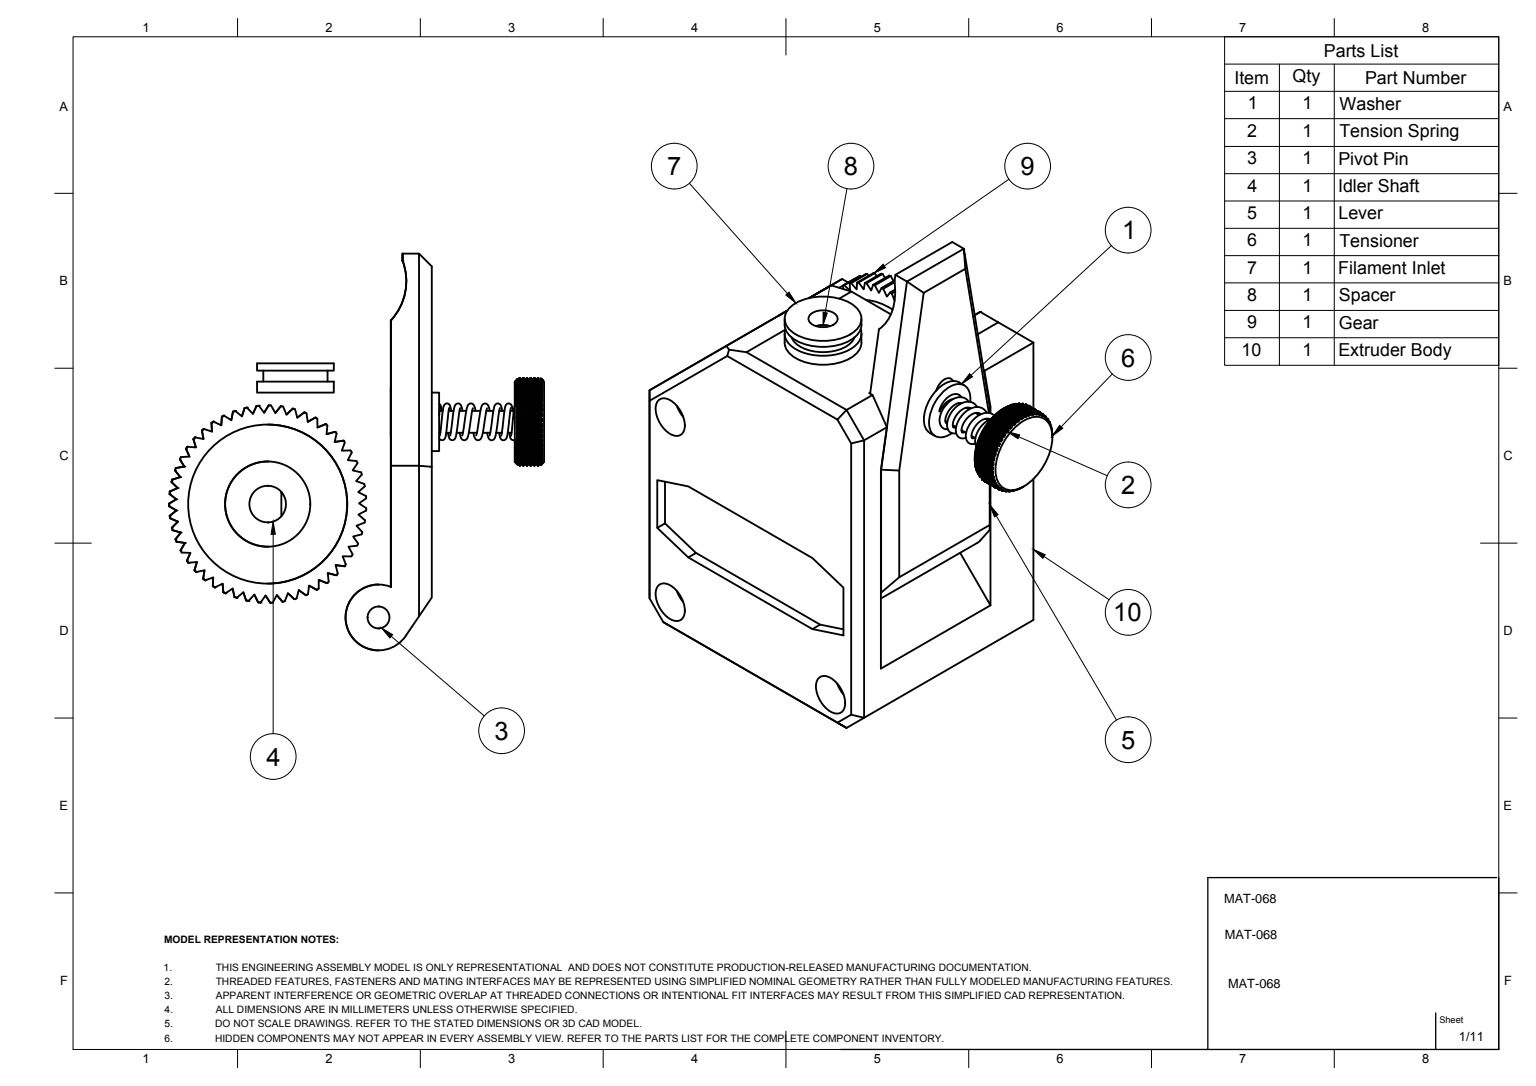
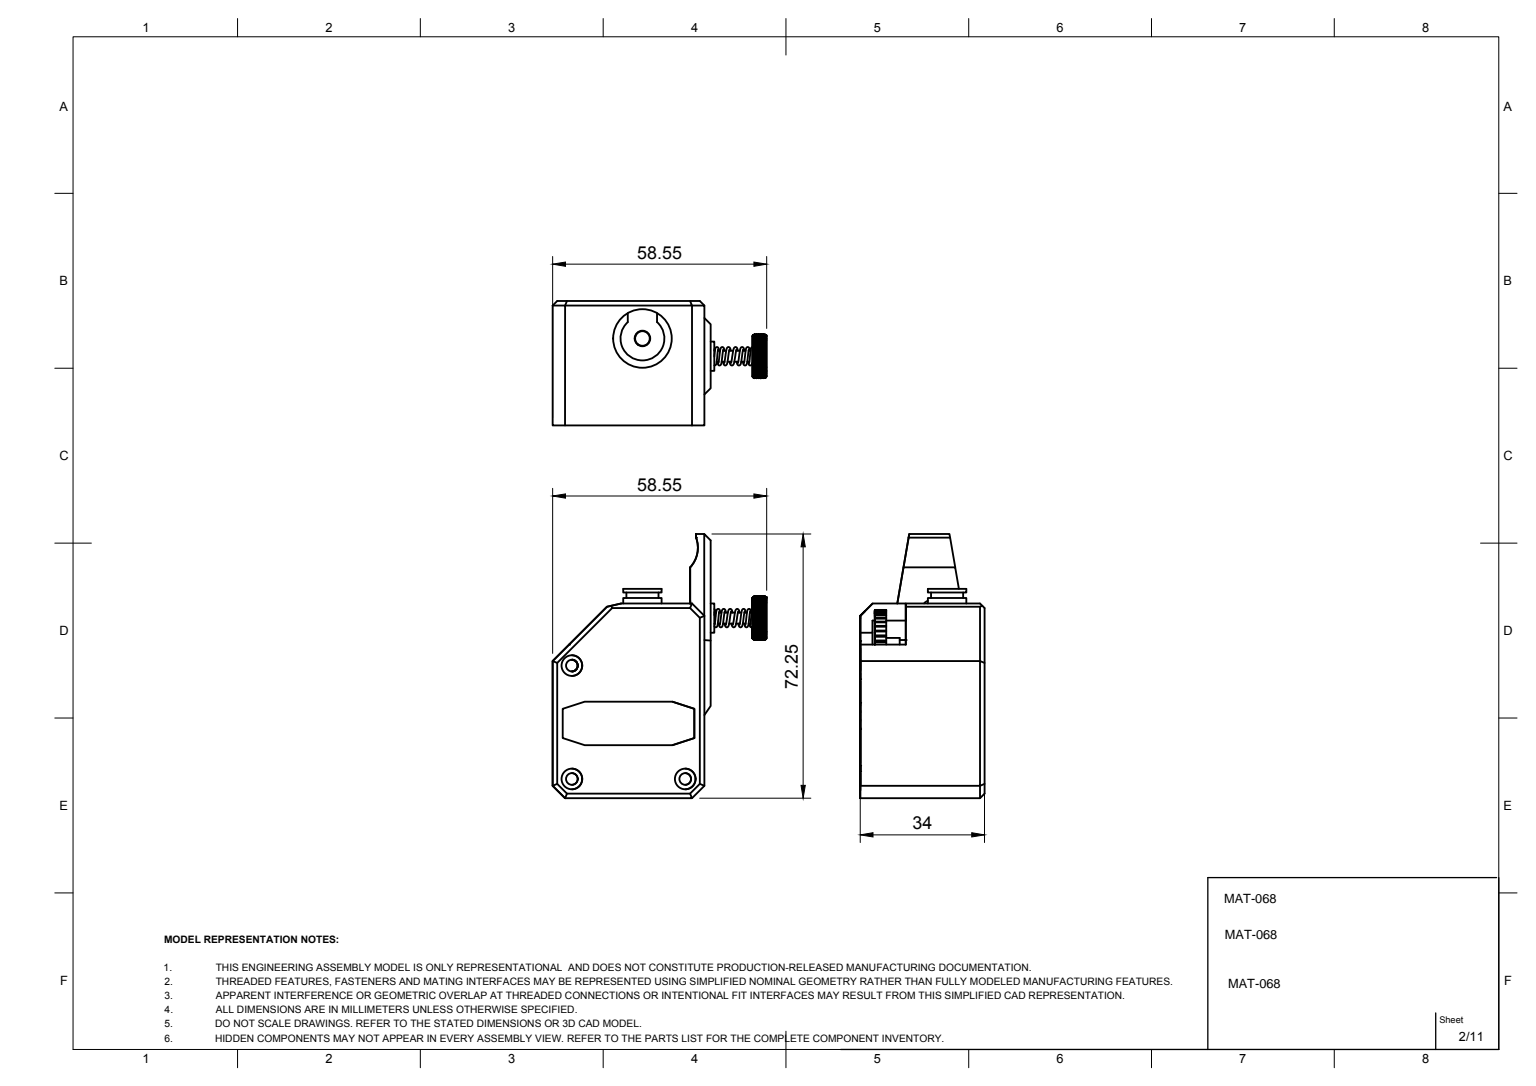
ISO-10303-21;
HEADER;
/* Generated by software containing ST-Developer
 * from STEP Tools, Inc. (www.steptools.com) 
 */

FILE_DESCRIPTION(
/* description */ ('CAx-IF Rec.Pracs.---Representation and Presentation of Product Manufa
cturing Information (PMI)---4.0---2014-10-13'),
/* implementation_level */ '2;1');

FILE_NAME(
/* name */ 'MAT-068',
/* time_stamp */ '2026-10-24T16:53:48-07:00',
/* author */ (''),
/* organization */ (''),
/* preprocessor_version */ 'ST-DEVELOPER v20.2',
/* originating_system */ 'Autodesk Translation Framework v15.17.0.0',
/* authorisation */ '');

FILE_SCHEMA (('AP242_MANAGED_MODEL_BASED_3D_ENGINEERING_MIM_LF { 1 0 10303 442 2 1 4 }'));
ENDSEC;

DATA;
#10=MECHANICAL_DESIGN_GEOMETRIC_PRESENTATION_REPRESENTATION('',(#3489,#3490,
#3491,#3492,#3493,#3494,#3495,#3496,#3497,#3498),#107910);
#11=ITEM_DEFINED_TRANSFORMATION($,$,#45659,#50366);
#12=ITEM_DEFINED_TRANSFORMATION($,$,#45668,#50367);
#13=ITEM_DEFINED_TRANSFORMATION($,$,#45671,#50368);
#14=ITEM_DEFINED_TRANSFORMATION($,$,#45680,#50369);
#15=ITEM_DEFINED_TRANSFORMATION($,$,#45688,#50370);
#16=ITEM_DEFINED_TRANSFORMATION($,$,#45717,#50371);
#17=ITEM_DEFINED_TRANSFORMATION($,$,#49877,#50372);
#18=ITEM_DEFINED_TRANSFORMATION($,$,#49890,#50373);
#19=ITEM_DEFINED_TRANSFORMATION($,$,#49899,#50374);
#20=ITEM_DEFINED_TRANSFORMATION($,$,#50173,#50375);
#21=(
REPRESENTATION_RELATIONSHIP($,$,#107947,#107946)
REPRESENTATION_RELATIONSHIP_WITH_TRANSFORMATION(#11)
SHAPE_REPRESENTATION_RELATIONSHIP()
);
#22=(
REPRESENTATION_RELATIONSHIP($,$,#107948,#107946)
REPRESENTATION_RELATIONSHIP_WITH_TRANSFORMATION(#12)
SHAPE_REPRESENTATION_RELATIONSHIP()
);
#23=(
REPRESENTATION_RELATIONSHIP($,$,#107949,#107946)
REPRESENTATION_RELATIONSHIP_WITH_TRANSFORMATION(#13)
SHAPE_REPRESENTATION_RELATIONSHIP()
);
#24=(
REPRESENTATION_RELATIONSHIP($,$,#107950,#107946)
REPRESENTATION_RELATIONSHIP_WITH_TRANSFORMATION(#14)
SHAPE_REPRESENTATION_RELATIONSHIP()
);
#25=(
REPRESENTATION_RELATIONSHIP($,$,#107951,#107946)
REPRESENTATION_RELATIONSHIP_WITH_TRANSFORMATION(#15)
SHAPE_REPRESENTATION_RELATIONSHIP()
);
#26=(
REPRESENTATION_RELATIONSHIP($,$,#107952,#107946)
REPRESENTATION_RELATIONSHIP_WITH_TRANSFORMATION(#16)
SHAPE_REPRESENTATION_RELATIONSHIP()
);
#27=(
REPRESENTATION_RELATIONSHIP($,$,#107953,#107946)
REPRESENTATION_RELATIONSHIP_WITH_TRANSFORMATION(#17)
SHAPE_REPRESENTATION_RELATIONSHIP()
);
#28=(
REPRESENTATION_RELATIONSHIP($,$,#107954,#107946)
REPRESENTATION_RELATIONSHIP_WITH_TRANSFORMATION(#18)
SHAPE_REPRESENTATION_RELATIONSHIP()
);
#29=(
REPRESENTATION_RELATIONSHIP($,$,#107955,#107946)
REPRESENTATION_RELATIONSHIP_WITH_TRANSFORMATION(#19)
SHAPE_REPRESENTATION_RELATIONSHIP()
);
#30=(
REPRESENTATION_RELATIONSHIP($,$,#107956,#107946)
REPRESENTATION_RELATIONSHIP_WITH_TRANSFORMATION(#20)
SHAPE_REPRESENTATION_RELATIONSHIP()
);
#31=CONTEXT_DEPENDENT_SHAPE_REPRESENTATION(#21,#107936);
#32=CONTEXT_DEPENDENT_SHAPE_REPRESENTATION(#22,#107937);
#33=CONTEXT_DEPENDENT_SHAPE_REPRESENTATION(#23,#107938);
#34=CONTEXT_DEPENDENT_SHAPE_REPRESENTATION(#24,#107939);
#35=CONTEXT_DEPENDENT_SHAPE_REPRESENTATION(#25,#107940);
#36=CONTEXT_DEPENDENT_SHAPE_REPRESENTATION(#26,#107941);
#37=CONTEXT_DEPENDENT_SHAPE_REPRESENTATION(#27,#107942);
#38=CONTEXT_DEPENDENT_SHAPE_REPRESENTATION(#28,#107943);
#39=CONTEXT_DEPENDENT_SHAPE_REPRESENTATION(#29,#107944);
#40=CONTEXT_DEPENDENT_SHAPE_REPRESENTATION(#30,#107945);
#41=NEXT_ASSEMBLY_USAGE_OCCURRENCE('Washer:1','Washer:1','Washer:1',#107958,
#107959,'Washer:1');
#42=NEXT_ASSEMBLY_USAGE_OCCURRENCE('Tension Spring:1',
'Tension Spring:1','Tension Spring:1',#107958,#107960,
'Tension Spring:1');
#43=NEXT_ASSEMBLY_USAGE_OCCURRENCE('Pivot Pin:1','Pivot Pin:1',
'Pivot Pin:1',#107958,#107961,'Pivot Pin:1');
#44=NEXT_ASSEMBLY_USAGE_OCCURRENCE('Idler Shaft:1','Idler Shaft:1',
'Idler Shaft:1',#107958,#107962,'Idler Shaft:1');
#45=NEXT_ASSEMBLY_USAGE_OCCURRENCE('Lever:1','Lever:1','Lever:1',#107958,
#107963,'Lever:1');
#46=NEXT_ASSEMBLY_USAGE_OCCURRENCE('Tensioner:1','Tensioner:1',
'Tensioner:1',#107958,#107964,'Tensioner:1');
#47=NEXT_ASSEMBLY_USAGE_OCCURRENCE('filament inlet:1',
'filament inlet:1','filament inlet:1',#107958,#107965,
'filament inlet:1');
#48=NEXT_ASSEMBLY_USAGE_OCCURRENCE('Spacer:1','Spacer:1','Spacer:1',#107958,
#107966,'Spacer:1');
#49=NEXT_ASSEMBLY_USAGE_OCCURRENCE('Gear:1','Gear:1','Gear:1',#107958,#107967,
'Gear:1');
#50=NEXT_ASSEMBLY_USAGE_OCCURRENCE('Extruder Body:1','Extruder Body:1',
'Extruder Body:1',#107958,#107968,'Extruder Body:1');
#51=(
BOUNDED_CURVE()
B_SPLINE_CURVE(2,(#91091,#91092,#91093,#91094,#91095),.UNSPECIFIED.,.F.,
 .F.)
B_SPLINE_CURVE_WITH_KNOTS((3,2,3),(0.457349576892943,0.480683592164461,
0.539236617436895),.UNSPECIFIED.)
CURVE()
GEOMETRIC_REPRESENTATION_ITEM()
RATIONAL_B_SPLINE_CURVE((0.999326490452302,0.99964606396824,1.,0.999111853439226,
0.998440080679707))
REPRESENTATION_ITEM('')
);
#52=(
BOUNDED_CURVE()
B_SPLINE_CURVE(2,(#91384,#91385,#91386,#91387,#91388),.UNSPECIFIED.,.F.,
 .F.)
B_SPLINE_CURVE_WITH_KNOTS((3,2,3),(0.457349576892961,0.480683592164461,
0.539236615838568),.UNSPECIFIED.)
CURVE()
GEOMETRIC_REPRESENTATION_ITEM()
RATIONAL_B_SPLINE_CURVE((0.999326490452302,0.999646063968241,1.,0.99911185346347,
0.998440080716382))
REPRESENTATION_ITEM('')
);
#53=(
BOUNDED_CURVE()
B_SPLINE_CURVE(2,(#91904,#91905,#91906,#91907,#91908),.UNSPECIFIED.,.F.,
 .F.)
B_SPLINE_CURVE_WITH_KNOTS((3,2,3),(0.457349576892952,0.480683592164462,
0.539236618408897),.UNSPECIFIED.)
CURVE()
GEOMETRIC_REPRESENTATION_ITEM()
RATIONAL_B_SPLINE_CURVE((0.999326490452302,0.999646063968241,1.,0.999111853424483,
0.998440080657404))
REPRESENTATION_ITEM('')
);
#54=(
BOUNDED_CURVE()
B_SPLINE_CURVE(2,(#92179,#92180,#92181,#92182,#92183),.UNSPECIFIED.,.F.,
 .F.)
B_SPLINE_CURVE_WITH_KNOTS((3,2,3),(0.457349576892958,0.480683592164462,
0.539236618408893),.UNSPECIFIED.)
CURVE()
GEOMETRIC_REPRESENTATION_ITEM()
RATIONAL_B_SPLINE_CURVE((0.999326490452302,0.999646063968241,1.,0.999111853424483,
0.998440080657404))
REPRESENTATION_ITEM('')
);
#55=(
BOUNDED_CURVE()
B_SPLINE_CURVE(2,(#92403,#92404,#92405,#92406,#92407),.UNSPECIFIED.,.F.,
 .F.)
B_SPLINE_CURVE_WITH_KNOTS((3,2,3),(0.457349576892958,0.480683592164463,
0.539236618408894),.UNSPECIFIED.)
CURVE()
GEOMETRIC_REPRESENTATION_ITEM()
RATIONAL_B_SPLINE_CURVE((0.999326490452302,0.999646063968241,1.,0.999111853424483,
0.998440080657404))
REPRESENTATION_ITEM('')
);
#56=(
BOUNDED_CURVE()
B_SPLINE_CURVE(2,(#92707,#92708,#92709,#92710,#92711),.UNSPECIFIED.,.F.,
 .F.)
B_SPLINE_CURVE_WITH_KNOTS((3,2,3),(0.457349576892963,0.480683592164461,
0.539236618408894),.UNSPECIFIED.)
CURVE()
GEOMETRIC_REPRESENTATION_ITEM()
RATIONAL_B_SPLINE_CURVE((0.999326490452302,0.999646063968241,1.,0.999111853424483,
0.998440080657404))
REPRESENTATION_ITEM('')
);
#57=(
BOUNDED_CURVE()
B_SPLINE_CURVE(2,(#93011,#93012,#93013,#93014,#93015),.UNSPECIFIED.,.F.,
 .F.)
B_SPLINE_CURVE_WITH_KNOTS((3,2,3),(0.457349576892959,0.480683592164461,
0.539236618408895),.UNSPECIFIED.)
CURVE()
GEOMETRIC_REPRESENTATION_ITEM()
RATIONAL_B_SPLINE_CURVE((0.999326490452302,0.999646063968241,1.,0.999111853424483,
0.998440080657404))
REPRESENTATION_ITEM('')
);
#58=(
BOUNDED_CURVE()
B_SPLINE_CURVE(2,(#93315,#93316,#93317,#93318,#93319),.UNSPECIFIED.,.F.,
 .F.)
B_SPLINE_CURVE_WITH_KNOTS((3,2,3),(0.457349576892959,0.480683592164461,
0.539236615838582),.UNSPECIFIED.)
CURVE()
GEOMETRIC_REPRESENTATION_ITEM()
RATIONAL_B_SPLINE_CURVE((0.999326490452302,0.999646063968241,1.,0.99911185346347,
0.998440080716382))
REPRESENTATION_ITEM('')
);
#59=(
BOUNDED_CURVE()
B_SPLINE_CURVE(2,(#93619,#93620,#93621,#93622,#93623),.UNSPECIFIED.,.F.,
 .F.)
B_SPLINE_CURVE_WITH_KNOTS((3,2,3),(0.457349576892961,0.480683592164461,
0.539236618408892),.UNSPECIFIED.)
CURVE()
GEOMETRIC_REPRESENTATION_ITEM()
RATIONAL_B_SPLINE_CURVE((0.999326490452302,0.999646063968241,1.,0.999111853424483,
0.998440080657404))
REPRESENTATION_ITEM('')
);
#60=(
BOUNDED_CURVE()
B_SPLINE_CURVE(2,(#93923,#93924,#93925,#93926,#93927),.UNSPECIFIED.,.F.,
 .F.)
B_SPLINE_CURVE_WITH_KNOTS((3,2,3),(0.457349576892952,0.480683592164462,
0.539236615838583),.UNSPECIFIED.)
CURVE()
GEOMETRIC_REPRESENTATION_ITEM()
RATIONAL_B_SPLINE_CURVE((0.999326490452302,0.999646063968241,1.,0.99911185346347,
0.998440080716382))
REPRESENTATION_ITEM('')
);
#61=(
BOUNDED_CURVE()
B_SPLINE_CURVE(2,(#94227,#94228,#94229,#94230,#94231),.UNSPECIFIED.,.F.,
 .F.)
B_SPLINE_CURVE_WITH_KNOTS((3,2,3),(0.457349576892963,0.48068359216447,0.539236618408901),
 .UNSPECIFIED.)
CURVE()
GEOMETRIC_REPRESENTATION_ITEM()
RATIONAL_B_SPLINE_CURVE((0.999326490452302,0.999646063968241,1.,0.999111853424483,
0.998440080657404))
REPRESENTATION_ITEM('')
);
#62=(
BOUNDED_CURVE()
B_SPLINE_CURVE(2,(#94531,#94532,#94533,#94534,#94535),.UNSPECIFIED.,.F.,
 .F.)
B_SPLINE_CURVE_WITH_KNOTS((3,2,3),(0.457349576892948,0.48068359216446,0.539236618408892),
 .UNSPECIFIED.)
CURVE()
GEOMETRIC_REPRESENTATION_ITEM()
RATIONAL_B_SPLINE_CURVE((0.999326490452302,0.999646063968241,1.,0.999111853424483,
0.998440080657404))
REPRESENTATION_ITEM('')
);
#63=(
BOUNDED_CURVE()
B_SPLINE_CURVE(2,(#94835,#94836,#94837,#94838,#94839),.UNSPECIFIED.,.F.,
 .F.)
B_SPLINE_CURVE_WITH_KNOTS((3,2,3),(0.457349576892957,0.480683592164462,
0.539236618408896),.UNSPECIFIED.)
CURVE()
GEOMETRIC_REPRESENTATION_ITEM()
RATIONAL_B_SPLINE_CURVE((0.999326490452302,0.999646063968241,1.,0.999111853424483,
0.998440080657404))
REPRESENTATION_ITEM('')
);
#64=(
BOUNDED_CURVE()
B_SPLINE_CURVE(2,(#95139,#95140,#95141,#95142,#95143),.UNSPECIFIED.,.F.,
 .F.)
B_SPLINE_CURVE_WITH_KNOTS((3,2,3),(0.457349576892956,0.48068359216446,0.539236617436898),
 .UNSPECIFIED.)
CURVE()
GEOMETRIC_REPRESENTATION_ITEM()
RATIONAL_B_SPLINE_CURVE((0.999326490452302,0.999646063968241,1.,0.999111853439226,
0.998440080679707))
REPRESENTATION_ITEM('')
);
#65=(
BOUNDED_CURVE()
B_SPLINE_CURVE(2,(#95443,#95444,#95445,#95446,#95447),.UNSPECIFIED.,.F.,
 .F.)
B_SPLINE_CURVE_WITH_KNOTS((3,2,3),(0.457349576892961,0.480683592164473,
0.539236615838594),.UNSPECIFIED.)
CURVE()
GEOMETRIC_REPRESENTATION_ITEM()
RATIONAL_B_SPLINE_CURVE((0.999326490452302,0.999646063968241,1.,0.99911185346347,
0.998440080716382))
REPRESENTATION_ITEM('')
);
#66=(
BOUNDED_CURVE()
B_SPLINE_CURVE(2,(#95747,#95748,#95749,#95750,#95751),.UNSPECIFIED.,.F.,
 .F.)
B_SPLINE_CURVE_WITH_KNOTS((3,2,3),(0.457349576892959,0.480683592164459,
0.539236618408898),.UNSPECIFIED.)
CURVE()
GEOMETRIC_REPRESENTATION_ITEM()
RATIONAL_B_SPLINE_CURVE((0.999326490452302,0.999646063968241,1.,0.999111853424483,
0.998440080657404))
REPRESENTATION_ITEM('')
);
#67=(
BOUNDED_CURVE()
B_SPLINE_CURVE(2,(#96051,#96052,#96053,#96054,#96055),.UNSPECIFIED.,.F.,
 .F.)
B_SPLINE_CURVE_WITH_KNOTS((3,2,3),(0.457349576892962,0.480683592164469,
0.539236618408905),.UNSPECIFIED.)
CURVE()
GEOMETRIC_REPRESENTATION_ITEM()
RATIONAL_B_SPLINE_CURVE((0.999326490452302,0.999646063968241,1.,0.999111853424483,
0.998440080657404))
REPRESENTATION_ITEM('')
);
#68=(
BOUNDED_CURVE()
B_SPLINE_CURVE(2,(#96355,#96356,#96357,#96358,#96359),.UNSPECIFIED.,.F.,
 .F.)
B_SPLINE_CURVE_WITH_KNOTS((3,2,3),(0.457349576892966,0.480683592164469,
0.539236618408905),.UNSPECIFIED.)
CURVE()
GEOMETRIC_REPRESENTATION_ITEM()
RATIONAL_B_SPLINE_CURVE((0.999326490452302,0.999646063968241,1.,0.999111853424483,
0.998440080657404))
REPRESENTATION_ITEM('')
);
#69=(
BOUNDED_CURVE()
B_SPLINE_CURVE(2,(#96659,#96660,#96661,#96662,#96663),.UNSPECIFIED.,.F.,
 .F.)
B_SPLINE_CURVE_WITH_KNOTS((3,2,3),(0.457349576892951,0.48068359216446,0.539236618408896),
 .UNSPECIFIED.)
CURVE()
GEOMETRIC_REPRESENTATION_ITEM()
RATIONAL_B_SPLINE_CURVE((0.999326490452302,0.999646063968241,1.,0.999111853424483,
0.998440080657404))
REPRESENTATION_ITEM('')
);
#70=(
BOUNDED_CURVE()
B_SPLINE_CURVE(2,(#96963,#96964,#96965,#96966,#96967),.UNSPECIFIED.,.F.,
 .F.)
B_SPLINE_CURVE_WITH_KNOTS((3,2,3),(0.457349576892956,0.480683592164461,
0.539236618408896),.UNSPECIFIED.)
CURVE()
GEOMETRIC_REPRESENTATION_ITEM()
RATIONAL_B_SPLINE_CURVE((0.999326490452302,0.999646063968241,1.,0.999111853424483,
0.998440080657404))
REPRESENTATION_ITEM('')
);
#71=(
BOUNDED_CURVE()
B_SPLINE_CURVE(2,(#97267,#97268,#97269,#97270,#97271),.UNSPECIFIED.,.F.,
 .F.)
B_SPLINE_CURVE_WITH_KNOTS((3,2,3),(0.457349576892952,0.480683592164461,
0.539236618408892),.UNSPECIFIED.)
CURVE()
GEOMETRIC_REPRESENTATION_ITEM()
RATIONAL_B_SPLINE_CURVE((0.999326490452302,0.999646063968241,1.,0.999111853424483,
0.998440080657404))
REPRESENTATION_ITEM('')
);
#72=(
BOUNDED_CURVE()
B_SPLINE_CURVE(2,(#97571,#97572,#97573,#97574,#97575),.UNSPECIFIED.,.F.,
 .F.)
B_SPLINE_CURVE_WITH_KNOTS((3,2,3),(0.457349576892964,0.480683592164459,
0.539236618408898),.UNSPECIFIED.)
CURVE()
GEOMETRIC_REPRESENTATION_ITEM()
RATIONAL_B_SPLINE_CURVE((0.999326490452302,0.999646063968241,1.,0.999111853424483,
0.998440080657404))
REPRESENTATION_ITEM('')
);
#73=(
BOUNDED_CURVE()
B_SPLINE_CURVE(2,(#97875,#97876,#97877,#97878,#97879),.UNSPECIFIED.,.F.,
 .F.)
B_SPLINE_CURVE_WITH_KNOTS((3,2,3),(0.457349576892949,0.480683592164462,
0.539236618408898),.UNSPECIFIED.)
CURVE()
GEOMETRIC_REPRESENTATION_ITEM()
RATIONAL_B_SPLINE_CURVE((0.999326490452302,0.999646063968241,1.,0.999111853424483,
0.998440080657404))
REPRESENTATION_ITEM('')
);
#74=(
BOUNDED_CURVE()
B_SPLINE_CURVE(2,(#98179,#98180,#98181,#98182,#98183),.UNSPECIFIED.,.F.,
 .F.)
B_SPLINE_CURVE_WITH_KNOTS((3,2,3),(0.457349576892952,0.48068359216446,0.539236615838581),
 .UNSPECIFIED.)
CURVE()
GEOMETRIC_REPRESENTATION_ITEM()
RATIONAL_B_SPLINE_CURVE((0.999326490452302,0.999646063968241,1.,0.99911185346347,
0.998440080716382))
REPRESENTATION_ITEM('')
);
#75=(
BOUNDED_CURVE()
B_SPLINE_CURVE(2,(#98483,#98484,#98485,#98486,#98487),.UNSPECIFIED.,.F.,
 .F.)
B_SPLINE_CURVE_WITH_KNOTS((3,2,3),(0.457349576892958,0.48068359216446,0.539236618408894),
 .UNSPECIFIED.)
CURVE()
GEOMETRIC_REPRESENTATION_ITEM()
RATIONAL_B_SPLINE_CURVE((0.999326490452302,0.999646063968241,1.,0.999111853424483,
0.998440080657404))
REPRESENTATION_ITEM('')
);
#76=(
BOUNDED_CURVE()
B_SPLINE_CURVE(2,(#98787,#98788,#98789,#98790,#98791),.UNSPECIFIED.,.F.,
 .F.)
B_SPLINE_CURVE_WITH_KNOTS((3,2,3),(0.457349576892947,0.480683592164461,
0.539236617436902),.UNSPECIFIED.)
CURVE()
GEOMETRIC_REPRESENTATION_ITEM()
RATIONAL_B_SPLINE_CURVE((0.999326490452302,0.999646063968241,1.,0.999111853439226,
0.998440080679707))
REPRESENTATION_ITEM('')
);
#77=(
BOUNDED_CURVE()
B_SPLINE_CURVE(2,(#99091,#99092,#99093,#99094,#99095),.UNSPECIFIED.,.F.,
 .F.)
B_SPLINE_CURVE_WITH_KNOTS((3,2,3),(0.457349576892974,0.48068359216447,0.539236615838595),
 .UNSPECIFIED.)
CURVE()
GEOMETRIC_REPRESENTATION_ITEM()
RATIONAL_B_SPLINE_CURVE((0.999326490452302,0.999646063968241,1.,0.99911185346347,
0.998440080716382))
REPRESENTATION_ITEM('')
);
#78=(
BOUNDED_CURVE()
B_SPLINE_CURVE(2,(#99395,#99396,#99397,#99398,#99399),.UNSPECIFIED.,.F.,
 .F.)
B_SPLINE_CURVE_WITH_KNOTS((3,2,3),(0.457349576892952,0.480683592164461,
0.539236615838591),.UNSPECIFIED.)
CURVE()
GEOMETRIC_REPRESENTATION_ITEM()
RATIONAL_B_SPLINE_CURVE((0.999326490452302,0.999646063968241,1.,0.99911185346347,
0.998440080716382))
REPRESENTATION_ITEM('')
);
#79=(
BOUNDED_CURVE()
B_SPLINE_CURVE(2,(#99699,#99700,#99701,#99702,#99703),.UNSPECIFIED.,.F.,
 .F.)
B_SPLINE_CURVE_WITH_KNOTS((3,2,3),(0.457349576892966,0.480683592164471,
0.539236615838593),.UNSPECIFIED.)
CURVE()
GEOMETRIC_REPRESENTATION_ITEM()
RATIONAL_B_SPLINE_CURVE((0.999326490452302,0.999646063968241,1.,0.99911185346347,
0.998440080716382))
REPRESENTATION_ITEM('')
);
#80=(
BOUNDED_CURVE()
B_SPLINE_CURVE(2,(#100003,#100004,#100005,#100006,#100007),
 .UNSPECIFIED.,.F.,.F.)
B_SPLINE_CURVE_WITH_KNOTS((3,2,3),(0.457349576892955,0.48068359216446,0.539236618408892),
 .UNSPECIFIED.)
CURVE()
GEOMETRIC_REPRESENTATION_ITEM()
RATIONAL_B_SPLINE_CURVE((0.999326490452302,0.999646063968241,1.,0.999111853424483,
0.998440080657404))
REPRESENTATION_ITEM('')
);
#81=(
BOUNDED_CURVE()
B_SPLINE_CURVE(2,(#100307,#100308,#100309,#100310,#100311),
 .UNSPECIFIED.,.F.,.F.)
B_SPLINE_CURVE_WITH_KNOTS((3,2,3),(0.457349576892948,0.480683592164461,
0.539236618408894),.UNSPECIFIED.)
CURVE()
GEOMETRIC_REPRESENTATION_ITEM()
RATIONAL_B_SPLINE_CURVE((0.999326490452302,0.999646063968241,1.,0.999111853424483,
0.998440080657404))
REPRESENTATION_ITEM('')
);
#82=(
BOUNDED_CURVE()
B_SPLINE_CURVE(2,(#100611,#100612,#100613,#100614,#100615),
 .UNSPECIFIED.,.F.,.F.)
B_SPLINE_CURVE_WITH_KNOTS((3,2,3),(0.457349576892958,0.480683592164462,
0.539236615838579),.UNSPECIFIED.)
CURVE()
GEOMETRIC_REPRESENTATION_ITEM()
RATIONAL_B_SPLINE_CURVE((0.999326490452302,0.999646063968241,1.,0.99911185346347,
0.998440080716382))
REPRESENTATION_ITEM('')
);
#83=(
BOUNDED_CURVE()
B_SPLINE_CURVE(2,(#100915,#100916,#100917,#100918,#100919),
 .UNSPECIFIED.,.F.,.F.)
B_SPLINE_CURVE_WITH_KNOTS((3,2,3),(0.457349576892956,0.48068359216446,0.539236618408897),
 .UNSPECIFIED.)
CURVE()
GEOMETRIC_REPRESENTATION_ITEM()
RATIONAL_B_SPLINE_CURVE((0.999326490452302,0.999646063968241,1.,0.999111853424483,
0.998440080657404))
REPRESENTATION_ITEM('')
);
#84=(
BOUNDED_CURVE()
B_SPLINE_CURVE(2,(#101219,#101220,#101221,#101222,#101223),
 .UNSPECIFIED.,.F.,.F.)
B_SPLINE_CURVE_WITH_KNOTS((3,2,3),(0.457349576892958,0.480683592164462,
0.539236618408895),.UNSPECIFIED.)
CURVE()
GEOMETRIC_REPRESENTATION_ITEM()
RATIONAL_B_SPLINE_CURVE((0.999326490452302,0.999646063968241,1.,0.999111853424483,
0.998440080657404))
REPRESENTATION_ITEM('')
);
#85=(
BOUNDED_CURVE()
B_SPLINE_CURVE(2,(#101523,#101524,#101525,#101526,#101527),
 .UNSPECIFIED.,.F.,.F.)
B_SPLINE_CURVE_WITH_KNOTS((3,2,3),(0.457349576892956,0.480683592164458,
0.539236615838573),.UNSPECIFIED.)
CURVE()
GEOMETRIC_REPRESENTATION_ITEM()
RATIONAL_B_SPLINE_CURVE((0.999326490452302,0.999646063968241,1.,0.99911185346347,
0.998440080716382))
REPRESENTATION_ITEM('')
);
#86=(
BOUNDED_CURVE()
B_SPLINE_CURVE(2,(#101827,#101828,#101829,#101830,#101831),
 .UNSPECIFIED.,.F.,.F.)
B_SPLINE_CURVE_WITH_KNOTS((3,2,3),(0.457349576892953,0.48068359216446,0.539236618408898),
 .UNSPECIFIED.)
CURVE()
GEOMETRIC_REPRESENTATION_ITEM()
RATIONAL_B_SPLINE_CURVE((0.999326490452302,0.999646063968241,1.,0.999111853424483,
0.998440080657404))
REPRESENTATION_ITEM('')
);
#87=(
BOUNDED_CURVE()
B_SPLINE_CURVE(2,(#102131,#102132,#102133,#102134,#102135),
 .UNSPECIFIED.,.F.,.F.)
B_SPLINE_CURVE_WITH_KNOTS((3,2,3),(0.457349576892963,0.480683592164461,
0.539236618408896),.UNSPECIFIED.)
CURVE()
GEOMETRIC_REPRESENTATION_ITEM()
RATIONAL_B_SPLINE_CURVE((0.999326490452302,0.999646063968241,1.,0.999111853424483,
0.998440080657404))
REPRESENTATION_ITEM('')
);
#88=(
BOUNDED_CURVE()
B_SPLINE_CURVE(2,(#102435,#102436,#102437,#102438,#102439),
 .UNSPECIFIED.,.F.,.F.)
B_SPLINE_CURVE_WITH_KNOTS((3,2,3),(0.457349576892965,0.480683592164474,
0.539236615838598),.UNSPECIFIED.)
CURVE()
GEOMETRIC_REPRESENTATION_ITEM()
RATIONAL_B_SPLINE_CURVE((0.999326490452302,0.999646063968241,1.,0.99911185346347,
0.998440080716382))
REPRESENTATION_ITEM('')
);
#89=(
BOUNDED_CURVE()
B_SPLINE_CURVE(2,(#102739,#102740,#102741,#102742,#102743),
 .UNSPECIFIED.,.F.,.F.)
B_SPLINE_CURVE_WITH_KNOTS((3,2,3),(0.457349576892951,0.480683592164463,
0.5392366174369),.UNSPECIFIED.)
CURVE()
GEOMETRIC_REPRESENTATION_ITEM()
RATIONAL_B_SPLINE_CURVE((0.999326490452302,0.999646063968241,1.,0.999111853439226,
0.998440080679707))
REPRESENTATION_ITEM('')
);
#90=(
BOUNDED_CURVE()
B_SPLINE_CURVE(2,(#103043,#103044,#103045,#103046,#103047),
 .UNSPECIFIED.,.F.,.F.)
B_SPLINE_CURVE_WITH_KNOTS((3,2,3),(0.45734957689296,0.480683592164459,0.539236618408886),
 .UNSPECIFIED.)
CURVE()
GEOMETRIC_REPRESENTATION_ITEM()
RATIONAL_B_SPLINE_CURVE((0.999326490452302,0.999646063968241,1.,0.999111853424483,
0.998440080657404))
REPRESENTATION_ITEM('')
);
#91=(
BOUNDED_CURVE()
B_SPLINE_CURVE(2,(#103347,#103348,#103349,#103350,#103351),
 .UNSPECIFIED.,.F.,.F.)
B_SPLINE_CURVE_WITH_KNOTS((3,2,3),(0.457349576892963,0.48068359216447,0.5392366184089),
 .UNSPECIFIED.)
CURVE()
GEOMETRIC_REPRESENTATION_ITEM()
RATIONAL_B_SPLINE_CURVE((0.999326490452302,0.999646063968241,1.,0.999111853424483,
0.998440080657404))
REPRESENTATION_ITEM('')
);
#92=(
BOUNDED_CURVE()
B_SPLINE_CURVE(2,(#103651,#103652,#103653,#103654,#103655),
 .UNSPECIFIED.,.F.,.F.)
B_SPLINE_CURVE_WITH_KNOTS((3,2,3),(0.457349576892972,0.480683592164467,
0.539236618408904),.UNSPECIFIED.)
CURVE()
GEOMETRIC_REPRESENTATION_ITEM()
RATIONAL_B_SPLINE_CURVE((0.999326490452302,0.999646063968241,1.,0.999111853424483,
0.998440080657404))
REPRESENTATION_ITEM('')
);
#93=(
BOUNDED_CURVE()
B_SPLINE_CURVE(2,(#103955,#103956,#103957,#103958,#103959),
 .UNSPECIFIED.,.F.,.F.)
B_SPLINE_CURVE_WITH_KNOTS((3,2,3),(0.457349576892955,0.480683592164463,
0.539236618408902),.UNSPECIFIED.)
CURVE()
GEOMETRIC_REPRESENTATION_ITEM()
RATIONAL_B_SPLINE_CURVE((0.999326490452302,0.999646063968241,1.,0.999111853424483,
0.998440080657404))
REPRESENTATION_ITEM('')
);
#94=(
BOUNDED_CURVE()
B_SPLINE_CURVE(2,(#104259,#104260,#104261,#104262,#104263),
 .UNSPECIFIED.,.F.,.F.)
B_SPLINE_CURVE_WITH_KNOTS((3,2,3),(0.457349576892956,0.48068359216446,0.539236618408889),
 .UNSPECIFIED.)
CURVE()
GEOMETRIC_REPRESENTATION_ITEM()
RATIONAL_B_SPLINE_CURVE((0.999326490452302,0.999646063968241,1.,0.999111853424483,
0.998440080657404))
REPRESENTATION_ITEM('')
);
#95=(
BOUNDED_CURVE()
B_SPLINE_CURVE(2,(#104563,#104564,#104565,#104566,#104567),
 .UNSPECIFIED.,.F.,.F.)
B_SPLINE_CURVE_WITH_KNOTS((3,2,3),(0.457349576892965,0.480683592164471,
0.539236618408903),.UNSPECIFIED.)
CURVE()
GEOMETRIC_REPRESENTATION_ITEM()
RATIONAL_B_SPLINE_CURVE((0.999326490452302,0.999646063968241,1.,0.999111853424483,
0.998440080657404))
REPRESENTATION_ITEM('')
);
#96=(
BOUNDED_CURVE()
B_SPLINE_CURVE(2,(#104867,#104868,#104869,#104870,#104871),
 .UNSPECIFIED.,.F.,.F.)
B_SPLINE_CURVE_WITH_KNOTS((3,2,3),(0.457349576892956,0.480683592164462,
0.539236618408896),.UNSPECIFIED.)
CURVE()
GEOMETRIC_REPRESENTATION_ITEM()
RATIONAL_B_SPLINE_CURVE((0.999326490452302,0.999646063968241,1.,0.999111853424483,
0.998440080657404))
REPRESENTATION_ITEM('')
);
#97=(
BOUNDED_CURVE()
B_SPLINE_CURVE(2,(#105171,#105172,#105173,#105174,#105175),
 .UNSPECIFIED.,.F.,.F.)
B_SPLINE_CURVE_WITH_KNOTS((3,2,3),(0.45734957689296,0.480683592164462,0.539236618408894),
 .UNSPECIFIED.)
CURVE()
GEOMETRIC_REPRESENTATION_ITEM()
RATIONAL_B_SPLINE_CURVE((0.999326490452302,0.999646063968241,1.,0.999111853424483,
0.998440080657404))
REPRESENTATION_ITEM('')
);
#98=(
BOUNDED_CURVE()
B_SPLINE_CURVE(2,(#105475,#105476,#105477,#105478,#105479),
 .UNSPECIFIED.,.F.,.F.)
B_SPLINE_CURVE_WITH_KNOTS((3,2,3),(0.457349576892957,0.480683592164459,
0.539236618408901),.UNSPECIFIED.)
CURVE()
GEOMETRIC_REPRESENTATION_ITEM()
RATIONAL_B_SPLINE_CURVE((0.999326490452302,0.999646063968241,1.,0.999111853424483,
0.998440080657404))
REPRESENTATION_ITEM('')
);
#99=(
BOUNDED_CURVE()
B_SPLINE_CURVE(2,(#105779,#105780,#105781,#105782,#105783),
 .UNSPECIFIED.,.F.,.F.)
B_SPLINE_CURVE_WITH_KNOTS((3,2,3),(0.457349576892957,0.480683592164462,
0.539236615838586),.UNSPECIFIED.)
CURVE()
GEOMETRIC_REPRESENTATION_ITEM()
RATIONAL_B_SPLINE_CURVE((0.999326490452302,0.999646063968241,1.,0.99911185346347,
0.998440080716382))
REPRESENTATION_ITEM('')
);
#100=(
BOUNDED_CURVE()
B_SPLINE_CURVE(2,(#106083,#106084,#106085,#106086,#106087),
 .UNSPECIFIED.,.F.,.F.)
B_SPLINE_CURVE_WITH_KNOTS((3,2,3),(0.457349576892964,0.480683592164471,
0.539236615838594),.UNSPECIFIED.)
CURVE()
GEOMETRIC_REPRESENTATION_ITEM()
RATIONAL_B_SPLINE_CURVE((0.999326490452302,0.999646063968241,1.,0.99911185346347,
0.998440080716382))
REPRESENTATION_ITEM('')
);
#101=(
BOUNDED_SURFACE()
B_SPLINE_SURFACE(1,2,((#65259,#65260,#65261),(#65262,#65263,#65264)),
 .UNSPECIFIED.,.F.,.F.,.F.)
B_SPLINE_SURFACE_WITH_KNOTS((2,2),(3,3),(0.,1.),(0.0556006976418392,0.0675888856590501),
 .UNSPECIFIED.)
GEOMETRIC_REPRESENTATION_ITEM()
RATIONAL_B_SPLINE_SURFACE(((0.996397562408606,0.996150386832629,0.997319912843745),
(0.996397562408606,0.996150386832629,0.997319912843745)))
REPRESENTATION_ITEM('')
SURFACE()
);
#102=(
BOUNDED_SURFACE()
B_SPLINE_SURFACE(1,2,((#65277,#65278,#65279),(#65280,#65281,#65282),(#65283,
#65284,#65285)),.UNSPECIFIED.,.F.,.F.,.F.)
B_SPLINE_SURFACE_WITH_KNOTS((2,1,2),(3,3),(-0.000171761237665326,1.,1.00600020634817),
(0.066589869885605,0.0751324139155164),.UNSPECIFIED.)
GEOMETRIC_REPRESENTATION_ITEM()
RATIONAL_B_SPLINE_SURFACE(((0.997134830028878,0.997884084852412,0.999352698774608),
(0.997134830028878,0.997884084852412,0.999352698774608),(0.997134830028879,
0.997884084852412,0.999352698774608)))
REPRESENTATION_ITEM('')
SURFACE()
);
#103=(
BOUNDED_SURFACE()
B_SPLINE_SURFACE(1,2,((#65395,#65396,#65397),(#65398,#65399,#65400),(#65401,
#65402,#65403)),.UNSPECIFIED.,.F.,.F.,.F.)
B_SPLINE_SURFACE_WITH_KNOTS((2,1,2),(3,3),(0.,1.,1.01),(0.0456081671210044,
0.057598944781882),.UNSPECIFIED.)
GEOMETRIC_REPRESENTATION_ITEM()
RATIONAL_B_SPLINE_SURFACE(((0.997793907739636,0.996365558499688,0.996354522974128),
(0.997793907739636,0.996365558499688,0.996354522974128),(0.997793907739636,
0.996365558499688,0.996354522974128)))
REPRESENTATION_ITEM('')
SURFACE()
);
#104=(
BOUNDED_SURFACE()
B_SPLINE_SURFACE(1,2,((#65416,#65417,#65418),(#65419,#65420,#65421),(#65422,
#65423,#65424)),.UNSPECIFIED.,.F.,.F.,.F.)
B_SPLINE_SURFACE_WITH_KNOTS((2,1,2),(3,3),(0.,1.,1.01),(0.0556006976418428,
0.0675888856590486),.UNSPECIFIED.)
GEOMETRIC_REPRESENTATION_ITEM()
RATIONAL_B_SPLINE_SURFACE(((0.996397562408606,0.996150386832629,0.997319912843744),
(0.996397562408606,0.996150386832629,0.997319912843744),(0.996397562408606,
0.996150386832629,0.997319912843744)))
REPRESENTATION_ITEM('')
SURFACE()
);
#105=(
BOUNDED_SURFACE()
B_SPLINE_SURFACE(1,2,((#65482,#65483,#65484),(#65485,#65486,#65487),(#65488,
#65489,#65490)),.UNSPECIFIED.,.F.,.F.,.F.)
B_SPLINE_SURFACE_WITH_KNOTS((2,1,2),(3,3),(-0.00286810173538045,0.,0.477902879811279),
(0.0466073985929118,0.053183492915798),.UNSPECIFIED.)
GEOMETRIC_REPRESENTATION_ITEM()
RATIONAL_B_SPLINE_SURFACE(((0.997565691989291,0.996847118055594,0.996554836292953),
(0.997565691989291,0.996847118055594,0.996554836292953),(0.997565691989291,
0.996847118055594,0.996554836292953)))
REPRESENTATION_ITEM('')
SURFACE()
);
#106=(
BOUNDED_SURFACE()
B_SPLINE_SURFACE(1,2,((#65501,#65502,#65503),(#65504,#65505,#65506),(#65507,
#65508,#65509)),.UNSPECIFIED.,.F.,.F.,.F.)
B_SPLINE_SURFACE_WITH_KNOTS((2,1,2),(3,3),(-0.00286764392039102,0.,0.477902879807514),
(0.0565997133101203,0.0631721430887056),.UNSPECIFIED.)
GEOMETRIC_REPRESENTATION_ITEM()
RATIONAL_B_SPLINE_SURFACE(((0.996366204684738,0.996295417244646,0.996650447003324),
(0.996366204684738,0.996295417244646,0.996650447003324),(0.996366204684738,
0.996295417244646,0.996650447003324)))
REPRESENTATION_ITEM('')
SURFACE()
);
#107=(
BOUNDED_SURFACE()
B_SPLINE_SURFACE(1,2,((#65532,#65533,#65534,#65535,#65536),(#65537,#65538,
#65539,#65540,#65541),(#65542,#65543,#65544,#65545,#65546)),
 .UNSPECIFIED.,.F.,.F.,.F.)
B_SPLINE_SURFACE_WITH_KNOTS((2,1,2),(3,2,3),(0.,1.,1.01),(0.03559319327139,
0.0384615384615384,0.0476086899858148),.UNSPECIFIED.)
GEOMETRIC_REPRESENTATION_ITEM()
RATIONAL_B_SPLINE_SURFACE(((0.998993602249807,0.999456249886298,1.,0.9982659811314,
0.997356751596327),(0.998993602249807,0.999456249886298,1.,0.9982659811314,
0.997356751596327),(0.998993602249807,0.999456249886298,1.,0.9982659811314,
0.997356751596327)))
REPRESENTATION_ITEM('')
SURFACE()
);
#108=(
BOUNDED_SURFACE()
B_SPLINE_SURFACE(1,2,((#65572,#65573,#65574),(#65575,#65576,#65577)),
 .UNSPECIFIED.,.F.,.F.,.F.)
B_SPLINE_SURFACE_WITH_KNOTS((2,2),(3,3),(0.,1.),(0.0456081671210079,0.0575989447818804),
 .UNSPECIFIED.)
GEOMETRIC_REPRESENTATION_ITEM()
RATIONAL_B_SPLINE_SURFACE(((0.997793907739635,0.996365558499688,0.996354522974128),
(0.997793907739635,0.996365558499688,0.996354522974128)))
REPRESENTATION_ITEM('')
SURFACE()
);
#109=(
BOUNDED_SURFACE()
B_SPLINE_SURFACE(1,2,((#65635,#65636,#65637,#65638,#65639),(#65640,#65641,
#65642,#65643,#65644),(#65645,#65646,#65647,#65648,#65649)),
 .UNSPECIFIED.,.F.,.F.,.F.)
B_SPLINE_SURFACE_WITH_KNOTS((2,1,2),(3,2,3),(-0.00286743094908464,0.,0.480770297171449),
(0.0365944846643089,0.0384615384615384,0.0431859280915203),
 .UNSPECIFIED.)
GEOMETRIC_REPRESENTATION_ITEM()
RATIONAL_B_SPLINE_SURFACE(((0.999326490452167,0.999646063968166,1.,0.999104400890347,
0.9984288220563),(0.999326490452167,0.999646063968166,1.,0.999104400890347,
0.9984288220563),(0.999326490452167,0.999646063968166,1.,0.999104400890347,
0.9984288220563)))
REPRESENTATION_ITEM('')
SURFACE()
);
#110=(
BOUNDED_SURFACE()
B_SPLINE_SURFACE(1,2,((#65665,#65666,#65667),(#65668,#65669,#65670),(#65671,
#65672,#65673)),.UNSPECIFIED.,.F.,.F.,.F.)
B_SPLINE_SURFACE_WITH_KNOTS((2,1,2),(3,3),(-0.0028681017738025,0.,0.477902879812032),
(0.046607398592911,0.0531834933545499),.UNSPECIFIED.)
GEOMETRIC_REPRESENTATION_ITEM()
RATIONAL_B_SPLINE_SURFACE(((0.997565691989291,0.99684711800765,0.996554836253951),
(0.997565691989291,0.99684711800765,0.996554836253951),(0.997565691989291,
0.99684711800765,0.996554836253951)))
REPRESENTATION_ITEM('')
SURFACE()
);
#111=(
BOUNDED_SURFACE()
B_SPLINE_SURFACE(1,2,((#65701,#65702,#65703),(#65704,#65705,#65706)),
 .UNSPECIFIED.,.F.,.F.,.F.)
B_SPLINE_SURFACE_WITH_KNOTS((2,2),(3,3),(0.,1.),(0.0255903596131799,0.0375948596693886),
 .UNSPECIFIED.)
GEOMETRIC_REPRESENTATION_ITEM()
RATIONAL_B_SPLINE_SURFACE(((0.996753121755999,0.997505687613148,0.999678813023854),
(0.996753121755999,0.997505687613148,0.999678813023854)))
REPRESENTATION_ITEM('')
SURFACE()
);
#112=(
BOUNDED_SURFACE()
B_SPLINE_SURFACE(1,2,((#65719,#65720,#65721,#65722,#65723),(#65724,#65725,
#65726,#65727,#65728),(#65729,#65730,#65731,#65732,#65733)),
 .UNSPECIFIED.,.F.,.F.,.F.)
B_SPLINE_SURFACE_WITH_KNOTS((2,1,2),(3,2,3),(0.,1.,1.01),(0.0355931932713904,
0.0384615384615384,0.0476086899858121),.UNSPECIFIED.)
GEOMETRIC_REPRESENTATION_ITEM()
RATIONAL_B_SPLINE_SURFACE(((0.998993602249807,0.999456249886298,1.,0.998265981131401,
0.997356751596327),(0.998993602249807,0.999456249886298,1.,0.998265981131401,
0.997356751596327),(0.998993602249807,0.999456249886298,1.,0.998265981131401,
0.997356751596327)))
REPRESENTATION_ITEM('')
SURFACE()
);
#113=(
BOUNDED_SURFACE()
B_SPLINE_SURFACE(1,2,((#65830,#65831,#65832,#65833,#65834),(#65835,#65836,
#65837,#65838,#65839)),.UNSPECIFIED.,.F.,.F.,.F.)
B_SPLINE_SURFACE_WITH_KNOTS((2,2),(3,2,3),(0.,0.480770297146589),(0.0365944846642941,
0.0384615384615384,0.0431859280915188),.UNSPECIFIED.)
GEOMETRIC_REPRESENTATION_ITEM()
RATIONAL_B_SPLINE_SURFACE(((0.999326490452162,0.999646063968163,1.,0.999104400890347,
0.9984288220563),(0.999326490452162,0.999646063968163,1.,0.999104400890347,
0.9984288220563)))
REPRESENTATION_ITEM('')
SURFACE()
);
#114=(
BOUNDED_SURFACE()
B_SPLINE_SURFACE(1,2,((#65900,#65901,#65902),(#65903,#65904,#65905),(#65906,
#65907,#65908)),.UNSPECIFIED.,.F.,.F.,.F.)
B_SPLINE_SURFACE_WITH_KNOTS((2,1,2),(3,3),(-0.01,0.,1.),(0.0255903596131809,
0.0375948596693858),.UNSPECIFIED.)
GEOMETRIC_REPRESENTATION_ITEM()
RATIONAL_B_SPLINE_SURFACE(((0.996753121755999,0.997505687613148,0.999678813023853),
(0.996753121755999,0.997505687613148,0.999678813023853),(0.996753121755999,
0.997505687613148,0.999678813023853)))
REPRESENTATION_ITEM('')
SURFACE()
);
#115=(
BOUNDED_SURFACE()
B_SPLINE_SURFACE(1,2,((#66030,#66031,#66032),(#66033,#66034,#66035),(#66036,
#66037,#66038)),.UNSPECIFIED.,.F.,.F.,.F.)
B_SPLINE_SURFACE_WITH_KNOTS((2,1,2),(3,3),(-0.01,0.,1.00000001517992),(0.00560769168370699,
0.0176009700440532),.UNSPECIFIED.)
GEOMETRIC_REPRESENTATION_ITEM()
RATIONAL_B_SPLINE_SURFACE(((0.99818389211382,0.99657330421516,0.996380621259469),
(0.99818389211382,0.99657330421516,0.996380621259469),(0.99818389211382,
0.99657330421516,0.996380621259469)))
REPRESENTATION_ITEM('')
SURFACE()
);
#116=(
BOUNDED_SURFACE()
B_SPLINE_SURFACE(1,2,((#66180,#66181,#66182),(#66183,#66184,#66185),(#66186,
#66187,#66188)),.UNSPECIFIED.,.F.,.F.,.F.)
B_SPLINE_SURFACE_WITH_KNOTS((2,1,2),(3,3),(-0.01,0.,1.00000001523837),(0.0056076916836887,
0.0176009700440532),.UNSPECIFIED.)
GEOMETRIC_REPRESENTATION_ITEM()
RATIONAL_B_SPLINE_SURFACE(((0.998183892113825,0.99657330421516,0.996380621259469),
(0.998183892113825,0.99657330421516,0.996380621259469),(0.998183892113825,
0.99657330421516,0.996380621259469)))
REPRESENTATION_ITEM('')
SURFACE()
);
#117=(
BOUNDED_SURFACE()
B_SPLINE_SURFACE(1,2,((#66306,#66307,#66308),(#66309,#66310,#66311)),
 .UNSPECIFIED.,.F.,.F.,.F.)
B_SPLINE_SURFACE_WITH_KNOTS((2,2),(3,3),(0.,1.),(0.0556006976418416,0.0675888856590493),
 .UNSPECIFIED.)
GEOMETRIC_REPRESENTATION_ITEM()
RATIONAL_B_SPLINE_SURFACE(((0.996397562408606,0.996150386832629,0.997319912843745),
(0.996397562408606,0.996150386832629,0.997319912843745)))
REPRESENTATION_ITEM('')
SURFACE()
);
#118=(
BOUNDED_SURFACE()
B_SPLINE_SURFACE(1,2,((#66374,#66375,#66376),(#66377,#66378,#66379),(#66380,
#66381,#66382)),.UNSPECIFIED.,.F.,.F.,.F.)
B_SPLINE_SURFACE_WITH_KNOTS((2,1,2),(3,3),(0.,1.,1.01),(0.0456081671210036,
0.0575989447818809),.UNSPECIFIED.)
GEOMETRIC_REPRESENTATION_ITEM()
RATIONAL_B_SPLINE_SURFACE(((0.997793907739636,0.996365558499688,0.996354522974128),
(0.997793907739636,0.996365558499688,0.996354522974128),(0.997793907739636,
0.996365558499688,0.996354522974128)))
REPRESENTATION_ITEM('')
SURFACE()
);
#119=(
BOUNDED_SURFACE()
B_SPLINE_SURFACE(1,2,((#66394,#66395,#66396),(#66397,#66398,#66399),(#66400,
#66401,#66402)),.UNSPECIFIED.,.F.,.F.,.F.)
B_SPLINE_SURFACE_WITH_KNOTS((2,1,2),(3,3),(-0.00286810173540422,0.,0.477902879809766),
(0.0466073985929115,0.0531834929157974),.UNSPECIFIED.)
GEOMETRIC_REPRESENTATION_ITEM()
RATIONAL_B_SPLINE_SURFACE(((0.997565691989291,0.996847118055594,0.996554836292953),
(0.997565691989291,0.996847118055594,0.996554836292953),(0.997565691989291,
0.996847118055593,0.996554836292953)))
REPRESENTATION_ITEM('')
SURFACE()
);
#120=(
BOUNDED_SURFACE()
B_SPLINE_SURFACE(1,2,((#66448,#66449,#66450,#66451,#66452),(#66453,#66454,
#66455,#66456,#66457),(#66458,#66459,#66460,#66461,#66462)),
 .UNSPECIFIED.,.F.,.F.,.F.)
B_SPLINE_SURFACE_WITH_KNOTS((2,1,2),(3,2,3),(0.,1.,1.01),(0.0355931932713902,
0.0384615384615384,0.0476086899858131),.UNSPECIFIED.)
GEOMETRIC_REPRESENTATION_ITEM()
RATIONAL_B_SPLINE_SURFACE(((0.998993602249807,0.999456249886298,1.,0.998265981131401,
0.997356751596327),(0.998993602249807,0.999456249886298,1.,0.998265981131401,
0.997356751596327),(0.998993602249807,0.999456249886298,1.,0.998265981131401,
0.997356751596327)))
REPRESENTATION_ITEM('')
SURFACE()
);
#121=(
BOUNDED_SURFACE()
B_SPLINE_SURFACE(1,2,((#66510,#66511,#66512,#66513,#66514),(#66515,#66516,
#66517,#66518,#66519),(#66520,#66521,#66522,#66523,#66524)),
 .UNSPECIFIED.,.F.,.F.,.F.)
B_SPLINE_SURFACE_WITH_KNOTS((2,1,2),(3,2,3),(-0.00286743095031093,0.,0.480770297170425),
(0.0365944846643235,0.0384615384615384,0.0431859280915194),
 .UNSPECIFIED.)
GEOMETRIC_REPRESENTATION_ITEM()
RATIONAL_B_SPLINE_SURFACE(((0.999326490452172,0.999646063968169,1.,0.999104400890347,
0.9984288220563),(0.999326490452172,0.999646063968169,1.,0.999104400890347,
0.9984288220563),(0.999326490452172,0.999646063968169,1.,0.999104400890347,
0.9984288220563)))
REPRESENTATION_ITEM('')
SURFACE()
);
#122=(
BOUNDED_SURFACE()
B_SPLINE_SURFACE(1,2,((#66551,#66552,#66553),(#66554,#66555,#66556)),
 .UNSPECIFIED.,.F.,.F.,.F.)
B_SPLINE_SURFACE_WITH_KNOTS((2,2),(3,3),(0.,1.),(0.025590359613181,0.0375948596693881),
 .UNSPECIFIED.)
GEOMETRIC_REPRESENTATION_ITEM()
RATIONAL_B_SPLINE_SURFACE(((0.996753121755999,0.997505687613148,0.999678813023854),
(0.996753121755999,0.997505687613148,0.999678813023854)))
REPRESENTATION_ITEM('')
SURFACE()
);
#123=(
BOUNDED_SURFACE()
B_SPLINE_SURFACE(1,2,((#66591,#66592,#66593),(#66594,#66595,#66596),(#66597,
#66598,#66599)),.UNSPECIFIED.,.F.,.F.,.F.)
B_SPLINE_SURFACE_WITH_KNOTS((2,1,2),(3,3),(-0.00286823356222208,0.,0.477902879811012),
(0.0265907346180619,0.0331702037252919),.UNSPECIFIED.)
GEOMETRIC_REPRESENTATION_ITEM()
RATIONAL_B_SPLINE_SURFACE(((0.996888414395785,0.99736576547994,0.998269846384985),
(0.996888414395785,0.99736576547994,0.998269846384985),(0.996888414395785,
0.99736576547994,0.998269846384985)))
REPRESENTATION_ITEM('')
SURFACE()
);
#124=(
BOUNDED_SURFACE()
B_SPLINE_SURFACE(1,2,((#66698,#66699,#66700),(#66701,#66702,#66703),(#66704,
#66705,#66706),(#66707,#66708,#66709)),.UNSPECIFIED.,.F.,.F.,.F.)
B_SPLINE_SURFACE_WITH_KNOTS((2,1,1,2),(3,3),(-0.01,0.,1.,1.0101),(0.00560769168370619,
0.0176009700440517),.UNSPECIFIED.)
GEOMETRIC_REPRESENTATION_ITEM()
RATIONAL_B_SPLINE_SURFACE(((0.99818389211382,0.99657330421516,0.996380621259469),
(0.99818389211382,0.99657330421516,0.996380621259469),(0.99818389211382,
0.99657330421516,0.996380621259469),(0.99818389211382,0.99657330421516,
0.996380621259469)))
REPRESENTATION_ITEM('')
SURFACE()
);
#125=(
BOUNDED_SURFACE()
B_SPLINE_SURFACE(1,2,((#66832,#66833,#66834),(#66835,#66836,#66837)),
 .UNSPECIFIED.,.F.,.F.,.F.)
B_SPLINE_SURFACE_WITH_KNOTS((2,2),(3,3),(0.,1.),(0.0556006976418412,0.0675888856590511),
 .UNSPECIFIED.)
GEOMETRIC_REPRESENTATION_ITEM()
RATIONAL_B_SPLINE_SURFACE(((0.996397562408606,0.996150386832629,0.997319912843745),
(0.996397562408606,0.996150386832629,0.997319912843745)))
REPRESENTATION_ITEM('')
SURFACE()
);
#126=(
BOUNDED_SURFACE()
B_SPLINE_SURFACE(1,2,((#66906,#66907,#66908),(#66909,#66910,#66911),(#66912,
#66913,#66914)),.UNSPECIFIED.,.F.,.F.,.F.)
B_SPLINE_SURFACE_WITH_KNOTS((2,1,2),(3,3),(0.,1.,1.01),(0.0456081671210034,
0.0575989447818821),.UNSPECIFIED.)
GEOMETRIC_REPRESENTATION_ITEM()
RATIONAL_B_SPLINE_SURFACE(((0.997793907739636,0.996365558499688,0.996354522974128),
(0.997793907739636,0.996365558499688,0.996354522974128),(0.997793907739636,
0.996365558499688,0.996354522974128)))
REPRESENTATION_ITEM('')
SURFACE()
);
#127=(
BOUNDED_SURFACE()
B_SPLINE_SURFACE(1,2,((#66949,#66950,#66951),(#66952,#66953,#66954),(#66955,
#66956,#66957)),.UNSPECIFIED.,.F.,.F.,.F.)
B_SPLINE_SURFACE_WITH_KNOTS((2,1,2),(3,3),(-0.00286810173547451,0.,0.477902879808668),
(0.0466073985929113,0.0531834929157984),.UNSPECIFIED.)
GEOMETRIC_REPRESENTATION_ITEM()
RATIONAL_B_SPLINE_SURFACE(((0.997565691989291,0.996847118055593,0.996554836292953),
(0.997565691989291,0.996847118055593,0.996554836292953),(0.997565691989291,
0.996847118055593,0.996554836292953)))
REPRESENTATION_ITEM('')
SURFACE()
);
#128=(
BOUNDED_SURFACE()
B_SPLINE_SURFACE(1,2,((#66968,#66969,#66970,#66971,#66972),(#66973,#66974,
#66975,#66976,#66977),(#66978,#66979,#66980,#66981,#66982)),
 .UNSPECIFIED.,.F.,.F.,.F.)
B_SPLINE_SURFACE_WITH_KNOTS((2,1,2),(3,2,3),(0.,1.,1.01),(0.0355931932713904,
0.0384615384615384,0.0476086899858127),.UNSPECIFIED.)
GEOMETRIC_REPRESENTATION_ITEM()
RATIONAL_B_SPLINE_SURFACE(((0.998993602249807,0.999456249886298,1.,0.998265981131401,
0.997356751596327),(0.998993602249807,0.999456249886298,1.,0.998265981131401,
0.997356751596327),(0.998993602249807,0.999456249886298,1.,0.998265981131401,
0.997356751596327)))
REPRESENTATION_ITEM('')
SURFACE()
);
#129=(
BOUNDED_SURFACE()
B_SPLINE_SURFACE(1,2,((#67007,#67008,#67009,#67010,#67011),(#67012,#67013,
#67014,#67015,#67016),(#67017,#67018,#67019,#67020,#67021)),
 .UNSPECIFIED.,.F.,.F.,.F.)
B_SPLINE_SURFACE_WITH_KNOTS((2,1,2),(3,2,3),(-0.00141401191197287,0.,0.480770297102985),
(0.0365944846645793,0.0384615384615384,0.0431859280915182),
 .UNSPECIFIED.)
GEOMETRIC_REPRESENTATION_ITEM()
RATIONAL_B_SPLINE_SURFACE(((0.99932649045226,0.999646063968218,1.,0.999104400890347,
0.9984288220563),(0.99932649045226,0.999646063968218,1.,0.999104400890347,
0.9984288220563),(0.99932649045226,0.999646063968218,1.,0.999104400890347,
0.9984288220563)))
REPRESENTATION_ITEM('')
SURFACE()
);
#130=(
BOUNDED_SURFACE()
B_SPLINE_SURFACE(1,2,((#67077,#67078,#67079),(#67080,#67081,#67082),(#67083,
#67084,#67085)),.UNSPECIFIED.,.F.,.F.,.F.)
B_SPLINE_SURFACE_WITH_KNOTS((2,1,2),(3,3),(0.,1.,1.01),(0.0255903596131785,
0.0375948596693883),.UNSPECIFIED.)
GEOMETRIC_REPRESENTATION_ITEM()
RATIONAL_B_SPLINE_SURFACE(((0.996753121755999,0.997505687613148,0.999678813023854),
(0.996753121755999,0.997505687613148,0.999678813023854),(0.996753121755999,
0.997505687613148,0.999678813023854)))
REPRESENTATION_ITEM('')
SURFACE()
);
#131=(
BOUNDED_SURFACE()
B_SPLINE_SURFACE(1,2,((#67120,#67121,#67122),(#67123,#67124,#67125),(#67126,
#67127,#67128)),.UNSPECIFIED.,.F.,.F.,.F.)
B_SPLINE_SURFACE_WITH_KNOTS((2,1,2),(3,3),(-0.00286823356243391,0.,0.477902879809815),
(0.0265907346180619,0.0331702037252936),.UNSPECIFIED.)
GEOMETRIC_REPRESENTATION_ITEM()
RATIONAL_B_SPLINE_SURFACE(((0.996888414395785,0.997365765479939,0.998269846384985),
(0.996888414395785,0.997365765479939,0.998269846384985),(0.996888414395785,
0.997365765479939,0.998269846384985)))
REPRESENTATION_ITEM('')
SURFACE()
);
#132=(
BOUNDED_SURFACE()
B_SPLINE_SURFACE(1,2,((#67195,#67196,#67197),(#67198,#67199,#67200),(#67201,
#67202,#67203)),.UNSPECIFIED.,.F.,.F.,.F.)
B_SPLINE_SURFACE_WITH_KNOTS((2,1,2),(3,3),(-0.00286753128221124,0.,0.477902879810469),
(0.0166015299238957,0.023173678811188),.UNSPECIFIED.)
GEOMETRIC_REPRESENTATION_ITEM()
RATIONAL_B_SPLINE_SURFACE(((0.996422581660833,0.996252244737342,0.996507688616405),
(0.996422581660833,0.996252244737342,0.996507688616405),(0.996422581660833,
0.996252244737342,0.996507688616405)))
REPRESENTATION_ITEM('')
SURFACE()
);
#133=(
BOUNDED_SURFACE()
B_SPLINE_SURFACE(1,2,((#67220,#67221,#67222),(#67223,#67224,#67225),(#67226,
#67227,#67228),(#67229,#67230,#67231)),.UNSPECIFIED.,.F.,.F.,.F.)
B_SPLINE_SURFACE_WITH_KNOTS((2,1,1,2),(3,3),(-0.0101,0.,1.,1.01),(0.00560769168370512,
0.0176009700440517),.UNSPECIFIED.)
GEOMETRIC_REPRESENTATION_ITEM()
RATIONAL_B_SPLINE_SURFACE(((0.99818389211382,0.99657330421516,0.996380621259469),
(0.99818389211382,0.99657330421516,0.996380621259469),(0.99818389211382,
0.99657330421516,0.996380621259469),(0.99818389211382,0.99657330421516,
0.996380621259469)))
REPRESENTATION_ITEM('')
SURFACE()
);
#134=(
BOUNDED_SURFACE()
B_SPLINE_SURFACE(1,2,((#67354,#67355,#67356),(#67357,#67358,#67359)),
 .UNSPECIFIED.,.F.,.F.,.F.)
B_SPLINE_SURFACE_WITH_KNOTS((2,2),(3,3),(0.,1.),(0.0556006976418415,0.0675888856590488),
 .UNSPECIFIED.)
GEOMETRIC_REPRESENTATION_ITEM()
RATIONAL_B_SPLINE_SURFACE(((0.996397562408606,0.996150386832629,0.997319912843745),
(0.996397562408606,0.996150386832629,0.997319912843745)))
REPRESENTATION_ITEM('')
SURFACE()
);
#135=(
BOUNDED_SURFACE()
B_SPLINE_SURFACE(1,2,((#67428,#67429,#67430),(#67431,#67432,#67433),(#67434,
#67435,#67436)),.UNSPECIFIED.,.F.,.F.,.F.)
B_SPLINE_SURFACE_WITH_KNOTS((2,1,2),(3,3),(0.,1.,1.01),(0.0456081671210055,
0.0575989447818817),.UNSPECIFIED.)
GEOMETRIC_REPRESENTATION_ITEM()
RATIONAL_B_SPLINE_SURFACE(((0.997793907739636,0.996365558499688,0.996354522974128),
(0.997793907739636,0.996365558499688,0.996354522974128),(0.997793907739636,
0.996365558499688,0.996354522974128)))
REPRESENTATION_ITEM('')
SURFACE()
);
#136=(
BOUNDED_SURFACE()
B_SPLINE_SURFACE(1,2,((#67471,#67472,#67473),(#67474,#67475,#67476),(#67477,
#67478,#67479)),.UNSPECIFIED.,.F.,.F.,.F.)
B_SPLINE_SURFACE_WITH_KNOTS((2,1,2),(3,3),(-0.00286810173546857,0.,0.477902879806836),
(0.0466073985929116,0.0531834929157973),.UNSPECIFIED.)
GEOMETRIC_REPRESENTATION_ITEM()
RATIONAL_B_SPLINE_SURFACE(((0.997565691989291,0.996847118055594,0.996554836292953),
(0.997565691989291,0.996847118055594,0.996554836292953),(0.997565691989291,
0.996847118055594,0.996554836292953)))
REPRESENTATION_ITEM('')
SURFACE()
);
#137=(
BOUNDED_SURFACE()
B_SPLINE_SURFACE(1,2,((#67496,#67497,#67498,#67499,#67500),(#67501,#67502,
#67503,#67504,#67505),(#67506,#67507,#67508,#67509,#67510)),
 .UNSPECIFIED.,.F.,.F.,.F.)
B_SPLINE_SURFACE_WITH_KNOTS((2,1,2),(3,2,3),(0.,1.,1.01),(0.0355931932713903,
0.0384615384615384,0.0476086899858126),.UNSPECIFIED.)
GEOMETRIC_REPRESENTATION_ITEM()
RATIONAL_B_SPLINE_SURFACE(((0.998993602249807,0.999456249886298,1.,0.998265981131401,
0.997356751596327),(0.998993602249807,0.999456249886298,1.,0.998265981131401,
0.997356751596327),(0.998993602249807,0.999456249886298,1.,0.998265981131401,
0.997356751596327)))
REPRESENTATION_ITEM('')
SURFACE()
);
#138=(
BOUNDED_SURFACE()
B_SPLINE_SURFACE(1,2,((#67558,#67559,#67560,#67561,#67562),(#67563,#67564,
#67565,#67566,#67567),(#67568,#67569,#67570,#67571,#67572)),
 .UNSPECIFIED.,.F.,.F.,.F.)
B_SPLINE_SURFACE_WITH_KNOTS((2,1,2),(3,2,3),(-0.00141401191198394,0.,0.480770297101345),
(0.0365944846645757,0.0384615384615384,0.0431859280915184),
 .UNSPECIFIED.)
GEOMETRIC_REPRESENTATION_ITEM()
RATIONAL_B_SPLINE_SURFACE(((0.999326490452258,0.999646063968217,1.,0.999104400890347,
0.9984288220563),(0.999326490452258,0.999646063968217,1.,0.999104400890347,
0.9984288220563),(0.999326490452258,0.999646063968217,1.,0.999104400890347,
0.9984288220563)))
REPRESENTATION_ITEM('')
SURFACE()
);
#139=(
BOUNDED_SURFACE()
B_SPLINE_SURFACE(1,2,((#67588,#67589,#67590),(#67591,#67592,#67593),(#67594,
#67595,#67596)),.UNSPECIFIED.,.F.,.F.,.F.)
B_SPLINE_SURFACE_WITH_KNOTS((2,1,2),(3,3),(0.,1.,1.01),(0.0255903596131788,
0.0375948596693866),.UNSPECIFIED.)
GEOMETRIC_REPRESENTATION_ITEM()
RATIONAL_B_SPLINE_SURFACE(((0.996753121755999,0.997505687613147,0.999678813023853),
(0.996753121755999,0.997505687613147,0.999678813023853),(0.996753121755999,
0.997505687613147,0.999678813023853)))
REPRESENTATION_ITEM('')
SURFACE()
);
#140=(
BOUNDED_SURFACE()
B_SPLINE_SURFACE(1,2,((#67608,#67609,#67610),(#67611,#67612,#67613),(#67614,
#67615,#67616)),.UNSPECIFIED.,.F.,.F.,.F.)
B_SPLINE_SURFACE_WITH_KNOTS((2,1,2),(3,3),(-0.00286823356237821,0.,0.477902879808255),
(0.0265907346180626,0.0331702037252925),.UNSPECIFIED.)
GEOMETRIC_REPRESENTATION_ITEM()
RATIONAL_B_SPLINE_SURFACE(((0.996888414395785,0.997365765479939,0.998269846384986),
(0.996888414395785,0.997365765479939,0.998269846384986),(0.996888414395785,
0.997365765479939,0.998269846384986)))
REPRESENTATION_ITEM('')
SURFACE()
);
#141=(
BOUNDED_SURFACE()
B_SPLINE_SURFACE(1,2,((#67717,#67718,#67719),(#67720,#67721,#67722),(#67723,
#67724,#67725)),.UNSPECIFIED.,.F.,.F.,.F.)
B_SPLINE_SURFACE_WITH_KNOTS((2,1,2),(3,3),(-0.00286753128227487,0.,0.477902879809176),
(0.0166015299238962,0.0231736788111887),.UNSPECIFIED.)
GEOMETRIC_REPRESENTATION_ITEM()
RATIONAL_B_SPLINE_SURFACE(((0.996422581660833,0.996252244737342,0.996507688616405),
(0.996422581660833,0.996252244737342,0.996507688616404),(0.996422581660833,
0.996252244737342,0.996507688616404)))
REPRESENTATION_ITEM('')
SURFACE()
);
#142=(
BOUNDED_SURFACE()
B_SPLINE_SURFACE(1,2,((#67742,#67743,#67744),(#67745,#67746,#67747),(#67748,
#67749,#67750)),.UNSPECIFIED.,.F.,.F.,.F.)
B_SPLINE_SURFACE_WITH_KNOTS((2,1,2),(3,3),(-0.01,0.,1.),(0.00560769168370637,
0.0176009700440516),.UNSPECIFIED.)
GEOMETRIC_REPRESENTATION_ITEM()
RATIONAL_B_SPLINE_SURFACE(((0.99818389211382,0.99657330421516,0.996380621259469),
(0.99818389211382,0.99657330421516,0.996380621259469),(0.99818389211382,
0.99657330421516,0.996380621259469)))
REPRESENTATION_ITEM('')
SURFACE()
);
#143=(
BOUNDED_SURFACE()
B_SPLINE_SURFACE(1,2,((#67785,#67786,#67787),(#67788,#67789,#67790),(#67791,
#67792,#67793)),.UNSPECIFIED.,.F.,.F.,.F.)
B_SPLINE_SURFACE_WITH_KNOTS((2,1,2),(3,3),(-0.00206901892693671,0.,0.346769728509108),
(0.0066071315471312,0.0131849431468896),.UNSPECIFIED.)
GEOMETRIC_REPRESENTATION_ITEM()
RATIONAL_B_SPLINE_SURFACE(((0.997925307359465,0.997106772384946,0.996714752253861),
(0.997925307359465,0.997106772384946,0.996714752253861),(0.997925307359465,
0.997106772384946,0.996714752253861)))
REPRESENTATION_ITEM('')
SURFACE()
);
#144=(
BOUNDED_SURFACE()
B_SPLINE_SURFACE(1,2,((#67866,#67867,#67868),(#67869,#67870,#67871)),
 .UNSPECIFIED.,.F.,.F.,.F.)
B_SPLINE_SURFACE_WITH_KNOTS((2,2),(3,3),(0.,1.),(0.0556006976418457,0.0675888856590507),
 .UNSPECIFIED.)
GEOMETRIC_REPRESENTATION_ITEM()
RATIONAL_B_SPLINE_SURFACE(((0.996397562408606,0.996150386832629,0.997319912843745),
(0.996397562408606,0.996150386832629,0.997319912843745)))
REPRESENTATION_ITEM('')
SURFACE()
);
#145=(
BOUNDED_SURFACE()
B_SPLINE_SURFACE(1,2,((#67940,#67941,#67942),(#67943,#67944,#67945),(#67946,
#67947,#67948)),.UNSPECIFIED.,.F.,.F.,.F.)
B_SPLINE_SURFACE_WITH_KNOTS((2,1,2),(3,3),(0.,1.,1.01),(0.0456081671210043,
0.0575989447818814),.UNSPECIFIED.)
GEOMETRIC_REPRESENTATION_ITEM()
RATIONAL_B_SPLINE_SURFACE(((0.997793907739636,0.996365558499688,0.996354522974128),
(0.997793907739636,0.996365558499688,0.996354522974128),(0.997793907739636,
0.996365558499688,0.996354522974128)))
REPRESENTATION_ITEM('')
SURFACE()
);
#146=(
BOUNDED_SURFACE()
B_SPLINE_SURFACE(1,2,((#67983,#67984,#67985),(#67986,#67987,#67988),(#67989,
#67990,#67991)),.UNSPECIFIED.,.F.,.F.,.F.)
B_SPLINE_SURFACE_WITH_KNOTS((2,1,2),(3,3),(-0.00286810173237255,0.,0.477902879804808),
(0.0466073985929115,0.0531834929157976),.UNSPECIFIED.)
GEOMETRIC_REPRESENTATION_ITEM()
RATIONAL_B_SPLINE_SURFACE(((0.997565691989291,0.996847118055593,0.996554836292953),
(0.997565691989291,0.996847118055593,0.996554836292953),(0.997565691989291,
0.996847118055593,0.996554836292953)))
REPRESENTATION_ITEM('')
SURFACE()
);
#147=(
BOUNDED_SURFACE()
B_SPLINE_SURFACE(1,2,((#68008,#68009,#68010,#68011,#68012),(#68013,#68014,
#68015,#68016,#68017),(#68018,#68019,#68020,#68021,#68022)),
 .UNSPECIFIED.,.F.,.F.,.F.)
B_SPLINE_SURFACE_WITH_KNOTS((2,1,2),(3,2,3),(0.,1.,1.01),(0.0355931932713902,
0.0384615384615384,0.0476086899858139),.UNSPECIFIED.)
GEOMETRIC_REPRESENTATION_ITEM()
RATIONAL_B_SPLINE_SURFACE(((0.998993602249807,0.999456249886298,1.,0.998265981131401,
0.997356751596327),(0.998993602249807,0.999456249886298,1.,0.998265981131401,
0.997356751596327),(0.998993602249807,0.999456249886298,1.,0.998265981131401,
0.997356751596327)))
REPRESENTATION_ITEM('')
SURFACE()
);
#148=(
BOUNDED_SURFACE()
B_SPLINE_SURFACE(1,2,((#68070,#68071,#68072,#68073,#68074),(#68075,#68076,
#68077,#68078,#68079),(#68080,#68081,#68082,#68083,#68084)),
 .UNSPECIFIED.,.F.,.F.,.F.)
B_SPLINE_SURFACE_WITH_KNOTS((2,1,2),(3,2,3),(-0.00141401191198009,0.,0.480770297099536),
(0.0365944846645796,0.0384615384615384,0.0431859280915184),
 .UNSPECIFIED.)
GEOMETRIC_REPRESENTATION_ITEM()
RATIONAL_B_SPLINE_SURFACE(((0.99932649045226,0.999646063968218,1.,0.999104400890347,
0.9984288220563),(0.99932649045226,0.999646063968218,1.,0.999104400890347,
0.9984288220563),(0.99932649045226,0.999646063968218,1.,0.999104400890347,
0.9984288220563)))
REPRESENTATION_ITEM('')
SURFACE()
);
#149=(
BOUNDED_SURFACE()
B_SPLINE_SURFACE(1,2,((#68111,#68112,#68113),(#68114,#68115,#68116),(#68117,
#68118,#68119)),.UNSPECIFIED.,.F.,.F.,.F.)
B_SPLINE_SURFACE_WITH_KNOTS((2,1,2),(3,3),(0.,1.,1.01),(0.025590359613181,
0.0375948596693874),.UNSPECIFIED.)
GEOMETRIC_REPRESENTATION_ITEM()
RATIONAL_B_SPLINE_SURFACE(((0.996753121755999,0.997505687613148,0.999678813023853),
(0.996753121755999,0.997505687613148,0.999678813023853),(0.996753121755999,
0.997505687613148,0.999678813023853)))
REPRESENTATION_ITEM('')
SURFACE()
);
#150=(
BOUNDED_SURFACE()
B_SPLINE_SURFACE(1,2,((#68154,#68155,#68156),(#68157,#68158,#68159),(#68160,
#68161,#68162)),.UNSPECIFIED.,.F.,.F.,.F.)
B_SPLINE_SURFACE_WITH_KNOTS((2,1,2),(3,3),(-0.00286823045912087,0.,0.477902879806536),
(0.0265907346180616,0.0331702036774538),.UNSPECIFIED.)
GEOMETRIC_REPRESENTATION_ITEM()
RATIONAL_B_SPLINE_SURFACE(((0.996888414395785,0.997365765476469,0.998269846371838),
(0.996888414395785,0.997365765476469,0.998269846371838),(0.996888414395785,
0.997365765476469,0.998269846371838)))
REPRESENTATION_ITEM('')
SURFACE()
);
#151=(
BOUNDED_SURFACE()
B_SPLINE_SURFACE(1,2,((#68200,#68201,#68202),(#68203,#68204,#68205),(#68206,
#68207,#68208)),.UNSPECIFIED.,.F.,.F.,.F.)
B_SPLINE_SURFACE_WITH_KNOTS((2,1,2),(3,3),(-0.00286753128222655,0.,0.477902879807592),
(0.0166015299238958,0.0231736788111887),.UNSPECIFIED.)
GEOMETRIC_REPRESENTATION_ITEM()
RATIONAL_B_SPLINE_SURFACE(((0.996422581660833,0.996252244737342,0.996507688616404),
(0.996422581660833,0.996252244737342,0.996507688616404),(0.996422581660833,
0.996252244737342,0.996507688616404)))
REPRESENTATION_ITEM('')
SURFACE()
);
#152=(
BOUNDED_SURFACE()
B_SPLINE_SURFACE(1,2,((#68254,#68255,#68256),(#68257,#68258,#68259),(#68260,
#68261,#68262)),.UNSPECIFIED.,.F.,.F.,.F.)
B_SPLINE_SURFACE_WITH_KNOTS((2,1,2),(3,3),(0.,1.,1.01),(0.00560769170937608,
0.0176009697616828),.UNSPECIFIED.)
GEOMETRIC_REPRESENTATION_ITEM()
RATIONAL_B_SPLINE_SURFACE(((0.998183892106926,0.996573304252667,0.996380621268542),
(0.998183892106926,0.996573304252667,0.996380621268542),(0.998183892106926,
0.996573304252667,0.996380621268542)))
REPRESENTATION_ITEM('')
SURFACE()
);
#153=(
BOUNDED_SURFACE()
B_SPLINE_SURFACE(1,2,((#68297,#68298,#68299),(#68300,#68301,#68302),(#68303,
#68304,#68305)),.UNSPECIFIED.,.F.,.F.,.F.)
B_SPLINE_SURFACE_WITH_KNOTS((2,1,2),(3,3),(-0.00206901892698856,0.,0.346769728507897),
(0.00660713154714496,0.0131849431468368),.UNSPECIFIED.)
GEOMETRIC_REPRESENTATION_ITEM()
RATIONAL_B_SPLINE_SURFACE(((0.997925307359461,0.997106772384952,0.996714752253867),
(0.997925307359461,0.997106772384952,0.996714752253867),(0.997925307359461,
0.997106772384952,0.996714752253867)))
REPRESENTATION_ITEM('')
SURFACE()
);
#154=(
BOUNDED_SURFACE()
B_SPLINE_SURFACE(1,2,((#68378,#68379,#68380),(#68381,#68382,#68383)),
 .UNSPECIFIED.,.F.,.F.,.F.)
B_SPLINE_SURFACE_WITH_KNOTS((2,2),(3,3),(0.,1.),(0.0556006976418394,0.0675888856590502),
 .UNSPECIFIED.)
GEOMETRIC_REPRESENTATION_ITEM()
RATIONAL_B_SPLINE_SURFACE(((0.996397562408606,0.996150386832629,0.997319912843745),
(0.996397562408606,0.996150386832629,0.997319912843745)))
REPRESENTATION_ITEM('')
SURFACE()
);
#155=(
BOUNDED_SURFACE()
B_SPLINE_SURFACE(1,2,((#68452,#68453,#68454),(#68455,#68456,#68457),(#68458,
#68459,#68460)),.UNSPECIFIED.,.F.,.F.,.F.)
B_SPLINE_SURFACE_WITH_KNOTS((2,1,2),(3,3),(0.,1.,1.01),(0.0456081671210063,
0.0575989447818833),.UNSPECIFIED.)
GEOMETRIC_REPRESENTATION_ITEM()
RATIONAL_B_SPLINE_SURFACE(((0.997793907739636,0.996365558499688,0.996354522974128),
(0.997793907739636,0.996365558499688,0.996354522974128),(0.997793907739636,
0.996365558499688,0.996354522974128)))
REPRESENTATION_ITEM('')
SURFACE()
);
#156=(
BOUNDED_SURFACE()
B_SPLINE_SURFACE(1,2,((#68495,#68496,#68497),(#68498,#68499,#68500),(#68501,
#68502,#68503)),.UNSPECIFIED.,.F.,.F.,.F.)
B_SPLINE_SURFACE_WITH_KNOTS((2,1,2),(3,3),(-0.00286810173241533,0.,0.477902879802667),
(0.0466073985929121,0.053183492915798),.UNSPECIFIED.)
GEOMETRIC_REPRESENTATION_ITEM()
RATIONAL_B_SPLINE_SURFACE(((0.997565691989291,0.996847118055593,0.996554836292953),
(0.997565691989291,0.996847118055593,0.996554836292953),(0.997565691989291,
0.996847118055593,0.996554836292953)))
REPRESENTATION_ITEM('')
SURFACE()
);
#157=(
BOUNDED_SURFACE()
B_SPLINE_SURFACE(1,2,((#68520,#68521,#68522,#68523,#68524),(#68525,#68526,
#68527,#68528,#68529),(#68530,#68531,#68532,#68533,#68534)),
 .UNSPECIFIED.,.F.,.F.,.F.)
B_SPLINE_SURFACE_WITH_KNOTS((2,1,2),(3,2,3),(0.,1.,1.01),(0.0355931932713904,
0.0384615384615384,0.0476086899858132),.UNSPECIFIED.)
GEOMETRIC_REPRESENTATION_ITEM()
RATIONAL_B_SPLINE_SURFACE(((0.998993602249807,0.999456249886298,1.,0.998265981131401,
0.997356751596327),(0.998993602249807,0.999456249886298,1.,0.998265981131401,
0.997356751596327),(0.998993602249807,0.999456249886298,1.,0.998265981131401,
0.997356751596327)))
REPRESENTATION_ITEM('')
SURFACE()
);
#158=(
BOUNDED_SURFACE()
B_SPLINE_SURFACE(1,2,((#68582,#68583,#68584,#68585,#68586),(#68587,#68588,
#68589,#68590,#68591),(#68592,#68593,#68594,#68595,#68596)),
 .UNSPECIFIED.,.F.,.F.,.F.)
B_SPLINE_SURFACE_WITH_KNOTS((2,1,2),(3,2,3),(-0.00141401191198431,0.,0.480770297097393),
(0.0365944846645793,0.0384615384615384,0.043185928091518),.UNSPECIFIED.)
GEOMETRIC_REPRESENTATION_ITEM()
RATIONAL_B_SPLINE_SURFACE(((0.99932649045226,0.999646063968218,1.,0.999104400890347,
0.9984288220563),(0.99932649045226,0.999646063968218,1.,0.999104400890347,
0.9984288220563),(0.99932649045226,0.999646063968218,1.,0.999104400890347,
0.9984288220563)))
REPRESENTATION_ITEM('')
SURFACE()
);
#159=(
BOUNDED_SURFACE()
B_SPLINE_SURFACE(1,2,((#68623,#68624,#68625),(#68626,#68627,#68628),(#68629,
#68630,#68631)),.UNSPECIFIED.,.F.,.F.,.F.)
B_SPLINE_SURFACE_WITH_KNOTS((2,1,2),(3,3),(0.,1.,1.01),(0.0255903596131799,
0.0375948596693881),.UNSPECIFIED.)
GEOMETRIC_REPRESENTATION_ITEM()
RATIONAL_B_SPLINE_SURFACE(((0.996753121755999,0.997505687613148,0.999678813023854),
(0.996753121755999,0.997505687613148,0.999678813023854),(0.996753121755999,
0.997505687613148,0.999678813023854)))
REPRESENTATION_ITEM('')
SURFACE()
);
#160=(
BOUNDED_SURFACE()
B_SPLINE_SURFACE(1,2,((#68666,#68667,#68668),(#68669,#68670,#68671),(#68672,
#68673,#68674)),.UNSPECIFIED.,.F.,.F.,.F.)
B_SPLINE_SURFACE_WITH_KNOTS((2,1,2),(3,3),(-0.00286823356251491,0.,0.477902879804656),
(0.0265907346180619,0.0331702037252935),.UNSPECIFIED.)
GEOMETRIC_REPRESENTATION_ITEM()
RATIONAL_B_SPLINE_SURFACE(((0.996888414395785,0.997365765479939,0.998269846384986),
(0.996888414395785,0.997365765479939,0.998269846384986),(0.996888414395785,
0.997365765479939,0.998269846384986)))
REPRESENTATION_ITEM('')
SURFACE()
);
#161=(
BOUNDED_SURFACE()
B_SPLINE_SURFACE(1,2,((#68741,#68742,#68743),(#68744,#68745,#68746),(#68747,
#68748,#68749)),.UNSPECIFIED.,.F.,.F.,.F.)
B_SPLINE_SURFACE_WITH_KNOTS((2,1,2),(3,3),(-0.00286753128226436,0.,0.477902879805871),
(0.0166015299238958,0.0231736788111887),.UNSPECIFIED.)
GEOMETRIC_REPRESENTATION_ITEM()
RATIONAL_B_SPLINE_SURFACE(((0.996422581660833,0.996252244737342,0.996507688616404),
(0.996422581660833,0.996252244737342,0.996507688616404),(0.996422581660833,
0.996252244737342,0.996507688616404)))
REPRESENTATION_ITEM('')
SURFACE()
);
#162=(
BOUNDED_SURFACE()
B_SPLINE_SURFACE(1,2,((#68760,#68761,#68762),(#68763,#68764,#68765),(#68766,
#68767,#68768),(#68769,#68770,#68771)),.UNSPECIFIED.,.F.,.F.,.F.)
B_SPLINE_SURFACE_WITH_KNOTS((2,1,1,2),(3,3),(-0.0101,0.,1.,1.01),(0.00560769168370509,
0.0176009700440523),.UNSPECIFIED.)
GEOMETRIC_REPRESENTATION_ITEM()
RATIONAL_B_SPLINE_SURFACE(((0.998183892113821,0.99657330421516,0.996380621259469),
(0.998183892113821,0.99657330421516,0.996380621259469),(0.998183892113821,
0.99657330421516,0.996380621259469),(0.998183892113821,0.99657330421516,
0.996380621259469)))
REPRESENTATION_ITEM('')
SURFACE()
);
#163=(
BOUNDED_SURFACE()
B_SPLINE_SURFACE(1,2,((#68783,#68784,#68785),(#68786,#68787,#68788),(#68789,
#68790,#68791)),.UNSPECIFIED.,.F.,.F.,.F.)
B_SPLINE_SURFACE_WITH_KNOTS((2,1,2),(3,3),(-0.00206901892703507,0.,0.346769728506472),
(0.00660713154710819,0.0131849431468896),.UNSPECIFIED.)
GEOMETRIC_REPRESENTATION_ITEM()
RATIONAL_B_SPLINE_SURFACE(((0.997925307359471,0.997106772384947,0.99671475225386),
(0.997925307359471,0.997106772384947,0.99671475225386),(0.997925307359471,
0.997106772384947,0.99671475225386)))
REPRESENTATION_ITEM('')
SURFACE()
);
#164=(
BOUNDED_SURFACE()
B_SPLINE_SURFACE(1,2,((#68893,#68894,#68895),(#68896,#68897,#68898)),
 .UNSPECIFIED.,.F.,.F.,.F.)
B_SPLINE_SURFACE_WITH_KNOTS((2,2),(3,3),(0.,1.),(0.0556006976418427,0.0675888856590493),
 .UNSPECIFIED.)
GEOMETRIC_REPRESENTATION_ITEM()
RATIONAL_B_SPLINE_SURFACE(((0.996397562408606,0.996150386832629,0.997319912843745),
(0.996397562408606,0.996150386832629,0.997319912843745)))
REPRESENTATION_ITEM('')
SURFACE()
);
#165=(
BOUNDED_SURFACE()
B_SPLINE_SURFACE(1,2,((#68967,#68968,#68969),(#68970,#68971,#68972),(#68973,
#68974,#68975)),.UNSPECIFIED.,.F.,.F.,.F.)
B_SPLINE_SURFACE_WITH_KNOTS((2,1,2),(3,3),(0.,1.,1.01),(0.0456081671210056,
0.0575989447818805),.UNSPECIFIED.)
GEOMETRIC_REPRESENTATION_ITEM()
RATIONAL_B_SPLINE_SURFACE(((0.997793907739636,0.996365558499688,0.996354522974128),
(0.997793907739636,0.996365558499688,0.996354522974128),(0.997793907739636,
0.996365558499688,0.996354522974128)))
REPRESENTATION_ITEM('')
SURFACE()
);
#166=(
BOUNDED_SURFACE()
B_SPLINE_SURFACE(1,2,((#69010,#69011,#69012),(#69013,#69014,#69015),(#69016,
#69017,#69018)),.UNSPECIFIED.,.F.,.F.,.F.)
B_SPLINE_SURFACE_WITH_KNOTS((2,1,2),(3,3),(-0.00286810173213876,0.,0.477902879800509),
(0.0466073985929119,0.0531834929157981),.UNSPECIFIED.)
GEOMETRIC_REPRESENTATION_ITEM()
RATIONAL_B_SPLINE_SURFACE(((0.997565691989292,0.996847118055594,0.996554836292953),
(0.997565691989292,0.996847118055594,0.996554836292953),(0.997565691989292,
0.996847118055594,0.996554836292953)))
REPRESENTATION_ITEM('')
SURFACE()
);
#167=(
BOUNDED_SURFACE()
B_SPLINE_SURFACE(1,2,((#69035,#69036,#69037,#69038,#69039),(#69040,#69041,
#69042,#69043,#69044),(#69045,#69046,#69047,#69048,#69049)),
 .UNSPECIFIED.,.F.,.F.,.F.)
B_SPLINE_SURFACE_WITH_KNOTS((2,1,2),(3,2,3),(0.,1.,1.01),(0.0355931932713901,
0.0384615384615384,0.0476086899858143),.UNSPECIFIED.)
GEOMETRIC_REPRESENTATION_ITEM()
RATIONAL_B_SPLINE_SURFACE(((0.998993602249807,0.999456249886298,1.,0.998265981131401,
0.997356751596327),(0.998993602249807,0.999456249886298,1.,0.998265981131401,
0.997356751596327),(0.998993602249807,0.999456249886298,1.,0.998265981131401,
0.997356751596327)))
REPRESENTATION_ITEM('')
SURFACE()
);
#168=(
BOUNDED_SURFACE()
B_SPLINE_SURFACE(1,2,((#69097,#69098,#69099,#69100,#69101),(#69102,#69103,
#69104,#69105,#69106),(#69107,#69108,#69109,#69110,#69111)),
 .UNSPECIFIED.,.F.,.F.,.F.)
B_SPLINE_SURFACE_WITH_KNOTS((2,1,2),(3,2,3),(-0.00141401191198412,0.,0.480770297095169),
(0.0365944846645757,0.0384615384615384,0.0431859280915181),
 .UNSPECIFIED.)
GEOMETRIC_REPRESENTATION_ITEM()
RATIONAL_B_SPLINE_SURFACE(((0.999326490452259,0.999646063968217,1.,0.999104400890347,
0.9984288220563),(0.999326490452259,0.999646063968217,1.,0.999104400890347,
0.9984288220563),(0.999326490452259,0.999646063968217,1.,0.999104400890347,
0.9984288220563)))
REPRESENTATION_ITEM('')
SURFACE()
);
#169=(
BOUNDED_SURFACE()
B_SPLINE_SURFACE(1,2,((#69138,#69139,#69140),(#69141,#69142,#69143),(#69144,
#69145,#69146)),.UNSPECIFIED.,.F.,.F.,.F.)
B_SPLINE_SURFACE_WITH_KNOTS((2,1,2),(3,3),(0.,1.,1.01),(0.0255903596131801,
0.0375948596693865),.UNSPECIFIED.)
GEOMETRIC_REPRESENTATION_ITEM()
RATIONAL_B_SPLINE_SURFACE(((0.996753121755999,0.997505687613148,0.999678813023853),
(0.996753121755999,0.997505687613148,0.999678813023853),(0.996753121755999,
0.997505687613148,0.999678813023853)))
REPRESENTATION_ITEM('')
SURFACE()
);
#170=(
BOUNDED_SURFACE()
B_SPLINE_SURFACE(1,2,((#69181,#69182,#69183),(#69184,#69185,#69186),(#69187,
#69188,#69189)),.UNSPECIFIED.,.F.,.F.,.F.)
B_SPLINE_SURFACE_WITH_KNOTS((2,1,2),(3,3),(-0.00286823356233756,0.,0.477902879802539),
(0.0265907346180619,0.0331702037252928),.UNSPECIFIED.)
GEOMETRIC_REPRESENTATION_ITEM()
RATIONAL_B_SPLINE_SURFACE(((0.996888414395785,0.997365765479939,0.998269846384985),
(0.996888414395785,0.997365765479939,0.998269846384985),(0.996888414395785,
0.997365765479939,0.998269846384985)))
REPRESENTATION_ITEM('')
SURFACE()
);
#171=(
BOUNDED_SURFACE()
B_SPLINE_SURFACE(1,2,((#69256,#69257,#69258),(#69259,#69260,#69261),(#69262,
#69263,#69264)),.UNSPECIFIED.,.F.,.F.,.F.)
B_SPLINE_SURFACE_WITH_KNOTS((2,1,2),(3,3),(-0.0028675312823971,0.,0.47790287980379),
(0.016601529923896,0.0231736788111898),.UNSPECIFIED.)
GEOMETRIC_REPRESENTATION_ITEM()
RATIONAL_B_SPLINE_SURFACE(((0.996422581660833,0.996252244737342,0.996507688616404),
(0.996422581660833,0.996252244737342,0.996507688616404),(0.996422581660833,
0.996252244737342,0.996507688616404)))
REPRESENTATION_ITEM('')
SURFACE()
);
#172=(
BOUNDED_SURFACE()
B_SPLINE_SURFACE(1,2,((#69281,#69282,#69283),(#69284,#69285,#69286),(#69287,
#69288,#69289),(#69290,#69291,#69292)),.UNSPECIFIED.,.F.,.F.,.F.)
B_SPLINE_SURFACE_WITH_KNOTS((2,1,1,2),(3,3),(-0.0101,0.,1.,1.01),(0.00560769168370544,
0.0176009700440511),.UNSPECIFIED.)
GEOMETRIC_REPRESENTATION_ITEM()
RATIONAL_B_SPLINE_SURFACE(((0.99818389211382,0.99657330421516,0.996380621259469),
(0.99818389211382,0.99657330421516,0.996380621259469),(0.99818389211382,
0.99657330421516,0.996380621259469),(0.99818389211382,0.99657330421516,
0.996380621259469)))
REPRESENTATION_ITEM('')
SURFACE()
);
#173=(
BOUNDED_SURFACE()
B_SPLINE_SURFACE(1,2,((#69327,#69328,#69329),(#69330,#69331,#69332),(#69333,
#69334,#69335)),.UNSPECIFIED.,.F.,.F.,.F.)
B_SPLINE_SURFACE_WITH_KNOTS((2,1,2),(3,3),(-0.00206901892705003,0.,0.346769728504996),
(0.0066071315471665,0.0131849431468897),.UNSPECIFIED.)
GEOMETRIC_REPRESENTATION_ITEM()
RATIONAL_B_SPLINE_SURFACE(((0.997925307359456,0.997106772384944,0.99671475225386),
(0.997925307359456,0.997106772384944,0.99671475225386),(0.997925307359456,
0.997106772384944,0.99671475225386)))
REPRESENTATION_ITEM('')
SURFACE()
);
#174=(
BOUNDED_SURFACE()
B_SPLINE_SURFACE(1,2,((#69408,#69409,#69410),(#69411,#69412,#69413)),
 .UNSPECIFIED.,.F.,.F.,.F.)
B_SPLINE_SURFACE_WITH_KNOTS((2,2),(3,3),(0.,1.),(0.0556006976418448,0.0675888856590502),
 .UNSPECIFIED.)
GEOMETRIC_REPRESENTATION_ITEM()
RATIONAL_B_SPLINE_SURFACE(((0.996397562408606,0.996150386832629,0.997319912843745),
(0.996397562408606,0.996150386832629,0.997319912843745)))
REPRESENTATION_ITEM('')
SURFACE()
);
#175=(
BOUNDED_SURFACE()
B_SPLINE_SURFACE(1,2,((#69482,#69483,#69484),(#69485,#69486,#69487),(#69488,
#69489,#69490)),.UNSPECIFIED.,.F.,.F.,.F.)
B_SPLINE_SURFACE_WITH_KNOTS((2,1,2),(3,3),(0.,1.,1.01),(0.0456081671210065,
0.0575989447818822),.UNSPECIFIED.)
GEOMETRIC_REPRESENTATION_ITEM()
RATIONAL_B_SPLINE_SURFACE(((0.997793907739636,0.996365558499688,0.996354522974128),
(0.997793907739636,0.996365558499688,0.996354522974128),(0.997793907739636,
0.996365558499688,0.996354522974128)))
REPRESENTATION_ITEM('')
SURFACE()
);
#176=(
BOUNDED_SURFACE()
B_SPLINE_SURFACE(1,2,((#69525,#69526,#69527),(#69528,#69529,#69530),(#69531,
#69532,#69533)),.UNSPECIFIED.,.F.,.F.,.F.)
B_SPLINE_SURFACE_WITH_KNOTS((2,1,2),(3,3),(-0.0028681017353746,0.,0.477902879797914),
(0.0466073985929116,0.0531834929157982),.UNSPECIFIED.)
GEOMETRIC_REPRESENTATION_ITEM()
RATIONAL_B_SPLINE_SURFACE(((0.997565691989291,0.996847118055594,0.996554836292953),
(0.997565691989291,0.996847118055594,0.996554836292953),(0.997565691989291,
0.996847118055594,0.996554836292953)))
REPRESENTATION_ITEM('')
SURFACE()
);
#177=(
BOUNDED_SURFACE()
B_SPLINE_SURFACE(1,2,((#69550,#69551,#69552,#69553,#69554),(#69555,#69556,
#69557,#69558,#69559),(#69560,#69561,#69562,#69563,#69564)),
 .UNSPECIFIED.,.F.,.F.,.F.)
B_SPLINE_SURFACE_WITH_KNOTS((2,1,2),(3,2,3),(0.,1.,1.01),(0.0355931932713903,
0.0384615384615384,0.0476086899858138),.UNSPECIFIED.)
GEOMETRIC_REPRESENTATION_ITEM()
RATIONAL_B_SPLINE_SURFACE(((0.998993602249807,0.999456249886298,1.,0.998265981131401,
0.997356751596327),(0.998993602249807,0.999456249886298,1.,0.998265981131401,
0.997356751596327),(0.998993602249807,0.999456249886298,1.,0.998265981131401,
0.997356751596327)))
REPRESENTATION_ITEM('')
SURFACE()
);
#178=(
BOUNDED_SURFACE()
B_SPLINE_SURFACE(1,2,((#69612,#69613,#69614,#69615,#69616),(#69617,#69618,
#69619,#69620,#69621),(#69622,#69623,#69624,#69625,#69626)),
 .UNSPECIFIED.,.F.,.F.,.F.)
B_SPLINE_SURFACE_WITH_KNOTS((2,1,2),(3,2,3),(-0.0014140119119741,0.,0.480770297092789),
(0.0365944846645798,0.0384615384615384,0.0431859280915187),
 .UNSPECIFIED.)
GEOMETRIC_REPRESENTATION_ITEM()
RATIONAL_B_SPLINE_SURFACE(((0.99932649045226,0.999646063968218,1.,0.999104400890347,
0.9984288220563),(0.99932649045226,0.999646063968218,1.,0.999104400890347,
0.9984288220563),(0.99932649045226,0.999646063968218,1.,0.999104400890347,
0.9984288220563)))
REPRESENTATION_ITEM('')
SURFACE()
);
#179=(
BOUNDED_SURFACE()
B_SPLINE_SURFACE(1,2,((#69653,#69654,#69655),(#69656,#69657,#69658),(#69659,
#69660,#69661)),.UNSPECIFIED.,.F.,.F.,.F.)
B_SPLINE_SURFACE_WITH_KNOTS((2,1,2),(3,3),(0.,1.,1.01),(0.0255903596131829,
0.0375948596693895),.UNSPECIFIED.)
GEOMETRIC_REPRESENTATION_ITEM()
RATIONAL_B_SPLINE_SURFACE(((0.996753121755999,0.997505687613148,0.999678813023854),
(0.996753121755999,0.997505687613148,0.999678813023854),(0.996753121755999,
0.997505687613148,0.999678813023854)))
REPRESENTATION_ITEM('')
SURFACE()
);
#180=(
BOUNDED_SURFACE()
B_SPLINE_SURFACE(1,2,((#69696,#69697,#69698),(#69699,#69700,#69701),(#69702,
#69703,#69704)),.UNSPECIFIED.,.F.,.F.,.F.)
B_SPLINE_SURFACE_WITH_KNOTS((2,1,2),(3,3),(-0.0028682335623885,0.,0.477902879800222),
(0.0265907346180618,0.0331702037252924),.UNSPECIFIED.)
GEOMETRIC_REPRESENTATION_ITEM()
RATIONAL_B_SPLINE_SURFACE(((0.996888414395785,0.997365765479939,0.998269846384985),
(0.996888414395785,0.997365765479939,0.998269846384985),(0.996888414395785,
0.997365765479939,0.998269846384985)))
REPRESENTATION_ITEM('')
SURFACE()
);
#181=(
BOUNDED_SURFACE()
B_SPLINE_SURFACE(1,2,((#69771,#69772,#69773),(#69774,#69775,#69776),(#69777,
#69778,#69779)),.UNSPECIFIED.,.F.,.F.,.F.)
B_SPLINE_SURFACE_WITH_KNOTS((2,1,2),(3,3),(-0.00286753128209166,0.,0.477902879801465),
(0.0166015299238953,0.0231736788111885),.UNSPECIFIED.)
GEOMETRIC_REPRESENTATION_ITEM()
RATIONAL_B_SPLINE_SURFACE(((0.996422581660833,0.996252244737341,0.996507688616404),
(0.996422581660833,0.996252244737341,0.996507688616404),(0.996422581660833,
0.996252244737341,0.996507688616404)))
REPRESENTATION_ITEM('')
SURFACE()
);
#182=(
BOUNDED_SURFACE()
B_SPLINE_SURFACE(1,2,((#69796,#69797,#69798),(#69799,#69800,#69801),(#69802,
#69803,#69804),(#69805,#69806,#69807)),.UNSPECIFIED.,.F.,.F.,.F.)
B_SPLINE_SURFACE_WITH_KNOTS((2,1,1,2),(3,3),(-0.0101,0.,1.,1.01),(0.00560769168370701,
0.0176009700440521),.UNSPECIFIED.)
GEOMETRIC_REPRESENTATION_ITEM()
RATIONAL_B_SPLINE_SURFACE(((0.99818389211382,0.99657330421516,0.996380621259469),
(0.99818389211382,0.99657330421516,0.996380621259469),(0.99818389211382,
0.99657330421516,0.996380621259469),(0.99818389211382,0.99657330421516,
0.996380621259469)))
REPRESENTATION_ITEM('')
SURFACE()
);
#183=(
BOUNDED_SURFACE()
B_SPLINE_SURFACE(1,2,((#69842,#69843,#69844),(#69845,#69846,#69847),(#69848,
#69849,#69850)),.UNSPECIFIED.,.F.,.F.,.F.)
B_SPLINE_SURFACE_WITH_KNOTS((2,1,2),(3,3),(-0.00206901892700914,0.,0.346769728503543),
(0.00660713154717611,0.0131849431468889),.UNSPECIFIED.)
GEOMETRIC_REPRESENTATION_ITEM()
RATIONAL_B_SPLINE_SURFACE(((0.997925307359454,0.997106772384943,0.99671475225386),
(0.997925307359454,0.997106772384943,0.99671475225386),(0.997925307359454,
0.997106772384943,0.99671475225386)))
REPRESENTATION_ITEM('')
SURFACE()
);
#184=(
BOUNDED_SURFACE()
B_SPLINE_SURFACE(1,2,((#69923,#69924,#69925),(#69926,#69927,#69928)),
 .UNSPECIFIED.,.F.,.F.,.F.)
B_SPLINE_SURFACE_WITH_KNOTS((2,2),(3,3),(0.,1.),(0.0556006976418403,0.0675888856590522),
 .UNSPECIFIED.)
GEOMETRIC_REPRESENTATION_ITEM()
RATIONAL_B_SPLINE_SURFACE(((0.996397562408606,0.996150386832629,0.997319912843745),
(0.996397562408606,0.996150386832629,0.997319912843745)))
REPRESENTATION_ITEM('')
SURFACE()
);
#185=(
BOUNDED_SURFACE()
B_SPLINE_SURFACE(1,2,((#69997,#69998,#69999),(#70000,#70001,#70002),(#70003,
#70004,#70005)),.UNSPECIFIED.,.F.,.F.,.F.)
B_SPLINE_SURFACE_WITH_KNOTS((2,1,2),(3,3),(0.,1.,1.01),(0.0456081671210032,
0.0575989447818836),.UNSPECIFIED.)
GEOMETRIC_REPRESENTATION_ITEM()
RATIONAL_B_SPLINE_SURFACE(((0.997793907739636,0.996365558499688,0.996354522974128),
(0.997793907739636,0.996365558499688,0.996354522974128),(0.997793907739636,
0.996365558499688,0.996354522974128)))
REPRESENTATION_ITEM('')
SURFACE()
);
#186=(
BOUNDED_SURFACE()
B_SPLINE_SURFACE(1,2,((#70040,#70041,#70042),(#70043,#70044,#70045),(#70046,
#70047,#70048)),.UNSPECIFIED.,.F.,.F.,.F.)
B_SPLINE_SURFACE_WITH_KNOTS((2,1,2),(3,3),(-0.00286810173537214,0.,0.477902879795336),
(0.0466073985929122,0.0531834929157976),.UNSPECIFIED.)
GEOMETRIC_REPRESENTATION_ITEM()
RATIONAL_B_SPLINE_SURFACE(((0.997565691989291,0.996847118055594,0.996554836292953),
(0.997565691989291,0.996847118055594,0.996554836292953),(0.997565691989291,
0.996847118055594,0.996554836292953)))
REPRESENTATION_ITEM('')
SURFACE()
);
#187=(
BOUNDED_SURFACE()
B_SPLINE_SURFACE(1,2,((#70065,#70066,#70067,#70068,#70069),(#70070,#70071,
#70072,#70073,#70074),(#70075,#70076,#70077,#70078,#70079)),
 .UNSPECIFIED.,.F.,.F.,.F.)
B_SPLINE_SURFACE_WITH_KNOTS((2,1,2),(3,2,3),(0.,1.,1.01),(0.0355931932713903,
0.0384615384615384,0.0476086899858143),.UNSPECIFIED.)
GEOMETRIC_REPRESENTATION_ITEM()
RATIONAL_B_SPLINE_SURFACE(((0.998993602249807,0.999456249886298,1.,0.998265981131401,
0.997356751596327),(0.998993602249807,0.999456249886298,1.,0.998265981131401,
0.997356751596327),(0.998993602249807,0.999456249886298,1.,0.998265981131401,
0.997356751596327)))
REPRESENTATION_ITEM('')
SURFACE()
);
#188=(
BOUNDED_SURFACE()
B_SPLINE_SURFACE(1,2,((#70127,#70128,#70129,#70130,#70131),(#70132,#70133,
#70134,#70135,#70136),(#70137,#70138,#70139,#70140,#70141)),
 .UNSPECIFIED.,.F.,.F.,.F.)
B_SPLINE_SURFACE_WITH_KNOTS((2,1,2),(3,2,3),(-0.00141401191198383,0.,0.480770297090291),
(0.0365944846645756,0.0384615384615384,0.0431859280915189),
 .UNSPECIFIED.)
GEOMETRIC_REPRESENTATION_ITEM()
RATIONAL_B_SPLINE_SURFACE(((0.999326490452258,0.999646063968217,1.,0.999104400890347,
0.9984288220563),(0.999326490452258,0.999646063968217,1.,0.999104400890347,
0.9984288220563),(0.999326490452258,0.999646063968217,1.,0.999104400890347,
0.9984288220563)))
REPRESENTATION_ITEM('')
SURFACE()
);
#189=(
BOUNDED_SURFACE()
B_SPLINE_SURFACE(1,2,((#70168,#70169,#70170),(#70171,#70172,#70173),(#70174,
#70175,#70176)),.UNSPECIFIED.,.F.,.F.,.F.)
B_SPLINE_SURFACE_WITH_KNOTS((2,1,2),(3,3),(0.,1.,1.01),(0.0255903596131799,
0.0375948596693882),.UNSPECIFIED.)
GEOMETRIC_REPRESENTATION_ITEM()
RATIONAL_B_SPLINE_SURFACE(((0.996753121755999,0.997505687613148,0.999678813023854),
(0.996753121755999,0.997505687613148,0.999678813023854),(0.996753121755999,
0.997505687613148,0.999678813023854)))
REPRESENTATION_ITEM('')
SURFACE()
);
#190=(
BOUNDED_SURFACE()
B_SPLINE_SURFACE(1,2,((#70211,#70212,#70213),(#70214,#70215,#70216),(#70217,
#70218,#70219)),.UNSPECIFIED.,.F.,.F.,.F.)
B_SPLINE_SURFACE_WITH_KNOTS((2,1,2),(3,3),(-0.00286823356229767,0.,0.477902879797869),
(0.0265907346180625,0.0331702037252934),.UNSPECIFIED.)
GEOMETRIC_REPRESENTATION_ITEM()
RATIONAL_B_SPLINE_SURFACE(((0.996888414395785,0.997365765479939,0.998269846384985),
(0.996888414395785,0.997365765479939,0.998269846384985),(0.996888414395785,
0.997365765479939,0.998269846384985)))
REPRESENTATION_ITEM('')
SURFACE()
);
#191=(
BOUNDED_SURFACE()
B_SPLINE_SURFACE(1,2,((#70286,#70287,#70288),(#70289,#70290,#70291),(#70292,
#70293,#70294)),.UNSPECIFIED.,.F.,.F.,.F.)
B_SPLINE_SURFACE_WITH_KNOTS((2,1,2),(3,3),(-0.0028675312822896,0.,0.477902879799127),
(0.0166015299238957,0.0231736788111886),.UNSPECIFIED.)
GEOMETRIC_REPRESENTATION_ITEM()
RATIONAL_B_SPLINE_SURFACE(((0.996422581660833,0.996252244737342,0.996507688616404),
(0.996422581660833,0.996252244737342,0.996507688616404),(0.996422581660833,
0.996252244737342,0.996507688616404)))
REPRESENTATION_ITEM('')
SURFACE()
);
#192=(
BOUNDED_SURFACE()
B_SPLINE_SURFACE(1,2,((#70311,#70312,#70313),(#70314,#70315,#70316),(#70317,
#70318,#70319),(#70320,#70321,#70322)),.UNSPECIFIED.,.F.,.F.,.F.)
B_SPLINE_SURFACE_WITH_KNOTS((2,1,1,2),(3,3),(-0.0101,0.,1.,1.01),(0.00560769168370382,
0.0176009700440517),.UNSPECIFIED.)
GEOMETRIC_REPRESENTATION_ITEM()
RATIONAL_B_SPLINE_SURFACE(((0.998183892113821,0.99657330421516,0.996380621259469),
(0.998183892113821,0.99657330421516,0.996380621259469),(0.998183892113821,
0.99657330421516,0.996380621259469),(0.998183892113821,0.99657330421516,
0.996380621259469)))
REPRESENTATION_ITEM('')
SURFACE()
);
#193=(
BOUNDED_SURFACE()
B_SPLINE_SURFACE(1,2,((#70357,#70358,#70359),(#70360,#70361,#70362),(#70363,
#70364,#70365)),.UNSPECIFIED.,.F.,.F.,.F.)
B_SPLINE_SURFACE_WITH_KNOTS((2,1,2),(3,3),(-0.00206901892692145,0.,0.346769728502048),
(0.0066071315471865,0.0131849431468885),.UNSPECIFIED.)
GEOMETRIC_REPRESENTATION_ITEM()
RATIONAL_B_SPLINE_SURFACE(((0.997925307359452,0.997106772384943,0.996714752253861),
(0.997925307359452,0.997106772384943,0.996714752253861),(0.997925307359452,
0.997106772384943,0.996714752253861)))
REPRESENTATION_ITEM('')
SURFACE()
);
#194=(
BOUNDED_SURFACE()
B_SPLINE_SURFACE(1,2,((#70438,#70439,#70440),(#70441,#70442,#70443)),
 .UNSPECIFIED.,.F.,.F.,.F.)
B_SPLINE_SURFACE_WITH_KNOTS((2,2),(3,3),(0.,1.),(0.0556006976418414,0.0675888856590493),
 .UNSPECIFIED.)
GEOMETRIC_REPRESENTATION_ITEM()
RATIONAL_B_SPLINE_SURFACE(((0.996397562408606,0.996150386832629,0.997319912843745),
(0.996397562408606,0.996150386832629,0.997319912843745)))
REPRESENTATION_ITEM('')
SURFACE()
);
#195=(
BOUNDED_SURFACE()
B_SPLINE_SURFACE(1,2,((#70512,#70513,#70514),(#70515,#70516,#70517),(#70518,
#70519,#70520)),.UNSPECIFIED.,.F.,.F.,.F.)
B_SPLINE_SURFACE_WITH_KNOTS((2,1,2),(3,3),(0.,1.,1.01),(0.0456081671210046,
0.0575989447818808),.UNSPECIFIED.)
GEOMETRIC_REPRESENTATION_ITEM()
RATIONAL_B_SPLINE_SURFACE(((0.997793907739636,0.996365558499688,0.996354522974128),
(0.997793907739636,0.996365558499688,0.996354522974128),(0.997793907739636,
0.996365558499688,0.996354522974128)))
REPRESENTATION_ITEM('')
SURFACE()
);
#196=(
BOUNDED_SURFACE()
B_SPLINE_SURFACE(1,2,((#70555,#70556,#70557),(#70558,#70559,#70560),(#70561,
#70562,#70563)),.UNSPECIFIED.,.F.,.F.,.F.)
B_SPLINE_SURFACE_WITH_KNOTS((2,1,2),(3,3),(-0.00286810173532013,0.,0.477902879792973),
(0.0466073985929103,0.0531834929157972),.UNSPECIFIED.)
GEOMETRIC_REPRESENTATION_ITEM()
RATIONAL_B_SPLINE_SURFACE(((0.997565691989292,0.996847118055594,0.996554836292953),
(0.997565691989292,0.996847118055594,0.996554836292953),(0.997565691989292,
0.996847118055594,0.996554836292953)))
REPRESENTATION_ITEM('')
SURFACE()
);
#197=(
BOUNDED_SURFACE()
B_SPLINE_SURFACE(1,2,((#70580,#70581,#70582,#70583,#70584),(#70585,#70586,
#70587,#70588,#70589),(#70590,#70591,#70592,#70593,#70594)),
 .UNSPECIFIED.,.F.,.F.,.F.)
B_SPLINE_SURFACE_WITH_KNOTS((2,1,2),(3,2,3),(0.,1.,1.01),(0.0355931932713892,
0.0384615384615384,0.0476086899858129),.UNSPECIFIED.)
GEOMETRIC_REPRESENTATION_ITEM()
RATIONAL_B_SPLINE_SURFACE(((0.998993602249806,0.999456249886298,1.,0.998265981131401,
0.997356751596327),(0.998993602249806,0.999456249886298,1.,0.998265981131401,
0.997356751596327),(0.998993602249806,0.999456249886298,1.,0.998265981131401,
0.997356751596327)))
REPRESENTATION_ITEM('')
SURFACE()
);
#198=(
BOUNDED_SURFACE()
B_SPLINE_SURFACE(1,2,((#70642,#70643,#70644,#70645,#70646),(#70647,#70648,
#70649,#70650,#70651),(#70652,#70653,#70654,#70655,#70656)),
 .UNSPECIFIED.,.F.,.F.,.F.)
B_SPLINE_SURFACE_WITH_KNOTS((2,1,2),(3,2,3),(-0.00141401191198409,0.,0.480770297087816),
(0.0365944846645747,0.0384615384615384,0.0431859280915185),
 .UNSPECIFIED.)
GEOMETRIC_REPRESENTATION_ITEM()
RATIONAL_B_SPLINE_SURFACE(((0.999326490452258,0.999646063968217,1.,0.999104400890347,
0.9984288220563),(0.999326490452258,0.999646063968217,1.,0.999104400890347,
0.9984288220563),(0.999326490452258,0.999646063968217,1.,0.999104400890347,
0.9984288220563)))
REPRESENTATION_ITEM('')
SURFACE()
);
#199=(
BOUNDED_SURFACE()
B_SPLINE_SURFACE(1,2,((#70683,#70684,#70685),(#70686,#70687,#70688),(#70689,
#70690,#70691)),.UNSPECIFIED.,.F.,.F.,.F.)
B_SPLINE_SURFACE_WITH_KNOTS((2,1,2),(3,3),(0.,1.,1.01),(0.0255903596131799,
0.0375948596693877),.UNSPECIFIED.)
GEOMETRIC_REPRESENTATION_ITEM()
RATIONAL_B_SPLINE_SURFACE(((0.996753121755999,0.997505687613148,0.999678813023853),
(0.996753121755999,0.997505687613148,0.999678813023853),(0.996753121755999,
0.997505687613148,0.999678813023853)))
REPRESENTATION_ITEM('')
SURFACE()
);
#200=(
BOUNDED_SURFACE()
B_SPLINE_SURFACE(1,2,((#70726,#70727,#70728),(#70729,#70730,#70731),(#70732,
#70733,#70734)),.UNSPECIFIED.,.F.,.F.,.F.)
B_SPLINE_SURFACE_WITH_KNOTS((2,1,2),(3,3),(-0.00286823356226583,0.,0.477902879795317),
(0.0265907346180613,0.0331702037252919),.UNSPECIFIED.)
GEOMETRIC_REPRESENTATION_ITEM()
RATIONAL_B_SPLINE_SURFACE(((0.996888414395785,0.997365765479939,0.998269846384985),
(0.996888414395785,0.997365765479939,0.998269846384985),(0.996888414395785,
0.997365765479939,0.998269846384985)))
REPRESENTATION_ITEM('')
SURFACE()
);
#201=(
BOUNDED_SURFACE()
B_SPLINE_SURFACE(1,2,((#70801,#70802,#70803),(#70804,#70805,#70806),(#70807,
#70808,#70809)),.UNSPECIFIED.,.F.,.F.,.F.)
B_SPLINE_SURFACE_WITH_KNOTS((2,1,2),(3,3),(-0.00286753114057915,0.,0.477902879796716),
(0.0166015299238963,0.0231736788090048),.UNSPECIFIED.)
GEOMETRIC_REPRESENTATION_ITEM()
RATIONAL_B_SPLINE_SURFACE(((0.996422581660833,0.996252244737398,0.996507688616234),
(0.996422581660833,0.996252244737398,0.996507688616234),(0.996422581660833,
0.996252244737398,0.996507688616234)))
REPRESENTATION_ITEM('')
SURFACE()
);
#202=(
BOUNDED_SURFACE()
B_SPLINE_SURFACE(1,2,((#70826,#70827,#70828),(#70829,#70830,#70831),(#70832,
#70833,#70834),(#70835,#70836,#70837)),.UNSPECIFIED.,.F.,.F.,.F.)
B_SPLINE_SURFACE_WITH_KNOTS((2,1,1,2),(3,3),(-0.0101,0.,1.,1.01),(0.00560769168370605,
0.0176009700440523),.UNSPECIFIED.)
GEOMETRIC_REPRESENTATION_ITEM()
RATIONAL_B_SPLINE_SURFACE(((0.99818389211382,0.99657330421516,0.996380621259469),
(0.99818389211382,0.99657330421516,0.996380621259469),(0.99818389211382,
0.99657330421516,0.996380621259469),(0.99818389211382,0.99657330421516,
0.996380621259469)))
REPRESENTATION_ITEM('')
SURFACE()
);
#203=(
BOUNDED_SURFACE()
B_SPLINE_SURFACE(1,2,((#70872,#70873,#70874),(#70875,#70876,#70877),(#70878,
#70879,#70880)),.UNSPECIFIED.,.F.,.F.,.F.)
B_SPLINE_SURFACE_WITH_KNOTS((2,1,2),(3,3),(-0.00206901892691817,0.,0.346769728500459),
(0.00660713154719582,0.0131849431468882),.UNSPECIFIED.)
GEOMETRIC_REPRESENTATION_ITEM()
RATIONAL_B_SPLINE_SURFACE(((0.997925307359449,0.997106772384942,0.99671475225386),
(0.997925307359449,0.997106772384942,0.996714752253861),(0.997925307359449,
0.997106772384942,0.996714752253861)))
REPRESENTATION_ITEM('')
SURFACE()
);
#204=(
BOUNDED_SURFACE()
B_SPLINE_SURFACE(1,2,((#70953,#70954,#70955),(#70956,#70957,#70958)),
 .UNSPECIFIED.,.F.,.F.,.F.)
B_SPLINE_SURFACE_WITH_KNOTS((2,2),(3,3),(0.,1.),(0.0556006976418436,0.0675888856590503),
 .UNSPECIFIED.)
GEOMETRIC_REPRESENTATION_ITEM()
RATIONAL_B_SPLINE_SURFACE(((0.996397562408606,0.996150386832629,0.997319912843745),
(0.996397562408606,0.996150386832629,0.997319912843745)))
REPRESENTATION_ITEM('')
SURFACE()
);
#205=(
BOUNDED_SURFACE()
B_SPLINE_SURFACE(1,2,((#71027,#71028,#71029),(#71030,#71031,#71032),(#71033,
#71034,#71035)),.UNSPECIFIED.,.F.,.F.,.F.)
B_SPLINE_SURFACE_WITH_KNOTS((2,1,2),(3,3),(0.,1.,1.01),(0.0456081671210056,
0.0575989447818813),.UNSPECIFIED.)
GEOMETRIC_REPRESENTATION_ITEM()
RATIONAL_B_SPLINE_SURFACE(((0.997793907739636,0.996365558499688,0.996354522974128),
(0.997793907739636,0.996365558499688,0.996354522974128),(0.997793907739636,
0.996365558499688,0.996354522974128)))
REPRESENTATION_ITEM('')
SURFACE()
);
#206=(
BOUNDED_SURFACE()
B_SPLINE_SURFACE(1,2,((#71070,#71071,#71072),(#71073,#71074,#71075),(#71076,
#71077,#71078)),.UNSPECIFIED.,.F.,.F.,.F.)
B_SPLINE_SURFACE_WITH_KNOTS((2,1,2),(3,3),(-0.00286810173524515,0.,0.477902879790257),
(0.0466073985929112,0.0531834929157974),.UNSPECIFIED.)
GEOMETRIC_REPRESENTATION_ITEM()
RATIONAL_B_SPLINE_SURFACE(((0.997565691989291,0.996847118055594,0.996554836292953),
(0.997565691989291,0.996847118055594,0.996554836292953),(0.997565691989291,
0.996847118055594,0.996554836292953)))
REPRESENTATION_ITEM('')
SURFACE()
);
#207=(
BOUNDED_SURFACE()
B_SPLINE_SURFACE(1,2,((#71095,#71096,#71097,#71098,#71099),(#71100,#71101,
#71102,#71103,#71104),(#71105,#71106,#71107,#71108,#71109)),
 .UNSPECIFIED.,.F.,.F.,.F.)
B_SPLINE_SURFACE_WITH_KNOTS((2,1,2),(3,2,3),(0.,1.,1.01),(0.0355931932713904,
0.0384615384615384,0.0476086899858132),.UNSPECIFIED.)
GEOMETRIC_REPRESENTATION_ITEM()
RATIONAL_B_SPLINE_SURFACE(((0.998993602249807,0.999456249886298,1.,0.998265981131401,
0.997356751596327),(0.998993602249807,0.999456249886298,1.,0.998265981131401,
0.997356751596327),(0.998993602249807,0.999456249886298,1.,0.998265981131401,
0.997356751596327)))
REPRESENTATION_ITEM('')
SURFACE()
);
#208=(
BOUNDED_SURFACE()
B_SPLINE_SURFACE(1,2,((#71157,#71158,#71159,#71160,#71161),(#71162,#71163,
#71164,#71165,#71166),(#71167,#71168,#71169,#71170,#71171)),
 .UNSPECIFIED.,.F.,.F.,.F.)
B_SPLINE_SURFACE_WITH_KNOTS((2,1,2),(3,2,3),(-0.00141401191198426,0.,0.480770297085224),
(0.0365944846645756,0.0384615384615384,0.0431859280915178),
 .UNSPECIFIED.)
GEOMETRIC_REPRESENTATION_ITEM()
RATIONAL_B_SPLINE_SURFACE(((0.999326490452258,0.999646063968217,1.,0.999104400890347,
0.9984288220563),(0.999326490452258,0.999646063968217,1.,0.999104400890347,
0.9984288220563),(0.999326490452258,0.999646063968217,1.,0.999104400890347,
0.9984288220563)))
REPRESENTATION_ITEM('')
SURFACE()
);
#209=(
BOUNDED_SURFACE()
B_SPLINE_SURFACE(1,2,((#71198,#71199,#71200),(#71201,#71202,#71203),(#71204,
#71205,#71206)),.UNSPECIFIED.,.F.,.F.,.F.)
B_SPLINE_SURFACE_WITH_KNOTS((2,1,2),(3,3),(0.,1.,1.01),(0.0255903596131787,
0.0375948596693877),.UNSPECIFIED.)
GEOMETRIC_REPRESENTATION_ITEM()
RATIONAL_B_SPLINE_SURFACE(((0.996753121755999,0.997505687613148,0.999678813023853),
(0.996753121755999,0.997505687613148,0.999678813023853),(0.996753121755999,
0.997505687613148,0.999678813023853)))
REPRESENTATION_ITEM('')
SURFACE()
);
#210=(
BOUNDED_SURFACE()
B_SPLINE_SURFACE(1,2,((#71241,#71242,#71243),(#71244,#71245,#71246),(#71247,
#71248,#71249)),.UNSPECIFIED.,.F.,.F.,.F.)
B_SPLINE_SURFACE_WITH_KNOTS((2,1,2),(3,3),(-0.00286823356222536,0.,0.477902879792683),
(0.0265907346180612,0.0331702037252918),.UNSPECIFIED.)
GEOMETRIC_REPRESENTATION_ITEM()
RATIONAL_B_SPLINE_SURFACE(((0.996888414395785,0.997365765479939,0.998269846384985),
(0.996888414395785,0.997365765479939,0.998269846384985),(0.996888414395785,
0.997365765479939,0.998269846384985)))
REPRESENTATION_ITEM('')
SURFACE()
);
#211=(
BOUNDED_SURFACE()
B_SPLINE_SURFACE(1,2,((#71316,#71317,#71318),(#71319,#71320,#71321),(#71322,
#71323,#71324)),.UNSPECIFIED.,.F.,.F.,.F.)
B_SPLINE_SURFACE_WITH_KNOTS((2,1,2),(3,3),(-0.00286753074374937,0.,0.477902879794037),
(0.0166015299238958,0.023173678802883),.UNSPECIFIED.)
GEOMETRIC_REPRESENTATION_ITEM()
RATIONAL_B_SPLINE_SURFACE(((0.996422581660833,0.996252244737557,0.996507688615759),
(0.996422581660833,0.996252244737557,0.996507688615759),(0.996422581660833,
0.996252244737557,0.996507688615759)))
REPRESENTATION_ITEM('')
SURFACE()
);
#212=(
BOUNDED_SURFACE()
B_SPLINE_SURFACE(1,2,((#71341,#71342,#71343),(#71344,#71345,#71346),(#71347,
#71348,#71349),(#71350,#71351,#71352)),.UNSPECIFIED.,.F.,.F.,.F.)
B_SPLINE_SURFACE_WITH_KNOTS((2,1,1,2),(3,3),(-0.0101,0.,1.,1.01),(0.00560769168370419,
0.0176009700440507),.UNSPECIFIED.)
GEOMETRIC_REPRESENTATION_ITEM()
RATIONAL_B_SPLINE_SURFACE(((0.998183892113821,0.99657330421516,0.996380621259469),
(0.998183892113821,0.99657330421516,0.996380621259469),(0.998183892113821,
0.99657330421516,0.996380621259469),(0.998183892113821,0.99657330421516,
0.996380621259469)))
REPRESENTATION_ITEM('')
SURFACE()
);
#213=(
BOUNDED_SURFACE()
B_SPLINE_SURFACE(1,2,((#71387,#71388,#71389),(#71390,#71391,#71392),(#71393,
#71394,#71395)),.UNSPECIFIED.,.F.,.F.,.F.)
B_SPLINE_SURFACE_WITH_KNOTS((2,1,2),(3,3),(-0.00206901892690419,0.,0.346769728499074),
(0.00660713154720198,0.0131849431468887),.UNSPECIFIED.)
GEOMETRIC_REPRESENTATION_ITEM()
RATIONAL_B_SPLINE_SURFACE(((0.997925307359448,0.997106772384942,0.996714752253861),
(0.997925307359448,0.997106772384942,0.996714752253861),(0.997925307359448,
0.997106772384942,0.996714752253861)))
REPRESENTATION_ITEM('')
SURFACE()
);
#214=(
BOUNDED_SURFACE()
B_SPLINE_SURFACE(1,2,((#71468,#71469,#71470),(#71471,#71472,#71473)),
 .UNSPECIFIED.,.F.,.F.,.F.)
B_SPLINE_SURFACE_WITH_KNOTS((2,2),(3,3),(0.,1.),(0.0556006976418414,0.06758888565905),
 .UNSPECIFIED.)
GEOMETRIC_REPRESENTATION_ITEM()
RATIONAL_B_SPLINE_SURFACE(((0.996397562408606,0.996150386832629,0.997319912843745),
(0.996397562408606,0.996150386832629,0.997319912843745)))
REPRESENTATION_ITEM('')
SURFACE()
);
#215=(
BOUNDED_SURFACE()
B_SPLINE_SURFACE(1,2,((#71542,#71543,#71544),(#71545,#71546,#71547),(#71548,
#71549,#71550)),.UNSPECIFIED.,.F.,.F.,.F.)
B_SPLINE_SURFACE_WITH_KNOTS((2,1,2),(3,3),(0.,1.,1.01),(0.0456081671210075,
0.0575989447818828),.UNSPECIFIED.)
GEOMETRIC_REPRESENTATION_ITEM()
RATIONAL_B_SPLINE_SURFACE(((0.997793907739635,0.996365558499688,0.996354522974128),
(0.997793907739635,0.996365558499688,0.996354522974128),(0.997793907739635,
0.996365558499688,0.996354522974128)))
REPRESENTATION_ITEM('')
SURFACE()
);
#216=(
BOUNDED_SURFACE()
B_SPLINE_SURFACE(1,2,((#71585,#71586,#71587),(#71588,#71589,#71590),(#71591,
#71592,#71593)),.UNSPECIFIED.,.F.,.F.,.F.)
B_SPLINE_SURFACE_WITH_KNOTS((2,1,2),(3,3),(-0.00286810172002,0.,0.477902879787716),
(0.0466073985929109,0.0531834927425526),.UNSPECIFIED.)
GEOMETRIC_REPRESENTATION_ITEM()
RATIONAL_B_SPLINE_SURFACE(((0.997565691989291,0.996847118074524,0.996554836308353),
(0.997565691989291,0.996847118074524,0.996554836308353),(0.997565691989291,
0.996847118074524,0.996554836308353)))
REPRESENTATION_ITEM('')
SURFACE()
);
#217=(
BOUNDED_SURFACE()
B_SPLINE_SURFACE(1,2,((#71610,#71611,#71612,#71613,#71614),(#71615,#71616,
#71617,#71618,#71619),(#71620,#71621,#71622,#71623,#71624)),
 .UNSPECIFIED.,.F.,.F.,.F.)
B_SPLINE_SURFACE_WITH_KNOTS((2,1,2),(3,2,3),(0.,1.,1.01),(0.0355931932713914,
0.0384615384615384,0.0476086899858133),.UNSPECIFIED.)
GEOMETRIC_REPRESENTATION_ITEM()
RATIONAL_B_SPLINE_SURFACE(((0.998993602249807,0.999456249886298,1.,0.998265981131401,
0.997356751596327),(0.998993602249807,0.999456249886298,1.,0.998265981131401,
0.997356751596327),(0.998993602249807,0.999456249886298,1.,0.998265981131401,
0.997356751596327)))
REPRESENTATION_ITEM('')
SURFACE()
);
#218=(
BOUNDED_SURFACE()
B_SPLINE_SURFACE(1,2,((#71672,#71673,#71674,#71675,#71676),(#71677,#71678,
#71679,#71680,#71681),(#71682,#71683,#71684,#71685,#71686)),
 .UNSPECIFIED.,.F.,.F.,.F.)
B_SPLINE_SURFACE_WITH_KNOTS((2,1,2),(3,2,3),(-0.00286742666571506,0.,0.480770297123148),
(0.0365944846644088,0.0384615384615384,0.043185928091519),.UNSPECIFIED.)
GEOMETRIC_REPRESENTATION_ITEM()
RATIONAL_B_SPLINE_SURFACE(((0.999326490452201,0.999646063968185,1.,0.999104400890347,
0.9984288220563),(0.999326490452201,0.999646063968185,1.,0.999104400890347,
0.9984288220563),(0.999326490452201,0.999646063968185,1.,0.999104400890347,
0.9984288220563)))
REPRESENTATION_ITEM('')
SURFACE()
);
#219=(
BOUNDED_SURFACE()
B_SPLINE_SURFACE(1,2,((#71713,#71714,#71715),(#71716,#71717,#71718),(#71719,
#71720,#71721)),.UNSPECIFIED.,.F.,.F.,.F.)
B_SPLINE_SURFACE_WITH_KNOTS((2,1,2),(3,3),(0.,1.,1.01),(0.025590359613181,
0.0375948596693869),.UNSPECIFIED.)
GEOMETRIC_REPRESENTATION_ITEM()
RATIONAL_B_SPLINE_SURFACE(((0.996753121755999,0.997505687613148,0.999678813023853),
(0.996753121755999,0.997505687613148,0.999678813023853),(0.996753121755999,
0.997505687613148,0.999678813023853)))
REPRESENTATION_ITEM('')
SURFACE()
);
#220=(
BOUNDED_SURFACE()
B_SPLINE_SURFACE(1,2,((#71756,#71757,#71758),(#71759,#71760,#71761),(#71762,
#71763,#71764)),.UNSPECIFIED.,.F.,.F.,.F.)
B_SPLINE_SURFACE_WITH_KNOTS((2,1,2),(3,3),(-0.00286823257317966,0.,0.477902879790169),
(0.0265907346180612,0.0331702037100437),.UNSPECIFIED.)
GEOMETRIC_REPRESENTATION_ITEM()
RATIONAL_B_SPLINE_SURFACE(((0.996888414395785,0.997365765478833,0.998269846380795),
(0.996888414395785,0.997365765478833,0.998269846380795),(0.996888414395785,
0.997365765478833,0.998269846380795)))
REPRESENTATION_ITEM('')
SURFACE()
);
#221=(
BOUNDED_SURFACE()
B_SPLINE_SURFACE(1,2,((#71831,#71832,#71833),(#71834,#71835,#71836),(#71837,
#71838,#71839)),.UNSPECIFIED.,.F.,.F.,.F.)
B_SPLINE_SURFACE_WITH_KNOTS((2,1,2),(3,3),(-0.00286753114053279,0.,0.477902879791518),
(0.0166015299238948,0.0231736788090038),.UNSPECIFIED.)
GEOMETRIC_REPRESENTATION_ITEM()
RATIONAL_B_SPLINE_SURFACE(((0.996422581660833,0.996252244737398,0.996507688616235),
(0.996422581660833,0.996252244737398,0.996507688616234),(0.996422581660833,
0.996252244737398,0.996507688616235)))
REPRESENTATION_ITEM('')
SURFACE()
);
#222=(
BOUNDED_SURFACE()
B_SPLINE_SURFACE(1,2,((#71856,#71857,#71858),(#71859,#71860,#71861),(#71862,
#71863,#71864),(#71865,#71866,#71867)),.UNSPECIFIED.,.F.,.F.,.F.)
B_SPLINE_SURFACE_WITH_KNOTS((2,1,1,2),(3,3),(-0.0101,0.,1.,1.01),(0.00560769168370626,
0.0176009700440511),.UNSPECIFIED.)
GEOMETRIC_REPRESENTATION_ITEM()
RATIONAL_B_SPLINE_SURFACE(((0.99818389211382,0.99657330421516,0.996380621259469),
(0.99818389211382,0.99657330421516,0.996380621259469),(0.99818389211382,
0.99657330421516,0.996380621259469),(0.99818389211382,0.99657330421516,
0.996380621259469)))
REPRESENTATION_ITEM('')
SURFACE()
);
#223=(
BOUNDED_SURFACE()
B_SPLINE_SURFACE(1,2,((#71902,#71903,#71904),(#71905,#71906,#71907),(#71908,
#71909,#71910)),.UNSPECIFIED.,.F.,.F.,.F.)
B_SPLINE_SURFACE_WITH_KNOTS((2,1,2),(3,3),(-0.00206901892684705,0.,0.346769728497568),
(0.00660713154720629,0.0131849431468891),.UNSPECIFIED.)
GEOMETRIC_REPRESENTATION_ITEM()
RATIONAL_B_SPLINE_SURFACE(((0.997925307359447,0.997106772384942,0.996714752253861),
(0.997925307359447,0.997106772384942,0.996714752253861),(0.997925307359447,
0.997106772384942,0.996714752253861)))
REPRESENTATION_ITEM('')
SURFACE()
);
#224=(
BOUNDED_SURFACE()
B_SPLINE_SURFACE(1,2,((#71983,#71984,#71985),(#71986,#71987,#71988)),
 .UNSPECIFIED.,.F.,.F.,.F.)
B_SPLINE_SURFACE_WITH_KNOTS((2,2),(3,3),(0.,1.),(0.0556006976418414,0.0675888856590497),
 .UNSPECIFIED.)
GEOMETRIC_REPRESENTATION_ITEM()
RATIONAL_B_SPLINE_SURFACE(((0.996397562408606,0.996150386832629,0.997319912843745),
(0.996397562408606,0.996150386832629,0.997319912843745)))
REPRESENTATION_ITEM('')
SURFACE()
);
#225=(
BOUNDED_SURFACE()
B_SPLINE_SURFACE(1,2,((#72057,#72058,#72059),(#72060,#72061,#72062),(#72063,
#72064,#72065)),.UNSPECIFIED.,.F.,.F.,.F.)
B_SPLINE_SURFACE_WITH_KNOTS((2,1,2),(3,3),(0.,1.,1.01),(0.0456081671210055,
0.0575989447818817),.UNSPECIFIED.)
GEOMETRIC_REPRESENTATION_ITEM()
RATIONAL_B_SPLINE_SURFACE(((0.997793907739636,0.996365558499688,0.996354522974128),
(0.997793907739636,0.996365558499688,0.996354522974128),(0.997793907739636,
0.996365558499688,0.996354522974128)))
REPRESENTATION_ITEM('')
SURFACE()
);
#226=(
BOUNDED_SURFACE()
B_SPLINE_SURFACE(1,2,((#72100,#72101,#72102),(#72103,#72104,#72105),(#72106,
#72107,#72108)),.UNSPECIFIED.,.F.,.F.,.F.)
B_SPLINE_SURFACE_WITH_KNOTS((2,1,2),(3,3),(-0.00286810173515641,0.,0.477902879786463),
(0.0466073985929113,0.0531834929157985),.UNSPECIFIED.)
GEOMETRIC_REPRESENTATION_ITEM()
RATIONAL_B_SPLINE_SURFACE(((0.997565691989292,0.996847118055594,0.996554836292953),
(0.997565691989292,0.996847118055594,0.996554836292953),(0.997565691989292,
0.996847118055594,0.996554836292953)))
REPRESENTATION_ITEM('')
SURFACE()
);
#227=(
BOUNDED_SURFACE()
B_SPLINE_SURFACE(1,2,((#72125,#72126,#72127,#72128,#72129),(#72130,#72131,
#72132,#72133,#72134),(#72135,#72136,#72137,#72138,#72139)),
 .UNSPECIFIED.,.F.,.F.,.F.)
B_SPLINE_SURFACE_WITH_KNOTS((2,1,2),(3,2,3),(0.,1.,1.01),(0.0355931932713902,
0.0384615384615384,0.0476086899858155),.UNSPECIFIED.)
GEOMETRIC_REPRESENTATION_ITEM()
RATIONAL_B_SPLINE_SURFACE(((0.998993602249807,0.999456249886298,1.,0.9982659811314,
0.997356751596326),(0.998993602249807,0.999456249886298,1.,0.9982659811314,
0.997356751596326),(0.998993602249807,0.999456249886298,1.,0.9982659811314,
0.997356751596326)))
REPRESENTATION_ITEM('')
SURFACE()
);
#228=(
BOUNDED_SURFACE()
B_SPLINE_SURFACE(1,2,((#72187,#72188,#72189,#72190,#72191),(#72192,#72193,
#72194,#72195,#72196),(#72197,#72198,#72199,#72200,#72201)),
 .UNSPECIFIED.,.F.,.F.,.F.)
B_SPLINE_SURFACE_WITH_KNOTS((2,1,2),(3,2,3),(-0.00286743097398646,0.,0.480770297146974),
(0.0365944846644077,0.0384615384615384,0.0431859280915196),
 .UNSPECIFIED.)
GEOMETRIC_REPRESENTATION_ITEM()
RATIONAL_B_SPLINE_SURFACE(((0.999326490452201,0.999646063968185,1.,0.999104400890347,
0.9984288220563),(0.999326490452201,0.999646063968185,1.,0.999104400890347,
0.9984288220563),(0.999326490452201,0.999646063968185,1.,0.999104400890347,
0.9984288220563)))
REPRESENTATION_ITEM('')
SURFACE()
);
#229=(
BOUNDED_SURFACE()
B_SPLINE_SURFACE(1,2,((#72228,#72229,#72230),(#72231,#72232,#72233),(#72234,
#72235,#72236)),.UNSPECIFIED.,.F.,.F.,.F.)
B_SPLINE_SURFACE_WITH_KNOTS((2,1,2),(3,3),(0.,1.,1.01),(0.0255903596131818,
0.0375948596693897),.UNSPECIFIED.)
GEOMETRIC_REPRESENTATION_ITEM()
RATIONAL_B_SPLINE_SURFACE(((0.996753121755999,0.997505687613148,0.999678813023854),
(0.996753121755999,0.997505687613148,0.999678813023854),(0.996753121755999,
0.997505687613148,0.999678813023854)))
REPRESENTATION_ITEM('')
SURFACE()
);
#230=(
BOUNDED_SURFACE()
B_SPLINE_SURFACE(1,2,((#72271,#72272,#72273),(#72274,#72275,#72276),(#72277,
#72278,#72279)),.UNSPECIFIED.,.F.,.F.,.F.)
B_SPLINE_SURFACE_WITH_KNOTS((2,1,2),(3,3),(-0.00286823045902527,0.,0.477902879787612),
(0.0265907346180616,0.0331702036774543),.UNSPECIFIED.)
GEOMETRIC_REPRESENTATION_ITEM()
RATIONAL_B_SPLINE_SURFACE(((0.996888414395785,0.997365765476469,0.998269846371839),
(0.996888414395785,0.997365765476469,0.998269846371839),(0.996888414395785,
0.997365765476469,0.998269846371839)))
REPRESENTATION_ITEM('')
SURFACE()
);
#231=(
BOUNDED_SURFACE()
B_SPLINE_SURFACE(1,2,((#72346,#72347,#72348),(#72349,#72350,#72351),(#72352,
#72353,#72354)),.UNSPECIFIED.,.F.,.F.,.F.)
B_SPLINE_SURFACE_WITH_KNOTS((2,1,2),(3,3),(-0.00286753128207188,0.,0.477902879788894),
(0.0166015299238944,0.0231736788111879),.UNSPECIFIED.)
GEOMETRIC_REPRESENTATION_ITEM()
RATIONAL_B_SPLINE_SURFACE(((0.996422581660833,0.996252244737341,0.996507688616404),
(0.996422581660833,0.996252244737341,0.996507688616404),(0.996422581660833,
0.996252244737341,0.996507688616404)))
REPRESENTATION_ITEM('')
SURFACE()
);
#232=(
BOUNDED_SURFACE()
B_SPLINE_SURFACE(1,2,((#72371,#72372,#72373),(#72374,#72375,#72376),(#72377,
#72378,#72379),(#72380,#72381,#72382)),.UNSPECIFIED.,.F.,.F.,.F.)
B_SPLINE_SURFACE_WITH_KNOTS((2,1,1,2),(3,3),(-0.0101,0.,1.,1.01),(0.00560769168370511,
0.0176009700440523),.UNSPECIFIED.)
GEOMETRIC_REPRESENTATION_ITEM()
RATIONAL_B_SPLINE_SURFACE(((0.998183892113821,0.99657330421516,0.996380621259469),
(0.998183892113821,0.99657330421516,0.996380621259469),(0.998183892113821,
0.99657330421516,0.996380621259469),(0.998183892113821,0.99657330421516,
0.996380621259469)))
REPRESENTATION_ITEM('')
SURFACE()
);
#233=(
BOUNDED_SURFACE()
B_SPLINE_SURFACE(1,2,((#72417,#72418,#72419),(#72420,#72421,#72422),(#72423,
#72424,#72425)),.UNSPECIFIED.,.F.,.F.,.F.)
B_SPLINE_SURFACE_WITH_KNOTS((2,1,2),(3,3),(-0.00206901892682504,0.,0.346769728496379),
(0.0066071315472073,0.0131849431468888),.UNSPECIFIED.)
GEOMETRIC_REPRESENTATION_ITEM()
RATIONAL_B_SPLINE_SURFACE(((0.997925307359446,0.997106772384942,0.996714752253861),
(0.997925307359446,0.997106772384942,0.996714752253861),(0.997925307359446,
0.997106772384942,0.996714752253861)))
REPRESENTATION_ITEM('')
SURFACE()
);
#234=(
BOUNDED_SURFACE()
B_SPLINE_SURFACE(1,2,((#72498,#72499,#72500),(#72501,#72502,#72503)),
 .UNSPECIFIED.,.F.,.F.,.F.)
B_SPLINE_SURFACE_WITH_KNOTS((2,2),(3,3),(0.,1.),(0.0556006976418428,0.0675888856590498),
 .UNSPECIFIED.)
GEOMETRIC_REPRESENTATION_ITEM()
RATIONAL_B_SPLINE_SURFACE(((0.996397562408606,0.996150386832629,0.997319912843745),
(0.996397562408606,0.996150386832629,0.997319912843745)))
REPRESENTATION_ITEM('')
SURFACE()
);
#235=(
BOUNDED_SURFACE()
B_SPLINE_SURFACE(1,2,((#72572,#72573,#72574),(#72575,#72576,#72577),(#72578,
#72579,#72580)),.UNSPECIFIED.,.F.,.F.,.F.)
B_SPLINE_SURFACE_WITH_KNOTS((2,1,2),(3,3),(0.,1.,1.01),(0.0456081671210033,
0.057598944781882),.UNSPECIFIED.)
GEOMETRIC_REPRESENTATION_ITEM()
RATIONAL_B_SPLINE_SURFACE(((0.997793907739636,0.996365558499688,0.996354522974128),
(0.997793907739636,0.996365558499688,0.996354522974128),(0.997793907739636,
0.996365558499688,0.996354522974128)))
REPRESENTATION_ITEM('')
SURFACE()
);
#236=(
BOUNDED_SURFACE()
B_SPLINE_SURFACE(1,2,((#72615,#72616,#72617),(#72618,#72619,#72620),(#72621,
#72622,#72623)),.UNSPECIFIED.,.F.,.F.,.F.)
B_SPLINE_SURFACE_WITH_KNOTS((2,1,2),(3,3),(-0.00286810173510994,0.,0.477902879786495),
(0.0466073985929119,0.0531834929157975),.UNSPECIFIED.)
GEOMETRIC_REPRESENTATION_ITEM()
RATIONAL_B_SPLINE_SURFACE(((0.997565691989291,0.996847118055594,0.996554836292953),
(0.997565691989291,0.996847118055594,0.996554836292953),(0.997565691989291,
0.996847118055594,0.996554836292953)))
REPRESENTATION_ITEM('')
SURFACE()
);
#237=(
BOUNDED_SURFACE()
B_SPLINE_SURFACE(1,2,((#72640,#72641,#72642,#72643,#72644),(#72645,#72646,
#72647,#72648,#72649),(#72650,#72651,#72652,#72653,#72654)),
 .UNSPECIFIED.,.F.,.F.,.F.)
B_SPLINE_SURFACE_WITH_KNOTS((2,1,2),(3,2,3),(0.,1.,1.01),(0.0355931932713904,
0.0384615384615384,0.0476086899858138),.UNSPECIFIED.)
GEOMETRIC_REPRESENTATION_ITEM()
RATIONAL_B_SPLINE_SURFACE(((0.998993602249807,0.999456249886298,1.,0.998265981131401,
0.997356751596327),(0.998993602249807,0.999456249886298,1.,0.998265981131401,
0.997356751596327),(0.998993602249807,0.999456249886298,1.,0.998265981131401,
0.997356751596327)))
REPRESENTATION_ITEM('')
SURFACE()
);
#238=(
BOUNDED_SURFACE()
B_SPLINE_SURFACE(1,2,((#72702,#72703,#72704,#72705,#72706),(#72707,#72708,
#72709,#72710,#72711),(#72712,#72713,#72714,#72715,#72716)),
 .UNSPECIFIED.,.F.,.F.,.F.)
B_SPLINE_SURFACE_WITH_KNOTS((2,1,2),(3,2,3),(-0.00141401191198139,0.,0.480770297079875),
(0.0365944846645798,0.0384615384615384,0.0431859280915183),
 .UNSPECIFIED.)
GEOMETRIC_REPRESENTATION_ITEM()
RATIONAL_B_SPLINE_SURFACE(((0.99932649045226,0.999646063968218,1.,0.999104400890347,
0.9984288220563),(0.99932649045226,0.999646063968218,1.,0.999104400890347,
0.9984288220563),(0.99932649045226,0.999646063968218,1.,0.999104400890347,
0.9984288220563)))
REPRESENTATION_ITEM('')
SURFACE()
);
#239=(
BOUNDED_SURFACE()
B_SPLINE_SURFACE(1,2,((#72743,#72744,#72745),(#72746,#72747,#72748),(#72749,
#72750,#72751)),.UNSPECIFIED.,.F.,.F.,.F.)
B_SPLINE_SURFACE_WITH_KNOTS((2,1,2),(3,3),(0.,1.,1.01),(0.0255903596131808,
0.0375948596693885),.UNSPECIFIED.)
GEOMETRIC_REPRESENTATION_ITEM()
RATIONAL_B_SPLINE_SURFACE(((0.996753121755999,0.997505687613148,0.999678813023854),
(0.996753121755999,0.997505687613148,0.999678813023854),(0.996753121755999,
0.997505687613148,0.999678813023854)))
REPRESENTATION_ITEM('')
SURFACE()
);
#240=(
BOUNDED_SURFACE()
B_SPLINE_SURFACE(1,2,((#72786,#72787,#72788),(#72789,#72790,#72791),(#72792,
#72793,#72794)),.UNSPECIFIED.,.F.,.F.,.F.)
B_SPLINE_SURFACE_WITH_KNOTS((2,1,2),(3,3),(-0.00286823356224596,0.,0.47790287978649),
(0.0265907346180609,0.0331702037252913),.UNSPECIFIED.)
GEOMETRIC_REPRESENTATION_ITEM()
RATIONAL_B_SPLINE_SURFACE(((0.996888414395785,0.997365765479939,0.998269846384985),
(0.996888414395785,0.997365765479939,0.998269846384985),(0.996888414395785,
0.997365765479939,0.998269846384985)))
REPRESENTATION_ITEM('')
SURFACE()
);
#241=(
BOUNDED_SURFACE()
B_SPLINE_SURFACE(1,2,((#72861,#72862,#72863),(#72864,#72865,#72866),(#72867,
#72868,#72869)),.UNSPECIFIED.,.F.,.F.,.F.)
B_SPLINE_SURFACE_WITH_KNOTS((2,1,2),(3,3),(-0.00286753128217537,0.,0.477902879803344),
(0.0166015299238946,0.0231736788111885),.UNSPECIFIED.)
GEOMETRIC_REPRESENTATION_ITEM()
RATIONAL_B_SPLINE_SURFACE(((0.996422581660833,0.996252244737341,0.996507688616404),
(0.996422581660833,0.996252244737341,0.996507688616404),(0.996422581660833,
0.996252244737341,0.996507688616404)))
REPRESENTATION_ITEM('')
SURFACE()
);
#242=(
BOUNDED_SURFACE()
B_SPLINE_SURFACE(1,2,((#72886,#72887,#72888),(#72889,#72890,#72891),(#72892,
#72893,#72894),(#72895,#72896,#72897)),.UNSPECIFIED.,.F.,.F.,.F.)
B_SPLINE_SURFACE_WITH_KNOTS((2,1,1,2),(3,3),(-0.0101,0.,1.,1.01),(0.0056076916837073,
0.0176009700440516),.UNSPECIFIED.)
GEOMETRIC_REPRESENTATION_ITEM()
RATIONAL_B_SPLINE_SURFACE(((0.99818389211382,0.99657330421516,0.996380621259469),
(0.99818389211382,0.99657330421516,0.996380621259469),(0.99818389211382,
0.99657330421516,0.996380621259469),(0.99818389211382,0.99657330421516,
0.996380621259469)))
REPRESENTATION_ITEM('')
SURFACE()
);
#243=(
BOUNDED_SURFACE()
B_SPLINE_SURFACE(1,2,((#72932,#72933,#72934),(#72935,#72936,#72937),(#72938,
#72939,#72940)),.UNSPECIFIED.,.F.,.F.,.F.)
B_SPLINE_SURFACE_WITH_KNOTS((2,1,2),(3,3),(-0.00206901892514686,0.,0.346769728494917),
(0.00660713154720862,0.0131849431292488),.UNSPECIFIED.)
GEOMETRIC_REPRESENTATION_ITEM()
RATIONAL_B_SPLINE_SURFACE(((0.997925307359446,0.997106772387137,0.996714752255963),
(0.997925307359446,0.997106772387137,0.996714752255963),(0.997925307359446,
0.997106772387137,0.996714752255963)))
REPRESENTATION_ITEM('')
SURFACE()
);
#244=(
BOUNDED_SURFACE()
B_SPLINE_SURFACE(1,2,((#73013,#73014,#73015),(#73016,#73017,#73018)),
 .UNSPECIFIED.,.F.,.F.,.F.)
B_SPLINE_SURFACE_WITH_KNOTS((2,2),(3,3),(0.,1.),(0.0556006976418414,0.0675888856590506),
 .UNSPECIFIED.)
GEOMETRIC_REPRESENTATION_ITEM()
RATIONAL_B_SPLINE_SURFACE(((0.996397562408606,0.996150386832629,0.997319912843745),
(0.996397562408606,0.996150386832629,0.997319912843745)))
REPRESENTATION_ITEM('')
SURFACE()
);
#245=(
BOUNDED_SURFACE()
B_SPLINE_SURFACE(1,2,((#73087,#73088,#73089),(#73090,#73091,#73092)),
 .UNSPECIFIED.,.F.,.F.,.F.)
B_SPLINE_SURFACE_WITH_KNOTS((2,2),(3,3),(0.,1.),(0.0456081671210034,0.0575989447818825),
 .UNSPECIFIED.)
GEOMETRIC_REPRESENTATION_ITEM()
RATIONAL_B_SPLINE_SURFACE(((0.997793907739636,0.996365558499688,0.996354522974128),
(0.997793907739636,0.996365558499688,0.996354522974128)))
REPRESENTATION_ITEM('')
SURFACE()
);
#246=(
BOUNDED_SURFACE()
B_SPLINE_SURFACE(1,2,((#73159,#73160,#73161,#73162,#73163),(#73164,#73165,
#73166,#73167,#73168),(#73169,#73170,#73171,#73172,#73173)),
 .UNSPECIFIED.,.F.,.F.,.F.)
B_SPLINE_SURFACE_WITH_KNOTS((2,1,2),(3,2,3),(0.,1.,1.01),(0.0355931932713903,
0.0384615384615384,0.0476086899858127),.UNSPECIFIED.)
GEOMETRIC_REPRESENTATION_ITEM()
RATIONAL_B_SPLINE_SURFACE(((0.998993602249807,0.999456249886298,1.,0.998265981131401,
0.997356751596327),(0.998993602249807,0.999456249886298,1.,0.998265981131401,
0.997356751596327),(0.998993602249807,0.999456249886298,1.,0.998265981131401,
0.997356751596327)))
REPRESENTATION_ITEM('')
SURFACE()
);
#247=(
BOUNDED_SURFACE()
B_SPLINE_SURFACE(1,2,((#73221,#73222,#73223,#73224,#73225),(#73226,#73227,
#73228,#73229,#73230),(#73231,#73232,#73233,#73234,#73235)),
 .UNSPECIFIED.,.F.,.F.,.F.)
B_SPLINE_SURFACE_WITH_KNOTS((2,1,2),(3,2,3),(-0.00141401191198094,0.,0.480770297079957),
(0.0365944846645789,0.0384615384615384,0.0431859280915187),
 .UNSPECIFIED.)
GEOMETRIC_REPRESENTATION_ITEM()
RATIONAL_B_SPLINE_SURFACE(((0.99932649045226,0.999646063968218,1.,0.999104400890347,
0.9984288220563),(0.99932649045226,0.999646063968218,1.,0.999104400890347,
0.9984288220563),(0.99932649045226,0.999646063968218,1.,0.999104400890347,
0.9984288220563)))
REPRESENTATION_ITEM('')
SURFACE()
);
#248=(
BOUNDED_SURFACE()
B_SPLINE_SURFACE(1,2,((#73262,#73263,#73264),(#73265,#73266,#73267),(#73268,
#73269,#73270)),.UNSPECIFIED.,.F.,.F.,.F.)
B_SPLINE_SURFACE_WITH_KNOTS((2,1,2),(3,3),(0.,1.,1.01),(0.0255903596131778,
0.0375948596693862),.UNSPECIFIED.)
GEOMETRIC_REPRESENTATION_ITEM()
RATIONAL_B_SPLINE_SURFACE(((0.996753121755999,0.997505687613147,0.999678813023853),
(0.996753121755999,0.997505687613147,0.999678813023853),(0.996753121755999,
0.997505687613147,0.999678813023853)))
REPRESENTATION_ITEM('')
SURFACE()
);
#249=(
BOUNDED_SURFACE()
B_SPLINE_SURFACE(1,2,((#73305,#73306,#73307),(#73308,#73309,#73310),(#73311,
#73312,#73313)),.UNSPECIFIED.,.F.,.F.,.F.)
B_SPLINE_SURFACE_WITH_KNOTS((2,1,2),(3,3),(-0.00286823045909901,0.,0.477902879786441),
(0.0265907346180619,0.0331702036774536),.UNSPECIFIED.)
GEOMETRIC_REPRESENTATION_ITEM()
RATIONAL_B_SPLINE_SURFACE(((0.996888414395785,0.997365765476469,0.998269846371839),
(0.996888414395785,0.997365765476469,0.998269846371839),(0.996888414395785,
0.997365765476469,0.998269846371839)))
REPRESENTATION_ITEM('')
SURFACE()
);
#250=(
BOUNDED_SURFACE()
B_SPLINE_SURFACE(1,2,((#73380,#73381,#73382),(#73383,#73384,#73385),(#73386,
#73387,#73388)),.UNSPECIFIED.,.F.,.F.,.F.)
B_SPLINE_SURFACE_WITH_KNOTS((2,1,2),(3,3),(-0.00286753128207195,0.,0.477902879786496),
(0.0166015299238956,0.0231736788111879),.UNSPECIFIED.)
GEOMETRIC_REPRESENTATION_ITEM()
RATIONAL_B_SPLINE_SURFACE(((0.996422581660832,0.996252244737341,0.996507688616404),
(0.996422581660832,0.996252244737341,0.996507688616404),(0.996422581660832,
0.996252244737341,0.996507688616404)))
REPRESENTATION_ITEM('')
SURFACE()
);
#251=(
BOUNDED_SURFACE()
B_SPLINE_SURFACE(1,2,((#73405,#73406,#73407),(#73408,#73409,#73410),(#73411,
#73412,#73413),(#73414,#73415,#73416)),.UNSPECIFIED.,.F.,.F.,.F.)
B_SPLINE_SURFACE_WITH_KNOTS((2,1,1,2),(3,3),(-0.0101,0.,1.,1.01),(0.00560769168370627,
0.0176009700440521),.UNSPECIFIED.)
GEOMETRIC_REPRESENTATION_ITEM()
RATIONAL_B_SPLINE_SURFACE(((0.99818389211382,0.99657330421516,0.996380621259469),
(0.99818389211382,0.99657330421516,0.996380621259469),(0.99818389211382,
0.99657330421516,0.996380621259469),(0.99818389211382,0.99657330421516,
0.996380621259469)))
REPRESENTATION_ITEM('')
SURFACE()
);
#252=(
BOUNDED_SURFACE()
B_SPLINE_SURFACE(1,2,((#73451,#73452,#73453),(#73454,#73455,#73456),(#73457,
#73458,#73459)),.UNSPECIFIED.,.F.,.F.,.F.)
B_SPLINE_SURFACE_WITH_KNOTS((2,1,2),(3,3),(-0.0020690189250989,0.,0.346769728493813),
(0.00660713154720725,0.0131849431292534),.UNSPECIFIED.)
GEOMETRIC_REPRESENTATION_ITEM()
RATIONAL_B_SPLINE_SURFACE(((0.997925307359446,0.997106772387136,0.996714752255963),
(0.997925307359446,0.997106772387136,0.996714752255963),(0.997925307359446,
0.997106772387136,0.996714752255963)))
REPRESENTATION_ITEM('')
SURFACE()
);
#253=(
BOUNDED_SURFACE()
B_SPLINE_SURFACE(1,2,((#73532,#73533,#73534),(#73535,#73536,#73537)),
 .UNSPECIFIED.,.F.,.F.,.F.)
B_SPLINE_SURFACE_WITH_KNOTS((2,2),(3,3),(0.,1.),(0.0556006976418393,0.0675888856590512),
 .UNSPECIFIED.)
GEOMETRIC_REPRESENTATION_ITEM()
RATIONAL_B_SPLINE_SURFACE(((0.996397562408606,0.996150386832629,0.997319912843745),
(0.996397562408606,0.996150386832629,0.997319912843745)))
REPRESENTATION_ITEM('')
SURFACE()
);
#254=(
BOUNDED_SURFACE()
B_SPLINE_SURFACE(1,2,((#73606,#73607,#73608),(#73609,#73610,#73611),(#73612,
#73613,#73614)),.UNSPECIFIED.,.F.,.F.,.F.)
B_SPLINE_SURFACE_WITH_KNOTS((2,1,2),(3,3),(0.,1.,1.01),(0.0456081671210001,
0.0575989447818822),.UNSPECIFIED.)
GEOMETRIC_REPRESENTATION_ITEM()
RATIONAL_B_SPLINE_SURFACE(((0.997793907739637,0.996365558499688,0.996354522974128),
(0.997793907739637,0.996365558499688,0.996354522974128),(0.997793907739637,
0.996365558499688,0.996354522974128)))
REPRESENTATION_ITEM('')
SURFACE()
);
#255=(
BOUNDED_SURFACE()
B_SPLINE_SURFACE(1,2,((#73649,#73650,#73651),(#73652,#73653,#73654),(#73655,
#73656,#73657)),.UNSPECIFIED.,.F.,.F.,.F.)
B_SPLINE_SURFACE_WITH_KNOTS((2,1,2),(3,3),(-0.0028681017350075,0.,0.47790287978652),
(0.0466073985929105,0.0531834929157979),.UNSPECIFIED.)
GEOMETRIC_REPRESENTATION_ITEM()
RATIONAL_B_SPLINE_SURFACE(((0.997565691989291,0.996847118055594,0.996554836292953),
(0.997565691989291,0.996847118055594,0.996554836292953),(0.997565691989291,
0.996847118055594,0.996554836292953)))
REPRESENTATION_ITEM('')
SURFACE()
);
#256=(
BOUNDED_SURFACE()
B_SPLINE_SURFACE(1,2,((#73674,#73675,#73676,#73677,#73678),(#73679,#73680,
#73681,#73682,#73683),(#73684,#73685,#73686,#73687,#73688)),
 .UNSPECIFIED.,.F.,.F.,.F.)
B_SPLINE_SURFACE_WITH_KNOTS((2,1,2),(3,2,3),(0.,1.,1.01),(0.0355931932713903,
0.0384615384615384,0.0476086899858126),.UNSPECIFIED.)
GEOMETRIC_REPRESENTATION_ITEM()
RATIONAL_B_SPLINE_SURFACE(((0.998993602249807,0.999456249886298,1.,0.998265981131401,
0.997356751596327),(0.998993602249807,0.999456249886298,1.,0.998265981131401,
0.997356751596327),(0.998993602249807,0.999456249886298,1.,0.998265981131401,
0.997356751596327)))
REPRESENTATION_ITEM('')
SURFACE()
);
#257=(
BOUNDED_SURFACE()
B_SPLINE_SURFACE(1,2,((#73736,#73737,#73738,#73739,#73740),(#73741,#73742,
#73743,#73744,#73745),(#73746,#73747,#73748,#73749,#73750)),
 .UNSPECIFIED.,.F.,.F.,.F.)
B_SPLINE_SURFACE_WITH_KNOTS((2,1,2),(3,2,3),(-0.00286743098086898,0.,0.480770297146936),
(0.0365944846643956,0.0384615384615384,0.0431859280915195),
 .UNSPECIFIED.)
GEOMETRIC_REPRESENTATION_ITEM()
RATIONAL_B_SPLINE_SURFACE(((0.999326490452197,0.999646063968182,1.,0.999104400890347,
0.9984288220563),(0.999326490452197,0.999646063968182,1.,0.999104400890347,
0.9984288220563),(0.999326490452197,0.999646063968182,1.,0.999104400890347,
0.9984288220563)))
REPRESENTATION_ITEM('')
SURFACE()
);
#258=(
BOUNDED_SURFACE()
B_SPLINE_SURFACE(1,2,((#73777,#73778,#73779),(#73780,#73781,#73782),(#73783,
#73784,#73785)),.UNSPECIFIED.,.F.,.F.,.F.)
B_SPLINE_SURFACE_WITH_KNOTS((2,1,2),(3,3),(0.,1.,1.01),(0.0255903596131777,
0.0375948596693867),.UNSPECIFIED.)
GEOMETRIC_REPRESENTATION_ITEM()
RATIONAL_B_SPLINE_SURFACE(((0.996753121755999,0.997505687613147,0.999678813023853),
(0.996753121755999,0.997505687613147,0.999678813023853),(0.996753121755999,
0.997505687613147,0.999678813023853)))
REPRESENTATION_ITEM('')
SURFACE()
);
#259=(
BOUNDED_SURFACE()
B_SPLINE_SURFACE(1,2,((#73820,#73821,#73822),(#73823,#73824,#73825),(#73826,
#73827,#73828)),.UNSPECIFIED.,.F.,.F.,.F.)
B_SPLINE_SURFACE_WITH_KNOTS((2,1,2),(3,3),(-0.00286823356216264,0.,0.477902879786493),
(0.0265907346180615,0.0331702037252919),.UNSPECIFIED.)
GEOMETRIC_REPRESENTATION_ITEM()
RATIONAL_B_SPLINE_SURFACE(((0.996888414395785,0.997365765479939,0.998269846384985),
(0.996888414395785,0.997365765479939,0.998269846384985),(0.996888414395785,
0.997365765479939,0.998269846384985)))
REPRESENTATION_ITEM('')
SURFACE()
);
#260=(
BOUNDED_SURFACE()
B_SPLINE_SURFACE(1,2,((#73895,#73896,#73897),(#73898,#73899,#73900),(#73901,
#73902,#73903)),.UNSPECIFIED.,.F.,.F.,.F.)
B_SPLINE_SURFACE_WITH_KNOTS((2,1,2),(3,3),(-0.00286753128208516,0.,0.47790287978643),
(0.0166015299238966,0.0231736788111885),.UNSPECIFIED.)
GEOMETRIC_REPRESENTATION_ITEM()
RATIONAL_B_SPLINE_SURFACE(((0.996422581660833,0.996252244737341,0.996507688616404),
(0.996422581660833,0.996252244737341,0.996507688616404),(0.996422581660833,
0.996252244737341,0.996507688616404)))
REPRESENTATION_ITEM('')
SURFACE()
);
#261=(
BOUNDED_SURFACE()
B_SPLINE_SURFACE(1,2,((#73920,#73921,#73922),(#73923,#73924,#73925),(#73926,
#73927,#73928),(#73929,#73930,#73931)),.UNSPECIFIED.,.F.,.F.,.F.)
B_SPLINE_SURFACE_WITH_KNOTS((2,1,1,2),(3,3),(-0.0101,0.,1.,1.01),(0.00560769168370496,
0.0176009700440518),.UNSPECIFIED.)
GEOMETRIC_REPRESENTATION_ITEM()
RATIONAL_B_SPLINE_SURFACE(((0.998183892113821,0.99657330421516,0.996380621259469),
(0.998183892113821,0.99657330421516,0.996380621259469),(0.998183892113821,
0.99657330421516,0.996380621259469),(0.998183892113821,0.99657330421516,
0.996380621259469)))
REPRESENTATION_ITEM('')
SURFACE()
);
#262=(
BOUNDED_SURFACE()
B_SPLINE_SURFACE(1,2,((#73966,#73967,#73968),(#73969,#73970,#73971),(#73972,
#73973,#73974)),.UNSPECIFIED.,.F.,.F.,.F.)
B_SPLINE_SURFACE_WITH_KNOTS((2,1,2),(3,3),(-0.00206901892662539,0.,0.346769728493036),
(0.00660713154720504,0.013184943146903),.UNSPECIFIED.)
GEOMETRIC_REPRESENTATION_ITEM()
RATIONAL_B_SPLINE_SURFACE(((0.997925307359447,0.99710677238494,0.996714752253859),
(0.997925307359447,0.99710677238494,0.996714752253859),(0.997925307359447,
0.99710677238494,0.996714752253859)))
REPRESENTATION_ITEM('')
SURFACE()
);
#263=(
BOUNDED_SURFACE()
B_SPLINE_SURFACE(1,2,((#74047,#74048,#74049),(#74050,#74051,#74052)),
 .UNSPECIFIED.,.F.,.F.,.F.)
B_SPLINE_SURFACE_WITH_KNOTS((2,2),(3,3),(0.,1.),(0.0556006976418428,0.0675888856590492),
 .UNSPECIFIED.)
GEOMETRIC_REPRESENTATION_ITEM()
RATIONAL_B_SPLINE_SURFACE(((0.996397562408606,0.996150386832629,0.997319912843745),
(0.996397562408606,0.996150386832629,0.997319912843745)))
REPRESENTATION_ITEM('')
SURFACE()
);
#264=(
BOUNDED_SURFACE()
B_SPLINE_SURFACE(1,2,((#74121,#74122,#74123),(#74124,#74125,#74126),(#74127,
#74128,#74129)),.UNSPECIFIED.,.F.,.F.,.F.)
B_SPLINE_SURFACE_WITH_KNOTS((2,1,2),(3,3),(0.,1.,1.01),(0.0456081671210057,
0.0575989447818801),.UNSPECIFIED.)
GEOMETRIC_REPRESENTATION_ITEM()
RATIONAL_B_SPLINE_SURFACE(((0.997793907739636,0.996365558499688,0.996354522974128),
(0.997793907739636,0.996365558499688,0.996354522974128),(0.997793907739636,
0.996365558499688,0.996354522974128)))
REPRESENTATION_ITEM('')
SURFACE()
);
#265=(
BOUNDED_SURFACE()
B_SPLINE_SURFACE(1,2,((#74164,#74165,#74166),(#74167,#74168,#74169),(#74170,
#74171,#74172)),.UNSPECIFIED.,.F.,.F.,.F.)
B_SPLINE_SURFACE_WITH_KNOTS((2,1,2),(3,3),(-0.00286810173496387,0.,0.477902879786524),
(0.0466073985929113,0.0531834929157973),.UNSPECIFIED.)
GEOMETRIC_REPRESENTATION_ITEM()
RATIONAL_B_SPLINE_SURFACE(((0.997565691989291,0.996847118055594,0.996554836292953),
(0.997565691989291,0.996847118055594,0.996554836292953),(0.997565691989291,
0.996847118055594,0.996554836292953)))
REPRESENTATION_ITEM('')
SURFACE()
);
#266=(
BOUNDED_SURFACE()
B_SPLINE_SURFACE(1,2,((#74189,#74190,#74191,#74192,#74193),(#74194,#74195,
#74196,#74197,#74198),(#74199,#74200,#74201,#74202,#74203)),
 .UNSPECIFIED.,.F.,.F.,.F.)
B_SPLINE_SURFACE_WITH_KNOTS((2,1,2),(3,2,3),(0.,1.,1.01),(0.0355931932713904,
0.0384615384615384,0.047608689985811),.UNSPECIFIED.)
GEOMETRIC_REPRESENTATION_ITEM()
RATIONAL_B_SPLINE_SURFACE(((0.998993602249807,0.999456249886298,1.,0.998265981131401,
0.997356751596327),(0.998993602249807,0.999456249886298,1.,0.998265981131401,
0.997356751596327),(0.998993602249807,0.999456249886298,1.,0.998265981131401,
0.997356751596327)))
REPRESENTATION_ITEM('')
SURFACE()
);
#267=(
BOUNDED_SURFACE()
B_SPLINE_SURFACE(1,2,((#74251,#74252,#74253,#74254,#74255),(#74256,#74257,
#74258,#74259,#74260),(#74261,#74262,#74263,#74264,#74265)),
 .UNSPECIFIED.,.F.,.F.,.F.)
B_SPLINE_SURFACE_WITH_KNOTS((2,1,2),(3,2,3),(-0.00141401191198245,0.,0.48077029708073),
(0.0365944846645754,0.0384615384615384,0.0431859280915184),
 .UNSPECIFIED.)
GEOMETRIC_REPRESENTATION_ITEM()
RATIONAL_B_SPLINE_SURFACE(((0.999326490452258,0.999646063968217,1.,0.999104400890347,
0.9984288220563),(0.999326490452258,0.999646063968217,1.,0.999104400890347,
0.9984288220563),(0.999326490452258,0.999646063968217,1.,0.999104400890347,
0.9984288220563)))
REPRESENTATION_ITEM('')
SURFACE()
);
#268=(
BOUNDED_SURFACE()
B_SPLINE_SURFACE(1,2,((#74292,#74293,#74294),(#74295,#74296,#74297),(#74298,
#74299,#74300)),.UNSPECIFIED.,.F.,.F.,.F.)
B_SPLINE_SURFACE_WITH_KNOTS((2,1,2),(3,3),(0.,1.,1.01),(0.025590359613179,
0.0375948596693855),.UNSPECIFIED.)
GEOMETRIC_REPRESENTATION_ITEM()
RATIONAL_B_SPLINE_SURFACE(((0.996753121755999,0.997505687613147,0.999678813023853),
(0.996753121755999,0.997505687613147,0.999678813023853),(0.996753121755999,
0.997505687613147,0.999678813023853)))
REPRESENTATION_ITEM('')
SURFACE()
);
#269=(
BOUNDED_SURFACE()
B_SPLINE_SURFACE(1,2,((#74335,#74336,#74337),(#74338,#74339,#74340),(#74341,
#74342,#74343)),.UNSPECIFIED.,.F.,.F.,.F.)
B_SPLINE_SURFACE_WITH_KNOTS((2,1,2),(3,3),(-0.00286823356219737,0.,0.477902879786498),
(0.0265907346180618,0.0331702037252923),.UNSPECIFIED.)
GEOMETRIC_REPRESENTATION_ITEM()
RATIONAL_B_SPLINE_SURFACE(((0.996888414395785,0.997365765479939,0.998269846384985),
(0.996888414395785,0.997365765479939,0.998269846384985),(0.996888414395785,
0.997365765479939,0.998269846384985)))
REPRESENTATION_ITEM('')
SURFACE()
);
#270=(
BOUNDED_SURFACE()
B_SPLINE_SURFACE(1,2,((#74410,#74411,#74412),(#74413,#74414,#74415),(#74416,
#74417,#74418)),.UNSPECIFIED.,.F.,.F.,.F.)
B_SPLINE_SURFACE_WITH_KNOTS((2,1,2),(3,3),(-0.00286753128207131,0.,0.477902879786491),
(0.0166015299238959,0.0231736788111888),.UNSPECIFIED.)
GEOMETRIC_REPRESENTATION_ITEM()
RATIONAL_B_SPLINE_SURFACE(((0.996422581660833,0.996252244737342,0.996507688616404),
(0.996422581660833,0.996252244737342,0.996507688616404),(0.996422581660833,
0.996252244737342,0.996507688616404)))
REPRESENTATION_ITEM('')
SURFACE()
);
#271=(
BOUNDED_SURFACE()
B_SPLINE_SURFACE(1,2,((#74435,#74436,#74437),(#74438,#74439,#74440),(#74441,
#74442,#74443),(#74444,#74445,#74446)),.UNSPECIFIED.,.F.,.F.,.F.)
B_SPLINE_SURFACE_WITH_KNOTS((2,1,1,2),(3,3),(-0.0101,0.,1.,1.01),(0.00560769168370524,
0.0176009700440501),.UNSPECIFIED.)
GEOMETRIC_REPRESENTATION_ITEM()
RATIONAL_B_SPLINE_SURFACE(((0.998183892113821,0.99657330421516,0.996380621259469),
(0.998183892113821,0.99657330421516,0.996380621259469),(0.998183892113821,
0.99657330421516,0.996380621259469),(0.998183892113821,0.99657330421516,
0.996380621259469)))
REPRESENTATION_ITEM('')
SURFACE()
);
#272=(
BOUNDED_SURFACE()
B_SPLINE_SURFACE(1,2,((#74481,#74482,#74483),(#74484,#74485,#74486),(#74487,
#74488,#74489)),.UNSPECIFIED.,.F.,.F.,.F.)
B_SPLINE_SURFACE_WITH_KNOTS((2,1,2),(3,3),(-0.00206901892656846,0.,0.346769728493026),
(0.00660713154720006,0.0131849431469154),.UNSPECIFIED.)
GEOMETRIC_REPRESENTATION_ITEM()
RATIONAL_B_SPLINE_SURFACE(((0.997925307359448,0.997106772384939,0.996714752253857),
(0.997925307359448,0.997106772384939,0.996714752253857),(0.997925307359448,
0.997106772384939,0.996714752253857)))
REPRESENTATION_ITEM('')
SURFACE()
);
#273=(
BOUNDED_SURFACE()
B_SPLINE_SURFACE(1,2,((#74562,#74563,#74564),(#74565,#74566,#74567)),
 .UNSPECIFIED.,.F.,.F.,.F.)
B_SPLINE_SURFACE_WITH_KNOTS((2,2),(3,3),(0.,1.),(0.0556006976418415,0.0675888856590505),
 .UNSPECIFIED.)
GEOMETRIC_REPRESENTATION_ITEM()
RATIONAL_B_SPLINE_SURFACE(((0.996397562408606,0.996150386832629,0.997319912843745),
(0.996397562408606,0.996150386832629,0.997319912843745)))
REPRESENTATION_ITEM('')
SURFACE()
);
#274=(
BOUNDED_SURFACE()
B_SPLINE_SURFACE(1,2,((#74636,#74637,#74638),(#74639,#74640,#74641),(#74642,
#74643,#74644)),.UNSPECIFIED.,.F.,.F.,.F.)
B_SPLINE_SURFACE_WITH_KNOTS((2,1,2),(3,3),(0.,1.,1.01),(0.0456081671210066,
0.0575989447818817),.UNSPECIFIED.)
GEOMETRIC_REPRESENTATION_ITEM()
RATIONAL_B_SPLINE_SURFACE(((0.997793907739636,0.996365558499688,0.996354522974128),
(0.997793907739636,0.996365558499688,0.996354522974128),(0.997793907739636,
0.996365558499688,0.996354522974128)))
REPRESENTATION_ITEM('')
SURFACE()
);
#275=(
BOUNDED_SURFACE()
B_SPLINE_SURFACE(1,2,((#74679,#74680,#74681),(#74682,#74683,#74684),(#74685,
#74686,#74687)),.UNSPECIFIED.,.F.,.F.,.F.)
B_SPLINE_SURFACE_WITH_KNOTS((2,1,2),(3,3),(-0.00286810173489828,0.,0.477902879786517),
(0.0466073985929122,0.0531834929157977),.UNSPECIFIED.)
GEOMETRIC_REPRESENTATION_ITEM()
RATIONAL_B_SPLINE_SURFACE(((0.997565691989291,0.996847118055593,0.996554836292953),
(0.997565691989291,0.996847118055593,0.996554836292953),(0.997565691989291,
0.996847118055593,0.996554836292953)))
REPRESENTATION_ITEM('')
SURFACE()
);
#276=(
BOUNDED_SURFACE()
B_SPLINE_SURFACE(1,2,((#74704,#74705,#74706,#74707,#74708),(#74709,#74710,
#74711,#74712,#74713),(#74714,#74715,#74716,#74717,#74718)),
 .UNSPECIFIED.,.F.,.F.,.F.)
B_SPLINE_SURFACE_WITH_KNOTS((2,1,2),(3,2,3),(0.,1.,1.01),(0.0355931932713902,
0.0384615384615384,0.0476086899858138),.UNSPECIFIED.)
GEOMETRIC_REPRESENTATION_ITEM()
RATIONAL_B_SPLINE_SURFACE(((0.998993602249807,0.999456249886298,1.,0.998265981131401,
0.997356751596327),(0.998993602249807,0.999456249886298,1.,0.998265981131401,
0.997356751596327),(0.998993602249807,0.999456249886298,1.,0.998265981131401,
0.997356751596327)))
REPRESENTATION_ITEM('')
SURFACE()
);
#277=(
BOUNDED_SURFACE()
B_SPLINE_SURFACE(1,2,((#74766,#74767,#74768,#74769,#74770),(#74771,#74772,
#74773,#74774,#74775),(#74776,#74777,#74778,#74779,#74780)),
 .UNSPECIFIED.,.F.,.F.,.F.)
B_SPLINE_SURFACE_WITH_KNOTS((2,1,2),(3,2,3),(-0.00141401191198367,0.,0.480770297080774),
(0.0365944846645756,0.0384615384615384,0.0431859280915187),
 .UNSPECIFIED.)
GEOMETRIC_REPRESENTATION_ITEM()
RATIONAL_B_SPLINE_SURFACE(((0.999326490452259,0.999646063968217,1.,0.999104400890347,
0.9984288220563),(0.999326490452258,0.999646063968217,1.,0.999104400890347,
0.9984288220563),(0.999326490452258,0.999646063968217,1.,0.999104400890347,
0.9984288220563)))
REPRESENTATION_ITEM('')
SURFACE()
);
#278=(
BOUNDED_SURFACE()
B_SPLINE_SURFACE(1,2,((#74807,#74808,#74809),(#74810,#74811,#74812),(#74813,
#74814,#74815)),.UNSPECIFIED.,.F.,.F.,.F.)
B_SPLINE_SURFACE_WITH_KNOTS((2,1,2),(3,3),(0.,1.,1.01),(0.0255903596131811,
0.0375948596693875),.UNSPECIFIED.)
GEOMETRIC_REPRESENTATION_ITEM()
RATIONAL_B_SPLINE_SURFACE(((0.996753121755999,0.997505687613148,0.999678813023853),
(0.996753121755999,0.997505687613148,0.999678813023853),(0.996753121755999,
0.997505687613148,0.999678813023853)))
REPRESENTATION_ITEM('')
SURFACE()
);
#279=(
BOUNDED_SURFACE()
B_SPLINE_SURFACE(1,2,((#74850,#74851,#74852),(#74853,#74854,#74855),(#74856,
#74857,#74858)),.UNSPECIFIED.,.F.,.F.,.F.)
B_SPLINE_SURFACE_WITH_KNOTS((2,1,2),(3,3),(-0.00286823356220283,0.,0.477902879786487),
(0.0265907346180614,0.0331702037252926),.UNSPECIFIED.)
GEOMETRIC_REPRESENTATION_ITEM()
RATIONAL_B_SPLINE_SURFACE(((0.996888414395785,0.997365765479939,0.998269846384985),
(0.996888414395785,0.997365765479939,0.998269846384985),(0.996888414395785,
0.997365765479939,0.998269846384985)))
REPRESENTATION_ITEM('')
SURFACE()
);
#280=(
BOUNDED_SURFACE()
B_SPLINE_SURFACE(1,2,((#74925,#74926,#74927),(#74928,#74929,#74930),(#74931,
#74932,#74933)),.UNSPECIFIED.,.F.,.F.,.F.)
B_SPLINE_SURFACE_WITH_KNOTS((2,1,2),(3,3),(-0.00286753128207528,0.,0.477902879786539),
(0.0166015299238958,0.0231736788111881),.UNSPECIFIED.)
GEOMETRIC_REPRESENTATION_ITEM()
RATIONAL_B_SPLINE_SURFACE(((0.996422581660833,0.996252244737342,0.996507688616404),
(0.996422581660833,0.996252244737342,0.996507688616404),(0.996422581660833,
0.996252244737342,0.996507688616404)))
REPRESENTATION_ITEM('')
SURFACE()
);
#281=(
BOUNDED_SURFACE()
B_SPLINE_SURFACE(1,2,((#74950,#74951,#74952),(#74953,#74954,#74955),(#74956,
#74957,#74958),(#74959,#74960,#74961)),.UNSPECIFIED.,.F.,.F.,.F.)
B_SPLINE_SURFACE_WITH_KNOTS((2,1,1,2),(3,3),(-0.0101,0.,1.,1.01),(0.00560769168370515,
0.0176009700440511),.UNSPECIFIED.)
GEOMETRIC_REPRESENTATION_ITEM()
RATIONAL_B_SPLINE_SURFACE(((0.998183892113821,0.99657330421516,0.996380621259469),
(0.998183892113821,0.99657330421516,0.996380621259469),(0.998183892113821,
0.99657330421516,0.996380621259469),(0.998183892113821,0.99657330421516,
0.996380621259469)))
REPRESENTATION_ITEM('')
SURFACE()
);
#282=(
BOUNDED_SURFACE()
B_SPLINE_SURFACE(1,2,((#74996,#74997,#74998),(#74999,#75000,#75001),(#75002,
#75003,#75004)),.UNSPECIFIED.,.F.,.F.,.F.)
B_SPLINE_SURFACE_WITH_KNOTS((2,1,2),(3,3),(-0.00206901892653575,0.,0.346769728493005),
(0.00660713154719305,0.0131849431468706),.UNSPECIFIED.)
GEOMETRIC_REPRESENTATION_ITEM()
RATIONAL_B_SPLINE_SURFACE(((0.99792530735945,0.997106772384944,0.996714752253862),
(0.99792530735945,0.997106772384944,0.996714752253862),(0.99792530735945,
0.997106772384944,0.996714752253862)))
REPRESENTATION_ITEM('')
SURFACE()
);
#283=(
BOUNDED_SURFACE()
B_SPLINE_SURFACE(1,2,((#75077,#75078,#75079),(#75080,#75081,#75082)),
 .UNSPECIFIED.,.F.,.F.,.F.)
B_SPLINE_SURFACE_WITH_KNOTS((2,2),(3,3),(0.,1.),(0.0556006976418437,0.0675888856590508),
 .UNSPECIFIED.)
GEOMETRIC_REPRESENTATION_ITEM()
RATIONAL_B_SPLINE_SURFACE(((0.996397562408606,0.996150386832629,0.997319912843745),
(0.996397562408606,0.996150386832629,0.997319912843745)))
REPRESENTATION_ITEM('')
SURFACE()
);
#284=(
BOUNDED_SURFACE()
B_SPLINE_SURFACE(1,2,((#75151,#75152,#75153),(#75154,#75155,#75156),(#75157,
#75158,#75159)),.UNSPECIFIED.,.F.,.F.,.F.)
B_SPLINE_SURFACE_WITH_KNOTS((2,1,2),(3,3),(0.,1.,1.01),(0.0456081671210055,
0.0575989447818818),.UNSPECIFIED.)
GEOMETRIC_REPRESENTATION_ITEM()
RATIONAL_B_SPLINE_SURFACE(((0.997793907739636,0.996365558499688,0.996354522974128),
(0.997793907739636,0.996365558499688,0.996354522974128),(0.997793907739636,
0.996365558499688,0.996354522974128)))
REPRESENTATION_ITEM('')
SURFACE()
);
#285=(
BOUNDED_SURFACE()
B_SPLINE_SURFACE(1,2,((#75194,#75195,#75196),(#75197,#75198,#75199),(#75200,
#75201,#75202)),.UNSPECIFIED.,.F.,.F.,.F.)
B_SPLINE_SURFACE_WITH_KNOTS((2,1,2),(3,3),(-0.00286810173486603,0.,0.477902879786523),
(0.0466073985929115,0.0531834929157976),.UNSPECIFIED.)
GEOMETRIC_REPRESENTATION_ITEM()
RATIONAL_B_SPLINE_SURFACE(((0.997565691989291,0.996847118055594,0.996554836292953),
(0.997565691989291,0.996847118055594,0.996554836292953),(0.997565691989291,
0.996847118055594,0.996554836292953)))
REPRESENTATION_ITEM('')
SURFACE()
);
#286=(
BOUNDED_SURFACE()
B_SPLINE_SURFACE(1,2,((#75219,#75220,#75221,#75222,#75223),(#75224,#75225,
#75226,#75227,#75228),(#75229,#75230,#75231,#75232,#75233)),
 .UNSPECIFIED.,.F.,.F.,.F.)
B_SPLINE_SURFACE_WITH_KNOTS((2,1,2),(3,2,3),(0.,1.,1.01),(0.0355931932713902,
0.0384615384615384,0.0476086899858144),.UNSPECIFIED.)
GEOMETRIC_REPRESENTATION_ITEM()
RATIONAL_B_SPLINE_SURFACE(((0.998993602249807,0.999456249886298,1.,0.998265981131401,
0.997356751596327),(0.998993602249807,0.999456249886298,1.,0.998265981131401,
0.997356751596327),(0.998993602249807,0.999456249886298,1.,0.998265981131401,
0.997356751596327)))
REPRESENTATION_ITEM('')
SURFACE()
);
#287=(
BOUNDED_SURFACE()
B_SPLINE_SURFACE(1,2,((#75281,#75282,#75283,#75284,#75285),(#75286,#75287,
#75288,#75289,#75290),(#75291,#75292,#75293,#75294,#75295)),
 .UNSPECIFIED.,.F.,.F.,.F.)
B_SPLINE_SURFACE_WITH_KNOTS((2,1,2),(3,2,3),(-0.00286743098587475,0.,0.480770297146967),
(0.0365944846643704,0.0384615384615384,0.0431859280915192),
 .UNSPECIFIED.)
GEOMETRIC_REPRESENTATION_ITEM()
RATIONAL_B_SPLINE_SURFACE(((0.999326490452188,0.999646063968178,1.,0.999104400890346,
0.9984288220563),(0.999326490452188,0.999646063968178,1.,0.999104400890347,
0.9984288220563),(0.999326490452188,0.999646063968178,1.,0.999104400890347,
0.9984288220563)))
REPRESENTATION_ITEM('')
SURFACE()
);
#288=(
BOUNDED_SURFACE()
B_SPLINE_SURFACE(1,2,((#75322,#75323,#75324),(#75325,#75326,#75327),(#75328,
#75329,#75330)),.UNSPECIFIED.,.F.,.F.,.F.)
B_SPLINE_SURFACE_WITH_KNOTS((2,1,2),(3,3),(0.,1.,1.01),(0.025590359613181,
0.0375948596693885),.UNSPECIFIED.)
GEOMETRIC_REPRESENTATION_ITEM()
RATIONAL_B_SPLINE_SURFACE(((0.996753121755999,0.997505687613148,0.999678813023854),
(0.996753121755999,0.997505687613148,0.999678813023854),(0.996753121755999,
0.997505687613148,0.999678813023854)))
REPRESENTATION_ITEM('')
SURFACE()
);
#289=(
BOUNDED_SURFACE()
B_SPLINE_SURFACE(1,2,((#75365,#75366,#75367),(#75368,#75369,#75370),(#75371,
#75372,#75373)),.UNSPECIFIED.,.F.,.F.,.F.)
B_SPLINE_SURFACE_WITH_KNOTS((2,1,2),(3,3),(-0.00286823356216702,0.,0.477902879786504),
(0.0265907346180616,0.0331702037252923),.UNSPECIFIED.)
GEOMETRIC_REPRESENTATION_ITEM()
RATIONAL_B_SPLINE_SURFACE(((0.996888414395785,0.997365765479939,0.998269846384985),
(0.996888414395785,0.997365765479939,0.998269846384985),(0.996888414395785,
0.997365765479939,0.998269846384985)))
REPRESENTATION_ITEM('')
SURFACE()
);
#290=(
BOUNDED_SURFACE()
B_SPLINE_SURFACE(1,2,((#75440,#75441,#75442),(#75443,#75444,#75445),(#75446,
#75447,#75448)),.UNSPECIFIED.,.F.,.F.,.F.)
B_SPLINE_SURFACE_WITH_KNOTS((2,1,2),(3,3),(-0.00286753128206841,0.,0.477902879786505),
(0.0166015299238955,0.0231736788111888),.UNSPECIFIED.)
GEOMETRIC_REPRESENTATION_ITEM()
RATIONAL_B_SPLINE_SURFACE(((0.996422581660833,0.996252244737341,0.996507688616404),
(0.996422581660833,0.996252244737341,0.996507688616404),(0.996422581660833,
0.996252244737341,0.996507688616404)))
REPRESENTATION_ITEM('')
SURFACE()
);
#291=(
BOUNDED_SURFACE()
B_SPLINE_SURFACE(1,2,((#75465,#75466,#75467),(#75468,#75469,#75470),(#75471,
#75472,#75473),(#75474,#75475,#75476)),.UNSPECIFIED.,.F.,.F.,.F.)
B_SPLINE_SURFACE_WITH_KNOTS((2,1,1,2),(3,3),(-0.0101,0.,1.,1.01),(0.00560769168370622,
0.0176009700440522),.UNSPECIFIED.)
GEOMETRIC_REPRESENTATION_ITEM()
RATIONAL_B_SPLINE_SURFACE(((0.99818389211382,0.99657330421516,0.996380621259469),
(0.99818389211382,0.99657330421516,0.996380621259469),(0.99818389211382,
0.99657330421516,0.996380621259469),(0.99818389211382,0.99657330421516,
0.996380621259469)))
REPRESENTATION_ITEM('')
SURFACE()
);
#292=(
BOUNDED_SURFACE()
B_SPLINE_SURFACE(1,2,((#75511,#75512,#75513),(#75514,#75515,#75516),(#75517,
#75518,#75519)),.UNSPECIFIED.,.F.,.F.,.F.)
B_SPLINE_SURFACE_WITH_KNOTS((2,1,2),(3,3),(-0.00206901892646732,0.,0.346769728493036),
(0.00660713154718544,0.013184943146879),.UNSPECIFIED.)
GEOMETRIC_REPRESENTATION_ITEM()
RATIONAL_B_SPLINE_SURFACE(((0.997925307359452,0.997106772384944,0.996714752253861),
(0.997925307359452,0.997106772384944,0.996714752253861),(0.997925307359452,
0.997106772384944,0.996714752253861)))
REPRESENTATION_ITEM('')
SURFACE()
);
#293=(
BOUNDED_SURFACE()
B_SPLINE_SURFACE(1,2,((#75592,#75593,#75594),(#75595,#75596,#75597)),
 .UNSPECIFIED.,.F.,.F.,.F.)
B_SPLINE_SURFACE_WITH_KNOTS((2,2),(3,3),(0.,1.),(0.0556006976418415,0.0675888856590505),
 .UNSPECIFIED.)
GEOMETRIC_REPRESENTATION_ITEM()
RATIONAL_B_SPLINE_SURFACE(((0.996397562408606,0.996150386832629,0.997319912843745),
(0.996397562408606,0.996150386832629,0.997319912843745)))
REPRESENTATION_ITEM('')
SURFACE()
);
#294=(
BOUNDED_SURFACE()
B_SPLINE_SURFACE(1,2,((#75666,#75667,#75668),(#75669,#75670,#75671)),
 .UNSPECIFIED.,.F.,.F.,.F.)
B_SPLINE_SURFACE_WITH_KNOTS((2,2),(3,3),(0.,1.),(0.0456081671210054,0.0575989447818824),
 .UNSPECIFIED.)
GEOMETRIC_REPRESENTATION_ITEM()
RATIONAL_B_SPLINE_SURFACE(((0.997793907739636,0.996365558499688,0.996354522974128),
(0.997793907739636,0.996365558499688,0.996354522974128)))
REPRESENTATION_ITEM('')
SURFACE()
);
#295=(
BOUNDED_SURFACE()
B_SPLINE_SURFACE(1,2,((#75738,#75739,#75740,#75741,#75742),(#75743,#75744,
#75745,#75746,#75747),(#75748,#75749,#75750,#75751,#75752)),
 .UNSPECIFIED.,.F.,.F.,.F.)
B_SPLINE_SURFACE_WITH_KNOTS((2,1,2),(3,2,3),(0.,1.,1.01),(0.0355931932713902,
0.0384615384615384,0.0476086899858138),.UNSPECIFIED.)
GEOMETRIC_REPRESENTATION_ITEM()
RATIONAL_B_SPLINE_SURFACE(((0.998993602249807,0.999456249886298,1.,0.998265981131401,
0.997356751596327),(0.998993602249807,0.999456249886298,1.,0.998265981131401,
0.997356751596327),(0.998993602249807,0.999456249886298,1.,0.998265981131401,
0.997356751596327)))
REPRESENTATION_ITEM('')
SURFACE()
);
#296=(
BOUNDED_SURFACE()
B_SPLINE_SURFACE(1,2,((#75800,#75801,#75802,#75803,#75804),(#75805,#75806,
#75807,#75808,#75809),(#75810,#75811,#75812,#75813,#75814)),
 .UNSPECIFIED.,.F.,.F.,.F.)
B_SPLINE_SURFACE_WITH_KNOTS((2,1,2),(3,2,3),(-0.00141401191198346,0.,0.480770297080816),
(0.0365944846645752,0.0384615384615384,0.0431859280915184),
 .UNSPECIFIED.)
GEOMETRIC_REPRESENTATION_ITEM()
RATIONAL_B_SPLINE_SURFACE(((0.999326490452258,0.999646063968217,1.,0.999104400890347,
0.9984288220563),(0.999326490452258,0.999646063968217,1.,0.999104400890347,
0.9984288220563),(0.999326490452258,0.999646063968217,1.,0.999104400890347,
0.9984288220563)))
REPRESENTATION_ITEM('')
SURFACE()
);
#297=(
BOUNDED_SURFACE()
B_SPLINE_SURFACE(1,2,((#75841,#75842,#75843),(#75844,#75845,#75846),(#75847,
#75848,#75849)),.UNSPECIFIED.,.F.,.F.,.F.)
B_SPLINE_SURFACE_WITH_KNOTS((2,1,2),(3,3),(0.,1.,1.01),(0.025590359613181,
0.0375948596693879),.UNSPECIFIED.)
GEOMETRIC_REPRESENTATION_ITEM()
RATIONAL_B_SPLINE_SURFACE(((0.996753121755999,0.997505687613148,0.999678813023854),
(0.996753121755999,0.997505687613148,0.999678813023854),(0.996753121755999,
0.997505687613148,0.999678813023854)))
REPRESENTATION_ITEM('')
SURFACE()
);
#298=(
BOUNDED_SURFACE()
B_SPLINE_SURFACE(1,2,((#75884,#75885,#75886),(#75887,#75888,#75889),(#75890,
#75891,#75892)),.UNSPECIFIED.,.F.,.F.,.F.)
B_SPLINE_SURFACE_WITH_KNOTS((2,1,2),(3,3),(-0.00286823045904505,0.,0.477902879786501),
(0.0265907346180621,0.0331702036774533),.UNSPECIFIED.)
GEOMETRIC_REPRESENTATION_ITEM()
RATIONAL_B_SPLINE_SURFACE(((0.996888414395786,0.997365765476469,0.998269846371839),
(0.996888414395786,0.997365765476469,0.998269846371839),(0.996888414395786,
0.997365765476469,0.998269846371839)))
REPRESENTATION_ITEM('')
SURFACE()
);
#299=(
BOUNDED_SURFACE()
B_SPLINE_SURFACE(1,2,((#75959,#75960,#75961),(#75962,#75963,#75964),(#75965,
#75966,#75967)),.UNSPECIFIED.,.F.,.F.,.F.)
B_SPLINE_SURFACE_WITH_KNOTS((2,1,2),(3,3),(-0.00286753128206318,0.,0.477902879786521),
(0.0166015299238956,0.0231736788111887),.UNSPECIFIED.)
GEOMETRIC_REPRESENTATION_ITEM()
RATIONAL_B_SPLINE_SURFACE(((0.996422581660833,0.996252244737341,0.996507688616404),
(0.996422581660833,0.996252244737341,0.996507688616404),(0.996422581660833,
0.996252244737341,0.996507688616404)))
REPRESENTATION_ITEM('')
SURFACE()
);
#300=(
BOUNDED_SURFACE()
B_SPLINE_SURFACE(1,2,((#75984,#75985,#75986),(#75987,#75988,#75989),(#75990,
#75991,#75992),(#75993,#75994,#75995)),.UNSPECIFIED.,.F.,.F.,.F.)
B_SPLINE_SURFACE_WITH_KNOTS((2,1,1,2),(3,3),(-0.0101,0.,1.,1.01),(0.00560769168370531,
0.0176009700440517),.UNSPECIFIED.)
GEOMETRIC_REPRESENTATION_ITEM()
RATIONAL_B_SPLINE_SURFACE(((0.998183892113821,0.99657330421516,0.996380621259469),
(0.998183892113821,0.99657330421516,0.996380621259469),(0.998183892113821,
0.99657330421516,0.996380621259469),(0.998183892113821,0.99657330421516,
0.996380621259469)))
REPRESENTATION_ITEM('')
SURFACE()
);
#301=(
BOUNDED_SURFACE()
B_SPLINE_SURFACE(1,2,((#76030,#76031,#76032),(#76033,#76034,#76035),(#76036,
#76037,#76038)),.UNSPECIFIED.,.F.,.F.,.F.)
B_SPLINE_SURFACE_WITH_KNOTS((2,1,2),(3,3),(-0.00206901892640366,0.,0.346769728493003),
(0.00660713154717563,0.013184943146939),.UNSPECIFIED.)
GEOMETRIC_REPRESENTATION_ITEM()
RATIONAL_B_SPLINE_SURFACE(((0.997925307359454,0.997106772384937,0.996714752253855),
(0.997925307359454,0.997106772384937,0.996714752253855),(0.997925307359454,
0.997106772384937,0.996714752253854)))
REPRESENTATION_ITEM('')
SURFACE()
);
#302=(
BOUNDED_SURFACE()
B_SPLINE_SURFACE(1,2,((#76111,#76112,#76113),(#76114,#76115,#76116)),
 .UNSPECIFIED.,.F.,.F.,.F.)
B_SPLINE_SURFACE_WITH_KNOTS((2,2),(3,3),(0.,1.),(0.0556006976418414,0.0675888856590511),
 .UNSPECIFIED.)
GEOMETRIC_REPRESENTATION_ITEM()
RATIONAL_B_SPLINE_SURFACE(((0.996397562408606,0.996150386832629,0.997319912843745),
(0.996397562408606,0.996150386832629,0.997319912843745)))
REPRESENTATION_ITEM('')
SURFACE()
);
#303=(
BOUNDED_SURFACE()
B_SPLINE_SURFACE(1,2,((#76185,#76186,#76187),(#76188,#76189,#76190),(#76191,
#76192,#76193)),.UNSPECIFIED.,.F.,.F.,.F.)
B_SPLINE_SURFACE_WITH_KNOTS((2,1,2),(3,3),(0.,1.,1.01),(0.0456081671210045,
0.0575989447818814),.UNSPECIFIED.)
GEOMETRIC_REPRESENTATION_ITEM()
RATIONAL_B_SPLINE_SURFACE(((0.997793907739636,0.996365558499688,0.996354522974128),
(0.997793907739636,0.996365558499688,0.996354522974128),(0.997793907739636,
0.996365558499688,0.996354522974128)))
REPRESENTATION_ITEM('')
SURFACE()
);
#304=(
BOUNDED_SURFACE()
B_SPLINE_SURFACE(1,2,((#76228,#76229,#76230),(#76231,#76232,#76233),(#76234,
#76235,#76236)),.UNSPECIFIED.,.F.,.F.,.F.)
B_SPLINE_SURFACE_WITH_KNOTS((2,1,2),(3,3),(-0.00286810173474343,0.,0.477902879786529),
(0.0466073985929116,0.0531834929157972),.UNSPECIFIED.)
GEOMETRIC_REPRESENTATION_ITEM()
RATIONAL_B_SPLINE_SURFACE(((0.997565691989291,0.996847118055594,0.996554836292953),
(0.997565691989291,0.996847118055594,0.996554836292953),(0.997565691989291,
0.996847118055594,0.996554836292953)))
REPRESENTATION_ITEM('')
SURFACE()
);
#305=(
BOUNDED_SURFACE()
B_SPLINE_SURFACE(1,2,((#76314,#76315,#76316,#76317,#76318),(#76319,#76320,
#76321,#76322,#76323)),.UNSPECIFIED.,.F.,.F.,.F.)
B_SPLINE_SURFACE_WITH_KNOTS((2,2),(3,2,3),(0.,0.480770297080784),(0.0365944846645756,
0.0384615384615384,0.0431859280915184),.UNSPECIFIED.)
GEOMETRIC_REPRESENTATION_ITEM()
RATIONAL_B_SPLINE_SURFACE(((0.999326490452258,0.999646063968217,1.,0.999104400890347,
0.9984288220563),(0.999326490452258,0.999646063968217,1.,0.999104400890347,
0.9984288220563)))
REPRESENTATION_ITEM('')
SURFACE()
);
#306=(
BOUNDED_SURFACE()
B_SPLINE_SURFACE(1,2,((#76350,#76351,#76352),(#76353,#76354,#76355),(#76356,
#76357,#76358)),.UNSPECIFIED.,.F.,.F.,.F.)
B_SPLINE_SURFACE_WITH_KNOTS((2,1,2),(3,3),(0.,1.,1.01),(0.02559035961318,
0.0375948596693876),.UNSPECIFIED.)
GEOMETRIC_REPRESENTATION_ITEM()
RATIONAL_B_SPLINE_SURFACE(((0.996753121755999,0.997505687613148,0.999678813023853),
(0.996753121755999,0.997505687613148,0.999678813023853),(0.996753121755999,
0.997505687613148,0.999678813023853)))
REPRESENTATION_ITEM('')
SURFACE()
);
#307=(
BOUNDED_SURFACE()
B_SPLINE_SURFACE(1,2,((#76393,#76394,#76395),(#76396,#76397,#76398),(#76399,
#76400,#76401)),.UNSPECIFIED.,.F.,.F.,.F.)
B_SPLINE_SURFACE_WITH_KNOTS((2,1,2),(3,3),(-0.00286823045901626,0.,0.47790287978655),
(0.0265907346180616,0.0331702036774535),.UNSPECIFIED.)
GEOMETRIC_REPRESENTATION_ITEM()
RATIONAL_B_SPLINE_SURFACE(((0.996888414395785,0.997365765476469,0.998269846371839),
(0.996888414395785,0.997365765476469,0.998269846371838),(0.996888414395785,
0.997365765476469,0.998269846371838)))
REPRESENTATION_ITEM('')
SURFACE()
);
#308=(
BOUNDED_SURFACE()
B_SPLINE_SURFACE(1,2,((#76468,#76469,#76470),(#76471,#76472,#76473),(#76474,
#76475,#76476)),.UNSPECIFIED.,.F.,.F.,.F.)
B_SPLINE_SURFACE_WITH_KNOTS((2,1,2),(3,3),(-0.00286753128201114,0.,0.477902879786504),
(0.0166015299238954,0.0231736788111883),.UNSPECIFIED.)
GEOMETRIC_REPRESENTATION_ITEM()
RATIONAL_B_SPLINE_SURFACE(((0.996422581660833,0.996252244737342,0.996507688616404),
(0.996422581660833,0.996252244737342,0.996507688616404),(0.996422581660833,
0.996252244737342,0.996507688616404)))
REPRESENTATION_ITEM('')
SURFACE()
);
#309=(
BOUNDED_SURFACE()
B_SPLINE_SURFACE(1,2,((#76493,#76494,#76495),(#76496,#76497,#76498),(#76499,
#76500,#76501),(#76502,#76503,#76504)),.UNSPECIFIED.,.F.,.F.,.F.)
B_SPLINE_SURFACE_WITH_KNOTS((2,1,1,2),(3,3),(-0.0101,0.,1.,1.01),(0.00560769168370589,
0.0176009700440522),.UNSPECIFIED.)
GEOMETRIC_REPRESENTATION_ITEM()
RATIONAL_B_SPLINE_SURFACE(((0.99818389211382,0.99657330421516,0.996380621259469),
(0.99818389211382,0.99657330421516,0.996380621259469),(0.99818389211382,
0.99657330421516,0.996380621259469),(0.99818389211382,0.99657330421516,
0.996380621259469)))
REPRESENTATION_ITEM('')
SURFACE()
);
#310=(
BOUNDED_SURFACE()
B_SPLINE_SURFACE(1,2,((#76539,#76540,#76541),(#76542,#76543,#76544),(#76545,
#76546,#76547)),.UNSPECIFIED.,.F.,.F.,.F.)
B_SPLINE_SURFACE_WITH_KNOTS((2,1,2),(3,3),(-0.00206901892635118,0.,0.346769728493102),
(0.00660713154716551,0.0131849431469464),.UNSPECIFIED.)
GEOMETRIC_REPRESENTATION_ITEM()
RATIONAL_B_SPLINE_SURFACE(((0.997925307359457,0.997106772384937,0.996714752253854),
(0.997925307359457,0.997106772384937,0.996714752253854),(0.997925307359457,
0.997106772384937,0.996714752253854)))
REPRESENTATION_ITEM('')
SURFACE()
);
#311=(
BOUNDED_SURFACE()
B_SPLINE_SURFACE(1,2,((#76620,#76621,#76622),(#76623,#76624,#76625)),
 .UNSPECIFIED.,.F.,.F.,.F.)
B_SPLINE_SURFACE_WITH_KNOTS((2,2),(3,3),(0.,1.),(0.0556006976418414,0.0675888856590506),
 .UNSPECIFIED.)
GEOMETRIC_REPRESENTATION_ITEM()
RATIONAL_B_SPLINE_SURFACE(((0.996397562408606,0.996150386832629,0.997319912843745),
(0.996397562408606,0.996150386832629,0.997319912843745)))
REPRESENTATION_ITEM('')
SURFACE()
);
#312=(
BOUNDED_SURFACE()
B_SPLINE_SURFACE(1,2,((#76694,#76695,#76696),(#76697,#76698,#76699)),
 .UNSPECIFIED.,.F.,.F.,.F.)
B_SPLINE_SURFACE_WITH_KNOTS((2,2),(3,3),(0.,1.),(0.0456081671210044,0.0575989447818824),
 .UNSPECIFIED.)
GEOMETRIC_REPRESENTATION_ITEM()
RATIONAL_B_SPLINE_SURFACE(((0.997793907739636,0.996365558499688,0.996354522974128),
(0.997793907739636,0.996365558499688,0.996354522974128)))
REPRESENTATION_ITEM('')
SURFACE()
);
#313=(
BOUNDED_SURFACE()
B_SPLINE_SURFACE(1,2,((#76766,#76767,#76768,#76769,#76770),(#76771,#76772,
#76773,#76774,#76775),(#76776,#76777,#76778,#76779,#76780)),
 .UNSPECIFIED.,.F.,.F.,.F.)
B_SPLINE_SURFACE_WITH_KNOTS((2,1,2),(3,2,3),(0.,1.,1.01),(0.0355931932713903,
0.0384615384615384,0.0476086899858133),.UNSPECIFIED.)
GEOMETRIC_REPRESENTATION_ITEM()
RATIONAL_B_SPLINE_SURFACE(((0.998993602249807,0.999456249886298,1.,0.998265981131401,
0.997356751596327),(0.998993602249807,0.999456249886298,1.,0.998265981131401,
0.997356751596327),(0.998993602249807,0.999456249886298,1.,0.998265981131401,
0.997356751596327)))
REPRESENTATION_ITEM('')
SURFACE()
);
#314=(
BOUNDED_SURFACE()
B_SPLINE_SURFACE(1,2,((#76828,#76829,#76830,#76831,#76832),(#76833,#76834,
#76835,#76836,#76837),(#76838,#76839,#76840,#76841,#76842)),
 .UNSPECIFIED.,.F.,.F.,.F.)
B_SPLINE_SURFACE_WITH_KNOTS((2,1,2),(3,2,3),(-0.00286743098833038,0.,0.480770297147049),
(0.0365944846643319,0.0384615384615384,0.0431859280915196),
 .UNSPECIFIED.)
GEOMETRIC_REPRESENTATION_ITEM()
RATIONAL_B_SPLINE_SURFACE(((0.999326490452175,0.99964606396817,1.,0.999104400890347,
0.9984288220563),(0.999326490452175,0.99964606396817,1.,0.999104400890347,
0.9984288220563),(0.999326490452175,0.99964606396817,1.,0.999104400890347,
0.9984288220563)))
REPRESENTATION_ITEM('')
SURFACE()
);
#315=(
BOUNDED_SURFACE()
B_SPLINE_SURFACE(1,2,((#76869,#76870,#76871),(#76872,#76873,#76874)),
 .UNSPECIFIED.,.F.,.F.,.F.)
B_SPLINE_SURFACE_WITH_KNOTS((2,2),(3,3),(0.,1.),(0.0255903596131787,0.0375948596693877),
 .UNSPECIFIED.)
GEOMETRIC_REPRESENTATION_ITEM()
RATIONAL_B_SPLINE_SURFACE(((0.996753121755999,0.997505687613147,0.999678813023853),
(0.996753121755999,0.997505687613147,0.999678813023853)))
REPRESENTATION_ITEM('')
SURFACE()
);
#316=(
BOUNDED_SURFACE()
B_SPLINE_SURFACE(1,2,((#76991,#76992,#76993),(#76994,#76995,#76996),(#76997,
#76998,#76999)),.UNSPECIFIED.,.F.,.F.,.F.)
B_SPLINE_SURFACE_WITH_KNOTS((2,1,2),(3,3),(-0.00286753114038783,0.,0.477902879786557),
(0.0166015299238959,0.0231736788090033),.UNSPECIFIED.)
GEOMETRIC_REPRESENTATION_ITEM()
RATIONAL_B_SPLINE_SURFACE(((0.996422581660833,0.996252244737399,0.996507688616235),
(0.996422581660833,0.996252244737399,0.996507688616235),(0.996422581660833,
0.996252244737399,0.996507688616235)))
REPRESENTATION_ITEM('')
SURFACE()
);
#317=(
BOUNDED_SURFACE()
B_SPLINE_SURFACE(1,2,((#77016,#77017,#77018),(#77019,#77020,#77021),(#77022,
#77023,#77024),(#77025,#77026,#77027)),.UNSPECIFIED.,.F.,.F.,.F.)
B_SPLINE_SURFACE_WITH_KNOTS((2,1,1,2),(3,3),(-0.0101,0.,1.,1.01),(0.00560769168370523,
0.0176009700440517),.UNSPECIFIED.)
GEOMETRIC_REPRESENTATION_ITEM()
RATIONAL_B_SPLINE_SURFACE(((0.99818389211382,0.99657330421516,0.996380621259469),
(0.99818389211382,0.99657330421516,0.996380621259469),(0.99818389211382,
0.99657330421516,0.996380621259469),(0.99818389211382,0.99657330421516,
0.996380621259469)))
REPRESENTATION_ITEM('')
SURFACE()
);
#318=(
BOUNDED_SURFACE()
B_SPLINE_SURFACE(1,2,((#77062,#77063,#77064),(#77065,#77066,#77067),(#77068,
#77069,#77070)),.UNSPECIFIED.,.F.,.F.,.F.)
B_SPLINE_SURFACE_WITH_KNOTS((2,1,2),(3,3),(-0.0020690189263002,0.,0.346769728493041),
(0.00660713154715324,0.0131849431469514),.UNSPECIFIED.)
GEOMETRIC_REPRESENTATION_ITEM()
RATIONAL_B_SPLINE_SURFACE(((0.99792530735946,0.997106772384937,0.996714752253853),
(0.99792530735946,0.997106772384937,0.996714752253853),(0.99792530735946,
0.997106772384937,0.996714752253853)))
REPRESENTATION_ITEM('')
SURFACE()
);
#319=(
BOUNDED_SURFACE()
B_SPLINE_SURFACE(1,2,((#77143,#77144,#77145),(#77146,#77147,#77148)),
 .UNSPECIFIED.,.F.,.F.,.F.)
B_SPLINE_SURFACE_WITH_KNOTS((2,2),(3,3),(0.,1.),(0.0556006976418415,0.06758888565905),
 .UNSPECIFIED.)
GEOMETRIC_REPRESENTATION_ITEM()
RATIONAL_B_SPLINE_SURFACE(((0.996397562408606,0.996150386832629,0.997319912843745),
(0.996397562408606,0.996150386832629,0.997319912843745)))
REPRESENTATION_ITEM('')
SURFACE()
);
#320=(
BOUNDED_SURFACE()
B_SPLINE_SURFACE(1,2,((#77217,#77218,#77219),(#77220,#77221,#77222),(#77223,
#77224,#77225)),.UNSPECIFIED.,.F.,.F.,.F.)
B_SPLINE_SURFACE_WITH_KNOTS((2,1,2),(3,3),(0.,1.,1.01),(0.0456081671210055,
0.0575989447818818),.UNSPECIFIED.)
GEOMETRIC_REPRESENTATION_ITEM()
RATIONAL_B_SPLINE_SURFACE(((0.997793907739636,0.996365558499688,0.996354522974128),
(0.997793907739636,0.996365558499688,0.996354522974128),(0.997793907739636,
0.996365558499688,0.996354522974128)))
REPRESENTATION_ITEM('')
SURFACE()
);
#321=(
BOUNDED_SURFACE()
B_SPLINE_SURFACE(1,2,((#77260,#77261,#77262),(#77263,#77264,#77265),(#77266,
#77267,#77268)),.UNSPECIFIED.,.F.,.F.,.F.)
B_SPLINE_SURFACE_WITH_KNOTS((2,1,2),(3,3),(-0.00286810173465011,0.,0.477902879786603),
(0.0466073985929122,0.0531834929157972),.UNSPECIFIED.)
GEOMETRIC_REPRESENTATION_ITEM()
RATIONAL_B_SPLINE_SURFACE(((0.997565691989291,0.996847118055594,0.996554836292953),
(0.997565691989291,0.996847118055594,0.996554836292953),(0.997565691989291,
0.996847118055594,0.996554836292953)))
REPRESENTATION_ITEM('')
SURFACE()
);
#322=(
BOUNDED_SURFACE()
B_SPLINE_SURFACE(1,2,((#77285,#77286,#77287,#77288,#77289),(#77290,#77291,
#77292,#77293,#77294),(#77295,#77296,#77297,#77298,#77299)),
 .UNSPECIFIED.,.F.,.F.,.F.)
B_SPLINE_SURFACE_WITH_KNOTS((2,1,2),(3,2,3),(0.,1.,1.01),(0.0355931932713912,
0.0384615384615384,0.0476086899858135),.UNSPECIFIED.)
GEOMETRIC_REPRESENTATION_ITEM()
RATIONAL_B_SPLINE_SURFACE(((0.998993602249807,0.999456249886298,1.,0.998265981131401,
0.997356751596327),(0.998993602249807,0.999456249886298,1.,0.998265981131401,
0.997356751596327),(0.998993602249807,0.999456249886298,1.,0.998265981131401,
0.997356751596327)))
REPRESENTATION_ITEM('')
SURFACE()
);
#323=(
BOUNDED_SURFACE()
B_SPLINE_SURFACE(1,2,((#77347,#77348,#77349,#77350,#77351),(#77352,#77353,
#77354,#77355,#77356),(#77357,#77358,#77359,#77360,#77361)),
 .UNSPECIFIED.,.F.,.F.,.F.)
B_SPLINE_SURFACE_WITH_KNOTS((2,1,2),(3,2,3),(-0.00286743098864766,0.,0.480770297147027),
(0.0365944846643192,0.0384615384615384,0.0431859280915204),
 .UNSPECIFIED.)
GEOMETRIC_REPRESENTATION_ITEM()
RATIONAL_B_SPLINE_SURFACE(((0.999326490452171,0.999646063968168,1.,0.999104400890346,
0.998428822056299),(0.999326490452171,0.999646063968168,1.,0.999104400890346,
0.998428822056299),(0.999326490452171,0.999646063968168,1.,0.999104400890346,
0.998428822056299)))
REPRESENTATION_ITEM('')
SURFACE()
);
#324=(
BOUNDED_SURFACE()
B_SPLINE_SURFACE(1,2,((#77388,#77389,#77390),(#77391,#77392,#77393),(#77394,
#77395,#77396)),.UNSPECIFIED.,.F.,.F.,.F.)
B_SPLINE_SURFACE_WITH_KNOTS((2,1,2),(3,3),(0.,1.,1.01),(0.02559035961318,
0.0375948596693866),.UNSPECIFIED.)
GEOMETRIC_REPRESENTATION_ITEM()
RATIONAL_B_SPLINE_SURFACE(((0.996753121755999,0.997505687613148,0.999678813023853),
(0.996753121755999,0.997505687613148,0.999678813023853),(0.996753121755999,
0.997505687613148,0.999678813023853)))
REPRESENTATION_ITEM('')
SURFACE()
);
#325=(
BOUNDED_SURFACE()
B_SPLINE_SURFACE(1,2,((#77431,#77432,#77433),(#77434,#77435,#77436),(#77437,
#77438,#77439)),.UNSPECIFIED.,.F.,.F.,.F.)
B_SPLINE_SURFACE_WITH_KNOTS((2,1,2),(3,3),(-0.00286823356211481,0.,0.477902879786507),
(0.0265907346180626,0.0331702037252924),.UNSPECIFIED.)
GEOMETRIC_REPRESENTATION_ITEM()
RATIONAL_B_SPLINE_SURFACE(((0.996888414395785,0.997365765479939,0.998269846384985),
(0.996888414395785,0.997365765479939,0.998269846384985),(0.996888414395785,
0.997365765479939,0.998269846384985)))
REPRESENTATION_ITEM('')
SURFACE()
);
#326=(
BOUNDED_SURFACE()
B_SPLINE_SURFACE(1,2,((#77538,#77539,#77540),(#77541,#77542,#77543),(#77544,
#77545,#77546),(#77547,#77548,#77549)),.UNSPECIFIED.,.F.,.F.,.F.)
B_SPLINE_SURFACE_WITH_KNOTS((2,1,1,2),(3,3),(-0.0101,0.,1.,1.01),(0.00560769168370627,
0.0176009700440506),.UNSPECIFIED.)
GEOMETRIC_REPRESENTATION_ITEM()
RATIONAL_B_SPLINE_SURFACE(((0.99818389211382,0.99657330421516,0.996380621259469),
(0.99818389211382,0.99657330421516,0.996380621259469),(0.99818389211382,
0.99657330421516,0.996380621259469),(0.99818389211382,0.99657330421516,
0.996380621259469)))
REPRESENTATION_ITEM('')
SURFACE()
);
#327=(
BOUNDED_SURFACE()
B_SPLINE_SURFACE(1,2,((#77584,#77585,#77586),(#77587,#77588,#77589),(#77590,
#77591,#77592)),.UNSPECIFIED.,.F.,.F.,.F.)
B_SPLINE_SURFACE_WITH_KNOTS((2,1,2),(3,3),(-0.00206901892627739,0.,0.346769728493106),
(0.00660713154713986,0.013184943146955),.UNSPECIFIED.)
GEOMETRIC_REPRESENTATION_ITEM()
RATIONAL_B_SPLINE_SURFACE(((0.997925307359463,0.997106772384937,0.996714752253853),
(0.997925307359463,0.997106772384937,0.996714752253853),(0.997925307359463,
0.997106772384937,0.996714752253853)))
REPRESENTATION_ITEM('')
SURFACE()
);
#328=(
BOUNDED_SURFACE()
B_SPLINE_SURFACE(1,2,((#77665,#77666,#77667),(#77668,#77669,#77670)),
 .UNSPECIFIED.,.F.,.F.,.F.)
B_SPLINE_SURFACE_WITH_KNOTS((2,2),(3,3),(0.,1.),(0.0556006976418401,0.0675888856590505),
 .UNSPECIFIED.)
GEOMETRIC_REPRESENTATION_ITEM()
RATIONAL_B_SPLINE_SURFACE(((0.996397562408606,0.996150386832629,0.997319912843745),
(0.996397562408606,0.996150386832629,0.997319912843745)))
REPRESENTATION_ITEM('')
SURFACE()
);
#329=(
BOUNDED_SURFACE()
B_SPLINE_SURFACE(1,2,((#77739,#77740,#77741),(#77742,#77743,#77744),(#77745,
#77746,#77747)),.UNSPECIFIED.,.F.,.F.,.F.)
B_SPLINE_SURFACE_WITH_KNOTS((2,1,2),(3,3),(0.,1.,1.01),(0.0456081671210034,
0.0575989447818819),.UNSPECIFIED.)
GEOMETRIC_REPRESENTATION_ITEM()
RATIONAL_B_SPLINE_SURFACE(((0.997793907739636,0.996365558499688,0.996354522974128),
(0.997793907739636,0.996365558499688,0.996354522974128),(0.997793907739636,
0.996365558499688,0.996354522974128)))
REPRESENTATION_ITEM('')
SURFACE()
);
#330=(
BOUNDED_SURFACE()
B_SPLINE_SURFACE(1,2,((#77782,#77783,#77784),(#77785,#77786,#77787),(#77788,
#77789,#77790)),.UNSPECIFIED.,.F.,.F.,.F.)
B_SPLINE_SURFACE_WITH_KNOTS((2,1,2),(3,3),(-0.00286810173460448,0.,0.477902879786547),
(0.0466073985929112,0.0531834929157984),.UNSPECIFIED.)
GEOMETRIC_REPRESENTATION_ITEM()
RATIONAL_B_SPLINE_SURFACE(((0.997565691989291,0.996847118055593,0.996554836292953),
(0.997565691989291,0.996847118055593,0.996554836292953),(0.997565691989291,
0.996847118055593,0.996554836292953)))
REPRESENTATION_ITEM('')
SURFACE()
);
#331=(
BOUNDED_SURFACE()
B_SPLINE_SURFACE(1,2,((#77807,#77808,#77809,#77810,#77811),(#77812,#77813,
#77814,#77815,#77816),(#77817,#77818,#77819,#77820,#77821)),
 .UNSPECIFIED.,.F.,.F.,.F.)
B_SPLINE_SURFACE_WITH_KNOTS((2,1,2),(3,2,3),(0.,1.,1.01),(0.0355931932713902,
0.0384615384615384,0.0476086899858139),.UNSPECIFIED.)
GEOMETRIC_REPRESENTATION_ITEM()
RATIONAL_B_SPLINE_SURFACE(((0.998993602249807,0.999456249886298,1.,0.998265981131401,
0.997356751596327),(0.998993602249807,0.999456249886298,1.,0.998265981131401,
0.997356751596327),(0.998993602249807,0.999456249886298,1.,0.998265981131401,
0.997356751596327)))
REPRESENTATION_ITEM('')
SURFACE()
);
#332=(
BOUNDED_SURFACE()
B_SPLINE_SURFACE(1,2,((#77869,#77870,#77871,#77872,#77873),(#77874,#77875,
#77876,#77877,#77878),(#77879,#77880,#77881,#77882,#77883)),
 .UNSPECIFIED.,.F.,.F.,.F.)
B_SPLINE_SURFACE_WITH_KNOTS((2,1,2),(3,2,3),(-0.00286743098852175,0.,0.480770297147094),
(0.0365944846643036,0.0384615384615384,0.04318592809152),.UNSPECIFIED.)
GEOMETRIC_REPRESENTATION_ITEM()
RATIONAL_B_SPLINE_SURFACE(((0.999326490452165,0.999646063968165,1.,0.999104400890347,
0.9984288220563),(0.999326490452165,0.999646063968165,1.,0.999104400890347,
0.9984288220563),(0.999326490452165,0.999646063968165,1.,0.999104400890347,
0.9984288220563)))
REPRESENTATION_ITEM('')
SURFACE()
);
#333=(
BOUNDED_SURFACE()
B_SPLINE_SURFACE(1,2,((#77910,#77911,#77912),(#77913,#77914,#77915),(#77916,
#77917,#77918)),.UNSPECIFIED.,.F.,.F.,.F.)
B_SPLINE_SURFACE_WITH_KNOTS((2,1,2),(3,3),(0.,1.,1.01),(0.0255903596131798,
0.0375948596693887),.UNSPECIFIED.)
GEOMETRIC_REPRESENTATION_ITEM()
RATIONAL_B_SPLINE_SURFACE(((0.996753121755999,0.997505687613148,0.999678813023854),
(0.996753121755999,0.997505687613148,0.999678813023854),(0.996753121755999,
0.997505687613148,0.999678813023854)))
REPRESENTATION_ITEM('')
SURFACE()
);
#334=(
BOUNDED_SURFACE()
B_SPLINE_SURFACE(1,2,((#77953,#77954,#77955),(#77956,#77957,#77958),(#77959,
#77960,#77961)),.UNSPECIFIED.,.F.,.F.,.F.)
B_SPLINE_SURFACE_WITH_KNOTS((2,1,2),(3,3),(-0.0028682325730164,0.,0.477902879786577),
(0.0265907346180616,0.0331702037100451),.UNSPECIFIED.)
GEOMETRIC_REPRESENTATION_ITEM()
RATIONAL_B_SPLINE_SURFACE(((0.996888414395785,0.997365765478833,0.998269846380795),
(0.996888414395785,0.997365765478833,0.998269846380795),(0.996888414395785,
0.997365765478833,0.998269846380795)))
REPRESENTATION_ITEM('')
SURFACE()
);
#335=(
BOUNDED_SURFACE()
B_SPLINE_SURFACE(1,2,((#78028,#78029,#78030),(#78031,#78032,#78033),(#78034,
#78035,#78036)),.UNSPECIFIED.,.F.,.F.,.F.)
B_SPLINE_SURFACE_WITH_KNOTS((2,1,2),(3,3),(-0.0028675311404356,0.,0.47790287978656),
(0.0166015299238945,0.023173678809005),.UNSPECIFIED.)
GEOMETRIC_REPRESENTATION_ITEM()
RATIONAL_B_SPLINE_SURFACE(((0.996422581660833,0.996252244737399,0.996507688616235),
(0.996422581660833,0.996252244737399,0.996507688616235),(0.996422581660833,
0.996252244737399,0.996507688616235)))
REPRESENTATION_ITEM('')
SURFACE()
);
#336=(
BOUNDED_SURFACE()
B_SPLINE_SURFACE(1,2,((#78053,#78054,#78055),(#78056,#78057,#78058),(#78059,
#78060,#78061)),.UNSPECIFIED.,.F.,.F.,.F.)
B_SPLINE_SURFACE_WITH_KNOTS((2,1,2),(3,3),(-0.01,0.,1.00000001523966),(0.00560769168370504,
0.0176009700440523),.UNSPECIFIED.)
GEOMETRIC_REPRESENTATION_ITEM()
RATIONAL_B_SPLINE_SURFACE(((0.998183892113821,0.99657330421516,0.996380621259469),
(0.998183892113821,0.99657330421516,0.996380621259469),(0.998183892113821,
0.99657330421516,0.996380621259469)))
REPRESENTATION_ITEM('')
SURFACE()
);
#337=(
BOUNDED_SURFACE()
B_SPLINE_SURFACE(1,2,((#78184,#78185,#78186),(#78187,#78188,#78189)),
 .UNSPECIFIED.,.F.,.F.,.F.)
B_SPLINE_SURFACE_WITH_KNOTS((2,2),(3,3),(0.,1.),(0.0556006976418415,0.0675888856590494),
 .UNSPECIFIED.)
GEOMETRIC_REPRESENTATION_ITEM()
RATIONAL_B_SPLINE_SURFACE(((0.996397562408606,0.996150386832629,0.997319912843745),
(0.996397562408606,0.996150386832629,0.997319912843745)))
REPRESENTATION_ITEM('')
SURFACE()
);
#338=(
BOUNDED_SURFACE()
B_SPLINE_SURFACE(1,2,((#78258,#78259,#78260),(#78261,#78262,#78263),(#78264,
#78265,#78266)),.UNSPECIFIED.,.F.,.F.,.F.)
B_SPLINE_SURFACE_WITH_KNOTS((2,1,2),(3,3),(0.,1.,1.01),(0.0456081671210047,
0.0575989447818808),.UNSPECIFIED.)
GEOMETRIC_REPRESENTATION_ITEM()
RATIONAL_B_SPLINE_SURFACE(((0.997793907739636,0.996365558499688,0.996354522974128),
(0.997793907739636,0.996365558499688,0.996354522974128),(0.997793907739636,
0.996365558499688,0.996354522974128)))
REPRESENTATION_ITEM('')
SURFACE()
);
#339=(
BOUNDED_SURFACE()
B_SPLINE_SURFACE(1,2,((#78301,#78302,#78303),(#78304,#78305,#78306),(#78307,
#78308,#78309)),.UNSPECIFIED.,.F.,.F.,.F.)
B_SPLINE_SURFACE_WITH_KNOTS((2,1,2),(3,3),(-0.00286810171938679,0.,0.47790287978657),
(0.0466073985929119,0.0531834927425516),.UNSPECIFIED.)
GEOMETRIC_REPRESENTATION_ITEM()
RATIONAL_B_SPLINE_SURFACE(((0.997565691989291,0.996847118074524,0.996554836308353),
(0.997565691989291,0.996847118074524,0.996554836308353),(0.997565691989291,
0.996847118074524,0.996554836308353)))
REPRESENTATION_ITEM('')
SURFACE()
);
#340=(
BOUNDED_SURFACE()
B_SPLINE_SURFACE(1,2,((#78326,#78327,#78328,#78329,#78330),(#78331,#78332,
#78333,#78334,#78335),(#78336,#78337,#78338,#78339,#78340)),
 .UNSPECIFIED.,.F.,.F.,.F.)
B_SPLINE_SURFACE_WITH_KNOTS((2,1,2),(3,2,3),(0.,1.,1.01),(0.0355931932713914,
0.0384615384615384,0.0476086899858119),.UNSPECIFIED.)
GEOMETRIC_REPRESENTATION_ITEM()
RATIONAL_B_SPLINE_SURFACE(((0.998993602249807,0.999456249886298,1.,0.998265981131401,
0.997356751596327),(0.998993602249807,0.999456249886298,1.,0.998265981131401,
0.997356751596327),(0.998993602249807,0.999456249886298,1.,0.998265981131401,
0.997356751596327)))
REPRESENTATION_ITEM('')
SURFACE()
);
#341=(
BOUNDED_SURFACE()
B_SPLINE_SURFACE(1,2,((#78388,#78389,#78390,#78391,#78392),(#78393,#78394,
#78395,#78396,#78397),(#78398,#78399,#78400,#78401,#78402)),
 .UNSPECIFIED.,.F.,.F.,.F.)
B_SPLINE_SURFACE_WITH_KNOTS((2,1,2),(3,2,3),(-0.00286742668227491,0.,0.480770297121352),
(0.03659448466429,0.0384615384615384,0.0431859280915197),.UNSPECIFIED.)
GEOMETRIC_REPRESENTATION_ITEM()
RATIONAL_B_SPLINE_SURFACE(((0.99932649045216,0.999646063968162,1.,0.999104400890347,
0.9984288220563),(0.99932649045216,0.999646063968162,1.,0.999104400890347,
0.9984288220563),(0.99932649045216,0.999646063968162,1.,0.999104400890347,
0.9984288220563)))
REPRESENTATION_ITEM('')
SURFACE()
);
#342=(
BOUNDED_SURFACE()
B_SPLINE_SURFACE(1,2,((#78429,#78430,#78431),(#78432,#78433,#78434),(#78435,
#78436,#78437)),.UNSPECIFIED.,.F.,.F.,.F.)
B_SPLINE_SURFACE_WITH_KNOTS((2,1,2),(3,3),(0.,1.,1.01),(0.02559035961318,
0.0375948596693869),.UNSPECIFIED.)
GEOMETRIC_REPRESENTATION_ITEM()
RATIONAL_B_SPLINE_SURFACE(((0.996753121755999,0.997505687613148,0.999678813023853),
(0.996753121755999,0.997505687613148,0.999678813023853),(0.996753121755999,
0.997505687613148,0.999678813023853)))
REPRESENTATION_ITEM('')
SURFACE()
);
#343=(
BOUNDED_SURFACE()
B_SPLINE_SURFACE(1,2,((#78472,#78473,#78474),(#78475,#78476,#78477),(#78478,
#78479,#78480)),.UNSPECIFIED.,.F.,.F.,.F.)
B_SPLINE_SURFACE_WITH_KNOTS((2,1,2),(3,3),(-0.00286823257304667,0.,0.477902879786519),
(0.0265907346180622,0.0331702037100437),.UNSPECIFIED.)
GEOMETRIC_REPRESENTATION_ITEM()
RATIONAL_B_SPLINE_SURFACE(((0.996888414395785,0.997365765478833,0.998269846380795),
(0.996888414395785,0.997365765478833,0.998269846380795),(0.996888414395785,
0.997365765478833,0.998269846380795)))
REPRESENTATION_ITEM('')
SURFACE()
);
#344=(
BOUNDED_SURFACE()
B_SPLINE_SURFACE(1,2,((#78547,#78548,#78549),(#78550,#78551,#78552),(#78553,
#78554,#78555)),.UNSPECIFIED.,.F.,.F.,.F.)
B_SPLINE_SURFACE_WITH_KNOTS((2,1,2),(3,3),(-0.00286753114035171,0.,0.477902879786553),
(0.0166015299238961,0.0231736788090039),.UNSPECIFIED.)
GEOMETRIC_REPRESENTATION_ITEM()
RATIONAL_B_SPLINE_SURFACE(((0.996422581660833,0.996252244737399,0.996507688616235),
(0.996422581660833,0.996252244737399,0.996507688616235),(0.996422581660833,
0.996252244737398,0.996507688616234)))
REPRESENTATION_ITEM('')
SURFACE()
);
#345=(
BOUNDED_SURFACE()
B_SPLINE_SURFACE(1,2,((#78572,#78573,#78574),(#78575,#78576,#78577),(#78578,
#78579,#78580),(#78581,#78582,#78583)),.UNSPECIFIED.,.F.,.F.,.F.)
B_SPLINE_SURFACE_WITH_KNOTS((2,1,1,2),(3,3),(-0.0101,0.,1.,1.01),(0.00560769168370619,
0.0176009700440505),.UNSPECIFIED.)
GEOMETRIC_REPRESENTATION_ITEM()
RATIONAL_B_SPLINE_SURFACE(((0.99818389211382,0.99657330421516,0.996380621259469),
(0.99818389211382,0.99657330421516,0.996380621259469),(0.99818389211382,
0.99657330421516,0.996380621259469),(0.99818389211382,0.99657330421516,
0.996380621259469)))
REPRESENTATION_ITEM('')
SURFACE()
);
#346=(
BOUNDED_SURFACE()
B_SPLINE_SURFACE(1,2,((#78618,#78619,#78620),(#78621,#78622,#78623),(#78624,
#78625,#78626)),.UNSPECIFIED.,.F.,.F.,.F.)
B_SPLINE_SURFACE_WITH_KNOTS((2,1,2),(3,3),(-0.00206901892609941,0.,0.346769728493053),
(0.00660713154711239,0.0131849431469057),.UNSPECIFIED.)
GEOMETRIC_REPRESENTATION_ITEM()
RATIONAL_B_SPLINE_SURFACE(((0.99792530735947,0.997106772384945,0.996714752253859),
(0.99792530735947,0.997106772384945,0.996714752253859),(0.99792530735947,
0.997106772384945,0.996714752253859)))
REPRESENTATION_ITEM('')
SURFACE()
);
#347=(
BOUNDED_SURFACE()
B_SPLINE_SURFACE(1,2,((#78699,#78700,#78701),(#78702,#78703,#78704)),
 .UNSPECIFIED.,.F.,.F.,.F.)
B_SPLINE_SURFACE_WITH_KNOTS((2,2),(3,3),(0.,1.),(0.0556006976418415,0.0675888856590505),
 .UNSPECIFIED.)
GEOMETRIC_REPRESENTATION_ITEM()
RATIONAL_B_SPLINE_SURFACE(((0.996397562408606,0.996150386832629,0.997319912843745),
(0.996397562408606,0.996150386832629,0.997319912843745)))
REPRESENTATION_ITEM('')
SURFACE()
);
#348=(
BOUNDED_SURFACE()
B_SPLINE_SURFACE(1,2,((#78773,#78774,#78775),(#78776,#78777,#78778),(#78779,
#78780,#78781)),.UNSPECIFIED.,.F.,.F.,.F.)
B_SPLINE_SURFACE_WITH_KNOTS((2,1,2),(3,3),(0.,1.,1.01),(0.0456081671210044,
0.0575989447818814),.UNSPECIFIED.)
GEOMETRIC_REPRESENTATION_ITEM()
RATIONAL_B_SPLINE_SURFACE(((0.997793907739636,0.996365558499688,0.996354522974128),
(0.997793907739636,0.996365558499688,0.996354522974128),(0.997793907739636,
0.996365558499688,0.996354522974128)))
REPRESENTATION_ITEM('')
SURFACE()
);
#349=(
BOUNDED_SURFACE()
B_SPLINE_SURFACE(1,2,((#78816,#78817,#78818),(#78819,#78820,#78821),(#78822,
#78823,#78824)),.UNSPECIFIED.,.F.,.F.,.F.)
B_SPLINE_SURFACE_WITH_KNOTS((2,1,2),(3,3),(-0.00286810173453871,0.,0.477902879786588),
(0.0466073985929109,0.0531834929157976),.UNSPECIFIED.)
GEOMETRIC_REPRESENTATION_ITEM()
RATIONAL_B_SPLINE_SURFACE(((0.997565691989291,0.996847118055593,0.996554836292953),
(0.997565691989291,0.996847118055593,0.996554836292953),(0.997565691989291,
0.996847118055593,0.996554836292953)))
REPRESENTATION_ITEM('')
SURFACE()
);
#350=(
BOUNDED_SURFACE()
B_SPLINE_SURFACE(1,2,((#78841,#78842,#78843,#78844,#78845),(#78846,#78847,
#78848,#78849,#78850),(#78851,#78852,#78853,#78854,#78855)),
 .UNSPECIFIED.,.F.,.F.,.F.)
B_SPLINE_SURFACE_WITH_KNOTS((2,1,2),(3,2,3),(0.,1.,1.01),(0.0355931932713903,
0.0384615384615384,0.0476086899858134),.UNSPECIFIED.)
GEOMETRIC_REPRESENTATION_ITEM()
RATIONAL_B_SPLINE_SURFACE(((0.998993602249807,0.999456249886298,1.,0.998265981131401,
0.997356751596327),(0.998993602249807,0.999456249886298,1.,0.998265981131401,
0.997356751596327),(0.998993602249807,0.999456249886298,1.,0.998265981131401,
0.997356751596327)))
REPRESENTATION_ITEM('')
SURFACE()
);
#351=(
BOUNDED_SURFACE()
B_SPLINE_SURFACE(1,2,((#78903,#78904,#78905,#78906,#78907),(#78908,#78909,
#78910,#78911,#78912),(#78913,#78914,#78915,#78916,#78917)),
 .UNSPECIFIED.,.F.,.F.,.F.)
B_SPLINE_SURFACE_WITH_KNOTS((2,1,2),(3,2,3),(-0.00141401191198416,0.,0.480770297080041),
(0.0365944846645786,0.0384615384615384,0.0431859280915184),
 .UNSPECIFIED.)
GEOMETRIC_REPRESENTATION_ITEM()
RATIONAL_B_SPLINE_SURFACE(((0.999326490452259,0.999646063968217,1.,0.999104400890347,
0.9984288220563),(0.999326490452259,0.999646063968217,1.,0.999104400890347,
0.9984288220563),(0.999326490452259,0.999646063968217,1.,0.999104400890347,
0.9984288220563)))
REPRESENTATION_ITEM('')
SURFACE()
);
#352=(
BOUNDED_SURFACE()
B_SPLINE_SURFACE(1,2,((#78944,#78945,#78946),(#78947,#78948,#78949),(#78950,
#78951,#78952)),.UNSPECIFIED.,.F.,.F.,.F.)
B_SPLINE_SURFACE_WITH_KNOTS((2,1,2),(3,3),(0.,1.,1.01),(0.0255903596131787,
0.0375948596693877),.UNSPECIFIED.)
GEOMETRIC_REPRESENTATION_ITEM()
RATIONAL_B_SPLINE_SURFACE(((0.996753121755999,0.997505687613148,0.999678813023853),
(0.996753121755999,0.997505687613148,0.999678813023853),(0.996753121755999,
0.997505687613148,0.999678813023853)))
REPRESENTATION_ITEM('')
SURFACE()
);
#353=(
BOUNDED_SURFACE()
B_SPLINE_SURFACE(1,2,((#78987,#78988,#78989),(#78990,#78991,#78992),(#78993,
#78994,#78995)),.UNSPECIFIED.,.F.,.F.,.F.)
B_SPLINE_SURFACE_WITH_KNOTS((2,1,2),(3,3),(-0.00286823356215784,0.,0.477902879786496),
(0.0265907346180615,0.0331702037252929),.UNSPECIFIED.)
GEOMETRIC_REPRESENTATION_ITEM()
RATIONAL_B_SPLINE_SURFACE(((0.996888414395785,0.997365765479939,0.998269846384985),
(0.996888414395785,0.997365765479939,0.998269846384985),(0.996888414395785,
0.997365765479939,0.998269846384985)))
REPRESENTATION_ITEM('')
SURFACE()
);
#354=(
BOUNDED_SURFACE()
B_SPLINE_SURFACE(1,2,((#79062,#79063,#79064),(#79065,#79066,#79067),(#79068,
#79069,#79070)),.UNSPECIFIED.,.F.,.F.,.F.)
B_SPLINE_SURFACE_WITH_KNOTS((2,1,2),(3,3),(-0.00286753074356712,0.,0.47790287978649),
(0.0166015299238963,0.0231736788028835),.UNSPECIFIED.)
GEOMETRIC_REPRESENTATION_ITEM()
RATIONAL_B_SPLINE_SURFACE(((0.996422581660833,0.996252244737557,0.996507688615759),
(0.996422581660833,0.996252244737557,0.996507688615759),(0.996422581660833,
0.996252244737557,0.996507688615759)))
REPRESENTATION_ITEM('')
SURFACE()
);
#355=(
BOUNDED_SURFACE()
B_SPLINE_SURFACE(1,2,((#79087,#79088,#79089),(#79090,#79091,#79092),(#79093,
#79094,#79095),(#79096,#79097,#79098)),.UNSPECIFIED.,.F.,.F.,.F.)
B_SPLINE_SURFACE_WITH_KNOTS((2,1,1,2),(3,3),(-0.0101,0.,1.,1.01),(0.00560769168370609,
0.0176009700440527),.UNSPECIFIED.)
GEOMETRIC_REPRESENTATION_ITEM()
RATIONAL_B_SPLINE_SURFACE(((0.99818389211382,0.99657330421516,0.996380621259469),
(0.99818389211382,0.99657330421516,0.996380621259469),(0.99818389211382,
0.99657330421516,0.996380621259469),(0.99818389211382,0.99657330421516,
0.996380621259469)))
REPRESENTATION_ITEM('')
SURFACE()
);
#356=(
BOUNDED_SURFACE()
B_SPLINE_SURFACE(1,2,((#79133,#79134,#79135),(#79136,#79137,#79138),(#79139,
#79140,#79141)),.UNSPECIFIED.,.F.,.F.,.F.)
B_SPLINE_SURFACE_WITH_KNOTS((2,1,2),(3,3),(-0.00206901892446915,0.,0.346769728493051),
(0.00660713154709824,0.0131849431293194),.UNSPECIFIED.)
GEOMETRIC_REPRESENTATION_ITEM()
RATIONAL_B_SPLINE_SURFACE(((0.997925307359474,0.997106772387135,0.996714752255955),
(0.997925307359474,0.997106772387135,0.996714752255955),(0.997925307359474,
0.997106772387135,0.996714752255955)))
REPRESENTATION_ITEM('')
SURFACE()
);
#357=(
BOUNDED_SURFACE()
B_SPLINE_SURFACE(1,2,((#79214,#79215,#79216),(#79217,#79218,#79219)),
 .UNSPECIFIED.,.F.,.F.,.F.)
B_SPLINE_SURFACE_WITH_KNOTS((2,2),(3,3),(0.,1.),(0.0556006976418428,0.0675888856590498),
 .UNSPECIFIED.)
GEOMETRIC_REPRESENTATION_ITEM()
RATIONAL_B_SPLINE_SURFACE(((0.996397562408606,0.996150386832629,0.997319912843745),
(0.996397562408606,0.996150386832629,0.997319912843745)))
REPRESENTATION_ITEM('')
SURFACE()
);
#358=(
BOUNDED_SURFACE()
B_SPLINE_SURFACE(1,2,((#79288,#79289,#79290),(#79291,#79292,#79293),(#79294,
#79295,#79296)),.UNSPECIFIED.,.F.,.F.,.F.)
B_SPLINE_SURFACE_WITH_KNOTS((2,1,2),(3,3),(0.,1.,1.01),(0.0456081671210055,
0.0575989447818819),.UNSPECIFIED.)
GEOMETRIC_REPRESENTATION_ITEM()
RATIONAL_B_SPLINE_SURFACE(((0.997793907739636,0.996365558499688,0.996354522974128),
(0.997793907739636,0.996365558499688,0.996354522974128),(0.997793907739636,
0.996365558499688,0.996354522974128)))
REPRESENTATION_ITEM('')
SURFACE()
);
#359=(
BOUNDED_SURFACE()
B_SPLINE_SURFACE(1,2,((#79331,#79332,#79333),(#79334,#79335,#79336),(#79337,
#79338,#79339)),.UNSPECIFIED.,.F.,.F.,.F.)
B_SPLINE_SURFACE_WITH_KNOTS((2,1,2),(3,3),(-0.00286810173451702,0.,0.47790287978659),
(0.0466073985929117,0.0531834929157972),.UNSPECIFIED.)
GEOMETRIC_REPRESENTATION_ITEM()
RATIONAL_B_SPLINE_SURFACE(((0.997565691989291,0.996847118055593,0.996554836292953),
(0.997565691989291,0.996847118055593,0.996554836292953),(0.997565691989291,
0.996847118055594,0.996554836292953)))
REPRESENTATION_ITEM('')
SURFACE()
);
#360=(
BOUNDED_SURFACE()
B_SPLINE_SURFACE(1,2,((#79356,#79357,#79358,#79359,#79360),(#79361,#79362,
#79363,#79364,#79365),(#79366,#79367,#79368,#79369,#79370)),
 .UNSPECIFIED.,.F.,.F.,.F.)
B_SPLINE_SURFACE_WITH_KNOTS((2,1,2),(3,2,3),(0.,1.,1.01),(0.0355931932713904,
0.0384615384615384,0.0476086899858127),.UNSPECIFIED.)
GEOMETRIC_REPRESENTATION_ITEM()
RATIONAL_B_SPLINE_SURFACE(((0.998993602249807,0.999456249886298,1.,0.998265981131401,
0.997356751596327),(0.998993602249807,0.999456249886298,1.,0.998265981131401,
0.997356751596327),(0.998993602249807,0.999456249886298,1.,0.998265981131401,
0.997356751596327)))
REPRESENTATION_ITEM('')
SURFACE()
);
#361=(
BOUNDED_SURFACE()
B_SPLINE_SURFACE(1,2,((#79418,#79419,#79420,#79421,#79422),(#79423,#79424,
#79425,#79426,#79427),(#79428,#79429,#79430,#79431,#79432)),
 .UNSPECIFIED.,.F.,.F.,.F.)
B_SPLINE_SURFACE_WITH_KNOTS((2,1,2),(3,2,3),(-0.00286743098642913,0.,0.480770297146903),
(0.0365944846642603,0.0384615384615384,0.0431859280915195),
 .UNSPECIFIED.)
GEOMETRIC_REPRESENTATION_ITEM()
RATIONAL_B_SPLINE_SURFACE(((0.999326490452151,0.999646063968157,1.,0.999104400890347,
0.9984288220563),(0.999326490452151,0.999646063968157,1.,0.999104400890347,
0.9984288220563),(0.999326490452151,0.999646063968157,1.,0.999104400890347,
0.9984288220563)))
REPRESENTATION_ITEM('')
SURFACE()
);
#362=(
BOUNDED_SURFACE()
B_SPLINE_SURFACE(1,2,((#79459,#79460,#79461),(#79462,#79463,#79464),(#79465,
#79466,#79467)),.UNSPECIFIED.,.F.,.F.,.F.)
B_SPLINE_SURFACE_WITH_KNOTS((2,1,2),(3,3),(0.,1.,1.01),(0.0255903596131786,
0.0375948596693872),.UNSPECIFIED.)
GEOMETRIC_REPRESENTATION_ITEM()
RATIONAL_B_SPLINE_SURFACE(((0.996753121755999,0.997505687613147,0.999678813023853),
(0.996753121755999,0.997505687613147,0.999678813023853),(0.996753121755999,
0.997505687613147,0.999678813023853)))
REPRESENTATION_ITEM('')
SURFACE()
);
#363=(
BOUNDED_SURFACE()
B_SPLINE_SURFACE(1,2,((#79502,#79503,#79504),(#79505,#79506,#79507),(#79508,
#79509,#79510)),.UNSPECIFIED.,.F.,.F.,.F.)
B_SPLINE_SURFACE_WITH_KNOTS((2,1,2),(3,3),(-0.00286823356208571,0.,0.477902879786613),
(0.0265907346180613,0.0331702037252923),.UNSPECIFIED.)
GEOMETRIC_REPRESENTATION_ITEM()
RATIONAL_B_SPLINE_SURFACE(((0.996888414395785,0.997365765479939,0.998269846384985),
(0.996888414395785,0.997365765479939,0.998269846384985),(0.996888414395785,
0.997365765479939,0.998269846384985)))
REPRESENTATION_ITEM('')
SURFACE()
);
#364=(
BOUNDED_SURFACE()
B_SPLINE_SURFACE(1,2,((#79577,#79578,#79579),(#79580,#79581,#79582),(#79583,
#79584,#79585)),.UNSPECIFIED.,.F.,.F.,.F.)
B_SPLINE_SURFACE_WITH_KNOTS((2,1,2),(3,3),(-0.00286753128194045,0.,0.477902879786441),
(0.0166015299238959,0.0231736788111881),.UNSPECIFIED.)
GEOMETRIC_REPRESENTATION_ITEM()
RATIONAL_B_SPLINE_SURFACE(((0.996422581660833,0.996252244737342,0.996507688616404),
(0.996422581660833,0.996252244737342,0.996507688616404),(0.996422581660833,
0.996252244737342,0.996507688616404)))
REPRESENTATION_ITEM('')
SURFACE()
);
#365=(
BOUNDED_SURFACE()
B_SPLINE_SURFACE(1,2,((#79602,#79603,#79604),(#79605,#79606,#79607),(#79608,
#79609,#79610),(#79611,#79612,#79613)),.UNSPECIFIED.,.F.,.F.,.F.)
B_SPLINE_SURFACE_WITH_KNOTS((2,1,1,2),(3,3),(-0.0101,0.,1.,1.01),(0.00560769168370533,
0.0176009700440512),.UNSPECIFIED.)
GEOMETRIC_REPRESENTATION_ITEM()
RATIONAL_B_SPLINE_SURFACE(((0.998183892113821,0.99657330421516,0.996380621259469),
(0.998183892113821,0.99657330421516,0.996380621259469),(0.998183892113821,
0.99657330421516,0.996380621259469),(0.998183892113821,0.99657330421516,
0.996380621259469)))
REPRESENTATION_ITEM('')
SURFACE()
);
#366=(
BOUNDED_SURFACE()
B_SPLINE_SURFACE(1,2,((#79648,#79649,#79650),(#79651,#79652,#79653),(#79654,
#79655,#79656)),.UNSPECIFIED.,.F.,.F.,.F.)
B_SPLINE_SURFACE_WITH_KNOTS((2,1,2),(3,3),(-0.00206901892451206,0.,0.346769728493621),
(0.00660713154708297,0.0131849431293158),.UNSPECIFIED.)
GEOMETRIC_REPRESENTATION_ITEM()
RATIONAL_B_SPLINE_SURFACE(((0.997925307359477,0.997106772387136,0.996714752255955),
(0.997925307359477,0.997106772387136,0.996714752255955),(0.997925307359477,
0.997106772387136,0.996714752255955)))
REPRESENTATION_ITEM('')
SURFACE()
);
#367=(
BOUNDED_SURFACE()
B_SPLINE_SURFACE(1,2,((#79729,#79730,#79731),(#79732,#79733,#79734)),
 .UNSPECIFIED.,.F.,.F.,.F.)
B_SPLINE_SURFACE_WITH_KNOTS((2,2),(3,3),(0.,1.),(0.0556006976418427,0.0675888856590503),
 .UNSPECIFIED.)
GEOMETRIC_REPRESENTATION_ITEM()
RATIONAL_B_SPLINE_SURFACE(((0.996397562408606,0.996150386832629,0.997319912843745),
(0.996397562408606,0.996150386832629,0.997319912843745)))
REPRESENTATION_ITEM('')
SURFACE()
);
#368=(
BOUNDED_SURFACE()
B_SPLINE_SURFACE(1,2,((#79803,#79804,#79805),(#79806,#79807,#79808),(#79809,
#79810,#79811)),.UNSPECIFIED.,.F.,.F.,.F.)
B_SPLINE_SURFACE_WITH_KNOTS((2,1,2),(3,3),(0.,1.,1.01),(0.0456081671210046,
0.0575989447818824),.UNSPECIFIED.)
GEOMETRIC_REPRESENTATION_ITEM()
RATIONAL_B_SPLINE_SURFACE(((0.997793907739636,0.996365558499688,0.996354522974129),
(0.997793907739636,0.996365558499688,0.996354522974129),(0.997793907739636,
0.996365558499688,0.996354522974129)))
REPRESENTATION_ITEM('')
SURFACE()
);
#369=(
BOUNDED_SURFACE()
B_SPLINE_SURFACE(1,2,((#79846,#79847,#79848),(#79849,#79850,#79851),(#79852,
#79853,#79854)),.UNSPECIFIED.,.F.,.F.,.F.)
B_SPLINE_SURFACE_WITH_KNOTS((2,1,2),(3,3),(-0.00286810173448454,0.,0.477902879786614),
(0.0466073985929115,0.0531834929157978),.UNSPECIFIED.)
GEOMETRIC_REPRESENTATION_ITEM()
RATIONAL_B_SPLINE_SURFACE(((0.997565691989291,0.996847118055593,0.996554836292953),
(0.997565691989291,0.996847118055593,0.996554836292953),(0.997565691989291,
0.996847118055593,0.996554836292953)))
REPRESENTATION_ITEM('')
SURFACE()
);
#370=(
BOUNDED_SURFACE()
B_SPLINE_SURFACE(1,2,((#79871,#79872,#79873,#79874,#79875),(#79876,#79877,
#79878,#79879,#79880),(#79881,#79882,#79883,#79884,#79885)),
 .UNSPECIFIED.,.F.,.F.,.F.)
B_SPLINE_SURFACE_WITH_KNOTS((2,1,2),(3,2,3),(0.,1.,1.01),(0.0355931932713903,
0.0384615384615384,0.0476086899858137),.UNSPECIFIED.)
GEOMETRIC_REPRESENTATION_ITEM()
RATIONAL_B_SPLINE_SURFACE(((0.998993602249807,0.999456249886298,1.,0.998265981131401,
0.997356751596327),(0.998993602249807,0.999456249886298,1.,0.998265981131401,
0.997356751596327),(0.998993602249807,0.999456249886298,1.,0.998265981131401,
0.997356751596327)))
REPRESENTATION_ITEM('')
SURFACE()
);
#371=(
BOUNDED_SURFACE()
B_SPLINE_SURFACE(1,2,((#79933,#79934,#79935,#79936,#79937),(#79938,#79939,
#79940,#79941,#79942),(#79943,#79944,#79945,#79946,#79947)),
 .UNSPECIFIED.,.F.,.F.,.F.)
B_SPLINE_SURFACE_WITH_KNOTS((2,1,2),(3,2,3),(-0.00141401191197124,0.,0.48077029708092),
(0.0365944846645755,0.0384615384615384,0.0431859280915187),
 .UNSPECIFIED.)
GEOMETRIC_REPRESENTATION_ITEM()
RATIONAL_B_SPLINE_SURFACE(((0.999326490452259,0.999646063968217,1.,0.999104400890347,
0.9984288220563),(0.999326490452259,0.999646063968217,1.,0.999104400890347,
0.9984288220563),(0.999326490452259,0.999646063968217,1.,0.999104400890347,
0.9984288220563)))
REPRESENTATION_ITEM('')
SURFACE()
);
#372=(
BOUNDED_SURFACE()
B_SPLINE_SURFACE(1,2,((#79974,#79975,#79976),(#79977,#79978,#79979),(#79980,
#79981,#79982)),.UNSPECIFIED.,.F.,.F.,.F.)
B_SPLINE_SURFACE_WITH_KNOTS((2,1,2),(3,3),(0.,1.,1.01),(0.0255903596131801,
0.037594859669387),.UNSPECIFIED.)
GEOMETRIC_REPRESENTATION_ITEM()
RATIONAL_B_SPLINE_SURFACE(((0.996753121755999,0.997505687613148,0.999678813023853),
(0.996753121755999,0.997505687613148,0.999678813023853),(0.996753121755999,
0.997505687613148,0.999678813023853)))
REPRESENTATION_ITEM('')
SURFACE()
);
#373=(
BOUNDED_SURFACE()
B_SPLINE_SURFACE(1,2,((#80017,#80018,#80019),(#80020,#80021,#80022),(#80023,
#80024,#80025)),.UNSPECIFIED.,.F.,.F.,.F.)
B_SPLINE_SURFACE_WITH_KNOTS((2,1,2),(3,3),(-0.00286823356213617,0.,0.477902879786565),
(0.0265907346180619,0.0331702037252924),.UNSPECIFIED.)
GEOMETRIC_REPRESENTATION_ITEM()
RATIONAL_B_SPLINE_SURFACE(((0.996888414395785,0.997365765479939,0.998269846384985),
(0.996888414395785,0.997365765479939,0.998269846384985),(0.996888414395785,
0.997365765479939,0.998269846384985)))
REPRESENTATION_ITEM('')
SURFACE()
);
#374=(
BOUNDED_SURFACE()
B_SPLINE_SURFACE(1,2,((#80092,#80093,#80094),(#80095,#80096,#80097),(#80098,
#80099,#80100)),.UNSPECIFIED.,.F.,.F.,.F.)
B_SPLINE_SURFACE_WITH_KNOTS((2,1,2),(3,3),(-0.00286753128190398,0.,0.477902879786596),
(0.0166015299238956,0.0231736788111882),.UNSPECIFIED.)
GEOMETRIC_REPRESENTATION_ITEM()
RATIONAL_B_SPLINE_SURFACE(((0.996422581660833,0.996252244737342,0.996507688616404),
(0.996422581660833,0.996252244737342,0.996507688616404),(0.996422581660833,
0.996252244737342,0.996507688616404)))
REPRESENTATION_ITEM('')
SURFACE()
);
#375=(
BOUNDED_SURFACE()
B_SPLINE_SURFACE(1,2,((#80117,#80118,#80119),(#80120,#80121,#80122),(#80123,
#80124,#80125),(#80126,#80127,#80128)),.UNSPECIFIED.,.F.,.F.,.F.)
B_SPLINE_SURFACE_WITH_KNOTS((2,1,1,2),(3,3),(-0.0101,0.,1.,1.01),(0.00560769168370618,
0.0176009700440517),.UNSPECIFIED.)
GEOMETRIC_REPRESENTATION_ITEM()
RATIONAL_B_SPLINE_SURFACE(((0.99818389211382,0.99657330421516,0.996380621259469),
(0.99818389211382,0.99657330421516,0.996380621259469),(0.99818389211382,
0.99657330421516,0.996380621259469),(0.99818389211382,0.99657330421516,
0.996380621259469)))
REPRESENTATION_ITEM('')
SURFACE()
);
#376=(
BOUNDED_SURFACE()
B_SPLINE_SURFACE(1,2,((#80163,#80164,#80165),(#80166,#80167,#80168),(#80169,
#80170,#80171)),.UNSPECIFIED.,.F.,.F.,.F.)
B_SPLINE_SURFACE_WITH_KNOTS((2,1,2),(3,3),(-0.00206901892603345,0.,0.346769728494672),
(0.00660713154706902,0.013184943146953),.UNSPECIFIED.)
GEOMETRIC_REPRESENTATION_ITEM()
RATIONAL_B_SPLINE_SURFACE(((0.99792530735948,0.997106772384942,0.996714752253853),
(0.99792530735948,0.997106772384942,0.996714752253853),(0.99792530735948,
0.997106772384942,0.996714752253853)))
REPRESENTATION_ITEM('')
SURFACE()
);
#377=(
BOUNDED_SURFACE()
B_SPLINE_SURFACE(1,2,((#80244,#80245,#80246),(#80247,#80248,#80249)),
 .UNSPECIFIED.,.F.,.F.,.F.)
B_SPLINE_SURFACE_WITH_KNOTS((2,2),(3,3),(0.,1.),(0.0556006976418414,0.0675888856590506),
 .UNSPECIFIED.)
GEOMETRIC_REPRESENTATION_ITEM()
RATIONAL_B_SPLINE_SURFACE(((0.996397562408606,0.996150386832629,0.997319912843745),
(0.996397562408606,0.996150386832629,0.997319912843745)))
REPRESENTATION_ITEM('')
SURFACE()
);
#378=(
BOUNDED_SURFACE()
B_SPLINE_SURFACE(1,2,((#80318,#80319,#80320),(#80321,#80322,#80323),(#80324,
#80325,#80326)),.UNSPECIFIED.,.F.,.F.,.F.)
B_SPLINE_SURFACE_WITH_KNOTS((2,1,2),(3,3),(0.,1.,1.01),(0.0456081671210044,
0.0575989447818825),.UNSPECIFIED.)
GEOMETRIC_REPRESENTATION_ITEM()
RATIONAL_B_SPLINE_SURFACE(((0.997793907739636,0.996365558499688,0.996354522974128),
(0.997793907739636,0.996365558499688,0.996354522974128),(0.997793907739636,
0.996365558499688,0.996354522974128)))
REPRESENTATION_ITEM('')
SURFACE()
);
#379=(
BOUNDED_SURFACE()
B_SPLINE_SURFACE(1,2,((#80361,#80362,#80363),(#80364,#80365,#80366),(#80367,
#80368,#80369)),.UNSPECIFIED.,.F.,.F.,.F.)
B_SPLINE_SURFACE_WITH_KNOTS((2,1,2),(3,3),(-0.00286810173447193,0.,0.4779028797867),
(0.0466073985929119,0.0531834929157973),.UNSPECIFIED.)
GEOMETRIC_REPRESENTATION_ITEM()
RATIONAL_B_SPLINE_SURFACE(((0.997565691989291,0.996847118055594,0.996554836292953),
(0.997565691989291,0.996847118055594,0.996554836292953),(0.997565691989291,
0.996847118055594,0.996554836292953)))
REPRESENTATION_ITEM('')
SURFACE()
);
#380=(
BOUNDED_SURFACE()
B_SPLINE_SURFACE(1,2,((#80386,#80387,#80388,#80389,#80390),(#80391,#80392,
#80393,#80394,#80395),(#80396,#80397,#80398,#80399,#80400)),
 .UNSPECIFIED.,.F.,.F.,.F.)
B_SPLINE_SURFACE_WITH_KNOTS((2,1,2),(3,2,3),(0.,1.,1.01),(0.0355931932713903,
0.0384615384615384,0.0476086899858133),.UNSPECIFIED.)
GEOMETRIC_REPRESENTATION_ITEM()
RATIONAL_B_SPLINE_SURFACE(((0.998993602249807,0.999456249886298,1.,0.998265981131401,
0.997356751596327),(0.998993602249807,0.999456249886298,1.,0.998265981131401,
0.997356751596327),(0.998993602249807,0.999456249886298,1.,0.998265981131401,
0.997356751596327)))
REPRESENTATION_ITEM('')
SURFACE()
);
#381=(
BOUNDED_SURFACE()
B_SPLINE_SURFACE(1,2,((#80448,#80449,#80450,#80451,#80452),(#80453,#80454,
#80455,#80456,#80457),(#80458,#80459,#80460,#80461,#80462)),
 .UNSPECIFIED.,.F.,.F.,.F.)
B_SPLINE_SURFACE_WITH_KNOTS((2,1,2),(3,2,3),(-0.00141401191198348,0.,0.480770297080689),
(0.0365944846645759,0.0384615384615384,0.0431859280915187),
 .UNSPECIFIED.)
GEOMETRIC_REPRESENTATION_ITEM()
RATIONAL_B_SPLINE_SURFACE(((0.999326490452259,0.999646063968217,1.,0.999104400890347,
0.9984288220563),(0.999326490452259,0.999646063968217,1.,0.999104400890347,
0.9984288220563),(0.999326490452259,0.999646063968217,1.,0.999104400890347,
0.9984288220563)))
REPRESENTATION_ITEM('')
SURFACE()
);
#382=(
BOUNDED_SURFACE()
B_SPLINE_SURFACE(1,2,((#80489,#80490,#80491),(#80492,#80493,#80494),(#80495,
#80496,#80497)),.UNSPECIFIED.,.F.,.F.,.F.)
B_SPLINE_SURFACE_WITH_KNOTS((2,1,2),(3,3),(0.,1.,1.01),(0.0255903596131798,
0.0375948596693881),.UNSPECIFIED.)
GEOMETRIC_REPRESENTATION_ITEM()
RATIONAL_B_SPLINE_SURFACE(((0.996753121755999,0.997505687613148,0.999678813023854),
(0.996753121755999,0.997505687613148,0.999678813023854),(0.996753121755999,
0.997505687613148,0.999678813023854)))
REPRESENTATION_ITEM('')
SURFACE()
);
#383=(
BOUNDED_SURFACE()
B_SPLINE_SURFACE(1,2,((#80532,#80533,#80534),(#80535,#80536,#80537),(#80538,
#80539,#80540)),.UNSPECIFIED.,.F.,.F.,.F.)
B_SPLINE_SURFACE_WITH_KNOTS((2,1,2),(3,3),(-0.00286823045888591,0.,0.477902879786571),
(0.0265907346180616,0.0331702036774535),.UNSPECIFIED.)
GEOMETRIC_REPRESENTATION_ITEM()
RATIONAL_B_SPLINE_SURFACE(((0.996888414395785,0.997365765476469,0.998269846371838),
(0.996888414395785,0.997365765476469,0.998269846371838),(0.996888414395785,
0.997365765476469,0.998269846371838)))
REPRESENTATION_ITEM('')
SURFACE()
);
#384=(
BOUNDED_SURFACE()
B_SPLINE_SURFACE(1,2,((#80607,#80608,#80609),(#80610,#80611,#80612),(#80613,
#80614,#80615)),.UNSPECIFIED.,.F.,.F.,.F.)
B_SPLINE_SURFACE_WITH_KNOTS((2,1,2),(3,3),(-0.00286753128209032,0.,0.477902879786622),
(0.016601529923896,0.0231736788111887),.UNSPECIFIED.)
GEOMETRIC_REPRESENTATION_ITEM()
RATIONAL_B_SPLINE_SURFACE(((0.996422581660833,0.996252244737342,0.996507688616404),
(0.996422581660833,0.996252244737342,0.996507688616404),(0.996422581660833,
0.996252244737342,0.996507688616404)))
REPRESENTATION_ITEM('')
SURFACE()
);
#385=(
BOUNDED_SURFACE()
B_SPLINE_SURFACE(1,2,((#80632,#80633,#80634),(#80635,#80636,#80637),(#80638,
#80639,#80640),(#80641,#80642,#80643)),.UNSPECIFIED.,.F.,.F.,.F.)
B_SPLINE_SURFACE_WITH_KNOTS((2,1,1,2),(3,3),(-0.0101,0.,1.,1.01),(0.00560769168370516,
0.0176009700440517),.UNSPECIFIED.)
GEOMETRIC_REPRESENTATION_ITEM()
RATIONAL_B_SPLINE_SURFACE(((0.998183892113821,0.99657330421516,0.996380621259469),
(0.998183892113821,0.99657330421516,0.996380621259469),(0.998183892113821,
0.99657330421516,0.996380621259469),(0.998183892113821,0.99657330421516,
0.996380621259469)))
REPRESENTATION_ITEM('')
SURFACE()
);
#386=(
BOUNDED_SURFACE()
B_SPLINE_SURFACE(1,2,((#80678,#80679,#80680),(#80681,#80682,#80683),(#80684,
#80685,#80686)),.UNSPECIFIED.,.F.,.F.,.F.)
B_SPLINE_SURFACE_WITH_KNOTS((2,1,2),(3,3),(-0.00206901892596923,0.,0.346769728495858),
(0.00660713154705422,0.0131849431469467),.UNSPECIFIED.)
GEOMETRIC_REPRESENTATION_ITEM()
RATIONAL_B_SPLINE_SURFACE(((0.997925307359485,0.997106772384944,0.996714752253854),
(0.997925307359485,0.997106772384944,0.996714752253854),(0.997925307359485,
0.997106772384944,0.996714752253854)))
REPRESENTATION_ITEM('')
SURFACE()
);
#387=(
BOUNDED_SURFACE()
B_SPLINE_SURFACE(1,2,((#80759,#80760,#80761),(#80762,#80763,#80764)),
 .UNSPECIFIED.,.F.,.F.,.F.)
B_SPLINE_SURFACE_WITH_KNOTS((2,2),(3,3),(0.,1.),(0.0556006976418415,0.0675888856590506),
 .UNSPECIFIED.)
GEOMETRIC_REPRESENTATION_ITEM()
RATIONAL_B_SPLINE_SURFACE(((0.996397562408606,0.996150386832629,0.997319912843745),
(0.996397562408606,0.996150386832629,0.997319912843745)))
REPRESENTATION_ITEM('')
SURFACE()
);
#388=(
BOUNDED_SURFACE()
B_SPLINE_SURFACE(1,2,((#80833,#80834,#80835),(#80836,#80837,#80838),(#80839,
#80840,#80841)),.UNSPECIFIED.,.F.,.F.,.F.)
B_SPLINE_SURFACE_WITH_KNOTS((2,1,2),(3,3),(0.,1.,1.01),(0.0456081671210032,
0.0575989447818814),.UNSPECIFIED.)
GEOMETRIC_REPRESENTATION_ITEM()
RATIONAL_B_SPLINE_SURFACE(((0.997793907739636,0.996365558499688,0.996354522974128),
(0.997793907739636,0.996365558499688,0.996354522974128),(0.997793907739636,
0.996365558499688,0.996354522974128)))
REPRESENTATION_ITEM('')
SURFACE()
);
#389=(
BOUNDED_SURFACE()
B_SPLINE_SURFACE(1,2,((#80876,#80877,#80878),(#80879,#80880,#80881),(#80882,
#80883,#80884)),.UNSPECIFIED.,.F.,.F.,.F.)
B_SPLINE_SURFACE_WITH_KNOTS((2,1,2),(3,3),(-0.00286810173442196,0.,0.477902879786453),
(0.0466073985929114,0.0531834929157971),.UNSPECIFIED.)
GEOMETRIC_REPRESENTATION_ITEM()
RATIONAL_B_SPLINE_SURFACE(((0.997565691989291,0.996847118055594,0.996554836292953),
(0.997565691989291,0.996847118055594,0.996554836292953),(0.997565691989291,
0.996847118055594,0.996554836292953)))
REPRESENTATION_ITEM('')
SURFACE()
);
#390=(
BOUNDED_SURFACE()
B_SPLINE_SURFACE(1,2,((#80901,#80902,#80903,#80904,#80905),(#80906,#80907,
#80908,#80909,#80910),(#80911,#80912,#80913,#80914,#80915)),
 .UNSPECIFIED.,.F.,.F.,.F.)
B_SPLINE_SURFACE_WITH_KNOTS((2,1,2),(3,2,3),(0.,1.,1.01),(0.0355931932713903,
0.0384615384615384,0.0476086899858133),.UNSPECIFIED.)
GEOMETRIC_REPRESENTATION_ITEM()
RATIONAL_B_SPLINE_SURFACE(((0.998993602249807,0.999456249886298,1.,0.998265981131401,
0.997356751596327),(0.998993602249807,0.999456249886298,1.,0.998265981131401,
0.997356751596327),(0.998993602249807,0.999456249886298,1.,0.998265981131401,
0.997356751596327)))
REPRESENTATION_ITEM('')
SURFACE()
);
#391=(
BOUNDED_SURFACE()
B_SPLINE_SURFACE(1,2,((#80963,#80964,#80965,#80966,#80967),(#80968,#80969,
#80970,#80971,#80972),(#80973,#80974,#80975,#80976,#80977)),
 .UNSPECIFIED.,.F.,.F.,.F.)
B_SPLINE_SURFACE_WITH_KNOTS((2,1,2),(3,2,3),(-0.0014140119119804,0.,0.480770297080892),
(0.0365944846645756,0.0384615384615384,0.0431859280915182),
 .UNSPECIFIED.)
GEOMETRIC_REPRESENTATION_ITEM()
RATIONAL_B_SPLINE_SURFACE(((0.999326490452258,0.999646063968217,1.,0.999104400890347,
0.9984288220563),(0.999326490452258,0.999646063968217,1.,0.999104400890347,
0.9984288220563),(0.999326490452258,0.999646063968217,1.,0.999104400890347,
0.9984288220563)))
REPRESENTATION_ITEM('')
SURFACE()
);
#392=(
BOUNDED_SURFACE()
B_SPLINE_SURFACE(1,2,((#81004,#81005,#81006),(#81007,#81008,#81009),(#81010,
#81011,#81012)),.UNSPECIFIED.,.F.,.F.,.F.)
B_SPLINE_SURFACE_WITH_KNOTS((2,1,2),(3,3),(0.,1.,1.01),(0.0255903596131789,
0.0375948596693871),.UNSPECIFIED.)
GEOMETRIC_REPRESENTATION_ITEM()
RATIONAL_B_SPLINE_SURFACE(((0.996753121755999,0.997505687613148,0.999678813023853),
(0.996753121755999,0.997505687613148,0.999678813023853),(0.996753121755999,
0.997505687613148,0.999678813023853)))
REPRESENTATION_ITEM('')
SURFACE()
);
#393=(
BOUNDED_SURFACE()
B_SPLINE_SURFACE(1,2,((#81047,#81048,#81049),(#81050,#81051,#81052),(#81053,
#81054,#81055)),.UNSPECIFIED.,.F.,.F.,.F.)
B_SPLINE_SURFACE_WITH_KNOTS((2,1,2),(3,3),(-0.00286823356211971,0.,0.477902879786608),
(0.0265907346180618,0.0331702037252924),.UNSPECIFIED.)
GEOMETRIC_REPRESENTATION_ITEM()
RATIONAL_B_SPLINE_SURFACE(((0.996888414395785,0.997365765479939,0.998269846384985),
(0.996888414395785,0.997365765479939,0.998269846384985),(0.996888414395785,
0.997365765479939,0.998269846384985)))
REPRESENTATION_ITEM('')
SURFACE()
);
#394=(
BOUNDED_SURFACE()
B_SPLINE_SURFACE(1,2,((#81122,#81123,#81124),(#81125,#81126,#81127),(#81128,
#81129,#81130)),.UNSPECIFIED.,.F.,.F.,.F.)
B_SPLINE_SURFACE_WITH_KNOTS((2,1,2),(3,3),(-0.00286753128194112,0.,0.477902879786505),
(0.0166015299238958,0.0231736788111885),.UNSPECIFIED.)
GEOMETRIC_REPRESENTATION_ITEM()
RATIONAL_B_SPLINE_SURFACE(((0.996422581660833,0.996252244737342,0.996507688616404),
(0.996422581660833,0.996252244737342,0.996507688616404),(0.996422581660833,
0.996252244737342,0.996507688616404)))
REPRESENTATION_ITEM('')
SURFACE()
);
#395=(
BOUNDED_SURFACE()
B_SPLINE_SURFACE(1,2,((#81147,#81148,#81149),(#81150,#81151,#81152),(#81153,
#81154,#81155),(#81156,#81157,#81158)),.UNSPECIFIED.,.F.,.F.,.F.)
B_SPLINE_SURFACE_WITH_KNOTS((2,1,1,2),(3,3),(-0.0101,0.,1.,1.01),(0.00560769168370521,
0.0176009700440511),.UNSPECIFIED.)
GEOMETRIC_REPRESENTATION_ITEM()
RATIONAL_B_SPLINE_SURFACE(((0.998183892113821,0.99657330421516,0.996380621259469),
(0.998183892113821,0.99657330421516,0.996380621259469),(0.998183892113821,
0.99657330421516,0.996380621259469),(0.998183892113821,0.99657330421516,
0.996380621259469)))
REPRESENTATION_ITEM('')
SURFACE()
);
#396=(
BOUNDED_SURFACE()
B_SPLINE_SURFACE(1,2,((#81193,#81194,#81195),(#81196,#81197,#81198),(#81199,
#81200,#81201)),.UNSPECIFIED.,.F.,.F.,.F.)
B_SPLINE_SURFACE_WITH_KNOTS((2,1,2),(3,3),(-0.00206901892602457,0.,0.346769728497025),
(0.00660713154704112,0.0131849431469406),.UNSPECIFIED.)
GEOMETRIC_REPRESENTATION_ITEM()
RATIONAL_B_SPLINE_SURFACE(((0.997925307359487,0.997106772384945,0.996714752253855),
(0.997925307359487,0.997106772384945,0.996714752253855),(0.997925307359487,
0.997106772384945,0.996714752253855)))
REPRESENTATION_ITEM('')
SURFACE()
);
#397=(
BOUNDED_SURFACE()
B_SPLINE_SURFACE(1,2,((#81274,#81275,#81276),(#81277,#81278,#81279)),
 .UNSPECIFIED.,.F.,.F.,.F.)
B_SPLINE_SURFACE_WITH_KNOTS((2,2),(3,3),(0.,1.),(0.0556006976418426,0.067588885659051),
 .UNSPECIFIED.)
GEOMETRIC_REPRESENTATION_ITEM()
RATIONAL_B_SPLINE_SURFACE(((0.996397562408606,0.996150386832629,0.997319912843745),
(0.996397562408606,0.996150386832629,0.997319912843745)))
REPRESENTATION_ITEM('')
SURFACE()
);
#398=(
BOUNDED_SURFACE()
B_SPLINE_SURFACE(1,2,((#81348,#81349,#81350),(#81351,#81352,#81353)),
 .UNSPECIFIED.,.F.,.F.,.F.)
B_SPLINE_SURFACE_WITH_KNOTS((2,2),(3,3),(0.,1.),(0.0456081671210033,0.0575989447818814),
 .UNSPECIFIED.)
GEOMETRIC_REPRESENTATION_ITEM()
RATIONAL_B_SPLINE_SURFACE(((0.997793907739636,0.996365558499688,0.996354522974128),
(0.997793907739636,0.996365558499688,0.996354522974128)))
REPRESENTATION_ITEM('')
SURFACE()
);
#399=(
BOUNDED_SURFACE()
B_SPLINE_SURFACE(1,2,((#81420,#81421,#81422,#81423,#81424),(#81425,#81426,
#81427,#81428,#81429),(#81430,#81431,#81432,#81433,#81434)),
 .UNSPECIFIED.,.F.,.F.,.F.)
B_SPLINE_SURFACE_WITH_KNOTS((2,1,2),(3,2,3),(0.,1.,1.01),(0.0355931932713904,
0.0384615384615384,0.0476086899858126),.UNSPECIFIED.)
GEOMETRIC_REPRESENTATION_ITEM()
RATIONAL_B_SPLINE_SURFACE(((0.998993602249807,0.999456249886298,1.,0.998265981131401,
0.997356751596327),(0.998993602249807,0.999456249886298,1.,0.998265981131401,
0.997356751596327),(0.998993602249807,0.999456249886298,1.,0.998265981131401,
0.997356751596327)))
REPRESENTATION_ITEM('')
SURFACE()
);
#400=(
BOUNDED_SURFACE()
B_SPLINE_SURFACE(1,2,((#81482,#81483,#81484,#81485,#81486),(#81487,#81488,
#81489,#81490,#81491),(#81492,#81493,#81494,#81495,#81496)),
 .UNSPECIFIED.,.F.,.F.,.F.)
B_SPLINE_SURFACE_WITH_KNOTS((2,1,2),(3,2,3),(-0.00141401191198374,0.,0.480770297080743),
(0.0365944846645755,0.0384615384615384,0.0431859280915181),
 .UNSPECIFIED.)
GEOMETRIC_REPRESENTATION_ITEM()
RATIONAL_B_SPLINE_SURFACE(((0.999326490452259,0.999646063968217,1.,0.999104400890347,
0.9984288220563),(0.999326490452258,0.999646063968217,1.,0.999104400890347,
0.9984288220563),(0.999326490452258,0.999646063968217,1.,0.999104400890347,
0.9984288220563)))
REPRESENTATION_ITEM('')
SURFACE()
);
#401=(
BOUNDED_SURFACE()
B_SPLINE_SURFACE(1,2,((#81523,#81524,#81525),(#81526,#81527,#81528),(#81529,
#81530,#81531)),.UNSPECIFIED.,.F.,.F.,.F.)
B_SPLINE_SURFACE_WITH_KNOTS((2,1,2),(3,3),(0.,1.,1.01),(0.0255903596131787,
0.0375948596693867),.UNSPECIFIED.)
GEOMETRIC_REPRESENTATION_ITEM()
RATIONAL_B_SPLINE_SURFACE(((0.996753121755999,0.997505687613147,0.999678813023853),
(0.996753121755999,0.997505687613147,0.999678813023853),(0.996753121755999,
0.997505687613147,0.999678813023853)))
REPRESENTATION_ITEM('')
SURFACE()
);
#402=(
BOUNDED_SURFACE()
B_SPLINE_SURFACE(1,2,((#81566,#81567,#81568),(#81569,#81570,#81571),(#81572,
#81573,#81574)),.UNSPECIFIED.,.F.,.F.,.F.)
B_SPLINE_SURFACE_WITH_KNOTS((2,1,2),(3,3),(-0.00286823356207599,0.,0.477902879786576),
(0.0265907346180618,0.0331702037252926),.UNSPECIFIED.)
GEOMETRIC_REPRESENTATION_ITEM()
RATIONAL_B_SPLINE_SURFACE(((0.996888414395785,0.997365765479939,0.998269846384985),
(0.996888414395785,0.997365765479939,0.998269846384985),(0.996888414395785,
0.997365765479939,0.998269846384985)))
REPRESENTATION_ITEM('')
SURFACE()
);
#403=(
BOUNDED_SURFACE()
B_SPLINE_SURFACE(1,2,((#81641,#81642,#81643),(#81644,#81645,#81646),(#81647,
#81648,#81649)),.UNSPECIFIED.,.F.,.F.,.F.)
B_SPLINE_SURFACE_WITH_KNOTS((2,1,2),(3,3),(-0.00286753074348226,0.,0.477902879786661),
(0.0166015299238961,0.0231736788028833),.UNSPECIFIED.)
GEOMETRIC_REPRESENTATION_ITEM()
RATIONAL_B_SPLINE_SURFACE(((0.996422581660833,0.996252244737557,0.996507688615759),
(0.996422581660833,0.996252244737557,0.996507688615759),(0.996422581660833,
0.996252244737557,0.996507688615759)))
REPRESENTATION_ITEM('')
SURFACE()
);
#404=(
BOUNDED_SURFACE()
B_SPLINE_SURFACE(1,2,((#81666,#81667,#81668),(#81669,#81670,#81671),(#81672,
#81673,#81674),(#81675,#81676,#81677)),.UNSPECIFIED.,.F.,.F.,.F.)
B_SPLINE_SURFACE_WITH_KNOTS((2,1,1,2),(3,3),(-0.0101,0.,1.,1.01),(0.0056076916837051,
0.0176009700440511),.UNSPECIFIED.)
GEOMETRIC_REPRESENTATION_ITEM()
RATIONAL_B_SPLINE_SURFACE(((0.998183892113821,0.99657330421516,0.996380621259469),
(0.998183892113821,0.99657330421516,0.996380621259469),(0.998183892113821,
0.99657330421516,0.996380621259469),(0.998183892113821,0.99657330421516,
0.996380621259469)))
REPRESENTATION_ITEM('')
SURFACE()
);
#405=(
BOUNDED_SURFACE()
B_SPLINE_SURFACE(1,2,((#81712,#81713,#81714),(#81715,#81716,#81717),(#81718,
#81719,#81720)),.UNSPECIFIED.,.F.,.F.,.F.)
B_SPLINE_SURFACE_WITH_KNOTS((2,1,2),(3,3),(-0.0020690189259847,0.,0.346769728498705),
(0.00660713154702827,0.0131849431469338),.UNSPECIFIED.)
GEOMETRIC_REPRESENTATION_ITEM()
RATIONAL_B_SPLINE_SURFACE(((0.997925307359491,0.997106772384947,0.996714752253855),
(0.997925307359491,0.997106772384947,0.996714752253855),(0.997925307359491,
0.997106772384947,0.996714752253855)))
REPRESENTATION_ITEM('')
SURFACE()
);
#406=(
BOUNDED_SURFACE()
B_SPLINE_SURFACE(1,2,((#81793,#81794,#81795),(#81796,#81797,#81798)),
 .UNSPECIFIED.,.F.,.F.,.F.)
B_SPLINE_SURFACE_WITH_KNOTS((2,2),(3,3),(0.,1.),(0.0556006976418394,0.0675888856590496),
 .UNSPECIFIED.)
GEOMETRIC_REPRESENTATION_ITEM()
RATIONAL_B_SPLINE_SURFACE(((0.996397562408606,0.996150386832629,0.997319912843745),
(0.996397562408606,0.996150386832629,0.997319912843745)))
REPRESENTATION_ITEM('')
SURFACE()
);
#407=(
BOUNDED_SURFACE()
B_SPLINE_SURFACE(1,2,((#81867,#81868,#81869),(#81870,#81871,#81872),(#81873,
#81874,#81875)),.UNSPECIFIED.,.F.,.F.,.F.)
B_SPLINE_SURFACE_WITH_KNOTS((2,1,2),(3,3),(0.,1.,1.01),(0.0456081671210036,
0.0575989447818819),.UNSPECIFIED.)
GEOMETRIC_REPRESENTATION_ITEM()
RATIONAL_B_SPLINE_SURFACE(((0.997793907739636,0.996365558499688,0.996354522974128),
(0.997793907739636,0.996365558499688,0.996354522974128),(0.997793907739636,
0.996365558499688,0.996354522974128)))
REPRESENTATION_ITEM('')
SURFACE()
);
#408=(
BOUNDED_SURFACE()
B_SPLINE_SURFACE(1,2,((#81910,#81911,#81912),(#81913,#81914,#81915),(#81916,
#81917,#81918)),.UNSPECIFIED.,.F.,.F.,.F.)
B_SPLINE_SURFACE_WITH_KNOTS((2,1,2),(3,3),(-0.00286810173449685,0.,0.477902879786636),
(0.0466073985929117,0.0531834929157983),.UNSPECIFIED.)
GEOMETRIC_REPRESENTATION_ITEM()
RATIONAL_B_SPLINE_SURFACE(((0.997565691989291,0.996847118055593,0.996554836292953),
(0.997565691989291,0.996847118055593,0.996554836292953),(0.997565691989291,
0.996847118055593,0.996554836292953)))
REPRESENTATION_ITEM('')
SURFACE()
);
#409=(
BOUNDED_SURFACE()
B_SPLINE_SURFACE(1,2,((#81996,#81997,#81998,#81999,#82000),(#82001,#82002,
#82003,#82004,#82005)),.UNSPECIFIED.,.F.,.F.,.F.)
B_SPLINE_SURFACE_WITH_KNOTS((2,2),(3,2,3),(0.,0.480770297080763),(0.0365944846645756,
0.0384615384615384,0.0431859280915182),.UNSPECIFIED.)
GEOMETRIC_REPRESENTATION_ITEM()
RATIONAL_B_SPLINE_SURFACE(((0.999326490452258,0.999646063968217,1.,0.999104400890347,
0.9984288220563),(0.999326490452258,0.999646063968217,1.,0.999104400890347,
0.9984288220563)))
REPRESENTATION_ITEM('')
SURFACE()
);
#410=(
BOUNDED_SURFACE()
B_SPLINE_SURFACE(1,2,((#82032,#82033,#82034),(#82035,#82036,#82037),(#82038,
#82039,#82040)),.UNSPECIFIED.,.F.,.F.,.F.)
B_SPLINE_SURFACE_WITH_KNOTS((2,1,2),(3,3),(0.,1.,1.01),(0.0255903596131788,
0.0375948596693871),.UNSPECIFIED.)
GEOMETRIC_REPRESENTATION_ITEM()
RATIONAL_B_SPLINE_SURFACE(((0.996753121755999,0.997505687613148,0.999678813023853),
(0.996753121755999,0.997505687613148,0.999678813023853),(0.996753121755999,
0.997505687613148,0.999678813023853)))
REPRESENTATION_ITEM('')
SURFACE()
);
#411=(
BOUNDED_SURFACE()
B_SPLINE_SURFACE(1,2,((#82075,#82076,#82077),(#82078,#82079,#82080),(#82081,
#82082,#82083)),.UNSPECIFIED.,.F.,.F.,.F.)
B_SPLINE_SURFACE_WITH_KNOTS((2,1,2),(3,3),(-0.00286823356213975,0.,0.47790287978654),
(0.0265907346180619,0.0331702037252932),.UNSPECIFIED.)
GEOMETRIC_REPRESENTATION_ITEM()
RATIONAL_B_SPLINE_SURFACE(((0.996888414395785,0.997365765479939,0.998269846384986),
(0.996888414395785,0.997365765479939,0.998269846384986),(0.996888414395785,
0.997365765479939,0.998269846384986)))
REPRESENTATION_ITEM('')
SURFACE()
);
#412=(
BOUNDED_SURFACE()
B_SPLINE_SURFACE(1,2,((#82150,#82151,#82152),(#82153,#82154,#82155),(#82156,
#82157,#82158)),.UNSPECIFIED.,.F.,.F.,.F.)
B_SPLINE_SURFACE_WITH_KNOTS((2,1,2),(3,3),(-0.00286753128198799,0.,0.477902879786589),
(0.0166015299238963,0.023173678811189),.UNSPECIFIED.)
GEOMETRIC_REPRESENTATION_ITEM()
RATIONAL_B_SPLINE_SURFACE(((0.996422581660833,0.996252244737342,0.996507688616404),
(0.996422581660833,0.996252244737342,0.996507688616404),(0.996422581660833,
0.996252244737342,0.996507688616404)))
REPRESENTATION_ITEM('')
SURFACE()
);
#413=(
BOUNDED_SURFACE()
B_SPLINE_SURFACE(1,2,((#82175,#82176,#82177),(#82178,#82179,#82180),(#82181,
#82182,#82183),(#82184,#82185,#82186)),.UNSPECIFIED.,.F.,.F.,.F.)
B_SPLINE_SURFACE_WITH_KNOTS((2,1,1,2),(3,3),(-0.0101,0.,1.,1.01),(0.00560769168370525,
0.0176009700440511),.UNSPECIFIED.)
GEOMETRIC_REPRESENTATION_ITEM()
RATIONAL_B_SPLINE_SURFACE(((0.99818389211382,0.99657330421516,0.996380621259469),
(0.99818389211382,0.99657330421516,0.996380621259469),(0.99818389211382,
0.99657330421516,0.996380621259469),(0.99818389211382,0.99657330421516,
0.996380621259469)))
REPRESENTATION_ITEM('')
SURFACE()
);
#414=(
BOUNDED_SURFACE()
B_SPLINE_SURFACE(1,2,((#82221,#82222,#82223),(#82224,#82225,#82226),(#82227,
#82228,#82229)),.UNSPECIFIED.,.F.,.F.,.F.)
B_SPLINE_SURFACE_WITH_KNOTS((2,1,2),(3,3),(-0.00206901892598934,0.,0.346769728500098),
(0.00660713154701696,0.0131849431469243),.UNSPECIFIED.)
GEOMETRIC_REPRESENTATION_ITEM()
RATIONAL_B_SPLINE_SURFACE(((0.997925307359493,0.997106772384949,0.996714752253856),
(0.997925307359493,0.997106772384949,0.996714752253856),(0.997925307359494,
0.997106772384949,0.996714752253856)))
REPRESENTATION_ITEM('')
SURFACE()
);
#415=(
BOUNDED_SURFACE()
B_SPLINE_SURFACE(1,2,((#82302,#82303,#82304),(#82305,#82306,#82307)),
 .UNSPECIFIED.,.F.,.F.,.F.)
B_SPLINE_SURFACE_WITH_KNOTS((2,2),(3,3),(0.,1.),(0.0556006976418415,0.0675888856590506),
 .UNSPECIFIED.)
GEOMETRIC_REPRESENTATION_ITEM()
RATIONAL_B_SPLINE_SURFACE(((0.996397562408606,0.996150386832629,0.997319912843745),
(0.996397562408606,0.996150386832629,0.997319912843745)))
REPRESENTATION_ITEM('')
SURFACE()
);
#416=(
BOUNDED_SURFACE()
B_SPLINE_SURFACE(1,2,((#82376,#82377,#82378),(#82379,#82380,#82381),(#82382,
#82383,#82384)),.UNSPECIFIED.,.F.,.F.,.F.)
B_SPLINE_SURFACE_WITH_KNOTS((2,1,2),(3,3),(0.,1.,1.01),(0.0456081671210023,
0.057598944781881),.UNSPECIFIED.)
GEOMETRIC_REPRESENTATION_ITEM()
RATIONAL_B_SPLINE_SURFACE(((0.997793907739637,0.996365558499688,0.996354522974128),
(0.997793907739637,0.996365558499688,0.996354522974128),(0.997793907739637,
0.996365558499688,0.996354522974128)))
REPRESENTATION_ITEM('')
SURFACE()
);
#417=(
BOUNDED_SURFACE()
B_SPLINE_SURFACE(1,2,((#82419,#82420,#82421),(#82422,#82423,#82424),(#82425,
#82426,#82427)),.UNSPECIFIED.,.F.,.F.,.F.)
B_SPLINE_SURFACE_WITH_KNOTS((2,1,2),(3,3),(-0.00286810173498889,0.,0.477902879865112),
(0.0466073985929115,0.0531834929157973),.UNSPECIFIED.)
GEOMETRIC_REPRESENTATION_ITEM()
RATIONAL_B_SPLINE_SURFACE(((0.997565691989291,0.996847118055594,0.996554836292953),
(0.997565691989291,0.996847118055594,0.996554836292953),(0.997565691989291,
0.996847118055593,0.996554836292953)))
REPRESENTATION_ITEM('')
SURFACE()
);
#418=(
BOUNDED_SURFACE()
B_SPLINE_SURFACE(1,2,((#82444,#82445,#82446,#82447,#82448),(#82449,#82450,
#82451,#82452,#82453),(#82454,#82455,#82456,#82457,#82458)),
 .UNSPECIFIED.,.F.,.F.,.F.)
B_SPLINE_SURFACE_WITH_KNOTS((2,1,2),(3,2,3),(0.,1.,1.01),(0.0355931932713904,
0.0384615384615384,0.0476086899858127),.UNSPECIFIED.)
GEOMETRIC_REPRESENTATION_ITEM()
RATIONAL_B_SPLINE_SURFACE(((0.998993602249807,0.999456249886298,1.,0.998265981131401,
0.997356751596327),(0.998993602249807,0.999456249886298,1.,0.998265981131401,
0.997356751596327),(0.998993602249807,0.999456249886298,1.,0.998265981131401,
0.997356751596327)))
REPRESENTATION_ITEM('')
SURFACE()
);
#419=(
BOUNDED_SURFACE()
B_SPLINE_SURFACE(1,2,((#82506,#82507,#82508,#82509,#82510),(#82511,#82512,
#82513,#82514,#82515),(#82516,#82517,#82518,#82519,#82520)),
 .UNSPECIFIED.,.F.,.F.,.F.)
B_SPLINE_SURFACE_WITH_KNOTS((2,1,2),(3,2,3),(-0.00141401191196798,0.,0.480770297080667),
(0.0365944846645755,0.0384615384615384,0.0431859280915186),
 .UNSPECIFIED.)
GEOMETRIC_REPRESENTATION_ITEM()
RATIONAL_B_SPLINE_SURFACE(((0.999326490452258,0.999646063968217,1.,0.999104400890347,
0.9984288220563),(0.999326490452259,0.999646063968217,1.,0.999104400890347,
0.9984288220563),(0.999326490452259,0.999646063968217,1.,0.999104400890347,
0.9984288220563)))
REPRESENTATION_ITEM('')
SURFACE()
);
#420=(
BOUNDED_SURFACE()
B_SPLINE_SURFACE(1,2,((#82547,#82548,#82549),(#82550,#82551,#82552)),
 .UNSPECIFIED.,.F.,.F.,.F.)
B_SPLINE_SURFACE_WITH_KNOTS((2,2),(3,3),(0.,1.),(0.0255903596131801,0.0375948596693865),
 .UNSPECIFIED.)
GEOMETRIC_REPRESENTATION_ITEM()
RATIONAL_B_SPLINE_SURFACE(((0.996753121755999,0.997505687613148,0.999678813023853),
(0.996753121755999,0.997505687613148,0.999678813023853)))
REPRESENTATION_ITEM('')
SURFACE()
);
#421=(
BOUNDED_SURFACE()
B_SPLINE_SURFACE(1,2,((#82669,#82670,#82671),(#82672,#82673,#82674),(#82675,
#82676,#82677)),.UNSPECIFIED.,.F.,.F.,.F.)
B_SPLINE_SURFACE_WITH_KNOTS((2,1,2),(3,3),(-0.00286753074352407,0.,0.477902879786511),
(0.0166015299238963,0.0231736788028833),.UNSPECIFIED.)
GEOMETRIC_REPRESENTATION_ITEM()
RATIONAL_B_SPLINE_SURFACE(((0.996422581660833,0.996252244737557,0.996507688615759),
(0.996422581660833,0.996252244737557,0.996507688615759),(0.996422581660833,
0.996252244737557,0.996507688615759)))
REPRESENTATION_ITEM('')
SURFACE()
);
#422=(
BOUNDED_SURFACE()
B_SPLINE_SURFACE(1,2,((#82694,#82695,#82696),(#82697,#82698,#82699),(#82700,
#82701,#82702),(#82703,#82704,#82705)),.UNSPECIFIED.,.F.,.F.,.F.)
B_SPLINE_SURFACE_WITH_KNOTS((2,1,1,2),(3,3),(-0.0101,0.,1.,1.01),(0.00560769168370406,
0.0176009700440506),.UNSPECIFIED.)
GEOMETRIC_REPRESENTATION_ITEM()
RATIONAL_B_SPLINE_SURFACE(((0.998183892113821,0.99657330421516,0.996380621259469),
(0.998183892113821,0.99657330421516,0.996380621259469),(0.998183892113821,
0.99657330421516,0.996380621259469),(0.998183892113821,0.99657330421516,
0.996380621259469)))
REPRESENTATION_ITEM('')
SURFACE()
);
#423=(
BOUNDED_SURFACE()
B_SPLINE_SURFACE(1,2,((#82740,#82741,#82742),(#82743,#82744,#82745),(#82746,
#82747,#82748)),.UNSPECIFIED.,.F.,.F.,.F.)
B_SPLINE_SURFACE_WITH_KNOTS((2,1,2),(3,3),(-0.00206901892599668,0.,0.346769728501626),
(0.0066071315470067,0.013184943146863),.UNSPECIFIED.)
GEOMETRIC_REPRESENTATION_ITEM()
RATIONAL_B_SPLINE_SURFACE(((0.997925307359496,0.997106772384957,0.996714752253863),
(0.997925307359496,0.997106772384957,0.996714752253863),(0.997925307359496,
0.997106772384957,0.996714752253863)))
REPRESENTATION_ITEM('')
SURFACE()
);
#424=(
BOUNDED_SURFACE()
B_SPLINE_SURFACE(1,2,((#82821,#82822,#82823),(#82824,#82825,#82826)),
 .UNSPECIFIED.,.F.,.F.,.F.)
B_SPLINE_SURFACE_WITH_KNOTS((2,2),(3,3),(0.,1.),(0.0556006976418438,0.0675888856590503),
 .UNSPECIFIED.)
GEOMETRIC_REPRESENTATION_ITEM()
RATIONAL_B_SPLINE_SURFACE(((0.996397562408606,0.996150386832629,0.997319912843745),
(0.996397562408606,0.996150386832629,0.997319912843745)))
REPRESENTATION_ITEM('')
SURFACE()
);
#425=(
BOUNDED_SURFACE()
B_SPLINE_SURFACE(1,2,((#82895,#82896,#82897),(#82898,#82899,#82900),(#82901,
#82902,#82903)),.UNSPECIFIED.,.F.,.F.,.F.)
B_SPLINE_SURFACE_WITH_KNOTS((2,1,2),(3,3),(0.,1.,1.01),(0.0456081671210055,
0.0575989447818814),.UNSPECIFIED.)
GEOMETRIC_REPRESENTATION_ITEM()
RATIONAL_B_SPLINE_SURFACE(((0.997793907739636,0.996365558499688,0.996354522974128),
(0.997793907739636,0.996365558499688,0.996354522974128),(0.997793907739636,
0.996365558499688,0.996354522974128)))
REPRESENTATION_ITEM('')
SURFACE()
);
#426=(
BOUNDED_SURFACE()
B_SPLINE_SURFACE(1,2,((#82938,#82939,#82940),(#82941,#82942,#82943),(#82944,
#82945,#82946)),.UNSPECIFIED.,.F.,.F.,.F.)
B_SPLINE_SURFACE_WITH_KNOTS((2,1,2),(3,3),(-0.00286810173450747,0.,0.477902879789481),
(0.046607398592912,0.0531834929157981),.UNSPECIFIED.)
GEOMETRIC_REPRESENTATION_ITEM()
RATIONAL_B_SPLINE_SURFACE(((0.997565691989291,0.996847118055593,0.996554836292953),
(0.997565691989291,0.996847118055593,0.996554836292953),(0.997565691989291,
0.996847118055593,0.996554836292953)))
REPRESENTATION_ITEM('')
SURFACE()
);
#427=(
BOUNDED_SURFACE()
B_SPLINE_SURFACE(1,2,((#82963,#82964,#82965,#82966,#82967),(#82968,#82969,
#82970,#82971,#82972),(#82973,#82974,#82975,#82976,#82977)),
 .UNSPECIFIED.,.F.,.F.,.F.)
B_SPLINE_SURFACE_WITH_KNOTS((2,1,2),(3,2,3),(0.,1.,1.01),(0.0355931932713904,
0.0384615384615384,0.0476086899858121),.UNSPECIFIED.)
GEOMETRIC_REPRESENTATION_ITEM()
RATIONAL_B_SPLINE_SURFACE(((0.998993602249807,0.999456249886298,1.,0.998265981131401,
0.997356751596327),(0.998993602249807,0.999456249886298,1.,0.998265981131401,
0.997356751596327),(0.998993602249807,0.999456249886298,1.,0.998265981131401,
0.997356751596327)))
REPRESENTATION_ITEM('')
SURFACE()
);
#428=(
BOUNDED_SURFACE()
B_SPLINE_SURFACE(1,2,((#83025,#83026,#83027,#83028,#83029),(#83030,#83031,
#83032,#83033,#83034),(#83035,#83036,#83037,#83038,#83039)),
 .UNSPECIFIED.,.F.,.F.,.F.)
B_SPLINE_SURFACE_WITH_KNOTS((2,1,2),(3,2,3),(-0.00141401191198176,0.,0.480770297081945),
(0.0365944846645797,0.0384615384615384,0.0431859280915184),
 .UNSPECIFIED.)
GEOMETRIC_REPRESENTATION_ITEM()
RATIONAL_B_SPLINE_SURFACE(((0.99932649045226,0.999646063968218,1.,0.999104400890347,
0.9984288220563),(0.99932649045226,0.999646063968218,1.,0.999104400890347,
0.9984288220563),(0.99932649045226,0.999646063968218,1.,0.999104400890347,
0.9984288220563)))
REPRESENTATION_ITEM('')
SURFACE()
);
#429=(
BOUNDED_SURFACE()
B_SPLINE_SURFACE(1,2,((#83066,#83067,#83068),(#83069,#83070,#83071),(#83072,
#83073,#83074)),.UNSPECIFIED.,.F.,.F.,.F.)
B_SPLINE_SURFACE_WITH_KNOTS((2,1,2),(3,3),(0.,1.,1.01),(0.0255903596131819,
0.0375948596693879),.UNSPECIFIED.)
GEOMETRIC_REPRESENTATION_ITEM()
RATIONAL_B_SPLINE_SURFACE(((0.996753121755999,0.997505687613148,0.999678813023854),
(0.996753121755999,0.997505687613148,0.999678813023854),(0.996753121755999,
0.997505687613148,0.999678813023854)))
REPRESENTATION_ITEM('')
SURFACE()
);
#430=(
BOUNDED_SURFACE()
B_SPLINE_SURFACE(1,2,((#83109,#83110,#83111),(#83112,#83113,#83114),(#83115,
#83116,#83117)),.UNSPECIFIED.,.F.,.F.,.F.)
B_SPLINE_SURFACE_WITH_KNOTS((2,1,2),(3,3),(-0.00286823356200407,0.,0.477902879786893),
(0.0265907346180622,0.033170203725293),.UNSPECIFIED.)
GEOMETRIC_REPRESENTATION_ITEM()
RATIONAL_B_SPLINE_SURFACE(((0.996888414395785,0.997365765479939,0.998269846384985),
(0.996888414395785,0.997365765479939,0.998269846384985),(0.996888414395785,
0.997365765479939,0.998269846384985)))
REPRESENTATION_ITEM('')
SURFACE()
);
#431=(
BOUNDED_SURFACE()
B_SPLINE_SURFACE(1,2,((#83216,#83217,#83218),(#83219,#83220,#83221),(#83222,
#83223,#83224),(#83225,#83226,#83227)),.UNSPECIFIED.,.F.,.F.,.F.)
B_SPLINE_SURFACE_WITH_KNOTS((2,1,1,2),(3,3),(-0.0101,0.,1.,1.01),(0.00560769168370728,
0.0176009700440516),.UNSPECIFIED.)
GEOMETRIC_REPRESENTATION_ITEM()
RATIONAL_B_SPLINE_SURFACE(((0.99818389211382,0.99657330421516,0.996380621259469),
(0.99818389211382,0.99657330421516,0.996380621259469),(0.99818389211382,
0.99657330421516,0.996380621259469),(0.99818389211382,0.99657330421516,
0.996380621259469)))
REPRESENTATION_ITEM('')
SURFACE()
);
#432=(
BOUNDED_SURFACE()
B_SPLINE_SURFACE(1,2,((#83262,#83263,#83264),(#83265,#83266,#83267),(#83268,
#83269,#83270)),.UNSPECIFIED.,.F.,.F.,.F.)
B_SPLINE_SURFACE_WITH_KNOTS((2,1,2),(3,3),(-0.00206901892604864,0.,0.346769728503092),
(0.00660713154699752,0.0131849431469057),.UNSPECIFIED.)
GEOMETRIC_REPRESENTATION_ITEM()
RATIONAL_B_SPLINE_SURFACE(((0.997925307359498,0.997106772384952,0.996714752253859),
(0.997925307359498,0.997106772384952,0.996714752253859),(0.997925307359498,
0.997106772384952,0.996714752253858)))
REPRESENTATION_ITEM('')
SURFACE()
);
#433=(
BOUNDED_SURFACE()
B_SPLINE_SURFACE(1,2,((#83343,#83344,#83345),(#83346,#83347,#83348)),
 .UNSPECIFIED.,.F.,.F.,.F.)
B_SPLINE_SURFACE_WITH_KNOTS((2,2),(3,3),(0.,1.),(0.0556006976418438,0.0675888856590507),
 .UNSPECIFIED.)
GEOMETRIC_REPRESENTATION_ITEM()
RATIONAL_B_SPLINE_SURFACE(((0.996397562408606,0.996150386832629,0.997319912843745),
(0.996397562408606,0.996150386832629,0.997319912843745)))
REPRESENTATION_ITEM('')
SURFACE()
);
#434=(
BOUNDED_SURFACE()
B_SPLINE_SURFACE(1,2,((#83417,#83418,#83419),(#83420,#83421,#83422),(#83423,
#83424,#83425)),.UNSPECIFIED.,.F.,.F.,.F.)
B_SPLINE_SURFACE_WITH_KNOTS((2,1,2),(3,3),(0.,1.,1.01),(0.0456081671210054,
0.0575989447818828),.UNSPECIFIED.)
GEOMETRIC_REPRESENTATION_ITEM()
RATIONAL_B_SPLINE_SURFACE(((0.997793907739636,0.996365558499688,0.996354522974128),
(0.997793907739636,0.996365558499688,0.996354522974128),(0.997793907739636,
0.996365558499688,0.996354522974128)))
REPRESENTATION_ITEM('')
SURFACE()
);
#435=(
BOUNDED_SURFACE()
B_SPLINE_SURFACE(1,2,((#83460,#83461,#83462),(#83463,#83464,#83465),(#83466,
#83467,#83468)),.UNSPECIFIED.,.F.,.F.,.F.)
B_SPLINE_SURFACE_WITH_KNOTS((2,1,2),(3,3),(-0.00286810173452563,0.,0.477902879792037),
(0.0466073985929119,0.0531834929157979),.UNSPECIFIED.)
GEOMETRIC_REPRESENTATION_ITEM()
RATIONAL_B_SPLINE_SURFACE(((0.997565691989291,0.996847118055594,0.996554836292953),
(0.997565691989291,0.996847118055594,0.996554836292953),(0.997565691989291,
0.996847118055594,0.996554836292953)))
REPRESENTATION_ITEM('')
SURFACE()
);
#436=(
BOUNDED_SURFACE()
B_SPLINE_SURFACE(1,2,((#83485,#83486,#83487,#83488,#83489),(#83490,#83491,
#83492,#83493,#83494),(#83495,#83496,#83497,#83498,#83499)),
 .UNSPECIFIED.,.F.,.F.,.F.)
B_SPLINE_SURFACE_WITH_KNOTS((2,1,2),(3,2,3),(0.,1.,1.01),(0.0355931932713903,
0.0384615384615384,0.0476086899858139),.UNSPECIFIED.)
GEOMETRIC_REPRESENTATION_ITEM()
RATIONAL_B_SPLINE_SURFACE(((0.998993602249807,0.999456249886298,1.,0.998265981131401,
0.997356751596327),(0.998993602249807,0.999456249886298,1.,0.998265981131401,
0.997356751596327),(0.998993602249807,0.999456249886298,1.,0.998265981131401,
0.997356751596327)))
REPRESENTATION_ITEM('')
SURFACE()
);
#437=(
BOUNDED_SURFACE()
B_SPLINE_SURFACE(1,2,((#83547,#83548,#83549,#83550,#83551),(#83552,#83553,
#83554,#83555,#83556),(#83557,#83558,#83559,#83560,#83561)),
 .UNSPECIFIED.,.F.,.F.,.F.)
B_SPLINE_SURFACE_WITH_KNOTS((2,1,2),(3,2,3),(-0.00141401191198388,0.,0.480770297084423),
(0.0365944846645751,0.0384615384615384,0.0431859280915186),
 .UNSPECIFIED.)
GEOMETRIC_REPRESENTATION_ITEM()
RATIONAL_B_SPLINE_SURFACE(((0.999326490452258,0.999646063968217,1.,0.999104400890347,
0.9984288220563),(0.999326490452258,0.999646063968217,1.,0.999104400890347,
0.9984288220563),(0.999326490452258,0.999646063968217,1.,0.999104400890347,
0.9984288220563)))
REPRESENTATION_ITEM('')
SURFACE()
);
#438=(
BOUNDED_SURFACE()
B_SPLINE_SURFACE(1,2,((#83588,#83589,#83590),(#83591,#83592,#83593),(#83594,
#83595,#83596)),.UNSPECIFIED.,.F.,.F.,.F.)
B_SPLINE_SURFACE_WITH_KNOTS((2,1,2),(3,3),(0.,1.,1.01),(0.0255903596131801,
0.0375948596693865),.UNSPECIFIED.)
GEOMETRIC_REPRESENTATION_ITEM()
RATIONAL_B_SPLINE_SURFACE(((0.996753121755999,0.997505687613148,0.999678813023853),
(0.996753121755999,0.997505687613148,0.999678813023853),(0.996753121755999,
0.997505687613148,0.999678813023853)))
REPRESENTATION_ITEM('')
SURFACE()
);
#439=(
BOUNDED_SURFACE()
B_SPLINE_SURFACE(1,2,((#83631,#83632,#83633),(#83634,#83635,#83636),(#83637,
#83638,#83639)),.UNSPECIFIED.,.F.,.F.,.F.)
B_SPLINE_SURFACE_WITH_KNOTS((2,1,2),(3,3),(-0.00286823045906607,0.,0.477902879789481),
(0.0265907346180612,0.0331702036774533),.UNSPECIFIED.)
GEOMETRIC_REPRESENTATION_ITEM()
RATIONAL_B_SPLINE_SURFACE(((0.996888414395785,0.997365765476469,0.998269846371838),
(0.996888414395785,0.997365765476469,0.998269846371838),(0.996888414395785,
0.997365765476469,0.998269846371838)))
REPRESENTATION_ITEM('')
SURFACE()
);
#440=(
BOUNDED_SURFACE()
B_SPLINE_SURFACE(1,2,((#83706,#83707,#83708),(#83709,#83710,#83711),(#83712,
#83713,#83714)),.UNSPECIFIED.,.F.,.F.,.F.)
B_SPLINE_SURFACE_WITH_KNOTS((2,1,2),(3,3),(-0.00286753114037982,0.,0.47790287978806),
(0.016601529923896,0.0231736788090044),.UNSPECIFIED.)
GEOMETRIC_REPRESENTATION_ITEM()
RATIONAL_B_SPLINE_SURFACE(((0.996422581660833,0.996252244737399,0.996507688616235),
(0.996422581660833,0.996252244737399,0.996507688616235),(0.996422581660833,
0.996252244737399,0.996507688616235)))
REPRESENTATION_ITEM('')
SURFACE()
);
#441=(
BOUNDED_SURFACE()
B_SPLINE_SURFACE(1,2,((#83731,#83732,#83733),(#83734,#83735,#83736),(#83737,
#83738,#83739)),.UNSPECIFIED.,.F.,.F.,.F.)
B_SPLINE_SURFACE_WITH_KNOTS((2,1,2),(3,3),(-0.01,0.,1.00000001523928),(0.0056076916837061,
0.0176009700440528),.UNSPECIFIED.)
GEOMETRIC_REPRESENTATION_ITEM()
RATIONAL_B_SPLINE_SURFACE(((0.99818389211382,0.99657330421516,0.996380621259469),
(0.99818389211382,0.99657330421516,0.996380621259469),(0.99818389211382,
0.99657330421516,0.996380621259469)))
REPRESENTATION_ITEM('')
SURFACE()
);
#442=(
BOUNDED_SURFACE()
B_SPLINE_SURFACE(1,2,((#83862,#83863,#83864),(#83865,#83866,#83867)),
 .UNSPECIFIED.,.F.,.F.,.F.)
B_SPLINE_SURFACE_WITH_KNOTS((2,2),(3,3),(0.,1.),(0.0556006976418436,0.0675888856590519),
 .UNSPECIFIED.)
GEOMETRIC_REPRESENTATION_ITEM()
RATIONAL_B_SPLINE_SURFACE(((0.996397562408606,0.996150386832629,0.997319912843745),
(0.996397562408606,0.996150386832629,0.997319912843745)))
REPRESENTATION_ITEM('')
SURFACE()
);
#443=(
BOUNDED_SURFACE()
B_SPLINE_SURFACE(1,2,((#83936,#83937,#83938),(#83939,#83940,#83941),(#83942,
#83943,#83944)),.UNSPECIFIED.,.F.,.F.,.F.)
B_SPLINE_SURFACE_WITH_KNOTS((2,1,2),(3,3),(0.,1.,1.01),(0.0456081671210043,
0.057598944781883),.UNSPECIFIED.)
GEOMETRIC_REPRESENTATION_ITEM()
RATIONAL_B_SPLINE_SURFACE(((0.997793907739636,0.996365558499688,0.996354522974128),
(0.997793907739636,0.996365558499688,0.996354522974128),(0.997793907739636,
0.996365558499688,0.996354522974128)))
REPRESENTATION_ITEM('')
SURFACE()
);
#444=(
BOUNDED_SURFACE()
B_SPLINE_SURFACE(1,2,((#83979,#83980,#83981),(#83982,#83983,#83984),(#83985,
#83986,#83987)),.UNSPECIFIED.,.F.,.F.,.F.)
B_SPLINE_SURFACE_WITH_KNOTS((2,1,2),(3,3),(-0.00286810173457896,0.,0.477902879794604),
(0.0466073985929109,0.0531834929157975),.UNSPECIFIED.)
GEOMETRIC_REPRESENTATION_ITEM()
RATIONAL_B_SPLINE_SURFACE(((0.997565691989291,0.996847118055594,0.996554836292953),
(0.997565691989291,0.996847118055594,0.996554836292953),(0.997565691989291,
0.996847118055594,0.996554836292953)))
REPRESENTATION_ITEM('')
SURFACE()
);
#445=(
BOUNDED_SURFACE()
B_SPLINE_SURFACE(1,2,((#84004,#84005,#84006,#84007,#84008),(#84009,#84010,
#84011,#84012,#84013),(#84014,#84015,#84016,#84017,#84018)),
 .UNSPECIFIED.,.F.,.F.,.F.)
B_SPLINE_SURFACE_WITH_KNOTS((2,1,2),(3,2,3),(0.,1.,1.01),(0.0355931932713903,
0.0384615384615384,0.0476086899858138),.UNSPECIFIED.)
GEOMETRIC_REPRESENTATION_ITEM()
RATIONAL_B_SPLINE_SURFACE(((0.998993602249807,0.999456249886298,1.,0.998265981131401,
0.997356751596327),(0.998993602249807,0.999456249886298,1.,0.998265981131401,
0.997356751596327),(0.998993602249807,0.999456249886298,1.,0.998265981131401,
0.997356751596327)))
REPRESENTATION_ITEM('')
SURFACE()
);
#446=(
BOUNDED_SURFACE()
B_SPLINE_SURFACE(1,2,((#84066,#84067,#84068,#84069,#84070),(#84071,#84072,
#84073,#84074,#84075),(#84076,#84077,#84078,#84079,#84080)),
 .UNSPECIFIED.,.F.,.F.,.F.)
B_SPLINE_SURFACE_WITH_KNOTS((2,1,2),(3,2,3),(-0.00286743096746644,0.,0.480770297153185),
(0.0365944846641764,0.0384615384615384,0.0431859280915206),
 .UNSPECIFIED.)
GEOMETRIC_REPRESENTATION_ITEM()
RATIONAL_B_SPLINE_SURFACE(((0.999326490452122,0.999646063968141,1.,0.999104400890346,
0.998428822056299),(0.999326490452122,0.999646063968141,1.,0.999104400890346,
0.998428822056299),(0.999326490452122,0.999646063968141,1.,0.999104400890346,
0.998428822056299)))
REPRESENTATION_ITEM('')
SURFACE()
);
#447=(
BOUNDED_SURFACE()
B_SPLINE_SURFACE(1,2,((#84107,#84108,#84109),(#84110,#84111,#84112),(#84113,
#84114,#84115)),.UNSPECIFIED.,.F.,.F.,.F.)
B_SPLINE_SURFACE_WITH_KNOTS((2,1,2),(3,3),(0.,1.,1.01),(0.0255903596131786,
0.0375948596693872),.UNSPECIFIED.)
GEOMETRIC_REPRESENTATION_ITEM()
RATIONAL_B_SPLINE_SURFACE(((0.996753121755999,0.997505687613147,0.999678813023853),
(0.996753121755999,0.997505687613147,0.999678813023853),(0.996753121755999,
0.997505687613147,0.999678813023853)))
REPRESENTATION_ITEM('')
SURFACE()
);
#448=(
BOUNDED_SURFACE()
B_SPLINE_SURFACE(1,2,((#84150,#84151,#84152),(#84153,#84154,#84155),(#84156,
#84157,#84158)),.UNSPECIFIED.,.F.,.F.,.F.)
B_SPLINE_SURFACE_WITH_KNOTS((2,1,2),(3,3),(-0.00286823356217506,0.,0.477902879792038),
(0.0265907346180622,0.0331702037252929),.UNSPECIFIED.)
GEOMETRIC_REPRESENTATION_ITEM()
RATIONAL_B_SPLINE_SURFACE(((0.996888414395785,0.997365765479939,0.998269846384985),
(0.996888414395785,0.997365765479939,0.998269846384985),(0.996888414395785,
0.997365765479939,0.998269846384985)))
REPRESENTATION_ITEM('')
SURFACE()
);
#449=(
BOUNDED_SURFACE()
B_SPLINE_SURFACE(1,2,((#84225,#84226,#84227),(#84228,#84229,#84230),(#84231,
#84232,#84233)),.UNSPECIFIED.,.F.,.F.,.F.)
B_SPLINE_SURFACE_WITH_KNOTS((2,1,2),(3,3),(-0.00286753114037473,0.,0.477902879790725),
(0.0166015299238962,0.0231736788090045),.UNSPECIFIED.)
GEOMETRIC_REPRESENTATION_ITEM()
RATIONAL_B_SPLINE_SURFACE(((0.996422581660833,0.996252244737398,0.996507688616234),
(0.996422581660833,0.996252244737398,0.996507688616234),(0.996422581660833,
0.996252244737399,0.996507688616235)))
REPRESENTATION_ITEM('')
SURFACE()
);
#450=(
BOUNDED_SURFACE()
B_SPLINE_SURFACE(1,2,((#84250,#84251,#84252),(#84253,#84254,#84255),(#84256,
#84257,#84258),(#84259,#84260,#84261)),.UNSPECIFIED.,.F.,.F.,.F.)
B_SPLINE_SURFACE_WITH_KNOTS((2,1,1,2),(3,3),(-0.0101,0.,1.,1.01),(0.00560769168370621,
0.0176009700440521),.UNSPECIFIED.)
GEOMETRIC_REPRESENTATION_ITEM()
RATIONAL_B_SPLINE_SURFACE(((0.99818389211382,0.99657330421516,0.996380621259469),
(0.99818389211382,0.99657330421516,0.996380621259469),(0.99818389211382,
0.99657330421516,0.996380621259469),(0.99818389211382,0.99657330421516,
0.996380621259469)))
REPRESENTATION_ITEM('')
SURFACE()
);
#451=(
BOUNDED_SURFACE()
B_SPLINE_SURFACE(1,2,((#84296,#84297,#84298),(#84299,#84300,#84301),(#84302,
#84303,#84304)),.UNSPECIFIED.,.F.,.F.,.F.)
B_SPLINE_SURFACE_WITH_KNOTS((2,1,2),(3,3),(-0.0020690189260231,0.,0.346769728505991),
(0.00660713154698392,0.0131849431468902),.UNSPECIFIED.)
GEOMETRIC_REPRESENTATION_ITEM()
RATIONAL_B_SPLINE_SURFACE(((0.997925307359502,0.997106772384955,0.996714752253861),
(0.997925307359502,0.997106772384955,0.996714752253861),(0.997925307359502,
0.997106772384955,0.996714752253861)))
REPRESENTATION_ITEM('')
SURFACE()
);
#452=(
BOUNDED_SURFACE()
B_SPLINE_SURFACE(1,2,((#84377,#84378,#84379),(#84380,#84381,#84382)),
 .UNSPECIFIED.,.F.,.F.,.F.)
B_SPLINE_SURFACE_WITH_KNOTS((2,2),(3,3),(0.,1.),(0.0556006976418385,0.0675888856590485),
 .UNSPECIFIED.)
GEOMETRIC_REPRESENTATION_ITEM()
RATIONAL_B_SPLINE_SURFACE(((0.996397562408606,0.996150386832629,0.997319912843744),
(0.996397562408606,0.996150386832629,0.997319912843744)))
REPRESENTATION_ITEM('')
SURFACE()
);
#453=(
BOUNDED_SURFACE()
B_SPLINE_SURFACE(1,2,((#84451,#84452,#84453),(#84454,#84455,#84456),(#84457,
#84458,#84459)),.UNSPECIFIED.,.F.,.F.,.F.)
B_SPLINE_SURFACE_WITH_KNOTS((2,1,2),(3,3),(0.,1.,1.01),(0.0456081671210087,
0.057598944781882),.UNSPECIFIED.)
GEOMETRIC_REPRESENTATION_ITEM()
RATIONAL_B_SPLINE_SURFACE(((0.997793907739635,0.996365558499688,0.996354522974128),
(0.997793907739635,0.996365558499688,0.996354522974128),(0.997793907739635,
0.996365558499688,0.996354522974128)))
REPRESENTATION_ITEM('')
SURFACE()
);
#454=(
BOUNDED_SURFACE()
B_SPLINE_SURFACE(1,2,((#84494,#84495,#84496),(#84497,#84498,#84499),(#84500,
#84501,#84502)),.UNSPECIFIED.,.F.,.F.,.F.)
B_SPLINE_SURFACE_WITH_KNOTS((2,1,2),(3,3),(-0.0028681017194608,0.,0.477902879797066),
(0.046607398592912,0.0531834927425532),.UNSPECIFIED.)
GEOMETRIC_REPRESENTATION_ITEM()
RATIONAL_B_SPLINE_SURFACE(((0.997565691989291,0.996847118074524,0.996554836308353),
(0.997565691989291,0.996847118074524,0.996554836308353),(0.997565691989291,
0.996847118074524,0.996554836308353)))
REPRESENTATION_ITEM('')
SURFACE()
);
#455=(
BOUNDED_SURFACE()
B_SPLINE_SURFACE(1,2,((#84519,#84520,#84521,#84522,#84523),(#84524,#84525,
#84526,#84527,#84528),(#84529,#84530,#84531,#84532,#84533)),
 .UNSPECIFIED.,.F.,.F.,.F.)
B_SPLINE_SURFACE_WITH_KNOTS((2,1,2),(3,2,3),(0.,1.,1.01),(0.0355931932713903,
0.0384615384615384,0.0476086899858133),.UNSPECIFIED.)
GEOMETRIC_REPRESENTATION_ITEM()
RATIONAL_B_SPLINE_SURFACE(((0.998993602249807,0.999456249886298,1.,0.998265981131401,
0.997356751596327),(0.998993602249807,0.999456249886298,1.,0.998265981131401,
0.997356751596327),(0.998993602249807,0.999456249886298,1.,0.998265981131401,
0.997356751596327)))
REPRESENTATION_ITEM('')
SURFACE()
);
#456=(
BOUNDED_SURFACE()
B_SPLINE_SURFACE(1,2,((#84581,#84582,#84583,#84584,#84585),(#84586,#84587,
#84588,#84589,#84590),(#84591,#84592,#84593,#84594,#84595)),
 .UNSPECIFIED.,.F.,.F.,.F.)
B_SPLINE_SURFACE_WITH_KNOTS((2,1,2),(3,2,3),(-0.00286742665919738,0.,0.480770297130077),
(0.036594484664175,0.0384615384615384,0.0431859280915206),.UNSPECIFIED.)
GEOMETRIC_REPRESENTATION_ITEM()
RATIONAL_B_SPLINE_SURFACE(((0.999326490452121,0.99964606396814,1.,0.999104400890346,
0.998428822056299),(0.999326490452121,0.99964606396814,1.,0.999104400890346,
0.998428822056299),(0.999326490452121,0.99964606396814,1.,0.999104400890346,
0.998428822056299)))
REPRESENTATION_ITEM('')
SURFACE()
);
#457=(
BOUNDED_SURFACE()
B_SPLINE_SURFACE(1,2,((#84622,#84623,#84624),(#84625,#84626,#84627),(#84628,
#84629,#84630)),.UNSPECIFIED.,.F.,.F.,.F.)
B_SPLINE_SURFACE_WITH_KNOTS((2,1,2),(3,3),(0.,1.,1.01),(0.02559035961318,
0.0375948596693871),.UNSPECIFIED.)
GEOMETRIC_REPRESENTATION_ITEM()
RATIONAL_B_SPLINE_SURFACE(((0.996753121755999,0.997505687613148,0.999678813023853),
(0.996753121755999,0.997505687613148,0.999678813023853),(0.996753121755999,
0.997505687613148,0.999678813023853)))
REPRESENTATION_ITEM('')
SURFACE()
);
#458=(
BOUNDED_SURFACE()
B_SPLINE_SURFACE(1,2,((#84665,#84666,#84667),(#84668,#84669,#84670),(#84671,
#84672,#84673)),.UNSPECIFIED.,.F.,.F.,.F.)
B_SPLINE_SURFACE_WITH_KNOTS((2,1,2),(3,3),(-0.00286823257315062,0.,0.477902879794566),
(0.0265907346180623,0.0331702037100443),.UNSPECIFIED.)
GEOMETRIC_REPRESENTATION_ITEM()
RATIONAL_B_SPLINE_SURFACE(((0.996888414395785,0.997365765478833,0.998269846380795),
(0.996888414395785,0.997365765478833,0.998269846380795),(0.996888414395785,
0.997365765478833,0.998269846380795)))
REPRESENTATION_ITEM('')
SURFACE()
);
#459=(
BOUNDED_SURFACE()
B_SPLINE_SURFACE(1,2,((#84740,#84741,#84742),(#84743,#84744,#84745),(#84746,
#84747,#84748)),.UNSPECIFIED.,.F.,.F.,.F.)
B_SPLINE_SURFACE_WITH_KNOTS((2,1,2),(3,3),(-0.00286753114032031,0.,0.477902879793208),
(0.0166015299238958,0.0231736788090044),.UNSPECIFIED.)
GEOMETRIC_REPRESENTATION_ITEM()
RATIONAL_B_SPLINE_SURFACE(((0.996422581660833,0.996252244737398,0.996507688616235),
(0.996422581660833,0.996252244737398,0.996507688616235),(0.996422581660833,
0.996252244737399,0.996507688616235)))
REPRESENTATION_ITEM('')
SURFACE()
);
#460=(
BOUNDED_SURFACE()
B_SPLINE_SURFACE(1,2,((#84765,#84766,#84767),(#84768,#84769,#84770),(#84771,
#84772,#84773),(#84774,#84775,#84776)),.UNSPECIFIED.,.F.,.F.,.F.)
B_SPLINE_SURFACE_WITH_KNOTS((2,1,1,2),(3,3),(-0.0101,0.,1.,1.01),(0.00560769168370516,
0.0176009700440511),.UNSPECIFIED.)
GEOMETRIC_REPRESENTATION_ITEM()
RATIONAL_B_SPLINE_SURFACE(((0.998183892113821,0.99657330421516,0.996380621259469),
(0.998183892113821,0.99657330421516,0.996380621259469),(0.998183892113821,
0.99657330421516,0.996380621259469),(0.998183892113821,0.99657330421516,
0.996380621259469)))
REPRESENTATION_ITEM('')
SURFACE()
);
#461=(
BOUNDED_SURFACE()
B_SPLINE_SURFACE(1,2,((#84811,#84812,#84813),(#84814,#84815,#84816),(#84817,
#84818,#84819)),.UNSPECIFIED.,.F.,.F.,.F.)
B_SPLINE_SURFACE_WITH_KNOTS((2,1,2),(3,3),(-0.00206901892615475,0.,0.346769728507453),
(0.00660713154697986,0.0131849431468375),.UNSPECIFIED.)
GEOMETRIC_REPRESENTATION_ITEM()
RATIONAL_B_SPLINE_SURFACE(((0.997925307359503,0.997106772384962,0.996714752253866),
(0.997925307359503,0.997106772384962,0.996714752253866),(0.997925307359503,
0.997106772384962,0.996714752253866)))
REPRESENTATION_ITEM('')
SURFACE()
);
#462=(
BOUNDED_SURFACE()
B_SPLINE_SURFACE(1,2,((#84892,#84893,#84894),(#84895,#84896,#84897)),
 .UNSPECIFIED.,.F.,.F.,.F.)
B_SPLINE_SURFACE_WITH_KNOTS((2,2),(3,3),(0.,1.),(0.0556006976418427,0.0675888856590499),
 .UNSPECIFIED.)
GEOMETRIC_REPRESENTATION_ITEM()
RATIONAL_B_SPLINE_SURFACE(((0.996397562408606,0.996150386832629,0.997319912843745),
(0.996397562408606,0.996150386832629,0.997319912843745)))
REPRESENTATION_ITEM('')
SURFACE()
);
#463=(
BOUNDED_SURFACE()
B_SPLINE_SURFACE(1,2,((#84966,#84967,#84968),(#84969,#84970,#84971),(#84972,
#84973,#84974)),.UNSPECIFIED.,.F.,.F.,.F.)
B_SPLINE_SURFACE_WITH_KNOTS((2,1,2),(3,3),(0.,1.,1.01),(0.0456081671210024,
0.0575989447818799),.UNSPECIFIED.)
GEOMETRIC_REPRESENTATION_ITEM()
RATIONAL_B_SPLINE_SURFACE(((0.997793907739637,0.996365558499689,0.996354522974128),
(0.997793907739637,0.996365558499689,0.996354522974128),(0.997793907739637,
0.996365558499689,0.996354522974128)))
REPRESENTATION_ITEM('')
SURFACE()
);
#464=(
BOUNDED_SURFACE()
B_SPLINE_SURFACE(1,2,((#85009,#85010,#85011),(#85012,#85013,#85014),(#85015,
#85016,#85017)),.UNSPECIFIED.,.F.,.F.,.F.)
B_SPLINE_SURFACE_WITH_KNOTS((2,1,2),(3,3),(-0.00286810173468854,0.,0.47790287979959),
(0.0466073985929113,0.0531834929157972),.UNSPECIFIED.)
GEOMETRIC_REPRESENTATION_ITEM()
RATIONAL_B_SPLINE_SURFACE(((0.997565691989291,0.996847118055593,0.996554836292953),
(0.997565691989291,0.996847118055593,0.996554836292953),(0.997565691989291,
0.996847118055593,0.996554836292953)))
REPRESENTATION_ITEM('')
SURFACE()
);
#465=(
BOUNDED_SURFACE()
B_SPLINE_SURFACE(1,2,((#85034,#85035,#85036,#85037,#85038),(#85039,#85040,
#85041,#85042,#85043),(#85044,#85045,#85046,#85047,#85048)),
 .UNSPECIFIED.,.F.,.F.,.F.)
B_SPLINE_SURFACE_WITH_KNOTS((2,1,2),(3,2,3),(0.,1.,1.01),(0.0355931932713903,
0.0384615384615384,0.0476086899858149),.UNSPECIFIED.)
GEOMETRIC_REPRESENTATION_ITEM()
RATIONAL_B_SPLINE_SURFACE(((0.998993602249807,0.999456249886298,1.,0.9982659811314,
0.997356751596327),(0.998993602249807,0.999456249886298,1.,0.9982659811314,
0.997356751596327),(0.998993602249807,0.999456249886298,1.,0.9982659811314,
0.997356751596327)))
REPRESENTATION_ITEM('')
SURFACE()
);
#466=(
BOUNDED_SURFACE()
B_SPLINE_SURFACE(1,2,((#85096,#85097,#85098,#85099,#85100),(#85101,#85102,
#85103,#85104,#85105),(#85106,#85107,#85108,#85109,#85110)),
 .UNSPECIFIED.,.F.,.F.,.F.)
B_SPLINE_SURFACE_WITH_KNOTS((2,1,2),(3,2,3),(-0.00141401191198397,0.,0.480770297092029),
(0.0365944846645762,0.0384615384615384,0.043185928091518),.UNSPECIFIED.)
GEOMETRIC_REPRESENTATION_ITEM()
RATIONAL_B_SPLINE_SURFACE(((0.999326490452258,0.999646063968217,1.,0.999104400890347,
0.9984288220563),(0.999326490452259,0.999646063968217,1.,0.999104400890347,
0.9984288220563),(0.999326490452259,0.999646063968217,1.,0.999104400890347,
0.9984288220563)))
REPRESENTATION_ITEM('')
SURFACE()
);
#467=(
BOUNDED_SURFACE()
B_SPLINE_SURFACE(1,2,((#85137,#85138,#85139),(#85140,#85141,#85142),(#85143,
#85144,#85145)),.UNSPECIFIED.,.F.,.F.,.F.)
B_SPLINE_SURFACE_WITH_KNOTS((2,1,2),(3,3),(0.,1.,1.01),(0.025590359613181,
0.0375948596693886),.UNSPECIFIED.)
GEOMETRIC_REPRESENTATION_ITEM()
RATIONAL_B_SPLINE_SURFACE(((0.996753121755999,0.997505687613148,0.999678813023854),
(0.996753121755999,0.997505687613148,0.999678813023854),(0.996753121755999,
0.997505687613148,0.999678813023854)))
REPRESENTATION_ITEM('')
SURFACE()
);
#468=(
BOUNDED_SURFACE()
B_SPLINE_SURFACE(1,2,((#85180,#85181,#85182),(#85183,#85184,#85185),(#85186,
#85187,#85188)),.UNSPECIFIED.,.F.,.F.,.F.)
B_SPLINE_SURFACE_WITH_KNOTS((2,1,2),(3,3),(-0.00286823356219242,0.,0.477902879797069),
(0.0265907346180625,0.0331702037252923),.UNSPECIFIED.)
GEOMETRIC_REPRESENTATION_ITEM()
RATIONAL_B_SPLINE_SURFACE(((0.996888414395785,0.997365765479939,0.998269846384986),
(0.996888414395785,0.997365765479939,0.998269846384985),(0.996888414395786,
0.997365765479939,0.998269846384985)))
REPRESENTATION_ITEM('')
SURFACE()
);
#469=(
BOUNDED_SURFACE()
B_SPLINE_SURFACE(1,2,((#85255,#85256,#85257),(#85258,#85259,#85260),(#85261,
#85262,#85263)),.UNSPECIFIED.,.F.,.F.,.F.)
B_SPLINE_SURFACE_WITH_KNOTS((2,1,2),(3,3),(-0.00286753128209527,0.,0.477902879795792),
(0.016601529923896,0.0231736788111884),.UNSPECIFIED.)
GEOMETRIC_REPRESENTATION_ITEM()
RATIONAL_B_SPLINE_SURFACE(((0.996422581660833,0.996252244737341,0.996507688616404),
(0.996422581660833,0.996252244737341,0.996507688616404),(0.996422581660833,
0.996252244737341,0.996507688616404)))
REPRESENTATION_ITEM('')
SURFACE()
);
#470=(
BOUNDED_SURFACE()
B_SPLINE_SURFACE(1,2,((#85280,#85281,#85282),(#85283,#85284,#85285),(#85286,
#85287,#85288),(#85289,#85290,#85291)),.UNSPECIFIED.,.F.,.F.,.F.)
B_SPLINE_SURFACE_WITH_KNOTS((2,1,1,2),(3,3),(-0.0101,0.,1.,1.01),(0.00560769168370618,
0.0176009700440511),.UNSPECIFIED.)
GEOMETRIC_REPRESENTATION_ITEM()
RATIONAL_B_SPLINE_SURFACE(((0.99818389211382,0.99657330421516,0.996380621259469),
(0.99818389211382,0.99657330421516,0.996380621259469),(0.99818389211382,
0.99657330421516,0.996380621259469),(0.99818389211382,0.99657330421516,
0.996380621259469)))
REPRESENTATION_ITEM('')
SURFACE()
);
#471=(
BOUNDED_SURFACE()
B_SPLINE_SURFACE(1,2,((#85326,#85327,#85328),(#85329,#85330,#85331),(#85332,
#85333,#85334)),.UNSPECIFIED.,.F.,.F.,.F.)
B_SPLINE_SURFACE_WITH_KNOTS((2,1,2),(3,3),(-0.00206901892616219,0.,0.346769728508837),
(0.0066071315469777,0.0131849431468903),.UNSPECIFIED.)
GEOMETRIC_REPRESENTATION_ITEM()
RATIONAL_B_SPLINE_SURFACE(((0.997925307359503,0.997106772384955,0.996714752253861),
(0.997925307359503,0.997106772384955,0.99671475225386),(0.997925307359504,
0.997106772384955,0.99671475225386)))
REPRESENTATION_ITEM('')
SURFACE()
);
#472=(
BOUNDED_SURFACE()
B_SPLINE_SURFACE(1,2,((#85407,#85408,#85409),(#85410,#85411,#85412)),
 .UNSPECIFIED.,.F.,.F.,.F.)
B_SPLINE_SURFACE_WITH_KNOTS((2,2),(3,3),(0.,1.),(0.0556006976418383,0.0675888856590508),
 .UNSPECIFIED.)
GEOMETRIC_REPRESENTATION_ITEM()
RATIONAL_B_SPLINE_SURFACE(((0.996397562408606,0.996150386832629,0.997319912843745),
(0.996397562408606,0.996150386832629,0.997319912843745)))
REPRESENTATION_ITEM('')
SURFACE()
);
#473=(
BOUNDED_SURFACE()
B_SPLINE_SURFACE(1,2,((#85481,#85482,#85483),(#85484,#85485,#85486),(#85487,
#85488,#85489)),.UNSPECIFIED.,.F.,.F.,.F.)
B_SPLINE_SURFACE_WITH_KNOTS((2,1,2),(3,3),(0.,1.,1.01),(0.0456081671210034,
0.057598944781882),.UNSPECIFIED.)
GEOMETRIC_REPRESENTATION_ITEM()
RATIONAL_B_SPLINE_SURFACE(((0.997793907739636,0.996365558499688,0.996354522974128),
(0.997793907739636,0.996365558499688,0.996354522974128),(0.997793907739636,
0.996365558499688,0.996354522974128)))
REPRESENTATION_ITEM('')
SURFACE()
);
#474=(
BOUNDED_SURFACE()
B_SPLINE_SURFACE(1,2,((#85524,#85525,#85526),(#85527,#85528,#85529),(#85530,
#85531,#85532)),.UNSPECIFIED.,.F.,.F.,.F.)
B_SPLINE_SURFACE_WITH_KNOTS((2,1,2),(3,3),(-0.00286810173476254,0.,0.477902879801921),
(0.0466073985929117,0.0531834929157977),.UNSPECIFIED.)
GEOMETRIC_REPRESENTATION_ITEM()
RATIONAL_B_SPLINE_SURFACE(((0.997565691989291,0.996847118055594,0.996554836292953),
(0.997565691989291,0.996847118055594,0.996554836292953),(0.997565691989291,
0.996847118055594,0.996554836292953)))
REPRESENTATION_ITEM('')
SURFACE()
);
#475=(
BOUNDED_SURFACE()
B_SPLINE_SURFACE(1,2,((#85549,#85550,#85551,#85552,#85553),(#85554,#85555,
#85556,#85557,#85558),(#85559,#85560,#85561,#85562,#85563)),
 .UNSPECIFIED.,.F.,.F.,.F.)
B_SPLINE_SURFACE_WITH_KNOTS((2,1,2),(3,2,3),(0.,1.,1.01),(0.0355931932713904,
0.0384615384615384,0.0476086899858116),.UNSPECIFIED.)
GEOMETRIC_REPRESENTATION_ITEM()
RATIONAL_B_SPLINE_SURFACE(((0.998993602249807,0.999456249886298,1.,0.998265981131401,
0.997356751596327),(0.998993602249807,0.999456249886298,1.,0.998265981131401,
0.997356751596327),(0.998993602249807,0.999456249886298,1.,0.998265981131401,
0.997356751596327)))
REPRESENTATION_ITEM('')
SURFACE()
);
#476=(
BOUNDED_SURFACE()
B_SPLINE_SURFACE(1,2,((#85611,#85612,#85613,#85614,#85615),(#85616,#85617,
#85618,#85619,#85620),(#85621,#85622,#85623,#85624,#85625)),
 .UNSPECIFIED.,.F.,.F.,.F.)
B_SPLINE_SURFACE_WITH_KNOTS((2,1,2),(3,2,3),(-0.00141401191198296,0.,0.480770297094429),
(0.0365944846645748,0.0384615384615384,0.0431859280915183),
 .UNSPECIFIED.)
GEOMETRIC_REPRESENTATION_ITEM()
RATIONAL_B_SPLINE_SURFACE(((0.999326490452258,0.999646063968217,1.,0.999104400890347,
0.9984288220563),(0.999326490452258,0.999646063968217,1.,0.999104400890347,
0.9984288220563),(0.999326490452258,0.999646063968217,1.,0.999104400890347,
0.9984288220563)))
REPRESENTATION_ITEM('')
SURFACE()
);
#477=(
BOUNDED_SURFACE()
B_SPLINE_SURFACE(1,2,((#85652,#85653,#85654),(#85655,#85656,#85657),(#85658,
#85659,#85660)),.UNSPECIFIED.,.F.,.F.,.F.)
B_SPLINE_SURFACE_WITH_KNOTS((2,1,2),(3,3),(0.,1.,1.01),(0.0255903596131811,
0.0375948596693879),.UNSPECIFIED.)
GEOMETRIC_REPRESENTATION_ITEM()
RATIONAL_B_SPLINE_SURFACE(((0.996753121755999,0.997505687613148,0.999678813023854),
(0.996753121755999,0.997505687613148,0.999678813023854),(0.996753121755999,
0.997505687613148,0.999678813023854)))
REPRESENTATION_ITEM('')
SURFACE()
);
#478=(
BOUNDED_SURFACE()
B_SPLINE_SURFACE(1,2,((#85695,#85696,#85697),(#85698,#85699,#85700),(#85701,
#85702,#85703)),.UNSPECIFIED.,.F.,.F.,.F.)
B_SPLINE_SURFACE_WITH_KNOTS((2,1,2),(3,3),(-0.00286823356221668,0.,0.477902879799528),
(0.0265907346180627,0.0331702037252926),.UNSPECIFIED.)
GEOMETRIC_REPRESENTATION_ITEM()
RATIONAL_B_SPLINE_SURFACE(((0.996888414395785,0.997365765479939,0.998269846384985),
(0.996888414395785,0.997365765479939,0.998269846384985),(0.996888414395785,
0.997365765479939,0.998269846384985)))
REPRESENTATION_ITEM('')
SURFACE()
);
#479=(
BOUNDED_SURFACE()
B_SPLINE_SURFACE(1,2,((#85770,#85771,#85772),(#85773,#85774,#85775),(#85776,
#85777,#85778)),.UNSPECIFIED.,.F.,.F.,.F.)
B_SPLINE_SURFACE_WITH_KNOTS((2,1,2),(3,3),(-0.00286753128205672,0.,0.477902879798263),
(0.0166015299238967,0.0231736788111887),.UNSPECIFIED.)
GEOMETRIC_REPRESENTATION_ITEM()
RATIONAL_B_SPLINE_SURFACE(((0.996422581660833,0.996252244737342,0.996507688616404),
(0.996422581660833,0.996252244737342,0.996507688616404),(0.996422581660833,
0.996252244737342,0.996507688616404)))
REPRESENTATION_ITEM('')
SURFACE()
);
#480=(
BOUNDED_SURFACE()
B_SPLINE_SURFACE(1,2,((#85795,#85796,#85797),(#85798,#85799,#85800),(#85801,
#85802,#85803),(#85804,#85805,#85806)),.UNSPECIFIED.,.F.,.F.,.F.)
B_SPLINE_SURFACE_WITH_KNOTS((2,1,1,2),(3,3),(-0.0101,0.,1.,1.01),(0.00560769168370501,
0.0176009700440522),.UNSPECIFIED.)
GEOMETRIC_REPRESENTATION_ITEM()
RATIONAL_B_SPLINE_SURFACE(((0.998183892113821,0.99657330421516,0.996380621259469),
(0.998183892113821,0.99657330421516,0.996380621259469),(0.998183892113821,
0.99657330421516,0.996380621259469),(0.998183892113821,0.99657330421516,
0.996380621259469)))
REPRESENTATION_ITEM('')
SURFACE()
);
#481=(
BOUNDED_SURFACE()
B_SPLINE_SURFACE(1,2,((#85841,#85842,#85843),(#85844,#85845,#85846),(#85847,
#85848,#85849)),.UNSPECIFIED.,.F.,.F.,.F.)
B_SPLINE_SURFACE_WITH_KNOTS((2,1,2),(3,3),(-0.00206901892463095,0.,0.346769728509987),
(0.00660713154697685,0.0131849431292506),.UNSPECIFIED.)
GEOMETRIC_REPRESENTATION_ITEM()
RATIONAL_B_SPLINE_SURFACE(((0.997925307359503,0.99710677238715,0.996714752255963),
(0.997925307359503,0.99710677238715,0.996714752255963),(0.997925307359503,
0.99710677238715,0.996714752255963)))
REPRESENTATION_ITEM('')
SURFACE()
);
#482=(
BOUNDED_SURFACE()
B_SPLINE_SURFACE(1,2,((#85922,#85923,#85924),(#85925,#85926,#85927)),
 .UNSPECIFIED.,.F.,.F.,.F.)
B_SPLINE_SURFACE_WITH_KNOTS((2,2),(3,3),(0.,1.),(0.0556006976418437,0.0675888856590492),
 .UNSPECIFIED.)
GEOMETRIC_REPRESENTATION_ITEM()
RATIONAL_B_SPLINE_SURFACE(((0.996397562408606,0.996150386832629,0.997319912843745),
(0.996397562408606,0.996150386832629,0.997319912843745)))
REPRESENTATION_ITEM('')
SURFACE()
);
#483=(
BOUNDED_SURFACE()
B_SPLINE_SURFACE(1,2,((#85996,#85997,#85998),(#85999,#86000,#86001),(#86002,
#86003,#86004)),.UNSPECIFIED.,.F.,.F.,.F.)
B_SPLINE_SURFACE_WITH_KNOTS((2,1,2),(3,3),(0.,1.,1.01),(0.0456081671210057,
0.0575989447818802),.UNSPECIFIED.)
GEOMETRIC_REPRESENTATION_ITEM()
RATIONAL_B_SPLINE_SURFACE(((0.997793907739636,0.996365558499688,0.996354522974128),
(0.997793907739636,0.996365558499688,0.996354522974128),(0.997793907739636,
0.996365558499688,0.996354522974128)))
REPRESENTATION_ITEM('')
SURFACE()
);
#484=(
BOUNDED_SURFACE()
B_SPLINE_SURFACE(1,2,((#86039,#86040,#86041),(#86042,#86043,#86044),(#86045,
#86046,#86047)),.UNSPECIFIED.,.F.,.F.,.F.)
B_SPLINE_SURFACE_WITH_KNOTS((2,1,2),(3,3),(-0.00286810173481973,0.,0.477902879804097),
(0.0466073985929127,0.053183492915797),.UNSPECIFIED.)
GEOMETRIC_REPRESENTATION_ITEM()
RATIONAL_B_SPLINE_SURFACE(((0.997565691989291,0.996847118055594,0.996554836292953),
(0.997565691989291,0.996847118055594,0.996554836292953),(0.997565691989291,
0.996847118055594,0.996554836292953)))
REPRESENTATION_ITEM('')
SURFACE()
);
#485=(
BOUNDED_SURFACE()
B_SPLINE_SURFACE(1,2,((#86064,#86065,#86066,#86067,#86068),(#86069,#86070,
#86071,#86072,#86073),(#86074,#86075,#86076,#86077,#86078)),
 .UNSPECIFIED.,.F.,.F.,.F.)
B_SPLINE_SURFACE_WITH_KNOTS((2,1,2),(3,2,3),(0.,1.,1.01),(0.0355931932713904,
0.0384615384615384,0.0476086899858128),.UNSPECIFIED.)
GEOMETRIC_REPRESENTATION_ITEM()
RATIONAL_B_SPLINE_SURFACE(((0.998993602249807,0.999456249886298,1.,0.998265981131401,
0.997356751596327),(0.998993602249807,0.999456249886298,1.,0.998265981131401,
0.997356751596327),(0.998993602249807,0.999456249886298,1.,0.998265981131401,
0.997356751596327)))
REPRESENTATION_ITEM('')
SURFACE()
);
#486=(
BOUNDED_SURFACE()
B_SPLINE_SURFACE(1,2,((#86126,#86127,#86128,#86129,#86130),(#86131,#86132,
#86133,#86134,#86135),(#86136,#86137,#86138,#86139,#86140)),
 .UNSPECIFIED.,.F.,.F.,.F.)
B_SPLINE_SURFACE_WITH_KNOTS((2,1,2),(3,2,3),(-0.00141401191198409,0.,0.4807702970967),
(0.0365944846645792,0.0384615384615384,0.043185928091518),.UNSPECIFIED.)
GEOMETRIC_REPRESENTATION_ITEM()
RATIONAL_B_SPLINE_SURFACE(((0.999326490452259,0.999646063968217,1.,0.999104400890347,
0.9984288220563),(0.999326490452259,0.999646063968217,1.,0.999104400890347,
0.9984288220563),(0.999326490452259,0.999646063968217,1.,0.999104400890347,
0.9984288220563)))
REPRESENTATION_ITEM('')
SURFACE()
);
#487=(
BOUNDED_SURFACE()
B_SPLINE_SURFACE(1,2,((#86167,#86168,#86169),(#86170,#86171,#86172),(#86173,
#86174,#86175)),.UNSPECIFIED.,.F.,.F.,.F.)
B_SPLINE_SURFACE_WITH_KNOTS((2,1,2),(3,3),(0.,1.,1.01),(0.0255903596131777,
0.0375948596693867),.UNSPECIFIED.)
GEOMETRIC_REPRESENTATION_ITEM()
RATIONAL_B_SPLINE_SURFACE(((0.996753121755999,0.997505687613147,0.999678813023853),
(0.996753121755999,0.997505687613147,0.999678813023853),(0.996753121755999,
0.997505687613147,0.999678813023853)))
REPRESENTATION_ITEM('')
SURFACE()
);
#488=(
BOUNDED_SURFACE()
B_SPLINE_SURFACE(1,2,((#86210,#86211,#86212),(#86213,#86214,#86215),(#86216,
#86217,#86218)),.UNSPECIFIED.,.F.,.F.,.F.)
B_SPLINE_SURFACE_WITH_KNOTS((2,1,2),(3,3),(-0.00286823356225374,0.,0.477902879801828),
(0.0265907346180626,0.0331702037252923),.UNSPECIFIED.)
GEOMETRIC_REPRESENTATION_ITEM()
RATIONAL_B_SPLINE_SURFACE(((0.996888414395785,0.997365765479939,0.998269846384985),
(0.996888414395785,0.997365765479939,0.998269846384985),(0.996888414395785,
0.997365765479939,0.998269846384985)))
REPRESENTATION_ITEM('')
SURFACE()
);
#489=(
BOUNDED_SURFACE()
B_SPLINE_SURFACE(1,2,((#86285,#86286,#86287),(#86288,#86289,#86290),(#86291,
#86292,#86293)),.UNSPECIFIED.,.F.,.F.,.F.)
B_SPLINE_SURFACE_WITH_KNOTS((2,1,2),(3,3),(-0.00286753128208184,0.,0.477902879800619),
(0.0166015299238959,0.0231736788111884),.UNSPECIFIED.)
GEOMETRIC_REPRESENTATION_ITEM()
RATIONAL_B_SPLINE_SURFACE(((0.996422581660833,0.996252244737341,0.996507688616404),
(0.996422581660833,0.996252244737341,0.996507688616404),(0.996422581660833,
0.996252244737341,0.996507688616404)))
REPRESENTATION_ITEM('')
SURFACE()
);
#490=(
BOUNDED_SURFACE()
B_SPLINE_SURFACE(1,2,((#86310,#86311,#86312),(#86313,#86314,#86315),(#86316,
#86317,#86318),(#86319,#86320,#86321)),.UNSPECIFIED.,.F.,.F.,.F.)
B_SPLINE_SURFACE_WITH_KNOTS((2,1,1,2),(3,3),(-0.0101,0.,1.,1.01),(0.00560769168370726,
0.0176009700440521),.UNSPECIFIED.)
GEOMETRIC_REPRESENTATION_ITEM()
RATIONAL_B_SPLINE_SURFACE(((0.99818389211382,0.99657330421516,0.996380621259469),
(0.99818389211382,0.99657330421516,0.996380621259469),(0.99818389211382,
0.99657330421516,0.996380621259469),(0.99818389211382,0.99657330421516,
0.996380621259469)))
REPRESENTATION_ITEM('')
SURFACE()
);
#491=(
BOUNDED_SURFACE()
B_SPLINE_SURFACE(1,2,((#86356,#86357,#86358),(#86359,#86360,#86361),(#86362,
#86363,#86364)),.UNSPECIFIED.,.F.,.F.,.F.)
B_SPLINE_SURFACE_WITH_KNOTS((2,1,2),(3,3),(-0.00206901892625295,0.,0.346769728511189),
(0.00660713154697812,0.013184943146838),.UNSPECIFIED.)
GEOMETRIC_REPRESENTATION_ITEM()
RATIONAL_B_SPLINE_SURFACE(((0.997925307359503,0.997106772384961,0.996714752253866),
(0.997925307359503,0.997106772384961,0.996714752253866),(0.997925307359503,
0.997106772384961,0.996714752253866)))
REPRESENTATION_ITEM('')
SURFACE()
);
#492=(
BOUNDED_SURFACE()
B_SPLINE_SURFACE(1,2,((#86437,#86438,#86439),(#86440,#86441,#86442)),
 .UNSPECIFIED.,.F.,.F.,.F.)
B_SPLINE_SURFACE_WITH_KNOTS((2,2),(3,3),(0.,1.),(0.0556006976418426,0.0675888856590519),
 .UNSPECIFIED.)
GEOMETRIC_REPRESENTATION_ITEM()
RATIONAL_B_SPLINE_SURFACE(((0.996397562408606,0.996150386832629,0.997319912843745),
(0.996397562408606,0.996150386832629,0.997319912843745)))
REPRESENTATION_ITEM('')
SURFACE()
);
#493=(
BOUNDED_SURFACE()
B_SPLINE_SURFACE(1,2,((#86511,#86512,#86513),(#86514,#86515,#86516),(#86517,
#86518,#86519)),.UNSPECIFIED.,.F.,.F.,.F.)
B_SPLINE_SURFACE_WITH_KNOTS((2,1,2),(3,3),(0.,1.,1.01),(0.0456081671210031,
0.0575989447818832),.UNSPECIFIED.)
GEOMETRIC_REPRESENTATION_ITEM()
RATIONAL_B_SPLINE_SURFACE(((0.997793907739636,0.996365558499688,0.996354522974128),
(0.997793907739636,0.996365558499688,0.996354522974128),(0.997793907739636,
0.996365558499688,0.996354522974128)))
REPRESENTATION_ITEM('')
SURFACE()
);
#494=(
BOUNDED_SURFACE()
B_SPLINE_SURFACE(1,2,((#86554,#86555,#86556),(#86557,#86558,#86559),(#86560,
#86561,#86562)),.UNSPECIFIED.,.F.,.F.,.F.)
B_SPLINE_SURFACE_WITH_KNOTS((2,1,2),(3,3),(-0.00286810173489927,0.,0.477902879806116),
(0.046607398592912,0.0531834929157973),.UNSPECIFIED.)
GEOMETRIC_REPRESENTATION_ITEM()
RATIONAL_B_SPLINE_SURFACE(((0.997565691989291,0.996847118055593,0.996554836292953),
(0.997565691989291,0.996847118055593,0.996554836292953),(0.997565691989291,
0.996847118055593,0.996554836292953)))
REPRESENTATION_ITEM('')
SURFACE()
);
#495=(
BOUNDED_SURFACE()
B_SPLINE_SURFACE(1,2,((#86579,#86580,#86581,#86582,#86583),(#86584,#86585,
#86586,#86587,#86588),(#86589,#86590,#86591,#86592,#86593)),
 .UNSPECIFIED.,.F.,.F.,.F.)
B_SPLINE_SURFACE_WITH_KNOTS((2,1,2),(3,2,3),(0.,1.,1.01),(0.0355931932713903,
0.0384615384615384,0.0476086899858138),.UNSPECIFIED.)
GEOMETRIC_REPRESENTATION_ITEM()
RATIONAL_B_SPLINE_SURFACE(((0.998993602249807,0.999456249886298,1.,0.998265981131401,
0.997356751596327),(0.998993602249807,0.999456249886298,1.,0.998265981131401,
0.997356751596327),(0.998993602249807,0.999456249886298,1.,0.998265981131401,
0.997356751596327)))
REPRESENTATION_ITEM('')
SURFACE()
);
#496=(
BOUNDED_SURFACE()
B_SPLINE_SURFACE(1,2,((#86641,#86642,#86643,#86644,#86645),(#86646,#86647,
#86648,#86649,#86650),(#86651,#86652,#86653,#86654,#86655)),
 .UNSPECIFIED.,.F.,.F.,.F.)
B_SPLINE_SURFACE_WITH_KNOTS((2,1,2),(3,2,3),(-0.00286743095560886,0.,0.480770297165012),
(0.0365944846641869,0.0384615384615384,0.0431859280915204),
 .UNSPECIFIED.)
GEOMETRIC_REPRESENTATION_ITEM()
RATIONAL_B_SPLINE_SURFACE(((0.999326490452125,0.999646063968143,1.,0.999104400890347,
0.9984288220563),(0.999326490452125,0.999646063968143,1.,0.999104400890347,
0.9984288220563),(0.999326490452125,0.999646063968143,1.,0.999104400890347,
0.9984288220563)))
REPRESENTATION_ITEM('')
SURFACE()
);
#497=(
BOUNDED_SURFACE()
B_SPLINE_SURFACE(1,2,((#86682,#86683,#86684),(#86685,#86686,#86687),(#86688,
#86689,#86690)),.UNSPECIFIED.,.F.,.F.,.F.)
B_SPLINE_SURFACE_WITH_KNOTS((2,1,2),(3,3),(0.,1.,1.01),(0.0255903596131801,
0.0375948596693875),.UNSPECIFIED.)
GEOMETRIC_REPRESENTATION_ITEM()
RATIONAL_B_SPLINE_SURFACE(((0.996753121755999,0.997505687613148,0.999678813023853),
(0.996753121755999,0.997505687613148,0.999678813023853),(0.996753121755999,
0.997505687613148,0.999678813023853)))
REPRESENTATION_ITEM('')
SURFACE()
);
#498=(
BOUNDED_SURFACE()
B_SPLINE_SURFACE(1,2,((#86725,#86726,#86727),(#86728,#86729,#86730),(#86731,
#86732,#86733)),.UNSPECIFIED.,.F.,.F.,.F.)
B_SPLINE_SURFACE_WITH_KNOTS((2,1,2),(3,3),(-0.00286823356225963,0.,0.477902879804001),
(0.0265907346180617,0.0331702037252925),.UNSPECIFIED.)
GEOMETRIC_REPRESENTATION_ITEM()
RATIONAL_B_SPLINE_SURFACE(((0.996888414395785,0.997365765479939,0.998269846384985),
(0.996888414395785,0.997365765479939,0.998269846384985),(0.996888414395785,
0.997365765479939,0.998269846384985)))
REPRESENTATION_ITEM('')
SURFACE()
);
#499=(
BOUNDED_SURFACE()
B_SPLINE_SURFACE(1,2,((#86800,#86801,#86802),(#86803,#86804,#86805),(#86806,
#86807,#86808)),.UNSPECIFIED.,.F.,.F.,.F.)
B_SPLINE_SURFACE_WITH_KNOTS((2,1,2),(3,3),(-0.0028675312820472,0.,0.477902879803021),
(0.0166015299238958,0.023173678811189),.UNSPECIFIED.)
GEOMETRIC_REPRESENTATION_ITEM()
RATIONAL_B_SPLINE_SURFACE(((0.996422581660833,0.996252244737342,0.996507688616404),
(0.996422581660833,0.996252244737342,0.996507688616404),(0.996422581660833,
0.996252244737342,0.996507688616404)))
REPRESENTATION_ITEM('')
SURFACE()
);
#500=(
BOUNDED_SURFACE()
B_SPLINE_SURFACE(1,2,((#86825,#86826,#86827),(#86828,#86829,#86830),(#86831,
#86832,#86833),(#86834,#86835,#86836)),.UNSPECIFIED.,.F.,.F.,.F.)
B_SPLINE_SURFACE_WITH_KNOTS((2,1,1,2),(3,3),(-0.0101,0.,1.,1.01),(0.00560769168370729,
0.0176009700440515),.UNSPECIFIED.)
GEOMETRIC_REPRESENTATION_ITEM()
RATIONAL_B_SPLINE_SURFACE(((0.99818389211382,0.99657330421516,0.996380621259469),
(0.99818389211382,0.99657330421516,0.996380621259469),(0.99818389211382,
0.99657330421516,0.996380621259469),(0.99818389211382,0.99657330421516,
0.996380621259469)))
REPRESENTATION_ITEM('')
SURFACE()
);
#501=(
BOUNDED_SURFACE()
B_SPLINE_SURFACE(1,2,((#86871,#86872,#86873),(#86874,#86875,#86876),(#86877,
#86878,#86879)),.UNSPECIFIED.,.F.,.F.,.F.)
B_SPLINE_SURFACE_WITH_KNOTS((2,1,2),(3,3),(-0.00206901892633123,0.,0.346769728512148),
(0.00660713154698074,0.0131849431468902),.UNSPECIFIED.)
GEOMETRIC_REPRESENTATION_ITEM()
RATIONAL_B_SPLINE_SURFACE(((0.997925307359502,0.997106772384955,0.99671475225386),
(0.997925307359502,0.997106772384955,0.99671475225386),(0.997925307359502,
0.997106772384955,0.99671475225386)))
REPRESENTATION_ITEM('')
SURFACE()
);
#502=(
BOUNDED_SURFACE()
B_SPLINE_SURFACE(1,2,((#86952,#86953,#86954),(#86955,#86956,#86957)),
 .UNSPECIFIED.,.F.,.F.,.F.)
B_SPLINE_SURFACE_WITH_KNOTS((2,2),(3,3),(0.,1.),(0.0556006976418428,0.0675888856590498),
 .UNSPECIFIED.)
GEOMETRIC_REPRESENTATION_ITEM()
RATIONAL_B_SPLINE_SURFACE(((0.996397562408606,0.996150386832629,0.997319912843745),
(0.996397562408606,0.996150386832629,0.997319912843745)))
REPRESENTATION_ITEM('')
SURFACE()
);
#503=(
BOUNDED_SURFACE()
B_SPLINE_SURFACE(1,2,((#87026,#87027,#87028),(#87029,#87030,#87031),(#87032,
#87033,#87034)),.UNSPECIFIED.,.F.,.F.,.F.)
B_SPLINE_SURFACE_WITH_KNOTS((2,1,2),(3,3),(0.,1.,1.01),(0.0456081671210065,
0.0575989447818823),.UNSPECIFIED.)
GEOMETRIC_REPRESENTATION_ITEM()
RATIONAL_B_SPLINE_SURFACE(((0.997793907739636,0.996365558499688,0.996354522974128),
(0.997793907739636,0.996365558499688,0.996354522974128),(0.997793907739636,
0.996365558499688,0.996354522974128)))
REPRESENTATION_ITEM('')
SURFACE()
);
#504=(
BOUNDED_SURFACE()
B_SPLINE_SURFACE(1,2,((#87069,#87070,#87071),(#87072,#87073,#87074),(#87075,
#87076,#87077)),.UNSPECIFIED.,.F.,.F.,.F.)
B_SPLINE_SURFACE_WITH_KNOTS((2,1,2),(3,3),(-0.00286810173493617,0.,0.477902879807942),
(0.046607398592912,0.0531834929157968),.UNSPECIFIED.)
GEOMETRIC_REPRESENTATION_ITEM()
RATIONAL_B_SPLINE_SURFACE(((0.997565691989291,0.996847118055594,0.996554836292953),
(0.997565691989291,0.996847118055594,0.996554836292953),(0.997565691989291,
0.996847118055594,0.996554836292953)))
REPRESENTATION_ITEM('')
SURFACE()
);
#505=(
BOUNDED_SURFACE()
B_SPLINE_SURFACE(1,2,((#87094,#87095,#87096,#87097,#87098),(#87099,#87100,
#87101,#87102,#87103),(#87104,#87105,#87106,#87107,#87108)),
 .UNSPECIFIED.,.F.,.F.,.F.)
B_SPLINE_SURFACE_WITH_KNOTS((2,1,2),(3,2,3),(0.,1.,1.01),(0.0355931932713904,
0.0384615384615384,0.0476086899858133),.UNSPECIFIED.)
GEOMETRIC_REPRESENTATION_ITEM()
RATIONAL_B_SPLINE_SURFACE(((0.998993602249807,0.999456249886298,1.,0.998265981131401,
0.997356751596327),(0.998993602249807,0.999456249886298,1.,0.998265981131401,
0.997356751596327),(0.998993602249807,0.999456249886298,1.,0.998265981131401,
0.997356751596327)))
REPRESENTATION_ITEM('')
SURFACE()
);
#506=(
BOUNDED_SURFACE()
B_SPLINE_SURFACE(1,2,((#87156,#87157,#87158,#87159,#87160),(#87161,#87162,
#87163,#87164,#87165),(#87166,#87167,#87168,#87169,#87170)),
 .UNSPECIFIED.,.F.,.F.,.F.)
B_SPLINE_SURFACE_WITH_KNOTS((2,1,2),(3,2,3),(-0.00141401191198266,0.,0.48077029710071),
(0.0365944846645759,0.0384615384615384,0.0431859280915189),
 .UNSPECIFIED.)
GEOMETRIC_REPRESENTATION_ITEM()
RATIONAL_B_SPLINE_SURFACE(((0.999326490452258,0.999646063968217,1.,0.999104400890347,
0.9984288220563),(0.999326490452258,0.999646063968217,1.,0.999104400890347,
0.9984288220563),(0.999326490452258,0.999646063968217,1.,0.999104400890347,
0.9984288220563)))
REPRESENTATION_ITEM('')
SURFACE()
);
#507=(
BOUNDED_SURFACE()
B_SPLINE_SURFACE(1,2,((#87197,#87198,#87199),(#87200,#87201,#87202),(#87203,
#87204,#87205)),.UNSPECIFIED.,.F.,.F.,.F.)
B_SPLINE_SURFACE_WITH_KNOTS((2,1,2),(3,3),(0.,1.,1.01),(0.0255903596131819,
0.0375948596693869),.UNSPECIFIED.)
GEOMETRIC_REPRESENTATION_ITEM()
RATIONAL_B_SPLINE_SURFACE(((0.996753121755999,0.997505687613148,0.999678813023853),
(0.996753121755999,0.997505687613148,0.999678813023853),(0.996753121755999,
0.997505687613148,0.999678813023853)))
REPRESENTATION_ITEM('')
SURFACE()
);
#508=(
BOUNDED_SURFACE()
B_SPLINE_SURFACE(1,2,((#87240,#87241,#87242),(#87243,#87244,#87245),(#87246,
#87247,#87248)),.UNSPECIFIED.,.F.,.F.,.F.)
B_SPLINE_SURFACE_WITH_KNOTS((2,1,2),(3,3),(-0.00286823356225022,0.,0.477902879806047),
(0.0265907346180628,0.0331702037252935),.UNSPECIFIED.)
GEOMETRIC_REPRESENTATION_ITEM()
RATIONAL_B_SPLINE_SURFACE(((0.996888414395785,0.997365765479939,0.998269846384985),
(0.996888414395785,0.997365765479939,0.998269846384985),(0.996888414395785,
0.997365765479939,0.998269846384985)))
REPRESENTATION_ITEM('')
SURFACE()
);
#509=(
BOUNDED_SURFACE()
B_SPLINE_SURFACE(1,2,((#87315,#87316,#87317),(#87318,#87319,#87320),(#87321,
#87322,#87323)),.UNSPECIFIED.,.F.,.F.,.F.)
B_SPLINE_SURFACE_WITH_KNOTS((2,1,2),(3,3),(-0.00286753074368029,0.,0.47790287980504),
(0.0166015299238948,0.0231736788028833),.UNSPECIFIED.)
GEOMETRIC_REPRESENTATION_ITEM()
RATIONAL_B_SPLINE_SURFACE(((0.996422581660833,0.996252244737556,0.996507688615758),
(0.996422581660833,0.996252244737556,0.996507688615758),(0.996422581660833,
0.996252244737556,0.996507688615758)))
REPRESENTATION_ITEM('')
SURFACE()
);
#510=(
BOUNDED_SURFACE()
B_SPLINE_SURFACE(1,2,((#87340,#87341,#87342),(#87343,#87344,#87345),(#87346,
#87347,#87348),(#87349,#87350,#87351)),.UNSPECIFIED.,.F.,.F.,.F.)
B_SPLINE_SURFACE_WITH_KNOTS((2,1,1,2),(3,3),(-0.0101,0.,1.,1.01),(0.00560769168370531,
0.0176009700440506),.UNSPECIFIED.)
GEOMETRIC_REPRESENTATION_ITEM()
RATIONAL_B_SPLINE_SURFACE(((0.99818389211382,0.99657330421516,0.996380621259469),
(0.99818389211382,0.99657330421516,0.996380621259469),(0.99818389211382,
0.99657330421516,0.996380621259469),(0.99818389211382,0.99657330421516,
0.996380621259469)))
REPRESENTATION_ITEM('')
SURFACE()
);
#511=(
BOUNDED_SURFACE()
B_SPLINE_SURFACE(1,2,((#87386,#87387,#87388),(#87389,#87390,#87391),(#87392,
#87393,#87394)),.UNSPECIFIED.,.F.,.F.,.F.)
B_SPLINE_SURFACE_WITH_KNOTS((2,1,2),(3,3),(-0.00206901892636993,0.,0.346769728513067),
(0.00660713154698595,0.0131849431468901),.UNSPECIFIED.)
GEOMETRIC_REPRESENTATION_ITEM()
RATIONAL_B_SPLINE_SURFACE(((0.997925307359501,0.997106772384955,0.99671475225386),
(0.997925307359501,0.997106772384955,0.99671475225386),(0.997925307359501,
0.997106772384955,0.99671475225386)))
REPRESENTATION_ITEM('')
SURFACE()
);
#512=(
BOUNDED_SURFACE()
B_SPLINE_SURFACE(1,2,((#87467,#87468,#87469),(#87470,#87471,#87472)),
 .UNSPECIFIED.,.F.,.F.,.F.)
B_SPLINE_SURFACE_WITH_KNOTS((2,2),(3,3),(0.,1.),(0.0556006976418437,0.0675888856590502),
 .UNSPECIFIED.)
GEOMETRIC_REPRESENTATION_ITEM()
RATIONAL_B_SPLINE_SURFACE(((0.996397562408606,0.996150386832629,0.997319912843745),
(0.996397562408606,0.996150386832629,0.997319912843745)))
REPRESENTATION_ITEM('')
SURFACE()
);
#513=(
BOUNDED_SURFACE()
B_SPLINE_SURFACE(1,2,((#87541,#87542,#87543),(#87544,#87545,#87546),(#87547,
#87548,#87549)),.UNSPECIFIED.,.F.,.F.,.F.)
B_SPLINE_SURFACE_WITH_KNOTS((2,1,2),(3,3),(0.,1.,1.01),(0.0456081671210055,
0.0575989447818823),.UNSPECIFIED.)
GEOMETRIC_REPRESENTATION_ITEM()
RATIONAL_B_SPLINE_SURFACE(((0.997793907739636,0.996365558499688,0.996354522974128),
(0.997793907739636,0.996365558499688,0.996354522974128),(0.997793907739636,
0.996365558499688,0.996354522974128)))
REPRESENTATION_ITEM('')
SURFACE()
);
#514=(
BOUNDED_SURFACE()
B_SPLINE_SURFACE(1,2,((#87584,#87585,#87586),(#87587,#87588,#87589),(#87590,
#87591,#87592)),.UNSPECIFIED.,.F.,.F.,.F.)
B_SPLINE_SURFACE_WITH_KNOTS((2,1,2),(3,3),(-0.00286810173500546,0.,0.477902879809462),
(0.0466073985929117,0.0531834929157977),.UNSPECIFIED.)
GEOMETRIC_REPRESENTATION_ITEM()
RATIONAL_B_SPLINE_SURFACE(((0.997565691989291,0.996847118055593,0.996554836292953),
(0.997565691989291,0.996847118055593,0.996554836292953),(0.997565691989291,
0.996847118055593,0.996554836292953)))
REPRESENTATION_ITEM('')
SURFACE()
);
#515=(
BOUNDED_SURFACE()
B_SPLINE_SURFACE(1,2,((#87609,#87610,#87611,#87612,#87613),(#87614,#87615,
#87616,#87617,#87618),(#87619,#87620,#87621,#87622,#87623)),
 .UNSPECIFIED.,.F.,.F.,.F.)
B_SPLINE_SURFACE_WITH_KNOTS((2,1,2),(3,2,3),(0.,1.,1.01),(0.0355931932713903,
0.0384615384615384,0.0476086899858143),.UNSPECIFIED.)
GEOMETRIC_REPRESENTATION_ITEM()
RATIONAL_B_SPLINE_SURFACE(((0.998993602249807,0.999456249886298,1.,0.998265981131401,
0.997356751596327),(0.998993602249807,0.999456249886298,1.,0.998265981131401,
0.997356751596327),(0.998993602249807,0.999456249886298,1.,0.998265981131401,
0.997356751596327)))
REPRESENTATION_ITEM('')
SURFACE()
);
#516=(
BOUNDED_SURFACE()
B_SPLINE_SURFACE(1,2,((#87671,#87672,#87673,#87674,#87675),(#87676,#87677,
#87678,#87679,#87680),(#87681,#87682,#87683,#87684,#87685)),
 .UNSPECIFIED.,.F.,.F.,.F.)
B_SPLINE_SURFACE_WITH_KNOTS((2,1,2),(3,2,3),(-0.00286743095205352,0.,0.480770297168586),
(0.0365944846642022,0.0384615384615384,0.04318592809152),.UNSPECIFIED.)
GEOMETRIC_REPRESENTATION_ITEM()
RATIONAL_B_SPLINE_SURFACE(((0.999326490452131,0.999646063968146,1.,0.999104400890347,
0.9984288220563),(0.999326490452131,0.999646063968146,1.,0.999104400890347,
0.998428822056299),(0.999326490452131,0.999646063968146,1.,0.999104400890347,
0.998428822056299)))
REPRESENTATION_ITEM('')
SURFACE()
);
#517=(
BOUNDED_SURFACE()
B_SPLINE_SURFACE(1,2,((#87712,#87713,#87714),(#87715,#87716,#87717),(#87718,
#87719,#87720)),.UNSPECIFIED.,.F.,.F.,.F.)
B_SPLINE_SURFACE_WITH_KNOTS((2,1,2),(3,3),(0.,1.,1.01),(0.025590359613181,
0.0375948596693874),.UNSPECIFIED.)
GEOMETRIC_REPRESENTATION_ITEM()
RATIONAL_B_SPLINE_SURFACE(((0.996753121755999,0.997505687613148,0.999678813023853),
(0.996753121755999,0.997505687613148,0.999678813023853),(0.996753121755999,
0.997505687613148,0.999678813023853)))
REPRESENTATION_ITEM('')
SURFACE()
);
#518=(
BOUNDED_SURFACE()
B_SPLINE_SURFACE(1,2,((#87755,#87756,#87757),(#87758,#87759,#87760),(#87761,
#87762,#87763)),.UNSPECIFIED.,.F.,.F.,.F.)
B_SPLINE_SURFACE_WITH_KNOTS((2,1,2),(3,3),(-0.00286823356227653,0.,0.477902879807841),
(0.0265907346180622,0.0331702037252924),.UNSPECIFIED.)
GEOMETRIC_REPRESENTATION_ITEM()
RATIONAL_B_SPLINE_SURFACE(((0.996888414395785,0.997365765479939,0.998269846384985),
(0.996888414395785,0.997365765479939,0.998269846384985),(0.996888414395785,
0.997365765479939,0.998269846384985)))
REPRESENTATION_ITEM('')
SURFACE()
);
#519=(
BOUNDED_SURFACE()
B_SPLINE_SURFACE(1,2,((#87830,#87831,#87832),(#87833,#87834,#87835),(#87836,
#87837,#87838)),.UNSPECIFIED.,.F.,.F.,.F.)
B_SPLINE_SURFACE_WITH_KNOTS((2,1,2),(3,3),(-0.00286753128216935,0.,0.477902879807046),
(0.0166015299238956,0.0231736788111884),.UNSPECIFIED.)
GEOMETRIC_REPRESENTATION_ITEM()
RATIONAL_B_SPLINE_SURFACE(((0.996422581660833,0.996252244737342,0.996507688616404),
(0.996422581660833,0.996252244737342,0.996507688616404),(0.996422581660833,
0.996252244737342,0.996507688616404)))
REPRESENTATION_ITEM('')
SURFACE()
);
#520=(
BOUNDED_SURFACE()
B_SPLINE_SURFACE(1,2,((#87855,#87856,#87857),(#87858,#87859,#87860),(#87861,
#87862,#87863),(#87864,#87865,#87866)),.UNSPECIFIED.,.F.,.F.,.F.)
B_SPLINE_SURFACE_WITH_KNOTS((2,1,1,2),(3,3),(-0.0101,0.,1.,1.01),(0.00560769168370714,
0.0176009700440521),.UNSPECIFIED.)
GEOMETRIC_REPRESENTATION_ITEM()
RATIONAL_B_SPLINE_SURFACE(((0.99818389211382,0.99657330421516,0.996380621259469),
(0.99818389211382,0.99657330421516,0.996380621259469),(0.99818389211382,
0.99657330421516,0.996380621259469),(0.99818389211382,0.99657330421516,
0.996380621259469)))
REPRESENTATION_ITEM('')
SURFACE()
);
#521=(
BOUNDED_SURFACE()
B_SPLINE_SURFACE(1,2,((#87901,#87902,#87903),(#87904,#87905,#87906),(#87907,
#87908,#87909)),.UNSPECIFIED.,.F.,.F.,.F.)
B_SPLINE_SURFACE_WITH_KNOTS((2,1,2),(3,3),(-0.00206901892643086,0.,0.346769728513646),
(0.00660713154699298,0.0131849431468898),.UNSPECIFIED.)
GEOMETRIC_REPRESENTATION_ITEM()
RATIONAL_B_SPLINE_SURFACE(((0.997925307359499,0.997106772384954,0.99671475225386),
(0.997925307359499,0.997106772384954,0.99671475225386),(0.997925307359499,
0.997106772384954,0.99671475225386)))
REPRESENTATION_ITEM('')
SURFACE()
);
#522=(
BOUNDED_SURFACE()
B_SPLINE_SURFACE(1,2,((#87982,#87983,#87984),(#87985,#87986,#87987)),
 .UNSPECIFIED.,.F.,.F.,.F.)
B_SPLINE_SURFACE_WITH_KNOTS((2,2),(3,3),(0.,1.),(0.0556006976418426,0.0675888856590509),
 .UNSPECIFIED.)
GEOMETRIC_REPRESENTATION_ITEM()
RATIONAL_B_SPLINE_SURFACE(((0.996397562408606,0.996150386832629,0.997319912843745),
(0.996397562408606,0.996150386832629,0.997319912843745)))
REPRESENTATION_ITEM('')
SURFACE()
);
#523=(
BOUNDED_SURFACE()
B_SPLINE_SURFACE(1,2,((#88056,#88057,#88058),(#88059,#88060,#88061),(#88062,
#88063,#88064)),.UNSPECIFIED.,.F.,.F.,.F.)
B_SPLINE_SURFACE_WITH_KNOTS((2,1,2),(3,3),(0.,1.,1.01),(0.0456081671207015,
0.0575989447852278),.UNSPECIFIED.)
GEOMETRIC_REPRESENTATION_ITEM()
RATIONAL_B_SPLINE_SURFACE(((0.997793907739708,0.99636555849929,0.996354522974122),
(0.997793907739708,0.99636555849929,0.996354522974122),(0.997793907739708,
0.99636555849929,0.996354522974122)))
REPRESENTATION_ITEM('')
SURFACE()
);
#524=(
BOUNDED_SURFACE()
B_SPLINE_SURFACE(1,2,((#88099,#88100,#88101),(#88102,#88103,#88104),(#88105,
#88106,#88107)),.UNSPECIFIED.,.F.,.F.,.F.)
B_SPLINE_SURFACE_WITH_KNOTS((2,1,2),(3,3),(-0.00286810173509,0.,0.477902879810816),
(0.0466073985929116,0.053183492915798),.UNSPECIFIED.)
GEOMETRIC_REPRESENTATION_ITEM()
RATIONAL_B_SPLINE_SURFACE(((0.997565691989291,0.996847118055594,0.996554836292953),
(0.997565691989291,0.996847118055594,0.996554836292953),(0.997565691989291,
0.996847118055594,0.996554836292953)))
REPRESENTATION_ITEM('')
SURFACE()
);
#525=(
BOUNDED_SURFACE()
B_SPLINE_SURFACE(1,2,((#88124,#88125,#88126,#88127,#88128),(#88129,#88130,
#88131,#88132,#88133),(#88134,#88135,#88136,#88137,#88138)),
 .UNSPECIFIED.,.F.,.F.,.F.)
B_SPLINE_SURFACE_WITH_KNOTS((2,1,2),(3,2,3),(0.,1.,1.01),(0.0355931932713903,
0.0384615384615384,0.0476086899858139),.UNSPECIFIED.)
GEOMETRIC_REPRESENTATION_ITEM()
RATIONAL_B_SPLINE_SURFACE(((0.998993602249807,0.999456249886298,1.,0.998265981131401,
0.997356751596327),(0.998993602249807,0.999456249886298,1.,0.998265981131401,
0.997356751596327),(0.998993602249807,0.999456249886298,1.,0.998265981131401,
0.997356751596327)))
REPRESENTATION_ITEM('')
SURFACE()
);
#526=(
BOUNDED_SURFACE()
B_SPLINE_SURFACE(1,2,((#88186,#88187,#88188,#88189,#88190),(#88191,#88192,
#88193,#88194,#88195),(#88196,#88197,#88198,#88199,#88200)),
 .UNSPECIFIED.,.F.,.F.,.F.)
B_SPLINE_SURFACE_WITH_KNOTS((2,1,2),(3,2,3),(-0.00141401191198401,0.,0.480770297103859),
(0.0365944846645752,0.0384615384615384,0.0431859280915187),
 .UNSPECIFIED.)
GEOMETRIC_REPRESENTATION_ITEM()
RATIONAL_B_SPLINE_SURFACE(((0.999326490452258,0.999646063968217,1.,0.999104400890347,
0.9984288220563),(0.999326490452258,0.999646063968217,1.,0.999104400890347,
0.9984288220563),(0.999326490452258,0.999646063968217,1.,0.999104400890347,
0.9984288220563)))
REPRESENTATION_ITEM('')
SURFACE()
);
#527=(
BOUNDED_SURFACE()
B_SPLINE_SURFACE(1,2,((#88227,#88228,#88229),(#88230,#88231,#88232),(#88233,
#88234,#88235)),.UNSPECIFIED.,.F.,.F.,.F.)
B_SPLINE_SURFACE_WITH_KNOTS((2,1,2),(3,3),(0.,1.,1.01),(0.0255903596131799,
0.0375948596693882),.UNSPECIFIED.)
GEOMETRIC_REPRESENTATION_ITEM()
RATIONAL_B_SPLINE_SURFACE(((0.996753121755999,0.997505687613148,0.999678813023854),
(0.996753121755999,0.997505687613148,0.999678813023854),(0.996753121755999,
0.997505687613148,0.999678813023854)))
REPRESENTATION_ITEM('')
SURFACE()
);
#528=(
BOUNDED_SURFACE()
B_SPLINE_SURFACE(1,2,((#88270,#88271,#88272),(#88273,#88274,#88275),(#88276,
#88277,#88278)),.UNSPECIFIED.,.F.,.F.,.F.)
B_SPLINE_SURFACE_WITH_KNOTS((2,1,2),(3,3),(-0.00286823356231214,0.,0.477902879809393),
(0.0265907346180619,0.033170203725292),.UNSPECIFIED.)
GEOMETRIC_REPRESENTATION_ITEM()
RATIONAL_B_SPLINE_SURFACE(((0.996888414395785,0.997365765479939,0.998269846384985),
(0.996888414395785,0.997365765479939,0.998269846384985),(0.996888414395785,
0.997365765479939,0.998269846384985)))
REPRESENTATION_ITEM('')
SURFACE()
);
#529=(
BOUNDED_SURFACE()
B_SPLINE_SURFACE(1,2,((#88345,#88346,#88347),(#88348,#88349,#88350),(#88351,
#88352,#88353)),.UNSPECIFIED.,.F.,.F.,.F.)
B_SPLINE_SURFACE_WITH_KNOTS((2,1,2),(3,3),(-0.00286753074372667,0.,0.477902879808682),
(0.0166015299238963,0.023173678802884),.UNSPECIFIED.)
GEOMETRIC_REPRESENTATION_ITEM()
RATIONAL_B_SPLINE_SURFACE(((0.996422581660833,0.996252244737557,0.996507688615759),
(0.996422581660833,0.996252244737557,0.996507688615759),(0.996422581660833,
0.996252244737557,0.996507688615759)))
REPRESENTATION_ITEM('')
SURFACE()
);
#530=(
BOUNDED_SURFACE()
B_SPLINE_SURFACE(1,2,((#88370,#88371,#88372),(#88373,#88374,#88375),(#88376,
#88377,#88378),(#88379,#88380,#88381)),.UNSPECIFIED.,.F.,.F.,.F.)
B_SPLINE_SURFACE_WITH_KNOTS((2,1,1,2),(3,3),(-0.0101,0.,1.,1.01),(0.00560769168370498,
0.0176009700440528),.UNSPECIFIED.)
GEOMETRIC_REPRESENTATION_ITEM()
RATIONAL_B_SPLINE_SURFACE(((0.998183892113821,0.99657330421516,0.996380621259469),
(0.998183892113821,0.99657330421516,0.996380621259469),(0.998183892113821,
0.99657330421516,0.996380621259469),(0.998183892113821,0.99657330421516,
0.996380621259469)))
REPRESENTATION_ITEM('')
SURFACE()
);
#531=(
BOUNDED_SURFACE()
B_SPLINE_SURFACE(1,2,((#88416,#88417,#88418),(#88419,#88420,#88421),(#88422,
#88423,#88424)),.UNSPECIFIED.,.F.,.F.,.F.)
B_SPLINE_SURFACE_WITH_KNOTS((2,1,2),(3,3),(-0.00206901892651131,0.,0.346769728514169),
(0.00660713154700106,0.0131849431468915),.UNSPECIFIED.)
GEOMETRIC_REPRESENTATION_ITEM()
RATIONAL_B_SPLINE_SURFACE(((0.997925307359498,0.997106772384953,0.99671475225386),
(0.997925307359498,0.997106772384953,0.99671475225386),(0.997925307359498,
0.997106772384953,0.99671475225386)))
REPRESENTATION_ITEM('')
SURFACE()
);
#532=(
BOUNDED_SURFACE()
B_SPLINE_SURFACE(1,2,((#88506,#88507,#88508),(#88509,#88510,#88511),(#88512,
#88513,#88514)),.UNSPECIFIED.,.F.,.F.,.F.)
B_SPLINE_SURFACE_WITH_KNOTS((2,1,2),(3,3),(-0.01,0.,1.),(0.0556006976418415,
0.0675888856590499),.UNSPECIFIED.)
GEOMETRIC_REPRESENTATION_ITEM()
RATIONAL_B_SPLINE_SURFACE(((0.996397562408606,0.996150386832629,0.997319912843745),
(0.996397562408606,0.996150386832629,0.997319912843745),(0.996397562408606,
0.996150386832629,0.997319912843745)))
REPRESENTATION_ITEM('')
SURFACE()
);
#533=(
BOUNDED_SURFACE()
B_SPLINE_SURFACE(1,2,((#88574,#88575,#88576),(#88577,#88578,#88579)),
 .UNSPECIFIED.,.F.,.F.,.F.)
B_SPLINE_SURFACE_WITH_KNOTS((2,2),(3,3),(0.,1.),(0.0456081671210044,0.0575989447818823),
 .UNSPECIFIED.)
GEOMETRIC_REPRESENTATION_ITEM()
RATIONAL_B_SPLINE_SURFACE(((0.997793907739636,0.996365558499688,0.996354522974128),
(0.997793907739636,0.996365558499688,0.996354522974128)))
REPRESENTATION_ITEM('')
SURFACE()
);
#534=(
BOUNDED_SURFACE()
B_SPLINE_SURFACE(1,2,((#88646,#88647,#88648,#88649,#88650),(#88651,#88652,
#88653,#88654,#88655),(#88656,#88657,#88658,#88659,#88660)),
 .UNSPECIFIED.,.F.,.F.,.F.)
B_SPLINE_SURFACE_WITH_KNOTS((2,1,2),(3,2,3),(0.,1.,1.01),(0.0355931932713903,
0.0384615384615384,0.0476086899858139),.UNSPECIFIED.)
GEOMETRIC_REPRESENTATION_ITEM()
RATIONAL_B_SPLINE_SURFACE(((0.998993602249807,0.999456249886298,1.,0.998265981131401,
0.997356751596327),(0.998993602249807,0.999456249886298,1.,0.998265981131401,
0.997356751596327),(0.998993602249807,0.999456249886298,1.,0.998265981131401,
0.997356751596327)))
REPRESENTATION_ITEM('')
SURFACE()
);
#535=(
BOUNDED_SURFACE()
B_SPLINE_SURFACE(1,2,((#88708,#88709,#88710,#88711,#88712),(#88713,#88714,
#88715,#88716,#88717),(#88718,#88719,#88720,#88721,#88722)),
 .UNSPECIFIED.,.F.,.F.,.F.)
B_SPLINE_SURFACE_WITH_KNOTS((2,1,2),(3,2,3),(-0.0014140119119827,0.,0.480770297104947),
(0.0365944846645793,0.0384615384615384,0.0431859280915189),
 .UNSPECIFIED.)
GEOMETRIC_REPRESENTATION_ITEM()
RATIONAL_B_SPLINE_SURFACE(((0.99932649045226,0.999646063968218,1.,0.999104400890347,
0.9984288220563),(0.99932649045226,0.999646063968218,1.,0.999104400890347,
0.9984288220563),(0.99932649045226,0.999646063968218,1.,0.999104400890347,
0.9984288220563)))
REPRESENTATION_ITEM('')
SURFACE()
);
#536=(
BOUNDED_SURFACE()
B_SPLINE_SURFACE(1,2,((#88749,#88750,#88751),(#88752,#88753,#88754),(#88755,
#88756,#88757)),.UNSPECIFIED.,.F.,.F.,.F.)
B_SPLINE_SURFACE_WITH_KNOTS((2,1,2),(3,3),(0.,1.,1.01),(0.0255903596131785,
0.0375948596693877),.UNSPECIFIED.)
GEOMETRIC_REPRESENTATION_ITEM()
RATIONAL_B_SPLINE_SURFACE(((0.996753121755999,0.997505687613148,0.999678813023853),
(0.996753121755999,0.997505687613148,0.999678813023853),(0.996753121755999,
0.997505687613148,0.999678813023853)))
REPRESENTATION_ITEM('')
SURFACE()
);
#537=(
BOUNDED_SURFACE()
B_SPLINE_SURFACE(1,2,((#88792,#88793,#88794),(#88795,#88796,#88797),(#88798,
#88799,#88800)),.UNSPECIFIED.,.F.,.F.,.F.)
B_SPLINE_SURFACE_WITH_KNOTS((2,1,2),(3,3),(-0.00286823356223954,0.,0.477902879810711),
(0.0265907346180618,0.0331702037252911),.UNSPECIFIED.)
GEOMETRIC_REPRESENTATION_ITEM()
RATIONAL_B_SPLINE_SURFACE(((0.996888414395785,0.997365765479939,0.998269846384985),
(0.996888414395785,0.997365765479939,0.998269846384985),(0.996888414395785,
0.997365765479939,0.998269846384985)))
REPRESENTATION_ITEM('')
SURFACE()
);
#538=(
BOUNDED_SURFACE()
B_SPLINE_SURFACE(1,2,((#88867,#88868,#88869),(#88870,#88871,#88872),(#88873,
#88874,#88875)),.UNSPECIFIED.,.F.,.F.,.F.)
B_SPLINE_SURFACE_WITH_KNOTS((2,1,2),(3,3),(-0.00286753128216343,0.,0.477902879810108),
(0.0166015299238955,0.0231736788111875),.UNSPECIFIED.)
GEOMETRIC_REPRESENTATION_ITEM()
RATIONAL_B_SPLINE_SURFACE(((0.996422581660833,0.996252244737342,0.996507688616404),
(0.996422581660833,0.996252244737342,0.996507688616404),(0.996422581660833,
0.996252244737342,0.996507688616404)))
REPRESENTATION_ITEM('')
SURFACE()
);
#539=(
BOUNDED_SURFACE()
B_SPLINE_SURFACE(1,2,((#88892,#88893,#88894),(#88895,#88896,#88897),(#88898,
#88899,#88900),(#88901,#88902,#88903)),.UNSPECIFIED.,.F.,.F.,.F.)
B_SPLINE_SURFACE_WITH_KNOTS((2,1,1,2),(3,3),(-0.0101,0.,1.,1.01),(0.00560769168370538,
0.0176009700440511),.UNSPECIFIED.)
GEOMETRIC_REPRESENTATION_ITEM()
RATIONAL_B_SPLINE_SURFACE(((0.99818389211382,0.99657330421516,0.996380621259469),
(0.99818389211382,0.99657330421516,0.996380621259469),(0.99818389211382,
0.99657330421516,0.996380621259469),(0.99818389211382,0.99657330421516,
0.996380621259469)))
REPRESENTATION_ITEM('')
SURFACE()
);
#540=(
BOUNDED_SURFACE()
B_SPLINE_SURFACE(1,2,((#88938,#88939,#88940),(#88941,#88942,#88943),(#88944,
#88945,#88946)),.UNSPECIFIED.,.F.,.F.,.F.)
B_SPLINE_SURFACE_WITH_KNOTS((2,1,2),(3,3),(-0.00206901892655097,0.,0.346769728514504),
(0.00660713154700985,0.0131849431468903),.UNSPECIFIED.)
GEOMETRIC_REPRESENTATION_ITEM()
RATIONAL_B_SPLINE_SURFACE(((0.997925307359495,0.997106772384953,0.99671475225386),
(0.997925307359495,0.997106772384953,0.99671475225386),(0.997925307359495,
0.997106772384953,0.99671475225386)))
REPRESENTATION_ITEM('')
SURFACE()
);
#541=(
BOUNDED_SURFACE()
B_SPLINE_SURFACE(1,2,((#88983,#88984,#88985),(#88986,#88987,#88988)),
 .UNSPECIFIED.,.F.,.F.,.F.)
B_SPLINE_SURFACE_WITH_KNOTS((2,2),(3,3),(0.,1.),(0.0556006976418414,0.0675888856590499),
 .UNSPECIFIED.)
GEOMETRIC_REPRESENTATION_ITEM()
RATIONAL_B_SPLINE_SURFACE(((0.996397562408606,0.996150386832629,0.997319912843745),
(0.996397562408606,0.996150386832629,0.997319912843745)))
REPRESENTATION_ITEM('')
SURFACE()
);
#542=(
BOUNDED_SURFACE()
B_SPLINE_SURFACE(1,2,((#89048,#89049,#89050),(#89051,#89052,#89053),(#89054,
#89055,#89056),(#89057,#89058,#89059)),.UNSPECIFIED.,.F.,.F.,.F.)
B_SPLINE_SURFACE_WITH_KNOTS((2,1,1,2),(3,3),(-0.01,0.,1.,1.0101),(0.0456081671210032,
0.0575989447818821),.UNSPECIFIED.)
GEOMETRIC_REPRESENTATION_ITEM()
RATIONAL_B_SPLINE_SURFACE(((0.997793907739636,0.996365558499688,0.996354522974128),
(0.997793907739636,0.996365558499688,0.996354522974128),(0.997793907739636,
0.996365558499688,0.996354522974128),(0.997793907739636,0.996365558499688,
0.996354522974128)))
REPRESENTATION_ITEM('')
SURFACE()
);
#543=(
BOUNDED_SURFACE()
B_SPLINE_SURFACE(1,2,((#89094,#89095,#89096),(#89097,#89098,#89099),(#89100,
#89101,#89102)),.UNSPECIFIED.,.F.,.F.,.F.)
B_SPLINE_SURFACE_WITH_KNOTS((2,1,2),(3,3),(-0.00286810173515549,0.,0.477902879812476),
(0.0466073985929118,0.0531834929157986),.UNSPECIFIED.)
GEOMETRIC_REPRESENTATION_ITEM()
RATIONAL_B_SPLINE_SURFACE(((0.997565691989291,0.996847118055593,0.996554836292953),
(0.997565691989291,0.996847118055593,0.996554836292953),(0.997565691989291,
0.996847118055593,0.996554836292953)))
REPRESENTATION_ITEM('')
SURFACE()
);
#544=(
BOUNDED_SURFACE()
B_SPLINE_SURFACE(1,2,((#89171,#89172,#89173,#89174,#89175),(#89176,#89177,
#89178,#89179,#89180)),.UNSPECIFIED.,.F.,.F.,.F.)
B_SPLINE_SURFACE_WITH_KNOTS((2,2),(3,2,3),(0.,0.480770297105795),(0.0365944846645799,
0.0384615384615384,0.0431859280915184),.UNSPECIFIED.)
GEOMETRIC_REPRESENTATION_ITEM()
RATIONAL_B_SPLINE_SURFACE(((0.99932649045226,0.999646063968218,1.,0.999104400890347,
0.9984288220563),(0.99932649045226,0.999646063968218,1.,0.999104400890347,
0.9984288220563)))
REPRESENTATION_ITEM('')
SURFACE()
);
#545=(
BOUNDED_SURFACE()
B_SPLINE_SURFACE(1,2,((#89196,#89197,#89198),(#89199,#89200,#89201),(#89202,
#89203,#89204)),.UNSPECIFIED.,.F.,.F.,.F.)
B_SPLINE_SURFACE_WITH_KNOTS((2,1,2),(3,3),(-0.000171761234198046,1.,1.00600020634825),
(0.066589869885604,0.0751324139120509),.UNSPECIFIED.)
GEOMETRIC_REPRESENTATION_ITEM()
RATIONAL_B_SPLINE_SURFACE(((0.997134830028879,0.997884084852109,0.999352698773416),
(0.997134830028879,0.997884084852109,0.999352698773416),(0.997134830028878,
0.997884084852109,0.999352698773416)))
REPRESENTATION_ITEM('')
SURFACE()
);
#546=(
BOUNDED_SURFACE()
B_SPLINE_SURFACE(1,2,((#89254,#89255,#89256),(#89257,#89258,#89259),(#89260,
#89261,#89262)),.UNSPECIFIED.,.F.,.F.,.F.)
B_SPLINE_SURFACE_WITH_KNOTS((2,1,2),(3,3),(0.,1.,1.01),(0.0255903596131786,
0.0375948596693877),.UNSPECIFIED.)
GEOMETRIC_REPRESENTATION_ITEM()
RATIONAL_B_SPLINE_SURFACE(((0.996753121755999,0.997505687613148,0.999678813023853),
(0.996753121755999,0.997505687613148,0.999678813023853),(0.996753121755999,
0.997505687613148,0.999678813023853)))
REPRESENTATION_ITEM('')
SURFACE()
);
#547=(
BOUNDED_SURFACE()
B_SPLINE_SURFACE(1,2,((#89297,#89298,#89299),(#89300,#89301,#89302),(#89303,
#89304,#89305)),.UNSPECIFIED.,.F.,.F.,.F.)
B_SPLINE_SURFACE_WITH_KNOTS((2,1,2),(3,3),(-0.00286823356227599,0.,0.477902879811651),
(0.0265907346180628,0.033170203725292),.UNSPECIFIED.)
GEOMETRIC_REPRESENTATION_ITEM()
RATIONAL_B_SPLINE_SURFACE(((0.996888414395785,0.997365765479939,0.998269846384985),
(0.996888414395785,0.997365765479939,0.998269846384985),(0.996888414395785,
0.997365765479939,0.998269846384985)))
REPRESENTATION_ITEM('')
SURFACE()
);
#548=(
BOUNDED_SURFACE()
B_SPLINE_SURFACE(1,2,((#89372,#89373,#89374),(#89375,#89376,#89377),(#89378,
#89379,#89380)),.UNSPECIFIED.,.F.,.F.,.F.)
B_SPLINE_SURFACE_WITH_KNOTS((2,1,2),(3,3),(-0.00286753074369785,0.,0.477902879811209),
(0.0166015299238962,0.0231736788028824),.UNSPECIFIED.)
GEOMETRIC_REPRESENTATION_ITEM()
RATIONAL_B_SPLINE_SURFACE(((0.996422581660833,0.996252244737557,0.996507688615759),
(0.996422581660833,0.996252244737557,0.996507688615759),(0.996422581660833,
0.996252244737558,0.996507688615759)))
REPRESENTATION_ITEM('')
SURFACE()
);
#549=(
BOUNDED_SURFACE()
B_SPLINE_SURFACE(1,2,((#89397,#89398,#89399),(#89400,#89401,#89402),(#89403,
#89404,#89405),(#89406,#89407,#89408)),.UNSPECIFIED.,.F.,.F.,.F.)
B_SPLINE_SURFACE_WITH_KNOTS((2,1,1,2),(3,3),(-0.0101,0.,1.,1.01),(0.00560769168370639,
0.0176009700440511),.UNSPECIFIED.)
GEOMETRIC_REPRESENTATION_ITEM()
RATIONAL_B_SPLINE_SURFACE(((0.99818389211382,0.99657330421516,0.996380621259469),
(0.99818389211382,0.99657330421516,0.996380621259469),(0.99818389211382,
0.99657330421516,0.996380621259469),(0.99818389211382,0.99657330421516,
0.996380621259469)))
REPRESENTATION_ITEM('')
SURFACE()
);
#550=(
BOUNDED_SURFACE()
B_SPLINE_SURFACE(1,2,((#89443,#89444,#89445),(#89446,#89447,#89448),(#89449,
#89450,#89451)),.UNSPECIFIED.,.F.,.F.,.F.)
B_SPLINE_SURFACE_WITH_KNOTS((2,1,2),(3,3),(-0.00206901892662418,0.,0.346769728514616),
(0.00660713154702066,0.0131849431468895),.UNSPECIFIED.)
GEOMETRIC_REPRESENTATION_ITEM()
RATIONAL_B_SPLINE_SURFACE(((0.997925307359492,0.997106772384953,0.99671475225386),
(0.997925307359492,0.997106772384953,0.99671475225386),(0.997925307359492,
0.997106772384953,0.99671475225386)))
REPRESENTATION_ITEM('')
SURFACE()
);
#551=(
BOUNDED_SURFACE()
B_SPLINE_SURFACE(1,2,((#89507,#89508,#89509),(#89510,#89511,#89512)),
 .UNSPECIFIED.,.F.,.F.,.F.)
B_SPLINE_SURFACE_WITH_KNOTS((2,2),(3,3),(0.,1.),(0.0456081671210045,0.0575989447818819),
 .UNSPECIFIED.)
GEOMETRIC_REPRESENTATION_ITEM()
RATIONAL_B_SPLINE_SURFACE(((0.997793907739636,0.996365558499688,0.996354522974128),
(0.997793907739636,0.996365558499688,0.996354522974128)))
REPRESENTATION_ITEM('')
SURFACE()
);
#552=(
BOUNDED_SURFACE()
B_SPLINE_SURFACE(1,2,((#89570,#89571,#89572,#89573,#89574),(#89575,#89576,
#89577,#89578,#89579),(#89580,#89581,#89582,#89583,#89584),(#89585,#89586,
#89587,#89588,#89589)),.UNSPECIFIED.,.F.,.F.,.F.)
B_SPLINE_SURFACE_WITH_KNOTS((2,1,1,2),(3,2,3),(-0.01,0.,1.,1.0101),(0.0355931932713904,
0.0384615384615384,0.0476086899858126),.UNSPECIFIED.)
GEOMETRIC_REPRESENTATION_ITEM()
RATIONAL_B_SPLINE_SURFACE(((0.998993602249807,0.999456249886298,1.,0.998265981131401,
0.997356751596327),(0.998993602249807,0.999456249886298,1.,0.998265981131401,
0.997356751596327),(0.998993602249807,0.999456249886298,1.,0.998265981131401,
0.997356751596327),(0.998993602249807,0.999456249886298,1.,0.998265981131401,
0.997356751596327)))
REPRESENTATION_ITEM('')
SURFACE()
);
#553=(
BOUNDED_SURFACE()
B_SPLINE_SURFACE(1,2,((#89637,#89638,#89639,#89640,#89641),(#89642,#89643,
#89644,#89645,#89646),(#89647,#89648,#89649,#89650,#89651)),
 .UNSPECIFIED.,.F.,.F.,.F.)
B_SPLINE_SURFACE_WITH_KNOTS((2,1,2),(3,2,3),(-0.00141401191197939,0.,0.480770297106305),
(0.0365944846645761,0.0384615384615384,0.0431859280915181),
 .UNSPECIFIED.)
GEOMETRIC_REPRESENTATION_ITEM()
RATIONAL_B_SPLINE_SURFACE(((0.999326490452259,0.999646063968217,1.,0.999104400890347,
0.9984288220563),(0.999326490452259,0.999646063968217,1.,0.999104400890347,
0.9984288220563),(0.999326490452259,0.999646063968217,1.,0.999104400890347,
0.9984288220563)))
REPRESENTATION_ITEM('')
SURFACE()
);
#554=(
BOUNDED_SURFACE()
B_SPLINE_SURFACE(1,2,((#89659,#89660,#89661),(#89662,#89663,#89664)),
 .UNSPECIFIED.,.F.,.F.,.F.)
B_SPLINE_SURFACE_WITH_KNOTS((2,2),(3,3),(0.,1.),(0.02559035961318,0.0375948596693869),
 .UNSPECIFIED.)
GEOMETRIC_REPRESENTATION_ITEM()
RATIONAL_B_SPLINE_SURFACE(((0.996753121755999,0.997505687613148,0.999678813023853),
(0.996753121755999,0.997505687613148,0.999678813023853)))
REPRESENTATION_ITEM('')
SURFACE()
);
#555=(
BOUNDED_SURFACE()
B_SPLINE_SURFACE(1,2,((#89725,#89726,#89727),(#89728,#89729,#89730),(#89731,
#89732,#89733)),.UNSPECIFIED.,.F.,.F.,.F.)
B_SPLINE_SURFACE_WITH_KNOTS((2,1,2),(3,3),(-0.000171761234875073,1.,1.00600020634811),
(0.0665898698856039,0.0751324139127276),.UNSPECIFIED.)
GEOMETRIC_REPRESENTATION_ITEM()
RATIONAL_B_SPLINE_SURFACE(((0.997134830028879,0.997884084852167,0.999352698773649),
(0.997134830028879,0.997884084852167,0.999352698773649),(0.997134830028879,
0.997884084852167,0.999352698773649)))
REPRESENTATION_ITEM('')
SURFACE()
);
#556=(
BOUNDED_SURFACE()
B_SPLINE_SURFACE(1,2,((#89772,#89773,#89774),(#89775,#89776,#89777),(#89778,
#89779,#89780),(#89781,#89782,#89783)),.UNSPECIFIED.,.F.,.F.,.F.)
B_SPLINE_SURFACE_WITH_KNOTS((2,1,1,2),(3,3),(-0.01,0.,1.,1.0101),(0.0556006976418396,
0.0675888856590483),.UNSPECIFIED.)
GEOMETRIC_REPRESENTATION_ITEM()
RATIONAL_B_SPLINE_SURFACE(((0.996397562408606,0.996150386832629,0.997319912843744),
(0.996397562408606,0.996150386832629,0.997319912843744),(0.996397562408606,
0.996150386832629,0.997319912843744),(0.996397562408606,0.996150386832629,
0.997319912843744)))
REPRESENTATION_ITEM('')
SURFACE()
);
#557=(
BOUNDED_SURFACE()
B_SPLINE_SURFACE(1,2,((#89899,#89900,#89901),(#89902,#89903,#89904),(#89905,
#89906,#89907)),.UNSPECIFIED.,.F.,.F.,.F.)
B_SPLINE_SURFACE_WITH_KNOTS((2,1,2),(3,3),(-0.00286753114067742,0.,0.477902879812045),
(0.0166015299238962,0.0231736788090054),.UNSPECIFIED.)
GEOMETRIC_REPRESENTATION_ITEM()
RATIONAL_B_SPLINE_SURFACE(((0.996422581660833,0.996252244737399,0.996507688616235),
(0.996422581660833,0.996252244737399,0.996507688616235),(0.996422581660833,
0.996252244737399,0.996507688616235)))
REPRESENTATION_ITEM('')
SURFACE()
);
#558=(
BOUNDED_SURFACE()
B_SPLINE_SURFACE(1,2,((#89924,#89925,#89926),(#89927,#89928,#89929),(#89930,
#89931,#89932),(#89933,#89934,#89935)),.UNSPECIFIED.,.F.,.F.,.F.)
B_SPLINE_SURFACE_WITH_KNOTS((2,1,1,2),(3,3),(-0.0101,0.,1.,1.01),(0.00560769168370519,
0.0176009700440511),.UNSPECIFIED.)
GEOMETRIC_REPRESENTATION_ITEM()
RATIONAL_B_SPLINE_SURFACE(((0.998183892113821,0.99657330421516,0.996380621259469),
(0.998183892113821,0.99657330421516,0.996380621259469),(0.998183892113821,
0.99657330421516,0.996380621259469),(0.998183892113821,0.99657330421516,
0.996380621259469)))
REPRESENTATION_ITEM('')
SURFACE()
);
#559=(
BOUNDED_SURFACE()
B_SPLINE_SURFACE(1,2,((#89970,#89971,#89972),(#89973,#89974,#89975),(#89976,
#89977,#89978)),.UNSPECIFIED.,.F.,.F.,.F.)
B_SPLINE_SURFACE_WITH_KNOTS((2,1,2),(3,3),(-0.00206901892668318,0.,0.346769728514577),
(0.00660713154703276,0.0131849431468903),.UNSPECIFIED.)
GEOMETRIC_REPRESENTATION_ITEM()
RATIONAL_B_SPLINE_SURFACE(((0.99792530735949,0.997106772384952,0.996714752253861),
(0.99792530735949,0.997106772384952,0.996714752253861),(0.99792530735949,
0.997106772384952,0.996714752253861)))
REPRESENTATION_ITEM('')
SURFACE()
);
#560=(
BOUNDED_SURFACE()
B_SPLINE_SURFACE(1,2,((#90104,#90105,#90106,#90107,#90108),(#90109,#90110,
#90111,#90112,#90113)),.UNSPECIFIED.,.F.,.F.,.F.)
B_SPLINE_SURFACE_WITH_KNOTS((2,2),(3,2,3),(0.,0.480770297106543),(0.0365944846645797,
0.0384615384615384,0.0431859280915183),.UNSPECIFIED.)
GEOMETRIC_REPRESENTATION_ITEM()
RATIONAL_B_SPLINE_SURFACE(((0.999326490452259,0.999646063968217,1.,0.999104400890347,
0.9984288220563),(0.999326490452259,0.999646063968217,1.,0.999104400890347,
0.9984288220563)))
REPRESENTATION_ITEM('')
SURFACE()
);
#561=(
BOUNDED_SURFACE()
B_SPLINE_SURFACE(1,2,((#90121,#90122,#90123),(#90124,#90125,#90126),(#90127,
#90128,#90129),(#90130,#90131,#90132)),.UNSPECIFIED.,.F.,.F.,.F.)
B_SPLINE_SURFACE_WITH_KNOTS((2,1,1,2),(3,3),(-0.01,0.,1.,1.0101),(0.0255903596131811,
0.0375948596693868),.UNSPECIFIED.)
GEOMETRIC_REPRESENTATION_ITEM()
RATIONAL_B_SPLINE_SURFACE(((0.996753121755999,0.997505687613148,0.999678813023853),
(0.996753121755999,0.997505687613148,0.999678813023853),(0.996753121755999,
0.997505687613148,0.999678813023853),(0.996753121755999,0.997505687613148,
0.999678813023853)))
REPRESENTATION_ITEM('')
SURFACE()
);
#562=(
BOUNDED_SURFACE()
B_SPLINE_SURFACE(1,2,((#90167,#90168,#90169),(#90170,#90171,#90172),(#90173,
#90174,#90175)),.UNSPECIFIED.,.F.,.F.,.F.)
B_SPLINE_SURFACE_WITH_KNOTS((2,1,2),(3,3),(-0.00286823356239707,0.,0.47790287981273),
(0.0265907346180625,0.033170203725292),.UNSPECIFIED.)
GEOMETRIC_REPRESENTATION_ITEM()
RATIONAL_B_SPLINE_SURFACE(((0.996888414395785,0.997365765479939,0.998269846384985),
(0.996888414395785,0.997365765479939,0.998269846384985),(0.996888414395785,
0.997365765479939,0.998269846384985)))
REPRESENTATION_ITEM('')
SURFACE()
);
#563=(
BOUNDED_SURFACE()
B_SPLINE_SURFACE(1,2,((#90290,#90291,#90292),(#90293,#90294,#90295),(#90296,
#90297,#90298)),.UNSPECIFIED.,.F.,.F.,.F.)
B_SPLINE_SURFACE_WITH_KNOTS((2,1,2),(3,3),(-0.00286833998609553,0.,0.477902879812572),
(0.0665898698862494,0.073171619874849),.UNSPECIFIED.)
GEOMETRIC_REPRESENTATION_ITEM()
RATIONAL_B_SPLINE_SURFACE(((0.997134830028992,0.997712106295797,0.998716408300625),
(0.997134830028992,0.997712106295797,0.998716408300625),(0.997134830028992,
0.997712106295797,0.998716408300625)))
REPRESENTATION_ITEM('')
SURFACE()
);
#564=(
BOUNDED_SURFACE()
B_SPLINE_SURFACE(1,2,((#90306,#90307,#90308),(#90309,#90310,#90311),(#90312,
#90313,#90314),(#90315,#90316,#90317)),.UNSPECIFIED.,.F.,.F.,.F.)
B_SPLINE_SURFACE_WITH_KNOTS((2,1,1,2),(3,3),(-0.0101,0.,1.,1.01),(0.0556006976418405,
0.0675888856590483),.UNSPECIFIED.)
GEOMETRIC_REPRESENTATION_ITEM()
RATIONAL_B_SPLINE_SURFACE(((0.996397562408606,0.996150386832629,0.997319912843744),
(0.996397562408606,0.996150386832629,0.997319912843744),(0.996397562408606,
0.996150386832629,0.997319912843744),(0.996397562408606,0.996150386832629,
0.997319912843744)))
REPRESENTATION_ITEM('')
SURFACE()
);
#565=(
BOUNDED_SURFACE()
B_SPLINE_SURFACE(1,2,((#90377,#90378,#90379),(#90380,#90381,#90382),(#90383,
#90384,#90385),(#90386,#90387,#90388)),.UNSPECIFIED.,.F.,.F.,.F.)
B_SPLINE_SURFACE_WITH_KNOTS((2,1,1,2),(3,3),(-0.01,0.,1.,1.0101),(0.0456081671210023,
0.0575989447818803),.UNSPECIFIED.)
GEOMETRIC_REPRESENTATION_ITEM()
RATIONAL_B_SPLINE_SURFACE(((0.997793907739637,0.996365558499688,0.996354522974128),
(0.997793907739637,0.996365558499688,0.996354522974128),(0.997793907739637,
0.996365558499688,0.996354522974128),(0.997793907739637,0.996365558499688,
0.996354522974128)))
REPRESENTATION_ITEM('')
SURFACE()
);
#566=(
BOUNDED_SURFACE()
B_SPLINE_SURFACE(1,2,((#90423,#90424,#90425),(#90426,#90427,#90428),(#90429,
#90430,#90431)),.UNSPECIFIED.,.F.,.F.,.F.)
B_SPLINE_SURFACE_WITH_KNOTS((2,1,2),(3,3),(-0.0028681017353273,0.,0.477902879815827),
(0.0466073985929115,0.0531834929157966),.UNSPECIFIED.)
GEOMETRIC_REPRESENTATION_ITEM()
RATIONAL_B_SPLINE_SURFACE(((0.997565691989291,0.996847118055594,0.996554836292953),
(0.997565691989291,0.996847118055594,0.996554836292953),(0.997565691989291,
0.996847118055594,0.996554836292953)))
REPRESENTATION_ITEM('')
SURFACE()
);
#567=(
BOUNDED_SURFACE()
B_SPLINE_SURFACE(1,2,((#90445,#90446,#90447),(#90448,#90449,#90450),(#90451,
#90452,#90453),(#90454,#90455,#90456)),.UNSPECIFIED.,.F.,.F.,.F.)
B_SPLINE_SURFACE_WITH_KNOTS((2,1,1,2),(3,3),(-0.0101,0.,1.,1.01),(0.0056076916837051,
0.0176009700440511),.UNSPECIFIED.)
GEOMETRIC_REPRESENTATION_ITEM()
RATIONAL_B_SPLINE_SURFACE(((0.998183892113821,0.99657330421516,0.996380621259469),
(0.998183892113821,0.99657330421516,0.996380621259469),(0.998183892113821,
0.99657330421516,0.996380621259469),(0.998183892113821,0.99657330421516,
0.996380621259469)))
REPRESENTATION_ITEM('')
SURFACE()
);
#568=(
BOUNDED_SURFACE()
B_SPLINE_SURFACE(1,2,((#90491,#90492,#90493),(#90494,#90495,#90496),(#90497,
#90498,#90499)),.UNSPECIFIED.,.F.,.F.,.F.)
B_SPLINE_SURFACE_WITH_KNOTS((2,1,2),(3,3),(-0.00206901892672331,0.,0.346769728514296),
(0.00660713154704671,0.0131849431468893),.UNSPECIFIED.)
GEOMETRIC_REPRESENTATION_ITEM()
RATIONAL_B_SPLINE_SURFACE(((0.997925307359486,0.997106772384951,0.99671475225386),
(0.997925307359486,0.997106772384951,0.99671475225386),(0.997925307359486,
0.997106772384951,0.99671475225386)))
REPRESENTATION_ITEM('')
SURFACE()
);
#569=(
BOUNDED_SURFACE()
B_SPLINE_SURFACE(1,2,((#90573,#90574,#90575),(#90576,#90577,#90578)),
 .UNSPECIFIED.,.F.,.F.,.F.)
B_SPLINE_SURFACE_WITH_KNOTS((2,2),(3,3),(0.,1.),(0.0255903596131799,0.0375948596693882),
 .UNSPECIFIED.)
GEOMETRIC_REPRESENTATION_ITEM()
RATIONAL_B_SPLINE_SURFACE(((0.996753121755999,0.997505687613148,0.999678813023854),
(0.996753121755999,0.997505687613148,0.999678813023854)))
REPRESENTATION_ITEM('')
SURFACE()
);
#570=(
BOUNDED_SURFACE()
B_SPLINE_SURFACE(1,2,((#90635,#90636,#90637),(#90638,#90639,#90640),(#90641,
#90642,#90643),(#90644,#90645,#90646)),.UNSPECIFIED.,.F.,.F.,.F.)
B_SPLINE_SURFACE_WITH_KNOTS((2,1,1,2),(3,3),(-0.00600004466592092,0.,1.,
1.00399715809618),(0.0166015299238287,0.0265907346180642),.UNSPECIFIED.)
GEOMETRIC_REPRESENTATION_ITEM()
RATIONAL_B_SPLINE_SURFACE(((0.996422581660836,0.996163681501244,0.996888414395786),
(0.996422581660836,0.996163681501244,0.996888414395786),(0.996422581660836,
0.996163681501244,0.996888414395786),(0.996422581660836,0.996163681501244,
0.996888414395786)))
REPRESENTATION_ITEM('')
SURFACE()
);
#571=(
BOUNDED_SURFACE()
B_SPLINE_SURFACE(1,2,((#90680,#90681,#90682),(#90683,#90684,#90685),(#90686,
#90687,#90688)),.UNSPECIFIED.,.F.,.F.,.F.)
B_SPLINE_SURFACE_WITH_KNOTS((2,1,2),(3,3),(-0.00286753114071372,0.,0.477902879812748),
(0.0166015299238963,0.0231736788090055),.UNSPECIFIED.)
GEOMETRIC_REPRESENTATION_ITEM()
RATIONAL_B_SPLINE_SURFACE(((0.996422581660833,0.996252244737399,0.996507688616235),
(0.996422581660833,0.996252244737399,0.996507688616235),(0.996422581660833,
0.996252244737399,0.996507688616235)))
REPRESENTATION_ITEM('')
SURFACE()
);
#572=(
BOUNDED_SURFACE()
B_SPLINE_SURFACE(1,2,((#90696,#90697,#90698),(#90699,#90700,#90701),(#90702,
#90703,#90704)),.UNSPECIFIED.,.F.,.F.,.F.)
B_SPLINE_SURFACE_WITH_KNOTS((2,1,2),(3,3),(-0.01,0.,1.00000001523839),(0.00560769168370637,
0.0176009700440516),.UNSPECIFIED.)
GEOMETRIC_REPRESENTATION_ITEM()
RATIONAL_B_SPLINE_SURFACE(((0.99818389211382,0.99657330421516,0.996380621259469),
(0.99818389211382,0.99657330421516,0.996380621259469),(0.99818389211382,
0.99657330421516,0.996380621259469)))
REPRESENTATION_ITEM('')
SURFACE()
);
#573=(
BOUNDED_SURFACE()
B_SPLINE_SURFACE(1,2,((#90757,#90758,#90759),(#90760,#90761,#90762),(#90763,
#90764,#90765)),.UNSPECIFIED.,.F.,.F.,.F.)
B_SPLINE_SURFACE_WITH_KNOTS((2,1,2),(3,3),(-0.000171761236754886,1.,1.00600020634818),
(0.0665898698856032,0.0751324139146066),.UNSPECIFIED.)
GEOMETRIC_REPRESENTATION_ITEM()
RATIONAL_B_SPLINE_SURFACE(((0.997134830028878,0.997884084852332,0.999352698774295),
(0.997134830028878,0.997884084852332,0.999352698774295),(0.997134830028878,
0.997884084852332,0.999352698774295)))
REPRESENTATION_ITEM('')
SURFACE()
);
#574=(
BOUNDED_SURFACE()
B_SPLINE_SURFACE(1,2,((#90780,#90781,#90782),(#90783,#90784,#90785),(#90786,
#90787,#90788)),.UNSPECIFIED.,.F.,.F.,.F.)
B_SPLINE_SURFACE_WITH_KNOTS((2,1,2),(3,3),(-0.00286833998615812,0.,0.477902879812017),
(0.0665898698862492,0.07317161987485),.UNSPECIFIED.)
GEOMETRIC_REPRESENTATION_ITEM()
RATIONAL_B_SPLINE_SURFACE(((0.997134830028992,0.997712106295797,0.998716408300625),
(0.997134830028992,0.997712106295797,0.998716408300625),(0.997134830028992,
0.997712106295797,0.998716408300625)))
REPRESENTATION_ITEM('')
SURFACE()
);
#575=(
BOUNDED_SURFACE()
B_SPLINE_SURFACE(1,2,((#90796,#90797,#90798),(#90799,#90800,#90801),(#90802,
#90803,#90804)),.UNSPECIFIED.,.F.,.F.,.F.)
B_SPLINE_SURFACE_WITH_KNOTS((2,1,2),(3,3),(-0.01,0.,1.),(0.0556006976418417,
0.0675888856590487),.UNSPECIFIED.)
GEOMETRIC_REPRESENTATION_ITEM()
RATIONAL_B_SPLINE_SURFACE(((0.996397562408606,0.996150386832629,0.997319912843744),
(0.996397562408606,0.996150386832629,0.997319912843744),(0.996397562408606,
0.996150386832629,0.997319912843744)))
REPRESENTATION_ITEM('')
SURFACE()
);
#576=(
BOUNDED_SURFACE()
B_SPLINE_SURFACE(1,2,((#90840,#90841,#90842),(#90843,#90844,#90845),(#90846,
#90847,#90848)),.UNSPECIFIED.,.F.,.F.,.F.)
B_SPLINE_SURFACE_WITH_KNOTS((2,1,2),(3,3),(-0.00286764392049501,0.,0.47790287980793),
(0.0565997133101191,0.0631721430887064),.UNSPECIFIED.)
GEOMETRIC_REPRESENTATION_ITEM()
RATIONAL_B_SPLINE_SURFACE(((0.996366204684739,0.996295417244646,0.996650447003323),
(0.996366204684739,0.996295417244646,0.996650447003323),(0.996366204684738,
0.996295417244646,0.996650447003323)))
REPRESENTATION_ITEM('')
SURFACE()
);
#577=(
BOUNDED_SURFACE()
B_SPLINE_SURFACE(1,2,((#90856,#90857,#90858),(#90859,#90860,#90861),(#90862,
#90863,#90864),(#90865,#90866,#90867)),.UNSPECIFIED.,.F.,.F.,.F.)
B_SPLINE_SURFACE_WITH_KNOTS((2,1,1,2),(3,3),(-0.0101,0.,1.,1.01),(0.0456081671210031,
0.057598944781881),.UNSPECIFIED.)
GEOMETRIC_REPRESENTATION_ITEM()
RATIONAL_B_SPLINE_SURFACE(((0.997793907739636,0.996365558499688,0.996354522974128),
(0.997793907739636,0.996365558499688,0.996354522974128),(0.997793907739636,
0.996365558499688,0.996354522974128),(0.997793907739636,0.996365558499688,
0.996354522974128)))
REPRESENTATION_ITEM('')
SURFACE()
);
#578=(
BOUNDED_SURFACE()
B_SPLINE_SURFACE(1,2,((#90901,#90902,#90903),(#90904,#90905,#90906),(#90907,
#90908,#90909)),.UNSPECIFIED.,.F.,.F.,.F.)
B_SPLINE_SURFACE_WITH_KNOTS((2,1,2),(3,3),(-0.00286810173531933,0.,0.477902879812644),
(0.046607398592911,0.0531834929157964),.UNSPECIFIED.)
GEOMETRIC_REPRESENTATION_ITEM()
RATIONAL_B_SPLINE_SURFACE(((0.997565691989291,0.996847118055594,0.996554836292953),
(0.997565691989291,0.996847118055594,0.996554836292953),(0.997565691989291,
0.996847118055594,0.996554836292953)))
REPRESENTATION_ITEM('')
SURFACE()
);
#579=(
BOUNDED_SURFACE()
B_SPLINE_SURFACE(1,2,((#90917,#90918,#90919,#90920,#90921),(#90922,#90923,
#90924,#90925,#90926),(#90927,#90928,#90929,#90930,#90931),(#90932,#90933,
#90934,#90935,#90936)),.UNSPECIFIED.,.F.,.F.,.F.)
B_SPLINE_SURFACE_WITH_KNOTS((2,1,1,2),(3,2,3),(-0.01,0.,1.,1.0101),(0.0355931932713894,
0.0384615384615384,0.0476086899858116),.UNSPECIFIED.)
GEOMETRIC_REPRESENTATION_ITEM()
RATIONAL_B_SPLINE_SURFACE(((0.998993602249806,0.999456249886298,1.,0.998265981131401,
0.997356751596327),(0.998993602249806,0.999456249886298,1.,0.998265981131401,
0.997356751596327),(0.998993602249806,0.999456249886298,1.,0.998265981131401,
0.997356751596327),(0.998993602249806,0.999456249886298,1.,0.998265981131401,
0.997356751596327)))
REPRESENTATION_ITEM('')
SURFACE()
);
#580=(
BOUNDED_SURFACE()
B_SPLINE_SURFACE(1,2,((#90983,#90984,#90985,#90986,#90987),(#90988,#90989,
#90990,#90991,#90992),(#90993,#90994,#90995,#90996,#90997)),
 .UNSPECIFIED.,.F.,.F.,.F.)
B_SPLINE_SURFACE_WITH_KNOTS((2,1,2),(3,2,3),(-0.00286743094794425,0.,0.48077029717846),
(0.0365944846642787,0.0384615384615384,0.0431859280915192),
 .UNSPECIFIED.)
GEOMETRIC_REPRESENTATION_ITEM()
RATIONAL_B_SPLINE_SURFACE(((0.999326490452157,0.99964606396816,1.,0.999104400890347,
0.998428822056299),(0.999326490452157,0.99964606396816,1.,0.999104400890347,
0.998428822056299),(0.999326490452157,0.99964606396816,1.,0.999104400890347,
0.998428822056299)))
REPRESENTATION_ITEM('')
SURFACE()
);
#581=(
BOUNDED_SURFACE()
B_SPLINE_SURFACE(1,2,((#91058,#91059,#91060),(#91061,#91062,#91063)),
 .UNSPECIFIED.,.F.,.F.,.F.)
B_SPLINE_SURFACE_WITH_KNOTS((2,2),(3,3),(0.,1.),(0.0255903596132002,0.0375948596691635),
 .UNSPECIFIED.)
GEOMETRIC_REPRESENTATION_ITEM()
RATIONAL_B_SPLINE_SURFACE(((0.996753121756002,0.997505687613137,0.999678813023772),
(0.996753121756002,0.997505687613137,0.999678813023772)))
REPRESENTATION_ITEM('')
SURFACE()
);
#582=(
BOUNDED_SURFACE()
B_SPLINE_SURFACE(1,2,((#91081,#91082,#91083,#91084,#91085),(#91086,#91087,
#91088,#91089,#91090)),.UNSPECIFIED.,.F.,.F.,.F.)
B_SPLINE_SURFACE_WITH_KNOTS((2,2),(3,2,3),(0.519229702917177,1.),(0.0365944846644287,
0.0384615384615384,0.0431859278099541),.UNSPECIFIED.)
GEOMETRIC_REPRESENTATION_ITEM()
RATIONAL_B_SPLINE_SURFACE(((0.999326490452208,0.999646063968189,1.,0.999104400943723,
0.998428822136826),(0.999326490452208,0.999646063968189,1.,0.999104400943723,
0.998428822136826)))
REPRESENTATION_ITEM('')
SURFACE()
);
#583=(
BOUNDED_SURFACE()
B_SPLINE_SURFACE(1,2,((#91146,#91147,#91148),(#91149,#91150,#91151)),
 .UNSPECIFIED.,.F.,.F.,.F.)
B_SPLINE_SURFACE_WITH_KNOTS((2,2),(3,3),(0.,1.),(0.0456081671210052,0.0575989447818612),
 .UNSPECIFIED.)
GEOMETRIC_REPRESENTATION_ITEM()
RATIONAL_B_SPLINE_SURFACE(((0.997793907739636,0.996365558499691,0.996354522974128),
(0.997793907739636,0.996365558499691,0.996354522974128)))
REPRESENTATION_ITEM('')
SURFACE()
);
#584=(
BOUNDED_SURFACE()
B_SPLINE_SURFACE(1,2,((#91186,#91187,#91188),(#91189,#91190,#91191)),
 .UNSPECIFIED.,.F.,.F.,.F.)
B_SPLINE_SURFACE_WITH_KNOTS((2,2),(3,3),(0.,1.),(0.0556006976522449,0.067588885544615),
 .UNSPECIFIED.)
GEOMETRIC_REPRESENTATION_ITEM()
RATIONAL_B_SPLINE_SURFACE(((0.996397562408177,0.996150386836003,0.997319912821417),
(0.996397562408177,0.996150386836003,0.997319912821417)))
REPRESENTATION_ITEM('')
SURFACE()
);
#585=(
BOUNDED_SURFACE()
B_SPLINE_SURFACE(1,2,((#91226,#91227,#91228),(#91229,#91230,#91231)),
 .UNSPECIFIED.,.F.,.F.,.F.)
B_SPLINE_SURFACE_WITH_KNOTS((2,2),(3,3),(0.,1.),(0.0657448619281078,0.0758849574338243),
 .UNSPECIFIED.)
GEOMETRIC_REPRESENTATION_ITEM()
RATIONAL_B_SPLINE_SURFACE(((0.996993639757276,0.997798549146192,0.999617032345115),
(0.996993639757276,0.997798549146192,0.999617032345115)))
REPRESENTATION_ITEM('')
SURFACE()
);
#586=(
BOUNDED_SURFACE()
B_SPLINE_SURFACE(1,2,((#91272,#91273,#91274),(#91275,#91276,#91277)),
 .UNSPECIFIED.,.F.,.F.,.F.)
B_SPLINE_SURFACE_WITH_KNOTS((2,2),(3,3),(0.,1.),(0.00560769170938426,0.0176009697615929),
 .UNSPECIFIED.)
GEOMETRIC_REPRESENTATION_ITEM()
RATIONAL_B_SPLINE_SURFACE(((0.998183892106924,0.996573304252679,0.996380621268545),
(0.998183892106924,0.996573304252679,0.996380621268545)))
REPRESENTATION_ITEM('')
SURFACE()
);
#587=(
BOUNDED_SURFACE()
B_SPLINE_SURFACE(1,2,((#91368,#91369,#91370),(#91371,#91372,#91373)),
 .UNSPECIFIED.,.F.,.F.,.F.)
B_SPLINE_SURFACE_WITH_KNOTS((2,2),(3,3),(0.,1.),(0.00560769170938315,0.0176009697615924),
 .UNSPECIFIED.)
GEOMETRIC_REPRESENTATION_ITEM()
RATIONAL_B_SPLINE_SURFACE(((0.998183892106924,0.996573304252679,0.996380621268545),
(0.998183892106924,0.996573304252679,0.996380621268545)))
REPRESENTATION_ITEM('')
SURFACE()
);
#588=(
BOUNDED_SURFACE()
B_SPLINE_SURFACE(1,2,((#91374,#91375,#91376,#91377,#91378),(#91379,#91380,
#91381,#91382,#91383)),.UNSPECIFIED.,.F.,.F.,.F.)
B_SPLINE_SURFACE_WITH_KNOTS((2,2),(3,2,3),(0.519229702914946,1.),(0.0365944846644327,
0.0384615384615384,0.0431859276813001),.UNSPECIFIED.)
GEOMETRIC_REPRESENTATION_ITEM()
RATIONAL_B_SPLINE_SURFACE(((0.999326490452209,0.999646063968189,1.,0.999104400968112,
0.998428822173621),(0.999326490452209,0.999646063968189,1.,0.999104400968112,
0.998428822173621)))
REPRESENTATION_ITEM('')
SURFACE()
);
#589=(
BOUNDED_SURFACE()
B_SPLINE_SURFACE(1,2,((#91456,#91457,#91458),(#91459,#91460,#91461)),
 .UNSPECIFIED.,.F.,.F.,.F.)
B_SPLINE_SURFACE_WITH_KNOTS((2,2),(3,3),(0.,1.),(0.045608167121004,0.0575989447818607),
 .UNSPECIFIED.)
GEOMETRIC_REPRESENTATION_ITEM()
RATIONAL_B_SPLINE_SURFACE(((0.997793907739636,0.996365558499691,0.996354522974128),
(0.997793907739636,0.996365558499691,0.996354522974128)))
REPRESENTATION_ITEM('')
SURFACE()
);
#590=(
BOUNDED_SURFACE()
B_SPLINE_SURFACE(1,2,((#91496,#91497,#91498),(#91499,#91500,#91501)),
 .UNSPECIFIED.,.F.,.F.,.F.)
B_SPLINE_SURFACE_WITH_KNOTS((2,2),(3,3),(0.,1.),(0.0556006976522436,0.0675888855446153),
 .UNSPECIFIED.)
GEOMETRIC_REPRESENTATION_ITEM()
RATIONAL_B_SPLINE_SURFACE(((0.996397562408177,0.996150386836003,0.997319912821417),
(0.996397562408177,0.996150386836003,0.997319912821417)))
REPRESENTATION_ITEM('')
SURFACE()
);
#591=(
BOUNDED_SURFACE()
B_SPLINE_SURFACE(1,2,((#91536,#91537,#91538),(#91539,#91540,#91541)),
 .UNSPECIFIED.,.F.,.F.,.F.)
B_SPLINE_SURFACE_WITH_KNOTS((2,2),(3,3),(0.,1.),(0.0657450014656856,0.0758834225204709),
 .UNSPECIFIED.)
GEOMETRIC_REPRESENTATION_ITEM()
RATIONAL_B_SPLINE_SURFACE(((0.99699366191014,0.997798452328481,0.99961648183819),
(0.99699366191014,0.997798452328481,0.99961648183819)))
REPRESENTATION_ITEM('')
SURFACE()
);
#592=(
BOUNDED_SURFACE()
B_SPLINE_SURFACE(1,2,((#91592,#91593,#91594),(#91595,#91596,#91597)),
 .UNSPECIFIED.,.F.,.F.,.F.)
B_SPLINE_SURFACE_WITH_KNOTS((2,2),(3,3),(0.,1.),(0.0255903596132011,0.037594859669167),
 .UNSPECIFIED.)
GEOMETRIC_REPRESENTATION_ITEM()
RATIONAL_B_SPLINE_SURFACE(((0.996753121756002,0.997505687613138,0.999678813023773),
(0.996753121756002,0.997505687613138,0.999678813023773)))
REPRESENTATION_ITEM('')
SURFACE()
);
#593=(
BOUNDED_SURFACE()
B_SPLINE_SURFACE(1,2,((#91672,#91673,#91674),(#91675,#91676,#91677)),
 .UNSPECIFIED.,.F.,.F.,.F.)
B_SPLINE_SURFACE_WITH_KNOTS((2,2),(3,3),(0.,1.),(0.00560769170938355,0.0176009697615912),
 .UNSPECIFIED.)
GEOMETRIC_REPRESENTATION_ITEM()
RATIONAL_B_SPLINE_SURFACE(((0.998183892106924,0.996573304252679,0.996380621268545),
(0.998183892106924,0.996573304252679,0.996380621268545)))
REPRESENTATION_ITEM('')
SURFACE()
);
#594=(
BOUNDED_SURFACE()
B_SPLINE_SURFACE(1,2,((#91762,#91763,#91764),(#91765,#91766,#91767)),
 .UNSPECIFIED.,.F.,.F.,.F.)
B_SPLINE_SURFACE_WITH_KNOTS((2,2),(3,3),(0.,1.),(0.0456081671210064,0.0575989447818599),
 .UNSPECIFIED.)
GEOMETRIC_REPRESENTATION_ITEM()
RATIONAL_B_SPLINE_SURFACE(((0.997793907739636,0.996365558499691,0.996354522974128),
(0.997793907739636,0.996365558499691,0.996354522974128)))
REPRESENTATION_ITEM('')
SURFACE()
);
#595=(
BOUNDED_SURFACE()
B_SPLINE_SURFACE(1,2,((#91802,#91803,#91804),(#91805,#91806,#91807)),
 .UNSPECIFIED.,.F.,.F.,.F.)
B_SPLINE_SURFACE_WITH_KNOTS((2,2),(3,3),(0.,1.),(0.0556006976522427,0.0675888855446155),
 .UNSPECIFIED.)
GEOMETRIC_REPRESENTATION_ITEM()
RATIONAL_B_SPLINE_SURFACE(((0.996397562408177,0.996150386836003,0.997319912821417),
(0.996397562408177,0.996150386836003,0.997319912821417)))
REPRESENTATION_ITEM('')
SURFACE()
);
#596=(
BOUNDED_SURFACE()
B_SPLINE_SURFACE(1,2,((#91842,#91843,#91844),(#91845,#91846,#91847)),
 .UNSPECIFIED.,.F.,.F.,.F.)
B_SPLINE_SURFACE_WITH_KNOTS((2,2),(3,3),(0.,1.),(0.065744861928108,0.0758849574338245),
 .UNSPECIFIED.)
GEOMETRIC_REPRESENTATION_ITEM()
RATIONAL_B_SPLINE_SURFACE(((0.996993639757276,0.997798549146192,0.999617032345115),
(0.996993639757276,0.997798549146192,0.999617032345115)))
REPRESENTATION_ITEM('')
SURFACE()
);
#597=(
BOUNDED_SURFACE()
B_SPLINE_SURFACE(1,2,((#91882,#91883,#91884),(#91885,#91886,#91887)),
 .UNSPECIFIED.,.F.,.F.,.F.)
B_SPLINE_SURFACE_WITH_KNOTS((2,2),(3,3),(0.,1.),(0.0255903596131999,0.0375948596691669),
 .UNSPECIFIED.)
GEOMETRIC_REPRESENTATION_ITEM()
RATIONAL_B_SPLINE_SURFACE(((0.996753121756002,0.997505687613138,0.999678813023773),
(0.996753121756002,0.997505687613138,0.999678813023773)))
REPRESENTATION_ITEM('')
SURFACE()
);
#598=(
BOUNDED_SURFACE()
B_SPLINE_SURFACE(1,2,((#91910,#91911,#91912,#91913,#91914),(#91915,#91916,
#91917,#91918,#91919)),.UNSPECIFIED.,.F.,.F.,.F.)
B_SPLINE_SURFACE_WITH_KNOTS((2,2),(3,2,3),(0.519229702917952,1.),(0.0365944846644359,
0.0384615384615384,0.0431859278882002),.UNSPECIFIED.)
GEOMETRIC_REPRESENTATION_ITEM()
RATIONAL_B_SPLINE_SURFACE(((0.99932649045221,0.99964606396819,1.,0.99910440092889,
0.998428822114449),(0.99932649045221,0.99964606396819,1.,0.99910440092889,
0.998428822114449)))
REPRESENTATION_ITEM('')
SURFACE()
);
#599=(
BOUNDED_SURFACE()
B_SPLINE_SURFACE(1,2,((#91976,#91977,#91978),(#91979,#91980,#91981)),
 .UNSPECIFIED.,.F.,.F.,.F.)
B_SPLINE_SURFACE_WITH_KNOTS((2,2),(3,3),(0.,1.),(0.00560769170938407,0.0176009697615916),
 .UNSPECIFIED.)
GEOMETRIC_REPRESENTATION_ITEM()
RATIONAL_B_SPLINE_SURFACE(((0.998183892106924,0.996573304252679,0.996380621268545),
(0.998183892106924,0.996573304252679,0.996380621268545)))
REPRESENTATION_ITEM('')
SURFACE()
);
#600=(
BOUNDED_SURFACE()
B_SPLINE_SURFACE(1,2,((#92066,#92067,#92068),(#92069,#92070,#92071)),
 .UNSPECIFIED.,.F.,.F.,.F.)
B_SPLINE_SURFACE_WITH_KNOTS((2,2),(3,3),(0.,1.),(0.0255903596131989,0.0375948596691652),
 .UNSPECIFIED.)
GEOMETRIC_REPRESENTATION_ITEM()
RATIONAL_B_SPLINE_SURFACE(((0.996753121756001,0.997505687613137,0.999678813023773),
(0.996753121756001,0.997505687613137,0.999678813023773)))
REPRESENTATION_ITEM('')
SURFACE()
);
#601=(
BOUNDED_SURFACE()
B_SPLINE_SURFACE(1,2,((#92106,#92107,#92108),(#92109,#92110,#92111)),
 .UNSPECIFIED.,.F.,.F.,.F.)
B_SPLINE_SURFACE_WITH_KNOTS((2,2),(3,3),(0.,1.),(0.0556006976522448,0.0675888855446141),
 .UNSPECIFIED.)
GEOMETRIC_REPRESENTATION_ITEM()
RATIONAL_B_SPLINE_SURFACE(((0.996397562408177,0.996150386836003,0.997319912821417),
(0.996397562408177,0.996150386836003,0.997319912821417)))
REPRESENTATION_ITEM('')
SURFACE()
);
#602=(
BOUNDED_SURFACE()
B_SPLINE_SURFACE(1,2,((#92146,#92147,#92148),(#92149,#92150,#92151)),
 .UNSPECIFIED.,.F.,.F.,.F.)
B_SPLINE_SURFACE_WITH_KNOTS((2,2),(3,3),(0.,1.),(0.0657448619281069,0.0758849574338248),
 .UNSPECIFIED.)
GEOMETRIC_REPRESENTATION_ITEM()
RATIONAL_B_SPLINE_SURFACE(((0.996993639757276,0.997798549146192,0.999617032345115),
(0.996993639757276,0.997798549146192,0.999617032345115)))
REPRESENTATION_ITEM('')
SURFACE()
);
#603=(
BOUNDED_SURFACE()
B_SPLINE_SURFACE(1,2,((#92169,#92170,#92171,#92172,#92173),(#92174,#92175,
#92176,#92177,#92178)),.UNSPECIFIED.,.F.,.F.,.F.)
B_SPLINE_SURFACE_WITH_KNOTS((2,2),(3,2,3),(0.519229702915815,1.),(0.0365944846644425,
0.0384615384615384,0.0431859278882058),.UNSPECIFIED.)
GEOMETRIC_REPRESENTATION_ITEM()
RATIONAL_B_SPLINE_SURFACE(((0.999326490452213,0.999646063968191,1.,0.999104400928889,
0.998428822114447),(0.999326490452213,0.999646063968191,1.,0.999104400928889,
0.998428822114447)))
REPRESENTATION_ITEM('')
SURFACE()
);
#604=(
BOUNDED_SURFACE()
B_SPLINE_SURFACE(1,2,((#92200,#92201,#92202),(#92203,#92204,#92205)),
 .UNSPECIFIED.,.F.,.F.,.F.)
B_SPLINE_SURFACE_WITH_KNOTS((2,2),(3,3),(0.,1.),(0.0456081671210052,0.0575989447818616),
 .UNSPECIFIED.)
GEOMETRIC_REPRESENTATION_ITEM()
RATIONAL_B_SPLINE_SURFACE(((0.997793907739636,0.996365558499691,0.996354522974128),
(0.997793907739636,0.996365558499691,0.996354522974128)))
REPRESENTATION_ITEM('')
SURFACE()
);
#605=(
BOUNDED_SURFACE()
B_SPLINE_SURFACE(1,2,((#92280,#92281,#92282),(#92283,#92284,#92285)),
 .UNSPECIFIED.,.F.,.F.,.F.)
B_SPLINE_SURFACE_WITH_KNOTS((2,2),(3,3),(0.,1.),(0.00560769170938321,0.0176009697615924),
 .UNSPECIFIED.)
GEOMETRIC_REPRESENTATION_ITEM()
RATIONAL_B_SPLINE_SURFACE(((0.998183892106924,0.996573304252679,0.996380621268545),
(0.998183892106924,0.996573304252679,0.996380621268545)))
REPRESENTATION_ITEM('')
SURFACE()
);
#606=(
BOUNDED_SURFACE()
B_SPLINE_SURFACE(1,2,((#92370,#92371,#92372),(#92373,#92374,#92375)),
 .UNSPECIFIED.,.F.,.F.,.F.)
B_SPLINE_SURFACE_WITH_KNOTS((2,2),(3,3),(0.,1.),(0.0255903596131988,0.0375948596691661),
 .UNSPECIFIED.)
GEOMETRIC_REPRESENTATION_ITEM()
RATIONAL_B_SPLINE_SURFACE(((0.996753121756001,0.997505687613137,0.999678813023773),
(0.996753121756001,0.997505687613137,0.999678813023773)))
REPRESENTATION_ITEM('')
SURFACE()
);
#607=(
BOUNDED_SURFACE()
B_SPLINE_SURFACE(1,2,((#92393,#92394,#92395,#92396,#92397),(#92398,#92399,
#92400,#92401,#92402)),.UNSPECIFIED.,.F.,.F.,.F.)
B_SPLINE_SURFACE_WITH_KNOTS((2,2),(3,2,3),(0.519229702913765,1.),(0.0365944846644499,
0.0384615384615384,0.0431859278882126),.UNSPECIFIED.)
GEOMETRIC_REPRESENTATION_ITEM()
RATIONAL_B_SPLINE_SURFACE(((0.999326490452215,0.999646063968193,1.,0.999104400928888,
0.998428822114445),(0.999326490452215,0.999646063968193,1.,0.999104400928888,
0.998428822114445)))
REPRESENTATION_ITEM('')
SURFACE()
);
#608=(
BOUNDED_SURFACE()
B_SPLINE_SURFACE(1,2,((#92441,#92442,#92443),(#92444,#92445,#92446)),
 .UNSPECIFIED.,.F.,.F.,.F.)
B_SPLINE_SURFACE_WITH_KNOTS((2,2),(3,3),(0.,1.),(0.0657448619281088,0.0758849574338248),
 .UNSPECIFIED.)
GEOMETRIC_REPRESENTATION_ITEM()
RATIONAL_B_SPLINE_SURFACE(((0.996993639757276,0.997798549146193,0.999617032345115),
(0.996993639757276,0.997798549146193,0.999617032345115)))
REPRESENTATION_ITEM('')
SURFACE()
);
#609=(
BOUNDED_SURFACE()
B_SPLINE_SURFACE(1,2,((#92498,#92499,#92500),(#92501,#92502,#92503)),
 .UNSPECIFIED.,.F.,.F.,.F.)
B_SPLINE_SURFACE_WITH_KNOTS((2,2),(3,3),(0.,1.),(0.0456081671210064,0.0575989447818615),
 .UNSPECIFIED.)
GEOMETRIC_REPRESENTATION_ITEM()
RATIONAL_B_SPLINE_SURFACE(((0.997793907739636,0.996365558499691,0.996354522974128),
(0.997793907739636,0.996365558499691,0.996354522974128)))
REPRESENTATION_ITEM('')
SURFACE()
);
#610=(
BOUNDED_SURFACE()
B_SPLINE_SURFACE(1,2,((#92504,#92505,#92506),(#92507,#92508,#92509)),
 .UNSPECIFIED.,.F.,.F.,.F.)
B_SPLINE_SURFACE_WITH_KNOTS((2,2),(3,3),(0.,1.),(0.0556006976522447,0.0675888855446161),
 .UNSPECIFIED.)
GEOMETRIC_REPRESENTATION_ITEM()
RATIONAL_B_SPLINE_SURFACE(((0.996397562408177,0.996150386836003,0.997319912821417),
(0.996397562408177,0.996150386836003,0.997319912821417)))
REPRESENTATION_ITEM('')
SURFACE()
);
#611=(
BOUNDED_SURFACE()
B_SPLINE_SURFACE(1,2,((#92584,#92585,#92586),(#92587,#92588,#92589)),
 .UNSPECIFIED.,.F.,.F.,.F.)
B_SPLINE_SURFACE_WITH_KNOTS((2,2),(3,3),(0.,1.),(0.00560769170938333,0.0176009697615919),
 .UNSPECIFIED.)
GEOMETRIC_REPRESENTATION_ITEM()
RATIONAL_B_SPLINE_SURFACE(((0.998183892106924,0.996573304252679,0.996380621268545),
(0.998183892106924,0.996573304252679,0.996380621268545)))
REPRESENTATION_ITEM('')
SURFACE()
);
#612=(
BOUNDED_SURFACE()
B_SPLINE_SURFACE(1,2,((#92674,#92675,#92676),(#92677,#92678,#92679)),
 .UNSPECIFIED.,.F.,.F.,.F.)
B_SPLINE_SURFACE_WITH_KNOTS((2,2),(3,3),(0.,1.),(0.0255903596131999,0.037594859669166),
 .UNSPECIFIED.)
GEOMETRIC_REPRESENTATION_ITEM()
RATIONAL_B_SPLINE_SURFACE(((0.996753121756002,0.997505687613138,0.999678813023773),
(0.996753121756002,0.997505687613138,0.999678813023773)))
REPRESENTATION_ITEM('')
SURFACE()
);
#613=(
BOUNDED_SURFACE()
B_SPLINE_SURFACE(1,2,((#92697,#92698,#92699,#92700,#92701),(#92702,#92703,
#92704,#92705,#92706)),.UNSPECIFIED.,.F.,.F.,.F.)
B_SPLINE_SURFACE_WITH_KNOTS((2,2),(3,2,3),(0.519229702912058,1.),(0.0365944846644593,
0.0384615384615384,0.0431859278882214),.UNSPECIFIED.)
GEOMETRIC_REPRESENTATION_ITEM()
RATIONAL_B_SPLINE_SURFACE(((0.999326490452218,0.999646063968195,1.,0.999104400928886,
0.998428822114442),(0.999326490452218,0.999646063968195,1.,0.999104400928886,
0.998428822114442)))
REPRESENTATION_ITEM('')
SURFACE()
);
#614=(
BOUNDED_SURFACE()
B_SPLINE_SURFACE(1,2,((#92762,#92763,#92764),(#92765,#92766,#92767)),
 .UNSPECIFIED.,.F.,.F.,.F.)
B_SPLINE_SURFACE_WITH_KNOTS((2,2),(3,3),(0.,1.),(0.0456081671210073,0.057598944781862),
 .UNSPECIFIED.)
GEOMETRIC_REPRESENTATION_ITEM()
RATIONAL_B_SPLINE_SURFACE(((0.997793907739635,0.99636555849969,0.996354522974128),
(0.997793907739635,0.99636555849969,0.996354522974128)))
REPRESENTATION_ITEM('')
SURFACE()
);
#615=(
BOUNDED_SURFACE()
B_SPLINE_SURFACE(1,2,((#92802,#92803,#92804),(#92805,#92806,#92807)),
 .UNSPECIFIED.,.F.,.F.,.F.)
B_SPLINE_SURFACE_WITH_KNOTS((2,2),(3,3),(0.,1.),(0.0556006976522459,0.0675888855446161),
 .UNSPECIFIED.)
GEOMETRIC_REPRESENTATION_ITEM()
RATIONAL_B_SPLINE_SURFACE(((0.996397562408177,0.996150386836003,0.997319912821417),
(0.996397562408177,0.996150386836003,0.997319912821417)))
REPRESENTATION_ITEM('')
SURFACE()
);
#616=(
BOUNDED_SURFACE()
B_SPLINE_SURFACE(1,2,((#92808,#92809,#92810),(#92811,#92812,#92813)),
 .UNSPECIFIED.,.F.,.F.,.F.)
B_SPLINE_SURFACE_WITH_KNOTS((2,2),(3,3),(0.,1.),(0.0657448619281089,0.0758849574338248),
 .UNSPECIFIED.)
GEOMETRIC_REPRESENTATION_ITEM()
RATIONAL_B_SPLINE_SURFACE(((0.996993639757276,0.997798549146193,0.999617032345115),
(0.996993639757276,0.997798549146193,0.999617032345115)))
REPRESENTATION_ITEM('')
SURFACE()
);
#617=(
BOUNDED_SURFACE()
B_SPLINE_SURFACE(1,2,((#92888,#92889,#92890),(#92891,#92892,#92893)),
 .UNSPECIFIED.,.F.,.F.,.F.)
B_SPLINE_SURFACE_WITH_KNOTS((2,2),(3,3),(0.,1.),(0.00560769170938518,0.0176009697615933),
 .UNSPECIFIED.)
GEOMETRIC_REPRESENTATION_ITEM()
RATIONAL_B_SPLINE_SURFACE(((0.998183892106923,0.996573304252679,0.996380621268545),
(0.998183892106923,0.996573304252679,0.996380621268545)))
REPRESENTATION_ITEM('')
SURFACE()
);
#618=(
BOUNDED_SURFACE()
B_SPLINE_SURFACE(1,2,((#92978,#92979,#92980),(#92981,#92982,#92983)),
 .UNSPECIFIED.,.F.,.F.,.F.)
B_SPLINE_SURFACE_WITH_KNOTS((2,2),(3,3),(0.,1.),(0.025590359613201,0.0375948596691667),
 .UNSPECIFIED.)
GEOMETRIC_REPRESENTATION_ITEM()
RATIONAL_B_SPLINE_SURFACE(((0.996753121756002,0.997505687613138,0.999678813023773),
(0.996753121756002,0.997505687613138,0.999678813023773)))
REPRESENTATION_ITEM('')
SURFACE()
);
#619=(
BOUNDED_SURFACE()
B_SPLINE_SURFACE(1,2,((#93001,#93002,#93003,#93004,#93005),(#93006,#93007,
#93008,#93009,#93010)),.UNSPECIFIED.,.F.,.F.,.F.)
B_SPLINE_SURFACE_WITH_KNOTS((2,2),(3,2,3),(0.519229702910745,1.),(0.0365944846644696,
0.0384615384615384,0.0431859278882312),.UNSPECIFIED.)
GEOMETRIC_REPRESENTATION_ITEM()
RATIONAL_B_SPLINE_SURFACE(((0.999326490452223,0.999646063968197,1.,0.999104400928884,
0.998428822114439),(0.999326490452222,0.999646063968197,1.,0.999104400928884,
0.998428822114439)))
REPRESENTATION_ITEM('')
SURFACE()
);
#620=(
BOUNDED_SURFACE()
B_SPLINE_SURFACE(1,2,((#93066,#93067,#93068),(#93069,#93070,#93071)),
 .UNSPECIFIED.,.F.,.F.,.F.)
B_SPLINE_SURFACE_WITH_KNOTS((2,2),(3,3),(0.,1.),(0.045608167121007,0.0575989447818626),
 .UNSPECIFIED.)
GEOMETRIC_REPRESENTATION_ITEM()
RATIONAL_B_SPLINE_SURFACE(((0.997793907739636,0.996365558499691,0.996354522974128),
(0.997793907739636,0.996365558499691,0.996354522974128)))
REPRESENTATION_ITEM('')
SURFACE()
);
#621=(
BOUNDED_SURFACE()
B_SPLINE_SURFACE(1,2,((#93106,#93107,#93108),(#93109,#93110,#93111)),
 .UNSPECIFIED.,.F.,.F.,.F.)
B_SPLINE_SURFACE_WITH_KNOTS((2,2),(3,3),(0.,1.),(0.0556006976522467,0.0675888855446182),
 .UNSPECIFIED.)
GEOMETRIC_REPRESENTATION_ITEM()
RATIONAL_B_SPLINE_SURFACE(((0.996397562408177,0.996150386836003,0.997319912821418),
(0.996397562408177,0.996150386836003,0.997319912821418)))
REPRESENTATION_ITEM('')
SURFACE()
);
#622=(
BOUNDED_SURFACE()
B_SPLINE_SURFACE(1,2,((#93112,#93113,#93114),(#93115,#93116,#93117)),
 .UNSPECIFIED.,.F.,.F.,.F.)
B_SPLINE_SURFACE_WITH_KNOTS((2,2),(3,3),(0.,1.),(0.0657448619281111,0.0758849574338245),
 .UNSPECIFIED.)
GEOMETRIC_REPRESENTATION_ITEM()
RATIONAL_B_SPLINE_SURFACE(((0.996993639757276,0.997798549146193,0.999617032345115),
(0.996993639757276,0.997798549146193,0.999617032345115)))
REPRESENTATION_ITEM('')
SURFACE()
);
#623=(
BOUNDED_SURFACE()
B_SPLINE_SURFACE(1,2,((#93192,#93193,#93194),(#93195,#93196,#93197)),
 .UNSPECIFIED.,.F.,.F.,.F.)
B_SPLINE_SURFACE_WITH_KNOTS((2,2),(3,3),(0.,1.),(0.00560769170938328,0.0176009697615929),
 .UNSPECIFIED.)
GEOMETRIC_REPRESENTATION_ITEM()
RATIONAL_B_SPLINE_SURFACE(((0.998183892106924,0.996573304252679,0.996380621268545),
(0.998183892106924,0.996573304252679,0.996380621268545)))
REPRESENTATION_ITEM('')
SURFACE()
);
#624=(
BOUNDED_SURFACE()
B_SPLINE_SURFACE(1,2,((#93282,#93283,#93284),(#93285,#93286,#93287)),
 .UNSPECIFIED.,.F.,.F.,.F.)
B_SPLINE_SURFACE_WITH_KNOTS((2,2),(3,3),(0.,1.),(0.0255903596132023,0.0375948596691656),
 .UNSPECIFIED.)
GEOMETRIC_REPRESENTATION_ITEM()
RATIONAL_B_SPLINE_SURFACE(((0.996753121756002,0.997505687613138,0.999678813023773),
(0.996753121756002,0.997505687613138,0.999678813023773)))
REPRESENTATION_ITEM('')
SURFACE()
);
#625=(
BOUNDED_SURFACE()
B_SPLINE_SURFACE(1,2,((#93305,#93306,#93307,#93308,#93309),(#93310,#93311,
#93312,#93313,#93314)),.UNSPECIFIED.,.F.,.F.,.F.)
B_SPLINE_SURFACE_WITH_KNOTS((2,2),(3,2,3),(0.519229702909494,1.),(0.0365944846644814,
0.0384615384615384,0.0431859276813475),.UNSPECIFIED.)
GEOMETRIC_REPRESENTATION_ITEM()
RATIONAL_B_SPLINE_SURFACE(((0.999326490452226,0.999646063968199,1.,0.999104400968103,
0.998428822173607),(0.999326490452226,0.999646063968199,1.,0.999104400968103,
0.998428822173607)))
REPRESENTATION_ITEM('')
SURFACE()
);
#626=(
BOUNDED_SURFACE()
B_SPLINE_SURFACE(1,2,((#93370,#93371,#93372),(#93373,#93374,#93375)),
 .UNSPECIFIED.,.F.,.F.,.F.)
B_SPLINE_SURFACE_WITH_KNOTS((2,2),(3,3),(0.,1.),(0.0456081671210083,0.0575989447818618),
 .UNSPECIFIED.)
GEOMETRIC_REPRESENTATION_ITEM()
RATIONAL_B_SPLINE_SURFACE(((0.997793907739635,0.996365558499691,0.996354522974128),
(0.997793907739635,0.996365558499691,0.996354522974128)))
REPRESENTATION_ITEM('')
SURFACE()
);
#627=(
BOUNDED_SURFACE()
B_SPLINE_SURFACE(1,2,((#93410,#93411,#93412),(#93413,#93414,#93415)),
 .UNSPECIFIED.,.F.,.F.,.F.)
B_SPLINE_SURFACE_WITH_KNOTS((2,2),(3,3),(0.,1.),(0.0556006976522459,0.067588885544616),
 .UNSPECIFIED.)
GEOMETRIC_REPRESENTATION_ITEM()
RATIONAL_B_SPLINE_SURFACE(((0.996397562408177,0.996150386836003,0.997319912821417),
(0.996397562408177,0.996150386836003,0.997319912821417)))
REPRESENTATION_ITEM('')
SURFACE()
);
#628=(
BOUNDED_SURFACE()
B_SPLINE_SURFACE(1,2,((#93416,#93417,#93418),(#93419,#93420,#93421)),
 .UNSPECIFIED.,.F.,.F.,.F.)
B_SPLINE_SURFACE_WITH_KNOTS((2,2),(3,3),(0.,1.),(0.0657448619281089,0.0758849574338248),
 .UNSPECIFIED.)
GEOMETRIC_REPRESENTATION_ITEM()
RATIONAL_B_SPLINE_SURFACE(((0.996993639757276,0.997798549146193,0.999617032345115),
(0.996993639757276,0.997798549146193,0.999617032345115)))
REPRESENTATION_ITEM('')
SURFACE()
);
#629=(
BOUNDED_SURFACE()
B_SPLINE_SURFACE(1,2,((#93496,#93497,#93498),(#93499,#93500,#93501)),
 .UNSPECIFIED.,.F.,.F.,.F.)
B_SPLINE_SURFACE_WITH_KNOTS((2,2),(3,3),(0.,1.),(0.00560769170938487,0.0176009697615911),
 .UNSPECIFIED.)
GEOMETRIC_REPRESENTATION_ITEM()
RATIONAL_B_SPLINE_SURFACE(((0.998183892106923,0.996573304252679,0.996380621268545),
(0.998183892106923,0.996573304252679,0.996380621268545)))
REPRESENTATION_ITEM('')
SURFACE()
);
#630=(
BOUNDED_SURFACE()
B_SPLINE_SURFACE(1,2,((#93586,#93587,#93588),(#93589,#93590,#93591)),
 .UNSPECIFIED.,.F.,.F.,.F.)
B_SPLINE_SURFACE_WITH_KNOTS((2,2),(3,3),(0.,1.),(0.0255903596132002,0.0375948596691649),
 .UNSPECIFIED.)
GEOMETRIC_REPRESENTATION_ITEM()
RATIONAL_B_SPLINE_SURFACE(((0.996753121756002,0.997505687613138,0.999678813023773),
(0.996753121756002,0.997505687613138,0.999678813023773)))
REPRESENTATION_ITEM('')
SURFACE()
);
#631=(
BOUNDED_SURFACE()
B_SPLINE_SURFACE(1,2,((#93609,#93610,#93611,#93612,#93613),(#93614,#93615,
#93616,#93617,#93618)),.UNSPECIFIED.,.F.,.F.,.F.)
B_SPLINE_SURFACE_WITH_KNOTS((2,2),(3,2,3),(0.519229702908737,1.),(0.0365944846644944,
0.0384615384615384,0.0431859278882546),.UNSPECIFIED.)
GEOMETRIC_REPRESENTATION_ITEM()
RATIONAL_B_SPLINE_SURFACE(((0.999326490452231,0.999646063968201,1.,0.99910440092888,
0.998428822114433),(0.999326490452231,0.999646063968201,1.,0.99910440092888,
0.998428822114433)))
REPRESENTATION_ITEM('')
SURFACE()
);
#632=(
BOUNDED_SURFACE()
B_SPLINE_SURFACE(1,2,((#93674,#93675,#93676),(#93677,#93678,#93679)),
 .UNSPECIFIED.,.F.,.F.,.F.)
B_SPLINE_SURFACE_WITH_KNOTS((2,2),(3,3),(0.,1.),(0.0456081671210051,0.0575989447818623),
 .UNSPECIFIED.)
GEOMETRIC_REPRESENTATION_ITEM()
RATIONAL_B_SPLINE_SURFACE(((0.997793907739636,0.99636555849969,0.996354522974128),
(0.997793907739636,0.99636555849969,0.996354522974128)))
REPRESENTATION_ITEM('')
SURFACE()
);
#633=(
BOUNDED_SURFACE()
B_SPLINE_SURFACE(1,2,((#93714,#93715,#93716),(#93717,#93718,#93719)),
 .UNSPECIFIED.,.F.,.F.,.F.)
B_SPLINE_SURFACE_WITH_KNOTS((2,2),(3,3),(0.,1.),(0.0556006976522459,0.067588885544615),
 .UNSPECIFIED.)
GEOMETRIC_REPRESENTATION_ITEM()
RATIONAL_B_SPLINE_SURFACE(((0.996397562408177,0.996150386836003,0.997319912821417),
(0.996397562408177,0.996150386836003,0.997319912821417)))
REPRESENTATION_ITEM('')
SURFACE()
);
#634=(
BOUNDED_SURFACE()
B_SPLINE_SURFACE(1,2,((#93720,#93721,#93722),(#93723,#93724,#93725)),
 .UNSPECIFIED.,.F.,.F.,.F.)
B_SPLINE_SURFACE_WITH_KNOTS((2,2),(3,3),(0.,1.),(0.0657448619281078,0.0758849574338246),
 .UNSPECIFIED.)
GEOMETRIC_REPRESENTATION_ITEM()
RATIONAL_B_SPLINE_SURFACE(((0.996993639757276,0.997798549146192,0.999617032345115),
(0.996993639757276,0.997798549146192,0.999617032345115)))
REPRESENTATION_ITEM('')
SURFACE()
);
#635=(
BOUNDED_SURFACE()
B_SPLINE_SURFACE(1,2,((#93800,#93801,#93802),(#93803,#93804,#93805)),
 .UNSPECIFIED.,.F.,.F.,.F.)
B_SPLINE_SURFACE_WITH_KNOTS((2,2),(3,3),(0.,1.),(0.00560769170938445,0.0176009697615928),
 .UNSPECIFIED.)
GEOMETRIC_REPRESENTATION_ITEM()
RATIONAL_B_SPLINE_SURFACE(((0.998183892106924,0.996573304252679,0.996380621268545),
(0.998183892106924,0.996573304252679,0.996380621268545)))
REPRESENTATION_ITEM('')
SURFACE()
);
#636=(
BOUNDED_SURFACE()
B_SPLINE_SURFACE(1,2,((#93890,#93891,#93892),(#93893,#93894,#93895)),
 .UNSPECIFIED.,.F.,.F.,.F.)
B_SPLINE_SURFACE_WITH_KNOTS((2,2),(3,3),(0.,1.),(0.0255903596131976,0.037594859669167),
 .UNSPECIFIED.)
GEOMETRIC_REPRESENTATION_ITEM()
RATIONAL_B_SPLINE_SURFACE(((0.996753121756001,0.997505687613137,0.999678813023773),
(0.996753121756001,0.997505687613137,0.999678813023773)))
REPRESENTATION_ITEM('')
SURFACE()
);
#637=(
BOUNDED_SURFACE()
B_SPLINE_SURFACE(1,2,((#93913,#93914,#93915,#93916,#93917),(#93918,#93919,
#93920,#93921,#93922)),.UNSPECIFIED.,.F.,.F.,.F.)
B_SPLINE_SURFACE_WITH_KNOTS((2,2),(3,2,3),(0.519229702908059,1.),(0.0365944846645068,
0.0384615384615384,0.0431859276813725),.UNSPECIFIED.)
GEOMETRIC_REPRESENTATION_ITEM()
RATIONAL_B_SPLINE_SURFACE(((0.999326490452235,0.999646063968204,1.,0.999104400968098,
0.9984288221736),(0.999326490452235,0.999646063968204,1.,0.999104400968098,
0.9984288221736)))
REPRESENTATION_ITEM('')
SURFACE()
);
#638=(
BOUNDED_SURFACE()
B_SPLINE_SURFACE(1,2,((#93978,#93979,#93980),(#93981,#93982,#93983)),
 .UNSPECIFIED.,.F.,.F.,.F.)
B_SPLINE_SURFACE_WITH_KNOTS((2,2),(3,3),(0.,1.),(0.0456081671210074,0.0575989447818625),
 .UNSPECIFIED.)
GEOMETRIC_REPRESENTATION_ITEM()
RATIONAL_B_SPLINE_SURFACE(((0.997793907739636,0.996365558499691,0.996354522974128),
(0.997793907739636,0.996365558499691,0.996354522974128)))
REPRESENTATION_ITEM('')
SURFACE()
);
#639=(
BOUNDED_SURFACE()
B_SPLINE_SURFACE(1,2,((#94018,#94019,#94020),(#94021,#94022,#94023)),
 .UNSPECIFIED.,.F.,.F.,.F.)
B_SPLINE_SURFACE_WITH_KNOTS((2,2),(3,3),(0.,1.),(0.0556006976522466,0.0675888855446203),
 .UNSPECIFIED.)
GEOMETRIC_REPRESENTATION_ITEM()
RATIONAL_B_SPLINE_SURFACE(((0.996397562408177,0.996150386836003,0.997319912821418),
(0.996397562408177,0.996150386836003,0.997319912821418)))
REPRESENTATION_ITEM('')
SURFACE()
);
#640=(
BOUNDED_SURFACE()
B_SPLINE_SURFACE(1,2,((#94024,#94025,#94026),(#94027,#94028,#94029)),
 .UNSPECIFIED.,.F.,.F.,.F.)
B_SPLINE_SURFACE_WITH_KNOTS((2,2),(3,3),(0.,1.),(0.0657448619281133,0.0758849574338239),
 .UNSPECIFIED.)
GEOMETRIC_REPRESENTATION_ITEM()
RATIONAL_B_SPLINE_SURFACE(((0.996993639757277,0.997798549146193,0.999617032345115),
(0.996993639757277,0.997798549146193,0.999617032345115)))
REPRESENTATION_ITEM('')
SURFACE()
);
#641=(
BOUNDED_SURFACE()
B_SPLINE_SURFACE(1,2,((#94104,#94105,#94106),(#94107,#94108,#94109)),
 .UNSPECIFIED.,.F.,.F.,.F.)
B_SPLINE_SURFACE_WITH_KNOTS((2,2),(3,3),(0.,1.),(0.00560769170938316,0.0176009697615929),
 .UNSPECIFIED.)
GEOMETRIC_REPRESENTATION_ITEM()
RATIONAL_B_SPLINE_SURFACE(((0.998183892106924,0.996573304252679,0.996380621268545),
(0.998183892106924,0.996573304252679,0.996380621268545)))
REPRESENTATION_ITEM('')
SURFACE()
);
#642=(
BOUNDED_SURFACE()
B_SPLINE_SURFACE(1,2,((#94194,#94195,#94196),(#94197,#94198,#94199)),
 .UNSPECIFIED.,.F.,.F.,.F.)
B_SPLINE_SURFACE_WITH_KNOTS((2,2),(3,3),(0.,1.),(0.0255903596132013,0.0375948596691634),
 .UNSPECIFIED.)
GEOMETRIC_REPRESENTATION_ITEM()
RATIONAL_B_SPLINE_SURFACE(((0.996753121756002,0.997505687613138,0.999678813023772),
(0.996753121756002,0.997505687613138,0.999678813023772)))
REPRESENTATION_ITEM('')
SURFACE()
);
#643=(
BOUNDED_SURFACE()
B_SPLINE_SURFACE(1,2,((#94217,#94218,#94219,#94220,#94221),(#94222,#94223,
#94224,#94225,#94226)),.UNSPECIFIED.,.F.,.F.,.F.)
B_SPLINE_SURFACE_WITH_KNOTS((2,2),(3,2,3),(0.519229702907959,1.),(0.0365944846645215,
0.0384615384615384,0.0431859278882817),.UNSPECIFIED.)
GEOMETRIC_REPRESENTATION_ITEM()
RATIONAL_B_SPLINE_SURFACE(((0.99932649045224,0.999646063968206,1.,0.999104400928875,
0.998428822114425),(0.99932649045224,0.999646063968206,1.,0.999104400928875,
0.998428822114425)))
REPRESENTATION_ITEM('')
SURFACE()
);
#644=(
BOUNDED_SURFACE()
B_SPLINE_SURFACE(1,2,((#94282,#94283,#94284),(#94285,#94286,#94287)),
 .UNSPECIFIED.,.F.,.F.,.F.)
B_SPLINE_SURFACE_WITH_KNOTS((2,2),(3,3),(0.,1.),(0.0456081671210053,0.0575989447818599),
 .UNSPECIFIED.)
GEOMETRIC_REPRESENTATION_ITEM()
RATIONAL_B_SPLINE_SURFACE(((0.997793907739636,0.996365558499691,0.996354522974128),
(0.997793907739636,0.996365558499691,0.996354522974128)))
REPRESENTATION_ITEM('')
SURFACE()
);
#645=(
BOUNDED_SURFACE()
B_SPLINE_SURFACE(1,2,((#94322,#94323,#94324),(#94325,#94326,#94327)),
 .UNSPECIFIED.,.F.,.F.,.F.)
B_SPLINE_SURFACE_WITH_KNOTS((2,2),(3,3),(0.,1.),(0.0556006976522416,0.0675888855446144),
 .UNSPECIFIED.)
GEOMETRIC_REPRESENTATION_ITEM()
RATIONAL_B_SPLINE_SURFACE(((0.996397562408177,0.996150386836003,0.997319912821417),
(0.996397562408177,0.996150386836003,0.997319912821417)))
REPRESENTATION_ITEM('')
SURFACE()
);
#646=(
BOUNDED_SURFACE()
B_SPLINE_SURFACE(1,2,((#94328,#94329,#94330),(#94331,#94332,#94333)),
 .UNSPECIFIED.,.F.,.F.,.F.)
B_SPLINE_SURFACE_WITH_KNOTS((2,2),(3,3),(0.,1.),(0.0657448619281068,0.0758849574338251),
 .UNSPECIFIED.)
GEOMETRIC_REPRESENTATION_ITEM()
RATIONAL_B_SPLINE_SURFACE(((0.996993639757276,0.997798549146192,0.999617032345115),
(0.996993639757276,0.997798549146192,0.999617032345115)))
REPRESENTATION_ITEM('')
SURFACE()
);
#647=(
BOUNDED_SURFACE()
B_SPLINE_SURFACE(1,2,((#94408,#94409,#94410),(#94411,#94412,#94413)),
 .UNSPECIFIED.,.F.,.F.,.F.)
B_SPLINE_SURFACE_WITH_KNOTS((2,2),(3,3),(0.,1.),(0.00560769170938346,0.0176009697615929),
 .UNSPECIFIED.)
GEOMETRIC_REPRESENTATION_ITEM()
RATIONAL_B_SPLINE_SURFACE(((0.998183892106924,0.996573304252679,0.996380621268545),
(0.998183892106924,0.996573304252679,0.996380621268545)))
REPRESENTATION_ITEM('')
SURFACE()
);
#648=(
BOUNDED_SURFACE()
B_SPLINE_SURFACE(1,2,((#94498,#94499,#94500),(#94501,#94502,#94503)),
 .UNSPECIFIED.,.F.,.F.,.F.)
B_SPLINE_SURFACE_WITH_KNOTS((2,2),(3,3),(0.,1.),(0.0255903596132008,0.0375948596691676),
 .UNSPECIFIED.)
GEOMETRIC_REPRESENTATION_ITEM()
RATIONAL_B_SPLINE_SURFACE(((0.996753121756002,0.997505687613138,0.999678813023774),
(0.996753121756002,0.997505687613138,0.999678813023774)))
REPRESENTATION_ITEM('')
SURFACE()
);
#649=(
BOUNDED_SURFACE()
B_SPLINE_SURFACE(1,2,((#94521,#94522,#94523,#94524,#94525),(#94526,#94527,
#94528,#94529,#94530)),.UNSPECIFIED.,.F.,.F.,.F.)
B_SPLINE_SURFACE_WITH_KNOTS((2,2),(3,2,3),(0.519229702908038,1.),(0.0365944846645354,
0.0384615384615384,0.0431859278882965),.UNSPECIFIED.)
GEOMETRIC_REPRESENTATION_ITEM()
RATIONAL_B_SPLINE_SURFACE(((0.999326490452245,0.999646063968209,1.,0.999104400928872,
0.998428822114421),(0.999326490452245,0.999646063968209,1.,0.999104400928872,
0.998428822114421)))
REPRESENTATION_ITEM('')
SURFACE()
);
#650=(
BOUNDED_SURFACE()
B_SPLINE_SURFACE(1,2,((#94586,#94587,#94588),(#94589,#94590,#94591)),
 .UNSPECIFIED.,.F.,.F.,.F.)
B_SPLINE_SURFACE_WITH_KNOTS((2,2),(3,3),(0.,1.),(0.0456081671210039,0.0575989447818623),
 .UNSPECIFIED.)
GEOMETRIC_REPRESENTATION_ITEM()
RATIONAL_B_SPLINE_SURFACE(((0.997793907739636,0.996365558499691,0.996354522974129),
(0.997793907739636,0.996365558499691,0.996354522974129)))
REPRESENTATION_ITEM('')
SURFACE()
);
#651=(
BOUNDED_SURFACE()
B_SPLINE_SURFACE(1,2,((#94626,#94627,#94628),(#94629,#94630,#94631)),
 .UNSPECIFIED.,.F.,.F.,.F.)
B_SPLINE_SURFACE_WITH_KNOTS((2,2),(3,3),(0.,1.),(0.0556006976522458,0.0675888855446171),
 .UNSPECIFIED.)
GEOMETRIC_REPRESENTATION_ITEM()
RATIONAL_B_SPLINE_SURFACE(((0.996397562408177,0.996150386836003,0.997319912821417),
(0.996397562408177,0.996150386836003,0.997319912821417)))
REPRESENTATION_ITEM('')
SURFACE()
);
#652=(
BOUNDED_SURFACE()
B_SPLINE_SURFACE(1,2,((#94632,#94633,#94634),(#94635,#94636,#94637)),
 .UNSPECIFIED.,.F.,.F.,.F.)
B_SPLINE_SURFACE_WITH_KNOTS((2,2),(3,3),(0.,1.),(0.06574486192811,0.0758849574338243),
 .UNSPECIFIED.)
GEOMETRIC_REPRESENTATION_ITEM()
RATIONAL_B_SPLINE_SURFACE(((0.996993639757276,0.997798549146193,0.999617032345115),
(0.996993639757276,0.997798549146193,0.999617032345115)))
REPRESENTATION_ITEM('')
SURFACE()
);
#653=(
BOUNDED_SURFACE()
B_SPLINE_SURFACE(1,2,((#94712,#94713,#94714),(#94715,#94716,#94717)),
 .UNSPECIFIED.,.F.,.F.,.F.)
B_SPLINE_SURFACE_WITH_KNOTS((2,2),(3,3),(0.,1.),(0.00560769170938328,0.0176009697615924),
 .UNSPECIFIED.)
GEOMETRIC_REPRESENTATION_ITEM()
RATIONAL_B_SPLINE_SURFACE(((0.998183892106924,0.996573304252679,0.996380621268545),
(0.998183892106924,0.996573304252679,0.996380621268545)))
REPRESENTATION_ITEM('')
SURFACE()
);
#654=(
BOUNDED_SURFACE()
B_SPLINE_SURFACE(1,2,((#94802,#94803,#94804),(#94805,#94806,#94807)),
 .UNSPECIFIED.,.F.,.F.,.F.)
B_SPLINE_SURFACE_WITH_KNOTS((2,2),(3,3),(0.,1.),(0.0255903596131998,0.0375948596691678),
 .UNSPECIFIED.)
GEOMETRIC_REPRESENTATION_ITEM()
RATIONAL_B_SPLINE_SURFACE(((0.996753121756002,0.997505687613138,0.999678813023774),
(0.996753121756002,0.997505687613138,0.999678813023774)))
REPRESENTATION_ITEM('')
SURFACE()
);
#655=(
BOUNDED_SURFACE()
B_SPLINE_SURFACE(1,2,((#94825,#94826,#94827,#94828,#94829),(#94830,#94831,
#94832,#94833,#94834)),.UNSPECIFIED.,.F.,.F.,.F.)
B_SPLINE_SURFACE_WITH_KNOTS((2,2),(3,2,3),(0.519229702908415,1.),(0.0365944846645497,
0.0384615384615384,0.0431859278883109),.UNSPECIFIED.)
GEOMETRIC_REPRESENTATION_ITEM()
RATIONAL_B_SPLINE_SURFACE(((0.99932649045225,0.999646063968212,1.,0.999104400928869,
0.998428822114416),(0.99932649045225,0.999646063968212,1.,0.999104400928869,
0.998428822114416)))
REPRESENTATION_ITEM('')
SURFACE()
);
#656=(
BOUNDED_SURFACE()
B_SPLINE_SURFACE(1,2,((#94890,#94891,#94892),(#94893,#94894,#94895)),
 .UNSPECIFIED.,.F.,.F.,.F.)
B_SPLINE_SURFACE_WITH_KNOTS((2,2),(3,3),(0.,1.),(0.045608167121011,0.0575989447818594),
 .UNSPECIFIED.)
GEOMETRIC_REPRESENTATION_ITEM()
RATIONAL_B_SPLINE_SURFACE(((0.997793907739635,0.996365558499691,0.996354522974128),
(0.997793907739635,0.996365558499691,0.996354522974128)))
REPRESENTATION_ITEM('')
SURFACE()
);
#657=(
BOUNDED_SURFACE()
B_SPLINE_SURFACE(1,2,((#94930,#94931,#94932),(#94933,#94934,#94935)),
 .UNSPECIFIED.,.F.,.F.,.F.)
B_SPLINE_SURFACE_WITH_KNOTS((2,2),(3,3),(0.,1.),(0.0556006976522414,0.0675888855446165),
 .UNSPECIFIED.)
GEOMETRIC_REPRESENTATION_ITEM()
RATIONAL_B_SPLINE_SURFACE(((0.996397562408177,0.996150386836003,0.997319912821417),
(0.996397562408177,0.996150386836003,0.997319912821417)))
REPRESENTATION_ITEM('')
SURFACE()
);
#658=(
BOUNDED_SURFACE()
B_SPLINE_SURFACE(1,2,((#94936,#94937,#94938),(#94939,#94940,#94941)),
 .UNSPECIFIED.,.F.,.F.,.F.)
B_SPLINE_SURFACE_WITH_KNOTS((2,2),(3,3),(0.,1.),(0.0657448619281089,0.0758849574338246),
 .UNSPECIFIED.)
GEOMETRIC_REPRESENTATION_ITEM()
RATIONAL_B_SPLINE_SURFACE(((0.996993639757276,0.997798549146193,0.999617032345115),
(0.996993639757276,0.997798549146193,0.999617032345115)))
REPRESENTATION_ITEM('')
SURFACE()
);
#659=(
BOUNDED_SURFACE()
B_SPLINE_SURFACE(1,2,((#95016,#95017,#95018),(#95019,#95020,#95021)),
 .UNSPECIFIED.,.F.,.F.,.F.)
B_SPLINE_SURFACE_WITH_KNOTS((2,2),(3,3),(0.,1.),(0.00560769170938354,0.0176009697615918),
 .UNSPECIFIED.)
GEOMETRIC_REPRESENTATION_ITEM()
RATIONAL_B_SPLINE_SURFACE(((0.998183892106924,0.996573304252679,0.996380621268545),
(0.998183892106924,0.996573304252679,0.996380621268545)))
REPRESENTATION_ITEM('')
SURFACE()
);
#660=(
BOUNDED_SURFACE()
B_SPLINE_SURFACE(1,2,((#95106,#95107,#95108),(#95109,#95110,#95111)),
 .UNSPECIFIED.,.F.,.F.,.F.)
B_SPLINE_SURFACE_WITH_KNOTS((2,2),(3,3),(0.,1.),(0.0255903596131989,0.037594859669165),
 .UNSPECIFIED.)
GEOMETRIC_REPRESENTATION_ITEM()
RATIONAL_B_SPLINE_SURFACE(((0.996753121756001,0.997505687613137,0.999678813023773),
(0.996753121756001,0.997505687613137,0.999678813023773)))
REPRESENTATION_ITEM('')
SURFACE()
);
#661=(
BOUNDED_SURFACE()
B_SPLINE_SURFACE(1,2,((#95129,#95130,#95131,#95132,#95133),(#95134,#95135,
#95136,#95137,#95138)),.UNSPECIFIED.,.F.,.F.,.F.)
B_SPLINE_SURFACE_WITH_KNOTS((2,2),(3,2,3),(0.519229702909028,1.),(0.036594484664565,
0.0384615384615384,0.0431859278100856),.UNSPECIFIED.)
GEOMETRIC_REPRESENTATION_ITEM()
RATIONAL_B_SPLINE_SURFACE(((0.999326490452255,0.999646063968215,1.,0.999104400943698,
0.998428822136789),(0.999326490452255,0.999646063968215,1.,0.999104400943698,
0.998428822136789)))
REPRESENTATION_ITEM('')
SURFACE()
);
#662=(
BOUNDED_SURFACE()
B_SPLINE_SURFACE(1,2,((#95194,#95195,#95196),(#95197,#95198,#95199)),
 .UNSPECIFIED.,.F.,.F.,.F.)
B_SPLINE_SURFACE_WITH_KNOTS((2,2),(3,3),(0.,1.),(0.0456081671210063,0.0575989447818626),
 .UNSPECIFIED.)
GEOMETRIC_REPRESENTATION_ITEM()
RATIONAL_B_SPLINE_SURFACE(((0.997793907739636,0.99636555849969,0.996354522974128),
(0.997793907739636,0.99636555849969,0.996354522974128)))
REPRESENTATION_ITEM('')
SURFACE()
);
#663=(
BOUNDED_SURFACE()
B_SPLINE_SURFACE(1,2,((#95234,#95235,#95236),(#95237,#95238,#95239)),
 .UNSPECIFIED.,.F.,.F.,.F.)
B_SPLINE_SURFACE_WITH_KNOTS((2,2),(3,3),(0.,1.),(0.0556006976522473,0.0675888855446128),
 .UNSPECIFIED.)
GEOMETRIC_REPRESENTATION_ITEM()
RATIONAL_B_SPLINE_SURFACE(((0.996397562408177,0.996150386836004,0.997319912821417),
(0.996397562408177,0.996150386836004,0.997319912821417)))
REPRESENTATION_ITEM('')
SURFACE()
);
#664=(
BOUNDED_SURFACE()
B_SPLINE_SURFACE(1,2,((#95240,#95241,#95242),(#95243,#95244,#95245)),
 .UNSPECIFIED.,.F.,.F.,.F.)
B_SPLINE_SURFACE_WITH_KNOTS((2,2),(3,3),(0.,1.),(0.0657448619281057,0.0758849574338256),
 .UNSPECIFIED.)
GEOMETRIC_REPRESENTATION_ITEM()
RATIONAL_B_SPLINE_SURFACE(((0.996993639757275,0.997798549146192,0.999617032345116),
(0.996993639757275,0.997798549146192,0.999617032345116)))
REPRESENTATION_ITEM('')
SURFACE()
);
#665=(
BOUNDED_SURFACE()
B_SPLINE_SURFACE(1,2,((#95320,#95321,#95322),(#95323,#95324,#95325)),
 .UNSPECIFIED.,.F.,.F.,.F.)
B_SPLINE_SURFACE_WITH_KNOTS((2,2),(3,3),(0.,1.),(0.00560769170938434,0.0176009697615933),
 .UNSPECIFIED.)
GEOMETRIC_REPRESENTATION_ITEM()
RATIONAL_B_SPLINE_SURFACE(((0.998183892106924,0.996573304252679,0.996380621268545),
(0.998183892106924,0.996573304252679,0.996380621268545)))
REPRESENTATION_ITEM('')
SURFACE()
);
#666=(
BOUNDED_SURFACE()
B_SPLINE_SURFACE(1,2,((#95410,#95411,#95412),(#95413,#95414,#95415)),
 .UNSPECIFIED.,.F.,.F.,.F.)
B_SPLINE_SURFACE_WITH_KNOTS((2,2),(3,3),(0.,1.),(0.0255903596132,0.037594859669166),
 .UNSPECIFIED.)
GEOMETRIC_REPRESENTATION_ITEM()
RATIONAL_B_SPLINE_SURFACE(((0.996753121756002,0.997505687613138,0.999678813023773),
(0.996753121756002,0.997505687613138,0.999678813023773)))
REPRESENTATION_ITEM('')
SURFACE()
);
#667=(
BOUNDED_SURFACE()
B_SPLINE_SURFACE(1,2,((#95433,#95434,#95435,#95436,#95437),(#95438,#95439,
#95440,#95441,#95442)),.UNSPECIFIED.,.F.,.F.,.F.)
B_SPLINE_SURFACE_WITH_KNOTS((2,2),(3,2,3),(0.519229702909967,1.),(0.0365944846645798,
0.0384615384615384,0.0431859276814445),.UNSPECIFIED.)
GEOMETRIC_REPRESENTATION_ITEM()
RATIONAL_B_SPLINE_SURFACE(((0.99932649045226,0.999646063968218,1.,0.999104400968085,
0.99842882217358),(0.99932649045226,0.999646063968218,1.,0.999104400968085,
0.99842882217358)))
REPRESENTATION_ITEM('')
SURFACE()
);
#668=(
BOUNDED_SURFACE()
B_SPLINE_SURFACE(1,2,((#95498,#95499,#95500),(#95501,#95502,#95503)),
 .UNSPECIFIED.,.F.,.F.,.F.)
B_SPLINE_SURFACE_WITH_KNOTS((2,2),(3,3),(0.,1.),(0.0456081671210074,0.0575989447818626),
 .UNSPECIFIED.)
GEOMETRIC_REPRESENTATION_ITEM()
RATIONAL_B_SPLINE_SURFACE(((0.997793907739635,0.996365558499691,0.996354522974128),
(0.997793907739635,0.996365558499691,0.996354522974128)))
REPRESENTATION_ITEM('')
SURFACE()
);
#669=(
BOUNDED_SURFACE()
B_SPLINE_SURFACE(1,2,((#95538,#95539,#95540),(#95541,#95542,#95543)),
 .UNSPECIFIED.,.F.,.F.,.F.)
B_SPLINE_SURFACE_WITH_KNOTS((2,2),(3,3),(0.,1.),(0.0556006976522466,0.0675888855446202),
 .UNSPECIFIED.)
GEOMETRIC_REPRESENTATION_ITEM()
RATIONAL_B_SPLINE_SURFACE(((0.996397562408177,0.996150386836003,0.997319912821418),
(0.996397562408177,0.996150386836003,0.997319912821418)))
REPRESENTATION_ITEM('')
SURFACE()
);
#670=(
BOUNDED_SURFACE()
B_SPLINE_SURFACE(1,2,((#95544,#95545,#95546),(#95547,#95548,#95549)),
 .UNSPECIFIED.,.F.,.F.,.F.)
B_SPLINE_SURFACE_WITH_KNOTS((2,2),(3,3),(0.,1.),(0.0657448619281132,0.0758849574338236),
 .UNSPECIFIED.)
GEOMETRIC_REPRESENTATION_ITEM()
RATIONAL_B_SPLINE_SURFACE(((0.996993639757277,0.997798549146193,0.999617032345115),
(0.996993639757277,0.997798549146193,0.999617032345115)))
REPRESENTATION_ITEM('')
SURFACE()
);
#671=(
BOUNDED_SURFACE()
B_SPLINE_SURFACE(1,2,((#95624,#95625,#95626),(#95627,#95628,#95629)),
 .UNSPECIFIED.,.F.,.F.,.F.)
B_SPLINE_SURFACE_WITH_KNOTS((2,2),(3,3),(0.,1.),(0.00560769170938474,0.0176009697615934),
 .UNSPECIFIED.)
GEOMETRIC_REPRESENTATION_ITEM()
RATIONAL_B_SPLINE_SURFACE(((0.998183892106924,0.996573304252679,0.996380621268545),
(0.998183892106924,0.996573304252679,0.996380621268545)))
REPRESENTATION_ITEM('')
SURFACE()
);
#672=(
BOUNDED_SURFACE()
B_SPLINE_SURFACE(1,2,((#95714,#95715,#95716),(#95717,#95718,#95719)),
 .UNSPECIFIED.,.F.,.F.,.F.)
B_SPLINE_SURFACE_WITH_KNOTS((2,2),(3,3),(0.,1.),(0.0255903596132025,0.0375948596691633),
 .UNSPECIFIED.)
GEOMETRIC_REPRESENTATION_ITEM()
RATIONAL_B_SPLINE_SURFACE(((0.996753121756002,0.997505687613138,0.999678813023772),
(0.996753121756002,0.997505687613138,0.999678813023772)))
REPRESENTATION_ITEM('')
SURFACE()
);
#673=(
BOUNDED_SURFACE()
B_SPLINE_SURFACE(1,2,((#95737,#95738,#95739,#95740,#95741),(#95742,#95743,
#95744,#95745,#95746)),.UNSPECIFIED.,.F.,.F.,.F.)
B_SPLINE_SURFACE_WITH_KNOTS((2,2),(3,2,3),(0.519229702911282,1.),(0.036594484664593,
0.0384615384615384,0.0431859278883545),.UNSPECIFIED.)
GEOMETRIC_REPRESENTATION_ITEM()
RATIONAL_B_SPLINE_SURFACE(((0.999326490452264,0.99964606396822,1.,0.999104400928861,
0.998428822114404),(0.999326490452264,0.99964606396822,1.,0.999104400928861,
0.998428822114404)))
REPRESENTATION_ITEM('')
SURFACE()
);
#674=(
BOUNDED_SURFACE()
B_SPLINE_SURFACE(1,2,((#95802,#95803,#95804),(#95805,#95806,#95807)),
 .UNSPECIFIED.,.F.,.F.,.F.)
B_SPLINE_SURFACE_WITH_KNOTS((2,2),(3,3),(0.,1.),(0.045608167121007,0.0575989447818626),
 .UNSPECIFIED.)
GEOMETRIC_REPRESENTATION_ITEM()
RATIONAL_B_SPLINE_SURFACE(((0.997793907739636,0.996365558499691,0.996354522974128),
(0.997793907739636,0.996365558499691,0.996354522974128)))
REPRESENTATION_ITEM('')
SURFACE()
);
#675=(
BOUNDED_SURFACE()
B_SPLINE_SURFACE(1,2,((#95842,#95843,#95844),(#95845,#95846,#95847)),
 .UNSPECIFIED.,.F.,.F.,.F.)
B_SPLINE_SURFACE_WITH_KNOTS((2,2),(3,3),(0.,1.),(0.0556006976522468,0.067588885544617),
 .UNSPECIFIED.)
GEOMETRIC_REPRESENTATION_ITEM()
RATIONAL_B_SPLINE_SURFACE(((0.996397562408177,0.996150386836003,0.997319912821417),
(0.996397562408177,0.996150386836003,0.997319912821417)))
REPRESENTATION_ITEM('')
SURFACE()
);
#676=(
BOUNDED_SURFACE()
B_SPLINE_SURFACE(1,2,((#95848,#95849,#95850),(#95851,#95852,#95853)),
 .UNSPECIFIED.,.F.,.F.,.F.)
B_SPLINE_SURFACE_WITH_KNOTS((2,2),(3,3),(0.,1.),(0.06574486192811,0.0758849574338238),
 .UNSPECIFIED.)
GEOMETRIC_REPRESENTATION_ITEM()
RATIONAL_B_SPLINE_SURFACE(((0.996993639757276,0.997798549146193,0.999617032345115),
(0.996993639757276,0.997798549146193,0.999617032345115)))
REPRESENTATION_ITEM('')
SURFACE()
);
#677=(
BOUNDED_SURFACE()
B_SPLINE_SURFACE(1,2,((#95928,#95929,#95930),(#95931,#95932,#95933)),
 .UNSPECIFIED.,.F.,.F.,.F.)
B_SPLINE_SURFACE_WITH_KNOTS((2,2),(3,3),(0.,1.),(0.00560769170938203,0.017600969761593),
 .UNSPECIFIED.)
GEOMETRIC_REPRESENTATION_ITEM()
RATIONAL_B_SPLINE_SURFACE(((0.998183892106924,0.996573304252679,0.996380621268545),
(0.998183892106924,0.996573304252679,0.996380621268545)))
REPRESENTATION_ITEM('')
SURFACE()
);
#678=(
BOUNDED_SURFACE()
B_SPLINE_SURFACE(1,2,((#96018,#96019,#96020),(#96021,#96022,#96023)),
 .UNSPECIFIED.,.F.,.F.,.F.)
B_SPLINE_SURFACE_WITH_KNOTS((2,2),(3,3),(0.,1.),(0.0255903596131999,0.0375948596691669),
 .UNSPECIFIED.)
GEOMETRIC_REPRESENTATION_ITEM()
RATIONAL_B_SPLINE_SURFACE(((0.996753121756002,0.997505687613138,0.999678813023773),
(0.996753121756002,0.997505687613138,0.999678813023773)))
REPRESENTATION_ITEM('')
SURFACE()
);
#679=(
BOUNDED_SURFACE()
B_SPLINE_SURFACE(1,2,((#96041,#96042,#96043,#96044,#96045),(#96046,#96047,
#96048,#96049,#96050)),.UNSPECIFIED.,.F.,.F.,.F.)
B_SPLINE_SURFACE_WITH_KNOTS((2,2),(3,2,3),(0.51922970291275,1.),(0.036594484664607,
0.0384615384615384,0.0431859278883671),.UNSPECIFIED.)
GEOMETRIC_REPRESENTATION_ITEM()
RATIONAL_B_SPLINE_SURFACE(((0.999326490452269,0.999646063968222,1.,0.999104400928858,
0.998428822114401),(0.999326490452269,0.999646063968222,1.,0.999104400928858,
0.998428822114401)))
REPRESENTATION_ITEM('')
SURFACE()
);
#680=(
BOUNDED_SURFACE()
B_SPLINE_SURFACE(1,2,((#96106,#96107,#96108),(#96109,#96110,#96111)),
 .UNSPECIFIED.,.F.,.F.,.F.)
B_SPLINE_SURFACE_WITH_KNOTS((2,2),(3,3),(0.,1.),(0.0456081671210039,0.0575989447818618),
 .UNSPECIFIED.)
GEOMETRIC_REPRESENTATION_ITEM()
RATIONAL_B_SPLINE_SURFACE(((0.997793907739636,0.996365558499691,0.996354522974128),
(0.997793907739636,0.996365558499691,0.996354522974128)))
REPRESENTATION_ITEM('')
SURFACE()
);
#681=(
BOUNDED_SURFACE()
B_SPLINE_SURFACE(1,2,((#96146,#96147,#96148),(#96149,#96150,#96151)),
 .UNSPECIFIED.,.F.,.F.,.F.)
B_SPLINE_SURFACE_WITH_KNOTS((2,2),(3,3),(0.,1.),(0.0556006976522446,0.0675888855446173),
 .UNSPECIFIED.)
GEOMETRIC_REPRESENTATION_ITEM()
RATIONAL_B_SPLINE_SURFACE(((0.996397562408177,0.996150386836003,0.997319912821418),
(0.996397562408177,0.996150386836003,0.997319912821418)))
REPRESENTATION_ITEM('')
SURFACE()
);
#682=(
BOUNDED_SURFACE()
B_SPLINE_SURFACE(1,2,((#96152,#96153,#96154),(#96155,#96156,#96157)),
 .UNSPECIFIED.,.F.,.F.,.F.)
B_SPLINE_SURFACE_WITH_KNOTS((2,2),(3,3),(0.,1.),(0.0657448619281101,0.0758849574338239),
 .UNSPECIFIED.)
GEOMETRIC_REPRESENTATION_ITEM()
RATIONAL_B_SPLINE_SURFACE(((0.996993639757276,0.997798549146193,0.999617032345115),
(0.996993639757276,0.997798549146193,0.999617032345115)))
REPRESENTATION_ITEM('')
SURFACE()
);
#683=(
BOUNDED_SURFACE()
B_SPLINE_SURFACE(1,2,((#96232,#96233,#96234),(#96235,#96236,#96237)),
 .UNSPECIFIED.,.F.,.F.,.F.)
B_SPLINE_SURFACE_WITH_KNOTS((2,2),(3,3),(0.,1.),(0.00560769170938346,0.0176009697615912),
 .UNSPECIFIED.)
GEOMETRIC_REPRESENTATION_ITEM()
RATIONAL_B_SPLINE_SURFACE(((0.998183892106924,0.996573304252679,0.996380621268545),
(0.998183892106924,0.996573304252679,0.996380621268545)))
REPRESENTATION_ITEM('')
SURFACE()
);
#684=(
BOUNDED_SURFACE()
B_SPLINE_SURFACE(1,2,((#96322,#96323,#96324),(#96325,#96326,#96327)),
 .UNSPECIFIED.,.F.,.F.,.F.)
B_SPLINE_SURFACE_WITH_KNOTS((2,2),(3,3),(0.,1.),(0.0255903596131992,0.0375948596691636),
 .UNSPECIFIED.)
GEOMETRIC_REPRESENTATION_ITEM()
RATIONAL_B_SPLINE_SURFACE(((0.996753121756001,0.997505687613137,0.999678813023772),
(0.996753121756001,0.997505687613137,0.999678813023772)))
REPRESENTATION_ITEM('')
SURFACE()
);
#685=(
BOUNDED_SURFACE()
B_SPLINE_SURFACE(1,2,((#96345,#96346,#96347,#96348,#96349),(#96350,#96351,
#96352,#96353,#96354)),.UNSPECIFIED.,.F.,.F.,.F.)
B_SPLINE_SURFACE_WITH_KNOTS((2,2),(3,2,3),(0.51922970291459,1.),(0.0365944846646184,
0.0384615384615384,0.0431859278883792),.UNSPECIFIED.)
GEOMETRIC_REPRESENTATION_ITEM()
RATIONAL_B_SPLINE_SURFACE(((0.999326490452273,0.999646063968225,1.,0.999104400928856,
0.998428822114397),(0.999326490452273,0.999646063968225,1.,0.999104400928856,
0.998428822114397)))
REPRESENTATION_ITEM('')
SURFACE()
);
#686=(
BOUNDED_SURFACE()
B_SPLINE_SURFACE(1,2,((#96410,#96411,#96412),(#96413,#96414,#96415)),
 .UNSPECIFIED.,.F.,.F.,.F.)
B_SPLINE_SURFACE_WITH_KNOTS((2,2),(3,3),(0.,1.),(0.0456081671210053,0.0575989447818604),
 .UNSPECIFIED.)
GEOMETRIC_REPRESENTATION_ITEM()
RATIONAL_B_SPLINE_SURFACE(((0.997793907739636,0.996365558499691,0.996354522974128),
(0.997793907739636,0.996365558499691,0.996354522974128)))
REPRESENTATION_ITEM('')
SURFACE()
);
#687=(
BOUNDED_SURFACE()
B_SPLINE_SURFACE(1,2,((#96450,#96451,#96452),(#96453,#96454,#96455)),
 .UNSPECIFIED.,.F.,.F.,.F.)
B_SPLINE_SURFACE_WITH_KNOTS((2,2),(3,3),(0.,1.),(0.0556006976522424,0.0675888855446163),
 .UNSPECIFIED.)
GEOMETRIC_REPRESENTATION_ITEM()
RATIONAL_B_SPLINE_SURFACE(((0.996397562408177,0.996150386836003,0.997319912821417),
(0.996397562408177,0.996150386836003,0.997319912821417)))
REPRESENTATION_ITEM('')
SURFACE()
);
#688=(
BOUNDED_SURFACE()
B_SPLINE_SURFACE(1,2,((#96456,#96457,#96458),(#96459,#96460,#96461)),
 .UNSPECIFIED.,.F.,.F.,.F.)
B_SPLINE_SURFACE_WITH_KNOTS((2,2),(3,3),(0.,1.),(0.065744861928109,0.0758849574338236),
 .UNSPECIFIED.)
GEOMETRIC_REPRESENTATION_ITEM()
RATIONAL_B_SPLINE_SURFACE(((0.996993639757276,0.997798549146192,0.999617032345115),
(0.996993639757276,0.997798549146192,0.999617032345115)))
REPRESENTATION_ITEM('')
SURFACE()
);
#689=(
BOUNDED_SURFACE()
B_SPLINE_SURFACE(1,2,((#96536,#96537,#96538),(#96539,#96540,#96541)),
 .UNSPECIFIED.,.F.,.F.,.F.)
B_SPLINE_SURFACE_WITH_KNOTS((2,2),(3,3),(0.,1.),(0.00560769170938321,0.0176009697615924),
 .UNSPECIFIED.)
GEOMETRIC_REPRESENTATION_ITEM()
RATIONAL_B_SPLINE_SURFACE(((0.998183892106924,0.996573304252679,0.996380621268545),
(0.998183892106924,0.996573304252679,0.996380621268545)))
REPRESENTATION_ITEM('')
SURFACE()
);
#690=(
BOUNDED_SURFACE()
B_SPLINE_SURFACE(1,2,((#96626,#96627,#96628),(#96629,#96630,#96631)),
 .UNSPECIFIED.,.F.,.F.,.F.)
B_SPLINE_SURFACE_WITH_KNOTS((2,2),(3,3),(0.,1.),(0.0255903596131988,0.0375948596691661),
 .UNSPECIFIED.)
GEOMETRIC_REPRESENTATION_ITEM()
RATIONAL_B_SPLINE_SURFACE(((0.996753121756001,0.997505687613137,0.999678813023773),
(0.996753121756001,0.997505687613137,0.999678813023773)))
REPRESENTATION_ITEM('')
SURFACE()
);
#691=(
BOUNDED_SURFACE()
B_SPLINE_SURFACE(1,2,((#96649,#96650,#96651,#96652,#96653),(#96654,#96655,
#96656,#96657,#96658)),.UNSPECIFIED.,.F.,.F.,.F.)
B_SPLINE_SURFACE_WITH_KNOTS((2,2),(3,2,3),(0.519229702916504,1.),(0.036594484664629,
0.0384615384615384,0.0431859278883907),.UNSPECIFIED.)
GEOMETRIC_REPRESENTATION_ITEM()
RATIONAL_B_SPLINE_SURFACE(((0.999326490452277,0.999646063968227,1.,0.999104400928854,
0.998428822114394),(0.999326490452277,0.999646063968227,1.,0.999104400928854,
0.998428822114394)))
REPRESENTATION_ITEM('')
SURFACE()
);
#692=(
BOUNDED_SURFACE()
B_SPLINE_SURFACE(1,2,((#96714,#96715,#96716),(#96717,#96718,#96719)),
 .UNSPECIFIED.,.F.,.F.,.F.)
B_SPLINE_SURFACE_WITH_KNOTS((2,2),(3,3),(0.,1.),(0.0456081671210051,0.0575989447818622),
 .UNSPECIFIED.)
GEOMETRIC_REPRESENTATION_ITEM()
RATIONAL_B_SPLINE_SURFACE(((0.997793907739636,0.996365558499691,0.996354522974128),
(0.997793907739636,0.996365558499691,0.996354522974128)))
REPRESENTATION_ITEM('')
SURFACE()
);
#693=(
BOUNDED_SURFACE()
B_SPLINE_SURFACE(1,2,((#96754,#96755,#96756),(#96757,#96758,#96759)),
 .UNSPECIFIED.,.F.,.F.,.F.)
B_SPLINE_SURFACE_WITH_KNOTS((2,2),(3,3),(0.,1.),(0.0556006976522459,0.0675888855446151),
 .UNSPECIFIED.)
GEOMETRIC_REPRESENTATION_ITEM()
RATIONAL_B_SPLINE_SURFACE(((0.996397562408177,0.996150386836003,0.997319912821417),
(0.996397562408177,0.996150386836003,0.997319912821417)))
REPRESENTATION_ITEM('')
SURFACE()
);
#694=(
BOUNDED_SURFACE()
B_SPLINE_SURFACE(1,2,((#96760,#96761,#96762),(#96763,#96764,#96765)),
 .UNSPECIFIED.,.F.,.F.,.F.)
B_SPLINE_SURFACE_WITH_KNOTS((2,2),(3,3),(0.,1.),(0.065744861928108,0.0758849574338239),
 .UNSPECIFIED.)
GEOMETRIC_REPRESENTATION_ITEM()
RATIONAL_B_SPLINE_SURFACE(((0.996993639757276,0.997798549146192,0.999617032345115),
(0.996993639757276,0.997798549146192,0.999617032345115)))
REPRESENTATION_ITEM('')
SURFACE()
);
#695=(
BOUNDED_SURFACE()
B_SPLINE_SURFACE(1,2,((#96840,#96841,#96842),(#96843,#96844,#96845)),
 .UNSPECIFIED.,.F.,.F.,.F.)
B_SPLINE_SURFACE_WITH_KNOTS((2,2),(3,3),(0.,1.),(0.0056076917093823,0.0176009697615919),
 .UNSPECIFIED.)
GEOMETRIC_REPRESENTATION_ITEM()
RATIONAL_B_SPLINE_SURFACE(((0.998183892106924,0.996573304252679,0.996380621268545),
(0.998183892106924,0.996573304252679,0.996380621268545)))
REPRESENTATION_ITEM('')
SURFACE()
);
#696=(
BOUNDED_SURFACE()
B_SPLINE_SURFACE(1,2,((#96930,#96931,#96932),(#96933,#96934,#96935)),
 .UNSPECIFIED.,.F.,.F.,.F.)
B_SPLINE_SURFACE_WITH_KNOTS((2,2),(3,3),(0.,1.),(0.0255903596131989,0.0375948596691636),
 .UNSPECIFIED.)
GEOMETRIC_REPRESENTATION_ITEM()
RATIONAL_B_SPLINE_SURFACE(((0.996753121756001,0.997505687613137,0.999678813023772),
(0.996753121756001,0.997505687613137,0.999678813023772)))
REPRESENTATION_ITEM('')
SURFACE()
);
#697=(
BOUNDED_SURFACE()
B_SPLINE_SURFACE(1,2,((#96953,#96954,#96955,#96956,#96957),(#96958,#96959,
#96960,#96961,#96962)),.UNSPECIFIED.,.F.,.F.,.F.)
B_SPLINE_SURFACE_WITH_KNOTS((2,2),(3,2,3),(0.519229702918739,1.),(0.0365944846646386,
0.0384615384615384,0.0431859278884007),.UNSPECIFIED.)
GEOMETRIC_REPRESENTATION_ITEM()
RATIONAL_B_SPLINE_SURFACE(((0.99932649045228,0.999646063968229,1.,0.999104400928852,
0.998428822114391),(0.99932649045228,0.999646063968229,1.,0.999104400928852,
0.998428822114391)))
REPRESENTATION_ITEM('')
SURFACE()
);
#698=(
BOUNDED_SURFACE()
B_SPLINE_SURFACE(1,2,((#97018,#97019,#97020),(#97021,#97022,#97023)),
 .UNSPECIFIED.,.F.,.F.,.F.)
B_SPLINE_SURFACE_WITH_KNOTS((2,2),(3,3),(0.,1.),(0.0456081671210051,0.0575989447818617),
 .UNSPECIFIED.)
GEOMETRIC_REPRESENTATION_ITEM()
RATIONAL_B_SPLINE_SURFACE(((0.997793907739636,0.996365558499691,0.996354522974128),
(0.997793907739636,0.996365558499691,0.996354522974128)))
REPRESENTATION_ITEM('')
SURFACE()
);
#699=(
BOUNDED_SURFACE()
B_SPLINE_SURFACE(1,2,((#97058,#97059,#97060),(#97061,#97062,#97063)),
 .UNSPECIFIED.,.F.,.F.,.F.)
B_SPLINE_SURFACE_WITH_KNOTS((2,2),(3,3),(0.,1.),(0.0556006976522445,0.0675888855446183),
 .UNSPECIFIED.)
GEOMETRIC_REPRESENTATION_ITEM()
RATIONAL_B_SPLINE_SURFACE(((0.996397562408177,0.996150386836003,0.997319912821418),
(0.996397562408177,0.996150386836003,0.997319912821418)))
REPRESENTATION_ITEM('')
SURFACE()
);
#700=(
BOUNDED_SURFACE()
B_SPLINE_SURFACE(1,2,((#97064,#97065,#97066),(#97067,#97068,#97069)),
 .UNSPECIFIED.,.F.,.F.,.F.)
B_SPLINE_SURFACE_WITH_KNOTS((2,2),(3,3),(0.,1.),(0.0657448619281112,0.0758849574338233),
 .UNSPECIFIED.)
GEOMETRIC_REPRESENTATION_ITEM()
RATIONAL_B_SPLINE_SURFACE(((0.996993639757276,0.997798549146193,0.999617032345115),
(0.996993639757276,0.997798549146193,0.999617032345115)))
REPRESENTATION_ITEM('')
SURFACE()
);
#701=(
BOUNDED_SURFACE()
B_SPLINE_SURFACE(1,2,((#97144,#97145,#97146),(#97147,#97148,#97149)),
 .UNSPECIFIED.,.F.,.F.,.F.)
B_SPLINE_SURFACE_WITH_KNOTS((2,2),(3,3),(0.,1.),(0.00560769170938328,0.0176009697615924),
 .UNSPECIFIED.)
GEOMETRIC_REPRESENTATION_ITEM()
RATIONAL_B_SPLINE_SURFACE(((0.998183892106924,0.996573304252679,0.996380621268545),
(0.998183892106924,0.996573304252679,0.996380621268545)))
REPRESENTATION_ITEM('')
SURFACE()
);
#702=(
BOUNDED_SURFACE()
B_SPLINE_SURFACE(1,2,((#97234,#97235,#97236),(#97237,#97238,#97239)),
 .UNSPECIFIED.,.F.,.F.,.F.)
B_SPLINE_SURFACE_WITH_KNOTS((2,2),(3,3),(0.,1.),(0.0255903596132,0.0375948596691669),
 .UNSPECIFIED.)
GEOMETRIC_REPRESENTATION_ITEM()
RATIONAL_B_SPLINE_SURFACE(((0.996753121756002,0.997505687613138,0.999678813023773),
(0.996753121756002,0.997505687613138,0.999678813023773)))
REPRESENTATION_ITEM('')
SURFACE()
);
#703=(
BOUNDED_SURFACE()
B_SPLINE_SURFACE(1,2,((#97257,#97258,#97259,#97260,#97261),(#97262,#97263,
#97264,#97265,#97266)),.UNSPECIFIED.,.F.,.F.,.F.)
B_SPLINE_SURFACE_WITH_KNOTS((2,2),(3,2,3),(0.519229702920879,1.),(0.0365944846646469,
0.0384615384615384,0.0431859278884089),.UNSPECIFIED.)
GEOMETRIC_REPRESENTATION_ITEM()
RATIONAL_B_SPLINE_SURFACE(((0.999326490452283,0.99964606396823,1.,0.99910440092885,
0.998428822114389),(0.999326490452283,0.99964606396823,1.,0.99910440092885,
0.998428822114389)))
REPRESENTATION_ITEM('')
SURFACE()
);
#704=(
BOUNDED_SURFACE()
B_SPLINE_SURFACE(1,2,((#97322,#97323,#97324),(#97325,#97326,#97327)),
 .UNSPECIFIED.,.F.,.F.,.F.)
B_SPLINE_SURFACE_WITH_KNOTS((2,2),(3,3),(0.,1.),(0.0456081671210064,0.0575989447818616),
 .UNSPECIFIED.)
GEOMETRIC_REPRESENTATION_ITEM()
RATIONAL_B_SPLINE_SURFACE(((0.997793907739636,0.996365558499691,0.996354522974128),
(0.997793907739636,0.996365558499691,0.996354522974128)))
REPRESENTATION_ITEM('')
SURFACE()
);
#705=(
BOUNDED_SURFACE()
B_SPLINE_SURFACE(1,2,((#97362,#97363,#97364),(#97365,#97366,#97367)),
 .UNSPECIFIED.,.F.,.F.,.F.)
B_SPLINE_SURFACE_WITH_KNOTS((2,2),(3,3),(0.,1.),(0.0556006976522447,0.0675888855446172),
 .UNSPECIFIED.)
GEOMETRIC_REPRESENTATION_ITEM()
RATIONAL_B_SPLINE_SURFACE(((0.996397562408177,0.996150386836003,0.997319912821417),
(0.996397562408177,0.996150386836003,0.997319912821417)))
REPRESENTATION_ITEM('')
SURFACE()
);
#706=(
BOUNDED_SURFACE()
B_SPLINE_SURFACE(1,2,((#97368,#97369,#97370),(#97371,#97372,#97373)),
 .UNSPECIFIED.,.F.,.F.,.F.)
B_SPLINE_SURFACE_WITH_KNOTS((2,2),(3,3),(0.,1.),(0.0657448619281101,0.0758849574338232),
 .UNSPECIFIED.)
GEOMETRIC_REPRESENTATION_ITEM()
RATIONAL_B_SPLINE_SURFACE(((0.996993639757276,0.997798549146193,0.999617032345115),
(0.996993639757276,0.997798549146193,0.999617032345115)))
REPRESENTATION_ITEM('')
SURFACE()
);
#707=(
BOUNDED_SURFACE()
B_SPLINE_SURFACE(1,2,((#97448,#97449,#97450),(#97451,#97452,#97453)),
 .UNSPECIFIED.,.F.,.F.,.F.)
B_SPLINE_SURFACE_WITH_KNOTS((2,2),(3,3),(0.,1.),(0.00560769170938317,0.0176009697615924),
 .UNSPECIFIED.)
GEOMETRIC_REPRESENTATION_ITEM()
RATIONAL_B_SPLINE_SURFACE(((0.998183892106924,0.996573304252679,0.996380621268545),
(0.998183892106924,0.996573304252679,0.996380621268545)))
REPRESENTATION_ITEM('')
SURFACE()
);
#708=(
BOUNDED_SURFACE()
B_SPLINE_SURFACE(1,2,((#97538,#97539,#97540),(#97541,#97542,#97543)),
 .UNSPECIFIED.,.F.,.F.,.F.)
B_SPLINE_SURFACE_WITH_KNOTS((2,2),(3,3),(0.,1.),(0.0255903596132,0.0375948596691668),
 .UNSPECIFIED.)
GEOMETRIC_REPRESENTATION_ITEM()
RATIONAL_B_SPLINE_SURFACE(((0.996753121756002,0.997505687613138,0.999678813023773),
(0.996753121756002,0.997505687613138,0.999678813023773)))
REPRESENTATION_ITEM('')
SURFACE()
);
#709=(
BOUNDED_SURFACE()
B_SPLINE_SURFACE(1,2,((#97561,#97562,#97563,#97564,#97565),(#97566,#97567,
#97568,#97569,#97570)),.UNSPECIFIED.,.F.,.F.,.F.)
B_SPLINE_SURFACE_WITH_KNOTS((2,2),(3,2,3),(0.519229702923312,1.),(0.0365944846646546,
0.0384615384615384,0.0431859278884165),.UNSPECIFIED.)
GEOMETRIC_REPRESENTATION_ITEM()
RATIONAL_B_SPLINE_SURFACE(((0.999326490452285,0.999646063968232,1.,0.999104400928849,
0.998428822114386),(0.999326490452285,0.999646063968232,1.,0.999104400928849,
0.998428822114386)))
REPRESENTATION_ITEM('')
SURFACE()
);
#710=(
BOUNDED_SURFACE()
B_SPLINE_SURFACE(1,2,((#97626,#97627,#97628),(#97629,#97630,#97631)),
 .UNSPECIFIED.,.F.,.F.,.F.)
B_SPLINE_SURFACE_WITH_KNOTS((2,2),(3,3),(0.,1.),(0.0456081671210064,0.057598944781862),
 .UNSPECIFIED.)
GEOMETRIC_REPRESENTATION_ITEM()
RATIONAL_B_SPLINE_SURFACE(((0.997793907739636,0.996365558499691,0.996354522974128),
(0.997793907739636,0.996365558499691,0.996354522974128)))
REPRESENTATION_ITEM('')
SURFACE()
);
#711=(
BOUNDED_SURFACE()
B_SPLINE_SURFACE(1,2,((#97666,#97667,#97668),(#97669,#97670,#97671)),
 .UNSPECIFIED.,.F.,.F.,.F.)
B_SPLINE_SURFACE_WITH_KNOTS((2,2),(3,3),(0.,1.),(0.0556006976522457,0.0675888855446172),
 .UNSPECIFIED.)
GEOMETRIC_REPRESENTATION_ITEM()
RATIONAL_B_SPLINE_SURFACE(((0.996397562408177,0.996150386836003,0.997319912821417),
(0.996397562408177,0.996150386836003,0.997319912821417)))
REPRESENTATION_ITEM('')
SURFACE()
);
#712=(
BOUNDED_SURFACE()
B_SPLINE_SURFACE(1,2,((#97672,#97673,#97674),(#97675,#97676,#97677)),
 .UNSPECIFIED.,.F.,.F.,.F.)
B_SPLINE_SURFACE_WITH_KNOTS((2,2),(3,3),(0.,1.),(0.0657448619281102,0.0758849574338228),
 .UNSPECIFIED.)
GEOMETRIC_REPRESENTATION_ITEM()
RATIONAL_B_SPLINE_SURFACE(((0.996993639757276,0.997798549146193,0.999617032345115),
(0.996993639757276,0.997798549146193,0.999617032345115)))
REPRESENTATION_ITEM('')
SURFACE()
);
#713=(
BOUNDED_SURFACE()
B_SPLINE_SURFACE(1,2,((#97752,#97753,#97754),(#97755,#97756,#97757)),
 .UNSPECIFIED.,.F.,.F.,.F.)
B_SPLINE_SURFACE_WITH_KNOTS((2,2),(3,3),(0.,1.),(0.00560769170938325,0.0176009697615924),
 .UNSPECIFIED.)
GEOMETRIC_REPRESENTATION_ITEM()
RATIONAL_B_SPLINE_SURFACE(((0.998183892106924,0.996573304252679,0.996380621268545),
(0.998183892106924,0.996573304252679,0.996380621268545)))
REPRESENTATION_ITEM('')
SURFACE()
);
#714=(
BOUNDED_SURFACE()
B_SPLINE_SURFACE(1,2,((#97842,#97843,#97844),(#97845,#97846,#97847)),
 .UNSPECIFIED.,.F.,.F.,.F.)
B_SPLINE_SURFACE_WITH_KNOTS((2,2),(3,3),(0.,1.),(0.0255903596131989,0.0375948596691661),
 .UNSPECIFIED.)
GEOMETRIC_REPRESENTATION_ITEM()
RATIONAL_B_SPLINE_SURFACE(((0.996753121756001,0.997505687613137,0.999678813023773),
(0.996753121756001,0.997505687613137,0.999678813023773)))
REPRESENTATION_ITEM('')
SURFACE()
);
#715=(
BOUNDED_SURFACE()
B_SPLINE_SURFACE(1,2,((#97865,#97866,#97867,#97868,#97869),(#97870,#97871,
#97872,#97873,#97874)),.UNSPECIFIED.,.F.,.F.,.F.)
B_SPLINE_SURFACE_WITH_KNOTS((2,2),(3,2,3),(0.519229702925686,1.),(0.0365944846646577,
0.0384615384615384,0.0431859278884218),.UNSPECIFIED.)
GEOMETRIC_REPRESENTATION_ITEM()
RATIONAL_B_SPLINE_SURFACE(((0.999326490452286,0.999646063968232,1.,0.999104400928848,
0.998428822114385),(0.999326490452286,0.999646063968232,1.,0.999104400928848,
0.998428822114385)))
REPRESENTATION_ITEM('')
SURFACE()
);
#716=(
BOUNDED_SURFACE()
B_SPLINE_SURFACE(1,2,((#97930,#97931,#97932),(#97933,#97934,#97935)),
 .UNSPECIFIED.,.F.,.F.,.F.)
B_SPLINE_SURFACE_WITH_KNOTS((2,2),(3,3),(0.,1.),(0.0456081671210071,0.057598944781862),
 .UNSPECIFIED.)
GEOMETRIC_REPRESENTATION_ITEM()
RATIONAL_B_SPLINE_SURFACE(((0.997793907739636,0.996365558499691,0.996354522974128),
(0.997793907739636,0.996365558499691,0.996354522974128)))
REPRESENTATION_ITEM('')
SURFACE()
);
#717=(
BOUNDED_SURFACE()
B_SPLINE_SURFACE(1,2,((#97970,#97971,#97972),(#97973,#97974,#97975)),
 .UNSPECIFIED.,.F.,.F.,.F.)
B_SPLINE_SURFACE_WITH_KNOTS((2,2),(3,3),(0.,1.),(0.0556006976522457,0.0675888855446172),
 .UNSPECIFIED.)
GEOMETRIC_REPRESENTATION_ITEM()
RATIONAL_B_SPLINE_SURFACE(((0.996397562408177,0.996150386836003,0.997319912821417),
(0.996397562408177,0.996150386836003,0.997319912821417)))
REPRESENTATION_ITEM('')
SURFACE()
);
#718=(
BOUNDED_SURFACE()
B_SPLINE_SURFACE(1,2,((#97976,#97977,#97978),(#97979,#97980,#97981)),
 .UNSPECIFIED.,.F.,.F.,.F.)
B_SPLINE_SURFACE_WITH_KNOTS((2,2),(3,3),(0.,1.),(0.0657448619281102,0.0758849574338228),
 .UNSPECIFIED.)
GEOMETRIC_REPRESENTATION_ITEM()
RATIONAL_B_SPLINE_SURFACE(((0.996993639757276,0.997798549146193,0.999617032345115),
(0.996993639757276,0.997798549146193,0.999617032345115)))
REPRESENTATION_ITEM('')
SURFACE()
);
#719=(
BOUNDED_SURFACE()
B_SPLINE_SURFACE(1,2,((#98056,#98057,#98058),(#98059,#98060,#98061)),
 .UNSPECIFIED.,.F.,.F.,.F.)
B_SPLINE_SURFACE_WITH_KNOTS((2,2),(3,3),(0.,1.),(0.0056076917093843,0.0176009697615923),
 .UNSPECIFIED.)
GEOMETRIC_REPRESENTATION_ITEM()
RATIONAL_B_SPLINE_SURFACE(((0.998183892106924,0.996573304252679,0.996380621268545),
(0.998183892106924,0.996573304252679,0.996380621268545)))
REPRESENTATION_ITEM('')
SURFACE()
);
#720=(
BOUNDED_SURFACE()
B_SPLINE_SURFACE(1,2,((#98146,#98147,#98148),(#98149,#98150,#98151)),
 .UNSPECIFIED.,.F.,.F.,.F.)
B_SPLINE_SURFACE_WITH_KNOTS((2,2),(3,3),(0.,1.),(0.0255903596131988,0.037594859669166),
 .UNSPECIFIED.)
GEOMETRIC_REPRESENTATION_ITEM()
RATIONAL_B_SPLINE_SURFACE(((0.996753121756001,0.997505687613137,0.999678813023773),
(0.996753121756001,0.997505687613137,0.999678813023773)))
REPRESENTATION_ITEM('')
SURFACE()
);
#721=(
BOUNDED_SURFACE()
B_SPLINE_SURFACE(1,2,((#98169,#98170,#98171,#98172,#98173),(#98174,#98175,
#98176,#98177,#98178)),.UNSPECIFIED.,.F.,.F.,.F.)
B_SPLINE_SURFACE_WITH_KNOTS((2,2),(3,2,3),(0.519229702928186,1.),(0.0365944846646617,
0.0384615384615384,0.0431859276815302),.UNSPECIFIED.)
GEOMETRIC_REPRESENTATION_ITEM()
RATIONAL_B_SPLINE_SURFACE(((0.999326490452288,0.999646063968233,1.,0.999104400968069,
0.998428822173555),(0.999326490452288,0.999646063968233,1.,0.999104400968069,
0.998428822173555)))
REPRESENTATION_ITEM('')
SURFACE()
);
#722=(
BOUNDED_SURFACE()
B_SPLINE_SURFACE(1,2,((#98234,#98235,#98236),(#98237,#98238,#98239)),
 .UNSPECIFIED.,.F.,.F.,.F.)
B_SPLINE_SURFACE_WITH_KNOTS((2,2),(3,3),(0.,1.),(0.0456081671210064,0.0575989447818616),
 .UNSPECIFIED.)
GEOMETRIC_REPRESENTATION_ITEM()
RATIONAL_B_SPLINE_SURFACE(((0.997793907739636,0.996365558499691,0.996354522974128),
(0.997793907739636,0.996365558499691,0.996354522974128)))
REPRESENTATION_ITEM('')
SURFACE()
);
#723=(
BOUNDED_SURFACE()
B_SPLINE_SURFACE(1,2,((#98274,#98275,#98276),(#98277,#98278,#98279)),
 .UNSPECIFIED.,.F.,.F.,.F.)
B_SPLINE_SURFACE_WITH_KNOTS((2,2),(3,3),(0.,1.),(0.0556006976522447,0.0675888855446151),
 .UNSPECIFIED.)
GEOMETRIC_REPRESENTATION_ITEM()
RATIONAL_B_SPLINE_SURFACE(((0.996397562408177,0.996150386836003,0.997319912821417),
(0.996397562408177,0.996150386836003,0.997319912821417)))
REPRESENTATION_ITEM('')
SURFACE()
);
#724=(
BOUNDED_SURFACE()
B_SPLINE_SURFACE(1,2,((#98280,#98281,#98282),(#98283,#98284,#98285)),
 .UNSPECIFIED.,.F.,.F.,.F.)
B_SPLINE_SURFACE_WITH_KNOTS((2,2),(3,3),(0.,1.),(0.065744861928108,0.075884957433823),
 .UNSPECIFIED.)
GEOMETRIC_REPRESENTATION_ITEM()
RATIONAL_B_SPLINE_SURFACE(((0.996993639757276,0.997798549146192,0.999617032345115),
(0.996993639757276,0.997798549146192,0.999617032345115)))
REPRESENTATION_ITEM('')
SURFACE()
);
#725=(
BOUNDED_SURFACE()
B_SPLINE_SURFACE(1,2,((#98360,#98361,#98362),(#98363,#98364,#98365)),
 .UNSPECIFIED.,.F.,.F.,.F.)
B_SPLINE_SURFACE_WITH_KNOTS((2,2),(3,3),(0.,1.),(0.00560769170938324,0.017600969761593),
 .UNSPECIFIED.)
GEOMETRIC_REPRESENTATION_ITEM()
RATIONAL_B_SPLINE_SURFACE(((0.998183892106924,0.996573304252679,0.996380621268545),
(0.998183892106924,0.996573304252679,0.996380621268545)))
REPRESENTATION_ITEM('')
SURFACE()
);
#726=(
BOUNDED_SURFACE()
B_SPLINE_SURFACE(1,2,((#98450,#98451,#98452),(#98453,#98454,#98455)),
 .UNSPECIFIED.,.F.,.F.,.F.)
B_SPLINE_SURFACE_WITH_KNOTS((2,2),(3,3),(0.,1.),(0.0255903596132001,0.0375948596691658),
 .UNSPECIFIED.)
GEOMETRIC_REPRESENTATION_ITEM()
RATIONAL_B_SPLINE_SURFACE(((0.996753121756002,0.997505687613138,0.999678813023773),
(0.996753121756002,0.997505687613138,0.999678813023773)))
REPRESENTATION_ITEM('')
SURFACE()
);
#727=(
BOUNDED_SURFACE()
B_SPLINE_SURFACE(1,2,((#98473,#98474,#98475,#98476,#98477),(#98478,#98479,
#98480,#98481,#98482)),.UNSPECIFIED.,.F.,.F.,.F.)
B_SPLINE_SURFACE_WITH_KNOTS((2,2),(3,2,3),(0.519229702930507,1.),(0.0365944846646633,
0.0384615384615384,0.0431859278884275),.UNSPECIFIED.)
GEOMETRIC_REPRESENTATION_ITEM()
RATIONAL_B_SPLINE_SURFACE(((0.999326490452288,0.999646063968233,1.,0.999104400928847,
0.998428822114384),(0.999326490452288,0.999646063968233,1.,0.999104400928847,
0.998428822114384)))
REPRESENTATION_ITEM('')
SURFACE()
);
#728=(
BOUNDED_SURFACE()
B_SPLINE_SURFACE(1,2,((#98538,#98539,#98540),(#98541,#98542,#98543)),
 .UNSPECIFIED.,.F.,.F.,.F.)
B_SPLINE_SURFACE_WITH_KNOTS((2,2),(3,3),(0.,1.),(0.0456081671210063,0.0575989447818616),
 .UNSPECIFIED.)
GEOMETRIC_REPRESENTATION_ITEM()
RATIONAL_B_SPLINE_SURFACE(((0.997793907739636,0.996365558499691,0.996354522974128),
(0.997793907739636,0.996365558499691,0.996354522974128)))
REPRESENTATION_ITEM('')
SURFACE()
);
#729=(
BOUNDED_SURFACE()
B_SPLINE_SURFACE(1,2,((#98578,#98579,#98580),(#98581,#98582,#98583)),
 .UNSPECIFIED.,.F.,.F.,.F.)
B_SPLINE_SURFACE_WITH_KNOTS((2,2),(3,3),(0.,1.),(0.0556006976522446,0.0675888855446162),
 .UNSPECIFIED.)
GEOMETRIC_REPRESENTATION_ITEM()
RATIONAL_B_SPLINE_SURFACE(((0.996397562408177,0.996150386836003,0.997319912821417),
(0.996397562408177,0.996150386836003,0.997319912821417)))
REPRESENTATION_ITEM('')
SURFACE()
);
#730=(
BOUNDED_SURFACE()
B_SPLINE_SURFACE(1,2,((#98584,#98585,#98586),(#98587,#98588,#98589)),
 .UNSPECIFIED.,.F.,.F.,.F.)
B_SPLINE_SURFACE_WITH_KNOTS((2,2),(3,3),(0.,1.),(0.0657448619281091,0.0758849574338227),
 .UNSPECIFIED.)
GEOMETRIC_REPRESENTATION_ITEM()
RATIONAL_B_SPLINE_SURFACE(((0.996993639757276,0.997798549146192,0.999617032345115),
(0.996993639757276,0.997798549146192,0.999617032345115)))
REPRESENTATION_ITEM('')
SURFACE()
);
#731=(
BOUNDED_SURFACE()
B_SPLINE_SURFACE(1,2,((#98664,#98665,#98666),(#98667,#98668,#98669)),
 .UNSPECIFIED.,.F.,.F.,.F.)
B_SPLINE_SURFACE_WITH_KNOTS((2,2),(3,3),(0.,1.),(0.00560769170938338,0.0176009697615912),
 .UNSPECIFIED.)
GEOMETRIC_REPRESENTATION_ITEM()
RATIONAL_B_SPLINE_SURFACE(((0.998183892106924,0.996573304252679,0.996380621268545),
(0.998183892106924,0.996573304252679,0.996380621268545)))
REPRESENTATION_ITEM('')
SURFACE()
);
#732=(
BOUNDED_SURFACE()
B_SPLINE_SURFACE(1,2,((#98754,#98755,#98756),(#98757,#98758,#98759)),
 .UNSPECIFIED.,.F.,.F.,.F.)
B_SPLINE_SURFACE_WITH_KNOTS((2,2),(3,3),(0.,1.),(0.0255903596132001,0.037594859669166),
 .UNSPECIFIED.)
GEOMETRIC_REPRESENTATION_ITEM()
RATIONAL_B_SPLINE_SURFACE(((0.996753121756002,0.997505687613138,0.999678813023773),
(0.996753121756002,0.997505687613138,0.999678813023773)))
REPRESENTATION_ITEM('')
SURFACE()
);
#733=(
BOUNDED_SURFACE()
B_SPLINE_SURFACE(1,2,((#98777,#98778,#98779,#98780,#98781),(#98782,#98783,
#98784,#98785,#98786)),.UNSPECIFIED.,.F.,.F.,.F.)
B_SPLINE_SURFACE_WITH_KNOTS((2,2),(3,2,3),(0.519229702931999,1.),(0.0365944846646612,
0.0384615384615384,0.0431859278101874),.UNSPECIFIED.)
GEOMETRIC_REPRESENTATION_ITEM()
RATIONAL_B_SPLINE_SURFACE(((0.999326490452287,0.999646063968233,1.,0.999104400943679,
0.998428822136759),(0.999326490452287,0.999646063968233,1.,0.999104400943679,
0.998428822136759)))
REPRESENTATION_ITEM('')
SURFACE()
);
#734=(
BOUNDED_SURFACE()
B_SPLINE_SURFACE(1,2,((#98842,#98843,#98844),(#98845,#98846,#98847)),
 .UNSPECIFIED.,.F.,.F.,.F.)
B_SPLINE_SURFACE_WITH_KNOTS((2,2),(3,3),(0.,1.),(0.0456081671210053,0.0575989447818606),
 .UNSPECIFIED.)
GEOMETRIC_REPRESENTATION_ITEM()
RATIONAL_B_SPLINE_SURFACE(((0.997793907739636,0.996365558499691,0.996354522974128),
(0.997793907739636,0.996365558499691,0.996354522974128)))
REPRESENTATION_ITEM('')
SURFACE()
);
#735=(
BOUNDED_SURFACE()
B_SPLINE_SURFACE(1,2,((#98882,#98883,#98884),(#98885,#98886,#98887)),
 .UNSPECIFIED.,.F.,.F.,.F.)
B_SPLINE_SURFACE_WITH_KNOTS((2,2),(3,3),(0.,1.),(0.0556006976522437,0.0675888855446153),
 .UNSPECIFIED.)
GEOMETRIC_REPRESENTATION_ITEM()
RATIONAL_B_SPLINE_SURFACE(((0.996397562408177,0.996150386836003,0.997319912821417),
(0.996397562408177,0.996150386836003,0.997319912821417)))
REPRESENTATION_ITEM('')
SURFACE()
);
#736=(
BOUNDED_SURFACE()
B_SPLINE_SURFACE(1,2,((#98888,#98889,#98890),(#98891,#98892,#98893)),
 .UNSPECIFIED.,.F.,.F.,.F.)
B_SPLINE_SURFACE_WITH_KNOTS((2,2),(3,3),(0.,1.),(0.0657448619281082,0.0758849574338225),
 .UNSPECIFIED.)
GEOMETRIC_REPRESENTATION_ITEM()
RATIONAL_B_SPLINE_SURFACE(((0.996993639757276,0.997798549146192,0.999617032345115),
(0.996993639757276,0.997798549146192,0.999617032345115)))
REPRESENTATION_ITEM('')
SURFACE()
);
#737=(
BOUNDED_SURFACE()
B_SPLINE_SURFACE(1,2,((#98968,#98969,#98970),(#98971,#98972,#98973)),
 .UNSPECIFIED.,.F.,.F.,.F.)
B_SPLINE_SURFACE_WITH_KNOTS((2,2),(3,3),(0.,1.),(0.00560769170938422,0.0176009697615929),
 .UNSPECIFIED.)
GEOMETRIC_REPRESENTATION_ITEM()
RATIONAL_B_SPLINE_SURFACE(((0.998183892106924,0.996573304252679,0.996380621268545),
(0.998183892106924,0.996573304252679,0.996380621268545)))
REPRESENTATION_ITEM('')
SURFACE()
);
#738=(
BOUNDED_SURFACE()
B_SPLINE_SURFACE(1,2,((#99058,#99059,#99060),(#99061,#99062,#99063)),
 .UNSPECIFIED.,.F.,.F.,.F.)
B_SPLINE_SURFACE_WITH_KNOTS((2,2),(3,3),(0.,1.),(0.0255903596131999,0.037594859669168),
 .UNSPECIFIED.)
GEOMETRIC_REPRESENTATION_ITEM()
RATIONAL_B_SPLINE_SURFACE(((0.996753121756002,0.997505687613138,0.999678813023774),
(0.996753121756002,0.997505687613138,0.999678813023774)))
REPRESENTATION_ITEM('')
SURFACE()
);
#739=(
BOUNDED_SURFACE()
B_SPLINE_SURFACE(1,2,((#99081,#99082,#99083,#99084,#99085),(#99086,#99087,
#99088,#99089,#99090)),.UNSPECIFIED.,.F.,.F.,.F.)
B_SPLINE_SURFACE_WITH_KNOTS((2,2),(3,2,3),(0.519229702931916,1.),(0.0365944846646506,
0.0384615384615384,0.0431859276815304),.UNSPECIFIED.)
GEOMETRIC_REPRESENTATION_ITEM()
RATIONAL_B_SPLINE_SURFACE(((0.999326490452284,0.999646063968231,1.,0.999104400968068,
0.998428822173555),(0.999326490452284,0.999646063968231,1.,0.999104400968068,
0.998428822173555)))
REPRESENTATION_ITEM('')
SURFACE()
);
#740=(
BOUNDED_SURFACE()
B_SPLINE_SURFACE(1,2,((#99146,#99147,#99148),(#99149,#99150,#99151)),
 .UNSPECIFIED.,.F.,.F.,.F.)
B_SPLINE_SURFACE_WITH_KNOTS((2,2),(3,3),(0.,1.),(0.0456081671210071,0.057598944781862),
 .UNSPECIFIED.)
GEOMETRIC_REPRESENTATION_ITEM()
RATIONAL_B_SPLINE_SURFACE(((0.997793907739636,0.996365558499691,0.996354522974128),
(0.997793907739636,0.996365558499691,0.996354522974128)))
REPRESENTATION_ITEM('')
SURFACE()
);
#741=(
BOUNDED_SURFACE()
B_SPLINE_SURFACE(1,2,((#99186,#99187,#99188),(#99189,#99190,#99191)),
 .UNSPECIFIED.,.F.,.F.,.F.)
B_SPLINE_SURFACE_WITH_KNOTS((2,2),(3,3),(0.,1.),(0.0556006976522447,0.0675888855446163),
 .UNSPECIFIED.)
GEOMETRIC_REPRESENTATION_ITEM()
RATIONAL_B_SPLINE_SURFACE(((0.996397562408177,0.996150386836003,0.997319912821417),
(0.996397562408177,0.996150386836003,0.997319912821417)))
REPRESENTATION_ITEM('')
SURFACE()
);
#742=(
BOUNDED_SURFACE()
B_SPLINE_SURFACE(1,2,((#99192,#99193,#99194),(#99195,#99196,#99197)),
 .UNSPECIFIED.,.F.,.F.,.F.)
B_SPLINE_SURFACE_WITH_KNOTS((2,2),(3,3),(0.,1.),(0.0657450014656867,0.0758834225204695),
 .UNSPECIFIED.)
GEOMETRIC_REPRESENTATION_ITEM()
RATIONAL_B_SPLINE_SURFACE(((0.99699366191014,0.997798452328481,0.99961648183819),
(0.99699366191014,0.997798452328481,0.99961648183819)))
REPRESENTATION_ITEM('')
SURFACE()
);
#743=(
BOUNDED_SURFACE()
B_SPLINE_SURFACE(1,2,((#99272,#99273,#99274),(#99275,#99276,#99277)),
 .UNSPECIFIED.,.F.,.F.,.F.)
B_SPLINE_SURFACE_WITH_KNOTS((2,2),(3,3),(0.,1.),(0.0056076917093829,0.0176009697615918),
 .UNSPECIFIED.)
GEOMETRIC_REPRESENTATION_ITEM()
RATIONAL_B_SPLINE_SURFACE(((0.998183892106924,0.996573304252679,0.996380621268545),
(0.998183892106924,0.996573304252679,0.996380621268545)))
REPRESENTATION_ITEM('')
SURFACE()
);
#744=(
BOUNDED_SURFACE()
B_SPLINE_SURFACE(1,2,((#99362,#99363,#99364),(#99365,#99366,#99367)),
 .UNSPECIFIED.,.F.,.F.,.F.)
B_SPLINE_SURFACE_WITH_KNOTS((2,2),(3,3),(0.,1.),(0.0255903596131988,0.037594859669165),
 .UNSPECIFIED.)
GEOMETRIC_REPRESENTATION_ITEM()
RATIONAL_B_SPLINE_SURFACE(((0.996753121756001,0.997505687613137,0.999678813023773),
(0.996753121756001,0.997505687613137,0.999678813023773)))
REPRESENTATION_ITEM('')
SURFACE()
);
#745=(
BOUNDED_SURFACE()
B_SPLINE_SURFACE(1,2,((#99385,#99386,#99387,#99388,#99389),(#99390,#99391,
#99392,#99393,#99394)),.UNSPECIFIED.,.F.,.F.,.F.)
B_SPLINE_SURFACE_WITH_KNOTS((2,2),(3,2,3),(0.519229702931731,1.),(0.0365944846646451,
0.0384615384615384,0.0431859276815275),.UNSPECIFIED.)
GEOMETRIC_REPRESENTATION_ITEM()
RATIONAL_B_SPLINE_SURFACE(((0.999326490452282,0.99964606396823,1.,0.999104400968069,
0.998428822173556),(0.999326490452282,0.99964606396823,1.,0.999104400968069,
0.998428822173556)))
REPRESENTATION_ITEM('')
SURFACE()
);
#746=(
BOUNDED_SURFACE()
B_SPLINE_SURFACE(1,2,((#99450,#99451,#99452),(#99453,#99454,#99455)),
 .UNSPECIFIED.,.F.,.F.,.F.)
B_SPLINE_SURFACE_WITH_KNOTS((2,2),(3,3),(0.,1.),(0.0456081671210062,0.0575989447818616),
 .UNSPECIFIED.)
GEOMETRIC_REPRESENTATION_ITEM()
RATIONAL_B_SPLINE_SURFACE(((0.997793907739636,0.996365558499691,0.996354522974128),
(0.997793907739636,0.996365558499691,0.996354522974128)))
REPRESENTATION_ITEM('')
SURFACE()
);
#747=(
BOUNDED_SURFACE()
B_SPLINE_SURFACE(1,2,((#99490,#99491,#99492),(#99493,#99494,#99495)),
 .UNSPECIFIED.,.F.,.F.,.F.)
B_SPLINE_SURFACE_WITH_KNOTS((2,2),(3,3),(0.,1.),(0.0556006976522447,0.0675888855446162),
 .UNSPECIFIED.)
GEOMETRIC_REPRESENTATION_ITEM()
RATIONAL_B_SPLINE_SURFACE(((0.996397562408177,0.996150386836003,0.997319912821417),
(0.996397562408177,0.996150386836003,0.997319912821417)))
REPRESENTATION_ITEM('')
SURFACE()
);
#748=(
BOUNDED_SURFACE()
B_SPLINE_SURFACE(1,2,((#99496,#99497,#99498),(#99499,#99500,#99501)),
 .UNSPECIFIED.,.F.,.F.,.F.)
B_SPLINE_SURFACE_WITH_KNOTS((2,2),(3,3),(0.,1.),(0.0657448619281091,0.0758849574338226),
 .UNSPECIFIED.)
GEOMETRIC_REPRESENTATION_ITEM()
RATIONAL_B_SPLINE_SURFACE(((0.996993639757276,0.997798549146192,0.999617032345115),
(0.996993639757276,0.997798549146192,0.999617032345115)))
REPRESENTATION_ITEM('')
SURFACE()
);
#749=(
BOUNDED_SURFACE()
B_SPLINE_SURFACE(1,2,((#99576,#99577,#99578),(#99579,#99580,#99581)),
 .UNSPECIFIED.,.F.,.F.,.F.)
B_SPLINE_SURFACE_WITH_KNOTS((2,2),(3,3),(0.,1.),(0.00560769170938373,0.0176009697615924),
 .UNSPECIFIED.)
GEOMETRIC_REPRESENTATION_ITEM()
RATIONAL_B_SPLINE_SURFACE(((0.998183892106924,0.996573304252679,0.996380621268545),
(0.998183892106924,0.996573304252679,0.996380621268545)))
REPRESENTATION_ITEM('')
SURFACE()
);
#750=(
BOUNDED_SURFACE()
B_SPLINE_SURFACE(1,2,((#99666,#99667,#99668),(#99669,#99670,#99671)),
 .UNSPECIFIED.,.F.,.F.,.F.)
B_SPLINE_SURFACE_WITH_KNOTS((2,2),(3,3),(0.,1.),(0.0255903596132,0.037594859669166),
 .UNSPECIFIED.)
GEOMETRIC_REPRESENTATION_ITEM()
RATIONAL_B_SPLINE_SURFACE(((0.996753121756002,0.997505687613138,0.999678813023773),
(0.996753121756002,0.997505687613138,0.999678813023773)))
REPRESENTATION_ITEM('')
SURFACE()
);
#751=(
BOUNDED_SURFACE()
B_SPLINE_SURFACE(1,2,((#99689,#99690,#99691,#99692,#99693),(#99694,#99695,
#99696,#99697,#99698)),.UNSPECIFIED.,.F.,.F.,.F.)
B_SPLINE_SURFACE_WITH_KNOTS((2,2),(3,2,3),(0.519229702931711,1.),(0.036594484664649,
0.0384615384615384,0.043185927681521),.UNSPECIFIED.)
GEOMETRIC_REPRESENTATION_ITEM()
RATIONAL_B_SPLINE_SURFACE(((0.999326490452283,0.999646063968231,1.,0.99910440096807,
0.998428822173557),(0.999326490452283,0.999646063968231,1.,0.99910440096807,
0.998428822173557)))
REPRESENTATION_ITEM('')
SURFACE()
);
#752=(
BOUNDED_SURFACE()
B_SPLINE_SURFACE(1,2,((#99754,#99755,#99756),(#99757,#99758,#99759)),
 .UNSPECIFIED.,.F.,.F.,.F.)
B_SPLINE_SURFACE_WITH_KNOTS((2,2),(3,3),(0.,1.),(0.0456081671210063,0.0575989447818621),
 .UNSPECIFIED.)
GEOMETRIC_REPRESENTATION_ITEM()
RATIONAL_B_SPLINE_SURFACE(((0.997793907739636,0.996365558499691,0.996354522974128),
(0.997793907739636,0.996365558499691,0.996354522974128)))
REPRESENTATION_ITEM('')
SURFACE()
);
#753=(
BOUNDED_SURFACE()
B_SPLINE_SURFACE(1,2,((#99794,#99795,#99796),(#99797,#99798,#99799)),
 .UNSPECIFIED.,.F.,.F.,.F.)
B_SPLINE_SURFACE_WITH_KNOTS((2,2),(3,3),(0.,1.),(0.0556006976522445,0.0675888855446172),
 .UNSPECIFIED.)
GEOMETRIC_REPRESENTATION_ITEM()
RATIONAL_B_SPLINE_SURFACE(((0.996397562408177,0.996150386836003,0.997319912821417),
(0.996397562408177,0.996150386836003,0.997319912821417)))
REPRESENTATION_ITEM('')
SURFACE()
);
#754=(
BOUNDED_SURFACE()
B_SPLINE_SURFACE(1,2,((#99800,#99801,#99802),(#99803,#99804,#99805)),
 .UNSPECIFIED.,.F.,.F.,.F.)
B_SPLINE_SURFACE_WITH_KNOTS((2,2),(3,3),(0.,1.),(0.0657448619281102,0.0758849574338218),
 .UNSPECIFIED.)
GEOMETRIC_REPRESENTATION_ITEM()
RATIONAL_B_SPLINE_SURFACE(((0.996993639757276,0.997798549146192,0.999617032345114),
(0.996993639757276,0.997798549146192,0.999617032345114)))
REPRESENTATION_ITEM('')
SURFACE()
);
#755=(
BOUNDED_SURFACE()
B_SPLINE_SURFACE(1,2,((#99880,#99881,#99882),(#99883,#99884,#99885)),
 .UNSPECIFIED.,.F.,.F.,.F.)
B_SPLINE_SURFACE_WITH_KNOTS((2,2),(3,3),(0.,1.),(0.0056076917093831,0.017600969761593),
 .UNSPECIFIED.)
GEOMETRIC_REPRESENTATION_ITEM()
RATIONAL_B_SPLINE_SURFACE(((0.998183892106924,0.996573304252679,0.996380621268545),
(0.998183892106924,0.996573304252679,0.996380621268545)))
REPRESENTATION_ITEM('')
SURFACE()
);
#756=(
BOUNDED_SURFACE()
B_SPLINE_SURFACE(1,2,((#99970,#99971,#99972),(#99973,#99974,#99975)),
 .UNSPECIFIED.,.F.,.F.,.F.)
B_SPLINE_SURFACE_WITH_KNOTS((2,2),(3,3),(0.,1.),(0.025590359613201,0.0375948596691668),
 .UNSPECIFIED.)
GEOMETRIC_REPRESENTATION_ITEM()
RATIONAL_B_SPLINE_SURFACE(((0.996753121756002,0.997505687613138,0.999678813023773),
(0.996753121756002,0.997505687613138,0.999678813023773)))
REPRESENTATION_ITEM('')
SURFACE()
);
#757=(
BOUNDED_SURFACE()
B_SPLINE_SURFACE(1,2,((#99993,#99994,#99995,#99996,#99997),(#99998,#99999,
#100000,#100001,#100002)),.UNSPECIFIED.,.F.,.F.,.F.)
B_SPLINE_SURFACE_WITH_KNOTS((2,2),(3,2,3),(0.519229702931684,1.),(0.0365944846646416,
0.0384615384615384,0.0431859278884089),.UNSPECIFIED.)
GEOMETRIC_REPRESENTATION_ITEM()
RATIONAL_B_SPLINE_SURFACE(((0.999326490452281,0.999646063968229,1.,0.99910440092885,
0.998428822114388),(0.999326490452281,0.999646063968229,1.,0.99910440092885,
0.998428822114388)))
REPRESENTATION_ITEM('')
SURFACE()
);
#758=(
BOUNDED_SURFACE()
B_SPLINE_SURFACE(1,2,((#100058,#100059,#100060),(#100061,#100062,#100063)),
 .UNSPECIFIED.,.F.,.F.,.F.)
B_SPLINE_SURFACE_WITH_KNOTS((2,2),(3,3),(0.,1.),(0.0456081671210073,0.0575989447818615),
 .UNSPECIFIED.)
GEOMETRIC_REPRESENTATION_ITEM()
RATIONAL_B_SPLINE_SURFACE(((0.997793907739636,0.996365558499691,0.996354522974128),
(0.997793907739636,0.996365558499691,0.996354522974128)))
REPRESENTATION_ITEM('')
SURFACE()
);
#759=(
BOUNDED_SURFACE()
B_SPLINE_SURFACE(1,2,((#100098,#100099,#100100),(#100101,#100102,#100103)),
 .UNSPECIFIED.,.F.,.F.,.F.)
B_SPLINE_SURFACE_WITH_KNOTS((2,2),(3,3),(0.,1.),(0.0556006976522446,0.0675888855446172),
 .UNSPECIFIED.)
GEOMETRIC_REPRESENTATION_ITEM()
RATIONAL_B_SPLINE_SURFACE(((0.996397562408177,0.996150386836003,0.997319912821418),
(0.996397562408177,0.996150386836003,0.997319912821418)))
REPRESENTATION_ITEM('')
SURFACE()
);
#760=(
BOUNDED_SURFACE()
B_SPLINE_SURFACE(1,2,((#100104,#100105,#100106),(#100107,#100108,#100109)),
 .UNSPECIFIED.,.F.,.F.,.F.)
B_SPLINE_SURFACE_WITH_KNOTS((2,2),(3,3),(0.,1.),(0.0657448619281101,0.0758849574338219),
 .UNSPECIFIED.)
GEOMETRIC_REPRESENTATION_ITEM()
RATIONAL_B_SPLINE_SURFACE(((0.996993639757276,0.997798549146193,0.999617032345114),
(0.996993639757276,0.997798549146193,0.999617032345114)))
REPRESENTATION_ITEM('')
SURFACE()
);
#761=(
BOUNDED_SURFACE()
B_SPLINE_SURFACE(1,2,((#100184,#100185,#100186),(#100187,#100188,#100189)),
 .UNSPECIFIED.,.F.,.F.,.F.)
B_SPLINE_SURFACE_WITH_KNOTS((2,2),(3,3),(0.,1.),(0.00560769170938418,0.0176009697615923),
 .UNSPECIFIED.)
GEOMETRIC_REPRESENTATION_ITEM()
RATIONAL_B_SPLINE_SURFACE(((0.998183892106923,0.996573304252679,0.996380621268545),
(0.998183892106923,0.996573304252679,0.996380621268545)))
REPRESENTATION_ITEM('')
SURFACE()
);
#762=(
BOUNDED_SURFACE()
B_SPLINE_SURFACE(1,2,((#100274,#100275,#100276),(#100277,#100278,#100279)),
 .UNSPECIFIED.,.F.,.F.,.F.)
B_SPLINE_SURFACE_WITH_KNOTS((2,2),(3,3),(0.,1.),(0.025590359613201,0.0375948596691677),
 .UNSPECIFIED.)
GEOMETRIC_REPRESENTATION_ITEM()
RATIONAL_B_SPLINE_SURFACE(((0.996753121756002,0.997505687613138,0.999678813023774),
(0.996753121756002,0.997505687613138,0.999678813023774)))
REPRESENTATION_ITEM('')
SURFACE()
);
#763=(
BOUNDED_SURFACE()
B_SPLINE_SURFACE(1,2,((#100297,#100298,#100299,#100300,#100301),(#100302,
#100303,#100304,#100305,#100306)),.UNSPECIFIED.,.F.,.F.,.F.)
B_SPLINE_SURFACE_WITH_KNOTS((2,2),(3,2,3),(0.519229702931402,1.),(0.0365944846646318,
0.0384615384615384,0.0431859278884006),.UNSPECIFIED.)
GEOMETRIC_REPRESENTATION_ITEM()
RATIONAL_B_SPLINE_SURFACE(((0.999326490452278,0.999646063968227,1.,0.999104400928852,
0.998428822114391),(0.999326490452278,0.999646063968227,1.,0.999104400928852,
0.998428822114391)))
REPRESENTATION_ITEM('')
SURFACE()
);
#764=(
BOUNDED_SURFACE()
B_SPLINE_SURFACE(1,2,((#100362,#100363,#100364),(#100365,#100366,#100367)),
 .UNSPECIFIED.,.F.,.F.,.F.)
B_SPLINE_SURFACE_WITH_KNOTS((2,2),(3,3),(0.,1.),(0.045608167121007,0.0575989447818626),
 .UNSPECIFIED.)
GEOMETRIC_REPRESENTATION_ITEM()
RATIONAL_B_SPLINE_SURFACE(((0.997793907739636,0.996365558499691,0.996354522974128),
(0.997793907739636,0.996365558499691,0.996354522974128)))
REPRESENTATION_ITEM('')
SURFACE()
);
#765=(
BOUNDED_SURFACE()
B_SPLINE_SURFACE(1,2,((#100402,#100403,#100404),(#100405,#100406,#100407)),
 .UNSPECIFIED.,.F.,.F.,.F.)
B_SPLINE_SURFACE_WITH_KNOTS((2,2),(3,3),(0.,1.),(0.0556006976522468,0.0675888855446172),
 .UNSPECIFIED.)
GEOMETRIC_REPRESENTATION_ITEM()
RATIONAL_B_SPLINE_SURFACE(((0.996397562408177,0.996150386836004,0.997319912821418),
(0.996397562408177,0.996150386836004,0.997319912821418)))
REPRESENTATION_ITEM('')
SURFACE()
);
#766=(
BOUNDED_SURFACE()
B_SPLINE_SURFACE(1,2,((#100408,#100409,#100410),(#100411,#100412,#100413)),
 .UNSPECIFIED.,.F.,.F.,.F.)
B_SPLINE_SURFACE_WITH_KNOTS((2,2),(3,3),(0.,1.),(0.0657448619281104,0.075884957433822),
 .UNSPECIFIED.)
GEOMETRIC_REPRESENTATION_ITEM()
RATIONAL_B_SPLINE_SURFACE(((0.996993639757276,0.997798549146193,0.999617032345114),
(0.996993639757276,0.997798549146193,0.999617032345114)))
REPRESENTATION_ITEM('')
SURFACE()
);
#767=(
BOUNDED_SURFACE()
B_SPLINE_SURFACE(1,2,((#100488,#100489,#100490),(#100491,#100492,#100493)),
 .UNSPECIFIED.,.F.,.F.,.F.)
B_SPLINE_SURFACE_WITH_KNOTS((2,2),(3,3),(0.,1.),(0.00560769170938319,0.0176009697615929),
 .UNSPECIFIED.)
GEOMETRIC_REPRESENTATION_ITEM()
RATIONAL_B_SPLINE_SURFACE(((0.998183892106924,0.996573304252679,0.996380621268545),
(0.998183892106924,0.996573304252679,0.996380621268545)))
REPRESENTATION_ITEM('')
SURFACE()
);
#768=(
BOUNDED_SURFACE()
B_SPLINE_SURFACE(1,2,((#100578,#100579,#100580),(#100581,#100582,#100583)),
 .UNSPECIFIED.,.F.,.F.,.F.)
B_SPLINE_SURFACE_WITH_KNOTS((2,2),(3,3),(0.,1.),(0.0255903596132008,0.037594859669168),
 .UNSPECIFIED.)
GEOMETRIC_REPRESENTATION_ITEM()
RATIONAL_B_SPLINE_SURFACE(((0.996753121756002,0.997505687613138,0.999678813023774),
(0.996753121756002,0.997505687613138,0.999678813023774)))
REPRESENTATION_ITEM('')
SURFACE()
);
#769=(
BOUNDED_SURFACE()
B_SPLINE_SURFACE(1,2,((#100601,#100602,#100603,#100604,#100605),(#100606,
#100607,#100608,#100609,#100610)),.UNSPECIFIED.,.F.,.F.,.F.)
B_SPLINE_SURFACE_WITH_KNOTS((2,2),(3,2,3),(0.519229702931324,1.),(0.0365944846646224,
0.0384615384615384,0.0431859276814949),.UNSPECIFIED.)
GEOMETRIC_REPRESENTATION_ITEM()
RATIONAL_B_SPLINE_SURFACE(((0.999326490452275,0.999646063968226,1.,0.999104400968075,
0.998428822173566),(0.999326490452275,0.999646063968226,1.,0.999104400968075,
0.998428822173566)))
REPRESENTATION_ITEM('')
SURFACE()
);
#770=(
BOUNDED_SURFACE()
B_SPLINE_SURFACE(1,2,((#100666,#100667,#100668),(#100669,#100670,#100671)),
 .UNSPECIFIED.,.F.,.F.,.F.)
B_SPLINE_SURFACE_WITH_KNOTS((2,2),(3,3),(0.,1.),(0.0456081671210084,0.0575989447818613),
 .UNSPECIFIED.)
GEOMETRIC_REPRESENTATION_ITEM()
RATIONAL_B_SPLINE_SURFACE(((0.997793907739635,0.996365558499691,0.996354522974128),
(0.997793907739635,0.996365558499691,0.996354522974128)))
REPRESENTATION_ITEM('')
SURFACE()
);
#771=(
BOUNDED_SURFACE()
B_SPLINE_SURFACE(1,2,((#100706,#100707,#100708),(#100709,#100710,#100711)),
 .UNSPECIFIED.,.F.,.F.,.F.)
B_SPLINE_SURFACE_WITH_KNOTS((2,2),(3,3),(0.,1.),(0.0556006976522446,0.0675888855446172),
 .UNSPECIFIED.)
GEOMETRIC_REPRESENTATION_ITEM()
RATIONAL_B_SPLINE_SURFACE(((0.996397562408177,0.996150386836003,0.997319912821417),
(0.996397562408177,0.996150386836003,0.997319912821417)))
REPRESENTATION_ITEM('')
SURFACE()
);
#772=(
BOUNDED_SURFACE()
B_SPLINE_SURFACE(1,2,((#100712,#100713,#100714),(#100715,#100716,#100717)),
 .UNSPECIFIED.,.F.,.F.,.F.)
B_SPLINE_SURFACE_WITH_KNOTS((2,2),(3,3),(0.,1.),(0.0657448619281102,0.0758849574338218),
 .UNSPECIFIED.)
GEOMETRIC_REPRESENTATION_ITEM()
RATIONAL_B_SPLINE_SURFACE(((0.996993639757276,0.997798549146193,0.999617032345114),
(0.996993639757276,0.997798549146193,0.999617032345114)))
REPRESENTATION_ITEM('')
SURFACE()
);
#773=(
BOUNDED_SURFACE()
B_SPLINE_SURFACE(1,2,((#100792,#100793,#100794),(#100795,#100796,#100797)),
 .UNSPECIFIED.,.F.,.F.,.F.)
B_SPLINE_SURFACE_WITH_KNOTS((2,2),(3,3),(0.,1.),(0.00560769170938338,0.0176009697615918),
 .UNSPECIFIED.)
GEOMETRIC_REPRESENTATION_ITEM()
RATIONAL_B_SPLINE_SURFACE(((0.998183892106924,0.996573304252679,0.996380621268545),
(0.998183892106924,0.996573304252679,0.996380621268545)))
REPRESENTATION_ITEM('')
SURFACE()
);
#774=(
BOUNDED_SURFACE()
B_SPLINE_SURFACE(1,2,((#100882,#100883,#100884),(#100885,#100886,#100887)),
 .UNSPECIFIED.,.F.,.F.,.F.)
B_SPLINE_SURFACE_WITH_KNOTS((2,2),(3,3),(0.,1.),(0.0255903596131989,0.0375948596691661),
 .UNSPECIFIED.)
GEOMETRIC_REPRESENTATION_ITEM()
RATIONAL_B_SPLINE_SURFACE(((0.996753121756001,0.997505687613137,0.999678813023773),
(0.996753121756001,0.997505687613137,0.999678813023773)))
REPRESENTATION_ITEM('')
SURFACE()
);
#775=(
BOUNDED_SURFACE()
B_SPLINE_SURFACE(1,2,((#100905,#100906,#100907,#100908,#100909),(#100910,
#100911,#100912,#100913,#100914)),.UNSPECIFIED.,.F.,.F.,.F.)
B_SPLINE_SURFACE_WITH_KNOTS((2,2),(3,2,3),(0.519229702931156,1.),(0.0365944846646104,
0.0384615384615384,0.0431859278883797),.UNSPECIFIED.)
GEOMETRIC_REPRESENTATION_ITEM()
RATIONAL_B_SPLINE_SURFACE(((0.99932649045227,0.999646063968223,1.,0.999104400928856,
0.998428822114396),(0.99932649045227,0.999646063968223,1.,0.999104400928856,
0.998428822114396)))
REPRESENTATION_ITEM('')
SURFACE()
);
#776=(
BOUNDED_SURFACE()
B_SPLINE_SURFACE(1,2,((#100970,#100971,#100972),(#100973,#100974,#100975)),
 .UNSPECIFIED.,.F.,.F.,.F.)
B_SPLINE_SURFACE_WITH_KNOTS((2,2),(3,3),(0.,1.),(0.0456081671210071,0.0575989447818621),
 .UNSPECIFIED.)
GEOMETRIC_REPRESENTATION_ITEM()
RATIONAL_B_SPLINE_SURFACE(((0.997793907739635,0.996365558499691,0.996354522974128),
(0.997793907739635,0.996365558499691,0.996354522974128)))
REPRESENTATION_ITEM('')
SURFACE()
);
#777=(
BOUNDED_SURFACE()
B_SPLINE_SURFACE(1,2,((#101010,#101011,#101012),(#101013,#101014,#101015)),
 .UNSPECIFIED.,.F.,.F.,.F.)
B_SPLINE_SURFACE_WITH_KNOTS((2,2),(3,3),(0.,1.),(0.0556006976522457,0.0675888855446171),
 .UNSPECIFIED.)
GEOMETRIC_REPRESENTATION_ITEM()
RATIONAL_B_SPLINE_SURFACE(((0.996397562408177,0.996150386836003,0.997319912821417),
(0.996397562408177,0.996150386836003,0.997319912821417)))
REPRESENTATION_ITEM('')
SURFACE()
);
#778=(
BOUNDED_SURFACE()
B_SPLINE_SURFACE(1,2,((#101016,#101017,#101018),(#101019,#101020,#101021)),
 .UNSPECIFIED.,.F.,.F.,.F.)
B_SPLINE_SURFACE_WITH_KNOTS((2,2),(3,3),(0.,1.),(0.0657448619281101,0.0758849574338219),
 .UNSPECIFIED.)
GEOMETRIC_REPRESENTATION_ITEM()
RATIONAL_B_SPLINE_SURFACE(((0.996993639757276,0.997798549146193,0.999617032345114),
(0.996993639757276,0.997798549146193,0.999617032345114)))
REPRESENTATION_ITEM('')
SURFACE()
);
#779=(
BOUNDED_SURFACE()
B_SPLINE_SURFACE(1,2,((#101096,#101097,#101098),(#101099,#101100,#101101)),
 .UNSPECIFIED.,.F.,.F.,.F.)
B_SPLINE_SURFACE_WITH_KNOTS((2,2),(3,3),(0.,1.),(0.00560769170938345,0.0176009697615912),
 .UNSPECIFIED.)
GEOMETRIC_REPRESENTATION_ITEM()
RATIONAL_B_SPLINE_SURFACE(((0.998183892106924,0.996573304252679,0.996380621268545),
(0.998183892106924,0.996573304252679,0.996380621268545)))
REPRESENTATION_ITEM('')
SURFACE()
);
#780=(
BOUNDED_SURFACE()
B_SPLINE_SURFACE(1,2,((#101186,#101187,#101188),(#101189,#101190,#101191)),
 .UNSPECIFIED.,.F.,.F.,.F.)
B_SPLINE_SURFACE_WITH_KNOTS((2,2),(3,3),(0.,1.),(0.0255903596131981,0.0375948596691614),
 .UNSPECIFIED.)
GEOMETRIC_REPRESENTATION_ITEM()
RATIONAL_B_SPLINE_SURFACE(((0.996753121756001,0.997505687613137,0.999678813023771),
(0.996753121756001,0.997505687613137,0.999678813023771)))
REPRESENTATION_ITEM('')
SURFACE()
);
#781=(
BOUNDED_SURFACE()
B_SPLINE_SURFACE(1,2,((#101209,#101210,#101211,#101212,#101213),(#101214,
#101215,#101216,#101217,#101218)),.UNSPECIFIED.,.F.,.F.,.F.)
B_SPLINE_SURFACE_WITH_KNOTS((2,2),(3,2,3),(0.519229702931099,1.),(0.0365944846645983,
0.0384615384615384,0.0431859278883673),.UNSPECIFIED.)
GEOMETRIC_REPRESENTATION_ITEM()
RATIONAL_B_SPLINE_SURFACE(((0.999326490452266,0.999646063968221,1.,0.999104400928858,
0.998428822114401),(0.999326490452266,0.999646063968221,1.,0.999104400928858,
0.998428822114401)))
REPRESENTATION_ITEM('')
SURFACE()
);
#782=(
BOUNDED_SURFACE()
B_SPLINE_SURFACE(1,2,((#101274,#101275,#101276),(#101277,#101278,#101279)),
 .UNSPECIFIED.,.F.,.F.,.F.)
B_SPLINE_SURFACE_WITH_KNOTS((2,2),(3,3),(0.,1.),(0.0456081671210021,0.0575989447818602),
 .UNSPECIFIED.)
GEOMETRIC_REPRESENTATION_ITEM()
RATIONAL_B_SPLINE_SURFACE(((0.997793907739637,0.996365558499691,0.996354522974128),
(0.997793907739637,0.996365558499691,0.996354522974128)))
REPRESENTATION_ITEM('')
SURFACE()
);
#783=(
BOUNDED_SURFACE()
B_SPLINE_SURFACE(1,2,((#101314,#101315,#101316),(#101317,#101318,#101319)),
 .UNSPECIFIED.,.F.,.F.,.F.)
B_SPLINE_SURFACE_WITH_KNOTS((2,2),(3,3),(0.,1.),(0.0556006976522425,0.0675888855446155),
 .UNSPECIFIED.)
GEOMETRIC_REPRESENTATION_ITEM()
RATIONAL_B_SPLINE_SURFACE(((0.996397562408177,0.996150386836003,0.997319912821417),
(0.996397562408177,0.996150386836003,0.997319912821417)))
REPRESENTATION_ITEM('')
SURFACE()
);
#784=(
BOUNDED_SURFACE()
B_SPLINE_SURFACE(1,2,((#101320,#101321,#101322),(#101323,#101324,#101325)),
 .UNSPECIFIED.,.F.,.F.,.F.)
B_SPLINE_SURFACE_WITH_KNOTS((2,2),(3,3),(0.,1.),(0.0657448619281082,0.0758849574338231),
 .UNSPECIFIED.)
GEOMETRIC_REPRESENTATION_ITEM()
RATIONAL_B_SPLINE_SURFACE(((0.996993639757276,0.997798549146192,0.999617032345115),
(0.996993639757276,0.997798549146192,0.999617032345115)))
REPRESENTATION_ITEM('')
SURFACE()
);
#785=(
BOUNDED_SURFACE()
B_SPLINE_SURFACE(1,2,((#101400,#101401,#101402),(#101403,#101404,#101405)),
 .UNSPECIFIED.,.F.,.F.,.F.)
B_SPLINE_SURFACE_WITH_KNOTS((2,2),(3,3),(0.,1.),(0.00560769170938436,0.0176009697615923),
 .UNSPECIFIED.)
GEOMETRIC_REPRESENTATION_ITEM()
RATIONAL_B_SPLINE_SURFACE(((0.998183892106924,0.996573304252679,0.996380621268545),
(0.998183892106924,0.996573304252679,0.996380621268545)))
REPRESENTATION_ITEM('')
SURFACE()
);
#786=(
BOUNDED_SURFACE()
B_SPLINE_SURFACE(1,2,((#101490,#101491,#101492),(#101493,#101494,#101495)),
 .UNSPECIFIED.,.F.,.F.,.F.)
B_SPLINE_SURFACE_WITH_KNOTS((2,2),(3,3),(0.,1.),(0.0255903596131979,0.0375948596691638),
 .UNSPECIFIED.)
GEOMETRIC_REPRESENTATION_ITEM()
RATIONAL_B_SPLINE_SURFACE(((0.996753121756001,0.997505687613137,0.999678813023772),
(0.996753121756001,0.997505687613137,0.999678813023772)))
REPRESENTATION_ITEM('')
SURFACE()
);
#787=(
BOUNDED_SURFACE()
B_SPLINE_SURFACE(1,2,((#101513,#101514,#101515,#101516,#101517),(#101518,
#101519,#101520,#101521,#101522)),.UNSPECIFIED.,.F.,.F.,.F.)
B_SPLINE_SURFACE_WITH_KNOTS((2,2),(3,2,3),(0.519229702930943,1.),(0.0365944846645846,
0.0384615384615384,0.0431859276814578),.UNSPECIFIED.)
GEOMETRIC_REPRESENTATION_ITEM()
RATIONAL_B_SPLINE_SURFACE(((0.999326490452261,0.999646063968218,1.,0.999104400968082,
0.998428822173576),(0.999326490452261,0.999646063968218,1.,0.999104400968082,
0.998428822173576)))
REPRESENTATION_ITEM('')
SURFACE()
);
#788=(
BOUNDED_SURFACE()
B_SPLINE_SURFACE(1,2,((#101578,#101579,#101580),(#101581,#101582,#101583)),
 .UNSPECIFIED.,.F.,.F.,.F.)
B_SPLINE_SURFACE_WITH_KNOTS((2,2),(3,3),(0.,1.),(0.0456081671210052,0.0575989447818616),
 .UNSPECIFIED.)
GEOMETRIC_REPRESENTATION_ITEM()
RATIONAL_B_SPLINE_SURFACE(((0.997793907739636,0.996365558499691,0.996354522974128),
(0.997793907739636,0.996365558499691,0.996354522974128)))
REPRESENTATION_ITEM('')
SURFACE()
);
#789=(
BOUNDED_SURFACE()
B_SPLINE_SURFACE(1,2,((#101618,#101619,#101620),(#101621,#101622,#101623)),
 .UNSPECIFIED.,.F.,.F.,.F.)
B_SPLINE_SURFACE_WITH_KNOTS((2,2),(3,3),(0.,1.),(0.0556006976522446,0.0675888855446172),
 .UNSPECIFIED.)
GEOMETRIC_REPRESENTATION_ITEM()
RATIONAL_B_SPLINE_SURFACE(((0.996397562408177,0.996150386836003,0.997319912821417),
(0.996397562408177,0.996150386836003,0.997319912821417)))
REPRESENTATION_ITEM('')
SURFACE()
);
#790=(
BOUNDED_SURFACE()
B_SPLINE_SURFACE(1,2,((#101624,#101625,#101626),(#101627,#101628,#101629)),
 .UNSPECIFIED.,.F.,.F.,.F.)
B_SPLINE_SURFACE_WITH_KNOTS((2,2),(3,3),(0.,1.),(0.0657448619281102,0.0758849574338215),
 .UNSPECIFIED.)
GEOMETRIC_REPRESENTATION_ITEM()
RATIONAL_B_SPLINE_SURFACE(((0.996993639757276,0.997798549146193,0.999617032345114),
(0.996993639757276,0.997798549146193,0.999617032345114)))
REPRESENTATION_ITEM('')
SURFACE()
);
#791=(
BOUNDED_SURFACE()
B_SPLINE_SURFACE(1,2,((#101704,#101705,#101706),(#101707,#101708,#101709)),
 .UNSPECIFIED.,.F.,.F.,.F.)
B_SPLINE_SURFACE_WITH_KNOTS((2,2),(3,3),(0.,1.),(0.00560769170938512,0.0176009697615927),
 .UNSPECIFIED.)
GEOMETRIC_REPRESENTATION_ITEM()
RATIONAL_B_SPLINE_SURFACE(((0.998183892106923,0.996573304252679,0.996380621268545),
(0.998183892106923,0.996573304252679,0.996380621268545)))
REPRESENTATION_ITEM('')
SURFACE()
);
#792=(
BOUNDED_SURFACE()
B_SPLINE_SURFACE(1,2,((#101794,#101795,#101796),(#101797,#101798,#101799)),
 .UNSPECIFIED.,.F.,.F.,.F.)
B_SPLINE_SURFACE_WITH_KNOTS((2,2),(3,3),(0.,1.),(0.0255903596132013,0.0375948596691634),
 .UNSPECIFIED.)
GEOMETRIC_REPRESENTATION_ITEM()
RATIONAL_B_SPLINE_SURFACE(((0.996753121756002,0.997505687613138,0.999678813023772),
(0.996753121756002,0.997505687613138,0.999678813023772)))
REPRESENTATION_ITEM('')
SURFACE()
);
#793=(
BOUNDED_SURFACE()
B_SPLINE_SURFACE(1,2,((#101817,#101818,#101819,#101820,#101821),(#101822,
#101823,#101824,#101825,#101826)),.UNSPECIFIED.,.F.,.F.,.F.)
B_SPLINE_SURFACE_WITH_KNOTS((2,2),(3,2,3),(0.519229702930844,1.),(0.0365944846645699,
0.0384615384615384,0.0431859278883406),.UNSPECIFIED.)
GEOMETRIC_REPRESENTATION_ITEM()
RATIONAL_B_SPLINE_SURFACE(((0.999326490452256,0.999646063968215,1.,0.999104400928863,
0.998428822114408),(0.999326490452256,0.999646063968215,1.,0.999104400928863,
0.998428822114408)))
REPRESENTATION_ITEM('')
SURFACE()
);
#794=(
BOUNDED_SURFACE()
B_SPLINE_SURFACE(1,2,((#101882,#101883,#101884),(#101885,#101886,#101887)),
 .UNSPECIFIED.,.F.,.F.,.F.)
B_SPLINE_SURFACE_WITH_KNOTS((2,2),(3,3),(0.,1.),(0.0456081671210051,0.0575989447818622),
 .UNSPECIFIED.)
GEOMETRIC_REPRESENTATION_ITEM()
RATIONAL_B_SPLINE_SURFACE(((0.997793907739636,0.996365558499691,0.996354522974128),
(0.997793907739636,0.996365558499691,0.996354522974128)))
REPRESENTATION_ITEM('')
SURFACE()
);
#795=(
BOUNDED_SURFACE()
B_SPLINE_SURFACE(1,2,((#101922,#101923,#101924),(#101925,#101926,#101927)),
 .UNSPECIFIED.,.F.,.F.,.F.)
B_SPLINE_SURFACE_WITH_KNOTS((2,2),(3,3),(0.,1.),(0.0556006976522459,0.0675888855446171),
 .UNSPECIFIED.)
GEOMETRIC_REPRESENTATION_ITEM()
RATIONAL_B_SPLINE_SURFACE(((0.996397562408177,0.996150386836003,0.997319912821417),
(0.996397562408177,0.996150386836003,0.997319912821417)))
REPRESENTATION_ITEM('')
SURFACE()
);
#796=(
BOUNDED_SURFACE()
B_SPLINE_SURFACE(1,2,((#101928,#101929,#101930),(#101931,#101932,#101933)),
 .UNSPECIFIED.,.F.,.F.,.F.)
B_SPLINE_SURFACE_WITH_KNOTS((2,2),(3,3),(0.,1.),(0.0657448619281102,0.0758849574338221),
 .UNSPECIFIED.)
GEOMETRIC_REPRESENTATION_ITEM()
RATIONAL_B_SPLINE_SURFACE(((0.996993639757276,0.997798549146193,0.999617032345114),
(0.996993639757276,0.997798549146193,0.999617032345114)))
REPRESENTATION_ITEM('')
SURFACE()
);
#797=(
BOUNDED_SURFACE()
B_SPLINE_SURFACE(1,2,((#102008,#102009,#102010),(#102011,#102012,#102013)),
 .UNSPECIFIED.,.F.,.F.,.F.)
B_SPLINE_SURFACE_WITH_KNOTS((2,2),(3,3),(0.,1.),(0.00560769170938337,0.0176009697615918),
 .UNSPECIFIED.)
GEOMETRIC_REPRESENTATION_ITEM()
RATIONAL_B_SPLINE_SURFACE(((0.998183892106924,0.996573304252679,0.996380621268545),
(0.998183892106924,0.996573304252679,0.996380621268545)))
REPRESENTATION_ITEM('')
SURFACE()
);
#798=(
BOUNDED_SURFACE()
B_SPLINE_SURFACE(1,2,((#102098,#102099,#102100),(#102101,#102102,#102103)),
 .UNSPECIFIED.,.F.,.F.,.F.)
B_SPLINE_SURFACE_WITH_KNOTS((2,2),(3,3),(0.,1.),(0.0255903596132021,0.0375948596691676),
 .UNSPECIFIED.)
GEOMETRIC_REPRESENTATION_ITEM()
RATIONAL_B_SPLINE_SURFACE(((0.996753121756002,0.997505687613138,0.999678813023774),
(0.996753121756002,0.997505687613138,0.999678813023774)))
REPRESENTATION_ITEM('')
SURFACE()
);
#799=(
BOUNDED_SURFACE()
B_SPLINE_SURFACE(1,2,((#102121,#102122,#102123,#102124,#102125),(#102126,
#102127,#102128,#102129,#102130)),.UNSPECIFIED.,.F.,.F.,.F.)
B_SPLINE_SURFACE_WITH_KNOTS((2,2),(3,2,3),(0.519229702930734,1.),(0.0365944846645561,
0.0384615384615384,0.0431859278883255),.UNSPECIFIED.)
GEOMETRIC_REPRESENTATION_ITEM()
RATIONAL_B_SPLINE_SURFACE(((0.999326490452252,0.999646063968213,1.,0.999104400928866,
0.998428822114412),(0.999326490452252,0.999646063968213,1.,0.999104400928866,
0.998428822114412)))
REPRESENTATION_ITEM('')
SURFACE()
);
#800=(
BOUNDED_SURFACE()
B_SPLINE_SURFACE(1,2,((#102186,#102187,#102188),(#102189,#102190,#102191)),
 .UNSPECIFIED.,.F.,.F.,.F.)
B_SPLINE_SURFACE_WITH_KNOTS((2,2),(3,3),(0.,1.),(0.0456081671210071,0.0575989447818615),
 .UNSPECIFIED.)
GEOMETRIC_REPRESENTATION_ITEM()
RATIONAL_B_SPLINE_SURFACE(((0.997793907739636,0.996365558499691,0.996354522974128),
(0.997793907739636,0.996365558499691,0.996354522974128)))
REPRESENTATION_ITEM('')
SURFACE()
);
#801=(
BOUNDED_SURFACE()
B_SPLINE_SURFACE(1,2,((#102226,#102227,#102228),(#102229,#102230,#102231)),
 .UNSPECIFIED.,.F.,.F.,.F.)
B_SPLINE_SURFACE_WITH_KNOTS((2,2),(3,3),(0.,1.),(0.0556006976522447,0.0675888855446152),
 .UNSPECIFIED.)
GEOMETRIC_REPRESENTATION_ITEM()
RATIONAL_B_SPLINE_SURFACE(((0.996397562408177,0.996150386836003,0.997319912821417),
(0.996397562408177,0.996150386836003,0.997319912821417)))
REPRESENTATION_ITEM('')
SURFACE()
);
#802=(
BOUNDED_SURFACE()
B_SPLINE_SURFACE(1,2,((#102232,#102233,#102234),(#102235,#102236,#102237)),
 .UNSPECIFIED.,.F.,.F.,.F.)
B_SPLINE_SURFACE_WITH_KNOTS((2,2),(3,3),(0.,1.),(0.0657448619281081,0.0758849574338218),
 .UNSPECIFIED.)
GEOMETRIC_REPRESENTATION_ITEM()
RATIONAL_B_SPLINE_SURFACE(((0.996993639757276,0.997798549146192,0.999617032345114),
(0.996993639757276,0.997798549146192,0.999617032345114)))
REPRESENTATION_ITEM('')
SURFACE()
);
#803=(
BOUNDED_SURFACE()
B_SPLINE_SURFACE(1,2,((#102312,#102313,#102314),(#102315,#102316,#102317)),
 .UNSPECIFIED.,.F.,.F.,.F.)
B_SPLINE_SURFACE_WITH_KNOTS((2,2),(3,3),(0.,1.),(0.00560769170938437,0.0176009697615918),
 .UNSPECIFIED.)
GEOMETRIC_REPRESENTATION_ITEM()
RATIONAL_B_SPLINE_SURFACE(((0.998183892106924,0.996573304252679,0.996380621268545),
(0.998183892106924,0.996573304252679,0.996380621268545)))
REPRESENTATION_ITEM('')
SURFACE()
);
#804=(
BOUNDED_SURFACE()
B_SPLINE_SURFACE(1,2,((#102402,#102403,#102404),(#102405,#102406,#102407)),
 .UNSPECIFIED.,.F.,.F.,.F.)
B_SPLINE_SURFACE_WITH_KNOTS((2,2),(3,3),(0.,1.),(0.0255903596132008,0.0375948596691702),
 .UNSPECIFIED.)
GEOMETRIC_REPRESENTATION_ITEM()
RATIONAL_B_SPLINE_SURFACE(((0.996753121756002,0.997505687613138,0.999678813023775),
(0.996753121756002,0.997505687613138,0.999678813023775)))
REPRESENTATION_ITEM('')
SURFACE()
);
#805=(
BOUNDED_SURFACE()
B_SPLINE_SURFACE(1,2,((#102425,#102426,#102427,#102428,#102429),(#102430,
#102431,#102432,#102433,#102434)),.UNSPECIFIED.,.F.,.F.,.F.)
B_SPLINE_SURFACE_WITH_KNOTS((2,2),(3,2,3),(0.519229702930626,1.),(0.0365944846645412,
0.0384615384615384,0.0431859276814168),.UNSPECIFIED.)
GEOMETRIC_REPRESENTATION_ITEM()
RATIONAL_B_SPLINE_SURFACE(((0.999326490452246,0.99964606396821,1.,0.99910440096809,
0.998428822173588),(0.999326490452246,0.99964606396821,1.,0.99910440096809,
0.998428822173588)))
REPRESENTATION_ITEM('')
SURFACE()
);
#806=(
BOUNDED_SURFACE()
B_SPLINE_SURFACE(1,2,((#102490,#102491,#102492),(#102493,#102494,#102495)),
 .UNSPECIFIED.,.F.,.F.,.F.)
B_SPLINE_SURFACE_WITH_KNOTS((2,2),(3,3),(0.,1.),(0.0456081671210094,0.0575989447818618),
 .UNSPECIFIED.)
GEOMETRIC_REPRESENTATION_ITEM()
RATIONAL_B_SPLINE_SURFACE(((0.997793907739635,0.996365558499691,0.996354522974128),
(0.997793907739635,0.996365558499691,0.996354522974128)))
REPRESENTATION_ITEM('')
SURFACE()
);
#807=(
BOUNDED_SURFACE()
B_SPLINE_SURFACE(1,2,((#102530,#102531,#102532),(#102533,#102534,#102535)),
 .UNSPECIFIED.,.F.,.F.,.F.)
B_SPLINE_SURFACE_WITH_KNOTS((2,2),(3,3),(0.,1.),(0.0556006976522449,0.0675888855446151),
 .UNSPECIFIED.)
GEOMETRIC_REPRESENTATION_ITEM()
RATIONAL_B_SPLINE_SURFACE(((0.996397562408177,0.996150386836003,0.997319912821417),
(0.996397562408177,0.996150386836003,0.997319912821417)))
REPRESENTATION_ITEM('')
SURFACE()
);
#808=(
BOUNDED_SURFACE()
B_SPLINE_SURFACE(1,2,((#102536,#102537,#102538),(#102539,#102540,#102541)),
 .UNSPECIFIED.,.F.,.F.,.F.)
B_SPLINE_SURFACE_WITH_KNOTS((2,2),(3,3),(0.,1.),(0.0657448619281081,0.0758849574338224),
 .UNSPECIFIED.)
GEOMETRIC_REPRESENTATION_ITEM()
RATIONAL_B_SPLINE_SURFACE(((0.996993639757276,0.997798549146192,0.999617032345114),
(0.996993639757276,0.997798549146192,0.999617032345114)))
REPRESENTATION_ITEM('')
SURFACE()
);
#809=(
BOUNDED_SURFACE()
B_SPLINE_SURFACE(1,2,((#102616,#102617,#102618),(#102619,#102620,#102621)),
 .UNSPECIFIED.,.F.,.F.,.F.)
B_SPLINE_SURFACE_WITH_KNOTS((2,2),(3,3),(0.,1.),(0.00560769170938164,0.0176009697615925),
 .UNSPECIFIED.)
GEOMETRIC_REPRESENTATION_ITEM()
RATIONAL_B_SPLINE_SURFACE(((0.998183892106924,0.996573304252679,0.996380621268545),
(0.998183892106924,0.996573304252679,0.996380621268545)))
REPRESENTATION_ITEM('')
SURFACE()
);
#810=(
BOUNDED_SURFACE()
B_SPLINE_SURFACE(1,2,((#102706,#102707,#102708),(#102709,#102710,#102711)),
 .UNSPECIFIED.,.F.,.F.,.F.)
B_SPLINE_SURFACE_WITH_KNOTS((2,2),(3,3),(0.,1.),(0.0255903596131988,0.0375948596691661),
 .UNSPECIFIED.)
GEOMETRIC_REPRESENTATION_ITEM()
RATIONAL_B_SPLINE_SURFACE(((0.996753121756001,0.997505687613137,0.999678813023773),
(0.996753121756001,0.997505687613137,0.999678813023773)))
REPRESENTATION_ITEM('')
SURFACE()
);
#811=(
BOUNDED_SURFACE()
B_SPLINE_SURFACE(1,2,((#102729,#102730,#102731,#102732,#102733),(#102734,
#102735,#102736,#102737,#102738)),.UNSPECIFIED.,.F.,.F.,.F.)
B_SPLINE_SURFACE_WITH_KNOTS((2,2),(3,2,3),(0.519229702930531,1.),(0.0365944846645262,
0.0384615384615384,0.0431859278100564),.UNSPECIFIED.)
GEOMETRIC_REPRESENTATION_ITEM()
RATIONAL_B_SPLINE_SURFACE(((0.999326490452241,0.999646063968207,1.,0.999104400943704,
0.998428822136797),(0.999326490452241,0.999646063968207,1.,0.999104400943704,
0.998428822136797)))
REPRESENTATION_ITEM('')
SURFACE()
);
#812=(
BOUNDED_SURFACE()
B_SPLINE_SURFACE(1,2,((#102794,#102795,#102796),(#102797,#102798,#102799)),
 .UNSPECIFIED.,.F.,.F.,.F.)
B_SPLINE_SURFACE_WITH_KNOTS((2,2),(3,3),(0.,1.),(0.0456081671210071,0.0575989447818625),
 .UNSPECIFIED.)
GEOMETRIC_REPRESENTATION_ITEM()
RATIONAL_B_SPLINE_SURFACE(((0.997793907739635,0.99636555849969,0.996354522974128),
(0.997793907739635,0.99636555849969,0.996354522974128)))
REPRESENTATION_ITEM('')
SURFACE()
);
#813=(
BOUNDED_SURFACE()
B_SPLINE_SURFACE(1,2,((#102834,#102835,#102836),(#102837,#102838,#102839)),
 .UNSPECIFIED.,.F.,.F.,.F.)
B_SPLINE_SURFACE_WITH_KNOTS((2,2),(3,3),(0.,1.),(0.0556006976522469,0.067588885544616),
 .UNSPECIFIED.)
GEOMETRIC_REPRESENTATION_ITEM()
RATIONAL_B_SPLINE_SURFACE(((0.996397562408177,0.996150386836004,0.997319912821417),
(0.996397562408177,0.996150386836004,0.997319912821417)))
REPRESENTATION_ITEM('')
SURFACE()
);
#814=(
BOUNDED_SURFACE()
B_SPLINE_SURFACE(1,2,((#102840,#102841,#102842),(#102843,#102844,#102845)),
 .UNSPECIFIED.,.F.,.F.,.F.)
B_SPLINE_SURFACE_WITH_KNOTS((2,2),(3,3),(0.,1.),(0.0657448619281091,0.0758849574338235),
 .UNSPECIFIED.)
GEOMETRIC_REPRESENTATION_ITEM()
RATIONAL_B_SPLINE_SURFACE(((0.996993639757276,0.997798549146192,0.999617032345115),
(0.996993639757276,0.997798549146192,0.999617032345115)))
REPRESENTATION_ITEM('')
SURFACE()
);
#815=(
BOUNDED_SURFACE()
B_SPLINE_SURFACE(1,2,((#102920,#102921,#102922),(#102923,#102924,#102925)),
 .UNSPECIFIED.,.F.,.F.,.F.)
B_SPLINE_SURFACE_WITH_KNOTS((2,2),(3,3),(0.,1.),(0.00560769170938326,0.0176009697615917),
 .UNSPECIFIED.)
GEOMETRIC_REPRESENTATION_ITEM()
RATIONAL_B_SPLINE_SURFACE(((0.998183892106924,0.996573304252679,0.996380621268545),
(0.998183892106924,0.996573304252679,0.996380621268545)))
REPRESENTATION_ITEM('')
SURFACE()
);
#816=(
BOUNDED_SURFACE()
B_SPLINE_SURFACE(1,2,((#103010,#103011,#103012),(#103013,#103014,#103015)),
 .UNSPECIFIED.,.F.,.F.,.F.)
B_SPLINE_SURFACE_WITH_KNOTS((2,2),(3,3),(0.,1.),(0.0255903596132,0.0375948596691658),
 .UNSPECIFIED.)
GEOMETRIC_REPRESENTATION_ITEM()
RATIONAL_B_SPLINE_SURFACE(((0.996753121756002,0.997505687613138,0.999678813023773),
(0.996753121756002,0.997505687613138,0.999678813023773)))
REPRESENTATION_ITEM('')
SURFACE()
);
#817=(
BOUNDED_SURFACE()
B_SPLINE_SURFACE(1,2,((#103033,#103034,#103035,#103036,#103037),(#103038,
#103039,#103040,#103041,#103042)),.UNSPECIFIED.,.F.,.F.,.F.)
B_SPLINE_SURFACE_WITH_KNOTS((2,2),(3,2,3),(0.519229702930332,1.),(0.0365944846645122,
0.0384615384615384,0.0431859278882811),.UNSPECIFIED.)
GEOMETRIC_REPRESENTATION_ITEM()
RATIONAL_B_SPLINE_SURFACE(((0.999326490452237,0.999646063968205,1.,0.999104400928875,
0.998428822114426),(0.999326490452237,0.999646063968205,1.,0.999104400928875,
0.998428822114426)))
REPRESENTATION_ITEM('')
SURFACE()
);
#818=(
BOUNDED_SURFACE()
B_SPLINE_SURFACE(1,2,((#103098,#103099,#103100),(#103101,#103102,#103103)),
 .UNSPECIFIED.,.F.,.F.,.F.)
B_SPLINE_SURFACE_WITH_KNOTS((2,2),(3,3),(0.,1.),(0.0456081671210064,0.0575989447818616),
 .UNSPECIFIED.)
GEOMETRIC_REPRESENTATION_ITEM()
RATIONAL_B_SPLINE_SURFACE(((0.997793907739636,0.996365558499691,0.996354522974128),
(0.997793907739636,0.996365558499691,0.996354522974128)))
REPRESENTATION_ITEM('')
SURFACE()
);
#819=(
BOUNDED_SURFACE()
B_SPLINE_SURFACE(1,2,((#103138,#103139,#103140),(#103141,#103142,#103143)),
 .UNSPECIFIED.,.F.,.F.,.F.)
B_SPLINE_SURFACE_WITH_KNOTS((2,2),(3,3),(0.,1.),(0.0556006976522446,0.067588885544616),
 .UNSPECIFIED.)
GEOMETRIC_REPRESENTATION_ITEM()
RATIONAL_B_SPLINE_SURFACE(((0.996397562408177,0.996150386836003,0.997319912821417),
(0.996397562408177,0.996150386836003,0.997319912821417)))
REPRESENTATION_ITEM('')
SURFACE()
);
#820=(
BOUNDED_SURFACE()
B_SPLINE_SURFACE(1,2,((#103144,#103145,#103146),(#103147,#103148,#103149)),
 .UNSPECIFIED.,.F.,.F.,.F.)
B_SPLINE_SURFACE_WITH_KNOTS((2,2),(3,3),(0.,1.),(0.0657448619281089,0.0758849574338229),
 .UNSPECIFIED.)
GEOMETRIC_REPRESENTATION_ITEM()
RATIONAL_B_SPLINE_SURFACE(((0.996993639757276,0.997798549146192,0.999617032345115),
(0.996993639757276,0.997798549146192,0.999617032345115)))
REPRESENTATION_ITEM('')
SURFACE()
);
#821=(
BOUNDED_SURFACE()
B_SPLINE_SURFACE(1,2,((#103224,#103225,#103226),(#103227,#103228,#103229)),
 .UNSPECIFIED.,.F.,.F.,.F.)
B_SPLINE_SURFACE_WITH_KNOTS((2,2),(3,3),(0.,1.),(0.005607691709382,0.0176009697615936),
 .UNSPECIFIED.)
GEOMETRIC_REPRESENTATION_ITEM()
RATIONAL_B_SPLINE_SURFACE(((0.998183892106924,0.996573304252679,0.996380621268545),
(0.998183892106924,0.996573304252679,0.996380621268545)))
REPRESENTATION_ITEM('')
SURFACE()
);
#822=(
BOUNDED_SURFACE()
B_SPLINE_SURFACE(1,2,((#103314,#103315,#103316),(#103317,#103318,#103319)),
 .UNSPECIFIED.,.F.,.F.,.F.)
B_SPLINE_SURFACE_WITH_KNOTS((2,2),(3,3),(0.,1.),(0.0255903596132,0.037594859669166),
 .UNSPECIFIED.)
GEOMETRIC_REPRESENTATION_ITEM()
RATIONAL_B_SPLINE_SURFACE(((0.996753121756002,0.997505687613138,0.999678813023773),
(0.996753121756002,0.997505687613138,0.999678813023773)))
REPRESENTATION_ITEM('')
SURFACE()
);
#823=(
BOUNDED_SURFACE()
B_SPLINE_SURFACE(1,2,((#103337,#103338,#103339,#103340,#103341),(#103342,
#103343,#103344,#103345,#103346)),.UNSPECIFIED.,.F.,.F.,.F.)
B_SPLINE_SURFACE_WITH_KNOTS((2,2),(3,2,3),(0.519229702930221,1.),(0.0365944846644977,
0.0384615384615384,0.0431859278882677),.UNSPECIFIED.)
GEOMETRIC_REPRESENTATION_ITEM()
RATIONAL_B_SPLINE_SURFACE(((0.999326490452232,0.999646063968202,1.,0.999104400928877,
0.998428822114429),(0.999326490452232,0.999646063968202,1.,0.999104400928877,
0.998428822114429)))
REPRESENTATION_ITEM('')
SURFACE()
);
#824=(
BOUNDED_SURFACE()
B_SPLINE_SURFACE(1,2,((#103402,#103403,#103404),(#103405,#103406,#103407)),
 .UNSPECIFIED.,.F.,.F.,.F.)
B_SPLINE_SURFACE_WITH_KNOTS((2,2),(3,3),(0.,1.),(0.0456081671210053,0.0575989447818605),
 .UNSPECIFIED.)
GEOMETRIC_REPRESENTATION_ITEM()
RATIONAL_B_SPLINE_SURFACE(((0.997793907739636,0.996365558499691,0.996354522974128),
(0.997793907739636,0.996365558499691,0.996354522974128)))
REPRESENTATION_ITEM('')
SURFACE()
);
#825=(
BOUNDED_SURFACE()
B_SPLINE_SURFACE(1,2,((#103442,#103443,#103444),(#103445,#103446,#103447)),
 .UNSPECIFIED.,.F.,.F.,.F.)
B_SPLINE_SURFACE_WITH_KNOTS((2,2),(3,3),(0.,1.),(0.0556006976522437,0.0675888855446152),
 .UNSPECIFIED.)
GEOMETRIC_REPRESENTATION_ITEM()
RATIONAL_B_SPLINE_SURFACE(((0.996397562408177,0.996150386836003,0.997319912821417),
(0.996397562408177,0.996150386836003,0.997319912821417)))
REPRESENTATION_ITEM('')
SURFACE()
);
#826=(
BOUNDED_SURFACE()
B_SPLINE_SURFACE(1,2,((#103448,#103449,#103450),(#103451,#103452,#103453)),
 .UNSPECIFIED.,.F.,.F.,.F.)
B_SPLINE_SURFACE_WITH_KNOTS((2,2),(3,3),(0.,1.),(0.065744861928108,0.0758849574338232),
 .UNSPECIFIED.)
GEOMETRIC_REPRESENTATION_ITEM()
RATIONAL_B_SPLINE_SURFACE(((0.996993639757276,0.997798549146192,0.999617032345115),
(0.996993639757276,0.997798549146192,0.999617032345115)))
REPRESENTATION_ITEM('')
SURFACE()
);
#827=(
BOUNDED_SURFACE()
B_SPLINE_SURFACE(1,2,((#103528,#103529,#103530),(#103531,#103532,#103533)),
 .UNSPECIFIED.,.F.,.F.,.F.)
B_SPLINE_SURFACE_WITH_KNOTS((2,2),(3,3),(0.,1.),(0.00560769170938538,0.0176009697615917),
 .UNSPECIFIED.)
GEOMETRIC_REPRESENTATION_ITEM()
RATIONAL_B_SPLINE_SURFACE(((0.998183892106923,0.996573304252679,0.996380621268545),
(0.998183892106923,0.996573304252679,0.996380621268545)))
REPRESENTATION_ITEM('')
SURFACE()
);
#828=(
BOUNDED_SURFACE()
B_SPLINE_SURFACE(1,2,((#103618,#103619,#103620),(#103621,#103622,#103623)),
 .UNSPECIFIED.,.F.,.F.,.F.)
B_SPLINE_SURFACE_WITH_KNOTS((2,2),(3,3),(0.,1.),(0.0255903596132031,0.0375948596691665),
 .UNSPECIFIED.)
GEOMETRIC_REPRESENTATION_ITEM()
RATIONAL_B_SPLINE_SURFACE(((0.996753121756002,0.997505687613138,0.999678813023773),
(0.996753121756002,0.997505687613138,0.999678813023773)))
REPRESENTATION_ITEM('')
SURFACE()
);
#829=(
BOUNDED_SURFACE()
B_SPLINE_SURFACE(1,2,((#103641,#103642,#103643,#103644,#103645),(#103646,
#103647,#103648,#103649,#103650)),.UNSPECIFIED.,.F.,.F.,.F.)
B_SPLINE_SURFACE_WITH_KNOTS((2,2),(3,2,3),(0.519229702930174,1.),(0.0365944846644854,
0.0384615384615384,0.0431859278882548),.UNSPECIFIED.)
GEOMETRIC_REPRESENTATION_ITEM()
RATIONAL_B_SPLINE_SURFACE(((0.999326490452227,0.999646063968199,1.,0.99910440092888,
0.998428822114433),(0.999326490452227,0.999646063968199,1.,0.99910440092888,
0.998428822114433)))
REPRESENTATION_ITEM('')
SURFACE()
);
#830=(
BOUNDED_SURFACE()
B_SPLINE_SURFACE(1,2,((#103706,#103707,#103708),(#103709,#103710,#103711)),
 .UNSPECIFIED.,.F.,.F.,.F.)
B_SPLINE_SURFACE_WITH_KNOTS((2,2),(3,3),(0.,1.),(0.0456081671210082,0.057598944781862),
 .UNSPECIFIED.)
GEOMETRIC_REPRESENTATION_ITEM()
RATIONAL_B_SPLINE_SURFACE(((0.997793907739635,0.996365558499691,0.996354522974128),
(0.997793907739635,0.996365558499691,0.996354522974128)))
REPRESENTATION_ITEM('')
SURFACE()
);
#831=(
BOUNDED_SURFACE()
B_SPLINE_SURFACE(1,2,((#103746,#103747,#103748),(#103749,#103750,#103751)),
 .UNSPECIFIED.,.F.,.F.,.F.)
B_SPLINE_SURFACE_WITH_KNOTS((2,2),(3,3),(0.,1.),(0.0556006976522477,0.067588885544619),
 .UNSPECIFIED.)
GEOMETRIC_REPRESENTATION_ITEM()
RATIONAL_B_SPLINE_SURFACE(((0.996397562408177,0.996150386836004,0.997319912821418),
(0.996397562408177,0.996150386836004,0.997319912821418)))
REPRESENTATION_ITEM('')
SURFACE()
);
#832=(
BOUNDED_SURFACE()
B_SPLINE_SURFACE(1,2,((#103752,#103753,#103754),(#103755,#103756,#103757)),
 .UNSPECIFIED.,.F.,.F.,.F.)
B_SPLINE_SURFACE_WITH_KNOTS((2,2),(3,3),(0.,1.),(0.0657448619281122,0.0758849574338225),
 .UNSPECIFIED.)
GEOMETRIC_REPRESENTATION_ITEM()
RATIONAL_B_SPLINE_SURFACE(((0.996993639757277,0.997798549146193,0.999617032345115),
(0.996993639757277,0.997798549146193,0.999617032345115)))
REPRESENTATION_ITEM('')
SURFACE()
);
#833=(
BOUNDED_SURFACE()
B_SPLINE_SURFACE(1,2,((#103832,#103833,#103834),(#103835,#103836,#103837)),
 .UNSPECIFIED.,.F.,.F.,.F.)
B_SPLINE_SURFACE_WITH_KNOTS((2,2),(3,3),(0.,1.),(0.00560769170938322,0.0176009697615935),
 .UNSPECIFIED.)
GEOMETRIC_REPRESENTATION_ITEM()
RATIONAL_B_SPLINE_SURFACE(((0.998183892106924,0.996573304252679,0.996380621268545),
(0.998183892106924,0.996573304252679,0.996380621268545)))
REPRESENTATION_ITEM('')
SURFACE()
);
#834=(
BOUNDED_SURFACE()
B_SPLINE_SURFACE(1,2,((#103922,#103923,#103924),(#103925,#103926,#103927)),
 .UNSPECIFIED.,.F.,.F.,.F.)
B_SPLINE_SURFACE_WITH_KNOTS((2,2),(3,3),(0.,1.),(0.0255903596131996,0.0375948596691703),
 .UNSPECIFIED.)
GEOMETRIC_REPRESENTATION_ITEM()
RATIONAL_B_SPLINE_SURFACE(((0.996753121756002,0.997505687613138,0.999678813023775),
(0.996753121756002,0.997505687613138,0.999678813023775)))
REPRESENTATION_ITEM('')
SURFACE()
);
#835=(
BOUNDED_SURFACE()
B_SPLINE_SURFACE(1,2,((#103945,#103946,#103947,#103948,#103949),(#103950,
#103951,#103952,#103953,#103954)),.UNSPECIFIED.,.F.,.F.,.F.)
B_SPLINE_SURFACE_WITH_KNOTS((2,2),(3,2,3),(0.519229702929906,1.),(0.036594484664473,
0.0384615384615384,0.043185927888243),.UNSPECIFIED.)
GEOMETRIC_REPRESENTATION_ITEM()
RATIONAL_B_SPLINE_SURFACE(((0.999326490452223,0.999646063968197,1.,0.999104400928882,
0.998428822114436),(0.999326490452223,0.999646063968197,1.,0.999104400928882,
0.998428822114436)))
REPRESENTATION_ITEM('')
SURFACE()
);
#836=(
BOUNDED_SURFACE()
B_SPLINE_SURFACE(1,2,((#104010,#104011,#104012),(#104013,#104014,#104015)),
 .UNSPECIFIED.,.F.,.F.,.F.)
B_SPLINE_SURFACE_WITH_KNOTS((2,2),(3,3),(0.,1.),(0.0456081671210071,0.0575989447818621),
 .UNSPECIFIED.)
GEOMETRIC_REPRESENTATION_ITEM()
RATIONAL_B_SPLINE_SURFACE(((0.997793907739636,0.996365558499691,0.996354522974128),
(0.997793907739636,0.996365558499691,0.996354522974128)))
REPRESENTATION_ITEM('')
SURFACE()
);
#837=(
BOUNDED_SURFACE()
B_SPLINE_SURFACE(1,2,((#104050,#104051,#104052),(#104053,#104054,#104055)),
 .UNSPECIFIED.,.F.,.F.,.F.)
B_SPLINE_SURFACE_WITH_KNOTS((2,2),(3,3),(0.,1.),(0.055600697652246,0.0675888855446162),
 .UNSPECIFIED.)
GEOMETRIC_REPRESENTATION_ITEM()
RATIONAL_B_SPLINE_SURFACE(((0.996397562408177,0.996150386836003,0.997319912821417),
(0.996397562408177,0.996150386836003,0.997319912821417)))
REPRESENTATION_ITEM('')
SURFACE()
);
#838=(
BOUNDED_SURFACE()
B_SPLINE_SURFACE(1,2,((#104056,#104057,#104058),(#104059,#104060,#104061)),
 .UNSPECIFIED.,.F.,.F.,.F.)
B_SPLINE_SURFACE_WITH_KNOTS((2,2),(3,3),(0.,1.),(0.0657448619281092,0.0758849574338239),
 .UNSPECIFIED.)
GEOMETRIC_REPRESENTATION_ITEM()
RATIONAL_B_SPLINE_SURFACE(((0.996993639757276,0.997798549146193,0.999617032345115),
(0.996993639757276,0.997798549146193,0.999617032345115)))
REPRESENTATION_ITEM('')
SURFACE()
);
#839=(
BOUNDED_SURFACE()
B_SPLINE_SURFACE(1,2,((#104130,#104131,#104132),(#104133,#104134,#104135)),
 .UNSPECIFIED.,.F.,.F.,.F.)
B_SPLINE_SURFACE_WITH_KNOTS((2,2),(3,3),(0.,1.),(0.00560769170938336,0.0176009697615918),
 .UNSPECIFIED.)
GEOMETRIC_REPRESENTATION_ITEM()
RATIONAL_B_SPLINE_SURFACE(((0.998183892106924,0.996573304252679,0.996380621268545),
(0.998183892106924,0.996573304252679,0.996380621268545)))
REPRESENTATION_ITEM('')
SURFACE()
);
#840=(
BOUNDED_SURFACE()
B_SPLINE_SURFACE(1,2,((#104226,#104227,#104228),(#104229,#104230,#104231)),
 .UNSPECIFIED.,.F.,.F.,.F.)
B_SPLINE_SURFACE_WITH_KNOTS((2,2),(3,3),(0.,1.),(0.0255903596132001,0.0375948596691636),
 .UNSPECIFIED.)
GEOMETRIC_REPRESENTATION_ITEM()
RATIONAL_B_SPLINE_SURFACE(((0.996753121756002,0.997505687613137,0.999678813023772),
(0.996753121756002,0.997505687613137,0.999678813023772)))
REPRESENTATION_ITEM('')
SURFACE()
);
#841=(
BOUNDED_SURFACE()
B_SPLINE_SURFACE(1,2,((#104249,#104250,#104251,#104252,#104253),(#104254,
#104255,#104256,#104257,#104258)),.UNSPECIFIED.,.F.,.F.,.F.)
B_SPLINE_SURFACE_WITH_KNOTS((2,2),(3,2,3),(0.519229702929822,1.),(0.0365944846644523,
0.0384615384615384,0.0431859278882314),.UNSPECIFIED.)
GEOMETRIC_REPRESENTATION_ITEM()
RATIONAL_B_SPLINE_SURFACE(((0.999326490452216,0.999646063968193,1.,0.999104400928884,
0.998428822114439),(0.999326490452216,0.999646063968193,1.,0.999104400928884,
0.998428822114439)))
REPRESENTATION_ITEM('')
SURFACE()
);
#842=(
BOUNDED_SURFACE()
B_SPLINE_SURFACE(1,2,((#104314,#104315,#104316),(#104317,#104318,#104319)),
 .UNSPECIFIED.,.F.,.F.,.F.)
B_SPLINE_SURFACE_WITH_KNOTS((2,2),(3,3),(0.,1.),(0.0456081671210085,0.0575989447818603),
 .UNSPECIFIED.)
GEOMETRIC_REPRESENTATION_ITEM()
RATIONAL_B_SPLINE_SURFACE(((0.997793907739635,0.996365558499691,0.996354522974128),
(0.997793907739635,0.996365558499691,0.996354522974128)))
REPRESENTATION_ITEM('')
SURFACE()
);
#843=(
BOUNDED_SURFACE()
B_SPLINE_SURFACE(1,2,((#104354,#104355,#104356),(#104357,#104358,#104359)),
 .UNSPECIFIED.,.F.,.F.,.F.)
B_SPLINE_SURFACE_WITH_KNOTS((2,2),(3,3),(0.,1.),(0.0556006976522427,0.0675888855446153),
 .UNSPECIFIED.)
GEOMETRIC_REPRESENTATION_ITEM()
RATIONAL_B_SPLINE_SURFACE(((0.996397562408177,0.996150386836003,0.997319912821417),
(0.996397562408177,0.996150386836003,0.997319912821417)))
REPRESENTATION_ITEM('')
SURFACE()
);
#844=(
BOUNDED_SURFACE()
B_SPLINE_SURFACE(1,2,((#104360,#104361,#104362),(#104363,#104364,#104365)),
 .UNSPECIFIED.,.F.,.F.,.F.)
B_SPLINE_SURFACE_WITH_KNOTS((2,2),(3,3),(0.,1.),(0.065744861928108,0.0758849574338233),
 .UNSPECIFIED.)
GEOMETRIC_REPRESENTATION_ITEM()
RATIONAL_B_SPLINE_SURFACE(((0.996993639757276,0.997798549146192,0.999617032345115),
(0.996993639757276,0.997798549146192,0.999617032345115)))
REPRESENTATION_ITEM('')
SURFACE()
);
#845=(
BOUNDED_SURFACE()
B_SPLINE_SURFACE(1,2,((#104440,#104441,#104442),(#104443,#104444,#104445)),
 .UNSPECIFIED.,.F.,.F.,.F.)
B_SPLINE_SURFACE_WITH_KNOTS((2,2),(3,3),(0.,1.),(0.00560769170938435,0.0176009697615927),
 .UNSPECIFIED.)
GEOMETRIC_REPRESENTATION_ITEM()
RATIONAL_B_SPLINE_SURFACE(((0.998183892106924,0.996573304252679,0.996380621268545),
(0.998183892106924,0.996573304252679,0.996380621268545)))
REPRESENTATION_ITEM('')
SURFACE()
);
#846=(
BOUNDED_SURFACE()
B_SPLINE_SURFACE(1,2,((#104530,#104531,#104532),(#104533,#104534,#104535)),
 .UNSPECIFIED.,.F.,.F.,.F.)
B_SPLINE_SURFACE_WITH_KNOTS((2,2),(3,3),(0.,1.),(0.025590359613201,0.0375948596691668),
 .UNSPECIFIED.)
GEOMETRIC_REPRESENTATION_ITEM()
RATIONAL_B_SPLINE_SURFACE(((0.996753121756002,0.997505687613138,0.999678813023773),
(0.996753121756002,0.997505687613138,0.999678813023773)))
REPRESENTATION_ITEM('')
SURFACE()
);
#847=(
BOUNDED_SURFACE()
B_SPLINE_SURFACE(1,2,((#104553,#104554,#104555,#104556,#104557),(#104558,
#104559,#104560,#104561,#104562)),.UNSPECIFIED.,.F.,.F.,.F.)
B_SPLINE_SURFACE_WITH_KNOTS((2,2),(3,2,3),(0.519229702929727,1.),(0.0365944846644431,
0.0384615384615384,0.0431859278882212),.UNSPECIFIED.)
GEOMETRIC_REPRESENTATION_ITEM()
RATIONAL_B_SPLINE_SURFACE(((0.999326490452213,0.999646063968191,1.,0.999104400928886,
0.998428822114442),(0.999326490452213,0.999646063968191,1.,0.999104400928886,
0.998428822114442)))
REPRESENTATION_ITEM('')
SURFACE()
);
#848=(
BOUNDED_SURFACE()
B_SPLINE_SURFACE(1,2,((#104618,#104619,#104620),(#104621,#104622,#104623)),
 .UNSPECIFIED.,.F.,.F.,.F.)
B_SPLINE_SURFACE_WITH_KNOTS((2,2),(3,3),(0.,1.),(0.0456081671210059,0.0575989447818637),
 .UNSPECIFIED.)
GEOMETRIC_REPRESENTATION_ITEM()
RATIONAL_B_SPLINE_SURFACE(((0.997793907739636,0.99636555849969,0.996354522974128),
(0.997793907739636,0.99636555849969,0.996354522974128)))
REPRESENTATION_ITEM('')
SURFACE()
);
#849=(
BOUNDED_SURFACE()
B_SPLINE_SURFACE(1,2,((#104658,#104659,#104660),(#104661,#104662,#104663)),
 .UNSPECIFIED.,.F.,.F.,.F.)
B_SPLINE_SURFACE_WITH_KNOTS((2,2),(3,3),(0.,1.),(0.055600697652249,0.0675888855446156),
 .UNSPECIFIED.)
GEOMETRIC_REPRESENTATION_ITEM()
RATIONAL_B_SPLINE_SURFACE(((0.996397562408177,0.996150386836004,0.997319912821417),
(0.996397562408177,0.996150386836004,0.997319912821417)))
REPRESENTATION_ITEM('')
SURFACE()
);
#850=(
BOUNDED_SURFACE()
B_SPLINE_SURFACE(1,2,((#104664,#104665,#104666),(#104667,#104668,#104669)),
 .UNSPECIFIED.,.F.,.F.,.F.)
B_SPLINE_SURFACE_WITH_KNOTS((2,2),(3,3),(0.,1.),(0.0657448619281089,0.0758849574338234),
 .UNSPECIFIED.)
GEOMETRIC_REPRESENTATION_ITEM()
RATIONAL_B_SPLINE_SURFACE(((0.996993639757276,0.997798549146192,0.999617032345115),
(0.996993639757276,0.997798549146192,0.999617032345115)))
REPRESENTATION_ITEM('')
SURFACE()
);
#851=(
BOUNDED_SURFACE()
B_SPLINE_SURFACE(1,2,((#104744,#104745,#104746),(#104747,#104748,#104749)),
 .UNSPECIFIED.,.F.,.F.,.F.)
B_SPLINE_SURFACE_WITH_KNOTS((2,2),(3,3),(0.,1.),(0.00560769170938427,0.0176009697615923),
 .UNSPECIFIED.)
GEOMETRIC_REPRESENTATION_ITEM()
RATIONAL_B_SPLINE_SURFACE(((0.998183892106924,0.996573304252679,0.996380621268545),
(0.998183892106924,0.996573304252679,0.996380621268545)))
REPRESENTATION_ITEM('')
SURFACE()
);
#852=(
BOUNDED_SURFACE()
B_SPLINE_SURFACE(1,2,((#104834,#104835,#104836),(#104837,#104838,#104839)),
 .UNSPECIFIED.,.F.,.F.,.F.)
B_SPLINE_SURFACE_WITH_KNOTS((2,2),(3,3),(0.,1.),(0.0255903596131988,0.0375948596691661),
 .UNSPECIFIED.)
GEOMETRIC_REPRESENTATION_ITEM()
RATIONAL_B_SPLINE_SURFACE(((0.996753121756001,0.997505687613137,0.999678813023773),
(0.996753121756001,0.997505687613137,0.999678813023773)))
REPRESENTATION_ITEM('')
SURFACE()
);
#853=(
BOUNDED_SURFACE()
B_SPLINE_SURFACE(1,2,((#104857,#104858,#104859,#104860,#104861),(#104862,
#104863,#104864,#104865,#104866)),.UNSPECIFIED.,.F.,.F.,.F.)
B_SPLINE_SURFACE_WITH_KNOTS((2,2),(3,2,3),(0.519229702929575,1.),(0.0365944846644434,
0.0384615384615384,0.0431859278882126),.UNSPECIFIED.)
GEOMETRIC_REPRESENTATION_ITEM()
RATIONAL_B_SPLINE_SURFACE(((0.999326490452213,0.999646063968191,1.,0.999104400928888,
0.998428822114445),(0.999326490452213,0.999646063968191,1.,0.999104400928888,
0.998428822114445)))
REPRESENTATION_ITEM('')
SURFACE()
);
#854=(
BOUNDED_SURFACE()
B_SPLINE_SURFACE(1,2,((#104922,#104923,#104924),(#104925,#104926,#104927)),
 .UNSPECIFIED.,.F.,.F.,.F.)
B_SPLINE_SURFACE_WITH_KNOTS((2,2),(3,3),(0.,1.),(0.0456081671210072,0.0575989447818615),
 .UNSPECIFIED.)
GEOMETRIC_REPRESENTATION_ITEM()
RATIONAL_B_SPLINE_SURFACE(((0.997793907739636,0.996365558499691,0.996354522974128),
(0.997793907739636,0.996365558499691,0.996354522974128)))
REPRESENTATION_ITEM('')
SURFACE()
);
#855=(
BOUNDED_SURFACE()
B_SPLINE_SURFACE(1,2,((#104962,#104963,#104964),(#104965,#104966,#104967)),
 .UNSPECIFIED.,.F.,.F.,.F.)
B_SPLINE_SURFACE_WITH_KNOTS((2,2),(3,3),(0.,1.),(0.0556006976522444,0.0675888855446182),
 .UNSPECIFIED.)
GEOMETRIC_REPRESENTATION_ITEM()
RATIONAL_B_SPLINE_SURFACE(((0.996397562408177,0.996150386836003,0.997319912821418),
(0.996397562408177,0.996150386836003,0.997319912821418)))
REPRESENTATION_ITEM('')
SURFACE()
);
#856=(
BOUNDED_SURFACE()
B_SPLINE_SURFACE(1,2,((#104968,#104969,#104970),(#104971,#104972,#104973)),
 .UNSPECIFIED.,.F.,.F.,.F.)
B_SPLINE_SURFACE_WITH_KNOTS((2,2),(3,3),(0.,1.),(0.0657448619281111,0.0758849574338232),
 .UNSPECIFIED.)
GEOMETRIC_REPRESENTATION_ITEM()
RATIONAL_B_SPLINE_SURFACE(((0.996993639757276,0.997798549146193,0.999617032345115),
(0.996993639757276,0.997798549146193,0.999617032345115)))
REPRESENTATION_ITEM('')
SURFACE()
);
#857=(
BOUNDED_SURFACE()
B_SPLINE_SURFACE(1,2,((#105048,#105049,#105050),(#105051,#105052,#105053)),
 .UNSPECIFIED.,.F.,.F.,.F.)
B_SPLINE_SURFACE_WITH_KNOTS((2,2),(3,3),(0.,1.),(0.00560769170938328,0.0176009697615924),
 .UNSPECIFIED.)
GEOMETRIC_REPRESENTATION_ITEM()
RATIONAL_B_SPLINE_SURFACE(((0.998183892106924,0.996573304252679,0.996380621268545),
(0.998183892106924,0.996573304252679,0.996380621268545)))
REPRESENTATION_ITEM('')
SURFACE()
);
#858=(
BOUNDED_SURFACE()
B_SPLINE_SURFACE(1,2,((#105138,#105139,#105140),(#105141,#105142,#105143)),
 .UNSPECIFIED.,.F.,.F.,.F.)
B_SPLINE_SURFACE_WITH_KNOTS((2,2),(3,3),(0.,1.),(0.025590359613199,0.0375948596691636),
 .UNSPECIFIED.)
GEOMETRIC_REPRESENTATION_ITEM()
RATIONAL_B_SPLINE_SURFACE(((0.996753121756001,0.997505687613137,0.999678813023772),
(0.996753121756001,0.997505687613137,0.999678813023772)))
REPRESENTATION_ITEM('')
SURFACE()
);
#859=(
BOUNDED_SURFACE()
B_SPLINE_SURFACE(1,2,((#105161,#105162,#105163,#105164,#105165),(#105166,
#105167,#105168,#105169,#105170)),.UNSPECIFIED.,.F.,.F.,.F.)
B_SPLINE_SURFACE_WITH_KNOTS((2,2),(3,2,3),(0.519229702927906,1.),(0.0365944846644382,
0.0384615384615384,0.0431859278882051),.UNSPECIFIED.)
GEOMETRIC_REPRESENTATION_ITEM()
RATIONAL_B_SPLINE_SURFACE(((0.999326490452211,0.999646063968191,1.,0.999104400928889,
0.998428822114447),(0.999326490452211,0.999646063968191,1.,0.999104400928889,
0.998428822114447)))
REPRESENTATION_ITEM('')
SURFACE()
);
#860=(
BOUNDED_SURFACE()
B_SPLINE_SURFACE(1,2,((#105226,#105227,#105228),(#105229,#105230,#105231)),
 .UNSPECIFIED.,.F.,.F.,.F.)
B_SPLINE_SURFACE_WITH_KNOTS((2,2),(3,3),(0.,1.),(0.0456081671210052,0.0575989447818616),
 .UNSPECIFIED.)
GEOMETRIC_REPRESENTATION_ITEM()
RATIONAL_B_SPLINE_SURFACE(((0.997793907739636,0.996365558499691,0.996354522974128),
(0.997793907739636,0.996365558499691,0.996354522974128)))
REPRESENTATION_ITEM('')
SURFACE()
);
#861=(
BOUNDED_SURFACE()
B_SPLINE_SURFACE(1,2,((#105266,#105267,#105268),(#105269,#105270,#105271)),
 .UNSPECIFIED.,.F.,.F.,.F.)
B_SPLINE_SURFACE_WITH_KNOTS((2,2),(3,3),(0.,1.),(0.0556006976522447,0.0675888855446152),
 .UNSPECIFIED.)
GEOMETRIC_REPRESENTATION_ITEM()
RATIONAL_B_SPLINE_SURFACE(((0.996397562408177,0.996150386836003,0.997319912821417),
(0.996397562408177,0.996150386836003,0.997319912821417)))
REPRESENTATION_ITEM('')
SURFACE()
);
#862=(
BOUNDED_SURFACE()
B_SPLINE_SURFACE(1,2,((#105272,#105273,#105274),(#105275,#105276,#105277)),
 .UNSPECIFIED.,.F.,.F.,.F.)
B_SPLINE_SURFACE_WITH_KNOTS((2,2),(3,3),(0.,1.),(0.065744861928108,0.0758849574338236),
 .UNSPECIFIED.)
GEOMETRIC_REPRESENTATION_ITEM()
RATIONAL_B_SPLINE_SURFACE(((0.996993639757276,0.997798549146192,0.999617032345115),
(0.996993639757276,0.997798549146192,0.999617032345115)))
REPRESENTATION_ITEM('')
SURFACE()
);
#863=(
BOUNDED_SURFACE()
B_SPLINE_SURFACE(1,2,((#105352,#105353,#105354),(#105355,#105356,#105357)),
 .UNSPECIFIED.,.F.,.F.,.F.)
B_SPLINE_SURFACE_WITH_KNOTS((2,2),(3,3),(0.,1.),(0.00560769170938434,0.0176009697615923),
 .UNSPECIFIED.)
GEOMETRIC_REPRESENTATION_ITEM()
RATIONAL_B_SPLINE_SURFACE(((0.998183892106924,0.996573304252679,0.996380621268545),
(0.998183892106924,0.996573304252679,0.996380621268545)))
REPRESENTATION_ITEM('')
SURFACE()
);
#864=(
BOUNDED_SURFACE()
B_SPLINE_SURFACE(1,2,((#105442,#105443,#105444),(#105445,#105446,#105447)),
 .UNSPECIFIED.,.F.,.F.,.F.)
B_SPLINE_SURFACE_WITH_KNOTS((2,2),(3,3),(0.,1.),(0.0255903596132011,0.0375948596691667),
 .UNSPECIFIED.)
GEOMETRIC_REPRESENTATION_ITEM()
RATIONAL_B_SPLINE_SURFACE(((0.996753121756002,0.997505687613138,0.999678813023773),
(0.996753121756002,0.997505687613138,0.999678813023773)))
REPRESENTATION_ITEM('')
SURFACE()
);
#865=(
BOUNDED_SURFACE()
B_SPLINE_SURFACE(1,2,((#105465,#105466,#105467,#105468,#105469),(#105470,
#105471,#105472,#105473,#105474)),.UNSPECIFIED.,.F.,.F.,.F.)
B_SPLINE_SURFACE_WITH_KNOTS((2,2),(3,2,3),(0.519229702925083,1.),(0.0365944846644329,
0.0384615384615384,0.0431859278882006),.UNSPECIFIED.)
GEOMETRIC_REPRESENTATION_ITEM()
RATIONAL_B_SPLINE_SURFACE(((0.99932649045221,0.99964606396819,1.,0.99910440092889,
0.998428822114448),(0.99932649045221,0.99964606396819,1.,0.99910440092889,
0.998428822114448)))
REPRESENTATION_ITEM('')
SURFACE()
);
#866=(
BOUNDED_SURFACE()
B_SPLINE_SURFACE(1,2,((#105530,#105531,#105532),(#105533,#105534,#105535)),
 .UNSPECIFIED.,.F.,.F.,.F.)
B_SPLINE_SURFACE_WITH_KNOTS((2,2),(3,3),(0.,1.),(0.0456081671210051,0.0575989447818617),
 .UNSPECIFIED.)
GEOMETRIC_REPRESENTATION_ITEM()
RATIONAL_B_SPLINE_SURFACE(((0.997793907739636,0.996365558499691,0.996354522974128),
(0.997793907739636,0.996365558499691,0.996354522974128)))
REPRESENTATION_ITEM('')
SURFACE()
);
#867=(
BOUNDED_SURFACE()
B_SPLINE_SURFACE(1,2,((#105570,#105571,#105572),(#105573,#105574,#105575)),
 .UNSPECIFIED.,.F.,.F.,.F.)
B_SPLINE_SURFACE_WITH_KNOTS((2,2),(3,3),(0.,1.),(0.0556006976522446,0.0675888855446173),
 .UNSPECIFIED.)
GEOMETRIC_REPRESENTATION_ITEM()
RATIONAL_B_SPLINE_SURFACE(((0.996397562408177,0.996150386836003,0.997319912821418),
(0.996397562408177,0.996150386836003,0.997319912821418)))
REPRESENTATION_ITEM('')
SURFACE()
);
#868=(
BOUNDED_SURFACE()
B_SPLINE_SURFACE(1,2,((#105576,#105577,#105578),(#105579,#105580,#105581)),
 .UNSPECIFIED.,.F.,.F.,.F.)
B_SPLINE_SURFACE_WITH_KNOTS((2,2),(3,3),(0.,1.),(0.0657448619281101,0.0758849574338238),
 .UNSPECIFIED.)
GEOMETRIC_REPRESENTATION_ITEM()
RATIONAL_B_SPLINE_SURFACE(((0.996993639757276,0.997798549146193,0.999617032345115),
(0.996993639757276,0.997798549146193,0.999617032345115)))
REPRESENTATION_ITEM('')
SURFACE()
);
#869=(
BOUNDED_SURFACE()
B_SPLINE_SURFACE(1,2,((#105656,#105657,#105658),(#105659,#105660,#105661)),
 .UNSPECIFIED.,.F.,.F.,.F.)
B_SPLINE_SURFACE_WITH_KNOTS((2,2),(3,3),(0.,1.),(0.00560769170938528,0.0176009697615926),
 .UNSPECIFIED.)
GEOMETRIC_REPRESENTATION_ITEM()
RATIONAL_B_SPLINE_SURFACE(((0.998183892106923,0.996573304252679,0.996380621268545),
(0.998183892106923,0.996573304252679,0.996380621268545)))
REPRESENTATION_ITEM('')
SURFACE()
);
#870=(
BOUNDED_SURFACE()
B_SPLINE_SURFACE(1,2,((#105746,#105747,#105748),(#105749,#105750,#105751)),
 .UNSPECIFIED.,.F.,.F.,.F.)
B_SPLINE_SURFACE_WITH_KNOTS((2,2),(3,3),(0.,1.),(0.0255903596132,0.0375948596691668),
 .UNSPECIFIED.)
GEOMETRIC_REPRESENTATION_ITEM()
RATIONAL_B_SPLINE_SURFACE(((0.996753121756002,0.997505687613138,0.999678813023773),
(0.996753121756002,0.997505687613138,0.999678813023773)))
REPRESENTATION_ITEM('')
SURFACE()
);
#871=(
BOUNDED_SURFACE()
B_SPLINE_SURFACE(1,2,((#105769,#105770,#105771,#105772,#105773),(#105774,
#105775,#105776,#105777,#105778)),.UNSPECIFIED.,.F.,.F.,.F.)
B_SPLINE_SURFACE_WITH_KNOTS((2,2),(3,2,3),(0.5192297029227,1.),(0.0365944846644306,
0.0384615384615384,0.0431859276813022),.UNSPECIFIED.)
GEOMETRIC_REPRESENTATION_ITEM()
RATIONAL_B_SPLINE_SURFACE(((0.999326490452209,0.999646063968189,1.,0.999104400968112,
0.99842882217362),(0.999326490452208,0.999646063968189,1.,0.999104400968112,
0.99842882217362)))
REPRESENTATION_ITEM('')
SURFACE()
);
#872=(
BOUNDED_SURFACE()
B_SPLINE_SURFACE(1,2,((#105834,#105835,#105836),(#105837,#105838,#105839)),
 .UNSPECIFIED.,.F.,.F.,.F.)
B_SPLINE_SURFACE_WITH_KNOTS((2,2),(3,3),(0.,1.),(0.0456081671210065,0.0575989447818604),
 .UNSPECIFIED.)
GEOMETRIC_REPRESENTATION_ITEM()
RATIONAL_B_SPLINE_SURFACE(((0.997793907739636,0.996365558499691,0.996354522974128),
(0.997793907739636,0.996365558499691,0.996354522974128)))
REPRESENTATION_ITEM('')
SURFACE()
);
#873=(
BOUNDED_SURFACE()
B_SPLINE_SURFACE(1,2,((#105874,#105875,#105876),(#105877,#105878,#105879)),
 .UNSPECIFIED.,.F.,.F.,.F.)
B_SPLINE_SURFACE_WITH_KNOTS((2,2),(3,3),(0.,1.),(0.0556006976522425,0.0675888855446154),
 .UNSPECIFIED.)
GEOMETRIC_REPRESENTATION_ITEM()
RATIONAL_B_SPLINE_SURFACE(((0.996397562408177,0.996150386836003,0.997319912821417),
(0.996397562408177,0.996150386836003,0.997319912821417)))
REPRESENTATION_ITEM('')
SURFACE()
);
#874=(
BOUNDED_SURFACE()
B_SPLINE_SURFACE(1,2,((#105880,#105881,#105882),(#105883,#105884,#105885)),
 .UNSPECIFIED.,.F.,.F.,.F.)
B_SPLINE_SURFACE_WITH_KNOTS((2,2),(3,3),(0.,1.),(0.065744861928108,0.075884957433824),
 .UNSPECIFIED.)
GEOMETRIC_REPRESENTATION_ITEM()
RATIONAL_B_SPLINE_SURFACE(((0.996993639757276,0.997798549146192,0.999617032345115),
(0.996993639757276,0.997798549146192,0.999617032345115)))
REPRESENTATION_ITEM('')
SURFACE()
);
#875=(
BOUNDED_SURFACE()
B_SPLINE_SURFACE(1,2,((#105960,#105961,#105962),(#105963,#105964,#105965)),
 .UNSPECIFIED.,.F.,.F.,.F.)
B_SPLINE_SURFACE_WITH_KNOTS((2,2),(3,3),(0.,1.),(0.00560769170938643,0.0176009697615936),
 .UNSPECIFIED.)
GEOMETRIC_REPRESENTATION_ITEM()
RATIONAL_B_SPLINE_SURFACE(((0.998183892106923,0.996573304252679,0.996380621268545),
(0.998183892106923,0.996573304252679,0.996380621268545)))
REPRESENTATION_ITEM('')
SURFACE()
);
#876=(
BOUNDED_SURFACE()
B_SPLINE_SURFACE(1,2,((#106050,#106051,#106052),(#106053,#106054,#106055)),
 .UNSPECIFIED.,.F.,.F.,.F.)
B_SPLINE_SURFACE_WITH_KNOTS((2,2),(3,3),(0.,1.),(0.025590359613201,0.037594859669168),
 .UNSPECIFIED.)
GEOMETRIC_REPRESENTATION_ITEM()
RATIONAL_B_SPLINE_SURFACE(((0.996753121756002,0.997505687613138,0.999678813023774),
(0.996753121756002,0.997505687613138,0.999678813023774)))
REPRESENTATION_ITEM('')
SURFACE()
);
#877=(
BOUNDED_SURFACE()
B_SPLINE_SURFACE(1,2,((#106073,#106074,#106075,#106076,#106077),(#106078,
#106079,#106080,#106081,#106082)),.UNSPECIFIED.,.F.,.F.,.F.)
B_SPLINE_SURFACE_WITH_KNOTS((2,2),(3,2,3),(0.519229702919849,1.),(0.0365944846644282,
0.0384615384615384,0.043185927681299),.UNSPECIFIED.)
GEOMETRIC_REPRESENTATION_ITEM()
RATIONAL_B_SPLINE_SURFACE(((0.999326490452208,0.999646063968189,1.,0.999104400968112,
0.998428822173621),(0.999326490452208,0.999646063968189,1.,0.999104400968112,
0.998428822173621)))
REPRESENTATION_ITEM('')
SURFACE()
);
#878=(
BOUNDED_SURFACE()
B_SPLINE_SURFACE(1,2,((#106138,#106139,#106140),(#106141,#106142,#106143)),
 .UNSPECIFIED.,.F.,.F.,.F.)
B_SPLINE_SURFACE_WITH_KNOTS((2,2),(3,3),(0.,1.),(0.0456081671210094,0.0575989447818618),
 .UNSPECIFIED.)
GEOMETRIC_REPRESENTATION_ITEM()
RATIONAL_B_SPLINE_SURFACE(((0.997793907739635,0.996365558499691,0.996354522974128),
(0.997793907739635,0.996365558499691,0.996354522974128)))
REPRESENTATION_ITEM('')
SURFACE()
);
#879=(
BOUNDED_SURFACE()
B_SPLINE_SURFACE(1,2,((#106178,#106179,#106180),(#106181,#106182,#106183)),
 .UNSPECIFIED.,.F.,.F.,.F.)
B_SPLINE_SURFACE_WITH_KNOTS((2,2),(3,3),(0.,1.),(0.0556006976522459,0.067588885544616),
 .UNSPECIFIED.)
GEOMETRIC_REPRESENTATION_ITEM()
RATIONAL_B_SPLINE_SURFACE(((0.996397562408177,0.996150386836004,0.997319912821417),
(0.996397562408177,0.996150386836004,0.997319912821417)))
REPRESENTATION_ITEM('')
SURFACE()
);
#880=(
BOUNDED_SURFACE()
B_SPLINE_SURFACE(1,2,((#106184,#106185,#106186),(#106187,#106188,#106189)),
 .UNSPECIFIED.,.F.,.F.,.F.)
B_SPLINE_SURFACE_WITH_KNOTS((2,2),(3,3),(0.,1.),(0.0657448619281089,0.0758849574338248),
 .UNSPECIFIED.)
GEOMETRIC_REPRESENTATION_ITEM()
RATIONAL_B_SPLINE_SURFACE(((0.996993639757276,0.997798549146193,0.999617032345115),
(0.996993639757276,0.997798549146193,0.999617032345115)))
REPRESENTATION_ITEM('')
SURFACE()
);
#881=CONICAL_SURFACE('',#45721,0.006,0.78539816339745);
#882=CONICAL_SURFACE('',#45823,0.0055,0.78539816339746);
#883=CONICAL_SURFACE('',#50193,0.005875,0.694738276196703);
#884=ELLIPSE('',#45698,0.00800033336362062,0.00788400944250588);
#885=ELLIPSE('',#45699,0.00800033336362222,0.0078840094425091);
#886=ELLIPSE('',#46076,0.00505204240379114,0.00230472370237008);
#887=ELLIPSE('',#46082,0.00460880147227119,0.00192167872360598);
#888=ELLIPSE('',#46092,0.00865509473932915,0.00758557668119749);
#889=ELLIPSE('',#46180,0.00621516716548231,0.00601620425193647);
#890=ELLIPSE('',#46181,0.00648423822157093,0.00593239723153129);
#891=ELLIPSE('',#46187,0.0070905986611636,0.0012893204637363);
#892=ELLIPSE('',#46191,0.0050534643241034,0.00230601081969104);
#893=ELLIPSE('',#46202,0.00865512552606261,0.00758560652833544);
#894=ELLIPSE('',#46246,0.00621537602140178,0.00601630533451007);
#895=ELLIPSE('',#46247,0.00648435333080737,0.00593260142270717);
#896=ELLIPSE('',#46249,0.00709129851600952,0.00128949452168959);
#897=ELLIPSE('',#46252,0.00505210470082459,0.00230478008540994);
#898=ELLIPSE('',#46263,0.00865513528145594,0.00758561599623131);
#899=ELLIPSE('',#46307,0.00621524391851374,0.00601624139928821);
#900=ELLIPSE('',#46308,0.0064843122029582,0.00593252852474117);
#901=ELLIPSE('',#46310,0.00709039114265013,0.00128926885533352);
#902=ELLIPSE('',#46313,0.00505390723859556,0.00230641180953775);
#903=ELLIPSE('',#46324,0.00865509821766808,0.00758558009748805);
#904=ELLIPSE('',#46368,0.00621529545248987,0.00601626634096811);
#905=ELLIPSE('',#46369,0.0064843319772775,0.00593256359853056);
#906=ELLIPSE('',#46371,0.00709065821253241,0.0012893352089985);
#907=ELLIPSE('',#46374,0.0050890313490455,0.00233831897377822);
#908=ELLIPSE('',#46385,0.00865510845069279,0.00758559005407188);
#909=ELLIPSE('',#46429,0.00621534731034554,0.0060162914392953);
#910=ELLIPSE('',#46430,0.00648437887335218,0.00593264681892162);
#911=ELLIPSE('',#46432,0.00709002873922731,0.00128917846438477);
#912=ELLIPSE('',#46435,0.0050520856182914,0.00230476281589073);
#913=ELLIPSE('',#46446,0.00865511426296996,0.00758559562353494);
#914=ELLIPSE('',#46490,0.00621521803085549,0.00601622887006362);
#915=ELLIPSE('',#46491,0.00648442221515968,0.00593272364388297);
#916=ELLIPSE('',#46493,0.00709090319602856,0.00128939616487807);
#917=ELLIPSE('',#46496,0.00505269719487927,0.00230531637340278);
#918=ELLIPSE('',#46507,0.00865513573468569,0.00758561645123289);
#919=ELLIPSE('',#46551,0.00621526992760936,0.00601625398735536);
#920=ELLIPSE('',#46552,0.00648433724962787,0.00593257294843176);
#921=ELLIPSE('',#46554,0.00709023333512276,0.00128922949570934);
#922=ELLIPSE('',#46557,0.0050526446036089,0.00230526876880624);
#923=ELLIPSE('',#46568,0.00865513735985754,0.00758561798170201);
#924=ELLIPSE('',#46612,0.00621519248449229,0.00601621650592652);
#925=ELLIPSE('',#46613,0.00648435975442786,0.00593261285788805);
#926=ELLIPSE('',#46615,0.00709078687884672,0.00128936725092669);
#927=ELLIPSE('',#46618,0.00505218071000825,0.00230484888152921);
#928=ELLIPSE('',#46629,0.00865511153964906,0.0075855930117702);
#929=ELLIPSE('',#46673,0.00621521819686636,0.00601622895043552);
#930=ELLIPSE('',#46674,0.00648435621900189,0.0059326065851825);
#931=ELLIPSE('',#46676,0.00709157095271754,0.00128956239099297);
#932=ELLIPSE('',#46679,0.00505287260556312,0.00230547515433253);
#933=ELLIPSE('',#46690,0.00865512124916736,0.00758560240185387);
#934=ELLIPSE('',#46734,0.00621534747320918,0.00601629151811313);
#935=ELLIPSE('',#46735,0.00648436926222662,0.00593262969405175);
#936=ELLIPSE('',#46737,0.00709121156280895,0.00128947288156415);
#937=ELLIPSE('',#46740,0.00505234254805064,0.00230499536293981);
#938=ELLIPSE('',#46751,0.00865510577377427,0.00758558737369668);
#939=ELLIPSE('',#46795,0.0062152056610705,0.00601622288331262);
#940=ELLIPSE('',#46796,0.00648437614788083,0.00593264193050572);
#941=ELLIPSE('',#46798,0.00709079551933392,0.00128936945124519);
#942=ELLIPSE('',#46801,0.00505308063550296,0.00230566346961813);
#943=ELLIPSE('',#46812,0.00865516464328738,0.00758564444626258);
#944=ELLIPSE('',#46856,0.00621525717507994,0.00601624781537191);
#945=ELLIPSE('',#46857,0.00648435399756577,0.00593260264617468);
#946=ELLIPSE('',#46859,0.00709125807572499,0.00128948456247621);
#947=ELLIPSE('',#46862,0.00505407572626888,0.00230656436075209);
#948=ELLIPSE('',#46873,0.00865507611239517,0.00758555855456918);
#949=ELLIPSE('',#46917,0.00621529569567966,0.00601626645859758);
#950=ELLIPSE('',#46918,0.00648434122881266,0.00593257999422627);
#951=ELLIPSE('',#46920,0.00709052630964259,0.00128930239034199);
#952=ELLIPSE('',#46923,0.00505216738260241,0.00230483681883502);
#953=ELLIPSE('',#46934,0.0086551013472187,0.00758558314017204);
#954=ELLIPSE('',#46978,0.00621523480011978,0.0060162369862471);
#955=ELLIPSE('',#46979,0.00648435210818557,0.00593259930385406);
#956=ELLIPSE('',#46981,0.00709110677776559,0.0012894465833154);
#957=ELLIPSE('',#46984,0.00505386286247069,0.00230637163389658);
#958=ELLIPSE('',#46995,0.00865508082772966,0.00758556319306449);
#959=ELLIPSE('',#47039,0.00621524583016535,0.00601624232453474);
#960=ELLIPSE('',#47040,0.00648433993340202,0.00593257769459382);
#961=ELLIPSE('',#47042,0.00709064233112991,0.0012893311074234);
#962=ELLIPSE('',#47045,0.00497700215010779,0.00223729133900348);
#963=ELLIPSE('',#47056,0.0086551050322695,0.00758558656708154);
#964=ELLIPSE('',#47100,0.00621523774150067,0.0060162384097202);
#965=ELLIPSE('',#47101,0.0064843246995372,0.00593255066143694);
#966=ELLIPSE('',#47103,0.00709045075792868,0.00128928348314944);
#967=ELLIPSE('',#47106,0.0049942788104379,0.00225273055972324);
#968=ELLIPSE('',#47117,0.00865514878432738,0.00758562908741592);
#969=ELLIPSE('',#47161,0.00621525709474776,0.00601624777632549);
#970=ELLIPSE('',#47162,0.00648435246172703,0.00593259993727655);
#971=ELLIPSE('',#47164,0.00709029022462916,0.00128924346647885);
#972=ELLIPSE('',#47167,0.00505405294220357,0.00230654373401579);
#973=ELLIPSE('',#47178,0.00865514566750678,0.00758562601058983);
#974=ELLIPSE('',#47222,0.00621520533038221,0.00601622272323379);
#975=ELLIPSE('',#47223,0.00648434821407422,0.00593259239188297);
#976=ELLIPSE('',#47225,0.00709096491369054,0.00128941161665014);
#977=ELLIPSE('',#47228,0.00505353081443679,0.00230607101122026);
#978=ELLIPSE('',#47239,0.00865505354911252,0.00758553677638153);
#979=ELLIPSE('',#47283,0.00621527010598489,0.00601625407364374);
#980=ELLIPSE('',#47284,0.00648438806646418,0.00593266310364782);
#981=ELLIPSE('',#47286,0.00709071191997087,0.0012893485270995);
#982=ELLIPSE('',#47289,0.00505346384021596,0.00230601037853248);
#983=ELLIPSE('',#47300,0.00865510202610495,0.00758558385576672);
#984=ELLIPSE('',#47344,0.00621524420609326,0.00601624153854915);
#985=ELLIPSE('',#47345,0.00648436364018349,0.00593261972706044);
#986=ELLIPSE('',#47347,0.00709069660148338,0.0012893447619227);
#987=ELLIPSE('',#47350,0.00505505780866651,0.00230745364042269);
#988=ELLIPSE('',#47361,0.00865515793670053,0.0075856380555555);
#989=ELLIPSE('',#47405,0.00621521863585752,0.00601622916295315);
#990=ELLIPSE('',#47406,0.00648436189412657,0.0059326166804513);
#991=ELLIPSE('',#47408,0.00709088846227213,0.00128939245022837);
#992=ELLIPSE('',#47411,0.00504563136550804,0.00229892492076941);
#993=ELLIPSE('',#47422,0.00865510725747081,0.00758558883147086);
#994=ELLIPSE('',#47466,0.00621519257981388,0.00601621655201505);
#995=ELLIPSE('',#47467,0.0064843435728204,0.00593258411188729);
#996=ELLIPSE('',#47469,0.00709119685945131,0.00128946934905443);
#997=ELLIPSE('',#47472,0.00505391488108627,0.00230641873073941);
#998=ELLIPSE('',#47483,0.00865515520019524,0.00758563531672948);
#999=ELLIPSE('',#47527,0.00621537347876877,0.00601630410400769);
#1000=ELLIPSE('',#47528,0.0064843388243652,0.00593257571394916);
#1001=ELLIPSE('',#47530,0.00709076450352905,0.00128936161857139);
#1002=ELLIPSE('',#47533,0.005053948238314,0.00230644893380194);
#1003=ELLIPSE('',#47544,0.00865509653169551,0.00758557854237256);
#1004=ELLIPSE('',#47588,0.00621514106793808,0.00601619162089527);
#1005=ELLIPSE('',#47589,0.00648424807037612,0.00593241469410971);
#1006=ELLIPSE('',#47591,0.00709079105844187,0.00128936836893104);
#1007=ELLIPSE('',#47594,0.00505231057978,0.00230496642628584);
#1008=ELLIPSE('',#47605,0.00865508149523495,0.00758556383848639);
#1009=ELLIPSE('',#47649,0.00621539900993303,0.00601631646068148);
#1010=ELLIPSE('',#47650,0.00648433706096967,0.00593257260494097);
#1011=ELLIPSE('',#47652,0.00709114959659087,0.0012894575414131);
#1012=ELLIPSE('',#47655,0.00505417128153103,0.00230665088079652);
#1013=ELLIPSE('',#47666,0.00865512007154011,0.00758560124867166);
#1014=ELLIPSE('',#47710,0.0062153221253105,0.00601627925005241);
#1015=ELLIPSE('',#47711,0.00648437107278222,0.00593263291279239);
#1016=ELLIPSE('',#47713,0.00709055276537754,0.00128930892171807);
#1017=ELLIPSE('',#47716,0.00504571052979579,0.00229899647725242);
#1018=ELLIPSE('',#47727,0.00865515831542652,0.00758563843237898);
#1019=ELLIPSE('',#47771,0.00621504059289944,0.00601614299178234);
#1020=ELLIPSE('',#47772,0.00648435366732346,0.00593260206262849);
#1021=ELLIPSE('',#47774,0.00709067179251568,0.00128933848534169);
#1022=ELLIPSE('',#47777,0.0049748455941374,0.00223536775184007);
#1023=ELLIPSE('',#47788,0.00865512077413154,0.00758560196280287);
#1024=ELLIPSE('',#47832,0.00621529596421664,0.00601626658841289);
#1025=ELLIPSE('',#47833,0.00648438623642478,0.00593265985810756);
#1026=ELLIPSE('',#47835,0.0070908495799914,0.00128938276638011);
#1027=ELLIPSE('',#47838,0.00498598901432705,0.00224531598960363);
#1028=ELLIPSE('',#47849,0.00865514380798239,0.00758562431463873);
#1029=ELLIPSE('',#47893,0.00621521820687037,0.00601622895494);
#1030=ELLIPSE('',#47894,0.00648432613400307,0.00593255322684216);
#1031=ELLIPSE('',#47896,0.00709071216078011,0.00128934845297877);
#1032=ELLIPSE('',#47899,0.00505220961919958,0.00230487504732119);
#1033=ELLIPSE('',#47910,0.00865515886241701,0.00758563894485504);
#1034=ELLIPSE('',#47954,0.00621539897200116,0.00601631644192197);
#1035=ELLIPSE('',#47955,0.00648429433668458,0.00593249679273564);
#1036=ELLIPSE('',#47957,0.00709092653210478,0.00128940198033132);
#1037=ELLIPSE('',#47960,0.00505363409789085,0.00230616451930728);
#1038=ELLIPSE('',#47971,0.00865511993115791,0.00758560120699035);
#1039=ELLIPSE('',#48015,0.00621534716993814,0.00601629137100437);
#1040=ELLIPSE('',#48016,0.00648432509643861,0.0059325513838022);
#1041=ELLIPSE('',#48018,0.0070912200594845,0.00128947495864189);
#1042=ELLIPSE('',#48021,0.00505222431865997,0.00230488835088698);
#1043=ELLIPSE('',#48032,0.00865506890500387,0.00758555170092938);
#1044=ELLIPSE('',#48076,0.00621514063419339,0.00601619141091768);
#1045=ELLIPSE('',#48077,0.00648435306981849,0.00593260099471013);
#1046=ELLIPSE('',#48079,0.00709071025182221,0.00128934820887216);
#1047=ELLIPSE('',#48082,0.00505327809031931,0.00230584221748581);
#1048=ELLIPSE('',#48093,0.00865515228595944,0.00758563259983201);
#1049=ELLIPSE('',#48137,0.00621534746386843,0.00601629151335203);
#1050=ELLIPSE('',#48138,0.00648433641997979,0.00593257147747394);
#1051=ELLIPSE('',#48140,0.00709090941811193,0.00128939770831554);
#1052=ELLIPSE('',#48143,0.00505253275184091,0.00230516752406919);
#1053=ELLIPSE('',#48154,0.00865507528679423,0.00758555773898941);
#1054=ELLIPSE('',#48198,0.00621533449362357,0.00601628523588446);
#1055=ELLIPSE('',#48199,0.00648433275812308,0.0059325649596866);
#1056=ELLIPSE('',#48201,0.00709058807553439,0.00128931769610372);
#1057=ELLIPSE('',#48204,0.00505264582740208,0.00230526987582819);
#1058=ELLIPSE('',#48215,0.00865516225075192,0.00758564219542599);
#1059=ELLIPSE('',#48259,0.00621532149524689,0.00601627894494369);
#1060=ELLIPSE('',#48260,0.00648439073664356,0.00593266783283331);
#1061=ELLIPSE('',#48262,0.00709118291446364,0.00128946573593998);
#1062=ELLIPSE('',#48265,0.00505239964645357,0.00230504704486186);
#1063=ELLIPSE('',#48276,0.0086550935418262,0.00758557553418211);
#1064=ELLIPSE('',#48320,0.00621523121561208,0.00601623525106577);
#1065=ELLIPSE('',#48321,0.0064843641048612,0.00593262058267339);
#1066=ELLIPSE('',#48323,0.00709104236502589,0.00128943077820424);
#1067=ELLIPSE('',#48326,0.0050525425659858,0.0023051764069886);
#1068=ELLIPSE('',#48337,0.00865508682964421,0.00758556902181305);
#1069=ELLIPSE('',#48381,0.00621523116343429,0.00601623522580888);
#1070=ELLIPSE('',#48382,0.0064843477615119,0.00593259158809656);
#1071=ELLIPSE('',#48384,0.00709066162127243,0.0012893359428282);
#1072=ELLIPSE('',#48387,0.00498500862158727,0.00224443989119654);
#1073=ELLIPSE('',#48398,0.00865510656953884,0.00758558822009033);
#1074=ELLIPSE('',#48442,0.00621517946931786,0.0060162102065265);
#1075=ELLIPSE('',#48443,0.00648435291446554,0.00593260071268177);
#1076=ELLIPSE('',#48445,0.00709069939164397,0.00128934538239027);
#1077=ELLIPSE('',#48448,0.00505387585032357,0.00230638339351009);
#1078=ELLIPSE('',#48459,0.00865517106043899,0.00758565079628095);
#1079=ELLIPSE('',#48503,0.00621524417632009,0.00601624152393858);
#1080=ELLIPSE('',#48504,0.00648433396300445,0.00593256709201826);
#1081=ELLIPSE('',#48506,0.00709056942096103,0.00128931313168986);
#1082=ELLIPSE('',#48509,0.00505243006869415,0.00230507457996915);
#1083=ELLIPSE('',#48520,0.00865518739164197,0.00758566662396141);
#1084=ELLIPSE('',#48564,0.00621526384282503,0.00601625104227291);
#1085=ELLIPSE('',#48565,0.00648434251869749,0.00593258228049829);
#1086=ELLIPSE('',#48567,0.00709045845399877,0.00128928544995619);
#1087=ELLIPSE('',#48570,0.00505342198852363,0.00230597248826897);
#1088=ELLIPSE('',#48581,0.00865509832858885,0.00758558021126826);
#1089=ELLIPSE('',#48625,0.00621520544883468,0.00601622278028145);
#1090=ELLIPSE('',#48626,0.00648436223366202,0.00593261726583697);
#1091=ELLIPSE('',#48628,0.00709066606273037,0.0012893371910688);
#1092=ELLIPSE('',#48631,0.00505290596600244,0.00230550535243315);
#1093=ELLIPSE('',#48642,0.00865511613860218,0.00758559749223903);
#1094=ELLIPSE('',#48686,0.00621524420773405,0.0060162415391342);
#1095=ELLIPSE('',#48687,0.00648436382412113,0.00593262008351636);
#1096=ELLIPSE('',#48689,0.00709084298865159,0.00128938119659501);
#1097=ELLIPSE('',#48692,0.00505273138252932,0.00230534731942932);
#1098=ELLIPSE('',#48703,0.00865515121971655,0.00758563144244627);
#1099=ELLIPSE('',#48747,0.00621534729708559,0.00601629143262738);
#1100=ELLIPSE('',#48748,0.00648437791316611,0.0059326450846128);
#1101=ELLIPSE('',#48750,0.00709077396930198,0.00128936401951887);
#1102=ELLIPSE('',#48758,0.0050525152800079,0.00230515170877071);
#1103=ELLIPSE('',#48764,0.00865510594678074,0.00758558765394751);
#1104=ELLIPSE('',#48808,0.00621537342646163,0.00601630407875128);
#1105=ELLIPSE('',#48809,0.00648430341187163,0.00593251290911168);
#1106=ELLIPSE('',#48811,0.00709066882204238,0.00128933789968135);
#1107=ELLIPSE('',#48824,0.00505237134147902,0.0023050214260488);
#1108=ELLIPSE('',#48830,0.00865513889575835,0.00758561962224155);
#1109=ELLIPSE('',#48869,0.00621527020298751,0.00601625412034941);
#1110=ELLIPSE('',#48870,0.00648435578149643,0.00593260581661072);
#1111=ELLIPSE('',#48872,0.00709059988545386,0.00128932076398224);
#1112=ELLIPSE('',#48893,0.00865512097604794,0.00758560212593767);
#1113=ELLIPSE('',#48902,0.00460921634661896,0.00192202285706926);
#1114=ELLIPSE('',#48930,0.00621514084277246,0.00601619151211962);
#1115=ELLIPSE('',#48931,0.0064843629627248,0.00593261855117462);
#1116=ELLIPSE('',#48933,0.00709081214989054,0.00128937362404988);
#1117=ELLIPSE('',#48965,0.00461178042656441,0.00192415041839508);
#1118=ELLIPSE('',#48971,0.00865515359670422,0.00758563388640994);
#1119=ELLIPSE('',#48991,0.00621526986242424,0.0060162539556225);
#1120=ELLIPSE('',#48992,0.00648432994839084,0.00593255998262295);
#1121=ELLIPSE('',#48994,0.00709045362965754,0.00128928441829338);
#1122=ELLIPSE('',#49031,0.00505250516664137,0.00230514255651931);
#1123=ELLIPSE('',#49037,0.00865516221802523,0.00758564206595745);
#1124=ELLIPSE('',#49052,0.00621521875625456,0.00601622922104769);
#1125=ELLIPSE('',#49053,0.0064843251186602,0.00593255145155149);
#1126=ELLIPSE('',#49055,0.00709092921434546,0.00128940267805035);
#1127=ELLIPSE('',#49099,0.00460883271893841,0.00192170463706111);
#1128=ELLIPSE('',#49105,0.00865514794548704,0.00758562834632257);
#1129=ELLIPSE('',#49113,0.00621529595082828,0.00601626658192771);
#1130=ELLIPSE('',#49114,0.00648438224890444,0.00593265271232124);
#1131=ELLIPSE('',#49116,0.00709044419804569,0.00128928198746711);
#1132=ELLIPSE('',#49118,0.00621547662594353,0.00601635402501883);
#1133=ELLIPSE('',#49119,0.00648431602834799,0.00593253527427483);
#1134=ELLIPSE('',#49121,0.00709091596384868,0.00128939945197051);
#1135=ELLIPSE('',#49123,0.00865512107813427,0.00758560229656082);
#1136=TOROIDAL_SURFACE('',#45672,0.001,0.0005);
#1137=B_SPLINE_CURVE_WITH_KNOTS('',3,(#63074,#63075,#63076,#63077,#63078,
#63079,#63080,#63081,#63082,#63083,#63084,#63085,#63086,#63087,#63088,#63089,
#63090,#63091,#63092,#63093,#63094,#63095,#63096,#63097,#63098,#63099,#63100,
#63101,#63102,#63103,#63104,#63105,#63106,#63107,#63108,#63109,#63110,#63111,
#63112,#63113,#63114,#63115,#63116,#63117,#63118,#63119,#63120,#63121,#63122,
#63123,#63124,#63125,#63126,#63127,#63128,#63129,#63130,#63131,#63132,#63133,
#63134,#63135,#63136,#63137,#63138,#63139,#63140,#63141,#63142,#63143,#63144,
#63145,#63146,#63147,#63148,#63149,#63150,#63151,#63152,#63153,#63154,#63155,
#63156),.UNSPECIFIED.,.T.,.F.,(4,2,2,2,2,2,2,2,2,2,2,2,3,2,2,2,2,2,2,2,
2,2,2,2,2,2,2,2,2,2,2,2,2,2,2,2,2,2,2,2,4),(-0.599947803193285,-0.598210079042782,
-0.595023554691837,-0.589519553668659,-0.577119648198067,-0.557048780033889,
-0.513453225651634,-0.469622814326577,-0.408953064788174,-0.324588709422408,
-0.21162571525016,-0.096634471246167,0.,0.0616122332173725,0.106433599409592,
0.154580821050161,0.198356973080929,0.2347927451485,0.252280410989761,0.259282926921628,
0.262487356696865,0.264544192713024,0.266469924405381,0.268877657633077,
0.272576047854324,0.281287606126543,0.323717973586198,0.361493711229503,
0.406553787309279,0.452201240933876,0.498262558787684,0.554089254539195,
0.609870344197402,0.658248710788607,0.705297953991042,0.768328967391763,
0.788964957538382,0.796607886518312,0.800333694334371,0.802819259400907,
0.803509190912599),.UNSPECIFIED.);
#1138=B_SPLINE_CURVE_WITH_KNOTS('',3,(#63158,#63159,#63160,#63161,#63162,
#63163,#63164,#63165,#63166,#63167,#63168,#63169,#63170,#63171,#63172,#63173,
#63174,#63175,#63176,#63177,#63178,#63179,#63180,#63181,#63182,#63183,#63184,
#63185,#63186,#63187,#63188,#63189,#63190,#63191,#63192,#63193,#63194,#63195,
#63196,#63197,#63198,#63199,#63200,#63201,#63202,#63203,#63204,#63205,#63206,
#63207,#63208,#63209,#63210,#63211,#63212,#63213,#63214,#63215,#63216,#63217,
#63218,#63219,#63220,#63221,#63222,#63223,#63224,#63225,#63226,#63227,#63228,
#63229,#63230,#63231,#63232,#63233,#63234,#63235,#63236,#63237,#63238,#63239,
#63240,#63241,#63242,#63243,#63244,#63245,#63246,#63247,#63248,#63249,#63250,
#63251,#63252,#63253,#63254,#63255,#63256,#63257,#63258,#63259,#63260,#63261,
#63262,#63263,#63264,#63265,#63266,#63267,#63268,#63269,#63270,#63271,#63272,
#63273),.UNSPECIFIED.,.F.,.F.,(4,2,2,2,2,2,2,2,2,2,2,2,2,2,2,2,2,2,2,2,
2,2,2,2,2,2,2,2,2,2,2,2,2,2,2,2,2,2,2,2,2,2,2,2,2,2,2,2,2,2,2,2,2,2,2,2,
2,4),(-0.961745163027192,-0.959551497797208,-0.949439372246509,-0.939327246695811,
-0.929215121145113,-0.919102995594415,-0.90600602698209,-0.892909058369764,
-0.879812089757439,-0.866715121145113,-0.853618152532788,-0.840521183920462,
-0.827424215308137,-0.814327246695811,-0.801230278083486,-0.78813330947116,
-0.775036340858835,-0.761939372246509,-0.748842403634184,-0.735745435021858,
-0.722648466409533,-0.709551497797208,-0.696454529184882,-0.683357560572557,
-0.670260591960231,-0.657163623347906,-0.630969686123255,-0.604775748898604,
-0.578581811673953,-0.552387874449302,-0.526193937224651,-0.5,-0.484375,
-0.46875,-0.453125,-0.4375,-0.421875,-0.40625,-0.390625,-0.375,-0.359375,
-0.34375,-0.328125,-0.3125,-0.296875,-0.28125,-0.265625,-0.25,-0.234375,
-0.21875,-0.203125,-0.1875,-0.171875,-0.15625,-0.140625,-0.125,-0.109375,
-0.0989179337808057),.UNSPECIFIED.);
#1139=B_SPLINE_CURVE_WITH_KNOTS('',3,(#63275,#63276,#63277,#63278,#63279,
#63280,#63281,#63282,#63283,#63284,#63285,#63286,#63287,#63288,#63289,#63290,
#63291,#63292,#63293,#63294,#63295,#63296,#63297,#63298,#63299,#63300,#63301,
#63302,#63303,#63304,#63305,#63306,#63307,#63308,#63309,#63310,#63311,#63312,
#63313,#63314,#63315,#63316,#63317,#63318,#63319,#63320),.UNSPECIFIED.,
 .F.,.F.,(4,2,2,2,2,2,2,2,2,2,2,2,2,2,2,2,2,2,2,2,2,2,4),(-0.312874562310564,
-0.312343318679824,-0.311777586933697,-0.310438784231193,-0.306394877451961,
-0.293785182499551,-0.270387674138583,-0.246836971206823,-0.225592982310943,
-0.204563523252551,-0.183676969037245,-0.162538995601613,-0.140338814786806,
-0.119352240670363,-0.0971458868601155,-0.0708223711118798,-0.0453771530160624,
-0.0210971413466181,-0.00826159404632588,-0.00338196220690753,-0.00156167910744416,
-0.000763386858963189,-1.00001651581749E-6),.UNSPECIFIED.);
#1140=B_SPLINE_CURVE_WITH_KNOTS('',3,(#63321,#63322,#63323,#63324,#63325,
#63326,#63327,#63328,#63329,#63330,#63331,#63332,#63333,#63334,#63335,#63336,
#63337,#63338,#63339,#63340,#63341,#63342,#63343,#63344,#63345,#63346,#63347,
#63348,#63349,#63350,#63351,#63352,#63353,#63354,#63355,#63356,#63357,#63358,
#63359,#63360,#63361,#63362),.UNSPECIFIED.,.F.,.F.,(4,2,2,2,2,2,2,2,2,2,
2,2,2,2,2,2,2,2,2,2,4),(-0.324422676430501,-0.322867183051822,-0.321207977750209,
-0.317288633341995,-0.30789162270818,-0.28791232922133,-0.250322309326329,
-0.219033304596212,-0.190889649268595,-0.159649528873206,-0.130027804319714,
-0.101827459859418,-0.0752726588112276,-0.0561355587291201,-0.0422771346435577,
-0.0237288423555526,-0.01099220502612,-0.00489383549143937,-0.00219752038096737,
-0.00104712084043852,-1.00002643327324E-6),.UNSPECIFIED.);
#1141=B_SPLINE_CURVE_WITH_KNOTS('',3,(#63387,#63388,#63389,#63390,#63391,
#63392,#63393,#63394,#63395,#63396,#63397,#63398,#63399,#63400,#63401,#63402,
#63403,#63404,#63405,#63406,#63407,#63408,#63409,#63410,#63411,#63412,#63413),
 .UNSPECIFIED.,.F.,.F.,(4,3,2,2,2,2,2,2,2,2,2,2,4),(-0.0542367397696986,
0.,0.0558778999014289,0.111755799802858,0.16455192751495,0.212643516719156,
0.260735105923363,0.308826695127569,0.356918284331776,0.409714412043867,
0.465592311945296,0.521470211846725,0.575706951616422),.UNSPECIFIED.);
#1142=B_SPLINE_CURVE_WITH_KNOTS('',3,(#63532,#63533,#63534,#63535,#63536,
#63537),.UNSPECIFIED.,.F.,.F.,(4,2,4),(0.00611332411698155,0.00920174751816869,
0.0184034950186372),.UNSPECIFIED.);
#1143=B_SPLINE_CURVE_WITH_KNOTS('',3,(#63542,#63543,#63544,#63545),
 .UNSPECIFIED.,.F.,.F.,(4,4),(0.,0.00611332411698155),.UNSPECIFIED.);
#1144=B_SPLINE_CURVE_WITH_KNOTS('',3,(#63551,#63552,#63553,#63554,#63555,
#63556),.UNSPECIFIED.,.F.,.F.,(4,2,4),(-0.0184046527946452,-0.00920271228272339,
-9.99999999399051E-7),.UNSPECIFIED.);
#1145=B_SPLINE_CURVE_WITH_KNOTS('',3,(#63558,#63559,#63560,#63561,#63562,
#63563),.UNSPECIFIED.,.F.,.F.,(4,2,4),(-0.0184034950181132,-0.00920121908066632,
0.),.UNSPECIFIED.);
#1146=B_SPLINE_CURVE_WITH_KNOTS('',3,(#63569,#63570,#63571,#63572,#63573,
#63574),.UNSPECIFIED.,.F.,.F.,(4,2,4),(-0.0184046552084519,-0.00920271305813145,
-9.99999998350369E-7),.UNSPECIFIED.);
#1147=B_SPLINE_CURVE_WITH_KNOTS('',3,(#63576,#63577,#63578,#63579,#63580,
#63581),.UNSPECIFIED.,.F.,.F.,(4,2,4),(-0.0184034950162585,-0.00920171905417117,
0.),.UNSPECIFIED.);
#1148=B_SPLINE_CURVE_WITH_KNOTS('',3,(#63587,#63588,#63589,#63590,#63591,
#63592),.UNSPECIFIED.,.F.,.F.,(4,2,4),(-0.0184046525439867,-0.00920271218195336,
-9.99999998588597E-7),.UNSPECIFIED.);
#1149=B_SPLINE_CURVE_WITH_KNOTS('',3,(#63594,#63595,#63596,#63597,#63598,
#63599),.UNSPECIFIED.,.F.,.F.,(4,2,4),(-0.0184034950137807,-0.0092012190782782,
0.),.UNSPECIFIED.);
#1150=B_SPLINE_CURVE_WITH_KNOTS('',3,(#63605,#63606,#63607,#63608,#63609,
#63610),.UNSPECIFIED.,.F.,.F.,(4,2,4),(-0.0184046538139259,-0.0092027126177381,
-9.99999998292297E-7),.UNSPECIFIED.);
#1151=B_SPLINE_CURVE_WITH_KNOTS('',3,(#63612,#63613,#63614,#63615,#63616,
#63617),.UNSPECIFIED.,.F.,.F.,(4,2,4),(-0.0184034922219404,-0.00920171720053826,
0.),.UNSPECIFIED.);
#1152=B_SPLINE_CURVE_WITH_KNOTS('',3,(#63623,#63624,#63625,#63626,#63627,
#63628),.UNSPECIFIED.,.F.,.F.,(4,2,4),(-0.0184046552625379,-0.00920321307301659,
-9.99999997544632E-7),.UNSPECIFIED.);
#1153=B_SPLINE_CURVE_WITH_KNOTS('',3,(#63630,#63631,#63632,#63633,#63634,
#63635),.UNSPECIFIED.,.F.,.F.,(4,2,4),(-0.0184034934971486,-0.00920171804671571,
0.),.UNSPECIFIED.);
#1154=B_SPLINE_CURVE_WITH_KNOTS('',3,(#63641,#63642,#63643,#63644,#63645,
#63646),.UNSPECIFIED.,.F.,.F.,(4,2,4),(-0.0184046527956429,-0.00920271228294938,
-9.9999999874853E-7),.UNSPECIFIED.);
#1155=B_SPLINE_CURVE_WITH_KNOTS('',3,(#63648,#63649,#63650,#63651,#63652,
#63653),.UNSPECIFIED.,.F.,.F.,(4,2,4),(-0.0184034934960222,-0.00920121807191662,
0.),.UNSPECIFIED.);
#1156=B_SPLINE_CURVE_WITH_KNOTS('',3,(#63659,#63660,#63661,#63662,#63663,
#63664),.UNSPECIFIED.,.F.,.F.,(4,2,4),(-0.0184046552623352,-0.00920321307304284,
-9.99999995192347E-7),.UNSPECIFIED.);
#1157=B_SPLINE_CURVE_WITH_KNOTS('',3,(#63666,#63667,#63668,#63669,#63670,
#63671),.UNSPECIFIED.,.F.,.F.,(4,2,4),(-0.0184034950209319,-0.00920171905609732,
0.),.UNSPECIFIED.);
#1158=B_SPLINE_CURVE_WITH_KNOTS('',3,(#63677,#63678,#63679,#63680,#63681,
#63682),.UNSPECIFIED.,.F.,.F.,(4,2,4),(-0.0184046552624292,-0.00920321307301334,
-9.99999998405054E-7),.UNSPECIFIED.);
#1159=B_SPLINE_CURVE_WITH_KNOTS('',3,(#63684,#63685,#63686,#63687,#63688,
#63689),.UNSPECIFIED.,.F.,.F.,(4,2,4),(-0.0184034922316533,-0.00920121723059212,
0.),.UNSPECIFIED.);
#1160=B_SPLINE_CURVE_WITH_KNOTS('',3,(#63695,#63696,#63697,#63698,#63699,
#63700),.UNSPECIFIED.,.F.,.F.,(4,2,4),(-0.0184046538159848,-0.00920321259746976,
-9.99999995355411E-7),.UNSPECIFIED.);
#1161=B_SPLINE_CURVE_WITH_KNOTS('',3,(#63702,#63703,#63704,#63705,#63706,
#63707),.UNSPECIFIED.,.F.,.F.,(4,2,4),(-0.0184034935073226,-0.00920121807649925,
0.),.UNSPECIFIED.);
#1162=B_SPLINE_CURVE_WITH_KNOTS('',3,(#63713,#63714,#63715,#63716,#63717,
#63718),.UNSPECIFIED.,.F.,.F.,(4,2,4),(-0.0184046538140245,-0.00920321259680655,
-9.99999999765078E-7),.UNSPECIFIED.);
#1163=B_SPLINE_CURVE_WITH_KNOTS('',3,(#63720,#63721,#63722,#63723,#63724,
#63725),.UNSPECIFIED.,.F.,.F.,(4,2,4),(-0.0184034922241276,-0.0092017172013849,
0.),.UNSPECIFIED.);
#1164=B_SPLINE_CURVE_WITH_KNOTS('',3,(#63731,#63732,#63733,#63734,#63735,
#63736),.UNSPECIFIED.,.F.,.F.,(4,2,4),(-0.0184046552624612,-0.009203213073035,
-9.99999994151513E-7),.UNSPECIFIED.);
#1165=B_SPLINE_CURVE_WITH_KNOTS('',3,(#63738,#63739,#63740,#63741,#63742,
#63743),.UNSPECIFIED.,.F.,.F.,(4,2,4),(-0.018403495013842,-0.00920171905315888,
0.),.UNSPECIFIED.);
#1166=B_SPLINE_CURVE_WITH_KNOTS('',3,(#63749,#63750,#63751,#63752,#63753,
#63754),.UNSPECIFIED.,.F.,.F.,(4,2,4),(-0.0184046538158014,-0.00920321259735261,
-9.99999998127499E-7),.UNSPECIFIED.);
#1167=B_SPLINE_CURVE_WITH_KNOTS('',3,(#63756,#63757,#63758,#63759,#63760,
#63761),.UNSPECIFIED.,.F.,.F.,(4,2,4),(-0.0184034935026953,-0.00920121807403472,
0.),.UNSPECIFIED.);
#1168=B_SPLINE_CURVE_WITH_KNOTS('',3,(#63767,#63768,#63769,#63770,#63771,
#63772),.UNSPECIFIED.,.F.,.F.,(4,2,4),(-0.018404655262374,-0.00920271309393877,
-1.00000000437944E-6),.UNSPECIFIED.);
#1169=B_SPLINE_CURVE_WITH_KNOTS('',3,(#63774,#63775,#63776,#63777,#63778,
#63779),.UNSPECIFIED.,.F.,.F.,(4,2,4),(-0.0184034922298959,-0.00920171720445481,
0.),.UNSPECIFIED.);
#1170=B_SPLINE_CURVE_WITH_KNOTS('',3,(#63785,#63786,#63787,#63788,#63789,
#63790),.UNSPECIFIED.,.F.,.F.,(4,2,4),(-0.0184046538164437,-0.00920321259763748,
-9.99999998085865E-7),.UNSPECIFIED.);
#1171=B_SPLINE_CURVE_WITH_KNOTS('',3,(#63792,#63793,#63794,#63795,#63796,
#63797),.UNSPECIFIED.,.F.,.F.,(4,2,4),(-0.0184034922283115,-0.00920121722873323,
0.),.UNSPECIFIED.);
#1172=B_SPLINE_CURVE_WITH_KNOTS('',3,(#63803,#63804,#63805,#63806,#63807,
#63808),.UNSPECIFIED.,.F.,.F.,(4,2,4),(-0.0184046552620133,-0.0092027130938019,
-1.00000000659958E-6),.UNSPECIFIED.);
#1173=B_SPLINE_CURVE_WITH_KNOTS('',3,(#63810,#63811,#63812,#63813,#63814,
#63815),.UNSPECIFIED.,.F.,.F.,(4,2,4),(-0.0184034950211358,-0.00920121908139663,
0.),.UNSPECIFIED.);
#1174=B_SPLINE_CURVE_WITH_KNOTS('',3,(#63821,#63822,#63823,#63824,#63825,
#63826),.UNSPECIFIED.,.F.,.F.,(4,2,4),(-0.0184046552623167,-0.00920321307295721,
-9.99999992049028E-7),.UNSPECIFIED.);
#1175=B_SPLINE_CURVE_WITH_KNOTS('',3,(#63828,#63829,#63830,#63831,#63832,
#63833),.UNSPECIFIED.,.F.,.F.,(4,2,4),(-0.018403495020376,-0.00920171905578727,
0.),.UNSPECIFIED.);
#1176=B_SPLINE_CURVE_WITH_KNOTS('',3,(#63839,#63840,#63841,#63842,#63843,
#63844),.UNSPECIFIED.,.F.,.F.,(4,2,4),(-0.0184046552623086,-0.00920321307293521,
-9.99999992045558E-7),.UNSPECIFIED.);
#1177=B_SPLINE_CURVE_WITH_KNOTS('',3,(#63846,#63847,#63848,#63849,#63850,
#63851),.UNSPECIFIED.,.F.,.F.,(4,2,4),(-0.0184034950217447,-0.00920121908163889,
0.),.UNSPECIFIED.);
#1178=B_SPLINE_CURVE_WITH_KNOTS('',3,(#63857,#63858,#63859,#63860,#63861,
#63862),.UNSPECIFIED.,.F.,.F.,(4,2,4),(-0.0184046538153619,-0.00920321259730723,
-9.99999998842205E-7),.UNSPECIFIED.);
#1179=B_SPLINE_CURVE_WITH_KNOTS('',3,(#63864,#63865,#63866,#63867,#63868,
#63869),.UNSPECIFIED.,.F.,.F.,(4,2,4),(-0.018403492225561,-0.00920171720238882,
0.),.UNSPECIFIED.);
#1180=B_SPLINE_CURVE_WITH_KNOTS('',3,(#63875,#63876,#63877,#63878,#63879,
#63880),.UNSPECIFIED.,.F.,.F.,(4,2,4),(-0.0184046552621458,-0.00920321307288206,
-9.99999994595602E-7),.UNSPECIFIED.);
#1181=B_SPLINE_CURVE_WITH_KNOTS('',3,(#63882,#63883,#63884,#63885,#63886,
#63887),.UNSPECIFIED.,.F.,.F.,(4,2,4),(-0.0184034922345392,-0.0092017172066897,
0.),.UNSPECIFIED.);
#1182=B_SPLINE_CURVE_WITH_KNOTS('',3,(#63893,#63894,#63895,#63896,#63897,
#63898),.UNSPECIFIED.,.F.,.F.,(4,2,4),(-0.0184046552622753,-0.00920321307294581,
-9.9999999906078E-7),.UNSPECIFIED.);
#1183=B_SPLINE_CURVE_WITH_KNOTS('',3,(#63900,#63901,#63902,#63903,#63904,
#63905),.UNSPECIFIED.,.F.,.F.,(4,2,4),(-0.0184034950134852,-0.00920121907819735,
0.),.UNSPECIFIED.);
#1184=B_SPLINE_CURVE_WITH_KNOTS('',3,(#63911,#63912,#63913,#63914,#63915,
#63916),.UNSPECIFIED.,.F.,.F.,(4,2,4),(-0.0184046552618532,-0.0092032130728355,
-9.99999998443218E-7),.UNSPECIFIED.);
#1185=B_SPLINE_CURVE_WITH_KNOTS('',3,(#63918,#63919,#63920,#63921,#63922,
#63923),.UNSPECIFIED.,.F.,.F.,(4,2,4),(-0.0184034950182595,-0.00920121908026001,
0.),.UNSPECIFIED.);
#1186=B_SPLINE_CURVE_WITH_KNOTS('',3,(#63929,#63930,#63931,#63932,#63933,
#63934),.UNSPECIFIED.,.F.,.F.,(4,2,4),(-0.0184046552615148,-0.00920321307277643,
-9.9999999743014E-7),.UNSPECIFIED.);
#1187=B_SPLINE_CURVE_WITH_KNOTS('',3,(#63936,#63937,#63938,#63939,#63940,
#63941),.UNSPECIFIED.,.F.,.F.,(4,2,4),(-0.0184034935070808,-0.00920121807681914,
0.),.UNSPECIFIED.);
#1188=B_SPLINE_CURVE_WITH_KNOTS('',3,(#63947,#63948,#63949,#63950,#63951,
#63952),.UNSPECIFIED.,.F.,.F.,(4,2,4),(-0.0184046538151697,-0.0092027126181944,
-9.99999999591605E-7),.UNSPECIFIED.);
#1189=B_SPLINE_CURVE_WITH_KNOTS('',3,(#63954,#63955,#63956,#63957,#63958,
#63959),.UNSPECIFIED.,.F.,.F.,(4,2,4),(-0.0184034935055579,-0.00920171805030441,
0.),.UNSPECIFIED.);
#1190=B_SPLINE_CURVE_WITH_KNOTS('',3,(#63965,#63966,#63967,#63968,#63969,
#63970),.UNSPECIFIED.,.F.,.F.,(4,2,4),(-0.0184046552616214,-0.00920321307281472,
-9.99999998259338E-7),.UNSPECIFIED.);
#1191=B_SPLINE_CURVE_WITH_KNOTS('',3,(#63972,#63973,#63974,#63975,#63976,
#63977),.UNSPECIFIED.,.F.,.F.,(4,2,4),(-0.0184034950180823,-0.00920171905488093,
0.),.UNSPECIFIED.);
#1192=B_SPLINE_CURVE_WITH_KNOTS('',3,(#63983,#63984,#63985,#63986,#63987,
#63988),.UNSPECIFIED.,.F.,.F.,(4,2,4),(-0.0184046552617036,-0.00920321307280033,
-9.99999998373829E-7),.UNSPECIFIED.);
#1193=B_SPLINE_CURVE_WITH_KNOTS('',3,(#63990,#63991,#63992,#63993,#63994,
#63995),.UNSPECIFIED.,.F.,.F.,(4,2,4),(-0.018403495017296,-0.00920171905455372,
0.),.UNSPECIFIED.);
#1194=B_SPLINE_CURVE_WITH_KNOTS('',3,(#64001,#64002,#64003,#64004,#64005,
#64006),.UNSPECIFIED.,.F.,.F.,(4,2,4),(-0.018404652798285,-0.0092027122837556,
-9.99999999265477E-7),.UNSPECIFIED.);
#1195=B_SPLINE_CURVE_WITH_KNOTS('',3,(#64008,#64009,#64010,#64011,#64012,
#64013),.UNSPECIFIED.,.F.,.F.,(4,2,4),(-0.0184034950141069,-0.00920121907865255,
0.),.UNSPECIFIED.);
#1196=B_SPLINE_CURVE_WITH_KNOTS('',3,(#64019,#64020,#64021,#64022,#64023,
#64024),.UNSPECIFIED.,.F.,.F.,(4,2,4),(-0.018404655262912,-0.00920271309410598,
-9.9999999990559E-7),.UNSPECIFIED.);
#1197=B_SPLINE_CURVE_WITH_KNOTS('',3,(#64026,#64027,#64028,#64029,#64030,
#64031),.UNSPECIFIED.,.F.,.F.,(4,2,4),(-0.0184034935030653,-0.00920121807424569,
0.),.UNSPECIFIED.);
#1198=B_SPLINE_CURVE_WITH_KNOTS('',3,(#64037,#64038,#64039,#64040,#64041,
#64042),.UNSPECIFIED.,.F.,.F.,(4,2,4),(-0.0184046538166818,-0.00920321259763074,
-9.99999998269746E-7),.UNSPECIFIED.);
#1199=B_SPLINE_CURVE_WITH_KNOTS('',3,(#64044,#64045,#64046,#64047,#64048,
#64049),.UNSPECIFIED.,.F.,.F.,(4,2,4),(-0.0184034935060984,-0.00920171805076214,
0.),.UNSPECIFIED.);
#1200=B_SPLINE_CURVE_WITH_KNOTS('',3,(#64055,#64056,#64057,#64058,#64059,
#64060),.UNSPECIFIED.,.F.,.F.,(4,2,4),(-0.0184046552627787,-0.00920271309404019,
-1.00000000020223E-6),.UNSPECIFIED.);
#1201=B_SPLINE_CURVE_WITH_KNOTS('',3,(#64062,#64063,#64064,#64065,#64066,
#64067),.UNSPECIFIED.,.F.,.F.,(4,2,4),(-0.0184034950154033,-0.00920121907917747,
0.),.UNSPECIFIED.);
#1202=B_SPLINE_CURVE_WITH_KNOTS('',3,(#64073,#64074,#64075,#64076,#64077,
#64078),.UNSPECIFIED.,.F.,.F.,(4,2,4),(-0.0184046527954837,-0.00920271228290404,
-9.99999998804041E-7),.UNSPECIFIED.);
#1203=B_SPLINE_CURVE_WITH_KNOTS('',3,(#64080,#64081,#64082,#64083,#64084,
#64085),.UNSPECIFIED.,.F.,.F.,(4,2,4),(-0.0184034922305112,-0.00920171720460419,
0.),.UNSPECIFIED.);
#1204=B_SPLINE_CURVE_WITH_KNOTS('',3,(#64091,#64092,#64093,#64094,#64095,
#64096),.UNSPECIFIED.,.F.,.F.,(4,2,4),(-0.0184046538149872,-0.00920271261810088,
-9.99999999161394E-7),.UNSPECIFIED.);
#1205=B_SPLINE_CURVE_WITH_KNOTS('',3,(#64098,#64099,#64100,#64101,#64102,
#64103),.UNSPECIFIED.,.F.,.F.,(4,2,4),(-0.0184034950171307,-0.00920121907998442,
0.),.UNSPECIFIED.);
#1206=B_SPLINE_CURVE_WITH_KNOTS('',3,(#64109,#64110,#64111,#64112,#64113,
#64114),.UNSPECIFIED.,.F.,.F.,(4,2,4),(-0.0184046552620757,-0.00920271309386517,
-9.99999998351278E-7),.UNSPECIFIED.);
#1207=B_SPLINE_CURVE_WITH_KNOTS('',3,(#64116,#64117,#64118,#64119,#64120,
#64121),.UNSPECIFIED.,.F.,.F.,(4,2,4),(-0.0184034950179269,-0.00920121908024188,
0.),.UNSPECIFIED.);
#1208=B_SPLINE_CURVE_WITH_KNOTS('',3,(#64127,#64128,#64129,#64130,#64131,
#64132),.UNSPECIFIED.,.F.,.F.,(4,2,4),(-0.0184046552620944,-0.00920321307293593,
-9.99999996004197E-7),.UNSPECIFIED.);
#1209=B_SPLINE_CURVE_WITH_KNOTS('',3,(#64134,#64135,#64136,#64137,#64138,
#64139),.UNSPECIFIED.,.F.,.F.,(4,2,4),(-0.018403495018241,-0.00920121908043562,
0.),.UNSPECIFIED.);
#1210=B_SPLINE_CURVE_WITH_KNOTS('',3,(#64145,#64146,#64147,#64148,#64149,
#64150),.UNSPECIFIED.,.F.,.F.,(4,2,4),(-0.0184046552624699,-0.00920271309392275,
-9.99999999333132E-7),.UNSPECIFIED.);
#1211=B_SPLINE_CURVE_WITH_KNOTS('',3,(#64152,#64153,#64154,#64155,#64156,
#64157),.UNSPECIFIED.,.F.,.F.,(4,2,4),(-0.0184034935021887,-0.00920171804868947,
0.),.UNSPECIFIED.);
#1212=B_SPLINE_CURVE_WITH_KNOTS('',3,(#64163,#64164,#64165,#64166,#64167,
#64168),.UNSPECIFIED.,.F.,.F.,(4,2,4),(-0.018404655261847,-0.00920321307284733,
-9.9999999673972E-7),.UNSPECIFIED.);
#1213=B_SPLINE_CURVE_WITH_KNOTS('',3,(#64170,#64171,#64172,#64173,#64174,
#64175),.UNSPECIFIED.,.F.,.F.,(4,2,4),(-0.0184034950156038,-0.00920171905399093,
0.),.UNSPECIFIED.);
#1214=B_SPLINE_CURVE_WITH_KNOTS('',3,(#64181,#64182,#64183,#64184,#64185,
#64186),.UNSPECIFIED.,.F.,.F.,(4,2,4),(-0.0184046552619265,-0.00920271309381794,
-1.00000000422852E-6),.UNSPECIFIED.);
#1215=B_SPLINE_CURVE_WITH_KNOTS('',3,(#64188,#64189,#64190,#64191,#64192,
#64193),.UNSPECIFIED.,.F.,.F.,(4,2,4),(-0.0184034935053294,-0.00920171805006122,
0.),.UNSPECIFIED.);
#1216=B_SPLINE_CURVE_WITH_KNOTS('',3,(#64199,#64200,#64201,#64202,#64203,
#64204),.UNSPECIFIED.,.F.,.F.,(4,2,4),(-0.0184046552617174,-0.0092027130937688,
-1.0000000028737E-6),.UNSPECIFIED.);
#1217=B_SPLINE_CURVE_WITH_KNOTS('',3,(#64206,#64207,#64208,#64209,#64210,
#64211),.UNSPECIFIED.,.F.,.F.,(4,2,4),(-0.0184034935071716,-0.00920121807651139,
0.),.UNSPECIFIED.);
#1218=B_SPLINE_CURVE_WITH_KNOTS('',3,(#64217,#64218,#64219,#64220,#64221,
#64222),.UNSPECIFIED.,.F.,.F.,(4,2,4),(-0.0184046552619574,-0.00920321307285213,
-9.99999993825385E-7),.UNSPECIFIED.);
#1219=B_SPLINE_CURVE_WITH_KNOTS('',3,(#64224,#64225,#64226,#64227,#64228,
#64229),.UNSPECIFIED.,.F.,.F.,(4,2,4),(-0.0184034950150159,-0.0092012190789793,
0.),.UNSPECIFIED.);
#1220=B_SPLINE_CURVE_WITH_KNOTS('',3,(#64235,#64236,#64237,#64238,#64239,
#64240),.UNSPECIFIED.,.F.,.F.,(4,2,4),(-0.0184046538169765,-0.00920321259774155,
-9.99999998980983E-7),.UNSPECIFIED.);
#1221=B_SPLINE_CURVE_WITH_KNOTS('',3,(#64242,#64243,#64244,#64245,#64246,
#64247),.UNSPECIFIED.,.F.,.F.,(4,2,4),(-0.0184034922295949,-0.00920171720370545,
0.),.UNSPECIFIED.);
#1222=B_SPLINE_CURVE_WITH_KNOTS('',3,(#64253,#64254,#64255,#64256,#64257,
#64258),.UNSPECIFIED.,.F.,.F.,(4,2,4),(-0.0184046552619846,-0.00920321307289419,
-9.99999994213963E-7),.UNSPECIFIED.);
#1223=B_SPLINE_CURVE_WITH_KNOTS('',3,(#64260,#64261,#64262,#64263,#64264,
#64265),.UNSPECIFIED.,.F.,.F.,(4,2,4),(-0.0184034950135014,-0.00920121907842531,
0.),.UNSPECIFIED.);
#1224=B_SPLINE_CURVE_WITH_KNOTS('',3,(#64271,#64272,#64273,#64274,#64275,
#64276),.UNSPECIFIED.,.F.,.F.,(4,2,4),(-0.0184046552620079,-0.00920321307288379,
-9.99999996600942E-7),.UNSPECIFIED.);
#1225=B_SPLINE_CURVE_WITH_KNOTS('',3,(#64278,#64279,#64280,#64281,#64282,
#64283),.UNSPECIFIED.,.F.,.F.,(4,2,4),(-0.0184034934973619,-0.00920121807230492,
0.),.UNSPECIFIED.);
#1226=B_SPLINE_CURVE_WITH_KNOTS('',3,(#64289,#64290,#64291,#64292,#64293,
#64294),.UNSPECIFIED.,.F.,.F.,(4,2,4),(-0.0184046552621581,-0.00920271309384943,
-1.00000000408974E-6),.UNSPECIFIED.);
#1227=B_SPLINE_CURVE_WITH_KNOTS('',3,(#64296,#64297,#64298,#64299,#64300,
#64301),.UNSPECIFIED.,.F.,.F.,(4,2,4),(-0.0184034935033682,-0.00920171804998622,
0.),.UNSPECIFIED.);
#1228=B_SPLINE_CURVE_WITH_KNOTS('',3,(#64307,#64308,#64309,#64310,#64311,
#64312),.UNSPECIFIED.,.F.,.F.,(4,2,4),(-0.0184046552616837,-0.00920271309374225,
-1.0000000056235E-6),.UNSPECIFIED.);
#1229=B_SPLINE_CURVE_WITH_KNOTS('',3,(#64314,#64315,#64316,#64317,#64318,
#64319),.UNSPECIFIED.,.F.,.F.,(4,2,4),(-0.0184034922272409,-0.0092012172282045,
0.),.UNSPECIFIED.);
#1230=B_SPLINE_CURVE_WITH_KNOTS('',3,(#64325,#64326,#64327,#64328,#64329,
#64330),.UNSPECIFIED.,.F.,.F.,(4,2,4),(-0.01840465526186,-0.00920321307287029,
-9.99999999317519E-7),.UNSPECIFIED.);
#1231=B_SPLINE_CURVE_WITH_KNOTS('',3,(#64332,#64333,#64334,#64335,#64336,
#64337),.UNSPECIFIED.,.F.,.F.,(4,2,4),(-0.0184034950163261,-0.00920121907951736,
0.),.UNSPECIFIED.);
#1232=B_SPLINE_CURVE_WITH_KNOTS('',3,(#64343,#64344,#64345,#64346,#64347,
#64348),.UNSPECIFIED.,.F.,.F.,(4,2,4),(-0.0184046527928335,-0.00920321226108215,
-9.99999998651385E-7),.UNSPECIFIED.);
#1233=B_SPLINE_CURVE_WITH_KNOTS('',3,(#64350,#64351,#64352,#64353,#64354,
#64355),.UNSPECIFIED.,.F.,.F.,(4,2,4),(-0.0184034935007121,-0.0092012180734001,
0.),.UNSPECIFIED.);
#1234=B_SPLINE_CURVE_WITH_KNOTS('',3,(#64361,#64362,#64363,#64364,#64365,
#64366),.UNSPECIFIED.,.F.,.F.,(4,2,4),(-0.01840465526219,-0.00920271309386883,
-1.0000000022093E-6),.UNSPECIFIED.);
#1235=B_SPLINE_CURVE_WITH_KNOTS('',3,(#64368,#64369,#64370,#64371,#64372,
#64373),.UNSPECIFIED.,.F.,.F.,(4,2,4),(-0.0184034950219852,-0.00920171905652633,
0.),.UNSPECIFIED.);
#1236=B_SPLINE_CURVE_WITH_KNOTS('',3,(#64379,#64380,#64381,#64382,#64383,
#64384),.UNSPECIFIED.,.F.,.F.,(4,2,4),(-0.0184046538120481,-0.00920321259614537,
-9.9999999918915E-7),.UNSPECIFIED.);
#1237=B_SPLINE_CURVE_WITH_KNOTS('',3,(#64386,#64387,#64388,#64389,#64390,
#64391),.UNSPECIFIED.,.F.,.F.,(4,2,4),(-0.0184034950175798,-0.00920171905480655,
0.),.UNSPECIFIED.);
#1238=B_SPLINE_CURVE_WITH_KNOTS('',3,(#64397,#64398,#64399,#64400,#64401,
#64402),.UNSPECIFIED.,.F.,.F.,(4,2,4),(-0.0184046552618216,-0.00920271309381456,
-9.99999998805776E-7),.UNSPECIFIED.);
#1239=B_SPLINE_CURVE_WITH_KNOTS('',3,(#64404,#64405,#64406,#64407,#64408,
#64409),.UNSPECIFIED.,.F.,.F.,(4,2,4),(-0.0184034950228819,-0.00920171905700514,
0.),.UNSPECIFIED.);
#1240=B_SPLINE_CURVE_WITH_KNOTS('',3,(#64415,#64416,#64417,#64418,#64419,
#64420),.UNSPECIFIED.,.F.,.F.,(4,2,4),(-0.0184046552095742,-0.00920271305842647,
-9.9999999915099E-7),.UNSPECIFIED.);
#1241=B_SPLINE_CURVE_WITH_KNOTS('',3,(#64422,#64423,#64424,#64425,#64426,
#64427),.UNSPECIFIED.,.F.,.F.,(4,2,4),(-0.0184034935059472,-0.00920171805058506,
0.),.UNSPECIFIED.);
#1242=B_SPLINE_CURVE_WITH_KNOTS('',3,(#64432,#64433,#64434,#64435,#64436,
#64437),.UNSPECIFIED.,.F.,.F.,(4,2,4),(-0.01840465254103,-0.00920271218116683,
-9.99999999315784E-7),.UNSPECIFIED.);
#1243=B_SPLINE_CURVE_WITH_KNOTS('',3,(#64441,#64442,#64443,#64444),
 .UNSPECIFIED.,.F.,.F.,(4,4),(0.0165621619175432,0.0219133296771791),
 .UNSPECIFIED.);
#1244=B_SPLINE_CURVE_WITH_KNOTS('',3,(#64449,#64450,#64451,#64452,#64453,
#64454),.UNSPECIFIED.,.F.,.F.,(4,2,4),(9.99962477529338E-7,0.0105693184169416,
0.0165621619175432),.UNSPECIFIED.);
#1245=B_SPLINE_CURVE_WITH_KNOTS('',3,(#64464,#64465,#64466,#64467),
 .UNSPECIFIED.,.F.,.F.,(4,4),(4.75255497207553,4.76308887897647),
 .UNSPECIFIED.);
#1246=B_SPLINE_CURVE_WITH_KNOTS('',3,(#64479,#64480,#64481,#64482),
 .UNSPECIFIED.,.F.,.F.,(4,4),(4.75255497207216,4.76308887897314),
 .UNSPECIFIED.);
#1247=B_SPLINE_CURVE_WITH_KNOTS('',3,(#64494,#64495,#64496,#64497),
 .UNSPECIFIED.,.F.,.F.,(4,4),(4.75255497206109,4.7630888789621),
 .UNSPECIFIED.);
#1248=B_SPLINE_CURVE_WITH_KNOTS('',3,(#64509,#64510,#64511,#64512),
 .UNSPECIFIED.,.F.,.F.,(4,4),(4.75255497207336,4.76308887897441),
 .UNSPECIFIED.);
#1249=B_SPLINE_CURVE_WITH_KNOTS('',3,(#64524,#64525,#64526,#64527),
 .UNSPECIFIED.,.F.,.F.,(4,4),(4.7525549721169,4.763088879018),
 .UNSPECIFIED.);
#1250=B_SPLINE_CURVE_WITH_KNOTS('',3,(#64539,#64540,#64541,#64542),
 .UNSPECIFIED.,.F.,.F.,(4,4),(4.75255497216149,4.76308887906267),
 .UNSPECIFIED.);
#1251=B_SPLINE_CURVE_WITH_KNOTS('',3,(#64554,#64555,#64556,#64557),
 .UNSPECIFIED.,.F.,.F.,(4,4),(4.75255497220882,4.76308887911007),
 .UNSPECIFIED.);
#1252=B_SPLINE_CURVE_WITH_KNOTS('',3,(#64569,#64570,#64571,#64572),
 .UNSPECIFIED.,.F.,.F.,(4,4),(4.75255497220738,4.76308887910871),
 .UNSPECIFIED.);
#1253=B_SPLINE_CURVE_WITH_KNOTS('',3,(#64584,#64585,#64586,#64587),
 .UNSPECIFIED.,.F.,.F.,(4,4),(4.75255497208619,4.7630888789876),
 .UNSPECIFIED.);
#1254=B_SPLINE_CURVE_WITH_KNOTS('',3,(#64599,#64600,#64601,#64602),
 .UNSPECIFIED.,.F.,.F.,(4,4),(4.75255497206892,4.76308887897041),
 .UNSPECIFIED.);
#1255=B_SPLINE_CURVE_WITH_KNOTS('',3,(#64614,#64615,#64616,#64617),
 .UNSPECIFIED.,.F.,.F.,(4,4),(4.75255497207531,4.7630888789769),
 .UNSPECIFIED.);
#1256=B_SPLINE_CURVE_WITH_KNOTS('',3,(#64629,#64630,#64631,#64632),
 .UNSPECIFIED.,.F.,.F.,(4,4),(4.75255497209236,4.76308887899405),
 .UNSPECIFIED.);
#1257=B_SPLINE_CURVE_WITH_KNOTS('',3,(#64644,#64645,#64646,#64647),
 .UNSPECIFIED.,.F.,.F.,(4,4),(4.75255497206474,4.76308887896652),
 .UNSPECIFIED.);
#1258=B_SPLINE_CURVE_WITH_KNOTS('',3,(#64659,#64660,#64661,#64662),
 .UNSPECIFIED.,.F.,.F.,(4,4),(4.75255497207158,4.76308887897344),
 .UNSPECIFIED.);
#1259=B_SPLINE_CURVE_WITH_KNOTS('',3,(#64674,#64675,#64676,#64677),
 .UNSPECIFIED.,.F.,.F.,(4,4),(4.75255497208885,4.76308887899078),
 .UNSPECIFIED.);
#1260=B_SPLINE_CURVE_WITH_KNOTS('',3,(#64689,#64690,#64691,#64692),
 .UNSPECIFIED.,.F.,.F.,(4,4),(4.75255497206809,4.76308887897013),
 .UNSPECIFIED.);
#1261=B_SPLINE_CURVE_WITH_KNOTS('',3,(#64704,#64705,#64706,#64707),
 .UNSPECIFIED.,.F.,.F.,(4,4),(4.75255497207646,4.76308887897857),
 .UNSPECIFIED.);
#1262=B_SPLINE_CURVE_WITH_KNOTS('',3,(#64719,#64720,#64721,#64722),
 .UNSPECIFIED.,.F.,.F.,(4,4),(4.75255497207436,4.76308887897653),
 .UNSPECIFIED.);
#1263=B_SPLINE_CURVE_WITH_KNOTS('',3,(#64734,#64735,#64736,#64737),
 .UNSPECIFIED.,.F.,.F.,(4,4),(4.75255497208078,4.763088878983),
 .UNSPECIFIED.);
#1264=B_SPLINE_CURVE_WITH_KNOTS('',3,(#64749,#64750,#64751,#64752),
 .UNSPECIFIED.,.F.,.F.,(4,4),(4.75255497227339,4.76308887917565),
 .UNSPECIFIED.);
#1265=B_SPLINE_CURVE_WITH_KNOTS('',3,(#64764,#64765,#64766,#64767),
 .UNSPECIFIED.,.F.,.F.,(4,4),(4.75255497224816,4.76308887915048),
 .UNSPECIFIED.);
#1266=B_SPLINE_CURVE_WITH_KNOTS('',3,(#64779,#64780,#64781,#64782),
 .UNSPECIFIED.,.F.,.F.,(4,4),(4.75255497220241,4.76308887910477),
 .UNSPECIFIED.);
#1267=B_SPLINE_CURVE_WITH_KNOTS('',3,(#64794,#64795,#64796,#64797),
 .UNSPECIFIED.,.F.,.F.,(4,4),(4.75255497215918,4.76308887906153),
 .UNSPECIFIED.);
#1268=B_SPLINE_CURVE_WITH_KNOTS('',3,(#64809,#64810,#64811,#64812),
 .UNSPECIFIED.,.F.,.F.,(4,4),(4.752554972119,4.7630888790214),
 .UNSPECIFIED.);
#1269=B_SPLINE_CURVE_WITH_KNOTS('',3,(#64824,#64825,#64826,#64827),
 .UNSPECIFIED.,.F.,.F.,(4,4),(4.75255497209406,4.76308887915569),
 .UNSPECIFIED.);
#1270=B_SPLINE_CURVE_WITH_KNOTS('',3,(#64839,#64840,#64841,#64842),
 .UNSPECIFIED.,.F.,.F.,(4,4),(4.75255497213315,4.76308887903548),
 .UNSPECIFIED.);
#1271=B_SPLINE_CURVE_WITH_KNOTS('',3,(#64854,#64855,#64856,#64857),
 .UNSPECIFIED.,.F.,.F.,(4,4),(4.75255497214093,4.76308887904322),
 .UNSPECIFIED.);
#1272=B_SPLINE_CURVE_WITH_KNOTS('',3,(#64869,#64870,#64871,#64872),
 .UNSPECIFIED.,.F.,.F.,(4,4),(4.75255497222018,4.76308887912243),
 .UNSPECIFIED.);
#1273=B_SPLINE_CURVE_WITH_KNOTS('',3,(#64884,#64885,#64886,#64887),
 .UNSPECIFIED.,.F.,.F.,(4,4),(4.75255497202817,4.76308887893043),
 .UNSPECIFIED.);
#1274=B_SPLINE_CURVE_WITH_KNOTS('',3,(#64899,#64900,#64901,#64902),
 .UNSPECIFIED.,.F.,.F.,(4,4),(4.75255497204426,4.76308887894642),
 .UNSPECIFIED.);
#1275=B_SPLINE_CURVE_WITH_KNOTS('',3,(#64914,#64915,#64916,#64917),
 .UNSPECIFIED.,.F.,.F.,(4,4),(4.75255497203009,4.76308887893217),
 .UNSPECIFIED.);
#1276=B_SPLINE_CURVE_WITH_KNOTS('',3,(#64929,#64930,#64931,#64932),
 .UNSPECIFIED.,.F.,.F.,(4,4),(4.7525549720349,4.76308887893693),
 .UNSPECIFIED.);
#1277=B_SPLINE_CURVE_WITH_KNOTS('',3,(#64944,#64945,#64946,#64947),
 .UNSPECIFIED.,.F.,.F.,(4,4),(4.75255497200156,4.76308887890348),
 .UNSPECIFIED.);
#1278=B_SPLINE_CURVE_WITH_KNOTS('',3,(#64959,#64960,#64961,#64962),
 .UNSPECIFIED.,.F.,.F.,(4,4),(4.75255497203018,4.76308887893203),
 .UNSPECIFIED.);
#1279=B_SPLINE_CURVE_WITH_KNOTS('',3,(#64974,#64975,#64976,#64977),
 .UNSPECIFIED.,.F.,.F.,(4,4),(4.75255497199264,4.7630888788944),
 .UNSPECIFIED.);
#1280=B_SPLINE_CURVE_WITH_KNOTS('',3,(#64989,#64990,#64991,#64992),
 .UNSPECIFIED.,.F.,.F.,(4,4),(4.75255497198854,4.76308887889023),
 .UNSPECIFIED.);
#1281=B_SPLINE_CURVE_WITH_KNOTS('',3,(#65004,#65005,#65006,#65007),
 .UNSPECIFIED.,.F.,.F.,(4,4),(4.75255497197651,4.76308887887812),
 .UNSPECIFIED.);
#1282=B_SPLINE_CURVE_WITH_KNOTS('',3,(#65019,#65020,#65021,#65022),
 .UNSPECIFIED.,.F.,.F.,(4,4),(4.75255497195996,4.76308887886144),
 .UNSPECIFIED.);
#1283=B_SPLINE_CURVE_WITH_KNOTS('',3,(#65034,#65035,#65036,#65037),
 .UNSPECIFIED.,.F.,.F.,(4,4),(4.75255497195405,4.76308887885545),
 .UNSPECIFIED.);
#1284=B_SPLINE_CURVE_WITH_KNOTS('',3,(#65049,#65050,#65051,#65052),
 .UNSPECIFIED.,.F.,.F.,(4,4),(4.75255497194695,4.76308887884825),
 .UNSPECIFIED.);
#1285=B_SPLINE_CURVE_WITH_KNOTS('',3,(#65064,#65065,#65066,#65067),
 .UNSPECIFIED.,.F.,.F.,(4,4),(4.7525549719234,4.76308887882463),
 .UNSPECIFIED.);
#1286=B_SPLINE_CURVE_WITH_KNOTS('',3,(#65079,#65080,#65081,#65082),
 .UNSPECIFIED.,.F.,.F.,(4,4),(4.75255497193489,4.76308887883606),
 .UNSPECIFIED.);
#1287=B_SPLINE_CURVE_WITH_KNOTS('',3,(#65094,#65095,#65096,#65097),
 .UNSPECIFIED.,.F.,.F.,(4,4),(4.75255497192173,4.76308887882284),
 .UNSPECIFIED.);
#1288=B_SPLINE_CURVE_WITH_KNOTS('',3,(#65109,#65110,#65111,#65112),
 .UNSPECIFIED.,.F.,.F.,(4,4),(4.75255497191409,4.76308887881513),
 .UNSPECIFIED.);
#1289=B_SPLINE_CURVE_WITH_KNOTS('',3,(#65124,#65125,#65126,#65127),
 .UNSPECIFIED.,.F.,.F.,(4,4),(4.75255497190642,4.76308887880743),
 .UNSPECIFIED.);
#1290=B_SPLINE_CURVE_WITH_KNOTS('',3,(#65139,#65140,#65141,#65142),
 .UNSPECIFIED.,.F.,.F.,(4,4),(4.75255497190071,4.76308887880165),
 .UNSPECIFIED.);
#1291=B_SPLINE_CURVE_WITH_KNOTS('',3,(#65154,#65155,#65156,#65157),
 .UNSPECIFIED.,.F.,.F.,(4,4),(4.75255497189559,4.76308887879652),
 .UNSPECIFIED.);
#1292=B_SPLINE_CURVE_WITH_KNOTS('',3,(#65169,#65170,#65171,#65172),
 .UNSPECIFIED.,.F.,.F.,(4,4),(4.75255497189571,4.76308887879664),
 .UNSPECIFIED.);
#1293=B_SPLINE_CURVE_WITH_KNOTS('',3,(#65184,#65185,#65186,#65187),
 .UNSPECIFIED.,.F.,.F.,(4,4),(4.75255497188971,4.76308887879064),
 .UNSPECIFIED.);
#1294=B_SPLINE_CURVE_WITH_KNOTS('',3,(#65198,#65199,#65200,#65201),
 .UNSPECIFIED.,.F.,.F.,(4,4),(4.75255497186513,4.76308887897258),
 .UNSPECIFIED.);
#1295=B_SPLINE_CURVE_WITH_KNOTS('',3,(#65223,#65224,#65225,#65226,#65227,
#65228,#65229),.UNSPECIFIED.,.F.,.F.,(4,3,4),(0.,0.5,0.999990117119694),
 .UNSPECIFIED.);
#1296=B_SPLINE_CURVE_WITH_KNOTS('',3,(#65252,#65253,#65254,#65255,#65256,
#65257),.UNSPECIFIED.,.F.,.F.,(4,2,4),(0.,0.0198677118939269,0.039736333875931),
 .UNSPECIFIED.);
#1297=B_SPLINE_CURVE_WITH_KNOTS('',3,(#65287,#65288,#65289,#65290,#65291,
#65292,#65293),.UNSPECIFIED.,.F.,.F.,(4,3,4),(0.,0.5,0.999990115107466),
 .UNSPECIFIED.);
#1298=B_SPLINE_CURVE_WITH_KNOTS('',3,(#65319,#65320,#65321,#65322,#65323,
#65324),.UNSPECIFIED.,.F.,.F.,(4,2,4),(0.,0.019903067966103,0.0398070346017422),
 .UNSPECIFIED.);
#1299=B_SPLINE_CURVE_WITH_KNOTS('',3,(#65346,#65347,#65348,#65349,#65350,
#65351),.UNSPECIFIED.,.F.,.F.,(4,2,4),(0.,0.0198677117249203,0.0397363335964693),
 .UNSPECIFIED.);
#1300=B_SPLINE_CURVE_WITH_KNOTS('',3,(#65375,#65376,#65377,#65378,#65379,
#65380),.UNSPECIFIED.,.F.,.F.,(4,2,4),(0.,0.0198973966006019,0.0397956843350417),
 .UNSPECIFIED.);
#1301=B_SPLINE_CURVE_WITH_KNOTS('',3,(#65453,#65454,#65455,#65456,#65457,
#65458),.UNSPECIFIED.,.F.,.F.,(4,2,4),(0.,0.0198994178811908,0.0397997368662755),
 .UNSPECIFIED.);
#1302=B_SPLINE_CURVE_WITH_KNOTS('',3,(#65475,#65476,#65477,#65478,#65479,
#65480),.UNSPECIFIED.,.F.,.F.,(4,2,4),(0.,0.0198973966005004,0.039795684334322),
 .UNSPECIFIED.);
#1303=B_SPLINE_CURVE_WITH_KNOTS('',3,(#65494,#65495,#65496,#65497,#65498,
#65499),.UNSPECIFIED.,.F.,.F.,(4,2,4),(0.,0.0198905179568995,0.0397819072566626),
 .UNSPECIFIED.);
#1304=B_SPLINE_CURVE_WITH_KNOTS('',3,(#65514,#65515,#65516,#65517,#65518,
#65519),.UNSPECIFIED.,.F.,.F.,(4,2,4),(0.,0.0199030098319572,0.0398069010941151),
 .UNSPECIFIED.);
#1305=B_SPLINE_CURVE_WITH_KNOTS('',3,(#65549,#65550,#65551,#65552,#65553,
#65554,#65555),.UNSPECIFIED.,.F.,.F.,(4,3,4),(0.0365944846647011,0.0384615384615384,
0.0431466153076602),.UNSPECIFIED.);
#1306=B_SPLINE_CURVE_WITH_KNOTS('',3,(#65557,#65558,#65559,#65560,#65561,
#65562,#65563,#65564),.UNSPECIFIED.,.F.,.F.,(4,2,2,4),(1.77350755374016E-6,
0.00863675573580245,0.0171409052851941,0.0172810535282736),
 .UNSPECIFIED.);
#1307=B_SPLINE_CURVE_WITH_KNOTS('',3,(#65606,#65607,#65608,#65609,#65610,
#65611),.UNSPECIFIED.,.F.,.F.,(4,2,4),(0.,0.0198536183249784,0.0397081496300452),
 .UNSPECIFIED.);
#1308=B_SPLINE_CURVE_WITH_KNOTS('',3,(#65628,#65629,#65630,#65631,#65632,
#65633),.UNSPECIFIED.,.F.,.F.,(4,2,4),(0.,0.0198994178801103,0.039799736862051),
 .UNSPECIFIED.);
#1309=B_SPLINE_CURVE_WITH_KNOTS('',3,(#65652,#65653,#65654,#65655,#65656,
#65657),.UNSPECIFIED.,.F.,.F.,(4,2,4),(-0.00212389296650024,-0.00106194370310601,
0.),.UNSPECIFIED.);
#1310=B_SPLINE_CURVE_WITH_KNOTS('',3,(#65658,#65659,#65660,#65661,#65662,
#65663),.UNSPECIFIED.,.F.,.F.,(4,2,4),(9.99998418911506E-7,0.0193527846137979,
0.0387045795163393),.UNSPECIFIED.);
#1311=B_SPLINE_CURVE_WITH_KNOTS('',3,(#65678,#65679,#65680,#65681,#65682,
#65683),.UNSPECIFIED.,.F.,.F.,(4,2,4),(0.,0.0198905190016668,0.0397819091577267),
 .UNSPECIFIED.);
#1312=B_SPLINE_CURVE_WITH_KNOTS('',3,(#65688,#65689,#65690,#65691,#65692,
#65693),.UNSPECIFIED.,.F.,.F.,(4,2,4),(-0.00212486200559533,-0.00106293275925874,
-9.99999998182793E-7),.UNSPECIFIED.);
#1313=B_SPLINE_CURVE_WITH_KNOTS('',3,(#65741,#65742,#65743,#65744,#65745,
#65746,#65747),.UNSPECIFIED.,.F.,.F.,(4,3,4),(0.0365944846647015,0.0384615384615384,
0.0431466153076587),.UNSPECIFIED.);
#1314=B_SPLINE_CURVE_WITH_KNOTS('',3,(#65749,#65750,#65751,#65752,#65753,
#65754,#65755,#65756),.UNSPECIFIED.,.F.,.F.,(4,2,2,4),(1.77292721144812E-6,
0.00863675579268646,0.0171409291098449,0.0172810748822113),
 .UNSPECIFIED.);
#1315=B_SPLINE_CURVE_WITH_KNOTS('',3,(#65775,#65776,#65777,#65778,#65779,
#65780),.UNSPECIFIED.,.F.,.F.,(4,2,4),(0.,0.0198583386697715,0.0397175618272593),
 .UNSPECIFIED.);
#1316=B_SPLINE_CURVE_WITH_KNOTS('',3,(#65797,#65798,#65799,#65800,#65801,
#65802),.UNSPECIFIED.,.F.,.F.,(4,2,4),(0.,0.0198536183213069,0.0397081496154716),
 .UNSPECIFIED.);
#1317=B_SPLINE_CURVE_WITH_KNOTS('',3,(#65823,#65824,#65825,#65826,#65827,
#65828),.UNSPECIFIED.,.F.,.F.,(4,2,4),(0.,0.019876258198358,0.0397534246592788),
 .UNSPECIFIED.);
#1318=B_SPLINE_CURVE_WITH_KNOTS('',3,(#65843,#65844,#65845,#65846,#65847,
#65848),.UNSPECIFIED.,.F.,.F.,(4,2,4),(-0.00212389454210504,-0.00106194431286647,
0.),.UNSPECIFIED.);
#1319=B_SPLINE_CURVE_WITH_KNOTS('',3,(#65849,#65850,#65851,#65852,#65853,
#65854),.UNSPECIFIED.,.F.,.F.,(4,2,4),(9.99998417577743E-7,0.0193522748428586,
0.038704569289107),.UNSPECIFIED.);
#1320=B_SPLINE_CURVE_WITH_KNOTS('',3,(#65866,#65867,#65868,#65869,#65870,
#65871),.UNSPECIFIED.,.F.,.F.,(4,2,4),(-0.00212486139194619,-0.00106293275903844,
-1.00000000112337E-6),.UNSPECIFIED.);
#1321=B_SPLINE_CURVE_WITH_KNOTS('',3,(#65937,#65938,#65939,#65940,#65941,
#65942),.UNSPECIFIED.,.F.,.F.,(4,2,4),(0.,0.0199008240806452,0.0398025406855435),
 .UNSPECIFIED.);
#1322=B_SPLINE_CURVE_WITH_KNOTS('',3,(#65959,#65960,#65961,#65962,#65963,
#65964),.UNSPECIFIED.,.F.,.F.,(4,2,4),(0.,0.0198583386680412,0.0397175618203158),
 .UNSPECIFIED.);
#1323=B_SPLINE_CURVE_WITH_KNOTS('',3,(#65985,#65986,#65987,#65988,#65989,
#65990),.UNSPECIFIED.,.F.,.F.,(4,2,4),(0.,0.0199042621693574,0.0398094213946847),
 .UNSPECIFIED.);
#1324=B_SPLINE_CURVE_WITH_KNOTS('',3,(#66012,#66013,#66014,#66015,#66016,
#66017),.UNSPECIFIED.,.F.,.F.,(4,2,4),(0.,0.0198762582949225,0.0397534248643712),
 .UNSPECIFIED.);
#1325=B_SPLINE_CURVE_WITH_KNOTS('',3,(#66095,#66096,#66097,#66098,#66099,
#66100),.UNSPECIFIED.,.F.,.F.,(4,2,4),(0.,0.019895479367571,0.0397918615427886),
 .UNSPECIFIED.);
#1326=B_SPLINE_CURVE_WITH_KNOTS('',3,(#66117,#66118,#66119,#66120,#66121,
#66122),.UNSPECIFIED.,.F.,.F.,(4,2,4),(0.,0.0199008240758206,0.0398025406664044),
 .UNSPECIFIED.);
#1327=B_SPLINE_CURVE_WITH_KNOTS('',3,(#66162,#66163,#66164,#66165,#66166,
#66167),.UNSPECIFIED.,.F.,.F.,(4,2,4),(0.,0.0199042621633849,0.0398094213825159),
 .UNSPECIFIED.);
#1328=B_SPLINE_CURVE_WITH_KNOTS('',3,(#66218,#66219,#66220,#66221,#66222,
#66223),.UNSPECIFIED.,.F.,.F.,(4,2,4),(0.,0.0198954793631272,0.0397918615243005),
 .UNSPECIFIED.);
#1329=B_SPLINE_CURVE_WITH_KNOTS('',3,(#66264,#66265,#66266,#66267,#66268,
#66269,#66270),.UNSPECIFIED.,.F.,.F.,(4,3,4),(0.,0.5,0.99999011712143),
 .UNSPECIFIED.);
#1330=B_SPLINE_CURVE_WITH_KNOTS('',3,(#66293,#66294,#66295,#66296,#66297,
#66298),.UNSPECIFIED.,.F.,.F.,(4,2,4),(0.,0.0198677118963707,0.0397363338857673),
 .UNSPECIFIED.);
#1331=B_SPLINE_CURVE_WITH_KNOTS('',3,(#66340,#66341,#66342,#66343,#66344,
#66345),.UNSPECIFIED.,.F.,.F.,(4,2,4),(0.,0.0198973966012806,0.0397956843374697),
 .UNSPECIFIED.);
#1332=B_SPLINE_CURVE_WITH_KNOTS('',3,(#66367,#66368,#66369,#66370,#66371,
#66372),.UNSPECIFIED.,.F.,.F.,(4,2,4),(0.,0.0199030679677246,0.0398070346083461),
 .UNSPECIFIED.);
#1333=B_SPLINE_CURVE_WITH_KNOTS('',3,(#66406,#66407,#66408,#66409,#66410,
#66411),.UNSPECIFIED.,.F.,.F.,(4,2,4),(0.,0.0198905179566254,0.039781907255294),
 .UNSPECIFIED.);
#1334=B_SPLINE_CURVE_WITH_KNOTS('',3,(#66436,#66437,#66438,#66439,#66440,
#66441),.UNSPECIFIED.,.F.,.F.,(4,2,4),(0.,0.0198994178826517,0.0397997368722785),
 .UNSPECIFIED.);
#1335=B_SPLINE_CURVE_WITH_KNOTS('',3,(#66465,#66466,#66467,#66468,#66469,
#66470,#66471),.UNSPECIFIED.,.F.,.F.,(4,3,4),(0.0365944846647268,0.0384615384615384,
0.0431466153076594),.UNSPECIFIED.);
#1336=B_SPLINE_CURVE_WITH_KNOTS('',3,(#66472,#66473,#66474,#66475,#66476,
#66477,#66478,#66479),.UNSPECIFIED.,.F.,.F.,(4,2,2,4),(1.77350715213377E-6,
0.0086367558589756,0.0171409489082422,0.0172810924755889),.UNSPECIFIED.);
#1337=B_SPLINE_CURVE_WITH_KNOTS('',3,(#66504,#66505,#66506,#66507,#66508,
#66509),.UNSPECIFIED.,.F.,.F.,(4,2,4),(0.,0.0198536183240437,0.0397081496263899),
 .UNSPECIFIED.);
#1338=B_SPLINE_CURVE_WITH_KNOTS('',3,(#66527,#66528,#66529,#66530,#66531,
#66532),.UNSPECIFIED.,.F.,.F.,(4,2,4),(-0.0021238913584622,-0.00106194304649518,
0.),.UNSPECIFIED.);
#1339=B_SPLINE_CURVE_WITH_KNOTS('',3,(#66533,#66534,#66535,#66536,#66537,
#66538),.UNSPECIFIED.,.F.,.F.,(4,2,4),(9.99998417920556E-7,0.0193527846142068,
0.0387045795170656),.UNSPECIFIED.);
#1340=B_SPLINE_CURVE_WITH_KNOTS('',3,(#66544,#66545,#66546,#66547,#66548,
#66549),.UNSPECIFIED.,.F.,.F.,(4,2,4),(-0.00212486263447062,-0.00106293275266832,
-9.99999998948673E-7),.UNSPECIFIED.);
#1341=B_SPLINE_CURVE_WITH_KNOTS('',3,(#66585,#66586,#66587,#66588,#66589,
#66590),.UNSPECIFIED.,.F.,.F.,(4,2,4),(0.,0.0198583386708035,0.0397175618316024),
 .UNSPECIFIED.);
#1342=B_SPLINE_CURVE_WITH_KNOTS('',3,(#66603,#66604,#66605,#66606,#66607,
#66608),.UNSPECIFIED.,.F.,.F.,(4,2,4),(0.,0.0198761967030548,0.0397532849661016),
 .UNSPECIFIED.);
#1343=B_SPLINE_CURVE_WITH_KNOTS('',3,(#66660,#66661,#66662,#66663,#66664,
#66665),.UNSPECIFIED.,.F.,.F.,(4,2,4),(0.,0.0199008240827659,0.0398025406936002),
 .UNSPECIFIED.);
#1344=B_SPLINE_CURVE_WITH_KNOTS('',3,(#66685,#66686,#66687,#66688,#66689,
#66690),.UNSPECIFIED.,.F.,.F.,(4,2,4),(0.,0.0199042621706517,0.0398094213994398),
 .UNSPECIFIED.);
#1345=B_SPLINE_CURVE_WITH_KNOTS('',3,(#66738,#66739,#66740,#66741,#66742,
#66743),.UNSPECIFIED.,.F.,.F.,(4,2,4),(0.,0.0198954793707845,0.0397918615553697),
 .UNSPECIFIED.);
#1346=B_SPLINE_CURVE_WITH_KNOTS('',3,(#66790,#66791,#66792,#66793,#66794,
#66795,#66796),.UNSPECIFIED.,.F.,.F.,(4,3,4),(0.,0.5,0.999990117122412),
 .UNSPECIFIED.);
#1347=B_SPLINE_CURVE_WITH_KNOTS('',3,(#66819,#66820,#66821,#66822,#66823,
#66824),.UNSPECIFIED.,.F.,.F.,(4,2,4),(0.,0.019867711898593,0.0397363338947165),
 .UNSPECIFIED.);
#1348=B_SPLINE_CURVE_WITH_KNOTS('',3,(#66866,#66867,#66868,#66869,#66870,
#66871),.UNSPECIFIED.,.F.,.F.,(4,2,4),(0.,0.0198973966022289,0.0397956843415848),
 .UNSPECIFIED.);
#1349=B_SPLINE_CURVE_WITH_KNOTS('',3,(#66893,#66894,#66895,#66896,#66897,
#66898),.UNSPECIFIED.,.F.,.F.,(4,2,4),(0.,0.0199030679688408,0.03980703461301),
 .UNSPECIFIED.);
#1350=B_SPLINE_CURVE_WITH_KNOTS('',3,(#66943,#66944,#66945,#66946,#66947,
#66948),.UNSPECIFIED.,.F.,.F.,(4,2,4),(0.,0.0198994178838214,0.0397997368769709),
 .UNSPECIFIED.);
#1351=B_SPLINE_CURVE_WITH_KNOTS('',3,(#66961,#66962,#66963,#66964,#66965,
#66966),.UNSPECIFIED.,.F.,.F.,(4,2,4),(0.,0.0198905179566607,0.0397819072561946),
 .UNSPECIFIED.);
#1352=B_SPLINE_CURVE_WITH_KNOTS('',3,(#66985,#66986,#66987,#66988,#66989,
#66990,#66991),.UNSPECIFIED.,.F.,.F.,(4,3,4),(0.036594484664701,0.0384615384615384,
0.0431466153076598),.UNSPECIFIED.);
#1353=B_SPLINE_CURVE_WITH_KNOTS('',3,(#66992,#66993,#66994,#66995,#66996,
#66997,#66998,#66999),.UNSPECIFIED.,.F.,.F.,(4,2,2,4),(1.77257448215108E-6,
0.00863675575236804,0.0171409239383189,0.0172810702978924),
 .UNSPECIFIED.);
#1354=B_SPLINE_CURVE_WITH_KNOTS('',3,(#67024,#67025,#67026,#67027,#67028,
#67029),.UNSPECIFIED.,.F.,.F.,(4,2,4),(-0.00212388996317658,-0.00106194249137579,
0.),.UNSPECIFIED.);
#1355=B_SPLINE_CURVE_WITH_KNOTS('',3,(#67030,#67031,#67032,#67033,#67034,
#67035),.UNSPECIFIED.,.F.,.F.,(4,2,4),(9.99998418160754E-7,0.0193522753881725,
0.0387045692982265),.UNSPECIFIED.);
#1356=B_SPLINE_CURVE_WITH_KNOTS('',3,(#67060,#67061,#67062,#67063,#67064,
#67065),.UNSPECIFIED.,.F.,.F.,(4,2,4),(0.,0.0198536183256091,0.039708149632394),
 .UNSPECIFIED.);
#1357=B_SPLINE_CURVE_WITH_KNOTS('',3,(#67070,#67071,#67072,#67073,#67074,
#67075),.UNSPECIFIED.,.F.,.F.,(4,2,4),(-0.00212486323669885,-0.00106293276579889,
-9.99999996992874E-7),.UNSPECIFIED.);
#1358=B_SPLINE_CURVE_WITH_KNOTS('',3,(#67114,#67115,#67116,#67117,#67118,
#67119),.UNSPECIFIED.,.F.,.F.,(4,2,4),(0.,0.0198583386720477,0.0397175618366298),
 .UNSPECIFIED.);
#1359=B_SPLINE_CURVE_WITH_KNOTS('',3,(#67132,#67133,#67134,#67135,#67136,
#67137),.UNSPECIFIED.,.F.,.F.,(4,2,4),(0.,0.0198761966979935,0.0397532849518538),
 .UNSPECIFIED.);
#1360=B_SPLINE_CURVE_WITH_KNOTS('',3,(#67189,#67190,#67191,#67192,#67193,
#67194),.UNSPECIFIED.,.F.,.F.,(4,2,4),(0.,0.0199008240838985,0.039802540698102),
 .UNSPECIFIED.);
#1361=B_SPLINE_CURVE_WITH_KNOTS('',3,(#67207,#67208,#67209,#67210,#67211,
#67212),.UNSPECIFIED.,.F.,.F.,(4,2,4),(0.,0.0199042047183892,0.039809289175465),
 .UNSPECIFIED.);
#1362=B_SPLINE_CURVE_WITH_KNOTS('',3,(#67260,#67261,#67262,#67263,#67264,
#67265),.UNSPECIFIED.,.F.,.F.,(4,2,4),(0.,0.0198954793043815,0.0397918613553301),
 .UNSPECIFIED.);
#1363=B_SPLINE_CURVE_WITH_KNOTS('',3,(#67312,#67313,#67314,#67315,#67316,
#67317,#67318),.UNSPECIFIED.,.F.,.F.,(4,3,4),(0.,0.5,0.999990117123793),
 .UNSPECIFIED.);
#1364=B_SPLINE_CURVE_WITH_KNOTS('',3,(#67341,#67342,#67343,#67344,#67345,
#67346),.UNSPECIFIED.,.F.,.F.,(4,2,4),(0.,0.0198677119029657,0.039736333911811),
 .UNSPECIFIED.);
#1365=B_SPLINE_CURVE_WITH_KNOTS('',3,(#67388,#67389,#67390,#67391,#67392,
#67393),.UNSPECIFIED.,.F.,.F.,(4,2,4),(0.,0.0198973966033577,0.0397956843461078),
 .UNSPECIFIED.);
#1366=B_SPLINE_CURVE_WITH_KNOTS('',3,(#67415,#67416,#67417,#67418,#67419,
#67420),.UNSPECIFIED.,.F.,.F.,(4,2,4),(0.,0.0199030679707897,0.0398070346211267),
 .UNSPECIFIED.);
#1367=B_SPLINE_CURVE_WITH_KNOTS('',3,(#67465,#67466,#67467,#67468,#67469,
#67470),.UNSPECIFIED.,.F.,.F.,(4,2,4),(0.,0.0198994178847544,0.0397997368809266),
 .UNSPECIFIED.);
#1368=B_SPLINE_CURVE_WITH_KNOTS('',3,(#67483,#67484,#67485,#67486,#67487,
#67488),.UNSPECIFIED.,.F.,.F.,(4,2,4),(0.,0.0198905179563737,0.0397819072583148),
 .UNSPECIFIED.);
#1369=B_SPLINE_CURVE_WITH_KNOTS('',3,(#67513,#67514,#67515,#67516,#67517,
#67518,#67519),.UNSPECIFIED.,.F.,.F.,(4,3,4),(0.0365944846647015,0.0384615384615384,
0.0431466153076599),.UNSPECIFIED.);
#1370=B_SPLINE_CURVE_WITH_KNOTS('',3,(#67520,#67521,#67522,#67523,#67524,
#67525,#67526,#67527),.UNSPECIFIED.,.F.,.F.,(4,2,2,4),(1.77257433175202E-6,
0.00863675581122146,0.0171409325034123,0.0172810779526648),
 .UNSPECIFIED.);
#1371=B_SPLINE_CURVE_WITH_KNOTS('',3,(#67552,#67553,#67554,#67555,#67556,
#67557),.UNSPECIFIED.,.F.,.F.,(4,2,4),(0.,0.0198536183270368,0.0397081496382176),
 .UNSPECIFIED.);
#1372=B_SPLINE_CURVE_WITH_KNOTS('',3,(#67575,#67576,#67577,#67578,#67579,
#67580),.UNSPECIFIED.,.F.,.F.,(4,2,4),(-0.00212388914888901,-0.00106194216549549,
0.),.UNSPECIFIED.);
#1373=B_SPLINE_CURVE_WITH_KNOTS('',3,(#67581,#67582,#67583,#67584,#67585,
#67586),.UNSPECIFIED.,.F.,.F.,(4,2,4),(9.99998418999774E-7,0.019352785409166,
0.0387045795316142),.UNSPECIFIED.);
#1374=B_SPLINE_CURVE_WITH_KNOTS('',3,(#67620,#67621,#67622,#67623,#67624,
#67625),.UNSPECIFIED.,.F.,.F.,(4,2,4),(0.,0.0198761967017776,0.0397532849566243),
 .UNSPECIFIED.);
#1375=B_SPLINE_CURVE_WITH_KNOTS('',3,(#67631,#67632,#67633,#67634,#67635,
#67636),.UNSPECIFIED.,.F.,.F.,(4,2,4),(-0.00212486385494385,-0.00106293276454614,
-1.00000000456354E-6),.UNSPECIFIED.);
#1376=B_SPLINE_CURVE_WITH_KNOTS('',3,(#67655,#67656,#67657,#67658,#67659,
#67660),.UNSPECIFIED.,.F.,.F.,(4,2,4),(0.,0.0198583386741828,0.0397175618451867),
 .UNSPECIFIED.);
#1377=B_SPLINE_CURVE_WITH_KNOTS('',3,(#67711,#67712,#67713,#67714,#67715,
#67716),.UNSPECIFIED.,.F.,.F.,(4,2,4),(0.,0.0199008240853172,0.0398025407040322),
 .UNSPECIFIED.);
#1378=B_SPLINE_CURVE_WITH_KNOTS('',3,(#67729,#67730,#67731,#67732,#67733,
#67734),.UNSPECIFIED.,.F.,.F.,(4,2,4),(0.,0.0199042047179996,0.0398092891748803),
 .UNSPECIFIED.);
#1379=B_SPLINE_CURVE_WITH_KNOTS('',3,(#67779,#67780,#67781,#67782,#67783,
#67784),.UNSPECIFIED.,.F.,.F.,(4,2,4),(0.,0.0198954793727932,0.0397918615634901),
 .UNSPECIFIED.);
#1380=B_SPLINE_CURVE_WITH_KNOTS('',3,(#67824,#67825,#67826,#67827,#67828,
#67829,#67830),.UNSPECIFIED.,.F.,.F.,(4,3,4),(0.,0.5,0.999990117126542),
 .UNSPECIFIED.);
#1381=B_SPLINE_CURVE_WITH_KNOTS('',3,(#67853,#67854,#67855,#67856,#67857,
#67858),.UNSPECIFIED.,.F.,.F.,(4,2,4),(0.,0.0198677119061941,0.0397363339249417),
 .UNSPECIFIED.);
#1382=B_SPLINE_CURVE_WITH_KNOTS('',3,(#67900,#67901,#67902,#67903,#67904,
#67905),.UNSPECIFIED.,.F.,.F.,(4,2,4),(0.,0.0198973966042074,0.0397956843497479),
 .UNSPECIFIED.);
#1383=B_SPLINE_CURVE_WITH_KNOTS('',3,(#67927,#67928,#67929,#67930,#67931,
#67932),.UNSPECIFIED.,.F.,.F.,(4,2,4),(0.,0.0199030679727059,0.0398070346286982),
 .UNSPECIFIED.);
#1384=B_SPLINE_CURVE_WITH_KNOTS('',3,(#67977,#67978,#67979,#67980,#67981,
#67982),.UNSPECIFIED.,.F.,.F.,(4,2,4),(0.,0.0198994178163347,0.0397997366745588),
 .UNSPECIFIED.);
#1385=B_SPLINE_CURVE_WITH_KNOTS('',3,(#67995,#67996,#67997,#67998,#67999,
#68000),.UNSPECIFIED.,.F.,.F.,(4,2,4),(0.,0.0198905179567855,0.0397819072575837),
 .UNSPECIFIED.);
#1386=B_SPLINE_CURVE_WITH_KNOTS('',3,(#68025,#68026,#68027,#68028,#68029,
#68030,#68031),.UNSPECIFIED.,.F.,.F.,(4,3,4),(0.0365944846647011,0.0384615384615384,
0.0431466153076599),.UNSPECIFIED.);
#1387=B_SPLINE_CURVE_WITH_KNOTS('',3,(#68032,#68033,#68034,#68035,#68036,
#68037,#68038,#68039),.UNSPECIFIED.,.F.,.F.,(4,2,2,4),(1.77256723985765E-6,
0.00863675584772395,0.017140965275147,0.0172811072181662),.UNSPECIFIED.);
#1388=B_SPLINE_CURVE_WITH_KNOTS('',3,(#68064,#68065,#68066,#68067,#68068,
#68069),.UNSPECIFIED.,.F.,.F.,(4,2,4),(0.,0.0198536183277256,0.0397081496406794),
 .UNSPECIFIED.);
#1389=B_SPLINE_CURVE_WITH_KNOTS('',3,(#68087,#68088,#68089,#68090,#68091,
#68092),.UNSPECIFIED.,.F.,.F.,(4,2,4),(-0.00212388605083564,-0.00106194091765259,
0.),.UNSPECIFIED.);
#1390=B_SPLINE_CURVE_WITH_KNOTS('',3,(#68093,#68094,#68095,#68096,#68097,
#68098),.UNSPECIFIED.,.F.,.F.,(4,2,4),(9.99998419401124E-7,0.0193527854087786,
0.0387045795309009),.UNSPECIFIED.);
#1391=B_SPLINE_CURVE_WITH_KNOTS('',3,(#68104,#68105,#68106,#68107,#68108,
#68109),.UNSPECIFIED.,.F.,.F.,(4,2,4),(-0.00212486447982969,-0.00106293277044209,
-9.99999998075674E-7),.UNSPECIFIED.);
#1392=B_SPLINE_CURVE_WITH_KNOTS('',3,(#68148,#68149,#68150,#68151,#68152,
#68153),.UNSPECIFIED.,.F.,.F.,(4,2,4),(0.,0.0198583386755922,0.0397175618510719),
 .UNSPECIFIED.);
#1393=B_SPLINE_CURVE_WITH_KNOTS('',3,(#68166,#68167,#68168,#68169,#68170,
#68171),.UNSPECIFIED.,.F.,.F.,(4,2,4),(0.,0.0198761965810603,0.039753284719404),
 .UNSPECIFIED.);
#1394=B_SPLINE_CURVE_WITH_KNOTS('',3,(#68212,#68213,#68214,#68215,#68216,
#68217),.UNSPECIFIED.,.F.,.F.,(4,2,4),(0.,0.0199042047183857,0.0398092891790922),
 .UNSPECIFIED.);
#1395=B_SPLINE_CURVE_WITH_KNOTS('',3,(#68242,#68243,#68244,#68245,#68246,
#68247),.UNSPECIFIED.,.F.,.F.,(4,2,4),(0.,0.0199008240861043,0.0398025407072504),
 .UNSPECIFIED.);
#1396=B_SPLINE_CURVE_WITH_KNOTS('',3,(#68291,#68292,#68293,#68294,#68295,
#68296),.UNSPECIFIED.,.F.,.F.,(4,2,4),(0.,0.0198954793743314,0.0397918615697323),
 .UNSPECIFIED.);
#1397=B_SPLINE_CURVE_WITH_KNOTS('',3,(#68336,#68337,#68338,#68339,#68340,
#68341,#68342),.UNSPECIFIED.,.F.,.F.,(4,3,4),(0.,0.5,0.9999901171293),
 .UNSPECIFIED.);
#1398=B_SPLINE_CURVE_WITH_KNOTS('',3,(#68365,#68366,#68367,#68368,#68369,
#68370),.UNSPECIFIED.,.F.,.F.,(4,2,4),(0.,0.0198677119105387,0.0397363339423693),
 .UNSPECIFIED.);
#1399=B_SPLINE_CURVE_WITH_KNOTS('',3,(#68412,#68413,#68414,#68415,#68416,
#68417),.UNSPECIFIED.,.F.,.F.,(4,2,4),(0.,0.019897396605077,0.0397956843531935),
 .UNSPECIFIED.);
#1400=B_SPLINE_CURVE_WITH_KNOTS('',3,(#68439,#68440,#68441,#68442,#68443,
#68444),.UNSPECIFIED.,.F.,.F.,(4,2,4),(0.,0.0199030679766039,0.0398070346443927),
 .UNSPECIFIED.);
#1401=B_SPLINE_CURVE_WITH_KNOTS('',3,(#68489,#68490,#68491,#68492,#68493,
#68494),.UNSPECIFIED.,.F.,.F.,(4,2,4),(0.,0.0198994178865019,0.0397997368880701),
 .UNSPECIFIED.);
#1402=B_SPLINE_CURVE_WITH_KNOTS('',3,(#68507,#68508,#68509,#68510,#68511,
#68512),.UNSPECIFIED.,.F.,.F.,(4,2,4),(0.,0.0198905179569301,0.0397819072590209),
 .UNSPECIFIED.);
#1403=B_SPLINE_CURVE_WITH_KNOTS('',3,(#68537,#68538,#68539,#68540,#68541,
#68542,#68543),.UNSPECIFIED.,.F.,.F.,(4,3,4),(0.0365944846647007,0.0384615384615384,
0.0431466153076595),.UNSPECIFIED.);
#1404=B_SPLINE_CURVE_WITH_KNOTS('',3,(#68544,#68545,#68546,#68547,#68548,
#68549,#68550,#68551),.UNSPECIFIED.,.F.,.F.,(4,2,2,4),(1.77256358031356E-6,
0.00863675581093288,0.017140951289934,0.0172810947306584),.UNSPECIFIED.);
#1405=B_SPLINE_CURVE_WITH_KNOTS('',3,(#68576,#68577,#68578,#68579,#68580,
#68581),.UNSPECIFIED.,.F.,.F.,(4,2,4),(0.,0.0198536183285242,0.0397081496440867),
 .UNSPECIFIED.);
#1406=B_SPLINE_CURVE_WITH_KNOTS('',3,(#68599,#68600,#68601,#68602,#68603,
#68604),.UNSPECIFIED.,.F.,.F.,(4,2,4),(-0.00212388353492024,-0.00106193992386253,
0.),.UNSPECIFIED.);
#1407=B_SPLINE_CURVE_WITH_KNOTS('',3,(#68605,#68606,#68607,#68608,#68609,
#68610),.UNSPECIFIED.,.F.,.F.,(4,2,4),(9.99998415477424E-7,0.0193522803902194,
0.0387045693967639),.UNSPECIFIED.);
#1408=B_SPLINE_CURVE_WITH_KNOTS('',3,(#68616,#68617,#68618,#68619,#68620,
#68621),.UNSPECIFIED.,.F.,.F.,(4,2,4),(-0.00212486501284603,-0.00106293275806993,
-9.99999997913477E-7),.UNSPECIFIED.);
#1409=B_SPLINE_CURVE_WITH_KNOTS('',3,(#68660,#68661,#68662,#68663,#68664,
#68665),.UNSPECIFIED.,.F.,.F.,(4,2,4),(0.,0.0198583386762458,0.0397175618534314),
 .UNSPECIFIED.);
#1410=B_SPLINE_CURVE_WITH_KNOTS('',3,(#68678,#68679,#68680,#68681,#68682,
#68683),.UNSPECIFIED.,.F.,.F.,(4,2,4),(0.,0.019876196696537,0.0397532849500752),
 .UNSPECIFIED.);
#1411=B_SPLINE_CURVE_WITH_KNOTS('',3,(#68735,#68736,#68737,#68738,#68739,
#68740),.UNSPECIFIED.,.F.,.F.,(4,2,4),(0.,0.0199008240870978,0.039802540710855),
 .UNSPECIFIED.);
#1412=B_SPLINE_CURVE_WITH_KNOTS('',3,(#68753,#68754,#68755,#68756,#68757,
#68758),.UNSPECIFIED.,.F.,.F.,(4,2,4),(0.,0.019904204718409,0.0398092891761761),
 .UNSPECIFIED.);
#1413=B_SPLINE_CURVE_WITH_KNOTS('',3,(#68817,#68818,#68819,#68820,#68821,
#68822),.UNSPECIFIED.,.F.,.F.,(4,2,4),(0.,0.0198954793770109,0.039791861578122),
 .UNSPECIFIED.);
#1414=B_SPLINE_CURVE_WITH_KNOTS('',3,(#68851,#68852,#68853,#68854,#68855,
#68856,#68857),.UNSPECIFIED.,.F.,.F.,(4,3,4),(0.,0.5,0.999990117130999),
 .UNSPECIFIED.);
#1415=B_SPLINE_CURVE_WITH_KNOTS('',3,(#68880,#68881,#68882,#68883,#68884,
#68885),.UNSPECIFIED.,.F.,.F.,(4,2,4),(0.,0.0198677119151675,0.0397363339609174),
 .UNSPECIFIED.);
#1416=B_SPLINE_CURVE_WITH_KNOTS('',3,(#68927,#68928,#68929,#68930,#68931,
#68932),.UNSPECIFIED.,.F.,.F.,(4,2,4),(0.,0.0198973966056516,0.039795684355372),
 .UNSPECIFIED.);
#1417=B_SPLINE_CURVE_WITH_KNOTS('',3,(#68954,#68955,#68956,#68957,#68958,
#68959),.UNSPECIFIED.,.F.,.F.,(4,2,4),(0.,0.0199030679802205,0.0398070346592923),
 .UNSPECIFIED.);
#1418=B_SPLINE_CURVE_WITH_KNOTS('',3,(#69004,#69005,#69006,#69007,#69008,
#69009),.UNSPECIFIED.,.F.,.F.,(4,2,4),(0.,0.0198994178870172,0.0397997368900241),
 .UNSPECIFIED.);
#1419=B_SPLINE_CURVE_WITH_KNOTS('',3,(#69022,#69023,#69024,#69025,#69026,
#69027),.UNSPECIFIED.,.F.,.F.,(4,2,4),(0.,0.0198905179567028,0.039781907256152),
 .UNSPECIFIED.);
#1420=B_SPLINE_CURVE_WITH_KNOTS('',3,(#69052,#69053,#69054,#69055,#69056,
#69057,#69058),.UNSPECIFIED.,.F.,.F.,(4,3,4),(0.0365944846647009,0.0384615384615384,
0.0431466153076596),.UNSPECIFIED.);
#1421=B_SPLINE_CURVE_WITH_KNOTS('',3,(#69059,#69060,#69061,#69062,#69063,
#69064,#69065,#69066),.UNSPECIFIED.,.F.,.F.,(4,2,2,4),(1.77256703655956E-6,
0.00863675592193242,0.017140984838655,0.0172811247032637),.UNSPECIFIED.);
#1422=B_SPLINE_CURVE_WITH_KNOTS('',3,(#69091,#69092,#69093,#69094,#69095,
#69096),.UNSPECIFIED.,.F.,.F.,(4,2,4),(0.,0.0198536183299061,0.0397081496493331),
 .UNSPECIFIED.);
#1423=B_SPLINE_CURVE_WITH_KNOTS('',3,(#69114,#69115,#69116,#69117,#69118,
#69119),.UNSPECIFIED.,.F.,.F.,(4,2,4),(-0.00212388200777003,-0.0010619393097638,
0.),.UNSPECIFIED.);
#1424=B_SPLINE_CURVE_WITH_KNOTS('',3,(#69120,#69121,#69122,#69123,#69124,
#69125),.UNSPECIFIED.,.F.,.F.,(4,2,4),(9.99998423274043E-7,0.01935278540972,
0.0387045795326976),.UNSPECIFIED.);
#1425=B_SPLINE_CURVE_WITH_KNOTS('',3,(#69131,#69132,#69133,#69134,#69135,
#69136),.UNSPECIFIED.,.F.,.F.,(4,2,4),(-0.0021248655886198,-0.00106293276740361,
-9.99999997247777E-7),.UNSPECIFIED.);
#1426=B_SPLINE_CURVE_WITH_KNOTS('',3,(#69175,#69176,#69177,#69178,#69179,
#69180),.UNSPECIFIED.,.F.,.F.,(4,2,4),(0.,0.0198583386771501,0.0397175618572917),
 .UNSPECIFIED.);
#1427=B_SPLINE_CURVE_WITH_KNOTS('',3,(#69193,#69194,#69195,#69196,#69197,
#69198),.UNSPECIFIED.,.F.,.F.,(4,2,4),(0.,0.0198761966897326,0.0397532849443772),
 .UNSPECIFIED.);
#1428=B_SPLINE_CURVE_WITH_KNOTS('',3,(#69250,#69251,#69252,#69253,#69254,
#69255),.UNSPECIFIED.,.F.,.F.,(4,2,4),(0.,0.0199008240880666,0.0398025407146116),
 .UNSPECIFIED.);
#1429=B_SPLINE_CURVE_WITH_KNOTS('',3,(#69268,#69269,#69270,#69271,#69272,
#69273),.UNSPECIFIED.,.F.,.F.,(4,2,4),(0.,0.0199042047186014,0.0398092891759251),
 .UNSPECIFIED.);
#1430=B_SPLINE_CURVE_WITH_KNOTS('',3,(#69321,#69322,#69323,#69324,#69325,
#69326),.UNSPECIFIED.,.F.,.F.,(4,2,4),(0.,0.019895479376471,0.039791861578371),
 .UNSPECIFIED.);
#1431=B_SPLINE_CURVE_WITH_KNOTS('',3,(#69366,#69367,#69368,#69369,#69370,
#69371,#69372),.UNSPECIFIED.,.F.,.F.,(4,3,4),(0.,0.5,0.999990117134267),
 .UNSPECIFIED.);
#1432=B_SPLINE_CURVE_WITH_KNOTS('',3,(#69395,#69396,#69397,#69398,#69399,
#69400),.UNSPECIFIED.,.F.,.F.,(4,2,4),(0.,0.0198677119197326,0.0397363339795572),
 .UNSPECIFIED.);
#1433=B_SPLINE_CURVE_WITH_KNOTS('',3,(#69442,#69443,#69444,#69445,#69446,
#69447),.UNSPECIFIED.,.F.,.F.,(4,2,4),(0.,0.0198973966056449,0.0397956843554118),
 .UNSPECIFIED.);
#1434=B_SPLINE_CURVE_WITH_KNOTS('',3,(#69469,#69470,#69471,#69472,#69473,
#69474),.UNSPECIFIED.,.F.,.F.,(4,2,4),(0.,0.0199030679854828,0.0398070346804227),
 .UNSPECIFIED.);
#1435=B_SPLINE_CURVE_WITH_KNOTS('',3,(#69519,#69520,#69521,#69522,#69523,
#69524),.UNSPECIFIED.,.F.,.F.,(4,2,4),(0.,0.0198994178876402,0.0397997368926258),
 .UNSPECIFIED.);
#1436=B_SPLINE_CURVE_WITH_KNOTS('',3,(#69537,#69538,#69539,#69540,#69541,
#69542),.UNSPECIFIED.,.F.,.F.,(4,2,4),(0.,0.019890517957229,0.0397819072577925),
 .UNSPECIFIED.);
#1437=B_SPLINE_CURVE_WITH_KNOTS('',3,(#69567,#69568,#69569,#69570,#69571,
#69572,#69573),.UNSPECIFIED.,.F.,.F.,(4,3,4),(0.036594484664701,0.0384615384615384,
0.0431466153076602),.UNSPECIFIED.);
#1438=B_SPLINE_CURVE_WITH_KNOTS('',3,(#69574,#69575,#69576,#69577,#69578,
#69579,#69580,#69581),.UNSPECIFIED.,.F.,.F.,(4,2,2,4),(1.77256732140101E-6,
0.00863675581872223,0.0171409391189963,0.0172810838451956),
 .UNSPECIFIED.);
#1439=B_SPLINE_CURVE_WITH_KNOTS('',3,(#69606,#69607,#69608,#69609,#69610,
#69611),.UNSPECIFIED.,.F.,.F.,(4,2,4),(0.,0.0198536183299362,0.0397081496494468),
 .UNSPECIFIED.);
#1440=B_SPLINE_CURVE_WITH_KNOTS('',3,(#69629,#69630,#69631,#69632,#69633,
#69634),.UNSPECIFIED.,.F.,.F.,(4,2,4),(-0.00212387831185543,-0.00106193782572264,
0.),.UNSPECIFIED.);
#1441=B_SPLINE_CURVE_WITH_KNOTS('',3,(#69635,#69636,#69637,#69638,#69639,
#69640),.UNSPECIFIED.,.F.,.F.,(4,2,4),(9.99998423982381E-7,0.0193522753882191,
0.038704569298396),.UNSPECIFIED.);
#1442=B_SPLINE_CURVE_WITH_KNOTS('',3,(#69646,#69647,#69648,#69649,#69650,
#69651),.UNSPECIFIED.,.F.,.F.,(4,2,4),(-0.00212486605241449,-0.00106293275969741,
-9.99999995914859E-7),.UNSPECIFIED.);
#1443=B_SPLINE_CURVE_WITH_KNOTS('',3,(#69690,#69691,#69692,#69693,#69694,
#69695),.UNSPECIFIED.,.F.,.F.,(4,2,4),(0.,0.019858338677387,0.0397175618584201),
 .UNSPECIFIED.);
#1444=B_SPLINE_CURVE_WITH_KNOTS('',3,(#69708,#69709,#69710,#69711,#69712,
#69713),.UNSPECIFIED.,.F.,.F.,(4,2,4),(0.,0.0198761967027802,0.0397532849636417),
 .UNSPECIFIED.);
#1445=B_SPLINE_CURVE_WITH_KNOTS('',3,(#69765,#69766,#69767,#69768,#69769,
#69770),.UNSPECIFIED.,.F.,.F.,(4,2,4),(0.,0.0199008240889834,0.039802540718122),
 .UNSPECIFIED.);
#1446=B_SPLINE_CURVE_WITH_KNOTS('',3,(#69783,#69784,#69785,#69786,#69787,
#69788),.UNSPECIFIED.,.F.,.F.,(4,2,4),(0.,0.0199042047184434,0.0398092891758487),
 .UNSPECIFIED.);
#1447=B_SPLINE_CURVE_WITH_KNOTS('',3,(#69836,#69837,#69838,#69839,#69840,
#69841),.UNSPECIFIED.,.F.,.F.,(4,2,4),(0.,0.0198954793771532,0.0397918615810156),
 .UNSPECIFIED.);
#1448=B_SPLINE_CURVE_WITH_KNOTS('',3,(#69881,#69882,#69883,#69884,#69885,
#69886,#69887),.UNSPECIFIED.,.F.,.F.,(4,3,4),(0.,0.5,0.999990117136375),
 .UNSPECIFIED.);
#1449=B_SPLINE_CURVE_WITH_KNOTS('',3,(#69910,#69911,#69912,#69913,#69914,
#69915),.UNSPECIFIED.,.F.,.F.,(4,2,4),(0.,0.0198677119243952,0.0397363339986725),
 .UNSPECIFIED.);
#1450=B_SPLINE_CURVE_WITH_KNOTS('',3,(#69957,#69958,#69959,#69960,#69961,
#69962),.UNSPECIFIED.,.F.,.F.,(4,2,4),(0.,0.0198973966060797,0.0397956843571033),
 .UNSPECIFIED.);
#1451=B_SPLINE_CURVE_WITH_KNOTS('',3,(#69984,#69985,#69986,#69987,#69988,
#69989),.UNSPECIFIED.,.F.,.F.,(4,2,4),(0.,0.0199030679898499,0.0398070346983652),
 .UNSPECIFIED.);
#1452=B_SPLINE_CURVE_WITH_KNOTS('',3,(#70034,#70035,#70036,#70037,#70038,
#70039),.UNSPECIFIED.,.F.,.F.,(4,2,4),(0.,0.0198994178878564,0.03979973689336),
 .UNSPECIFIED.);
#1453=B_SPLINE_CURVE_WITH_KNOTS('',3,(#70052,#70053,#70054,#70055,#70056,
#70057),.UNSPECIFIED.,.F.,.F.,(4,2,4),(0.,0.0198905179571636,0.0397819072599618),
 .UNSPECIFIED.);
#1454=B_SPLINE_CURVE_WITH_KNOTS('',3,(#70082,#70083,#70084,#70085,#70086,
#70087,#70088),.UNSPECIFIED.,.F.,.F.,(4,3,4),(0.0365944846647013,0.0384615384615384,
0.0431466153076604),.UNSPECIFIED.);
#1455=B_SPLINE_CURVE_WITH_KNOTS('',3,(#70089,#70090,#70091,#70092,#70093,
#70094,#70095,#70096),.UNSPECIFIED.,.F.,.F.,(4,2,2,4),(1.7725671724742E-6,
0.00863675585766041,0.0171409671998102,0.0172811089329915),
 .UNSPECIFIED.);
#1456=B_SPLINE_CURVE_WITH_KNOTS('',3,(#70121,#70122,#70123,#70124,#70125,
#70126),.UNSPECIFIED.,.F.,.F.,(4,2,4),(0.,0.0198536183343959,0.0397081496659324),
 .UNSPECIFIED.);
#1457=B_SPLINE_CURVE_WITH_KNOTS('',3,(#70144,#70145,#70146,#70147,#70148,
#70149),.UNSPECIFIED.,.F.,.F.,(4,2,4),(-0.00212387641773327,-0.0010619370665021,
0.),.UNSPECIFIED.);
#1458=B_SPLINE_CURVE_WITH_KNOTS('',3,(#70150,#70151,#70152,#70153,#70154,
#70155),.UNSPECIFIED.,.F.,.F.,(4,2,4),(9.99998414701243E-7,0.0193527803906903,
0.0387045693989795),.UNSPECIFIED.);
#1459=B_SPLINE_CURVE_WITH_KNOTS('',3,(#70161,#70162,#70163,#70164,#70165,
#70166),.UNSPECIFIED.,.F.,.F.,(4,2,4),(-0.00212486654942059,-0.00106293276399481,
-9.99999993921228E-7),.UNSPECIFIED.);
#1460=B_SPLINE_CURVE_WITH_KNOTS('',3,(#70205,#70206,#70207,#70208,#70209,
#70210),.UNSPECIFIED.,.F.,.F.,(4,2,4),(0.,0.0198583386780391,0.0397175618608395),
 .UNSPECIFIED.);
#1461=B_SPLINE_CURVE_WITH_KNOTS('',3,(#70223,#70224,#70225,#70226,#70227,
#70228),.UNSPECIFIED.,.F.,.F.,(4,2,4),(0.,0.0198761967007073,0.0397532849594556),
 .UNSPECIFIED.);
#1462=B_SPLINE_CURVE_WITH_KNOTS('',3,(#70280,#70281,#70282,#70283,#70284,
#70285),.UNSPECIFIED.,.F.,.F.,(4,2,4),(0.,0.0199008240893237,0.0398025407191679),
 .UNSPECIFIED.);
#1463=B_SPLINE_CURVE_WITH_KNOTS('',3,(#70298,#70299,#70300,#70301,#70302,
#70303),.UNSPECIFIED.,.F.,.F.,(4,2,4),(0.,0.0199042047187462,0.0398092891746098),
 .UNSPECIFIED.);
#1464=B_SPLINE_CURVE_WITH_KNOTS('',3,(#70351,#70352,#70353,#70354,#70355,
#70356),.UNSPECIFIED.,.F.,.F.,(4,2,4),(0.,0.019895479377941,0.0397918615841521),
 .UNSPECIFIED.);
#1465=B_SPLINE_CURVE_WITH_KNOTS('',3,(#70396,#70397,#70398,#70399,#70400,
#70401,#70402),.UNSPECIFIED.,.F.,.F.,(4,3,4),(0.,0.5,0.999990117139493),
 .UNSPECIFIED.);
#1466=B_SPLINE_CURVE_WITH_KNOTS('',3,(#70425,#70426,#70427,#70428,#70429,
#70430),.UNSPECIFIED.,.F.,.F.,(4,2,4),(0.,0.0198677119298734,0.0397363340203713),
 .UNSPECIFIED.);
#1467=B_SPLINE_CURVE_WITH_KNOTS('',3,(#70472,#70473,#70474,#70475,#70476,
#70477),.UNSPECIFIED.,.F.,.F.,(4,2,4),(0.,0.019897396605761,0.0397956843558467),
 .UNSPECIFIED.);
#1468=B_SPLINE_CURVE_WITH_KNOTS('',3,(#70499,#70500,#70501,#70502,#70503,
#70504),.UNSPECIFIED.,.F.,.F.,(4,2,4),(0.,0.0199030679943856,0.0398070347169293),
 .UNSPECIFIED.);
#1469=B_SPLINE_CURVE_WITH_KNOTS('',3,(#70549,#70550,#70551,#70552,#70553,
#70554),.UNSPECIFIED.,.F.,.F.,(4,2,4),(0.,0.0198994178880039,0.0397997368943815),
 .UNSPECIFIED.);
#1470=B_SPLINE_CURVE_WITH_KNOTS('',3,(#70567,#70568,#70569,#70570,#70571,
#70572),.UNSPECIFIED.,.F.,.F.,(4,2,4),(0.,0.0198905179572561,0.039781907255197),
 .UNSPECIFIED.);
#1471=B_SPLINE_CURVE_WITH_KNOTS('',3,(#70597,#70598,#70599,#70600,#70601,
#70602,#70603),.UNSPECIFIED.,.F.,.F.,(4,3,4),(0.0365944846647005,0.0384615384615384,
0.04314661530766),.UNSPECIFIED.);
#1472=B_SPLINE_CURVE_WITH_KNOTS('',3,(#70604,#70605,#70606,#70607,#70608,
#70609,#70610,#70611),.UNSPECIFIED.,.F.,.F.,(4,2,2,4),(1.77256358748408E-6,
0.00863675582048878,0.0171409428335954,0.0172810871701512),
 .UNSPECIFIED.);
#1473=B_SPLINE_CURVE_WITH_KNOTS('',3,(#70636,#70637,#70638,#70639,#70640,
#70641),.UNSPECIFIED.,.F.,.F.,(4,2,4),(0.,0.0198536183313603,0.0397081496548265),
 .UNSPECIFIED.);
#1474=B_SPLINE_CURVE_WITH_KNOTS('',3,(#70659,#70660,#70661,#70662,#70663,
#70664),.UNSPECIFIED.,.F.,.F.,(4,2,4),(-0.00212387341997532,-0.00106193587239301,
0.),.UNSPECIFIED.);
#1475=B_SPLINE_CURVE_WITH_KNOTS('',3,(#70665,#70666,#70667,#70668,#70669,
#70670),.UNSPECIFIED.,.F.,.F.,(4,2,4),(9.99998417067894E-7,0.0193527854098381,
0.0387045795330794),.UNSPECIFIED.);
#1476=B_SPLINE_CURVE_WITH_KNOTS('',3,(#70676,#70677,#70678,#70679,#70680,
#70681),.UNSPECIFIED.,.F.,.F.,(4,2,4),(-0.00212486691426954,-0.00106293276048919,
-9.99999995782153E-7),.UNSPECIFIED.);
#1477=B_SPLINE_CURVE_WITH_KNOTS('',3,(#70720,#70721,#70722,#70723,#70724,
#70725),.UNSPECIFIED.,.F.,.F.,(4,2,4),(0.,0.0198583386780509,0.0397175618608029),
 .UNSPECIFIED.);
#1478=B_SPLINE_CURVE_WITH_KNOTS('',3,(#70738,#70739,#70740,#70741,#70742,
#70743),.UNSPECIFIED.,.F.,.F.,(4,2,4),(0.,0.019876196698291,0.0397532849502144),
 .UNSPECIFIED.);
#1479=B_SPLINE_CURVE_WITH_KNOTS('',3,(#70795,#70796,#70797,#70798,#70799,
#70800),.UNSPECIFIED.,.F.,.F.,(4,2,4),(0.,0.0199008240898987,0.0398025407215578),
 .UNSPECIFIED.);
#1480=B_SPLINE_CURVE_WITH_KNOTS('',3,(#70813,#70814,#70815,#70816,#70817,
#70818),.UNSPECIFIED.,.F.,.F.,(4,2,4),(0.,0.0199042047126661,0.0398092891636698),
 .UNSPECIFIED.);
#1481=B_SPLINE_CURVE_WITH_KNOTS('',3,(#70866,#70867,#70868,#70869,#70870,
#70871),.UNSPECIFIED.,.F.,.F.,(4,2,4),(0.,0.0198954793785179,0.0397918615868151),
 .UNSPECIFIED.);
#1482=B_SPLINE_CURVE_WITH_KNOTS('',3,(#70911,#70912,#70913,#70914,#70915,
#70916,#70917),.UNSPECIFIED.,.F.,.F.,(4,3,4),(0.,0.5,0.99999011714245),
 .UNSPECIFIED.);
#1483=B_SPLINE_CURVE_WITH_KNOTS('',3,(#70940,#70941,#70942,#70943,#70944,
#70945),.UNSPECIFIED.,.F.,.F.,(4,2,4),(0.,0.0198677119349441,0.0397363340407095),
 .UNSPECIFIED.);
#1484=B_SPLINE_CURVE_WITH_KNOTS('',3,(#70987,#70988,#70989,#70990,#70991,
#70992),.UNSPECIFIED.,.F.,.F.,(4,2,4),(0.,0.0198973966055972,0.0397956843554853),
 .UNSPECIFIED.);
#1485=B_SPLINE_CURVE_WITH_KNOTS('',3,(#71014,#71015,#71016,#71017,#71018,
#71019),.UNSPECIFIED.,.F.,.F.,(4,2,4),(0.,0.0199030680000759,0.0398070347395109),
 .UNSPECIFIED.);
#1486=B_SPLINE_CURVE_WITH_KNOTS('',3,(#71064,#71065,#71066,#71067,#71068,
#71069),.UNSPECIFIED.,.F.,.F.,(4,2,4),(0.,0.0198994178881233,0.0397997368947557),
 .UNSPECIFIED.);
#1487=B_SPLINE_CURVE_WITH_KNOTS('',3,(#71082,#71083,#71084,#71085,#71086,
#71087),.UNSPECIFIED.,.F.,.F.,(4,2,4),(0.,0.0198905179572044,0.039781907261386),
 .UNSPECIFIED.);
#1488=B_SPLINE_CURVE_WITH_KNOTS('',3,(#71112,#71113,#71114,#71115,#71116,
#71117,#71118),.UNSPECIFIED.,.F.,.F.,(4,3,4),(0.0365944846647007,0.0384615384615384,
0.0431466153076593),.UNSPECIFIED.);
#1489=B_SPLINE_CURVE_WITH_KNOTS('',3,(#71119,#71120,#71121,#71122,#71123,
#71124,#71125,#71126),.UNSPECIFIED.,.F.,.F.,(4,2,2,4),(1.77256357976421E-6,
0.00863675581873873,0.017140945662596,0.0172810896980204),.UNSPECIFIED.);
#1490=B_SPLINE_CURVE_WITH_KNOTS('',3,(#71151,#71152,#71153,#71154,#71155,
#71156),.UNSPECIFIED.,.F.,.F.,(4,2,4),(0.,0.0198536183310732,0.03970814965373),
 .UNSPECIFIED.);
#1491=B_SPLINE_CURVE_WITH_KNOTS('',3,(#71174,#71175,#71176,#71177,#71178,
#71179),.UNSPECIFIED.,.F.,.F.,(4,2,4),(-0.00212387063254784,-0.00106193475602023,
0.),.UNSPECIFIED.);
#1492=B_SPLINE_CURVE_WITH_KNOTS('',3,(#71180,#71181,#71182,#71183,#71184,
#71185),.UNSPECIFIED.,.F.,.F.,(4,2,4),(9.99998414999011E-7,0.0193527753884389,
0.0387045692999441),.UNSPECIFIED.);
#1493=B_SPLINE_CURVE_WITH_KNOTS('',3,(#71191,#71192,#71193,#71194,#71195,
#71196),.UNSPECIFIED.,.F.,.F.,(4,2,4),(-0.00212486729427008,-0.00106293276111579,
-9.99999993211292E-7),.UNSPECIFIED.);
#1494=B_SPLINE_CURVE_WITH_KNOTS('',3,(#71235,#71236,#71237,#71238,#71239,
#71240),.UNSPECIFIED.,.F.,.F.,(4,2,4),(0.,0.019858338678372,0.0397175618622352),
 .UNSPECIFIED.);
#1495=B_SPLINE_CURVE_WITH_KNOTS('',3,(#71253,#71254,#71255,#71256,#71257,
#71258),.UNSPECIFIED.,.F.,.F.,(4,2,4),(0.,0.0198761967066437,0.0397532849678352),
 .UNSPECIFIED.);
#1496=B_SPLINE_CURVE_WITH_KNOTS('',3,(#71310,#71311,#71312,#71313,#71314,
#71315),.UNSPECIFIED.,.F.,.F.,(4,2,4),(0.,0.0199008240895588,0.0398025407203014),
 .UNSPECIFIED.);
#1497=B_SPLINE_CURVE_WITH_KNOTS('',3,(#71328,#71329,#71330,#71331,#71332,
#71333),.UNSPECIFIED.,.F.,.F.,(4,2,4),(0.,0.0199042046961962,0.0398092891330403),
 .UNSPECIFIED.);
#1498=B_SPLINE_CURVE_WITH_KNOTS('',3,(#71381,#71382,#71383,#71384,#71385,
#71386),.UNSPECIFIED.,.F.,.F.,(4,2,4),(0.,0.0198954793788172,0.0397918615878541),
 .UNSPECIFIED.);
#1499=B_SPLINE_CURVE_WITH_KNOTS('',3,(#71426,#71427,#71428,#71429,#71430,
#71431,#71432),.UNSPECIFIED.,.F.,.F.,(4,3,4),(0.,0.5,0.999990117145692),
 .UNSPECIFIED.);
#1500=B_SPLINE_CURVE_WITH_KNOTS('',3,(#71455,#71456,#71457,#71458,#71459,
#71460),.UNSPECIFIED.,.F.,.F.,(4,2,4),(0.,0.0198677119382913,0.0397363340538751),
 .UNSPECIFIED.);
#1501=B_SPLINE_CURVE_WITH_KNOTS('',3,(#71502,#71503,#71504,#71505,#71506,
#71507),.UNSPECIFIED.,.F.,.F.,(4,2,4),(0.,0.0198973966054705,0.0397956843550537),
 .UNSPECIFIED.);
#1502=B_SPLINE_CURVE_WITH_KNOTS('',3,(#71529,#71530,#71531,#71532,#71533,
#71534),.UNSPECIFIED.,.F.,.F.,(4,2,4),(0.,0.019903068003928,0.0398070347549453),
 .UNSPECIFIED.);
#1503=B_SPLINE_CURVE_WITH_KNOTS('',3,(#71579,#71580,#71581,#71582,#71583,
#71584),.UNSPECIFIED.,.F.,.F.,(4,2,4),(0.,0.0198994178874679,0.0397997368920064),
 .UNSPECIFIED.);
#1504=B_SPLINE_CURVE_WITH_KNOTS('',3,(#71597,#71598,#71599,#71600,#71601,
#71602),.UNSPECIFIED.,.F.,.F.,(4,2,4),(0.,0.0198905174414553,0.0397819062199287),
 .UNSPECIFIED.);
#1505=B_SPLINE_CURVE_WITH_KNOTS('',3,(#71627,#71628,#71629,#71630,#71631,
#71632,#71633),.UNSPECIFIED.,.F.,.F.,(4,3,4),(0.0365944846647015,0.0384615384615384,
0.0431466153076595),.UNSPECIFIED.);
#1506=B_SPLINE_CURVE_WITH_KNOTS('',3,(#71634,#71635,#71636,#71637,#71638,
#71639,#71640,#71641),.UNSPECIFIED.,.F.,.F.,(4,2,2,4),(1.77291495321644E-6,
0.00863675579526595,0.0171409306756836,0.0172810762685451),
 .UNSPECIFIED.);
#1507=B_SPLINE_CURVE_WITH_KNOTS('',3,(#71666,#71667,#71668,#71669,#71670,
#71671),.UNSPECIFIED.,.F.,.F.,(4,2,4),(0.,0.0198536183312814,0.0397081496542885),
 .UNSPECIFIED.);
#1508=B_SPLINE_CURVE_WITH_KNOTS('',3,(#71689,#71690,#71691,#71692,#71693,
#71694),.UNSPECIFIED.,.F.,.F.,(4,2,4),(-0.00212386760957224,-0.00106193354766672,
0.),.UNSPECIFIED.);
#1509=B_SPLINE_CURVE_WITH_KNOTS('',3,(#71695,#71696,#71697,#71698,#71699,
#71700),.UNSPECIFIED.,.F.,.F.,(4,2,4),(9.99998413909848E-7,0.0193527748421895,
0.038704569287749),.UNSPECIFIED.);
#1510=B_SPLINE_CURVE_WITH_KNOTS('',3,(#71706,#71707,#71708,#71709,#71710,
#71711),.UNSPECIFIED.,.F.,.F.,(4,2,4),(-0.0021248675435194,-0.00106293275918252,
-1.00000000268332E-6),.UNSPECIFIED.);
#1511=B_SPLINE_CURVE_WITH_KNOTS('',3,(#71750,#71751,#71752,#71753,#71754,
#71755),.UNSPECIFIED.,.F.,.F.,(4,2,4),(0.,0.0198583386782803,0.0397175618619299),
 .UNSPECIFIED.);
#1512=B_SPLINE_CURVE_WITH_KNOTS('',3,(#71768,#71769,#71770,#71771,#71772,
#71773),.UNSPECIFIED.,.F.,.F.,(4,2,4),(0.,0.0198761966619282,0.0397532848848484),
 .UNSPECIFIED.);
#1513=B_SPLINE_CURVE_WITH_KNOTS('',3,(#71825,#71826,#71827,#71828,#71829,
#71830),.UNSPECIFIED.,.F.,.F.,(4,2,4),(0.,0.0199008240900917,0.0398025407223278),
 .UNSPECIFIED.);
#1514=B_SPLINE_CURVE_WITH_KNOTS('',3,(#71843,#71844,#71845,#71846,#71847,
#71848),.UNSPECIFIED.,.F.,.F.,(4,2,4),(0.,0.0199042047128343,0.0398092891614523),
 .UNSPECIFIED.);
#1515=B_SPLINE_CURVE_WITH_KNOTS('',3,(#71896,#71897,#71898,#71899,#71900,
#71901),.UNSPECIFIED.,.F.,.F.,(4,2,4),(0.,0.0198954793788647,0.0397918615880732),
 .UNSPECIFIED.);
#1516=B_SPLINE_CURVE_WITH_KNOTS('',3,(#71941,#71942,#71943,#71944,#71945,
#71946,#71947),.UNSPECIFIED.,.F.,.F.,(4,3,4),(0.,0.5,0.999990117148444),
 .UNSPECIFIED.);
#1517=B_SPLINE_CURVE_WITH_KNOTS('',3,(#71970,#71971,#71972,#71973,#71974,
#71975),.UNSPECIFIED.,.F.,.F.,(4,2,4),(0.,0.0198677119395526,0.0397363340592826),
 .UNSPECIFIED.);
#1518=B_SPLINE_CURVE_WITH_KNOTS('',3,(#72017,#72018,#72019,#72020,#72021,
#72022),.UNSPECIFIED.,.F.,.F.,(4,2,4),(0.,0.0198973966050765,0.0397956843534938),
 .UNSPECIFIED.);
#1519=B_SPLINE_CURVE_WITH_KNOTS('',3,(#72044,#72045,#72046,#72047,#72048,
#72049),.UNSPECIFIED.,.F.,.F.,(4,2,4),(0.,0.0199030680059554,0.0398070347632472),
 .UNSPECIFIED.);
#1520=B_SPLINE_CURVE_WITH_KNOTS('',3,(#72094,#72095,#72096,#72097,#72098,
#72099),.UNSPECIFIED.,.F.,.F.,(4,2,4),(0.,0.0198994178873714,0.0397997368914788),
 .UNSPECIFIED.);
#1521=B_SPLINE_CURVE_WITH_KNOTS('',3,(#72112,#72113,#72114,#72115,#72116,
#72117),.UNSPECIFIED.,.F.,.F.,(4,2,4),(0.,0.0198905179568428,0.0397819072611588),
 .UNSPECIFIED.);
#1522=B_SPLINE_CURVE_WITH_KNOTS('',3,(#72142,#72143,#72144,#72145,#72146,
#72147,#72148),.UNSPECIFIED.,.F.,.F.,(4,3,4),(0.0365944846647007,0.0384615384615384,
0.0431466153076601),.UNSPECIFIED.);
#1523=B_SPLINE_CURVE_WITH_KNOTS('',3,(#72149,#72150,#72151,#72152,#72153,
#72154,#72155,#72156),.UNSPECIFIED.,.F.,.F.,(4,2,2,4),(1.77349251834674E-6,
0.00863675583297312,0.017140940164705,0.0172810846677369),.UNSPECIFIED.);
#1524=B_SPLINE_CURVE_WITH_KNOTS('',3,(#72181,#72182,#72183,#72184,#72185,
#72186),.UNSPECIFIED.,.F.,.F.,(4,2,4),(0.,0.0198536183306229,0.0397081496516829),
 .UNSPECIFIED.);
#1525=B_SPLINE_CURVE_WITH_KNOTS('',3,(#72204,#72205,#72206,#72207,#72208,
#72209),.UNSPECIFIED.,.F.,.F.,(4,2,4),(-0.00212386483367974,-0.00106193243731324,
0.),.UNSPECIFIED.);
#1526=B_SPLINE_CURVE_WITH_KNOTS('',3,(#72210,#72211,#72212,#72213,#72214,
#72215),.UNSPECIFIED.,.F.,.F.,(4,2,4),(9.99998414062903E-7,0.0193527795959641,
0.0387045693836927),.UNSPECIFIED.);
#1527=B_SPLINE_CURVE_WITH_KNOTS('',3,(#72221,#72222,#72223,#72224,#72225,
#72226),.UNSPECIFIED.,.F.,.F.,(4,2,4),(-0.0021248677897174,-0.00106293276009572,
-1.0000000007246E-6),.UNSPECIFIED.);
#1528=B_SPLINE_CURVE_WITH_KNOTS('',3,(#72265,#72266,#72267,#72268,#72269,
#72270),.UNSPECIFIED.,.F.,.F.,(4,2,4),(0.,0.0198583386780633,0.0397175618609683),
 .UNSPECIFIED.);
#1529=B_SPLINE_CURVE_WITH_KNOTS('',3,(#72283,#72284,#72285,#72286,#72287,
#72288),.UNSPECIFIED.,.F.,.F.,(4,2,4),(0.,0.0198761965838071,0.0397532847185604),
 .UNSPECIFIED.);
#1530=B_SPLINE_CURVE_WITH_KNOTS('',3,(#72340,#72341,#72342,#72343,#72344,
#72345),.UNSPECIFIED.,.F.,.F.,(4,2,4),(0.,0.0199008240900329,0.0398025407218782),
 .UNSPECIFIED.);
#1531=B_SPLINE_CURVE_WITH_KNOTS('',3,(#72358,#72359,#72360,#72361,#72362,
#72363),.UNSPECIFIED.,.F.,.F.,(4,2,4),(0.,0.0199042047189754,0.0398092891731179),
 .UNSPECIFIED.);
#1532=B_SPLINE_CURVE_WITH_KNOTS('',3,(#72411,#72412,#72413,#72414,#72415,
#72416),.UNSPECIFIED.,.F.,.F.,(4,2,4),(0.,0.0198954793789966,0.0397918615887045),
 .UNSPECIFIED.);
#1533=B_SPLINE_CURVE_WITH_KNOTS('',3,(#72456,#72457,#72458,#72459,#72460,
#72461,#72462),.UNSPECIFIED.,.F.,.F.,(4,3,4),(0.,0.5,0.999990117151347),
 .UNSPECIFIED.);
#1534=B_SPLINE_CURVE_WITH_KNOTS('',3,(#72485,#72486,#72487,#72488,#72489,
#72490),.UNSPECIFIED.,.F.,.F.,(4,2,4),(0.,0.0198677119409769,0.0397363340651177),
 .UNSPECIFIED.);
#1535=B_SPLINE_CURVE_WITH_KNOTS('',3,(#72532,#72533,#72534,#72535,#72536,
#72537),.UNSPECIFIED.,.F.,.F.,(4,2,4),(0.,0.0198973966047253,0.0397956843521631),
 .UNSPECIFIED.);
#1536=B_SPLINE_CURVE_WITH_KNOTS('',3,(#72559,#72560,#72561,#72562,#72563,
#72564),.UNSPECIFIED.,.F.,.F.,(4,2,4),(0.,0.0199030680072161,0.0398070347685307),
 .UNSPECIFIED.);
#1537=B_SPLINE_CURVE_WITH_KNOTS('',3,(#72609,#72610,#72611,#72612,#72613,
#72614),.UNSPECIFIED.,.F.,.F.,(4,2,4),(0.,0.0198994178862985,0.0397997368875154),
 .UNSPECIFIED.);
#1538=B_SPLINE_CURVE_WITH_KNOTS('',3,(#72627,#72628,#72629,#72630,#72631,
#72632),.UNSPECIFIED.,.F.,.F.,(4,2,4),(0.,0.0198905179568695,0.0397819072595301),
 .UNSPECIFIED.);
#1539=B_SPLINE_CURVE_WITH_KNOTS('',3,(#72657,#72658,#72659,#72660,#72661,
#72662,#72663),.UNSPECIFIED.,.F.,.F.,(4,3,4),(0.0365944846647013,0.0384615384615384,
0.0431466153076599),.UNSPECIFIED.);
#1540=B_SPLINE_CURVE_WITH_KNOTS('',3,(#72664,#72665,#72666,#72667,#72668,
#72669,#72670,#72671),.UNSPECIFIED.,.F.,.F.,(4,2,2,4),(1.77256738873533E-6,
0.00863675579260533,0.0171409324946532,0.0172810779368845),
 .UNSPECIFIED.);
#1541=B_SPLINE_CURVE_WITH_KNOTS('',3,(#72696,#72697,#72698,#72699,#72700,
#72701),.UNSPECIFIED.,.F.,.F.,(4,2,4),(0.,0.0198536183302958,0.0397081496500012),
 .UNSPECIFIED.);
#1542=B_SPLINE_CURVE_WITH_KNOTS('',3,(#72719,#72720,#72721,#72722,#72723,
#72724),.UNSPECIFIED.,.F.,.F.,(4,2,4),(-0.00212386114999187,-0.00106193096416825,
0.),.UNSPECIFIED.);
#1543=B_SPLINE_CURVE_WITH_KNOTS('',3,(#72725,#72726,#72727,#72728,#72729,
#72730),.UNSPECIFIED.,.F.,.F.,(4,2,4),(9.99998414494249E-7,0.0193527803897854,
0.0387045693971851),.UNSPECIFIED.);
#1544=B_SPLINE_CURVE_WITH_KNOTS('',3,(#72736,#72737,#72738,#72739,#72740,
#72741),.UNSPECIFIED.,.F.,.F.,(4,2,4),(-0.00212486788589273,-0.00106293275882422,
-1.00000000009728E-6),.UNSPECIFIED.);
#1545=B_SPLINE_CURVE_WITH_KNOTS('',3,(#72780,#72781,#72782,#72783,#72784,
#72785),.UNSPECIFIED.,.F.,.F.,(4,2,4),(0.,0.0198583386778968,0.0397175618601019),
 .UNSPECIFIED.);
#1546=B_SPLINE_CURVE_WITH_KNOTS('',3,(#72798,#72799,#72800,#72801,#72802,
#72803),.UNSPECIFIED.,.F.,.F.,(4,2,4),(0.,0.0198761967018805,0.0397532849590274),
 .UNSPECIFIED.);
#1547=B_SPLINE_CURVE_WITH_KNOTS('',3,(#72855,#72856,#72857,#72858,#72859,
#72860),.UNSPECIFIED.,.F.,.F.,(4,2,4),(0.,0.0199008240895138,0.0398025407194746),
 .UNSPECIFIED.);
#1548=B_SPLINE_CURVE_WITH_KNOTS('',3,(#72873,#72874,#72875,#72876,#72877,
#72878),.UNSPECIFIED.,.F.,.F.,(4,2,4),(0.,0.0199042047188044,0.0398092891658421),
 .UNSPECIFIED.);
#1549=B_SPLINE_CURVE_WITH_KNOTS('',3,(#72926,#72927,#72928,#72929,#72930,
#72931),.UNSPECIFIED.,.F.,.F.,(4,2,4),(0.,0.0198954793786522,0.0397918615872593),
 .UNSPECIFIED.);
#1550=B_SPLINE_CURVE_WITH_KNOTS('',3,(#72971,#72972,#72973,#72974,#72975,
#72976,#72977),.UNSPECIFIED.,.F.,.F.,(4,3,4),(0.,0.5,0.99999011715422),
 .UNSPECIFIED.);
#1551=B_SPLINE_CURVE_WITH_KNOTS('',3,(#73000,#73001,#73002,#73003,#73004,
#73005),.UNSPECIFIED.,.F.,.F.,(4,2,4),(0.,0.0198677119426146,0.0397363340713369),
 .UNSPECIFIED.);
#1552=B_SPLINE_CURVE_WITH_KNOTS('',3,(#73047,#73048,#73049,#73050,#73051,
#73052),.UNSPECIFIED.,.F.,.F.,(4,2,4),(0.,0.0198973966035302,0.0397956843468986),
 .UNSPECIFIED.);
#1553=B_SPLINE_CURVE_WITH_KNOTS('',3,(#73074,#73075,#73076,#73077,#73078,
#73079),.UNSPECIFIED.,.F.,.F.,(4,2,4),(0.,0.0199030680084652,0.0398070347735349),
 .UNSPECIFIED.);
#1554=B_SPLINE_CURVE_WITH_KNOTS('',3,(#73121,#73122,#73123,#73124,#73125,
#73126),.UNSPECIFIED.,.F.,.F.,(4,2,4),(0.,0.0198994178853394,0.0397997368837477),
 .UNSPECIFIED.);
#1555=B_SPLINE_CURVE_WITH_KNOTS('',3,(#73146,#73147,#73148,#73149,#73150,
#73151),.UNSPECIFIED.,.F.,.F.,(4,2,4),(0.,0.0198905727746721,0.0397820348055632),
 .UNSPECIFIED.);
#1556=B_SPLINE_CURVE_WITH_KNOTS('',3,(#73176,#73177,#73178,#73179,#73180,
#73181,#73182),.UNSPECIFIED.,.F.,.F.,(4,3,4),(0.0365944846647006,0.0384615384615384,
0.0431466153076602),.UNSPECIFIED.);
#1557=B_SPLINE_CURVE_WITH_KNOTS('',3,(#73183,#73184,#73185,#73186,#73187,
#73188,#73189,#73190),.UNSPECIFIED.,.F.,.F.,(4,2,2,4),(1.77256368440199E-6,
0.00863675579558576,0.0171409356063339,0.0172810807143027),
 .UNSPECIFIED.);
#1558=B_SPLINE_CURVE_WITH_KNOTS('',3,(#73215,#73216,#73217,#73218,#73219,
#73220),.UNSPECIFIED.,.F.,.F.,(4,2,4),(0.,0.0198536183296266,0.0397081496475667),
 .UNSPECIFIED.);
#1559=B_SPLINE_CURVE_WITH_KNOTS('',3,(#73238,#73239,#73240,#73241,#73242,
#73243),.UNSPECIFIED.,.F.,.F.,(4,2,4),(-0.0021238584746236,-0.00106192989366009,
0.),.UNSPECIFIED.);
#1560=B_SPLINE_CURVE_WITH_KNOTS('',3,(#73244,#73245,#73246,#73247,#73248,
#73249),.UNSPECIFIED.,.F.,.F.,(4,2,4),(9.99998415229336E-7,0.0193527803903097,
0.0387045693981831),.UNSPECIFIED.);
#1561=B_SPLINE_CURVE_WITH_KNOTS('',3,(#73255,#73256,#73257,#73258,#73259,
#73260),.UNSPECIFIED.,.F.,.F.,(4,2,4),(-0.00212486797083145,-0.00106293275865109,
-9.99999996147095E-7),.UNSPECIFIED.);
#1562=B_SPLINE_CURVE_WITH_KNOTS('',3,(#73299,#73300,#73301,#73302,#73303,
#73304),.UNSPECIFIED.,.F.,.F.,(4,2,4),(0.,0.0198583386770375,0.0397175618570197),
 .UNSPECIFIED.);
#1563=B_SPLINE_CURVE_WITH_KNOTS('',3,(#73317,#73318,#73319,#73320,#73321,
#73322),.UNSPECIFIED.,.F.,.F.,(4,2,4),(0.,0.0198761965570183,0.039753284662268),
 .UNSPECIFIED.);
#1564=B_SPLINE_CURVE_WITH_KNOTS('',3,(#73374,#73375,#73376,#73377,#73378,
#73379),.UNSPECIFIED.,.F.,.F.,(4,2,4),(0.,0.0199008240890413,0.0398025407175076),
 .UNSPECIFIED.);
#1565=B_SPLINE_CURVE_WITH_KNOTS('',3,(#73392,#73393,#73394,#73395,#73396,
#73397),.UNSPECIFIED.,.F.,.F.,(4,2,4),(0.,0.0199042047190454,0.0398092891796812),
 .UNSPECIFIED.);
#1566=B_SPLINE_CURVE_WITH_KNOTS('',3,(#73445,#73446,#73447,#73448,#73449,
#73450),.UNSPECIFIED.,.F.,.F.,(4,2,4),(0.,0.019895479378126,0.0397918615851958),
 .UNSPECIFIED.);
#1567=B_SPLINE_CURVE_WITH_KNOTS('',3,(#73490,#73491,#73492,#73493,#73494,
#73495,#73496),.UNSPECIFIED.,.F.,.F.,(4,3,4),(0.,0.5,0.999990117157017),
 .UNSPECIFIED.);
#1568=B_SPLINE_CURVE_WITH_KNOTS('',3,(#73519,#73520,#73521,#73522,#73523,
#73524),.UNSPECIFIED.,.F.,.F.,(4,2,4),(0.,0.0198677119443712,0.0397363340782618),
 .UNSPECIFIED.);
#1569=B_SPLINE_CURVE_WITH_KNOTS('',3,(#73566,#73567,#73568,#73569,#73570,
#73571),.UNSPECIFIED.,.F.,.F.,(4,2,4),(0.,0.0198973966024781,0.0397956843428114),
 .UNSPECIFIED.);
#1570=B_SPLINE_CURVE_WITH_KNOTS('',3,(#73593,#73594,#73595,#73596,#73597,
#73598),.UNSPECIFIED.,.F.,.F.,(4,2,4),(0.,0.0199030680104709,0.0398070347819283),
 .UNSPECIFIED.);
#1571=B_SPLINE_CURVE_WITH_KNOTS('',3,(#73643,#73644,#73645,#73646,#73647,
#73648),.UNSPECIFIED.,.F.,.F.,(4,2,4),(0.,0.0198994178844569,0.0397997368800826),
 .UNSPECIFIED.);
#1572=B_SPLINE_CURVE_WITH_KNOTS('',3,(#73661,#73662,#73663,#73664,#73665,
#73666),.UNSPECIFIED.,.F.,.F.,(4,2,4),(0.,0.0198905179569914,0.0397819072575795),
 .UNSPECIFIED.);
#1573=B_SPLINE_CURVE_WITH_KNOTS('',3,(#73691,#73692,#73693,#73694,#73695,
#73696,#73697),.UNSPECIFIED.,.F.,.F.,(4,3,4),(0.0365944846647009,0.0384615384615384,
0.04314661530766),.UNSPECIFIED.);
#1574=B_SPLINE_CURVE_WITH_KNOTS('',3,(#73698,#73699,#73700,#73701,#73702,
#73703,#73704,#73705),.UNSPECIFIED.,.F.,.F.,(4,2,2,4),(1.77349250019423E-6,
0.00863675584712622,0.017140946030412,0.0172810899018738),.UNSPECIFIED.);
#1575=B_SPLINE_CURVE_WITH_KNOTS('',3,(#73730,#73731,#73732,#73733,#73734,
#73735),.UNSPECIFIED.,.F.,.F.,(4,2,4),(0.,0.0198536183292936,0.0397081496458144),
 .UNSPECIFIED.);
#1576=B_SPLINE_CURVE_WITH_KNOTS('',3,(#73753,#73754,#73755,#73756,#73757,
#73758),.UNSPECIFIED.,.F.,.F.,(4,2,4),(-0.00212385697820441,-0.00106192928909173,
0.),.UNSPECIFIED.);
#1577=B_SPLINE_CURVE_WITH_KNOTS('',3,(#73759,#73760,#73761,#73762,#73763,
#73764),.UNSPECIFIED.,.F.,.F.,(4,2,4),(9.99998411255266E-7,0.0193532896046044,
0.0387045796181942),.UNSPECIFIED.);
#1578=B_SPLINE_CURVE_WITH_KNOTS('',3,(#73770,#73771,#73772,#73773,#73774,
#73775),.UNSPECIFIED.,.F.,.F.,(4,2,4),(-0.00212486795133422,-0.0010629327604503,
-9.99999996965017E-7),.UNSPECIFIED.);
#1579=B_SPLINE_CURVE_WITH_KNOTS('',3,(#73814,#73815,#73816,#73817,#73818,
#73819),.UNSPECIFIED.,.F.,.F.,(4,2,4),(0.,0.0198583386764475,0.0397175618547699),
 .UNSPECIFIED.);
#1580=B_SPLINE_CURVE_WITH_KNOTS('',3,(#73832,#73833,#73834,#73835,#73836,
#73837),.UNSPECIFIED.,.F.,.F.,(4,2,4),(0.,0.0198761967067316,0.0397532849617256),
 .UNSPECIFIED.);
#1581=B_SPLINE_CURVE_WITH_KNOTS('',3,(#73889,#73890,#73891,#73892,#73893,
#73894),.UNSPECIFIED.,.F.,.F.,(4,2,4),(0.,0.0199008240884147,0.0398025407150453),
 .UNSPECIFIED.);
#1582=B_SPLINE_CURVE_WITH_KNOTS('',3,(#73907,#73908,#73909,#73910,#73911,
#73912),.UNSPECIFIED.,.F.,.F.,(4,2,4),(0.,0.0199042047189995,0.0398092891650532),
 .UNSPECIFIED.);
#1583=B_SPLINE_CURVE_WITH_KNOTS('',3,(#73960,#73961,#73962,#73963,#73964,
#73965),.UNSPECIFIED.,.F.,.F.,(4,2,4),(0.,0.0198954793777621,0.0397918615838469),
 .UNSPECIFIED.);
#1584=B_SPLINE_CURVE_WITH_KNOTS('',3,(#74005,#74006,#74007,#74008,#74009,
#74010,#74011),.UNSPECIFIED.,.F.,.F.,(4,3,4),(0.,0.5,0.99999011715892),
 .UNSPECIFIED.);
#1585=B_SPLINE_CURVE_WITH_KNOTS('',3,(#74034,#74035,#74036,#74037,#74038,
#74039),.UNSPECIFIED.,.F.,.F.,(4,2,4),(0.,0.0198677119454309,0.0397363340830025),
 .UNSPECIFIED.);
#1586=B_SPLINE_CURVE_WITH_KNOTS('',3,(#74081,#74082,#74083,#74084,#74085,
#74086),.UNSPECIFIED.,.F.,.F.,(4,2,4),(0.,0.0198973966015896,0.0397956843389232),
 .UNSPECIFIED.);
#1587=B_SPLINE_CURVE_WITH_KNOTS('',3,(#74108,#74109,#74110,#74111,#74112,
#74113),.UNSPECIFIED.,.F.,.F.,(4,2,4),(0.,0.0199030680114917,0.0398070347856482),
 .UNSPECIFIED.);
#1588=B_SPLINE_CURVE_WITH_KNOTS('',3,(#74158,#74159,#74160,#74161,#74162,
#74163),.UNSPECIFIED.,.F.,.F.,(4,2,4),(0.,0.0198994178840687,0.0397997368781493),
 .UNSPECIFIED.);
#1589=B_SPLINE_CURVE_WITH_KNOTS('',3,(#74176,#74177,#74178,#74179,#74180,
#74181),.UNSPECIFIED.,.F.,.F.,(4,2,4),(0.,0.019890517957065,0.0397819072698597),
 .UNSPECIFIED.);
#1590=B_SPLINE_CURVE_WITH_KNOTS('',3,(#74206,#74207,#74208,#74209,#74210,
#74211,#74212),.UNSPECIFIED.,.F.,.F.,(4,3,4),(0.0365944846647012,0.0384615384615384,
0.0431466153076599),.UNSPECIFIED.);
#1591=B_SPLINE_CURVE_WITH_KNOTS('',3,(#74213,#74214,#74215,#74216,#74217,
#74218,#74219,#74220),.UNSPECIFIED.,.F.,.F.,(4,2,2,4),(1.7725636922617E-6,
0.00863675577788347,0.0171409340540784,0.0172810793308343),
 .UNSPECIFIED.);
#1592=B_SPLINE_CURVE_WITH_KNOTS('',3,(#74245,#74246,#74247,#74248,#74249,
#74250),.UNSPECIFIED.,.F.,.F.,(4,2,4),(0.,0.0198536183279069,0.0397081496402279),
 .UNSPECIFIED.);
#1593=B_SPLINE_CURVE_WITH_KNOTS('',3,(#74268,#74269,#74270,#74271,#74272,
#74273),.UNSPECIFIED.,.F.,.F.,(4,2,4),(-0.00212385473939844,-0.00106192839292651,
0.),.UNSPECIFIED.);
#1594=B_SPLINE_CURVE_WITH_KNOTS('',3,(#74274,#74275,#74276,#74277,#74278,
#74279),.UNSPECIFIED.,.F.,.F.,(4,2,4),(9.99998421610724E-7,0.0193522803912436,
0.0387045693987194),.UNSPECIFIED.);
#1595=B_SPLINE_CURVE_WITH_KNOTS('',3,(#74285,#74286,#74287,#74288,#74289,
#74290),.UNSPECIFIED.,.F.,.F.,(4,2,4),(-0.0021248678892231,-0.00106293275681277,
-1.00000000261284E-6),.UNSPECIFIED.);
#1596=B_SPLINE_CURVE_WITH_KNOTS('',3,(#74329,#74330,#74331,#74332,#74333,
#74334),.UNSPECIFIED.,.F.,.F.,(4,2,4),(0.,0.0198583386753345,0.039717561849955),
 .UNSPECIFIED.);
#1597=B_SPLINE_CURVE_WITH_KNOTS('',3,(#74347,#74348,#74349,#74350,#74351,
#74352),.UNSPECIFIED.,.F.,.F.,(4,2,4),(0.,0.0198761967127292,0.0397532849960256),
 .UNSPECIFIED.);
#1598=B_SPLINE_CURVE_WITH_KNOTS('',3,(#74404,#74405,#74406,#74407,#74408,
#74409),.UNSPECIFIED.,.F.,.F.,(4,2,4),(0.,0.0199008240880627,0.0398025407135643),
 .UNSPECIFIED.);
#1599=B_SPLINE_CURVE_WITH_KNOTS('',3,(#74422,#74423,#74424,#74425,#74426,
#74427),.UNSPECIFIED.,.F.,.F.,(4,2,4),(0.,0.0199042047187738,0.0398092891784042),
 .UNSPECIFIED.);
#1600=B_SPLINE_CURVE_WITH_KNOTS('',3,(#74475,#74476,#74477,#74478,#74479,
#74480),.UNSPECIFIED.,.F.,.F.,(4,2,4),(0.,0.0198954793773227,0.0397918615821683),
 .UNSPECIFIED.);
#1601=B_SPLINE_CURVE_WITH_KNOTS('',3,(#74520,#74521,#74522,#74523,#74524,
#74525,#74526),.UNSPECIFIED.,.F.,.F.,(4,3,4),(0.,0.5,0.99999011716107),
 .UNSPECIFIED.);
#1602=B_SPLINE_CURVE_WITH_KNOTS('',3,(#74549,#74550,#74551,#74552,#74553,
#74554),.UNSPECIFIED.,.F.,.F.,(4,2,4),(0.,0.0198677119468207,0.0397363340885719),
 .UNSPECIFIED.);
#1603=B_SPLINE_CURVE_WITH_KNOTS('',3,(#74596,#74597,#74598,#74599,#74600,
#74601),.UNSPECIFIED.,.F.,.F.,(4,2,4),(0.,0.0198973966000579,0.0397956843329122),
 .UNSPECIFIED.);
#1604=B_SPLINE_CURVE_WITH_KNOTS('',3,(#74623,#74624,#74625,#74626,#74627,
#74628),.UNSPECIFIED.,.F.,.F.,(4,2,4),(0.,0.01990306801314,0.0398070347925831),
 .UNSPECIFIED.);
#1605=B_SPLINE_CURVE_WITH_KNOTS('',3,(#74673,#74674,#74675,#74676,#74677,
#74678),.UNSPECIFIED.,.F.,.F.,(4,2,4),(0.,0.0198994178828134,0.0397997368733775),
 .UNSPECIFIED.);
#1606=B_SPLINE_CURVE_WITH_KNOTS('',3,(#74691,#74692,#74693,#74694,#74695,
#74696),.UNSPECIFIED.,.F.,.F.,(4,2,4),(0.,0.0198905179570001,0.0397819072527676),
 .UNSPECIFIED.);
#1607=B_SPLINE_CURVE_WITH_KNOTS('',3,(#74721,#74722,#74723,#74724,#74725,
#74726,#74727),.UNSPECIFIED.,.F.,.F.,(4,3,4),(0.0365944846647015,0.0384615384615384,
0.0431466153076602),.UNSPECIFIED.);
#1608=B_SPLINE_CURVE_WITH_KNOTS('',3,(#74728,#74729,#74730,#74731,#74732,
#74733,#74734,#74735),.UNSPECIFIED.,.F.,.F.,(4,2,2,4),(1.77256369998672E-6,
0.00863675578444654,0.0171409282122659,0.0172810740976024),
 .UNSPECIFIED.);
#1609=B_SPLINE_CURVE_WITH_KNOTS('',3,(#74760,#74761,#74762,#74763,#74764,
#74765),.UNSPECIFIED.,.F.,.F.,(4,2,4),(0.,0.0198536183267392,0.039708149635655),
 .UNSPECIFIED.);
#1610=B_SPLINE_CURVE_WITH_KNOTS('',3,(#74783,#74784,#74785,#74786,#74787,
#74788),.UNSPECIFIED.,.F.,.F.,(4,2,4),(-0.00212385284338186,-0.00106192763760952,
0.),.UNSPECIFIED.);
#1611=B_SPLINE_CURVE_WITH_KNOTS('',3,(#74789,#74790,#74791,#74792,#74793,
#74794),.UNSPECIFIED.,.F.,.F.,(4,2,4),(9.99998414498686E-7,0.0193532903994283,
0.0387045796339771),.UNSPECIFIED.);
#1612=B_SPLINE_CURVE_WITH_KNOTS('',3,(#74800,#74801,#74802,#74803,#74804,
#74805),.UNSPECIFIED.,.F.,.F.,(4,2,4),(-0.00212486777295456,-0.00106293276548707,
-1.00000000054809E-6),.UNSPECIFIED.);
#1613=B_SPLINE_CURVE_WITH_KNOTS('',3,(#74844,#74845,#74846,#74847,#74848,
#74849),.UNSPECIFIED.,.F.,.F.,(4,2,4),(0.,0.0198583386744434,0.0397175618466529),
 .UNSPECIFIED.);
#1614=B_SPLINE_CURVE_WITH_KNOTS('',3,(#74862,#74863,#74864,#74865,#74866,
#74867),.UNSPECIFIED.,.F.,.F.,(4,2,4),(0.,0.0198761967069154,0.0397532849758011),
 .UNSPECIFIED.);
#1615=B_SPLINE_CURVE_WITH_KNOTS('',3,(#74919,#74920,#74921,#74922,#74923,
#74924),.UNSPECIFIED.,.F.,.F.,(4,2,4),(0.,0.0199008240869926,0.0398025407092003),
 .UNSPECIFIED.);
#1616=B_SPLINE_CURVE_WITH_KNOTS('',3,(#74937,#74938,#74939,#74940,#74941,
#74942),.UNSPECIFIED.,.F.,.F.,(4,2,4),(0.,0.0199042047190074,0.0398092891779339),
 .UNSPECIFIED.);
#1617=B_SPLINE_CURVE_WITH_KNOTS('',3,(#74990,#74991,#74992,#74993,#74994,
#74995),.UNSPECIFIED.,.F.,.F.,(4,2,4),(0.,0.0198954793762232,0.0397918615774369),
 .UNSPECIFIED.);
#1618=B_SPLINE_CURVE_WITH_KNOTS('',3,(#75035,#75036,#75037,#75038,#75039,
#75040,#75041),.UNSPECIFIED.,.F.,.F.,(4,3,4),(0.,0.5,0.999990117163183),
 .UNSPECIFIED.);
#1619=B_SPLINE_CURVE_WITH_KNOTS('',3,(#75064,#75065,#75066,#75067,#75068,
#75069),.UNSPECIFIED.,.F.,.F.,(4,2,4),(0.,0.0198677119479282,0.0397363340928585),
 .UNSPECIFIED.);
#1620=B_SPLINE_CURVE_WITH_KNOTS('',3,(#75111,#75112,#75113,#75114,#75115,
#75116),.UNSPECIFIED.,.F.,.F.,(4,2,4),(0.,0.0198973965989467,0.039795684329128),
 .UNSPECIFIED.);
#1621=B_SPLINE_CURVE_WITH_KNOTS('',3,(#75138,#75139,#75140,#75141,#75142,
#75143),.UNSPECIFIED.,.F.,.F.,(4,2,4),(0.,0.0199030680141118,0.0398070347963341),
 .UNSPECIFIED.);
#1622=B_SPLINE_CURVE_WITH_KNOTS('',3,(#75188,#75189,#75190,#75191,#75192,
#75193),.UNSPECIFIED.,.F.,.F.,(4,2,4),(0.,0.0198994178815675,0.0397997368683613),
 .UNSPECIFIED.);
#1623=B_SPLINE_CURVE_WITH_KNOTS('',3,(#75206,#75207,#75208,#75209,#75210,
#75211),.UNSPECIFIED.,.F.,.F.,(4,2,4),(0.,0.0198905179569802,0.0397819072620881),
 .UNSPECIFIED.);
#1624=B_SPLINE_CURVE_WITH_KNOTS('',3,(#75236,#75237,#75238,#75239,#75240,
#75241,#75242),.UNSPECIFIED.,.F.,.F.,(4,3,4),(0.0365944846647007,0.0384615384615384,
0.0431466153076595),.UNSPECIFIED.);
#1625=B_SPLINE_CURVE_WITH_KNOTS('',3,(#75243,#75244,#75245,#75246,#75247,
#75248,#75249,#75250),.UNSPECIFIED.,.F.,.F.,(4,2,2,4),(1.77349269128769E-6,
0.00863675576722594,0.0171409186233939,0.0172810654209329),
 .UNSPECIFIED.);
#1626=B_SPLINE_CURVE_WITH_KNOTS('',3,(#75275,#75276,#75277,#75278,#75279,
#75280),.UNSPECIFIED.,.F.,.F.,(4,2,4),(0.,0.0198536183260036,0.0397081496324284),
 .UNSPECIFIED.);
#1627=B_SPLINE_CURVE_WITH_KNOTS('',3,(#75298,#75299,#75300,#75301,#75302,
#75303),.UNSPECIFIED.,.F.,.F.,(4,2,4),(-0.00212385118147093,-0.00106192697594493,
0.),.UNSPECIFIED.);
#1628=B_SPLINE_CURVE_WITH_KNOTS('',3,(#75304,#75305,#75306,#75307,#75308,
#75309),.UNSPECIFIED.,.F.,.F.,(4,2,4),(9.99998416995636E-7,0.0193522795956267,
0.0387045693813799),.UNSPECIFIED.);
#1629=B_SPLINE_CURVE_WITH_KNOTS('',3,(#75315,#75316,#75317,#75318,#75319,
#75320),.UNSPECIFIED.,.F.,.F.,(4,2,4),(-0.00212486747589103,-0.00106293275719458,
-9.99999997170799E-7),.UNSPECIFIED.);
#1630=B_SPLINE_CURVE_WITH_KNOTS('',3,(#75359,#75360,#75361,#75362,#75363,
#75364),.UNSPECIFIED.,.F.,.F.,(4,2,4),(0.,0.0198583386732508,0.0397175618416976),
 .UNSPECIFIED.);
#1631=B_SPLINE_CURVE_WITH_KNOTS('',3,(#75377,#75378,#75379,#75380,#75381,
#75382),.UNSPECIFIED.,.F.,.F.,(4,2,4),(0.,0.019876196698315,0.0397532849596158),
 .UNSPECIFIED.);
#1632=B_SPLINE_CURVE_WITH_KNOTS('',3,(#75434,#75435,#75436,#75437,#75438,
#75439),.UNSPECIFIED.,.F.,.F.,(4,2,4),(0.,0.0199008240858154,0.0398025407041441),
 .UNSPECIFIED.);
#1633=B_SPLINE_CURVE_WITH_KNOTS('',3,(#75452,#75453,#75454,#75455,#75456,
#75457),.UNSPECIFIED.,.F.,.F.,(4,2,4),(0.,0.019904204718824,0.0398092891828929),
 .UNSPECIFIED.);
#1634=B_SPLINE_CURVE_WITH_KNOTS('',3,(#75505,#75506,#75507,#75508,#75509,
#75510),.UNSPECIFIED.,.F.,.F.,(4,2,4),(0.,0.0198954793749717,0.0397918615725202),
 .UNSPECIFIED.);
#1635=B_SPLINE_CURVE_WITH_KNOTS('',3,(#75550,#75551,#75552,#75553,#75554,
#75555,#75556),.UNSPECIFIED.,.F.,.F.,(4,3,4),(0.,0.5,0.999990117164291),
 .UNSPECIFIED.);
#1636=B_SPLINE_CURVE_WITH_KNOTS('',3,(#75579,#75580,#75581,#75582,#75583,
#75584),.UNSPECIFIED.,.F.,.F.,(4,2,4),(0.,0.0198677119492189,0.0397363340978274),
 .UNSPECIFIED.);
#1637=B_SPLINE_CURVE_WITH_KNOTS('',3,(#75626,#75627,#75628,#75629,#75630,
#75631),.UNSPECIFIED.,.F.,.F.,(4,2,4),(0.,0.0198973965974829,0.0397956843228074),
 .UNSPECIFIED.);
#1638=B_SPLINE_CURVE_WITH_KNOTS('',3,(#75653,#75654,#75655,#75656,#75657,
#75658),.UNSPECIFIED.,.F.,.F.,(4,2,4),(0.,0.0199030680152636,0.0398070348010775),
 .UNSPECIFIED.);
#1639=B_SPLINE_CURVE_WITH_KNOTS('',3,(#75700,#75701,#75702,#75703,#75704,
#75705),.UNSPECIFIED.,.F.,.F.,(4,2,4),(0.,0.0198994178801307,0.0397997368625414),
 .UNSPECIFIED.);
#1640=B_SPLINE_CURVE_WITH_KNOTS('',3,(#75725,#75726,#75727,#75728,#75729,
#75730),.UNSPECIFIED.,.F.,.F.,(4,2,4),(0.,0.019890572780449,0.0397820348288668),
 .UNSPECIFIED.);
#1641=B_SPLINE_CURVE_WITH_KNOTS('',3,(#75755,#75756,#75757,#75758,#75759,
#75760,#75761),.UNSPECIFIED.,.F.,.F.,(4,3,4),(0.0365944846647011,0.0384615384615384,
0.0431466153076599),.UNSPECIFIED.);
#1642=B_SPLINE_CURVE_WITH_KNOTS('',3,(#75762,#75763,#75764,#75765,#75766,
#75767,#75768,#75769),.UNSPECIFIED.,.F.,.F.,(4,2,2,4),(1.77256738234578E-6,
0.00863675579810489,0.0171409372906893,0.0172810822319369),
 .UNSPECIFIED.);
#1643=B_SPLINE_CURVE_WITH_KNOTS('',3,(#75794,#75795,#75796,#75797,#75798,
#75799),.UNSPECIFIED.,.F.,.F.,(4,2,4),(0.,0.019853618324023,0.0397081496247761),
 .UNSPECIFIED.);
#1644=B_SPLINE_CURVE_WITH_KNOTS('',3,(#75817,#75818,#75819,#75820,#75821,
#75822),.UNSPECIFIED.,.F.,.F.,(4,2,4),(-0.00212384980647466,-0.00106192642804374,
0.),.UNSPECIFIED.);
#1645=B_SPLINE_CURVE_WITH_KNOTS('',3,(#75823,#75824,#75825,#75826,#75827,
#75828),.UNSPECIFIED.,.F.,.F.,(4,2,4),(9.99998416490131E-7,0.0193522803905122,
0.0387045693972246),.UNSPECIFIED.);
#1646=B_SPLINE_CURVE_WITH_KNOTS('',3,(#75834,#75835,#75836,#75837,#75838,
#75839),.UNSPECIFIED.,.F.,.F.,(4,2,4),(-0.00212486726074812,-0.00106293276493776,
-9.99999998992909E-7),.UNSPECIFIED.);
#1647=B_SPLINE_CURVE_WITH_KNOTS('',3,(#75878,#75879,#75880,#75881,#75882,
#75883),.UNSPECIFIED.,.F.,.F.,(4,2,4),(0.,0.0198583386718413,0.0397175618360036),
 .UNSPECIFIED.);
#1648=B_SPLINE_CURVE_WITH_KNOTS('',3,(#75896,#75897,#75898,#75899,#75900,
#75901),.UNSPECIFIED.,.F.,.F.,(4,2,4),(0.,0.0198761965659768,0.0397532846823463),
 .UNSPECIFIED.);
#1649=B_SPLINE_CURVE_WITH_KNOTS('',3,(#75953,#75954,#75955,#75956,#75957,
#75958),.UNSPECIFIED.,.F.,.F.,(4,2,4),(0.,0.0199008240845495,0.0398025406993579),
 .UNSPECIFIED.);
#1650=B_SPLINE_CURVE_WITH_KNOTS('',3,(#75971,#75972,#75973,#75974,#75975,
#75976),.UNSPECIFIED.,.F.,.F.,(4,2,4),(0.,0.0199042047188238,0.0398092891624507),
 .UNSPECIFIED.);
#1651=B_SPLINE_CURVE_WITH_KNOTS('',3,(#76024,#76025,#76026,#76027,#76028,
#76029),.UNSPECIFIED.,.F.,.F.,(4,2,4),(0.,0.0198954793737053,0.0397918615673638),
 .UNSPECIFIED.);
#1652=B_SPLINE_CURVE_WITH_KNOTS('',3,(#76069,#76070,#76071,#76072,#76073,
#76074,#76075),.UNSPECIFIED.,.F.,.F.,(4,3,4),(0.,0.5,0.999990117165551),
 .UNSPECIFIED.);
#1653=B_SPLINE_CURVE_WITH_KNOTS('',3,(#76098,#76099,#76100,#76101,#76102,
#76103),.UNSPECIFIED.,.F.,.F.,(4,2,4),(0.,0.0198677119501225,0.0397363341016526),
 .UNSPECIFIED.);
#1654=B_SPLINE_CURVE_WITH_KNOTS('',3,(#76145,#76146,#76147,#76148,#76149,
#76150),.UNSPECIFIED.,.F.,.F.,(4,2,4),(0.,0.0198973965964354,0.0397956843184013),
 .UNSPECIFIED.);
#1655=B_SPLINE_CURVE_WITH_KNOTS('',3,(#76172,#76173,#76174,#76175,#76176,
#76177),.UNSPECIFIED.,.F.,.F.,(4,2,4),(0.,0.0199030680160421,0.0398070348041842),
 .UNSPECIFIED.);
#1656=B_SPLINE_CURVE_WITH_KNOTS('',3,(#76222,#76223,#76224,#76225,#76226,
#76227),.UNSPECIFIED.,.F.,.F.,(4,2,4),(0.,0.0198994178785787,0.0397997368562093),
 .UNSPECIFIED.);
#1657=B_SPLINE_CURVE_WITH_KNOTS('',3,(#76240,#76241,#76242,#76243,#76244,
#76245),.UNSPECIFIED.,.F.,.F.,(4,2,4),(0.,0.019890517956938,0.0397819072549784),
 .UNSPECIFIED.);
#1658=B_SPLINE_CURVE_WITH_KNOTS('',3,(#76271,#76272,#76273,#76274,#76275,
#76276),.UNSPECIFIED.,.F.,.F.,(4,2,4),(0.036594484664701,0.0384615384615384,
0.0431466153076599),.UNSPECIFIED.);
#1659=B_SPLINE_CURVE_WITH_KNOTS('',3,(#76277,#76278,#76279,#76280,#76281,
#76282,#76283),.UNSPECIFIED.,.F.,.F.,(4,3,4),(0.,0.00863415824006578,0.0172757258251161),
 .UNSPECIFIED.);
#1660=B_SPLINE_CURVE_WITH_KNOTS('',3,(#76308,#76309,#76310,#76311,#76312,
#76313),.UNSPECIFIED.,.F.,.F.,(4,2,4),(0.,0.0198541182823923,0.0397081495471127),
 .UNSPECIFIED.);
#1661=B_SPLINE_CURVE_WITH_KNOTS('',3,(#76326,#76327,#76328,#76329,#76330,
#76331),.UNSPECIFIED.,.F.,.F.,(4,2,4),(-0.00212384884036098,-0.00106192603334971,
0.),.UNSPECIFIED.);
#1662=B_SPLINE_CURVE_WITH_KNOTS('',3,(#76332,#76333,#76334,#76335,#76336,
#76337),.UNSPECIFIED.,.F.,.F.,(4,2,4),(9.99998417286137E-7,0.0193522803914762,
0.0387045693990307),.UNSPECIFIED.);
#1663=B_SPLINE_CURVE_WITH_KNOTS('',3,(#76343,#76344,#76345,#76346,#76347,
#76348),.UNSPECIFIED.,.F.,.F.,(4,2,4),(-0.00212486683933188,-0.0010629327524213,
-9.99999998585899E-7),.UNSPECIFIED.);
#1664=B_SPLINE_CURVE_WITH_KNOTS('',3,(#76387,#76388,#76389,#76390,#76391,
#76392),.UNSPECIFIED.,.F.,.F.,(4,2,4),(0.,0.0198583386710425,0.0397175618327234),
 .UNSPECIFIED.);
#1665=B_SPLINE_CURVE_WITH_KNOTS('',3,(#76405,#76406,#76407,#76408,#76409,
#76410),.UNSPECIFIED.,.F.,.F.,(4,2,4),(0.,0.0198761965784973,0.0397532847182389),
 .UNSPECIFIED.);
#1666=B_SPLINE_CURVE_WITH_KNOTS('',3,(#76462,#76463,#76464,#76465,#76466,
#76467),.UNSPECIFIED.,.F.,.F.,(4,2,4),(0.,0.0199008240829753,0.0398025406932351),
 .UNSPECIFIED.);
#1667=B_SPLINE_CURVE_WITH_KNOTS('',3,(#76480,#76481,#76482,#76483,#76484,
#76485),.UNSPECIFIED.,.F.,.F.,(4,2,4),(0.,0.0199047046187306,0.0398092889177888),
 .UNSPECIFIED.);
#1668=B_SPLINE_CURVE_WITH_KNOTS('',3,(#76533,#76534,#76535,#76536,#76537,
#76538),.UNSPECIFIED.,.F.,.F.,(4,2,4),(0.,0.0198954793723645,0.0397918615620052),
 .UNSPECIFIED.);
#1669=B_SPLINE_CURVE_WITH_KNOTS('',3,(#76578,#76579,#76580,#76581,#76582,
#76583,#76584),.UNSPECIFIED.,.F.,.F.,(4,3,4),(0.,0.5,0.999990117166381),
 .UNSPECIFIED.);
#1670=B_SPLINE_CURVE_WITH_KNOTS('',3,(#76607,#76608,#76609,#76610,#76611,
#76612),.UNSPECIFIED.,.F.,.F.,(4,2,4),(0.,0.0198677119506905,0.0397363341039637),
 .UNSPECIFIED.);
#1671=B_SPLINE_CURVE_WITH_KNOTS('',3,(#76654,#76655,#76656,#76657,#76658,
#76659),.UNSPECIFIED.,.F.,.F.,(4,2,4),(0.,0.0198973965943807,0.0397956843103301),
 .UNSPECIFIED.);
#1672=B_SPLINE_CURVE_WITH_KNOTS('',3,(#76681,#76682,#76683,#76684,#76685,
#76686),.UNSPECIFIED.,.F.,.F.,(4,2,4),(0.,0.0199030680172143,0.0398070348088722),
 .UNSPECIFIED.);
#1673=B_SPLINE_CURVE_WITH_KNOTS('',3,(#76728,#76729,#76730,#76731,#76732,
#76733),.UNSPECIFIED.,.F.,.F.,(4,2,4),(0.,0.0198994178771943,0.0397997368507428),
 .UNSPECIFIED.);
#1674=B_SPLINE_CURVE_WITH_KNOTS('',3,(#76753,#76754,#76755,#76756,#76757,
#76758),.UNSPECIFIED.,.F.,.F.,(4,2,4),(0.,0.0198905727828279,0.0397820348383145),
 .UNSPECIFIED.);
#1675=B_SPLINE_CURVE_WITH_KNOTS('',3,(#76783,#76784,#76785,#76786,#76787,
#76788,#76789),.UNSPECIFIED.,.F.,.F.,(4,3,4),(0.0365944846647011,0.0384615384615384,
0.0431466153076597),.UNSPECIFIED.);
#1676=B_SPLINE_CURVE_WITH_KNOTS('',3,(#76790,#76791,#76792,#76793,#76794,
#76795,#76796,#76797),.UNSPECIFIED.,.F.,.F.,(4,2,2,4),(1.77349269003237E-6,
0.00863675577167021,0.0171409216007662,0.0172810680711004),
 .UNSPECIFIED.);
#1677=B_SPLINE_CURVE_WITH_KNOTS('',3,(#76822,#76823,#76824,#76825,#76826,
#76827),.UNSPECIFIED.,.F.,.F.,(4,2,4),(0.,0.0198536183208147,0.0397081496118954),
 .UNSPECIFIED.);
#1678=B_SPLINE_CURVE_WITH_KNOTS('',3,(#76845,#76846,#76847,#76848,#76849,
#76850),.UNSPECIFIED.,.F.,.F.,(4,2,4),(-0.00212384825724064,-0.00106192581024466,
0.),.UNSPECIFIED.);
#1679=B_SPLINE_CURVE_WITH_KNOTS('',3,(#76851,#76852,#76853,#76854,#76855,
#76856),.UNSPECIFIED.,.F.,.F.,(4,2,4),(9.99998417360777E-7,0.0193522795962004,
0.0387045693826146),.UNSPECIFIED.);
#1680=B_SPLINE_CURVE_WITH_KNOTS('',3,(#76862,#76863,#76864,#76865,#76866,
#76867),.UNSPECIFIED.,.F.,.F.,(4,2,4),(-0.00212486648408312,-0.00106293275900954,
-9.99999996604845E-7),.UNSPECIFIED.);
#1681=B_SPLINE_CURVE_WITH_KNOTS('',3,(#76903,#76904,#76905,#76906,#76907,
#76908),.UNSPECIFIED.,.F.,.F.,(4,2,4),(0.,0.0198583386697237,0.0397175618277278),
 .UNSPECIFIED.);
#1682=B_SPLINE_CURVE_WITH_KNOTS('',3,(#76928,#76929,#76930,#76931,#76932,
#76933),.UNSPECIFIED.,.F.,.F.,(4,2,4),(0.,0.0198762582556093,0.0397534248900765),
 .UNSPECIFIED.);
#1683=B_SPLINE_CURVE_WITH_KNOTS('',3,(#76985,#76986,#76987,#76988,#76989,
#76990),.UNSPECIFIED.,.F.,.F.,(4,2,4),(0.,0.019901323992909,0.0398025404511413),
 .UNSPECIFIED.);
#1684=B_SPLINE_CURVE_WITH_KNOTS('',3,(#77003,#77004,#77005,#77006,#77007,
#77008),.UNSPECIFIED.,.F.,.F.,(4,2,4),(0.,0.019904204713085,0.0398092891717569),
 .UNSPECIFIED.);
#1685=B_SPLINE_CURVE_WITH_KNOTS('',3,(#77056,#77057,#77058,#77059,#77060,
#77061),.UNSPECIFIED.,.F.,.F.,(4,2,4),(0.,0.0198954793706761,0.0397918615552283),
 .UNSPECIFIED.);
#1686=B_SPLINE_CURVE_WITH_KNOTS('',3,(#77101,#77102,#77103,#77104,#77105,
#77106,#77107),.UNSPECIFIED.,.F.,.F.,(4,3,4),(0.,0.5,0.999990117166621),
 .UNSPECIFIED.);
#1687=B_SPLINE_CURVE_WITH_KNOTS('',3,(#77130,#77131,#77132,#77133,#77134,
#77135),.UNSPECIFIED.,.F.,.F.,(4,2,4),(0.,0.0198677119511838,0.0397363341058345),
 .UNSPECIFIED.);
#1688=B_SPLINE_CURVE_WITH_KNOTS('',3,(#77177,#77178,#77179,#77180,#77181,
#77182),.UNSPECIFIED.,.F.,.F.,(4,2,4),(0.,0.0198973965935688,0.0397956843067912),
 .UNSPECIFIED.);
#1689=B_SPLINE_CURVE_WITH_KNOTS('',3,(#77204,#77205,#77206,#77207,#77208,
#77209),.UNSPECIFIED.,.F.,.F.,(4,2,4),(0.,0.0199030680177893,0.0398070348110941),
 .UNSPECIFIED.);
#1690=B_SPLINE_CURVE_WITH_KNOTS('',3,(#77254,#77255,#77256,#77257,#77258,
#77259),.UNSPECIFIED.,.F.,.F.,(4,2,4),(0.,0.0198994178756067,0.0397997368447963),
 .UNSPECIFIED.);
#1691=B_SPLINE_CURVE_WITH_KNOTS('',3,(#77272,#77273,#77274,#77275,#77276,
#77277),.UNSPECIFIED.,.F.,.F.,(4,2,4),(0.,0.0198905179569198,0.039781907258255),
 .UNSPECIFIED.);
#1692=B_SPLINE_CURVE_WITH_KNOTS('',3,(#77302,#77303,#77304,#77305,#77306,
#77307,#77308),.UNSPECIFIED.,.F.,.F.,(4,3,4),(0.0365944846647018,0.0384615384615384,
0.0431466153076603),.UNSPECIFIED.);
#1693=B_SPLINE_CURVE_WITH_KNOTS('',3,(#77309,#77310,#77311,#77312,#77313,
#77314,#77315,#77316),.UNSPECIFIED.,.F.,.F.,(4,2,2,4),(1.7734928133057E-6,
0.00863675575681659,0.0171409114737263,0.017281059029724),.UNSPECIFIED.);
#1694=B_SPLINE_CURVE_WITH_KNOTS('',3,(#77341,#77342,#77343,#77344,#77345,
#77346),.UNSPECIFIED.,.F.,.F.,(4,2,4),(0.,0.0198536183197665,0.0397081496077481),
 .UNSPECIFIED.);
#1695=B_SPLINE_CURVE_WITH_KNOTS('',3,(#77364,#77365,#77366,#77367,#77368,
#77369),.UNSPECIFIED.,.F.,.F.,(4,2,4),(-0.0021238480623822,-0.00106192573417119,
0.),.UNSPECIFIED.);
#1696=B_SPLINE_CURVE_WITH_KNOTS('',3,(#77370,#77371,#77372,#77373,#77374,
#77375),.UNSPECIFIED.,.F.,.F.,(4,2,4),(9.99998409595905E-7,0.0193532896051288,
0.0387045796195939),.UNSPECIFIED.);
#1697=B_SPLINE_CURVE_WITH_KNOTS('',3,(#77381,#77382,#77383,#77384,#77385,
#77386),.UNSPECIFIED.,.F.,.F.,(4,2,4),(-0.00212486601988817,-0.00106293275364175,
-1.00000000020982E-6),.UNSPECIFIED.);
#1698=B_SPLINE_CURVE_WITH_KNOTS('',3,(#77425,#77426,#77427,#77428,#77429,
#77430),.UNSPECIFIED.,.F.,.F.,(4,2,4),(0.,0.0198583386674524,0.0397175618184792),
 .UNSPECIFIED.);
#1699=B_SPLINE_CURVE_WITH_KNOTS('',3,(#77443,#77444,#77445,#77446,#77447,
#77448),.UNSPECIFIED.,.F.,.F.,(4,2,4),(0.,0.0198761967044215,0.039753284959996),
 .UNSPECIFIED.);
#1700=B_SPLINE_CURVE_WITH_KNOTS('',3,(#77500,#77501,#77502,#77503,#77504,
#77505),.UNSPECIFIED.,.F.,.F.,(4,2,4),(0.,0.0199008240805986,0.0398025406833724),
 .UNSPECIFIED.);
#1701=B_SPLINE_CURVE_WITH_KNOTS('',3,(#77525,#77526,#77527,#77528,#77529,
#77530),.UNSPECIFIED.,.F.,.F.,(4,2,4),(0.,0.0199042622206626,0.039809421612776),
 .UNSPECIFIED.);
#1702=B_SPLINE_CURVE_WITH_KNOTS('',3,(#77578,#77579,#77580,#77581,#77582,
#77583),.UNSPECIFIED.,.F.,.F.,(4,2,4),(0.,0.0198954793698275,0.0397918615516674),
 .UNSPECIFIED.);
#1703=B_SPLINE_CURVE_WITH_KNOTS('',3,(#77623,#77624,#77625,#77626,#77627,
#77628,#77629),.UNSPECIFIED.,.F.,.F.,(4,3,4),(0.,0.5,0.999990117166003),
 .UNSPECIFIED.);
#1704=B_SPLINE_CURVE_WITH_KNOTS('',3,(#77652,#77653,#77654,#77655,#77656,
#77657),.UNSPECIFIED.,.F.,.F.,(4,2,4),(0.,0.0198677119515248,0.0397363341074989),
 .UNSPECIFIED.);
#1705=B_SPLINE_CURVE_WITH_KNOTS('',3,(#77699,#77700,#77701,#77702,#77703,
#77704),.UNSPECIFIED.,.F.,.F.,(4,2,4),(0.,0.0198973965915467,0.0397956842989783),
 .UNSPECIFIED.);
#1706=B_SPLINE_CURVE_WITH_KNOTS('',3,(#77726,#77727,#77728,#77729,#77730,
#77731),.UNSPECIFIED.,.F.,.F.,(4,2,4),(0.,0.0199030680180883,0.0398070348124307),
 .UNSPECIFIED.);
#1707=B_SPLINE_CURVE_WITH_KNOTS('',3,(#77776,#77777,#77778,#77779,#77780,
#77781),.UNSPECIFIED.,.F.,.F.,(4,2,4),(0.,0.0198994178738356,0.0397997368373613),
 .UNSPECIFIED.);
#1708=B_SPLINE_CURVE_WITH_KNOTS('',3,(#77794,#77795,#77796,#77797,#77798,
#77799),.UNSPECIFIED.,.F.,.F.,(4,2,4),(0.,0.0198905179569007,0.0397819072607639),
 .UNSPECIFIED.);
#1709=B_SPLINE_CURVE_WITH_KNOTS('',3,(#77824,#77825,#77826,#77827,#77828,
#77829,#77830),.UNSPECIFIED.,.F.,.F.,(4,3,4),(0.0365944846647006,0.0384615384615384,
0.0431466153076599),.UNSPECIFIED.);
#1710=B_SPLINE_CURVE_WITH_KNOTS('',3,(#77831,#77832,#77833,#77834,#77835,
#77836,#77837,#77838),.UNSPECIFIED.,.F.,.F.,(4,2,2,4),(1.77349264648523E-6,
0.00863675580432023,0.017140932899279,0.0172810781627562),.UNSPECIFIED.);
#1711=B_SPLINE_CURVE_WITH_KNOTS('',3,(#77863,#77864,#77865,#77866,#77867,
#77868),.UNSPECIFIED.,.F.,.F.,(4,2,4),(0.,0.0198536183179197,0.0397081496007127),
 .UNSPECIFIED.);
#1712=B_SPLINE_CURVE_WITH_KNOTS('',3,(#77886,#77887,#77888,#77889,#77890,
#77891),.UNSPECIFIED.,.F.,.F.,(4,2,4),(-0.00212384826848124,-0.00106192580172268,
0.),.UNSPECIFIED.);
#1713=B_SPLINE_CURVE_WITH_KNOTS('',3,(#77892,#77893,#77894,#77895,#77896,
#77897),.UNSPECIFIED.,.F.,.F.,(4,2,4),(9.99998409484697E-7,0.0193527745925596,
0.0387045692823788),.UNSPECIFIED.);
#1714=B_SPLINE_CURVE_WITH_KNOTS('',3,(#77903,#77904,#77905,#77906,#77907,
#77908),.UNSPECIFIED.,.F.,.F.,(4,2,4),(-0.00212486549577526,-0.00106293274763414,
-9.99999999081163E-7),.UNSPECIFIED.);
#1715=B_SPLINE_CURVE_WITH_KNOTS('',3,(#77947,#77948,#77949,#77950,#77951,
#77952),.UNSPECIFIED.,.F.,.F.,(4,2,4),(0.,0.0198583386666685,0.0397175618153152),
 .UNSPECIFIED.);
#1716=B_SPLINE_CURVE_WITH_KNOTS('',3,(#77965,#77966,#77967,#77968,#77969,
#77970),.UNSPECIFIED.,.F.,.F.,(4,2,4),(0.,0.0198761966603836,0.0397532848690265),
 .UNSPECIFIED.);
#1717=B_SPLINE_CURVE_WITH_KNOTS('',3,(#78022,#78023,#78024,#78025,#78026,
#78027),.UNSPECIFIED.,.F.,.F.,(4,2,4),(0.,0.0199008240786792,0.039802540676266),
 .UNSPECIFIED.);
#1718=B_SPLINE_CURVE_WITH_KNOTS('',3,(#78040,#78041,#78042,#78043,#78044,
#78045),.UNSPECIFIED.,.F.,.F.,(4,2,4),(0.,0.0199042047132145,0.0398092891672759),
 .UNSPECIFIED.);
#1719=B_SPLINE_CURVE_WITH_KNOTS('',3,(#78090,#78091,#78092,#78093,#78094,
#78095),.UNSPECIFIED.,.F.,.F.,(4,2,4),(0.,0.0198954793679848,0.0397918615443618),
 .UNSPECIFIED.);
#1720=B_SPLINE_CURVE_WITH_KNOTS('',3,(#78142,#78143,#78144,#78145,#78146,
#78147,#78148),.UNSPECIFIED.,.F.,.F.,(4,3,4),(0.,0.5,0.999990117166367),
 .UNSPECIFIED.);
#1721=B_SPLINE_CURVE_WITH_KNOTS('',3,(#78171,#78172,#78173,#78174,#78175,
#78176),.UNSPECIFIED.,.F.,.F.,(4,2,4),(0.,0.0198677119512784,0.039736334106876),
 .UNSPECIFIED.);
#1722=B_SPLINE_CURVE_WITH_KNOTS('',3,(#78218,#78219,#78220,#78221,#78222,
#78223),.UNSPECIFIED.,.F.,.F.,(4,2,4),(0.,0.019897396590471,0.0397956842942256),
 .UNSPECIFIED.);
#1723=B_SPLINE_CURVE_WITH_KNOTS('',3,(#78245,#78246,#78247,#78248,#78249,
#78250),.UNSPECIFIED.,.F.,.F.,(4,2,4),(0.,0.0199030680183993,0.0398070348136018),
 .UNSPECIFIED.);
#1724=B_SPLINE_CURVE_WITH_KNOTS('',3,(#78295,#78296,#78297,#78298,#78299,
#78300),.UNSPECIFIED.,.F.,.F.,(4,2,4),(0.,0.0198994178727326,0.0397997368327952),
 .UNSPECIFIED.);
#1725=B_SPLINE_CURVE_WITH_KNOTS('',3,(#78313,#78314,#78315,#78316,#78317,
#78318),.UNSPECIFIED.,.F.,.F.,(4,2,4),(0.,0.0198905174670392,0.0397819062735446),
 .UNSPECIFIED.);
#1726=B_SPLINE_CURVE_WITH_KNOTS('',3,(#78343,#78344,#78345,#78346,#78347,
#78348,#78349),.UNSPECIFIED.,.F.,.F.,(4,3,4),(0.0365944846647016,0.0384615384615384,
0.0431466153076595),.UNSPECIFIED.);
#1727=B_SPLINE_CURVE_WITH_KNOTS('',3,(#78350,#78351,#78352,#78353,#78354,
#78355,#78356,#78357),.UNSPECIFIED.,.F.,.F.,(4,2,2,4),(1.77292731488234E-6,
0.00863675577096559,0.0171409248953735,0.0172810711148425),
 .UNSPECIFIED.);
#1728=B_SPLINE_CURVE_WITH_KNOTS('',3,(#78382,#78383,#78384,#78385,#78386,
#78387),.UNSPECIFIED.,.F.,.F.,(4,2,4),(0.,0.0198536183160875,0.0397081495930974),
 .UNSPECIFIED.);
#1729=B_SPLINE_CURVE_WITH_KNOTS('',3,(#78405,#78406,#78407,#78408,#78409,
#78410),.UNSPECIFIED.,.F.,.F.,(4,2,4),(-0.00212384862416112,-0.00106192594848514,
0.),.UNSPECIFIED.);
#1730=B_SPLINE_CURVE_WITH_KNOTS('',3,(#78411,#78412,#78413,#78414,#78415,
#78416),.UNSPECIFIED.,.F.,.F.,(4,2,4),(9.9999841687486E-7,0.0193527898667748,
0.0387045796213571),.UNSPECIFIED.);
#1731=B_SPLINE_CURVE_WITH_KNOTS('',3,(#78422,#78423,#78424,#78425,#78426,
#78427),.UNSPECIFIED.,.F.,.F.,(4,2,4),(-0.00212486503056007,-0.00106293275801356,
-1.00000000012482E-6),.UNSPECIFIED.);
#1732=B_SPLINE_CURVE_WITH_KNOTS('',3,(#78466,#78467,#78468,#78469,#78470,
#78471),.UNSPECIFIED.,.F.,.F.,(4,2,4),(0.,0.0198583386648012,0.0397175618073442),
 .UNSPECIFIED.);
#1733=B_SPLINE_CURVE_WITH_KNOTS('',3,(#78484,#78485,#78486,#78487,#78488,
#78489),.UNSPECIFIED.,.F.,.F.,(4,2,4),(0.,0.0198761966601199,0.0397532848749042),
 .UNSPECIFIED.);
#1734=B_SPLINE_CURVE_WITH_KNOTS('',3,(#78541,#78542,#78543,#78544,#78545,
#78546),.UNSPECIFIED.,.F.,.F.,(4,2,4),(0.,0.0199008240773645,0.0398025406710212),
 .UNSPECIFIED.);
#1735=B_SPLINE_CURVE_WITH_KNOTS('',3,(#78559,#78560,#78561,#78562,#78563,
#78564),.UNSPECIFIED.,.F.,.F.,(4,2,4),(0.,0.0199042047128573,0.0398092891591882),
 .UNSPECIFIED.);
#1736=B_SPLINE_CURVE_WITH_KNOTS('',3,(#78612,#78613,#78614,#78615,#78616,
#78617),.UNSPECIFIED.,.F.,.F.,(4,2,4),(0.,0.0198954793664142,0.0397918615380289),
 .UNSPECIFIED.);
#1737=B_SPLINE_CURVE_WITH_KNOTS('',3,(#78657,#78658,#78659,#78660,#78661,
#78662,#78663),.UNSPECIFIED.,.F.,.F.,(4,3,4),(0.,0.5,0.999990117164971),
 .UNSPECIFIED.);
#1738=B_SPLINE_CURVE_WITH_KNOTS('',3,(#78686,#78687,#78688,#78689,#78690,
#78691),.UNSPECIFIED.,.F.,.F.,(4,2,4),(0.,0.0198677119514339,0.0397363341070424),
 .UNSPECIFIED.);
#1739=B_SPLINE_CURVE_WITH_KNOTS('',3,(#78733,#78734,#78735,#78736,#78737,
#78738),.UNSPECIFIED.,.F.,.F.,(4,2,4),(0.,0.0198973965889047,0.0397956842881278),
 .UNSPECIFIED.);
#1740=B_SPLINE_CURVE_WITH_KNOTS('',3,(#78760,#78761,#78762,#78763,#78764,
#78765),.UNSPECIFIED.,.F.,.F.,(4,2,4),(0.,0.0199030680184938,0.0398070348140193),
 .UNSPECIFIED.);
#1741=B_SPLINE_CURVE_WITH_KNOTS('',3,(#78810,#78811,#78812,#78813,#78814,
#78815),.UNSPECIFIED.,.F.,.F.,(4,2,4),(0.,0.0198994178707068,0.0397997368248638),
 .UNSPECIFIED.);
#1742=B_SPLINE_CURVE_WITH_KNOTS('',3,(#78828,#78829,#78830,#78831,#78832,
#78833),.UNSPECIFIED.,.F.,.F.,(4,2,4),(0.,0.0198905179572786,0.0397819072688436),
 .UNSPECIFIED.);
#1743=B_SPLINE_CURVE_WITH_KNOTS('',3,(#78858,#78859,#78860,#78861,#78862,
#78863,#78864),.UNSPECIFIED.,.F.,.F.,(4,3,4),(0.0365944846647006,0.0384615384615384,
0.0431466153076599),.UNSPECIFIED.);
#1744=B_SPLINE_CURVE_WITH_KNOTS('',3,(#78865,#78866,#78867,#78868,#78869,
#78870,#78871,#78872),.UNSPECIFIED.,.F.,.F.,(4,2,2,4),(1.77258020099164E-6,
0.00863675570858734,0.0171409061550788,0.0172810544018275),
 .UNSPECIFIED.);
#1745=B_SPLINE_CURVE_WITH_KNOTS('',3,(#78897,#78898,#78899,#78900,#78901,
#78902),.UNSPECIFIED.,.F.,.F.,(4,2,4),(0.,0.0198536183145067,0.0397081495869588),
 .UNSPECIFIED.);
#1746=B_SPLINE_CURVE_WITH_KNOTS('',3,(#78920,#78921,#78922,#78923,#78924,
#78925),.UNSPECIFIED.,.F.,.F.,(4,2,4),(-0.00212384856218078,-0.00106192592379002,
0.),.UNSPECIFIED.);
#1747=B_SPLINE_CURVE_WITH_KNOTS('',3,(#78926,#78927,#78928,#78929,#78930,
#78931),.UNSPECIFIED.,.F.,.F.,(4,2,4),(9.99998415920771E-7,0.0193527803902452,
0.0387045693980609),.UNSPECIFIED.);
#1748=B_SPLINE_CURVE_WITH_KNOTS('',3,(#78937,#78938,#78939,#78940,#78941,
#78942),.UNSPECIFIED.,.F.,.F.,(4,2,4),(-0.00212486443485167,-0.00106293275784374,
-9.99999999056443E-7),.UNSPECIFIED.);
#1749=B_SPLINE_CURVE_WITH_KNOTS('',3,(#78981,#78982,#78983,#78984,#78985,
#78986),.UNSPECIFIED.,.F.,.F.,(4,2,4),(0.,0.0198583386637869,0.0397175618035615),
 .UNSPECIFIED.);
#1750=B_SPLINE_CURVE_WITH_KNOTS('',3,(#78999,#79000,#79001,#79002,#79003,
#79004),.UNSPECIFIED.,.F.,.F.,(4,2,4),(0.,0.0198761967104589,0.0397532849902813),
 .UNSPECIFIED.);
#1751=B_SPLINE_CURVE_WITH_KNOTS('',3,(#79056,#79057,#79058,#79059,#79060,
#79061),.UNSPECIFIED.,.F.,.F.,(4,2,4),(0.,0.0199008240757587,0.0398025406643214),
 .UNSPECIFIED.);
#1752=B_SPLINE_CURVE_WITH_KNOTS('',3,(#79074,#79075,#79076,#79077,#79078,
#79079),.UNSPECIFIED.,.F.,.F.,(4,2,4),(0.,0.0199042046967123,0.0398092891327804),
 .UNSPECIFIED.);
#1753=B_SPLINE_CURVE_WITH_KNOTS('',3,(#79127,#79128,#79129,#79130,#79131,
#79132),.UNSPECIFIED.,.F.,.F.,(4,2,4),(0.,0.0198954793650519,0.039791861532841),
 .UNSPECIFIED.);
#1754=B_SPLINE_CURVE_WITH_KNOTS('',3,(#79172,#79173,#79174,#79175,#79176,
#79177,#79178),.UNSPECIFIED.,.F.,.F.,(4,3,4),(0.,0.5,0.999990117164572),
 .UNSPECIFIED.);
#1755=B_SPLINE_CURVE_WITH_KNOTS('',3,(#79201,#79202,#79203,#79204,#79205,
#79206),.UNSPECIFIED.,.F.,.F.,(4,2,4),(0.,0.019867711951081,0.0397363341059826),
 .UNSPECIFIED.);
#1756=B_SPLINE_CURVE_WITH_KNOTS('',3,(#79248,#79249,#79250,#79251,#79252,
#79253),.UNSPECIFIED.,.F.,.F.,(4,2,4),(0.,0.0198973965879299,0.0397956842843274),
 .UNSPECIFIED.);
#1757=B_SPLINE_CURVE_WITH_KNOTS('',3,(#79275,#79276,#79277,#79278,#79279,
#79280),.UNSPECIFIED.,.F.,.F.,(4,2,4),(0.,0.0199030680185526,0.0398070348141684),
 .UNSPECIFIED.);
#1758=B_SPLINE_CURVE_WITH_KNOTS('',3,(#79325,#79326,#79327,#79328,#79329,
#79330),.UNSPECIFIED.,.F.,.F.,(4,2,4),(0.,0.0198994178698969,0.0397997368217084),
 .UNSPECIFIED.);
#1759=B_SPLINE_CURVE_WITH_KNOTS('',3,(#79343,#79344,#79345,#79346,#79347,
#79348),.UNSPECIFIED.,.F.,.F.,(4,2,4),(0.,0.0198905179572962,0.039781907256784),
 .UNSPECIFIED.);
#1760=B_SPLINE_CURVE_WITH_KNOTS('',3,(#79373,#79374,#79375,#79376,#79377,
#79378,#79379),.UNSPECIFIED.,.F.,.F.,(4,3,4),(0.0365944846647006,0.0384615384615384,
0.0431466153076591),.UNSPECIFIED.);
#1761=B_SPLINE_CURVE_WITH_KNOTS('',3,(#79380,#79381,#79382,#79383,#79384,
#79385,#79386,#79387),.UNSPECIFIED.,.F.,.F.,(4,2,2,4),(1.77350751380791E-6,
0.0086367557881011,0.0171409177879644,0.0172810646875839),.UNSPECIFIED.);
#1762=B_SPLINE_CURVE_WITH_KNOTS('',3,(#79412,#79413,#79414,#79415,#79416,
#79417),.UNSPECIFIED.,.F.,.F.,(4,2,4),(0.,0.0198536183132773,0.0397081495822158),
 .UNSPECIFIED.);
#1763=B_SPLINE_CURVE_WITH_KNOTS('',3,(#79435,#79436,#79437,#79438,#79439,
#79440),.UNSPECIFIED.,.F.,.F.,(4,2,4),(-0.00212385087314715,-0.00106192684123349,
0.),.UNSPECIFIED.);
#1764=B_SPLINE_CURVE_WITH_KNOTS('',3,(#79441,#79442,#79443,#79444,#79445,
#79446),.UNSPECIFIED.,.F.,.F.,(4,2,4),(9.99998417712879E-7,0.0193527846157326,
0.0387045795193881),.UNSPECIFIED.);
#1765=B_SPLINE_CURVE_WITH_KNOTS('',3,(#79452,#79453,#79454,#79455,#79456,
#79457),.UNSPECIFIED.,.F.,.F.,(4,2,4),(-0.00212486389546323,-0.0010629327504673,
-9.99999998651385E-7),.UNSPECIFIED.);
#1766=B_SPLINE_CURVE_WITH_KNOTS('',3,(#79496,#79497,#79498,#79499,#79500,
#79501),.UNSPECIFIED.,.F.,.F.,(4,2,4),(0.,0.0198583386619873,0.0397175617964205),
 .UNSPECIFIED.);
#1767=B_SPLINE_CURVE_WITH_KNOTS('',3,(#79514,#79515,#79516,#79517,#79518,
#79519),.UNSPECIFIED.,.F.,.F.,(4,2,4),(0.,0.0198761967014612,0.0397532849518429),
 .UNSPECIFIED.);
#1768=B_SPLINE_CURVE_WITH_KNOTS('',3,(#79571,#79572,#79573,#79574,#79575,
#79576),.UNSPECIFIED.,.F.,.F.,(4,2,4),(0.,0.0199008240741428,0.0398025406583395),
 .UNSPECIFIED.);
#1769=B_SPLINE_CURVE_WITH_KNOTS('',3,(#79589,#79590,#79591,#79592,#79593,
#79594),.UNSPECIFIED.,.F.,.F.,(4,2,4),(0.,0.0199042047186291,0.0398092891745138),
 .UNSPECIFIED.);
#1770=B_SPLINE_CURVE_WITH_KNOTS('',3,(#79642,#79643,#79644,#79645,#79646,
#79647),.UNSPECIFIED.,.F.,.F.,(4,2,4),(0.,0.0198954793632857,0.0397918615254757),
 .UNSPECIFIED.);
#1771=B_SPLINE_CURVE_WITH_KNOTS('',3,(#79687,#79688,#79689,#79690,#79691,
#79692,#79693),.UNSPECIFIED.,.F.,.F.,(4,3,4),(0.,0.5,0.999990117162871),
 .UNSPECIFIED.);
#1772=B_SPLINE_CURVE_WITH_KNOTS('',3,(#79716,#79717,#79718,#79719,#79720,
#79721),.UNSPECIFIED.,.F.,.F.,(4,2,4),(0.,0.0198677119513824,0.0397363341067771),
 .UNSPECIFIED.);
#1773=B_SPLINE_CURVE_WITH_KNOTS('',3,(#79763,#79764,#79765,#79766,#79767,
#79768),.UNSPECIFIED.,.F.,.F.,(4,2,4),(0.,0.019897396586304,0.0397956842776212),
 .UNSPECIFIED.);
#1774=B_SPLINE_CURVE_WITH_KNOTS('',3,(#79790,#79791,#79792,#79793,#79794,
#79795),.UNSPECIFIED.,.F.,.F.,(4,2,4),(0.,0.0199030680185807,0.0398070348140608),
 .UNSPECIFIED.);
#1775=B_SPLINE_CURVE_WITH_KNOTS('',3,(#79840,#79841,#79842,#79843,#79844,
#79845),.UNSPECIFIED.,.F.,.F.,(4,2,4),(0.,0.0198994178679604,0.0397997368137069),
 .UNSPECIFIED.);
#1776=B_SPLINE_CURVE_WITH_KNOTS('',3,(#79858,#79859,#79860,#79861,#79862,
#79863),.UNSPECIFIED.,.F.,.F.,(4,2,4),(0.,0.0198905179567476,0.0397819072467453),
 .UNSPECIFIED.);
#1777=B_SPLINE_CURVE_WITH_KNOTS('',3,(#79888,#79889,#79890,#79891,#79892,
#79893,#79894),.UNSPECIFIED.,.F.,.F.,(4,3,4),(0.0365944846647015,0.0384615384615384,
0.0431466153076602),.UNSPECIFIED.);
#1778=B_SPLINE_CURVE_WITH_KNOTS('',3,(#79895,#79896,#79897,#79898,#79899,
#79900,#79901,#79902),.UNSPECIFIED.,.F.,.F.,(4,2,2,4),(1.77257984617272E-6,
0.00863675584960567,0.0171409478371716,0.0172810916427102),
 .UNSPECIFIED.);
#1779=B_SPLINE_CURVE_WITH_KNOTS('',3,(#79927,#79928,#79929,#79930,#79931,
#79932),.UNSPECIFIED.,.F.,.F.,(4,2,4),(0.,0.0198536183117049,0.0397081495761841),
 .UNSPECIFIED.);
#1780=B_SPLINE_CURVE_WITH_KNOTS('',3,(#79950,#79951,#79952,#79953,#79954,
#79955),.UNSPECIFIED.,.F.,.F.,(4,2,4),(-0.00212385226401534,-0.00106192740973201,
0.),.UNSPECIFIED.);
#1781=B_SPLINE_CURVE_WITH_KNOTS('',3,(#79956,#79957,#79958,#79959,#79960,
#79961),.UNSPECIFIED.,.F.,.F.,(4,2,4),(9.99998417825365E-7,0.0193527904136142,
0.0387045796348744),.UNSPECIFIED.);
#1782=B_SPLINE_CURVE_WITH_KNOTS('',3,(#79967,#79968,#79969,#79970,#79971,
#79972),.UNSPECIFIED.,.F.,.F.,(4,2,4),(-0.00212486331074845,-0.00106293275284134,
-1.00000000155683E-6),.UNSPECIFIED.);
#1783=B_SPLINE_CURVE_WITH_KNOTS('',3,(#80011,#80012,#80013,#80014,#80015,
#80016),.UNSPECIFIED.,.F.,.F.,(4,2,4),(0.,0.0198583386611987,0.0397175617931082),
 .UNSPECIFIED.);
#1784=B_SPLINE_CURVE_WITH_KNOTS('',3,(#80029,#80030,#80031,#80032,#80033,
#80034),.UNSPECIFIED.,.F.,.F.,(4,2,4),(0.,0.0198761966899037,0.039753284941563),
 .UNSPECIFIED.);
#1785=B_SPLINE_CURVE_WITH_KNOTS('',3,(#80086,#80087,#80088,#80089,#80090,
#80091),.UNSPECIFIED.,.F.,.F.,(4,2,4),(0.,0.0199008240728521,0.0398025406528661),
 .UNSPECIFIED.);
#1786=B_SPLINE_CURVE_WITH_KNOTS('',3,(#80104,#80105,#80106,#80107,#80108,
#80109),.UNSPECIFIED.,.F.,.F.,(4,2,4),(0.,0.0199042047187496,0.03980928917477),
 .UNSPECIFIED.);
#1787=B_SPLINE_CURVE_WITH_KNOTS('',3,(#80157,#80158,#80159,#80160,#80161,
#80162),.UNSPECIFIED.,.F.,.F.,(4,2,4),(0.,0.0198954793619581,0.0397918615199839),
 .UNSPECIFIED.);
#1788=B_SPLINE_CURVE_WITH_KNOTS('',3,(#80202,#80203,#80204,#80205,#80206,
#80207,#80208),.UNSPECIFIED.,.F.,.F.,(4,3,4),(0.,0.5,0.999990117160646),
 .UNSPECIFIED.);
#1789=B_SPLINE_CURVE_WITH_KNOTS('',3,(#80231,#80232,#80233,#80234,#80235,
#80236),.UNSPECIFIED.,.F.,.F.,(4,2,4),(0.,0.0198677119502807,0.039736334103427),
 .UNSPECIFIED.);
#1790=B_SPLINE_CURVE_WITH_KNOTS('',3,(#80278,#80279,#80280,#80281,#80282,
#80283),.UNSPECIFIED.,.F.,.F.,(4,2,4),(0.,0.0198973965839471,0.0397956842684524),
 .UNSPECIFIED.);
#1791=B_SPLINE_CURVE_WITH_KNOTS('',3,(#80305,#80306,#80307,#80308,#80309,
#80310),.UNSPECIFIED.,.F.,.F.,(4,2,4),(0.,0.0199030680177332,0.0398070348109682),
 .UNSPECIFIED.);
#1792=B_SPLINE_CURVE_WITH_KNOTS('',3,(#80355,#80356,#80357,#80358,#80359,
#80360),.UNSPECIFIED.,.F.,.F.,(4,2,4),(0.,0.0198994178663628,0.0397997368074939),
 .UNSPECIFIED.);
#1793=B_SPLINE_CURVE_WITH_KNOTS('',3,(#80373,#80374,#80375,#80376,#80377,
#80378),.UNSPECIFIED.,.F.,.F.,(4,2,4),(0.,0.0198905179571887,0.0397819072607149),
 .UNSPECIFIED.);
#1794=B_SPLINE_CURVE_WITH_KNOTS('',3,(#80403,#80404,#80405,#80406,#80407,
#80408,#80409),.UNSPECIFIED.,.F.,.F.,(4,3,4),(0.0365944846647005,0.0384615384615384,
0.0431466153076602),.UNSPECIFIED.);
#1795=B_SPLINE_CURVE_WITH_KNOTS('',3,(#80410,#80411,#80412,#80413,#80414,
#80415,#80416,#80417),.UNSPECIFIED.,.F.,.F.,(4,2,2,4),(1.77257993802502E-6,
0.00863675581682755,0.0171409344827175,0.0172810797173663),
 .UNSPECIFIED.);
#1796=B_SPLINE_CURVE_WITH_KNOTS('',3,(#80442,#80443,#80444,#80445,#80446,
#80447),.UNSPECIFIED.,.F.,.F.,(4,2,4),(0.,0.0198536183101753,0.0397081495702501),
 .UNSPECIFIED.);
#1797=B_SPLINE_CURVE_WITH_KNOTS('',3,(#80465,#80466,#80467,#80468,#80469,
#80470),.UNSPECIFIED.,.F.,.F.,(4,2,4),(-0.0021238541167507,-0.00106192814372196,
0.),.UNSPECIFIED.);
#1798=B_SPLINE_CURVE_WITH_KNOTS('',3,(#80471,#80472,#80473,#80474,#80475,
#80476),.UNSPECIFIED.,.F.,.F.,(4,2,4),(9.99998419123142E-7,0.0193527904127871,
0.0387045796331662),.UNSPECIFIED.);
#1799=B_SPLINE_CURVE_WITH_KNOTS('',3,(#80482,#80483,#80484,#80485,#80486,
#80487),.UNSPECIFIED.,.F.,.F.,(4,2,4),(-0.00212486283058553,-0.00106293276585407,
-1.00000000193045E-6),.UNSPECIFIED.);
#1800=B_SPLINE_CURVE_WITH_KNOTS('',3,(#80526,#80527,#80528,#80529,#80530,
#80531),.UNSPECIFIED.,.F.,.F.,(4,2,4),(0.,0.0198583386596414,0.0397175617869763),
 .UNSPECIFIED.);
#1801=B_SPLINE_CURVE_WITH_KNOTS('',3,(#80544,#80545,#80546,#80547,#80548,
#80549),.UNSPECIFIED.,.F.,.F.,(4,2,4),(0.,0.0198761965688489,0.0397532846844471),
 .UNSPECIFIED.);
#1802=B_SPLINE_CURVE_WITH_KNOTS('',3,(#80601,#80602,#80603,#80604,#80605,
#80606),.UNSPECIFIED.,.F.,.F.,(4,2,4),(0.,0.0199008240713145,0.0398025406471834),
 .UNSPECIFIED.);
#1803=B_SPLINE_CURVE_WITH_KNOTS('',3,(#80619,#80620,#80621,#80622,#80623,
#80624),.UNSPECIFIED.,.F.,.F.,(4,2,4),(0.,0.0199042047187008,0.0398092891715554),
 .UNSPECIFIED.);
#1804=B_SPLINE_CURVE_WITH_KNOTS('',3,(#80672,#80673,#80674,#80675,#80676,
#80677),.UNSPECIFIED.,.F.,.F.,(4,2,4),(0.,0.019895979281645,0.0397918613086002),
 .UNSPECIFIED.);
#1805=B_SPLINE_CURVE_WITH_KNOTS('',3,(#80717,#80718,#80719,#80720,#80721,
#80722,#80723),.UNSPECIFIED.,.F.,.F.,(4,3,4),(0.,0.5,0.99999011715943),
 .UNSPECIFIED.);
#1806=B_SPLINE_CURVE_WITH_KNOTS('',3,(#80746,#80747,#80748,#80749,#80750,
#80751),.UNSPECIFIED.,.F.,.F.,(4,2,4),(0.,0.0198677119493813,0.0397363340992066),
 .UNSPECIFIED.);
#1807=B_SPLINE_CURVE_WITH_KNOTS('',3,(#80793,#80794,#80795,#80796,#80797,
#80798),.UNSPECIFIED.,.F.,.F.,(4,2,4),(0.,0.0198973965800523,0.0397956842522655),
 .UNSPECIFIED.);
#1808=B_SPLINE_CURVE_WITH_KNOTS('',3,(#80820,#80821,#80822,#80823,#80824,
#80825),.UNSPECIFIED.,.F.,.F.,(4,2,4),(0.,0.0199030680179019,0.0398070348114157),
 .UNSPECIFIED.);
#1809=B_SPLINE_CURVE_WITH_KNOTS('',3,(#80870,#80871,#80872,#80873,#80874,
#80875),.UNSPECIFIED.,.F.,.F.,(4,2,4),(0.,0.0198994178626952,0.0397997367921896),
 .UNSPECIFIED.);
#1810=B_SPLINE_CURVE_WITH_KNOTS('',3,(#80888,#80889,#80890,#80891,#80892,
#80893),.UNSPECIFIED.,.F.,.F.,(4,2,4),(0.,0.0198905179575111,0.0397819072674916),
 .UNSPECIFIED.);
#1811=B_SPLINE_CURVE_WITH_KNOTS('',3,(#80918,#80919,#80920,#80921,#80922,
#80923,#80924),.UNSPECIFIED.,.F.,.F.,(4,3,4),(0.0365944846647006,0.0384615384615384,
0.0431466153076597),.UNSPECIFIED.);
#1812=B_SPLINE_CURVE_WITH_KNOTS('',3,(#80925,#80926,#80927,#80928,#80929,
#80930,#80931,#80932),.UNSPECIFIED.,.F.,.F.,(4,2,2,4),(1.77257997374341E-6,
0.00863675581523217,0.0171409311328255,0.0172810767227047),
 .UNSPECIFIED.);
#1813=B_SPLINE_CURVE_WITH_KNOTS('',3,(#80957,#80958,#80959,#80960,#80961,
#80962),.UNSPECIFIED.,.F.,.F.,(4,2,4),(0.,0.0198536183074313,0.0397081495588918),
 .UNSPECIFIED.);
#1814=B_SPLINE_CURVE_WITH_KNOTS('',3,(#80980,#80981,#80982,#80983,#80984,
#80985),.UNSPECIFIED.,.F.,.F.,(4,2,4),(-0.00212385633540368,-0.00106192904131713,
0.),.UNSPECIFIED.);
#1815=B_SPLINE_CURVE_WITH_KNOTS('',3,(#80986,#80987,#80988,#80989,#80990,
#80991),.UNSPECIFIED.,.F.,.F.,(4,2,4),(9.99998410553807E-7,0.0193527753876696,
0.0387045692985089),.UNSPECIFIED.);
#1816=B_SPLINE_CURVE_WITH_KNOTS('',3,(#80997,#80998,#80999,#81000,#81001,
#81002),.UNSPECIFIED.,.F.,.F.,(4,2,4),(-0.0021248622707656,-0.00106293276671975,
-1.00000000055655E-6),.UNSPECIFIED.);
#1817=B_SPLINE_CURVE_WITH_KNOTS('',3,(#81041,#81042,#81043,#81044,#81045,
#81046),.UNSPECIFIED.,.F.,.F.,(4,2,4),(0.,0.0198583386584655,0.0397175617823022),
 .UNSPECIFIED.);
#1818=B_SPLINE_CURVE_WITH_KNOTS('',3,(#81059,#81060,#81061,#81062,#81063,
#81064),.UNSPECIFIED.,.F.,.F.,(4,2,4),(0.,0.0198761967007967,0.0397532849597277),
 .UNSPECIFIED.);
#1819=B_SPLINE_CURVE_WITH_KNOTS('',3,(#81116,#81117,#81118,#81119,#81120,
#81121),.UNSPECIFIED.,.F.,.F.,(4,2,4),(0.,0.0199008240701687,0.0398025406425139),
 .UNSPECIFIED.);
#1820=B_SPLINE_CURVE_WITH_KNOTS('',3,(#81134,#81135,#81136,#81137,#81138,
#81139),.UNSPECIFIED.,.F.,.F.,(4,2,4),(0.,0.0199042047188792,0.0398092891791789),
 .UNSPECIFIED.);
#1821=B_SPLINE_CURVE_WITH_KNOTS('',3,(#81187,#81188,#81189,#81190,#81191,
#81192),.UNSPECIFIED.,.F.,.F.,(4,2,4),(0.,0.0198954793595894,0.0397918615110356),
 .UNSPECIFIED.);
#1822=B_SPLINE_CURVE_WITH_KNOTS('',3,(#81232,#81233,#81234,#81235,#81236,
#81237,#81238),.UNSPECIFIED.,.F.,.F.,(4,3,4),(0.,0.5,0.999990117156445),
 .UNSPECIFIED.);
#1823=B_SPLINE_CURVE_WITH_KNOTS('',3,(#81261,#81262,#81263,#81264,#81265,
#81266),.UNSPECIFIED.,.F.,.F.,(4,2,4),(0.,0.0198677119497614,0.0397363341009546),
 .UNSPECIFIED.);
#1824=B_SPLINE_CURVE_WITH_KNOTS('',3,(#81308,#81309,#81310,#81311,#81312,
#81313),.UNSPECIFIED.,.F.,.F.,(4,2,4),(0.,0.0198973965760269,0.0397956842361046),
 .UNSPECIFIED.);
#1825=B_SPLINE_CURVE_WITH_KNOTS('',3,(#81335,#81336,#81337,#81338,#81339,
#81340),.UNSPECIFIED.,.F.,.F.,(4,2,4),(0.,0.0199030680172686,0.0398070348086195),
 .UNSPECIFIED.);
#1826=B_SPLINE_CURVE_WITH_KNOTS('',3,(#81382,#81383,#81384,#81385,#81386,
#81387),.UNSPECIFIED.,.F.,.F.,(4,2,4),(0.,0.0198994178579901,0.0397997367735032),
 .UNSPECIFIED.);
#1827=B_SPLINE_CURVE_WITH_KNOTS('',3,(#81407,#81408,#81409,#81410,#81411,
#81412),.UNSPECIFIED.,.F.,.F.,(4,2,4),(0.,0.0198905727828699,0.0397820348380782),
 .UNSPECIFIED.);
#1828=B_SPLINE_CURVE_WITH_KNOTS('',3,(#81437,#81438,#81439,#81440,#81441,
#81442,#81443),.UNSPECIFIED.,.F.,.F.,(4,3,4),(0.0365944846647011,0.0384615384615384,
0.0431466153076595),.UNSPECIFIED.);
#1829=B_SPLINE_CURVE_WITH_KNOTS('',3,(#81444,#81445,#81446,#81447,#81448,
#81449,#81450,#81451),.UNSPECIFIED.,.F.,.F.,(4,2,2,4),(1.77258011691398E-6,
0.00863675577077701,0.0171409165754082,0.017281063727439),.UNSPECIFIED.);
#1830=B_SPLINE_CURVE_WITH_KNOTS('',3,(#81476,#81477,#81478,#81479,#81480,
#81481),.UNSPECIFIED.,.F.,.F.,(4,2,4),(0.,0.0198536183030717,0.039708149541506),
 .UNSPECIFIED.);
#1831=B_SPLINE_CURVE_WITH_KNOTS('',3,(#81499,#81500,#81501,#81502,#81503,
#81504),.UNSPECIFIED.,.F.,.F.,(4,2,4),(-0.00212385871063614,-0.00106192998404695,
0.),.UNSPECIFIED.);
#1832=B_SPLINE_CURVE_WITH_KNOTS('',3,(#81505,#81506,#81507,#81508,#81509,
#81510),.UNSPECIFIED.,.F.,.F.,(4,2,4),(9.99998418614826E-7,0.0193527904140548,
0.0387045796357254),.UNSPECIFIED.);
#1833=B_SPLINE_CURVE_WITH_KNOTS('',3,(#81516,#81517,#81518,#81519,#81520,
#81521),.UNSPECIFIED.,.F.,.F.,(4,2,4),(-0.00212486175378365,-0.00106293276587914,
-1.00000000015431E-6),.UNSPECIFIED.);
#1834=B_SPLINE_CURVE_WITH_KNOTS('',3,(#81560,#81561,#81562,#81563,#81564,
#81565),.UNSPECIFIED.,.F.,.F.,(4,2,4),(0.,0.0198583386549503,0.0397175617682779),
 .UNSPECIFIED.);
#1835=B_SPLINE_CURVE_WITH_KNOTS('',3,(#81578,#81579,#81580,#81581,#81582,
#81583),.UNSPECIFIED.,.F.,.F.,(4,2,4),(0.,0.0198761966973816,0.0397532849399191),
 .UNSPECIFIED.);
#1836=B_SPLINE_CURVE_WITH_KNOTS('',3,(#81635,#81636,#81637,#81638,#81639,
#81640),.UNSPECIFIED.,.F.,.F.,(4,2,4),(0.,0.0199008240672371,0.0398025406305121),
 .UNSPECIFIED.);
#1837=B_SPLINE_CURVE_WITH_KNOTS('',3,(#81653,#81654,#81655,#81656,#81657,
#81658),.UNSPECIFIED.,.F.,.F.,(4,2,4),(0.,0.0199042046967335,0.0398092891201385),
 .UNSPECIFIED.);
#1838=B_SPLINE_CURVE_WITH_KNOTS('',3,(#81706,#81707,#81708,#81709,#81710,
#81711),.UNSPECIFIED.,.F.,.F.,(4,2,4),(0.,0.0198954793574705,0.0397918615025454),
 .UNSPECIFIED.);
#1839=B_SPLINE_CURVE_WITH_KNOTS('',3,(#81751,#81752,#81753,#81754,#81755,
#81756,#81757),.UNSPECIFIED.,.F.,.F.,(4,3,4),(0.,0.5,0.999990117154057),
 .UNSPECIFIED.);
#1840=B_SPLINE_CURVE_WITH_KNOTS('',3,(#81780,#81781,#81782,#81783,#81784,
#81785),.UNSPECIFIED.,.F.,.F.,(4,2,4),(0.,0.0198677119483035,0.0397363340951872),
 .UNSPECIFIED.);
#1841=B_SPLINE_CURVE_WITH_KNOTS('',3,(#81827,#81828,#81829,#81830,#81831,
#81832),.UNSPECIFIED.,.F.,.F.,(4,2,4),(0.,0.0198973965729276,0.0397956842231821),
 .UNSPECIFIED.);
#1842=B_SPLINE_CURVE_WITH_KNOTS('',3,(#81854,#81855,#81856,#81857,#81858,
#81859),.UNSPECIFIED.,.F.,.F.,(4,2,4),(0.,0.0199030680155105,0.0398070348020406),
 .UNSPECIFIED.);
#1843=B_SPLINE_CURVE_WITH_KNOTS('',3,(#81904,#81905,#81906,#81907,#81908,
#81909),.UNSPECIFIED.,.F.,.F.,(4,2,4),(0.,0.0198994178544206,0.0397997367588171),
 .UNSPECIFIED.);
#1844=B_SPLINE_CURVE_WITH_KNOTS('',3,(#81922,#81923,#81924,#81925,#81926,
#81927),.UNSPECIFIED.,.F.,.F.,(4,2,4),(0.,0.0198905179573927,0.0397819072603145),
 .UNSPECIFIED.);
#1845=B_SPLINE_CURVE_WITH_KNOTS('',3,(#81953,#81954,#81955,#81956,#81957,
#81958),.UNSPECIFIED.,.F.,.F.,(4,2,4),(0.0365944846647007,0.0384615384615384,
0.0431466153076597),.UNSPECIFIED.);
#1846=B_SPLINE_CURVE_WITH_KNOTS('',3,(#81959,#81960,#81961,#81962,#81963,
#81964,#81965),.UNSPECIFIED.,.F.,.F.,(4,3,4),(0.,0.00863415824062196,0.0172757271482925),
 .UNSPECIFIED.);
#1847=B_SPLINE_CURVE_WITH_KNOTS('',3,(#81990,#81991,#81992,#81993,#81994,
#81995),.UNSPECIFIED.,.F.,.F.,(4,2,4),(0.,0.0198536182496097,0.0397081494264778),
 .UNSPECIFIED.);
#1848=B_SPLINE_CURVE_WITH_KNOTS('',3,(#82008,#82009,#82010,#82011,#82012,
#82013),.UNSPECIFIED.,.F.,.F.,(4,2,4),(-0.00212386114214876,-0.00106193095631279,
0.),.UNSPECIFIED.);
#1849=B_SPLINE_CURVE_WITH_KNOTS('',3,(#82014,#82015,#82016,#82017,#82018,
#82019),.UNSPECIFIED.,.F.,.F.,(4,2,4),(9.99998416295649E-7,0.0193522753878931,
0.0387045692978022),.UNSPECIFIED.);
#1850=B_SPLINE_CURVE_WITH_KNOTS('',3,(#82025,#82026,#82027,#82028,#82029,
#82030),.UNSPECIFIED.,.F.,.F.,(4,2,4),(-0.00212486125230607,-0.00106293276248913,
-9.99999999050588E-7),.UNSPECIFIED.);
#1851=B_SPLINE_CURVE_WITH_KNOTS('',3,(#82069,#82070,#82071,#82072,#82073,
#82074),.UNSPECIFIED.,.F.,.F.,(4,2,4),(0.,0.0198583386509932,0.0397175617519128),
 .UNSPECIFIED.);
#1852=B_SPLINE_CURVE_WITH_KNOTS('',3,(#82087,#82088,#82089,#82090,#82091,
#82092),.UNSPECIFIED.,.F.,.F.,(4,2,4),(0.,0.0198761967152631,0.0397532849904637),
 .UNSPECIFIED.);
#1853=B_SPLINE_CURVE_WITH_KNOTS('',3,(#82144,#82145,#82146,#82147,#82148,
#82149),.UNSPECIFIED.,.F.,.F.,(4,2,4),(0.,0.0199008240626534,0.0398025406124932),
 .UNSPECIFIED.);
#1854=B_SPLINE_CURVE_WITH_KNOTS('',3,(#82162,#82163,#82164,#82165,#82166,
#82167),.UNSPECIFIED.,.F.,.F.,(4,2,4),(0.,0.0199042047190279,0.0398092891738967),
 .UNSPECIFIED.);
#1855=B_SPLINE_CURVE_WITH_KNOTS('',3,(#82215,#82216,#82217,#82218,#82219,
#82220),.UNSPECIFIED.,.F.,.F.,(4,2,4),(0.,0.019895479353864,0.039791861487405),
 .UNSPECIFIED.);
#1856=B_SPLINE_CURVE_WITH_KNOTS('',3,(#82260,#82261,#82262,#82263,#82264,
#82265,#82266),.UNSPECIFIED.,.F.,.F.,(4,3,4),(0.,0.5,0.999990117151758),
 .UNSPECIFIED.);
#1857=B_SPLINE_CURVE_WITH_KNOTS('',3,(#82289,#82290,#82291,#82292,#82293,
#82294),.UNSPECIFIED.,.F.,.F.,(4,2,4),(0.,0.0198677119425251,0.0397363340720499),
 .UNSPECIFIED.);
#1858=B_SPLINE_CURVE_WITH_KNOTS('',3,(#82336,#82337,#82338,#82339,#82340,
#82341),.UNSPECIFIED.,.F.,.F.,(4,2,4),(0.,0.019897396570235,0.03979568421255),
 .UNSPECIFIED.);
#1859=B_SPLINE_CURVE_WITH_KNOTS('',3,(#82363,#82364,#82365,#82366,#82367,
#82368),.UNSPECIFIED.,.F.,.F.,(4,2,4),(0.,0.0199030680124401,0.039807034789456),
 .UNSPECIFIED.);
#1860=B_SPLINE_CURVE_WITH_KNOTS('',3,(#82413,#82414,#82415,#82416,#82417,
#82418),.UNSPECIFIED.,.F.,.F.,(4,2,4),(0.,0.0198994177390595,0.0397997364069847),
 .UNSPECIFIED.);
#1861=B_SPLINE_CURVE_WITH_KNOTS('',3,(#82431,#82432,#82433,#82434,#82435,
#82436),.UNSPECIFIED.,.F.,.F.,(4,2,4),(0.,0.0198905179574466,0.0397819072636344),
 .UNSPECIFIED.);
#1862=B_SPLINE_CURVE_WITH_KNOTS('',3,(#82461,#82462,#82463,#82464,#82465,
#82466,#82467),.UNSPECIFIED.,.F.,.F.,(4,3,4),(0.036594484664701,0.0384615384615384,
0.0431466153076601),.UNSPECIFIED.);
#1863=B_SPLINE_CURVE_WITH_KNOTS('',3,(#82468,#82469,#82470,#82471,#82472,
#82473,#82474,#82475),.UNSPECIFIED.,.F.,.F.,(4,2,2,4),(1.7725796662609E-6,
0.00863675589283121,0.0171409825398772,0.017281122632475),.UNSPECIFIED.);
#1864=B_SPLINE_CURVE_WITH_KNOTS('',3,(#82500,#82501,#82502,#82503,#82504,
#82505),.UNSPECIFIED.,.F.,.F.,(4,2,4),(0.,0.0198536182960252,0.0397081495129872),
 .UNSPECIFIED.);
#1865=B_SPLINE_CURVE_WITH_KNOTS('',3,(#82523,#82524,#82525,#82526,#82527,
#82528),.UNSPECIFIED.,.F.,.F.,(4,2,4),(-0.00212386406946142,-0.00106193213051581,
0.),.UNSPECIFIED.);
#1866=B_SPLINE_CURVE_WITH_KNOTS('',3,(#82529,#82530,#82531,#82532,#82533,
#82534),.UNSPECIFIED.,.F.,.F.,(4,2,4),(9.999984119248E-7,0.0193527803903459,
0.0387045693982159),.UNSPECIFIED.);
#1867=B_SPLINE_CURVE_WITH_KNOTS('',3,(#82540,#82541,#82542,#82543,#82544,
#82545),.UNSPECIFIED.,.F.,.F.,(4,2,4),(-0.00212486080361574,-0.0010629327631662,
-9.9999995856301E-7),.UNSPECIFIED.);
#1868=B_SPLINE_CURVE_WITH_KNOTS('',3,(#82581,#82582,#82583,#82584,#82585,
#82586),.UNSPECIFIED.,.F.,.F.,(4,2,4),(0.,0.0198583386475972,0.0397175617382976),
 .UNSPECIFIED.);
#1869=B_SPLINE_CURVE_WITH_KNOTS('',3,(#82606,#82607,#82608,#82609,#82610,
#82611),.UNSPECIFIED.,.F.,.F.,(4,2,4),(0.,0.0198762583887502,0.0397534251573493),
 .UNSPECIFIED.);
#1870=B_SPLINE_CURVE_WITH_KNOTS('',3,(#82663,#82664,#82665,#82666,#82667,
#82668),.UNSPECIFIED.,.F.,.F.,(4,2,4),(0.,0.0199008240587804,0.0398025405967764),
 .UNSPECIFIED.);
#1871=B_SPLINE_CURVE_WITH_KNOTS('',3,(#82681,#82682,#82683,#82684,#82685,
#82686),.UNSPECIFIED.,.F.,.F.,(4,2,4),(0.,0.0199042046968128,0.0398092891349481),
 .UNSPECIFIED.);
#1872=B_SPLINE_CURVE_WITH_KNOTS('',3,(#82734,#82735,#82736,#82737,#82738,
#82739),.UNSPECIFIED.,.F.,.F.,(4,2,4),(0.,0.0198954793496364,0.0397918614699736),
 .UNSPECIFIED.);
#1873=B_SPLINE_CURVE_WITH_KNOTS('',3,(#82779,#82780,#82781,#82782,#82783,
#82784,#82785),.UNSPECIFIED.,.F.,.F.,(4,3,4),(0.,0.5,0.999990117148265),
 .UNSPECIFIED.);
#1874=B_SPLINE_CURVE_WITH_KNOTS('',3,(#82808,#82809,#82810,#82811,#82812,
#82813),.UNSPECIFIED.,.F.,.F.,(4,2,4),(0.,0.0198677119379566,0.0397363340538177),
 .UNSPECIFIED.);
#1875=B_SPLINE_CURVE_WITH_KNOTS('',3,(#82855,#82856,#82857,#82858,#82859,
#82860),.UNSPECIFIED.,.F.,.F.,(4,2,4),(0.,0.0198973965677259,0.039795684202283),
 .UNSPECIFIED.);
#1876=B_SPLINE_CURVE_WITH_KNOTS('',3,(#82882,#82883,#82884,#82885,#82886,
#82887),.UNSPECIFIED.,.F.,.F.,(4,2,4),(0.,0.0199030680078316,0.0398070347704704),
 .UNSPECIFIED.);
#1877=B_SPLINE_CURVE_WITH_KNOTS('',3,(#82932,#82933,#82934,#82935,#82936,
#82937),.UNSPECIFIED.,.F.,.F.,(4,2,4),(0.,0.0198994178487356,0.0397997367357689),
 .UNSPECIFIED.);
#1878=B_SPLINE_CURVE_WITH_KNOTS('',3,(#82950,#82951,#82952,#82953,#82954,
#82955),.UNSPECIFIED.,.F.,.F.,(4,2,4),(0.,0.0198905179573299,0.0397819072639096),
 .UNSPECIFIED.);
#1879=B_SPLINE_CURVE_WITH_KNOTS('',3,(#82980,#82981,#82982,#82983,#82984,
#82985,#82986),.UNSPECIFIED.,.F.,.F.,(4,3,4),(0.0365944846647014,0.0384615384615384,
0.04314661530766),.UNSPECIFIED.);
#1880=B_SPLINE_CURVE_WITH_KNOTS('',3,(#82987,#82988,#82989,#82990,#82991,
#82992,#82993,#82994),.UNSPECIFIED.,.F.,.F.,(4,2,2,4),(1.77257983382598E-6,
0.00863675586255013,0.0171409553449648,0.0172810983525703),
 .UNSPECIFIED.);
#1881=B_SPLINE_CURVE_WITH_KNOTS('',3,(#83019,#83020,#83021,#83022,#83023,
#83024),.UNSPECIFIED.,.F.,.F.,(4,2,4),(0.,0.0198536182927432,0.0397081495002002),
 .UNSPECIFIED.);
#1882=B_SPLINE_CURVE_WITH_KNOTS('',3,(#83042,#83043,#83044,#83045,#83046,
#83047),.UNSPECIFIED.,.F.,.F.,(4,2,4),(-0.00212386589842508,-0.00106193285457721,
0.),.UNSPECIFIED.);
#1883=B_SPLINE_CURVE_WITH_KNOTS('',3,(#83048,#83049,#83050,#83051,#83052,
#83053),.UNSPECIFIED.,.F.,.F.,(4,2,4),(9.999984136454E-7,0.0193527803893325,
0.0387045693968282),.UNSPECIFIED.);
#1884=B_SPLINE_CURVE_WITH_KNOTS('',3,(#83059,#83060,#83061,#83062,#83063,
#83064),.UNSPECIFIED.,.F.,.F.,(4,2,4),(-0.00212486040271112,-0.00106293276267297,
-9.99999999499947E-7),.UNSPECIFIED.);
#1885=B_SPLINE_CURVE_WITH_KNOTS('',3,(#83103,#83104,#83105,#83106,#83107,
#83108),.UNSPECIFIED.,.F.,.F.,(4,2,4),(0.,0.0198583386450044,0.0397175617275022),
 .UNSPECIFIED.);
#1886=B_SPLINE_CURVE_WITH_KNOTS('',3,(#83121,#83122,#83123,#83124,#83125,
#83126),.UNSPECIFIED.,.F.,.F.,(4,2,4),(0.,0.0198761966898207,0.0397532849432792),
 .UNSPECIFIED.);
#1887=B_SPLINE_CURVE_WITH_KNOTS('',3,(#83178,#83179,#83180,#83181,#83182,
#83183),.UNSPECIFIED.,.F.,.F.,(4,2,4),(0.,0.0199008240557302,0.0398025405845411),
 .UNSPECIFIED.);
#1888=B_SPLINE_CURVE_WITH_KNOTS('',3,(#83203,#83204,#83205,#83206,#83207,
#83208),.UNSPECIFIED.,.F.,.F.,(4,2,4),(0.,0.0199042622253509,0.0398094216210589),
 .UNSPECIFIED.);
#1889=B_SPLINE_CURVE_WITH_KNOTS('',3,(#83256,#83257,#83258,#83259,#83260,
#83261),.UNSPECIFIED.,.F.,.F.,(4,2,4),(0.,0.0198954793460365,0.039791861455587),
 .UNSPECIFIED.);
#1890=B_SPLINE_CURVE_WITH_KNOTS('',3,(#83301,#83302,#83303,#83304,#83305,
#83306,#83307),.UNSPECIFIED.,.F.,.F.,(4,3,4),(0.,0.5,0.999990117145585),
 .UNSPECIFIED.);
#1891=B_SPLINE_CURVE_WITH_KNOTS('',3,(#83330,#83331,#83332,#83333,#83334,
#83335),.UNSPECIFIED.,.F.,.F.,(4,2,4),(0.,0.0198677119330699,0.0397363340341339),
 .UNSPECIFIED.);
#1892=B_SPLINE_CURVE_WITH_KNOTS('',3,(#83377,#83378,#83379,#83380,#83381,
#83382),.UNSPECIFIED.,.F.,.F.,(4,2,4),(0.,0.0198973965657402,0.0397956841946094),
 .UNSPECIFIED.);
#1893=B_SPLINE_CURVE_WITH_KNOTS('',3,(#83404,#83405,#83406,#83407,#83408,
#83409),.UNSPECIFIED.,.F.,.F.,(4,2,4),(0.,0.0199030680030106,0.0398070347510793),
 .UNSPECIFIED.);
#1894=B_SPLINE_CURVE_WITH_KNOTS('',3,(#83454,#83455,#83456,#83457,#83458,
#83459),.UNSPECIFIED.,.F.,.F.,(4,2,4),(0.,0.0198994178466467,0.0397997367273577),
 .UNSPECIFIED.);
#1895=B_SPLINE_CURVE_WITH_KNOTS('',3,(#83472,#83473,#83474,#83475,#83476,
#83477),.UNSPECIFIED.,.F.,.F.,(4,2,4),(0.,0.0198905179575656,0.0397819072622247),
 .UNSPECIFIED.);
#1896=B_SPLINE_CURVE_WITH_KNOTS('',3,(#83502,#83503,#83504,#83505,#83506,
#83507,#83508),.UNSPECIFIED.,.F.,.F.,(4,3,4),(0.0365944846647009,0.0384615384615384,
0.0431466153076601),.UNSPECIFIED.);
#1897=B_SPLINE_CURVE_WITH_KNOTS('',3,(#83509,#83510,#83511,#83512,#83513,
#83514,#83515,#83516),.UNSPECIFIED.,.F.,.F.,(4,2,2,4),(1.77257991476566E-6,
0.00863675580737219,0.017140944467863,0.017281088627107),.UNSPECIFIED.);
#1898=B_SPLINE_CURVE_WITH_KNOTS('',3,(#83541,#83542,#83543,#83544,#83545,
#83546),.UNSPECIFIED.,.F.,.F.,(4,2,4),(0.,0.0198536182901603,0.0397081494900814),
 .UNSPECIFIED.);
#1899=B_SPLINE_CURVE_WITH_KNOTS('',3,(#83564,#83565,#83566,#83567,#83568,
#83569),.UNSPECIFIED.,.F.,.F.,(4,2,4),(-0.00212386958331815,-0.0010619343358337,
0.),.UNSPECIFIED.);
#1900=B_SPLINE_CURVE_WITH_KNOTS('',3,(#83570,#83571,#83572,#83573,#83574,
#83575),.UNSPECIFIED.,.F.,.F.,(4,2,4),(9.99998417085594E-7,0.0193527904138238,
0.0387045796352013),.UNSPECIFIED.);
#1901=B_SPLINE_CURVE_WITH_KNOTS('',3,(#83581,#83582,#83583,#83584,#83585,
#83586),.UNSPECIFIED.,.F.,.F.,(4,2,4),(-0.00212486007883822,-0.00106293276263092,
-1.00000000208484E-6),.UNSPECIFIED.);
#1902=B_SPLINE_CURVE_WITH_KNOTS('',3,(#83625,#83626,#83627,#83628,#83629,
#83630),.UNSPECIFIED.,.F.,.F.,(4,2,4),(0.,0.0198583386419039,0.0397175617148195),
 .UNSPECIFIED.);
#1903=B_SPLINE_CURVE_WITH_KNOTS('',3,(#83643,#83644,#83645,#83646,#83647,
#83648),.UNSPECIFIED.,.F.,.F.,(4,2,4),(0.,0.0198761965843594,0.0397532847208746),
 .UNSPECIFIED.);
#1904=B_SPLINE_CURVE_WITH_KNOTS('',3,(#83700,#83701,#83702,#83703,#83704,
#83705),.UNSPECIFIED.,.F.,.F.,(4,2,4),(0.,0.0199008240528343,0.0398025405727771),
 .UNSPECIFIED.);
#1905=B_SPLINE_CURVE_WITH_KNOTS('',3,(#83718,#83719,#83720,#83721,#83722,
#83723),.UNSPECIFIED.,.F.,.F.,(4,2,4),(0.,0.0199042047135222,0.039809289172212),
 .UNSPECIFIED.);
#1906=B_SPLINE_CURVE_WITH_KNOTS('',3,(#83768,#83769,#83770,#83771,#83772,
#83773),.UNSPECIFIED.,.F.,.F.,(4,2,4),(0.,0.0198954793428837,0.0397918614431882),
 .UNSPECIFIED.);
#1907=B_SPLINE_CURVE_WITH_KNOTS('',3,(#83820,#83821,#83822,#83823,#83824,
#83825,#83826),.UNSPECIFIED.,.F.,.F.,(4,3,4),(0.,0.5,0.999990117143057),
 .UNSPECIFIED.);
#1908=B_SPLINE_CURVE_WITH_KNOTS('',3,(#83849,#83850,#83851,#83852,#83853,
#83854),.UNSPECIFIED.,.F.,.F.,(4,2,4),(0.,0.0198677119280884,0.0397363340135476),
 .UNSPECIFIED.);
#1909=B_SPLINE_CURVE_WITH_KNOTS('',3,(#83896,#83897,#83898,#83899,#83900,
#83901),.UNSPECIFIED.,.F.,.F.,(4,2,4),(0.,0.0198973965647451,0.0397956841902401),
 .UNSPECIFIED.);
#1910=B_SPLINE_CURVE_WITH_KNOTS('',3,(#83923,#83924,#83925,#83926,#83927,
#83928),.UNSPECIFIED.,.F.,.F.,(4,2,4),(0.,0.0199030679985029,0.0398070347325486),
 .UNSPECIFIED.);
#1911=B_SPLINE_CURVE_WITH_KNOTS('',3,(#83973,#83974,#83975,#83976,#83977,
#83978),.UNSPECIFIED.,.F.,.F.,(4,2,4),(0.,0.0198994178454141,0.0397997367225458),
 .UNSPECIFIED.);
#1912=B_SPLINE_CURVE_WITH_KNOTS('',3,(#83991,#83992,#83993,#83994,#83995,
#83996),.UNSPECIFIED.,.F.,.F.,(4,2,4),(0.,0.0198905179578417,0.039781907267824),
 .UNSPECIFIED.);
#1913=B_SPLINE_CURVE_WITH_KNOTS('',3,(#84021,#84022,#84023,#84024,#84025,
#84026,#84027),.UNSPECIFIED.,.F.,.F.,(4,3,4),(0.0365944846647011,0.0384615384615384,
0.0431466153076598),.UNSPECIFIED.);
#1914=B_SPLINE_CURVE_WITH_KNOTS('',3,(#84028,#84029,#84030,#84031,#84032,
#84033,#84034,#84035),.UNSPECIFIED.,.F.,.F.,(4,2,2,4),(1.77350747916397E-6,
0.00863675580036768,0.017140922315829,0.0172810687295207),.UNSPECIFIED.);
#1915=B_SPLINE_CURVE_WITH_KNOTS('',3,(#84060,#84061,#84062,#84063,#84064,
#84065),.UNSPECIFIED.,.F.,.F.,(4,2,4),(0.,0.0198536182877321,0.0397081494798666),
 .UNSPECIFIED.);
#1916=B_SPLINE_CURVE_WITH_KNOTS('',3,(#84083,#84084,#84085,#84086,#84087,
#84088),.UNSPECIFIED.,.F.,.F.,(4,2,4),(-0.00212387260142457,-0.00106193554358744,
0.),.UNSPECIFIED.);
#1917=B_SPLINE_CURVE_WITH_KNOTS('',3,(#84089,#84090,#84091,#84092,#84093,
#84094),.UNSPECIFIED.,.F.,.F.,(4,2,4),(9.99998417845244E-7,0.0193527896159823,
0.0387045796147699),.UNSPECIFIED.);
#1918=B_SPLINE_CURVE_WITH_KNOTS('',3,(#84100,#84101,#84102,#84103,#84104,
#84105),.UNSPECIFIED.,.F.,.F.,(4,2,4),(-0.00212485975597055,-0.00106293275863081,
-1.00000000247038E-6),.UNSPECIFIED.);
#1919=B_SPLINE_CURVE_WITH_KNOTS('',3,(#84144,#84145,#84146,#84147,#84148,
#84149),.UNSPECIFIED.,.F.,.F.,(4,2,4),(0.,0.0198583386395679,0.0397175617056758),
 .UNSPECIFIED.);
#1920=B_SPLINE_CURVE_WITH_KNOTS('',3,(#84162,#84163,#84164,#84165,#84166,
#84167),.UNSPECIFIED.,.F.,.F.,(4,2,4),(0.,0.0198761966924393,0.0397532849423359),
 .UNSPECIFIED.);
#1921=B_SPLINE_CURVE_WITH_KNOTS('',3,(#84219,#84220,#84221,#84222,#84223,
#84224),.UNSPECIFIED.,.F.,.F.,(4,2,4),(0.,0.0199008240503633,0.0398025405628424),
 .UNSPECIFIED.);
#1922=B_SPLINE_CURVE_WITH_KNOTS('',3,(#84237,#84238,#84239,#84240,#84241,
#84242),.UNSPECIFIED.,.F.,.F.,(4,2,4),(0.,0.0199042047129859,0.0398092891685953),
 .UNSPECIFIED.);
#1923=B_SPLINE_CURVE_WITH_KNOTS('',3,(#84290,#84291,#84292,#84293,#84294,
#84295),.UNSPECIFIED.,.F.,.F.,(4,2,4),(0.,0.0198954793400186,0.0397918614313439),
 .UNSPECIFIED.);
#1924=B_SPLINE_CURVE_WITH_KNOTS('',3,(#84335,#84336,#84337,#84338,#84339,
#84340,#84341),.UNSPECIFIED.,.F.,.F.,(4,3,4),(0.,0.5,0.999990117139736),
 .UNSPECIFIED.);
#1925=B_SPLINE_CURVE_WITH_KNOTS('',3,(#84364,#84365,#84366,#84367,#84368,
#84369),.UNSPECIFIED.,.F.,.F.,(4,2,4),(0.,0.0198677119226095,0.0397363339916417),
 .UNSPECIFIED.);
#1926=B_SPLINE_CURVE_WITH_KNOTS('',3,(#84411,#84412,#84413,#84414,#84415,
#84416),.UNSPECIFIED.,.F.,.F.,(4,2,4),(0.,0.0198973965640123,0.0397956841869985),
 .UNSPECIFIED.);
#1927=B_SPLINE_CURVE_WITH_KNOTS('',3,(#84438,#84439,#84440,#84441,#84442,
#84443),.UNSPECIFIED.,.F.,.F.,(4,2,4),(0.,0.0199030679932799,0.0398070347114654),
 .UNSPECIFIED.);
#1928=B_SPLINE_CURVE_WITH_KNOTS('',3,(#84488,#84489,#84490,#84491,#84492,
#84493),.UNSPECIFIED.,.F.,.F.,(4,2,4),(0.,0.0198994178439414,0.0397997367162081),
 .UNSPECIFIED.);
#1929=B_SPLINE_CURVE_WITH_KNOTS('',3,(#84506,#84507,#84508,#84509,#84510,
#84511),.UNSPECIFIED.,.F.,.F.,(4,2,4),(0.,0.019890517442833,0.0397819062338529),
 .UNSPECIFIED.);
#1930=B_SPLINE_CURVE_WITH_KNOTS('',3,(#84536,#84537,#84538,#84539,#84540,
#84541,#84542),.UNSPECIFIED.,.F.,.F.,(4,3,4),(0.0365944846647008,0.0384615384615384,
0.0431466153076597),.UNSPECIFIED.);
#1931=B_SPLINE_CURVE_WITH_KNOTS('',3,(#84543,#84544,#84545,#84546,#84547,
#84548,#84549,#84550),.UNSPECIFIED.,.F.,.F.,(4,2,2,4),(1.77292709988644E-6,
0.0086367558366745,0.0171409573179643,0.0172811000564802),.UNSPECIFIED.);
#1932=B_SPLINE_CURVE_WITH_KNOTS('',3,(#84575,#84576,#84577,#84578,#84579,
#84580),.UNSPECIFIED.,.F.,.F.,(4,2,4),(0.,0.0198536182904639,0.0397081494895467),
 .UNSPECIFIED.);
#1933=B_SPLINE_CURVE_WITH_KNOTS('',3,(#84598,#84599,#84600,#84601,#84602,
#84603),.UNSPECIFIED.,.F.,.F.,(4,2,4),(-0.00212387561594626,-0.00106193674627472,
0.),.UNSPECIFIED.);
#1934=B_SPLINE_CURVE_WITH_KNOTS('',3,(#84604,#84605,#84606,#84607,#84608,
#84609),.UNSPECIFIED.,.F.,.F.,(4,2,4),(9.99998416488062E-7,0.0193532848499299,
0.0387045795217607),.UNSPECIFIED.);
#1935=B_SPLINE_CURVE_WITH_KNOTS('',3,(#84615,#84616,#84617,#84618,#84619,
#84620),.UNSPECIFIED.,.F.,.F.,(4,2,4),(-0.00212485951467819,-0.00106293276219924,
-1.00000000035185E-6),.UNSPECIFIED.);
#1936=B_SPLINE_CURVE_WITH_KNOTS('',3,(#84659,#84660,#84661,#84662,#84663,
#84664),.UNSPECIFIED.,.F.,.F.,(4,2,4),(0.,0.0198583386383744,0.0397175617010874),
 .UNSPECIFIED.);
#1937=B_SPLINE_CURVE_WITH_KNOTS('',3,(#84677,#84678,#84679,#84680,#84681,
#84682),.UNSPECIFIED.,.F.,.F.,(4,2,4),(0.,0.0198761966567487,0.0397532848798819),
 .UNSPECIFIED.);
#1938=B_SPLINE_CURVE_WITH_KNOTS('',3,(#84734,#84735,#84736,#84737,#84738,
#84739),.UNSPECIFIED.,.F.,.F.,(4,2,4),(0.,0.0199008240483616,0.0398025405546555),
 .UNSPECIFIED.);
#1939=B_SPLINE_CURVE_WITH_KNOTS('',3,(#84752,#84753,#84754,#84755,#84756,
#84757),.UNSPECIFIED.,.F.,.F.,(4,2,4),(0.,0.0199042047130261,0.0398092891574592),
 .UNSPECIFIED.);
#1940=B_SPLINE_CURVE_WITH_KNOTS('',3,(#84805,#84806,#84807,#84808,#84809,
#84810),.UNSPECIFIED.,.F.,.F.,(4,2,4),(0.,0.0198954793377787,0.0397918614218809),
 .UNSPECIFIED.);
#1941=B_SPLINE_CURVE_WITH_KNOTS('',3,(#84850,#84851,#84852,#84853,#84854,
#84855,#84856),.UNSPECIFIED.,.F.,.F.,(4,3,4),(0.,0.5,0.999990117136952),
 .UNSPECIFIED.);
#1942=B_SPLINE_CURVE_WITH_KNOTS('',3,(#84879,#84880,#84881,#84882,#84883,
#84884),.UNSPECIFIED.,.F.,.F.,(4,2,4),(0.,0.0198677119178716,0.0397363339724512),
 .UNSPECIFIED.);
#1943=B_SPLINE_CURVE_WITH_KNOTS('',3,(#84926,#84927,#84928,#84929,#84930,
#84931),.UNSPECIFIED.,.F.,.F.,(4,2,4),(0.,0.019897396564037,0.0397956841876327),
 .UNSPECIFIED.);
#1944=B_SPLINE_CURVE_WITH_KNOTS('',3,(#84953,#84954,#84955,#84956,#84957,
#84958),.UNSPECIFIED.,.F.,.F.,(4,2,4),(0.,0.0199030679169175,0.0398070344753143),
 .UNSPECIFIED.);
#1945=B_SPLINE_CURVE_WITH_KNOTS('',3,(#85003,#85004,#85005,#85006,#85007,
#85008),.UNSPECIFIED.,.F.,.F.,(4,2,4),(0.,0.0198994178439266,0.0397997367162002),
 .UNSPECIFIED.);
#1946=B_SPLINE_CURVE_WITH_KNOTS('',3,(#85021,#85022,#85023,#85024,#85025,
#85026),.UNSPECIFIED.,.F.,.F.,(4,2,4),(0.,0.0198905179576396,0.0397819072528401),
 .UNSPECIFIED.);
#1947=B_SPLINE_CURVE_WITH_KNOTS('',3,(#85051,#85052,#85053,#85054,#85055,
#85056,#85057),.UNSPECIFIED.,.F.,.F.,(4,3,4),(0.0365944846647013,0.0384615384615384,
0.0431466153076595),.UNSPECIFIED.);
#1948=B_SPLINE_CURVE_WITH_KNOTS('',3,(#85058,#85059,#85060,#85061,#85062,
#85063,#85064,#85065),.UNSPECIFIED.,.F.,.F.,(4,2,2,4),(1.77257998041709E-6,
0.00863675581017835,0.0171409340093189,0.0172810792958315),
 .UNSPECIFIED.);
#1949=B_SPLINE_CURVE_WITH_KNOTS('',3,(#85090,#85091,#85092,#85093,#85094,
#85095),.UNSPECIFIED.,.F.,.F.,(4,2,4),(0.,0.0198536182858879,0.0397081494725743),
 .UNSPECIFIED.);
#1950=B_SPLINE_CURVE_WITH_KNOTS('',3,(#85113,#85114,#85115,#85116,#85117,
#85118),.UNSPECIFIED.,.F.,.F.,(4,2,4),(-0.00212387854594797,-0.00106193791950009,
0.),.UNSPECIFIED.);
#1951=B_SPLINE_CURVE_WITH_KNOTS('',3,(#85119,#85120,#85121,#85122,#85123,
#85124),.UNSPECIFIED.,.F.,.F.,(4,2,4),(9.9999841885959E-7,0.019352785410249,
0.0387045795338068),.UNSPECIFIED.);
#1952=B_SPLINE_CURVE_WITH_KNOTS('',3,(#85130,#85131,#85132,#85133,#85134,
#85135),.UNSPECIFIED.,.F.,.F.,(4,2,4),(-0.00212485939877907,-0.00106293275771695,
-1.0000000009139E-6),.UNSPECIFIED.);
#1953=B_SPLINE_CURVE_WITH_KNOTS('',3,(#85174,#85175,#85176,#85177,#85178,
#85179),.UNSPECIFIED.,.F.,.F.,(4,2,4),(0.,0.0198583386375086,0.0397175616972905),
 .UNSPECIFIED.);
#1954=B_SPLINE_CURVE_WITH_KNOTS('',3,(#85192,#85193,#85194,#85195,#85196,
#85197),.UNSPECIFIED.,.F.,.F.,(4,2,4),(0.,0.0198761967049228,0.0397532849789576),
 .UNSPECIFIED.);
#1955=B_SPLINE_CURVE_WITH_KNOTS('',3,(#85249,#85250,#85251,#85252,#85253,
#85254),.UNSPECIFIED.,.F.,.F.,(4,2,4),(0.,0.0199008240467533,0.0398025405489657),
 .UNSPECIFIED.);
#1956=B_SPLINE_CURVE_WITH_KNOTS('',3,(#85267,#85268,#85269,#85270,#85271,
#85272),.UNSPECIFIED.,.F.,.F.,(4,2,4),(0.,0.0199042047189651,0.0398092891742666),
 .UNSPECIFIED.);
#1957=B_SPLINE_CURVE_WITH_KNOTS('',3,(#85320,#85321,#85322,#85323,#85324,
#85325),.UNSPECIFIED.,.F.,.F.,(4,2,4),(0.,0.0198954793358551,0.0397918614147188),
 .UNSPECIFIED.);
#1958=B_SPLINE_CURVE_WITH_KNOTS('',3,(#85365,#85366,#85367,#85368,#85369,
#85370,#85371),.UNSPECIFIED.,.F.,.F.,(4,3,4),(0.,0.5,0.999990117133631),
 .UNSPECIFIED.);
#1959=B_SPLINE_CURVE_WITH_KNOTS('',3,(#85394,#85395,#85396,#85397,#85398,
#85399),.UNSPECIFIED.,.F.,.F.,(4,2,4),(0.,0.0198677119133151,0.0397363339545231),
 .UNSPECIFIED.);
#1960=B_SPLINE_CURVE_WITH_KNOTS('',3,(#85441,#85442,#85443,#85444,#85445,
#85446),.UNSPECIFIED.,.F.,.F.,(4,2,4),(0.,0.019897396565073,0.0397956841914982),
 .UNSPECIFIED.);
#1961=B_SPLINE_CURVE_WITH_KNOTS('',3,(#85468,#85469,#85470,#85471,#85472,
#85473),.UNSPECIFIED.,.F.,.F.,(4,2,4),(0.,0.019903067983549,0.0398070346719),
 .UNSPECIFIED.);
#1962=B_SPLINE_CURVE_WITH_KNOTS('',3,(#85518,#85519,#85520,#85521,#85522,
#85523),.UNSPECIFIED.,.F.,.F.,(4,2,4),(0.,0.0198994178443784,0.0397997367178181),
 .UNSPECIFIED.);
#1963=B_SPLINE_CURVE_WITH_KNOTS('',3,(#85536,#85537,#85538,#85539,#85540,
#85541),.UNSPECIFIED.,.F.,.F.,(4,2,4),(0.,0.0198905179573494,0.0397819072555251),
 .UNSPECIFIED.);
#1964=B_SPLINE_CURVE_WITH_KNOTS('',3,(#85566,#85567,#85568,#85569,#85570,
#85571,#85572),.UNSPECIFIED.,.F.,.F.,(4,3,4),(0.0365944846647011,0.0384615384615384,
0.0431466153076598),.UNSPECIFIED.);
#1965=B_SPLINE_CURVE_WITH_KNOTS('',3,(#85573,#85574,#85575,#85576,#85577,
#85578,#85579,#85580),.UNSPECIFIED.,.F.,.F.,(4,2,2,4),(1.77257445604461E-6,
0.0086367557856313,0.017140932747332,0.0172810781644652),.UNSPECIFIED.);
#1966=B_SPLINE_CURVE_WITH_KNOTS('',3,(#85605,#85606,#85607,#85608,#85609,
#85610),.UNSPECIFIED.,.F.,.F.,(4,2,4),(0.,0.0198536182864876,0.0397081494752219),
 .UNSPECIFIED.);
#1967=B_SPLINE_CURVE_WITH_KNOTS('',3,(#85628,#85629,#85630,#85631,#85632,
#85633),.UNSPECIFIED.,.F.,.F.,(4,2,4),(-0.00212388115337583,-0.00106193896363325,
0.),.UNSPECIFIED.);
#1968=B_SPLINE_CURVE_WITH_KNOTS('',3,(#85634,#85635,#85636,#85637,#85638,
#85639),.UNSPECIFIED.,.F.,.F.,(4,2,4),(9.99998415348017E-7,0.0193527753883658,
0.0387045692997803),.UNSPECIFIED.);
#1969=B_SPLINE_CURVE_WITH_KNOTS('',3,(#85645,#85646,#85647,#85648,#85649,
#85650),.UNSPECIFIED.,.F.,.F.,(4,2,4),(-0.00212485930517326,-0.00106293276164361,
-9.99999999790814E-7),.UNSPECIFIED.);
#1970=B_SPLINE_CURVE_WITH_KNOTS('',3,(#85689,#85690,#85691,#85692,#85693,
#85694),.UNSPECIFIED.,.F.,.F.,(4,2,4),(0.,0.0198583386372447,0.0397175616961046),
 .UNSPECIFIED.);
#1971=B_SPLINE_CURVE_WITH_KNOTS('',3,(#85707,#85708,#85709,#85710,#85711,
#85712),.UNSPECIFIED.,.F.,.F.,(4,2,4),(0.,0.0198761967024035,0.0397532849668273),
 .UNSPECIFIED.);
#1972=B_SPLINE_CURVE_WITH_KNOTS('',3,(#85764,#85765,#85766,#85767,#85768,
#85769),.UNSPECIFIED.,.F.,.F.,(4,2,4),(0.,0.0199008240468501,0.0398025405488885),
 .UNSPECIFIED.);
#1973=B_SPLINE_CURVE_WITH_KNOTS('',3,(#85782,#85783,#85784,#85785,#85786,
#85787),.UNSPECIFIED.,.F.,.F.,(4,2,4),(0.,0.0199042047191258,0.0398092891768156),
 .UNSPECIFIED.);
#1974=B_SPLINE_CURVE_WITH_KNOTS('',3,(#85835,#85836,#85837,#85838,#85839,
#85840),.UNSPECIFIED.,.F.,.F.,(4,2,4),(0.,0.0198954793351462,0.0397918614117019),
 .UNSPECIFIED.);
#1975=B_SPLINE_CURVE_WITH_KNOTS('',3,(#85880,#85881,#85882,#85883,#85884,
#85885,#85886),.UNSPECIFIED.,.F.,.F.,(4,3,4),(0.,0.5,0.999990117130729),
 .UNSPECIFIED.);
#1976=B_SPLINE_CURVE_WITH_KNOTS('',3,(#85909,#85910,#85911,#85912,#85913,
#85914),.UNSPECIFIED.,.F.,.F.,(4,2,4),(0.,0.0198677119088387,0.039736333935962),
 .UNSPECIFIED.);
#1977=B_SPLINE_CURVE_WITH_KNOTS('',3,(#85956,#85957,#85958,#85959,#85960,
#85961),.UNSPECIFIED.,.F.,.F.,(4,2,4),(0.,0.0198973965662461,0.0397956841962341),
 .UNSPECIFIED.);
#1978=B_SPLINE_CURVE_WITH_KNOTS('',3,(#85983,#85984,#85985,#85986,#85987,
#85988),.UNSPECIFIED.,.F.,.F.,(4,2,4),(0.,0.0199030679089294,0.0398070344430507),
 .UNSPECIFIED.);
#1979=B_SPLINE_CURVE_WITH_KNOTS('',3,(#86033,#86034,#86035,#86036,#86037,
#86038),.UNSPECIFIED.,.F.,.F.,(4,2,4),(0.,0.0198994178459843,0.0397997367240867),
 .UNSPECIFIED.);
#1980=B_SPLINE_CURVE_WITH_KNOTS('',3,(#86051,#86052,#86053,#86054,#86055,
#86056),.UNSPECIFIED.,.F.,.F.,(4,2,4),(0.,0.0198905179578903,0.0397819072560775),
 .UNSPECIFIED.);
#1981=B_SPLINE_CURVE_WITH_KNOTS('',3,(#86081,#86082,#86083,#86084,#86085,
#86086,#86087),.UNSPECIFIED.,.F.,.F.,(4,3,4),(0.0365944846647006,0.0384615384615384,
0.0431466153076595),.UNSPECIFIED.);
#1982=B_SPLINE_CURVE_WITH_KNOTS('',3,(#86088,#86089,#86090,#86091,#86092,
#86093,#86094,#86095),.UNSPECIFIED.,.F.,.F.,(4,2,2,4),(1.77257423772781E-6,
0.00863675585116524,0.0171409641324324,0.0172811061893529),
 .UNSPECIFIED.);
#1983=B_SPLINE_CURVE_WITH_KNOTS('',3,(#86120,#86121,#86122,#86123,#86124,
#86125),.UNSPECIFIED.,.F.,.F.,(4,2,4),(0.,0.019853618287136,0.03970814947742),
 .UNSPECIFIED.);
#1984=B_SPLINE_CURVE_WITH_KNOTS('',3,(#86143,#86144,#86145,#86146,#86147,
#86148),.UNSPECIFIED.,.F.,.F.,(4,2,4),(-0.00212388284445759,-0.00106193963809625,
0.),.UNSPECIFIED.);
#1985=B_SPLINE_CURVE_WITH_KNOTS('',3,(#86149,#86150,#86151,#86152,#86153,
#86154),.UNSPECIFIED.,.F.,.F.,(4,2,4),(9.99998416549644E-7,0.019353285396123,
0.0387045795327764),.UNSPECIFIED.);
#1986=B_SPLINE_CURVE_WITH_KNOTS('',3,(#86160,#86161,#86162,#86163,#86164,
#86165),.UNSPECIFIED.,.F.,.F.,(4,2,4),(-0.00212485927854704,-0.00106293275914596,
-1.00000000017165E-6),.UNSPECIFIED.);
#1987=B_SPLINE_CURVE_WITH_KNOTS('',3,(#86204,#86205,#86206,#86207,#86208,
#86209),.UNSPECIFIED.,.F.,.F.,(4,2,4),(0.,0.0198583386380477,0.0397175616990257),
 .UNSPECIFIED.);
#1988=B_SPLINE_CURVE_WITH_KNOTS('',3,(#86222,#86223,#86224,#86225,#86226,
#86227),.UNSPECIFIED.,.F.,.F.,(4,2,4),(0.,0.0198761967031353,0.0397532849810569),
 .UNSPECIFIED.);
#1989=B_SPLINE_CURVE_WITH_KNOTS('',3,(#86279,#86280,#86281,#86282,#86283,
#86284),.UNSPECIFIED.,.F.,.F.,(4,2,4),(0.,0.0199008240464419,0.0398025405473232),
 .UNSPECIFIED.);
#1990=B_SPLINE_CURVE_WITH_KNOTS('',3,(#86297,#86298,#86299,#86300,#86301,
#86302),.UNSPECIFIED.,.F.,.F.,(4,2,4),(0.,0.0199042047190527,0.039809289180571),
 .UNSPECIFIED.);
#1991=B_SPLINE_CURVE_WITH_KNOTS('',3,(#86350,#86351,#86352,#86353,#86354,
#86355),.UNSPECIFIED.,.F.,.F.,(4,2,4),(0.,0.0198954793351661,0.0397918614116676),
 .UNSPECIFIED.);
#1992=B_SPLINE_CURVE_WITH_KNOTS('',3,(#86395,#86396,#86397,#86398,#86399,
#86400,#86401),.UNSPECIFIED.,.F.,.F.,(4,3,4),(0.,0.5,0.999990117128898),
 .UNSPECIFIED.);
#1993=B_SPLINE_CURVE_WITH_KNOTS('',3,(#86424,#86425,#86426,#86427,#86428,
#86429),.UNSPECIFIED.,.F.,.F.,(4,2,4),(0.,0.0198677119052138,0.0397363339218776),
 .UNSPECIFIED.);
#1994=B_SPLINE_CURVE_WITH_KNOTS('',3,(#86471,#86472,#86473,#86474,#86475,
#86476),.UNSPECIFIED.,.F.,.F.,(4,2,4),(0.,0.0198973965680208,0.0397956842029936),
 .UNSPECIFIED.);
#1995=B_SPLINE_CURVE_WITH_KNOTS('',3,(#86498,#86499,#86500,#86501,#86502,
#86503),.UNSPECIFIED.,.F.,.F.,(4,2,4),(0.,0.0199030679777334,0.0398070346486175),
 .UNSPECIFIED.);
#1996=B_SPLINE_CURVE_WITH_KNOTS('',3,(#86548,#86549,#86550,#86551,#86552,
#86553),.UNSPECIFIED.,.F.,.F.,(4,2,4),(0.,0.0198994178470161,0.0397997367286354),
 .UNSPECIFIED.);
#1997=B_SPLINE_CURVE_WITH_KNOTS('',3,(#86566,#86567,#86568,#86569,#86570,
#86571),.UNSPECIFIED.,.F.,.F.,(4,2,4),(0.,0.0198905179576503,0.0397819072501323),
 .UNSPECIFIED.);
#1998=B_SPLINE_CURVE_WITH_KNOTS('',3,(#86596,#86597,#86598,#86599,#86600,
#86601,#86602),.UNSPECIFIED.,.F.,.F.,(4,3,4),(0.0365944846647007,0.0384615384615384,
0.0431466153076595),.UNSPECIFIED.);
#1999=B_SPLINE_CURVE_WITH_KNOTS('',3,(#86603,#86604,#86605,#86606,#86607,
#86608,#86609,#86610),.UNSPECIFIED.,.F.,.F.,(4,2,2,4),(1.77350725314824E-6,
0.00863675587077613,0.0171409468521658,0.0172810906422092),
 .UNSPECIFIED.);
#2000=B_SPLINE_CURVE_WITH_KNOTS('',3,(#86635,#86636,#86637,#86638,#86639,
#86640),.UNSPECIFIED.,.F.,.F.,(4,2,4),(0.,0.0198536182885339,0.0397081494834228),
 .UNSPECIFIED.);
#2001=B_SPLINE_CURVE_WITH_KNOTS('',3,(#86658,#86659,#86660,#86661,#86662,
#86663),.UNSPECIFIED.,.F.,.F.,(4,2,4),(-0.00212388622566706,-0.00106194099469101,
0.),.UNSPECIFIED.);
#2002=B_SPLINE_CURVE_WITH_KNOTS('',3,(#86664,#86665,#86666,#86667,#86668,
#86669),.UNSPECIFIED.,.F.,.F.,(4,2,4),(9.99998417676033E-7,0.0193527846155029,
0.0387045795199078),.UNSPECIFIED.);
#2003=B_SPLINE_CURVE_WITH_KNOTS('',3,(#86675,#86676,#86677,#86678,#86679,
#86680),.UNSPECIFIED.,.F.,.F.,(4,2,4),(-0.00212485935732975,-0.00106293275849113,
-9.9999999990987E-7),.UNSPECIFIED.);
#2004=B_SPLINE_CURVE_WITH_KNOTS('',3,(#86719,#86720,#86721,#86722,#86723,
#86724),.UNSPECIFIED.,.F.,.F.,(4,2,4),(0.,0.0198583386387385,0.0397175617020387),
 .UNSPECIFIED.);
#2005=B_SPLINE_CURVE_WITH_KNOTS('',3,(#86737,#86738,#86739,#86740,#86741,
#86742),.UNSPECIFIED.,.F.,.F.,(4,2,4),(0.,0.0198761966976469,0.0397532849454558),
 .UNSPECIFIED.);
#2006=B_SPLINE_CURVE_WITH_KNOTS('',3,(#86794,#86795,#86796,#86797,#86798,
#86799),.UNSPECIFIED.,.F.,.F.,(4,2,4),(0.,0.0199008240470287,0.0398025405500045),
 .UNSPECIFIED.);
#2007=B_SPLINE_CURVE_WITH_KNOTS('',3,(#86812,#86813,#86814,#86815,#86816,
#86817),.UNSPECIFIED.,.F.,.F.,(4,2,4),(0.,0.0199042047189135,0.0398092891728897),
 .UNSPECIFIED.);
#2008=B_SPLINE_CURVE_WITH_KNOTS('',3,(#86865,#86866,#86867,#86868,#86869,
#86870),.UNSPECIFIED.,.F.,.F.,(4,2,4),(0.,0.0198954793353804,0.0397918614125083),
 .UNSPECIFIED.);
#2009=B_SPLINE_CURVE_WITH_KNOTS('',3,(#86910,#86911,#86912,#86913,#86914,
#86915,#86916),.UNSPECIFIED.,.F.,.F.,(4,3,4),(0.,0.5,0.99999011712649),
 .UNSPECIFIED.);
#2010=B_SPLINE_CURVE_WITH_KNOTS('',3,(#86939,#86940,#86941,#86942,#86943,
#86944),.UNSPECIFIED.,.F.,.F.,(4,2,4),(0.,0.0198677119013193,0.0397363339055224),
 .UNSPECIFIED.);
#2011=B_SPLINE_CURVE_WITH_KNOTS('',3,(#86986,#86987,#86988,#86989,#86990,
#86991),.UNSPECIFIED.,.F.,.F.,(4,2,4),(0.,0.0198973965708148,0.0397956842143026),
 .UNSPECIFIED.);
#2012=B_SPLINE_CURVE_WITH_KNOTS('',3,(#87013,#87014,#87015,#87016,#87017,
#87018),.UNSPECIFIED.,.F.,.F.,(4,2,4),(0.,0.019903067974991,0.039807034637192),
 .UNSPECIFIED.);
#2013=B_SPLINE_CURVE_WITH_KNOTS('',3,(#87063,#87064,#87065,#87066,#87067,
#87068),.UNSPECIFIED.,.F.,.F.,(4,2,4),(0.,0.019899417849379,0.039799736737851),
 .UNSPECIFIED.);
#2014=B_SPLINE_CURVE_WITH_KNOTS('',3,(#87081,#87082,#87083,#87084,#87085,
#87086),.UNSPECIFIED.,.F.,.F.,(4,2,4),(0.,0.0198905179576478,0.0397819072520095),
 .UNSPECIFIED.);
#2015=B_SPLINE_CURVE_WITH_KNOTS('',3,(#87111,#87112,#87113,#87114,#87115,
#87116,#87117),.UNSPECIFIED.,.F.,.F.,(4,3,4),(0.0365944846647008,0.0384615384615384,
0.0431466153076604),.UNSPECIFIED.);
#2016=B_SPLINE_CURVE_WITH_KNOTS('',3,(#87118,#87119,#87120,#87121,#87122,
#87123,#87124,#87125),.UNSPECIFIED.,.F.,.F.,(4,2,2,4),(1.77257424359709E-6,
0.00863675585403953,0.0171409617643079,0.0172811040803507),
 .UNSPECIFIED.);
#2017=B_SPLINE_CURVE_WITH_KNOTS('',3,(#87150,#87151,#87152,#87153,#87154,
#87155),.UNSPECIFIED.,.F.,.F.,(4,2,4),(0.,0.0198536182903914,0.0397081494910964),
 .UNSPECIFIED.);
#2018=B_SPLINE_CURVE_WITH_KNOTS('',3,(#87173,#87174,#87175,#87176,#87177,
#87178),.UNSPECIFIED.,.F.,.F.,(4,2,4),(-0.00212388840135336,-0.00106194186675072,
0.),.UNSPECIFIED.);
#2019=B_SPLINE_CURVE_WITH_KNOTS('',3,(#87179,#87180,#87181,#87182,#87183,
#87184),.UNSPECIFIED.,.F.,.F.,(4,2,4),(9.99998422430955E-7,0.0193522803908578,
0.0387045693979158),.UNSPECIFIED.);
#2020=B_SPLINE_CURVE_WITH_KNOTS('',3,(#87190,#87191,#87192,#87193,#87194,
#87195),.UNSPECIFIED.,.F.,.F.,(4,2,4),(-0.00212485944936608,-0.00106293276036146,
-9.99999998619293E-7),.UNSPECIFIED.);
#2021=B_SPLINE_CURVE_WITH_KNOTS('',3,(#87234,#87235,#87236,#87237,#87238,
#87239),.UNSPECIFIED.,.F.,.F.,(4,2,4),(0.,0.0198583386404155,0.0397175617084474),
 .UNSPECIFIED.);
#2022=B_SPLINE_CURVE_WITH_KNOTS('',3,(#87252,#87253,#87254,#87255,#87256,
#87257),.UNSPECIFIED.,.F.,.F.,(4,2,4),(0.,0.0198761967052115,0.039753284964214),
 .UNSPECIFIED.);
#2023=B_SPLINE_CURVE_WITH_KNOTS('',3,(#87309,#87310,#87311,#87312,#87313,
#87314),.UNSPECIFIED.,.F.,.F.,(4,2,4),(0.,0.0199008240486882,0.0398025405564813),
 .UNSPECIFIED.);
#2024=B_SPLINE_CURVE_WITH_KNOTS('',3,(#87327,#87328,#87329,#87330,#87331,
#87332),.UNSPECIFIED.,.F.,.F.,(4,2,4),(0.,0.0199042046968269,0.0398092891377679),
 .UNSPECIFIED.);
#2025=B_SPLINE_CURVE_WITH_KNOTS('',3,(#87380,#87381,#87382,#87383,#87384,
#87385),.UNSPECIFIED.,.F.,.F.,(4,2,4),(0.,0.0198954793366912,0.0397918614176109),
 .UNSPECIFIED.);
#2026=B_SPLINE_CURVE_WITH_KNOTS('',3,(#87425,#87426,#87427,#87428,#87429,
#87430,#87431),.UNSPECIFIED.,.F.,.F.,(4,3,4),(0.,0.5,0.999990117124345),
 .UNSPECIFIED.);
#2027=B_SPLINE_CURVE_WITH_KNOTS('',3,(#87454,#87455,#87456,#87457,#87458,
#87459),.UNSPECIFIED.,.F.,.F.,(4,2,4),(0.,0.0198677118984356,0.0397363338941566),
 .UNSPECIFIED.);
#2028=B_SPLINE_CURVE_WITH_KNOTS('',3,(#87501,#87502,#87503,#87504,#87505,
#87506),.UNSPECIFIED.,.F.,.F.,(4,2,4),(0.,0.0198973965734549,0.0397956842251395),
 .UNSPECIFIED.);
#2029=B_SPLINE_CURVE_WITH_KNOTS('',3,(#87528,#87529,#87530,#87531,#87532,
#87533),.UNSPECIFIED.,.F.,.F.,(4,2,4),(0.,0.0199030679732815,0.0398070346300929),
 .UNSPECIFIED.);
#2030=B_SPLINE_CURVE_WITH_KNOTS('',3,(#87578,#87579,#87580,#87581,#87582,
#87583),.UNSPECIFIED.,.F.,.F.,(4,2,4),(0.,0.0198994178519258,0.0397997367485529),
 .UNSPECIFIED.);
#2031=B_SPLINE_CURVE_WITH_KNOTS('',3,(#87596,#87597,#87598,#87599,#87600,
#87601),.UNSPECIFIED.,.F.,.F.,(4,2,4),(0.,0.0198905179577305,0.0397819072604309),
 .UNSPECIFIED.);
#2032=B_SPLINE_CURVE_WITH_KNOTS('',3,(#87626,#87627,#87628,#87629,#87630,
#87631,#87632),.UNSPECIFIED.,.F.,.F.,(4,3,4),(0.0365944846647008,0.0384615384615384,
0.0431466153076593),.UNSPECIFIED.);
#2033=B_SPLINE_CURVE_WITH_KNOTS('',3,(#87633,#87634,#87635,#87636,#87637,
#87638,#87639,#87640),.UNSPECIFIED.,.F.,.F.,(4,2,2,4),(1.77350726836409E-6,
0.00863675583502219,0.0171409422935184,0.0172810865614791),
 .UNSPECIFIED.);
#2034=B_SPLINE_CURVE_WITH_KNOTS('',3,(#87665,#87666,#87667,#87668,#87669,
#87670),.UNSPECIFIED.,.F.,.F.,(4,2,4),(0.,0.0198536182928153,0.0397081495005046),
 .UNSPECIFIED.);
#2035=B_SPLINE_CURVE_WITH_KNOTS('',3,(#87688,#87689,#87690,#87691,#87692,
#87693),.UNSPECIFIED.,.F.,.F.,(4,2,4),(-0.00212389023527468,-0.00106194259666521,
0.),.UNSPECIFIED.);
#2036=B_SPLINE_CURVE_WITH_KNOTS('',3,(#87694,#87695,#87696,#87697,#87698,
#87699),.UNSPECIFIED.,.F.,.F.,(4,2,4),(9.9999841659296E-7,0.0193527846149201,
0.0387045795187982),.UNSPECIFIED.);
#2037=B_SPLINE_CURVE_WITH_KNOTS('',3,(#87705,#87706,#87707,#87708,#87709,
#87710),.UNSPECIFIED.,.F.,.F.,(4,2,4),(-0.0021248596145857,-0.0010629327539674,
-9.9999999555859E-7),.UNSPECIFIED.);
#2038=B_SPLINE_CURVE_WITH_KNOTS('',3,(#87749,#87750,#87751,#87752,#87753,
#87754),.UNSPECIFIED.,.F.,.F.,(4,2,4),(0.,0.01985833864266,0.0397175617172488),
 .UNSPECIFIED.);
#2039=B_SPLINE_CURVE_WITH_KNOTS('',3,(#87767,#87768,#87769,#87770,#87771,
#87772),.UNSPECIFIED.,.F.,.F.,(4,2,4),(0.,0.0198761966927882,0.0397532849301295),
 .UNSPECIFIED.);
#2040=B_SPLINE_CURVE_WITH_KNOTS('',3,(#87824,#87825,#87826,#87827,#87828,
#87829),.UNSPECIFIED.,.F.,.F.,(4,2,4),(0.,0.0199008240501793,0.0398025405623191),
 .UNSPECIFIED.);
#2041=B_SPLINE_CURVE_WITH_KNOTS('',3,(#87842,#87843,#87844,#87845,#87846,
#87847),.UNSPECIFIED.,.F.,.F.,(4,2,4),(0.,0.0199042047187131,0.0398092891818602),
 .UNSPECIFIED.);
#2042=B_SPLINE_CURVE_WITH_KNOTS('',3,(#87895,#87896,#87897,#87898,#87899,
#87900),.UNSPECIFIED.,.F.,.F.,(4,2,4),(0.,0.0198954793377096,0.0397918614217478),
 .UNSPECIFIED.);
#2043=B_SPLINE_CURVE_WITH_KNOTS('',3,(#87949,#87950,#87951,#87952,#87953,
#87954,#87955),.UNSPECIFIED.,.F.,.F.,(4,3,4),(0.,0.5,0.999990117122682),
 .UNSPECIFIED.);
#2044=B_SPLINE_CURVE_WITH_KNOTS('',3,(#87975,#87976,#87977,#87978,#87979,
#87980),.UNSPECIFIED.,.F.,.F.,(4,2,4),(0.,0.0198677118957237,0.0397363338827323),
 .UNSPECIFIED.);
#2045=B_SPLINE_CURVE_WITH_KNOTS('',3,(#88016,#88017,#88018,#88019,#88020,
#88021),.UNSPECIFIED.,.F.,.F.,(4,2,4),(0.,0.019897396576599,0.0397956842383687),
 .UNSPECIFIED.);
#2046=B_SPLINE_CURVE_WITH_KNOTS('',3,(#88043,#88044,#88045,#88046,#88047,
#88048),.UNSPECIFIED.,.F.,.F.,(4,2,4),(0.,0.0199030679703947,0.0398070346186951),
 .UNSPECIFIED.);
#2047=B_SPLINE_CURVE_WITH_KNOTS('',3,(#88093,#88094,#88095,#88096,#88097,
#88098),.UNSPECIFIED.,.F.,.F.,(4,2,4),(0.,0.0198994178551836,0.0397997367613937),
 .UNSPECIFIED.);
#2048=B_SPLINE_CURVE_WITH_KNOTS('',3,(#88111,#88112,#88113,#88114,#88115,
#88116),.UNSPECIFIED.,.F.,.F.,(4,2,4),(0.,0.0198905179579926,0.0397819072597309),
 .UNSPECIFIED.);
#2049=B_SPLINE_CURVE_WITH_KNOTS('',3,(#88141,#88142,#88143,#88144,#88145,
#88146,#88147),.UNSPECIFIED.,.F.,.F.,(4,3,4),(0.0365944846647007,0.0384615384615384,
0.0431466153076602),.UNSPECIFIED.);
#2050=B_SPLINE_CURVE_WITH_KNOTS('',3,(#88148,#88149,#88150,#88151,#88152,
#88153,#88154,#88155),.UNSPECIFIED.,.F.,.F.,(4,2,2,4),(1.77257431379691E-6,
0.00863675585003615,0.0171409480655562,0.0172810918447234),
 .UNSPECIFIED.);
#2051=B_SPLINE_CURVE_WITH_KNOTS('',3,(#88180,#88181,#88182,#88183,#88184,
#88185),.UNSPECIFIED.,.F.,.F.,(4,2,4),(0.,0.0198536182957362,0.0397081495124057),
 .UNSPECIFIED.);
#2052=B_SPLINE_CURVE_WITH_KNOTS('',3,(#88203,#88204,#88205,#88206,#88207,
#88208),.UNSPECIFIED.,.F.,.F.,(4,2,4),(-0.00212389196723753,-0.00106194329372377,
0.),.UNSPECIFIED.);
#2053=B_SPLINE_CURVE_WITH_KNOTS('',3,(#88209,#88210,#88211,#88212,#88213,
#88214),.UNSPECIFIED.,.F.,.F.,(4,2,4),(9.99998415913432E-7,0.0193532903992515,
0.0387045796335792),.UNSPECIFIED.);
#2054=B_SPLINE_CURVE_WITH_KNOTS('',3,(#88220,#88221,#88222,#88223,#88224,
#88225),.UNSPECIFIED.,.F.,.F.,(4,2,4),(-0.00212485993964147,-0.00106293276514982,
-9.99999999241842E-7),.UNSPECIFIED.);
#2055=B_SPLINE_CURVE_WITH_KNOTS('',3,(#88264,#88265,#88266,#88267,#88268,
#88269),.UNSPECIFIED.,.F.,.F.,(4,2,4),(0.,0.0198583386451148,0.0397175617274757),
 .UNSPECIFIED.);
#2056=B_SPLINE_CURVE_WITH_KNOTS('',3,(#88282,#88283,#88284,#88285,#88286,
#88287),.UNSPECIFIED.,.F.,.F.,(4,2,4),(0.,0.0198761967052751,0.0397532849527076),
 .UNSPECIFIED.);
#2057=B_SPLINE_CURVE_WITH_KNOTS('',3,(#88339,#88340,#88341,#88342,#88343,
#88344),.UNSPECIFIED.,.F.,.F.,(4,2,4),(0.,0.0199008240526954,0.0398025405729508),
 .UNSPECIFIED.);
#2058=B_SPLINE_CURVE_WITH_KNOTS('',3,(#88357,#88358,#88359,#88360,#88361,
#88362),.UNSPECIFIED.,.F.,.F.,(4,2,4),(0.,0.0199042046062945,0.03980928886621),
 .UNSPECIFIED.);
#2059=B_SPLINE_CURVE_WITH_KNOTS('',3,(#88410,#88411,#88412,#88413,#88414,
#88415),.UNSPECIFIED.,.F.,.F.,(4,2,4),(0.,0.0198954793402216,0.0397918614318321),
 .UNSPECIFIED.);
#2060=B_SPLINE_CURVE_WITH_KNOTS('',3,(#88473,#88474,#88475,#88476,#88477,
#88478,#88479),.UNSPECIFIED.,.F.,.F.,(4,3,4),(0.,0.5,0.999990117121439),
 .UNSPECIFIED.);
#2061=B_SPLINE_CURVE_WITH_KNOTS('',3,(#88499,#88500,#88501,#88502,#88503,
#88504),.UNSPECIFIED.,.F.,.F.,(4,2,4),(0.,0.0198677118935691,0.0397363338743666),
 .UNSPECIFIED.);
#2062=B_SPLINE_CURVE_WITH_KNOTS('',3,(#88543,#88544,#88545,#88546,#88547,
#88548),.UNSPECIFIED.,.F.,.F.,(4,2,4),(0.,0.0198973965805586,0.0397956842538152),
 .UNSPECIFIED.);
#2063=B_SPLINE_CURVE_WITH_KNOTS('',3,(#88567,#88568,#88569,#88570,#88571,
#88572),.UNSPECIFIED.,.F.,.F.,(4,2,4),(0.,0.0199030679694276,0.0398070346147848),
 .UNSPECIFIED.);
#2064=B_SPLINE_CURVE_WITH_KNOTS('',3,(#88608,#88609,#88610,#88611,#88612,
#88613),.UNSPECIFIED.,.F.,.F.,(4,2,4),(0.,0.0198994178595983,0.039799736779155),
 .UNSPECIFIED.);
#2065=B_SPLINE_CURVE_WITH_KNOTS('',3,(#88633,#88634,#88635,#88636,#88637,
#88638),.UNSPECIFIED.,.F.,.F.,(4,2,4),(0.,0.0198905727313931,0.0397820346291919),
 .UNSPECIFIED.);
#2066=B_SPLINE_CURVE_WITH_KNOTS('',3,(#88663,#88664,#88665,#88666,#88667,
#88668,#88669),.UNSPECIFIED.,.F.,.F.,(4,3,4),(0.0365944846647009,0.0384615384615384,
0.0431466153076604),.UNSPECIFIED.);
#2067=B_SPLINE_CURVE_WITH_KNOTS('',3,(#88670,#88671,#88672,#88673,#88674,
#88675,#88676,#88677),.UNSPECIFIED.,.F.,.F.,(4,2,2,4),(1.77257444760541E-6,
0.00863675578236859,0.0171409366166497,0.0172810816176936),
 .UNSPECIFIED.);
#2068=B_SPLINE_CURVE_WITH_KNOTS('',3,(#88702,#88703,#88704,#88705,#88706,
#88707),.UNSPECIFIED.,.F.,.F.,(4,2,4),(0.,0.0198536182988451,0.0397081495254481),
 .UNSPECIFIED.);
#2069=B_SPLINE_CURVE_WITH_KNOTS('',3,(#88725,#88726,#88727,#88728,#88729,
#88730),.UNSPECIFIED.,.F.,.F.,(4,2,4),(-0.0021238923472171,-0.00106194344129639,
0.),.UNSPECIFIED.);
#2070=B_SPLINE_CURVE_WITH_KNOTS('',3,(#88731,#88732,#88733,#88734,#88735,
#88736),.UNSPECIFIED.,.F.,.F.,(4,2,4),(9.99998416362877E-7,0.0193527803909816,
0.0387045693995249),.UNSPECIFIED.);
#2071=B_SPLINE_CURVE_WITH_KNOTS('',3,(#88742,#88743,#88744,#88745,#88746,
#88747),.UNSPECIFIED.,.F.,.F.,(4,2,4),(-0.00212486022885731,-0.00106293276487756,
-9.99999998945638E-7),.UNSPECIFIED.);
#2072=B_SPLINE_CURVE_WITH_KNOTS('',3,(#88786,#88787,#88788,#88789,#88790,
#88791),.UNSPECIFIED.,.F.,.F.,(4,2,4),(0.,0.0198583386481131,0.0397175617395592),
 .UNSPECIFIED.);
#2073=B_SPLINE_CURVE_WITH_KNOTS('',3,(#88804,#88805,#88806,#88807,#88808,
#88809),.UNSPECIFIED.,.F.,.F.,(4,2,4),(0.,0.0198761966972832,0.0397532849531587),
 .UNSPECIFIED.);
#2074=B_SPLINE_CURVE_WITH_KNOTS('',3,(#88861,#88862,#88863,#88864,#88865,
#88866),.UNSPECIFIED.,.F.,.F.,(4,2,4),(0.,0.0199008240549723,0.0398025405821787),
 .UNSPECIFIED.);
#2075=B_SPLINE_CURVE_WITH_KNOTS('',3,(#88879,#88880,#88881,#88882,#88883,
#88884),.UNSPECIFIED.,.F.,.F.,(4,2,4),(0.,0.0199042047186047,0.0398092891806177),
 .UNSPECIFIED.);
#2076=B_SPLINE_CURVE_WITH_KNOTS('',3,(#88932,#88933,#88934,#88935,#88936,
#88937),.UNSPECIFIED.,.F.,.F.,(4,2,4),(0.,0.0198954793430153,0.039791861443219),
 .UNSPECIFIED.);
#2077=B_SPLINE_CURVE_WITH_KNOTS('',3,(#89017,#89018,#89019,#89020,#89021,
#89022),.UNSPECIFIED.,.F.,.F.,(4,2,4),(0.,0.0198973965846368,0.0397956842709046),
 .UNSPECIFIED.);
#2078=B_SPLINE_CURVE_WITH_KNOTS('',3,(#89041,#89042,#89043,#89044,#89045,
#89046),.UNSPECIFIED.,.F.,.F.,(4,2,4),(0.,0.01990306796779,0.0398070346084726),
 .UNSPECIFIED.);
#2079=B_SPLINE_CURVE_WITH_KNOTS('',3,(#89088,#89089,#89090,#89091,#89092,
#89093),.UNSPECIFIED.,.F.,.F.,(4,2,4),(0.,0.0198994178631783,0.0397997367937552),
 .UNSPECIFIED.);
#2080=B_SPLINE_CURVE_WITH_KNOTS('',3,(#89103,#89104,#89105,#89106,#89107,
#89108),.UNSPECIFIED.,.F.,.F.,(4,2,4),(0.,0.0198905179573968,0.0397819072752402),
 .UNSPECIFIED.);
#2081=B_SPLINE_CURVE_WITH_KNOTS('',3,(#89128,#89129,#89130,#89131,#89132,
#89133),.UNSPECIFIED.,.F.,.F.,(4,2,4),(0.0365944846647011,0.0384615384615384,
0.0431466153076599),.UNSPECIFIED.);
#2082=B_SPLINE_CURVE_WITH_KNOTS('',3,(#89134,#89135,#89136,#89137,#89138,
#89139,#89140),.UNSPECIFIED.,.F.,.F.,(4,3,4),(0.,0.00863415824051205,0.0172757293265222),
 .UNSPECIFIED.);
#2083=B_SPLINE_CURVE_WITH_KNOTS('',3,(#89165,#89166,#89167,#89168,#89169,
#89170),.UNSPECIFIED.,.F.,.F.,(4,2,4),(0.,0.0198536182040679,0.0397081492848769),
 .UNSPECIFIED.);
#2084=B_SPLINE_CURVE_WITH_KNOTS('',3,(#89183,#89184,#89185,#89186,#89187,
#89188),.UNSPECIFIED.,.F.,.F.,(4,2,4),(-0.00212389330288763,-0.00106194382034054,
0.),.UNSPECIFIED.);
#2085=B_SPLINE_CURVE_WITH_KNOTS('',3,(#89189,#89190,#89191,#89192,#89193,
#89194),.UNSPECIFIED.,.F.,.F.,(4,2,4),(9.99998421535138E-7,0.0193527854095481,
0.0387045795324334),.UNSPECIFIED.);
#2086=B_SPLINE_CURVE_WITH_KNOTS('',3,(#89210,#89211,#89212,#89213,#89214,
#89215,#89216),.UNSPECIFIED.,.F.,.F.,(4,3,4),(0.,0.5,0.999990115097979),
 .UNSPECIFIED.);
#2087=B_SPLINE_CURVE_WITH_KNOTS('',3,(#89236,#89237,#89238,#89239,#89240,
#89241),.UNSPECIFIED.,.F.,.F.,(4,2,4),(0.,0.0198677117286434,0.0397363336110727),
 .UNSPECIFIED.);
#2088=B_SPLINE_CURVE_WITH_KNOTS('',3,(#89247,#89248,#89249,#89250,#89251,
#89252),.UNSPECIFIED.,.F.,.F.,(4,2,4),(-0.00212486061334155,-0.00106293276465332,
-9.99999994678421E-7),.UNSPECIFIED.);
#2089=B_SPLINE_CURVE_WITH_KNOTS('',3,(#89291,#89292,#89293,#89294,#89295,
#89296),.UNSPECIFIED.,.F.,.F.,(4,2,4),(0.,0.0198583386511999,0.0397175617526615),
 .UNSPECIFIED.);
#2090=B_SPLINE_CURVE_WITH_KNOTS('',3,(#89309,#89310,#89311,#89312,#89313,
#89314),.UNSPECIFIED.,.F.,.F.,(4,2,4),(0.,0.0198761967019296,0.0397532849637006),
 .UNSPECIFIED.);
#2091=B_SPLINE_CURVE_WITH_KNOTS('',3,(#89366,#89367,#89368,#89369,#89370,
#89371),.UNSPECIFIED.,.F.,.F.,(4,2,4),(0.,0.0199008240588883,0.0398025405977883),
 .UNSPECIFIED.);
#2092=B_SPLINE_CURVE_WITH_KNOTS('',3,(#89384,#89385,#89386,#89387,#89388,
#89389),.UNSPECIFIED.,.F.,.F.,(4,2,4),(0.,0.0199042046965285,0.039809289131505),
 .UNSPECIFIED.);
#2093=B_SPLINE_CURVE_WITH_KNOTS('',3,(#89437,#89438,#89439,#89440,#89441,
#89442),.UNSPECIFIED.,.F.,.F.,(4,2,4),(0.,0.0198954793465745,0.0397918614572659),
 .UNSPECIFIED.);
#2094=B_SPLINE_CURVE_WITH_KNOTS('',3,(#89484,#89485,#89486,#89487,#89488,
#89489),.UNSPECIFIED.,.F.,.F.,(4,2,4),(-0.00212486106831169,-0.00106293275660098,
-9.99999994408878E-7),.UNSPECIFIED.);
#2095=B_SPLINE_CURVE_WITH_KNOTS('',3,(#89491,#89492,#89493,#89494,#89495,
#89496),.UNSPECIFIED.,.F.,.F.,(4,2,4),(-0.00212389479901396,-0.00106194442085412,
0.),.UNSPECIFIED.);
#2096=B_SPLINE_CURVE_WITH_KNOTS('',3,(#89541,#89542,#89543,#89544,#89545,
#89546),.UNSPECIFIED.,.F.,.F.,(4,2,4),(0.,0.0198994178670901,0.0397997368094576),
 .UNSPECIFIED.);
#2097=B_SPLINE_CURVE_WITH_KNOTS('',3,(#89563,#89564,#89565,#89566,#89567,
#89568),.UNSPECIFIED.,.F.,.F.,(4,2,4),(0.,0.0198905727281448,0.0397820346162575),
 .UNSPECIFIED.);
#2098=B_SPLINE_CURVE_WITH_KNOTS('',3,(#89592,#89593,#89594,#89595,#89596,
#89597,#89598),.UNSPECIFIED.,.F.,.F.,(4,3,4),(0.036594484664701,0.0384615384615384,
0.0431466153076596),.UNSPECIFIED.);
#2099=B_SPLINE_CURVE_WITH_KNOTS('',3,(#89599,#89600,#89601,#89602,#89603,
#89604,#89605,#89606),.UNSPECIFIED.,.F.,.F.,(4,2,2,4),(1.7725797502064E-6,
0.00863675584056385,0.0171399056837115,0.0172810927018386),
 .UNSPECIFIED.);
#2100=B_SPLINE_CURVE_WITH_KNOTS('',3,(#89631,#89632,#89633,#89634,#89635,
#89636),.UNSPECIFIED.,.F.,.F.,(4,2,4),(0.,0.0198536183073532,0.0397081495597498),
 .UNSPECIFIED.);
#2101=B_SPLINE_CURVE_WITH_KNOTS('',3,(#89652,#89653,#89654,#89655,#89656,
#89657),.UNSPECIFIED.,.F.,.F.,(4,2,4),(9.99998420096059E-7,0.0193522753886915,
0.0387045692994476),.UNSPECIFIED.);
#2102=B_SPLINE_CURVE_WITH_KNOTS('',3,(#89693,#89694,#89695,#89696,#89697,
#89698),.UNSPECIFIED.,.F.,.F.,(4,2,4),(0.,0.019858338655085,0.0397175617676976),
 .UNSPECIFIED.);
#2103=B_SPLINE_CURVE_WITH_KNOTS('',3,(#89718,#89719,#89720,#89721,#89722,
#89723),.UNSPECIFIED.,.F.,.F.,(4,2,4),(0.,0.0198762583335164,0.0397534249341096),
 .UNSPECIFIED.);
#2104=B_SPLINE_CURVE_WITH_KNOTS('',3,(#89739,#89740,#89741,#89742,#89743,
#89744,#89745),.UNSPECIFIED.,.F.,.F.,(4,3,4),(0.,0.5,0.999990115106081),
 .UNSPECIFIED.);
#2105=B_SPLINE_CURVE_WITH_KNOTS('',3,(#89765,#89766,#89767,#89768,#89769,
#89770),.UNSPECIFIED.,.F.,.F.,(4,2,4),(0.,0.0198677117239206,0.0397363335921476),
 .UNSPECIFIED.);
#2106=B_SPLINE_CURVE_WITH_KNOTS('',3,(#89812,#89813,#89814,#89815,#89816,
#89817),.UNSPECIFIED.,.F.,.F.,(4,2,4),(0.,0.0198973965928252,0.0397956843034983),
 .UNSPECIFIED.);
#2107=B_SPLINE_CURVE_WITH_KNOTS('',3,(#89836,#89837,#89838,#89839,#89840,
#89841),.UNSPECIFIED.,.F.,.F.,(4,2,4),(0.,0.0199030679705157,0.0398070346190355),
 .UNSPECIFIED.);
#2108=B_SPLINE_CURVE_WITH_KNOTS('',3,(#89893,#89894,#89895,#89896,#89897,
#89898),.UNSPECIFIED.,.F.,.F.,(4,2,4),(0.,0.0199008240622871,0.0398025406117409),
 .UNSPECIFIED.);
#2109=B_SPLINE_CURVE_WITH_KNOTS('',3,(#89911,#89912,#89913,#89914,#89915,
#89916),.UNSPECIFIED.,.F.,.F.,(4,2,4),(0.,0.0199042047128084,0.0398092891706494),
 .UNSPECIFIED.);
#2110=B_SPLINE_CURVE_WITH_KNOTS('',3,(#89964,#89965,#89966,#89967,#89968,
#89969),.UNSPECIFIED.,.F.,.F.,(4,2,4),(0.,0.0198954793500795,0.0397918614720059),
 .UNSPECIFIED.);
#2111=B_SPLINE_CURVE_WITH_KNOTS('',3,(#90029,#90030,#90031,#90032,#90033,
#90034),.UNSPECIFIED.,.F.,.F.,(4,2,4),(-0.00212486151725449,-0.00106293276451091,
-9.99999995882767E-7),.UNSPECIFIED.);
#2112=B_SPLINE_CURVE_WITH_KNOTS('',3,(#90036,#90037,#90038,#90039,#90040,
#90041),.UNSPECIFIED.,.F.,.F.,(4,2,4),(-0.00212389433155121,-0.00106194422672578,
0.),.UNSPECIFIED.);
#2113=B_SPLINE_CURVE_WITH_KNOTS('',3,(#90061,#90062,#90063,#90064,#90065,
#90066),.UNSPECIFIED.,.F.,.F.,(4,2,4),(0.0365944846647011,0.0384615384615384,
0.0431466153076599),.UNSPECIFIED.);
#2114=B_SPLINE_CURVE_WITH_KNOTS('',3,(#90067,#90068,#90069,#90070,#90071,
#90072,#90073),.UNSPECIFIED.,.F.,.F.,(4,3,4),(0.,0.00863415823997989,0.0172757326529418),
 .UNSPECIFIED.);
#2115=B_SPLINE_CURVE_WITH_KNOTS('',3,(#90098,#90099,#90100,#90101,#90102,
#90103),.UNSPECIFIED.,.F.,.F.,(4,2,4),(0.,0.0198541182711426,0.039708149503461),
 .UNSPECIFIED.);
#2116=B_SPLINE_CURVE_WITH_KNOTS('',3,(#90114,#90115,#90116,#90117,#90118,
#90119),.UNSPECIFIED.,.F.,.F.,(4,2,4),(9.9999842080534E-7,0.0193527904135635,
0.0387045796346496),.UNSPECIFIED.);
#2117=B_SPLINE_CURVE_WITH_KNOTS('',3,(#90161,#90162,#90163,#90164,#90165,
#90166),.UNSPECIFIED.,.F.,.F.,(4,2,4),(0.,0.0198583386593065,0.0397175617852667),
 .UNSPECIFIED.);
#2118=B_SPLINE_CURVE_WITH_KNOTS('',3,(#90176,#90177,#90178,#90179,#90180,
#90181),.UNSPECIFIED.,.F.,.F.,(4,2,4),(0.,0.0198761967046,0.0397532849569533),
 .UNSPECIFIED.);
#2119=B_SPLINE_CURVE_WITH_KNOTS('',3,(#90227,#90228,#90229,#90230,#90231,
#90232),.UNSPECIFIED.,.F.,.F.,(4,2,4),(0.,0.0199008240664257,0.0398025406285198),
 .UNSPECIFIED.);
#2120=B_SPLINE_CURVE_WITH_KNOTS('',3,(#90252,#90253,#90254,#90255,#90256,
#90257),.UNSPECIFIED.,.F.,.F.,(4,2,4),(0.,0.0199042621650074,0.0398094213886953),
 .UNSPECIFIED.);
#2121=B_SPLINE_CURVE_WITH_KNOTS('',3,(#90280,#90281,#90282,#90283,#90284,
#90285,#90286),.UNSPECIFIED.,.F.,.F.,(4,3,4),(0.,0.5,0.999990117119127),
 .UNSPECIFIED.);
#2122=B_SPLINE_CURVE_WITH_KNOTS('',3,(#90299,#90300,#90301,#90302,#90303,
#90304),.UNSPECIFIED.,.F.,.F.,(4,2,4),(0.,0.0198676496451984,0.0397361927455519),
 .UNSPECIFIED.);
#2123=B_SPLINE_CURVE_WITH_KNOTS('',3,(#90346,#90347,#90348,#90349,#90350,
#90351),.UNSPECIFIED.,.F.,.F.,(4,2,4),(0.,0.0198973965961517,0.0397956843169669),
 .UNSPECIFIED.);
#2124=B_SPLINE_CURVE_WITH_KNOTS('',3,(#90370,#90371,#90372,#90373,#90374,
#90375),.UNSPECIFIED.,.F.,.F.,(4,2,4),(0.,0.019903067966377,0.0398070346026983),
 .UNSPECIFIED.);
#2125=B_SPLINE_CURVE_WITH_KNOTS('',3,(#90417,#90418,#90419,#90420,#90421,
#90422),.UNSPECIFIED.,.F.,.F.,(4,2,4),(0.,0.0198994178758511,0.039799736844854),
 .UNSPECIFIED.);
#2126=B_SPLINE_CURVE_WITH_KNOTS('',3,(#90432,#90433,#90434,#90435,#90436,
#90437),.UNSPECIFIED.,.F.,.F.,(4,2,4),(0.,0.0198905179572641,0.0397819072592456),
 .UNSPECIFIED.);
#2127=B_SPLINE_CURVE_WITH_KNOTS('',3,(#90485,#90486,#90487,#90488,#90489,
#90490),.UNSPECIFIED.,.F.,.F.,(4,2,4),(0.,0.0198954793536976,0.0397918614864844),
 .UNSPECIFIED.);
#2128=B_SPLINE_CURVE_WITH_KNOTS('',3,(#90523,#90524,#90525,#90526,#90527,
#90528),.UNSPECIFIED.,.F.,.F.,(4,2,4),(-0.00212486217399669,-0.0010629327504893,
-9.99999997006E-7),.UNSPECIFIED.);
#2129=B_SPLINE_CURVE_WITH_KNOTS('',3,(#90530,#90531,#90532,#90533,#90534,
#90535),.UNSPECIFIED.,.F.,.F.,(4,2,4),(-0.00212389488246331,-0.00106194445546336,
0.),.UNSPECIFIED.);
#2130=B_SPLINE_CURVE_WITH_KNOTS('',3,(#90606,#90607,#90608,#90609,#90610,
#90611),.UNSPECIFIED.,.F.,.F.,(4,2,4),(0.,0.0198583386615053,0.0397175617941277),
 .UNSPECIFIED.);
#2131=B_SPLINE_CURVE_WITH_KNOTS('',3,(#90628,#90629,#90630,#90631,#90632,
#90633),.UNSPECIFIED.,.F.,.F.,(4,2,4),(0.,0.019876258198031,0.0397534246582595),
 .UNSPECIFIED.);
#2132=B_SPLINE_CURVE_WITH_KNOTS('',3,(#90674,#90675,#90676,#90677,#90678,
#90679),.UNSPECIFIED.,.F.,.F.,(4,2,4),(0.,0.0199013242067181,0.0398025408594927),
 .UNSPECIFIED.);
#2133=B_SPLINE_CURVE_WITH_KNOTS('',3,(#90689,#90690,#90691,#90692,#90693,
#90694),.UNSPECIFIED.,.F.,.F.,(4,2,4),(0.,0.019904704836476,0.0398092893406518),
 .UNSPECIFIED.);
#2134=B_SPLINE_CURVE_WITH_KNOTS('',3,(#90733,#90734,#90735,#90736,#90737,
#90738),.UNSPECIFIED.,.F.,.F.,(4,2,4),(0.,0.0198954793582144,0.0397918615045159),
 .UNSPECIFIED.);
#2135=B_SPLINE_CURVE_WITH_KNOTS('',3,(#90771,#90772,#90773,#90774,#90775,
#90776,#90777),.UNSPECIFIED.,.F.,.F.,(4,3,4),(0.,0.5,0.999990115106096),
 .UNSPECIFIED.);
#2136=B_SPLINE_CURVE_WITH_KNOTS('',3,(#90789,#90790,#90791,#90792,#90793,
#90794),.UNSPECIFIED.,.F.,.F.,(4,2,4),(0.,0.0198676494907608,0.0397361925123579),
 .UNSPECIFIED.);
#2137=B_SPLINE_CURVE_WITH_KNOTS('',3,(#90832,#90833,#90834,#90835,#90836,
#90837),.UNSPECIFIED.,.F.,.F.,(4,2,4),(0.,0.0198973965979104,0.0397956843240261),
 .UNSPECIFIED.);
#2138=B_SPLINE_CURVE_WITH_KNOTS('',3,(#90849,#90850,#90851,#90852,#90853,
#90854),.UNSPECIFIED.,.F.,.F.,(4,2,4),(0.,0.0199030098322562,0.0398069010987286),
 .UNSPECIFIED.);
#2139=B_SPLINE_CURVE_WITH_KNOTS('',3,(#90895,#90896,#90897,#90898,#90899,
#90900),.UNSPECIFIED.,.F.,.F.,(4,2,4),(0.,0.0198994178785925,0.0397997368562008),
 .UNSPECIFIED.);
#2140=B_SPLINE_CURVE_WITH_KNOTS('',3,(#90910,#90911,#90912,#90913,#90914,
#90915),.UNSPECIFIED.,.F.,.F.,(4,2,4),(0.,0.0198905179570912,0.0397819072622904),
 .UNSPECIFIED.);
#2141=B_SPLINE_CURVE_WITH_KNOTS('',3,(#90939,#90940,#90941,#90942,#90943,
#90944,#90945),.UNSPECIFIED.,.F.,.F.,(4,3,4),(0.0365944846647076,0.0384615384615384,
0.043146615307659),.UNSPECIFIED.);
#2142=B_SPLINE_CURVE_WITH_KNOTS('',3,(#90946,#90947,#90948,#90949,#90950,
#90951,#90952,#90953),.UNSPECIFIED.,.F.,.F.,(4,2,2,4),(1.77350714240743E-6,
0.00863675589070899,0.0171399223480672,0.0172811074735198),
 .UNSPECIFIED.);
#2143=B_SPLINE_CURVE_WITH_KNOTS('',3,(#90977,#90978,#90979,#90980,#90981,
#90982),.UNSPECIFIED.,.F.,.F.,(4,2,4),(0.,0.0198536183202665,0.0397081496113208),
 .UNSPECIFIED.);
#2144=B_SPLINE_CURVE_WITH_KNOTS('',3,(#90998,#90999,#91000,#91001,#91002,
#91003),.UNSPECIFIED.,.F.,.F.,(4,2,4),(9.99998420192272E-7,0.0193527896174958,
0.0387045796181448),.UNSPECIFIED.);
#2145=B_SPLINE_CURVE_WITH_KNOTS('',3,(#91233,#91234,#91235,#91236),
 .UNSPECIFIED.,.F.,.F.,(4,4),(3.44076343139105E-7,9.58822346085573E-5),
 .UNSPECIFIED.);
#2146=B_SPLINE_CURVE_WITH_KNOTS('',3,(#91329,#91330,#91331,#91332),
 .UNSPECIFIED.,.F.,.F.,(4,4),(3.44076343937661E-7,9.58822346085479E-5),
 .UNSPECIFIED.);
#2147=B_SPLINE_CURVE_WITH_KNOTS('',3,(#91633,#91634,#91635,#91636),
 .UNSPECIFIED.,.F.,.F.,(4,4),(3.44076344756528E-7,9.58822346085586E-5),
 .UNSPECIFIED.);
#2148=B_SPLINE_CURVE_WITH_KNOTS('',3,(#91937,#91938,#91939,#91940),
 .UNSPECIFIED.,.F.,.F.,(4,4),(3.44076345613438E-7,9.5882234608549E-5),
 .UNSPECIFIED.);
#2149=B_SPLINE_CURVE_WITH_KNOTS('',3,(#92241,#92242,#92243,#92244),
 .UNSPECIFIED.,.F.,.F.,(4,4),(3.44076346610602E-7,9.5882234608586E-5),
 .UNSPECIFIED.);
#2150=B_SPLINE_CURVE_WITH_KNOTS('',3,(#92545,#92546,#92547,#92548),
 .UNSPECIFIED.,.F.,.F.,(4,4),(3.44076347442387E-7,9.58822346085427E-5),
 .UNSPECIFIED.);
#2151=B_SPLINE_CURVE_WITH_KNOTS('',3,(#92849,#92850,#92851,#92852),
 .UNSPECIFIED.,.F.,.F.,(4,4),(3.4407634849255E-7,9.58822346085551E-5),
 .UNSPECIFIED.);
#2152=B_SPLINE_CURVE_WITH_KNOTS('',3,(#93153,#93154,#93155,#93156),
 .UNSPECIFIED.,.F.,.F.,(4,4),(3.44076349385464E-7,9.58822346085304E-5),
 .UNSPECIFIED.);
#2153=B_SPLINE_CURVE_WITH_KNOTS('',3,(#93457,#93458,#93459,#93460),
 .UNSPECIFIED.,.F.,.F.,(4,4),(3.44076350325311E-7,9.5882234608509E-5),
 .UNSPECIFIED.);
#2154=B_SPLINE_CURVE_WITH_KNOTS('',3,(#93761,#93762,#93763,#93764),
 .UNSPECIFIED.,.F.,.F.,(4,4),(3.44076351419414E-7,9.58822346086072E-5),
 .UNSPECIFIED.);
#2155=B_SPLINE_CURVE_WITH_KNOTS('',3,(#94065,#94066,#94067,#94068),
 .UNSPECIFIED.,.F.,.F.,(4,4),(3.44076352242797E-7,9.58822346085252E-5),
 .UNSPECIFIED.);
#2156=B_SPLINE_CURVE_WITH_KNOTS('',3,(#94369,#94370,#94371,#94372),
 .UNSPECIFIED.,.F.,.F.,(4,4),(3.44076353092136E-7,9.58822346085853E-5),
 .UNSPECIFIED.);
#2157=B_SPLINE_CURVE_WITH_KNOTS('',3,(#94673,#94674,#94675,#94676),
 .UNSPECIFIED.,.F.,.F.,(4,4),(3.44076353913147E-7,9.58822346085855E-5),
 .UNSPECIFIED.);
#2158=B_SPLINE_CURVE_WITH_KNOTS('',3,(#94977,#94978,#94979,#94980),
 .UNSPECIFIED.,.F.,.F.,(4,4),(3.44076354603741E-7,9.58822346086191E-5),
 .UNSPECIFIED.);
#2159=B_SPLINE_CURVE_WITH_KNOTS('',3,(#95281,#95282,#95283,#95284),
 .UNSPECIFIED.,.F.,.F.,(4,4),(3.440763552087E-7,9.58822346085434E-5),
 .UNSPECIFIED.);
#2160=B_SPLINE_CURVE_WITH_KNOTS('',3,(#95585,#95586,#95587,#95588),
 .UNSPECIFIED.,.F.,.F.,(4,4),(3.44076355662546E-7,9.5882234608571E-5),
 .UNSPECIFIED.);
#2161=B_SPLINE_CURVE_WITH_KNOTS('',3,(#95889,#95890,#95891,#95892),
 .UNSPECIFIED.,.F.,.F.,(4,4),(3.44076356005326E-7,9.58822346085531E-5),
 .UNSPECIFIED.);
#2162=B_SPLINE_CURVE_WITH_KNOTS('',3,(#96193,#96194,#96195,#96196),
 .UNSPECIFIED.,.F.,.F.,(4,4),(3.44076356300518E-7,9.58822346085333E-5),
 .UNSPECIFIED.);
#2163=B_SPLINE_CURVE_WITH_KNOTS('',3,(#96497,#96498,#96499,#96500),
 .UNSPECIFIED.,.F.,.F.,(4,4),(3.44076356438746E-7,9.58822346085612E-5),
 .UNSPECIFIED.);
#2164=B_SPLINE_CURVE_WITH_KNOTS('',3,(#96801,#96802,#96803,#96804),
 .UNSPECIFIED.,.F.,.F.,(4,4),(3.44076356391263E-7,9.58822346085676E-5),
 .UNSPECIFIED.);
#2165=B_SPLINE_CURVE_WITH_KNOTS('',3,(#97105,#97106,#97107,#97108),
 .UNSPECIFIED.,.F.,.F.,(4,4),(3.44076356413286E-7,9.58822346085746E-5),
 .UNSPECIFIED.);
#2166=B_SPLINE_CURVE_WITH_KNOTS('',3,(#97409,#97410,#97411,#97412),
 .UNSPECIFIED.,.F.,.F.,(4,4),(3.44076356099639E-7,9.58822346086219E-5),
 .UNSPECIFIED.);
#2167=B_SPLINE_CURVE_WITH_KNOTS('',3,(#97713,#97714,#97715,#97716),
 .UNSPECIFIED.,.F.,.F.,(4,4),(3.44076355765E-7,9.58822346085517E-5),
 .UNSPECIFIED.);
#2168=B_SPLINE_CURVE_WITH_KNOTS('',3,(#98017,#98018,#98019,#98020),
 .UNSPECIFIED.,.F.,.F.,(4,4),(3.44076355331457E-7,9.58822346085816E-5),
 .UNSPECIFIED.);
#2169=B_SPLINE_CURVE_WITH_KNOTS('',3,(#98321,#98322,#98323,#98324),
 .UNSPECIFIED.,.F.,.F.,(4,4),(3.44076354721354E-7,9.58822346085665E-5),
 .UNSPECIFIED.);
#2170=B_SPLINE_CURVE_WITH_KNOTS('',3,(#98625,#98626,#98627,#98628),
 .UNSPECIFIED.,.F.,.F.,(4,4),(3.44076354108817E-7,9.5882234608515E-5),
 .UNSPECIFIED.);
#2171=B_SPLINE_CURVE_WITH_KNOTS('',3,(#98929,#98930,#98931,#98932),
 .UNSPECIFIED.,.F.,.F.,(4,4),(3.44076353460809E-7,9.58822346085927E-5),
 .UNSPECIFIED.);
#2172=B_SPLINE_CURVE_WITH_KNOTS('',3,(#99233,#99234,#99235,#99236),
 .UNSPECIFIED.,.F.,.F.,(4,4),(3.44076352635546E-7,9.58822346085778E-5),
 .UNSPECIFIED.);
#2173=B_SPLINE_CURVE_WITH_KNOTS('',3,(#99537,#99538,#99539,#99540),
 .UNSPECIFIED.,.F.,.F.,(4,4),(3.44076351743482E-7,9.58822346085721E-5),
 .UNSPECIFIED.);
#2174=B_SPLINE_CURVE_WITH_KNOTS('',3,(#99841,#99842,#99843,#99844),
 .UNSPECIFIED.,.F.,.F.,(4,4),(3.44076350748374E-7,9.58822346085306E-5),
 .UNSPECIFIED.);
#2175=B_SPLINE_CURVE_WITH_KNOTS('',3,(#100145,#100146,#100147,#100148),
 .UNSPECIFIED.,.F.,.F.,(4,4),(3.44076349811527E-7,9.58822346085378E-5),
 .UNSPECIFIED.);
#2176=B_SPLINE_CURVE_WITH_KNOTS('',3,(#100449,#100450,#100451,#100452),
 .UNSPECIFIED.,.F.,.F.,(4,4),(3.44076348755265E-7,9.58822346085592E-5),
 .UNSPECIFIED.);
#2177=B_SPLINE_CURVE_WITH_KNOTS('',3,(#100753,#100754,#100755,#100756),
 .UNSPECIFIED.,.F.,.F.,(4,4),(3.44076347719767E-7,9.58822346085908E-5),
 .UNSPECIFIED.);
#2178=B_SPLINE_CURVE_WITH_KNOTS('',3,(#101057,#101058,#101059,#101060),
 .UNSPECIFIED.,.F.,.F.,(4,4),(3.44076346912447E-7,9.588223460854E-5),
 .UNSPECIFIED.);
#2179=B_SPLINE_CURVE_WITH_KNOTS('',3,(#101361,#101362,#101363,#101364),
 .UNSPECIFIED.,.F.,.F.,(4,4),(3.44076345873186E-7,9.58822346084459E-5),
 .UNSPECIFIED.);
#2180=B_SPLINE_CURVE_WITH_KNOTS('',3,(#101665,#101666,#101667,#101668),
 .UNSPECIFIED.,.F.,.F.,(4,4),(3.44076345035861E-7,9.58822346085724E-5),
 .UNSPECIFIED.);
#2181=B_SPLINE_CURVE_WITH_KNOTS('',3,(#101969,#101970,#101971,#101972),
 .UNSPECIFIED.,.F.,.F.,(4,4),(3.4407634418853E-7,9.58822346084491E-5),
 .UNSPECIFIED.);
#2182=B_SPLINE_CURVE_WITH_KNOTS('',3,(#102273,#102274,#102275,#102276),
 .UNSPECIFIED.,.F.,.F.,(4,4),(3.44076343458719E-7,9.58822346085829E-5),
 .UNSPECIFIED.);
#2183=B_SPLINE_CURVE_WITH_KNOTS('',3,(#102577,#102578,#102579,#102580),
 .UNSPECIFIED.,.F.,.F.,(4,4),(3.4407634265707E-7,9.58822346085594E-5),
 .UNSPECIFIED.);
#2184=B_SPLINE_CURVE_WITH_KNOTS('',3,(#102881,#102882,#102883,#102884),
 .UNSPECIFIED.,.F.,.F.,(4,4),(3.44076342139102E-7,9.5882234608581E-5),
 .UNSPECIFIED.);
#2185=B_SPLINE_CURVE_WITH_KNOTS('',3,(#103185,#103186,#103187,#103188),
 .UNSPECIFIED.,.F.,.F.,(4,4),(3.44076341609194E-7,9.58822346085673E-5),
 .UNSPECIFIED.);
#2186=B_SPLINE_CURVE_WITH_KNOTS('',3,(#103489,#103490,#103491,#103492),
 .UNSPECIFIED.,.F.,.F.,(4,4),(3.44076341299288E-7,9.58822346085517E-5),
 .UNSPECIFIED.);
#2187=B_SPLINE_CURVE_WITH_KNOTS('',3,(#103793,#103794,#103795,#103796),
 .UNSPECIFIED.,.F.,.F.,(4,4),(3.44076341018736E-7,9.5882234608553E-5),
 .UNSPECIFIED.);
#2188=B_SPLINE_CURVE_WITH_KNOTS('',3,(#104137,#104138,#104139,#104140),
 .UNSPECIFIED.,.F.,.F.,(4,4),(3.44076340792074E-7,9.58822346085118E-5),
 .UNSPECIFIED.);
#2189=B_SPLINE_CURVE_WITH_KNOTS('',3,(#104401,#104402,#104403,#104404),
 .UNSPECIFIED.,.F.,.F.,(4,4),(3.44076340724659E-7,9.58822346085855E-5),
 .UNSPECIFIED.);
#2190=B_SPLINE_CURVE_WITH_KNOTS('',3,(#104705,#104706,#104707,#104708),
 .UNSPECIFIED.,.F.,.F.,(4,4),(3.44076340891315E-7,9.58822346085796E-5),
 .UNSPECIFIED.);
#2191=B_SPLINE_CURVE_WITH_KNOTS('',3,(#105009,#105010,#105011,#105012),
 .UNSPECIFIED.,.F.,.F.,(4,4),(3.4407634120523E-7,9.5882234608577E-5),
 .UNSPECIFIED.);
#2192=B_SPLINE_CURVE_WITH_KNOTS('',3,(#105313,#105314,#105315,#105316),
 .UNSPECIFIED.,.F.,.F.,(4,4),(3.44076341566053E-7,9.5882234608583E-5),
 .UNSPECIFIED.);
#2193=B_SPLINE_CURVE_WITH_KNOTS('',3,(#105617,#105618,#105619,#105620),
 .UNSPECIFIED.,.F.,.F.,(4,4),(3.44076341947078E-7,9.58822346086343E-5),
 .UNSPECIFIED.);
#2194=B_SPLINE_CURVE_WITH_KNOTS('',3,(#105921,#105922,#105923,#105924),
 .UNSPECIFIED.,.F.,.F.,(4,4),(3.44076342475543E-7,9.58822346086365E-5),
 .UNSPECIFIED.);
#2195=B_SPLINE_CURVE_WITH_KNOTS('',3,(#107237,#107238,#107239,#107240,#107241,
#107242,#107243,#107244,#107245,#107246,#107247,#107248,#107249,#107250,
#107251,#107252,#107253,#107254,#107255,#107256,#107257,#107258,#107259,
#107260,#107261,#107262,#107263,#107264,#107265,#107266,#107267,#107268,
#107269,#107270,#107271,#107272,#107273,#107274,#107275,#107276,#107277,
#107278),.UNSPECIFIED.,.T.,.F.,(4,2,2,2,2,2,2,2,2,2,2,2,2,2,2,2,2,2,2,2,
4),(0.,0.0683756752227249,0.13675135044545,0.193430456509981,0.239974549812452,
0.286518643114923,0.333062736417395,0.379606829719866,0.436285935784398,
0.504661611007122,0.573037286229846,0.641412961452571,0.709788636675295,
0.766467742739827,0.813011836042298,0.859555929344769,0.906100022647241,
0.952644115949712,1.00932322201424,1.07769889723697,1.14607457245969),
 .UNSPECIFIED.);
#2196=B_SPLINE_CURVE_WITH_KNOTS('',3,(#107310,#107311,#107312,#107313,#107314,
#107315,#107316,#107317),.UNSPECIFIED.,.F.,.F.,(4,2,2,4),(3.52079202383874,
3.52667424117723,4.17784077952384,4.18520413953086),.UNSPECIFIED.);
#2197=B_SPLINE_CURVE_WITH_KNOTS('',3,(#107322,#107323,#107324,#107325,#107326,
#107327,#107328,#107329),.UNSPECIFIED.,.F.,.F.,(4,2,2,4),(1.56581126613039,
1.57317462613742,2.22434116448402,2.23022338182252),.UNSPECIFIED.);
#2198=B_SPLINE_SURFACE_WITH_KNOTS('',3,3,((#61813,#61814,#61815,#61816,
#61817,#61818,#61819,#61820,#61821,#61822,#61823,#61824,#61825,#61826,#61827,
#61828,#61829,#61830,#61831,#61832,#61833,#61834,#61835,#61836,#61837,#61838,
#61839,#61840,#61841,#61842,#61843,#61844,#61845,#61846,#61847,#61848,#61849,
#61850,#61851,#61852,#61853,#61854,#61855,#61856,#61857,#61858,#61859,#61860,
#61861,#61862,#61863,#61864,#61865,#61866,#61867,#61868,#61869,#61870,#61871,
#61872,#61873,#61874,#61875,#61876,#61877,#61878,#61879,#61880,#61881,#61882,
#61883,#61884,#61885,#61886,#61887,#61888,#61889,#61890,#61891,#61892,#61893,
#61894,#61895,#61896,#61897,#61898,#61899,#61900,#61901,#61902,#61903,#61904,
#61905,#61906,#61907,#61908,#61909,#61910,#61911,#61912,#61913,#61914,#61915,
#61916,#61917,#61918,#61919,#61920,#61921,#61922,#61923,#61924,#61925,#61926,
#61927,#61928,#61929,#61930,#61931,#61932,#61933,#61934,#61935,#61936,#61937,
#61938),(#61939,#61940,#61941,#61942,#61943,#61944,#61945,#61946,#61947,
#61948,#61949,#61950,#61951,#61952,#61953,#61954,#61955,#61956,#61957,#61958,
#61959,#61960,#61961,#61962,#61963,#61964,#61965,#61966,#61967,#61968,#61969,
#61970,#61971,#61972,#61973,#61974,#61975,#61976,#61977,#61978,#61979,#61980,
#61981,#61982,#61983,#61984,#61985,#61986,#61987,#61988,#61989,#61990,#61991,
#61992,#61993,#61994,#61995,#61996,#61997,#61998,#61999,#62000,#62001,#62002,
#62003,#62004,#62005,#62006,#62007,#62008,#62009,#62010,#62011,#62012,#62013,
#62014,#62015,#62016,#62017,#62018,#62019,#62020,#62021,#62022,#62023,#62024,
#62025,#62026,#62027,#62028,#62029,#62030,#62031,#62032,#62033,#62034,#62035,
#62036,#62037,#62038,#62039,#62040,#62041,#62042,#62043,#62044,#62045,#62046,
#62047,#62048,#62049,#62050,#62051,#62052,#62053,#62054,#62055,#62056,#62057,
#62058,#62059,#62060,#62061,#62062,#62063,#62064),(#62065,#62066,#62067,
#62068,#62069,#62070,#62071,#62072,#62073,#62074,#62075,#62076,#62077,#62078,
#62079,#62080,#62081,#62082,#62083,#62084,#62085,#62086,#62087,#62088,#62089,
#62090,#62091,#62092,#62093,#62094,#62095,#62096,#62097,#62098,#62099,#62100,
#62101,#62102,#62103,#62104,#62105,#62106,#62107,#62108,#62109,#62110,#62111,
#62112,#62113,#62114,#62115,#62116,#62117,#62118,#62119,#62120,#62121,#62122,
#62123,#62124,#62125,#62126,#62127,#62128,#62129,#62130,#62131,#62132,#62133,
#62134,#62135,#62136,#62137,#62138,#62139,#62140,#62141,#62142,#62143,#62144,
#62145,#62146,#62147,#62148,#62149,#62150,#62151,#62152,#62153,#62154,#62155,
#62156,#62157,#62158,#62159,#62160,#62161,#62162,#62163,#62164,#62165,#62166,
#62167,#62168,#62169,#62170,#62171,#62172,#62173,#62174,#62175,#62176,#62177,
#62178,#62179,#62180,#62181,#62182,#62183,#62184,#62185,#62186,#62187,#62188,
#62189,#62190),(#62191,#62192,#62193,#62194,#62195,#62196,#62197,#62198,
#62199,#62200,#62201,#62202,#62203,#62204,#62205,#62206,#62207,#62208,#62209,
#62210,#62211,#62212,#62213,#62214,#62215,#62216,#62217,#62218,#62219,#62220,
#62221,#62222,#62223,#62224,#62225,#62226,#62227,#62228,#62229,#62230,#62231,
#62232,#62233,#62234,#62235,#62236,#62237,#62238,#62239,#62240,#62241,#62242,
#62243,#62244,#62245,#62246,#62247,#62248,#62249,#62250,#62251,#62252,#62253,
#62254,#62255,#62256,#62257,#62258,#62259,#62260,#62261,#62262,#62263,#62264,
#62265,#62266,#62267,#62268,#62269,#62270,#62271,#62272,#62273,#62274,#62275,
#62276,#62277,#62278,#62279,#62280,#62281,#62282,#62283,#62284,#62285,#62286,
#62287,#62288,#62289,#62290,#62291,#62292,#62293,#62294,#62295,#62296,#62297,
#62298,#62299,#62300,#62301,#62302,#62303,#62304,#62305,#62306,#62307,#62308,
#62309,#62310,#62311,#62312,#62313,#62314,#62315,#62316),(#62317,#62318,
#62319,#62320,#62321,#62322,#62323,#62324,#62325,#62326,#62327,#62328,#62329,
#62330,#62331,#62332,#62333,#62334,#62335,#62336,#62337,#62338,#62339,#62340,
#62341,#62342,#62343,#62344,#62345,#62346,#62347,#62348,#62349,#62350,#62351,
#62352,#62353,#62354,#62355,#62356,#62357,#62358,#62359,#62360,#62361,#62362,
#62363,#62364,#62365,#62366,#62367,#62368,#62369,#62370,#62371,#62372,#62373,
#62374,#62375,#62376,#62377,#62378,#62379,#62380,#62381,#62382,#62383,#62384,
#62385,#62386,#62387,#62388,#62389,#62390,#62391,#62392,#62393,#62394,#62395,
#62396,#62397,#62398,#62399,#62400,#62401,#62402,#62403,#62404,#62405,#62406,
#62407,#62408,#62409,#62410,#62411,#62412,#62413,#62414,#62415,#62416,#62417,
#62418,#62419,#62420,#62421,#62422,#62423,#62424,#62425,#62426,#62427,#62428,
#62429,#62430,#62431,#62432,#62433,#62434,#62435,#62436,#62437,#62438,#62439,
#62440,#62441,#62442),(#62443,#62444,#62445,#62446,#62447,#62448,#62449,
#62450,#62451,#62452,#62453,#62454,#62455,#62456,#62457,#62458,#62459,#62460,
#62461,#62462,#62463,#62464,#62465,#62466,#62467,#62468,#62469,#62470,#62471,
#62472,#62473,#62474,#62475,#62476,#62477,#62478,#62479,#62480,#62481,#62482,
#62483,#62484,#62485,#62486,#62487,#62488,#62489,#62490,#62491,#62492,#62493,
#62494,#62495,#62496,#62497,#62498,#62499,#62500,#62501,#62502,#62503,#62504,
#62505,#62506,#62507,#62508,#62509,#62510,#62511,#62512,#62513,#62514,#62515,
#62516,#62517,#62518,#62519,#62520,#62521,#62522,#62523,#62524,#62525,#62526,
#62527,#62528,#62529,#62530,#62531,#62532,#62533,#62534,#62535,#62536,#62537,
#62538,#62539,#62540,#62541,#62542,#62543,#62544,#62545,#62546,#62547,#62548,
#62549,#62550,#62551,#62552,#62553,#62554,#62555,#62556,#62557,#62558,#62559,
#62560,#62561,#62562,#62563,#62564,#62565,#62566,#62567,#62568),(#62569,
#62570,#62571,#62572,#62573,#62574,#62575,#62576,#62577,#62578,#62579,#62580,
#62581,#62582,#62583,#62584,#62585,#62586,#62587,#62588,#62589,#62590,#62591,
#62592,#62593,#62594,#62595,#62596,#62597,#62598,#62599,#62600,#62601,#62602,
#62603,#62604,#62605,#62606,#62607,#62608,#62609,#62610,#62611,#62612,#62613,
#62614,#62615,#62616,#62617,#62618,#62619,#62620,#62621,#62622,#62623,#62624,
#62625,#62626,#62627,#62628,#62629,#62630,#62631,#62632,#62633,#62634,#62635,
#62636,#62637,#62638,#62639,#62640,#62641,#62642,#62643,#62644,#62645,#62646,
#62647,#62648,#62649,#62650,#62651,#62652,#62653,#62654,#62655,#62656,#62657,
#62658,#62659,#62660,#62661,#62662,#62663,#62664,#62665,#62666,#62667,#62668,
#62669,#62670,#62671,#62672,#62673,#62674,#62675,#62676,#62677,#62678,#62679,
#62680,#62681,#62682,#62683,#62684,#62685,#62686,#62687,#62688,#62689,#62690,
#62691,#62692,#62693,#62694),(#62695,#62696,#62697,#62698,#62699,#62700,
#62701,#62702,#62703,#62704,#62705,#62706,#62707,#62708,#62709,#62710,#62711,
#62712,#62713,#62714,#62715,#62716,#62717,#62718,#62719,#62720,#62721,#62722,
#62723,#62724,#62725,#62726,#62727,#62728,#62729,#62730,#62731,#62732,#62733,
#62734,#62735,#62736,#62737,#62738,#62739,#62740,#62741,#62742,#62743,#62744,
#62745,#62746,#62747,#62748,#62749,#62750,#62751,#62752,#62753,#62754,#62755,
#62756,#62757,#62758,#62759,#62760,#62761,#62762,#62763,#62764,#62765,#62766,
#62767,#62768,#62769,#62770,#62771,#62772,#62773,#62774,#62775,#62776,#62777,
#62778,#62779,#62780,#62781,#62782,#62783,#62784,#62785,#62786,#62787,#62788,
#62789,#62790,#62791,#62792,#62793,#62794,#62795,#62796,#62797,#62798,#62799,
#62800,#62801,#62802,#62803,#62804,#62805,#62806,#62807,#62808,#62809,#62810,
#62811,#62812,#62813,#62814,#62815,#62816,#62817,#62818,#62819,#62820),
(#62821,#62822,#62823,#62824,#62825,#62826,#62827,#62828,#62829,#62830,
#62831,#62832,#62833,#62834,#62835,#62836,#62837,#62838,#62839,#62840,#62841,
#62842,#62843,#62844,#62845,#62846,#62847,#62848,#62849,#62850,#62851,#62852,
#62853,#62854,#62855,#62856,#62857,#62858,#62859,#62860,#62861,#62862,#62863,
#62864,#62865,#62866,#62867,#62868,#62869,#62870,#62871,#62872,#62873,#62874,
#62875,#62876,#62877,#62878,#62879,#62880,#62881,#62882,#62883,#62884,#62885,
#62886,#62887,#62888,#62889,#62890,#62891,#62892,#62893,#62894,#62895,#62896,
#62897,#62898,#62899,#62900,#62901,#62902,#62903,#62904,#62905,#62906,#62907,
#62908,#62909,#62910,#62911,#62912,#62913,#62914,#62915,#62916,#62917,#62918,
#62919,#62920,#62921,#62922,#62923,#62924,#62925,#62926,#62927,#62928,#62929,
#62930,#62931,#62932,#62933,#62934,#62935,#62936,#62937,#62938,#62939,#62940,
#62941,#62942,#62943,#62944,#62945,#62946),(#62947,#62948,#62949,#62950,
#62951,#62952,#62953,#62954,#62955,#62956,#62957,#62958,#62959,#62960,#62961,
#62962,#62963,#62964,#62965,#62966,#62967,#62968,#62969,#62970,#62971,#62972,
#62973,#62974,#62975,#62976,#62977,#62978,#62979,#62980,#62981,#62982,#62983,
#62984,#62985,#62986,#62987,#62988,#62989,#62990,#62991,#62992,#62993,#62994,
#62995,#62996,#62997,#62998,#62999,#63000,#63001,#63002,#63003,#63004,#63005,
#63006,#63007,#63008,#63009,#63010,#63011,#63012,#63013,#63014,#63015,#63016,
#63017,#63018,#63019,#63020,#63021,#63022,#63023,#63024,#63025,#63026,#63027,
#63028,#63029,#63030,#63031,#63032,#63033,#63034,#63035,#63036,#63037,#63038,
#63039,#63040,#63041,#63042,#63043,#63044,#63045,#63046,#63047,#63048,#63049,
#63050,#63051,#63052,#63053,#63054,#63055,#63056,#63057,#63058,#63059,#63060,
#63061,#63062,#63063,#63064,#63065,#63066,#63067,#63068,#63069,#63070,#63071,
#63072)),.UNSPECIFIED.,.T.,.F.,.F.,(4,2,2,2,4),(4,2,2,2,2,2,2,2,2,2,2,2,
2,2,2,2,2,2,2,2,2,2,2,2,2,2,2,2,2,2,2,2,2,2,2,2,2,2,2,2,2,2,2,2,2,2,2,2,
2,2,2,2,2,2,2,2,2,2,2,2,2,2,4),(0.,0.25,0.5,0.75,1.),(0.0266743037386738,
0.03125,0.046875,0.0625,0.078125,0.09375,0.109375,0.125,0.140625,0.15625,
0.171875,0.1875,0.203125,0.21875,0.234375,0.25,0.265625,0.28125,0.296875,
0.3125,0.328125,0.34375,0.359375,0.375,0.390625,0.40625,0.421875,0.4375,
0.453125,0.46875,0.484375,0.5,0.526193937224651,0.552387874449302,0.578581811673953,
0.604775748898604,0.630969686123255,0.657163623347906,0.670260591960231,
0.683357560572557,0.696454529184882,0.709551497797208,0.722648466409533,
0.735745435021858,0.748842403634184,0.761939372246509,0.775036340858835,
0.78813330947116,0.801230278083486,0.814327246695811,0.827424215308137,
0.840521183920462,0.853618152532788,0.866715121145113,0.879812089757439,
0.892909058369764,0.90600602698209,0.919102995594415,0.929215121145113,
0.939327246695811,0.949439372246509,0.959551497797208,0.967322126402602),
 .UNSPECIFIED.);
#2199=B_SPLINE_SURFACE_WITH_KNOTS('',3,3,((#65202,#65203,#65204,#65205),
(#65206,#65207,#65208,#65209),(#65210,#65211,#65212,#65213),(#65214,#65215,
#65216,#65217)),.UNSPECIFIED.,.F.,.F.,.F.,(4,4),(4,4),(-0.000171895435141639,
1.00600020634823),(0.0665898698856052,0.0751325481130375),.UNSPECIFIED.);
#2200=B_SPLINE_SURFACE_WITH_KNOTS('',3,3,((#65233,#65234,#65235,#65236),
(#65237,#65238,#65239,#65240),(#65241,#65242,#65243,#65244),(#65245,#65246,
#65247,#65248)),.UNSPECIFIED.,.F.,.F.,.F.,(4,4),(4,4),(-0.00286833998603604,
0.477902879809884),(0.0665898698862512,0.0731716198748498),
 .UNSPECIFIED.);
#2201=B_SPLINE_SURFACE_WITH_KNOTS('',3,3,((#65300,#65301,#65302,#65303),
(#65304,#65305,#65306,#65307),(#65308,#65309,#65310,#65311),(#65312,#65313,
#65314,#65315)),.UNSPECIFIED.,.F.,.F.,.F.,(4,4),(4,4),(-0.00286764392048215,
0.477902879806999),(0.0565997133101203,0.0631721430887071),
 .UNSPECIFIED.);
#2202=B_SPLINE_SURFACE_WITH_KNOTS('',3,3,((#65326,#65327,#65328,#65329),
(#65330,#65331,#65332,#65333),(#65334,#65335,#65336,#65337),(#65338,#65339,
#65340,#65341)),.UNSPECIFIED.,.F.,.F.,.F.,(4,4),(4,4),(-0.00286833998604881,
0.477902879811004),(0.0665898698862518,0.0731716198748491),
 .UNSPECIFIED.);
#2203=B_SPLINE_SURFACE_WITH_KNOTS('',3,3,((#65358,#65359,#65360,#65361),
(#65362,#65363,#65364,#65365),(#65366,#65367,#65368,#65369),(#65370,#65371,
#65372,#65373)),.UNSPECIFIED.,.F.,.F.,.F.,(4,4),(4,4),(0.522097120207134,
1.00286791825535),(0.0600156865486949,0.0665898700060146),.UNSPECIFIED.);
#2204=B_SPLINE_SURFACE_WITH_KNOTS('',3,3,((#65436,#65437,#65438,#65439),
(#65440,#65441,#65442,#65443),(#65444,#65445,#65446,#65447),(#65448,#65449,
#65450,#65451)),.UNSPECIFIED.,.F.,.F.,.F.,(4,4),(4,4),(0.52209712020793,
1.00286780122186),(0.050026355085867,0.056599713310142),.UNSPECIFIED.);
#2205=B_SPLINE_SURFACE_WITH_KNOTS('',3,3,((#65459,#65460,#65461,#65462),
(#65463,#65464,#65465,#65466),(#65467,#65468,#65469,#65470),(#65471,#65472,
#65473,#65474)),.UNSPECIFIED.,.F.,.F.,.F.,(4,4),(4,4),(0.522097120207881,
1.0028679182553),(0.0600156865486941,0.0665898700060137),.UNSPECIFIED.);
#2206=B_SPLINE_SURFACE_WITH_KNOTS('',3,3,((#65589,#65590,#65591,#65592),
(#65593,#65594,#65595,#65596),(#65597,#65598,#65599,#65600),(#65601,#65602,
#65603,#65604)),.UNSPECIFIED.,.F.,.F.,.F.,(4,4),(4,4),(0.522097120205934,
1.00286848452567),(0.0400218729465712,0.0466073985929453),.UNSPECIFIED.);
#2207=B_SPLINE_SURFACE_WITH_KNOTS('',3,3,((#65612,#65613,#65614,#65615),
(#65616,#65617,#65618,#65619),(#65620,#65621,#65622,#65623),(#65624,#65625,
#65626,#65627)),.UNSPECIFIED.,.F.,.F.,.F.,(4,4),(4,4),(0.522097120207841,
1.0028678012217),(0.0500263550858681,0.0565997133101407),.UNSPECIFIED.);
#2208=B_SPLINE_SURFACE_WITH_KNOTS('',3,3,((#65758,#65759,#65760,#65761),
(#65762,#65763,#65764,#65765),(#65766,#65767,#65768,#65769),(#65770,#65771,
#65772,#65773)),.UNSPECIFIED.,.F.,.F.,.F.,(4,4),(4,4),(0.52209712020777,
1.0028686220115),(0.0300094532292152,0.0365944846647039),.UNSPECIFIED.);
#2209=B_SPLINE_SURFACE_WITH_KNOTS('',3,3,((#65781,#65782,#65783,#65784),
(#65785,#65786,#65787,#65788),(#65789,#65790,#65791,#65792),(#65793,#65794,
#65795,#65796)),.UNSPECIFIED.,.F.,.F.,.F.,(4,4),(4,4),(0.522097120207815,
1.00286848452581),(0.0400218729465705,0.0466073985929441),.UNSPECIFIED.);
#2210=B_SPLINE_SURFACE_WITH_KNOTS('',3,3,((#65804,#65805,#65806,#65807),
(#65808,#65809,#65810,#65811),(#65812,#65813,#65814,#65815),(#65816,#65817,
#65818,#65819)),.UNSPECIFIED.,.F.,.F.,.F.,(4,4),(4,4),(-0.00286823045918448,
0.477902879812007),(0.0265907346180622,0.0331702036774535),
 .UNSPECIFIED.);
#2211=B_SPLINE_SURFACE_WITH_KNOTS('',3,3,((#65872,#65873,#65874,#65875),
(#65876,#65877,#65878,#65879),(#65880,#65881,#65882,#65883),(#65884,#65885,
#65886,#65887)),.UNSPECIFIED.,.F.,.F.,.F.,(4,4),(4,4),(-0.00600003960325622,
1.),(0.0166015299238292,0.0265907346494256),.UNSPECIFIED.);
#2212=B_SPLINE_SURFACE_WITH_KNOTS('',3,3,((#65920,#65921,#65922,#65923),
(#65924,#65925,#65926,#65927),(#65928,#65929,#65930,#65931),(#65932,#65933,
#65934,#65935)),.UNSPECIFIED.,.F.,.F.,.F.,(4,4),(4,4),(0.522097120207639,
1.00286780293604),(0.0200175229645447,0.0265907346360307),.UNSPECIFIED.);
#2213=B_SPLINE_SURFACE_WITH_KNOTS('',3,3,((#65943,#65944,#65945,#65946),
(#65947,#65948,#65949,#65950),(#65951,#65952,#65953,#65954),(#65955,#65956,
#65957,#65958)),.UNSPECIFIED.,.F.,.F.,.F.,(4,4),(4,4),(0.522097120207691,
1.00286862201147),(0.0300094532292164,0.0365944846647027),.UNSPECIFIED.);
#2214=B_SPLINE_SURFACE_WITH_KNOTS('',3,3,((#65966,#65967,#65968,#65969),
(#65970,#65971,#65972,#65973),(#65974,#65975,#65976,#65977),(#65978,#65979,
#65980,#65981)),.UNSPECIFIED.,.F.,.F.,.F.,(4,4),(4,4),(-0.00286753128226228,
0.477902879812248),(0.0166015299238962,0.0231736788111887),
 .UNSPECIFIED.);
#2215=B_SPLINE_SURFACE_WITH_KNOTS('',3,3,((#65992,#65993,#65994,#65995),
(#65996,#65997,#65998,#65999),(#66000,#66001,#66002,#66003),(#66004,#66005,
#66006,#66007)),.UNSPECIFIED.,.F.,.F.,.F.,(4,4),(4,4),(-0.00286823257327278,
0.477902879814032),(0.0265907346180614,0.0331702037100441),
 .UNSPECIFIED.);
#2216=B_SPLINE_SURFACE_WITH_KNOTS('',3,3,((#66051,#66052,#66053,#66054),
(#66055,#66056,#66057,#66058),(#66059,#66060,#66061,#66062),(#66063,#66064,
#66065,#66066)),.UNSPECIFIED.,.F.,.F.,.F.,(4,4),(4,4),(-0.00600003960402798,
1.),(0.0166015299238298,0.0265907346180636),.UNSPECIFIED.);
#2217=B_SPLINE_SURFACE_WITH_KNOTS('',3,3,((#66078,#66079,#66080,#66081),
(#66082,#66083,#66084,#66085),(#66086,#66087,#66088,#66089),(#66090,#66091,
#66092,#66093)),.UNSPECIFIED.,.F.,.F.,.F.,(4,4),(4,4),(0.522097120211835,
1.00286791014268),(0.0100271466749328,0.0166015302184286),.UNSPECIFIED.);
#2218=B_SPLINE_SURFACE_WITH_KNOTS('',3,3,((#66101,#66102,#66103,#66104),
(#66105,#66106,#66107,#66108),(#66109,#66110,#66111,#66112),(#66113,#66114,
#66115,#66116)),.UNSPECIFIED.,.F.,.F.,.F.,(4,4),(4,4),(0.522097120210755,
1.00286780410477),(0.0200175229646526,0.0265907346180628),.UNSPECIFIED.);
#2219=B_SPLINE_SURFACE_WITH_KNOTS('',3,3,((#66124,#66125,#66126,#66127),
(#66128,#66129,#66130,#66131),(#66132,#66133,#66134,#66135),(#66136,#66137,
#66138,#66139)),.UNSPECIFIED.,.F.,.F.,.F.,(4,4),(4,4),(-0.00206901892528682,
0.346769728512502),(0.00660713154708869,0.0131849431292509),
 .UNSPECIFIED.);
#2220=B_SPLINE_SURFACE_WITH_KNOTS('',3,3,((#66142,#66143,#66144,#66145),
(#66146,#66147,#66148,#66149),(#66150,#66151,#66152,#66153),(#66154,#66155,
#66156,#66157)),.UNSPECIFIED.,.F.,.F.,.F.,(4,4),(4,4),(-0.00286753114059943,
0.477902879812669),(0.0166015299238967,0.0231736788090041),
 .UNSPECIFIED.);
#2221=B_SPLINE_SURFACE_WITH_KNOTS('',3,3,((#66202,#66203,#66204,#66205),
(#66206,#66207,#66208,#66209),(#66210,#66211,#66212,#66213),(#66214,#66215,
#66216,#66217)),.UNSPECIFIED.,.F.,.F.,.F.,(4,4),(4,4),(0.522097120209506,
1.00286791014276),(0.0100271466749321,0.0166015302184266),.UNSPECIFIED.);
#2222=B_SPLINE_SURFACE_WITH_KNOTS('',3,3,((#66225,#66226,#66227,#66228),
(#66229,#66230,#66231,#66232),(#66233,#66234,#66235,#66236),(#66237,#66238,
#66239,#66240)),.UNSPECIFIED.,.F.,.F.,.F.,(4,4),(4,4),(-0.00206901892681215,
0.346769728513212),(0.00660713154707451,0.0131849431468889),
 .UNSPECIFIED.);
#2223=B_SPLINE_SURFACE_WITH_KNOTS('',3,3,((#66243,#66244,#66245,#66246),
(#66247,#66248,#66249,#66250),(#66251,#66252,#66253,#66254),(#66255,#66256,
#66257,#66258)),.UNSPECIFIED.,.F.,.F.,.F.,(4,4),(4,4),(-0.00017189543604345,
1.00600020634822),(0.0665898698856049,0.0751325481139401),.UNSPECIFIED.);
#2224=B_SPLINE_SURFACE_WITH_KNOTS('',3,3,((#66274,#66275,#66276,#66277),
(#66278,#66279,#66280,#66281),(#66282,#66283,#66284,#66285),(#66286,#66287,
#66288,#66289)),.UNSPECIFIED.,.F.,.F.,.F.,(4,4),(4,4),(-0.00286833998606733,
0.477902879808364),(0.0665898698862513,0.0731716198748499),
 .UNSPECIFIED.);
#2225=B_SPLINE_SURFACE_WITH_KNOTS('',3,3,((#66323,#66324,#66325,#66326),
(#66327,#66328,#66329,#66330),(#66331,#66332,#66333,#66334),(#66335,#66336,
#66337,#66338)),.UNSPECIFIED.,.F.,.F.,.F.,(4,4),(4,4),(0.522097120207237,
1.00286791825536),(0.060015686548694,0.0665898700060145),.UNSPECIFIED.);
#2226=B_SPLINE_SURFACE_WITH_KNOTS('',3,3,((#66348,#66349,#66350,#66351),
(#66352,#66353,#66354,#66355),(#66356,#66357,#66358,#66359),(#66360,#66361,
#66362,#66363)),.UNSPECIFIED.,.F.,.F.,.F.,(4,4),(4,4),(-0.00286764392041053,
0.477902879806332),(0.0565997133101199,0.0631721430887065),
 .UNSPECIFIED.);
#2227=B_SPLINE_SURFACE_WITH_KNOTS('',3,3,((#66419,#66420,#66421,#66422),
(#66423,#66424,#66425,#66426),(#66427,#66428,#66429,#66430),(#66431,#66432,
#66433,#66434)),.UNSPECIFIED.,.F.,.F.,.F.,(4,4),(4,4),(0.522097120208047,
1.00286780122186),(0.0500263550858671,0.0565997133101429),.UNSPECIFIED.);
#2228=B_SPLINE_SURFACE_WITH_KNOTS('',3,3,((#66487,#66488,#66489,#66490),
(#66491,#66492,#66493,#66494),(#66495,#66496,#66497,#66498),(#66499,#66500,
#66501,#66502)),.UNSPECIFIED.,.F.,.F.,.F.,(4,4),(4,4),(0.522097120207861,
1.00286848452579),(0.04002187294657,0.0466073985929448),.UNSPECIFIED.);
#2229=B_SPLINE_SURFACE_WITH_KNOTS('',3,3,((#66568,#66569,#66570,#66571),
(#66572,#66573,#66574,#66575),(#66576,#66577,#66578,#66579),(#66580,#66581,
#66582,#66583)),.UNSPECIFIED.,.F.,.F.,.F.,(4,4),(4,4),(0.522097120207821,
1.00286862201146),(0.0300094532292163,0.0365944846647042),.UNSPECIFIED.);
#2230=B_SPLINE_SURFACE_WITH_KNOTS('',3,3,((#66616,#66617,#66618,#66619),
(#66620,#66621,#66622,#66623),(#66624,#66625,#66626,#66627),(#66628,#66629,
#66630,#66631)),.UNSPECIFIED.,.F.,.F.,.F.,(4,4),(4,4),(-0.00600003961893236,
1.00000000246922),(0.0166015299238283,0.0265907346180639),.UNSPECIFIED.);
#2231=B_SPLINE_SURFACE_WITH_KNOTS('',3,3,((#66643,#66644,#66645,#66646),
(#66647,#66648,#66649,#66650),(#66651,#66652,#66653,#66654),(#66655,#66656,
#66657,#66658)),.UNSPECIFIED.,.F.,.F.,.F.,(4,4),(4,4),(0.522097120207632,
1.00286780410469),(0.0200175229646513,0.0265907346180639),.UNSPECIFIED.);
#2232=B_SPLINE_SURFACE_WITH_KNOTS('',3,3,((#66666,#66667,#66668,#66669),
(#66670,#66671,#66672,#66673),(#66674,#66675,#66676,#66677),(#66678,#66679,
#66680,#66681)),.UNSPECIFIED.,.F.,.F.,.F.,(4,4),(4,4),(-0.00286753128237169,
0.477902879811433),(0.0166015299238964,0.0231736788111891),
 .UNSPECIFIED.);
#2233=B_SPLINE_SURFACE_WITH_KNOTS('',3,3,((#66721,#66722,#66723,#66724),
(#66725,#66726,#66727,#66728),(#66729,#66730,#66731,#66732),(#66733,#66734,
#66735,#66736)),.UNSPECIFIED.,.F.,.F.,.F.,(4,4),(4,4),(0.52209712020752,
1.00286791014276),(0.0100271466749314,0.0166015302184266),.UNSPECIFIED.);
#2234=B_SPLINE_SURFACE_WITH_KNOTS('',3,3,((#66744,#66745,#66746,#66747),
(#66748,#66749,#66750,#66751),(#66752,#66753,#66754,#66755),(#66756,#66757,
#66758,#66759)),.UNSPECIFIED.,.F.,.F.,.F.,(4,4),(4,4),(-0.00206901892532922,
0.346769728511554),(0.006607131547103,0.0131849431292508),.UNSPECIFIED.);
#2235=B_SPLINE_SURFACE_WITH_KNOTS('',3,3,((#66769,#66770,#66771,#66772),
(#66773,#66774,#66775,#66776),(#66777,#66778,#66779,#66780),(#66781,#66782,
#66783,#66784)),.UNSPECIFIED.,.F.,.F.,.F.,(4,4),(4,4),(-0.000171895436876361,
1.0060002063483),(0.0665898698856048,0.0751325481147718),.UNSPECIFIED.);
#2236=B_SPLINE_SURFACE_WITH_KNOTS('',3,3,((#66800,#66801,#66802,#66803),
(#66804,#66805,#66806,#66807),(#66808,#66809,#66810,#66811),(#66812,#66813,
#66814,#66815)),.UNSPECIFIED.,.F.,.F.,.F.,(4,4),(4,4),(-0.00286833998598439,
0.477902879806776),(0.0665898698862512,0.0731716198748508),
 .UNSPECIFIED.);
#2237=B_SPLINE_SURFACE_WITH_KNOTS('',3,3,((#66849,#66850,#66851,#66852),
(#66853,#66854,#66855,#66856),(#66857,#66858,#66859,#66860),(#66861,#66862,
#66863,#66864)),.UNSPECIFIED.,.F.,.F.,.F.,(4,4),(4,4),(0.52209712020747,
1.00286791825534),(0.0600156865486935,0.0665898700060149),.UNSPECIFIED.);
#2238=B_SPLINE_SURFACE_WITH_KNOTS('',3,3,((#66874,#66875,#66876,#66877),
(#66878,#66879,#66880,#66881),(#66882,#66883,#66884,#66885),(#66886,#66887,
#66888,#66889)),.UNSPECIFIED.,.F.,.F.,.F.,(4,4),(4,4),(-0.00286764392048183,
0.477902879805442),(0.0565997133101207,0.0631721430887071),
 .UNSPECIFIED.);
#2239=B_SPLINE_SURFACE_WITH_KNOTS('',3,3,((#66926,#66927,#66928,#66929),
(#66930,#66931,#66932,#66933),(#66934,#66935,#66936,#66937),(#66938,#66939,
#66940,#66941)),.UNSPECIFIED.,.F.,.F.,.F.,(4,4),(4,4),(0.52209712020814,
1.00286780122194),(0.0500263550858672,0.0565997133101429),.UNSPECIFIED.);
#2240=B_SPLINE_SURFACE_WITH_KNOTS('',3,3,((#67043,#67044,#67045,#67046),
(#67047,#67048,#67049,#67050),(#67051,#67052,#67053,#67054),(#67055,#67056,
#67057,#67058)),.UNSPECIFIED.,.F.,.F.,.F.,(4,4),(4,4),(0.522097120207753,
1.00286848452573),(0.0400218729465699,0.0466073985929442),.UNSPECIFIED.);
#2241=B_SPLINE_SURFACE_WITH_KNOTS('',3,3,((#67097,#67098,#67099,#67100),
(#67101,#67102,#67103,#67104),(#67105,#67106,#67107,#67108),(#67109,#67110,
#67111,#67112)),.UNSPECIFIED.,.F.,.F.,.F.,(4,4),(4,4),(0.522097120207934,
1.00286862201156),(0.0300094532292163,0.0365944846647036),.UNSPECIFIED.);
#2242=B_SPLINE_SURFACE_WITH_KNOTS('',3,3,((#67145,#67146,#67147,#67148),
(#67149,#67150,#67151,#67152),(#67153,#67154,#67155,#67156),(#67157,#67158,
#67159,#67160)),.UNSPECIFIED.,.F.,.F.,.F.,(4,4),(4,4),(-0.00600003960417136,
1.),(0.0166015299238285,0.0265907346180639),.UNSPECIFIED.);
#2243=B_SPLINE_SURFACE_WITH_KNOTS('',3,3,((#67172,#67173,#67174,#67175),
(#67176,#67177,#67178,#67179),(#67180,#67181,#67182,#67183),(#67184,#67185,
#67186,#67187)),.UNSPECIFIED.,.F.,.F.,.F.,(4,4),(4,4),(0.522097120207778,
1.00286780410464),(0.0200175229646509,0.0265907346180637),.UNSPECIFIED.);
#2244=B_SPLINE_SURFACE_WITH_KNOTS('',3,3,((#67243,#67244,#67245,#67246),
(#67247,#67248,#67249,#67250),(#67251,#67252,#67253,#67254),(#67255,#67256,
#67257,#67258)),.UNSPECIFIED.,.F.,.F.,.F.,(4,4),(4,4),(0.522097120207468,
1.00286791014282),(0.0100271466749307,0.0166015302184274),.UNSPECIFIED.);
#2245=B_SPLINE_SURFACE_WITH_KNOTS('',3,3,((#67266,#67267,#67268,#67269),
(#67270,#67271,#67272,#67273),(#67274,#67275,#67276,#67277),(#67278,#67279,
#67280,#67281)),.UNSPECIFIED.,.F.,.F.,.F.,(4,4),(4,4),(-0.00206901892691836,
0.346769728510449),(0.0066071315471172,0.01318494314689),.UNSPECIFIED.);
#2246=B_SPLINE_SURFACE_WITH_KNOTS('',3,3,((#67291,#67292,#67293,#67294),
(#67295,#67296,#67297,#67298),(#67299,#67300,#67301,#67302),(#67303,#67304,
#67305,#67306)),.UNSPECIFIED.,.F.,.F.,.F.,(4,4),(4,4),(-0.000171895437594373,
1.00600020634835),(0.0665898698856038,0.0751325481154914),.UNSPECIFIED.);
#2247=B_SPLINE_SURFACE_WITH_KNOTS('',3,3,((#67322,#67323,#67324,#67325),
(#67326,#67327,#67328,#67329),(#67330,#67331,#67332,#67333),(#67334,#67335,
#67336,#67337)),.UNSPECIFIED.,.F.,.F.,.F.,(4,4),(4,4),(-0.00286833998596821,
0.477902879804721),(0.0665898698862504,0.0731716198748499),
 .UNSPECIFIED.);
#2248=B_SPLINE_SURFACE_WITH_KNOTS('',3,3,((#67371,#67372,#67373,#67374),
(#67375,#67376,#67377,#67378),(#67379,#67380,#67381,#67382),(#67383,#67384,
#67385,#67386)),.UNSPECIFIED.,.F.,.F.,.F.,(4,4),(4,4),(0.522097120207427,
1.00286791825535),(0.0600156865486936,0.0665898700060144),.UNSPECIFIED.);
#2249=B_SPLINE_SURFACE_WITH_KNOTS('',3,3,((#67396,#67397,#67398,#67399),
(#67400,#67401,#67402,#67403),(#67404,#67405,#67406,#67407),(#67408,#67409,
#67410,#67411)),.UNSPECIFIED.,.F.,.F.,.F.,(4,4),(4,4),(-0.0028676439203989,
0.477902879804634),(0.0565997133101206,0.0631721430887066),
 .UNSPECIFIED.);
#2250=B_SPLINE_SURFACE_WITH_KNOTS('',3,3,((#67448,#67449,#67450,#67451),
(#67452,#67453,#67454,#67455),(#67456,#67457,#67458,#67459),(#67460,#67461,
#67462,#67463)),.UNSPECIFIED.,.F.,.F.,.F.,(4,4),(4,4),(0.522097120208323,
1.00286780122187),(0.0500263550858673,0.0565997133101427),.UNSPECIFIED.);
#2251=B_SPLINE_SURFACE_WITH_KNOTS('',3,3,((#67535,#67536,#67537,#67538),
(#67539,#67540,#67541,#67542),(#67543,#67544,#67545,#67546),(#67547,#67548,
#67549,#67550)),.UNSPECIFIED.,.F.,.F.,.F.,(4,4),(4,4),(0.522097120207898,
1.00286848452575),(0.0400218729465706,0.0466073985929453),.UNSPECIFIED.);
#2252=B_SPLINE_SURFACE_WITH_KNOTS('',3,3,((#67638,#67639,#67640,#67641),
(#67642,#67643,#67644,#67645),(#67646,#67647,#67648,#67649),(#67650,#67651,
#67652,#67653)),.UNSPECIFIED.,.F.,.F.,.F.,(4,4),(4,4),(0.52209712020705,
1.00286862201153),(0.0300094532292157,0.0365944846647043),.UNSPECIFIED.);
#2253=B_SPLINE_SURFACE_WITH_KNOTS('',3,3,((#67667,#67668,#67669,#67670),
(#67671,#67672,#67673,#67674),(#67675,#67676,#67677,#67678),(#67679,#67680,
#67681,#67682)),.UNSPECIFIED.,.F.,.F.,.F.,(4,4),(4,4),(-0.00600003961898803,
1.00000000246933),(0.0166015299238284,0.0265907346180633),.UNSPECIFIED.);
#2254=B_SPLINE_SURFACE_WITH_KNOTS('',3,3,((#67694,#67695,#67696,#67697),
(#67698,#67699,#67700,#67701),(#67702,#67703,#67704,#67705),(#67706,#67707,
#67708,#67709)),.UNSPECIFIED.,.F.,.F.,.F.,(4,4),(4,4),(0.522097120207611,
1.00286780410466),(0.0200175229646512,0.026590734618064),.UNSPECIFIED.);
#2255=B_SPLINE_SURFACE_WITH_KNOTS('',3,3,((#67762,#67763,#67764,#67765),
(#67766,#67767,#67768,#67769),(#67770,#67771,#67772,#67773),(#67774,#67775,
#67776,#67777)),.UNSPECIFIED.,.F.,.F.,.F.,(4,4),(4,4),(0.522097120207844,
1.00286791014275),(0.010027146674931,0.0166015302184281),.UNSPECIFIED.);
#2256=B_SPLINE_SURFACE_WITH_KNOTS('',3,3,((#67803,#67804,#67805,#67806),
(#67807,#67808,#67809,#67810),(#67811,#67812,#67813,#67814),(#67815,#67816,
#67817,#67818)),.UNSPECIFIED.,.F.,.F.,.F.,(4,4),(4,4),(-0.000171895438429025,
1.00600020634782),(0.0665898698856051,0.0751325481163243),.UNSPECIFIED.);
#2257=B_SPLINE_SURFACE_WITH_KNOTS('',3,3,((#67834,#67835,#67836,#67837),
(#67838,#67839,#67840,#67841),(#67842,#67843,#67844,#67845),(#67846,#67847,
#67848,#67849)),.UNSPECIFIED.,.F.,.F.,.F.,(4,4),(4,4),(-0.00286833998609855,
0.477902879802562),(0.0665898698862514,0.0731716198748506),
 .UNSPECIFIED.);
#2258=B_SPLINE_SURFACE_WITH_KNOTS('',3,3,((#67883,#67884,#67885,#67886),
(#67887,#67888,#67889,#67890),(#67891,#67892,#67893,#67894),(#67895,#67896,
#67897,#67898)),.UNSPECIFIED.,.F.,.F.,.F.,(4,4),(4,4),(0.522097120207539,
1.00286791825532),(0.0600156865486929,0.0665898700060141),.UNSPECIFIED.);
#2259=B_SPLINE_SURFACE_WITH_KNOTS('',3,3,((#67908,#67909,#67910,#67911),
(#67912,#67913,#67914,#67915),(#67916,#67917,#67918,#67919),(#67920,#67921,
#67922,#67923)),.UNSPECIFIED.,.F.,.F.,.F.,(4,4),(4,4),(-0.00286764392058903,
0.477902879803589),(0.0565997133101206,0.0631721430887071),
 .UNSPECIFIED.);
#2260=B_SPLINE_SURFACE_WITH_KNOTS('',3,3,((#67960,#67961,#67962,#67963),
(#67964,#67965,#67966,#67967),(#67968,#67969,#67970,#67971),(#67972,#67973,
#67974,#67975)),.UNSPECIFIED.,.F.,.F.,.F.,(4,4),(4,4),(0.522097120208424,
1.00286780122193),(0.0500263550858662,0.0565997133101414),.UNSPECIFIED.);
#2261=B_SPLINE_SURFACE_WITH_KNOTS('',3,3,((#68047,#68048,#68049,#68050),
(#68051,#68052,#68053,#68054),(#68055,#68056,#68057,#68058),(#68059,#68060,
#68061,#68062)),.UNSPECIFIED.,.F.,.F.,.F.,(4,4),(4,4),(0.522097120208083,
1.00286848452576),(0.0400218729465703,0.046607398592945),.UNSPECIFIED.);
#2262=B_SPLINE_SURFACE_WITH_KNOTS('',3,3,((#68131,#68132,#68133,#68134),
(#68135,#68136,#68137,#68138),(#68139,#68140,#68141,#68142),(#68143,#68144,
#68145,#68146)),.UNSPECIFIED.,.F.,.F.,.F.,(4,4),(4,4),(0.522097120207127,
1.00286862201156),(0.0300094532292159,0.0365944846647045),.UNSPECIFIED.);
#2263=B_SPLINE_SURFACE_WITH_KNOTS('',3,3,((#68173,#68174,#68175,#68176),
(#68177,#68178,#68179,#68180),(#68181,#68182,#68183,#68184),(#68185,#68186,
#68187,#68188)),.UNSPECIFIED.,.F.,.F.,.F.,(4,4),(4,4),(-0.00600003961897224,
1.00000000246921),(0.0166015299238289,0.0265907346180631),.UNSPECIFIED.);
#2264=B_SPLINE_SURFACE_WITH_KNOTS('',3,3,((#68225,#68226,#68227,#68228),
(#68229,#68230,#68231,#68232),(#68233,#68234,#68235,#68236),(#68237,#68238,
#68239,#68240)),.UNSPECIFIED.,.F.,.F.,.F.,(4,4),(4,4),(0.522097120208025,
1.0028678041047),(0.0200175229646515,0.0265907346180654),.UNSPECIFIED.);
#2265=B_SPLINE_SURFACE_WITH_KNOTS('',3,3,((#68274,#68275,#68276,#68277),
(#68278,#68279,#68280,#68281),(#68282,#68283,#68284,#68285),(#68286,#68287,
#68288,#68289)),.UNSPECIFIED.,.F.,.F.,.F.,(4,4),(4,4),(0.522097120207859,
1.0028679101242),(0.0100271466766969,0.0166015299239905),.UNSPECIFIED.);
#2266=B_SPLINE_SURFACE_WITH_KNOTS('',3,3,((#68315,#68316,#68317,#68318),
(#68319,#68320,#68321,#68322),(#68323,#68324,#68325,#68326),(#68327,#68328,
#68329,#68330)),.UNSPECIFIED.,.F.,.F.,.F.,(4,4),(4,4),(-0.000171895439399329,
1.00600020634824),(0.0665898698856054,0.075132548117295),.UNSPECIFIED.);
#2267=B_SPLINE_SURFACE_WITH_KNOTS('',3,3,((#68346,#68347,#68348,#68349),
(#68350,#68351,#68352,#68353),(#68354,#68355,#68356,#68357),(#68358,#68359,
#68360,#68361)),.UNSPECIFIED.,.F.,.F.,.F.,(4,4),(4,4),(-0.00286833998591409,
0.477902879800245),(0.0665898698862516,0.0731716198748497),
 .UNSPECIFIED.);
#2268=B_SPLINE_SURFACE_WITH_KNOTS('',3,3,((#68395,#68396,#68397,#68398),
(#68399,#68400,#68401,#68402),(#68403,#68404,#68405,#68406),(#68407,#68408,
#68409,#68410)),.UNSPECIFIED.,.F.,.F.,.F.,(4,4),(4,4),(0.522097120207782,
1.00286791825533),(0.0600156865486934,0.0665898700060146),.UNSPECIFIED.);
#2269=B_SPLINE_SURFACE_WITH_KNOTS('',3,3,((#68420,#68421,#68422,#68423),
(#68424,#68425,#68426,#68427),(#68428,#68429,#68430,#68431),(#68432,#68433,
#68434,#68435)),.UNSPECIFIED.,.F.,.F.,.F.,(4,4),(4,4),(-0.00286764392045514,
0.477902879801544),(0.0565997133101201,0.0631721430887063),
 .UNSPECIFIED.);
#2270=B_SPLINE_SURFACE_WITH_KNOTS('',3,3,((#68472,#68473,#68474,#68475),
(#68476,#68477,#68478,#68479),(#68480,#68481,#68482,#68483),(#68484,#68485,
#68486,#68487)),.UNSPECIFIED.,.F.,.F.,.F.,(4,4),(4,4),(0.522097120208516,
1.00286780122182),(0.0500263550858674,0.056599713310142),.UNSPECIFIED.);
#2271=B_SPLINE_SURFACE_WITH_KNOTS('',3,3,((#68559,#68560,#68561,#68562),
(#68563,#68564,#68565,#68566),(#68567,#68568,#68569,#68570),(#68571,#68572,
#68573,#68574)),.UNSPECIFIED.,.F.,.F.,.F.,(4,4),(4,4),(0.522097120208114,
1.00286848452572),(0.04002187294657,0.0466073985929447),.UNSPECIFIED.);
#2272=B_SPLINE_SURFACE_WITH_KNOTS('',3,3,((#68643,#68644,#68645,#68646),
(#68647,#68648,#68649,#68650),(#68651,#68652,#68653,#68654),(#68655,#68656,
#68657,#68658)),.UNSPECIFIED.,.F.,.F.,.F.,(4,4),(4,4),(0.522097120207307,
1.00286862201159),(0.0300094532292165,0.036594484664703),.UNSPECIFIED.);
#2273=B_SPLINE_SURFACE_WITH_KNOTS('',3,3,((#68691,#68692,#68693,#68694),
(#68695,#68696,#68697,#68698),(#68699,#68700,#68701,#68702),(#68703,#68704,
#68705,#68706)),.UNSPECIFIED.,.F.,.F.,.F.,(4,4),(4,4),(-0.00600003961900311,
1.00000000246904),(0.0166015299238284,0.0265907346180639),.UNSPECIFIED.);
#2274=B_SPLINE_SURFACE_WITH_KNOTS('',3,3,((#68718,#68719,#68720,#68721),
(#68722,#68723,#68724,#68725),(#68726,#68727,#68728,#68729),(#68730,#68731,
#68732,#68733)),.UNSPECIFIED.,.F.,.F.,.F.,(4,4),(4,4),(0.522097120208122,
1.00286780410469),(0.0200175229646511,0.0265907346180648),.UNSPECIFIED.);
#2275=B_SPLINE_SURFACE_WITH_KNOTS('',3,3,((#68800,#68801,#68802,#68803),
(#68804,#68805,#68806,#68807),(#68808,#68809,#68810,#68811),(#68812,#68813,
#68814,#68815)),.UNSPECIFIED.,.F.,.F.,.F.,(4,4),(4,4),(0.522097120208081,
1.00286791016343),(0.0100271466746118,0.0166015302184275),.UNSPECIFIED.);
#2276=B_SPLINE_SURFACE_WITH_KNOTS('',3,3,((#68830,#68831,#68832,#68833),
(#68834,#68835,#68836,#68837),(#68838,#68839,#68840,#68841),(#68842,#68843,
#68844,#68845)),.UNSPECIFIED.,.F.,.F.,.F.,(4,4),(4,4),(-0.000171895439914325,
1.00600020634824),(0.0665898698856042,0.0751325481178124),.UNSPECIFIED.);
#2277=B_SPLINE_SURFACE_WITH_KNOTS('',3,3,((#68861,#68862,#68863,#68864),
(#68865,#68866,#68867,#68868),(#68869,#68870,#68871,#68872),(#68873,#68874,
#68875,#68876)),.UNSPECIFIED.,.F.,.F.,.F.,(4,4),(4,4),(-0.00286833998599997,
0.477902879797889),(0.0665898698862502,0.0731716198748498),
 .UNSPECIFIED.);
#2278=B_SPLINE_SURFACE_WITH_KNOTS('',3,3,((#68910,#68911,#68912,#68913),
(#68914,#68915,#68916,#68917),(#68918,#68919,#68920,#68921),(#68922,#68923,
#68924,#68925)),.UNSPECIFIED.,.F.,.F.,.F.,(4,4),(4,4),(0.522097120207876,
1.00286791825534),(0.0600156865486929,0.0665898700060145),.UNSPECIFIED.);
#2279=B_SPLINE_SURFACE_WITH_KNOTS('',3,3,((#68935,#68936,#68937,#68938),
(#68939,#68940,#68941,#68942),(#68943,#68944,#68945,#68946),(#68947,#68948,
#68949,#68950)),.UNSPECIFIED.,.F.,.F.,.F.,(4,4),(4,4),(-0.00286764392042158,
0.477902879799075),(0.0565997133101205,0.0631721430887066),
 .UNSPECIFIED.);
#2280=B_SPLINE_SURFACE_WITH_KNOTS('',3,3,((#68987,#68988,#68989,#68990),
(#68991,#68992,#68993,#68994),(#68995,#68996,#68997,#68998),(#68999,#69000,
#69001,#69002)),.UNSPECIFIED.,.F.,.F.,.F.,(4,4),(4,4),(0.522097120208699,
1.0028678012219),(0.0500263550858663,0.056599713310142),.UNSPECIFIED.);
#2281=B_SPLINE_SURFACE_WITH_KNOTS('',3,3,((#69074,#69075,#69076,#69077),
(#69078,#69079,#69080,#69081),(#69082,#69083,#69084,#69085),(#69086,#69087,
#69088,#69089)),.UNSPECIFIED.,.F.,.F.,.F.,(4,4),(4,4),(0.522097120208235,
1.00286848452568),(0.0400218729465703,0.0466073985929451),.UNSPECIFIED.);
#2282=B_SPLINE_SURFACE_WITH_KNOTS('',3,3,((#69158,#69159,#69160,#69161),
(#69162,#69163,#69164,#69165),(#69166,#69167,#69168,#69169),(#69170,#69171,
#69172,#69173)),.UNSPECIFIED.,.F.,.F.,.F.,(4,4),(4,4),(0.522097120207369,
1.00286862201154),(0.0300094532292155,0.0365944846647039),.UNSPECIFIED.);
#2283=B_SPLINE_SURFACE_WITH_KNOTS('',3,3,((#69206,#69207,#69208,#69209),
(#69210,#69211,#69212,#69213),(#69214,#69215,#69216,#69217),(#69218,#69219,
#69220,#69221)),.UNSPECIFIED.,.F.,.F.,.F.,(4,4),(4,4),(-0.00600003961895626,
1.00000000246898),(0.0166015299238287,0.0265907346180638),.UNSPECIFIED.);
#2284=B_SPLINE_SURFACE_WITH_KNOTS('',3,3,((#69233,#69234,#69235,#69236),
(#69237,#69238,#69239,#69240),(#69241,#69242,#69243,#69244),(#69245,#69246,
#69247,#69248)),.UNSPECIFIED.,.F.,.F.,.F.,(4,4),(4,4),(0.52209712020829,
1.00286780410469),(0.0200175229646519,0.0265907346180654),.UNSPECIFIED.);
#2285=B_SPLINE_SURFACE_WITH_KNOTS('',3,3,((#69304,#69305,#69306,#69307),
(#69308,#69309,#69310,#69311),(#69312,#69313,#69314,#69315),(#69316,#69317,
#69318,#69319)),.UNSPECIFIED.,.F.,.F.,.F.,(4,4),(4,4),(0.522097120208155,
1.00286791014275),(0.0100271466749312,0.0166015302184278),.UNSPECIFIED.);
#2286=B_SPLINE_SURFACE_WITH_KNOTS('',3,3,((#69345,#69346,#69347,#69348),
(#69349,#69350,#69351,#69352),(#69353,#69354,#69355,#69356),(#69357,#69358,
#69359,#69360)),.UNSPECIFIED.,.F.,.F.,.F.,(4,4),(4,4),(-0.000171895440587519,
1.00600020634826),(0.0665898698856032,0.075132548118484),.UNSPECIFIED.);
#2287=B_SPLINE_SURFACE_WITH_KNOTS('',3,3,((#69376,#69377,#69378,#69379),
(#69380,#69381,#69382,#69383),(#69384,#69385,#69386,#69387),(#69388,#69389,
#69390,#69391)),.UNSPECIFIED.,.F.,.F.,.F.,(4,4),(4,4),(-0.00286833998609265,
0.477902879795302),(0.0665898698862507,0.0731716198748496),
 .UNSPECIFIED.);
#2288=B_SPLINE_SURFACE_WITH_KNOTS('',3,3,((#69425,#69426,#69427,#69428),
(#69429,#69430,#69431,#69432),(#69433,#69434,#69435,#69436),(#69437,#69438,
#69439,#69440)),.UNSPECIFIED.,.F.,.F.,.F.,(4,4),(4,4),(0.522097120207918,
1.0028679182553),(0.0600156865486945,0.0665898700060156),.UNSPECIFIED.);
#2289=B_SPLINE_SURFACE_WITH_KNOTS('',3,3,((#69450,#69451,#69452,#69453),
(#69454,#69455,#69456,#69457),(#69458,#69459,#69460,#69461),(#69462,#69463,
#69464,#69465)),.UNSPECIFIED.,.F.,.F.,.F.,(4,4),(4,4),(-0.00286764392026509,
0.477902879796714),(0.0565997133101197,0.0631721430887055),
 .UNSPECIFIED.);
#2290=B_SPLINE_SURFACE_WITH_KNOTS('',3,3,((#69502,#69503,#69504,#69505),
(#69506,#69507,#69508,#69509),(#69510,#69511,#69512,#69513),(#69514,#69515,
#69516,#69517)),.UNSPECIFIED.,.F.,.F.,.F.,(4,4),(4,4),(0.522097120208835,
1.00286780122186),(0.0500263550858674,0.0565997133101427),.UNSPECIFIED.);
#2291=B_SPLINE_SURFACE_WITH_KNOTS('',3,3,((#69589,#69590,#69591,#69592),
(#69593,#69594,#69595,#69596),(#69597,#69598,#69599,#69600),(#69601,#69602,
#69603,#69604)),.UNSPECIFIED.,.F.,.F.,.F.,(4,4),(4,4),(0.522097120208443,
1.00286848452571),(0.0400218729465707,0.0466073985929442),.UNSPECIFIED.);
#2292=B_SPLINE_SURFACE_WITH_KNOTS('',3,3,((#69673,#69674,#69675,#69676),
(#69677,#69678,#69679,#69680),(#69681,#69682,#69683,#69684),(#69685,#69686,
#69687,#69688)),.UNSPECIFIED.,.F.,.F.,.F.,(4,4),(4,4),(0.522097120207526,
1.00286862201152),(0.0300094532292168,0.0365944846647034),.UNSPECIFIED.);
#2293=B_SPLINE_SURFACE_WITH_KNOTS('',3,3,((#69721,#69722,#69723,#69724),
(#69725,#69726,#69727,#69728),(#69729,#69730,#69731,#69732),(#69733,#69734,
#69735,#69736)),.UNSPECIFIED.,.F.,.F.,.F.,(4,4),(4,4),(-0.00600003961890225,
1.00000000246947),(0.0166015299238274,0.0265907346180638),.UNSPECIFIED.);
#2294=B_SPLINE_SURFACE_WITH_KNOTS('',3,3,((#69748,#69749,#69750,#69751),
(#69752,#69753,#69754,#69755),(#69756,#69757,#69758,#69759),(#69760,#69761,
#69762,#69763)),.UNSPECIFIED.,.F.,.F.,.F.,(4,4),(4,4),(0.522097120208393,
1.00286780410469),(0.0200175229646505,0.0265907346180638),.UNSPECIFIED.);
#2295=B_SPLINE_SURFACE_WITH_KNOTS('',3,3,((#69819,#69820,#69821,#69822),
(#69823,#69824,#69825,#69826),(#69827,#69828,#69829,#69830),(#69831,#69832,
#69833,#69834)),.UNSPECIFIED.,.F.,.F.,.F.,(4,4),(4,4),(0.522097120208245,
1.00286791014273),(0.0100271466749314,0.0166015302184273),.UNSPECIFIED.);
#2296=B_SPLINE_SURFACE_WITH_KNOTS('',3,3,((#69860,#69861,#69862,#69863),
(#69864,#69865,#69866,#69867),(#69868,#69869,#69870,#69871),(#69872,#69873,
#69874,#69875)),.UNSPECIFIED.,.F.,.F.,.F.,(4,4),(4,4),(-0.000171895440979682,
1.00600020634811),(0.0665898698856036,0.0751325481188771),.UNSPECIFIED.);
#2297=B_SPLINE_SURFACE_WITH_KNOTS('',3,3,((#69891,#69892,#69893,#69894),
(#69895,#69896,#69897,#69898),(#69899,#69900,#69901,#69902),(#69903,#69904,
#69905,#69906)),.UNSPECIFIED.,.F.,.F.,.F.,(4,4),(4,4),(-0.00286833998597401,
0.477902879792813),(0.0665898698862506,0.0731716198748496),
 .UNSPECIFIED.);
#2298=B_SPLINE_SURFACE_WITH_KNOTS('',3,3,((#69940,#69941,#69942,#69943),
(#69944,#69945,#69946,#69947),(#69948,#69949,#69950,#69951),(#69952,#69953,
#69954,#69955)),.UNSPECIFIED.,.F.,.F.,.F.,(4,4),(4,4),(0.522097120208123,
1.0028679182553),(0.0600156865486942,0.0665898700060151),.UNSPECIFIED.);
#2299=B_SPLINE_SURFACE_WITH_KNOTS('',3,3,((#69965,#69966,#69967,#69968),
(#69969,#69970,#69971,#69972),(#69973,#69974,#69975,#69976),(#69977,#69978,
#69979,#69980)),.UNSPECIFIED.,.F.,.F.,.F.,(4,4),(4,4),(-0.00286764392041422,
0.477902879794138),(0.0565997133101191,0.0631721430887055),
 .UNSPECIFIED.);
#2300=B_SPLINE_SURFACE_WITH_KNOTS('',3,3,((#70017,#70018,#70019,#70020),
(#70021,#70022,#70023,#70024),(#70025,#70026,#70027,#70028),(#70029,#70030,
#70031,#70032)),.UNSPECIFIED.,.F.,.F.,.F.,(4,4),(4,4),(0.522097120208892,
1.00286780122189),(0.0500263550858667,0.0565997133101436),.UNSPECIFIED.);
#2301=B_SPLINE_SURFACE_WITH_KNOTS('',3,3,((#70104,#70105,#70106,#70107),
(#70108,#70109,#70110,#70111),(#70112,#70113,#70114,#70115),(#70116,#70117,
#70118,#70119)),.UNSPECIFIED.,.F.,.F.,.F.,(4,4),(4,4),(0.522097120208542,
1.00286848452571),(0.04002187294657,0.046607398592945),.UNSPECIFIED.);
#2302=B_SPLINE_SURFACE_WITH_KNOTS('',3,3,((#70188,#70189,#70190,#70191),
(#70192,#70193,#70194,#70195),(#70196,#70197,#70198,#70199),(#70200,#70201,
#70202,#70203)),.UNSPECIFIED.,.F.,.F.,.F.,(4,4),(4,4),(0.522097120207708,
1.00286862201152),(0.0300094532292153,0.0365944846647039),.UNSPECIFIED.);
#2303=B_SPLINE_SURFACE_WITH_KNOTS('',3,3,((#70236,#70237,#70238,#70239),
(#70240,#70241,#70242,#70243),(#70244,#70245,#70246,#70247),(#70248,#70249,
#70250,#70251)),.UNSPECIFIED.,.F.,.F.,.F.,(4,4),(4,4),(-0.0060000396189727,
1.00000000246903),(0.0166015299238285,0.0265907346180665),.UNSPECIFIED.);
#2304=B_SPLINE_SURFACE_WITH_KNOTS('',3,3,((#70263,#70264,#70265,#70266),
(#70267,#70268,#70269,#70270),(#70271,#70272,#70273,#70274),(#70275,#70276,
#70277,#70278)),.UNSPECIFIED.,.F.,.F.,.F.,(4,4),(4,4),(0.522097120208515,
1.0028678041046),(0.0200175229646511,0.0265907346180649),.UNSPECIFIED.);
#2305=B_SPLINE_SURFACE_WITH_KNOTS('',3,3,((#70334,#70335,#70336,#70337),
(#70338,#70339,#70340,#70341),(#70342,#70343,#70344,#70345),(#70346,#70347,
#70348,#70349)),.UNSPECIFIED.,.F.,.F.,.F.,(4,4),(4,4),(0.522097120208354,
1.00286791014275),(0.0100271466749302,0.0166015302184277),.UNSPECIFIED.);
#2306=B_SPLINE_SURFACE_WITH_KNOTS('',3,3,((#70375,#70376,#70377,#70378),
(#70379,#70380,#70381,#70382),(#70383,#70384,#70385,#70386),(#70387,#70388,
#70389,#70390)),.UNSPECIFIED.,.F.,.F.,.F.,(4,4),(4,4),(-0.000171895441186971,
1.00600020634811),(0.0665898698856045,0.0751325481190837),.UNSPECIFIED.);
#2307=B_SPLINE_SURFACE_WITH_KNOTS('',3,3,((#70406,#70407,#70408,#70409),
(#70410,#70411,#70412,#70413),(#70414,#70415,#70416,#70417),(#70418,#70419,
#70420,#70421)),.UNSPECIFIED.,.F.,.F.,.F.,(4,4),(4,4),(-0.00286833998595339,
0.477902879790259),(0.0665898698862505,0.0731716198748495),
 .UNSPECIFIED.);
#2308=B_SPLINE_SURFACE_WITH_KNOTS('',3,3,((#70455,#70456,#70457,#70458),
(#70459,#70460,#70461,#70462),(#70463,#70464,#70465,#70466),(#70467,#70468,
#70469,#70470)),.UNSPECIFIED.,.F.,.F.,.F.,(4,4),(4,4),(0.52209712020833,
1.00286791825539),(0.060015686548694,0.0665898700060138),.UNSPECIFIED.);
#2309=B_SPLINE_SURFACE_WITH_KNOTS('',3,3,((#70480,#70481,#70482,#70483),
(#70484,#70485,#70486,#70487),(#70488,#70489,#70490,#70491),(#70492,#70493,
#70494,#70495)),.UNSPECIFIED.,.F.,.F.,.F.,(4,4),(4,4),(-0.0028676439203935,
0.47790287979146),(0.0565997133101203,0.0631721430887067),.UNSPECIFIED.);
#2310=B_SPLINE_SURFACE_WITH_KNOTS('',3,3,((#70532,#70533,#70534,#70535),
(#70536,#70537,#70538,#70539),(#70540,#70541,#70542,#70543),(#70544,#70545,
#70546,#70547)),.UNSPECIFIED.,.F.,.F.,.F.,(4,4),(4,4),(0.522097120209094,
1.00286780122184),(0.0500263550858663,0.0565997133101416),.UNSPECIFIED.);
#2311=B_SPLINE_SURFACE_WITH_KNOTS('',3,3,((#70619,#70620,#70621,#70622),
(#70623,#70624,#70625,#70626),(#70627,#70628,#70629,#70630),(#70631,#70632,
#70633,#70634)),.UNSPECIFIED.,.F.,.F.,.F.,(4,4),(4,4),(0.522097120208589,
1.0028684845257),(0.0400218729465704,0.0466073985929445),.UNSPECIFIED.);
#2312=B_SPLINE_SURFACE_WITH_KNOTS('',3,3,((#70703,#70704,#70705,#70706),
(#70707,#70708,#70709,#70710),(#70711,#70712,#70713,#70714),(#70715,#70716,
#70717,#70718)),.UNSPECIFIED.,.F.,.F.,.F.,(4,4),(4,4),(0.522097120207781,
1.00286862201155),(0.0300094532292166,0.0365944846647042),.UNSPECIFIED.);
#2313=B_SPLINE_SURFACE_WITH_KNOTS('',3,3,((#70751,#70752,#70753,#70754),
(#70755,#70756,#70757,#70758),(#70759,#70760,#70761,#70762),(#70763,#70764,
#70765,#70766)),.UNSPECIFIED.,.F.,.F.,.F.,(4,4),(4,4),(-0.00600003962552284,
1.00000000356504),(0.0166015299238284,0.0265907346180639),.UNSPECIFIED.);
#2314=B_SPLINE_SURFACE_WITH_KNOTS('',3,3,((#70778,#70779,#70780,#70781),
(#70782,#70783,#70784,#70785),(#70786,#70787,#70788,#70789),(#70790,#70791,
#70792,#70793)),.UNSPECIFIED.,.F.,.F.,.F.,(4,4),(4,4),(0.522097120208704,
1.0028678041047),(0.0200175229646511,0.0265907346180645),.UNSPECIFIED.);
#2315=B_SPLINE_SURFACE_WITH_KNOTS('',3,3,((#70849,#70850,#70851,#70852),
(#70853,#70854,#70855,#70856),(#70857,#70858,#70859,#70860),(#70861,#70862,
#70863,#70864)),.UNSPECIFIED.,.F.,.F.,.F.,(4,4),(4,4),(0.522097120208485,
1.00286791014268),(0.0100271466749304,0.0166015302184274),.UNSPECIFIED.);
#2316=B_SPLINE_SURFACE_WITH_KNOTS('',3,3,((#70890,#70891,#70892,#70893),
(#70894,#70895,#70896,#70897),(#70898,#70899,#70900,#70901),(#70902,#70903,
#70904,#70905)),.UNSPECIFIED.,.F.,.F.,.F.,(4,4),(4,4),(-0.000171895441305832,
1.0060002063484),(0.0665898698856052,0.0751325481192021),.UNSPECIFIED.);
#2317=B_SPLINE_SURFACE_WITH_KNOTS('',3,3,((#70921,#70922,#70923,#70924),
(#70925,#70926,#70927,#70928),(#70929,#70930,#70931,#70932),(#70933,#70934,
#70935,#70936)),.UNSPECIFIED.,.F.,.F.,.F.,(4,4),(4,4),(-0.00286833998590792,
0.47790287978769),(0.0665898698862517,0.0731716198748515),.UNSPECIFIED.);
#2318=B_SPLINE_SURFACE_WITH_KNOTS('',3,3,((#70970,#70971,#70972,#70973),
(#70974,#70975,#70976,#70977),(#70978,#70979,#70980,#70981),(#70982,#70983,
#70984,#70985)),.UNSPECIFIED.,.F.,.F.,.F.,(4,4),(4,4),(0.522097120208308,
1.00286791825531),(0.0600156865486945,0.0665898700060152),.UNSPECIFIED.);
#2319=B_SPLINE_SURFACE_WITH_KNOTS('',3,3,((#70995,#70996,#70997,#70998),
(#70999,#71000,#71001,#71002),(#71003,#71004,#71005,#71006),(#71007,#71008,
#71009,#71010)),.UNSPECIFIED.,.F.,.F.,.F.,(4,4),(4,4),(-0.00286764392030075,
0.477902879788978),(0.0565997133101198,0.0631721430887066),
 .UNSPECIFIED.);
#2320=B_SPLINE_SURFACE_WITH_KNOTS('',3,3,((#71047,#71048,#71049,#71050),
(#71051,#71052,#71053,#71054),(#71055,#71056,#71057,#71058),(#71059,#71060,
#71061,#71062)),.UNSPECIFIED.,.F.,.F.,.F.,(4,4),(4,4),(0.522097120209165,
1.00286780122187),(0.0500263550858667,0.0565997133101418),.UNSPECIFIED.);
#2321=B_SPLINE_SURFACE_WITH_KNOTS('',3,3,((#71134,#71135,#71136,#71137),
(#71138,#71139,#71140,#71141),(#71142,#71143,#71144,#71145),(#71146,#71147,
#71148,#71149)),.UNSPECIFIED.,.F.,.F.,.F.,(4,4),(4,4),(0.522097120208777,
1.00286848452568),(0.0400218729465703,0.0466073985929443),.UNSPECIFIED.);
#2322=B_SPLINE_SURFACE_WITH_KNOTS('',3,3,((#71218,#71219,#71220,#71221),
(#71222,#71223,#71224,#71225),(#71226,#71227,#71228,#71229),(#71230,#71231,
#71232,#71233)),.UNSPECIFIED.,.F.,.F.,.F.,(4,4),(4,4),(0.522097120207874,
1.00286862201151),(0.030009453229216,0.0365944846647041),.UNSPECIFIED.);
#2323=B_SPLINE_SURFACE_WITH_KNOTS('',3,3,((#71266,#71267,#71268,#71269),
(#71270,#71271,#71272,#71273),(#71274,#71275,#71276,#71277),(#71278,#71279,
#71280,#71281)),.UNSPECIFIED.,.F.,.F.,.F.,(4,4),(4,4),(-0.00600003964383708,
1.00000000663581),(0.0166015299238285,0.0265907346180638),.UNSPECIFIED.);
#2324=B_SPLINE_SURFACE_WITH_KNOTS('',3,3,((#71293,#71294,#71295,#71296),
(#71297,#71298,#71299,#71300),(#71301,#71302,#71303,#71304),(#71305,#71306,
#71307,#71308)),.UNSPECIFIED.,.F.,.F.,.F.,(4,4),(4,4),(0.522097120208762,
1.00286780410467),(0.0200175229646509,0.0265907346180652),.UNSPECIFIED.);
#2325=B_SPLINE_SURFACE_WITH_KNOTS('',3,3,((#71364,#71365,#71366,#71367),
(#71368,#71369,#71370,#71371),(#71372,#71373,#71374,#71375),(#71376,#71377,
#71378,#71379)),.UNSPECIFIED.,.F.,.F.,.F.,(4,4),(4,4),(0.522097120208637,
1.0028679101427),(0.0100271466749316,0.016601530218427),.UNSPECIFIED.);
#2326=B_SPLINE_SURFACE_WITH_KNOTS('',3,3,((#71405,#71406,#71407,#71408),
(#71409,#71410,#71411,#71412),(#71413,#71414,#71415,#71416),(#71417,#71418,
#71419,#71420)),.UNSPECIFIED.,.F.,.F.,.F.,(4,4),(4,4),(-0.000171895441813873,
1.00600020634879),(0.0665898698856054,0.0751325481197112),.UNSPECIFIED.);
#2327=B_SPLINE_SURFACE_WITH_KNOTS('',3,3,((#71436,#71437,#71438,#71439),
(#71440,#71441,#71442,#71443),(#71444,#71445,#71446,#71447),(#71448,#71449,
#71450,#71451)),.UNSPECIFIED.,.F.,.F.,.F.,(4,4),(4,4),(-0.00286833998582016,
0.47790287978653),(0.0665898698862516,0.0731716198748501),.UNSPECIFIED.);
#2328=B_SPLINE_SURFACE_WITH_KNOTS('',3,3,((#71485,#71486,#71487,#71488),
(#71489,#71490,#71491,#71492),(#71493,#71494,#71495,#71496),(#71497,#71498,
#71499,#71500)),.UNSPECIFIED.,.F.,.F.,.F.,(4,4),(4,4),(0.52209712020856,
1.00286791825536),(0.0600156865486949,0.0665898700060146),.UNSPECIFIED.);
#2329=B_SPLINE_SURFACE_WITH_KNOTS('',3,3,((#71510,#71511,#71512,#71513),
(#71514,#71515,#71516,#71517),(#71518,#71519,#71520,#71521),(#71522,#71523,
#71524,#71525)),.UNSPECIFIED.,.F.,.F.,.F.,(4,4),(4,4),(-0.00286764392030322,
0.477902879786523),(0.0565997133101207,0.0631721430887062),
 .UNSPECIFIED.);
#2330=B_SPLINE_SURFACE_WITH_KNOTS('',3,3,((#71562,#71563,#71564,#71565),
(#71566,#71567,#71568,#71569),(#71570,#71571,#71572,#71573),(#71574,#71575,
#71576,#71577)),.UNSPECIFIED.,.F.,.F.,.F.,(4,4),(4,4),(0.522097120209218,
1.00286780122187),(0.0500263550858677,0.0565997133101425),.UNSPECIFIED.);
#2331=B_SPLINE_SURFACE_WITH_KNOTS('',3,3,((#71649,#71650,#71651,#71652),
(#71653,#71654,#71655,#71656),(#71657,#71658,#71659,#71660),(#71661,#71662,
#71663,#71664)),.UNSPECIFIED.,.F.,.F.,.F.,(4,4),(4,4),(0.522097120208972,
1.00286848452572),(0.0400218729465709,0.046607398592944),.UNSPECIFIED.);
#2332=B_SPLINE_SURFACE_WITH_KNOTS('',3,3,((#71733,#71734,#71735,#71736),
(#71737,#71738,#71739,#71740),(#71741,#71742,#71743,#71744),(#71745,#71746,
#71747,#71748)),.UNSPECIFIED.,.F.,.F.,.F.,(4,4),(4,4),(0.522097120207987,
1.00286862201156),(0.0300094532292159,0.0365944846647027),.UNSPECIFIED.);
#2333=B_SPLINE_SURFACE_WITH_KNOTS('',3,3,((#71781,#71782,#71783,#71784),
(#71785,#71786,#71787,#71788),(#71789,#71790,#71791,#71792),(#71793,#71794,
#71795,#71796)),.UNSPECIFIED.,.F.,.F.,.F.,(4,4),(4,4),(-0.00600003962543891,
1.00000000356508),(0.0166015299238274,0.0265907346180633),.UNSPECIFIED.);
#2334=B_SPLINE_SURFACE_WITH_KNOTS('',3,3,((#71808,#71809,#71810,#71811),
(#71812,#71813,#71814,#71815),(#71816,#71817,#71818,#71819),(#71820,#71821,
#71822,#71823)),.UNSPECIFIED.,.F.,.F.,.F.,(4,4),(4,4),(0.522097120208868,
1.00286780410463),(0.0200175229646521,0.0265907346180646),.UNSPECIFIED.);
#2335=B_SPLINE_SURFACE_WITH_KNOTS('',3,3,((#71879,#71880,#71881,#71882),
(#71883,#71884,#71885,#71886),(#71887,#71888,#71889,#71890),(#71891,#71892,
#71893,#71894)),.UNSPECIFIED.,.F.,.F.,.F.,(4,4),(4,4),(0.522097120208733,
1.00286791014268),(0.0100271466749324,0.0166015302184277),.UNSPECIFIED.);
#2336=B_SPLINE_SURFACE_WITH_KNOTS('',3,3,((#71920,#71921,#71922,#71923),
(#71924,#71925,#71926,#71927),(#71928,#71929,#71930,#71931),(#71932,#71933,
#71934,#71935)),.UNSPECIFIED.,.F.,.F.,.F.,(4,4),(4,4),(-0.000171895441749836,
1.00600020634798),(0.0665898698856038,0.0751325481196475),.UNSPECIFIED.);
#2337=B_SPLINE_SURFACE_WITH_KNOTS('',3,3,((#71951,#71952,#71953,#71954),
(#71955,#71956,#71957,#71958),(#71959,#71960,#71961,#71962),(#71963,#71964,
#71965,#71966)),.UNSPECIFIED.,.F.,.F.,.F.,(4,4),(4,4),(-0.00286833998593411,
0.477902879786537),(0.0665898698862503,0.0731716198748497),
 .UNSPECIFIED.);
#2338=B_SPLINE_SURFACE_WITH_KNOTS('',3,3,((#72000,#72001,#72002,#72003),
(#72004,#72005,#72006,#72007),(#72008,#72009,#72010,#72011),(#72012,#72013,
#72014,#72015)),.UNSPECIFIED.,.F.,.F.,.F.,(4,4),(4,4),(0.5220971202086,
1.00286791825529),(0.0600156865486942,0.0665898700060152),.UNSPECIFIED.);
#2339=B_SPLINE_SURFACE_WITH_KNOTS('',3,3,((#72025,#72026,#72027,#72028),
(#72029,#72030,#72031,#72032),(#72033,#72034,#72035,#72036),(#72037,#72038,
#72039,#72040)),.UNSPECIFIED.,.F.,.F.,.F.,(4,4),(4,4),(-0.00286764392031674,
0.477902879786535),(0.05659971331012,0.0631721430887066),.UNSPECIFIED.);
#2340=B_SPLINE_SURFACE_WITH_KNOTS('',3,3,((#72077,#72078,#72079,#72080),
(#72081,#72082,#72083,#72084),(#72085,#72086,#72087,#72088),(#72089,#72090,
#72091,#72092)),.UNSPECIFIED.,.F.,.F.,.F.,(4,4),(4,4),(0.522097120209359,
1.00286780122188),(0.0500263550858677,0.0565997133101425),.UNSPECIFIED.);
#2341=B_SPLINE_SURFACE_WITH_KNOTS('',3,3,((#72164,#72165,#72166,#72167),
(#72168,#72169,#72170,#72171),(#72172,#72173,#72174,#72175),(#72176,#72177,
#72178,#72179)),.UNSPECIFIED.,.F.,.F.,.F.,(4,4),(4,4),(0.522097120208958,
1.00286848452566),(0.0400218729465711,0.0466073985929456),.UNSPECIFIED.);
#2342=B_SPLINE_SURFACE_WITH_KNOTS('',3,3,((#72248,#72249,#72250,#72251),
(#72252,#72253,#72254,#72255),(#72256,#72257,#72258,#72259),(#72260,#72261,
#72262,#72263)),.UNSPECIFIED.,.F.,.F.,.F.,(4,4),(4,4),(0.52209712020823,
1.00286862201158),(0.0300094532292163,0.0365944846647038),.UNSPECIFIED.);
#2343=B_SPLINE_SURFACE_WITH_KNOTS('',3,3,((#72296,#72297,#72298,#72299),
(#72300,#72301,#72302,#72303),(#72304,#72305,#72306,#72307),(#72308,#72309,
#72310,#72311)),.UNSPECIFIED.,.F.,.F.,.F.,(4,4),(4,4),(-0.00600003961876303,
1.00000000246915),(0.0166015299238274,0.0265907346180639),.UNSPECIFIED.);
#2344=B_SPLINE_SURFACE_WITH_KNOTS('',3,3,((#72323,#72324,#72325,#72326),
(#72327,#72328,#72329,#72330),(#72331,#72332,#72333,#72334),(#72335,#72336,
#72337,#72338)),.UNSPECIFIED.,.F.,.F.,.F.,(4,4),(4,4),(0.52209712020903,
1.00286780410459),(0.0200175229646514,0.0265907346180651),.UNSPECIFIED.);
#2345=B_SPLINE_SURFACE_WITH_KNOTS('',3,3,((#72394,#72395,#72396,#72397),
(#72398,#72399,#72400,#72401),(#72402,#72403,#72404,#72405),(#72406,#72407,
#72408,#72409)),.UNSPECIFIED.,.F.,.F.,.F.,(4,4),(4,4),(0.522097120208794,
1.00286791014255),(0.0100271466749329,0.0166015302184292),.UNSPECIFIED.);
#2346=B_SPLINE_SURFACE_WITH_KNOTS('',3,3,((#72435,#72436,#72437,#72438),
(#72439,#72440,#72441,#72442),(#72443,#72444,#72445,#72446),(#72447,#72448,
#72449,#72450)),.UNSPECIFIED.,.F.,.F.,.F.,(4,4),(4,4),(-0.000171895441761731,
1.00600020634806),(0.0665898698856041,0.0751325481196596),.UNSPECIFIED.);
#2347=B_SPLINE_SURFACE_WITH_KNOTS('',3,3,((#72466,#72467,#72468,#72469),
(#72470,#72471,#72472,#72473),(#72474,#72475,#72476,#72477),(#72478,#72479,
#72480,#72481)),.UNSPECIFIED.,.F.,.F.,.F.,(4,4),(4,4),(-0.00286833998590083,
0.477902879786522),(0.0665898698862503,0.0731716198748499),
 .UNSPECIFIED.);
#2348=B_SPLINE_SURFACE_WITH_KNOTS('',3,3,((#72515,#72516,#72517,#72518),
(#72519,#72520,#72521,#72522),(#72523,#72524,#72525,#72526),(#72527,#72528,
#72529,#72530)),.UNSPECIFIED.,.F.,.F.,.F.,(4,4),(4,4),(0.522097120208708,
1.00286791825529),(0.060015686548694,0.0665898700060155),.UNSPECIFIED.);
#2349=B_SPLINE_SURFACE_WITH_KNOTS('',3,3,((#72540,#72541,#72542,#72543),
(#72544,#72545,#72546,#72547),(#72548,#72549,#72550,#72551),(#72552,#72553,
#72554,#72555)),.UNSPECIFIED.,.F.,.F.,.F.,(4,4),(4,4),(-0.00286764392027188,
0.477902879786551),(0.0565997133101198,0.0631721430887068),
 .UNSPECIFIED.);
#2350=B_SPLINE_SURFACE_WITH_KNOTS('',3,3,((#72592,#72593,#72594,#72595),
(#72596,#72597,#72598,#72599),(#72600,#72601,#72602,#72603),(#72604,#72605,
#72606,#72607)),.UNSPECIFIED.,.F.,.F.,.F.,(4,4),(4,4),(0.522097120209487,
1.00286780122187),(0.0500263550858668,0.0565997133101425),.UNSPECIFIED.);
#2351=B_SPLINE_SURFACE_WITH_KNOTS('',3,3,((#72679,#72680,#72681,#72682),
(#72683,#72684,#72685,#72686),(#72687,#72688,#72689,#72690),(#72691,#72692,
#72693,#72694)),.UNSPECIFIED.,.F.,.F.,.F.,(4,4),(4,4),(0.522097120209154,
1.00286848452568),(0.04002187294657,0.0466073985929447),.UNSPECIFIED.);
#2352=B_SPLINE_SURFACE_WITH_KNOTS('',3,3,((#72763,#72764,#72765,#72766),
(#72767,#72768,#72769,#72770),(#72771,#72772,#72773,#72774),(#72775,#72776,
#72777,#72778)),.UNSPECIFIED.,.F.,.F.,.F.,(4,4),(4,4),(0.522097120208207,
1.00286862201156),(0.0300094532292159,0.0365944846647044),.UNSPECIFIED.);
#2353=B_SPLINE_SURFACE_WITH_KNOTS('',3,3,((#72811,#72812,#72813,#72814),
(#72815,#72816,#72817,#72818),(#72819,#72820,#72821,#72822),(#72823,#72824,
#72825,#72826)),.UNSPECIFIED.,.F.,.F.,.F.,(4,4),(4,4),(-0.00600003961874595,
1.00000000246929),(0.0166015299238277,0.0265907346180653),.UNSPECIFIED.);
#2354=B_SPLINE_SURFACE_WITH_KNOTS('',3,3,((#72838,#72839,#72840,#72841),
(#72842,#72843,#72844,#72845),(#72846,#72847,#72848,#72849),(#72850,#72851,
#72852,#72853)),.UNSPECIFIED.,.F.,.F.,.F.,(4,4),(4,4),(0.522097120209191,
1.00286780410462),(0.0200175229646514,0.026590734618065),.UNSPECIFIED.);
#2355=B_SPLINE_SURFACE_WITH_KNOTS('',3,3,((#72909,#72910,#72911,#72912),
(#72913,#72914,#72915,#72916),(#72917,#72918,#72919,#72920),(#72921,#72922,
#72923,#72924)),.UNSPECIFIED.,.F.,.F.,.F.,(4,4),(4,4),(0.522097120208983,
1.00286791014259),(0.0100271466749312,0.0166015302184277),.UNSPECIFIED.);
#2356=B_SPLINE_SURFACE_WITH_KNOTS('',3,3,((#72950,#72951,#72952,#72953),
(#72954,#72955,#72956,#72957),(#72958,#72959,#72960,#72961),(#72962,#72963,
#72964,#72965)),.UNSPECIFIED.,.F.,.F.,.F.,(4,4),(4,4),(-0.000171895441537365,
1.00600020634792),(0.0665898698856057,0.0751325481194348),.UNSPECIFIED.);
#2357=B_SPLINE_SURFACE_WITH_KNOTS('',3,3,((#72981,#72982,#72983,#72984),
(#72985,#72986,#72987,#72988),(#72989,#72990,#72991,#72992),(#72993,#72994,
#72995,#72996)),.UNSPECIFIED.,.F.,.F.,.F.,(4,4),(4,4),(-0.00286833998593498,
0.477902879786539),(0.0665898698862505,0.073171619874851),.UNSPECIFIED.);
#2358=B_SPLINE_SURFACE_WITH_KNOTS('',3,3,((#73030,#73031,#73032,#73033),
(#73034,#73035,#73036,#73037),(#73038,#73039,#73040,#73041),(#73042,#73043,
#73044,#73045)),.UNSPECIFIED.,.F.,.F.,.F.,(4,4),(4,4),(0.52209712020883,
1.00286791825528),(0.0600156865486942,0.0665898700060142),.UNSPECIFIED.);
#2359=B_SPLINE_SURFACE_WITH_KNOTS('',3,3,((#73055,#73056,#73057,#73058),
(#73059,#73060,#73061,#73062),(#73063,#73064,#73065,#73066),(#73067,#73068,
#73069,#73070)),.UNSPECIFIED.,.F.,.F.,.F.,(4,4),(4,4),(-0.00286764392029753,
0.47790287978651),(0.0565997133101198,0.0631721430887059),.UNSPECIFIED.);
#2360=B_SPLINE_SURFACE_WITH_KNOTS('',3,3,((#73104,#73105,#73106,#73107),
(#73108,#73109,#73110,#73111),(#73112,#73113,#73114,#73115),(#73116,#73117,
#73118,#73119)),.UNSPECIFIED.,.F.,.F.,.F.,(4,4),(4,4),(0.522097120209604,
1.0028678012218),(0.0500263550858673,0.0565997133101429),.UNSPECIFIED.);
#2361=B_SPLINE_SURFACE_WITH_KNOTS('',3,3,((#73127,#73128,#73129,#73130),
(#73131,#73132,#73133,#73134),(#73135,#73136,#73137,#73138),(#73139,#73140,
#73141,#73142)),.UNSPECIFIED.,.F.,.F.,.F.,(4,4),(4,4),(-0.00286810177351708,
0.477902879786512),(0.0466073985929107,0.0531834933545498),
 .UNSPECIFIED.);
#2362=B_SPLINE_SURFACE_WITH_KNOTS('',3,3,((#73198,#73199,#73200,#73201),
(#73202,#73203,#73204,#73205),(#73206,#73207,#73208,#73209),(#73210,#73211,
#73212,#73213)),.UNSPECIFIED.,.F.,.F.,.F.,(4,4),(4,4),(0.522097120209231,
1.00286848452578),(0.0400218729465709,0.0466073985929455),.UNSPECIFIED.);
#2363=B_SPLINE_SURFACE_WITH_KNOTS('',3,3,((#73282,#73283,#73284,#73285),
(#73286,#73287,#73288,#73289),(#73290,#73291,#73292,#73293),(#73294,#73295,
#73296,#73297)),.UNSPECIFIED.,.F.,.F.,.F.,(4,4),(4,4),(0.522097120208532,
1.00286862201161),(0.0300094532292161,0.0365944846647031),.UNSPECIFIED.);
#2364=B_SPLINE_SURFACE_WITH_KNOTS('',3,3,((#73330,#73331,#73332,#73333),
(#73334,#73335,#73336,#73337),(#73338,#73339,#73340,#73341),(#73342,#73343,
#73344,#73345)),.UNSPECIFIED.,.F.,.F.,.F.,(4,4),(4,4),(-0.00600003961854877,
1.0000000024688),(0.0166015299238285,0.0265907346180647),.UNSPECIFIED.);
#2365=B_SPLINE_SURFACE_WITH_KNOTS('',3,3,((#73357,#73358,#73359,#73360),
(#73361,#73362,#73363,#73364),(#73365,#73366,#73367,#73368),(#73369,#73370,
#73371,#73372)),.UNSPECIFIED.,.F.,.F.,.F.,(4,4),(4,4),(0.522097120209233,
1.00286780410459),(0.020017522964652,0.026590734618065),.UNSPECIFIED.);
#2366=B_SPLINE_SURFACE_WITH_KNOTS('',3,3,((#73428,#73429,#73430,#73431),
(#73432,#73433,#73434,#73435),(#73436,#73437,#73438,#73439),(#73440,#73441,
#73442,#73443)),.UNSPECIFIED.,.F.,.F.,.F.,(4,4),(4,4),(0.522097120209193,
1.00286791014268),(0.0100271466749299,0.0166015302184267),.UNSPECIFIED.);
#2367=B_SPLINE_SURFACE_WITH_KNOTS('',3,3,((#73469,#73470,#73471,#73472),
(#73473,#73474,#73475,#73476),(#73477,#73478,#73479,#73480),(#73481,#73482,
#73483,#73484)),.UNSPECIFIED.,.F.,.F.,.F.,(4,4),(4,4),(-0.000171895441178554,
1.00600020634866),(0.0665898698856039,0.0751325481190739),.UNSPECIFIED.);
#2368=B_SPLINE_SURFACE_WITH_KNOTS('',3,3,((#73500,#73501,#73502,#73503),
(#73504,#73505,#73506,#73507),(#73508,#73509,#73510,#73511),(#73512,#73513,
#73514,#73515)),.UNSPECIFIED.,.F.,.F.,.F.,(4,4),(4,4),(-0.00286833998589992,
0.477902879786536),(0.066589869886251,0.0731716198748508),.UNSPECIFIED.);
#2369=B_SPLINE_SURFACE_WITH_KNOTS('',3,3,((#73549,#73550,#73551,#73552),
(#73553,#73554,#73555,#73556),(#73557,#73558,#73559,#73560),(#73561,#73562,
#73563,#73564)),.UNSPECIFIED.,.F.,.F.,.F.,(4,4),(4,4),(0.522097120208903,
1.00286791825528),(0.0600156865486934,0.0665898700060148),.UNSPECIFIED.);
#2370=B_SPLINE_SURFACE_WITH_KNOTS('',3,3,((#73574,#73575,#73576,#73577),
(#73578,#73579,#73580,#73581),(#73582,#73583,#73584,#73585),(#73586,#73587,
#73588,#73589)),.UNSPECIFIED.,.F.,.F.,.F.,(4,4),(4,4),(-0.00286764392025972,
0.477902879786554),(0.0565997133101205,0.0631721430887069),
 .UNSPECIFIED.);
#2371=B_SPLINE_SURFACE_WITH_KNOTS('',3,3,((#73626,#73627,#73628,#73629),
(#73630,#73631,#73632,#73633),(#73634,#73635,#73636,#73637),(#73638,#73639,
#73640,#73641)),.UNSPECIFIED.,.F.,.F.,.F.,(4,4),(4,4),(0.52209712020971,
1.00286780122195),(0.0500263550858671,0.0565997133101426),.UNSPECIFIED.);
#2372=B_SPLINE_SURFACE_WITH_KNOTS('',3,3,((#73713,#73714,#73715,#73716),
(#73717,#73718,#73719,#73720),(#73721,#73722,#73723,#73724),(#73725,#73726,
#73727,#73728)),.UNSPECIFIED.,.F.,.F.,.F.,(4,4),(4,4),(0.522097120209253,
1.0028684845256),(0.0400218729465702,0.046607398592945),.UNSPECIFIED.);
#2373=B_SPLINE_SURFACE_WITH_KNOTS('',3,3,((#73797,#73798,#73799,#73800),
(#73801,#73802,#73803,#73804),(#73805,#73806,#73807,#73808),(#73809,#73810,
#73811,#73812)),.UNSPECIFIED.,.F.,.F.,.F.,(4,4),(4,4),(0.52209712020847,
1.00286862201149),(0.0300094532292159,0.0365944846647042),.UNSPECIFIED.);
#2374=B_SPLINE_SURFACE_WITH_KNOTS('',3,3,((#73845,#73846,#73847,#73848),
(#73849,#73850,#73851,#73852),(#73853,#73854,#73855,#73856),(#73857,#73858,
#73859,#73860)),.UNSPECIFIED.,.F.,.F.,.F.,(4,4),(4,4),(-0.00600003961872756,
1.00000000246921),(0.0166015299238287,0.026590734618063),.UNSPECIFIED.);
#2375=B_SPLINE_SURFACE_WITH_KNOTS('',3,3,((#73872,#73873,#73874,#73875),
(#73876,#73877,#73878,#73879),(#73880,#73881,#73882,#73883),(#73884,#73885,
#73886,#73887)),.UNSPECIFIED.,.F.,.F.,.F.,(4,4),(4,4),(0.522097120209441,
1.00286780410464),(0.0200175229646508,0.0265907346180652),.UNSPECIFIED.);
#2376=B_SPLINE_SURFACE_WITH_KNOTS('',3,3,((#73943,#73944,#73945,#73946),
(#73947,#73948,#73949,#73950),(#73951,#73952,#73953,#73954),(#73955,#73956,
#73957,#73958)),.UNSPECIFIED.,.F.,.F.,.F.,(4,4),(4,4),(0.522097120209274,
1.00286791014271),(0.0100271466749308,0.0166015302184272),.UNSPECIFIED.);
#2377=B_SPLINE_SURFACE_WITH_KNOTS('',3,3,((#73984,#73985,#73986,#73987),
(#73988,#73989,#73990,#73991),(#73992,#73993,#73994,#73995),(#73996,#73997,
#73998,#73999)),.UNSPECIFIED.,.F.,.F.,.F.,(4,4),(4,4),(-0.000171895440844185,
1.00600020634819),(0.0665898698856036,0.0751325481187421),.UNSPECIFIED.);
#2378=B_SPLINE_SURFACE_WITH_KNOTS('',3,3,((#74015,#74016,#74017,#74018),
(#74019,#74020,#74021,#74022),(#74023,#74024,#74025,#74026),(#74027,#74028,
#74029,#74030)),.UNSPECIFIED.,.F.,.F.,.F.,(4,4),(4,4),(-0.00286833998589259,
0.477902879786537),(0.0665898698862502,0.0731716198748502),
 .UNSPECIFIED.);
#2379=B_SPLINE_SURFACE_WITH_KNOTS('',3,3,((#74064,#74065,#74066,#74067),
(#74068,#74069,#74070,#74071),(#74072,#74073,#74074,#74075),(#74076,#74077,
#74078,#74079)),.UNSPECIFIED.,.F.,.F.,.F.,(4,4),(4,4),(0.522097120208998,
1.0028679182553),(0.0600156865486937,0.0665898700060142),.UNSPECIFIED.);
#2380=B_SPLINE_SURFACE_WITH_KNOTS('',3,3,((#74089,#74090,#74091,#74092),
(#74093,#74094,#74095,#74096),(#74097,#74098,#74099,#74100),(#74101,#74102,
#74103,#74104)),.UNSPECIFIED.,.F.,.F.,.F.,(4,4),(4,4),(-0.00286764392026813,
0.477902879786526),(0.0565997133101208,0.0631721430887064),
 .UNSPECIFIED.);
#2381=B_SPLINE_SURFACE_WITH_KNOTS('',3,3,((#74141,#74142,#74143,#74144),
(#74145,#74146,#74147,#74148),(#74149,#74150,#74151,#74152),(#74153,#74154,
#74155,#74156)),.UNSPECIFIED.,.F.,.F.,.F.,(4,4),(4,4),(0.522097120209777,
1.00286780122189),(0.0500263550858672,0.0565997133101431),.UNSPECIFIED.);
#2382=B_SPLINE_SURFACE_WITH_KNOTS('',3,3,((#74228,#74229,#74230,#74231),
(#74232,#74233,#74234,#74235),(#74236,#74237,#74238,#74239),(#74240,#74241,
#74242,#74243)),.UNSPECIFIED.,.F.,.F.,.F.,(4,4),(4,4),(0.522097120209504,
1.00286848452574),(0.0400218729465704,0.046607398592945),.UNSPECIFIED.);
#2383=B_SPLINE_SURFACE_WITH_KNOTS('',3,3,((#74312,#74313,#74314,#74315),
(#74316,#74317,#74318,#74319),(#74320,#74321,#74322,#74323),(#74324,#74325,
#74326,#74327)),.UNSPECIFIED.,.F.,.F.,.F.,(4,4),(4,4),(0.52209712020866,
1.00286862201146),(0.0300094532292161,0.0365944846647038),.UNSPECIFIED.);
#2384=B_SPLINE_SURFACE_WITH_KNOTS('',3,3,((#74360,#74361,#74362,#74363),
(#74364,#74365,#74366,#74367),(#74368,#74369,#74370,#74371),(#74372,#74373,
#74374,#74375)),.UNSPECIFIED.,.F.,.F.,.F.,(4,4),(4,4),(-0.00600003961858661,
1.00000000246924),(0.0166015299238286,0.0265907346180638),.UNSPECIFIED.);
#2385=B_SPLINE_SURFACE_WITH_KNOTS('',3,3,((#74387,#74388,#74389,#74390),
(#74391,#74392,#74393,#74394),(#74395,#74396,#74397,#74398),(#74399,#74400,
#74401,#74402)),.UNSPECIFIED.,.F.,.F.,.F.,(4,4),(4,4),(0.522097120209524,
1.00286780410468),(0.020017522964651,0.0265907346180651),.UNSPECIFIED.);
#2386=B_SPLINE_SURFACE_WITH_KNOTS('',3,3,((#74458,#74459,#74460,#74461),
(#74462,#74463,#74464,#74465),(#74466,#74467,#74468,#74469),(#74470,#74471,
#74472,#74473)),.UNSPECIFIED.,.F.,.F.,.F.,(4,4),(4,4),(0.522097120209415,
1.00286791014287),(0.0100271466749306,0.0166015302184268),.UNSPECIFIED.);
#2387=B_SPLINE_SURFACE_WITH_KNOTS('',3,3,((#74499,#74500,#74501,#74502),
(#74503,#74504,#74505,#74506),(#74507,#74508,#74509,#74510),(#74511,#74512,
#74513,#74514)),.UNSPECIFIED.,.F.,.F.,.F.,(4,4),(4,4),(-0.000171895440408026,
1.0060002063483),(0.0665898698856056,0.0751325481183052),.UNSPECIFIED.);
#2388=B_SPLINE_SURFACE_WITH_KNOTS('',3,3,((#74530,#74531,#74532,#74533),
(#74534,#74535,#74536,#74537),(#74538,#74539,#74540,#74541),(#74542,#74543,
#74544,#74545)),.UNSPECIFIED.,.F.,.F.,.F.,(4,4),(4,4),(-0.00286833998588494,
0.477902879786516),(0.0665898698862518,0.0731716198748496),
 .UNSPECIFIED.);
#2389=B_SPLINE_SURFACE_WITH_KNOTS('',3,3,((#74579,#74580,#74581,#74582),
(#74583,#74584,#74585,#74586),(#74587,#74588,#74589,#74590),(#74591,#74592,
#74593,#74594)),.UNSPECIFIED.,.F.,.F.,.F.,(4,4),(4,4),(0.522097120209113,
1.00286791825532),(0.0600156865486933,0.066589870006014),.UNSPECIFIED.);
#2390=B_SPLINE_SURFACE_WITH_KNOTS('',3,3,((#74604,#74605,#74606,#74607),
(#74608,#74609,#74610,#74611),(#74612,#74613,#74614,#74615),(#74616,#74617,
#74618,#74619)),.UNSPECIFIED.,.F.,.F.,.F.,(4,4),(4,4),(-0.00286764392025136,
0.47790287978653),(0.0565997133101204,0.0631721430887062),.UNSPECIFIED.);
#2391=B_SPLINE_SURFACE_WITH_KNOTS('',3,3,((#74656,#74657,#74658,#74659),
(#74660,#74661,#74662,#74663),(#74664,#74665,#74666,#74667),(#74668,#74669,
#74670,#74671)),.UNSPECIFIED.,.F.,.F.,.F.,(4,4),(4,4),(0.52209712020994,
1.0028678012219),(0.0500263550858669,0.0565997133101416),.UNSPECIFIED.);
#2392=B_SPLINE_SURFACE_WITH_KNOTS('',3,3,((#74743,#74744,#74745,#74746),
(#74747,#74748,#74749,#74750),(#74751,#74752,#74753,#74754),(#74755,#74756,
#74757,#74758)),.UNSPECIFIED.,.F.,.F.,.F.,(4,4),(4,4),(0.522097120209583,
1.00286848452588),(0.0400218729465702,0.0466073985929453),.UNSPECIFIED.);
#2393=B_SPLINE_SURFACE_WITH_KNOTS('',3,3,((#74827,#74828,#74829,#74830),
(#74831,#74832,#74833,#74834),(#74835,#74836,#74837,#74838),(#74839,#74840,
#74841,#74842)),.UNSPECIFIED.,.F.,.F.,.F.,(4,4),(4,4),(0.522097120208653,
1.0028686220115),(0.0300094532292165,0.0365944846647038),.UNSPECIFIED.);
#2394=B_SPLINE_SURFACE_WITH_KNOTS('',3,3,((#74875,#74876,#74877,#74878),
(#74879,#74880,#74881,#74882),(#74883,#74884,#74885,#74886),(#74887,#74888,
#74889,#74890)),.UNSPECIFIED.,.F.,.F.,.F.,(4,4),(4,4),(-0.00600003961854107,
1.00000000246902),(0.0166015299238288,0.0265907346180632),.UNSPECIFIED.);
#2395=B_SPLINE_SURFACE_WITH_KNOTS('',3,3,((#74902,#74903,#74904,#74905),
(#74906,#74907,#74908,#74909),(#74910,#74911,#74912,#74913),(#74914,#74915,
#74916,#74917)),.UNSPECIFIED.,.F.,.F.,.F.,(4,4),(4,4),(0.522097120209538,
1.00286780410455),(0.0200175229646514,0.0265907346180652),.UNSPECIFIED.);
#2396=B_SPLINE_SURFACE_WITH_KNOTS('',3,3,((#74973,#74974,#74975,#74976),
(#74977,#74978,#74979,#74980),(#74981,#74982,#74983,#74984),(#74985,#74986,
#74987,#74988)),.UNSPECIFIED.,.F.,.F.,.F.,(4,4),(4,4),(0.522097120209429,
1.00286791014269),(0.0100271466749311,0.0166015302184276),.UNSPECIFIED.);
#2397=B_SPLINE_SURFACE_WITH_KNOTS('',3,3,((#75014,#75015,#75016,#75017),
(#75018,#75019,#75020,#75021),(#75022,#75023,#75024,#75025),(#75026,#75027,
#75028,#75029)),.UNSPECIFIED.,.F.,.F.,.F.,(4,4),(4,4),(-0.000171895439675098,
1.00600020634843),(0.0665898698856039,0.0751325481175709),.UNSPECIFIED.);
#2398=B_SPLINE_SURFACE_WITH_KNOTS('',3,3,((#75045,#75046,#75047,#75048),
(#75049,#75050,#75051,#75052),(#75053,#75054,#75055,#75056),(#75057,#75058,
#75059,#75060)),.UNSPECIFIED.,.F.,.F.,.F.,(4,4),(4,4),(-0.00286833998592894,
0.477902879786575),(0.0665898698862504,0.0731716198748503),
 .UNSPECIFIED.);
#2399=B_SPLINE_SURFACE_WITH_KNOTS('',3,3,((#75094,#75095,#75096,#75097),
(#75098,#75099,#75100,#75101),(#75102,#75103,#75104,#75105),(#75106,#75107,
#75108,#75109)),.UNSPECIFIED.,.F.,.F.,.F.,(4,4),(4,4),(0.52209712020939,
1.00286791825516),(0.0600156865486937,0.0665898700060151),.UNSPECIFIED.);
#2400=B_SPLINE_SURFACE_WITH_KNOTS('',3,3,((#75119,#75120,#75121,#75122),
(#75123,#75124,#75125,#75126),(#75127,#75128,#75129,#75130),(#75131,#75132,
#75133,#75134)),.UNSPECIFIED.,.F.,.F.,.F.,(4,4),(4,4),(-0.00286764392024561,
0.47790287978655),(0.0565997133101205,0.0631721430887062),.UNSPECIFIED.);
#2401=B_SPLINE_SURFACE_WITH_KNOTS('',3,3,((#75171,#75172,#75173,#75174),
(#75175,#75176,#75177,#75178),(#75179,#75180,#75181,#75182),(#75183,#75184,
#75185,#75186)),.UNSPECIFIED.,.F.,.F.,.F.,(4,4),(4,4),(0.522097120210138,
1.00286780122168),(0.0500263550858672,0.0565997133101423),.UNSPECIFIED.);
#2402=B_SPLINE_SURFACE_WITH_KNOTS('',3,3,((#75258,#75259,#75260,#75261),
(#75262,#75263,#75264,#75265),(#75266,#75267,#75268,#75269),(#75270,#75271,
#75272,#75273)),.UNSPECIFIED.,.F.,.F.,.F.,(4,4),(4,4),(0.522097120209848,
1.00286848452586),(0.0400218729465692,0.0466073985929449),.UNSPECIFIED.);
#2403=B_SPLINE_SURFACE_WITH_KNOTS('',3,3,((#75342,#75343,#75344,#75345),
(#75346,#75347,#75348,#75349),(#75350,#75351,#75352,#75353),(#75354,#75355,
#75356,#75357)),.UNSPECIFIED.,.F.,.F.,.F.,(4,4),(4,4),(0.52209712020886,
1.00286862201148),(0.0300094532292159,0.0365944846647037),.UNSPECIFIED.);
#2404=B_SPLINE_SURFACE_WITH_KNOTS('',3,3,((#75390,#75391,#75392,#75393),
(#75394,#75395,#75396,#75397),(#75398,#75399,#75400,#75401),(#75402,#75403,
#75404,#75405)),.UNSPECIFIED.,.F.,.F.,.F.,(4,4),(4,4),(-0.00600003961852695,
1.0000000024693),(0.0166015299238276,0.0265907346180643),.UNSPECIFIED.);
#2405=B_SPLINE_SURFACE_WITH_KNOTS('',3,3,((#75417,#75418,#75419,#75420),
(#75421,#75422,#75423,#75424),(#75425,#75426,#75427,#75428),(#75429,#75430,
#75431,#75432)),.UNSPECIFIED.,.F.,.F.,.F.,(4,4),(4,4),(0.522097120209692,
1.00286780410451),(0.0200175229646511,0.0265907346180654),.UNSPECIFIED.);
#2406=B_SPLINE_SURFACE_WITH_KNOTS('',3,3,((#75488,#75489,#75490,#75491),
(#75492,#75493,#75494,#75495),(#75496,#75497,#75498,#75499),(#75500,#75501,
#75502,#75503)),.UNSPECIFIED.,.F.,.F.,.F.,(4,4),(4,4),(0.522097120209553,
1.00286791014263),(0.0100271466749314,0.0166015302184278),.UNSPECIFIED.);
#2407=B_SPLINE_SURFACE_WITH_KNOTS('',3,3,((#75529,#75530,#75531,#75532),
(#75533,#75534,#75535,#75536),(#75537,#75538,#75539,#75540),(#75541,#75542,
#75543,#75544)),.UNSPECIFIED.,.F.,.F.,.F.,(4,4),(4,4),(-0.000171895438814887,
1.00600020634805),(0.0665898698856055,0.0751325481167114),.UNSPECIFIED.);
#2408=B_SPLINE_SURFACE_WITH_KNOTS('',3,3,((#75560,#75561,#75562,#75563),
(#75564,#75565,#75566,#75567),(#75568,#75569,#75570,#75571),(#75572,#75573,
#75574,#75575)),.UNSPECIFIED.,.F.,.F.,.F.,(4,4),(4,4),(-0.00286833998585249,
0.477902879786554),(0.0665898698862516,0.0731716198748504),
 .UNSPECIFIED.);
#2409=B_SPLINE_SURFACE_WITH_KNOTS('',3,3,((#75609,#75610,#75611,#75612),
(#75613,#75614,#75615,#75616),(#75617,#75618,#75619,#75620),(#75621,#75622,
#75623,#75624)),.UNSPECIFIED.,.F.,.F.,.F.,(4,4),(4,4),(0.522097120209408,
1.00286791825511),(0.0600156865486939,0.0665898700060147),.UNSPECIFIED.);
#2410=B_SPLINE_SURFACE_WITH_KNOTS('',3,3,((#75634,#75635,#75636,#75637),
(#75638,#75639,#75640,#75641),(#75642,#75643,#75644,#75645),(#75646,#75647,
#75648,#75649)),.UNSPECIFIED.,.F.,.F.,.F.,(4,4),(4,4),(-0.00286764392030078,
0.477902879786555),(0.0565997133101203,0.0631721430887069),
 .UNSPECIFIED.);
#2411=B_SPLINE_SURFACE_WITH_KNOTS('',3,3,((#75683,#75684,#75685,#75686),
(#75687,#75688,#75689,#75690),(#75691,#75692,#75693,#75694),(#75695,#75696,
#75697,#75698)),.UNSPECIFIED.,.F.,.F.,.F.,(4,4),(4,4),(0.522097120210099,
1.00286780122183),(0.050026355085867,0.0565997133101419),.UNSPECIFIED.);
#2412=B_SPLINE_SURFACE_WITH_KNOTS('',3,3,((#75706,#75707,#75708,#75709),
(#75710,#75711,#75712,#75713),(#75714,#75715,#75716,#75717),(#75718,#75719,
#75720,#75721)),.UNSPECIFIED.,.F.,.F.,.F.,(4,4),(4,4),(-0.00286810177325765,
0.477902879786541),(0.0466073985929107,0.05318349335455),.UNSPECIFIED.);
#2413=B_SPLINE_SURFACE_WITH_KNOTS('',3,3,((#75777,#75778,#75779,#75780),
(#75781,#75782,#75783,#75784),(#75785,#75786,#75787,#75788),(#75789,#75790,
#75791,#75792)),.UNSPECIFIED.,.F.,.F.,.F.,(4,4),(4,4),(0.522097120209848,
1.00286848452562),(0.0400218729465703,0.0466073985929447),.UNSPECIFIED.);
#2414=B_SPLINE_SURFACE_WITH_KNOTS('',3,3,((#75861,#75862,#75863,#75864),
(#75865,#75866,#75867,#75868),(#75869,#75870,#75871,#75872),(#75873,#75874,
#75875,#75876)),.UNSPECIFIED.,.F.,.F.,.F.,(4,4),(4,4),(0.522097120209105,
1.00286862201146),(0.0300094532292165,0.0365944846647027),.UNSPECIFIED.);
#2415=B_SPLINE_SURFACE_WITH_KNOTS('',3,3,((#75909,#75910,#75911,#75912),
(#75913,#75914,#75915,#75916),(#75917,#75918,#75919,#75920),(#75921,#75922,
#75923,#75924)),.UNSPECIFIED.,.F.,.F.,.F.,(4,4),(4,4),(-0.006000039618303,
1.00000000246901),(0.0166015299238286,0.026590734618064),.UNSPECIFIED.);
#2416=B_SPLINE_SURFACE_WITH_KNOTS('',3,3,((#75936,#75937,#75938,#75939),
(#75940,#75941,#75942,#75943),(#75944,#75945,#75946,#75947),(#75948,#75949,
#75950,#75951)),.UNSPECIFIED.,.F.,.F.,.F.,(4,4),(4,4),(0.522097120209899,
1.00286780410473),(0.0200175229646523,0.0265907346180642),.UNSPECIFIED.);
#2417=B_SPLINE_SURFACE_WITH_KNOTS('',3,3,((#76007,#76008,#76009,#76010),
(#76011,#76012,#76013,#76014),(#76015,#76016,#76017,#76018),(#76019,#76020,
#76021,#76022)),.UNSPECIFIED.,.F.,.F.,.F.,(4,4),(4,4),(0.5220971202096,
1.00286791014285),(0.0100271466749314,0.0166015302184275),.UNSPECIFIED.);
#2418=B_SPLINE_SURFACE_WITH_KNOTS('',3,3,((#76048,#76049,#76050,#76051),
(#76052,#76053,#76054,#76055),(#76056,#76057,#76058,#76059),(#76060,#76061,
#76062,#76063)),.UNSPECIFIED.,.F.,.F.,.F.,(4,4),(4,4),(-0.000171895438212527,
1.00600020634832),(0.0665898698856039,0.0751325481161105),.UNSPECIFIED.);
#2419=B_SPLINE_SURFACE_WITH_KNOTS('',3,3,((#76079,#76080,#76081,#76082),
(#76083,#76084,#76085,#76086),(#76087,#76088,#76089,#76090),(#76091,#76092,
#76093,#76094)),.UNSPECIFIED.,.F.,.F.,.F.,(4,4),(4,4),(-0.00286833998582986,
0.477902879786545),(0.0665898698862504,0.0731716198748493),
 .UNSPECIFIED.);
#2420=B_SPLINE_SURFACE_WITH_KNOTS('',3,3,((#76128,#76129,#76130,#76131),
(#76132,#76133,#76134,#76135),(#76136,#76137,#76138,#76139),(#76140,#76141,
#76142,#76143)),.UNSPECIFIED.,.F.,.F.,.F.,(4,4),(4,4),(0.522097120209601,
1.00286791825518),(0.060015686548695,0.0665898700060147),.UNSPECIFIED.);
#2421=B_SPLINE_SURFACE_WITH_KNOTS('',3,3,((#76153,#76154,#76155,#76156),
(#76157,#76158,#76159,#76160),(#76161,#76162,#76163,#76164),(#76165,#76166,
#76167,#76168)),.UNSPECIFIED.,.F.,.F.,.F.,(4,4),(4,4),(-0.00286764392023406,
0.477902879786583),(0.0565997133101206,0.0631721430887068),
 .UNSPECIFIED.);
#2422=B_SPLINE_SURFACE_WITH_KNOTS('',3,3,((#76205,#76206,#76207,#76208),
(#76209,#76210,#76211,#76212),(#76213,#76214,#76215,#76216),(#76217,#76218,
#76219,#76220)),.UNSPECIFIED.,.F.,.F.,.F.,(4,4),(4,4),(0.522097120210378,
1.00286780122182),(0.0500263550858676,0.0565997133101427),.UNSPECIFIED.);
#2423=B_SPLINE_SURFACE_WITH_KNOTS('',3,3,((#76253,#76254,#76255,#76256),
(#76257,#76258,#76259,#76260),(#76261,#76262,#76263,#76264),(#76265,#76266,
#76267,#76268)),.UNSPECIFIED.,.F.,.F.,.F.,(4,4),(4,4),(-0.0060001464356663,
1.),(0.0365944846640624,0.0466073985929451),.UNSPECIFIED.);
#2424=B_SPLINE_SURFACE_WITH_KNOTS('',3,3,((#76291,#76292,#76293,#76294),
(#76295,#76296,#76297,#76298),(#76299,#76300,#76301,#76302),(#76303,#76304,
#76305,#76306)),.UNSPECIFIED.,.F.,.F.,.F.,(4,4),(4,4),(0.522097120210012,
1.0028684845257),(0.0400218729465707,0.0466073985929451),.UNSPECIFIED.);
#2425=B_SPLINE_SURFACE_WITH_KNOTS('',3,3,((#76370,#76371,#76372,#76373),
(#76374,#76375,#76376,#76377),(#76378,#76379,#76380,#76381),(#76382,#76383,
#76384,#76385)),.UNSPECIFIED.,.F.,.F.,.F.,(4,4),(4,4),(0.522097120209054,
1.00286862201138),(0.0300094532292158,0.0365944846647039),.UNSPECIFIED.);
#2426=B_SPLINE_SURFACE_WITH_KNOTS('',3,3,((#76418,#76419,#76420,#76421),
(#76422,#76423,#76424,#76425),(#76426,#76427,#76428,#76429),(#76430,#76431,
#76432,#76433)),.UNSPECIFIED.,.F.,.F.,.F.,(4,4),(4,4),(-0.00600003961845795,
1.00000000246918),(0.0166015299238286,0.0265907346180636),.UNSPECIFIED.);
#2427=B_SPLINE_SURFACE_WITH_KNOTS('',3,3,((#76445,#76446,#76447,#76448),
(#76449,#76450,#76451,#76452),(#76453,#76454,#76455,#76456),(#76457,#76458,
#76459,#76460)),.UNSPECIFIED.,.F.,.F.,.F.,(4,4),(4,4),(0.522097120210085,
1.0028678041046),(0.0200175229646512,0.026590734618065),.UNSPECIFIED.);
#2428=B_SPLINE_SURFACE_WITH_KNOTS('',3,3,((#76516,#76517,#76518,#76519),
(#76520,#76521,#76522,#76523),(#76524,#76525,#76526,#76527),(#76528,#76529,
#76530,#76531)),.UNSPECIFIED.,.F.,.F.,.F.,(4,4),(4,4),(0.522097120209799,
1.00286791014274),(0.0100271466749313,0.0166015302184278),.UNSPECIFIED.);
#2429=B_SPLINE_SURFACE_WITH_KNOTS('',3,3,((#76557,#76558,#76559,#76560),
(#76561,#76562,#76563,#76564),(#76565,#76566,#76567,#76568),(#76569,#76570,
#76571,#76572)),.UNSPECIFIED.,.F.,.F.,.F.,(4,4),(4,4),(-0.000171895437403129,
1.00600020634821),(0.0665898698856045,0.0751325481152999),.UNSPECIFIED.);
#2430=B_SPLINE_SURFACE_WITH_KNOTS('',3,3,((#76588,#76589,#76590,#76591),
(#76592,#76593,#76594,#76595),(#76596,#76597,#76598,#76599),(#76600,#76601,
#76602,#76603)),.UNSPECIFIED.,.F.,.F.,.F.,(4,4),(4,4),(-0.00286833998592427,
0.477902879786586),(0.0665898698862519,0.0731716198748508),
 .UNSPECIFIED.);
#2431=B_SPLINE_SURFACE_WITH_KNOTS('',3,3,((#76637,#76638,#76639,#76640),
(#76641,#76642,#76643,#76644),(#76645,#76646,#76647,#76648),(#76649,#76650,
#76651,#76652)),.UNSPECIFIED.,.F.,.F.,.F.,(4,4),(4,4),(0.522097120209579,
1.00286791825534),(0.0600156865486934,0.0665898700060136),.UNSPECIFIED.);
#2432=B_SPLINE_SURFACE_WITH_KNOTS('',3,3,((#76662,#76663,#76664,#76665),
(#76666,#76667,#76668,#76669),(#76670,#76671,#76672,#76673),(#76674,#76675,
#76676,#76677)),.UNSPECIFIED.,.F.,.F.,.F.,(4,4),(4,4),(-0.00286764392025056,
0.477902879786533),(0.0565997133101202,0.0631721430887066),
 .UNSPECIFIED.);
#2433=B_SPLINE_SURFACE_WITH_KNOTS('',3,3,((#76711,#76712,#76713,#76714),
(#76715,#76716,#76717,#76718),(#76719,#76720,#76721,#76722),(#76723,#76724,
#76725,#76726)),.UNSPECIFIED.,.F.,.F.,.F.,(4,4),(4,4),(0.522097120210524,
1.00286780122199),(0.0500263550858677,0.0565997133101438),.UNSPECIFIED.);
#2434=B_SPLINE_SURFACE_WITH_KNOTS('',3,3,((#76734,#76735,#76736,#76737),
(#76738,#76739,#76740,#76741),(#76742,#76743,#76744,#76745),(#76746,#76747,
#76748,#76749)),.UNSPECIFIED.,.F.,.F.,.F.,(4,4),(4,4),(-0.00286810177311321,
0.477902879786528),(0.0466073985929115,0.0531834933545508),
 .UNSPECIFIED.);
#2435=B_SPLINE_SURFACE_WITH_KNOTS('',3,3,((#76805,#76806,#76807,#76808),
(#76809,#76810,#76811,#76812),(#76813,#76814,#76815,#76816),(#76817,#76818,
#76819,#76820)),.UNSPECIFIED.,.F.,.F.,.F.,(4,4),(4,4),(0.522097120210016,
1.00286848452579),(0.0400218729465696,0.0466073985929448),.UNSPECIFIED.);
#2436=B_SPLINE_SURFACE_WITH_KNOTS('',3,3,((#76886,#76887,#76888,#76889),
(#76890,#76891,#76892,#76893),(#76894,#76895,#76896,#76897),(#76898,#76899,
#76900,#76901)),.UNSPECIFIED.,.F.,.F.,.F.,(4,4),(4,4),(0.522097120209344,
1.00286862201151),(0.0300094532292164,0.0365944846647039),.UNSPECIFIED.);
#2437=B_SPLINE_SURFACE_WITH_KNOTS('',3,3,((#76909,#76910,#76911,#76912),
(#76913,#76914,#76915,#76916),(#76917,#76918,#76919,#76920),(#76921,#76922,
#76923,#76924)),.UNSPECIFIED.,.F.,.F.,.F.,(4,4),(4,4),(-0.00286823045904117,
0.477902879786487),(0.0265907346180614,0.0331702036774536),
 .UNSPECIFIED.);
#2438=B_SPLINE_SURFACE_WITH_KNOTS('',3,3,((#76941,#76942,#76943,#76944),
(#76945,#76946,#76947,#76948),(#76949,#76950,#76951,#76952),(#76953,#76954,
#76955,#76956)),.UNSPECIFIED.,.F.,.F.,.F.,(4,4),(4,4),(-0.00600003962494949,
1.00000000356517),(0.0166015299238284,0.0265907346180641),.UNSPECIFIED.);
#2439=B_SPLINE_SURFACE_WITH_KNOTS('',3,3,((#76968,#76969,#76970,#76971),
(#76972,#76973,#76974,#76975),(#76976,#76977,#76978,#76979),(#76980,#76981,
#76982,#76983)),.UNSPECIFIED.,.F.,.F.,.F.,(4,4),(4,4),(0.522097120210132,
1.00286780410458),(0.0200175229646515,0.0265907346180646),.UNSPECIFIED.);
#2440=B_SPLINE_SURFACE_WITH_KNOTS('',3,3,((#77039,#77040,#77041,#77042),
(#77043,#77044,#77045,#77046),(#77047,#77048,#77049,#77050),(#77051,#77052,
#77053,#77054)),.UNSPECIFIED.,.F.,.F.,.F.,(4,4),(4,4),(0.522097120209969,
1.00286791014268),(0.0100271466749314,0.0166015302184277),.UNSPECIFIED.);
#2441=B_SPLINE_SURFACE_WITH_KNOTS('',3,3,((#77080,#77081,#77082,#77083),
(#77084,#77085,#77086,#77087),(#77088,#77089,#77090,#77091),(#77092,#77093,
#77094,#77095)),.UNSPECIFIED.,.F.,.F.,.F.,(4,4),(4,4),(-0.000171895436535362,
1.00600020634832),(0.0665898698856043,0.075132548114432),.UNSPECIFIED.);
#2442=B_SPLINE_SURFACE_WITH_KNOTS('',3,3,((#77111,#77112,#77113,#77114),
(#77115,#77116,#77117,#77118),(#77119,#77120,#77121,#77122),(#77123,#77124,
#77125,#77126)),.UNSPECIFIED.,.F.,.F.,.F.,(4,4),(4,4),(-0.00286833998596488,
0.477902879786617),(0.0665898698862506,0.0731716198748498),
 .UNSPECIFIED.);
#2443=B_SPLINE_SURFACE_WITH_KNOTS('',3,3,((#77160,#77161,#77162,#77163),
(#77164,#77165,#77166,#77167),(#77168,#77169,#77170,#77171),(#77172,#77173,
#77174,#77175)),.UNSPECIFIED.,.F.,.F.,.F.,(4,4),(4,4),(0.522097120209847,
1.00286791825524),(0.0600156865486933,0.0665898700060139),.UNSPECIFIED.);
#2444=B_SPLINE_SURFACE_WITH_KNOTS('',3,3,((#77185,#77186,#77187,#77188),
(#77189,#77190,#77191,#77192),(#77193,#77194,#77195,#77196),(#77197,#77198,
#77199,#77200)),.UNSPECIFIED.,.F.,.F.,.F.,(4,4),(4,4),(-0.00286764392028603,
0.477902879786574),(0.0565997133101217,0.063172143088707),.UNSPECIFIED.);
#2445=B_SPLINE_SURFACE_WITH_KNOTS('',3,3,((#77237,#77238,#77239,#77240),
(#77241,#77242,#77243,#77244),(#77245,#77246,#77247,#77248),(#77249,#77250,
#77251,#77252)),.UNSPECIFIED.,.F.,.F.,.F.,(4,4),(4,4),(0.522097120210472,
1.00286780122192),(0.0500263550858672,0.0565997133101425),.UNSPECIFIED.);
#2446=B_SPLINE_SURFACE_WITH_KNOTS('',3,3,((#77324,#77325,#77326,#77327),
(#77328,#77329,#77330,#77331),(#77332,#77333,#77334,#77335),(#77336,#77337,
#77338,#77339)),.UNSPECIFIED.,.F.,.F.,.F.,(4,4),(4,4),(0.522097120210281,
1.00286848452586),(0.0400218729465702,0.0466073985929454),.UNSPECIFIED.);
#2447=B_SPLINE_SURFACE_WITH_KNOTS('',3,3,((#77408,#77409,#77410,#77411),
(#77412,#77413,#77414,#77415),(#77416,#77417,#77418,#77419),(#77420,#77421,
#77422,#77423)),.UNSPECIFIED.,.F.,.F.,.F.,(4,4),(4,4),(0.522097120209377,
1.00286862201145),(0.0300094532292159,0.0365944846647033),.UNSPECIFIED.);
#2448=B_SPLINE_SURFACE_WITH_KNOTS('',3,3,((#77456,#77457,#77458,#77459),
(#77460,#77461,#77462,#77463),(#77464,#77465,#77466,#77467),(#77468,#77469,
#77470,#77471)),.UNSPECIFIED.,.F.,.F.,.F.,(4,4),(4,4),(-0.00600003960349703,
1.),(0.0166015299238287,0.0265907346180644),.UNSPECIFIED.);
#2449=B_SPLINE_SURFACE_WITH_KNOTS('',3,3,((#77483,#77484,#77485,#77486),
(#77487,#77488,#77489,#77490),(#77491,#77492,#77493,#77494),(#77495,#77496,
#77497,#77498)),.UNSPECIFIED.,.F.,.F.,.F.,(4,4),(4,4),(0.522097120210262,
1.00286780410451),(0.0200175229646517,0.0265907346180652),.UNSPECIFIED.);
#2450=B_SPLINE_SURFACE_WITH_KNOTS('',3,3,((#77506,#77507,#77508,#77509),
(#77510,#77511,#77512,#77513),(#77514,#77515,#77516,#77517),(#77518,#77519,
#77520,#77521)),.UNSPECIFIED.,.F.,.F.,.F.,(4,4),(4,4),(-0.00286753114042522,
0.477902879786509),(0.0166015299238958,0.0231736788090039),
 .UNSPECIFIED.);
#2451=B_SPLINE_SURFACE_WITH_KNOTS('',3,3,((#77561,#77562,#77563,#77564),
(#77565,#77566,#77567,#77568),(#77569,#77570,#77571,#77572),(#77573,#77574,
#77575,#77576)),.UNSPECIFIED.,.F.,.F.,.F.,(4,4),(4,4),(0.522097120210089,
1.00286791014277),(0.0100271466749312,0.0166015302184273),.UNSPECIFIED.);
#2452=B_SPLINE_SURFACE_WITH_KNOTS('',3,3,((#77602,#77603,#77604,#77605),
(#77606,#77607,#77608,#77609),(#77610,#77611,#77612,#77613),(#77614,#77615,
#77616,#77617)),.UNSPECIFIED.,.F.,.F.,.F.,(4,4),(4,4),(-0.000171895435626065,
1.00600020634828),(0.0665898698856039,0.0751325481135236),.UNSPECIFIED.);
#2453=B_SPLINE_SURFACE_WITH_KNOTS('',3,3,((#77633,#77634,#77635,#77636),
(#77637,#77638,#77639,#77640),(#77641,#77642,#77643,#77644),(#77645,#77646,
#77647,#77648)),.UNSPECIFIED.,.F.,.F.,.F.,(4,4),(4,4),(-0.00286833998592586,
0.477902879786536),(0.0665898698862503,0.0731716198748495),
 .UNSPECIFIED.);
#2454=B_SPLINE_SURFACE_WITH_KNOTS('',3,3,((#77682,#77683,#77684,#77685),
(#77686,#77687,#77688,#77689),(#77690,#77691,#77692,#77693),(#77694,#77695,
#77696,#77697)),.UNSPECIFIED.,.F.,.F.,.F.,(4,4),(4,4),(0.522097120209945,
1.0028679182552),(0.0600156865486939,0.0665898700060147),.UNSPECIFIED.);
#2455=B_SPLINE_SURFACE_WITH_KNOTS('',3,3,((#77707,#77708,#77709,#77710),
(#77711,#77712,#77713,#77714),(#77715,#77716,#77717,#77718),(#77719,#77720,
#77721,#77722)),.UNSPECIFIED.,.F.,.F.,.F.,(4,4),(4,4),(-0.00286764392026067,
0.477902879786611),(0.0565997133101195,0.0631721430887069),
 .UNSPECIFIED.);
#2456=B_SPLINE_SURFACE_WITH_KNOTS('',3,3,((#77759,#77760,#77761,#77762),
(#77763,#77764,#77765,#77766),(#77767,#77768,#77769,#77770),(#77771,#77772,
#77773,#77774)),.UNSPECIFIED.,.F.,.F.,.F.,(4,4),(4,4),(0.522097120210691,
1.00286780122204),(0.0500263550858657,0.0565997133101437),.UNSPECIFIED.);
#2457=B_SPLINE_SURFACE_WITH_KNOTS('',3,3,((#77846,#77847,#77848,#77849),
(#77850,#77851,#77852,#77853),(#77854,#77855,#77856,#77857),(#77858,#77859,
#77860,#77861)),.UNSPECIFIED.,.F.,.F.,.F.,(4,4),(4,4),(0.522097120210333,
1.00286848452579),(0.0400218729465701,0.0466073985929457),.UNSPECIFIED.);
#2458=B_SPLINE_SURFACE_WITH_KNOTS('',3,3,((#77930,#77931,#77932,#77933),
(#77934,#77935,#77936,#77937),(#77938,#77939,#77940,#77941),(#77942,#77943,
#77944,#77945)),.UNSPECIFIED.,.F.,.F.,.F.,(4,4),(4,4),(0.522097120209519,
1.00286862201157),(0.0300094532292161,0.0365944846647038),.UNSPECIFIED.);
#2459=B_SPLINE_SURFACE_WITH_KNOTS('',3,3,((#77978,#77979,#77980,#77981),
(#77982,#77983,#77984,#77985),(#77986,#77987,#77988,#77989),(#77990,#77991,
#77992,#77993)),.UNSPECIFIED.,.F.,.F.,.F.,(4,4),(4,4),(-0.0060000396247669,
1.00000000356511),(0.0166015299238272,0.0265907346180642),.UNSPECIFIED.);
#2460=B_SPLINE_SURFACE_WITH_KNOTS('',3,3,((#78005,#78006,#78007,#78008),
(#78009,#78010,#78011,#78012),(#78013,#78014,#78015,#78016),(#78017,#78018,
#78019,#78020)),.UNSPECIFIED.,.F.,.F.,.F.,(4,4),(4,4),(0.522097120210314,
1.00286780410453),(0.0200175229646511,0.0265907346180649),.UNSPECIFIED.);
#2461=B_SPLINE_SURFACE_WITH_KNOTS('',3,3,((#78073,#78074,#78075,#78076),
(#78077,#78078,#78079,#78080),(#78081,#78082,#78083,#78084),(#78085,#78086,
#78087,#78088)),.UNSPECIFIED.,.F.,.F.,.F.,(4,4),(4,4),(0.522097120210105,
1.0028679101425),(0.0100271466749325,0.0166015302184282),.UNSPECIFIED.);
#2462=B_SPLINE_SURFACE_WITH_KNOTS('',3,3,((#78096,#78097,#78098,#78099),
(#78100,#78101,#78102,#78103),(#78104,#78105,#78106,#78107),(#78108,#78109,
#78110,#78111)),.UNSPECIFIED.,.F.,.F.,.F.,(4,4),(4,4),(-0.00206901892618064,
0.346769728493059),(0.00660713154712627,0.0131849431469577),
 .UNSPECIFIED.);
#2463=B_SPLINE_SURFACE_WITH_KNOTS('',3,3,((#78121,#78122,#78123,#78124),
(#78125,#78126,#78127,#78128),(#78129,#78130,#78131,#78132),(#78133,#78134,
#78135,#78136)),.UNSPECIFIED.,.F.,.F.,.F.,(4,4),(4,4),(-0.000171895434855279,
1.00600020634832),(0.0665898698856049,0.0751325481127517),.UNSPECIFIED.);
#2464=B_SPLINE_SURFACE_WITH_KNOTS('',3,3,((#78152,#78153,#78154,#78155),
(#78156,#78157,#78158,#78159),(#78160,#78161,#78162,#78163),(#78164,#78165,
#78166,#78167)),.UNSPECIFIED.,.F.,.F.,.F.,(4,4),(4,4),(-0.00286833998594799,
0.477902879786575),(0.066589869886252,0.0731716198748501),.UNSPECIFIED.);
#2465=B_SPLINE_SURFACE_WITH_KNOTS('',3,3,((#78201,#78202,#78203,#78204),
(#78205,#78206,#78207,#78208),(#78209,#78210,#78211,#78212),(#78213,#78214,
#78215,#78216)),.UNSPECIFIED.,.F.,.F.,.F.,(4,4),(4,4),(0.522097120210037,
1.00286791825517),(0.0600156865486943,0.0665898700060142),.UNSPECIFIED.);
#2466=B_SPLINE_SURFACE_WITH_KNOTS('',3,3,((#78226,#78227,#78228,#78229),
(#78230,#78231,#78232,#78233),(#78234,#78235,#78236,#78237),(#78238,#78239,
#78240,#78241)),.UNSPECIFIED.,.F.,.F.,.F.,(4,4),(4,4),(-0.00286764392024655,
0.477902879786472),(0.0565997133101204,0.0631721430887056),
 .UNSPECIFIED.);
#2467=B_SPLINE_SURFACE_WITH_KNOTS('',3,3,((#78278,#78279,#78280,#78281),
(#78282,#78283,#78284,#78285),(#78286,#78287,#78288,#78289),(#78290,#78291,
#78292,#78293)),.UNSPECIFIED.,.F.,.F.,.F.,(4,4),(4,4),(0.522097120210844,
1.0028678012219),(0.050026355085867,0.0565997133101422),.UNSPECIFIED.);
#2468=B_SPLINE_SURFACE_WITH_KNOTS('',3,3,((#78365,#78366,#78367,#78368),
(#78369,#78370,#78371,#78372),(#78373,#78374,#78375,#78376),(#78377,#78378,
#78379,#78380)),.UNSPECIFIED.,.F.,.F.,.F.,(4,4),(4,4),(0.522097120210373,
1.00286848452577),(0.0400218729465708,0.0466073985929444),.UNSPECIFIED.);
#2469=B_SPLINE_SURFACE_WITH_KNOTS('',3,3,((#78449,#78450,#78451,#78452),
(#78453,#78454,#78455,#78456),(#78457,#78458,#78459,#78460),(#78461,#78462,
#78463,#78464)),.UNSPECIFIED.,.F.,.F.,.F.,(4,4),(4,4),(0.522097120209569,
1.0028686220114),(0.0300094532292161,0.0365944846647028),.UNSPECIFIED.);
#2470=B_SPLINE_SURFACE_WITH_KNOTS('',3,3,((#78497,#78498,#78499,#78500),
(#78501,#78502,#78503,#78504),(#78505,#78506,#78507,#78508),(#78509,#78510,
#78511,#78512)),.UNSPECIFIED.,.F.,.F.,.F.,(4,4),(4,4),(-0.00600003962476691,
1.00000000356515),(0.016601529923829,0.0265907346180638),.UNSPECIFIED.);
#2471=B_SPLINE_SURFACE_WITH_KNOTS('',3,3,((#78524,#78525,#78526,#78527),
(#78528,#78529,#78530,#78531),(#78532,#78533,#78534,#78535),(#78536,#78537,
#78538,#78539)),.UNSPECIFIED.,.F.,.F.,.F.,(4,4),(4,4),(0.522097120210578,
1.0028678041046),(0.0200175229646522,0.0265907346180645),.UNSPECIFIED.);
#2472=B_SPLINE_SURFACE_WITH_KNOTS('',3,3,((#78595,#78596,#78597,#78598),
(#78599,#78600,#78601,#78602),(#78603,#78604,#78605,#78606),(#78607,#78608,
#78609,#78610)),.UNSPECIFIED.,.F.,.F.,.F.,(4,4),(4,4),(0.52209712021034,
1.00286791014272),(0.0100271466749315,0.0166015302184262),.UNSPECIFIED.);
#2473=B_SPLINE_SURFACE_WITH_KNOTS('',3,3,((#78636,#78637,#78638,#78639),
(#78640,#78641,#78642,#78643),(#78644,#78645,#78646,#78647),(#78648,#78649,
#78650,#78651)),.UNSPECIFIED.,.F.,.F.,.F.,(4,4),(4,4),(-0.000171895433735589,
1.00600020634835),(0.0665898698856037,0.0751325481116349),.UNSPECIFIED.);
#2474=B_SPLINE_SURFACE_WITH_KNOTS('',3,3,((#78667,#78668,#78669,#78670),
(#78671,#78672,#78673,#78674),(#78675,#78676,#78677,#78678),(#78679,#78680,
#78681,#78682)),.UNSPECIFIED.,.F.,.F.,.F.,(4,4),(4,4),(-0.00286833998586006,
0.477902879786518),(0.0665898698862502,0.0731716198748497),
 .UNSPECIFIED.);
#2475=B_SPLINE_SURFACE_WITH_KNOTS('',3,3,((#78716,#78717,#78718,#78719),
(#78720,#78721,#78722,#78723),(#78724,#78725,#78726,#78727),(#78728,#78729,
#78730,#78731)),.UNSPECIFIED.,.F.,.F.,.F.,(4,4),(4,4),(0.52209712021009,
1.00286791825523),(0.0600156865486944,0.0665898700060149),.UNSPECIFIED.);
#2476=B_SPLINE_SURFACE_WITH_KNOTS('',3,3,((#78741,#78742,#78743,#78744),
(#78745,#78746,#78747,#78748),(#78749,#78750,#78751,#78752),(#78753,#78754,
#78755,#78756)),.UNSPECIFIED.,.F.,.F.,.F.,(4,4),(4,4),(-0.00286764392027115,
0.477902879786605),(0.0565997133101205,0.0631721430887074),
 .UNSPECIFIED.);
#2477=B_SPLINE_SURFACE_WITH_KNOTS('',3,3,((#78793,#78794,#78795,#78796),
(#78797,#78798,#78799,#78800),(#78801,#78802,#78803,#78804),(#78805,#78806,
#78807,#78808)),.UNSPECIFIED.,.F.,.F.,.F.,(4,4),(4,4),(0.522097120210832,
1.00286780122184),(0.0500263550858676,0.0565997133101431),.UNSPECIFIED.);
#2478=B_SPLINE_SURFACE_WITH_KNOTS('',3,3,((#78880,#78881,#78882,#78883),
(#78884,#78885,#78886,#78887),(#78888,#78889,#78890,#78891),(#78892,#78893,
#78894,#78895)),.UNSPECIFIED.,.F.,.F.,.F.,(4,4),(4,4),(0.522097120210514,
1.00286848452574),(0.0400218729465704,0.0466073985929453),.UNSPECIFIED.);
#2479=B_SPLINE_SURFACE_WITH_KNOTS('',3,3,((#78964,#78965,#78966,#78967),
(#78968,#78969,#78970,#78971),(#78972,#78973,#78974,#78975),(#78976,#78977,
#78978,#78979)),.UNSPECIFIED.,.F.,.F.,.F.,(4,4),(4,4),(0.522097120209706,
1.00286862201148),(0.030009453229216,0.0365944846647038),.UNSPECIFIED.);
#2480=B_SPLINE_SURFACE_WITH_KNOTS('',3,3,((#79012,#79013,#79014,#79015),
(#79016,#79017,#79018,#79019),(#79020,#79021,#79022,#79023),(#79024,#79025,
#79026,#79027)),.UNSPECIFIED.,.F.,.F.,.F.,(4,4),(4,4),(-0.00600003964311649,
1.00000000663621),(0.0166015299238286,0.0265907346180639),.UNSPECIFIED.);
#2481=B_SPLINE_SURFACE_WITH_KNOTS('',3,3,((#79039,#79040,#79041,#79042),
(#79043,#79044,#79045,#79046),(#79047,#79048,#79049,#79050),(#79051,#79052,
#79053,#79054)),.UNSPECIFIED.,.F.,.F.,.F.,(4,4),(4,4),(0.522097120210579,
1.00286780410459),(0.0200175229646512,0.026590734618065),.UNSPECIFIED.);
#2482=B_SPLINE_SURFACE_WITH_KNOTS('',3,3,((#79110,#79111,#79112,#79113),
(#79114,#79115,#79116,#79117),(#79118,#79119,#79120,#79121),(#79122,#79123,
#79124,#79125)),.UNSPECIFIED.,.F.,.F.,.F.,(4,4),(4,4),(0.522097120210466,
1.00286791014274),(0.0100271466749329,0.0166015302184284),.UNSPECIFIED.);
#2483=B_SPLINE_SURFACE_WITH_KNOTS('',3,3,((#79151,#79152,#79153,#79154),
(#79155,#79156,#79157,#79158),(#79159,#79160,#79161,#79162),(#79163,#79164,
#79165,#79166)),.UNSPECIFIED.,.F.,.F.,.F.,(4,4),(4,4),(-0.000171895432979033,
1.00600020634818),(0.0665898698856052,0.0751325481108763),.UNSPECIFIED.);
#2484=B_SPLINE_SURFACE_WITH_KNOTS('',3,3,((#79182,#79183,#79184,#79185),
(#79186,#79187,#79188,#79189),(#79190,#79191,#79192,#79193),(#79194,#79195,
#79196,#79197)),.UNSPECIFIED.,.F.,.F.,.F.,(4,4),(4,4),(-0.00286833998587121,
0.477902879786704),(0.0665898698862514,0.0731716198748496),
 .UNSPECIFIED.);
#2485=B_SPLINE_SURFACE_WITH_KNOTS('',3,3,((#79231,#79232,#79233,#79234),
(#79235,#79236,#79237,#79238),(#79239,#79240,#79241,#79242),(#79243,#79244,
#79245,#79246)),.UNSPECIFIED.,.F.,.F.,.F.,(4,4),(4,4),(0.522097120210201,
1.0028679182551),(0.0600156865486941,0.0665898700060154),.UNSPECIFIED.);
#2486=B_SPLINE_SURFACE_WITH_KNOTS('',3,3,((#79256,#79257,#79258,#79259),
(#79260,#79261,#79262,#79263),(#79264,#79265,#79266,#79267),(#79268,#79269,
#79270,#79271)),.UNSPECIFIED.,.F.,.F.,.F.,(4,4),(4,4),(-0.00286764392018088,
0.477902879786574),(0.0565997133101201,0.0631721430887063),
 .UNSPECIFIED.);
#2487=B_SPLINE_SURFACE_WITH_KNOTS('',3,3,((#79308,#79309,#79310,#79311),
(#79312,#79313,#79314,#79315),(#79316,#79317,#79318,#79319),(#79320,#79321,
#79322,#79323)),.UNSPECIFIED.,.F.,.F.,.F.,(4,4),(4,4),(0.522097120211028,
1.00286780122187),(0.0500263550858676,0.0565997133101434),.UNSPECIFIED.);
#2488=B_SPLINE_SURFACE_WITH_KNOTS('',3,3,((#79395,#79396,#79397,#79398),
(#79399,#79400,#79401,#79402),(#79403,#79404,#79405,#79406),(#79407,#79408,
#79409,#79410)),.UNSPECIFIED.,.F.,.F.,.F.,(4,4),(4,4),(0.522097120210638,
1.00286848452575),(0.0400218729465699,0.046607398592945),.UNSPECIFIED.);
#2489=B_SPLINE_SURFACE_WITH_KNOTS('',3,3,((#79479,#79480,#79481,#79482),
(#79483,#79484,#79485,#79486),(#79487,#79488,#79489,#79490),(#79491,#79492,
#79493,#79494)),.UNSPECIFIED.,.F.,.F.,.F.,(4,4),(4,4),(0.522097120209859,
1.00286862201151),(0.0300094532292154,0.0365944846647027),.UNSPECIFIED.);
#2490=B_SPLINE_SURFACE_WITH_KNOTS('',3,3,((#79527,#79528,#79529,#79530),
(#79531,#79532,#79533,#79534),(#79535,#79536,#79537,#79538),(#79539,#79540,
#79541,#79542)),.UNSPECIFIED.,.F.,.F.,.F.,(4,4),(4,4),(-0.00600003961813093,
1.00000000246938),(0.0166015299238286,0.0265907346180632),.UNSPECIFIED.);
#2491=B_SPLINE_SURFACE_WITH_KNOTS('',3,3,((#79554,#79555,#79556,#79557),
(#79558,#79559,#79560,#79561),(#79562,#79563,#79564,#79565),(#79566,#79567,
#79568,#79569)),.UNSPECIFIED.,.F.,.F.,.F.,(4,4),(4,4),(0.522097120210637,
1.00286780410452),(0.0200175229646505,0.0265907346180656),.UNSPECIFIED.);
#2492=B_SPLINE_SURFACE_WITH_KNOTS('',3,3,((#79625,#79626,#79627,#79628),
(#79629,#79630,#79631,#79632),(#79633,#79634,#79635,#79636),(#79637,#79638,
#79639,#79640)),.UNSPECIFIED.,.F.,.F.,.F.,(4,4),(4,4),(0.522097120210457,
1.0028679101428),(0.0100271466749311,0.0166015302184272),.UNSPECIFIED.);
#2493=B_SPLINE_SURFACE_WITH_KNOTS('',3,3,((#79666,#79667,#79668,#79669),
(#79670,#79671,#79672,#79673),(#79674,#79675,#79676,#79677),(#79678,#79679,
#79680,#79681)),.UNSPECIFIED.,.F.,.F.,.F.,(4,4),(4,4),(-0.00017189543205102,
1.00600020634805),(0.0665898698856059,0.0751325481099475),.UNSPECIFIED.);
#2494=B_SPLINE_SURFACE_WITH_KNOTS('',3,3,((#79697,#79698,#79699,#79700),
(#79701,#79702,#79703,#79704),(#79705,#79706,#79707,#79708),(#79709,#79710,
#79711,#79712)),.UNSPECIFIED.,.F.,.F.,.F.,(4,4),(4,4),(-0.0028683399860157,
0.477902879786574),(0.0665898698862513,0.0731716198748509),
 .UNSPECIFIED.);
#2495=B_SPLINE_SURFACE_WITH_KNOTS('',3,3,((#79746,#79747,#79748,#79749),
(#79750,#79751,#79752,#79753),(#79754,#79755,#79756,#79757),(#79758,#79759,
#79760,#79761)),.UNSPECIFIED.,.F.,.F.,.F.,(4,4),(4,4),(0.522097120210386,
1.00286791825519),(0.0600156865486944,0.0665898700060139),.UNSPECIFIED.);
#2496=B_SPLINE_SURFACE_WITH_KNOTS('',3,3,((#79771,#79772,#79773,#79774),
(#79775,#79776,#79777,#79778),(#79779,#79780,#79781,#79782),(#79783,#79784,
#79785,#79786)),.UNSPECIFIED.,.F.,.F.,.F.,(4,4),(4,4),(-0.00286764392010482,
0.477902879786664),(0.0565997133101203,0.0631721430887056),
 .UNSPECIFIED.);
#2497=B_SPLINE_SURFACE_WITH_KNOTS('',3,3,((#79823,#79824,#79825,#79826),
(#79827,#79828,#79829,#79830),(#79831,#79832,#79833,#79834),(#79835,#79836,
#79837,#79838)),.UNSPECIFIED.,.F.,.F.,.F.,(4,4),(4,4),(0.522097120211212,
1.00286780122197),(0.0500263550858661,0.0565997133101428),.UNSPECIFIED.);
#2498=B_SPLINE_SURFACE_WITH_KNOTS('',3,3,((#79910,#79911,#79912,#79913),
(#79914,#79915,#79916,#79917),(#79918,#79919,#79920,#79921),(#79922,#79923,
#79924,#79925)),.UNSPECIFIED.,.F.,.F.,.F.,(4,4),(4,4),(0.522097120210728,
1.00286848452584),(0.04002187294657,0.0466073985929452),.UNSPECIFIED.);
#2499=B_SPLINE_SURFACE_WITH_KNOTS('',3,3,((#79994,#79995,#79996,#79997),
(#79998,#79999,#80000,#80001),(#80002,#80003,#80004,#80005),(#80006,#80007,
#80008,#80009)),.UNSPECIFIED.,.F.,.F.,.F.,(4,4),(4,4),(0.522097120209888,
1.00286862201144),(0.0300094532292169,0.0365944846647038),.UNSPECIFIED.);
#2500=B_SPLINE_SURFACE_WITH_KNOTS('',3,3,((#80042,#80043,#80044,#80045),
(#80046,#80047,#80048,#80049),(#80050,#80051,#80052,#80053),(#80054,#80055,
#80056,#80057)),.UNSPECIFIED.,.F.,.F.,.F.,(4,4),(4,4),(-0.00600003961812457,
1.00000000246936),(0.0166015299238285,0.0265907346180632),.UNSPECIFIED.);
#2501=B_SPLINE_SURFACE_WITH_KNOTS('',3,3,((#80069,#80070,#80071,#80072),
(#80073,#80074,#80075,#80076),(#80077,#80078,#80079,#80080),(#80081,#80082,
#80083,#80084)),.UNSPECIFIED.,.F.,.F.,.F.,(4,4),(4,4),(0.522097120210843,
1.00286780410462),(0.0200175229646514,0.026590734618064),.UNSPECIFIED.);
#2502=B_SPLINE_SURFACE_WITH_KNOTS('',3,3,((#80140,#80141,#80142,#80143),
(#80144,#80145,#80146,#80147),(#80148,#80149,#80150,#80151),(#80152,#80153,
#80154,#80155)),.UNSPECIFIED.,.F.,.F.,.F.,(4,4),(4,4),(0.522097120210691,
1.00286791014268),(0.0100271466749321,0.0166015302184286),.UNSPECIFIED.);
#2503=B_SPLINE_SURFACE_WITH_KNOTS('',3,3,((#80181,#80182,#80183,#80184),
(#80185,#80186,#80187,#80188),(#80189,#80190,#80191,#80192),(#80193,#80194,
#80195,#80196)),.UNSPECIFIED.,.F.,.F.,.F.,(4,4),(4,4),(-0.00017189543133579,
1.00600020634815),(0.0665898698856047,0.0751325481092326),.UNSPECIFIED.);
#2504=B_SPLINE_SURFACE_WITH_KNOTS('',3,3,((#80212,#80213,#80214,#80215),
(#80216,#80217,#80218,#80219),(#80220,#80221,#80222,#80223),(#80224,#80225,
#80226,#80227)),.UNSPECIFIED.,.F.,.F.,.F.,(4,4),(4,4),(-0.00286833998587508,
0.477902879786664),(0.0665898698862506,0.0731716198748496),
 .UNSPECIFIED.);
#2505=B_SPLINE_SURFACE_WITH_KNOTS('',3,3,((#80261,#80262,#80263,#80264),
(#80265,#80266,#80267,#80268),(#80269,#80270,#80271,#80272),(#80273,#80274,
#80275,#80276)),.UNSPECIFIED.,.F.,.F.,.F.,(4,4),(4,4),(0.522097120209475,
1.00286791825523),(0.0600156865486928,0.0665898700060142),.UNSPECIFIED.);
#2506=B_SPLINE_SURFACE_WITH_KNOTS('',3,3,((#80286,#80287,#80288,#80289),
(#80290,#80291,#80292,#80293),(#80294,#80295,#80296,#80297),(#80298,#80299,
#80300,#80301)),.UNSPECIFIED.,.F.,.F.,.F.,(4,4),(4,4),(-0.0028676439202061,
0.477902879786615),(0.0565997133101201,0.0631721430887064),
 .UNSPECIFIED.);
#2507=B_SPLINE_SURFACE_WITH_KNOTS('',3,3,((#80338,#80339,#80340,#80341),
(#80342,#80343,#80344,#80345),(#80346,#80347,#80348,#80349),(#80350,#80351,
#80352,#80353)),.UNSPECIFIED.,.F.,.F.,.F.,(4,4),(4,4),(0.522097120210878,
1.00286780122192),(0.0500263550858677,0.0565997133101427),.UNSPECIFIED.);
#2508=B_SPLINE_SURFACE_WITH_KNOTS('',3,3,((#80425,#80426,#80427,#80428),
(#80429,#80430,#80431,#80432),(#80433,#80434,#80435,#80436),(#80437,#80438,
#80439,#80440)),.UNSPECIFIED.,.F.,.F.,.F.,(4,4),(4,4),(0.522097120210891,
1.00286848452579),(0.0400218729465691,0.0466073985929451),.UNSPECIFIED.);
#2509=B_SPLINE_SURFACE_WITH_KNOTS('',3,3,((#80509,#80510,#80511,#80512),
(#80513,#80514,#80515,#80516),(#80517,#80518,#80519,#80520),(#80521,#80522,
#80523,#80524)),.UNSPECIFIED.,.F.,.F.,.F.,(4,4),(4,4),(0.522097120209977,
1.00286862201146),(0.0300094532292159,0.0365944846647041),.UNSPECIFIED.);
#2510=B_SPLINE_SURFACE_WITH_KNOTS('',3,3,((#80557,#80558,#80559,#80560),
(#80561,#80562,#80563,#80564),(#80565,#80566,#80567,#80568),(#80569,#80570,
#80571,#80572)),.UNSPECIFIED.,.F.,.F.,.F.,(4,4),(4,4),(-0.00600003961813121,
1.0000000024693),(0.0166015299238285,0.0265907346180638),.UNSPECIFIED.);
#2511=B_SPLINE_SURFACE_WITH_KNOTS('',3,3,((#80584,#80585,#80586,#80587),
(#80588,#80589,#80590,#80591),(#80592,#80593,#80594,#80595),(#80596,#80597,
#80598,#80599)),.UNSPECIFIED.,.F.,.F.,.F.,(4,4),(4,4),(0.522097120210981,
1.00286780410451),(0.0200175229646507,0.026590734618064),.UNSPECIFIED.);
#2512=B_SPLINE_SURFACE_WITH_KNOTS('',3,3,((#80655,#80656,#80657,#80658),
(#80659,#80660,#80661,#80662),(#80663,#80664,#80665,#80666),(#80667,#80668,
#80669,#80670)),.UNSPECIFIED.,.F.,.F.,.F.,(4,4),(4,4),(0.522097120210828,
1.00286791014284),(0.0100271466749304,0.0166015302184278),.UNSPECIFIED.);
#2513=B_SPLINE_SURFACE_WITH_KNOTS('',3,3,((#80696,#80697,#80698,#80699),
(#80700,#80701,#80702,#80703),(#80704,#80705,#80706,#80707),(#80708,#80709,
#80710,#80711)),.UNSPECIFIED.,.F.,.F.,.F.,(4,4),(4,4),(-0.00017189543037276,
1.00600020634836),(0.0665898698856047,0.0751325481082702),.UNSPECIFIED.);
#2514=B_SPLINE_SURFACE_WITH_KNOTS('',3,3,((#80727,#80728,#80729,#80730),
(#80731,#80732,#80733,#80734),(#80735,#80736,#80737,#80738),(#80739,#80740,
#80741,#80742)),.UNSPECIFIED.,.F.,.F.,.F.,(4,4),(4,4),(-0.00286833998584599,
0.477902879786607),(0.0665898698862517,0.07317161987485),.UNSPECIFIED.);
#2515=B_SPLINE_SURFACE_WITH_KNOTS('',3,3,((#80776,#80777,#80778,#80779),
(#80780,#80781,#80782,#80783),(#80784,#80785,#80786,#80787),(#80788,#80789,
#80790,#80791)),.UNSPECIFIED.,.F.,.F.,.F.,(4,4),(4,4),(0.522097120207303,
1.00286791825526),(0.0600156865486934,0.0665898700060142),.UNSPECIFIED.);
#2516=B_SPLINE_SURFACE_WITH_KNOTS('',3,3,((#80801,#80802,#80803,#80804),
(#80805,#80806,#80807,#80808),(#80809,#80810,#80811,#80812),(#80813,#80814,
#80815,#80816)),.UNSPECIFIED.,.F.,.F.,.F.,(4,4),(4,4),(-0.00286764392024303,
0.477902879786695),(0.0565997133101202,0.0631721430887064),
 .UNSPECIFIED.);
#2517=B_SPLINE_SURFACE_WITH_KNOTS('',3,3,((#80853,#80854,#80855,#80856),
(#80857,#80858,#80859,#80860),(#80861,#80862,#80863,#80864),(#80865,#80866,
#80867,#80868)),.UNSPECIFIED.,.F.,.F.,.F.,(4,4),(4,4),(0.522097120208596,
1.00286780122191),(0.0500263550858673,0.0565997133101421),.UNSPECIFIED.);
#2518=B_SPLINE_SURFACE_WITH_KNOTS('',3,3,((#80940,#80941,#80942,#80943),
(#80944,#80945,#80946,#80947),(#80948,#80949,#80950,#80951),(#80952,#80953,
#80954,#80955)),.UNSPECIFIED.,.F.,.F.,.F.,(4,4),(4,4),(0.522097120209593,
1.00286848452575),(0.0400218729465712,0.0466073985929449),.UNSPECIFIED.);
#2519=B_SPLINE_SURFACE_WITH_KNOTS('',3,3,((#81024,#81025,#81026,#81027),
(#81028,#81029,#81030,#81031),(#81032,#81033,#81034,#81035),(#81036,#81037,
#81038,#81039)),.UNSPECIFIED.,.F.,.F.,.F.,(4,4),(4,4),(0.522097120210169,
1.00286862201142),(0.0300094532292164,0.036594484664704),.UNSPECIFIED.);
#2520=B_SPLINE_SURFACE_WITH_KNOTS('',3,3,((#81072,#81073,#81074,#81075),
(#81076,#81077,#81078,#81079),(#81080,#81081,#81082,#81083),(#81084,#81085,
#81086,#81087)),.UNSPECIFIED.,.F.,.F.,.F.,(4,4),(4,4),(-0.00600003961800698,
1.00000000246934),(0.0166015299238286,0.0265907346180639),.UNSPECIFIED.);
#2521=B_SPLINE_SURFACE_WITH_KNOTS('',3,3,((#81099,#81100,#81101,#81102),
(#81103,#81104,#81105,#81106),(#81107,#81108,#81109,#81110),(#81111,#81112,
#81113,#81114)),.UNSPECIFIED.,.F.,.F.,.F.,(4,4),(4,4),(0.522097120210999,
1.0028678041046),(0.020017522964652,0.0265907346180649),.UNSPECIFIED.);
#2522=B_SPLINE_SURFACE_WITH_KNOTS('',3,3,((#81170,#81171,#81172,#81173),
(#81174,#81175,#81176,#81177),(#81178,#81179,#81180,#81181),(#81182,#81183,
#81184,#81185)),.UNSPECIFIED.,.F.,.F.,.F.,(4,4),(4,4),(0.522097120210868,
1.00286791014275),(0.0100271466749306,0.0166015302184266),.UNSPECIFIED.);
#2523=B_SPLINE_SURFACE_WITH_KNOTS('',3,3,((#81211,#81212,#81213,#81214),
(#81215,#81216,#81217,#81218),(#81219,#81220,#81221,#81222),(#81223,#81224,
#81225,#81226)),.UNSPECIFIED.,.F.,.F.,.F.,(4,4),(4,4),(-0.0001718954296519,
1.00600020634795),(0.0665898698856053,0.0751325481075477),.UNSPECIFIED.);
#2524=B_SPLINE_SURFACE_WITH_KNOTS('',3,3,((#81242,#81243,#81244,#81245),
(#81246,#81247,#81248,#81249),(#81250,#81251,#81252,#81253),(#81254,#81255,
#81256,#81257)),.UNSPECIFIED.,.F.,.F.,.F.,(4,4),(4,4),(-0.00286833998595421,
0.477902879786473),(0.0665898698862515,0.0731716198748503),
 .UNSPECIFIED.);
#2525=B_SPLINE_SURFACE_WITH_KNOTS('',3,3,((#81291,#81292,#81293,#81294),
(#81295,#81296,#81297,#81298),(#81299,#81300,#81301,#81302),(#81303,#81304,
#81305,#81306)),.UNSPECIFIED.,.F.,.F.,.F.,(4,4),(4,4),(0.522097120205134,
1.00286791825525),(0.060015686548694,0.0665898700060144),.UNSPECIFIED.);
#2526=B_SPLINE_SURFACE_WITH_KNOTS('',3,3,((#81316,#81317,#81318,#81319),
(#81320,#81321,#81322,#81323),(#81324,#81325,#81326,#81327),(#81328,#81329,
#81330,#81331)),.UNSPECIFIED.,.F.,.F.,.F.,(4,4),(4,4),(-0.00286764392015422,
0.477902879786423),(0.0565997133101208,0.0631721430887068),
 .UNSPECIFIED.);
#2527=B_SPLINE_SURFACE_WITH_KNOTS('',3,3,((#81365,#81366,#81367,#81368),
(#81369,#81370,#81371,#81372),(#81373,#81374,#81375,#81376),(#81377,#81378,
#81379,#81380)),.UNSPECIFIED.,.F.,.F.,.F.,(4,4),(4,4),(0.522097120206487,
1.00286780122197),(0.0500263550858671,0.0565997133101411),.UNSPECIFIED.);
#2528=B_SPLINE_SURFACE_WITH_KNOTS('',3,3,((#81388,#81389,#81390,#81391),
(#81392,#81393,#81394,#81395),(#81396,#81397,#81398,#81399),(#81400,#81401,
#81402,#81403)),.UNSPECIFIED.,.F.,.F.,.F.,(4,4),(4,4),(-0.00286810177283975,
0.477902879786577),(0.0466073985929119,0.0531834933545505),
 .UNSPECIFIED.);
#2529=B_SPLINE_SURFACE_WITH_KNOTS('',3,3,((#81459,#81460,#81461,#81462),
(#81463,#81464,#81465,#81466),(#81467,#81468,#81469,#81470),(#81471,#81472,
#81473,#81474)),.UNSPECIFIED.,.F.,.F.,.F.,(4,4),(4,4),(0.522097120207441,
1.00286848452585),(0.0400218729465689,0.0466073985929454),.UNSPECIFIED.);
#2530=B_SPLINE_SURFACE_WITH_KNOTS('',3,3,((#81543,#81544,#81545,#81546),
(#81547,#81548,#81549,#81550),(#81551,#81552,#81553,#81554),(#81555,#81556,
#81557,#81558)),.UNSPECIFIED.,.F.,.F.,.F.,(4,4),(4,4),(0.522097120208268,
1.00286862201145),(0.0300094532292153,0.0365944846647042),.UNSPECIFIED.);
#2531=B_SPLINE_SURFACE_WITH_KNOTS('',3,3,((#81591,#81592,#81593,#81594),
(#81595,#81596,#81597,#81598),(#81599,#81600,#81601,#81602),(#81603,#81604,
#81605,#81606)),.UNSPECIFIED.,.F.,.F.,.F.,(4,4),(4,4),(-0.00600003964319226,
1.00000000663601),(0.0166015299238287,0.0265907346180634),.UNSPECIFIED.);
#2532=B_SPLINE_SURFACE_WITH_KNOTS('',3,3,((#81618,#81619,#81620,#81621),
(#81622,#81623,#81624,#81625),(#81626,#81627,#81628,#81629),(#81630,#81631,
#81632,#81633)),.UNSPECIFIED.,.F.,.F.,.F.,(4,4),(4,4),(0.522097120209615,
1.00286780410456),(0.0200175229646514,0.0265907346180652),.UNSPECIFIED.);
#2533=B_SPLINE_SURFACE_WITH_KNOTS('',3,3,((#81689,#81690,#81691,#81692),
(#81693,#81694,#81695,#81696),(#81697,#81698,#81699,#81700),(#81701,#81702,
#81703,#81704)),.UNSPECIFIED.,.F.,.F.,.F.,(4,4),(4,4),(0.522097120210727,
1.0028679101428),(0.0100271466749319,0.0166015302184276),.UNSPECIFIED.);
#2534=B_SPLINE_SURFACE_WITH_KNOTS('',3,3,((#81730,#81731,#81732,#81733),
(#81734,#81735,#81736,#81737),(#81738,#81739,#81740,#81741),(#81742,#81743,
#81744,#81745)),.UNSPECIFIED.,.F.,.F.,.F.,(4,4),(4,4),(-0.00017189542896064,
1.00600020634802),(0.0665898698856043,0.0751325481068571),.UNSPECIFIED.);
#2535=B_SPLINE_SURFACE_WITH_KNOTS('',3,3,((#81761,#81762,#81763,#81764),
(#81765,#81766,#81767,#81768),(#81769,#81770,#81771,#81772),(#81773,#81774,
#81775,#81776)),.UNSPECIFIED.,.F.,.F.,.F.,(4,4),(4,4),(-0.00286833998593375,
0.47790287978645),(0.0665898698862501,0.07317161987485),.UNSPECIFIED.);
#2536=B_SPLINE_SURFACE_WITH_KNOTS('',3,3,((#81810,#81811,#81812,#81813),
(#81814,#81815,#81816,#81817),(#81818,#81819,#81820,#81821),(#81822,#81823,
#81824,#81825)),.UNSPECIFIED.,.F.,.F.,.F.,(4,4),(4,4),(0.522097120203271,
1.00286791825529),(0.0600156865486934,0.0665898700060131),.UNSPECIFIED.);
#2537=B_SPLINE_SURFACE_WITH_KNOTS('',3,3,((#81835,#81836,#81837,#81838),
(#81839,#81840,#81841,#81842),(#81843,#81844,#81845,#81846),(#81847,#81848,
#81849,#81850)),.UNSPECIFIED.,.F.,.F.,.F.,(4,4),(4,4),(-0.00286764392023632,
0.477902879786599),(0.0565997133101197,0.0631721430887068),
 .UNSPECIFIED.);
#2538=B_SPLINE_SURFACE_WITH_KNOTS('',3,3,((#81887,#81888,#81889,#81890),
(#81891,#81892,#81893,#81894),(#81895,#81896,#81897,#81898),(#81899,#81900,
#81901,#81902)),.UNSPECIFIED.,.F.,.F.,.F.,(4,4),(4,4),(0.522097120204332,
1.00286780122196),(0.0500263550858673,0.0565997133101428),.UNSPECIFIED.);
#2539=B_SPLINE_SURFACE_WITH_KNOTS('',3,3,((#81935,#81936,#81937,#81938),
(#81939,#81940,#81941,#81942),(#81943,#81944,#81945,#81946),(#81947,#81948,
#81949,#81950)),.UNSPECIFIED.,.F.,.F.,.F.,(4,4),(4,4),(-0.00600014643533104,
1.),(0.0365944846640577,0.046607398592944),.UNSPECIFIED.);
#2540=B_SPLINE_SURFACE_WITH_KNOTS('',3,3,((#81973,#81974,#81975,#81976),
(#81977,#81978,#81979,#81980),(#81981,#81982,#81983,#81984),(#81985,#81986,
#81987,#81988)),.UNSPECIFIED.,.F.,.F.,.F.,(4,4),(4,4),(0.522097120205363,
1.00286848452578),(0.0400218729465698,0.0466073985929445),.UNSPECIFIED.);
#2541=B_SPLINE_SURFACE_WITH_KNOTS('',3,3,((#82052,#82053,#82054,#82055),
(#82056,#82057,#82058,#82059),(#82060,#82061,#82062,#82063),(#82064,#82065,
#82066,#82067)),.UNSPECIFIED.,.F.,.F.,.F.,(4,4),(4,4),(0.522097120206,1.00286862201151),
(0.0300094532292161,0.0365944846647034),.UNSPECIFIED.);
#2542=B_SPLINE_SURFACE_WITH_KNOTS('',3,3,((#82100,#82101,#82102,#82103),
(#82104,#82105,#82106,#82107),(#82108,#82109,#82110,#82111),(#82112,#82113,
#82114,#82115)),.UNSPECIFIED.,.F.,.F.,.F.,(4,4),(4,4),(-0.00600003961801213,
1.00000000246949),(0.0166015299238286,0.0265907346180633),.UNSPECIFIED.);
#2543=B_SPLINE_SURFACE_WITH_KNOTS('',3,3,((#82127,#82128,#82129,#82130),
(#82131,#82132,#82133,#82134),(#82135,#82136,#82137,#82138),(#82139,#82140,
#82141,#82142)),.UNSPECIFIED.,.F.,.F.,.F.,(4,4),(4,4),(0.522097120207366,
1.00286780410456),(0.0200175229646512,0.0265907346180654),.UNSPECIFIED.);
#2544=B_SPLINE_SURFACE_WITH_KNOTS('',3,3,((#82198,#82199,#82200,#82201),
(#82202,#82203,#82204,#82205),(#82206,#82207,#82208,#82209),(#82210,#82211,
#82212,#82213)),.UNSPECIFIED.,.F.,.F.,.F.,(4,4),(4,4),(0.522097120208367,
1.00286791014273),(0.0100271466749317,0.0166015302184278),.UNSPECIFIED.);
#2545=B_SPLINE_SURFACE_WITH_KNOTS('',3,3,((#82239,#82240,#82241,#82242),
(#82243,#82244,#82245,#82246),(#82247,#82248,#82249,#82250),(#82251,#82252,
#82253,#82254)),.UNSPECIFIED.,.F.,.F.,.F.,(4,4),(4,4),(-0.000171895428571592,
1.00600020634813),(0.0665898698856047,0.0751325481064681),.UNSPECIFIED.);
#2546=B_SPLINE_SURFACE_WITH_KNOTS('',3,3,((#82270,#82271,#82272,#82273),
(#82274,#82275,#82276,#82277),(#82278,#82279,#82280,#82281),(#82282,#82283,
#82284,#82285)),.UNSPECIFIED.,.F.,.F.,.F.,(4,4),(4,4),(-0.00286833998598749,
0.477902879789405),(0.0665898698862508,0.0731716198748509),
 .UNSPECIFIED.);
#2547=B_SPLINE_SURFACE_WITH_KNOTS('',3,3,((#82319,#82320,#82321,#82322),
(#82323,#82324,#82325,#82326),(#82327,#82328,#82329,#82330),(#82331,#82332,
#82333,#82334)),.UNSPECIFIED.,.F.,.F.,.F.,(4,4),(4,4),(0.52209712020154,
1.00286791825529),(0.0600156865486932,0.0665898700060148),.UNSPECIFIED.);
#2548=B_SPLINE_SURFACE_WITH_KNOTS('',3,3,((#82344,#82345,#82346,#82347),
(#82348,#82349,#82350,#82351),(#82352,#82353,#82354,#82355),(#82356,#82357,
#82358,#82359)),.UNSPECIFIED.,.F.,.F.,.F.,(4,4),(4,4),(-0.00286764392027554,
0.477902879788135),(0.0565997133101202,0.0631721430887068),
 .UNSPECIFIED.);
#2549=B_SPLINE_SURFACE_WITH_KNOTS('',3,3,((#82396,#82397,#82398,#82399),
(#82400,#82401,#82402,#82403),(#82404,#82405,#82406,#82407),(#82408,#82409,
#82410,#82411)),.UNSPECIFIED.,.F.,.F.,.F.,(4,4),(4,4),(0.522097120202531,
1.00286780122197),(0.050026355085867,0.0565997133101419),.UNSPECIFIED.);
#2550=B_SPLINE_SURFACE_WITH_KNOTS('',3,3,((#82483,#82484,#82485,#82486),
(#82487,#82488,#82489,#82490),(#82491,#82492,#82493,#82494),(#82495,#82496,
#82497,#82498)),.UNSPECIFIED.,.F.,.F.,.F.,(4,4),(4,4),(0.522097120203339,
1.00286848452584),(0.0400218729465689,0.0466073985929463),.UNSPECIFIED.);
#2551=B_SPLINE_SURFACE_WITH_KNOTS('',3,3,((#82564,#82565,#82566,#82567),
(#82568,#82569,#82570,#82571),(#82572,#82573,#82574,#82575),(#82576,#82577,
#82578,#82579)),.UNSPECIFIED.,.F.,.F.,.F.,(4,4),(4,4),(0.522097120204001,
1.00286862201145),(0.0300094532292154,0.0365944846647039),.UNSPECIFIED.);
#2552=B_SPLINE_SURFACE_WITH_KNOTS('',3,3,((#82587,#82588,#82589,#82590),
(#82591,#82592,#82593,#82594),(#82595,#82596,#82597,#82598),(#82599,#82600,
#82601,#82602)),.UNSPECIFIED.,.F.,.F.,.F.,(4,4),(4,4),(-0.0028682335621104,
0.477902879786601),(0.026590734618062,0.0331702037252921),.UNSPECIFIED.);
#2553=B_SPLINE_SURFACE_WITH_KNOTS('',3,3,((#82619,#82620,#82621,#82622),
(#82623,#82624,#82625,#82626),(#82627,#82628,#82629,#82630),(#82631,#82632,
#82633,#82634)),.UNSPECIFIED.,.F.,.F.,.F.,(4,4),(4,4),(-0.00600003964307988,
1.00000000663629),(0.0166015299238289,0.0265907346180633),.UNSPECIFIED.);
#2554=B_SPLINE_SURFACE_WITH_KNOTS('',3,3,((#82646,#82647,#82648,#82649),
(#82650,#82651,#82652,#82653),(#82654,#82655,#82656,#82657),(#82658,#82659,
#82660,#82661)),.UNSPECIFIED.,.F.,.F.,.F.,(4,4),(4,4),(0.522097120205243,
1.00286780410455),(0.0200175229646507,0.0265907346180654),.UNSPECIFIED.);
#2555=B_SPLINE_SURFACE_WITH_KNOTS('',3,3,((#82717,#82718,#82719,#82720),
(#82721,#82722,#82723,#82724),(#82725,#82726,#82727,#82728),(#82729,#82730,
#82731,#82732)),.UNSPECIFIED.,.F.,.F.,.F.,(4,4),(4,4),(0.522097120206236,
1.00286791014282),(0.0100271466749313,0.0166015302184277),.UNSPECIFIED.);
#2556=B_SPLINE_SURFACE_WITH_KNOTS('',3,3,((#82758,#82759,#82760,#82761),
(#82762,#82763,#82764,#82765),(#82766,#82767,#82768,#82769),(#82770,#82771,
#82772,#82773)),.UNSPECIFIED.,.F.,.F.,.F.,(4,4),(4,4),(-0.000171895428076154,
1.00600020634796),(0.0665898698856047,0.0751325481059748),.UNSPECIFIED.);
#2557=B_SPLINE_SURFACE_WITH_KNOTS('',3,3,((#82789,#82790,#82791,#82792),
(#82793,#82794,#82795,#82796),(#82797,#82798,#82799,#82800),(#82801,#82802,
#82803,#82804)),.UNSPECIFIED.,.F.,.F.,.F.,(4,4),(4,4),(-0.002868339985951,
0.477902879791939),(0.0665898698862501,0.0731716198748492),
 .UNSPECIFIED.);
#2558=B_SPLINE_SURFACE_WITH_KNOTS('',3,3,((#82838,#82839,#82840,#82841),
(#82842,#82843,#82844,#82845),(#82846,#82847,#82848,#82849),(#82850,#82851,
#82852,#82853)),.UNSPECIFIED.,.F.,.F.,.F.,(4,4),(4,4),(0.522097120200109,
1.00286791825532),(0.0600156865486933,0.0665898700060144),.UNSPECIFIED.);
#2559=B_SPLINE_SURFACE_WITH_KNOTS('',3,3,((#82863,#82864,#82865,#82866),
(#82867,#82868,#82869,#82870),(#82871,#82872,#82873,#82874),(#82875,#82876,
#82877,#82878)),.UNSPECIFIED.,.F.,.F.,.F.,(4,4),(4,4),(-0.00286764392029188,
0.477902879790651),(0.0565997133101211,0.0631721430887068),
 .UNSPECIFIED.);
#2560=B_SPLINE_SURFACE_WITH_KNOTS('',3,3,((#82915,#82916,#82917,#82918),
(#82919,#82920,#82921,#82922),(#82923,#82924,#82925,#82926),(#82927,#82928,
#82929,#82930)),.UNSPECIFIED.,.F.,.F.,.F.,(4,4),(4,4),(0.522097120201025,
1.00286780122203),(0.0500263550858673,0.0565997133101423),.UNSPECIFIED.);
#2561=B_SPLINE_SURFACE_WITH_KNOTS('',3,3,((#83002,#83003,#83004,#83005),
(#83006,#83007,#83008,#83009),(#83010,#83011,#83012,#83013),(#83014,#83015,
#83016,#83017)),.UNSPECIFIED.,.F.,.F.,.F.,(4,4),(4,4),(0.522097120201695,
1.00286848452585),(0.0400218729465699,0.0466073985929445),.UNSPECIFIED.);
#2562=B_SPLINE_SURFACE_WITH_KNOTS('',3,3,((#83086,#83087,#83088,#83089),
(#83090,#83091,#83092,#83093),(#83094,#83095,#83096,#83097),(#83098,#83099,
#83100,#83101)),.UNSPECIFIED.,.F.,.F.,.F.,(4,4),(4,4),(0.522097120202243,
1.00286862201148),(0.0300094532292163,0.0365944846647038),.UNSPECIFIED.);
#2563=B_SPLINE_SURFACE_WITH_KNOTS('',3,3,((#83134,#83135,#83136,#83137),
(#83138,#83139,#83140,#83141),(#83142,#83143,#83144,#83145),(#83146,#83147,
#83148,#83149)),.UNSPECIFIED.,.F.,.F.,.F.,(4,4),(4,4),(-0.00600003960321525,
1.),(0.0166015299238289,0.0265907346180637),.UNSPECIFIED.);
#2564=B_SPLINE_SURFACE_WITH_KNOTS('',3,3,((#83161,#83162,#83163,#83164),
(#83165,#83166,#83167,#83168),(#83169,#83170,#83171,#83172),(#83173,#83174,
#83175,#83176)),.UNSPECIFIED.,.F.,.F.,.F.,(4,4),(4,4),(0.52209712020337,
1.00286780410461),(0.0200175229646522,0.0265907346180655),.UNSPECIFIED.);
#2565=B_SPLINE_SURFACE_WITH_KNOTS('',3,3,((#83184,#83185,#83186,#83187),
(#83188,#83189,#83190,#83191),(#83192,#83193,#83194,#83195),(#83196,#83197,
#83198,#83199)),.UNSPECIFIED.,.F.,.F.,.F.,(4,4),(4,4),(-0.00286753128207834,
0.477902879786653),(0.0166015299238961,0.0231736788111887),
 .UNSPECIFIED.);
#2566=B_SPLINE_SURFACE_WITH_KNOTS('',3,3,((#83239,#83240,#83241,#83242),
(#83243,#83244,#83245,#83246),(#83247,#83248,#83249,#83250),(#83251,#83252,
#83253,#83254)),.UNSPECIFIED.,.F.,.F.,.F.,(4,4),(4,4),(0.522097120204273,
1.00286791014282),(0.0100271466749313,0.0166015302184272),.UNSPECIFIED.);
#2567=B_SPLINE_SURFACE_WITH_KNOTS('',3,3,((#83280,#83281,#83282,#83283),
(#83284,#83285,#83286,#83287),(#83288,#83289,#83290,#83291),(#83292,#83293,
#83294,#83295)),.UNSPECIFIED.,.F.,.F.,.F.,(4,4),(4,4),(-0.000171895427606127,
1.006000206348),(0.0665898698856038,0.0751325481055029),.UNSPECIFIED.);
#2568=B_SPLINE_SURFACE_WITH_KNOTS('',3,3,((#83311,#83312,#83313,#83314),
(#83315,#83316,#83317,#83318),(#83319,#83320,#83321,#83322),(#83323,#83324,
#83325,#83326)),.UNSPECIFIED.,.F.,.F.,.F.,(4,4),(4,4),(-0.00286833998596085,
0.477902879794542),(0.0665898698862505,0.0731716198748491),
 .UNSPECIFIED.);
#2569=B_SPLINE_SURFACE_WITH_KNOTS('',3,3,((#83360,#83361,#83362,#83363),
(#83364,#83365,#83366,#83367),(#83368,#83369,#83370,#83371),(#83372,#83373,
#83374,#83375)),.UNSPECIFIED.,.F.,.F.,.F.,(4,4),(4,4),(0.522097120198851,
1.00286791825524),(0.060015686548694,0.0665898700060149),.UNSPECIFIED.);
#2570=B_SPLINE_SURFACE_WITH_KNOTS('',3,3,((#83385,#83386,#83387,#83388),
(#83389,#83390,#83391,#83392),(#83393,#83394,#83395,#83396),(#83397,#83398,
#83399,#83400)),.UNSPECIFIED.,.F.,.F.,.F.,(4,4),(4,4),(-0.00286764392021428,
0.477902879793322),(0.0565997133101211,0.063172143088707),.UNSPECIFIED.);
#2571=B_SPLINE_SURFACE_WITH_KNOTS('',3,3,((#83437,#83438,#83439,#83440),
(#83441,#83442,#83443,#83444),(#83445,#83446,#83447,#83448),(#83449,#83450,
#83451,#83452)),.UNSPECIFIED.,.F.,.F.,.F.,(4,4),(4,4),(0.522097120199709,
1.00286780122204),(0.0500263550858672,0.056599713310143),.UNSPECIFIED.);
#2572=B_SPLINE_SURFACE_WITH_KNOTS('',3,3,((#83524,#83525,#83526,#83527),
(#83528,#83529,#83530,#83531),(#83532,#83533,#83534,#83535),(#83536,#83537,
#83538,#83539)),.UNSPECIFIED.,.F.,.F.,.F.,(4,4),(4,4),(0.52209712020022,
1.00286848452585),(0.0400218729465699,0.0466073985929449),.UNSPECIFIED.);
#2573=B_SPLINE_SURFACE_WITH_KNOTS('',3,3,((#83608,#83609,#83610,#83611),
(#83612,#83613,#83614,#83615),(#83616,#83617,#83618,#83619),(#83620,#83621,
#83622,#83623)),.UNSPECIFIED.,.F.,.F.,.F.,(4,4),(4,4),(0.522097120200653,
1.00286862201151),(0.0300094532292151,0.0365944846647036),.UNSPECIFIED.);
#2574=B_SPLINE_SURFACE_WITH_KNOTS('',3,3,((#83656,#83657,#83658,#83659),
(#83660,#83661,#83662,#83663),(#83664,#83665,#83666,#83667),(#83668,#83669,
#83670,#83671)),.UNSPECIFIED.,.F.,.F.,.F.,(4,4),(4,4),(-0.0060000396247756,
1.00000000356517),(0.0166015299238288,0.0265907346180661),.UNSPECIFIED.);
#2575=B_SPLINE_SURFACE_WITH_KNOTS('',3,3,((#83683,#83684,#83685,#83686),
(#83687,#83688,#83689,#83690),(#83691,#83692,#83693,#83694),(#83695,#83696,
#83697,#83698)),.UNSPECIFIED.,.F.,.F.,.F.,(4,4),(4,4),(0.522097120201635,
1.0028678041046),(0.020017522964651,0.0265907346180654),.UNSPECIFIED.);
#2576=B_SPLINE_SURFACE_WITH_KNOTS('',3,3,((#83751,#83752,#83753,#83754),
(#83755,#83756,#83757,#83758),(#83759,#83760,#83761,#83762),(#83763,#83764,
#83765,#83766)),.UNSPECIFIED.,.F.,.F.,.F.,(4,4),(4,4),(0.522097120202428,
1.00286791014283),(0.0100271466749307,0.0166015302184278),.UNSPECIFIED.);
#2577=B_SPLINE_SURFACE_WITH_KNOTS('',3,3,((#83774,#83775,#83776,#83777),
(#83778,#83779,#83780,#83781),(#83782,#83783,#83784,#83785),(#83786,#83787,
#83788,#83789)),.UNSPECIFIED.,.F.,.F.,.F.,(4,4),(4,4),(-0.00206901892602344,
0.346769728504638),(0.00660713154698981,0.0131849431468423),
 .UNSPECIFIED.);
#2578=B_SPLINE_SURFACE_WITH_KNOTS('',3,3,((#83799,#83800,#83801,#83802),
(#83803,#83804,#83805,#83806),(#83807,#83808,#83809,#83810),(#83811,#83812,
#83813,#83814)),.UNSPECIFIED.,.F.,.F.,.F.,(4,4),(4,4),(-0.000171895427410773,
1.00600020634837),(0.0665898698856052,0.0751325481053073),.UNSPECIFIED.);
#2579=B_SPLINE_SURFACE_WITH_KNOTS('',3,3,((#83830,#83831,#83832,#83833),
(#83834,#83835,#83836,#83837),(#83838,#83839,#83840,#83841),(#83842,#83843,
#83844,#83845)),.UNSPECIFIED.,.F.,.F.,.F.,(4,4),(4,4),(-0.00286833998591909,
0.477902879796992),(0.0665898698862512,0.0731716198748501),
 .UNSPECIFIED.);
#2580=B_SPLINE_SURFACE_WITH_KNOTS('',3,3,((#83879,#83880,#83881,#83882),
(#83883,#83884,#83885,#83886),(#83887,#83888,#83889,#83890),(#83891,#83892,
#83893,#83894)),.UNSPECIFIED.,.F.,.F.,.F.,(4,4),(4,4),(0.522097120197966,
1.00286791825531),(0.0600156865486934,0.0665898700060137),.UNSPECIFIED.);
#2581=B_SPLINE_SURFACE_WITH_KNOTS('',3,3,((#83904,#83905,#83906,#83907),
(#83908,#83909,#83910,#83911),(#83912,#83913,#83914,#83915),(#83916,#83917,
#83918,#83919)),.UNSPECIFIED.,.F.,.F.,.F.,(4,4),(4,4),(-0.00286764392030516,
0.477902879795798),(0.0565997133101207,0.0631721430887073),
 .UNSPECIFIED.);
#2582=B_SPLINE_SURFACE_WITH_KNOTS('',3,3,((#83956,#83957,#83958,#83959),
(#83960,#83961,#83962,#83963),(#83964,#83965,#83966,#83967),(#83968,#83969,
#83970,#83971)),.UNSPECIFIED.,.F.,.F.,.F.,(4,4),(4,4),(0.522097120198643,
1.00286780122203),(0.0500263550858678,0.0565997133101423),.UNSPECIFIED.);
#2583=B_SPLINE_SURFACE_WITH_KNOTS('',3,3,((#84043,#84044,#84045,#84046),
(#84047,#84048,#84049,#84050),(#84051,#84052,#84053,#84054),(#84055,#84056,
#84057,#84058)),.UNSPECIFIED.,.F.,.F.,.F.,(4,4),(4,4),(0.52209712019902,
1.00286848452579),(0.0400218729465707,0.0466073985929451),.UNSPECIFIED.);
#2584=B_SPLINE_SURFACE_WITH_KNOTS('',3,3,((#84127,#84128,#84129,#84130),
(#84131,#84132,#84133,#84134),(#84135,#84136,#84137,#84138),(#84139,#84140,
#84141,#84142)),.UNSPECIFIED.,.F.,.F.,.F.,(4,4),(4,4),(0.522097120199269,
1.00286862201159),(0.0300094532292162,0.0365944846647032),.UNSPECIFIED.);
#2585=B_SPLINE_SURFACE_WITH_KNOTS('',3,3,((#84175,#84176,#84177,#84178),
(#84179,#84180,#84181,#84182),(#84183,#84184,#84185,#84186),(#84187,#84188,
#84189,#84190)),.UNSPECIFIED.,.F.,.F.,.F.,(4,4),(4,4),(-0.00600003962464963,
1.00000000356543),(0.0166015299238286,0.026590734618064),.UNSPECIFIED.);
#2586=B_SPLINE_SURFACE_WITH_KNOTS('',3,3,((#84202,#84203,#84204,#84205),
(#84206,#84207,#84208,#84209),(#84210,#84211,#84212,#84213),(#84214,#84215,
#84216,#84217)),.UNSPECIFIED.,.F.,.F.,.F.,(4,4),(4,4),(0.522097120200225,
1.00286780410463),(0.0200175229646515,0.0265907346180643),.UNSPECIFIED.);
#2587=B_SPLINE_SURFACE_WITH_KNOTS('',3,3,((#84273,#84274,#84275,#84276),
(#84277,#84278,#84279,#84280),(#84281,#84282,#84283,#84284),(#84285,#84286,
#84287,#84288)),.UNSPECIFIED.,.F.,.F.,.F.,(4,4),(4,4),(0.522097120200841,
1.00286791014282),(0.0100271466749316,0.0166015302184268),.UNSPECIFIED.);
#2588=B_SPLINE_SURFACE_WITH_KNOTS('',3,3,((#84314,#84315,#84316,#84317),
(#84318,#84319,#84320,#84321),(#84322,#84323,#84324,#84325),(#84326,#84327,
#84328,#84329)),.UNSPECIFIED.,.F.,.F.,.F.,(4,4),(4,4),(-0.00017189542728392,
1.00600020634822),(0.0665898698856043,0.0751325481051806),.UNSPECIFIED.);
#2589=B_SPLINE_SURFACE_WITH_KNOTS('',3,3,((#84345,#84346,#84347,#84348),
(#84349,#84350,#84351,#84352),(#84353,#84354,#84355,#84356),(#84357,#84358,
#84359,#84360)),.UNSPECIFIED.,.F.,.F.,.F.,(4,4),(4,4),(-0.00286833998600279,
0.47790287979949),(0.0665898698862503,0.0731716198748491),.UNSPECIFIED.);
#2590=B_SPLINE_SURFACE_WITH_KNOTS('',3,3,((#84394,#84395,#84396,#84397),
(#84398,#84399,#84400,#84401),(#84402,#84403,#84404,#84405),(#84406,#84407,
#84408,#84409)),.UNSPECIFIED.,.F.,.F.,.F.,(4,4),(4,4),(0.522097120197419,
1.00286791825534),(0.0600156865486943,0.0665898700060139),.UNSPECIFIED.);
#2591=B_SPLINE_SURFACE_WITH_KNOTS('',3,3,((#84419,#84420,#84421,#84422),
(#84423,#84424,#84425,#84426),(#84427,#84428,#84429,#84430),(#84431,#84432,
#84433,#84434)),.UNSPECIFIED.,.F.,.F.,.F.,(4,4),(4,4),(-0.00286764392029051,
0.477902879798242),(0.0565997133101205,0.0631721430887056),
 .UNSPECIFIED.);
#2592=B_SPLINE_SURFACE_WITH_KNOTS('',3,3,((#84471,#84472,#84473,#84474),
(#84475,#84476,#84477,#84478),(#84479,#84480,#84481,#84482),(#84483,#84484,
#84485,#84486)),.UNSPECIFIED.,.F.,.F.,.F.,(4,4),(4,4),(0.522097120197909,
1.00286780122208),(0.0500263550858677,0.0565997133101417),.UNSPECIFIED.);
#2593=B_SPLINE_SURFACE_WITH_KNOTS('',3,3,((#84558,#84559,#84560,#84561),
(#84562,#84563,#84564,#84565),(#84566,#84567,#84568,#84569),(#84570,#84571,
#84572,#84573)),.UNSPECIFIED.,.F.,.F.,.F.,(4,4),(4,4),(0.522097120198037,
1.00286848452582),(0.0400218729465713,0.0466073985929447),.UNSPECIFIED.);
#2594=B_SPLINE_SURFACE_WITH_KNOTS('',3,3,((#84642,#84643,#84644,#84645),
(#84646,#84647,#84648,#84649),(#84650,#84651,#84652,#84653),(#84654,#84655,
#84656,#84657)),.UNSPECIFIED.,.F.,.F.,.F.,(4,4),(4,4),(0.522097120198327,
1.00286862201147),(0.0300094532292163,0.0365944846647041),.UNSPECIFIED.);
#2595=B_SPLINE_SURFACE_WITH_KNOTS('',3,3,((#84690,#84691,#84692,#84693),
(#84694,#84695,#84696,#84697),(#84698,#84699,#84700,#84701),(#84702,#84703,
#84704,#84705)),.UNSPECIFIED.,.F.,.F.,.F.,(4,4),(4,4),(-0.00600003962474401,
1.00000000356551),(0.0166015299238287,0.0265907346180634),.UNSPECIFIED.);
#2596=B_SPLINE_SURFACE_WITH_KNOTS('',3,3,((#84717,#84718,#84719,#84720),
(#84721,#84722,#84723,#84724),(#84725,#84726,#84727,#84728),(#84729,#84730,
#84731,#84732)),.UNSPECIFIED.,.F.,.F.,.F.,(4,4),(4,4),(0.522097120199008,
1.00286780410468),(0.020017522964651,0.0265907346180643),.UNSPECIFIED.);
#2597=B_SPLINE_SURFACE_WITH_KNOTS('',3,3,((#84788,#84789,#84790,#84791),
(#84792,#84793,#84794,#84795),(#84796,#84797,#84798,#84799),(#84800,#84801,
#84802,#84803)),.UNSPECIFIED.,.F.,.F.,.F.,(4,4),(4,4),(0.522097120199533,
1.00286791014275),(0.0100271466749321,0.0166015302184269),.UNSPECIFIED.);
#2598=B_SPLINE_SURFACE_WITH_KNOTS('',3,3,((#84829,#84830,#84831,#84832),
(#84833,#84834,#84835,#84836),(#84837,#84838,#84839,#84840),(#84841,#84842,
#84843,#84844)),.UNSPECIFIED.,.F.,.F.,.F.,(4,4),(4,4),(-0.000171895427232253,
1.00600020634838),(0.0665898698856038,0.0751325481051289),.UNSPECIFIED.);
#2599=B_SPLINE_SURFACE_WITH_KNOTS('',3,3,((#84860,#84861,#84862,#84863),
(#84864,#84865,#84866,#84867),(#84868,#84869,#84870,#84871),(#84872,#84873,
#84874,#84875)),.UNSPECIFIED.,.F.,.F.,.F.,(4,4),(4,4),(-0.00286833998594681,
0.477902879801946),(0.0665898698862508,0.0731716198748497),
 .UNSPECIFIED.);
#2600=B_SPLINE_SURFACE_WITH_KNOTS('',3,3,((#84909,#84910,#84911,#84912),
(#84913,#84914,#84915,#84916),(#84917,#84918,#84919,#84920),(#84921,#84922,
#84923,#84924)),.UNSPECIFIED.,.F.,.F.,.F.,(4,4),(4,4),(0.522097120197177,
1.00286791825534),(0.0600156865486938,0.0665898700060139),.UNSPECIFIED.);
#2601=B_SPLINE_SURFACE_WITH_KNOTS('',3,3,((#84934,#84935,#84936,#84937),
(#84938,#84939,#84940,#84941),(#84942,#84943,#84944,#84945),(#84946,#84947,
#84948,#84949)),.UNSPECIFIED.,.F.,.F.,.F.,(4,4),(4,4),(-0.00286764392033648,
0.477902879800479),(0.056599713310121,0.0631721430887073),.UNSPECIFIED.);
#2602=B_SPLINE_SURFACE_WITH_KNOTS('',3,3,((#84986,#84987,#84988,#84989),
(#84990,#84991,#84992,#84993),(#84994,#84995,#84996,#84997),(#84998,#84999,
#85000,#85001)),.UNSPECIFIED.,.F.,.F.,.F.,(4,4),(4,4),(0.522097120197487,
1.00286780122204),(0.0500263550858663,0.0565997133101417),.UNSPECIFIED.);
#2603=B_SPLINE_SURFACE_WITH_KNOTS('',3,3,((#85073,#85074,#85075,#85076),
(#85077,#85078,#85079,#85080),(#85081,#85082,#85083,#85084),(#85085,#85086,
#85087,#85088)),.UNSPECIFIED.,.F.,.F.,.F.,(4,4),(4,4),(0.522097120197465,
1.00286848452583),(0.0400218729465712,0.0466073985929438),.UNSPECIFIED.);
#2604=B_SPLINE_SURFACE_WITH_KNOTS('',3,3,((#85157,#85158,#85159,#85160),
(#85161,#85162,#85163,#85164),(#85165,#85166,#85167,#85168),(#85169,#85170,
#85171,#85172)),.UNSPECIFIED.,.F.,.F.,.F.,(4,4),(4,4),(0.52209712019751,
1.00286862201153),(0.030009453229217,0.0365944846647047),.UNSPECIFIED.);
#2605=B_SPLINE_SURFACE_WITH_KNOTS('',3,3,((#85205,#85206,#85207,#85208),
(#85209,#85210,#85211,#85212),(#85213,#85214,#85215,#85216),(#85217,#85218,
#85219,#85220)),.UNSPECIFIED.,.F.,.F.,.F.,(4,4),(4,4),(-0.00600003961810723,
1.00000000246924),(0.0166015299238289,0.0265907346180637),.UNSPECIFIED.);
#2606=B_SPLINE_SURFACE_WITH_KNOTS('',3,3,((#85232,#85233,#85234,#85235),
(#85236,#85237,#85238,#85239),(#85240,#85241,#85242,#85243),(#85244,#85245,
#85246,#85247)),.UNSPECIFIED.,.F.,.F.,.F.,(4,4),(4,4),(0.522097120198131,
1.00286780410467),(0.020017522964652,0.0265907346180655),.UNSPECIFIED.);
#2607=B_SPLINE_SURFACE_WITH_KNOTS('',3,3,((#85303,#85304,#85305,#85306),
(#85307,#85308,#85309,#85310),(#85311,#85312,#85313,#85314),(#85315,#85316,
#85317,#85318)),.UNSPECIFIED.,.F.,.F.,.F.,(4,4),(4,4),(0.522097120198457,
1.00286791014282),(0.0100271466749326,0.0166015302184268),.UNSPECIFIED.);
#2608=B_SPLINE_SURFACE_WITH_KNOTS('',3,3,((#85344,#85345,#85346,#85347),
(#85348,#85349,#85350,#85351),(#85352,#85353,#85354,#85355),(#85356,#85357,
#85358,#85359)),.UNSPECIFIED.,.F.,.F.,.F.,(4,4),(4,4),(-0.000171895427308574,
1.00600020634819),(0.0665898698856039,0.075132548105205),.UNSPECIFIED.);
#2609=B_SPLINE_SURFACE_WITH_KNOTS('',3,3,((#85375,#85376,#85377,#85378),
(#85379,#85380,#85381,#85382),(#85383,#85384,#85385,#85386),(#85387,#85388,
#85389,#85390)),.UNSPECIFIED.,.F.,.F.,.F.,(4,4),(4,4),(-0.00286833998600449,
0.477902879804012),(0.0665898698862502,0.0731716198748502),
 .UNSPECIFIED.);
#2610=B_SPLINE_SURFACE_WITH_KNOTS('',3,3,((#85424,#85425,#85426,#85427),
(#85428,#85429,#85430,#85431),(#85432,#85433,#85434,#85435),(#85436,#85437,
#85438,#85439)),.UNSPECIFIED.,.F.,.F.,.F.,(4,4),(4,4),(0.522097120197181,
1.00286791825527),(0.060015686548694,0.0665898700060143),.UNSPECIFIED.);
#2611=B_SPLINE_SURFACE_WITH_KNOTS('',3,3,((#85449,#85450,#85451,#85452),
(#85453,#85454,#85455,#85456),(#85457,#85458,#85459,#85460),(#85461,#85462,
#85463,#85464)),.UNSPECIFIED.,.F.,.F.,.F.,(4,4),(4,4),(-0.0028676439203597,
0.477902879802986),(0.0565997133101214,0.0631721430887067),
 .UNSPECIFIED.);
#2612=B_SPLINE_SURFACE_WITH_KNOTS('',3,3,((#85501,#85502,#85503,#85504),
(#85505,#85506,#85507,#85508),(#85509,#85510,#85511,#85512),(#85513,#85514,
#85515,#85516)),.UNSPECIFIED.,.F.,.F.,.F.,(4,4),(4,4),(0.522097120197347,
1.00286780122201),(0.050026355085867,0.0565997133101426),.UNSPECIFIED.);
#2613=B_SPLINE_SURFACE_WITH_KNOTS('',3,3,((#85588,#85589,#85590,#85591),
(#85592,#85593,#85594,#85595),(#85596,#85597,#85598,#85599),(#85600,#85601,
#85602,#85603)),.UNSPECIFIED.,.F.,.F.,.F.,(4,4),(4,4),(0.522097120197233,
1.00286848452581),(0.0400218729465715,0.0466073985929451),.UNSPECIFIED.);
#2614=B_SPLINE_SURFACE_WITH_KNOTS('',3,3,((#85672,#85673,#85674,#85675),
(#85676,#85677,#85678,#85679),(#85680,#85681,#85682,#85683),(#85684,#85685,
#85686,#85687)),.UNSPECIFIED.,.F.,.F.,.F.,(4,4),(4,4),(0.522097120197018,
1.0028686220116),(0.0300094532292167,0.0365944846647034),.UNSPECIFIED.);
#2615=B_SPLINE_SURFACE_WITH_KNOTS('',3,3,((#85720,#85721,#85722,#85723),
(#85724,#85725,#85726,#85727),(#85728,#85729,#85730,#85731),(#85732,#85733,
#85734,#85735)),.UNSPECIFIED.,.F.,.F.,.F.,(4,4),(4,4),(-0.00600003961809443,
1.00000000246919),(0.0166015299238287,0.0265907346180648),.UNSPECIFIED.);
#2616=B_SPLINE_SURFACE_WITH_KNOTS('',3,3,((#85747,#85748,#85749,#85750),
(#85751,#85752,#85753,#85754),(#85755,#85756,#85757,#85758),(#85759,#85760,
#85761,#85762)),.UNSPECIFIED.,.F.,.F.,.F.,(4,4),(4,4),(0.522097120197489,
1.00286780410464),(0.020017522964652,0.0265907346180644),.UNSPECIFIED.);
#2617=B_SPLINE_SURFACE_WITH_KNOTS('',3,3,((#85818,#85819,#85820,#85821),
(#85822,#85823,#85824,#85825),(#85826,#85827,#85828,#85829),(#85830,#85831,
#85832,#85833)),.UNSPECIFIED.,.F.,.F.,.F.,(4,4),(4,4),(0.522097120197819,
1.00286791014287),(0.010027146674932,0.0166015302184279),.UNSPECIFIED.);
#2618=B_SPLINE_SURFACE_WITH_KNOTS('',3,3,((#85859,#85860,#85861,#85862),
(#85863,#85864,#85865,#85866),(#85867,#85868,#85869,#85870),(#85871,#85872,
#85873,#85874)),.UNSPECIFIED.,.F.,.F.,.F.,(4,4),(4,4),(-0.000171895427393694,
1.00600020634845),(0.0665898698856037,0.0751325481052895),.UNSPECIFIED.);
#2619=B_SPLINE_SURFACE_WITH_KNOTS('',3,3,((#85890,#85891,#85892,#85893),
(#85894,#85895,#85896,#85897),(#85898,#85899,#85900,#85901),(#85902,#85903,
#85904,#85905)),.UNSPECIFIED.,.F.,.F.,.F.,(4,4),(4,4),(-0.00286833998598056,
0.47790287980605),(0.0665898698862503,0.07317161987485),.UNSPECIFIED.);
#2620=B_SPLINE_SURFACE_WITH_KNOTS('',3,3,((#85939,#85940,#85941,#85942),
(#85943,#85944,#85945,#85946),(#85947,#85948,#85949,#85950),(#85951,#85952,
#85953,#85954)),.UNSPECIFIED.,.F.,.F.,.F.,(4,4),(4,4),(0.522097120197503,
1.00286791825538),(0.0600156865486932,0.066589870006015),.UNSPECIFIED.);
#2621=B_SPLINE_SURFACE_WITH_KNOTS('',3,3,((#85964,#85965,#85966,#85967),
(#85968,#85969,#85970,#85971),(#85972,#85973,#85974,#85975),(#85976,#85977,
#85978,#85979)),.UNSPECIFIED.,.F.,.F.,.F.,(4,4),(4,4),(-0.00286764392038191,
0.477902879804341),(0.0565997133101219,0.063172143088707),.UNSPECIFIED.);
#2622=B_SPLINE_SURFACE_WITH_KNOTS('',3,3,((#86016,#86017,#86018,#86019),
(#86020,#86021,#86022,#86023),(#86024,#86025,#86026,#86027),(#86028,#86029,
#86030,#86031)),.UNSPECIFIED.,.F.,.F.,.F.,(4,4),(4,4),(0.522097120197698,
1.00286780122194),(0.0500263550858669,0.0565997133101426),.UNSPECIFIED.);
#2623=B_SPLINE_SURFACE_WITH_KNOTS('',3,3,((#86103,#86104,#86105,#86106),
(#86107,#86108,#86109,#86110),(#86111,#86112,#86113,#86114),(#86115,#86116,
#86117,#86118)),.UNSPECIFIED.,.F.,.F.,.F.,(4,4),(4,4),(0.522097120197408,
1.00286848452587),(0.0400218729465692,0.0466073985929454),.UNSPECIFIED.);
#2624=B_SPLINE_SURFACE_WITH_KNOTS('',3,3,((#86187,#86188,#86189,#86190),
(#86191,#86192,#86193,#86194),(#86195,#86196,#86197,#86198),(#86199,#86200,
#86201,#86202)),.UNSPECIFIED.,.F.,.F.,.F.,(4,4),(4,4),(0.522097120197092,
1.00286862201155),(0.0300094532292162,0.0365944846647039),.UNSPECIFIED.);
#2625=B_SPLINE_SURFACE_WITH_KNOTS('',3,3,((#86235,#86236,#86237,#86238),
(#86239,#86240,#86241,#86242),(#86243,#86244,#86245,#86246),(#86247,#86248,
#86249,#86250)),.UNSPECIFIED.,.F.,.F.,.F.,(4,4),(4,4),(-0.00600003961847192,
1.00000000246937),(0.0166015299238286,0.0265907346180649),.UNSPECIFIED.);
#2626=B_SPLINE_SURFACE_WITH_KNOTS('',3,3,((#86262,#86263,#86264,#86265),
(#86266,#86267,#86268,#86269),(#86270,#86271,#86272,#86273),(#86274,#86275,
#86276,#86277)),.UNSPECIFIED.,.F.,.F.,.F.,(4,4),(4,4),(0.522097120197192,
1.00286780410466),(0.020017522964651,0.0265907346180642),.UNSPECIFIED.);
#2627=B_SPLINE_SURFACE_WITH_KNOTS('',3,3,((#86333,#86334,#86335,#86336),
(#86337,#86338,#86339,#86340),(#86341,#86342,#86343,#86344),(#86345,#86346,
#86347,#86348)),.UNSPECIFIED.,.F.,.F.,.F.,(4,4),(4,4),(0.522097120197277,
1.00286791014289),(0.0100271466749306,0.0166015302184277),.UNSPECIFIED.);
#2628=B_SPLINE_SURFACE_WITH_KNOTS('',3,3,((#86374,#86375,#86376,#86377),
(#86378,#86379,#86380,#86381),(#86382,#86383,#86384,#86385),(#86386,#86387,
#86388,#86389)),.UNSPECIFIED.,.F.,.F.,.F.,(4,4),(4,4),(-0.000171895427889023,
1.00600020634831),(0.0665898698856037,0.0751325481057876),.UNSPECIFIED.);
#2629=B_SPLINE_SURFACE_WITH_KNOTS('',3,3,((#86405,#86406,#86407,#86408),
(#86409,#86410,#86411,#86412),(#86413,#86414,#86415,#86416),(#86417,#86418,
#86419,#86420)),.UNSPECIFIED.,.F.,.F.,.F.,(4,4),(4,4),(-0.00286833998599298,
0.477902879807884),(0.0665898698862499,0.0731716198748494),
 .UNSPECIFIED.);
#2630=B_SPLINE_SURFACE_WITH_KNOTS('',3,3,((#86454,#86455,#86456,#86457),
(#86458,#86459,#86460,#86461),(#86462,#86463,#86464,#86465),(#86466,#86467,
#86468,#86469)),.UNSPECIFIED.,.F.,.F.,.F.,(4,4),(4,4),(0.522097120198093,
1.00286791825529),(0.0600156865486939,0.0665898700060143),.UNSPECIFIED.);
#2631=B_SPLINE_SURFACE_WITH_KNOTS('',3,3,((#86479,#86480,#86481,#86482),
(#86483,#86484,#86485,#86486),(#86487,#86488,#86489,#86490),(#86491,#86492,
#86493,#86494)),.UNSPECIFIED.,.F.,.F.,.F.,(4,4),(4,4),(-0.00286764392039988,
0.477902879805311),(0.0565997133101209,0.0631721430887081),
 .UNSPECIFIED.);
#2632=B_SPLINE_SURFACE_WITH_KNOTS('',3,3,((#86531,#86532,#86533,#86534),
(#86535,#86536,#86537,#86538),(#86539,#86540,#86541,#86542),(#86543,#86544,
#86545,#86546)),.UNSPECIFIED.,.F.,.F.,.F.,(4,4),(4,4),(0.522097120198022,
1.00286780122197),(0.0500263550858675,0.0565997133101425),.UNSPECIFIED.);
#2633=B_SPLINE_SURFACE_WITH_KNOTS('',3,3,((#86618,#86619,#86620,#86621),
(#86622,#86623,#86624,#86625),(#86626,#86627,#86628,#86629),(#86630,#86631,
#86632,#86633)),.UNSPECIFIED.,.F.,.F.,.F.,(4,4),(4,4),(0.522097120197733,
1.00286848452573),(0.0400218729465702,0.046607398592945),.UNSPECIFIED.);
#2634=B_SPLINE_SURFACE_WITH_KNOTS('',3,3,((#86702,#86703,#86704,#86705),
(#86706,#86707,#86708,#86709),(#86710,#86711,#86712,#86713),(#86714,#86715,
#86716,#86717)),.UNSPECIFIED.,.F.,.F.,.F.,(4,4),(4,4),(0.522097120197201,
1.00286862201148),(0.0300094532292163,0.0365944846647032),.UNSPECIFIED.);
#2635=B_SPLINE_SURFACE_WITH_KNOTS('',3,3,((#86750,#86751,#86752,#86753),
(#86754,#86755,#86756,#86757),(#86758,#86759,#86760,#86761),(#86762,#86763,
#86764,#86765)),.UNSPECIFIED.,.F.,.F.,.F.,(4,4),(4,4),(-0.006000039618272,
1.00000000246948),(0.0166015299238286,0.0265907346180638),.UNSPECIFIED.);
#2636=B_SPLINE_SURFACE_WITH_KNOTS('',3,3,((#86777,#86778,#86779,#86780),
(#86781,#86782,#86783,#86784),(#86785,#86786,#86787,#86788),(#86789,#86790,
#86791,#86792)),.UNSPECIFIED.,.F.,.F.,.F.,(4,4),(4,4),(0.522097120197316,
1.00286780410477),(0.0200175229646532,0.0265907346180642),.UNSPECIFIED.);
#2637=B_SPLINE_SURFACE_WITH_KNOTS('',3,3,((#86848,#86849,#86850,#86851),
(#86852,#86853,#86854,#86855),(#86856,#86857,#86858,#86859),(#86860,#86861,
#86862,#86863)),.UNSPECIFIED.,.F.,.F.,.F.,(4,4),(4,4),(0.522097120197198,
1.00286791014281),(0.0100271466749316,0.0166015302184268),.UNSPECIFIED.);
#2638=B_SPLINE_SURFACE_WITH_KNOTS('',3,3,((#86889,#86890,#86891,#86892),
(#86893,#86894,#86895,#86896),(#86897,#86898,#86899,#86900),(#86901,#86902,
#86903,#86904)),.UNSPECIFIED.,.F.,.F.,.F.,(4,4),(4,4),(-0.000171895428070672,
1.00600020634857),(0.0665898698856042,0.0751325481059675),.UNSPECIFIED.);
#2639=B_SPLINE_SURFACE_WITH_KNOTS('',3,3,((#86920,#86921,#86922,#86923),
(#86924,#86925,#86926,#86927),(#86928,#86929,#86930,#86931),(#86932,#86933,
#86934,#86935)),.UNSPECIFIED.,.F.,.F.,.F.,(4,4),(4,4),(-0.00286833998598336,
0.47790287980941),(0.0665898698862507,0.0731716198748504),.UNSPECIFIED.);
#2640=B_SPLINE_SURFACE_WITH_KNOTS('',3,3,((#86969,#86970,#86971,#86972),
(#86973,#86974,#86975,#86976),(#86977,#86978,#86979,#86980),(#86981,#86982,
#86983,#86984)),.UNSPECIFIED.,.F.,.F.,.F.,(4,4),(4,4),(0.522097120199068,
1.00286791825529),(0.0600156865486931,0.0665898700060154),.UNSPECIFIED.);
#2641=B_SPLINE_SURFACE_WITH_KNOTS('',3,3,((#86994,#86995,#86996,#86997),
(#86998,#86999,#87000,#87001),(#87002,#87003,#87004,#87005),(#87006,#87007,
#87008,#87009)),.UNSPECIFIED.,.F.,.F.,.F.,(4,4),(4,4),(-0.00286764392030641,
0.477902879806162),(0.0565997133101207,0.0631721430887058),
 .UNSPECIFIED.);
#2642=B_SPLINE_SURFACE_WITH_KNOTS('',3,3,((#87046,#87047,#87048,#87049),
(#87050,#87051,#87052,#87053),(#87054,#87055,#87056,#87057),(#87058,#87059,
#87060,#87061)),.UNSPECIFIED.,.F.,.F.,.F.,(4,4),(4,4),(0.522097120198757,
1.00286780122195),(0.0500263550858673,0.0565997133101423),.UNSPECIFIED.);
#2643=B_SPLINE_SURFACE_WITH_KNOTS('',3,3,((#87133,#87134,#87135,#87136),
(#87137,#87138,#87139,#87140),(#87141,#87142,#87143,#87144),(#87145,#87146,
#87147,#87148)),.UNSPECIFIED.,.F.,.F.,.F.,(4,4),(4,4),(0.52209712019838,
1.00286848452582),(0.0400218729465696,0.046607398592946),.UNSPECIFIED.);
#2644=B_SPLINE_SURFACE_WITH_KNOTS('',3,3,((#87217,#87218,#87219,#87220),
(#87221,#87222,#87223,#87224),(#87225,#87226,#87227,#87228),(#87229,#87230,
#87231,#87232)),.UNSPECIFIED.,.F.,.F.,.F.,(4,4),(4,4),(0.522097120197711,
1.00286862201152),(0.0300094532292164,0.0365944846647043),.UNSPECIFIED.);
#2645=B_SPLINE_SURFACE_WITH_KNOTS('',3,3,((#87265,#87266,#87267,#87268),
(#87269,#87270,#87271,#87272),(#87273,#87274,#87275,#87276),(#87277,#87278,
#87279,#87280)),.UNSPECIFIED.,.F.,.F.,.F.,(4,4),(4,4),(-0.00600003964343286,
1.00000000663609),(0.0166015299238276,0.0265907346180635),.UNSPECIFIED.);
#2646=B_SPLINE_SURFACE_WITH_KNOTS('',3,3,((#87292,#87293,#87294,#87295),
(#87296,#87297,#87298,#87299),(#87300,#87301,#87302,#87303),(#87304,#87305,
#87306,#87307)),.UNSPECIFIED.,.F.,.F.,.F.,(4,4),(4,4),(0.522097120197779,
1.0028678041047),(0.0200175229646511,0.0265907346180654),.UNSPECIFIED.);
#2647=B_SPLINE_SURFACE_WITH_KNOTS('',3,3,((#87363,#87364,#87365,#87366),
(#87367,#87368,#87369,#87370),(#87371,#87372,#87373,#87374),(#87375,#87376,
#87377,#87378)),.UNSPECIFIED.,.F.,.F.,.F.,(4,4),(4,4),(0.52209712019753,
1.00286791014286),(0.0100271466749306,0.0166015302184279),.UNSPECIFIED.);
#2648=B_SPLINE_SURFACE_WITH_KNOTS('',3,3,((#87404,#87405,#87406,#87407),
(#87408,#87409,#87410,#87411),(#87412,#87413,#87414,#87415),(#87416,#87417,
#87418,#87419)),.UNSPECIFIED.,.F.,.F.,.F.,(4,4),(4,4),(-0.000171895428638224,
1.00600020634821),(0.0665898698856058,0.0751325481065355),.UNSPECIFIED.);
#2649=B_SPLINE_SURFACE_WITH_KNOTS('',3,3,((#87435,#87436,#87437,#87438),
(#87439,#87440,#87441,#87442),(#87443,#87444,#87445,#87446),(#87447,#87448,
#87449,#87450)),.UNSPECIFIED.,.F.,.F.,.F.,(4,4),(4,4),(-0.00286833998602934,
0.477902879810758),(0.0665898698862525,0.0731716198748499),
 .UNSPECIFIED.);
#2650=B_SPLINE_SURFACE_WITH_KNOTS('',3,3,((#87484,#87485,#87486,#87487),
(#87488,#87489,#87490,#87491),(#87492,#87493,#87494,#87495),(#87496,#87497,
#87498,#87499)),.UNSPECIFIED.,.F.,.F.,.F.,(4,4),(4,4),(0.522097120200412,
1.00286791825534),(0.0600156865486936,0.0665898700060149),.UNSPECIFIED.);
#2651=B_SPLINE_SURFACE_WITH_KNOTS('',3,3,((#87509,#87510,#87511,#87512),
(#87513,#87514,#87515,#87516),(#87517,#87518,#87519,#87520),(#87521,#87522,
#87523,#87524)),.UNSPECIFIED.,.F.,.F.,.F.,(4,4),(4,4),(-0.00286764392033235,
0.477902879806884),(0.0565997133101206,0.0631721430887058),
 .UNSPECIFIED.);
#2652=B_SPLINE_SURFACE_WITH_KNOTS('',3,3,((#87561,#87562,#87563,#87564),
(#87565,#87566,#87567,#87568),(#87569,#87570,#87571,#87572),(#87573,#87574,
#87575,#87576)),.UNSPECIFIED.,.F.,.F.,.F.,(4,4),(4,4),(0.522097120200083,
1.00286780122198),(0.0500263550858671,0.0565997133101428),.UNSPECIFIED.);
#2653=B_SPLINE_SURFACE_WITH_KNOTS('',3,3,((#87648,#87649,#87650,#87651),
(#87652,#87653,#87654,#87655),(#87656,#87657,#87658,#87659),(#87660,#87661,
#87662,#87663)),.UNSPECIFIED.,.F.,.F.,.F.,(4,4),(4,4),(0.522097120199211,
1.00286848452593),(0.0400218729465695,0.0466073985929449),.UNSPECIFIED.);
#2654=B_SPLINE_SURFACE_WITH_KNOTS('',3,3,((#87732,#87733,#87734,#87735),
(#87736,#87737,#87738,#87739),(#87740,#87741,#87742,#87743),(#87744,#87745,
#87746,#87747)),.UNSPECIFIED.,.F.,.F.,.F.,(4,4),(4,4),(0.522097120198449,
1.00286862201144),(0.0300094532292165,0.0365944846647043),.UNSPECIFIED.);
#2655=B_SPLINE_SURFACE_WITH_KNOTS('',3,3,((#87780,#87781,#87782,#87783),
(#87784,#87785,#87786,#87787),(#87788,#87789,#87790,#87791),(#87792,#87793,
#87794,#87795)),.UNSPECIFIED.,.F.,.F.,.F.,(4,4),(4,4),(-0.00600003961843867,
1.00000000246921),(0.0166015299238294,0.0265907346180654),.UNSPECIFIED.);
#2656=B_SPLINE_SURFACE_WITH_KNOTS('',3,3,((#87807,#87808,#87809,#87810),
(#87811,#87812,#87813,#87814),(#87815,#87816,#87817,#87818),(#87819,#87820,
#87821,#87822)),.UNSPECIFIED.,.F.,.F.,.F.,(4,4),(4,4),(0.522097120198335,
1.00286780410464),(0.020017522964651,0.0265907346180648),.UNSPECIFIED.);
#2657=B_SPLINE_SURFACE_WITH_KNOTS('',3,3,((#87878,#87879,#87880,#87881),
(#87882,#87883,#87884,#87885),(#87886,#87887,#87888,#87889),(#87890,#87891,
#87892,#87893)),.UNSPECIFIED.,.F.,.F.,.F.,(4,4),(4,4),(0.522097120198003,
1.00286791014296),(0.0100271466749305,0.0166015302184264),.UNSPECIFIED.);
#2658=B_SPLINE_SURFACE_WITH_KNOTS('',3,3,((#87928,#87929,#87930,#87931),
(#87932,#87933,#87934,#87935),(#87936,#87937,#87938,#87939),(#87940,#87941,
#87942,#87943)),.UNSPECIFIED.,.F.,.F.,.F.,(4,4),(4,4),(-0.000171895430464311,
1.00600020634802),(0.0665898698856059,0.075132548107472),.UNSPECIFIED.);
#2659=B_SPLINE_SURFACE_WITH_KNOTS('',3,3,((#87959,#87960,#87961,#87962),
(#87963,#87964,#87965,#87966),(#87967,#87968,#87969,#87970),(#87971,#87972,
#87973,#87974)),.UNSPECIFIED.,.F.,.F.,.F.,(4,4),(4,4),(-0.00286833998604501,
0.477902879811737),(0.0665898698862518,0.0731716198748509),
 .UNSPECIFIED.);
#2660=B_SPLINE_SURFACE_WITH_KNOTS('',3,3,((#87999,#88000,#88001,#88002),
(#88003,#88004,#88005,#88006),(#88007,#88008,#88009,#88010),(#88011,#88012,
#88013,#88014)),.UNSPECIFIED.,.F.,.F.,.F.,(4,4),(4,4),(0.522097120201955,
1.00286791825535),(0.060015686548694,0.0665898700060146),.UNSPECIFIED.);
#2661=B_SPLINE_SURFACE_WITH_KNOTS('',3,3,((#88024,#88025,#88026,#88027),
(#88028,#88029,#88030,#88031),(#88032,#88033,#88034,#88035),(#88036,#88037,
#88038,#88039)),.UNSPECIFIED.,.F.,.F.,.F.,(4,4),(4,4),(-0.00286764392031658,
0.477902879807482),(0.0565997133101202,0.0631721430887052),
 .UNSPECIFIED.);
#2662=B_SPLINE_SURFACE_WITH_KNOTS('',3,3,((#88076,#88077,#88078,#88079),
(#88080,#88081,#88082,#88083),(#88084,#88085,#88086,#88087),(#88088,#88089,
#88090,#88091)),.UNSPECIFIED.,.F.,.F.,.F.,(4,4),(4,4),(0.522097120201401,
1.00286780122214),(0.050026355085846,0.0565997133136308),.UNSPECIFIED.);
#2663=B_SPLINE_SURFACE_WITH_KNOTS('',3,3,((#88163,#88164,#88165,#88166),
(#88167,#88168,#88169,#88170),(#88171,#88172,#88173,#88174),(#88175,#88176,
#88177,#88178)),.UNSPECIFIED.,.F.,.F.,.F.,(4,4),(4,4),(0.522097120200645,
1.0028684845258),(0.0400218729465706,0.046607398592945),.UNSPECIFIED.);
#2664=B_SPLINE_SURFACE_WITH_KNOTS('',3,3,((#88247,#88248,#88249,#88250),
(#88251,#88252,#88253,#88254),(#88255,#88256,#88257,#88258),(#88259,#88260,
#88261,#88262)),.UNSPECIFIED.,.F.,.F.,.F.,(4,4),(4,4),(0.52209712019984,
1.00286862201161),(0.030009453229216,0.0365944846647042),.UNSPECIFIED.);
#2665=B_SPLINE_SURFACE_WITH_KNOTS('',3,3,((#88295,#88296,#88297,#88298),
(#88299,#88300,#88301,#88302),(#88303,#88304,#88305,#88306),(#88307,#88308,
#88309,#88310)),.UNSPECIFIED.,.F.,.F.,.F.,(4,4),(4,4),(-0.00600003964349658,
1.00000000663616),(0.0166015299238282,0.0265907346180646),.UNSPECIFIED.);
#2666=B_SPLINE_SURFACE_WITH_KNOTS('',3,3,((#88322,#88323,#88324,#88325),
(#88326,#88327,#88328,#88329),(#88330,#88331,#88332,#88333),(#88334,#88335,
#88336,#88337)),.UNSPECIFIED.,.F.,.F.,.F.,(4,4),(4,4),(0.522097120199433,
1.00286780410456),(0.0200175229646522,0.0265907346180651),.UNSPECIFIED.);
#2667=B_SPLINE_SURFACE_WITH_KNOTS('',3,3,((#88393,#88394,#88395,#88396),
(#88397,#88398,#88399,#88400),(#88401,#88402,#88403,#88404),(#88405,#88406,
#88407,#88408)),.UNSPECIFIED.,.F.,.F.,.F.,(4,4),(4,4),(0.522097120198737,
1.00286791014283),(0.0100271466749313,0.0166015302184274),.UNSPECIFIED.);
#2668=B_SPLINE_SURFACE_WITH_KNOTS('',3,3,((#88452,#88453,#88454,#88455),
(#88456,#88457,#88458,#88459),(#88460,#88461,#88462,#88463),(#88464,#88465,
#88466,#88467)),.UNSPECIFIED.,.F.,.F.,.F.,(4,4),(4,4),(-0.00017189543000408,
1.00600020634828),(0.0665898698856059,0.0751325481078998),.UNSPECIFIED.);
#2669=B_SPLINE_SURFACE_WITH_KNOTS('',3,3,((#88483,#88484,#88485,#88486),
(#88487,#88488,#88489,#88490),(#88491,#88492,#88493,#88494),(#88495,#88496,
#88497,#88498)),.UNSPECIFIED.,.F.,.F.,.F.,(4,4),(4,4),(-0.00286833998600284,
0.47790287981238),(0.0665898698862513,0.0731716198748498),.UNSPECIFIED.);
#2670=B_SPLINE_SURFACE_WITH_KNOTS('',3,3,((#88526,#88527,#88528,#88529),
(#88530,#88531,#88532,#88533),(#88534,#88535,#88536,#88537),(#88538,#88539,
#88540,#88541)),.UNSPECIFIED.,.F.,.F.,.F.,(4,4),(4,4),(0.522097120203743,
1.00286791825528),(0.0600156865486936,0.0665898700060145),.UNSPECIFIED.);
#2671=B_SPLINE_SURFACE_WITH_KNOTS('',3,3,((#88551,#88552,#88553,#88554),
(#88555,#88556,#88557,#88558),(#88559,#88560,#88561,#88562),(#88563,#88564,
#88565,#88566)),.UNSPECIFIED.,.F.,.F.,.F.,(4,4),(4,4),(-0.00286764392046435,
0.477902879807759),(0.0565997133101208,0.0631721430887072),
 .UNSPECIFIED.);
#2672=B_SPLINE_SURFACE_WITH_KNOTS('',3,3,((#88591,#88592,#88593,#88594),
(#88595,#88596,#88597,#88598),(#88599,#88600,#88601,#88602),(#88603,#88604,
#88605,#88606)),.UNSPECIFIED.,.F.,.F.,.F.,(4,4),(4,4),(0.522097120203084,
1.00286780122204),(0.0500263550858665,0.0565997133101422),.UNSPECIFIED.);
#2673=B_SPLINE_SURFACE_WITH_KNOTS('',3,3,((#88614,#88615,#88616,#88617),
(#88618,#88619,#88620,#88621),(#88622,#88623,#88624,#88625),(#88626,#88627,
#88628,#88629)),.UNSPECIFIED.,.F.,.F.,.F.,(4,4),(4,4),(-0.00286810177351089,
0.477902879811734),(0.046607398592912,0.0531834933545505),.UNSPECIFIED.);
#2674=B_SPLINE_SURFACE_WITH_KNOTS('',3,3,((#88685,#88686,#88687,#88688),
(#88689,#88690,#88691,#88692),(#88693,#88694,#88695,#88696),(#88697,#88698,
#88699,#88700)),.UNSPECIFIED.,.F.,.F.,.F.,(4,4),(4,4),(0.522097120202046,
1.00286848452576),(0.0400218729465706,0.046607398592945),.UNSPECIFIED.);
#2675=B_SPLINE_SURFACE_WITH_KNOTS('',3,3,((#88769,#88770,#88771,#88772),
(#88773,#88774,#88775,#88776),(#88777,#88778,#88779,#88780),(#88781,#88782,
#88783,#88784)),.UNSPECIFIED.,.F.,.F.,.F.,(4,4),(4,4),(0.522097120201246,
1.0028686220115),(0.0300094532292166,0.0365944846647037),.UNSPECIFIED.);
#2676=B_SPLINE_SURFACE_WITH_KNOTS('',3,3,((#88817,#88818,#88819,#88820),
(#88821,#88822,#88823,#88824),(#88825,#88826,#88827,#88828),(#88829,#88830,
#88831,#88832)),.UNSPECIFIED.,.F.,.F.,.F.,(4,4),(4,4),(-0.00600003961857937,
1.00000000246931),(0.0166015299238284,0.0265907346180637),.UNSPECIFIED.);
#2677=B_SPLINE_SURFACE_WITH_KNOTS('',3,3,((#88844,#88845,#88846,#88847),
(#88848,#88849,#88850,#88851),(#88852,#88853,#88854,#88855),(#88856,#88857,
#88858,#88859)),.UNSPECIFIED.,.F.,.F.,.F.,(4,4),(4,4),(0.522097120200689,
1.00286780410456),(0.0200175229646513,0.0265907346180651),.UNSPECIFIED.);
#2678=B_SPLINE_SURFACE_WITH_KNOTS('',3,3,((#88915,#88916,#88917,#88918),
(#88919,#88920,#88921,#88922),(#88923,#88924,#88925,#88926),(#88927,#88928,
#88929,#88930)),.UNSPECIFIED.,.F.,.F.,.F.,(4,4),(4,4),(0.522097120199946,
1.00286791014292),(0.0100271466749312,0.0166015302184281),.UNSPECIFIED.);
#2679=B_SPLINE_SURFACE_WITH_KNOTS('',3,3,((#89000,#89001,#89002,#89003),
(#89004,#89005,#89006,#89007),(#89008,#89009,#89010,#89011),(#89012,#89013,
#89014,#89015)),.UNSPECIFIED.,.F.,.F.,.F.,(4,4),(4,4),(0.522097120206275,
1.00286791825534),(0.0600156865486935,0.0665898700060147),.UNSPECIFIED.);
#2680=B_SPLINE_SURFACE_WITH_KNOTS('',3,3,((#89025,#89026,#89027,#89028),
(#89029,#89030,#89031,#89032),(#89033,#89034,#89035,#89036),(#89037,#89038,
#89039,#89040)),.UNSPECIFIED.,.F.,.F.,.F.,(4,4),(4,4),(-0.00286764392045874,
0.477902879808112),(0.0565997133101205,0.0631721430887073),
 .UNSPECIFIED.);
#2681=B_SPLINE_SURFACE_WITH_KNOTS('',3,3,((#89071,#89072,#89073,#89074),
(#89075,#89076,#89077,#89078),(#89079,#89080,#89081,#89082),(#89083,#89084,
#89085,#89086)),.UNSPECIFIED.,.F.,.F.,.F.,(4,4),(4,4),(0.522097120204885,
1.00286780122186),(0.0500263550858663,0.0565997133101424),.UNSPECIFIED.);
#2682=B_SPLINE_SURFACE_WITH_KNOTS('',3,3,((#89110,#89111,#89112,#89113),
(#89114,#89115,#89116,#89117),(#89118,#89119,#89120,#89121),(#89122,#89123,
#89124,#89125)),.UNSPECIFIED.,.F.,.F.,.F.,(4,4),(4,4),(-0.00600014643596561,
1.),(0.036594484664054,0.0466073985929448),.UNSPECIFIED.);
#2683=B_SPLINE_SURFACE_WITH_KNOTS('',3,3,((#89148,#89149,#89150,#89151),
(#89152,#89153,#89154,#89155),(#89156,#89157,#89158,#89159),(#89160,#89161,
#89162,#89163)),.UNSPECIFIED.,.F.,.F.,.F.,(4,4),(4,4),(0.522097120203888,
1.00286848452563),(0.0400218729465705,0.046607398592945),.UNSPECIFIED.);
#2684=B_SPLINE_SURFACE_WITH_KNOTS('',3,3,((#89220,#89221,#89222,#89223),
(#89224,#89225,#89226,#89227),(#89228,#89229,#89230,#89231),(#89232,#89233,
#89234,#89235)),.UNSPECIFIED.,.F.,.F.,.F.,(4,4),(4,4),(-0.00286833998611542,
0.477902879815673),(0.0665898698862504,0.0731716198748485),
 .UNSPECIFIED.);
#2685=B_SPLINE_SURFACE_WITH_KNOTS('',3,3,((#89274,#89275,#89276,#89277),
(#89278,#89279,#89280,#89281),(#89282,#89283,#89284,#89285),(#89286,#89287,
#89288,#89289)),.UNSPECIFIED.,.F.,.F.,.F.,(4,4),(4,4),(0.52209712020296,
1.00286862201167),(0.0300094532292166,0.0365944846647042),.UNSPECIFIED.);
#2686=B_SPLINE_SURFACE_WITH_KNOTS('',3,3,((#89322,#89323,#89324,#89325),
(#89326,#89327,#89328,#89329),(#89330,#89331,#89332,#89333),(#89334,#89335,
#89336,#89337)),.UNSPECIFIED.,.F.,.F.,.F.,(4,4),(4,4),(-0.00600003964364205,
1.00000000663609),(0.0166015299238285,0.0265907346180648),.UNSPECIFIED.);
#2687=B_SPLINE_SURFACE_WITH_KNOTS('',3,3,((#89349,#89350,#89351,#89352),
(#89353,#89354,#89355,#89356),(#89357,#89358,#89359,#89360),(#89361,#89362,
#89363,#89364)),.UNSPECIFIED.,.F.,.F.,.F.,(4,4),(4,4),(0.522097120202179,
1.00286780410463),(0.020017522964651,0.026590734618065),.UNSPECIFIED.);
#2688=B_SPLINE_SURFACE_WITH_KNOTS('',3,3,((#89420,#89421,#89422,#89423),
(#89424,#89425,#89426,#89427),(#89428,#89429,#89430,#89431),(#89432,#89433,
#89434,#89435)),.UNSPECIFIED.,.F.,.F.,.F.,(4,4),(4,4),(0.522097120201302,
1.00286791014286),(0.0100271466749303,0.0166015302184269),.UNSPECIFIED.);
#2689=B_SPLINE_SURFACE_WITH_KNOTS('',3,3,((#89524,#89525,#89526,#89527),
(#89528,#89529,#89530,#89531),(#89532,#89533,#89534,#89535),(#89536,#89537,
#89538,#89539)),.UNSPECIFIED.,.F.,.F.,.F.,(4,4),(4,4),(0.52209712020732,
1.00286780122193),(0.050026355085867,0.0565997133101424),.UNSPECIFIED.);
#2690=B_SPLINE_SURFACE_WITH_KNOTS('',3,3,((#89547,#89548,#89549,#89550),
(#89551,#89552,#89553,#89554),(#89555,#89556,#89557,#89558),(#89559,#89560,
#89561,#89562)),.UNSPECIFIED.,.F.,.F.,.F.,(4,4),(4,4),(-0.00286810177367121,
0.477902879812735),(0.046607398592912,0.0531834933545511),.UNSPECIFIED.);
#2691=B_SPLINE_SURFACE_WITH_KNOTS('',3,3,((#89614,#89615,#89616,#89617),
(#89618,#89619,#89620,#89621),(#89622,#89623,#89624,#89625),(#89626,#89627,
#89628,#89629)),.UNSPECIFIED.,.F.,.F.,.F.,(4,4),(4,4),(0.522097120205853,
1.00286848452572),(0.0400218729465696,0.0466073985929448),.UNSPECIFIED.);
#2692=B_SPLINE_SURFACE_WITH_KNOTS('',3,3,((#89676,#89677,#89678,#89679),
(#89680,#89681,#89682,#89683),(#89684,#89685,#89686,#89687),(#89688,#89689,
#89690,#89691)),.UNSPECIFIED.,.F.,.F.,.F.,(4,4),(4,4),(0.52209712020468,
1.0028686220115),(0.0300094532292157,0.0365944846647038),.UNSPECIFIED.);
#2693=B_SPLINE_SURFACE_WITH_KNOTS('',3,3,((#89699,#89700,#89701,#89702),
(#89703,#89704,#89705,#89706),(#89707,#89708,#89709,#89710),(#89711,#89712,
#89713,#89714)),.UNSPECIFIED.,.F.,.F.,.F.,(4,4),(4,4),(-0.00286823356233573,
0.477902879812311),(0.0265907346180621,0.0331702037252922),
 .UNSPECIFIED.);
#2694=B_SPLINE_SURFACE_WITH_KNOTS('',3,3,((#89749,#89750,#89751,#89752),
(#89753,#89754,#89755,#89756),(#89757,#89758,#89759,#89760),(#89761,#89762,
#89763,#89764)),.UNSPECIFIED.,.F.,.F.,.F.,(4,4),(4,4),(-0.00286833998610001,
0.477902879812836),(0.0665898698862507,0.0731716198748494),
 .UNSPECIFIED.);
#2695=B_SPLINE_SURFACE_WITH_KNOTS('',3,3,((#89795,#89796,#89797,#89798),
(#89799,#89800,#89801,#89802),(#89803,#89804,#89805,#89806),(#89807,#89808,
#89809,#89810)),.UNSPECIFIED.,.F.,.F.,.F.,(4,4),(4,4),(0.522097120205365,
1.00286791825533),(0.0600156865486915,0.0665898700060128),.UNSPECIFIED.);
#2696=B_SPLINE_SURFACE_WITH_KNOTS('',3,3,((#89820,#89821,#89822,#89823),
(#89824,#89825,#89826,#89827),(#89828,#89829,#89830,#89831),(#89832,#89833,
#89834,#89835)),.UNSPECIFIED.,.F.,.F.,.F.,(4,4),(4,4),(-0.00286764392040503,
0.477902879811564),(0.0565997133101196,0.0631721430887057),
 .UNSPECIFIED.);
#2697=B_SPLINE_SURFACE_WITH_KNOTS('',3,3,((#89849,#89850,#89851,#89852),
(#89853,#89854,#89855,#89856),(#89857,#89858,#89859,#89860),(#89861,#89862,
#89863,#89864)),.UNSPECIFIED.,.F.,.F.,.F.,(4,4),(4,4),(-0.00600003962528381,
1.00000000356522),(0.0166015299238274,0.0265907346180631),.UNSPECIFIED.);
#2698=B_SPLINE_SURFACE_WITH_KNOTS('',3,3,((#89876,#89877,#89878,#89879),
(#89880,#89881,#89882,#89883),(#89884,#89885,#89886,#89887),(#89888,#89889,
#89890,#89891)),.UNSPECIFIED.,.F.,.F.,.F.,(4,4),(4,4),(0.522097120203962,
1.00286780410476),(0.0200175229646509,0.0265907346180654),.UNSPECIFIED.);
#2699=B_SPLINE_SURFACE_WITH_KNOTS('',3,3,((#89947,#89948,#89949,#89950),
(#89951,#89952,#89953,#89954),(#89955,#89956,#89957,#89958),(#89959,#89960,
#89961,#89962)),.UNSPECIFIED.,.F.,.F.,.F.,(4,4),(4,4),(0.52209712020327,
1.00286791014279),(0.0100271466749304,0.0166015302184271),.UNSPECIFIED.);
#2700=B_SPLINE_SURFACE_WITH_KNOTS('',3,3,((#90043,#90044,#90045,#90046),
(#90047,#90048,#90049,#90050),(#90051,#90052,#90053,#90054),(#90055,#90056,
#90057,#90058)),.UNSPECIFIED.,.F.,.F.,.F.,(4,4),(4,4),(-0.0060001464360308,
1.),(0.0365944846640544,0.0466073985929448),.UNSPECIFIED.);
#2701=B_SPLINE_SURFACE_WITH_KNOTS('',3,3,((#90081,#90082,#90083,#90084),
(#90085,#90086,#90087,#90088),(#90089,#90090,#90091,#90092),(#90093,#90094,
#90095,#90096)),.UNSPECIFIED.,.F.,.F.,.F.,(4,4),(4,4),(0.522097120208598,
1.00286848452568),(0.0400218729465714,0.0466073985929447),.UNSPECIFIED.);
#2702=B_SPLINE_SURFACE_WITH_KNOTS('',3,3,((#90144,#90145,#90146,#90147),
(#90148,#90149,#90150,#90151),(#90152,#90153,#90154,#90155),(#90156,#90157,
#90158,#90159)),.UNSPECIFIED.,.F.,.F.,.F.,(4,4),(4,4),(0.522097120206756,
1.00286862201145),(0.0300094532292163,0.0365944846647035),.UNSPECIFIED.);
#2703=B_SPLINE_SURFACE_WITH_KNOTS('',3,3,((#90183,#90184,#90185,#90186),
(#90187,#90188,#90189,#90190),(#90191,#90192,#90193,#90194),(#90195,#90196,
#90197,#90198)),.UNSPECIFIED.,.F.,.F.,.F.,(4,4),(4,4),(-0.00600003960396672,
1.),(0.0166015299238285,0.0265907346180638),.UNSPECIFIED.);
#2704=B_SPLINE_SURFACE_WITH_KNOTS('',3,3,((#90210,#90211,#90212,#90213),
(#90214,#90215,#90216,#90217),(#90218,#90219,#90220,#90221),(#90222,#90223,
#90224,#90225)),.UNSPECIFIED.,.F.,.F.,.F.,(4,4),(4,4),(0.522097120206069,
1.0028678041047),(0.0200175229646512,0.026590734618065),.UNSPECIFIED.);
#2705=B_SPLINE_SURFACE_WITH_KNOTS('',3,3,((#90233,#90234,#90235,#90236),
(#90237,#90238,#90239,#90240),(#90241,#90242,#90243,#90244),(#90245,#90246,
#90247,#90248)),.UNSPECIFIED.,.F.,.F.,.F.,(4,4),(4,4),(-0.00286753114062764,
0.477902879812649),(0.0166015299238962,0.0231736788090045),
 .UNSPECIFIED.);
#2706=B_SPLINE_SURFACE_WITH_KNOTS('',3,3,((#90259,#90260,#90261,#90262),
(#90263,#90264,#90265,#90266),(#90267,#90268,#90269,#90270),(#90271,#90272,
#90273,#90274)),.UNSPECIFIED.,.F.,.F.,.F.,(4,4),(4,4),(-0.000171895434491828,
1.00600020634819),(0.0665898698856031,0.0751325481108773),.UNSPECIFIED.);
#2707=B_SPLINE_SURFACE_WITH_KNOTS('',3,3,((#90329,#90330,#90331,#90332),
(#90333,#90334,#90335,#90336),(#90337,#90338,#90339,#90340),(#90341,#90342,
#90343,#90344)),.UNSPECIFIED.,.F.,.F.,.F.,(4,4),(4,4),(0.522097120206893,
1.00286791825543),(0.060015686548693,0.0665898700060125),.UNSPECIFIED.);
#2708=B_SPLINE_SURFACE_WITH_KNOTS('',3,3,((#90354,#90355,#90356,#90357),
(#90358,#90359,#90360,#90361),(#90362,#90363,#90364,#90365),(#90366,#90367,
#90368,#90369)),.UNSPECIFIED.,.F.,.F.,.F.,(4,4),(4,4),(-0.00286764392048026,
0.477902879808188),(0.056599713310119,0.0631721430887063),.UNSPECIFIED.);
#2709=B_SPLINE_SURFACE_WITH_KNOTS('',3,3,((#90400,#90401,#90402,#90403),
(#90404,#90405,#90406,#90407),(#90408,#90409,#90410,#90411),(#90412,#90413,
#90414,#90415)),.UNSPECIFIED.,.F.,.F.,.F.,(4,4),(4,4),(0.522097120206727,
1.00286780122188),(0.0500263550858663,0.0565997133101412),.UNSPECIFIED.);
#2710=B_SPLINE_SURFACE_WITH_KNOTS('',3,3,((#90468,#90469,#90470,#90471),
(#90472,#90473,#90474,#90475),(#90476,#90477,#90478,#90479),(#90480,#90481,
#90482,#90483)),.UNSPECIFIED.,.F.,.F.,.F.,(4,4),(4,4),(0.522097120204994,
1.0028679101427),(0.0100271466749314,0.0166015302184274),.UNSPECIFIED.);
#2711=B_SPLINE_SURFACE_WITH_KNOTS('',3,3,((#90589,#90590,#90591,#90592),
(#90593,#90594,#90595,#90596),(#90597,#90598,#90599,#90600),(#90601,#90602,
#90603,#90604)),.UNSPECIFIED.,.F.,.F.,.F.,(4,4),(4,4),(0.522097120209516,
1.00286862201142),(0.0300094532292164,0.0365944846647041),.UNSPECIFIED.);
#2712=B_SPLINE_SURFACE_WITH_KNOTS('',3,3,((#90612,#90613,#90614,#90615),
(#90616,#90617,#90618,#90619),(#90620,#90621,#90622,#90623),(#90624,#90625,
#90626,#90627)),.UNSPECIFIED.,.F.,.F.,.F.,(4,4),(4,4),(-0.00286823045920498,
0.477902879812828),(0.026590734618062,0.0331702036774536),.UNSPECIFIED.);
#2713=B_SPLINE_SURFACE_WITH_KNOTS('',3,3,((#90657,#90658,#90659,#90660),
(#90661,#90662,#90663,#90664),(#90665,#90666,#90667,#90668),(#90669,#90670,
#90671,#90672)),.UNSPECIFIED.,.F.,.F.,.F.,(4,4),(4,4),(0.522097120208285,
1.00286780410462),(0.0200175229646509,0.0265907346180644),.UNSPECIFIED.);
#2714=B_SPLINE_SURFACE_WITH_KNOTS('',3,3,((#90716,#90717,#90718,#90719),
(#90720,#90721,#90722,#90723),(#90724,#90725,#90726,#90727),(#90728,#90729,
#90730,#90731)),.UNSPECIFIED.,.F.,.F.,.F.,(4,4),(4,4),(0.522097120207253,
1.00286791014264),(0.0100271466749324,0.0166015302184276),.UNSPECIFIED.);
#2715=B_SPLINE_SURFACE_WITH_KNOTS('',3,3,((#90739,#90740,#90741,#90742),
(#90743,#90744,#90745,#90746),(#90747,#90748,#90749,#90750),(#90751,#90752,
#90753,#90754)),.UNSPECIFIED.,.F.,.F.,.F.,(4,4),(4,4),(-0.00206901892678166,
0.34676972851382),(0.00660713154702252,0.0131849431468904),
 .UNSPECIFIED.);
#2716=B_SPLINE_SURFACE_WITH_KNOTS('',3,3,((#90815,#90816,#90817,#90818),
(#90819,#90820,#90821,#90822),(#90823,#90824,#90825,#90826),(#90827,#90828,
#90829,#90830)),.UNSPECIFIED.,.F.,.F.,.F.,(4,4),(4,4),(0.522097120206813,
1.00286791825532),(0.0600156865486929,0.0665898700060134),.UNSPECIFIED.);
#2717=B_SPLINE_SURFACE_WITH_KNOTS('',3,3,((#90878,#90879,#90880,#90881),
(#90882,#90883,#90884,#90885),(#90886,#90887,#90888,#90889),(#90890,#90891,
#90892,#90893)),.UNSPECIFIED.,.F.,.F.,.F.,(4,4),(4,4),(0.522097120207726,
1.00286780122191),(0.0500263550858662,0.0565997133101415),.UNSPECIFIED.);
#2718=B_SPLINE_SURFACE_WITH_KNOTS('',3,3,((#90960,#90961,#90962,#90963),
(#90964,#90965,#90966,#90967),(#90968,#90969,#90970,#90971),(#90972,#90973,
#90974,#90975)),.UNSPECIFIED.,.F.,.F.,.F.,(4,4),(4,4),(0.522097120207574,
1.00286848452577),(0.0400218729465695,0.0466073985929437),.UNSPECIFIED.);
#2719=B_SPLINE_SURFACE_WITH_KNOTS('',3,3,((#91024,#91025,#91026,#91027),
(#91028,#91029,#91030,#91031),(#91032,#91033,#91034,#91035),(#91036,#91037,
#91038,#91039)),.UNSPECIFIED.,.F.,.F.,.F.,(4,4),(4,4),(0.522097120198755,
1.00286823669301),(0.0265907346180633,0.0331702036622765),.UNSPECIFIED.);
#2720=B_SPLINE_SURFACE_WITH_KNOTS('',3,3,((#91041,#91042,#91043,#91044),
(#91045,#91046,#91047,#91048),(#91049,#91050,#91051,#91052),(#91053,#91054,
#91055,#91056)),.UNSPECIFIED.,.F.,.F.,.F.,(4,4),(4,4),(-0.00286862201165793,
0.477902879801984),(0.0300094532292788,0.0365944846647005),
 .UNSPECIFIED.);
#2721=B_SPLINE_SURFACE_WITH_KNOTS('',3,3,((#91064,#91065,#91066,#91067),
(#91068,#91069,#91070,#91071),(#91072,#91073,#91074,#91075),(#91076,#91077,
#91078,#91079)),.UNSPECIFIED.,.F.,.F.,.F.,(4,4),(4,4),(-0.00286848453285561,
0.47790287980318),(0.0400218729466597,0.0466073985929426),.UNSPECIFIED.);
#2722=B_SPLINE_SURFACE_WITH_KNOTS('',3,3,((#91096,#91097,#91098,#91099),
(#91100,#91101,#91102,#91103),(#91104,#91105,#91106,#91107),(#91108,#91109,
#91110,#91111)),.UNSPECIFIED.,.F.,.F.,.F.,(4,4),(4,4),(0.,1.00600014639747),
(0.0365944846644987,0.046607398592915),.UNSPECIFIED.);
#2723=B_SPLINE_SURFACE_WITH_KNOTS('',3,3,((#91112,#91113,#91114,#91115),
(#91116,#91117,#91118,#91119),(#91120,#91121,#91122,#91123),(#91124,#91125,
#91126,#91127)),.UNSPECIFIED.,.F.,.F.,.F.,(4,4),(4,4),(-0.00286780122415295,
0.477902879802985),(0.0500263550858989,0.0565997133101389),
 .UNSPECIFIED.);
#2724=B_SPLINE_SURFACE_WITH_KNOTS('',3,3,((#91129,#91130,#91131,#91132),
(#91133,#91134,#91135,#91136),(#91137,#91138,#91139,#91140),(#91141,#91142,
#91143,#91144)),.UNSPECIFIED.,.F.,.F.,.F.,(4,4),(4,4),(0.522097120201262,
1.00286810177284),(0.0466073985929439,0.0531834933545494),.UNSPECIFIED.);
#2725=B_SPLINE_SURFACE_WITH_KNOTS('',3,3,((#91152,#91153,#91154,#91155),
(#91156,#91157,#91158,#91159),(#91160,#91161,#91162,#91163),(#91164,#91165,
#91166,#91167)),.UNSPECIFIED.,.F.,.F.,.F.,(4,4),(4,4),(-0.00286792598902313,
0.477902879802582),(0.0600156865494597,0.0665898698871158),
 .UNSPECIFIED.);
#2726=B_SPLINE_SURFACE_WITH_KNOTS('',3,3,((#91169,#91170,#91171,#91172),
(#91173,#91174,#91175,#91176),(#91177,#91178,#91179,#91180),(#91181,#91182,
#91183,#91184)),.UNSPECIFIED.,.F.,.F.,.F.,(4,4),(4,4),(0.522097120202546,
1.00286764392041),(0.0565997133101403,0.0631721430887051),.UNSPECIFIED.);
#2727=B_SPLINE_SURFACE_WITH_KNOTS('',3,3,((#91192,#91193,#91194,#91195),
(#91196,#91197,#91198,#91199),(#91200,#91201,#91202,#91203),(#91204,#91205,
#91206,#91207)),.UNSPECIFIED.,.F.,.F.,.F.,(4,4),(4,4),(0.522097120203716,
1.00286833998597),(0.0665898698871153,0.0731716198748442),.UNSPECIFIED.);
#2728=B_SPLINE_SURFACE_WITH_KNOTS('',3,3,((#91209,#91210,#91211,#91212),
(#91213,#91214,#91215,#91216),(#91217,#91218,#91219,#91220),(#91221,#91222,
#91223,#91224)),.UNSPECIFIED.,.F.,.F.,.F.,(4,4),(4,4),(-0.0012473153074531,
0.209045111704136),(0.0700194292965939,0.0749900982978269),
 .UNSPECIFIED.);
#2729=B_SPLINE_SURFACE_WITH_KNOTS('',3,3,((#91238,#91239,#91240,#91241),
(#91242,#91243,#91244,#91245),(#91246,#91247,#91248,#91249),(#91250,#91251,
#91252,#91253)),.UNSPECIFIED.,.F.,.F.,.F.,(4,4),(4,4),(-0.00286791014417758,
0.477902879802125),(0.0100271466769369,0.0166015299239865),
 .UNSPECIFIED.);
#2730=B_SPLINE_SURFACE_WITH_KNOTS('',3,3,((#91255,#91256,#91257,#91258),
(#91259,#91260,#91261,#91262),(#91263,#91264,#91265,#91266),(#91267,#91268,
#91269,#91270)),.UNSPECIFIED.,.F.,.F.,.F.,(4,4),(4,4),(0.653230271487925,
1.00206901891114),(0.00656788395392195,0.0131849432429873),
 .UNSPECIFIED.);
#2731=B_SPLINE_SURFACE_WITH_KNOTS('',3,3,((#91278,#91279,#91280,#91281),
(#91282,#91283,#91284,#91285),(#91286,#91287,#91288,#91289),(#91290,#91291,
#91292,#91293)),.UNSPECIFIED.,.F.,.F.,.F.,(4,4),(4,4),(0.,1.00600003961375),
(0.0166015299239895,0.0265907346180635),.UNSPECIFIED.);
#2732=B_SPLINE_SURFACE_WITH_KNOTS('',3,3,((#91296,#91297,#91298,#91299),
(#91300,#91301,#91302,#91303),(#91304,#91305,#91306,#91307),(#91308,#91309,
#91310,#91311)),.UNSPECIFIED.,.F.,.F.,.F.,(4,4),(4,4),(0.522097120198875,
1.0028675316012),(0.0166015299239866,0.0231736788037103),.UNSPECIFIED.);
#2733=B_SPLINE_SURFACE_WITH_KNOTS('',3,3,((#91312,#91313,#91314,#91315),
(#91316,#91317,#91318,#91319),(#91320,#91321,#91322,#91323),(#91324,#91325,
#91326,#91327)),.UNSPECIFIED.,.F.,.F.,.F.,(4,4),(4,4),(-0.00286780410483755,
0.47790287980203),(0.0200175229646903,0.0265907346180618),.UNSPECIFIED.);
#2734=B_SPLINE_SURFACE_WITH_KNOTS('',3,3,((#91334,#91335,#91336,#91337),
(#91338,#91339,#91340,#91341),(#91342,#91343,#91344,#91345),(#91346,#91347,
#91348,#91349)),.UNSPECIFIED.,.F.,.F.,.F.,(4,4),(4,4),(-0.00286791014425298,
0.477902879801941),(0.0100271466769356,0.0166015299239881),
 .UNSPECIFIED.);
#2735=B_SPLINE_SURFACE_WITH_KNOTS('',3,3,((#91351,#91352,#91353,#91354),
(#91355,#91356,#91357,#91358),(#91359,#91360,#91361,#91362),(#91363,#91364,
#91365,#91366)),.UNSPECIFIED.,.F.,.F.,.F.,(4,4),(4,4),(0.653230271487142,
1.002069018909),(0.00656788395391975,0.0131849432429877),.UNSPECIFIED.);
#2736=B_SPLINE_SURFACE_WITH_KNOTS('',3,3,((#91389,#91390,#91391,#91392),
(#91393,#91394,#91395,#91396),(#91397,#91398,#91399,#91400),(#91401,#91402,
#91403,#91404)),.UNSPECIFIED.,.F.,.F.,.F.,(4,4),(4,4),(-0.00286848453293753,
0.477902879803458),(0.0400218729466608,0.0466073985929422),
 .UNSPECIFIED.);
#2737=B_SPLINE_SURFACE_WITH_KNOTS('',3,3,((#91406,#91407,#91408,#91409),
(#91410,#91411,#91412,#91413),(#91414,#91415,#91416,#91417),(#91418,#91419,
#91420,#91421)),.UNSPECIFIED.,.F.,.F.,.F.,(4,4),(4,4),(0.,1.00600014639741),
(0.0365944846644992,0.0466073985929148),.UNSPECIFIED.);
#2738=B_SPLINE_SURFACE_WITH_KNOTS('',3,3,((#91422,#91423,#91424,#91425),
(#91426,#91427,#91428,#91429),(#91430,#91431,#91432,#91433),(#91434,#91435,
#91436,#91437)),.UNSPECIFIED.,.F.,.F.,.F.,(4,4),(4,4),(-0.00286780122418116,
0.477902879803416),(0.050026355085899,0.056599713310139),.UNSPECIFIED.);
#2739=B_SPLINE_SURFACE_WITH_KNOTS('',3,3,((#91439,#91440,#91441,#91442),
(#91443,#91444,#91445,#91446),(#91447,#91448,#91449,#91450),(#91451,#91452,
#91453,#91454)),.UNSPECIFIED.,.F.,.F.,.F.,(4,4),(4,4),(0.52209712019881,
1.00286810177268),(0.0466073985929444,0.053183492588891),.UNSPECIFIED.);
#2740=B_SPLINE_SURFACE_WITH_KNOTS('',3,3,((#91462,#91463,#91464,#91465),
(#91466,#91467,#91468,#91469),(#91470,#91471,#91472,#91473),(#91474,#91475,
#91476,#91477)),.UNSPECIFIED.,.F.,.F.,.F.,(4,4),(4,4),(-0.00286792598894552,
0.477902879803265),(0.0600156865494594,0.0665898698871161),
 .UNSPECIFIED.);
#2741=B_SPLINE_SURFACE_WITH_KNOTS('',3,3,((#91479,#91480,#91481,#91482),
(#91483,#91484,#91485,#91486),(#91487,#91488,#91489,#91490),(#91491,#91492,
#91493,#91494)),.UNSPECIFIED.,.F.,.F.,.F.,(4,4),(4,4),(0.522097120200067,
1.00286764392044),(0.0565997133101416,0.0631721430887055),.UNSPECIFIED.);
#2742=B_SPLINE_SURFACE_WITH_KNOTS('',3,3,((#91502,#91503,#91504,#91505),
(#91506,#91507,#91508,#91509),(#91510,#91511,#91512,#91513),(#91514,#91515,
#91516,#91517)),.UNSPECIFIED.,.F.,.F.,.F.,(4,4),(4,4),(0.522097120201106,
1.00286833998596),(0.0665898698871184,0.0731716198748444),.UNSPECIFIED.);
#2743=B_SPLINE_SURFACE_WITH_KNOTS('',3,3,((#91519,#91520,#91521,#91522),
(#91523,#91524,#91525,#91526),(#91527,#91528,#91529,#91530),(#91531,#91532,
#91533,#91534)),.UNSPECIFIED.,.F.,.F.,.F.,(4,4),(4,4),(-0.00124731530673201,
0.209045111704814),(0.0700194292966092,0.0749900982978298),
 .UNSPECIFIED.);
#2744=B_SPLINE_SURFACE_WITH_KNOTS('',3,3,((#91542,#91543,#91544,#91545),
(#91546,#91547,#91548,#91549),(#91550,#91551,#91552,#91553),(#91554,#91555,
#91556,#91557)),.UNSPECIFIED.,.F.,.F.,.F.,(4,4),(4,4),(-0.00286780410483184,
0.477902879802143),(0.0200175229646905,0.0265907346180623),
 .UNSPECIFIED.);
#2745=B_SPLINE_SURFACE_WITH_KNOTS('',3,3,((#91559,#91560,#91561,#91562),
(#91563,#91564,#91565,#91566),(#91567,#91568,#91569,#91570),(#91571,#91572,
#91573,#91574)),.UNSPECIFIED.,.F.,.F.,.F.,(4,4),(4,4),(0.5220971201967,
1.00286753160129),(0.0166015299239878,0.0231736788037118),.UNSPECIFIED.);
#2746=B_SPLINE_SURFACE_WITH_KNOTS('',3,3,((#91576,#91577,#91578,#91579),
(#91580,#91581,#91582,#91583),(#91584,#91585,#91586,#91587),(#91588,#91589,
#91590,#91591)),.UNSPECIFIED.,.F.,.F.,.F.,(4,4),(4,4),(0.,1.00600003961372),
(0.0166015299239882,0.0265907346180641),.UNSPECIFIED.);
#2747=B_SPLINE_SURFACE_WITH_KNOTS('',3,3,((#91600,#91601,#91602,#91603),
(#91604,#91605,#91606,#91607),(#91608,#91609,#91610,#91611),(#91612,#91613,
#91614,#91615)),.UNSPECIFIED.,.F.,.F.,.F.,(4,4),(4,4),(0.522097120197952,
1.00286823669295),(0.0265907346180637,0.0331702036051741),.UNSPECIFIED.);
#2748=B_SPLINE_SURFACE_WITH_KNOTS('',3,3,((#91616,#91617,#91618,#91619),
(#91620,#91621,#91622,#91623),(#91624,#91625,#91626,#91627),(#91628,#91629,
#91630,#91631)),.UNSPECIFIED.,.F.,.F.,.F.,(4,4),(4,4),(-0.00286862201161512,
0.477902879802719),(0.0300094532292791,0.0365944846647173),
 .UNSPECIFIED.);
#2749=B_SPLINE_SURFACE_WITH_KNOTS('',3,3,((#91638,#91639,#91640,#91641),
(#91642,#91643,#91644,#91645),(#91646,#91647,#91648,#91649),(#91650,#91651,
#91652,#91653)),.UNSPECIFIED.,.F.,.F.,.F.,(4,4),(4,4),(-0.00286791014429398,
0.477902879801375),(0.0100271466769348,0.0166015299239883),
 .UNSPECIFIED.);
#2750=B_SPLINE_SURFACE_WITH_KNOTS('',3,3,((#91655,#91656,#91657,#91658),
(#91659,#91660,#91661,#91662),(#91663,#91664,#91665,#91666),(#91667,#91668,
#91669,#91670)),.UNSPECIFIED.,.F.,.F.,.F.,(4,4),(4,4),(0.653230271486491,
1.00206901890709),(0.00656788395391518,0.013184943242987),.UNSPECIFIED.);
#2751=B_SPLINE_SURFACE_WITH_KNOTS('',3,3,((#91678,#91679,#91680,#91681),
(#91682,#91683,#91684,#91685),(#91686,#91687,#91688,#91689),(#91690,#91691,
#91692,#91693)),.UNSPECIFIED.,.F.,.F.,.F.,(4,4),(4,4),(-0.00286780410483956,
0.477902879801899),(0.0200175229646901,0.0265907346180625),
 .UNSPECIFIED.);
#2752=B_SPLINE_SURFACE_WITH_KNOTS('',3,3,((#91695,#91696,#91697,#91698),
(#91699,#91700,#91701,#91702),(#91703,#91704,#91705,#91706),(#91707,#91708,
#91709,#91710)),.UNSPECIFIED.,.F.,.F.,.F.,(4,4),(4,4),(0.52209712019461,
1.00286753160142),(0.0166015299239879,0.0231736788037111),.UNSPECIFIED.);
#2753=B_SPLINE_SURFACE_WITH_KNOTS('',3,3,((#91712,#91713,#91714,#91715),
(#91716,#91717,#91718,#91719),(#91720,#91721,#91722,#91723),(#91724,#91725,
#91726,#91727)),.UNSPECIFIED.,.F.,.F.,.F.,(4,4),(4,4),(0.,1.00600003961387),
(0.0166015299239869,0.0265907346180636),.UNSPECIFIED.);
#2754=B_SPLINE_SURFACE_WITH_KNOTS('',3,3,((#91728,#91729,#91730,#91731),
(#91732,#91733,#91734,#91735),(#91736,#91737,#91738,#91739),(#91740,#91741,
#91742,#91743)),.UNSPECIFIED.,.F.,.F.,.F.,(4,4),(4,4),(0.522097120196459,
1.00286810177292),(0.0466073985929452,0.0531834925888918),.UNSPECIFIED.);
#2755=B_SPLINE_SURFACE_WITH_KNOTS('',3,3,((#91745,#91746,#91747,#91748),
(#91749,#91750,#91751,#91752),(#91753,#91754,#91755,#91756),(#91757,#91758,
#91759,#91760)),.UNSPECIFIED.,.F.,.F.,.F.,(4,4),(4,4),(-0.00286780122426028,
0.477902879803546),(0.0500263550859001,0.056599713310138),.UNSPECIFIED.);
#2756=B_SPLINE_SURFACE_WITH_KNOTS('',3,3,((#91768,#91769,#91770,#91771),
(#91772,#91773,#91774,#91775),(#91776,#91777,#91778,#91779),(#91780,#91781,
#91782,#91783)),.UNSPECIFIED.,.F.,.F.,.F.,(4,4),(4,4),(-0.00286792598905476,
0.477902879803487),(0.0600156865494573,0.0665898698871151),
 .UNSPECIFIED.);
#2757=B_SPLINE_SURFACE_WITH_KNOTS('',3,3,((#91785,#91786,#91787,#91788),
(#91789,#91790,#91791,#91792),(#91793,#91794,#91795,#91796),(#91797,#91798,
#91799,#91800)),.UNSPECIFIED.,.F.,.F.,.F.,(4,4),(4,4),(0.522097120197693,
1.00286764392045),(0.0565997133101411,0.063172143088705),.UNSPECIFIED.);
#2758=B_SPLINE_SURFACE_WITH_KNOTS('',3,3,((#91808,#91809,#91810,#91811),
(#91812,#91813,#91814,#91815),(#91816,#91817,#91818,#91819),(#91820,#91821,
#91822,#91823)),.UNSPECIFIED.,.F.,.F.,.F.,(4,4),(4,4),(0.522097120198564,
1.002868339986),(0.0665898698871173,0.0731716198748439),.UNSPECIFIED.);
#2759=B_SPLINE_SURFACE_WITH_KNOTS('',3,3,((#91825,#91826,#91827,#91828),
(#91829,#91830,#91831,#91832),(#91833,#91834,#91835,#91836),(#91837,#91838,
#91839,#91840)),.UNSPECIFIED.,.F.,.F.,.F.,(4,4),(4,4),(-0.00124731530626188,
0.209045111705136),(0.0700194292966233,0.0749900982978318),
 .UNSPECIFIED.);
#2760=B_SPLINE_SURFACE_WITH_KNOTS('',3,3,((#91848,#91849,#91850,#91851),
(#91852,#91853,#91854,#91855),(#91856,#91857,#91858,#91859),(#91860,#91861,
#91862,#91863)),.UNSPECIFIED.,.F.,.F.,.F.,(4,4),(4,4),(-0.00286862201161757,
0.4779028798025),(0.0300094532292784,0.0365944846647023),.UNSPECIFIED.);
#2761=B_SPLINE_SURFACE_WITH_KNOTS('',3,3,((#91865,#91866,#91867,#91868),
(#91869,#91870,#91871,#91872),(#91873,#91874,#91875,#91876),(#91877,#91878,
#91879,#91880)),.UNSPECIFIED.,.F.,.F.,.F.,(4,4),(4,4),(0.522097120195729,
1.00286823669305),(0.0265907346180635,0.0331702036889927),.UNSPECIFIED.);
#2762=B_SPLINE_SURFACE_WITH_KNOTS('',3,3,((#91888,#91889,#91890,#91891),
(#91892,#91893,#91894,#91895),(#91896,#91897,#91898,#91899),(#91900,#91901,
#91902,#91903)),.UNSPECIFIED.,.F.,.F.,.F.,(4,4),(4,4),(0.,1.00600014639748),
(0.0365944846644978,0.0466073985929161),.UNSPECIFIED.);
#2763=B_SPLINE_SURFACE_WITH_KNOTS('',3,3,((#91920,#91921,#91922,#91923),
(#91924,#91925,#91926,#91927),(#91928,#91929,#91930,#91931),(#91932,#91933,
#91934,#91935)),.UNSPECIFIED.,.F.,.F.,.F.,(4,4),(4,4),(-0.00286848453299392,
0.47790287980232),(0.0400218729466594,0.046607398592943),.UNSPECIFIED.);
#2764=B_SPLINE_SURFACE_WITH_KNOTS('',3,3,((#91942,#91943,#91944,#91945),
(#91946,#91947,#91948,#91949),(#91950,#91951,#91952,#91953),(#91954,#91955,
#91956,#91957)),.UNSPECIFIED.,.F.,.F.,.F.,(4,4),(4,4),(-0.00286791014432967,
0.477902879800558),(0.0100271466769341,0.0166015299239865),
 .UNSPECIFIED.);
#2765=B_SPLINE_SURFACE_WITH_KNOTS('',3,3,((#91959,#91960,#91961,#91962),
(#91963,#91964,#91965,#91966),(#91967,#91968,#91969,#91970),(#91971,#91972,
#91973,#91974)),.UNSPECIFIED.,.F.,.F.,.F.,(4,4),(4,4),(0.65323027148601,
1.00206901890512),(0.00656788395390979,0.0131849432429878),
 .UNSPECIFIED.);
#2766=B_SPLINE_SURFACE_WITH_KNOTS('',3,3,((#91982,#91983,#91984,#91985),
(#91986,#91987,#91988,#91989),(#91990,#91991,#91992,#91993),(#91994,#91995,
#91996,#91997)),.UNSPECIFIED.,.F.,.F.,.F.,(4,4),(4,4),(-0.00286780410483655,
0.477902879801139),(0.0200175229646906,0.0265907346180617),
 .UNSPECIFIED.);
#2767=B_SPLINE_SURFACE_WITH_KNOTS('',3,3,((#91999,#92000,#92001,#92002),
(#92003,#92004,#92005,#92006),(#92007,#92008,#92009,#92010),(#92011,#92012,
#92013,#92014)),.UNSPECIFIED.,.F.,.F.,.F.,(4,4),(4,4),(0.522097120192733,
1.00286753160138),(0.016601529923988,0.0231736788037116),.UNSPECIFIED.);
#2768=B_SPLINE_SURFACE_WITH_KNOTS('',3,3,((#92016,#92017,#92018,#92019),
(#92020,#92021,#92022,#92023),(#92024,#92025,#92026,#92027),(#92028,#92029,
#92030,#92031)),.UNSPECIFIED.,.F.,.F.,.F.,(4,4),(4,4),(0.,1.00600003961361),
(0.0166015299239868,0.0265907346180624),.UNSPECIFIED.);
#2769=B_SPLINE_SURFACE_WITH_KNOTS('',3,3,((#92032,#92033,#92034,#92035),
(#92036,#92037,#92038,#92039),(#92040,#92041,#92042,#92043),(#92044,#92045,
#92046,#92047)),.UNSPECIFIED.,.F.,.F.,.F.,(4,4),(4,4),(-0.00286862201160953,
0.477902879801959),(0.0300094532292791,0.0365944846647172),
 .UNSPECIFIED.);
#2770=B_SPLINE_SURFACE_WITH_KNOTS('',3,3,((#92049,#92050,#92051,#92052),
(#92053,#92054,#92055,#92056),(#92057,#92058,#92059,#92060),(#92061,#92062,
#92063,#92064)),.UNSPECIFIED.,.F.,.F.,.F.,(4,4),(4,4),(0.522097120193524,
1.00286823669304),(0.026590734618063,0.0331702036889923),.UNSPECIFIED.);
#2771=B_SPLINE_SURFACE_WITH_KNOTS('',3,3,((#92072,#92073,#92074,#92075),
(#92076,#92077,#92078,#92079),(#92080,#92081,#92082,#92083),(#92084,#92085,
#92086,#92087)),.UNSPECIFIED.,.F.,.F.,.F.,(4,4),(4,4),(0.522097120195503,
1.00286764392042),(0.0565997133101417,0.0631721430887048),.UNSPECIFIED.);
#2772=B_SPLINE_SURFACE_WITH_KNOTS('',3,3,((#92089,#92090,#92091,#92092),
(#92093,#92094,#92095,#92096),(#92097,#92098,#92099,#92100),(#92101,#92102,
#92103,#92104)),.UNSPECIFIED.,.F.,.F.,.F.,(4,4),(4,4),(-0.00286792598905419,
0.477902879803423),(0.0600156865494597,0.0665898698871165),
 .UNSPECIFIED.);
#2773=B_SPLINE_SURFACE_WITH_KNOTS('',3,3,((#92112,#92113,#92114,#92115),
(#92116,#92117,#92118,#92119),(#92120,#92121,#92122,#92123),(#92124,#92125,
#92126,#92127)),.UNSPECIFIED.,.F.,.F.,.F.,(4,4),(4,4),(0.522097120196121,
1.00286833998585),(0.0665898698871173,0.073171619874844),.UNSPECIFIED.);
#2774=B_SPLINE_SURFACE_WITH_KNOTS('',3,3,((#92129,#92130,#92131,#92132),
(#92133,#92134,#92135,#92136),(#92137,#92138,#92139,#92140),(#92141,#92142,
#92143,#92144)),.UNSPECIFIED.,.F.,.F.,.F.,(4,4),(4,4),(-0.00124731530620073,
0.209045111705207),(0.0700194292966371,0.0749900982978334),
 .UNSPECIFIED.);
#2775=B_SPLINE_SURFACE_WITH_KNOTS('',3,3,((#92152,#92153,#92154,#92155),
(#92156,#92157,#92158,#92159),(#92160,#92161,#92162,#92163),(#92164,#92165,
#92166,#92167)),.UNSPECIFIED.,.F.,.F.,.F.,(4,4),(4,4),(-0.00286848453302246,
0.477902879801834),(0.0400218729466601,0.046607398592943),.UNSPECIFIED.);
#2776=B_SPLINE_SURFACE_WITH_KNOTS('',3,3,((#92184,#92185,#92186,#92187),
(#92188,#92189,#92190,#92191),(#92192,#92193,#92194,#92195),(#92196,#92197,
#92198,#92199)),.UNSPECIFIED.,.F.,.F.,.F.,(4,4),(4,4),(0.,1.00600014639736),
(0.0365944846644989,0.0466073985929157),.UNSPECIFIED.);
#2777=B_SPLINE_SURFACE_WITH_KNOTS('',3,3,((#92208,#92209,#92210,#92211),
(#92212,#92213,#92214,#92215),(#92216,#92217,#92218,#92219),(#92220,#92221,
#92222,#92223)),.UNSPECIFIED.,.F.,.F.,.F.,(4,4),(4,4),(0.522097120195486,
1.00286810177294),(0.0466073985929438,0.0531834933545495),.UNSPECIFIED.);
#2778=B_SPLINE_SURFACE_WITH_KNOTS('',3,3,((#92224,#92225,#92226,#92227),
(#92228,#92229,#92230,#92231),(#92232,#92233,#92234,#92235),(#92236,#92237,
#92238,#92239)),.UNSPECIFIED.,.F.,.F.,.F.,(4,4),(4,4),(-0.00286780122428723,
0.477902879802085),(0.0500263550858992,0.0565997133101407),
 .UNSPECIFIED.);
#2779=B_SPLINE_SURFACE_WITH_KNOTS('',3,3,((#92246,#92247,#92248,#92249),
(#92250,#92251,#92252,#92253),(#92254,#92255,#92256,#92257),(#92258,#92259,
#92260,#92261)),.UNSPECIFIED.,.F.,.F.,.F.,(4,4),(4,4),(-0.00286791014439694,
0.477902879799415),(0.0100271466769345,0.0166015299239855),
 .UNSPECIFIED.);
#2780=B_SPLINE_SURFACE_WITH_KNOTS('',3,3,((#92263,#92264,#92265,#92266),
(#92267,#92268,#92269,#92270),(#92271,#92272,#92273,#92274),(#92275,#92276,
#92277,#92278)),.UNSPECIFIED.,.F.,.F.,.F.,(4,4),(4,4),(0.653230271485745,
1.00206901890371),(0.00656788395390478,0.0131849432429869),
 .UNSPECIFIED.);
#2781=B_SPLINE_SURFACE_WITH_KNOTS('',3,3,((#92286,#92287,#92288,#92289),
(#92290,#92291,#92292,#92293),(#92294,#92295,#92296,#92297),(#92298,#92299,
#92300,#92301)),.UNSPECIFIED.,.F.,.F.,.F.,(4,4),(4,4),(-0.00286780410478452,
0.477902879800153),(0.0200175229646906,0.0265907346180619),
 .UNSPECIFIED.);
#2782=B_SPLINE_SURFACE_WITH_KNOTS('',3,3,((#92303,#92304,#92305,#92306),
(#92307,#92308,#92309,#92310),(#92311,#92312,#92313,#92314),(#92315,#92316,
#92317,#92318)),.UNSPECIFIED.,.F.,.F.,.F.,(4,4),(4,4),(0.522097120191154,
1.00286753160141),(0.016601529923988,0.0231736787930311),.UNSPECIFIED.);
#2783=B_SPLINE_SURFACE_WITH_KNOTS('',3,3,((#92320,#92321,#92322,#92323),
(#92324,#92325,#92326,#92327),(#92328,#92329,#92330,#92331),(#92332,#92333,
#92334,#92335)),.UNSPECIFIED.,.F.,.F.,.F.,(4,4),(4,4),(0.,1.00600003961398),
(0.0166015299239882,0.0265907346180622),.UNSPECIFIED.);
#2784=B_SPLINE_SURFACE_WITH_KNOTS('',3,3,((#92336,#92337,#92338,#92339),
(#92340,#92341,#92342,#92343),(#92344,#92345,#92346,#92347),(#92348,#92349,
#92350,#92351)),.UNSPECIFIED.,.F.,.F.,.F.,(4,4),(4,4),(-0.00286862201161503,
0.477902879801108),(0.0300094532292788,0.0365944846647166),
 .UNSPECIFIED.);
#2785=B_SPLINE_SURFACE_WITH_KNOTS('',3,3,((#92353,#92354,#92355,#92356),
(#92357,#92358,#92359,#92360),(#92361,#92362,#92363,#92364),(#92365,#92366,
#92367,#92368)),.UNSPECIFIED.,.F.,.F.,.F.,(4,4),(4,4),(0.522097120191805,
1.00286823669312),(0.0265907346180641,0.0331702036889924),.UNSPECIFIED.);
#2786=B_SPLINE_SURFACE_WITH_KNOTS('',3,3,((#92376,#92377,#92378,#92379),
(#92380,#92381,#92382,#92383),(#92384,#92385,#92386,#92387),(#92388,#92389,
#92390,#92391)),.UNSPECIFIED.,.F.,.F.,.F.,(4,4),(4,4),(-0.0028684845330722,
0.477902879801392),(0.0400218729466607,0.0466073985929435),
 .UNSPECIFIED.);
#2787=B_SPLINE_SURFACE_WITH_KNOTS('',3,3,((#92408,#92409,#92410,#92411),
(#92412,#92413,#92414,#92415),(#92416,#92417,#92418,#92419),(#92420,#92421,
#92422,#92423)),.UNSPECIFIED.,.F.,.F.,.F.,(4,4),(4,4),(0.,1.00600014639735),
(0.0365944846644988,0.0466073985929162),.UNSPECIFIED.);
#2788=B_SPLINE_SURFACE_WITH_KNOTS('',3,3,((#92424,#92425,#92426,#92427),
(#92428,#92429,#92430,#92431),(#92432,#92433,#92434,#92435),(#92436,#92437,
#92438,#92439)),.UNSPECIFIED.,.F.,.F.,.F.,(4,4),(4,4),(0.52209712019443,
1.00286833998601),(0.0665898698871202,0.073171619874844),.UNSPECIFIED.);
#2789=B_SPLINE_SURFACE_WITH_KNOTS('',3,3,((#92448,#92449,#92450,#92451),
(#92452,#92453,#92454,#92455),(#92456,#92457,#92458,#92459),(#92460,#92461,
#92462,#92463)),.UNSPECIFIED.,.F.,.F.,.F.,(4,4),(4,4),(-0.00124731530661292,
0.209045111704791),(0.0700194292966529,0.0749900982978302),
 .UNSPECIFIED.);
#2790=B_SPLINE_SURFACE_WITH_KNOTS('',3,3,((#92464,#92465,#92466,#92467),
(#92468,#92469,#92470,#92471),(#92472,#92473,#92474,#92475),(#92476,#92477,
#92478,#92479)),.UNSPECIFIED.,.F.,.F.,.F.,(4,4),(4,4),(-0.00286780122435983,
0.477902879801441),(0.0500263550858991,0.05659971331014),.UNSPECIFIED.);
#2791=B_SPLINE_SURFACE_WITH_KNOTS('',3,3,((#92481,#92482,#92483,#92484),
(#92485,#92486,#92487,#92488),(#92489,#92490,#92491,#92492),(#92493,#92494,
#92495,#92496)),.UNSPECIFIED.,.F.,.F.,.F.,(4,4),(4,4),(0.522097120193469,
1.00286810177265),(0.0466073985929449,0.0531834925888935),.UNSPECIFIED.);
#2792=B_SPLINE_SURFACE_WITH_KNOTS('',3,3,((#92512,#92513,#92514,#92515),
(#92516,#92517,#92518,#92519),(#92520,#92521,#92522,#92523),(#92524,#92525,
#92526,#92527)),.UNSPECIFIED.,.F.,.F.,.F.,(4,4),(4,4),(0.522097120195661,
1.00286764392054),(0.0565997133101417,0.0631721430887064),.UNSPECIFIED.);
#2793=B_SPLINE_SURFACE_WITH_KNOTS('',3,3,((#92528,#92529,#92530,#92531),
(#92532,#92533,#92534,#92535),(#92536,#92537,#92538,#92539),(#92540,#92541,
#92542,#92543)),.UNSPECIFIED.,.F.,.F.,.F.,(4,4),(4,4),(-0.00286792598902705,
0.477902879801742),(0.06001568654946,0.0665898698871169),.UNSPECIFIED.);
#2794=B_SPLINE_SURFACE_WITH_KNOTS('',3,3,((#92550,#92551,#92552,#92553),
(#92554,#92555,#92556,#92557),(#92558,#92559,#92560,#92561),(#92562,#92563,
#92564,#92565)),.UNSPECIFIED.,.F.,.F.,.F.,(4,4),(4,4),(-0.00286791014444834,
0.477902879798085),(0.0100271466769347,0.0166015299239865),
 .UNSPECIFIED.);
#2795=B_SPLINE_SURFACE_WITH_KNOTS('',3,3,((#92567,#92568,#92569,#92570),
(#92571,#92572,#92573,#92574),(#92575,#92576,#92577,#92578),(#92579,#92580,
#92581,#92582)),.UNSPECIFIED.,.F.,.F.,.F.,(4,4),(4,4),(0.653230271485697,
1.00206901890237),(0.00656788395389881,0.0131849432429867),
 .UNSPECIFIED.);
#2796=B_SPLINE_SURFACE_WITH_KNOTS('',3,3,((#92590,#92591,#92592,#92593),
(#92594,#92595,#92596,#92597),(#92598,#92599,#92600,#92601),(#92602,#92603,
#92604,#92605)),.UNSPECIFIED.,.F.,.F.,.F.,(4,4),(4,4),(-0.002867804104808,
0.477902879798951),(0.020017522964691,0.0265907346180616),.UNSPECIFIED.);
#2797=B_SPLINE_SURFACE_WITH_KNOTS('',3,3,((#92607,#92608,#92609,#92610),
(#92611,#92612,#92613,#92614),(#92615,#92616,#92617,#92618),(#92619,#92620,
#92621,#92622)),.UNSPECIFIED.,.F.,.F.,.F.,(4,4),(4,4),(0.52209712018981,
1.00286753160131),(0.0166015299239889,0.0231736788075213),.UNSPECIFIED.);
#2798=B_SPLINE_SURFACE_WITH_KNOTS('',3,3,((#92624,#92625,#92626,#92627),
(#92628,#92629,#92630,#92631),(#92632,#92633,#92634,#92635),(#92636,#92637,
#92638,#92639)),.UNSPECIFIED.,.F.,.F.,.F.,(4,4),(4,4),(0.,1.00600003961366),
(0.0166015299239869,0.0265907346180631),.UNSPECIFIED.);
#2799=B_SPLINE_SURFACE_WITH_KNOTS('',3,3,((#92640,#92641,#92642,#92643),
(#92644,#92645,#92646,#92647),(#92648,#92649,#92650,#92651),(#92652,#92653,
#92654,#92655)),.UNSPECIFIED.,.F.,.F.,.F.,(4,4),(4,4),(-0.00286862201162927,
0.477902879800058),(0.0300094532292786,0.0365944846647019),
 .UNSPECIFIED.);
#2800=B_SPLINE_SURFACE_WITH_KNOTS('',3,3,((#92657,#92658,#92659,#92660),
(#92661,#92662,#92663,#92664),(#92665,#92666,#92667,#92668),(#92669,#92670,
#92671,#92672)),.UNSPECIFIED.,.F.,.F.,.F.,(4,4),(4,4),(0.522097120190289,
1.00286823669302),(0.026590734618063,0.0331702036889927),.UNSPECIFIED.);
#2801=B_SPLINE_SURFACE_WITH_KNOTS('',3,3,((#92680,#92681,#92682,#92683),
(#92684,#92685,#92686,#92687),(#92688,#92689,#92690,#92691),(#92692,#92693,
#92694,#92695)),.UNSPECIFIED.,.F.,.F.,.F.,(4,4),(4,4),(-0.00286848453311717,
0.477902879800286),(0.0400218729466604,0.0466073985929421),
 .UNSPECIFIED.);
#2802=B_SPLINE_SURFACE_WITH_KNOTS('',3,3,((#92712,#92713,#92714,#92715),
(#92716,#92717,#92718,#92719),(#92720,#92721,#92722,#92723),(#92724,#92725,
#92726,#92727)),.UNSPECIFIED.,.F.,.F.,.F.,(4,4),(4,4),(0.,1.0060001463975),
(0.0365944846644987,0.0466073985929169),.UNSPECIFIED.);
#2803=B_SPLINE_SURFACE_WITH_KNOTS('',3,3,((#92728,#92729,#92730,#92731),
(#92732,#92733,#92734,#92735),(#92736,#92737,#92738,#92739),(#92740,#92741,
#92742,#92743)),.UNSPECIFIED.,.F.,.F.,.F.,(4,4),(4,4),(-0.00286780122439779,
0.477902879800689),(0.0500263550859002,0.0565997133101411),
 .UNSPECIFIED.);
#2804=B_SPLINE_SURFACE_WITH_KNOTS('',3,3,((#92745,#92746,#92747,#92748),
(#92749,#92750,#92751,#92752),(#92753,#92754,#92755,#92756),(#92757,#92758,
#92759,#92760)),.UNSPECIFIED.,.F.,.F.,.F.,(4,4),(4,4),(0.522097120191868,
1.00286810177297),(0.0466073985929451,0.0531834933545502),.UNSPECIFIED.);
#2805=B_SPLINE_SURFACE_WITH_KNOTS('',3,3,((#92768,#92769,#92770,#92771),
(#92772,#92773,#92774,#92775),(#92776,#92777,#92778,#92779),(#92780,#92781,
#92782,#92783)),.UNSPECIFIED.,.F.,.F.,.F.,(4,4),(4,4),(-0.00286792598900614,
0.47790287980102),(0.0600156865494604,0.0665898698871169),.UNSPECIFIED.);
#2806=B_SPLINE_SURFACE_WITH_KNOTS('',3,3,((#92785,#92786,#92787,#92788),
(#92789,#92790,#92791,#92792),(#92793,#92794,#92795,#92796),(#92797,#92798,
#92799,#92800)),.UNSPECIFIED.,.F.,.F.,.F.,(4,4),(4,4),(0.522097120194769,
1.00286764392045),(0.0565997133101423,0.0631721430887064),.UNSPECIFIED.);
#2807=B_SPLINE_SURFACE_WITH_KNOTS('',3,3,((#92816,#92817,#92818,#92819),
(#92820,#92821,#92822,#92823),(#92824,#92825,#92826,#92827),(#92828,#92829,
#92830,#92831)),.UNSPECIFIED.,.F.,.F.,.F.,(4,4),(4,4),(0.522097120193573,
1.00286833998603),(0.066589869887119,0.0731716198748446),.UNSPECIFIED.);
#2808=B_SPLINE_SURFACE_WITH_KNOTS('',3,3,((#92832,#92833,#92834,#92835),
(#92836,#92837,#92838,#92839),(#92840,#92841,#92842,#92843),(#92844,#92845,
#92846,#92847)),.UNSPECIFIED.,.F.,.F.,.F.,(4,4),(4,4),(-0.00124731530708468,
0.209045111704209),(0.070019429296666,0.0749900982978293),.UNSPECIFIED.);
#2809=B_SPLINE_SURFACE_WITH_KNOTS('',3,3,((#92854,#92855,#92856,#92857),
(#92858,#92859,#92860,#92861),(#92862,#92863,#92864,#92865),(#92866,#92867,
#92868,#92869)),.UNSPECIFIED.,.F.,.F.,.F.,(4,4),(4,4),(-0.00286791014448215,
0.477902879796417),(0.0100271466769337,0.0166015299239869),
 .UNSPECIFIED.);
#2810=B_SPLINE_SURFACE_WITH_KNOTS('',3,3,((#92871,#92872,#92873,#92874),
(#92875,#92876,#92877,#92878),(#92879,#92880,#92881,#92882),(#92883,#92884,
#92885,#92886)),.UNSPECIFIED.,.F.,.F.,.F.,(4,4),(4,4),(0.653230271485805,
1.00206901890132),(0.00656788395389165,0.0131849432429875),
 .UNSPECIFIED.);
#2811=B_SPLINE_SURFACE_WITH_KNOTS('',3,3,((#92894,#92895,#92896,#92897),
(#92898,#92899,#92900,#92901),(#92902,#92903,#92904,#92905),(#92906,#92907,
#92908,#92909)),.UNSPECIFIED.,.F.,.F.,.F.,(4,4),(4,4),(-0.00286780410477404,
0.477902879797415),(0.0200175229646904,0.0265907346180627),
 .UNSPECIFIED.);
#2812=B_SPLINE_SURFACE_WITH_KNOTS('',3,3,((#92911,#92912,#92913,#92914),
(#92915,#92916,#92917,#92918),(#92919,#92920,#92921,#92922),(#92923,#92924,
#92925,#92926)),.UNSPECIFIED.,.F.,.F.,.F.,(4,4),(4,4),(0.522097120188512,
1.00286753160135),(0.0166015299239885,0.0231736787930316),.UNSPECIFIED.);
#2813=B_SPLINE_SURFACE_WITH_KNOTS('',3,3,((#92928,#92929,#92930,#92931),
(#92932,#92933,#92934,#92935),(#92936,#92937,#92938,#92939),(#92940,#92941,
#92942,#92943)),.UNSPECIFIED.,.F.,.F.,.F.,(4,4),(4,4),(0.,1.00600003961351),
(0.0166015299239904,0.0265907346180641),.UNSPECIFIED.);
#2814=B_SPLINE_SURFACE_WITH_KNOTS('',3,3,((#92944,#92945,#92946,#92947),
(#92948,#92949,#92950,#92951),(#92952,#92953,#92954,#92955),(#92956,#92957,
#92958,#92959)),.UNSPECIFIED.,.F.,.F.,.F.,(4,4),(4,4),(-0.00286862201164203,
0.477902879798625),(0.0300094532292783,0.0365944846647018),
 .UNSPECIFIED.);
#2815=B_SPLINE_SURFACE_WITH_KNOTS('',3,3,((#92961,#92962,#92963,#92964),
(#92965,#92966,#92967,#92968),(#92969,#92970,#92971,#92972),(#92973,#92974,
#92975,#92976)),.UNSPECIFIED.,.F.,.F.,.F.,(4,4),(4,4),(0.522097120188926,
1.00286823669299),(0.0265907346180644,0.0331702036889922),.UNSPECIFIED.);
#2816=B_SPLINE_SURFACE_WITH_KNOTS('',3,3,((#92984,#92985,#92986,#92987),
(#92988,#92989,#92990,#92991),(#92992,#92993,#92994,#92995),(#92996,#92997,
#92998,#92999)),.UNSPECIFIED.,.F.,.F.,.F.,(4,4),(4,4),(-0.00286848453316085,
0.477902879799002),(0.0400218729466581,0.0466073985929425),
 .UNSPECIFIED.);
#2817=B_SPLINE_SURFACE_WITH_KNOTS('',3,3,((#93016,#93017,#93018,#93019),
(#93020,#93021,#93022,#93023),(#93024,#93025,#93026,#93027),(#93028,#93029,
#93030,#93031)),.UNSPECIFIED.,.F.,.F.,.F.,(4,4),(4,4),(0.,1.0060001463976),
(0.0365944846644989,0.0466073985929171),.UNSPECIFIED.);
#2818=B_SPLINE_SURFACE_WITH_KNOTS('',3,3,((#93032,#93033,#93034,#93035),
(#93036,#93037,#93038,#93039),(#93040,#93041,#93042,#93043),(#93044,#93045,
#93046,#93047)),.UNSPECIFIED.,.F.,.F.,.F.,(4,4),(4,4),(-0.00286780122443639,
0.477902879799573),(0.0500263550858993,0.0565997133101408),
 .UNSPECIFIED.);
#2819=B_SPLINE_SURFACE_WITH_KNOTS('',3,3,((#93049,#93050,#93051,#93052),
(#93053,#93054,#93055,#93056),(#93057,#93058,#93059,#93060),(#93061,#93062,
#93063,#93064)),.UNSPECIFIED.,.F.,.F.,.F.,(4,4),(4,4),(0.522097120190254,
1.00286810177252),(0.0466073985929451,0.0531834925888939),.UNSPECIFIED.);
#2820=B_SPLINE_SURFACE_WITH_KNOTS('',3,3,((#93072,#93073,#93074,#93075),
(#93076,#93077,#93078,#93079),(#93080,#93081,#93082,#93083),(#93084,#93085,
#93086,#93087)),.UNSPECIFIED.,.F.,.F.,.F.,(4,4),(4,4),(-0.00286792598898738,
0.477902879800105),(0.0600156865494592,0.0665898698871172),
 .UNSPECIFIED.);
#2821=B_SPLINE_SURFACE_WITH_KNOTS('',3,3,((#93089,#93090,#93091,#93092),
(#93093,#93094,#93095,#93096),(#93097,#93098,#93099,#93100),(#93101,#93102,
#93103,#93104)),.UNSPECIFIED.,.F.,.F.,.F.,(4,4),(4,4),(0.522097120193723,
1.00286764392043),(0.0565997133101425,0.0631721430887051),.UNSPECIFIED.);
#2822=B_SPLINE_SURFACE_WITH_KNOTS('',3,3,((#93120,#93121,#93122,#93123),
(#93124,#93125,#93126,#93127),(#93128,#93129,#93130,#93131),(#93132,#93133,
#93134,#93135)),.UNSPECIFIED.,.F.,.F.,.F.,(4,4),(4,4),(0.522097120191563,
1.00286833998597),(0.0665898698871186,0.0731716198748454),.UNSPECIFIED.);
#2823=B_SPLINE_SURFACE_WITH_KNOTS('',3,3,((#93136,#93137,#93138,#93139),
(#93140,#93141,#93142,#93143),(#93144,#93145,#93146,#93147),(#93148,#93149,
#93150,#93151)),.UNSPECIFIED.,.F.,.F.,.F.,(4,4),(4,4),(-0.00124731530803454,
0.209045111703296),(0.0700194292966781,0.0749900982978239),
 .UNSPECIFIED.);
#2824=B_SPLINE_SURFACE_WITH_KNOTS('',3,3,((#93158,#93159,#93160,#93161),
(#93162,#93163,#93164,#93165),(#93166,#93167,#93168,#93169),(#93170,#93171,
#93172,#93173)),.UNSPECIFIED.,.F.,.F.,.F.,(4,4),(4,4),(-0.00286791014452394,
0.477902879794564),(0.0100271466769348,0.0166015299239866),
 .UNSPECIFIED.);
#2825=B_SPLINE_SURFACE_WITH_KNOTS('',3,3,((#93175,#93176,#93177,#93178),
(#93179,#93180,#93181,#93182),(#93183,#93184,#93185,#93186),(#93187,#93188,
#93189,#93190)),.UNSPECIFIED.,.F.,.F.,.F.,(4,4),(4,4),(0.653230271486075,
1.00206901890076),(0.00656788395388381,0.0131849432429868),
 .UNSPECIFIED.);
#2826=B_SPLINE_SURFACE_WITH_KNOTS('',3,3,((#93198,#93199,#93200,#93201),
(#93202,#93203,#93204,#93205),(#93206,#93207,#93208,#93209),(#93210,#93211,
#93212,#93213)),.UNSPECIFIED.,.F.,.F.,.F.,(4,4),(4,4),(-0.002867804104759,
0.477902879795688),(0.0200175229646897,0.0265907346180626),
 .UNSPECIFIED.);
#2827=B_SPLINE_SURFACE_WITH_KNOTS('',3,3,((#93215,#93216,#93217,#93218),
(#93219,#93220,#93221,#93222),(#93223,#93224,#93225,#93226),(#93227,#93228,
#93229,#93230)),.UNSPECIFIED.,.F.,.F.,.F.,(4,4),(4,4),(0.522097120187777,
1.00286753160138),(0.0166015299239877,0.0231736788075219),.UNSPECIFIED.);
#2828=B_SPLINE_SURFACE_WITH_KNOTS('',3,3,((#93232,#93233,#93234,#93235),
(#93236,#93237,#93238,#93239),(#93240,#93241,#93242,#93243),(#93244,#93245,
#93246,#93247)),.UNSPECIFIED.,.F.,.F.,.F.,(4,4),(4,4),(0.,1.00600003961393),
(0.0166015299239902,0.0265907346180655),.UNSPECIFIED.);
#2829=B_SPLINE_SURFACE_WITH_KNOTS('',3,3,((#93248,#93249,#93250,#93251),
(#93252,#93253,#93254,#93255),(#93256,#93257,#93258,#93259),(#93260,#93261,
#93262,#93263)),.UNSPECIFIED.,.F.,.F.,.F.,(4,4),(4,4),(-0.0028686220116367,
0.477902879796942),(0.0300094532292783,0.0365944846647026),
 .UNSPECIFIED.);
#2830=B_SPLINE_SURFACE_WITH_KNOTS('',3,3,((#93265,#93266,#93267,#93268),
(#93269,#93270,#93271,#93272),(#93273,#93274,#93275,#93276),(#93277,#93278,
#93279,#93280)),.UNSPECIFIED.,.F.,.F.,.F.,(4,4),(4,4),(0.522097120188087,
1.00286823669321),(0.0265907346180629,0.0331702036889928),.UNSPECIFIED.);
#2831=B_SPLINE_SURFACE_WITH_KNOTS('',3,3,((#93288,#93289,#93290,#93291),
(#93292,#93293,#93294,#93295),(#93296,#93297,#93298,#93299),(#93300,#93301,
#93302,#93303)),.UNSPECIFIED.,.F.,.F.,.F.,(4,4),(4,4),(-0.00286848453322405,
0.477902879797452),(0.0400218729466589,0.0466073985929433),
 .UNSPECIFIED.);
#2832=B_SPLINE_SURFACE_WITH_KNOTS('',3,3,((#93320,#93321,#93322,#93323),
(#93324,#93325,#93326,#93327),(#93328,#93329,#93330,#93331),(#93332,#93333,
#93334,#93335)),.UNSPECIFIED.,.F.,.F.,.F.,(4,4),(4,4),(0.,1.00600014639746),
(0.0365944846644991,0.046607398592917),.UNSPECIFIED.);
#2833=B_SPLINE_SURFACE_WITH_KNOTS('',3,3,((#93336,#93337,#93338,#93339),
(#93340,#93341,#93342,#93343),(#93344,#93345,#93346,#93347),(#93348,#93349,
#93350,#93351)),.UNSPECIFIED.,.F.,.F.,.F.,(4,4),(4,4),(-0.00286780122450092,
0.477902879798157),(0.0500263550858995,0.0565997133101396),
 .UNSPECIFIED.);
#2834=B_SPLINE_SURFACE_WITH_KNOTS('',3,3,((#93353,#93354,#93355,#93356),
(#93357,#93358,#93359,#93360),(#93361,#93362,#93363,#93364),(#93365,#93366,
#93367,#93368)),.UNSPECIFIED.,.F.,.F.,.F.,(4,4),(4,4),(0.522097120189125,
1.00286810177271),(0.0466073985929443,0.0531834925888927),.UNSPECIFIED.);
#2835=B_SPLINE_SURFACE_WITH_KNOTS('',3,3,((#93376,#93377,#93378,#93379),
(#93380,#93381,#93382,#93383),(#93384,#93385,#93386,#93387),(#93388,#93389,
#93390,#93391)),.UNSPECIFIED.,.F.,.F.,.F.,(4,4),(4,4),(-0.00286792598902637,
0.477902879798802),(0.0600156865494596,0.0665898698871163),
 .UNSPECIFIED.);
#2836=B_SPLINE_SURFACE_WITH_KNOTS('',3,3,((#93393,#93394,#93395,#93396),
(#93397,#93398,#93399,#93400),(#93401,#93402,#93403,#93404),(#93405,#93406,
#93407,#93408)),.UNSPECIFIED.,.F.,.F.,.F.,(4,4),(4,4),(0.522097120193084,
1.00286764392051),(0.0565997133101423,0.0631721430887053),.UNSPECIFIED.);
#2837=B_SPLINE_SURFACE_WITH_KNOTS('',3,3,((#93424,#93425,#93426,#93427),
(#93428,#93429,#93430,#93431),(#93432,#93433,#93434,#93435),(#93436,#93437,
#93438,#93439)),.UNSPECIFIED.,.F.,.F.,.F.,(4,4),(4,4),(0.52209712019007,
1.00286833998607),(0.0665898698871196,0.0731716198748448),.UNSPECIFIED.);
#2838=B_SPLINE_SURFACE_WITH_KNOTS('',3,3,((#93440,#93441,#93442,#93443),
(#93444,#93445,#93446,#93447),(#93448,#93449,#93450,#93451),(#93452,#93453,
#93454,#93455)),.UNSPECIFIED.,.F.,.F.,.F.,(4,4),(4,4),(-0.00124731530915548,
0.209045111702115),(0.07001942929669,0.0749900982978186),.UNSPECIFIED.);
#2839=B_SPLINE_SURFACE_WITH_KNOTS('',3,3,((#93462,#93463,#93464,#93465),
(#93466,#93467,#93468,#93469),(#93470,#93471,#93472,#93473),(#93474,#93475,
#93476,#93477)),.UNSPECIFIED.,.F.,.F.,.F.,(4,4),(4,4),(-0.00286791014454036,
0.477902879792387),(0.0100271466769345,0.0166015299239863),
 .UNSPECIFIED.);
#2840=B_SPLINE_SURFACE_WITH_KNOTS('',3,3,((#93479,#93480,#93481,#93482),
(#93483,#93484,#93485,#93486),(#93487,#93488,#93489,#93490),(#93491,#93492,
#93493,#93494)),.UNSPECIFIED.,.F.,.F.,.F.,(4,4),(4,4),(0.653230271486586,
1.00206901890025),(0.00656788395387618,0.0131849432429879),
 .UNSPECIFIED.);
#2841=B_SPLINE_SURFACE_WITH_KNOTS('',3,3,((#93502,#93503,#93504,#93505),
(#93506,#93507,#93508,#93509),(#93510,#93511,#93512,#93513),(#93514,#93515,
#93516,#93517)),.UNSPECIFIED.,.F.,.F.,.F.,(4,4),(4,4),(-0.00286780410473863,
0.477902879793642),(0.0200175229646915,0.0265907346180612),
 .UNSPECIFIED.);
#2842=B_SPLINE_SURFACE_WITH_KNOTS('',3,3,((#93519,#93520,#93521,#93522),
(#93523,#93524,#93525,#93526),(#93527,#93528,#93529,#93530),(#93531,#93532,
#93533,#93534)),.UNSPECIFIED.,.F.,.F.,.F.,(4,4),(4,4),(0.522097120187455,
1.00286753160133),(0.0166015299239889,0.0231736787930312),.UNSPECIFIED.);
#2843=B_SPLINE_SURFACE_WITH_KNOTS('',3,3,((#93536,#93537,#93538,#93539),
(#93540,#93541,#93542,#93543),(#93544,#93545,#93546,#93547),(#93548,#93549,
#93550,#93551)),.UNSPECIFIED.,.F.,.F.,.F.,(4,4),(4,4),(0.,1.00600003961403),
(0.0166015299239862,0.0265907346180637),.UNSPECIFIED.);
#2844=B_SPLINE_SURFACE_WITH_KNOTS('',3,3,((#93552,#93553,#93554,#93555),
(#93556,#93557,#93558,#93559),(#93560,#93561,#93562,#93563),(#93564,#93565,
#93566,#93567)),.UNSPECIFIED.,.F.,.F.,.F.,(4,4),(4,4),(-0.00286862201162951,
0.477902879795088),(0.0300094532292795,0.0365944846647016),
 .UNSPECIFIED.);
#2845=B_SPLINE_SURFACE_WITH_KNOTS('',3,3,((#93569,#93570,#93571,#93572),
(#93573,#93574,#93575,#93576),(#93577,#93578,#93579,#93580),(#93581,#93582,
#93583,#93584)),.UNSPECIFIED.,.F.,.F.,.F.,(4,4),(4,4),(0.52209712018746,
1.00286823669317),(0.026590734618063,0.0331702036889934),.UNSPECIFIED.);
#2846=B_SPLINE_SURFACE_WITH_KNOTS('',3,3,((#93592,#93593,#93594,#93595),
(#93596,#93597,#93598,#93599),(#93600,#93601,#93602,#93603),(#93604,#93605,
#93606,#93607)),.UNSPECIFIED.,.F.,.F.,.F.,(4,4),(4,4),(-0.00286848453325639,
0.477902879795614),(0.0400218729466603,0.0466073985929429),
 .UNSPECIFIED.);
#2847=B_SPLINE_SURFACE_WITH_KNOTS('',3,3,((#93624,#93625,#93626,#93627),
(#93628,#93629,#93630,#93631),(#93632,#93633,#93634,#93635),(#93636,#93637,
#93638,#93639)),.UNSPECIFIED.,.F.,.F.,.F.,(4,4),(4,4),(0.,1.00600014639741),
(0.036594484664499,0.0466073985929158),.UNSPECIFIED.);
#2848=B_SPLINE_SURFACE_WITH_KNOTS('',3,3,((#93640,#93641,#93642,#93643),
(#93644,#93645,#93646,#93647),(#93648,#93649,#93650,#93651),(#93652,#93653,
#93654,#93655)),.UNSPECIFIED.,.F.,.F.,.F.,(4,4),(4,4),(-0.00286780122453885,
0.477902879796429),(0.0500263550859007,0.0565997133101406),
 .UNSPECIFIED.);
#2849=B_SPLINE_SURFACE_WITH_KNOTS('',3,3,((#93657,#93658,#93659,#93660),
(#93661,#93662,#93663,#93664),(#93665,#93666,#93667,#93668),(#93669,#93670,
#93671,#93672)),.UNSPECIFIED.,.F.,.F.,.F.,(4,4),(4,4),(0.522097120188107,
1.00286810177272),(0.0466073985929452,0.0531834925888921),.UNSPECIFIED.);
#2850=B_SPLINE_SURFACE_WITH_KNOTS('',3,3,((#93680,#93681,#93682,#93683),
(#93684,#93685,#93686,#93687),(#93688,#93689,#93690,#93691),(#93692,#93693,
#93694,#93695)),.UNSPECIFIED.,.F.,.F.,.F.,(4,4),(4,4),(-0.00286792598897243,
0.477902879797169),(0.0600156865494596,0.0665898698871175),
 .UNSPECIFIED.);
#2851=B_SPLINE_SURFACE_WITH_KNOTS('',3,3,((#93697,#93698,#93699,#93700),
(#93701,#93702,#93703,#93704),(#93705,#93706,#93707,#93708),(#93709,#93710,
#93711,#93712)),.UNSPECIFIED.,.F.,.F.,.F.,(4,4),(4,4),(0.522097120192675,
1.0028676439205),(0.0565997133101423,0.0631721430887056),.UNSPECIFIED.);
#2852=B_SPLINE_SURFACE_WITH_KNOTS('',3,3,((#93728,#93729,#93730,#93731),
(#93732,#93733,#93734,#93735),(#93736,#93737,#93738,#93739),(#93740,#93741,
#93742,#93743)),.UNSPECIFIED.,.F.,.F.,.F.,(4,4),(4,4),(0.522097120188981,
1.00286833998611),(0.0665898698871197,0.0731716198748445),.UNSPECIFIED.);
#2853=B_SPLINE_SURFACE_WITH_KNOTS('',3,3,((#93744,#93745,#93746,#93747),
(#93748,#93749,#93750,#93751),(#93752,#93753,#93754,#93755),(#93756,#93757,
#93758,#93759)),.UNSPECIFIED.,.F.,.F.,.F.,(4,4),(4,4),(-0.00124731531066159,
0.209045111700583),(0.0700194292967009,0.0749900982978111),
 .UNSPECIFIED.);
#2854=B_SPLINE_SURFACE_WITH_KNOTS('',3,3,((#93766,#93767,#93768,#93769),
(#93770,#93771,#93772,#93773),(#93774,#93775,#93776,#93777),(#93778,#93779,
#93780,#93781)),.UNSPECIFIED.,.F.,.F.,.F.,(4,4),(4,4),(-0.00286791014456512,
0.477902879790222),(0.0100271466769336,0.0166015299239865),
 .UNSPECIFIED.);
#2855=B_SPLINE_SURFACE_WITH_KNOTS('',3,3,((#93783,#93784,#93785,#93786),
(#93787,#93788,#93789,#93790),(#93791,#93792,#93793,#93794),(#93795,#93796,
#93797,#93798)),.UNSPECIFIED.,.F.,.F.,.F.,(4,4),(4,4),(0.653230271487221,
1.00206901890035),(0.00656788395386757,0.0131849432429867),
 .UNSPECIFIED.);
#2856=B_SPLINE_SURFACE_WITH_KNOTS('',3,3,((#93806,#93807,#93808,#93809),
(#93810,#93811,#93812,#93813),(#93814,#93815,#93816,#93817),(#93818,#93819,
#93820,#93821)),.UNSPECIFIED.,.F.,.F.,.F.,(4,4),(4,4),(-0.00286780410471625,
0.477902879791447),(0.0200175229646886,0.0265907346180621),
 .UNSPECIFIED.);
#2857=B_SPLINE_SURFACE_WITH_KNOTS('',3,3,((#93823,#93824,#93825,#93826),
(#93827,#93828,#93829,#93830),(#93831,#93832,#93833,#93834),(#93835,#93836,
#93837,#93838)),.UNSPECIFIED.,.F.,.F.,.F.,(4,4),(4,4),(0.522097120186926,
1.00286753160134),(0.0166015299239881,0.0231736788075218),.UNSPECIFIED.);
#2858=B_SPLINE_SURFACE_WITH_KNOTS('',3,3,((#93840,#93841,#93842,#93843),
(#93844,#93845,#93846,#93847),(#93848,#93849,#93850,#93851),(#93852,#93853,
#93854,#93855)),.UNSPECIFIED.,.F.,.F.,.F.,(4,4),(4,4),(0.,1.00600003961439),
(0.0166015299239894,0.0265907346180612),.UNSPECIFIED.);
#2859=B_SPLINE_SURFACE_WITH_KNOTS('',3,3,((#93856,#93857,#93858,#93859),
(#93860,#93861,#93862,#93863),(#93864,#93865,#93866,#93867),(#93868,#93869,
#93870,#93871)),.UNSPECIFIED.,.F.,.F.,.F.,(4,4),(4,4),(-0.00286862201160481,
0.477902879793087),(0.0300094532292791,0.0365944846647159),
 .UNSPECIFIED.);
#2860=B_SPLINE_SURFACE_WITH_KNOTS('',3,3,((#93873,#93874,#93875,#93876),
(#93877,#93878,#93879,#93880),(#93881,#93882,#93883,#93884),(#93885,#93886,
#93887,#93888)),.UNSPECIFIED.,.F.,.F.,.F.,(4,4),(4,4),(0.522097120186975,
1.00286823669319),(0.026590734618063,0.0331702036889921),.UNSPECIFIED.);
#2861=B_SPLINE_SURFACE_WITH_KNOTS('',3,3,((#93896,#93897,#93898,#93899),
(#93900,#93901,#93902,#93903),(#93904,#93905,#93906,#93907),(#93908,#93909,
#93910,#93911)),.UNSPECIFIED.,.F.,.F.,.F.,(4,4),(4,4),(-0.00286848453329562,
0.477902879793674),(0.0400218729466592,0.0466073985929428),
 .UNSPECIFIED.);
#2862=B_SPLINE_SURFACE_WITH_KNOTS('',3,3,((#93928,#93929,#93930,#93931),
(#93932,#93933,#93934,#93935),(#93936,#93937,#93938,#93939),(#93940,#93941,
#93942,#93943)),.UNSPECIFIED.,.F.,.F.,.F.,(4,4),(4,4),(0.,1.00600014639722),
(0.036594484664498,0.0466073985929171),.UNSPECIFIED.);
#2863=B_SPLINE_SURFACE_WITH_KNOTS('',3,3,((#93944,#93945,#93946,#93947),
(#93948,#93949,#93950,#93951),(#93952,#93953,#93954,#93955),(#93956,#93957,
#93958,#93959)),.UNSPECIFIED.,.F.,.F.,.F.,(4,4),(4,4),(-0.00286780122455666,
0.477902879794515),(0.0500263550858996,0.0565997133101404),
 .UNSPECIFIED.);
#2864=B_SPLINE_SURFACE_WITH_KNOTS('',3,3,((#93961,#93962,#93963,#93964),
(#93965,#93966,#93967,#93968),(#93969,#93970,#93971,#93972),(#93973,#93974,
#93975,#93976)),.UNSPECIFIED.,.F.,.F.,.F.,(4,4),(4,4),(0.522097120187377,
1.00286810177268),(0.046607398592944,0.0531834925888931),.UNSPECIFIED.);
#2865=B_SPLINE_SURFACE_WITH_KNOTS('',3,3,((#93984,#93985,#93986,#93987),
(#93988,#93989,#93990,#93991),(#93992,#93993,#93994,#93995),(#93996,#93997,
#93998,#93999)),.UNSPECIFIED.,.F.,.F.,.F.,(4,4),(4,4),(-0.00286792598896508,
0.477902879795425),(0.06001568654946,0.0665898698871157),.UNSPECIFIED.);
#2866=B_SPLINE_SURFACE_WITH_KNOTS('',3,3,((#94001,#94002,#94003,#94004),
(#94005,#94006,#94007,#94008),(#94009,#94010,#94011,#94012),(#94013,#94014,
#94015,#94016)),.UNSPECIFIED.,.F.,.F.,.F.,(4,4),(4,4),(0.522097120192157,
1.00286764392065),(0.056599713310142,0.0631721430887059),.UNSPECIFIED.);
#2867=B_SPLINE_SURFACE_WITH_KNOTS('',3,3,((#94032,#94033,#94034,#94035),
(#94036,#94037,#94038,#94039),(#94040,#94041,#94042,#94043),(#94044,#94045,
#94046,#94047)),.UNSPECIFIED.,.F.,.F.,.F.,(4,4),(4,4),(0.522097120187888,
1.00286833998592),(0.0665898698871188,0.0731716198748451),.UNSPECIFIED.);
#2868=B_SPLINE_SURFACE_WITH_KNOTS('',3,3,((#94048,#94049,#94050,#94051),
(#94052,#94053,#94054,#94055),(#94056,#94057,#94058,#94059),(#94060,#94061,
#94062,#94063)),.UNSPECIFIED.,.F.,.F.,.F.,(4,4),(4,4),(-0.0012473153123853,
0.20904511169894),(0.0700194292967067,0.0749900982978036),.UNSPECIFIED.);
#2869=B_SPLINE_SURFACE_WITH_KNOTS('',3,3,((#94070,#94071,#94072,#94073),
(#94074,#94075,#94076,#94077),(#94078,#94079,#94080,#94081),(#94082,#94083,
#94084,#94085)),.UNSPECIFIED.,.F.,.F.,.F.,(4,4),(4,4),(-0.00286791014463769,
0.477902879787847),(0.0100271466769354,0.0166015299239863),
 .UNSPECIFIED.);
#2870=B_SPLINE_SURFACE_WITH_KNOTS('',3,3,((#94087,#94088,#94089,#94090),
(#94091,#94092,#94093,#94094),(#94095,#94096,#94097,#94098),(#94099,#94100,
#94101,#94102)),.UNSPECIFIED.,.F.,.F.,.F.,(4,4),(4,4),(0.653230271487996,
1.00206901890057),(0.0065678839538601,0.0131849432428959),.UNSPECIFIED.);
#2871=B_SPLINE_SURFACE_WITH_KNOTS('',3,3,((#94110,#94111,#94112,#94113),
(#94114,#94115,#94116,#94117),(#94118,#94119,#94120,#94121),(#94122,#94123,
#94124,#94125)),.UNSPECIFIED.,.F.,.F.,.F.,(4,4),(4,4),(-0.00286780410470499,
0.477902879789078),(0.0200175229646918,0.0265907346180623),
 .UNSPECIFIED.);
#2872=B_SPLINE_SURFACE_WITH_KNOTS('',3,3,((#94127,#94128,#94129,#94130),
(#94131,#94132,#94133,#94134),(#94135,#94136,#94137,#94138),(#94139,#94140,
#94141,#94142)),.UNSPECIFIED.,.F.,.F.,.F.,(4,4),(4,4),(0.522097120187148,
1.00286753160136),(0.0166015299239889,0.023173678807522),.UNSPECIFIED.);
#2873=B_SPLINE_SURFACE_WITH_KNOTS('',3,3,((#94144,#94145,#94146,#94147),
(#94148,#94149,#94150,#94151),(#94152,#94153,#94154,#94155),(#94156,#94157,
#94158,#94159)),.UNSPECIFIED.,.F.,.F.,.F.,(4,4),(4,4),(0.,1.00600003961348),
(0.0166015299239894,0.0265907346180641),.UNSPECIFIED.);
#2874=B_SPLINE_SURFACE_WITH_KNOTS('',3,3,((#94160,#94161,#94162,#94163),
(#94164,#94165,#94166,#94167),(#94168,#94169,#94170,#94171),(#94172,#94173,
#94174,#94175)),.UNSPECIFIED.,.F.,.F.,.F.,(4,4),(4,4),(-0.00286862201164332,
0.47790287979074),(0.0300094532292789,0.0365944846647017),.UNSPECIFIED.);
#2875=B_SPLINE_SURFACE_WITH_KNOTS('',3,3,((#94177,#94178,#94179,#94180),
(#94181,#94182,#94183,#94184),(#94185,#94186,#94187,#94188),(#94189,#94190,
#94191,#94192)),.UNSPECIFIED.,.F.,.F.,.F.,(4,4),(4,4),(0.522097120187057,
1.00286823669314),(0.0265907346180631,0.0331702036889925),.UNSPECIFIED.);
#2876=B_SPLINE_SURFACE_WITH_KNOTS('',3,3,((#94200,#94201,#94202,#94203),
(#94204,#94205,#94206,#94207),(#94208,#94209,#94210,#94211),(#94212,#94213,
#94214,#94215)),.UNSPECIFIED.,.F.,.F.,.F.,(4,4),(4,4),(-0.00286848453332952,
0.477902879791493),(0.0400218729466608,0.0466073985929421),
 .UNSPECIFIED.);
#2877=B_SPLINE_SURFACE_WITH_KNOTS('',3,3,((#94232,#94233,#94234,#94235),
(#94236,#94237,#94238,#94239),(#94240,#94241,#94242,#94243),(#94244,#94245,
#94246,#94247)),.UNSPECIFIED.,.F.,.F.,.F.,(4,4),(4,4),(0.,1.00600014639748),
(0.0365944846644985,0.0466073985929158),.UNSPECIFIED.);
#2878=B_SPLINE_SURFACE_WITH_KNOTS('',3,3,((#94248,#94249,#94250,#94251),
(#94252,#94253,#94254,#94255),(#94256,#94257,#94258,#94259),(#94260,#94261,
#94262,#94263)),.UNSPECIFIED.,.F.,.F.,.F.,(4,4),(4,4),(-0.00286780122465239,
0.477902879792368),(0.0500263550858997,0.0565997133101407),
 .UNSPECIFIED.);
#2879=B_SPLINE_SURFACE_WITH_KNOTS('',3,3,((#94265,#94266,#94267,#94268),
(#94269,#94270,#94271,#94272),(#94273,#94274,#94275,#94276),(#94277,#94278,
#94279,#94280)),.UNSPECIFIED.,.F.,.F.,.F.,(4,4),(4,4),(0.522097120187087,
1.00286810177271),(0.046607398592944,0.0531834925888927),.UNSPECIFIED.);
#2880=B_SPLINE_SURFACE_WITH_KNOTS('',3,3,((#94288,#94289,#94290,#94291),
(#94292,#94293,#94294,#94295),(#94296,#94297,#94298,#94299),(#94300,#94301,
#94302,#94303)),.UNSPECIFIED.,.F.,.F.,.F.,(4,4),(4,4),(-0.00286792598898423,
0.477902879793432),(0.0600156865494613,0.0665898698871174),
 .UNSPECIFIED.);
#2881=B_SPLINE_SURFACE_WITH_KNOTS('',3,3,((#94305,#94306,#94307,#94308),
(#94309,#94310,#94311,#94312),(#94313,#94314,#94315,#94316),(#94317,#94318,
#94319,#94320)),.UNSPECIFIED.,.F.,.F.,.F.,(4,4),(4,4),(0.522097120191966,
1.00286764392046),(0.0565997133101417,0.0631721430887065),.UNSPECIFIED.);
#2882=B_SPLINE_SURFACE_WITH_KNOTS('',3,3,((#94336,#94337,#94338,#94339),
(#94340,#94341,#94342,#94343),(#94344,#94345,#94346,#94347),(#94348,#94349,
#94350,#94351)),.UNSPECIFIED.,.F.,.F.,.F.,(4,4),(4,4),(0.522097120187141,
1.00286833998606),(0.0665898698871199,0.0731716198748447),.UNSPECIFIED.);
#2883=B_SPLINE_SURFACE_WITH_KNOTS('',3,3,((#94352,#94353,#94354,#94355),
(#94356,#94357,#94358,#94359),(#94360,#94361,#94362,#94363),(#94364,#94365,
#94366,#94367)),.UNSPECIFIED.,.F.,.F.,.F.,(4,4),(4,4),(-0.00124731531428327,
0.20904511169693),(0.0700194292967153,0.0749900982977941),.UNSPECIFIED.);
#2884=B_SPLINE_SURFACE_WITH_KNOTS('',3,3,((#94374,#94375,#94376,#94377),
(#94378,#94379,#94380,#94381),(#94382,#94383,#94384,#94385),(#94386,#94387,
#94388,#94389)),.UNSPECIFIED.,.F.,.F.,.F.,(4,4),(4,4),(-0.00286791014465478,
0.47790287978797),(0.010027146676937,0.0166015299239869),.UNSPECIFIED.);
#2885=B_SPLINE_SURFACE_WITH_KNOTS('',3,3,((#94391,#94392,#94393,#94394),
(#94395,#94396,#94397,#94398),(#94399,#94400,#94401,#94402),(#94403,#94404,
#94405,#94406)),.UNSPECIFIED.,.F.,.F.,.F.,(4,4),(4,4),(0.653230271488951,
1.00206901890119),(0.00656788395403398,0.0131849432121938),
 .UNSPECIFIED.);
#2886=B_SPLINE_SURFACE_WITH_KNOTS('',3,3,((#94414,#94415,#94416,#94417),
(#94418,#94419,#94420,#94421),(#94422,#94423,#94424,#94425),(#94426,#94427,
#94428,#94429)),.UNSPECIFIED.,.F.,.F.,.F.,(4,4),(4,4),(-0.00286780410476047,
0.477902879787733),(0.0200175229646912,0.0265907346180626),
 .UNSPECIFIED.);
#2887=B_SPLINE_SURFACE_WITH_KNOTS('',3,3,((#94431,#94432,#94433,#94434),
(#94435,#94436,#94437,#94438),(#94439,#94440,#94441,#94442),(#94443,#94444,
#94445,#94446)),.UNSPECIFIED.,.F.,.F.,.F.,(4,4),(4,4),(0.522097120187582,
1.00286753160139),(0.016601529923988,0.0231736788075219),.UNSPECIFIED.);
#2888=B_SPLINE_SURFACE_WITH_KNOTS('',3,3,((#94448,#94449,#94450,#94451),
(#94452,#94453,#94454,#94455),(#94456,#94457,#94458,#94459),(#94460,#94461,
#94462,#94463)),.UNSPECIFIED.,.F.,.F.,.F.,(4,4),(4,4),(0.,1.00600003961397),
(0.0166015299239893,0.0265907346180646),.UNSPECIFIED.);
#2889=B_SPLINE_SURFACE_WITH_KNOTS('',3,3,((#94464,#94465,#94466,#94467),
(#94468,#94469,#94470,#94471),(#94472,#94473,#94474,#94475),(#94476,#94477,
#94478,#94479)),.UNSPECIFIED.,.F.,.F.,.F.,(4,4),(4,4),(-0.00286862201159924,
0.477902879789508),(0.0300094532292792,0.036594484664703),.UNSPECIFIED.);
#2890=B_SPLINE_SURFACE_WITH_KNOTS('',3,3,((#94481,#94482,#94483,#94484),
(#94485,#94486,#94487,#94488),(#94489,#94490,#94491,#94492),(#94493,#94494,
#94495,#94496)),.UNSPECIFIED.,.F.,.F.,.F.,(4,4),(4,4),(0.522097120187338,
1.00286823669316),(0.0265907346180638,0.0331702036889928),.UNSPECIFIED.);
#2891=B_SPLINE_SURFACE_WITH_KNOTS('',3,3,((#94504,#94505,#94506,#94507),
(#94508,#94509,#94510,#94511),(#94512,#94513,#94514,#94515),(#94516,#94517,
#94518,#94519)),.UNSPECIFIED.,.F.,.F.,.F.,(4,4),(4,4),(-0.0028684845333738,
0.477902879789181),(0.0400218729466608,0.0466073985929428),
 .UNSPECIFIED.);
#2892=B_SPLINE_SURFACE_WITH_KNOTS('',3,3,((#94536,#94537,#94538,#94539),
(#94540,#94541,#94542,#94543),(#94544,#94545,#94546,#94547),(#94548,#94549,
#94550,#94551)),.UNSPECIFIED.,.F.,.F.,.F.,(4,4),(4,4),(0.,1.00600014639733),
(0.0365944846644987,0.0466073985929149),.UNSPECIFIED.);
#2893=B_SPLINE_SURFACE_WITH_KNOTS('',3,3,((#94552,#94553,#94554,#94555),
(#94556,#94557,#94558,#94559),(#94560,#94561,#94562,#94563),(#94564,#94565,
#94566,#94567)),.UNSPECIFIED.,.F.,.F.,.F.,(4,4),(4,4),(-0.0028678012246552,
0.477902879790202),(0.0500263550859005,0.0565997133101566),
 .UNSPECIFIED.);
#2894=B_SPLINE_SURFACE_WITH_KNOTS('',3,3,((#94569,#94570,#94571,#94572),
(#94573,#94574,#94575,#94576),(#94577,#94578,#94579,#94580),(#94581,#94582,
#94583,#94584)),.UNSPECIFIED.,.F.,.F.,.F.,(4,4),(4,4),(0.522097120187115,
1.00286810177277),(0.0466073985929444,0.0531834925888919),.UNSPECIFIED.);
#2895=B_SPLINE_SURFACE_WITH_KNOTS('',3,3,((#94592,#94593,#94594,#94595),
(#94596,#94597,#94598,#94599),(#94600,#94601,#94602,#94603),(#94604,#94605,
#94606,#94607)),.UNSPECIFIED.,.F.,.F.,.F.,(4,4),(4,4),(-0.00286792598901002,
0.477902879791329),(0.0600156865494609,0.0665898698871177),
 .UNSPECIFIED.);
#2896=B_SPLINE_SURFACE_WITH_KNOTS('',3,3,((#94609,#94610,#94611,#94612),
(#94613,#94614,#94615,#94616),(#94617,#94618,#94619,#94620),(#94621,#94622,
#94623,#94624)),.UNSPECIFIED.,.F.,.F.,.F.,(4,4),(4,4),(0.522097120191972,
1.00286764392054),(0.0565997133101411,0.0631721430887067),.UNSPECIFIED.);
#2897=B_SPLINE_SURFACE_WITH_KNOTS('',3,3,((#94640,#94641,#94642,#94643),
(#94644,#94645,#94646,#94647),(#94648,#94649,#94650,#94651),(#94652,#94653,
#94654,#94655)),.UNSPECIFIED.,.F.,.F.,.F.,(4,4),(4,4),(0.522097120186964,
1.00286833998601),(0.0665898698871194,0.073171619874845),.UNSPECIFIED.);
#2898=B_SPLINE_SURFACE_WITH_KNOTS('',3,3,((#94656,#94657,#94658,#94659),
(#94660,#94661,#94662,#94663),(#94664,#94665,#94666,#94667),(#94668,#94669,
#94670,#94671)),.UNSPECIFIED.,.F.,.F.,.F.,(4,4),(4,4),(-0.00124731531647025,
0.209045111694821),(0.0700194292967201,0.0749900982977851),
 .UNSPECIFIED.);
#2899=B_SPLINE_SURFACE_WITH_KNOTS('',3,3,((#94678,#94679,#94680,#94681),
(#94682,#94683,#94684,#94685),(#94686,#94687,#94688,#94689),(#94690,#94691,
#94692,#94693)),.UNSPECIFIED.,.F.,.F.,.F.,(4,4),(4,4),(-0.00286791014469107,
0.477902879787991),(0.0100271466769376,0.0166015299239867),
 .UNSPECIFIED.);
#2900=B_SPLINE_SURFACE_WITH_KNOTS('',3,3,((#94695,#94696,#94697,#94698),
(#94699,#94700,#94701,#94702),(#94703,#94704,#94705,#94706),(#94707,#94708,
#94709,#94710)),.UNSPECIFIED.,.F.,.F.,.F.,(4,4),(4,4),(0.653230271490066,
1.00206901890208),(0.00656788395384224,0.013184943242989),.UNSPECIFIED.);
#2901=B_SPLINE_SURFACE_WITH_KNOTS('',3,3,((#94718,#94719,#94720,#94721),
(#94722,#94723,#94724,#94725),(#94726,#94727,#94728,#94729),(#94730,#94731,
#94732,#94733)),.UNSPECIFIED.,.F.,.F.,.F.,(4,4),(4,4),(-0.00286780410467914,
0.47790287978789),(0.0200175229646906,0.0265907346180624),.UNSPECIFIED.);
#2902=B_SPLINE_SURFACE_WITH_KNOTS('',3,3,((#94735,#94736,#94737,#94738),
(#94739,#94740,#94741,#94742),(#94743,#94744,#94745,#94746),(#94747,#94748,
#94749,#94750)),.UNSPECIFIED.,.F.,.F.,.F.,(4,4),(4,4),(0.522097120188421,
1.0028675316014),(0.0166015299239883,0.0231736788075223),.UNSPECIFIED.);
#2903=B_SPLINE_SURFACE_WITH_KNOTS('',3,3,((#94752,#94753,#94754,#94755),
(#94756,#94757,#94758,#94759),(#94760,#94761,#94762,#94763),(#94764,#94765,
#94766,#94767)),.UNSPECIFIED.,.F.,.F.,.F.,(4,4),(4,4),(0.,1.00600003961381),
(0.0166015299239883,0.0265907346180636),.UNSPECIFIED.);
#2904=B_SPLINE_SURFACE_WITH_KNOTS('',3,3,((#94768,#94769,#94770,#94771),
(#94772,#94773,#94774,#94775),(#94776,#94777,#94778,#94779),(#94780,#94781,
#94782,#94783)),.UNSPECIFIED.,.F.,.F.,.F.,(4,4),(4,4),(-0.00286862201160178,
0.477902879789629),(0.030009453229279,0.0365944846647018),.UNSPECIFIED.);
#2905=B_SPLINE_SURFACE_WITH_KNOTS('',3,3,((#94785,#94786,#94787,#94788),
(#94789,#94790,#94791,#94792),(#94793,#94794,#94795,#94796),(#94797,#94798,
#94799,#94800)),.UNSPECIFIED.,.F.,.F.,.F.,(4,4),(4,4),(0.522097120187916,
1.00286823669319),(0.0265907346180628,0.0331702036889921),.UNSPECIFIED.);
#2906=B_SPLINE_SURFACE_WITH_KNOTS('',3,3,((#94808,#94809,#94810,#94811),
(#94812,#94813,#94814,#94815),(#94816,#94817,#94818,#94819),(#94820,#94821,
#94822,#94823)),.UNSPECIFIED.,.F.,.F.,.F.,(4,4),(4,4),(-0.00286848453385445,
0.47790287986132),(0.0400218729466611,0.0466073985929426),.UNSPECIFIED.);
#2907=B_SPLINE_SURFACE_WITH_KNOTS('',3,3,((#94840,#94841,#94842,#94843),
(#94844,#94845,#94846,#94847),(#94848,#94849,#94850,#94851),(#94852,#94853,
#94854,#94855)),.UNSPECIFIED.,.F.,.F.,.F.,(4,4),(4,4),(0.,1.00600014639724),
(0.0365944846644992,0.0466073985929183),.UNSPECIFIED.);
#2908=B_SPLINE_SURFACE_WITH_KNOTS('',3,3,((#94856,#94857,#94858,#94859),
(#94860,#94861,#94862,#94863),(#94864,#94865,#94866,#94867),(#94868,#94869,
#94870,#94871)),.UNSPECIFIED.,.F.,.F.,.F.,(4,4),(4,4),(-0.00286780122466993,
0.477902879787799),(0.0500263550859,0.0565997133101405),.UNSPECIFIED.);
#2909=B_SPLINE_SURFACE_WITH_KNOTS('',3,3,((#94873,#94874,#94875,#94876),
(#94877,#94878,#94879,#94880),(#94881,#94882,#94883,#94884),(#94885,#94886,
#94887,#94888)),.UNSPECIFIED.,.F.,.F.,.F.,(4,4),(4,4),(0.522097120187333,
1.00286810177263),(0.0466073985929444,0.0531834925888926),.UNSPECIFIED.);
#2910=B_SPLINE_SURFACE_WITH_KNOTS('',3,3,((#94896,#94897,#94898,#94899),
(#94900,#94901,#94902,#94903),(#94904,#94905,#94906,#94907),(#94908,#94909,
#94910,#94911)),.UNSPECIFIED.,.F.,.F.,.F.,(4,4),(4,4),(-0.00286792598906402,
0.477902879788954),(0.0600156865494604,0.0665898698871162),
 .UNSPECIFIED.);
#2911=B_SPLINE_SURFACE_WITH_KNOTS('',3,3,((#94913,#94914,#94915,#94916),
(#94917,#94918,#94919,#94920),(#94921,#94922,#94923,#94924),(#94925,#94926,
#94927,#94928)),.UNSPECIFIED.,.F.,.F.,.F.,(4,4),(4,4),(0.52209712019194,
1.00286764392053),(0.0565997133101412,0.0631721430887059),.UNSPECIFIED.);
#2912=B_SPLINE_SURFACE_WITH_KNOTS('',3,3,((#94944,#94945,#94946,#94947),
(#94948,#94949,#94950,#94951),(#94952,#94953,#94954,#94955),(#94956,#94957,
#94958,#94959)),.UNSPECIFIED.,.F.,.F.,.F.,(4,4),(4,4),(0.522097120186829,
1.00286833998607),(0.0665898698871188,0.073171619874845),.UNSPECIFIED.);
#2913=B_SPLINE_SURFACE_WITH_KNOTS('',3,3,((#94960,#94961,#94962,#94963),
(#94964,#94965,#94966,#94967),(#94968,#94969,#94970,#94971),(#94972,#94973,
#94974,#94975)),.UNSPECIFIED.,.F.,.F.,.F.,(4,4),(4,4),(-0.00124731531869756,
0.209045111692496),(0.0700194292967225,0.0749900982977736),
 .UNSPECIFIED.);
#2914=B_SPLINE_SURFACE_WITH_KNOTS('',3,3,((#94982,#94983,#94984,#94985),
(#94986,#94987,#94988,#94989),(#94990,#94991,#94992,#94993),(#94994,#94995,
#94996,#94997)),.UNSPECIFIED.,.F.,.F.,.F.,(4,4),(4,4),(-0.00286791014473155,
0.477902879788205),(0.0100271466769362,0.0166015299239883),
 .UNSPECIFIED.);
#2915=B_SPLINE_SURFACE_WITH_KNOTS('',3,3,((#94999,#95000,#95001,#95002),
(#95003,#95004,#95005,#95006),(#95007,#95008,#95009,#95010),(#95011,#95012,
#95013,#95014)),.UNSPECIFIED.,.F.,.F.,.F.,(4,4),(4,4),(0.653230271491342,
1.00206901890342),(0.00656788395383524,0.0131849432428966),
 .UNSPECIFIED.);
#2916=B_SPLINE_SURFACE_WITH_KNOTS('',3,3,((#95022,#95023,#95024,#95025),
(#95026,#95027,#95028,#95029),(#95030,#95031,#95032,#95033),(#95034,#95035,
#95036,#95037)),.UNSPECIFIED.,.F.,.F.,.F.,(4,4),(4,4),(-0.00286780410464737,
0.477902879787977),(0.0200175229646909,0.0265907346180625),
 .UNSPECIFIED.);
#2917=B_SPLINE_SURFACE_WITH_KNOTS('',3,3,((#95039,#95040,#95041,#95042),
(#95043,#95044,#95045,#95046),(#95047,#95048,#95049,#95050),(#95051,#95052,
#95053,#95054)),.UNSPECIFIED.,.F.,.F.,.F.,(4,4),(4,4),(0.522097120189436,
1.0028675316014),(0.0166015299239882,0.0231736788037103),.UNSPECIFIED.);
#2918=B_SPLINE_SURFACE_WITH_KNOTS('',3,3,((#95056,#95057,#95058,#95059),
(#95060,#95061,#95062,#95063),(#95064,#95065,#95066,#95067),(#95068,#95069,
#95070,#95071)),.UNSPECIFIED.,.F.,.F.,.F.,(4,4),(4,4),(0.,1.00600003961361),
(0.0166015299239868,0.0265907346180623),.UNSPECIFIED.);
#2919=B_SPLINE_SURFACE_WITH_KNOTS('',3,3,((#95072,#95073,#95074,#95075),
(#95076,#95077,#95078,#95079),(#95080,#95081,#95082,#95083),(#95084,#95085,
#95086,#95087)),.UNSPECIFIED.,.F.,.F.,.F.,(4,4),(4,4),(-0.00286862201168353,
0.477902879789614),(0.0300094532292789,0.036594484664702),.UNSPECIFIED.);
#2920=B_SPLINE_SURFACE_WITH_KNOTS('',3,3,((#95089,#95090,#95091,#95092),
(#95093,#95094,#95095,#95096),(#95097,#95098,#95099,#95100),(#95101,#95102,
#95103,#95104)),.UNSPECIFIED.,.F.,.F.,.F.,(4,4),(4,4),(0.522097120188798,
1.00286823669314),(0.0265907346180632,0.0331702036622774),.UNSPECIFIED.);
#2921=B_SPLINE_SURFACE_WITH_KNOTS('',3,3,((#95112,#95113,#95114,#95115),
(#95116,#95117,#95118,#95119),(#95120,#95121,#95122,#95123),(#95124,#95125,
#95126,#95127)),.UNSPECIFIED.,.F.,.F.,.F.,(4,4),(4,4),(-0.00286848453343133,
0.477902879788268),(0.0400218729466607,0.046607398592943),.UNSPECIFIED.);
#2922=B_SPLINE_SURFACE_WITH_KNOTS('',3,3,((#95144,#95145,#95146,#95147),
(#95148,#95149,#95150,#95151),(#95152,#95153,#95154,#95155),(#95156,#95157,
#95158,#95159)),.UNSPECIFIED.,.F.,.F.,.F.,(4,4),(4,4),(0.,1.00600014639763),
(0.0365944846644997,0.0466073985929161),.UNSPECIFIED.);
#2923=B_SPLINE_SURFACE_WITH_KNOTS('',3,3,((#95160,#95161,#95162,#95163),
(#95164,#95165,#95166,#95167),(#95168,#95169,#95170,#95171),(#95172,#95173,
#95174,#95175)),.UNSPECIFIED.,.F.,.F.,.F.,(4,4),(4,4),(-0.00286780122468948,
0.477902879787664),(0.0500263550858997,0.0565997133101402),
 .UNSPECIFIED.);
#2924=B_SPLINE_SURFACE_WITH_KNOTS('',3,3,((#95177,#95178,#95179,#95180),
(#95181,#95182,#95183,#95184),(#95185,#95186,#95187,#95188),(#95189,#95190,
#95191,#95192)),.UNSPECIFIED.,.F.,.F.,.F.,(4,4),(4,4),(0.522097120187869,
1.00286810177258),(0.0466073985929447,0.0531834922865672),.UNSPECIFIED.);
#2925=B_SPLINE_SURFACE_WITH_KNOTS('',3,3,((#95200,#95201,#95202,#95203),
(#95204,#95205,#95206,#95207),(#95208,#95209,#95210,#95211),(#95212,#95213,
#95214,#95215)),.UNSPECIFIED.,.F.,.F.,.F.,(4,4),(4,4),(-0.00286792598893663,
0.477902879787536),(0.0600156865494607,0.0665898698871167),
 .UNSPECIFIED.);
#2926=B_SPLINE_SURFACE_WITH_KNOTS('',3,3,((#95217,#95218,#95219,#95220),
(#95221,#95222,#95223,#95224),(#95225,#95226,#95227,#95228),(#95229,#95230,
#95231,#95232)),.UNSPECIFIED.,.F.,.F.,.F.,(4,4),(4,4),(0.522097120192148,
1.00286764392044),(0.0565997133101418,0.0631721430887059),.UNSPECIFIED.);
#2927=B_SPLINE_SURFACE_WITH_KNOTS('',3,3,((#95248,#95249,#95250,#95251),
(#95252,#95253,#95254,#95255),(#95256,#95257,#95258,#95259),(#95260,#95261,
#95262,#95263)),.UNSPECIFIED.,.F.,.F.,.F.,(4,4),(4,4),(0.52209712018707,
1.00286833998598),(0.0665898698871193,0.0731716198748453),.UNSPECIFIED.);
#2928=B_SPLINE_SURFACE_WITH_KNOTS('',3,3,((#95264,#95265,#95266,#95267),
(#95268,#95269,#95270,#95271),(#95272,#95273,#95274,#95275),(#95276,#95277,
#95278,#95279)),.UNSPECIFIED.,.F.,.F.,.F.,(4,4),(4,4),(-0.00124731532117962,
0.209045111690077),(0.0700194292967239,0.0749900982977618),
 .UNSPECIFIED.);
#2929=B_SPLINE_SURFACE_WITH_KNOTS('',3,3,((#95286,#95287,#95288,#95289),
(#95290,#95291,#95292,#95293),(#95294,#95295,#95296,#95297),(#95298,#95299,
#95300,#95301)),.UNSPECIFIED.,.F.,.F.,.F.,(4,4),(4,4),(-0.00286791014476839,
0.477902879788331),(0.010027146676934,0.0166015299239869),.UNSPECIFIED.);
#2930=B_SPLINE_SURFACE_WITH_KNOTS('',3,3,((#95303,#95304,#95305,#95306),
(#95307,#95308,#95309,#95310),(#95311,#95312,#95313,#95314),(#95315,#95316,
#95317,#95318)),.UNSPECIFIED.,.F.,.F.,.F.,(4,4),(4,4),(0.653230271492636,
1.00206901890481),(0.00656788395382744,0.0131849432429878),
 .UNSPECIFIED.);
#2931=B_SPLINE_SURFACE_WITH_KNOTS('',3,3,((#95326,#95327,#95328,#95329),
(#95330,#95331,#95332,#95333),(#95334,#95335,#95336,#95337),(#95338,#95339,
#95340,#95341)),.UNSPECIFIED.,.F.,.F.,.F.,(4,4),(4,4),(-0.00286780410474824,
0.477902879788205),(0.0200175229646895,0.0265907346180613),
 .UNSPECIFIED.);
#2932=B_SPLINE_SURFACE_WITH_KNOTS('',3,3,((#95343,#95344,#95345,#95346),
(#95347,#95348,#95349,#95350),(#95351,#95352,#95353,#95354),(#95355,#95356,
#95357,#95358)),.UNSPECIFIED.,.F.,.F.,.F.,(4,4),(4,4),(0.522097120190702,
1.00286753160135),(0.0166015299239877,0.0231736788037103),.UNSPECIFIED.);
#2933=B_SPLINE_SURFACE_WITH_KNOTS('',3,3,((#95360,#95361,#95362,#95363),
(#95364,#95365,#95366,#95367),(#95368,#95369,#95370,#95371),(#95372,#95373,
#95374,#95375)),.UNSPECIFIED.,.F.,.F.,.F.,(4,4),(4,4),(0.,1.00600003961362),
(0.0166015299239903,0.0265907346180637),.UNSPECIFIED.);
#2934=B_SPLINE_SURFACE_WITH_KNOTS('',3,3,((#95376,#95377,#95378,#95379),
(#95380,#95381,#95382,#95383),(#95384,#95385,#95386,#95387),(#95388,#95389,
#95390,#95391)),.UNSPECIFIED.,.F.,.F.,.F.,(4,4),(4,4),(-0.0028686220116881,
0.477902879789794),(0.0300094532292792,0.0365944846647018),
 .UNSPECIFIED.);
#2935=B_SPLINE_SURFACE_WITH_KNOTS('',3,3,((#95393,#95394,#95395,#95396),
(#95397,#95398,#95399,#95400),(#95401,#95402,#95403,#95404),(#95405,#95406,
#95407,#95408)),.UNSPECIFIED.,.F.,.F.,.F.,(4,4),(4,4),(0.522097120190027,
1.00286823669311),(0.0265907346180631,0.0331702036889928),.UNSPECIFIED.);
#2936=B_SPLINE_SURFACE_WITH_KNOTS('',3,3,((#95416,#95417,#95418,#95419),
(#95420,#95421,#95422,#95423),(#95424,#95425,#95426,#95427),(#95428,#95429,
#95430,#95431)),.UNSPECIFIED.,.F.,.F.,.F.,(4,4),(4,4),(-0.00286848453347387,
0.477902879788492),(0.0400218729466595,0.0466073985929424),
 .UNSPECIFIED.);
#2937=B_SPLINE_SURFACE_WITH_KNOTS('',3,3,((#95448,#95449,#95450,#95451),
(#95452,#95453,#95454,#95455),(#95456,#95457,#95458,#95459),(#95460,#95461,
#95462,#95463)),.UNSPECIFIED.,.F.,.F.,.F.,(4,4),(4,4),(0.,1.00600014639749),
(0.0365944846644999,0.0466073985929169),.UNSPECIFIED.);
#2938=B_SPLINE_SURFACE_WITH_KNOTS('',3,3,((#95464,#95465,#95466,#95467),
(#95468,#95469,#95470,#95471),(#95472,#95473,#95474,#95475),(#95476,#95477,
#95478,#95479)),.UNSPECIFIED.,.F.,.F.,.F.,(4,4),(4,4),(-0.00286780122467789,
0.477902879787799),(0.0500263550858996,0.0565997133101406),
 .UNSPECIFIED.);
#2939=B_SPLINE_SURFACE_WITH_KNOTS('',3,3,((#95481,#95482,#95483,#95484),
(#95485,#95486,#95487,#95488),(#95489,#95490,#95491,#95492),(#95493,#95494,
#95495,#95496)),.UNSPECIFIED.,.F.,.F.,.F.,(4,4),(4,4),(0.522097120188824,
1.00286810177264),(0.0466073985929438,0.0531834925888932),.UNSPECIFIED.);
#2940=B_SPLINE_SURFACE_WITH_KNOTS('',3,3,((#95504,#95505,#95506,#95507),
(#95508,#95509,#95510,#95511),(#95512,#95513,#95514,#95515),(#95516,#95517,
#95518,#95519)),.UNSPECIFIED.,.F.,.F.,.F.,(4,4),(4,4),(-0.0028679259889164,
0.477902879787716),(0.0600156865494595,0.066589869887117),.UNSPECIFIED.);
#2941=B_SPLINE_SURFACE_WITH_KNOTS('',3,3,((#95521,#95522,#95523,#95524),
(#95525,#95526,#95527,#95528),(#95529,#95530,#95531,#95532),(#95533,#95534,
#95535,#95536)),.UNSPECIFIED.,.F.,.F.,.F.,(4,4),(4,4),(0.522097120192599,
1.00286764392051),(0.0565997133101417,0.0631721430887069),.UNSPECIFIED.);
#2942=B_SPLINE_SURFACE_WITH_KNOTS('',3,3,((#95552,#95553,#95554,#95555),
(#95556,#95557,#95558,#95559),(#95560,#95561,#95562,#95563),(#95564,#95565,
#95566,#95567)),.UNSPECIFIED.,.F.,.F.,.F.,(4,4),(4,4),(0.522097120187818,
1.00286833998607),(0.0665898698871186,0.0731716198748448),.UNSPECIFIED.);
#2943=B_SPLINE_SURFACE_WITH_KNOTS('',3,3,((#95568,#95569,#95570,#95571),
(#95572,#95573,#95574,#95575),(#95576,#95577,#95578,#95579),(#95580,#95581,
#95582,#95583)),.UNSPECIFIED.,.F.,.F.,.F.,(4,4),(4,4),(-0.0012473153236173,
0.209045111687613),(0.0700194292967237,0.0749900982977506),
 .UNSPECIFIED.);
#2944=B_SPLINE_SURFACE_WITH_KNOTS('',3,3,((#95590,#95591,#95592,#95593),
(#95594,#95595,#95596,#95597),(#95598,#95599,#95600,#95601),(#95602,#95603,
#95604,#95605)),.UNSPECIFIED.,.F.,.F.,.F.,(4,4),(4,4),(-0.00286791014474091,
0.477902879788312),(0.0100271466769347,0.0166015299239868),
 .UNSPECIFIED.);
#2945=B_SPLINE_SURFACE_WITH_KNOTS('',3,3,((#95607,#95608,#95609,#95610),
(#95611,#95612,#95613,#95614),(#95615,#95616,#95617,#95618),(#95619,#95620,
#95621,#95622)),.UNSPECIFIED.,.F.,.F.,.F.,(4,4),(4,4),(0.653230271494008,
1.00206901890662),(0.00656788395382045,0.0131849432428963),
 .UNSPECIFIED.);
#2946=B_SPLINE_SURFACE_WITH_KNOTS('',3,3,((#95630,#95631,#95632,#95633),
(#95634,#95635,#95636,#95637),(#95638,#95639,#95640,#95641),(#95642,#95643,
#95644,#95645)),.UNSPECIFIED.,.F.,.F.,.F.,(4,4),(4,4),(-0.00286780410476748,
0.477902879788327),(0.0200175229646906,0.0265907346180623),
 .UNSPECIFIED.);
#2947=B_SPLINE_SURFACE_WITH_KNOTS('',3,3,((#95647,#95648,#95649,#95650),
(#95651,#95652,#95653,#95654),(#95655,#95656,#95657,#95658),(#95659,#95660,
#95661,#95662)),.UNSPECIFIED.,.F.,.F.,.F.,(4,4),(4,4),(0.522097120192319,
1.00286753160135),(0.016601529923988,0.0231736788037106),.UNSPECIFIED.);
#2948=B_SPLINE_SURFACE_WITH_KNOTS('',3,3,((#95664,#95665,#95666,#95667),
(#95668,#95669,#95670,#95671),(#95672,#95673,#95674,#95675),(#95676,#95677,
#95678,#95679)),.UNSPECIFIED.,.F.,.F.,.F.,(4,4),(4,4),(0.,1.00600003961367),
(0.0166015299239903,0.0265907346180654),.UNSPECIFIED.);
#2949=B_SPLINE_SURFACE_WITH_KNOTS('',3,3,((#95680,#95681,#95682,#95683),
(#95684,#95685,#95686,#95687),(#95688,#95689,#95690,#95691),(#95692,#95693,
#95694,#95695)),.UNSPECIFIED.,.F.,.F.,.F.,(4,4),(4,4),(-0.00286862201167118,
0.477902879789893),(0.0300094532292783,0.0365944846647164),
 .UNSPECIFIED.);
#2950=B_SPLINE_SURFACE_WITH_KNOTS('',3,3,((#95697,#95698,#95699,#95700),
(#95701,#95702,#95703,#95704),(#95705,#95706,#95707,#95708),(#95709,#95710,
#95711,#95712)),.UNSPECIFIED.,.F.,.F.,.F.,(4,4),(4,4),(0.522097120191619,
1.0028682366931),(0.026590734618064,0.0331702036051744),.UNSPECIFIED.);
#2951=B_SPLINE_SURFACE_WITH_KNOTS('',3,3,((#95720,#95721,#95722,#95723),
(#95724,#95725,#95726,#95727),(#95728,#95729,#95730,#95731),(#95732,#95733,
#95734,#95735)),.UNSPECIFIED.,.F.,.F.,.F.,(4,4),(4,4),(-0.00286848453356115,
0.477902879788435),(0.0400218729466602,0.0466073985929428),
 .UNSPECIFIED.);
#2952=B_SPLINE_SURFACE_WITH_KNOTS('',3,3,((#95752,#95753,#95754,#95755),
(#95756,#95757,#95758,#95759),(#95760,#95761,#95762,#95763),(#95764,#95765,
#95766,#95767)),.UNSPECIFIED.,.F.,.F.,.F.,(4,4),(4,4),(0.,1.00600014639742),
(0.0365944846645018,0.046607398592917),.UNSPECIFIED.);
#2953=B_SPLINE_SURFACE_WITH_KNOTS('',3,3,((#95768,#95769,#95770,#95771),
(#95772,#95773,#95774,#95775),(#95776,#95777,#95778,#95779),(#95780,#95781,
#95782,#95783)),.UNSPECIFIED.,.F.,.F.,.F.,(4,4),(4,4),(-0.00286780122470004,
0.477902879787953),(0.0500263550858998,0.0565997133101408),
 .UNSPECIFIED.);
#2954=B_SPLINE_SURFACE_WITH_KNOTS('',3,3,((#95785,#95786,#95787,#95788),
(#95789,#95790,#95791,#95792),(#95793,#95794,#95795,#95796),(#95797,#95798,
#95799,#95800)),.UNSPECIFIED.,.F.,.F.,.F.,(4,4),(4,4),(0.522097120190077,
1.00286810177263),(0.0466073985929447,0.0531834925888939),.UNSPECIFIED.);
#2955=B_SPLINE_SURFACE_WITH_KNOTS('',3,3,((#95808,#95809,#95810,#95811),
(#95812,#95813,#95814,#95815),(#95816,#95817,#95818,#95819),(#95820,#95821,
#95822,#95823)),.UNSPECIFIED.,.F.,.F.,.F.,(4,4),(4,4),(-0.00286792598895217,
0.477902879787812),(0.0600156865494599,0.0665898698871171),
 .UNSPECIFIED.);
#2956=B_SPLINE_SURFACE_WITH_KNOTS('',3,3,((#95825,#95826,#95827,#95828),
(#95829,#95830,#95831,#95832),(#95833,#95834,#95835,#95836),(#95837,#95838,
#95839,#95840)),.UNSPECIFIED.,.F.,.F.,.F.,(4,4),(4,4),(0.522097120193104,
1.0028676439205),(0.0565997133101426,0.0631721430887066),.UNSPECIFIED.);
#2957=B_SPLINE_SURFACE_WITH_KNOTS('',3,3,((#95856,#95857,#95858,#95859),
(#95860,#95861,#95862,#95863),(#95864,#95865,#95866,#95867),(#95868,#95869,
#95870,#95871)),.UNSPECIFIED.,.F.,.F.,.F.,(4,4),(4,4),(0.522097120188608,
1.00286833998595),(0.0665898698871196,0.073171619874845),.UNSPECIFIED.);
#2958=B_SPLINE_SURFACE_WITH_KNOTS('',3,3,((#95872,#95873,#95874,#95875),
(#95876,#95877,#95878,#95879),(#95880,#95881,#95882,#95883),(#95884,#95885,
#95886,#95887)),.UNSPECIFIED.,.F.,.F.,.F.,(4,4),(4,4),(-0.00124731532625225,
0.209045111685989),(0.0700194292967225,0.0749900982977378),
 .UNSPECIFIED.);
#2959=B_SPLINE_SURFACE_WITH_KNOTS('',3,3,((#95894,#95895,#95896,#95897),
(#95898,#95899,#95900,#95901),(#95902,#95903,#95904,#95905),(#95906,#95907,
#95908,#95909)),.UNSPECIFIED.,.F.,.F.,.F.,(4,4),(4,4),(-0.00286791014464121,
0.477902879788685),(0.0100271466769344,0.0166015299239869),
 .UNSPECIFIED.);
#2960=B_SPLINE_SURFACE_WITH_KNOTS('',3,3,((#95911,#95912,#95913,#95914),
(#95915,#95916,#95917,#95918),(#95919,#95920,#95921,#95922),(#95923,#95924,
#95925,#95926)),.UNSPECIFIED.,.F.,.F.,.F.,(4,4),(4,4),(0.653230271495439,
1.00206901890855),(0.00656788395381374,0.0131849432429887),
 .UNSPECIFIED.);
#2961=B_SPLINE_SURFACE_WITH_KNOTS('',3,3,((#95934,#95935,#95936,#95937),
(#95938,#95939,#95940,#95941),(#95942,#95943,#95944,#95945),(#95946,#95947,
#95948,#95949)),.UNSPECIFIED.,.F.,.F.,.F.,(4,4),(4,4),(-0.00286780410480697,
0.477902879788339),(0.0200175229646895,0.026590734618062),.UNSPECIFIED.);
#2962=B_SPLINE_SURFACE_WITH_KNOTS('',3,3,((#95951,#95952,#95953,#95954),
(#95955,#95956,#95957,#95958),(#95959,#95960,#95961,#95962),(#95963,#95964,
#95965,#95966)),.UNSPECIFIED.,.F.,.F.,.F.,(4,4),(4,4),(0.522097120194227,
1.00286753160135),(0.0166015299239885,0.0231736788075229),.UNSPECIFIED.);
#2963=B_SPLINE_SURFACE_WITH_KNOTS('',3,3,((#95968,#95969,#95970,#95971),
(#95972,#95973,#95974,#95975),(#95976,#95977,#95978,#95979),(#95980,#95981,
#95982,#95983)),.UNSPECIFIED.,.F.,.F.,.F.,(4,4),(4,4),(0.,1.0060000396139),
(0.0166015299239893,0.0265907346180634),.UNSPECIFIED.);
#2964=B_SPLINE_SURFACE_WITH_KNOTS('',3,3,((#95984,#95985,#95986,#95987),
(#95988,#95989,#95990,#95991),(#95992,#95993,#95994,#95995),(#95996,#95997,
#95998,#95999)),.UNSPECIFIED.,.F.,.F.,.F.,(4,4),(4,4),(-0.00286862201168709,
0.477902879790105),(0.030009453229278,0.0365944846647019),.UNSPECIFIED.);
#2965=B_SPLINE_SURFACE_WITH_KNOTS('',3,3,((#96001,#96002,#96003,#96004),
(#96005,#96006,#96007,#96008),(#96009,#96010,#96011,#96012),(#96013,#96014,
#96015,#96016)),.UNSPECIFIED.,.F.,.F.,.F.,(4,4),(4,4),(0.522097120193262,
1.00286823669315),(0.0265907346180635,0.0331702036889921),.UNSPECIFIED.);
#2966=B_SPLINE_SURFACE_WITH_KNOTS('',3,3,((#96024,#96025,#96026,#96027),
(#96028,#96029,#96030,#96031),(#96032,#96033,#96034,#96035),(#96036,#96037,
#96038,#96039)),.UNSPECIFIED.,.F.,.F.,.F.,(4,4),(4,4),(-0.00286848453346161,
0.477902879788731),(0.0400218729466591,0.046607398592943),.UNSPECIFIED.);
#2967=B_SPLINE_SURFACE_WITH_KNOTS('',3,3,((#96056,#96057,#96058,#96059),
(#96060,#96061,#96062,#96063),(#96064,#96065,#96066,#96067),(#96068,#96069,
#96070,#96071)),.UNSPECIFIED.,.F.,.F.,.F.,(4,4),(4,4),(0.,1.00600014639745),
(0.0365944846645014,0.046607398592915),.UNSPECIFIED.);
#2968=B_SPLINE_SURFACE_WITH_KNOTS('',3,3,((#96072,#96073,#96074,#96075),
(#96076,#96077,#96078,#96079),(#96080,#96081,#96082,#96083),(#96084,#96085,
#96086,#96087)),.UNSPECIFIED.,.F.,.F.,.F.,(4,4),(4,4),(-0.00286780122479215,
0.477902879787963),(0.0500263550858996,0.0565997133101403),
 .UNSPECIFIED.);
#2969=B_SPLINE_SURFACE_WITH_KNOTS('',3,3,((#96089,#96090,#96091,#96092),
(#96093,#96094,#96095,#96096),(#96097,#96098,#96099,#96100),(#96101,#96102,
#96103,#96104)),.UNSPECIFIED.,.F.,.F.,.F.,(4,4),(4,4),(0.522097120191531,
1.00286810177261),(0.0466073985929444,0.0531834925888928),.UNSPECIFIED.);
#2970=B_SPLINE_SURFACE_WITH_KNOTS('',3,3,((#96112,#96113,#96114,#96115),
(#96116,#96117,#96118,#96119),(#96120,#96121,#96122,#96123),(#96124,#96125,
#96126,#96127)),.UNSPECIFIED.,.F.,.F.,.F.,(4,4),(4,4),(-0.0028679259889122,
0.47790287978794),(0.0600156865494595,0.0665898698871168),.UNSPECIFIED.);
#2971=B_SPLINE_SURFACE_WITH_KNOTS('',3,3,((#96129,#96130,#96131,#96132),
(#96133,#96134,#96135,#96136),(#96137,#96138,#96139,#96140),(#96141,#96142,
#96143,#96144)),.UNSPECIFIED.,.F.,.F.,.F.,(4,4),(4,4),(0.522097120193808,
1.00286764392049),(0.0565997133101416,0.0631721430887065),.UNSPECIFIED.);
#2972=B_SPLINE_SURFACE_WITH_KNOTS('',3,3,((#96160,#96161,#96162,#96163),
(#96164,#96165,#96166,#96167),(#96168,#96169,#96170,#96171),(#96172,#96173,
#96174,#96175)),.UNSPECIFIED.,.F.,.F.,.F.,(4,4),(4,4),(0.522097120189876,
1.00286833998599),(0.0665898698871201,0.073171619874845),.UNSPECIFIED.);
#2973=B_SPLINE_SURFACE_WITH_KNOTS('',3,3,((#96176,#96177,#96178,#96179),
(#96180,#96181,#96182,#96183),(#96184,#96185,#96186,#96187),(#96188,#96189,
#96190,#96191)),.UNSPECIFIED.,.F.,.F.,.F.,(4,4),(4,4),(-0.00124731532879475,
0.209045111684705),(0.070019429296718,0.0749900982977259),.UNSPECIFIED.);
#2974=B_SPLINE_SURFACE_WITH_KNOTS('',3,3,((#96198,#96199,#96200,#96201),
(#96202,#96203,#96204,#96205),(#96206,#96207,#96208,#96209),(#96210,#96211,
#96212,#96213)),.UNSPECIFIED.,.F.,.F.,.F.,(4,4),(4,4),(-0.00286791014460047,
0.477902879788786),(0.0100271466769346,0.0166015299239869),
 .UNSPECIFIED.);
#2975=B_SPLINE_SURFACE_WITH_KNOTS('',3,3,((#96215,#96216,#96217,#96218),
(#96219,#96220,#96221,#96222),(#96223,#96224,#96225,#96226),(#96227,#96228,
#96229,#96230)),.UNSPECIFIED.,.F.,.F.,.F.,(4,4),(4,4),(0.65323027149697,
1.00206901891073),(0.00656788395380929,0.0131849432428967),
 .UNSPECIFIED.);
#2976=B_SPLINE_SURFACE_WITH_KNOTS('',3,3,((#96238,#96239,#96240,#96241),
(#96242,#96243,#96244,#96245),(#96246,#96247,#96248,#96249),(#96250,#96251,
#96252,#96253)),.UNSPECIFIED.,.F.,.F.,.F.,(4,4),(4,4),(-0.0028678041047042,
0.477902879788517),(0.0200175229646909,0.0265907346180623),
 .UNSPECIFIED.);
#2977=B_SPLINE_SURFACE_WITH_KNOTS('',3,3,((#96255,#96256,#96257,#96258),
(#96259,#96260,#96261,#96262),(#96263,#96264,#96265,#96266),(#96267,#96268,
#96269,#96270)),.UNSPECIFIED.,.F.,.F.,.F.,(4,4),(4,4),(0.522097120196316,
1.00286753160137),(0.0166015299239891,0.0231736787930315),.UNSPECIFIED.);
#2978=B_SPLINE_SURFACE_WITH_KNOTS('',3,3,((#96272,#96273,#96274,#96275),
(#96276,#96277,#96278,#96279),(#96280,#96281,#96282,#96283),(#96284,#96285,
#96286,#96287)),.UNSPECIFIED.,.F.,.F.,.F.,(4,4),(4,4),(0.,1.00600003961326),
(0.016601529923986,0.0265907346180621),.UNSPECIFIED.);
#2979=B_SPLINE_SURFACE_WITH_KNOTS('',3,3,((#96288,#96289,#96290,#96291),
(#96292,#96293,#96294,#96295),(#96296,#96297,#96298,#96299),(#96300,#96301,
#96302,#96303)),.UNSPECIFIED.,.F.,.F.,.F.,(4,4),(4,4),(-0.002868622011607,
0.477902879790175),(0.0300094532292789,0.0365944846647016),
 .UNSPECIFIED.);
#2980=B_SPLINE_SURFACE_WITH_KNOTS('',3,3,((#96305,#96306,#96307,#96308),
(#96309,#96310,#96311,#96312),(#96313,#96314,#96315,#96316),(#96317,#96318,
#96319,#96320)),.UNSPECIFIED.,.F.,.F.,.F.,(4,4),(4,4),(0.522097120195324,
1.00286823669309),(0.0265907346180643,0.0331702036889928),.UNSPECIFIED.);
#2981=B_SPLINE_SURFACE_WITH_KNOTS('',3,3,((#96328,#96329,#96330,#96331),
(#96332,#96333,#96334,#96335),(#96336,#96337,#96338,#96339),(#96340,#96341,
#96342,#96343)),.UNSPECIFIED.,.F.,.F.,.F.,(4,4),(4,4),(-0.00286848453336819,
0.477902879788819),(0.0400218729466601,0.0466073985929425),
 .UNSPECIFIED.);
#2982=B_SPLINE_SURFACE_WITH_KNOTS('',3,3,((#96360,#96361,#96362,#96363),
(#96364,#96365,#96366,#96367),(#96368,#96369,#96370,#96371),(#96372,#96373,
#96374,#96375)),.UNSPECIFIED.,.F.,.F.,.F.,(4,4),(4,4),(0.,1.00600014639738),
(0.0365944846645024,0.0466073985929158),.UNSPECIFIED.);
#2983=B_SPLINE_SURFACE_WITH_KNOTS('',3,3,((#96376,#96377,#96378,#96379),
(#96380,#96381,#96382,#96383),(#96384,#96385,#96386,#96387),(#96388,#96389,
#96390,#96391)),.UNSPECIFIED.,.F.,.F.,.F.,(4,4),(4,4),(-0.00286780122472916,
0.477902879788083),(0.0500263550859002,0.0565997133101401),
 .UNSPECIFIED.);
#2984=B_SPLINE_SURFACE_WITH_KNOTS('',3,3,((#96393,#96394,#96395,#96396),
(#96397,#96398,#96399,#96400),(#96401,#96402,#96403,#96404),(#96405,#96406,
#96407,#96408)),.UNSPECIFIED.,.F.,.F.,.F.,(4,4),(4,4),(0.522097120193348,
1.0028681017726),(0.0466073985929442,0.0531834925888927),.UNSPECIFIED.);
#2985=B_SPLINE_SURFACE_WITH_KNOTS('',3,3,((#96416,#96417,#96418,#96419),
(#96420,#96421,#96422,#96423),(#96424,#96425,#96426,#96427),(#96428,#96429,
#96430,#96431)),.UNSPECIFIED.,.F.,.F.,.F.,(4,4),(4,4),(-0.00286792598894037,
0.477902879787975),(0.0600156865494599,0.0665898698871175),
 .UNSPECIFIED.);
#2986=B_SPLINE_SURFACE_WITH_KNOTS('',3,3,((#96433,#96434,#96435,#96436),
(#96437,#96438,#96439,#96440),(#96441,#96442,#96443,#96444),(#96445,#96446,
#96447,#96448)),.UNSPECIFIED.,.F.,.F.,.F.,(4,4),(4,4),(0.522097120194627,
1.00286764392052),(0.0565997133101422,0.0631721430887062),.UNSPECIFIED.);
#2987=B_SPLINE_SURFACE_WITH_KNOTS('',3,3,((#96464,#96465,#96466,#96467),
(#96468,#96469,#96470,#96471),(#96472,#96473,#96474,#96475),(#96476,#96477,
#96478,#96479)),.UNSPECIFIED.,.F.,.F.,.F.,(4,4),(4,4),(0.522097120191363,
1.00286833998609),(0.0665898698871185,0.0731716198748452),.UNSPECIFIED.);
#2988=B_SPLINE_SURFACE_WITH_KNOTS('',3,3,((#96480,#96481,#96482,#96483),
(#96484,#96485,#96486,#96487),(#96488,#96489,#96490,#96491),(#96492,#96493,
#96494,#96495)),.UNSPECIFIED.,.F.,.F.,.F.,(4,4),(4,4),(-0.00124731532115134,
0.209045111683166),(0.0700194292967135,0.0749900982977138),
 .UNSPECIFIED.);
#2989=B_SPLINE_SURFACE_WITH_KNOTS('',3,3,((#96502,#96503,#96504,#96505),
(#96506,#96507,#96508,#96509),(#96510,#96511,#96512,#96513),(#96514,#96515,
#96516,#96517)),.UNSPECIFIED.,.F.,.F.,.F.,(4,4),(4,4),(-0.00286791014476116,
0.477902879789011),(0.0100271466769342,0.0166015299239867),
 .UNSPECIFIED.);
#2990=B_SPLINE_SURFACE_WITH_KNOTS('',3,3,((#96519,#96520,#96521,#96522),
(#96523,#96524,#96525,#96526),(#96527,#96528,#96529,#96530),(#96531,#96532,
#96533,#96534)),.UNSPECIFIED.,.F.,.F.,.F.,(4,4),(4,4),(0.653230271498448,
1.00206901891297),(0.00656788395380222,0.013184943242988),.UNSPECIFIED.);
#2991=B_SPLINE_SURFACE_WITH_KNOTS('',3,3,((#96542,#96543,#96544,#96545),
(#96546,#96547,#96548,#96549),(#96550,#96551,#96552,#96553),(#96554,#96555,
#96556,#96557)),.UNSPECIFIED.,.F.,.F.,.F.,(4,4),(4,4),(-0.00286780410469616,
0.477902879788752),(0.0200175229646897,0.0265907346180627),
 .UNSPECIFIED.);
#2992=B_SPLINE_SURFACE_WITH_KNOTS('',3,3,((#96559,#96560,#96561,#96562),
(#96563,#96564,#96565,#96566),(#96567,#96568,#96569,#96570),(#96571,#96572,
#96573,#96574)),.UNSPECIFIED.,.F.,.F.,.F.,(4,4),(4,4),(0.522097120198486,
1.00286753160131),(0.0166015299239886,0.0231736788075218),.UNSPECIFIED.);
#2993=B_SPLINE_SURFACE_WITH_KNOTS('',3,3,((#96576,#96577,#96578,#96579),
(#96580,#96581,#96582,#96583),(#96584,#96585,#96586,#96587),(#96588,#96589,
#96590,#96591)),.UNSPECIFIED.,.F.,.F.,.F.,(4,4),(4,4),(0.,1.00600003961412),
(0.0166015299239884,0.0265907346180622),.UNSPECIFIED.);
#2994=B_SPLINE_SURFACE_WITH_KNOTS('',3,3,((#96592,#96593,#96594,#96595),
(#96596,#96597,#96598,#96599),(#96600,#96601,#96602,#96603),(#96604,#96605,
#96606,#96607)),.UNSPECIFIED.,.F.,.F.,.F.,(4,4),(4,4),(-0.00286862201157625,
0.477902879790364),(0.0300094532292792,0.0365944846647022),
 .UNSPECIFIED.);
#2995=B_SPLINE_SURFACE_WITH_KNOTS('',3,3,((#96609,#96610,#96611,#96612),
(#96613,#96614,#96615,#96616),(#96617,#96618,#96619,#96620),(#96621,#96622,
#96623,#96624)),.UNSPECIFIED.,.F.,.F.,.F.,(4,4),(4,4),(0.522097120197417,
1.0028682366931),(0.0265907346180633,0.0331702036889933),.UNSPECIFIED.);
#2996=B_SPLINE_SURFACE_WITH_KNOTS('',3,3,((#96632,#96633,#96634,#96635),
(#96636,#96637,#96638,#96639),(#96640,#96641,#96642,#96643),(#96644,#96645,
#96646,#96647)),.UNSPECIFIED.,.F.,.F.,.F.,(4,4),(4,4),(-0.00286848453359728,
0.477902879788827),(0.0400218729466586,0.0466073985929424),
 .UNSPECIFIED.);
#2997=B_SPLINE_SURFACE_WITH_KNOTS('',3,3,((#96664,#96665,#96666,#96667),
(#96668,#96669,#96670,#96671),(#96672,#96673,#96674,#96675),(#96676,#96677,
#96678,#96679)),.UNSPECIFIED.,.F.,.F.,.F.,(4,4),(4,4),(0.,1.00600014639725),
(0.0365944846645025,0.0466073985929155),.UNSPECIFIED.);
#2998=B_SPLINE_SURFACE_WITH_KNOTS('',3,3,((#96680,#96681,#96682,#96683),
(#96684,#96685,#96686,#96687),(#96688,#96689,#96690,#96691),(#96692,#96693,
#96694,#96695)),.UNSPECIFIED.,.F.,.F.,.F.,(4,4),(4,4),(-0.00286780122481621,
0.477902879788107),(0.0500263550858988,0.0565997133101405),
 .UNSPECIFIED.);
#2999=B_SPLINE_SURFACE_WITH_KNOTS('',3,3,((#96697,#96698,#96699,#96700),
(#96701,#96702,#96703,#96704),(#96705,#96706,#96707,#96708),(#96709,#96710,
#96711,#96712)),.UNSPECIFIED.,.F.,.F.,.F.,(4,4),(4,4),(0.5220971201952,
1.0028681017726),(0.0466073985929438,0.0531834925888936),.UNSPECIFIED.);
#3000=B_SPLINE_SURFACE_WITH_KNOTS('',3,3,((#96720,#96721,#96722,#96723),
(#96724,#96725,#96726,#96727),(#96728,#96729,#96730,#96731),(#96732,#96733,
#96734,#96735)),.UNSPECIFIED.,.F.,.F.,.F.,(4,4),(4,4),(-0.0028679259890384,
0.477902879788142),(0.0600156865494599,0.0665898698871172),
 .UNSPECIFIED.);
#3001=B_SPLINE_SURFACE_WITH_KNOTS('',3,3,((#96737,#96738,#96739,#96740),
(#96741,#96742,#96743,#96744),(#96745,#96746,#96747,#96748),(#96749,#96750,
#96751,#96752)),.UNSPECIFIED.,.F.,.F.,.F.,(4,4),(4,4),(0.522097120195508,
1.00286764392054),(0.0565997133101409,0.0631721430887068),.UNSPECIFIED.);
#3002=B_SPLINE_SURFACE_WITH_KNOTS('',3,3,((#96768,#96769,#96770,#96771),
(#96772,#96773,#96774,#96775),(#96776,#96777,#96778,#96779),(#96780,#96781,
#96782,#96783)),.UNSPECIFIED.,.F.,.F.,.F.,(4,4),(4,4),(0.52209712019312,
1.00286833998605),(0.066589869887118,0.0731716198748457),.UNSPECIFIED.);
#3003=B_SPLINE_SURFACE_WITH_KNOTS('',3,3,((#96784,#96785,#96786,#96787),
(#96788,#96789,#96790,#96791),(#96792,#96793,#96794,#96795),(#96796,#96797,
#96798,#96799)),.UNSPECIFIED.,.F.,.F.,.F.,(4,4),(4,4),(-0.0012473153211076,
0.209045111681666),(0.0700194292967032,0.0749900982977026),
 .UNSPECIFIED.);
#3004=B_SPLINE_SURFACE_WITH_KNOTS('',3,3,((#96806,#96807,#96808,#96809),
(#96810,#96811,#96812,#96813),(#96814,#96815,#96816,#96817),(#96818,#96819,
#96820,#96821)),.UNSPECIFIED.,.F.,.F.,.F.,(4,4),(4,4),(-0.00286791014473917,
0.477902879789097),(0.0100271466769336,0.0166015299239868),
 .UNSPECIFIED.);
#3005=B_SPLINE_SURFACE_WITH_KNOTS('',3,3,((#96823,#96824,#96825,#96826),
(#96827,#96828,#96829,#96830),(#96831,#96832,#96833,#96834),(#96835,#96836,
#96837,#96838)),.UNSPECIFIED.,.F.,.F.,.F.,(4,4),(4,4),(0.653230271499908,
1.00206901891551),(0.00656788395379813,0.0131849432429885),
 .UNSPECIFIED.);
#3006=B_SPLINE_SURFACE_WITH_KNOTS('',3,3,((#96846,#96847,#96848,#96849),
(#96850,#96851,#96852,#96853),(#96854,#96855,#96856,#96857),(#96858,#96859,
#96860,#96861)),.UNSPECIFIED.,.F.,.F.,.F.,(4,4),(4,4),(-0.00286780410476446,
0.477902879788805),(0.0200175229646903,0.0265907346180629),
 .UNSPECIFIED.);
#3007=B_SPLINE_SURFACE_WITH_KNOTS('',3,3,((#96863,#96864,#96865,#96866),
(#96867,#96868,#96869,#96870),(#96871,#96872,#96873,#96874),(#96875,#96876,
#96877,#96878)),.UNSPECIFIED.,.F.,.F.,.F.,(4,4),(4,4),(0.522097120200814,
1.00286753160131),(0.0166015299239891,0.0231736787930312),.UNSPECIFIED.);
#3008=B_SPLINE_SURFACE_WITH_KNOTS('',3,3,((#96880,#96881,#96882,#96883),
(#96884,#96885,#96886,#96887),(#96888,#96889,#96890,#96891),(#96892,#96893,
#96894,#96895)),.UNSPECIFIED.,.F.,.F.,.F.,(4,4),(4,4),(0.,1.00600003961374),
(0.0166015299239868,0.0265907346180621),.UNSPECIFIED.);
#3009=B_SPLINE_SURFACE_WITH_KNOTS('',3,3,((#96896,#96897,#96898,#96899),
(#96900,#96901,#96902,#96903),(#96904,#96905,#96906,#96907),(#96908,#96909,
#96910,#96911)),.UNSPECIFIED.,.F.,.F.,.F.,(4,4),(4,4),(-0.00286862201174504,
0.477902879790358),(0.0300094532292793,0.0365944846647016),
 .UNSPECIFIED.);
#3010=B_SPLINE_SURFACE_WITH_KNOTS('',3,3,((#96913,#96914,#96915,#96916),
(#96917,#96918,#96919,#96920),(#96921,#96922,#96923,#96924),(#96925,#96926,
#96927,#96928)),.UNSPECIFIED.,.F.,.F.,.F.,(4,4),(4,4),(0.522097120199715,
1.00286823669304),(0.0265907346180626,0.0331702036889934),.UNSPECIFIED.);
#3011=B_SPLINE_SURFACE_WITH_KNOTS('',3,3,((#96936,#96937,#96938,#96939),
(#96940,#96941,#96942,#96943),(#96944,#96945,#96946,#96947),(#96948,#96949,
#96950,#96951)),.UNSPECIFIED.,.F.,.F.,.F.,(4,4),(4,4),(-0.00286848453345688,
0.477902879788998),(0.0400218729466602,0.0466073985929435),
 .UNSPECIFIED.);
#3012=B_SPLINE_SURFACE_WITH_KNOTS('',3,3,((#96968,#96969,#96970,#96971),
(#96972,#96973,#96974,#96975),(#96976,#96977,#96978,#96979),(#96980,#96981,
#96982,#96983)),.UNSPECIFIED.,.F.,.F.,.F.,(4,4),(4,4),(0.,1.0060001463976),
(0.0365944846645024,0.0466073985929158),.UNSPECIFIED.);
#3013=B_SPLINE_SURFACE_WITH_KNOTS('',3,3,((#96984,#96985,#96986,#96987),
(#96988,#96989,#96990,#96991),(#96992,#96993,#96994,#96995),(#96996,#96997,
#96998,#96999)),.UNSPECIFIED.,.F.,.F.,.F.,(4,4),(4,4),(-0.00286780122472176,
0.47790287978859),(0.0500263550858996,0.0565997133101399),.UNSPECIFIED.);
#3014=B_SPLINE_SURFACE_WITH_KNOTS('',3,3,((#97001,#97002,#97003,#97004),
(#97005,#97006,#97007,#97008),(#97009,#97010,#97011,#97012),(#97013,#97014,
#97015,#97016)),.UNSPECIFIED.,.F.,.F.,.F.,(4,4),(4,4),(0.522097120197378,
1.00286810177282),(0.0466073985929436,0.0531834933545503),.UNSPECIFIED.);
#3015=B_SPLINE_SURFACE_WITH_KNOTS('',3,3,((#97024,#97025,#97026,#97027),
(#97028,#97029,#97030,#97031),(#97032,#97033,#97034,#97035),(#97036,#97037,
#97038,#97039)),.UNSPECIFIED.,.F.,.F.,.F.,(4,4),(4,4),(-0.00286792598899008,
0.477902879788161),(0.0600156865494598,0.0665898698871171),
 .UNSPECIFIED.);
#3016=B_SPLINE_SURFACE_WITH_KNOTS('',3,3,((#97041,#97042,#97043,#97044),
(#97045,#97046,#97047,#97048),(#97049,#97050,#97051,#97052),(#97053,#97054,
#97055,#97056)),.UNSPECIFIED.,.F.,.F.,.F.,(4,4),(4,4),(0.522097120196579,
1.00286764392047),(0.056599713310142,0.0631721430887062),.UNSPECIFIED.);
#3017=B_SPLINE_SURFACE_WITH_KNOTS('',3,3,((#97072,#97073,#97074,#97075),
(#97076,#97077,#97078,#97079),(#97080,#97081,#97082,#97083),(#97084,#97085,
#97086,#97087)),.UNSPECIFIED.,.F.,.F.,.F.,(4,4),(4,4),(0.522097120195032,
1.00286833998602),(0.0665898698871187,0.0731716198748464),.UNSPECIFIED.);
#3018=B_SPLINE_SURFACE_WITH_KNOTS('',3,3,((#97088,#97089,#97090,#97091),
(#97092,#97093,#97094,#97095),(#97096,#97097,#97098,#97099),(#97100,#97101,
#97102,#97103)),.UNSPECIFIED.,.F.,.F.,.F.,(4,4),(4,4),(-0.00124731532104556,
0.209045111680193),(0.0700194292966934,0.0749900982976918),
 .UNSPECIFIED.);
#3019=B_SPLINE_SURFACE_WITH_KNOTS('',3,3,((#97110,#97111,#97112,#97113),
(#97114,#97115,#97116,#97117),(#97118,#97119,#97120,#97121),(#97122,#97123,
#97124,#97125)),.UNSPECIFIED.,.F.,.F.,.F.,(4,4),(4,4),(-0.00286791014469159,
0.477902879789153),(0.0100271466769335,0.0166015299239866),
 .UNSPECIFIED.);
#3020=B_SPLINE_SURFACE_WITH_KNOTS('',3,3,((#97127,#97128,#97129,#97130),
(#97131,#97132,#97133,#97134),(#97135,#97136,#97137,#97138),(#97139,#97140,
#97141,#97142)),.UNSPECIFIED.,.F.,.F.,.F.,(4,4),(4,4),(0.65323027150149,
1.00206901891795),(0.0065678839537943,0.0131849432429871),.UNSPECIFIED.);
#3021=B_SPLINE_SURFACE_WITH_KNOTS('',3,3,((#97150,#97151,#97152,#97153),
(#97154,#97155,#97156,#97157),(#97158,#97159,#97160,#97161),(#97162,#97163,
#97164,#97165)),.UNSPECIFIED.,.F.,.F.,.F.,(4,4),(4,4),(-0.00286780410462738,
0.477902879788914),(0.0200175229646893,0.0265907346180623),
 .UNSPECIFIED.);
#3022=B_SPLINE_SURFACE_WITH_KNOTS('',3,3,((#97167,#97168,#97169,#97170),
(#97171,#97172,#97173,#97174),(#97175,#97176,#97177,#97178),(#97179,#97180,
#97181,#97182)),.UNSPECIFIED.,.F.,.F.,.F.,(4,4),(4,4),(0.522097120203192,
1.00286753160128),(0.0166015299239873,0.0231736788075223),.UNSPECIFIED.);
#3023=B_SPLINE_SURFACE_WITH_KNOTS('',3,3,((#97184,#97185,#97186,#97187),
(#97188,#97189,#97190,#97191),(#97192,#97193,#97194,#97195),(#97196,#97197,
#97198,#97199)),.UNSPECIFIED.,.F.,.F.,.F.,(4,4),(4,4),(0.,1.00600003961393),
(0.0166015299239881,0.0265907346180636),.UNSPECIFIED.);
#3024=B_SPLINE_SURFACE_WITH_KNOTS('',3,3,((#97200,#97201,#97202,#97203),
(#97204,#97205,#97206,#97207),(#97208,#97209,#97210,#97211),(#97212,#97213,
#97214,#97215)),.UNSPECIFIED.,.F.,.F.,.F.,(4,4),(4,4),(-0.00286862201168659,
0.477902879790677),(0.0300094532292788,0.0365944846647015),
 .UNSPECIFIED.);
#3025=B_SPLINE_SURFACE_WITH_KNOTS('',3,3,((#97217,#97218,#97219,#97220),
(#97221,#97222,#97223,#97224),(#97225,#97226,#97227,#97228),(#97229,#97230,
#97231,#97232)),.UNSPECIFIED.,.F.,.F.,.F.,(4,4),(4,4),(0.522097120202095,
1.00286823669305),(0.0265907346180628,0.0331702036889925),.UNSPECIFIED.);
#3026=B_SPLINE_SURFACE_WITH_KNOTS('',3,3,((#97240,#97241,#97242,#97243),
(#97244,#97245,#97246,#97247),(#97248,#97249,#97250,#97251),(#97252,#97253,
#97254,#97255)),.UNSPECIFIED.,.F.,.F.,.F.,(4,4),(4,4),(-0.00286848453351476,
0.47790287978917),(0.0400218729466592,0.0466073985929419),.UNSPECIFIED.);
#3027=B_SPLINE_SURFACE_WITH_KNOTS('',3,3,((#97272,#97273,#97274,#97275),
(#97276,#97277,#97278,#97279),(#97280,#97281,#97282,#97283),(#97284,#97285,
#97286,#97287)),.UNSPECIFIED.,.F.,.F.,.F.,(4,4),(4,4),(0.,1.00600014639755),
(0.0365944846645033,0.0466073985929164),.UNSPECIFIED.);
#3028=B_SPLINE_SURFACE_WITH_KNOTS('',3,3,((#97288,#97289,#97290,#97291),
(#97292,#97293,#97294,#97295),(#97296,#97297,#97298,#97299),(#97300,#97301,
#97302,#97303)),.UNSPECIFIED.,.F.,.F.,.F.,(4,4),(4,4),(-0.00286780122478771,
0.477902879788463),(0.0500263550858998,0.0565997133101397),
 .UNSPECIFIED.);
#3029=B_SPLINE_SURFACE_WITH_KNOTS('',3,3,((#97305,#97306,#97307,#97308),
(#97309,#97310,#97311,#97312),(#97313,#97314,#97315,#97316),(#97317,#97318,
#97319,#97320)),.UNSPECIFIED.,.F.,.F.,.F.,(4,4),(4,4),(0.522097120199638,
1.00286810177254),(0.0466073985929435,0.0531834925888921),.UNSPECIFIED.);
#3030=B_SPLINE_SURFACE_WITH_KNOTS('',3,3,((#97328,#97329,#97330,#97331),
(#97332,#97333,#97334,#97335),(#97336,#97337,#97338,#97339),(#97340,#97341,
#97342,#97343)),.UNSPECIFIED.,.F.,.F.,.F.,(4,4),(4,4),(-0.00286792598894184,
0.477902879788324),(0.0600156865494592,0.0665898698871167),
 .UNSPECIFIED.);
#3031=B_SPLINE_SURFACE_WITH_KNOTS('',3,3,((#97345,#97346,#97347,#97348),
(#97349,#97350,#97351,#97352),(#97353,#97354,#97355,#97356),(#97357,#97358,
#97359,#97360)),.UNSPECIFIED.,.F.,.F.,.F.,(4,4),(4,4),(0.522097120198475,
1.0028676439205),(0.0565997133101411,0.0631721430887063),.UNSPECIFIED.);
#3032=B_SPLINE_SURFACE_WITH_KNOTS('',3,3,((#97376,#97377,#97378,#97379),
(#97380,#97381,#97382,#97383),(#97384,#97385,#97386,#97387),(#97388,#97389,
#97390,#97391)),.UNSPECIFIED.,.F.,.F.,.F.,(4,4),(4,4),(0.522097120197217,
1.00286833998599),(0.0665898698871181,0.0731716198748449),.UNSPECIFIED.);
#3033=B_SPLINE_SURFACE_WITH_KNOTS('',3,3,((#97392,#97393,#97394,#97395),
(#97396,#97397,#97398,#97399),(#97400,#97401,#97402,#97403),(#97404,#97405,
#97406,#97407)),.UNSPECIFIED.,.F.,.F.,.F.,(4,4),(4,4),(-0.00124731532105012,
0.209045111678836),(0.0700194292966838,0.0749900982976822),
 .UNSPECIFIED.);
#3034=B_SPLINE_SURFACE_WITH_KNOTS('',3,3,((#97414,#97415,#97416,#97417),
(#97418,#97419,#97420,#97421),(#97422,#97423,#97424,#97425),(#97426,#97427,
#97428,#97429)),.UNSPECIFIED.,.F.,.F.,.F.,(4,4),(4,4),(-0.0028679101447297,
0.477902879789159),(0.0100271466769351,0.0166015299239871),
 .UNSPECIFIED.);
#3035=B_SPLINE_SURFACE_WITH_KNOTS('',3,3,((#97431,#97432,#97433,#97434),
(#97435,#97436,#97437,#97438),(#97439,#97440,#97441,#97442),(#97443,#97444,
#97445,#97446)),.UNSPECIFIED.,.F.,.F.,.F.,(4,4),(4,4),(0.653230271502837,
1.00206901892052),(0.00656788395379318,0.0131849432429889),
 .UNSPECIFIED.);
#3036=B_SPLINE_SURFACE_WITH_KNOTS('',3,3,((#97454,#97455,#97456,#97457),
(#97458,#97459,#97460,#97461),(#97462,#97463,#97464,#97465),(#97466,#97467,
#97468,#97469)),.UNSPECIFIED.,.F.,.F.,.F.,(4,4),(4,4),(-0.00286780410467987,
0.477902879789059),(0.0200175229646905,0.0265907346180626),
 .UNSPECIFIED.);
#3037=B_SPLINE_SURFACE_WITH_KNOTS('',3,3,((#97471,#97472,#97473,#97474),
(#97475,#97476,#97477,#97478),(#97479,#97480,#97481,#97482),(#97483,#97484,
#97485,#97486)),.UNSPECIFIED.,.F.,.F.,.F.,(4,4),(4,4),(0.522097120205828,
1.00286753160122),(0.016601529923988,0.0231736788075224),.UNSPECIFIED.);
#3038=B_SPLINE_SURFACE_WITH_KNOTS('',3,3,((#97488,#97489,#97490,#97491),
(#97492,#97493,#97494,#97495),(#97496,#97497,#97498,#97499),(#97500,#97501,
#97502,#97503)),.UNSPECIFIED.,.F.,.F.,.F.,(4,4),(4,4),(0.,1.00600003961379),
(0.016601529923988,0.0265907346180635),.UNSPECIFIED.);
#3039=B_SPLINE_SURFACE_WITH_KNOTS('',3,3,((#97504,#97505,#97506,#97507),
(#97508,#97509,#97510,#97511),(#97512,#97513,#97514,#97515),(#97516,#97517,
#97518,#97519)),.UNSPECIFIED.,.F.,.F.,.F.,(4,4),(4,4),(-0.00286862201166983,
0.477902879790738),(0.0300094532292793,0.0365944846647023),
 .UNSPECIFIED.);
#3040=B_SPLINE_SURFACE_WITH_KNOTS('',3,3,((#97521,#97522,#97523,#97524),
(#97525,#97526,#97527,#97528),(#97529,#97530,#97531,#97532),(#97533,#97534,
#97535,#97536)),.UNSPECIFIED.,.F.,.F.,.F.,(4,4),(4,4),(0.522097120204583,
1.00286823669297),(0.0265907346180627,0.0331702036051738),.UNSPECIFIED.);
#3041=B_SPLINE_SURFACE_WITH_KNOTS('',3,3,((#97544,#97545,#97546,#97547),
(#97548,#97549,#97550,#97551),(#97552,#97553,#97554,#97555),(#97556,#97557,
#97558,#97559)),.UNSPECIFIED.,.F.,.F.,.F.,(4,4),(4,4),(-0.0028684845334923,
0.477902879789434),(0.04002187294666,0.0466073985929439),.UNSPECIFIED.);
#3042=B_SPLINE_SURFACE_WITH_KNOTS('',3,3,((#97576,#97577,#97578,#97579),
(#97580,#97581,#97582,#97583),(#97584,#97585,#97586,#97587),(#97588,#97589,
#97590,#97591)),.UNSPECIFIED.,.F.,.F.,.F.,(4,4),(4,4),(0.,1.00600014639746),
(0.0365944846645047,0.0466073985929165),.UNSPECIFIED.);
#3043=B_SPLINE_SURFACE_WITH_KNOTS('',3,3,((#97592,#97593,#97594,#97595),
(#97596,#97597,#97598,#97599),(#97600,#97601,#97602,#97603),(#97604,#97605,
#97606,#97607)),.UNSPECIFIED.,.F.,.F.,.F.,(4,4),(4,4),(-0.00286780122482743,
0.477902879788715),(0.0500263550859003,0.0565997133101399),
 .UNSPECIFIED.);
#3044=B_SPLINE_SURFACE_WITH_KNOTS('',3,3,((#97609,#97610,#97611,#97612),
(#97613,#97614,#97615,#97616),(#97617,#97618,#97619,#97620),(#97621,#97622,
#97623,#97624)),.UNSPECIFIED.,.F.,.F.,.F.,(4,4),(4,4),(0.522097120202103,
1.00286810177252),(0.0466073985929445,0.0531834925888931),.UNSPECIFIED.);
#3045=B_SPLINE_SURFACE_WITH_KNOTS('',3,3,((#97632,#97633,#97634,#97635),
(#97636,#97637,#97638,#97639),(#97640,#97641,#97642,#97643),(#97644,#97645,
#97646,#97647)),.UNSPECIFIED.,.F.,.F.,.F.,(4,4),(4,4),(-0.00286792598910059,
0.477902879788515),(0.0600156865494612,0.0665898698871175),
 .UNSPECIFIED.);
#3046=B_SPLINE_SURFACE_WITH_KNOTS('',3,3,((#97649,#97650,#97651,#97652),
(#97653,#97654,#97655,#97656),(#97657,#97658,#97659,#97660),(#97661,#97662,
#97663,#97664)),.UNSPECIFIED.,.F.,.F.,.F.,(4,4),(4,4),(0.522097120200887,
1.0028676439205),(0.0565997133101418,0.0631721430887064),.UNSPECIFIED.);
#3047=B_SPLINE_SURFACE_WITH_KNOTS('',3,3,((#97680,#97681,#97682,#97683),
(#97684,#97685,#97686,#97687),(#97688,#97689,#97690,#97691),(#97692,#97693,
#97694,#97695)),.UNSPECIFIED.,.F.,.F.,.F.,(4,4),(4,4),(0.522097120199466,
1.00286833998596),(0.0665898698871184,0.0731716198748447),.UNSPECIFIED.);
#3048=B_SPLINE_SURFACE_WITH_KNOTS('',3,3,((#97696,#97697,#97698,#97699),
(#97700,#97701,#97702,#97703),(#97704,#97705,#97706,#97707),(#97708,#97709,
#97710,#97711)),.UNSPECIFIED.,.F.,.F.,.F.,(4,4),(4,4),(-0.0012473153211035,
0.2090451116773),(0.0700194292966747,0.0749900982976723),.UNSPECIFIED.);
#3049=B_SPLINE_SURFACE_WITH_KNOTS('',3,3,((#97718,#97719,#97720,#97721),
(#97722,#97723,#97724,#97725),(#97726,#97727,#97728,#97729),(#97730,#97731,
#97732,#97733)),.UNSPECIFIED.,.F.,.F.,.F.,(4,4),(4,4),(-0.00286791014464772,
0.477902879789483),(0.0100271466769355,0.0166015299239867),
 .UNSPECIFIED.);
#3050=B_SPLINE_SURFACE_WITH_KNOTS('',3,3,((#97735,#97736,#97737,#97738),
(#97739,#97740,#97741,#97742),(#97743,#97744,#97745,#97746),(#97747,#97748,
#97749,#97750)),.UNSPECIFIED.,.F.,.F.,.F.,(4,4),(4,4),(0.653230271504001,
1.00206901892309),(0.00656788395379142,0.0131849432429884),
 .UNSPECIFIED.);
#3051=B_SPLINE_SURFACE_WITH_KNOTS('',3,3,((#97758,#97759,#97760,#97761),
(#97762,#97763,#97764,#97765),(#97766,#97767,#97768,#97769),(#97770,#97771,
#97772,#97773)),.UNSPECIFIED.,.F.,.F.,.F.,(4,4),(4,4),(-0.00286780410480499,
0.477902879789146),(0.0200175229646898,0.0265907346180605),
 .UNSPECIFIED.);
#3052=B_SPLINE_SURFACE_WITH_KNOTS('',3,3,((#97775,#97776,#97777,#97778),
(#97779,#97780,#97781,#97782),(#97783,#97784,#97785,#97786),(#97787,#97788,
#97789,#97790)),.UNSPECIFIED.,.F.,.F.,.F.,(4,4),(4,4),(0.522097120208367,
1.0028675316012),(0.016601529923988,0.023173678807522),.UNSPECIFIED.);
#3053=B_SPLINE_SURFACE_WITH_KNOTS('',3,3,((#97792,#97793,#97794,#97795),
(#97796,#97797,#97798,#97799),(#97800,#97801,#97802,#97803),(#97804,#97805,
#97806,#97807)),.UNSPECIFIED.,.F.,.F.,.F.,(4,4),(4,4),(0.,1.0060000396137),
(0.016601529923988,0.0265907346180622),.UNSPECIFIED.);
#3054=B_SPLINE_SURFACE_WITH_KNOTS('',3,3,((#97808,#97809,#97810,#97811),
(#97812,#97813,#97814,#97815),(#97816,#97817,#97818,#97819),(#97820,#97821,
#97822,#97823)),.UNSPECIFIED.,.F.,.F.,.F.,(4,4),(4,4),(-0.00286862201158081,
0.47790287979081),(0.0300094532292784,0.0365944846647014),.UNSPECIFIED.);
#3055=B_SPLINE_SURFACE_WITH_KNOTS('',3,3,((#97825,#97826,#97827,#97828),
(#97829,#97830,#97831,#97832),(#97833,#97834,#97835,#97836),(#97837,#97838,
#97839,#97840)),.UNSPECIFIED.,.F.,.F.,.F.,(4,4),(4,4),(0.522097120207176,
1.00286823669295),(0.026590734618063,0.033170203688992),.UNSPECIFIED.);
#3056=B_SPLINE_SURFACE_WITH_KNOTS('',3,3,((#97848,#97849,#97850,#97851),
(#97852,#97853,#97854,#97855),(#97856,#97857,#97858,#97859),(#97860,#97861,
#97862,#97863)),.UNSPECIFIED.,.F.,.F.,.F.,(4,4),(4,4),(-0.00286848453347558,
0.477902879789301),(0.0400218729466597,0.0466073985929426),
 .UNSPECIFIED.);
#3057=B_SPLINE_SURFACE_WITH_KNOTS('',3,3,((#97880,#97881,#97882,#97883),
(#97884,#97885,#97886,#97887),(#97888,#97889,#97890,#97891),(#97892,#97893,
#97894,#97895)),.UNSPECIFIED.,.F.,.F.,.F.,(4,4),(4,4),(0.,1.00600014639744),
(0.0365944846645046,0.0466073985929167),.UNSPECIFIED.);
#3058=B_SPLINE_SURFACE_WITH_KNOTS('',3,3,((#97896,#97897,#97898,#97899),
(#97900,#97901,#97902,#97903),(#97904,#97905,#97906,#97907),(#97908,#97909,
#97910,#97911)),.UNSPECIFIED.,.F.,.F.,.F.,(4,4),(4,4),(-0.00286780122479574,
0.477902879788766),(0.0500263550859,0.0565997133101406),.UNSPECIFIED.);
#3059=B_SPLINE_SURFACE_WITH_KNOTS('',3,3,((#97913,#97914,#97915,#97916),
(#97917,#97918,#97919,#97920),(#97921,#97922,#97923,#97924),(#97925,#97926,
#97927,#97928)),.UNSPECIFIED.,.F.,.F.,.F.,(4,4),(4,4),(0.522097120204506,
1.00286810177246),(0.0466073985929448,0.0531834925888934),.UNSPECIFIED.);
#3060=B_SPLINE_SURFACE_WITH_KNOTS('',3,3,((#97936,#97937,#97938,#97939),
(#97940,#97941,#97942,#97943),(#97944,#97945,#97946,#97947),(#97948,#97949,
#97950,#97951)),.UNSPECIFIED.,.F.,.F.,.F.,(4,4),(4,4),(-0.00286792598892555,
0.477902879788712),(0.0600156865494599,0.0665898698871178),
 .UNSPECIFIED.);
#3061=B_SPLINE_SURFACE_WITH_KNOTS('',3,3,((#97953,#97954,#97955,#97956),
(#97957,#97958,#97959,#97960),(#97961,#97962,#97963,#97964),(#97965,#97966,
#97967,#97968)),.UNSPECIFIED.,.F.,.F.,.F.,(4,4),(4,4),(0.522097120203374,
1.00286764392044),(0.0565997133101419,0.0631721430887051),.UNSPECIFIED.);
#3062=B_SPLINE_SURFACE_WITH_KNOTS('',3,3,((#97984,#97985,#97986,#97987),
(#97988,#97989,#97990,#97991),(#97992,#97993,#97994,#97995),(#97996,#97997,
#97998,#97999)),.UNSPECIFIED.,.F.,.F.,.F.,(4,4),(4,4),(0.522097120201856,
1.00286833998603),(0.0665898698871177,0.0731716198748464),.UNSPECIFIED.);
#3063=B_SPLINE_SURFACE_WITH_KNOTS('',3,3,((#98000,#98001,#98002,#98003),
(#98004,#98005,#98006,#98007),(#98008,#98009,#98010,#98011),(#98012,#98013,
#98014,#98015)),.UNSPECIFIED.,.F.,.F.,.F.,(4,4),(4,4),(-0.00124731532103314,
0.209045111675863),(0.0700194292966633,0.074990098297664),.UNSPECIFIED.);
#3064=B_SPLINE_SURFACE_WITH_KNOTS('',3,3,((#98022,#98023,#98024,#98025),
(#98026,#98027,#98028,#98029),(#98030,#98031,#98032,#98033),(#98034,#98035,
#98036,#98037)),.UNSPECIFIED.,.F.,.F.,.F.,(4,4),(4,4),(-0.00286791014461308,
0.477902879789457),(0.0100271466769381,0.0166015299239867),
 .UNSPECIFIED.);
#3065=B_SPLINE_SURFACE_WITH_KNOTS('',3,3,((#98039,#98040,#98041,#98042),
(#98043,#98044,#98045,#98046),(#98047,#98048,#98049,#98050),(#98051,#98052,
#98053,#98054)),.UNSPECIFIED.,.F.,.F.,.F.,(4,4),(4,4),(0.653230271507036,
1.00206901892555),(0.00656788395397564,0.0131849432121935),
 .UNSPECIFIED.);
#3066=B_SPLINE_SURFACE_WITH_KNOTS('',3,3,((#98062,#98063,#98064,#98065),
(#98066,#98067,#98068,#98069),(#98070,#98071,#98072,#98073),(#98074,#98075,
#98076,#98077)),.UNSPECIFIED.,.F.,.F.,.F.,(4,4),(4,4),(-0.00286780410475934,
0.477902879789225),(0.02001752296469,0.026590734618062),.UNSPECIFIED.);
#3067=B_SPLINE_SURFACE_WITH_KNOTS('',3,3,((#98079,#98080,#98081,#98082),
(#98083,#98084,#98085,#98086),(#98087,#98088,#98089,#98090),(#98091,#98092,
#98093,#98094)),.UNSPECIFIED.,.F.,.F.,.F.,(4,4),(4,4),(0.522097120210828,
1.00286753160118),(0.0166015299239881,0.0231736788075221),.UNSPECIFIED.);
#3068=B_SPLINE_SURFACE_WITH_KNOTS('',3,3,((#98096,#98097,#98098,#98099),
(#98100,#98101,#98102,#98103),(#98104,#98105,#98106,#98107),(#98108,#98109,
#98110,#98111)),.UNSPECIFIED.,.F.,.F.,.F.,(4,4),(4,4),(0.,1.00600003961384),
(0.016601529923988,0.0265907346180622),.UNSPECIFIED.);
#3069=B_SPLINE_SURFACE_WITH_KNOTS('',3,3,((#98112,#98113,#98114,#98115),
(#98116,#98117,#98118,#98119),(#98120,#98121,#98122,#98123),(#98124,#98125,
#98126,#98127)),.UNSPECIFIED.,.F.,.F.,.F.,(4,4),(4,4),(-0.00286862201159159,
0.477902879791095),(0.0300094532292787,0.0365944846647163),
 .UNSPECIFIED.);
#3070=B_SPLINE_SURFACE_WITH_KNOTS('',3,3,((#98129,#98130,#98131,#98132),
(#98133,#98134,#98135,#98136),(#98137,#98138,#98139,#98140),(#98141,#98142,
#98143,#98144)),.UNSPECIFIED.,.F.,.F.,.F.,(4,4),(4,4),(0.522097120209687,
1.00286823669294),(0.0265907346180634,0.0331702036889921),.UNSPECIFIED.);
#3071=B_SPLINE_SURFACE_WITH_KNOTS('',3,3,((#98152,#98153,#98154,#98155),
(#98156,#98157,#98158,#98159),(#98160,#98161,#98162,#98163),(#98164,#98165,
#98166,#98167)),.UNSPECIFIED.,.F.,.F.,.F.,(4,4),(4,4),(-0.0028684845334302,
0.477902879789558),(0.0400218729466606,0.0466073985929422),
 .UNSPECIFIED.);
#3072=B_SPLINE_SURFACE_WITH_KNOTS('',3,3,((#98184,#98185,#98186,#98187),
(#98188,#98189,#98190,#98191),(#98192,#98193,#98194,#98195),(#98196,#98197,
#98198,#98199)),.UNSPECIFIED.,.F.,.F.,.F.,(4,4),(4,4),(0.,1.00600014639751),
(0.0365944846645049,0.0466073985929156),.UNSPECIFIED.);
#3073=B_SPLINE_SURFACE_WITH_KNOTS('',3,3,((#98200,#98201,#98202,#98203),
(#98204,#98205,#98206,#98207),(#98208,#98209,#98210,#98211),(#98212,#98213,
#98214,#98215)),.UNSPECIFIED.,.F.,.F.,.F.,(4,4),(4,4),(-0.00286780122473538,
0.477902879789028),(0.0500263550859005,0.0565997133101408),
 .UNSPECIFIED.);
#3074=B_SPLINE_SURFACE_WITH_KNOTS('',3,3,((#98217,#98218,#98219,#98220),
(#98221,#98222,#98223,#98224),(#98225,#98226,#98227,#98228),(#98229,#98230,
#98231,#98232)),.UNSPECIFIED.,.F.,.F.,.F.,(4,4),(4,4),(0.522097120207056,
1.00286810177249),(0.0466073985929443,0.0531834925888928),.UNSPECIFIED.);
#3075=B_SPLINE_SURFACE_WITH_KNOTS('',3,3,((#98240,#98241,#98242,#98243),
(#98244,#98245,#98246,#98247),(#98248,#98249,#98250,#98251),(#98252,#98253,
#98254,#98255)),.UNSPECIFIED.,.F.,.F.,.F.,(4,4),(4,4),(-0.00286792598897873,
0.47790287978871),(0.0600156865494609,0.0665898698871172),.UNSPECIFIED.);
#3076=B_SPLINE_SURFACE_WITH_KNOTS('',3,3,((#98257,#98258,#98259,#98260),
(#98261,#98262,#98263,#98264),(#98265,#98266,#98267,#98268),(#98269,#98270,
#98271,#98272)),.UNSPECIFIED.,.F.,.F.,.F.,(4,4),(4,4),(0.522097120205968,
1.00286764392047),(0.0565997133101421,0.0631721430887068),.UNSPECIFIED.);
#3077=B_SPLINE_SURFACE_WITH_KNOTS('',3,3,((#98288,#98289,#98290,#98291),
(#98292,#98293,#98294,#98295),(#98296,#98297,#98298,#98299),(#98300,#98301,
#98302,#98303)),.UNSPECIFIED.,.F.,.F.,.F.,(4,4),(4,4),(0.522097120204424,
1.00286833998594),(0.0665898698871185,0.073171619874845),.UNSPECIFIED.);
#3078=B_SPLINE_SURFACE_WITH_KNOTS('',3,3,((#98304,#98305,#98306,#98307),
(#98308,#98309,#98310,#98311),(#98312,#98313,#98314,#98315),(#98316,#98317,
#98318,#98319)),.UNSPECIFIED.,.F.,.F.,.F.,(4,4),(4,4),(-0.00124731532105512,
0.209045111674549),(0.0700194292966487,0.074990098297657),.UNSPECIFIED.);
#3079=B_SPLINE_SURFACE_WITH_KNOTS('',3,3,((#98326,#98327,#98328,#98329),
(#98330,#98331,#98332,#98333),(#98334,#98335,#98336,#98337),(#98338,#98339,
#98340,#98341)),.UNSPECIFIED.,.F.,.F.,.F.,(4,4),(4,4),(-0.00286791014458099,
0.477902879789525),(0.0100271466769368,0.0166015299239868),
 .UNSPECIFIED.);
#3080=B_SPLINE_SURFACE_WITH_KNOTS('',3,3,((#98343,#98344,#98345,#98346),
(#98347,#98348,#98349,#98350),(#98351,#98352,#98353,#98354),(#98355,#98356,
#98357,#98358)),.UNSPECIFIED.,.F.,.F.,.F.,(4,4),(4,4),(0.653230271506329,
1.00206901892807),(0.00656788395397555,0.0131849432122001),
 .UNSPECIFIED.);
#3081=B_SPLINE_SURFACE_WITH_KNOTS('',3,3,((#98366,#98367,#98368,#98369),
(#98370,#98371,#98372,#98373),(#98374,#98375,#98376,#98377),(#98378,#98379,
#98380,#98381)),.UNSPECIFIED.,.F.,.F.,.F.,(4,4),(4,4),(-0.00286780410469745,
0.477902879789348),(0.0200175229646915,0.026590734618063),.UNSPECIFIED.);
#3082=B_SPLINE_SURFACE_WITH_KNOTS('',3,3,((#98383,#98384,#98385,#98386),
(#98387,#98388,#98389,#98390),(#98391,#98392,#98393,#98394),(#98395,#98396,
#98397,#98398)),.UNSPECIFIED.,.F.,.F.,.F.,(4,4),(4,4),(0.522097120210687,
1.00286753160123),(0.016601529923989,0.023173678793031),.UNSPECIFIED.);
#3083=B_SPLINE_SURFACE_WITH_KNOTS('',3,3,((#98400,#98401,#98402,#98403),
(#98404,#98405,#98406,#98407),(#98408,#98409,#98410,#98411),(#98412,#98413,
#98414,#98415)),.UNSPECIFIED.,.F.,.F.,.F.,(4,4),(4,4),(0.,1.00600003961384),
(0.0166015299239892,0.0265907346180636),.UNSPECIFIED.);
#3084=B_SPLINE_SURFACE_WITH_KNOTS('',3,3,((#98416,#98417,#98418,#98419),
(#98420,#98421,#98422,#98423),(#98424,#98425,#98426,#98427),(#98428,#98429,
#98430,#98431)),.UNSPECIFIED.,.F.,.F.,.F.,(4,4),(4,4),(-0.00286862201150934,
0.477902879791048),(0.0300094532292786,0.0365944846647024),
 .UNSPECIFIED.);
#3085=B_SPLINE_SURFACE_WITH_KNOTS('',3,3,((#98433,#98434,#98435,#98436),
(#98437,#98438,#98439,#98440),(#98441,#98442,#98443,#98444),(#98445,#98446,
#98447,#98448)),.UNSPECIFIED.,.F.,.F.,.F.,(4,4),(4,4),(0.522097120210921,
1.00286823669297),(0.0265907346180638,0.0331702036889932),.UNSPECIFIED.);
#3086=B_SPLINE_SURFACE_WITH_KNOTS('',3,3,((#98456,#98457,#98458,#98459),
(#98460,#98461,#98462,#98463),(#98464,#98465,#98466,#98467),(#98468,#98469,
#98470,#98471)),.UNSPECIFIED.,.F.,.F.,.F.,(4,4),(4,4),(-0.00286848453340593,
0.47790287978974),(0.0400218729466611,0.0466073985929437),.UNSPECIFIED.);
#3087=B_SPLINE_SURFACE_WITH_KNOTS('',3,3,((#98488,#98489,#98490,#98491),
(#98492,#98493,#98494,#98495),(#98496,#98497,#98498,#98499),(#98500,#98501,
#98502,#98503)),.UNSPECIFIED.,.F.,.F.,.F.,(4,4),(4,4),(0.,1.00600014639748),
(0.0365944846645065,0.0466073985929166),.UNSPECIFIED.);
#3088=B_SPLINE_SURFACE_WITH_KNOTS('',3,3,((#98504,#98505,#98506,#98507),
(#98508,#98509,#98510,#98511),(#98512,#98513,#98514,#98515),(#98516,#98517,
#98518,#98519)),.UNSPECIFIED.,.F.,.F.,.F.,(4,4),(4,4),(-0.00286780122467488,
0.477902879789109),(0.0500263550859008,0.0565997133101401),
 .UNSPECIFIED.);
#3089=B_SPLINE_SURFACE_WITH_KNOTS('',3,3,((#98521,#98522,#98523,#98524),
(#98525,#98526,#98527,#98528),(#98529,#98530,#98531,#98532),(#98533,#98534,
#98535,#98536)),.UNSPECIFIED.,.F.,.F.,.F.,(4,4),(4,4),(0.522097120209639,
1.0028681017725),(0.0466073985929444,0.0531834925888927),.UNSPECIFIED.);
#3090=B_SPLINE_SURFACE_WITH_KNOTS('',3,3,((#98544,#98545,#98546,#98547),
(#98548,#98549,#98550,#98551),(#98552,#98553,#98554,#98555),(#98556,#98557,
#98558,#98559)),.UNSPECIFIED.,.F.,.F.,.F.,(4,4),(4,4),(-0.00286792598901557,
0.477902879789036),(0.0600156865494605,0.0665898698871177),
 .UNSPECIFIED.);
#3091=B_SPLINE_SURFACE_WITH_KNOTS('',3,3,((#98561,#98562,#98563,#98564),
(#98565,#98566,#98567,#98568),(#98569,#98570,#98571,#98572),(#98573,#98574,
#98575,#98576)),.UNSPECIFIED.,.F.,.F.,.F.,(4,4),(4,4),(0.522097120208366,
1.00286764392047),(0.056599713310141,0.0631721430887066),.UNSPECIFIED.);
#3092=B_SPLINE_SURFACE_WITH_KNOTS('',3,3,((#98592,#98593,#98594,#98595),
(#98596,#98597,#98598,#98599),(#98600,#98601,#98602,#98603),(#98604,#98605,
#98606,#98607)),.UNSPECIFIED.,.F.,.F.,.F.,(4,4),(4,4),(0.522097120206995,
1.00286833998595),(0.0665898698871194,0.0731716198748452),.UNSPECIFIED.);
#3093=B_SPLINE_SURFACE_WITH_KNOTS('',3,3,((#98608,#98609,#98610,#98611),
(#98612,#98613,#98614,#98615),(#98616,#98617,#98618,#98619),(#98620,#98621,
#98622,#98623)),.UNSPECIFIED.,.F.,.F.,.F.,(4,4),(4,4),(-0.00124731532103649,
0.209045111673288),(0.070019429296636,0.074990098297651),.UNSPECIFIED.);
#3094=B_SPLINE_SURFACE_WITH_KNOTS('',3,3,((#98630,#98631,#98632,#98633),
(#98634,#98635,#98636,#98637),(#98638,#98639,#98640,#98641),(#98642,#98643,
#98644,#98645)),.UNSPECIFIED.,.F.,.F.,.F.,(4,4),(4,4),(-0.00286791014454375,
0.477902879789698),(0.0100271466769373,0.0166015299239864),
 .UNSPECIFIED.);
#3095=B_SPLINE_SURFACE_WITH_KNOTS('',3,3,((#98647,#98648,#98649,#98650),
(#98651,#98652,#98653,#98654),(#98655,#98656,#98657,#98658),(#98659,#98660,
#98661,#98662)),.UNSPECIFIED.,.F.,.F.,.F.,(4,4),(4,4),(0.653230271507101,
1.00206901893051),(0.00656788395379447,0.0131849432429115),
 .UNSPECIFIED.);
#3096=B_SPLINE_SURFACE_WITH_KNOTS('',3,3,((#98670,#98671,#98672,#98673),
(#98674,#98675,#98676,#98677),(#98678,#98679,#98680,#98681),(#98682,#98683,
#98684,#98685)),.UNSPECIFIED.,.F.,.F.,.F.,(4,4),(4,4),(-0.00286780410484465,
0.47790287978942),(0.0200175229646894,0.0265907346180617),.UNSPECIFIED.);
#3097=B_SPLINE_SURFACE_WITH_KNOTS('',3,3,((#98687,#98688,#98689,#98690),
(#98691,#98692,#98693,#98694),(#98695,#98696,#98697,#98698),(#98699,#98700,
#98701,#98702)),.UNSPECIFIED.,.F.,.F.,.F.,(4,4),(4,4),(0.522097120210559,
1.00286753160123),(0.0166015299239872,0.0231736788037107),.UNSPECIFIED.);
#3098=B_SPLINE_SURFACE_WITH_KNOTS('',3,3,((#98704,#98705,#98706,#98707),
(#98708,#98709,#98710,#98711),(#98712,#98713,#98714,#98715),(#98716,#98717,
#98718,#98719)),.UNSPECIFIED.,.F.,.F.,.F.,(4,4),(4,4),(0.,1.00600003961392),
(0.016601529923987,0.0265907346180635),.UNSPECIFIED.);
#3099=B_SPLINE_SURFACE_WITH_KNOTS('',3,3,((#98720,#98721,#98722,#98723),
(#98724,#98725,#98726,#98727),(#98728,#98729,#98730,#98731),(#98732,#98733,
#98734,#98735)),.UNSPECIFIED.,.F.,.F.,.F.,(4,4),(4,4),(-0.00286862201165759,
0.477902879791254),(0.0300094532292787,0.0365944846647016),
 .UNSPECIFIED.);
#3100=B_SPLINE_SURFACE_WITH_KNOTS('',3,3,((#98737,#98738,#98739,#98740),
(#98741,#98742,#98743,#98744),(#98745,#98746,#98747,#98748),(#98749,#98750,
#98751,#98752)),.UNSPECIFIED.,.F.,.F.,.F.,(4,4),(4,4),(0.522097120210765,
1.00286823669301),(0.0265907346180635,0.0331702036622759),.UNSPECIFIED.);
#3101=B_SPLINE_SURFACE_WITH_KNOTS('',3,3,((#98760,#98761,#98762,#98763),
(#98764,#98765,#98766,#98767),(#98768,#98769,#98770,#98771),(#98772,#98773,
#98774,#98775)),.UNSPECIFIED.,.F.,.F.,.F.,(4,4),(4,4),(-0.00286848453341356,
0.477902879789721),(0.0400218729466614,0.0466073985929431),
 .UNSPECIFIED.);
#3102=B_SPLINE_SURFACE_WITH_KNOTS('',3,3,((#98792,#98793,#98794,#98795),
(#98796,#98797,#98798,#98799),(#98800,#98801,#98802,#98803),(#98804,#98805,
#98806,#98807)),.UNSPECIFIED.,.F.,.F.,.F.,(4,4),(4,4),(0.,1.00600014639744),
(0.0365944846645058,0.0466073985929154),.UNSPECIFIED.);
#3103=B_SPLINE_SURFACE_WITH_KNOTS('',3,3,((#98808,#98809,#98810,#98811),
(#98812,#98813,#98814,#98815),(#98816,#98817,#98818,#98819),(#98820,#98821,
#98822,#98823)),.UNSPECIFIED.,.F.,.F.,.F.,(4,4),(4,4),(-0.00286780122470342,
0.477902879789203),(0.0500263550858997,0.0565997133101398),
 .UNSPECIFIED.);
#3104=B_SPLINE_SURFACE_WITH_KNOTS('',3,3,((#98825,#98826,#98827,#98828),
(#98829,#98830,#98831,#98832),(#98833,#98834,#98835,#98836),(#98837,#98838,
#98839,#98840)),.UNSPECIFIED.,.F.,.F.,.F.,(4,4),(4,4),(0.522097120210796,
1.00286810177246),(0.0466073985929437,0.0531834922865657),.UNSPECIFIED.);
#3105=B_SPLINE_SURFACE_WITH_KNOTS('',3,3,((#98848,#98849,#98850,#98851),
(#98852,#98853,#98854,#98855),(#98856,#98857,#98858,#98859),(#98860,#98861,
#98862,#98863)),.UNSPECIFIED.,.F.,.F.,.F.,(4,4),(4,4),(-0.00286792598889512,
0.477902879788943),(0.060015686549461,0.0665898698871167),.UNSPECIFIED.);
#3106=B_SPLINE_SURFACE_WITH_KNOTS('',3,3,((#98865,#98866,#98867,#98868),
(#98869,#98870,#98871,#98872),(#98873,#98874,#98875,#98876),(#98877,#98878,
#98879,#98880)),.UNSPECIFIED.,.F.,.F.,.F.,(4,4),(4,4),(0.522097120210891,
1.0028676439204),(0.0565997133101416,0.0631721430887053),.UNSPECIFIED.);
#3107=B_SPLINE_SURFACE_WITH_KNOTS('',3,3,((#98896,#98897,#98898,#98899),
(#98900,#98901,#98902,#98903),(#98904,#98905,#98906,#98907),(#98908,#98909,
#98910,#98911)),.UNSPECIFIED.,.F.,.F.,.F.,(4,4),(4,4),(0.522097120209503,
1.00286833998596),(0.0665898698871188,0.073171619874845),.UNSPECIFIED.);
#3108=B_SPLINE_SURFACE_WITH_KNOTS('',3,3,((#98912,#98913,#98914,#98915),
(#98916,#98917,#98918,#98919),(#98920,#98921,#98922,#98923),(#98924,#98925,
#98926,#98927)),.UNSPECIFIED.,.F.,.F.,.F.,(4,4),(4,4),(-0.00124731532102576,
0.209045111672193),(0.0700194292966195,0.0749900982976457),
 .UNSPECIFIED.);
#3109=B_SPLINE_SURFACE_WITH_KNOTS('',3,3,((#98934,#98935,#98936,#98937),
(#98938,#98939,#98940,#98941),(#98942,#98943,#98944,#98945),(#98946,#98947,
#98948,#98949)),.UNSPECIFIED.,.F.,.F.,.F.,(4,4),(4,4),(-0.00286791014449015,
0.47790287978987),(0.0100271466769346,0.0166015299239873),.UNSPECIFIED.);
#3110=B_SPLINE_SURFACE_WITH_KNOTS('',3,3,((#98951,#98952,#98953,#98954),
(#98955,#98956,#98957,#98958),(#98959,#98960,#98961,#98962),(#98963,#98964,
#98965,#98966)),.UNSPECIFIED.,.F.,.F.,.F.,(4,4),(4,4),(0.653230271506975,
1.00206901893248),(0.00656788395379699,0.0131849432430145),
 .UNSPECIFIED.);
#3111=B_SPLINE_SURFACE_WITH_KNOTS('',3,3,((#98974,#98975,#98976,#98977),
(#98978,#98979,#98980,#98981),(#98982,#98983,#98984,#98985),(#98986,#98987,
#98988,#98989)),.UNSPECIFIED.,.F.,.F.,.F.,(4,4),(4,4),(-0.00286780410469933,
0.477902879789596),(0.0200175229646896,0.026590734618062),.UNSPECIFIED.);
#3112=B_SPLINE_SURFACE_WITH_KNOTS('',3,3,((#98991,#98992,#98993,#98994),
(#98995,#98996,#98997,#98998),(#98999,#99000,#99001,#99002),(#99003,#99004,
#99005,#99006)),.UNSPECIFIED.,.F.,.F.,.F.,(4,4),(4,4),(0.522097120210308,
1.00286753160123),(0.0166015299239883,0.0231736788037113),.UNSPECIFIED.);
#3113=B_SPLINE_SURFACE_WITH_KNOTS('',3,3,((#99008,#99009,#99010,#99011),
(#99012,#99013,#99014,#99015),(#99016,#99017,#99018,#99019),(#99020,#99021,
#99022,#99023)),.UNSPECIFIED.,.F.,.F.,.F.,(4,4),(4,4),(0.,1.0060000396139),
(0.0166015299239893,0.0265907346180633),.UNSPECIFIED.);
#3114=B_SPLINE_SURFACE_WITH_KNOTS('',3,3,((#99024,#99025,#99026,#99027),
(#99028,#99029,#99030,#99031),(#99032,#99033,#99034,#99035),(#99036,#99037,
#99038,#99039)),.UNSPECIFIED.,.F.,.F.,.F.,(4,4),(4,4),(-0.00286862201163364,
0.477902879791346),(0.030009453229279,0.0365944846647037),.UNSPECIFIED.);
#3115=B_SPLINE_SURFACE_WITH_KNOTS('',3,3,((#99041,#99042,#99043,#99044),
(#99045,#99046,#99047,#99048),(#99049,#99050,#99051,#99052),(#99053,#99054,
#99055,#99056)),.UNSPECIFIED.,.F.,.F.,.F.,(4,4),(4,4),(0.522097120210626,
1.00286823669299),(0.0265907346180645,0.0331702036622782),.UNSPECIFIED.);
#3116=B_SPLINE_SURFACE_WITH_KNOTS('',3,3,((#99064,#99065,#99066,#99067),
(#99068,#99069,#99070,#99071),(#99072,#99073,#99074,#99075),(#99076,#99077,
#99078,#99079)),.UNSPECIFIED.,.F.,.F.,.F.,(4,4),(4,4),(-0.00286848453330232,
0.47790287978981),(0.0400218729466605,0.0466073985929431),.UNSPECIFIED.);
#3117=B_SPLINE_SURFACE_WITH_KNOTS('',3,3,((#99096,#99097,#99098,#99099),
(#99100,#99101,#99102,#99103),(#99104,#99105,#99106,#99107),(#99108,#99109,
#99110,#99111)),.UNSPECIFIED.,.F.,.F.,.F.,(4,4),(4,4),(0.,1.0060001463974),
(0.036594484664507,0.0466073985929166),.UNSPECIFIED.);
#3118=B_SPLINE_SURFACE_WITH_KNOTS('',3,3,((#99112,#99113,#99114,#99115),
(#99116,#99117,#99118,#99119),(#99120,#99121,#99122,#99123),(#99124,#99125,
#99126,#99127)),.UNSPECIFIED.,.F.,.F.,.F.,(4,4),(4,4),(-0.00286780122463184,
0.477902879789366),(0.0500263550859003,0.0565997133101415),
 .UNSPECIFIED.);
#3119=B_SPLINE_SURFACE_WITH_KNOTS('',3,3,((#99129,#99130,#99131,#99132),
(#99133,#99134,#99135,#99136),(#99137,#99138,#99139,#99140),(#99141,#99142,
#99143,#99144)),.UNSPECIFIED.,.F.,.F.,.F.,(4,4),(4,4),(0.522097120210698,
1.0028681017726),(0.0466073985929441,0.0531834925888937),.UNSPECIFIED.);
#3120=B_SPLINE_SURFACE_WITH_KNOTS('',3,3,((#99152,#99153,#99154,#99155),
(#99156,#99157,#99158,#99159),(#99160,#99161,#99162,#99163),(#99164,#99165,
#99166,#99167)),.UNSPECIFIED.,.F.,.F.,.F.,(4,4),(4,4),(-0.00286792598895932,
0.477902879789034),(0.0600156865494597,0.0665898698871171),
 .UNSPECIFIED.);
#3121=B_SPLINE_SURFACE_WITH_KNOTS('',3,3,((#99169,#99170,#99171,#99172),
(#99173,#99174,#99175,#99176),(#99177,#99178,#99179,#99180),(#99181,#99182,
#99183,#99184)),.UNSPECIFIED.,.F.,.F.,.F.,(4,4),(4,4),(0.522097120210928,
1.00286764392042),(0.0565997133101425,0.0631721430887067),.UNSPECIFIED.);
#3122=B_SPLINE_SURFACE_WITH_KNOTS('',3,3,((#99200,#99201,#99202,#99203),
(#99204,#99205,#99206,#99207),(#99208,#99209,#99210,#99211),(#99212,#99213,
#99214,#99215)),.UNSPECIFIED.,.F.,.F.,.F.,(4,4),(4,4),(0.522097120210139,
1.002868339986),(0.0665898698871195,0.0731716198748449),.UNSPECIFIED.);
#3123=B_SPLINE_SURFACE_WITH_KNOTS('',3,3,((#99216,#99217,#99218,#99219),
(#99220,#99221,#99222,#99223),(#99224,#99225,#99226,#99227),(#99228,#99229,
#99230,#99231)),.UNSPECIFIED.,.F.,.F.,.F.,(4,4),(4,4),(-0.0012473153210028,
0.209045111671177),(0.0700194292966059,0.0749900982976427),
 .UNSPECIFIED.);
#3124=B_SPLINE_SURFACE_WITH_KNOTS('',3,3,((#99238,#99239,#99240,#99241),
(#99242,#99243,#99244,#99245),(#99246,#99247,#99248,#99249),(#99250,#99251,
#99252,#99253)),.UNSPECIFIED.,.F.,.F.,.F.,(4,4),(4,4),(-0.00286791014442176,
0.477902879789923),(0.0100271466769339,0.0166015299239868),
 .UNSPECIFIED.);
#3125=B_SPLINE_SURFACE_WITH_KNOTS('',3,3,((#99255,#99256,#99257,#99258),
(#99259,#99260,#99261,#99262),(#99263,#99264,#99265,#99266),(#99267,#99268,
#99269,#99270)),.UNSPECIFIED.,.F.,.F.,.F.,(4,4),(4,4),(0.653230271506902,
1.00206901893463),(0.00656788395380054,0.0131849432430249),
 .UNSPECIFIED.);
#3126=B_SPLINE_SURFACE_WITH_KNOTS('',3,3,((#99278,#99279,#99280,#99281),
(#99282,#99283,#99284,#99285),(#99286,#99287,#99288,#99289),(#99290,#99291,
#99292,#99293)),.UNSPECIFIED.,.F.,.F.,.F.,(4,4),(4,4),(-0.00286780410473915,
0.477902879789725),(0.0200175229646895,0.0265907346180625),
 .UNSPECIFIED.);
#3127=B_SPLINE_SURFACE_WITH_KNOTS('',3,3,((#99295,#99296,#99297,#99298),
(#99299,#99300,#99301,#99302),(#99303,#99304,#99305,#99306),(#99307,#99308,
#99309,#99310)),.UNSPECIFIED.,.F.,.F.,.F.,(4,4),(4,4),(0.522097120210315,
1.00286753160118),(0.0166015299239891,0.0231736788037108),.UNSPECIFIED.);
#3128=B_SPLINE_SURFACE_WITH_KNOTS('',3,3,((#99312,#99313,#99314,#99315),
(#99316,#99317,#99318,#99319),(#99320,#99321,#99322,#99323),(#99324,#99325,
#99326,#99327)),.UNSPECIFIED.,.F.,.F.,.F.,(4,4),(4,4),(0.,1.0060000396137),
(0.0166015299239869,0.0265907346180621),.UNSPECIFIED.);
#3129=B_SPLINE_SURFACE_WITH_KNOTS('',3,3,((#99328,#99329,#99330,#99331),
(#99332,#99333,#99334,#99335),(#99336,#99337,#99338,#99339),(#99340,#99341,
#99342,#99343)),.UNSPECIFIED.,.F.,.F.,.F.,(4,4),(4,4),(-0.00286862201153849,
0.477902879791419),(0.0300094532292795,0.0365944846647028),
 .UNSPECIFIED.);
#3130=B_SPLINE_SURFACE_WITH_KNOTS('',3,3,((#99345,#99346,#99347,#99348),
(#99349,#99350,#99351,#99352),(#99353,#99354,#99355,#99356),(#99357,#99358,
#99359,#99360)),.UNSPECIFIED.,.F.,.F.,.F.,(4,4),(4,4),(0.522097120210556,
1.00286823669293),(0.0265907346180642,0.0331702036889928),.UNSPECIFIED.);
#3131=B_SPLINE_SURFACE_WITH_KNOTS('',3,3,((#99368,#99369,#99370,#99371),
(#99372,#99373,#99374,#99375),(#99376,#99377,#99378,#99379),(#99380,#99381,
#99382,#99383)),.UNSPECIFIED.,.F.,.F.,.F.,(4,4),(4,4),(-0.00286848453325725,
0.477902879790036),(0.0400218729466594,0.0466073985929445),
 .UNSPECIFIED.);
#3132=B_SPLINE_SURFACE_WITH_KNOTS('',3,3,((#99400,#99401,#99402,#99403),
(#99404,#99405,#99406,#99407),(#99408,#99409,#99410,#99411),(#99412,#99413,
#99414,#99415)),.UNSPECIFIED.,.F.,.F.,.F.,(4,4),(4,4),(0.,1.00600014639735),
(0.0365944846645063,0.046607398592916),.UNSPECIFIED.);
#3133=B_SPLINE_SURFACE_WITH_KNOTS('',3,3,((#99416,#99417,#99418,#99419),
(#99420,#99421,#99422,#99423),(#99424,#99425,#99426,#99427),(#99428,#99429,
#99430,#99431)),.UNSPECIFIED.,.F.,.F.,.F.,(4,4),(4,4),(-0.00286780122456139,
0.477902879789289),(0.0500263550859003,0.0565997133101399),
 .UNSPECIFIED.);
#3134=B_SPLINE_SURFACE_WITH_KNOTS('',3,3,((#99433,#99434,#99435,#99436),
(#99437,#99438,#99439,#99440),(#99441,#99442,#99443,#99444),(#99445,#99446,
#99447,#99448)),.UNSPECIFIED.,.F.,.F.,.F.,(4,4),(4,4),(0.522097120210739,
1.00286810177251),(0.046607398592945,0.0531834925888924),.UNSPECIFIED.);
#3135=B_SPLINE_SURFACE_WITH_KNOTS('',3,3,((#99456,#99457,#99458,#99459),
(#99460,#99461,#99462,#99463),(#99464,#99465,#99466,#99467),(#99468,#99469,
#99470,#99471)),.UNSPECIFIED.,.F.,.F.,.F.,(4,4),(4,4),(-0.00286792598899,
0.477902879789314),(0.0600156865494594,0.0665898698871176),
 .UNSPECIFIED.);
#3136=B_SPLINE_SURFACE_WITH_KNOTS('',3,3,((#99473,#99474,#99475,#99476),
(#99477,#99478,#99479,#99480),(#99481,#99482,#99483,#99484),(#99485,#99486,
#99487,#99488)),.UNSPECIFIED.,.F.,.F.,.F.,(4,4),(4,4),(0.522097120210747,
1.00286764392045),(0.0565997133101418,0.0631721430887066),.UNSPECIFIED.);
#3137=B_SPLINE_SURFACE_WITH_KNOTS('',3,3,((#99504,#99505,#99506,#99507),
(#99508,#99509,#99510,#99511),(#99512,#99513,#99514,#99515),(#99516,#99517,
#99518,#99519)),.UNSPECIFIED.,.F.,.F.,.F.,(4,4),(4,4),(0.522097120209877,
1.00286833998603),(0.0665898698871188,0.0731716198748456),.UNSPECIFIED.);
#3138=B_SPLINE_SURFACE_WITH_KNOTS('',3,3,((#99520,#99521,#99522,#99523),
(#99524,#99525,#99526,#99527),(#99528,#99529,#99530,#99531),(#99532,#99533,
#99534,#99535)),.UNSPECIFIED.,.F.,.F.,.F.,(4,4),(4,4),(-0.00124731532106721,
0.209045111670196),(0.0700194292965919,0.0749900982976401),
 .UNSPECIFIED.);
#3139=B_SPLINE_SURFACE_WITH_KNOTS('',3,3,((#99542,#99543,#99544,#99545),
(#99546,#99547,#99548,#99549),(#99550,#99551,#99552,#99553),(#99554,#99555,
#99556,#99557)),.UNSPECIFIED.,.F.,.F.,.F.,(4,4),(4,4),(-0.00286791014437286,
0.477902879790058),(0.010027146676935,0.0166015299239852),.UNSPECIFIED.);
#3140=B_SPLINE_SURFACE_WITH_KNOTS('',3,3,((#99559,#99560,#99561,#99562),
(#99563,#99564,#99565,#99566),(#99567,#99568,#99569,#99570),(#99571,#99572,
#99573,#99574)),.UNSPECIFIED.,.F.,.F.,.F.,(4,4),(4,4),(0.653230271507036,
1.00206901892628),(0.00656788395380599,0.0131849432430315),
 .UNSPECIFIED.);
#3141=B_SPLINE_SURFACE_WITH_KNOTS('',3,3,((#99582,#99583,#99584,#99585),
(#99586,#99587,#99588,#99589),(#99590,#99591,#99592,#99593),(#99594,#99595,
#99596,#99597)),.UNSPECIFIED.,.F.,.F.,.F.,(4,4),(4,4),(-0.00286780410475729,
0.477902879789832),(0.02001752296469,0.026590734618062),.UNSPECIFIED.);
#3142=B_SPLINE_SURFACE_WITH_KNOTS('',3,3,((#99599,#99600,#99601,#99602),
(#99603,#99604,#99605,#99606),(#99607,#99608,#99609,#99610),(#99611,#99612,
#99613,#99614)),.UNSPECIFIED.,.F.,.F.,.F.,(4,4),(4,4),(0.52209712021033,
1.00286753160121),(0.0166015299239888,0.0231736788037107),.UNSPECIFIED.);
#3143=B_SPLINE_SURFACE_WITH_KNOTS('',3,3,((#99616,#99617,#99618,#99619),
(#99620,#99621,#99622,#99623),(#99624,#99625,#99626,#99627),(#99628,#99629,
#99630,#99631)),.UNSPECIFIED.,.F.,.F.,.F.,(4,4),(4,4),(0.,1.00600003961385),
(0.0166015299239882,0.0265907346180635),.UNSPECIFIED.);
#3144=B_SPLINE_SURFACE_WITH_KNOTS('',3,3,((#99632,#99633,#99634,#99635),
(#99636,#99637,#99638,#99639),(#99640,#99641,#99642,#99643),(#99644,#99645,
#99646,#99647)),.UNSPECIFIED.,.F.,.F.,.F.,(4,4),(4,4),(-0.00286862201164465,
0.477902879791502),(0.0300094532292795,0.0365944846647017),
 .UNSPECIFIED.);
#3145=B_SPLINE_SURFACE_WITH_KNOTS('',3,3,((#99649,#99650,#99651,#99652),
(#99653,#99654,#99655,#99656),(#99657,#99658,#99659,#99660),(#99661,#99662,
#99663,#99664)),.UNSPECIFIED.,.F.,.F.,.F.,(4,4),(4,4),(0.52209712021055,
1.00286823669298),(0.0265907346180646,0.0331702036051747),.UNSPECIFIED.);
#3146=B_SPLINE_SURFACE_WITH_KNOTS('',3,3,((#99672,#99673,#99674,#99675),
(#99676,#99677,#99678,#99679),(#99680,#99681,#99682,#99683),(#99684,#99685,
#99686,#99687)),.UNSPECIFIED.,.F.,.F.,.F.,(4,4),(4,4),(-0.00286848453320442,
0.477902879790044),(0.0400218729466604,0.0466073985929431),
 .UNSPECIFIED.);
#3147=B_SPLINE_SURFACE_WITH_KNOTS('',3,3,((#99704,#99705,#99706,#99707),
(#99708,#99709,#99710,#99711),(#99712,#99713,#99714,#99715),(#99716,#99717,
#99718,#99719)),.UNSPECIFIED.,.F.,.F.,.F.,(4,4),(4,4),(0.,1.00600014639742),
(0.0365944846645066,0.0466073985929164),.UNSPECIFIED.);
#3148=B_SPLINE_SURFACE_WITH_KNOTS('',3,3,((#99720,#99721,#99722,#99723),
(#99724,#99725,#99726,#99727),(#99728,#99729,#99730,#99731),(#99732,#99733,
#99734,#99735)),.UNSPECIFIED.,.F.,.F.,.F.,(4,4),(4,4),(-0.00286780122448064,
0.47790287978947),(0.0500263550859002,0.0565997133101405),.UNSPECIFIED.);
#3149=B_SPLINE_SURFACE_WITH_KNOTS('',3,3,((#99737,#99738,#99739,#99740),
(#99741,#99742,#99743,#99744),(#99745,#99746,#99747,#99748),(#99749,#99750,
#99751,#99752)),.UNSPECIFIED.,.F.,.F.,.F.,(4,4),(4,4),(0.522097120210521,
1.00286810177273),(0.0466073985929442,0.0531834933545511),.UNSPECIFIED.);
#3150=B_SPLINE_SURFACE_WITH_KNOTS('',3,3,((#99760,#99761,#99762,#99763),
(#99764,#99765,#99766,#99767),(#99768,#99769,#99770,#99771),(#99772,#99773,
#99774,#99775)),.UNSPECIFIED.,.F.,.F.,.F.,(4,4),(4,4),(-0.00286792598884402,
0.47790287978941),(0.0600156865494606,0.0665898698871172),.UNSPECIFIED.);
#3151=B_SPLINE_SURFACE_WITH_KNOTS('',3,3,((#99777,#99778,#99779,#99780),
(#99781,#99782,#99783,#99784),(#99785,#99786,#99787,#99788),(#99789,#99790,
#99791,#99792)),.UNSPECIFIED.,.F.,.F.,.F.,(4,4),(4,4),(0.522097120210711,
1.00286764392047),(0.0565997133101428,0.0631721430887067),.UNSPECIFIED.);
#3152=B_SPLINE_SURFACE_WITH_KNOTS('',3,3,((#99808,#99809,#99810,#99811),
(#99812,#99813,#99814,#99815),(#99816,#99817,#99818,#99819),(#99820,#99821,
#99822,#99823)),.UNSPECIFIED.,.F.,.F.,.F.,(4,4),(4,4),(0.522097120209842,
1.00286833998597),(0.0665898698871195,0.0731716198748457),.UNSPECIFIED.);
#3153=B_SPLINE_SURFACE_WITH_KNOTS('',3,3,((#99824,#99825,#99826,#99827),
(#99828,#99829,#99830,#99831),(#99832,#99833,#99834,#99835),(#99836,#99837,
#99838,#99839)),.UNSPECIFIED.,.F.,.F.,.F.,(4,4),(4,4),(-0.0012473153210368,
0.209045111669589),(0.0700194292965764,0.0749900982976409),
 .UNSPECIFIED.);
#3154=B_SPLINE_SURFACE_WITH_KNOTS('',3,3,((#99846,#99847,#99848,#99849),
(#99850,#99851,#99852,#99853),(#99854,#99855,#99856,#99857),(#99858,#99859,
#99860,#99861)),.UNSPECIFIED.,.F.,.F.,.F.,(4,4),(4,4),(-0.00286791014430819,
0.477902879790145),(0.0100271466769347,0.0166015299239866),
 .UNSPECIFIED.);
#3155=B_SPLINE_SURFACE_WITH_KNOTS('',3,3,((#99863,#99864,#99865,#99866),
(#99867,#99868,#99869,#99870),(#99871,#99872,#99873,#99874),(#99875,#99876,
#99877,#99878)),.UNSPECIFIED.,.F.,.F.,.F.,(4,4),(4,4),(0.65323027150708,
1.00206901892629),(0.00656788395381101,0.0131849432430403),
 .UNSPECIFIED.);
#3156=B_SPLINE_SURFACE_WITH_KNOTS('',3,3,((#99886,#99887,#99888,#99889),
(#99890,#99891,#99892,#99893),(#99894,#99895,#99896,#99897),(#99898,#99899,
#99900,#99901)),.UNSPECIFIED.,.F.,.F.,.F.,(4,4),(4,4),(-0.00286780410471765,
0.477902879789932),(0.0200175229646929,0.026590734618062),.UNSPECIFIED.);
#3157=B_SPLINE_SURFACE_WITH_KNOTS('',3,3,((#99903,#99904,#99905,#99906),
(#99907,#99908,#99909,#99910),(#99911,#99912,#99913,#99914),(#99915,#99916,
#99917,#99918)),.UNSPECIFIED.,.F.,.F.,.F.,(4,4),(4,4),(0.522097120210158,
1.00286753160114),(0.0166015299239891,0.0231736788075221),.UNSPECIFIED.);
#3158=B_SPLINE_SURFACE_WITH_KNOTS('',3,3,((#99920,#99921,#99922,#99923),
(#99924,#99925,#99926,#99927),(#99928,#99929,#99930,#99931),(#99932,#99933,
#99934,#99935)),.UNSPECIFIED.,.F.,.F.,.F.,(4,4),(4,4),(0.,1.00600003961369),
(0.0166015299239894,0.0265907346180634),.UNSPECIFIED.);
#3159=B_SPLINE_SURFACE_WITH_KNOTS('',3,3,((#99936,#99937,#99938,#99939),
(#99940,#99941,#99942,#99943),(#99944,#99945,#99946,#99947),(#99948,#99949,
#99950,#99951)),.UNSPECIFIED.,.F.,.F.,.F.,(4,4),(4,4),(-0.00286862201159803,
0.47790287979161),(0.0300094532292792,0.0365944846647022),.UNSPECIFIED.);
#3160=B_SPLINE_SURFACE_WITH_KNOTS('',3,3,((#99953,#99954,#99955,#99956),
(#99957,#99958,#99959,#99960),(#99961,#99962,#99963,#99964),(#99965,#99966,
#99967,#99968)),.UNSPECIFIED.,.F.,.F.,.F.,(4,4),(4,4),(0.52209712021027,
1.00286823669294),(0.0265907346180636,0.0331702036051739),.UNSPECIFIED.);
#3161=B_SPLINE_SURFACE_WITH_KNOTS('',3,3,((#99976,#99977,#99978,#99979),
(#99980,#99981,#99982,#99983),(#99984,#99985,#99986,#99987),(#99988,#99989,
#99990,#99991)),.UNSPECIFIED.,.F.,.F.,.F.,(4,4),(4,4),(-0.00286848453316211,
0.477902879790156),(0.0400218729466606,0.0466073985929427),
 .UNSPECIFIED.);
#3162=B_SPLINE_SURFACE_WITH_KNOTS('',3,3,((#100008,#100009,#100010,#100011),
(#100012,#100013,#100014,#100015),(#100016,#100017,#100018,#100019),(#100020,
#100021,#100022,#100023)),.UNSPECIFIED.,.F.,.F.,.F.,(4,4),(4,4),(0.,1.00600014639725),
(0.0365944846645068,0.0466073985929167),.UNSPECIFIED.);
#3163=B_SPLINE_SURFACE_WITH_KNOTS('',3,3,((#100024,#100025,#100026,#100027),
(#100028,#100029,#100030,#100031),(#100032,#100033,#100034,#100035),(#100036,
#100037,#100038,#100039)),.UNSPECIFIED.,.F.,.F.,.F.,(4,4),(4,4),(-0.00286780122448816,
0.477902879789605),(0.0500263550859002,0.0565997133101408),
 .UNSPECIFIED.);
#3164=B_SPLINE_SURFACE_WITH_KNOTS('',3,3,((#100041,#100042,#100043,#100044),
(#100045,#100046,#100047,#100048),(#100049,#100050,#100051,#100052),(#100053,
#100054,#100055,#100056)),.UNSPECIFIED.,.F.,.F.,.F.,(4,4),(4,4),(0.522097120210515,
1.00286810177255),(0.0466073985929452,0.0531834925888926),.UNSPECIFIED.);
#3165=B_SPLINE_SURFACE_WITH_KNOTS('',3,3,((#100064,#100065,#100066,#100067),
(#100068,#100069,#100070,#100071),(#100072,#100073,#100074,#100075),(#100076,
#100077,#100078,#100079)),.UNSPECIFIED.,.F.,.F.,.F.,(4,4),(4,4),(-0.00286792598896076,
0.477902879789448),(0.0600156865494602,0.0665898698871176),
 .UNSPECIFIED.);
#3166=B_SPLINE_SURFACE_WITH_KNOTS('',3,3,((#100081,#100082,#100083,#100084),
(#100085,#100086,#100087,#100088),(#100089,#100090,#100091,#100092),(#100093,
#100094,#100095,#100096)),.UNSPECIFIED.,.F.,.F.,.F.,(4,4),(4,4),(0.522097120210527,
1.00286764392044),(0.0565997133101414,0.0631721430887068),.UNSPECIFIED.);
#3167=B_SPLINE_SURFACE_WITH_KNOTS('',3,3,((#100112,#100113,#100114,#100115),
(#100116,#100117,#100118,#100119),(#100120,#100121,#100122,#100123),(#100124,
#100125,#100126,#100127)),.UNSPECIFIED.,.F.,.F.,.F.,(4,4),(4,4),(0.522097120209726,
1.00286833998588),(0.0665898698871198,0.0731716198748447),.UNSPECIFIED.);
#3168=B_SPLINE_SURFACE_WITH_KNOTS('',3,3,((#100128,#100129,#100130,#100131),
(#100132,#100133,#100134,#100135),(#100136,#100137,#100138,#100139),(#100140,
#100141,#100142,#100143)),.UNSPECIFIED.,.F.,.F.,.F.,(4,4),(4,4),(-0.00124731532101478,
0.209045111669004),(0.0700194292965637,0.0749900982976416),
 .UNSPECIFIED.);
#3169=B_SPLINE_SURFACE_WITH_KNOTS('',3,3,((#100150,#100151,#100152,#100153),
(#100154,#100155,#100156,#100157),(#100158,#100159,#100160,#100161),(#100162,
#100163,#100164,#100165)),.UNSPECIFIED.,.F.,.F.,.F.,(4,4),(4,4),(-0.00286791014427452,
0.477902879790323),(0.0100271466769346,0.0166015299239864),
 .UNSPECIFIED.);
#3170=B_SPLINE_SURFACE_WITH_KNOTS('',3,3,((#100167,#100168,#100169,#100170),
(#100171,#100172,#100173,#100174),(#100175,#100176,#100177,#100178),(#100179,
#100180,#100181,#100182)),.UNSPECIFIED.,.F.,.F.,.F.,(4,4),(4,4),(0.653230271507165,
1.00206901892629),(0.00656788395381716,0.0131849432430449),
 .UNSPECIFIED.);
#3171=B_SPLINE_SURFACE_WITH_KNOTS('',3,3,((#100190,#100191,#100192,#100193),
(#100194,#100195,#100196,#100197),(#100198,#100199,#100200,#100201),(#100202,
#100203,#100204,#100205)),.UNSPECIFIED.,.F.,.F.,.F.,(4,4),(4,4),(-0.00286780410474001,
0.477902879790114),(0.0200175229646904,0.0265907346180623),
 .UNSPECIFIED.);
#3172=B_SPLINE_SURFACE_WITH_KNOTS('',3,3,((#100207,#100208,#100209,#100210),
(#100211,#100212,#100213,#100214),(#100215,#100216,#100217,#100218),(#100219,
#100220,#100221,#100222)),.UNSPECIFIED.,.F.,.F.,.F.,(4,4),(4,4),(0.522097120209954,
1.00286753160118),(0.0166015299239876,0.0231736788075223),.UNSPECIFIED.);
#3173=B_SPLINE_SURFACE_WITH_KNOTS('',3,3,((#100224,#100225,#100226,#100227),
(#100228,#100229,#100230,#100231),(#100232,#100233,#100234,#100235),(#100236,
#100237,#100238,#100239)),.UNSPECIFIED.,.F.,.F.,.F.,(4,4),(4,4),(0.,1.00600003961382),
(0.0166015299239891,0.0265907346180641),.UNSPECIFIED.);
#3174=B_SPLINE_SURFACE_WITH_KNOTS('',3,3,((#100240,#100241,#100242,#100243),
(#100244,#100245,#100246,#100247),(#100248,#100249,#100250,#100251),(#100252,
#100253,#100254,#100255)),.UNSPECIFIED.,.F.,.F.,.F.,(4,4),(4,4),(-0.0028686220116151,
0.47790287979179),(0.0300094532292791,0.0365944846647015),.UNSPECIFIED.);
#3175=B_SPLINE_SURFACE_WITH_KNOTS('',3,3,((#100257,#100258,#100259,#100260),
(#100261,#100262,#100263,#100264),(#100265,#100266,#100267,#100268),(#100269,
#100270,#100271,#100272)),.UNSPECIFIED.,.F.,.F.,.F.,(4,4),(4,4),(0.522097120209979,
1.00286823669287),(0.0265907346180633,0.0331702036051745),.UNSPECIFIED.);
#3176=B_SPLINE_SURFACE_WITH_KNOTS('',3,3,((#100280,#100281,#100282,#100283),
(#100284,#100285,#100286,#100287),(#100288,#100289,#100290,#100291),(#100292,
#100293,#100294,#100295)),.UNSPECIFIED.,.F.,.F.,.F.,(4,4),(4,4),(-0.00286848453309324,
0.477902879790285),(0.0400218729466604,0.0466073985929427),
 .UNSPECIFIED.);
#3177=B_SPLINE_SURFACE_WITH_KNOTS('',3,3,((#100312,#100313,#100314,#100315),
(#100316,#100317,#100318,#100319),(#100320,#100321,#100322,#100323),(#100324,
#100325,#100326,#100327)),.UNSPECIFIED.,.F.,.F.,.F.,(4,4),(4,4),(0.,1.0060001463973),
(0.0365944846645066,0.0466073985929166),.UNSPECIFIED.);
#3178=B_SPLINE_SURFACE_WITH_KNOTS('',3,3,((#100328,#100329,#100330,#100331),
(#100332,#100333,#100334,#100335),(#100336,#100337,#100338,#100339),(#100340,
#100341,#100342,#100343)),.UNSPECIFIED.,.F.,.F.,.F.,(4,4),(4,4),(-0.00286780122440643,
0.47790287978969),(0.0500263550859002,0.0565997133101408),.UNSPECIFIED.);
#3179=B_SPLINE_SURFACE_WITH_KNOTS('',3,3,((#100345,#100346,#100347,#100348),
(#100349,#100350,#100351,#100352),(#100353,#100354,#100355,#100356),(#100357,
#100358,#100359,#100360)),.UNSPECIFIED.,.F.,.F.,.F.,(4,4),(4,4),(0.522097120210187,
1.00286810177275),(0.0466073985929441,0.0531834933545499),.UNSPECIFIED.);
#3180=B_SPLINE_SURFACE_WITH_KNOTS('',3,3,((#100368,#100369,#100370,#100371),
(#100372,#100373,#100374,#100375),(#100376,#100377,#100378,#100379),(#100380,
#100381,#100382,#100383)),.UNSPECIFIED.,.F.,.F.,.F.,(4,4),(4,4),(-0.0028679259889732,
0.477902879789529),(0.060015686549459,0.0665898698871156),.UNSPECIFIED.);
#3181=B_SPLINE_SURFACE_WITH_KNOTS('',3,3,((#100385,#100386,#100387,#100388),
(#100389,#100390,#100391,#100392),(#100393,#100394,#100395,#100396),(#100397,
#100398,#100399,#100400)),.UNSPECIFIED.,.F.,.F.,.F.,(4,4),(4,4),(0.52209712021033,
1.00286764392038),(0.0565997133101414,0.0631721430887063),.UNSPECIFIED.);
#3182=B_SPLINE_SURFACE_WITH_KNOTS('',3,3,((#100416,#100417,#100418,#100419),
(#100420,#100421,#100422,#100423),(#100424,#100425,#100426,#100427),(#100428,
#100429,#100430,#100431)),.UNSPECIFIED.,.F.,.F.,.F.,(4,4),(4,4),(0.522097120209495,
1.00286833998592),(0.0665898698871184,0.0731716198748455),.UNSPECIFIED.);
#3183=B_SPLINE_SURFACE_WITH_KNOTS('',3,3,((#100432,#100433,#100434,#100435),
(#100436,#100437,#100438,#100439),(#100440,#100441,#100442,#100443),(#100444,
#100445,#100446,#100447)),.UNSPECIFIED.,.F.,.F.,.F.,(4,4),(4,4),(-0.00124731532101882,
0.209045111668745),(0.0700194292965496,0.0749900982976448),
 .UNSPECIFIED.);
#3184=B_SPLINE_SURFACE_WITH_KNOTS('',3,3,((#100454,#100455,#100456,#100457),
(#100458,#100459,#100460,#100461),(#100462,#100463,#100464,#100465),(#100466,
#100467,#100468,#100469)),.UNSPECIFIED.,.F.,.F.,.F.,(4,4),(4,4),(-0.00286791014421451,
0.477902879790404),(0.0100271466769357,0.0166015299239858),
 .UNSPECIFIED.);
#3185=B_SPLINE_SURFACE_WITH_KNOTS('',3,3,((#100471,#100472,#100473,#100474),
(#100475,#100476,#100477,#100478),(#100479,#100480,#100481,#100482),(#100483,
#100484,#100485,#100486)),.UNSPECIFIED.,.F.,.F.,.F.,(4,4),(4,4),(0.653230271507083,
1.0020690189263),(0.0065678839538247,0.0131849432429598),.UNSPECIFIED.);
#3186=B_SPLINE_SURFACE_WITH_KNOTS('',3,3,((#100494,#100495,#100496,#100497),
(#100498,#100499,#100500,#100501),(#100502,#100503,#100504,#100505),(#100506,
#100507,#100508,#100509)),.UNSPECIFIED.,.F.,.F.,.F.,(4,4),(4,4),(-0.00286780410473929,
0.477902879790195),(0.0200175229646904,0.0265907346180615),
 .UNSPECIFIED.);
#3187=B_SPLINE_SURFACE_WITH_KNOTS('',3,3,((#100511,#100512,#100513,#100514),
(#100515,#100516,#100517,#100518),(#100519,#100520,#100521,#100522),(#100523,
#100524,#100525,#100526)),.UNSPECIFIED.,.F.,.F.,.F.,(4,4),(4,4),(0.522097120209717,
1.00286753160124),(0.0166015299239884,0.023173678807522),.UNSPECIFIED.);
#3188=B_SPLINE_SURFACE_WITH_KNOTS('',3,3,((#100528,#100529,#100530,#100531),
(#100532,#100533,#100534,#100535),(#100536,#100537,#100538,#100539),(#100540,
#100541,#100542,#100543)),.UNSPECIFIED.,.F.,.F.,.F.,(4,4),(4,4),(0.,1.00600003961404),
(0.0166015299239892,0.0265907346180639),.UNSPECIFIED.);
#3189=B_SPLINE_SURFACE_WITH_KNOTS('',3,3,((#100544,#100545,#100546,#100547),
(#100548,#100549,#100550,#100551),(#100552,#100553,#100554,#100555),(#100556,
#100557,#100558,#100559)),.UNSPECIFIED.,.F.,.F.,.F.,(4,4),(4,4),(-0.00286862201162821,
0.4779028797919),(0.0300094532292786,0.0365944846647022),.UNSPECIFIED.);
#3190=B_SPLINE_SURFACE_WITH_KNOTS('',3,3,((#100561,#100562,#100563,#100564),
(#100565,#100566,#100567,#100568),(#100569,#100570,#100571,#100572),(#100573,
#100574,#100575,#100576)),.UNSPECIFIED.,.F.,.F.,.F.,(4,4),(4,4),(0.522097120210013,
1.00286823669283),(0.0265907346180632,0.0331702036889939),.UNSPECIFIED.);
#3191=B_SPLINE_SURFACE_WITH_KNOTS('',3,3,((#100584,#100585,#100586,#100587),
(#100588,#100589,#100590,#100591),(#100592,#100593,#100594,#100595),(#100596,
#100597,#100598,#100599)),.UNSPECIFIED.,.F.,.F.,.F.,(4,4),(4,4),(-0.002868484533028,
0.477902879790492),(0.0400218729466594,0.0466073985929433),
 .UNSPECIFIED.);
#3192=B_SPLINE_SURFACE_WITH_KNOTS('',3,3,((#100616,#100617,#100618,#100619),
(#100620,#100621,#100622,#100623),(#100624,#100625,#100626,#100627),(#100628,
#100629,#100630,#100631)),.UNSPECIFIED.,.F.,.F.,.F.,(4,4),(4,4),(0.,1.00600014639751),
(0.0365944846645073,0.0466073985929175),.UNSPECIFIED.);
#3193=B_SPLINE_SURFACE_WITH_KNOTS('',3,3,((#100632,#100633,#100634,#100635),
(#100636,#100637,#100638,#100639),(#100640,#100641,#100642,#100643),(#100644,
#100645,#100646,#100647)),.UNSPECIFIED.,.F.,.F.,.F.,(4,4),(4,4),(-0.00286780122436653,
0.477902879789868),(0.0500263550858999,0.0565997133101414),
 .UNSPECIFIED.);
#3194=B_SPLINE_SURFACE_WITH_KNOTS('',3,3,((#100649,#100650,#100651,#100652),
(#100653,#100654,#100655,#100656),(#100657,#100658,#100659,#100660),(#100661,
#100662,#100663,#100664)),.UNSPECIFIED.,.F.,.F.,.F.,(4,4),(4,4),(0.522097120210068,
1.00286810177241),(0.0466073985929445,0.0531834925888927),.UNSPECIFIED.);
#3195=B_SPLINE_SURFACE_WITH_KNOTS('',3,3,((#100672,#100673,#100674,#100675),
(#100676,#100677,#100678,#100679),(#100680,#100681,#100682,#100683),(#100684,
#100685,#100686,#100687)),.UNSPECIFIED.,.F.,.F.,.F.,(4,4),(4,4),(-0.0028679259889283,
0.477902879789711),(0.0600156865494596,0.0665898698871177),
 .UNSPECIFIED.);
#3196=B_SPLINE_SURFACE_WITH_KNOTS('',3,3,((#100689,#100690,#100691,#100692),
(#100693,#100694,#100695,#100696),(#100697,#100698,#100699,#100700),(#100701,
#100702,#100703,#100704)),.UNSPECIFIED.,.F.,.F.,.F.,(4,4),(4,4),(0.522097120210247,
1.00286764392036),(0.0565997133101416,0.0631721430887064),.UNSPECIFIED.);
#3197=B_SPLINE_SURFACE_WITH_KNOTS('',3,3,((#100720,#100721,#100722,#100723),
(#100724,#100725,#100726,#100727),(#100728,#100729,#100730,#100731),(#100732,
#100733,#100734,#100735)),.UNSPECIFIED.,.F.,.F.,.F.,(4,4),(4,4),(0.522097120209502,
1.00286833998601),(0.0665898698871197,0.0731716198748448),.UNSPECIFIED.);
#3198=B_SPLINE_SURFACE_WITH_KNOTS('',3,3,((#100736,#100737,#100738,#100739),
(#100740,#100741,#100742,#100743),(#100744,#100745,#100746,#100747),(#100748,
#100749,#100750,#100751)),.UNSPECIFIED.,.F.,.F.,.F.,(4,4),(4,4),(-0.00124731532100415,
0.209045111668643),(0.0700194292965383,0.0749900982976484),
 .UNSPECIFIED.);
#3199=B_SPLINE_SURFACE_WITH_KNOTS('',3,3,((#100758,#100759,#100760,#100761),
(#100762,#100763,#100764,#100765),(#100766,#100767,#100768,#100769),(#100770,
#100771,#100772,#100773)),.UNSPECIFIED.,.F.,.F.,.F.,(4,4),(4,4),(-0.00286791014416191,
0.477902879790526),(0.0100271466769333,0.016601529923987),.UNSPECIFIED.);
#3200=B_SPLINE_SURFACE_WITH_KNOTS('',3,3,((#100775,#100776,#100777,#100778),
(#100779,#100780,#100781,#100782),(#100783,#100784,#100785,#100786),(#100787,
#100788,#100789,#100790)),.UNSPECIFIED.,.F.,.F.,.F.,(4,4),(4,4),(0.65323027150715,
1.0020690189263),(0.00656788395383221,0.0131849432429627),.UNSPECIFIED.);
#3201=B_SPLINE_SURFACE_WITH_KNOTS('',3,3,((#100798,#100799,#100800,#100801),
(#100802,#100803,#100804,#100805),(#100806,#100807,#100808,#100809),(#100810,
#100811,#100812,#100813)),.UNSPECIFIED.,.F.,.F.,.F.,(4,4),(4,4),(-0.00286780410472678,
0.47790287979035),(0.0200175229646902,0.0265907346180624),.UNSPECIFIED.);
#3202=B_SPLINE_SURFACE_WITH_KNOTS('',3,3,((#100815,#100816,#100817,#100818),
(#100819,#100820,#100821,#100822),(#100823,#100824,#100825,#100826),(#100827,
#100828,#100829,#100830)),.UNSPECIFIED.,.F.,.F.,.F.,(4,4),(4,4),(0.522097120209711,
1.00286753160107),(0.0166015299239882,0.0231736788075225),.UNSPECIFIED.);
#3203=B_SPLINE_SURFACE_WITH_KNOTS('',3,3,((#100832,#100833,#100834,#100835),
(#100836,#100837,#100838,#100839),(#100840,#100841,#100842,#100843),(#100844,
#100845,#100846,#100847)),.UNSPECIFIED.,.F.,.F.,.F.,(4,4),(4,4),(0.,1.00600003961419),
(0.0166015299239868,0.0265907346180623),.UNSPECIFIED.);
#3204=B_SPLINE_SURFACE_WITH_KNOTS('',3,3,((#100848,#100849,#100850,#100851),
(#100852,#100853,#100854,#100855),(#100856,#100857,#100858,#100859),(#100860,
#100861,#100862,#100863)),.UNSPECIFIED.,.F.,.F.,.F.,(4,4),(4,4),(-0.00286862201159017,
0.477902879792073),(0.0300094532292792,0.036594484664702),.UNSPECIFIED.);
#3205=B_SPLINE_SURFACE_WITH_KNOTS('',3,3,((#100865,#100866,#100867,#100868),
(#100869,#100870,#100871,#100872),(#100873,#100874,#100875,#100876),(#100877,
#100878,#100879,#100880)),.UNSPECIFIED.,.F.,.F.,.F.,(4,4),(4,4),(0.522097120209888,
1.00286823669285),(0.0265907346180635,0.0331702036889926),.UNSPECIFIED.);
#3206=B_SPLINE_SURFACE_WITH_KNOTS('',3,3,((#100888,#100889,#100890,#100891),
(#100892,#100893,#100894,#100895),(#100896,#100897,#100898,#100899),(#100900,
#100901,#100902,#100903)),.UNSPECIFIED.,.F.,.F.,.F.,(4,4),(4,4),(-0.00286848453299057,
0.477902879790606),(0.0400218729466602,0.0466073985929431),
 .UNSPECIFIED.);
#3207=B_SPLINE_SURFACE_WITH_KNOTS('',3,3,((#100920,#100921,#100922,#100923),
(#100924,#100925,#100926,#100927),(#100928,#100929,#100930,#100931),(#100932,
#100933,#100934,#100935)),.UNSPECIFIED.,.F.,.F.,.F.,(4,4),(4,4),(0.,1.00600014639753),
(0.0365944846645068,0.0466073985929167),.UNSPECIFIED.);
#3208=B_SPLINE_SURFACE_WITH_KNOTS('',3,3,((#100936,#100937,#100938,#100939),
(#100940,#100941,#100942,#100943),(#100944,#100945,#100946,#100947),(#100948,
#100949,#100950,#100951)),.UNSPECIFIED.,.F.,.F.,.F.,(4,4),(4,4),(-0.00286780122431204,
0.477902879789971),(0.0500263550858996,0.0565997133101401),
 .UNSPECIFIED.);
#3209=B_SPLINE_SURFACE_WITH_KNOTS('',3,3,((#100953,#100954,#100955,#100956),
(#100957,#100958,#100959,#100960),(#100961,#100962,#100963,#100964),(#100965,
#100966,#100967,#100968)),.UNSPECIFIED.,.F.,.F.,.F.,(4,4),(4,4),(0.522097120209995,
1.00286810177248),(0.0466073985929453,0.0531834925888927),.UNSPECIFIED.);
#3210=B_SPLINE_SURFACE_WITH_KNOTS('',3,3,((#100976,#100977,#100978,#100979),
(#100980,#100981,#100982,#100983),(#100984,#100985,#100986,#100987),(#100988,
#100989,#100990,#100991)),.UNSPECIFIED.,.F.,.F.,.F.,(4,4),(4,4),(-0.00286792598893965,
0.477902879789888),(0.0600156865494596,0.0665898698871179),
 .UNSPECIFIED.);
#3211=B_SPLINE_SURFACE_WITH_KNOTS('',3,3,((#100993,#100994,#100995,#100996),
(#100997,#100998,#100999,#101000),(#101001,#101002,#101003,#101004),(#101005,
#101006,#101007,#101008)),.UNSPECIFIED.,.F.,.F.,.F.,(4,4),(4,4),(0.522097120210143,
1.00286764392032),(0.0565997133101415,0.0631721430887063),.UNSPECIFIED.);
#3212=B_SPLINE_SURFACE_WITH_KNOTS('',3,3,((#101024,#101025,#101026,#101027),
(#101028,#101029,#101030,#101031),(#101032,#101033,#101034,#101035),(#101036,
#101037,#101038,#101039)),.UNSPECIFIED.,.F.,.F.,.F.,(4,4),(4,4),(0.522097120209265,
1.0028683399859),(0.066589869887119,0.0731716198748447),.UNSPECIFIED.);
#3213=B_SPLINE_SURFACE_WITH_KNOTS('',3,3,((#101040,#101041,#101042,#101043),
(#101044,#101045,#101046,#101047),(#101048,#101049,#101050,#101051),(#101052,
#101053,#101054,#101055)),.UNSPECIFIED.,.F.,.F.,.F.,(4,4),(4,4),(-0.00124731532099686,
0.209045111668682),(0.070019429296526,0.0749900982976544),.UNSPECIFIED.);
#3214=B_SPLINE_SURFACE_WITH_KNOTS('',3,3,((#101062,#101063,#101064,#101065),
(#101066,#101067,#101068,#101069),(#101070,#101071,#101072,#101073),(#101074,
#101075,#101076,#101077)),.UNSPECIFIED.,.F.,.F.,.F.,(4,4),(4,4),(-0.00286791014411575,
0.477902879790672),(0.0100271466769346,0.0166015299239877),
 .UNSPECIFIED.);
#3215=B_SPLINE_SURFACE_WITH_KNOTS('',3,3,((#101079,#101080,#101081,#101082),
(#101083,#101084,#101085,#101086),(#101087,#101088,#101089,#101090),(#101091,
#101092,#101093,#101094)),.UNSPECIFIED.,.F.,.F.,.F.,(4,4),(4,4),(0.653230271507093,
1.0020690189263),(0.00656788395384009,0.0131849432430558),.UNSPECIFIED.);
#3216=B_SPLINE_SURFACE_WITH_KNOTS('',3,3,((#101102,#101103,#101104,#101105),
(#101106,#101107,#101108,#101109),(#101110,#101111,#101112,#101113),(#101114,
#101115,#101116,#101117)),.UNSPECIFIED.,.F.,.F.,.F.,(4,4),(4,4),(-0.00286780410468854,
0.477902879790407),(0.0200175229646894,0.0265907346180616),
 .UNSPECIFIED.);
#3217=B_SPLINE_SURFACE_WITH_KNOTS('',3,3,((#101119,#101120,#101121,#101122),
(#101123,#101124,#101125,#101126),(#101127,#101128,#101129,#101130),(#101131,
#101132,#101133,#101134)),.UNSPECIFIED.,.F.,.F.,.F.,(4,4),(4,4),(0.522097120209609,
1.00286753160126),(0.0166015299239883,0.0231736788075222),.UNSPECIFIED.);
#3218=B_SPLINE_SURFACE_WITH_KNOTS('',3,3,((#101136,#101137,#101138,#101139),
(#101140,#101141,#101142,#101143),(#101144,#101145,#101146,#101147),(#101148,
#101149,#101150,#101151)),.UNSPECIFIED.,.F.,.F.,.F.,(4,4),(4,4),(0.,1.00600003961408),
(0.0166015299239858,0.0265907346180616),.UNSPECIFIED.);
#3219=B_SPLINE_SURFACE_WITH_KNOTS('',3,3,((#101152,#101153,#101154,#101155),
(#101156,#101157,#101158,#101159),(#101160,#101161,#101162,#101163),(#101164,
#101165,#101166,#101167)),.UNSPECIFIED.,.F.,.F.,.F.,(4,4),(4,4),(-0.00286862201157823,
0.477902879792094),(0.0300094532292784,0.0365944846647017),
 .UNSPECIFIED.);
#3220=B_SPLINE_SURFACE_WITH_KNOTS('',3,3,((#101169,#101170,#101171,#101172),
(#101173,#101174,#101175,#101176),(#101177,#101178,#101179,#101180),(#101181,
#101182,#101183,#101184)),.UNSPECIFIED.,.F.,.F.,.F.,(4,4),(4,4),(0.522097120209858,
1.00286823669298),(0.0265907346180633,0.033170203688993),.UNSPECIFIED.);
#3221=B_SPLINE_SURFACE_WITH_KNOTS('',3,3,((#101192,#101193,#101194,#101195),
(#101196,#101197,#101198,#101199),(#101200,#101201,#101202,#101203),(#101204,
#101205,#101206,#101207)),.UNSPECIFIED.,.F.,.F.,.F.,(4,4),(4,4),(-0.00286848453291097,
0.47790287979078),(0.0400218729466607,0.0466073985929428),.UNSPECIFIED.);
#3222=B_SPLINE_SURFACE_WITH_KNOTS('',3,3,((#101224,#101225,#101226,#101227),
(#101228,#101229,#101230,#101231),(#101232,#101233,#101234,#101235),(#101236,
#101237,#101238,#101239)),.UNSPECIFIED.,.F.,.F.,.F.,(4,4),(4,4),(0.,1.00600014639742),
(0.0365944846645073,0.0466073985929146),.UNSPECIFIED.);
#3223=B_SPLINE_SURFACE_WITH_KNOTS('',3,3,((#101240,#101241,#101242,#101243),
(#101244,#101245,#101246,#101247),(#101248,#101249,#101250,#101251),(#101252,
#101253,#101254,#101255)),.UNSPECIFIED.,.F.,.F.,.F.,(4,4),(4,4),(-0.00286780122425562,
0.477902879790124),(0.0500263550858987,0.0565997133101411),
 .UNSPECIFIED.);
#3224=B_SPLINE_SURFACE_WITH_KNOTS('',3,3,((#101257,#101258,#101259,#101260),
(#101261,#101262,#101263,#101264),(#101265,#101266,#101267,#101268),(#101269,
#101270,#101271,#101272)),.UNSPECIFIED.,.F.,.F.,.F.,(4,4),(4,4),(0.522097120209903,
1.00286810177251),(0.0466073985929444,0.0531834925888938),.UNSPECIFIED.);
#3225=B_SPLINE_SURFACE_WITH_KNOTS('',3,3,((#101280,#101281,#101282,#101283),
(#101284,#101285,#101286,#101287),(#101288,#101289,#101290,#101291),(#101292,
#101293,#101294,#101295)),.UNSPECIFIED.,.F.,.F.,.F.,(4,4),(4,4),(-0.00286792598893161,
0.477902879789993),(0.0600156865494595,0.0665898698871174),
 .UNSPECIFIED.);
#3226=B_SPLINE_SURFACE_WITH_KNOTS('',3,3,((#101297,#101298,#101299,#101300),
(#101301,#101302,#101303,#101304),(#101305,#101306,#101307,#101308),(#101309,
#101310,#101311,#101312)),.UNSPECIFIED.,.F.,.F.,.F.,(4,4),(4,4),(0.522097120210098,
1.00286764392041),(0.0565997133101421,0.0631721430887063),.UNSPECIFIED.);
#3227=B_SPLINE_SURFACE_WITH_KNOTS('',3,3,((#101328,#101329,#101330,#101331),
(#101332,#101333,#101334,#101335),(#101336,#101337,#101338,#101339),(#101340,
#101341,#101342,#101343)),.UNSPECIFIED.,.F.,.F.,.F.,(4,4),(4,4),(0.522097120209149,
1.00286833998593),(0.0665898698871195,0.0731716198748446),.UNSPECIFIED.);
#3228=B_SPLINE_SURFACE_WITH_KNOTS('',3,3,((#101344,#101345,#101346,#101347),
(#101348,#101349,#101350,#101351),(#101352,#101353,#101354,#101355),(#101356,
#101357,#101358,#101359)),.UNSPECIFIED.,.F.,.F.,.F.,(4,4),(4,4),(-0.0012473153209956,
0.20904511166891),(0.0700194292965164,0.0749900982976622),.UNSPECIFIED.);
#3229=B_SPLINE_SURFACE_WITH_KNOTS('',3,3,((#101366,#101367,#101368,#101369),
(#101370,#101371,#101372,#101373),(#101374,#101375,#101376,#101377),(#101378,
#101379,#101380,#101381)),.UNSPECIFIED.,.F.,.F.,.F.,(4,4),(4,4),(-0.00286791014405807,
0.477902879790714),(0.010027146676934,0.0166015299239858),.UNSPECIFIED.);
#3230=B_SPLINE_SURFACE_WITH_KNOTS('',3,3,((#101383,#101384,#101385,#101386),
(#101387,#101388,#101389,#101390),(#101391,#101392,#101393,#101394),(#101395,
#101396,#101397,#101398)),.UNSPECIFIED.,.F.,.F.,.F.,(4,4),(4,4),(0.653230271507078,
1.00206901892629),(0.00656788395384775,0.0131849432430557),
 .UNSPECIFIED.);
#3231=B_SPLINE_SURFACE_WITH_KNOTS('',3,3,((#101406,#101407,#101408,#101409),
(#101410,#101411,#101412,#101413),(#101414,#101415,#101416,#101417),(#101418,
#101419,#101420,#101421)),.UNSPECIFIED.,.F.,.F.,.F.,(4,4),(4,4),(-0.00286780410470242,
0.477902879790501),(0.0200175229646922,0.0265907346180627),
 .UNSPECIFIED.);
#3232=B_SPLINE_SURFACE_WITH_KNOTS('',3,3,((#101423,#101424,#101425,#101426),
(#101427,#101428,#101429,#101430),(#101431,#101432,#101433,#101434),(#101435,
#101436,#101437,#101438)),.UNSPECIFIED.,.F.,.F.,.F.,(4,4),(4,4),(0.522097120209468,
1.00286753160118),(0.016601529923988,0.0231736788075219),.UNSPECIFIED.);
#3233=B_SPLINE_SURFACE_WITH_KNOTS('',3,3,((#101440,#101441,#101442,#101443),
(#101444,#101445,#101446,#101447),(#101448,#101449,#101450,#101451),(#101452,
#101453,#101454,#101455)),.UNSPECIFIED.,.F.,.F.,.F.,(4,4),(4,4),(0.,1.00600003961353),
(0.0166015299239881,0.0265907346180615),.UNSPECIFIED.);
#3234=B_SPLINE_SURFACE_WITH_KNOTS('',3,3,((#101456,#101457,#101458,#101459),
(#101460,#101461,#101462,#101463),(#101464,#101465,#101466,#101467),(#101468,
#101469,#101470,#101471)),.UNSPECIFIED.,.F.,.F.,.F.,(4,4),(4,4),(-0.00286862201162393,
0.477902879792228),(0.0300094532292793,0.0365944846647173),
 .UNSPECIFIED.);
#3235=B_SPLINE_SURFACE_WITH_KNOTS('',3,3,((#101473,#101474,#101475,#101476),
(#101477,#101478,#101479,#101480),(#101481,#101482,#101483,#101484),(#101485,
#101486,#101487,#101488)),.UNSPECIFIED.,.F.,.F.,.F.,(4,4),(4,4),(0.52209712020978,
1.00286823669302),(0.0265907346180633,0.0331702036889924),.UNSPECIFIED.);
#3236=B_SPLINE_SURFACE_WITH_KNOTS('',3,3,((#101496,#101497,#101498,#101499),
(#101500,#101501,#101502,#101503),(#101504,#101505,#101506,#101507),(#101508,
#101509,#101510,#101511)),.UNSPECIFIED.,.F.,.F.,.F.,(4,4),(4,4),(-0.00286848453286967,
0.477902879790773),(0.0400218729466607,0.0466073985929426),
 .UNSPECIFIED.);
#3237=B_SPLINE_SURFACE_WITH_KNOTS('',3,3,((#101528,#101529,#101530,#101531),
(#101532,#101533,#101534,#101535),(#101536,#101537,#101538,#101539),(#101540,
#101541,#101542,#101543)),.UNSPECIFIED.,.F.,.F.,.F.,(4,4),(4,4),(0.,1.00600014639731),
(0.0365944846645069,0.0466073985929157),.UNSPECIFIED.);
#3238=B_SPLINE_SURFACE_WITH_KNOTS('',3,3,((#101544,#101545,#101546,#101547),
(#101548,#101549,#101550,#101551),(#101552,#101553,#101554,#101555),(#101556,
#101557,#101558,#101559)),.UNSPECIFIED.,.F.,.F.,.F.,(4,4),(4,4),(-0.00286780122421701,
0.477902879790205),(0.0500263550858998,0.0565997133101419),
 .UNSPECIFIED.);
#3239=B_SPLINE_SURFACE_WITH_KNOTS('',3,3,((#101561,#101562,#101563,#101564),
(#101565,#101566,#101567,#101568),(#101569,#101570,#101571,#101572),(#101573,
#101574,#101575,#101576)),.UNSPECIFIED.,.F.,.F.,.F.,(4,4),(4,4),(0.522097120209756,
1.00286810177259),(0.0466073985929451,0.0531834925888926),.UNSPECIFIED.);
#3240=B_SPLINE_SURFACE_WITH_KNOTS('',3,3,((#101584,#101585,#101586,#101587),
(#101588,#101589,#101590,#101591),(#101592,#101593,#101594,#101595),(#101596,
#101597,#101598,#101599)),.UNSPECIFIED.,.F.,.F.,.F.,(4,4),(4,4),(-0.00286792598891565,
0.477902879790097),(0.0600156865494599,0.066589869887118),.UNSPECIFIED.);
#3241=B_SPLINE_SURFACE_WITH_KNOTS('',3,3,((#101601,#101602,#101603,#101604),
(#101605,#101606,#101607,#101608),(#101609,#101610,#101611,#101612),(#101613,
#101614,#101615,#101616)),.UNSPECIFIED.,.F.,.F.,.F.,(4,4),(4,4),(0.52209712020998,
1.00286764392034),(0.0565997133101425,0.0631721430887065),.UNSPECIFIED.);
#3242=B_SPLINE_SURFACE_WITH_KNOTS('',3,3,((#101632,#101633,#101634,#101635),
(#101636,#101637,#101638,#101639),(#101640,#101641,#101642,#101643),(#101644,
#101645,#101646,#101647)),.UNSPECIFIED.,.F.,.F.,.F.,(4,4),(4,4),(0.522097120209037,
1.0028683399859),(0.0665898698871199,0.0731716198748443),.UNSPECIFIED.);
#3243=B_SPLINE_SURFACE_WITH_KNOTS('',3,3,((#101648,#101649,#101650,#101651),
(#101652,#101653,#101654,#101655),(#101656,#101657,#101658,#101659),(#101660,
#101661,#101662,#101663)),.UNSPECIFIED.,.F.,.F.,.F.,(4,4),(4,4),(-0.0012473153210096,
0.209045111670342),(0.0700194292965093,0.0749900982976691),
 .UNSPECIFIED.);
#3244=B_SPLINE_SURFACE_WITH_KNOTS('',3,3,((#101670,#101671,#101672,#101673),
(#101674,#101675,#101676,#101677),(#101678,#101679,#101680,#101681),(#101682,
#101683,#101684,#101685)),.UNSPECIFIED.,.F.,.F.,.F.,(4,4),(4,4),(-0.00286791014400684,
0.477902879790898),(0.0100271466769358,0.0166015299239862),
 .UNSPECIFIED.);
#3245=B_SPLINE_SURFACE_WITH_KNOTS('',3,3,((#101687,#101688,#101689,#101690),
(#101691,#101692,#101693,#101694),(#101695,#101696,#101697,#101698),(#101699,
#101700,#101701,#101702)),.UNSPECIFIED.,.F.,.F.,.F.,(4,4),(4,4),(0.653230271507063,
1.0020690189263),(0.00656788395403927,0.0131849432122613),.UNSPECIFIED.);
#3246=B_SPLINE_SURFACE_WITH_KNOTS('',3,3,((#101710,#101711,#101712,#101713),
(#101714,#101715,#101716,#101717),(#101718,#101719,#101720,#101721),(#101722,
#101723,#101724,#101725)),.UNSPECIFIED.,.F.,.F.,.F.,(4,4),(4,4),(-0.00286780410476689,
0.47790287979065),(0.0200175229646906,0.0265907346180626),.UNSPECIFIED.);
#3247=B_SPLINE_SURFACE_WITH_KNOTS('',3,3,((#101727,#101728,#101729,#101730),
(#101731,#101732,#101733,#101734),(#101735,#101736,#101737,#101738),(#101739,
#101740,#101741,#101742)),.UNSPECIFIED.,.F.,.F.,.F.,(4,4),(4,4),(0.522097120209285,
1.00286753160117),(0.016601529923988,0.0231736788075221),.UNSPECIFIED.);
#3248=B_SPLINE_SURFACE_WITH_KNOTS('',3,3,((#101744,#101745,#101746,#101747),
(#101748,#101749,#101750,#101751),(#101752,#101753,#101754,#101755),(#101756,
#101757,#101758,#101759)),.UNSPECIFIED.,.F.,.F.,.F.,(4,4),(4,4),(0.,1.00600003961394),
(0.0166015299239902,0.0265907346180641),.UNSPECIFIED.);
#3249=B_SPLINE_SURFACE_WITH_KNOTS('',3,3,((#101760,#101761,#101762,#101763),
(#101764,#101765,#101766,#101767),(#101768,#101769,#101770,#101771),(#101772,
#101773,#101774,#101775)),.UNSPECIFIED.,.F.,.F.,.F.,(4,4),(4,4),(-0.00286862201157575,
0.477902879792379),(0.0300094532292789,0.0365944846647167),
 .UNSPECIFIED.);
#3250=B_SPLINE_SURFACE_WITH_KNOTS('',3,3,((#101777,#101778,#101779,#101780),
(#101781,#101782,#101783,#101784),(#101785,#101786,#101787,#101788),(#101789,
#101790,#101791,#101792)),.UNSPECIFIED.,.F.,.F.,.F.,(4,4),(4,4),(0.522097120209556,
1.00286823669293),(0.0265907346180646,0.033170203605174),.UNSPECIFIED.);
#3251=B_SPLINE_SURFACE_WITH_KNOTS('',3,3,((#101800,#101801,#101802,#101803),
(#101804,#101805,#101806,#101807),(#101808,#101809,#101810,#101811),(#101812,
#101813,#101814,#101815)),.UNSPECIFIED.,.F.,.F.,.F.,(4,4),(4,4),(-0.00286848453283359,
0.47790287979088),(0.0400218729466603,0.0466073985929439),.UNSPECIFIED.);
#3252=B_SPLINE_SURFACE_WITH_KNOTS('',3,3,((#101832,#101833,#101834,#101835),
(#101836,#101837,#101838,#101839),(#101840,#101841,#101842,#101843),(#101844,
#101845,#101846,#101847)),.UNSPECIFIED.,.F.,.F.,.F.,(4,4),(4,4),(0.,1.00600014639716),
(0.0365944846645056,0.0466073985929156),.UNSPECIFIED.);
#3253=B_SPLINE_SURFACE_WITH_KNOTS('',3,3,((#101848,#101849,#101850,#101851),
(#101852,#101853,#101854,#101855),(#101856,#101857,#101858,#101859),(#101860,
#101861,#101862,#101863)),.UNSPECIFIED.,.F.,.F.,.F.,(4,4),(4,4),(-0.00286780122415958,
0.477902879790323),(0.0500263550859002,0.0565997133101402),
 .UNSPECIFIED.);
#3254=B_SPLINE_SURFACE_WITH_KNOTS('',3,3,((#101865,#101866,#101867,#101868),
(#101869,#101870,#101871,#101872),(#101873,#101874,#101875,#101876),(#101877,
#101878,#101879,#101880)),.UNSPECIFIED.,.F.,.F.,.F.,(4,4),(4,4),(0.522097120209669,
1.00286810177273),(0.0466073985929445,0.0531834933545507),.UNSPECIFIED.);
#3255=B_SPLINE_SURFACE_WITH_KNOTS('',3,3,((#101888,#101889,#101890,#101891),
(#101892,#101893,#101894,#101895),(#101896,#101897,#101898,#101899),(#101900,
#101901,#101902,#101903)),.UNSPECIFIED.,.F.,.F.,.F.,(4,4),(4,4),(-0.00286792598894784,
0.477902879790276),(0.0600156865494617,0.0665898698871163),
 .UNSPECIFIED.);
#3256=B_SPLINE_SURFACE_WITH_KNOTS('',3,3,((#101905,#101906,#101907,#101908),
(#101909,#101910,#101911,#101912),(#101913,#101914,#101915,#101916),(#101917,
#101918,#101919,#101920)),.UNSPECIFIED.,.F.,.F.,.F.,(4,4),(4,4),(0.522097120209863,
1.00286764392033),(0.0565997133101412,0.0631721430887067),.UNSPECIFIED.);
#3257=B_SPLINE_SURFACE_WITH_KNOTS('',3,3,((#101936,#101937,#101938,#101939),
(#101940,#101941,#101942,#101943),(#101944,#101945,#101946,#101947),(#101948,
#101949,#101950,#101951)),.UNSPECIFIED.,.F.,.F.,.F.,(4,4),(4,4),(0.522097120209008,
1.00286833998591),(0.0665898698871192,0.0731716198748459),.UNSPECIFIED.);
#3258=B_SPLINE_SURFACE_WITH_KNOTS('',3,3,((#101952,#101953,#101954,#101955),
(#101956,#101957,#101958,#101959),(#101960,#101961,#101962,#101963),(#101964,
#101965,#101966,#101967)),.UNSPECIFIED.,.F.,.F.,.F.,(4,4),(4,4),(-0.00124731532103255,
0.209045111672332),(0.0700194292965018,0.0749900982976787),
 .UNSPECIFIED.);
#3259=B_SPLINE_SURFACE_WITH_KNOTS('',3,3,((#101974,#101975,#101976,#101977),
(#101978,#101979,#101980,#101981),(#101982,#101983,#101984,#101985),(#101986,
#101987,#101988,#101989)),.UNSPECIFIED.,.F.,.F.,.F.,(4,4),(4,4),(-0.00286791014398595,
0.477902879790942),(0.0100271466769384,0.0166015299239859),
 .UNSPECIFIED.);
#3260=B_SPLINE_SURFACE_WITH_KNOTS('',3,3,((#101991,#101992,#101993,#101994),
(#101995,#101996,#101997,#101998),(#101999,#102000,#102001,#102002),(#102003,
#102004,#102005,#102006)),.UNSPECIFIED.,.F.,.F.,.F.,(4,4),(4,4),(0.65323027150641,
1.00206901892628),(0.0065678839540488,0.0131849432122596),.UNSPECIFIED.);
#3261=B_SPLINE_SURFACE_WITH_KNOTS('',3,3,((#102014,#102015,#102016,#102017),
(#102018,#102019,#102020,#102021),(#102022,#102023,#102024,#102025),(#102026,
#102027,#102028,#102029)),.UNSPECIFIED.,.F.,.F.,.F.,(4,4),(4,4),(-0.0028678041047262,
0.477902879790764),(0.0200175229646916,0.0265907346180621),
 .UNSPECIFIED.);
#3262=B_SPLINE_SURFACE_WITH_KNOTS('',3,3,((#102031,#102032,#102033,#102034),
(#102035,#102036,#102037,#102038),(#102039,#102040,#102041,#102042),(#102043,
#102044,#102045,#102046)),.UNSPECIFIED.,.F.,.F.,.F.,(4,4),(4,4),(0.522097120209154,
1.00286753160127),(0.0166015299239883,0.0231736788075222),.UNSPECIFIED.);
#3263=B_SPLINE_SURFACE_WITH_KNOTS('',3,3,((#102048,#102049,#102050,#102051),
(#102052,#102053,#102054,#102055),(#102056,#102057,#102058,#102059),(#102060,
#102061,#102062,#102063)),.UNSPECIFIED.,.F.,.F.,.F.,(4,4),(4,4),(0.,1.00600003961365),
(0.016601529923988,0.0265907346180656),.UNSPECIFIED.);
#3264=B_SPLINE_SURFACE_WITH_KNOTS('',3,3,((#102064,#102065,#102066,#102067),
(#102068,#102069,#102070,#102071),(#102072,#102073,#102074,#102075),(#102076,
#102077,#102078,#102079)),.UNSPECIFIED.,.F.,.F.,.F.,(4,4),(4,4),(-0.00286862201160525,
0.477902879792415),(0.0300094532292785,0.0365944846647022),
 .UNSPECIFIED.);
#3265=B_SPLINE_SURFACE_WITH_KNOTS('',3,3,((#102081,#102082,#102083,#102084),
(#102085,#102086,#102087,#102088),(#102089,#102090,#102091,#102092),(#102093,
#102094,#102095,#102096)),.UNSPECIFIED.,.F.,.F.,.F.,(4,4),(4,4),(0.522097120209503,
1.00286823669289),(0.0265907346180636,0.0331702036889927),.UNSPECIFIED.);
#3266=B_SPLINE_SURFACE_WITH_KNOTS('',3,3,((#102104,#102105,#102106,#102107),
(#102108,#102109,#102110,#102111),(#102112,#102113,#102114,#102115),(#102116,
#102117,#102118,#102119)),.UNSPECIFIED.,.F.,.F.,.F.,(4,4),(4,4),(-0.00286848453280808,
0.477902879791013),(0.0400218729466605,0.0466073985929591),
 .UNSPECIFIED.);
#3267=B_SPLINE_SURFACE_WITH_KNOTS('',3,3,((#102136,#102137,#102138,#102139),
(#102140,#102141,#102142,#102143),(#102144,#102145,#102146,#102147),(#102148,
#102149,#102150,#102151)),.UNSPECIFIED.,.F.,.F.,.F.,(4,4),(4,4),(0.,1.00600014639734),
(0.0365944846645064,0.0466073985929166),.UNSPECIFIED.);
#3268=B_SPLINE_SURFACE_WITH_KNOTS('',3,3,((#102152,#102153,#102154,#102155),
(#102156,#102157,#102158,#102159),(#102160,#102161,#102162,#102163),(#102164,
#102165,#102166,#102167)),.UNSPECIFIED.,.F.,.F.,.F.,(4,4),(4,4),(-0.00286780122410264,
0.477902879790367),(0.0500263550859007,0.0565997133101572),
 .UNSPECIFIED.);
#3269=B_SPLINE_SURFACE_WITH_KNOTS('',3,3,((#102169,#102170,#102171,#102172),
(#102173,#102174,#102175,#102176),(#102177,#102178,#102179,#102180),(#102181,
#102182,#102183,#102184)),.UNSPECIFIED.,.F.,.F.,.F.,(4,4),(4,4),(0.522097120209639,
1.00286810177254),(0.0466073985929443,0.0531834925888932),.UNSPECIFIED.);
#3270=B_SPLINE_SURFACE_WITH_KNOTS('',3,3,((#102192,#102193,#102194,#102195),
(#102196,#102197,#102198,#102199),(#102200,#102201,#102202,#102203),(#102204,
#102205,#102206,#102207)),.UNSPECIFIED.,.F.,.F.,.F.,(4,4),(4,4),(-0.00286792598890457,
0.477902879790256),(0.0600156865494609,0.0665898698871165),
 .UNSPECIFIED.);
#3271=B_SPLINE_SURFACE_WITH_KNOTS('',3,3,((#102209,#102210,#102211,#102212),
(#102213,#102214,#102215,#102216),(#102217,#102218,#102219,#102220),(#102221,
#102222,#102223,#102224)),.UNSPECIFIED.,.F.,.F.,.F.,(4,4),(4,4),(0.522097120209762,
1.0028676439204),(0.0565997133101423,0.063172143088706),.UNSPECIFIED.);
#3272=B_SPLINE_SURFACE_WITH_KNOTS('',3,3,((#102240,#102241,#102242,#102243),
(#102244,#102245,#102246,#102247),(#102248,#102249,#102250,#102251),(#102252,
#102253,#102254,#102255)),.UNSPECIFIED.,.F.,.F.,.F.,(4,4),(4,4),(0.522097120208856,
1.00286833998579),(0.0665898698871195,0.0731716198748446),.UNSPECIFIED.);
#3273=B_SPLINE_SURFACE_WITH_KNOTS('',3,3,((#102256,#102257,#102258,#102259),
(#102260,#102261,#102262,#102263),(#102264,#102265,#102266,#102267),(#102268,
#102269,#102270,#102271)),.UNSPECIFIED.,.F.,.F.,.F.,(4,4),(4,4),(-0.00124731532103141,
0.209045111674401),(0.0700194292964963,0.0749900982976873),
 .UNSPECIFIED.);
#3274=B_SPLINE_SURFACE_WITH_KNOTS('',3,3,((#102278,#102279,#102280,#102281),
(#102282,#102283,#102284,#102285),(#102286,#102287,#102288,#102289),(#102290,
#102291,#102292,#102293)),.UNSPECIFIED.,.F.,.F.,.F.,(4,4),(4,4),(-0.00286791014392198,
0.477902879791072),(0.0100271466769366,0.0166015299239864),
 .UNSPECIFIED.);
#3275=B_SPLINE_SURFACE_WITH_KNOTS('',3,3,((#102295,#102296,#102297,#102298),
(#102299,#102300,#102301,#102302),(#102303,#102304,#102305,#102306),(#102307,
#102308,#102309,#102310)),.UNSPECIFIED.,.F.,.F.,.F.,(4,4),(4,4),(0.653230271505284,
1.00206901892634),(0.00656788395387369,0.0131849432430505),
 .UNSPECIFIED.);
#3276=B_SPLINE_SURFACE_WITH_KNOTS('',3,3,((#102318,#102319,#102320,#102321),
(#102322,#102323,#102324,#102325),(#102326,#102327,#102328,#102329),(#102330,
#102331,#102332,#102333)),.UNSPECIFIED.,.F.,.F.,.F.,(4,4),(4,4),(-0.00286780410477936,
0.477902879790937),(0.0200175229646911,0.0265907346180616),
 .UNSPECIFIED.);
#3277=B_SPLINE_SURFACE_WITH_KNOTS('',3,3,((#102335,#102336,#102337,#102338),
(#102339,#102340,#102341,#102342),(#102343,#102344,#102345,#102346),(#102347,
#102348,#102349,#102350)),.UNSPECIFIED.,.F.,.F.,.F.,(4,4),(4,4),(0.522097120209068,
1.00286753160119),(0.0166015299239897,0.0231736788075218),.UNSPECIFIED.);
#3278=B_SPLINE_SURFACE_WITH_KNOTS('',3,3,((#102352,#102353,#102354,#102355),
(#102356,#102357,#102358,#102359),(#102360,#102361,#102362,#102363),(#102364,
#102365,#102366,#102367)),.UNSPECIFIED.,.F.,.F.,.F.,(4,4),(4,4),(0.,1.0060000396133),
(0.016601529923988,0.026590734618064),.UNSPECIFIED.);
#3279=B_SPLINE_SURFACE_WITH_KNOTS('',3,3,((#102368,#102369,#102370,#102371),
(#102372,#102373,#102374,#102375),(#102376,#102377,#102378,#102379),(#102380,
#102381,#102382,#102383)),.UNSPECIFIED.,.F.,.F.,.F.,(4,4),(4,4),(-0.00286862201155799,
0.477902879792543),(0.030009453229278,0.0365944846647016),.UNSPECIFIED.);
#3280=B_SPLINE_SURFACE_WITH_KNOTS('',3,3,((#102385,#102386,#102387,#102388),
(#102389,#102390,#102391,#102392),(#102393,#102394,#102395,#102396),(#102397,
#102398,#102399,#102400)),.UNSPECIFIED.,.F.,.F.,.F.,(4,4),(4,4),(0.522097120209334,
1.0028682366929),(0.0265907346180635,0.0331702036051743),.UNSPECIFIED.);
#3281=B_SPLINE_SURFACE_WITH_KNOTS('',3,3,((#102408,#102409,#102410,#102411),
(#102412,#102413,#102414,#102415),(#102416,#102417,#102418,#102419),(#102420,
#102421,#102422,#102423)),.UNSPECIFIED.,.F.,.F.,.F.,(4,4),(4,4),(-0.00286848453275135,
0.47790287979121),(0.0400218729466611,0.046607398592943),.UNSPECIFIED.);
#3282=B_SPLINE_SURFACE_WITH_KNOTS('',3,3,((#102440,#102441,#102442,#102443),
(#102444,#102445,#102446,#102447),(#102448,#102449,#102450,#102451),(#102452,
#102453,#102454,#102455)),.UNSPECIFIED.,.F.,.F.,.F.,(4,4),(4,4),(0.,1.00600014639758),
(0.0365944846645051,0.0466073985929177),.UNSPECIFIED.);
#3283=B_SPLINE_SURFACE_WITH_KNOTS('',3,3,((#102456,#102457,#102458,#102459),
(#102460,#102461,#102462,#102463),(#102464,#102465,#102466,#102467),(#102468,
#102469,#102470,#102471)),.UNSPECIFIED.,.F.,.F.,.F.,(4,4),(4,4),(-0.0028678012240823,
0.477902879790518),(0.0500263550859009,0.0565997133101415),
 .UNSPECIFIED.);
#3284=B_SPLINE_SURFACE_WITH_KNOTS('',3,3,((#102473,#102474,#102475,#102476),
(#102477,#102478,#102479,#102480),(#102481,#102482,#102483,#102484),(#102485,
#102486,#102487,#102488)),.UNSPECIFIED.,.F.,.F.,.F.,(4,4),(4,4),(0.522097120209443,
1.00286810177263),(0.0466073985929449,0.0531834925888939),.UNSPECIFIED.);
#3285=B_SPLINE_SURFACE_WITH_KNOTS('',3,3,((#102496,#102497,#102498,#102499),
(#102500,#102501,#102502,#102503),(#102504,#102505,#102506,#102507),(#102508,
#102509,#102510,#102511)),.UNSPECIFIED.,.F.,.F.,.F.,(4,4),(4,4),(-0.00286792598893081,
0.477902879790381),(0.0600156865494602,0.0665898698871173),
 .UNSPECIFIED.);
#3286=B_SPLINE_SURFACE_WITH_KNOTS('',3,3,((#102513,#102514,#102515,#102516),
(#102517,#102518,#102519,#102520),(#102521,#102522,#102523,#102524),(#102525,
#102526,#102527,#102528)),.UNSPECIFIED.,.F.,.F.,.F.,(4,4),(4,4),(0.522097120209564,
1.00286764392037),(0.0565997133101422,0.0631721430887063),.UNSPECIFIED.);
#3287=B_SPLINE_SURFACE_WITH_KNOTS('',3,3,((#102544,#102545,#102546,#102547),
(#102548,#102549,#102550,#102551),(#102552,#102553,#102554,#102555),(#102556,
#102557,#102558,#102559)),.UNSPECIFIED.,.F.,.F.,.F.,(4,4),(4,4),(0.522097120208792,
1.0028683399858),(0.0665898698871198,0.0731716198748449),.UNSPECIFIED.);
#3288=B_SPLINE_SURFACE_WITH_KNOTS('',3,3,((#102560,#102561,#102562,#102563),
(#102564,#102565,#102566,#102567),(#102568,#102569,#102570,#102571),(#102572,
#102573,#102574,#102575)),.UNSPECIFIED.,.F.,.F.,.F.,(4,4),(4,4),(-0.00124731532103917,
0.209045111676822),(0.0700194292964934,0.0749900982976999),
 .UNSPECIFIED.);
#3289=B_SPLINE_SURFACE_WITH_KNOTS('',3,3,((#102582,#102583,#102584,#102585),
(#102586,#102587,#102588,#102589),(#102590,#102591,#102592,#102593),(#102594,
#102595,#102596,#102597)),.UNSPECIFIED.,.F.,.F.,.F.,(4,4),(4,4),(-0.00286791014392413,
0.477902879791187),(0.0100271466769363,0.0166015299239868),
 .UNSPECIFIED.);
#3290=B_SPLINE_SURFACE_WITH_KNOTS('',3,3,((#102599,#102600,#102601,#102602),
(#102603,#102604,#102605,#102606),(#102607,#102608,#102609,#102610),(#102611,
#102612,#102613,#102614)),.UNSPECIFIED.,.F.,.F.,.F.,(4,4),(4,4),(0.653230271504036,
1.00206901892632),(0.0065678839538812,0.0131849432430442),.UNSPECIFIED.);
#3291=B_SPLINE_SURFACE_WITH_KNOTS('',3,3,((#102622,#102623,#102624,#102625),
(#102626,#102627,#102628,#102629),(#102630,#102631,#102632,#102633),(#102634,
#102635,#102636,#102637)),.UNSPECIFIED.,.F.,.F.,.F.,(4,4),(4,4),(-0.0028678041048232,
0.477902879791045),(0.0200175229646908,0.0265907346180622),
 .UNSPECIFIED.);
#3292=B_SPLINE_SURFACE_WITH_KNOTS('',3,3,((#102639,#102640,#102641,#102642),
(#102643,#102644,#102645,#102646),(#102647,#102648,#102649,#102650),(#102651,
#102652,#102653,#102654)),.UNSPECIFIED.,.F.,.F.,.F.,(4,4),(4,4),(0.522097120208956,
1.00286753160116),(0.0166015299239884,0.0231736788037111),.UNSPECIFIED.);
#3293=B_SPLINE_SURFACE_WITH_KNOTS('',3,3,((#102656,#102657,#102658,#102659),
(#102660,#102661,#102662,#102663),(#102664,#102665,#102666,#102667),(#102668,
#102669,#102670,#102671)),.UNSPECIFIED.,.F.,.F.,.F.,(4,4),(4,4),(0.,1.00600003961301),
(0.0166015299239882,0.0265907346180623),.UNSPECIFIED.);
#3294=B_SPLINE_SURFACE_WITH_KNOTS('',3,3,((#102672,#102673,#102674,#102675),
(#102676,#102677,#102678,#102679),(#102680,#102681,#102682,#102683),(#102684,
#102685,#102686,#102687)),.UNSPECIFIED.,.F.,.F.,.F.,(4,4),(4,4),(-0.00286862201159097,
0.477902879792634),(0.0300094532292799,0.0365944846647021),
 .UNSPECIFIED.);
#3295=B_SPLINE_SURFACE_WITH_KNOTS('',3,3,((#102689,#102690,#102691,#102692),
(#102693,#102694,#102695,#102696),(#102697,#102698,#102699,#102700),(#102701,
#102702,#102703,#102704)),.UNSPECIFIED.,.F.,.F.,.F.,(4,4),(4,4),(0.522097120209135,
1.00286823669292),(0.026590734618064,0.0331702036622762),.UNSPECIFIED.);
#3296=B_SPLINE_SURFACE_WITH_KNOTS('',3,3,((#102712,#102713,#102714,#102715),
(#102716,#102717,#102718,#102719),(#102720,#102721,#102722,#102723),(#102724,
#102725,#102726,#102727)),.UNSPECIFIED.,.F.,.F.,.F.,(4,4),(4,4),(-0.00286848453271382,
0.477902879791247),(0.0400218729466601,0.0466073985929429),
 .UNSPECIFIED.);
#3297=B_SPLINE_SURFACE_WITH_KNOTS('',3,3,((#102744,#102745,#102746,#102747),
(#102748,#102749,#102750,#102751),(#102752,#102753,#102754,#102755),(#102756,
#102757,#102758,#102759)),.UNSPECIFIED.,.F.,.F.,.F.,(4,4),(4,4),(0.,1.00600014639707),
(0.0365944846645049,0.0466073985929167),.UNSPECIFIED.);
#3298=B_SPLINE_SURFACE_WITH_KNOTS('',3,3,((#102760,#102761,#102762,#102763),
(#102764,#102765,#102766,#102767),(#102768,#102769,#102770,#102771),(#102772,
#102773,#102774,#102775)),.UNSPECIFIED.,.F.,.F.,.F.,(4,4),(4,4),(-0.00286780122400802,
0.477902879790596),(0.0500263550859,0.0565997133101411),.UNSPECIFIED.);
#3299=B_SPLINE_SURFACE_WITH_KNOTS('',3,3,((#102777,#102778,#102779,#102780),
(#102781,#102782,#102783,#102784),(#102785,#102786,#102787,#102788),(#102789,
#102790,#102791,#102792)),.UNSPECIFIED.,.F.,.F.,.F.,(4,4),(4,4),(0.522097120209334,
1.00286810177245),(0.0466073985929444,0.0531834922865668),.UNSPECIFIED.);
#3300=B_SPLINE_SURFACE_WITH_KNOTS('',3,3,((#102800,#102801,#102802,#102803),
(#102804,#102805,#102806,#102807),(#102808,#102809,#102810,#102811),(#102812,
#102813,#102814,#102815)),.UNSPECIFIED.,.F.,.F.,.F.,(4,4),(4,4),(-0.00286792598892004,
0.477902879790578),(0.0600156865494608,0.0665898698871175),
 .UNSPECIFIED.);
#3301=B_SPLINE_SURFACE_WITH_KNOTS('',3,3,((#102817,#102818,#102819,#102820),
(#102821,#102822,#102823,#102824),(#102825,#102826,#102827,#102828),(#102829,
#102830,#102831,#102832)),.UNSPECIFIED.,.F.,.F.,.F.,(4,4),(4,4),(0.522097120209435,
1.00286764392035),(0.0565997133101424,0.0631721430887057),.UNSPECIFIED.);
#3302=B_SPLINE_SURFACE_WITH_KNOTS('',3,3,((#102848,#102849,#102850,#102851),
(#102852,#102853,#102854,#102855),(#102856,#102857,#102858,#102859),(#102860,
#102861,#102862,#102863)),.UNSPECIFIED.,.F.,.F.,.F.,(4,4),(4,4),(0.522097120208655,
1.00286833998586),(0.0665898698871185,0.073171619874845),.UNSPECIFIED.);
#3303=B_SPLINE_SURFACE_WITH_KNOTS('',3,3,((#102864,#102865,#102866,#102867),
(#102868,#102869,#102870,#102871),(#102872,#102873,#102874,#102875),(#102876,
#102877,#102878,#102879)),.UNSPECIFIED.,.F.,.F.,.F.,(4,4),(4,4),(-0.00124731532105724,
0.209045111679254),(0.0700194292964913,0.0749900982977112),
 .UNSPECIFIED.);
#3304=B_SPLINE_SURFACE_WITH_KNOTS('',3,3,((#102886,#102887,#102888,#102889),
(#102890,#102891,#102892,#102893),(#102894,#102895,#102896,#102897),(#102898,
#102899,#102900,#102901)),.UNSPECIFIED.,.F.,.F.,.F.,(4,4),(4,4),(-0.0028679101439003,
0.477902879791482),(0.0100271466769351,0.0166015299239872),
 .UNSPECIFIED.);
#3305=B_SPLINE_SURFACE_WITH_KNOTS('',3,3,((#102903,#102904,#102905,#102906),
(#102907,#102908,#102909,#102910),(#102911,#102912,#102913,#102914),(#102915,
#102916,#102917,#102918)),.UNSPECIFIED.,.F.,.F.,.F.,(4,4),(4,4),(0.653230271502744,
1.00206901892634),(0.00656788395388827,0.0131849432430387),
 .UNSPECIFIED.);
#3306=B_SPLINE_SURFACE_WITH_KNOTS('',3,3,((#102926,#102927,#102928,#102929),
(#102930,#102931,#102932,#102933),(#102934,#102935,#102936,#102937),(#102938,
#102939,#102940,#102941)),.UNSPECIFIED.,.F.,.F.,.F.,(4,4),(4,4),(-0.00286780410472799,
0.477902879791192),(0.0200175229646904,0.0265907346180625),
 .UNSPECIFIED.);
#3307=B_SPLINE_SURFACE_WITH_KNOTS('',3,3,((#102943,#102944,#102945,#102946),
(#102947,#102948,#102949,#102950),(#102951,#102952,#102953,#102954),(#102955,
#102956,#102957,#102958)),.UNSPECIFIED.,.F.,.F.,.F.,(4,4),(4,4),(0.522097120208858,
1.00286753160116),(0.0166015299239879,0.0231736787930316),.UNSPECIFIED.);
#3308=B_SPLINE_SURFACE_WITH_KNOTS('',3,3,((#102960,#102961,#102962,#102963),
(#102964,#102965,#102966,#102967),(#102968,#102969,#102970,#102971),(#102972,
#102973,#102974,#102975)),.UNSPECIFIED.,.F.,.F.,.F.,(4,4),(4,4),(0.,1.00600003961341),
(0.0166015299239869,0.0265907346180636),.UNSPECIFIED.);
#3309=B_SPLINE_SURFACE_WITH_KNOTS('',3,3,((#102976,#102977,#102978,#102979),
(#102980,#102981,#102982,#102983),(#102984,#102985,#102986,#102987),(#102988,
#102989,#102990,#102991)),.UNSPECIFIED.,.F.,.F.,.F.,(4,4),(4,4),(-0.00286862201145934,
0.47790287979285),(0.0300094532292789,0.0365944846647005),.UNSPECIFIED.);
#3310=B_SPLINE_SURFACE_WITH_KNOTS('',3,3,((#102993,#102994,#102995,#102996),
(#102997,#102998,#102999,#103000),(#103001,#103002,#103003,#103004),(#103005,
#103006,#103007,#103008)),.UNSPECIFIED.,.F.,.F.,.F.,(4,4),(4,4),(0.52209712020909,
1.00286823669299),(0.0265907346180636,0.0331702036889924),.UNSPECIFIED.);
#3311=B_SPLINE_SURFACE_WITH_KNOTS('',3,3,((#103016,#103017,#103018,#103019),
(#103020,#103021,#103022,#103023),(#103024,#103025,#103026,#103027),(#103028,
#103029,#103030,#103031)),.UNSPECIFIED.,.F.,.F.,.F.,(4,4),(4,4),(-0.00286848453269722,
0.477902879791497),(0.0400218729466593,0.0466073985929421),
 .UNSPECIFIED.);
#3312=B_SPLINE_SURFACE_WITH_KNOTS('',3,3,((#103048,#103049,#103050,#103051),
(#103052,#103053,#103054,#103055),(#103056,#103057,#103058,#103059),(#103060,
#103061,#103062,#103063)),.UNSPECIFIED.,.F.,.F.,.F.,(4,4),(4,4),(0.,1.00600014639748),
(0.0365944846645053,0.0466073985929157),.UNSPECIFIED.);
#3313=B_SPLINE_SURFACE_WITH_KNOTS('',3,3,((#103064,#103065,#103066,#103067),
(#103068,#103069,#103070,#103071),(#103072,#103073,#103074,#103075),(#103076,
#103077,#103078,#103079)),.UNSPECIFIED.,.F.,.F.,.F.,(4,4),(4,4),(-0.00286780122401915,
0.477902879790796),(0.0500263550858998,0.0565997133101412),
 .UNSPECIFIED.);
#3314=B_SPLINE_SURFACE_WITH_KNOTS('',3,3,((#103081,#103082,#103083,#103084),
(#103085,#103086,#103087,#103088),(#103089,#103090,#103091,#103092),(#103093,
#103094,#103095,#103096)),.UNSPECIFIED.,.F.,.F.,.F.,(4,4),(4,4),(0.522097120209233,
1.0028681017726),(0.0466073985929452,0.0531834925888933),.UNSPECIFIED.);
#3315=B_SPLINE_SURFACE_WITH_KNOTS('',3,3,((#103104,#103105,#103106,#103107),
(#103108,#103109,#103110,#103111),(#103112,#103113,#103114,#103115),(#103116,
#103117,#103118,#103119)),.UNSPECIFIED.,.F.,.F.,.F.,(4,4),(4,4),(-0.0028679259889033,
0.477902879790691),(0.0600156865494593,0.0665898698871172),
 .UNSPECIFIED.);
#3316=B_SPLINE_SURFACE_WITH_KNOTS('',3,3,((#103121,#103122,#103123,#103124),
(#103125,#103126,#103127,#103128),(#103129,#103130,#103131,#103132),(#103133,
#103134,#103135,#103136)),.UNSPECIFIED.,.F.,.F.,.F.,(4,4),(4,4),(0.522097120209315,
1.00286764392042),(0.0565997133101412,0.0631721430887057),.UNSPECIFIED.);
#3317=B_SPLINE_SURFACE_WITH_KNOTS('',3,3,((#103152,#103153,#103154,#103155),
(#103156,#103157,#103158,#103159),(#103160,#103161,#103162,#103163),(#103164,
#103165,#103166,#103167)),.UNSPECIFIED.,.F.,.F.,.F.,(4,4),(4,4),(0.522097120208528,
1.00286833998594),(0.0665898698871192,0.0731716198748449),.UNSPECIFIED.);
#3318=B_SPLINE_SURFACE_WITH_KNOTS('',3,3,((#103168,#103169,#103170,#103171),
(#103172,#103173,#103174,#103175),(#103176,#103177,#103178,#103179),(#103180,
#103181,#103182,#103183)),.UNSPECIFIED.,.F.,.F.,.F.,(4,4),(4,4),(-0.00124731532975596,
0.209045111681729),(0.0700194292964918,0.0749900982977222),
 .UNSPECIFIED.);
#3319=B_SPLINE_SURFACE_WITH_KNOTS('',3,3,((#103190,#103191,#103192,#103193),
(#103194,#103195,#103196,#103197),(#103198,#103199,#103200,#103201),(#103202,
#103203,#103204,#103205)),.UNSPECIFIED.,.F.,.F.,.F.,(4,4),(4,4),(-0.00286791014389224,
0.477902879791565),(0.0100271466769338,0.0166015299239867),
 .UNSPECIFIED.);
#3320=B_SPLINE_SURFACE_WITH_KNOTS('',3,3,((#103207,#103208,#103209,#103210),
(#103211,#103212,#103213,#103214),(#103215,#103216,#103217,#103218),(#103219,
#103220,#103221,#103222)),.UNSPECIFIED.,.F.,.F.,.F.,(4,4),(4,4),(0.653230271501317,
1.00206901893493),(0.00656788395389535,0.0131849432430301),
 .UNSPECIFIED.);
#3321=B_SPLINE_SURFACE_WITH_KNOTS('',3,3,((#103230,#103231,#103232,#103233),
(#103234,#103235,#103236,#103237),(#103238,#103239,#103240,#103241),(#103242,
#103243,#103244,#103245)),.UNSPECIFIED.,.F.,.F.,.F.,(4,4),(4,4),(-0.00286780410465671,
0.477902879791354),(0.0200175229646905,0.0265907346180625),
 .UNSPECIFIED.);
#3322=B_SPLINE_SURFACE_WITH_KNOTS('',3,3,((#103247,#103248,#103249,#103250),
(#103251,#103252,#103253,#103254),(#103255,#103256,#103257,#103258),(#103259,
#103260,#103261,#103262)),.UNSPECIFIED.,.F.,.F.,.F.,(4,4),(4,4),(0.522097120208694,
1.00286753160118),(0.0166015299239879,0.023173678803712),.UNSPECIFIED.);
#3323=B_SPLINE_SURFACE_WITH_KNOTS('',3,3,((#103264,#103265,#103266,#103267),
(#103268,#103269,#103270,#103271),(#103272,#103273,#103274,#103275),(#103276,
#103277,#103278,#103279)),.UNSPECIFIED.,.F.,.F.,.F.,(4,4),(4,4),(0.,1.00600003961334),
(0.0166015299239903,0.0265907346180631),.UNSPECIFIED.);
#3324=B_SPLINE_SURFACE_WITH_KNOTS('',3,3,((#103280,#103281,#103282,#103283),
(#103284,#103285,#103286,#103287),(#103288,#103289,#103290,#103291),(#103292,
#103293,#103294,#103295)),.UNSPECIFIED.,.F.,.F.,.F.,(4,4),(4,4),(-0.00286862201163387,
0.477902879792968),(0.0300094532292794,0.0365944846647019),
 .UNSPECIFIED.);
#3325=B_SPLINE_SURFACE_WITH_KNOTS('',3,3,((#103297,#103298,#103299,#103300),
(#103301,#103302,#103303,#103304),(#103305,#103306,#103307,#103308),(#103309,
#103310,#103311,#103312)),.UNSPECIFIED.,.F.,.F.,.F.,(4,4),(4,4),(0.522097120208964,
1.00286823669293),(0.0265907346180636,0.0331702036889924),.UNSPECIFIED.);
#3326=B_SPLINE_SURFACE_WITH_KNOTS('',3,3,((#103320,#103321,#103322,#103323),
(#103324,#103325,#103326,#103327),(#103328,#103329,#103330,#103331),(#103332,
#103333,#103334,#103335)),.UNSPECIFIED.,.F.,.F.,.F.,(4,4),(4,4),(-0.00286848453307101,
0.477902879860464),(0.0400218729466602,0.0466073985929437),
 .UNSPECIFIED.);
#3327=B_SPLINE_SURFACE_WITH_KNOTS('',3,3,((#103352,#103353,#103354,#103355),
(#103356,#103357,#103358,#103359),(#103360,#103361,#103362,#103363),(#103364,
#103365,#103366,#103367)),.UNSPECIFIED.,.F.,.F.,.F.,(4,4),(4,4),(0.,1.0060001463973),
(0.036594484664504,0.0466073985929155),.UNSPECIFIED.);
#3328=B_SPLINE_SURFACE_WITH_KNOTS('',3,3,((#103368,#103369,#103370,#103371),
(#103372,#103373,#103374,#103375),(#103376,#103377,#103378,#103379),(#103380,
#103381,#103382,#103383)),.UNSPECIFIED.,.F.,.F.,.F.,(4,4),(4,4),(-0.0028678012239562,
0.477902879790876),(0.0500263550859004,0.0565997133101407),
 .UNSPECIFIED.);
#3329=B_SPLINE_SURFACE_WITH_KNOTS('',3,3,((#103385,#103386,#103387,#103388),
(#103389,#103390,#103391,#103392),(#103393,#103394,#103395,#103396),(#103397,
#103398,#103399,#103400)),.UNSPECIFIED.,.F.,.F.,.F.,(4,4),(4,4),(0.522097120209067,
1.00286810177257),(0.0466073985929454,0.0531834925888929),.UNSPECIFIED.);
#3330=B_SPLINE_SURFACE_WITH_KNOTS('',3,3,((#103408,#103409,#103410,#103411),
(#103412,#103413,#103414,#103415),(#103416,#103417,#103418,#103419),(#103420,
#103421,#103422,#103423)),.UNSPECIFIED.,.F.,.F.,.F.,(4,4),(4,4),(-0.00286792598887741,
0.477902879790768),(0.0600156865494596,0.0665898698871164),
 .UNSPECIFIED.);
#3331=B_SPLINE_SURFACE_WITH_KNOTS('',3,3,((#103425,#103426,#103427,#103428),
(#103429,#103430,#103431,#103432),(#103433,#103434,#103435,#103436),(#103437,
#103438,#103439,#103440)),.UNSPECIFIED.,.F.,.F.,.F.,(4,4),(4,4),(0.522097120209252,
1.00286764392032),(0.0565997133101418,0.063172143088706),.UNSPECIFIED.);
#3332=B_SPLINE_SURFACE_WITH_KNOTS('',3,3,((#103456,#103457,#103458,#103459),
(#103460,#103461,#103462,#103463),(#103464,#103465,#103466,#103467),(#103468,
#103469,#103470,#103471)),.UNSPECIFIED.,.F.,.F.,.F.,(4,4),(4,4),(0.522097120208404,
1.00286833998587),(0.0665898698871185,0.0731716198748446),.UNSPECIFIED.);
#3333=B_SPLINE_SURFACE_WITH_KNOTS('',3,3,((#103472,#103473,#103474,#103475),
(#103476,#103477,#103478,#103479),(#103480,#103481,#103482,#103483),(#103484,
#103485,#103486,#103487)),.UNSPECIFIED.,.F.,.F.,.F.,(4,4),(4,4),(-0.00124731532721796,
0.209045111684327),(0.0700194292964934,0.0749900982977344),
 .UNSPECIFIED.);
#3334=B_SPLINE_SURFACE_WITH_KNOTS('',3,3,((#103494,#103495,#103496,#103497),
(#103498,#103499,#103500,#103501),(#103502,#103503,#103504,#103505),(#103506,
#103507,#103508,#103509)),.UNSPECIFIED.,.F.,.F.,.F.,(4,4),(4,4),(-0.00286791014387768,
0.477902879791954),(0.0100271466769349,0.0166015299239877),
 .UNSPECIFIED.);
#3335=B_SPLINE_SURFACE_WITH_KNOTS('',3,3,((#103511,#103512,#103513,#103514),
(#103515,#103516,#103517,#103518),(#103519,#103520,#103521,#103522),(#103523,
#103524,#103525,#103526)),.UNSPECIFIED.,.F.,.F.,.F.,(4,4),(4,4),(0.653230271499819,
1.00206901893299),(0.00656788395390347,0.0131849432430213),
 .UNSPECIFIED.);
#3336=B_SPLINE_SURFACE_WITH_KNOTS('',3,3,((#103534,#103535,#103536,#103537),
(#103538,#103539,#103540,#103541),(#103542,#103543,#103544,#103545),(#103546,
#103547,#103548,#103549)),.UNSPECIFIED.,.F.,.F.,.F.,(4,4),(4,4),(-0.00286780410469178,
0.47790287979141),(0.0200175229646905,0.0265907346180624),.UNSPECIFIED.);
#3337=B_SPLINE_SURFACE_WITH_KNOTS('',3,3,((#103551,#103552,#103553,#103554),
(#103555,#103556,#103557,#103558),(#103559,#103560,#103561,#103562),(#103563,
#103564,#103565,#103566)),.UNSPECIFIED.,.F.,.F.,.F.,(4,4),(4,4),(0.5220971202086,
1.00286753160118),(0.0166015299239897,0.0231736788075225),.UNSPECIFIED.);
#3338=B_SPLINE_SURFACE_WITH_KNOTS('',3,3,((#103568,#103569,#103570,#103571),
(#103572,#103573,#103574,#103575),(#103576,#103577,#103578,#103579),(#103580,
#103581,#103582,#103583)),.UNSPECIFIED.,.F.,.F.,.F.,(4,4),(4,4),(0.,1.00600003961332),
(0.0166015299239879,0.026590734618066),.UNSPECIFIED.);
#3339=B_SPLINE_SURFACE_WITH_KNOTS('',3,3,((#103584,#103585,#103586,#103587),
(#103588,#103589,#103590,#103591),(#103592,#103593,#103594,#103595),(#103596,
#103597,#103598,#103599)),.UNSPECIFIED.,.F.,.F.,.F.,(4,4),(4,4),(-0.0028686220116214,
0.477902879792963),(0.030009453229279,0.036594484664717),.UNSPECIFIED.);
#3340=B_SPLINE_SURFACE_WITH_KNOTS('',3,3,((#103601,#103602,#103603,#103604),
(#103605,#103606,#103607,#103608),(#103609,#103610,#103611,#103612),(#103613,
#103614,#103615,#103616)),.UNSPECIFIED.,.F.,.F.,.F.,(4,4),(4,4),(0.522097120208826,
1.00286823669297),(0.0265907346180652,0.033170203688994),.UNSPECIFIED.);
#3341=B_SPLINE_SURFACE_WITH_KNOTS('',3,3,((#103624,#103625,#103626,#103627),
(#103628,#103629,#103630,#103631),(#103632,#103633,#103634,#103635),(#103636,
#103637,#103638,#103639)),.UNSPECIFIED.,.F.,.F.,.F.,(4,4),(4,4),(-0.00286848453262961,
0.477902879791565),(0.0400218729466602,0.046607398592943),.UNSPECIFIED.);
#3342=B_SPLINE_SURFACE_WITH_KNOTS('',3,3,((#103656,#103657,#103658,#103659),
(#103660,#103661,#103662,#103663),(#103664,#103665,#103666,#103667),(#103668,
#103669,#103670,#103671)),.UNSPECIFIED.,.F.,.F.,.F.,(4,4),(4,4),(0.,1.00600014639743),
(0.0365944846645039,0.0466073985929177),.UNSPECIFIED.);
#3343=B_SPLINE_SURFACE_WITH_KNOTS('',3,3,((#103672,#103673,#103674,#103675),
(#103676,#103677,#103678,#103679),(#103680,#103681,#103682,#103683),(#103684,
#103685,#103686,#103687)),.UNSPECIFIED.,.F.,.F.,.F.,(4,4),(4,4),(-0.00286780122392134,
0.477902879790918),(0.0500263550859004,0.0565997133101405),
 .UNSPECIFIED.);
#3344=B_SPLINE_SURFACE_WITH_KNOTS('',3,3,((#103689,#103690,#103691,#103692),
(#103693,#103694,#103695,#103696),(#103697,#103698,#103699,#103700),(#103701,
#103702,#103703,#103704)),.UNSPECIFIED.,.F.,.F.,.F.,(4,4),(4,4),(0.522097120208999,
1.00286810177259),(0.0466073985929454,0.0531834925888925),.UNSPECIFIED.);
#3345=B_SPLINE_SURFACE_WITH_KNOTS('',3,3,((#103712,#103713,#103714,#103715),
(#103716,#103717,#103718,#103719),(#103720,#103721,#103722,#103723),(#103724,
#103725,#103726,#103727)),.UNSPECIFIED.,.F.,.F.,.F.,(4,4),(4,4),(-0.00286792598891528,
0.477902879790847),(0.0600156865494608,0.0665898698871163),
 .UNSPECIFIED.);
#3346=B_SPLINE_SURFACE_WITH_KNOTS('',3,3,((#103729,#103730,#103731,#103732),
(#103733,#103734,#103735,#103736),(#103737,#103738,#103739,#103740),(#103741,
#103742,#103743,#103744)),.UNSPECIFIED.,.F.,.F.,.F.,(4,4),(4,4),(0.52209712020907,
1.00286764392035),(0.0565997133101428,0.063172143088705),.UNSPECIFIED.);
#3347=B_SPLINE_SURFACE_WITH_KNOTS('',3,3,((#103760,#103761,#103762,#103763),
(#103764,#103765,#103766,#103767),(#103768,#103769,#103770,#103771),(#103772,
#103773,#103774,#103775)),.UNSPECIFIED.,.F.,.F.,.F.,(4,4),(4,4),(0.522097120208342,
1.00286833998585),(0.06658986988712,0.0731716198748447),.UNSPECIFIED.);
#3348=B_SPLINE_SURFACE_WITH_KNOTS('',3,3,((#103776,#103777,#103778,#103779),
(#103780,#103781,#103782,#103783),(#103784,#103785,#103786,#103787),(#103788,
#103789,#103790,#103791)),.UNSPECIFIED.,.F.,.F.,.F.,(4,4),(4,4),(-0.00124731532471121,
0.209045111686916),(0.0700194292964978,0.0749900982977462),
 .UNSPECIFIED.);
#3349=B_SPLINE_SURFACE_WITH_KNOTS('',3,3,((#103798,#103799,#103800,#103801),
(#103802,#103803,#103804,#103805),(#103806,#103807,#103808,#103809),(#103810,
#103811,#103812,#103813)),.UNSPECIFIED.,.F.,.F.,.F.,(4,4),(4,4),(-0.00286791014388252,
0.477902879794285),(0.0100271466769349,0.0166015299239876),
 .UNSPECIFIED.);
#3350=B_SPLINE_SURFACE_WITH_KNOTS('',3,3,((#103815,#103816,#103817,#103818),
(#103819,#103820,#103821,#103822),(#103823,#103824,#103825,#103826),(#103827,
#103828,#103829,#103830)),.UNSPECIFIED.,.F.,.F.,.F.,(4,4),(4,4),(0.653230271498285,
1.0020690189308),(0.00656788395390921,0.013184943243012),.UNSPECIFIED.);
#3351=B_SPLINE_SURFACE_WITH_KNOTS('',3,3,((#103838,#103839,#103840,#103841),
(#103842,#103843,#103844,#103845),(#103846,#103847,#103848,#103849),(#103850,
#103851,#103852,#103853)),.UNSPECIFIED.,.F.,.F.,.F.,(4,4),(4,4),(-0.00286780410476033,
0.477902879793274),(0.0200175229646903,0.0265907346180623),
 .UNSPECIFIED.);
#3352=B_SPLINE_SURFACE_WITH_KNOTS('',3,3,((#103855,#103856,#103857,#103858),
(#103859,#103860,#103861,#103862),(#103863,#103864,#103865,#103866),(#103867,
#103868,#103869,#103870)),.UNSPECIFIED.,.F.,.F.,.F.,(4,4),(4,4),(0.522097120208445,
1.00286753160117),(0.0166015299239883,0.0231736788075214),.UNSPECIFIED.);
#3353=B_SPLINE_SURFACE_WITH_KNOTS('',3,3,((#103872,#103873,#103874,#103875),
(#103876,#103877,#103878,#103879),(#103880,#103881,#103882,#103883),(#103884,
#103885,#103886,#103887)),.UNSPECIFIED.,.F.,.F.,.F.,(4,4),(4,4),(0.,1.00600003961389),
(0.0166015299239904,0.0265907346180634),.UNSPECIFIED.);
#3354=B_SPLINE_SURFACE_WITH_KNOTS('',3,3,((#103888,#103889,#103890,#103891),
(#103892,#103893,#103894,#103895),(#103896,#103897,#103898,#103899),(#103900,
#103901,#103902,#103903)),.UNSPECIFIED.,.F.,.F.,.F.,(4,4),(4,4),(-0.00286862201160333,
0.477902879793387),(0.030009453229279,0.0365944846647018),.UNSPECIFIED.);
#3355=B_SPLINE_SURFACE_WITH_KNOTS('',3,3,((#103905,#103906,#103907,#103908),
(#103909,#103910,#103911,#103912),(#103913,#103914,#103915,#103916),(#103917,
#103918,#103919,#103920)),.UNSPECIFIED.,.F.,.F.,.F.,(4,4),(4,4),(0.522097120208658,
1.00286823669293),(0.0265907346180631,0.0331702036889929),.UNSPECIFIED.);
#3356=B_SPLINE_SURFACE_WITH_KNOTS('',3,3,((#103928,#103929,#103930,#103931),
(#103932,#103933,#103934,#103935),(#103936,#103937,#103938,#103939),(#103940,
#103941,#103942,#103943)),.UNSPECIFIED.,.F.,.F.,.F.,(4,4),(4,4),(-0.00286848453260555,
0.477902879791857),(0.0400218729466597,0.0466073985929431),
 .UNSPECIFIED.);
#3357=B_SPLINE_SURFACE_WITH_KNOTS('',3,3,((#103960,#103961,#103962,#103963),
(#103964,#103965,#103966,#103967),(#103968,#103969,#103970,#103971),(#103972,
#103973,#103974,#103975)),.UNSPECIFIED.,.F.,.F.,.F.,(4,4),(4,4),(0.,1.00600014639731),
(0.0365944846645024,0.0466073985929167),.UNSPECIFIED.);
#3358=B_SPLINE_SURFACE_WITH_KNOTS('',3,3,((#103976,#103977,#103978,#103979),
(#103980,#103981,#103982,#103983),(#103984,#103985,#103986,#103987),(#103988,
#103989,#103990,#103991)),.UNSPECIFIED.,.F.,.F.,.F.,(4,4),(4,4),(-0.00286780122392774,
0.477902879791221),(0.0500263550859004,0.0565997133101403),
 .UNSPECIFIED.);
#3359=B_SPLINE_SURFACE_WITH_KNOTS('',3,3,((#103993,#103994,#103995,#103996),
(#103997,#103998,#103999,#104000),(#104001,#104002,#104003,#104004),(#104005,
#104006,#104007,#104008)),.UNSPECIFIED.,.F.,.F.,.F.,(4,4),(4,4),(0.522097120208844,
1.0028681017726),(0.0466073985929452,0.0531834925888928),.UNSPECIFIED.);
#3360=B_SPLINE_SURFACE_WITH_KNOTS('',3,3,((#104016,#104017,#104018,#104019),
(#104020,#104021,#104022,#104023),(#104024,#104025,#104026,#104027),(#104028,
#104029,#104030,#104031)),.UNSPECIFIED.,.F.,.F.,.F.,(4,4),(4,4),(-0.00286792598900819,
0.47790287979099),(0.0600156865494602,0.0665898698871176),.UNSPECIFIED.);
#3361=B_SPLINE_SURFACE_WITH_KNOTS('',3,3,((#104033,#104034,#104035,#104036),
(#104037,#104038,#104039,#104040),(#104041,#104042,#104043,#104044),(#104045,
#104046,#104047,#104048)),.UNSPECIFIED.,.F.,.F.,.F.,(4,4),(4,4),(0.522097120208971,
1.00286764392034),(0.0565997133101411,0.0631721430887057),.UNSPECIFIED.);
#3362=B_SPLINE_SURFACE_WITH_KNOTS('',3,3,((#104064,#104065,#104066,#104067),
(#104068,#104069,#104070,#104071),(#104072,#104073,#104074,#104075),(#104076,
#104077,#104078,#104079)),.UNSPECIFIED.,.F.,.F.,.F.,(4,4),(4,4),(0.522097120208079,
1.00286833998585),(0.0665898698871197,0.0731716198748446),.UNSPECIFIED.);
#3363=B_SPLINE_SURFACE_WITH_KNOTS('',3,3,((#104080,#104081,#104082,#104083),
(#104084,#104085,#104086,#104087),(#104088,#104089,#104090,#104091),(#104092,
#104093,#104094,#104095)),.UNSPECIFIED.,.F.,.F.,.F.,(4,4),(4,4),(-0.00124731532213843,
0.209045111689404),(0.0700194292965034,0.074990098297759),.UNSPECIFIED.);
#3364=B_SPLINE_SURFACE_WITH_KNOTS('',3,3,((#104096,#104097,#104098,#104099),
(#104100,#104101,#104102,#104103),(#104104,#104105,#104106,#104107),(#104108,
#104109,#104110,#104111)),.UNSPECIFIED.,.F.,.F.,.F.,(4,4),(4,4),(-0.00286791014394406,
0.477902879796325),(0.010027146676379,0.0166015299239868),.UNSPECIFIED.);
#3365=B_SPLINE_SURFACE_WITH_KNOTS('',3,3,((#104113,#104114,#104115,#104116),
(#104117,#104118,#104119,#104120),(#104121,#104122,#104123,#104124),(#104125,
#104126,#104127,#104128)),.UNSPECIFIED.,.F.,.F.,.F.,(4,4),(4,4),(0.653230271496767,
1.0020690189285),(0.00656788395391393,0.0131849432430011),.UNSPECIFIED.);
#3366=B_SPLINE_SURFACE_WITH_KNOTS('',3,3,((#104142,#104143,#104144,#104145),
(#104146,#104147,#104148,#104149),(#104150,#104151,#104152,#104153),(#104154,
#104155,#104156,#104157)),.UNSPECIFIED.,.F.,.F.,.F.,(4,4),(4,4),(-0.0028678041047206,
0.47790287979547),(0.0200175229646906,0.0265907346180621),.UNSPECIFIED.);
#3367=B_SPLINE_SURFACE_WITH_KNOTS('',3,3,((#104159,#104160,#104161,#104162),
(#104163,#104164,#104165,#104166),(#104167,#104168,#104169,#104170),(#104171,
#104172,#104173,#104174)),.UNSPECIFIED.,.F.,.F.,.F.,(4,4),(4,4),(0.522097120208333,
1.00286753160119),(0.0166015299239887,0.0231736788075233),.UNSPECIFIED.);
#3368=B_SPLINE_SURFACE_WITH_KNOTS('',3,3,((#104176,#104177,#104178,#104179),
(#104180,#104181,#104182,#104183),(#104184,#104185,#104186,#104187),(#104188,
#104189,#104190,#104191)),.UNSPECIFIED.,.F.,.F.,.F.,(4,4),(4,4),(0.,1.0060000396136),
(0.016601529923987,0.0265907346180635),.UNSPECIFIED.);
#3369=B_SPLINE_SURFACE_WITH_KNOTS('',3,3,((#104192,#104193,#104194,#104195),
(#104196,#104197,#104198,#104199),(#104200,#104201,#104202,#104203),(#104204,
#104205,#104206,#104207)),.UNSPECIFIED.,.F.,.F.,.F.,(4,4),(4,4),(-0.00286862201162562,
0.477902879794753),(0.0300094532292787,0.0365944846647161),
 .UNSPECIFIED.);
#3370=B_SPLINE_SURFACE_WITH_KNOTS('',3,3,((#104209,#104210,#104211,#104212),
(#104213,#104214,#104215,#104216),(#104217,#104218,#104219,#104220),(#104221,
#104222,#104223,#104224)),.UNSPECIFIED.,.F.,.F.,.F.,(4,4),(4,4),(0.522097120208533,
1.00286823669298),(0.0265907346180623,0.0331702036889942),.UNSPECIFIED.);
#3371=B_SPLINE_SURFACE_WITH_KNOTS('',3,3,((#104232,#104233,#104234,#104235),
(#104236,#104237,#104238,#104239),(#104240,#104241,#104242,#104243),(#104244,
#104245,#104246,#104247)),.UNSPECIFIED.,.F.,.F.,.F.,(4,4),(4,4),(-0.00286848453263586,
0.477902879793197),(0.0400218729466601,0.0466073985929432),
 .UNSPECIFIED.);
#3372=B_SPLINE_SURFACE_WITH_KNOTS('',3,3,((#104264,#104265,#104266,#104267),
(#104268,#104269,#104270,#104271),(#104272,#104273,#104274,#104275),(#104276,
#104277,#104278,#104279)),.UNSPECIFIED.,.F.,.F.,.F.,(4,4),(4,4),(0.,1.0060001463976),
(0.0365944846645023,0.0466073985929169),.UNSPECIFIED.);
#3373=B_SPLINE_SURFACE_WITH_KNOTS('',3,3,((#104280,#104281,#104282,#104283),
(#104284,#104285,#104286,#104287),(#104288,#104289,#104290,#104291),(#104292,
#104293,#104294,#104295)),.UNSPECIFIED.,.F.,.F.,.F.,(4,4),(4,4),(-0.00286780122397318,
0.47790287979194),(0.0500263550859004,0.0565997133101409),.UNSPECIFIED.);
#3374=B_SPLINE_SURFACE_WITH_KNOTS('',3,3,((#104297,#104298,#104299,#104300),
(#104301,#104302,#104303,#104304),(#104305,#104306,#104307,#104308),(#104309,
#104310,#104311,#104312)),.UNSPECIFIED.,.F.,.F.,.F.,(4,4),(4,4),(0.522097120208675,
1.00286810177264),(0.0466073985929447,0.0531834925888942),.UNSPECIFIED.);
#3375=B_SPLINE_SURFACE_WITH_KNOTS('',3,3,((#104320,#104321,#104322,#104323),
(#104324,#104325,#104326,#104327),(#104328,#104329,#104330,#104331),(#104332,
#104333,#104334,#104335)),.UNSPECIFIED.,.F.,.F.,.F.,(4,4),(4,4),(-0.00286792598896076,
0.477902879791154),(0.0600156865494595,0.0665898698871175),
 .UNSPECIFIED.);
#3376=B_SPLINE_SURFACE_WITH_KNOTS('',3,3,((#104337,#104338,#104339,#104340),
(#104341,#104342,#104343,#104344),(#104345,#104346,#104347,#104348),(#104349,
#104350,#104351,#104352)),.UNSPECIFIED.,.F.,.F.,.F.,(4,4),(4,4),(0.522097120208892,
1.00286764392033),(0.056599713310143,0.0631721430887063),.UNSPECIFIED.);
#3377=B_SPLINE_SURFACE_WITH_KNOTS('',3,3,((#104368,#104369,#104370,#104371),
(#104372,#104373,#104374,#104375),(#104376,#104377,#104378,#104379),(#104380,
#104381,#104382,#104383)),.UNSPECIFIED.,.F.,.F.,.F.,(4,4),(4,4),(0.522097120208067,
1.00286833998587),(0.0665898698871201,0.0731716198748447),.UNSPECIFIED.);
#3378=B_SPLINE_SURFACE_WITH_KNOTS('',3,3,((#104384,#104385,#104386,#104387),
(#104388,#104389,#104390,#104391),(#104392,#104393,#104394,#104395),(#104396,
#104397,#104398,#104399)),.UNSPECIFIED.,.F.,.F.,.F.,(4,4),(4,4),(-0.00124731531958877,
0.209045111691966),(0.0700194292965107,0.0749900982977698),
 .UNSPECIFIED.);
#3379=B_SPLINE_SURFACE_WITH_KNOTS('',3,3,((#104406,#104407,#104408,#104409),
(#104410,#104411,#104412,#104413),(#104414,#104415,#104416,#104417),(#104418,
#104419,#104420,#104421)),.UNSPECIFIED.,.F.,.F.,.F.,(4,4),(4,4),(-0.00286791014395316,
0.477902879798327),(0.0100271466769336,0.0166015299239876),
 .UNSPECIFIED.);
#3380=B_SPLINE_SURFACE_WITH_KNOTS('',3,3,((#104423,#104424,#104425,#104426),
(#104427,#104428,#104429,#104430),(#104431,#104432,#104433,#104434),(#104435,
#104436,#104437,#104438)),.UNSPECIFIED.,.F.,.F.,.F.,(4,4),(4,4),(0.653230271495359,
1.00206901892606),(0.00656788395391684,0.0131849432429894),
 .UNSPECIFIED.);
#3381=B_SPLINE_SURFACE_WITH_KNOTS('',3,3,((#104446,#104447,#104448,#104449),
(#104450,#104451,#104452,#104453),(#104454,#104455,#104456,#104457),(#104458,
#104459,#104460,#104461)),.UNSPECIFIED.,.F.,.F.,.F.,(4,4),(4,4),(-0.00286780410466546,
0.477902879797445),(0.0200175229646907,0.0265907346180625),
 .UNSPECIFIED.);
#3382=B_SPLINE_SURFACE_WITH_KNOTS('',3,3,((#104463,#104464,#104465,#104466),
(#104467,#104468,#104469,#104470),(#104471,#104472,#104473,#104474),(#104475,
#104476,#104477,#104478)),.UNSPECIFIED.,.F.,.F.,.F.,(4,4),(4,4),(0.52209712020821,
1.00286753160119),(0.0166015299239882,0.0231736788075225),.UNSPECIFIED.);
#3383=B_SPLINE_SURFACE_WITH_KNOTS('',3,3,((#104480,#104481,#104482,#104483),
(#104484,#104485,#104486,#104487),(#104488,#104489,#104490,#104491),(#104492,
#104493,#104494,#104495)),.UNSPECIFIED.,.F.,.F.,.F.,(4,4),(4,4),(0.,1.00600003961386),
(0.0166015299239892,0.0265907346180634),.UNSPECIFIED.);
#3384=B_SPLINE_SURFACE_WITH_KNOTS('',3,3,((#104496,#104497,#104498,#104499),
(#104500,#104501,#104502,#104503),(#104504,#104505,#104506,#104507),(#104508,
#104509,#104510,#104511)),.UNSPECIFIED.,.F.,.F.,.F.,(4,4),(4,4),(-0.0028686220115229,
0.477902879796868),(0.0300094532292789,0.0365944846647172),
 .UNSPECIFIED.);
#3385=B_SPLINE_SURFACE_WITH_KNOTS('',3,3,((#104513,#104514,#104515,#104516),
(#104517,#104518,#104519,#104520),(#104521,#104522,#104523,#104524),(#104525,
#104526,#104527,#104528)),.UNSPECIFIED.,.F.,.F.,.F.,(4,4),(4,4),(0.522097120208426,
1.00286823669299),(0.0265907346180636,0.0331702036889942),.UNSPECIFIED.);
#3386=B_SPLINE_SURFACE_WITH_KNOTS('',3,3,((#104536,#104537,#104538,#104539),
(#104540,#104541,#104542,#104543),(#104544,#104545,#104546,#104547),(#104548,
#104549,#104550,#104551)),.UNSPECIFIED.,.F.,.F.,.F.,(4,4),(4,4),(-0.00286848453265357,
0.477902879795543),(0.0400218729466598,0.0466073985929427),
 .UNSPECIFIED.);
#3387=B_SPLINE_SURFACE_WITH_KNOTS('',3,3,((#104568,#104569,#104570,#104571),
(#104572,#104573,#104574,#104575),(#104576,#104577,#104578,#104579),(#104580,
#104581,#104582,#104583)),.UNSPECIFIED.,.F.,.F.,.F.,(4,4),(4,4),(0.,1.00600014639755),
(0.0365944846645018,0.0466073985929159),.UNSPECIFIED.);
#3388=B_SPLINE_SURFACE_WITH_KNOTS('',3,3,((#104584,#104585,#104586,#104587),
(#104588,#104589,#104590,#104591),(#104592,#104593,#104594,#104595),(#104596,
#104597,#104598,#104599)),.UNSPECIFIED.,.F.,.F.,.F.,(4,4),(4,4),(-0.00286780122398932,
0.477902879794246),(0.0500263550858991,0.0565997133101411),
 .UNSPECIFIED.);
#3389=B_SPLINE_SURFACE_WITH_KNOTS('',3,3,((#104601,#104602,#104603,#104604),
(#104605,#104606,#104607,#104608),(#104609,#104610,#104611,#104612),(#104613,
#104614,#104615,#104616)),.UNSPECIFIED.,.F.,.F.,.F.,(4,4),(4,4),(0.522097120208498,
1.00286810177262),(0.0466073985929433,0.0531834925888932),.UNSPECIFIED.);
#3390=B_SPLINE_SURFACE_WITH_KNOTS('',3,3,((#104624,#104625,#104626,#104627),
(#104628,#104629,#104630,#104631),(#104632,#104633,#104634,#104635),(#104636,
#104637,#104638,#104639)),.UNSPECIFIED.,.F.,.F.,.F.,(4,4),(4,4),(-0.00286792598894048,
0.477902879792958),(0.0600156865494587,0.0665898698871172),
 .UNSPECIFIED.);
#3391=B_SPLINE_SURFACE_WITH_KNOTS('',3,3,((#104641,#104642,#104643,#104644),
(#104645,#104646,#104647,#104648),(#104649,#104650,#104651,#104652),(#104653,
#104654,#104655,#104656)),.UNSPECIFIED.,.F.,.F.,.F.,(4,4),(4,4),(0.522097120208652,
1.00286764392037),(0.0565997133101409,0.0631721430887067),.UNSPECIFIED.);
#3392=B_SPLINE_SURFACE_WITH_KNOTS('',3,3,((#104672,#104673,#104674,#104675),
(#104676,#104677,#104678,#104679),(#104680,#104681,#104682,#104683),(#104684,
#104685,#104686,#104687)),.UNSPECIFIED.,.F.,.F.,.F.,(4,4),(4,4),(0.522097120207924,
1.00286833998585),(0.0665898698871192,0.0731716198748446),.UNSPECIFIED.);
#3393=B_SPLINE_SURFACE_WITH_KNOTS('',3,3,((#104688,#104689,#104690,#104691),
(#104692,#104693,#104694,#104695),(#104696,#104697,#104698,#104699),(#104700,
#104701,#104702,#104703)),.UNSPECIFIED.,.F.,.F.,.F.,(4,4),(4,4),(-0.00124731531729226,
0.209045111694373),(0.0700194292965185,0.0749900982977811),
 .UNSPECIFIED.);
#3394=B_SPLINE_SURFACE_WITH_KNOTS('',3,3,((#104710,#104711,#104712,#104713),
(#104714,#104715,#104716,#104717),(#104718,#104719,#104720,#104721),(#104722,
#104723,#104724,#104725)),.UNSPECIFIED.,.F.,.F.,.F.,(4,4),(4,4),(-0.00286791014398744,
0.477902879799781),(0.0100271466769349,0.0166015299239874),
 .UNSPECIFIED.);
#3395=B_SPLINE_SURFACE_WITH_KNOTS('',3,3,((#104727,#104728,#104729,#104730),
(#104731,#104732,#104733,#104734),(#104735,#104736,#104737,#104738),(#104739,
#104740,#104741,#104742)),.UNSPECIFIED.,.F.,.F.,.F.,(4,4),(4,4),(0.653230271493824,
1.00206901892362),(0.00656788395392139,0.013184943242896),.UNSPECIFIED.);
#3396=B_SPLINE_SURFACE_WITH_KNOTS('',3,3,((#104750,#104751,#104752,#104753),
(#104754,#104755,#104756,#104757),(#104758,#104759,#104760,#104761),(#104762,
#104763,#104764,#104765)),.UNSPECIFIED.,.F.,.F.,.F.,(4,4),(4,4),(-0.00286780410473367,
0.477902879799223),(0.0200175229646907,0.0265907346180625),
 .UNSPECIFIED.);
#3397=B_SPLINE_SURFACE_WITH_KNOTS('',3,3,((#104767,#104768,#104769,#104770),
(#104771,#104772,#104773,#104774),(#104775,#104776,#104777,#104778),(#104779,
#104780,#104781,#104782)),.UNSPECIFIED.,.F.,.F.,.F.,(4,4),(4,4),(0.522097120208011,
1.0028675316012),(0.0166015299239878,0.0231736788075225),.UNSPECIFIED.);
#3398=B_SPLINE_SURFACE_WITH_KNOTS('',3,3,((#104784,#104785,#104786,#104787),
(#104788,#104789,#104790,#104791),(#104792,#104793,#104794,#104795),(#104796,
#104797,#104798,#104799)),.UNSPECIFIED.,.F.,.F.,.F.,(4,4),(4,4),(0.,1.00600003961381),
(0.016601529923988,0.0265907346180629),.UNSPECIFIED.);
#3399=B_SPLINE_SURFACE_WITH_KNOTS('',3,3,((#104800,#104801,#104802,#104803),
(#104804,#104805,#104806,#104807),(#104808,#104809,#104810,#104811),(#104812,
#104813,#104814,#104815)),.UNSPECIFIED.,.F.,.F.,.F.,(4,4),(4,4),(-0.00286862201153651,
0.477902879798629),(0.0300094532292788,0.0365944846647022),
 .UNSPECIFIED.);
#3400=B_SPLINE_SURFACE_WITH_KNOTS('',3,3,((#104817,#104818,#104819,#104820),
(#104821,#104822,#104823,#104824),(#104825,#104826,#104827,#104828),(#104829,
#104830,#104831,#104832)),.UNSPECIFIED.,.F.,.F.,.F.,(4,4),(4,4),(0.522097120208293,
1.0028682366929),(0.0265907346180642,0.0331702036051743),.UNSPECIFIED.);
#3401=B_SPLINE_SURFACE_WITH_KNOTS('',3,3,((#104840,#104841,#104842,#104843),
(#104844,#104845,#104846,#104847),(#104848,#104849,#104850,#104851),(#104852,
#104853,#104854,#104855)),.UNSPECIFIED.,.F.,.F.,.F.,(4,4),(4,4),(-0.00286848453268432,
0.477902879797276),(0.0400218729466601,0.046607398592943),.UNSPECIFIED.);
#3402=B_SPLINE_SURFACE_WITH_KNOTS('',3,3,((#104872,#104873,#104874,#104875),
(#104876,#104877,#104878,#104879),(#104880,#104881,#104882,#104883),(#104884,
#104885,#104886,#104887)),.UNSPECIFIED.,.F.,.F.,.F.,(4,4),(4,4),(0.,1.00600014639734),
(0.0365944846645009,0.0466073985929168),.UNSPECIFIED.);
#3403=B_SPLINE_SURFACE_WITH_KNOTS('',3,3,((#104888,#104889,#104890,#104891),
(#104892,#104893,#104894,#104895),(#104896,#104897,#104898,#104899),(#104900,
#104901,#104902,#104903)),.UNSPECIFIED.,.F.,.F.,.F.,(4,4),(4,4),(-0.00286780122404455,
0.477902879796201),(0.0500263550858999,0.0565997133101408),
 .UNSPECIFIED.);
#3404=B_SPLINE_SURFACE_WITH_KNOTS('',3,3,((#104905,#104906,#104907,#104908),
(#104909,#104910,#104911,#104912),(#104913,#104914,#104915,#104916),(#104917,
#104918,#104919,#104920)),.UNSPECIFIED.,.F.,.F.,.F.,(4,4),(4,4),(0.522097120208524,
1.00286810177264),(0.0466073985929456,0.0531834925888943),.UNSPECIFIED.);
#3405=B_SPLINE_SURFACE_WITH_KNOTS('',3,3,((#104928,#104929,#104930,#104931),
(#104932,#104933,#104934,#104935),(#104936,#104937,#104938,#104939),(#104940,
#104941,#104942,#104943)),.UNSPECIFIED.,.F.,.F.,.F.,(4,4),(4,4),(-0.0028679259890379,
0.47790287979535),(0.0600156865494599,0.0665898698871175),.UNSPECIFIED.);
#3406=B_SPLINE_SURFACE_WITH_KNOTS('',3,3,((#104945,#104946,#104947,#104948),
(#104949,#104950,#104951,#104952),(#104953,#104954,#104955,#104956),(#104957,
#104958,#104959,#104960)),.UNSPECIFIED.,.F.,.F.,.F.,(4,4),(4,4),(0.522097120208551,
1.00286764392039),(0.0565997133101416,0.0631721430887072),.UNSPECIFIED.);
#3407=B_SPLINE_SURFACE_WITH_KNOTS('',3,3,((#104976,#104977,#104978,#104979),
(#104980,#104981,#104982,#104983),(#104984,#104985,#104986,#104987),(#104988,
#104989,#104990,#104991)),.UNSPECIFIED.,.F.,.F.,.F.,(4,4),(4,4),(0.522097120207716,
1.0028683399859),(0.0665898698871188,0.073171619874846),.UNSPECIFIED.);
#3408=B_SPLINE_SURFACE_WITH_KNOTS('',3,3,((#104992,#104993,#104994,#104995),
(#104996,#104997,#104998,#104999),(#105000,#105001,#105002,#105003),(#105004,
#105005,#105006,#105007)),.UNSPECIFIED.,.F.,.F.,.F.,(4,4),(4,4),(-0.00124731531514357,
0.20904511169649),(0.0700194292965287,0.0749900982977919),.UNSPECIFIED.);
#3409=B_SPLINE_SURFACE_WITH_KNOTS('',3,3,((#105014,#105015,#105016,#105017),
(#105018,#105019,#105020,#105021),(#105022,#105023,#105024,#105025),(#105026,
#105027,#105028,#105029)),.UNSPECIFIED.,.F.,.F.,.F.,(4,4),(4,4),(-0.0028679101440714,
0.477902879801083),(0.0100271466769349,0.0166015299239868),
 .UNSPECIFIED.);
#3410=B_SPLINE_SURFACE_WITH_KNOTS('',3,3,((#105031,#105032,#105033,#105034),
(#105035,#105036,#105037,#105038),(#105039,#105040,#105041,#105042),(#105043,
#105044,#105045,#105046)),.UNSPECIFIED.,.F.,.F.,.F.,(4,4),(4,4),(0.653230271492592,
1.00206901892104),(0.00656788395392352,0.0131849432429891),
 .UNSPECIFIED.);
#3411=B_SPLINE_SURFACE_WITH_KNOTS('',3,3,((#105054,#105055,#105056,#105057),
(#105058,#105059,#105060,#105061),(#105062,#105063,#105064,#105065),(#105066,
#105067,#105068,#105069)),.UNSPECIFIED.,.F.,.F.,.F.,(4,4),(4,4),(-0.00286780410466828,
0.477902879800657),(0.0200175229646911,0.0265907346180624),
 .UNSPECIFIED.);
#3412=B_SPLINE_SURFACE_WITH_KNOTS('',3,3,((#105071,#105072,#105073,#105074),
(#105075,#105076,#105077,#105078),(#105079,#105080,#105081,#105082),(#105083,
#105084,#105085,#105086)),.UNSPECIFIED.,.F.,.F.,.F.,(4,4),(4,4),(0.522097120207656,
1.00286753160124),(0.0166015299239886,0.0231736788075226),.UNSPECIFIED.);
#3413=B_SPLINE_SURFACE_WITH_KNOTS('',3,3,((#105088,#105089,#105090,#105091),
(#105092,#105093,#105094,#105095),(#105096,#105097,#105098,#105099),(#105100,
#105101,#105102,#105103)),.UNSPECIFIED.,.F.,.F.,.F.,(4,4),(4,4),(0.,1.00600003961359),
(0.0166015299239881,0.0265907346180622),.UNSPECIFIED.);
#3414=B_SPLINE_SURFACE_WITH_KNOTS('',3,3,((#105104,#105105,#105106,#105107),
(#105108,#105109,#105110,#105111),(#105112,#105113,#105114,#105115),(#105116,
#105117,#105118,#105119)),.UNSPECIFIED.,.F.,.F.,.F.,(4,4),(4,4),(-0.00286862201158194,
0.477902879799869),(0.030009453229279,0.036594484664716),.UNSPECIFIED.);
#3415=B_SPLINE_SURFACE_WITH_KNOTS('',3,3,((#105121,#105122,#105123,#105124),
(#105125,#105126,#105127,#105128),(#105129,#105130,#105131,#105132),(#105133,
#105134,#105135,#105136)),.UNSPECIFIED.,.F.,.F.,.F.,(4,4),(4,4),(0.522097120208047,
1.00286823669304),(0.0265907346180626,0.0331702036889935),.UNSPECIFIED.);
#3416=B_SPLINE_SURFACE_WITH_KNOTS('',3,3,((#105144,#105145,#105146,#105147),
(#105148,#105149,#105150,#105151),(#105152,#105153,#105154,#105155),(#105156,
#105157,#105158,#105159)),.UNSPECIFIED.,.F.,.F.,.F.,(4,4),(4,4),(-0.0028684845327302,
0.477902879799251),(0.0400218729466597,0.0466073985929431),
 .UNSPECIFIED.);
#3417=B_SPLINE_SURFACE_WITH_KNOTS('',3,3,((#105176,#105177,#105178,#105179),
(#105180,#105181,#105182,#105183),(#105184,#105185,#105186,#105187),(#105188,
#105189,#105190,#105191)),.UNSPECIFIED.,.F.,.F.,.F.,(4,4),(4,4),(0.,1.00600014639743),
(0.0365944846645017,0.0466073985929158),.UNSPECIFIED.);
#3418=B_SPLINE_SURFACE_WITH_KNOTS('',3,3,((#105192,#105193,#105194,#105195),
(#105196,#105197,#105198,#105199),(#105200,#105201,#105202,#105203),(#105204,
#105205,#105206,#105207)),.UNSPECIFIED.,.F.,.F.,.F.,(4,4),(4,4),(-0.00286780122399644,
0.477902879798194),(0.0500263550859006,0.0565997133101405),
 .UNSPECIFIED.);
#3419=B_SPLINE_SURFACE_WITH_KNOTS('',3,3,((#105209,#105210,#105211,#105212),
(#105213,#105214,#105215,#105216),(#105217,#105218,#105219,#105220),(#105221,
#105222,#105223,#105224)),.UNSPECIFIED.,.F.,.F.,.F.,(4,4),(4,4),(0.522097120208366,
1.00286810177262),(0.046607398592945,0.0531834925888933),.UNSPECIFIED.);
#3420=B_SPLINE_SURFACE_WITH_KNOTS('',3,3,((#105232,#105233,#105234,#105235),
(#105236,#105237,#105238,#105239),(#105240,#105241,#105242,#105243),(#105244,
#105245,#105246,#105247)),.UNSPECIFIED.,.F.,.F.,.F.,(4,4),(4,4),(-0.00286792598896392,
0.477902879797277),(0.0600156865494601,0.0665898698871176),
 .UNSPECIFIED.);
#3421=B_SPLINE_SURFACE_WITH_KNOTS('',3,3,((#105249,#105250,#105251,#105252),
(#105253,#105254,#105255,#105256),(#105257,#105258,#105259,#105260),(#105261,
#105262,#105263,#105264)),.UNSPECIFIED.,.F.,.F.,.F.,(4,4),(4,4),(0.522097120208508,
1.0028676439203),(0.0565997133101424,0.0631721430887051),.UNSPECIFIED.);
#3422=B_SPLINE_SURFACE_WITH_KNOTS('',3,3,((#105280,#105281,#105282,#105283),
(#105284,#105285,#105286,#105287),(#105288,#105289,#105290,#105291),(#105292,
#105293,#105294,#105295)),.UNSPECIFIED.,.F.,.F.,.F.,(4,4),(4,4),(0.522097120207604,
1.00286833998584),(0.0665898698871184,0.0731716198748442),.UNSPECIFIED.);
#3423=B_SPLINE_SURFACE_WITH_KNOTS('',3,3,((#105296,#105297,#105298,#105299),
(#105300,#105301,#105302,#105303),(#105304,#105305,#105306,#105307),(#105308,
#105309,#105310,#105311)),.UNSPECIFIED.,.F.,.F.,.F.,(4,4),(4,4),(-0.00124731531299614,
0.209045111698441),(0.0700194292965412,0.074990098297801),.UNSPECIFIED.);
#3424=B_SPLINE_SURFACE_WITH_KNOTS('',3,3,((#105318,#105319,#105320,#105321),
(#105322,#105323,#105324,#105325),(#105326,#105327,#105328,#105329),(#105330,
#105331,#105332,#105333)),.UNSPECIFIED.,.F.,.F.,.F.,(4,4),(4,4),(-0.00286791014406684,
0.477902879802145),(0.0100271466769343,0.0166015299239869),
 .UNSPECIFIED.);
#3425=B_SPLINE_SURFACE_WITH_KNOTS('',3,3,((#105335,#105336,#105337,#105338),
(#105339,#105340,#105341,#105342),(#105343,#105344,#105345,#105346),(#105347,
#105348,#105349,#105350)),.UNSPECIFIED.,.F.,.F.,.F.,(4,4),(4,4),(0.653230271491155,
1.00206901891852),(0.00656788395392543,0.0131849432429894),
 .UNSPECIFIED.);
#3426=B_SPLINE_SURFACE_WITH_KNOTS('',3,3,((#105358,#105359,#105360,#105361),
(#105362,#105363,#105364,#105365),(#105366,#105367,#105368,#105369),(#105370,
#105371,#105372,#105373)),.UNSPECIFIED.,.F.,.F.,.F.,(4,4),(4,4),(-0.00286780410478348,
0.477902879801889),(0.0200175229646909,0.0265907346180623),
 .UNSPECIFIED.);
#3427=B_SPLINE_SURFACE_WITH_KNOTS('',3,3,((#105375,#105376,#105377,#105378),
(#105379,#105380,#105381,#105382),(#105383,#105384,#105385,#105386),(#105387,
#105388,#105389,#105390)),.UNSPECIFIED.,.F.,.F.,.F.,(4,4),(4,4),(0.522097120204887,
1.00286753160122),(0.0166015299239819,0.0231736788075228),.UNSPECIFIED.);
#3428=B_SPLINE_SURFACE_WITH_KNOTS('',3,3,((#105392,#105393,#105394,#105395),
(#105396,#105397,#105398,#105399),(#105400,#105401,#105402,#105403),(#105404,
#105405,#105406,#105407)),.UNSPECIFIED.,.F.,.F.,.F.,(4,4),(4,4),(0.,1.00600003961353),
(0.0166015299239881,0.0265907346180637),.UNSPECIFIED.);
#3429=B_SPLINE_SURFACE_WITH_KNOTS('',3,3,((#105408,#105409,#105410,#105411),
(#105412,#105413,#105414,#105415),(#105416,#105417,#105418,#105419),(#105420,
#105421,#105422,#105423)),.UNSPECIFIED.,.F.,.F.,.F.,(4,4),(4,4),(-0.00286862201163699,
0.47790287980125),(0.0300094532292782,0.036594484664716),.UNSPECIFIED.);
#3430=B_SPLINE_SURFACE_WITH_KNOTS('',3,3,((#105425,#105426,#105427,#105428),
(#105429,#105430,#105431,#105432),(#105433,#105434,#105435,#105436),(#105437,
#105438,#105439,#105440)),.UNSPECIFIED.,.F.,.F.,.F.,(4,4),(4,4),(0.522097120206289,
1.00286823669298),(0.0265907346180629,0.0331702036889933),.UNSPECIFIED.);
#3431=B_SPLINE_SURFACE_WITH_KNOTS('',3,3,((#105448,#105449,#105450,#105451),
(#105452,#105453,#105454,#105455),(#105456,#105457,#105458,#105459),(#105460,
#105461,#105462,#105463)),.UNSPECIFIED.,.F.,.F.,.F.,(4,4),(4,4),(-0.00286848453269418,
0.477902879800586),(0.0400218729466597,0.0466073985929435),
 .UNSPECIFIED.);
#3432=B_SPLINE_SURFACE_WITH_KNOTS('',3,3,((#105480,#105481,#105482,#105483),
(#105484,#105485,#105486,#105487),(#105488,#105489,#105490,#105491),(#105492,
#105493,#105494,#105495)),.UNSPECIFIED.,.F.,.F.,.F.,(4,4),(4,4),(0.,1.00600014639743),
(0.0365944846645011,0.0466073985929158),.UNSPECIFIED.);
#3433=B_SPLINE_SURFACE_WITH_KNOTS('',3,3,((#105496,#105497,#105498,#105499),
(#105500,#105501,#105502,#105503),(#105504,#105505,#105506,#105507),(#105508,
#105509,#105510,#105511)),.UNSPECIFIED.,.F.,.F.,.F.,(4,4),(4,4),(-0.0028678012240359,
0.477902879799762),(0.0500263550858998,0.0565997133101407),
 .UNSPECIFIED.);
#3434=B_SPLINE_SURFACE_WITH_KNOTS('',3,3,((#105513,#105514,#105515,#105516),
(#105517,#105518,#105519,#105520),(#105521,#105522,#105523,#105524),(#105525,
#105526,#105527,#105528)),.UNSPECIFIED.,.F.,.F.,.F.,(4,4),(4,4),(0.522097120208308,
1.00286810177265),(0.0466073985929458,0.0531834925888935),.UNSPECIFIED.);
#3435=B_SPLINE_SURFACE_WITH_KNOTS('',3,3,((#105536,#105537,#105538,#105539),
(#105540,#105541,#105542,#105543),(#105544,#105545,#105546,#105547),(#105548,
#105549,#105550,#105551)),.UNSPECIFIED.,.F.,.F.,.F.,(4,4),(4,4),(-0.00286792598883179,
0.477902879798954),(0.0600156865494597,0.0665898698871172),
 .UNSPECIFIED.);
#3436=B_SPLINE_SURFACE_WITH_KNOTS('',3,3,((#105553,#105554,#105555,#105556),
(#105557,#105558,#105559,#105560),(#105561,#105562,#105563,#105564),(#105565,
#105566,#105567,#105568)),.UNSPECIFIED.,.F.,.F.,.F.,(4,4),(4,4),(0.522097120208306,
1.00286764392041),(0.056599713310142,0.0631721430887071),.UNSPECIFIED.);
#3437=B_SPLINE_SURFACE_WITH_KNOTS('',3,3,((#105584,#105585,#105586,#105587),
(#105588,#105589,#105590,#105591),(#105592,#105593,#105594,#105595),(#105596,
#105597,#105598,#105599)),.UNSPECIFIED.,.F.,.F.,.F.,(4,4),(4,4),(0.522097120207573,
1.00286833998592),(0.0665898698871191,0.0731716198748462),.UNSPECIFIED.);
#3438=B_SPLINE_SURFACE_WITH_KNOTS('',3,3,((#105600,#105601,#105602,#105603),
(#105604,#105605,#105606,#105607),(#105608,#105609,#105610,#105611),(#105612,
#105613,#105614,#105615)),.UNSPECIFIED.,.F.,.F.,.F.,(4,4),(4,4),(-0.00124731531130942,
0.209045111700277),(0.0700194292965537,0.0749900982978096),
 .UNSPECIFIED.);
#3439=B_SPLINE_SURFACE_WITH_KNOTS('',3,3,((#105622,#105623,#105624,#105625),
(#105626,#105627,#105628,#105629),(#105630,#105631,#105632,#105633),(#105634,
#105635,#105636,#105637)),.UNSPECIFIED.,.F.,.F.,.F.,(4,4),(4,4),(-0.0028679101440672,
0.477902879801822),(0.0100271466769372,0.0166015299239861),
 .UNSPECIFIED.);
#3440=B_SPLINE_SURFACE_WITH_KNOTS('',3,3,((#105639,#105640,#105641,#105642),
(#105643,#105644,#105645,#105646),(#105647,#105648,#105649,#105650),(#105651,
#105652,#105653,#105654)),.UNSPECIFIED.,.F.,.F.,.F.,(4,4),(4,4),(0.653230271507192,
1.00206901891588),(0.00656788395410992,0.0131849432121928),
 .UNSPECIFIED.);
#3441=B_SPLINE_SURFACE_WITH_KNOTS('',3,3,((#105662,#105663,#105664,#105665),
(#105666,#105667,#105668,#105669),(#105670,#105671,#105672,#105673),(#105674,
#105675,#105676,#105677)),.UNSPECIFIED.,.F.,.F.,.F.,(4,4),(4,4),(-0.00286780410472287,
0.477902879802779),(0.0200175229646914,0.0265907346180623),
 .UNSPECIFIED.);
#3442=B_SPLINE_SURFACE_WITH_KNOTS('',3,3,((#105679,#105680,#105681,#105682),
(#105683,#105684,#105685,#105686),(#105687,#105688,#105689,#105690),(#105691,
#105692,#105693,#105694)),.UNSPECIFIED.,.F.,.F.,.F.,(4,4),(4,4),(0.522097120202547,
1.00286753160126),(0.0166015299239893,0.0231736788075226),.UNSPECIFIED.);
#3443=B_SPLINE_SURFACE_WITH_KNOTS('',3,3,((#105696,#105697,#105698,#105699),
(#105700,#105701,#105702,#105703),(#105704,#105705,#105706,#105707),(#105708,
#105709,#105710,#105711)),.UNSPECIFIED.,.F.,.F.,.F.,(4,4),(4,4),(0.,1.0060000396138),
(0.0166015299239891,0.0265907346180633),.UNSPECIFIED.);
#3444=B_SPLINE_SURFACE_WITH_KNOTS('',3,3,((#105712,#105713,#105714,#105715),
(#105716,#105717,#105718,#105719),(#105720,#105721,#105722,#105723),(#105724,
#105725,#105726,#105727)),.UNSPECIFIED.,.F.,.F.,.F.,(4,4),(4,4),(-0.00286862201157427,
0.477902879802343),(0.0300094532292775,0.0365944846647152),
 .UNSPECIFIED.);
#3445=B_SPLINE_SURFACE_WITH_KNOTS('',3,3,((#105729,#105730,#105731,#105732),
(#105733,#105734,#105735,#105736),(#105737,#105738,#105739,#105740),(#105741,
#105742,#105743,#105744)),.UNSPECIFIED.,.F.,.F.,.F.,(4,4),(4,4),(0.52209712020368,
1.00286823669299),(0.0265907346180624,0.0331702036889926),.UNSPECIFIED.);
#3446=B_SPLINE_SURFACE_WITH_KNOTS('',3,3,((#105752,#105753,#105754,#105755),
(#105756,#105757,#105758,#105759),(#105760,#105761,#105762,#105763),(#105764,
#105765,#105766,#105767)),.UNSPECIFIED.,.F.,.F.,.F.,(4,4),(4,4),(-0.00286848453279188,
0.477902879802615),(0.040021872946661,0.0466073985929422),.UNSPECIFIED.);
#3447=B_SPLINE_SURFACE_WITH_KNOTS('',3,3,((#105784,#105785,#105786,#105787),
(#105788,#105789,#105790,#105791),(#105792,#105793,#105794,#105795),(#105796,
#105797,#105798,#105799)),.UNSPECIFIED.,.F.,.F.,.F.,(4,4),(4,4),(0.,1.0060001463974),
(0.0365944846645005,0.0466073985929165),.UNSPECIFIED.);
#3448=B_SPLINE_SURFACE_WITH_KNOTS('',3,3,((#105800,#105801,#105802,#105803),
(#105804,#105805,#105806,#105807),(#105808,#105809,#105810,#105811),(#105812,
#105813,#105814,#105815)),.UNSPECIFIED.,.F.,.F.,.F.,(4,4),(4,4),(-0.00286780122402792,
0.47790287980117),(0.0500263550859001,0.0565997133101407),.UNSPECIFIED.);
#3449=B_SPLINE_SURFACE_WITH_KNOTS('',3,3,((#105817,#105818,#105819,#105820),
(#105821,#105822,#105823,#105824),(#105825,#105826,#105827,#105828),(#105829,
#105830,#105831,#105832)),.UNSPECIFIED.,.F.,.F.,.F.,(4,4),(4,4),(0.522097120206262,
1.00286810177263),(0.0466073985929405,0.0531834925888929),.UNSPECIFIED.);
#3450=B_SPLINE_SURFACE_WITH_KNOTS('',3,3,((#105840,#105841,#105842,#105843),
(#105844,#105845,#105846,#105847),(#105848,#105849,#105850,#105851),(#105852,
#105853,#105854,#105855)),.UNSPECIFIED.,.F.,.F.,.F.,(4,4),(4,4),(-0.00286792598904179,
0.477902879800371),(0.060015686549462,0.0665898698871172),.UNSPECIFIED.);
#3451=B_SPLINE_SURFACE_WITH_KNOTS('',3,3,((#105857,#105858,#105859,#105860),
(#105861,#105862,#105863,#105864),(#105865,#105866,#105867,#105868),(#105869,
#105870,#105871,#105872)),.UNSPECIFIED.,.F.,.F.,.F.,(4,4),(4,4),(0.522097120207651,
1.00286764392039),(0.0565997133101423,0.0631721430887065),.UNSPECIFIED.);
#3452=B_SPLINE_SURFACE_WITH_KNOTS('',3,3,((#105888,#105889,#105890,#105891),
(#105892,#105893,#105894,#105895),(#105896,#105897,#105898,#105899),(#105900,
#105901,#105902,#105903)),.UNSPECIFIED.,.F.,.F.,.F.,(4,4),(4,4),(0.522097120207396,
1.0028683399859),(0.0665898698871197,0.0731716198748454),.UNSPECIFIED.);
#3453=B_SPLINE_SURFACE_WITH_KNOTS('',3,3,((#105904,#105905,#105906,#105907),
(#105908,#105909,#105910,#105911),(#105912,#105913,#105914,#105915),(#105916,
#105917,#105918,#105919)),.UNSPECIFIED.,.F.,.F.,.F.,(4,4),(4,4),(-0.0012473153096852,
0.209045111701724),(0.0700194292965668,0.0749900982978162),
 .UNSPECIFIED.);
#3454=B_SPLINE_SURFACE_WITH_KNOTS('',3,3,((#105926,#105927,#105928,#105929),
(#105930,#105931,#105932,#105933),(#105934,#105935,#105936,#105937),(#105938,
#105939,#105940,#105941)),.UNSPECIFIED.,.F.,.F.,.F.,(4,4),(4,4),(-0.00286791014414908,
0.477902879802002),(0.010027146676936,0.0166015299239886),.UNSPECIFIED.);
#3455=B_SPLINE_SURFACE_WITH_KNOTS('',3,3,((#105943,#105944,#105945,#105946),
(#105947,#105948,#105949,#105950),(#105951,#105952,#105953,#105954),(#105955,
#105956,#105957,#105958)),.UNSPECIFIED.,.F.,.F.,.F.,(4,4),(4,4),(0.653230271488838,
1.00206901891347),(0.00656788395410877,0.0131849432121942),
 .UNSPECIFIED.);
#3456=B_SPLINE_SURFACE_WITH_KNOTS('',3,3,((#105966,#105967,#105968,#105969),
(#105970,#105971,#105972,#105973),(#105974,#105975,#105976,#105977),(#105978,
#105979,#105980,#105981)),.UNSPECIFIED.,.F.,.F.,.F.,(4,4),(4,4),(-0.00286780410486259,
0.477902879801869),(0.0200175229646921,0.026590734618063),.UNSPECIFIED.);
#3457=B_SPLINE_SURFACE_WITH_KNOTS('',3,3,((#105983,#105984,#105985,#105986),
(#105987,#105988,#105989,#105990),(#105991,#105992,#105993,#105994),(#105995,
#105996,#105997,#105998)),.UNSPECIFIED.,.F.,.F.,.F.,(4,4),(4,4),(0.522097120201399,
1.00286753160122),(0.0166015299239896,0.023173678807522),.UNSPECIFIED.);
#3458=B_SPLINE_SURFACE_WITH_KNOTS('',3,3,((#106000,#106001,#106002,#106003),
(#106004,#106005,#106006,#106007),(#106008,#106009,#106010,#106011),(#106012,
#106013,#106014,#106015)),.UNSPECIFIED.,.F.,.F.,.F.,(4,4),(4,4),(0.,1.00600003961373),
(0.0166015299239904,0.0265907346180639),.UNSPECIFIED.);
#3459=B_SPLINE_SURFACE_WITH_KNOTS('',3,3,((#106016,#106017,#106018,#106019),
(#106020,#106021,#106022,#106023),(#106024,#106025,#106026,#106027),(#106028,
#106029,#106030,#106031)),.UNSPECIFIED.,.F.,.F.,.F.,(4,4),(4,4),(-0.002868622011642,
0.477902879803106),(0.0300094532292785,0.036594484664702),.UNSPECIFIED.);
#3460=B_SPLINE_SURFACE_WITH_KNOTS('',3,3,((#106033,#106034,#106035,#106036),
(#106037,#106038,#106039,#106040),(#106041,#106042,#106043,#106044),(#106045,
#106046,#106047,#106048)),.UNSPECIFIED.,.F.,.F.,.F.,(4,4),(4,4),(0.522097120201145,
1.00286823669288),(0.0265907346180634,0.0331702036051743),.UNSPECIFIED.);
#3461=B_SPLINE_SURFACE_WITH_KNOTS('',3,3,((#106056,#106057,#106058,#106059),
(#106060,#106061,#106062,#106063),(#106064,#106065,#106066,#106067),(#106068,
#106069,#106070,#106071)),.UNSPECIFIED.,.F.,.F.,.F.,(4,4),(4,4),(-0.00286848453282375,
0.477902879802511),(0.0400218729466607,0.0466073985929425),
 .UNSPECIFIED.);
#3462=B_SPLINE_SURFACE_WITH_KNOTS('',3,3,((#106088,#106089,#106090,#106091),
(#106092,#106093,#106094,#106095),(#106096,#106097,#106098,#106099),(#106100,
#106101,#106102,#106103)),.UNSPECIFIED.,.F.,.F.,.F.,(4,4),(4,4),(0.,1.00600014639744),
(0.0365944846644989,0.0466073985929176),.UNSPECIFIED.);
#3463=B_SPLINE_SURFACE_WITH_KNOTS('',3,3,((#106104,#106105,#106106,#106107),
(#106108,#106109,#106110,#106111),(#106112,#106113,#106114,#106115),(#106116,
#106117,#106118,#106119)),.UNSPECIFIED.,.F.,.F.,.F.,(4,4),(4,4),(-0.0028678012241247,
0.477902879802034),(0.0500263550859004,0.0565997133101407),
 .UNSPECIFIED.);
#3464=B_SPLINE_SURFACE_WITH_KNOTS('',3,3,((#106121,#106122,#106123,#106124),
(#106125,#106126,#106127,#106128),(#106129,#106130,#106131,#106132),(#106133,
#106134,#106135,#106136)),.UNSPECIFIED.,.F.,.F.,.F.,(4,4),(4,4),(0.522097120203794,
1.00286810177261),(0.0466073985929449,0.0531834925888935),.UNSPECIFIED.);
#3465=B_SPLINE_SURFACE_WITH_KNOTS('',3,3,((#106144,#106145,#106146,#106147),
(#106148,#106149,#106150,#106151),(#106152,#106153,#106154,#106155),(#106156,
#106157,#106158,#106159)),.UNSPECIFIED.,.F.,.F.,.F.,(4,4),(4,4),(-0.00286792598902487,
0.477902879801679),(0.0600156865494608,0.0665898698871168),
 .UNSPECIFIED.);
#3466=B_SPLINE_SURFACE_WITH_KNOTS('',3,3,((#106161,#106162,#106163,#106164),
(#106165,#106166,#106167,#106168),(#106169,#106170,#106171,#106172),(#106173,
#106174,#106175,#106176)),.UNSPECIFIED.,.F.,.F.,.F.,(4,4),(4,4),(0.522097120205029,
1.00286764392032),(0.0565997133101419,0.0631721430887061),.UNSPECIFIED.);
#3467=B_SPLINE_SURFACE_WITH_KNOTS('',3,3,((#106192,#106193,#106194,#106195),
(#106196,#106197,#106198,#106199),(#106200,#106201,#106202,#106203),(#106204,
#106205,#106206,#106207)),.UNSPECIFIED.,.F.,.F.,.F.,(4,4),(4,4),(0.522097120206208,
1.00286833998589),(0.0665898698871188,0.0731716198748447),.UNSPECIFIED.);
#3468=B_SPLINE_SURFACE_WITH_KNOTS('',3,3,((#106208,#106209,#106210,#106211),
(#106212,#106213,#106214,#106215),(#106216,#106217,#106218,#106219),(#106220,
#106221,#106222,#106223)),.UNSPECIFIED.,.F.,.F.,.F.,(4,4),(4,4),(-0.00124731530851986,
0.209045111703167),(0.0700194292965804,0.0749900982978226),
 .UNSPECIFIED.);
#3469=SHAPE_REPRESENTATION_RELATIONSHIP('SRR','None',#107947,#3479);
#3470=SHAPE_REPRESENTATION_RELATIONSHIP('SRR','None',#107948,#3480);
#3471=SHAPE_REPRESENTATION_RELATIONSHIP('SRR','None',#107949,#3481);
#3472=SHAPE_REPRESENTATION_RELATIONSHIP('SRR','None',#107950,#3482);
#3473=SHAPE_REPRESENTATION_RELATIONSHIP('SRR','None',#107951,#3483);
#3474=SHAPE_REPRESENTATION_RELATIONSHIP('SRR','None',#107952,#3484);
#3475=SHAPE_REPRESENTATION_RELATIONSHIP('SRR','None',#107953,#3485);
#3476=SHAPE_REPRESENTATION_RELATIONSHIP('SRR','None',#107954,#3486);
#3477=SHAPE_REPRESENTATION_RELATIONSHIP('SRR','None',#107955,#3487);
#3478=SHAPE_REPRESENTATION_RELATIONSHIP('SRR','None',#107956,#3488);
#3479=ADVANCED_BREP_SHAPE_REPRESENTATION('',(#3499),#107900);
#3480=ADVANCED_BREP_SHAPE_REPRESENTATION('',(#3500),#107901);
#3481=ADVANCED_BREP_SHAPE_REPRESENTATION('',(#3501),#107902);
#3482=ADVANCED_BREP_SHAPE_REPRESENTATION('',(#3502),#107903);
#3483=ADVANCED_BREP_SHAPE_REPRESENTATION('',(#3503),#107904);
#3484=ADVANCED_BREP_SHAPE_REPRESENTATION('',(#3504),#107905);
#3485=ADVANCED_BREP_SHAPE_REPRESENTATION('',(#3505),#107906);
#3486=ADVANCED_BREP_SHAPE_REPRESENTATION('',(#3506),#107907);
#3487=ADVANCED_BREP_SHAPE_REPRESENTATION('',(#3507),#107908);
#3488=ADVANCED_BREP_SHAPE_REPRESENTATION('',(#3508),#107909);
#3489=STYLED_ITEM('',(#108006),#3499);
#3490=STYLED_ITEM('',(#108007),#3500);
#3491=STYLED_ITEM('',(#108008),#3501);
#3492=STYLED_ITEM('',(#108009),#3502);
#3493=STYLED_ITEM('',(#108006),#3503);
#3494=STYLED_ITEM('',(#108010),#3504);
#3495=STYLED_ITEM('',(#108008),#3505);
#3496=STYLED_ITEM('',(#108011),#3506);
#3497=STYLED_ITEM('',(#108006),#3507);
#3498=STYLED_ITEM('',(#108007),#3508);
#3499=MANIFOLD_SOLID_BREP('Body1',#45537);
#3500=MANIFOLD_SOLID_BREP('Body1',#45538);
#3501=MANIFOLD_SOLID_BREP('Body1',#45539);
#3502=MANIFOLD_SOLID_BREP('Body1',#45540);
#3503=MANIFOLD_SOLID_BREP('Body1',#45541);
#3504=MANIFOLD_SOLID_BREP('Body1',#45542);
#3505=MANIFOLD_SOLID_BREP('Body1',#45543);
#3506=MANIFOLD_SOLID_BREP('Body1',#45544);
#3507=MANIFOLD_SOLID_BREP('Body1',#45545);
#3508=MANIFOLD_SOLID_BREP('Body1',#45546);
#3509=FACE_BOUND('',#6685,.T.);
#3510=FACE_BOUND('',#6687,.T.);
#3511=FACE_BOUND('',#6702,.T.);
#3512=FACE_BOUND('',#6707,.T.);
#3513=FACE_BOUND('',#8176,.T.);
#3514=FACE_BOUND('',#9332,.T.);
#3515=FACE_BOUND('',#9334,.T.);
#3516=FACE_BOUND('',#9336,.T.);
#3517=FACE_BOUND('',#9340,.T.);
#3518=FACE_BOUND('',#9342,.T.);
#3519=FACE_BOUND('',#9399,.T.);
#3520=FACE_BOUND('',#9401,.T.);
#3521=FACE_BOUND('',#9403,.T.);
#3522=FACE_BOUND('',#9405,.T.);
#3523=FACE_BOUND('',#9512,.T.);
#3524=FACE_BOUND('',#9516,.T.);
#3525=FACE_BOUND('',#9542,.T.);
#3526=FACE_BOUND('',#9543,.T.);
#3527=FACE_BOUND('',#9544,.T.);
#3528=FACE_BOUND('',#9545,.T.);
#3529=FACE_BOUND('',#9547,.T.);
#3530=FACE_BOUND('',#9548,.T.);
#3531=FACE_BOUND('',#9549,.T.);
#3532=FACE_BOUND('',#9550,.T.);
#3533=FACE_BOUND('',#9551,.T.);
#3534=FACE_BOUND('',#9552,.T.);
#3535=FACE_BOUND('',#9557,.T.);
#3536=FACE_BOUND('',#9563,.T.);
#3537=FACE_BOUND('',#9573,.T.);
#3538=FACE_BOUND('',#9575,.T.);
#3539=FACE_BOUND('',#9577,.T.);
#3540=FACE_BOUND('',#9607,.T.);
#3541=FACE_BOUND('',#9633,.T.);
#3542=PLANE('',#45666);
#3543=PLANE('',#45667);
#3544=PLANE('',#45669);
#3545=PLANE('',#45670);
#3546=PLANE('',#45678);
#3547=PLANE('',#45679);
#3548=PLANE('',#45685);
#3549=PLANE('',#45686);
#3550=PLANE('',#45695);
#3551=PLANE('',#45700);
#3552=PLANE('',#45701);
#3553=PLANE('',#45702);
#3554=PLANE('',#45704);
#3555=PLANE('',#45705);
#3556=PLANE('',#45706);
#3557=PLANE('',#45707);
#3558=PLANE('',#45708);
#3559=PLANE('',#45710);
#3560=PLANE('',#45711);
#3561=PLANE('',#45712);
#3562=PLANE('',#45713);
#3563=PLANE('',#45714);
#3564=PLANE('',#45715);
#3565=PLANE('',#45716);
#3566=PLANE('',#49124);
#3567=PLANE('',#49125);
#3568=PLANE('',#49126);
#3569=PLANE('',#49887);
#3570=PLANE('',#49888);
#3571=PLANE('',#49889);
#3572=PLANE('',#49897);
#3573=PLANE('',#49898);
#3574=PLANE('',#50065);
#3575=PLANE('',#50066);
#3576=PLANE('',#50067);
#3577=PLANE('',#50068);
#3578=PLANE('',#50069);
#3579=PLANE('',#50070);
#3580=PLANE('',#50071);
#3581=PLANE('',#50072);
#3582=PLANE('',#50073);
#3583=PLANE('',#50074);
#3584=PLANE('',#50075);
#3585=PLANE('',#50076);
#3586=PLANE('',#50077);
#3587=PLANE('',#50078);
#3588=PLANE('',#50079);
#3589=PLANE('',#50080);
#3590=PLANE('',#50081);
#3591=PLANE('',#50082);
#3592=PLANE('',#50083);
#3593=PLANE('',#50084);
#3594=PLANE('',#50085);
#3595=PLANE('',#50086);
#3596=PLANE('',#50087);
#3597=PLANE('',#50088);
#3598=PLANE('',#50089);
#3599=PLANE('',#50090);
#3600=PLANE('',#50091);
#3601=PLANE('',#50092);
#3602=PLANE('',#50093);
#3603=PLANE('',#50094);
#3604=PLANE('',#50095);
#3605=PLANE('',#50096);
#3606=PLANE('',#50097);
#3607=PLANE('',#50098);
#3608=PLANE('',#50099);
#3609=PLANE('',#50100);
#3610=PLANE('',#50101);
#3611=PLANE('',#50102);
#3612=PLANE('',#50103);
#3613=PLANE('',#50104);
#3614=PLANE('',#50105);
#3615=PLANE('',#50106);
#3616=PLANE('',#50107);
#3617=PLANE('',#50108);
#3618=PLANE('',#50109);
#3619=PLANE('',#50110);
#3620=PLANE('',#50111);
#3621=PLANE('',#50112);
#3622=PLANE('',#50113);
#3623=PLANE('',#50114);
#3624=PLANE('',#50115);
#3625=PLANE('',#50116);
#3626=PLANE('',#50117);
#3627=PLANE('',#50118);
#3628=PLANE('',#50119);
#3629=PLANE('',#50120);
#3630=PLANE('',#50121);
#3631=PLANE('',#50122);
#3632=PLANE('',#50123);
#3633=PLANE('',#50124);
#3634=PLANE('',#50125);
#3635=PLANE('',#50126);
#3636=PLANE('',#50127);
#3637=PLANE('',#50128);
#3638=PLANE('',#50129);
#3639=PLANE('',#50130);
#3640=PLANE('',#50131);
#3641=PLANE('',#50132);
#3642=PLANE('',#50133);
#3643=PLANE('',#50134);
#3644=PLANE('',#50135);
#3645=PLANE('',#50136);
#3646=PLANE('',#50137);
#3647=PLANE('',#50138);
#3648=PLANE('',#50139);
#3649=PLANE('',#50140);
#3650=PLANE('',#50141);
#3651=PLANE('',#50142);
#3652=PLANE('',#50143);
#3653=PLANE('',#50144);
#3654=PLANE('',#50145);
#3655=PLANE('',#50146);
#3656=PLANE('',#50147);
#3657=PLANE('',#50148);
#3658=PLANE('',#50149);
#3659=PLANE('',#50150);
#3660=PLANE('',#50151);
#3661=PLANE('',#50152);
#3662=PLANE('',#50153);
#3663=PLANE('',#50154);
#3664=PLANE('',#50155);
#3665=PLANE('',#50156);
#3666=PLANE('',#50157);
#3667=PLANE('',#50158);
#3668=PLANE('',#50159);
#3669=PLANE('',#50160);
#3670=PLANE('',#50161);
#3671=PLANE('',#50162);
#3672=PLANE('',#50163);
#3673=PLANE('',#50164);
#3674=PLANE('',#50165);
#3675=PLANE('',#50166);
#3676=PLANE('',#50167);
#3677=PLANE('',#50168);
#3678=PLANE('',#50169);
#3679=PLANE('',#50170);
#3680=PLANE('',#50171);
#3681=PLANE('',#50172);
#3682=PLANE('',#50239);
#3683=PLANE('',#50245);
#3684=PLANE('',#50248);
#3685=PLANE('',#50249);
#3686=PLANE('',#50250);
#3687=PLANE('',#50251);
#3688=PLANE('',#50263);
#3689=PLANE('',#50264);
#3690=PLANE('',#50265);
#3691=PLANE('',#50266);
#3692=PLANE('',#50276);
#3693=PLANE('',#50277);
#3694=PLANE('',#50278);
#3695=PLANE('',#50279);
#3696=PLANE('',#50280);
#3697=PLANE('',#50281);
#3698=PLANE('',#50282);
#3699=PLANE('',#50283);
#3700=PLANE('',#50284);
#3701=PLANE('',#50285);
#3702=PLANE('',#50286);
#3703=PLANE('',#50287);
#3704=PLANE('',#50288);
#3705=PLANE('',#50289);
#3706=PLANE('',#50290);
#3707=PLANE('',#50291);
#3708=PLANE('',#50292);
#3709=PLANE('',#50293);
#3710=PLANE('',#50294);
#3711=PLANE('',#50295);
#3712=PLANE('',#50296);
#3713=PLANE('',#50299);
#3714=PLANE('',#50302);
#3715=PLANE('',#50305);
#3716=PLANE('',#50308);
#3717=PLANE('',#50309);
#3718=PLANE('',#50310);
#3719=PLANE('',#50311);
#3720=PLANE('',#50314);
#3721=PLANE('',#50317);
#3722=PLANE('',#50318);
#3723=PLANE('',#50319);
#3724=PLANE('',#50321);
#3725=PLANE('',#50323);
#3726=PLANE('',#50325);
#3727=PLANE('',#50326);
#3728=PLANE('',#50329);
#3729=PLANE('',#50330);
#3730=PLANE('',#50331);
#3731=PLANE('',#50332);
#3732=PLANE('',#50333);
#3733=PLANE('',#50334);
#3734=PLANE('',#50335);
#3735=PLANE('',#50336);
#3736=PLANE('',#50337);
#3737=PLANE('',#50338);
#3738=PLANE('',#50339);
#3739=PLANE('',#50340);
#3740=PLANE('',#50341);
#3741=PLANE('',#50342);
#3742=PLANE('',#50345);
#3743=PLANE('',#50346);
#3744=PLANE('',#50349);
#3745=PLANE('',#50350);
#3746=PLANE('',#50351);
#3747=PLANE('',#50352);
#3748=PLANE('',#50353);
#3749=PLANE('',#50354);
#3750=PLANE('',#50355);
#3751=PLANE('',#50356);
#3752=PLANE('',#50357);
#3753=PLANE('',#50358);
#3754=PLANE('',#50359);
#3755=PLANE('',#50363);
#3756=PLANE('',#50364);
#3757=PLANE('',#50365);
#3758=FACE_OUTER_BOUND('',#6682,.T.);
#3759=FACE_OUTER_BOUND('',#6683,.T.);
#3760=FACE_OUTER_BOUND('',#6684,.T.);
#3761=FACE_OUTER_BOUND('',#6686,.T.);
#3762=FACE_OUTER_BOUND('',#6688,.T.);
#3763=FACE_OUTER_BOUND('',#6689,.T.);
#3764=FACE_OUTER_BOUND('',#6690,.T.);
#3765=FACE_OUTER_BOUND('',#6691,.T.);
#3766=FACE_OUTER_BOUND('',#6692,.T.);
#3767=FACE_OUTER_BOUND('',#6693,.T.);
#3768=FACE_OUTER_BOUND('',#6694,.T.);
#3769=FACE_OUTER_BOUND('',#6695,.T.);
#3770=FACE_OUTER_BOUND('',#6696,.T.);
#3771=FACE_OUTER_BOUND('',#6697,.T.);
#3772=FACE_OUTER_BOUND('',#6698,.T.);
#3773=FACE_OUTER_BOUND('',#6699,.T.);
#3774=FACE_OUTER_BOUND('',#6700,.T.);
#3775=FACE_OUTER_BOUND('',#6701,.T.);
#3776=FACE_OUTER_BOUND('',#6703,.T.);
#3777=FACE_OUTER_BOUND('',#6704,.T.);
#3778=FACE_OUTER_BOUND('',#6705,.T.);
#3779=FACE_OUTER_BOUND('',#6706,.T.);
#3780=FACE_OUTER_BOUND('',#6708,.T.);
#3781=FACE_OUTER_BOUND('',#6709,.T.);
#3782=FACE_OUTER_BOUND('',#6710,.T.);
#3783=FACE_OUTER_BOUND('',#6711,.T.);
#3784=FACE_OUTER_BOUND('',#6712,.T.);
#3785=FACE_OUTER_BOUND('',#6713,.T.);
#3786=FACE_OUTER_BOUND('',#6714,.T.);
#3787=FACE_OUTER_BOUND('',#6715,.T.);
#3788=FACE_OUTER_BOUND('',#6716,.T.);
#3789=FACE_OUTER_BOUND('',#6717,.T.);
#3790=FACE_OUTER_BOUND('',#6718,.T.);
#3791=FACE_OUTER_BOUND('',#6719,.T.);
#3792=FACE_OUTER_BOUND('',#6720,.T.);
#3793=FACE_OUTER_BOUND('',#6721,.T.);
#3794=FACE_OUTER_BOUND('',#6722,.T.);
#3795=FACE_OUTER_BOUND('',#6723,.T.);
#3796=FACE_OUTER_BOUND('',#6724,.T.);
#3797=FACE_OUTER_BOUND('',#6725,.T.);
#3798=FACE_OUTER_BOUND('',#6726,.T.);
#3799=FACE_OUTER_BOUND('',#6727,.T.);
#3800=FACE_OUTER_BOUND('',#6728,.T.);
#3801=FACE_OUTER_BOUND('',#6729,.T.);
#3802=FACE_OUTER_BOUND('',#6730,.T.);
#3803=FACE_OUTER_BOUND('',#6731,.T.);
#3804=FACE_OUTER_BOUND('',#6732,.T.);
#3805=FACE_OUTER_BOUND('',#6733,.T.);
#3806=FACE_OUTER_BOUND('',#6734,.T.);
#3807=FACE_OUTER_BOUND('',#6735,.T.);
#3808=FACE_OUTER_BOUND('',#6736,.T.);
#3809=FACE_OUTER_BOUND('',#6737,.T.);
#3810=FACE_OUTER_BOUND('',#6738,.T.);
#3811=FACE_OUTER_BOUND('',#6739,.T.);
#3812=FACE_OUTER_BOUND('',#6740,.T.);
#3813=FACE_OUTER_BOUND('',#6741,.T.);
#3814=FACE_OUTER_BOUND('',#6742,.T.);
#3815=FACE_OUTER_BOUND('',#6743,.T.);
#3816=FACE_OUTER_BOUND('',#6744,.T.);
#3817=FACE_OUTER_BOUND('',#6745,.T.);
#3818=FACE_OUTER_BOUND('',#6746,.T.);
#3819=FACE_OUTER_BOUND('',#6747,.T.);
#3820=FACE_OUTER_BOUND('',#6748,.T.);
#3821=FACE_OUTER_BOUND('',#6749,.T.);
#3822=FACE_OUTER_BOUND('',#6750,.T.);
#3823=FACE_OUTER_BOUND('',#6751,.T.);
#3824=FACE_OUTER_BOUND('',#6752,.T.);
#3825=FACE_OUTER_BOUND('',#6753,.T.);
#3826=FACE_OUTER_BOUND('',#6754,.T.);
#3827=FACE_OUTER_BOUND('',#6755,.T.);
#3828=FACE_OUTER_BOUND('',#6756,.T.);
#3829=FACE_OUTER_BOUND('',#6757,.T.);
#3830=FACE_OUTER_BOUND('',#6758,.T.);
#3831=FACE_OUTER_BOUND('',#6759,.T.);
#3832=FACE_OUTER_BOUND('',#6760,.T.);
#3833=FACE_OUTER_BOUND('',#6761,.T.);
#3834=FACE_OUTER_BOUND('',#6762,.T.);
#3835=FACE_OUTER_BOUND('',#6763,.T.);
#3836=FACE_OUTER_BOUND('',#6764,.T.);
#3837=FACE_OUTER_BOUND('',#6765,.T.);
#3838=FACE_OUTER_BOUND('',#6766,.T.);
#3839=FACE_OUTER_BOUND('',#6767,.T.);
#3840=FACE_OUTER_BOUND('',#6768,.T.);
#3841=FACE_OUTER_BOUND('',#6769,.T.);
#3842=FACE_OUTER_BOUND('',#6770,.T.);
#3843=FACE_OUTER_BOUND('',#6771,.T.);
#3844=FACE_OUTER_BOUND('',#6772,.T.);
#3845=FACE_OUTER_BOUND('',#6773,.T.);
#3846=FACE_OUTER_BOUND('',#6774,.T.);
#3847=FACE_OUTER_BOUND('',#6775,.T.);
#3848=FACE_OUTER_BOUND('',#6776,.T.);
#3849=FACE_OUTER_BOUND('',#6777,.T.);
#3850=FACE_OUTER_BOUND('',#6778,.T.);
#3851=FACE_OUTER_BOUND('',#6779,.T.);
#3852=FACE_OUTER_BOUND('',#6780,.T.);
#3853=FACE_OUTER_BOUND('',#6781,.T.);
#3854=FACE_OUTER_BOUND('',#6782,.T.);
#3855=FACE_OUTER_BOUND('',#6783,.T.);
#3856=FACE_OUTER_BOUND('',#6784,.T.);
#3857=FACE_OUTER_BOUND('',#6785,.T.);
#3858=FACE_OUTER_BOUND('',#6786,.T.);
#3859=FACE_OUTER_BOUND('',#6787,.T.);
#3860=FACE_OUTER_BOUND('',#6788,.T.);
#3861=FACE_OUTER_BOUND('',#6789,.T.);
#3862=FACE_OUTER_BOUND('',#6790,.T.);
#3863=FACE_OUTER_BOUND('',#6791,.T.);
#3864=FACE_OUTER_BOUND('',#6792,.T.);
#3865=FACE_OUTER_BOUND('',#6793,.T.);
#3866=FACE_OUTER_BOUND('',#6794,.T.);
#3867=FACE_OUTER_BOUND('',#6795,.T.);
#3868=FACE_OUTER_BOUND('',#6796,.T.);
#3869=FACE_OUTER_BOUND('',#6797,.T.);
#3870=FACE_OUTER_BOUND('',#6798,.T.);
#3871=FACE_OUTER_BOUND('',#6799,.T.);
#3872=FACE_OUTER_BOUND('',#6800,.T.);
#3873=FACE_OUTER_BOUND('',#6801,.T.);
#3874=FACE_OUTER_BOUND('',#6802,.T.);
#3875=FACE_OUTER_BOUND('',#6803,.T.);
#3876=FACE_OUTER_BOUND('',#6804,.T.);
#3877=FACE_OUTER_BOUND('',#6805,.T.);
#3878=FACE_OUTER_BOUND('',#6806,.T.);
#3879=FACE_OUTER_BOUND('',#6807,.T.);
#3880=FACE_OUTER_BOUND('',#6808,.T.);
#3881=FACE_OUTER_BOUND('',#6809,.T.);
#3882=FACE_OUTER_BOUND('',#6810,.T.);
#3883=FACE_OUTER_BOUND('',#6811,.T.);
#3884=FACE_OUTER_BOUND('',#6812,.T.);
#3885=FACE_OUTER_BOUND('',#6813,.T.);
#3886=FACE_OUTER_BOUND('',#6814,.T.);
#3887=FACE_OUTER_BOUND('',#6815,.T.);
#3888=FACE_OUTER_BOUND('',#6816,.T.);
#3889=FACE_OUTER_BOUND('',#6817,.T.);
#3890=FACE_OUTER_BOUND('',#6818,.T.);
#3891=FACE_OUTER_BOUND('',#6819,.T.);
#3892=FACE_OUTER_BOUND('',#6820,.T.);
#3893=FACE_OUTER_BOUND('',#6821,.T.);
#3894=FACE_OUTER_BOUND('',#6822,.T.);
#3895=FACE_OUTER_BOUND('',#6823,.T.);
#3896=FACE_OUTER_BOUND('',#6824,.T.);
#3897=FACE_OUTER_BOUND('',#6825,.T.);
#3898=FACE_OUTER_BOUND('',#6826,.T.);
#3899=FACE_OUTER_BOUND('',#6827,.T.);
#3900=FACE_OUTER_BOUND('',#6828,.T.);
#3901=FACE_OUTER_BOUND('',#6829,.T.);
#3902=FACE_OUTER_BOUND('',#6830,.T.);
#3903=FACE_OUTER_BOUND('',#6831,.T.);
#3904=FACE_OUTER_BOUND('',#6832,.T.);
#3905=FACE_OUTER_BOUND('',#6833,.T.);
#3906=FACE_OUTER_BOUND('',#6834,.T.);
#3907=FACE_OUTER_BOUND('',#6835,.T.);
#3908=FACE_OUTER_BOUND('',#6836,.T.);
#3909=FACE_OUTER_BOUND('',#6837,.T.);
#3910=FACE_OUTER_BOUND('',#6838,.T.);
#3911=FACE_OUTER_BOUND('',#6839,.T.);
#3912=FACE_OUTER_BOUND('',#6840,.T.);
#3913=FACE_OUTER_BOUND('',#6841,.T.);
#3914=FACE_OUTER_BOUND('',#6842,.T.);
#3915=FACE_OUTER_BOUND('',#6843,.T.);
#3916=FACE_OUTER_BOUND('',#6844,.T.);
#3917=FACE_OUTER_BOUND('',#6845,.T.);
#3918=FACE_OUTER_BOUND('',#6846,.T.);
#3919=FACE_OUTER_BOUND('',#6847,.T.);
#3920=FACE_OUTER_BOUND('',#6848,.T.);
#3921=FACE_OUTER_BOUND('',#6849,.T.);
#3922=FACE_OUTER_BOUND('',#6850,.T.);
#3923=FACE_OUTER_BOUND('',#6851,.T.);
#3924=FACE_OUTER_BOUND('',#6852,.T.);
#3925=FACE_OUTER_BOUND('',#6853,.T.);
#3926=FACE_OUTER_BOUND('',#6854,.T.);
#3927=FACE_OUTER_BOUND('',#6855,.T.);
#3928=FACE_OUTER_BOUND('',#6856,.T.);
#3929=FACE_OUTER_BOUND('',#6857,.T.);
#3930=FACE_OUTER_BOUND('',#6858,.T.);
#3931=FACE_OUTER_BOUND('',#6859,.T.);
#3932=FACE_OUTER_BOUND('',#6860,.T.);
#3933=FACE_OUTER_BOUND('',#6861,.T.);
#3934=FACE_OUTER_BOUND('',#6862,.T.);
#3935=FACE_OUTER_BOUND('',#6863,.T.);
#3936=FACE_OUTER_BOUND('',#6864,.T.);
#3937=FACE_OUTER_BOUND('',#6865,.T.);
#3938=FACE_OUTER_BOUND('',#6866,.T.);
#3939=FACE_OUTER_BOUND('',#6867,.T.);
#3940=FACE_OUTER_BOUND('',#6868,.T.);
#3941=FACE_OUTER_BOUND('',#6869,.T.);
#3942=FACE_OUTER_BOUND('',#6870,.T.);
#3943=FACE_OUTER_BOUND('',#6871,.T.);
#3944=FACE_OUTER_BOUND('',#6872,.T.);
#3945=FACE_OUTER_BOUND('',#6873,.T.);
#3946=FACE_OUTER_BOUND('',#6874,.T.);
#3947=FACE_OUTER_BOUND('',#6875,.T.);
#3948=FACE_OUTER_BOUND('',#6876,.T.);
#3949=FACE_OUTER_BOUND('',#6877,.T.);
#3950=FACE_OUTER_BOUND('',#6878,.T.);
#3951=FACE_OUTER_BOUND('',#6879,.T.);
#3952=FACE_OUTER_BOUND('',#6880,.T.);
#3953=FACE_OUTER_BOUND('',#6881,.T.);
#3954=FACE_OUTER_BOUND('',#6882,.T.);
#3955=FACE_OUTER_BOUND('',#6883,.T.);
#3956=FACE_OUTER_BOUND('',#6884,.T.);
#3957=FACE_OUTER_BOUND('',#6885,.T.);
#3958=FACE_OUTER_BOUND('',#6886,.T.);
#3959=FACE_OUTER_BOUND('',#6887,.T.);
#3960=FACE_OUTER_BOUND('',#6888,.T.);
#3961=FACE_OUTER_BOUND('',#6889,.T.);
#3962=FACE_OUTER_BOUND('',#6890,.T.);
#3963=FACE_OUTER_BOUND('',#6891,.T.);
#3964=FACE_OUTER_BOUND('',#6892,.T.);
#3965=FACE_OUTER_BOUND('',#6893,.T.);
#3966=FACE_OUTER_BOUND('',#6894,.T.);
#3967=FACE_OUTER_BOUND('',#6895,.T.);
#3968=FACE_OUTER_BOUND('',#6896,.T.);
#3969=FACE_OUTER_BOUND('',#6897,.T.);
#3970=FACE_OUTER_BOUND('',#6898,.T.);
#3971=FACE_OUTER_BOUND('',#6899,.T.);
#3972=FACE_OUTER_BOUND('',#6900,.T.);
#3973=FACE_OUTER_BOUND('',#6901,.T.);
#3974=FACE_OUTER_BOUND('',#6902,.T.);
#3975=FACE_OUTER_BOUND('',#6903,.T.);
#3976=FACE_OUTER_BOUND('',#6904,.T.);
#3977=FACE_OUTER_BOUND('',#6905,.T.);
#3978=FACE_OUTER_BOUND('',#6906,.T.);
#3979=FACE_OUTER_BOUND('',#6907,.T.);
#3980=FACE_OUTER_BOUND('',#6908,.T.);
#3981=FACE_OUTER_BOUND('',#6909,.T.);
#3982=FACE_OUTER_BOUND('',#6910,.T.);
#3983=FACE_OUTER_BOUND('',#6911,.T.);
#3984=FACE_OUTER_BOUND('',#6912,.T.);
#3985=FACE_OUTER_BOUND('',#6913,.T.);
#3986=FACE_OUTER_BOUND('',#6914,.T.);
#3987=FACE_OUTER_BOUND('',#6915,.T.);
#3988=FACE_OUTER_BOUND('',#6916,.T.);
#3989=FACE_OUTER_BOUND('',#6917,.T.);
#3990=FACE_OUTER_BOUND('',#6918,.T.);
#3991=FACE_OUTER_BOUND('',#6919,.T.);
#3992=FACE_OUTER_BOUND('',#6920,.T.);
#3993=FACE_OUTER_BOUND('',#6921,.T.);
#3994=FACE_OUTER_BOUND('',#6922,.T.);
#3995=FACE_OUTER_BOUND('',#6923,.T.);
#3996=FACE_OUTER_BOUND('',#6924,.T.);
#3997=FACE_OUTER_BOUND('',#6925,.T.);
#3998=FACE_OUTER_BOUND('',#6926,.T.);
#3999=FACE_OUTER_BOUND('',#6927,.T.);
#4000=FACE_OUTER_BOUND('',#6928,.T.);
#4001=FACE_OUTER_BOUND('',#6929,.T.);
#4002=FACE_OUTER_BOUND('',#6930,.T.);
#4003=FACE_OUTER_BOUND('',#6931,.T.);
#4004=FACE_OUTER_BOUND('',#6932,.T.);
#4005=FACE_OUTER_BOUND('',#6933,.T.);
#4006=FACE_OUTER_BOUND('',#6934,.T.);
#4007=FACE_OUTER_BOUND('',#6935,.T.);
#4008=FACE_OUTER_BOUND('',#6936,.T.);
#4009=FACE_OUTER_BOUND('',#6937,.T.);
#4010=FACE_OUTER_BOUND('',#6938,.T.);
#4011=FACE_OUTER_BOUND('',#6939,.T.);
#4012=FACE_OUTER_BOUND('',#6940,.T.);
#4013=FACE_OUTER_BOUND('',#6941,.T.);
#4014=FACE_OUTER_BOUND('',#6942,.T.);
#4015=FACE_OUTER_BOUND('',#6943,.T.);
#4016=FACE_OUTER_BOUND('',#6944,.T.);
#4017=FACE_OUTER_BOUND('',#6945,.T.);
#4018=FACE_OUTER_BOUND('',#6946,.T.);
#4019=FACE_OUTER_BOUND('',#6947,.T.);
#4020=FACE_OUTER_BOUND('',#6948,.T.);
#4021=FACE_OUTER_BOUND('',#6949,.T.);
#4022=FACE_OUTER_BOUND('',#6950,.T.);
#4023=FACE_OUTER_BOUND('',#6951,.T.);
#4024=FACE_OUTER_BOUND('',#6952,.T.);
#4025=FACE_OUTER_BOUND('',#6953,.T.);
#4026=FACE_OUTER_BOUND('',#6954,.T.);
#4027=FACE_OUTER_BOUND('',#6955,.T.);
#4028=FACE_OUTER_BOUND('',#6956,.T.);
#4029=FACE_OUTER_BOUND('',#6957,.T.);
#4030=FACE_OUTER_BOUND('',#6958,.T.);
#4031=FACE_OUTER_BOUND('',#6959,.T.);
#4032=FACE_OUTER_BOUND('',#6960,.T.);
#4033=FACE_OUTER_BOUND('',#6961,.T.);
#4034=FACE_OUTER_BOUND('',#6962,.T.);
#4035=FACE_OUTER_BOUND('',#6963,.T.);
#4036=FACE_OUTER_BOUND('',#6964,.T.);
#4037=FACE_OUTER_BOUND('',#6965,.T.);
#4038=FACE_OUTER_BOUND('',#6966,.T.);
#4039=FACE_OUTER_BOUND('',#6967,.T.);
#4040=FACE_OUTER_BOUND('',#6968,.T.);
#4041=FACE_OUTER_BOUND('',#6969,.T.);
#4042=FACE_OUTER_BOUND('',#6970,.T.);
#4043=FACE_OUTER_BOUND('',#6971,.T.);
#4044=FACE_OUTER_BOUND('',#6972,.T.);
#4045=FACE_OUTER_BOUND('',#6973,.T.);
#4046=FACE_OUTER_BOUND('',#6974,.T.);
#4047=FACE_OUTER_BOUND('',#6975,.T.);
#4048=FACE_OUTER_BOUND('',#6976,.T.);
#4049=FACE_OUTER_BOUND('',#6977,.T.);
#4050=FACE_OUTER_BOUND('',#6978,.T.);
#4051=FACE_OUTER_BOUND('',#6979,.T.);
#4052=FACE_OUTER_BOUND('',#6980,.T.);
#4053=FACE_OUTER_BOUND('',#6981,.T.);
#4054=FACE_OUTER_BOUND('',#6982,.T.);
#4055=FACE_OUTER_BOUND('',#6983,.T.);
#4056=FACE_OUTER_BOUND('',#6984,.T.);
#4057=FACE_OUTER_BOUND('',#6985,.T.);
#4058=FACE_OUTER_BOUND('',#6986,.T.);
#4059=FACE_OUTER_BOUND('',#6987,.T.);
#4060=FACE_OUTER_BOUND('',#6988,.T.);
#4061=FACE_OUTER_BOUND('',#6989,.T.);
#4062=FACE_OUTER_BOUND('',#6990,.T.);
#4063=FACE_OUTER_BOUND('',#6991,.T.);
#4064=FACE_OUTER_BOUND('',#6992,.T.);
#4065=FACE_OUTER_BOUND('',#6993,.T.);
#4066=FACE_OUTER_BOUND('',#6994,.T.);
#4067=FACE_OUTER_BOUND('',#6995,.T.);
#4068=FACE_OUTER_BOUND('',#6996,.T.);
#4069=FACE_OUTER_BOUND('',#6997,.T.);
#4070=FACE_OUTER_BOUND('',#6998,.T.);
#4071=FACE_OUTER_BOUND('',#6999,.T.);
#4072=FACE_OUTER_BOUND('',#7000,.T.);
#4073=FACE_OUTER_BOUND('',#7001,.T.);
#4074=FACE_OUTER_BOUND('',#7002,.T.);
#4075=FACE_OUTER_BOUND('',#7003,.T.);
#4076=FACE_OUTER_BOUND('',#7004,.T.);
#4077=FACE_OUTER_BOUND('',#7005,.T.);
#4078=FACE_OUTER_BOUND('',#7006,.T.);
#4079=FACE_OUTER_BOUND('',#7007,.T.);
#4080=FACE_OUTER_BOUND('',#7008,.T.);
#4081=FACE_OUTER_BOUND('',#7009,.T.);
#4082=FACE_OUTER_BOUND('',#7010,.T.);
#4083=FACE_OUTER_BOUND('',#7011,.T.);
#4084=FACE_OUTER_BOUND('',#7012,.T.);
#4085=FACE_OUTER_BOUND('',#7013,.T.);
#4086=FACE_OUTER_BOUND('',#7014,.T.);
#4087=FACE_OUTER_BOUND('',#7015,.T.);
#4088=FACE_OUTER_BOUND('',#7016,.T.);
#4089=FACE_OUTER_BOUND('',#7017,.T.);
#4090=FACE_OUTER_BOUND('',#7018,.T.);
#4091=FACE_OUTER_BOUND('',#7019,.T.);
#4092=FACE_OUTER_BOUND('',#7020,.T.);
#4093=FACE_OUTER_BOUND('',#7021,.T.);
#4094=FACE_OUTER_BOUND('',#7022,.T.);
#4095=FACE_OUTER_BOUND('',#7023,.T.);
#4096=FACE_OUTER_BOUND('',#7024,.T.);
#4097=FACE_OUTER_BOUND('',#7025,.T.);
#4098=FACE_OUTER_BOUND('',#7026,.T.);
#4099=FACE_OUTER_BOUND('',#7027,.T.);
#4100=FACE_OUTER_BOUND('',#7028,.T.);
#4101=FACE_OUTER_BOUND('',#7029,.T.);
#4102=FACE_OUTER_BOUND('',#7030,.T.);
#4103=FACE_OUTER_BOUND('',#7031,.T.);
#4104=FACE_OUTER_BOUND('',#7032,.T.);
#4105=FACE_OUTER_BOUND('',#7033,.T.);
#4106=FACE_OUTER_BOUND('',#7034,.T.);
#4107=FACE_OUTER_BOUND('',#7035,.T.);
#4108=FACE_OUTER_BOUND('',#7036,.T.);
#4109=FACE_OUTER_BOUND('',#7037,.T.);
#4110=FACE_OUTER_BOUND('',#7038,.T.);
#4111=FACE_OUTER_BOUND('',#7039,.T.);
#4112=FACE_OUTER_BOUND('',#7040,.T.);
#4113=FACE_OUTER_BOUND('',#7041,.T.);
#4114=FACE_OUTER_BOUND('',#7042,.T.);
#4115=FACE_OUTER_BOUND('',#7043,.T.);
#4116=FACE_OUTER_BOUND('',#7044,.T.);
#4117=FACE_OUTER_BOUND('',#7045,.T.);
#4118=FACE_OUTER_BOUND('',#7046,.T.);
#4119=FACE_OUTER_BOUND('',#7047,.T.);
#4120=FACE_OUTER_BOUND('',#7048,.T.);
#4121=FACE_OUTER_BOUND('',#7049,.T.);
#4122=FACE_OUTER_BOUND('',#7050,.T.);
#4123=FACE_OUTER_BOUND('',#7051,.T.);
#4124=FACE_OUTER_BOUND('',#7052,.T.);
#4125=FACE_OUTER_BOUND('',#7053,.T.);
#4126=FACE_OUTER_BOUND('',#7054,.T.);
#4127=FACE_OUTER_BOUND('',#7055,.T.);
#4128=FACE_OUTER_BOUND('',#7056,.T.);
#4129=FACE_OUTER_BOUND('',#7057,.T.);
#4130=FACE_OUTER_BOUND('',#7058,.T.);
#4131=FACE_OUTER_BOUND('',#7059,.T.);
#4132=FACE_OUTER_BOUND('',#7060,.T.);
#4133=FACE_OUTER_BOUND('',#7061,.T.);
#4134=FACE_OUTER_BOUND('',#7062,.T.);
#4135=FACE_OUTER_BOUND('',#7063,.T.);
#4136=FACE_OUTER_BOUND('',#7064,.T.);
#4137=FACE_OUTER_BOUND('',#7065,.T.);
#4138=FACE_OUTER_BOUND('',#7066,.T.);
#4139=FACE_OUTER_BOUND('',#7067,.T.);
#4140=FACE_OUTER_BOUND('',#7068,.T.);
#4141=FACE_OUTER_BOUND('',#7069,.T.);
#4142=FACE_OUTER_BOUND('',#7070,.T.);
#4143=FACE_OUTER_BOUND('',#7071,.T.);
#4144=FACE_OUTER_BOUND('',#7072,.T.);
#4145=FACE_OUTER_BOUND('',#7073,.T.);
#4146=FACE_OUTER_BOUND('',#7074,.T.);
#4147=FACE_OUTER_BOUND('',#7075,.T.);
#4148=FACE_OUTER_BOUND('',#7076,.T.);
#4149=FACE_OUTER_BOUND('',#7077,.T.);
#4150=FACE_OUTER_BOUND('',#7078,.T.);
#4151=FACE_OUTER_BOUND('',#7079,.T.);
#4152=FACE_OUTER_BOUND('',#7080,.T.);
#4153=FACE_OUTER_BOUND('',#7081,.T.);
#4154=FACE_OUTER_BOUND('',#7082,.T.);
#4155=FACE_OUTER_BOUND('',#7083,.T.);
#4156=FACE_OUTER_BOUND('',#7084,.T.);
#4157=FACE_OUTER_BOUND('',#7085,.T.);
#4158=FACE_OUTER_BOUND('',#7086,.T.);
#4159=FACE_OUTER_BOUND('',#7087,.T.);
#4160=FACE_OUTER_BOUND('',#7088,.T.);
#4161=FACE_OUTER_BOUND('',#7089,.T.);
#4162=FACE_OUTER_BOUND('',#7090,.T.);
#4163=FACE_OUTER_BOUND('',#7091,.T.);
#4164=FACE_OUTER_BOUND('',#7092,.T.);
#4165=FACE_OUTER_BOUND('',#7093,.T.);
#4166=FACE_OUTER_BOUND('',#7094,.T.);
#4167=FACE_OUTER_BOUND('',#7095,.T.);
#4168=FACE_OUTER_BOUND('',#7096,.T.);
#4169=FACE_OUTER_BOUND('',#7097,.T.);
#4170=FACE_OUTER_BOUND('',#7098,.T.);
#4171=FACE_OUTER_BOUND('',#7099,.T.);
#4172=FACE_OUTER_BOUND('',#7100,.T.);
#4173=FACE_OUTER_BOUND('',#7101,.T.);
#4174=FACE_OUTER_BOUND('',#7102,.T.);
#4175=FACE_OUTER_BOUND('',#7103,.T.);
#4176=FACE_OUTER_BOUND('',#7104,.T.);
#4177=FACE_OUTER_BOUND('',#7105,.T.);
#4178=FACE_OUTER_BOUND('',#7106,.T.);
#4179=FACE_OUTER_BOUND('',#7107,.T.);
#4180=FACE_OUTER_BOUND('',#7108,.T.);
#4181=FACE_OUTER_BOUND('',#7109,.T.);
#4182=FACE_OUTER_BOUND('',#7110,.T.);
#4183=FACE_OUTER_BOUND('',#7111,.T.);
#4184=FACE_OUTER_BOUND('',#7112,.T.);
#4185=FACE_OUTER_BOUND('',#7113,.T.);
#4186=FACE_OUTER_BOUND('',#7114,.T.);
#4187=FACE_OUTER_BOUND('',#7115,.T.);
#4188=FACE_OUTER_BOUND('',#7116,.T.);
#4189=FACE_OUTER_BOUND('',#7117,.T.);
#4190=FACE_OUTER_BOUND('',#7118,.T.);
#4191=FACE_OUTER_BOUND('',#7119,.T.);
#4192=FACE_OUTER_BOUND('',#7120,.T.);
#4193=FACE_OUTER_BOUND('',#7121,.T.);
#4194=FACE_OUTER_BOUND('',#7122,.T.);
#4195=FACE_OUTER_BOUND('',#7123,.T.);
#4196=FACE_OUTER_BOUND('',#7124,.T.);
#4197=FACE_OUTER_BOUND('',#7125,.T.);
#4198=FACE_OUTER_BOUND('',#7126,.T.);
#4199=FACE_OUTER_BOUND('',#7127,.T.);
#4200=FACE_OUTER_BOUND('',#7128,.T.);
#4201=FACE_OUTER_BOUND('',#7129,.T.);
#4202=FACE_OUTER_BOUND('',#7130,.T.);
#4203=FACE_OUTER_BOUND('',#7131,.T.);
#4204=FACE_OUTER_BOUND('',#7132,.T.);
#4205=FACE_OUTER_BOUND('',#7133,.T.);
#4206=FACE_OUTER_BOUND('',#7134,.T.);
#4207=FACE_OUTER_BOUND('',#7135,.T.);
#4208=FACE_OUTER_BOUND('',#7136,.T.);
#4209=FACE_OUTER_BOUND('',#7137,.T.);
#4210=FACE_OUTER_BOUND('',#7138,.T.);
#4211=FACE_OUTER_BOUND('',#7139,.T.);
#4212=FACE_OUTER_BOUND('',#7140,.T.);
#4213=FACE_OUTER_BOUND('',#7141,.T.);
#4214=FACE_OUTER_BOUND('',#7142,.T.);
#4215=FACE_OUTER_BOUND('',#7143,.T.);
#4216=FACE_OUTER_BOUND('',#7144,.T.);
#4217=FACE_OUTER_BOUND('',#7145,.T.);
#4218=FACE_OUTER_BOUND('',#7146,.T.);
#4219=FACE_OUTER_BOUND('',#7147,.T.);
#4220=FACE_OUTER_BOUND('',#7148,.T.);
#4221=FACE_OUTER_BOUND('',#7149,.T.);
#4222=FACE_OUTER_BOUND('',#7150,.T.);
#4223=FACE_OUTER_BOUND('',#7151,.T.);
#4224=FACE_OUTER_BOUND('',#7152,.T.);
#4225=FACE_OUTER_BOUND('',#7153,.T.);
#4226=FACE_OUTER_BOUND('',#7154,.T.);
#4227=FACE_OUTER_BOUND('',#7155,.T.);
#4228=FACE_OUTER_BOUND('',#7156,.T.);
#4229=FACE_OUTER_BOUND('',#7157,.T.);
#4230=FACE_OUTER_BOUND('',#7158,.T.);
#4231=FACE_OUTER_BOUND('',#7159,.T.);
#4232=FACE_OUTER_BOUND('',#7160,.T.);
#4233=FACE_OUTER_BOUND('',#7161,.T.);
#4234=FACE_OUTER_BOUND('',#7162,.T.);
#4235=FACE_OUTER_BOUND('',#7163,.T.);
#4236=FACE_OUTER_BOUND('',#7164,.T.);
#4237=FACE_OUTER_BOUND('',#7165,.T.);
#4238=FACE_OUTER_BOUND('',#7166,.T.);
#4239=FACE_OUTER_BOUND('',#7167,.T.);
#4240=FACE_OUTER_BOUND('',#7168,.T.);
#4241=FACE_OUTER_BOUND('',#7169,.T.);
#4242=FACE_OUTER_BOUND('',#7170,.T.);
#4243=FACE_OUTER_BOUND('',#7171,.T.);
#4244=FACE_OUTER_BOUND('',#7172,.T.);
#4245=FACE_OUTER_BOUND('',#7173,.T.);
#4246=FACE_OUTER_BOUND('',#7174,.T.);
#4247=FACE_OUTER_BOUND('',#7175,.T.);
#4248=FACE_OUTER_BOUND('',#7176,.T.);
#4249=FACE_OUTER_BOUND('',#7177,.T.);
#4250=FACE_OUTER_BOUND('',#7178,.T.);
#4251=FACE_OUTER_BOUND('',#7179,.T.);
#4252=FACE_OUTER_BOUND('',#7180,.T.);
#4253=FACE_OUTER_BOUND('',#7181,.T.);
#4254=FACE_OUTER_BOUND('',#7182,.T.);
#4255=FACE_OUTER_BOUND('',#7183,.T.);
#4256=FACE_OUTER_BOUND('',#7184,.T.);
#4257=FACE_OUTER_BOUND('',#7185,.T.);
#4258=FACE_OUTER_BOUND('',#7186,.T.);
#4259=FACE_OUTER_BOUND('',#7187,.T.);
#4260=FACE_OUTER_BOUND('',#7188,.T.);
#4261=FACE_OUTER_BOUND('',#7189,.T.);
#4262=FACE_OUTER_BOUND('',#7190,.T.);
#4263=FACE_OUTER_BOUND('',#7191,.T.);
#4264=FACE_OUTER_BOUND('',#7192,.T.);
#4265=FACE_OUTER_BOUND('',#7193,.T.);
#4266=FACE_OUTER_BOUND('',#7194,.T.);
#4267=FACE_OUTER_BOUND('',#7195,.T.);
#4268=FACE_OUTER_BOUND('',#7196,.T.);
#4269=FACE_OUTER_BOUND('',#7197,.T.);
#4270=FACE_OUTER_BOUND('',#7198,.T.);
#4271=FACE_OUTER_BOUND('',#7199,.T.);
#4272=FACE_OUTER_BOUND('',#7200,.T.);
#4273=FACE_OUTER_BOUND('',#7201,.T.);
#4274=FACE_OUTER_BOUND('',#7202,.T.);
#4275=FACE_OUTER_BOUND('',#7203,.T.);
#4276=FACE_OUTER_BOUND('',#7204,.T.);
#4277=FACE_OUTER_BOUND('',#7205,.T.);
#4278=FACE_OUTER_BOUND('',#7206,.T.);
#4279=FACE_OUTER_BOUND('',#7207,.T.);
#4280=FACE_OUTER_BOUND('',#7208,.T.);
#4281=FACE_OUTER_BOUND('',#7209,.T.);
#4282=FACE_OUTER_BOUND('',#7210,.T.);
#4283=FACE_OUTER_BOUND('',#7211,.T.);
#4284=FACE_OUTER_BOUND('',#7212,.T.);
#4285=FACE_OUTER_BOUND('',#7213,.T.);
#4286=FACE_OUTER_BOUND('',#7214,.T.);
#4287=FACE_OUTER_BOUND('',#7215,.T.);
#4288=FACE_OUTER_BOUND('',#7216,.T.);
#4289=FACE_OUTER_BOUND('',#7217,.T.);
#4290=FACE_OUTER_BOUND('',#7218,.T.);
#4291=FACE_OUTER_BOUND('',#7219,.T.);
#4292=FACE_OUTER_BOUND('',#7220,.T.);
#4293=FACE_OUTER_BOUND('',#7221,.T.);
#4294=FACE_OUTER_BOUND('',#7222,.T.);
#4295=FACE_OUTER_BOUND('',#7223,.T.);
#4296=FACE_OUTER_BOUND('',#7224,.T.);
#4297=FACE_OUTER_BOUND('',#7225,.T.);
#4298=FACE_OUTER_BOUND('',#7226,.T.);
#4299=FACE_OUTER_BOUND('',#7227,.T.);
#4300=FACE_OUTER_BOUND('',#7228,.T.);
#4301=FACE_OUTER_BOUND('',#7229,.T.);
#4302=FACE_OUTER_BOUND('',#7230,.T.);
#4303=FACE_OUTER_BOUND('',#7231,.T.);
#4304=FACE_OUTER_BOUND('',#7232,.T.);
#4305=FACE_OUTER_BOUND('',#7233,.T.);
#4306=FACE_OUTER_BOUND('',#7234,.T.);
#4307=FACE_OUTER_BOUND('',#7235,.T.);
#4308=FACE_OUTER_BOUND('',#7236,.T.);
#4309=FACE_OUTER_BOUND('',#7237,.T.);
#4310=FACE_OUTER_BOUND('',#7238,.T.);
#4311=FACE_OUTER_BOUND('',#7239,.T.);
#4312=FACE_OUTER_BOUND('',#7240,.T.);
#4313=FACE_OUTER_BOUND('',#7241,.T.);
#4314=FACE_OUTER_BOUND('',#7242,.T.);
#4315=FACE_OUTER_BOUND('',#7243,.T.);
#4316=FACE_OUTER_BOUND('',#7244,.T.);
#4317=FACE_OUTER_BOUND('',#7245,.T.);
#4318=FACE_OUTER_BOUND('',#7246,.T.);
#4319=FACE_OUTER_BOUND('',#7247,.T.);
#4320=FACE_OUTER_BOUND('',#7248,.T.);
#4321=FACE_OUTER_BOUND('',#7249,.T.);
#4322=FACE_OUTER_BOUND('',#7250,.T.);
#4323=FACE_OUTER_BOUND('',#7251,.T.);
#4324=FACE_OUTER_BOUND('',#7252,.T.);
#4325=FACE_OUTER_BOUND('',#7253,.T.);
#4326=FACE_OUTER_BOUND('',#7254,.T.);
#4327=FACE_OUTER_BOUND('',#7255,.T.);
#4328=FACE_OUTER_BOUND('',#7256,.T.);
#4329=FACE_OUTER_BOUND('',#7257,.T.);
#4330=FACE_OUTER_BOUND('',#7258,.T.);
#4331=FACE_OUTER_BOUND('',#7259,.T.);
#4332=FACE_OUTER_BOUND('',#7260,.T.);
#4333=FACE_OUTER_BOUND('',#7261,.T.);
#4334=FACE_OUTER_BOUND('',#7262,.T.);
#4335=FACE_OUTER_BOUND('',#7263,.T.);
#4336=FACE_OUTER_BOUND('',#7264,.T.);
#4337=FACE_OUTER_BOUND('',#7265,.T.);
#4338=FACE_OUTER_BOUND('',#7266,.T.);
#4339=FACE_OUTER_BOUND('',#7267,.T.);
#4340=FACE_OUTER_BOUND('',#7268,.T.);
#4341=FACE_OUTER_BOUND('',#7269,.T.);
#4342=FACE_OUTER_BOUND('',#7270,.T.);
#4343=FACE_OUTER_BOUND('',#7271,.T.);
#4344=FACE_OUTER_BOUND('',#7272,.T.);
#4345=FACE_OUTER_BOUND('',#7273,.T.);
#4346=FACE_OUTER_BOUND('',#7274,.T.);
#4347=FACE_OUTER_BOUND('',#7275,.T.);
#4348=FACE_OUTER_BOUND('',#7276,.T.);
#4349=FACE_OUTER_BOUND('',#7277,.T.);
#4350=FACE_OUTER_BOUND('',#7278,.T.);
#4351=FACE_OUTER_BOUND('',#7279,.T.);
#4352=FACE_OUTER_BOUND('',#7280,.T.);
#4353=FACE_OUTER_BOUND('',#7281,.T.);
#4354=FACE_OUTER_BOUND('',#7282,.T.);
#4355=FACE_OUTER_BOUND('',#7283,.T.);
#4356=FACE_OUTER_BOUND('',#7284,.T.);
#4357=FACE_OUTER_BOUND('',#7285,.T.);
#4358=FACE_OUTER_BOUND('',#7286,.T.);
#4359=FACE_OUTER_BOUND('',#7287,.T.);
#4360=FACE_OUTER_BOUND('',#7288,.T.);
#4361=FACE_OUTER_BOUND('',#7289,.T.);
#4362=FACE_OUTER_BOUND('',#7290,.T.);
#4363=FACE_OUTER_BOUND('',#7291,.T.);
#4364=FACE_OUTER_BOUND('',#7292,.T.);
#4365=FACE_OUTER_BOUND('',#7293,.T.);
#4366=FACE_OUTER_BOUND('',#7294,.T.);
#4367=FACE_OUTER_BOUND('',#7295,.T.);
#4368=FACE_OUTER_BOUND('',#7296,.T.);
#4369=FACE_OUTER_BOUND('',#7297,.T.);
#4370=FACE_OUTER_BOUND('',#7298,.T.);
#4371=FACE_OUTER_BOUND('',#7299,.T.);
#4372=FACE_OUTER_BOUND('',#7300,.T.);
#4373=FACE_OUTER_BOUND('',#7301,.T.);
#4374=FACE_OUTER_BOUND('',#7302,.T.);
#4375=FACE_OUTER_BOUND('',#7303,.T.);
#4376=FACE_OUTER_BOUND('',#7304,.T.);
#4377=FACE_OUTER_BOUND('',#7305,.T.);
#4378=FACE_OUTER_BOUND('',#7306,.T.);
#4379=FACE_OUTER_BOUND('',#7307,.T.);
#4380=FACE_OUTER_BOUND('',#7308,.T.);
#4381=FACE_OUTER_BOUND('',#7309,.T.);
#4382=FACE_OUTER_BOUND('',#7310,.T.);
#4383=FACE_OUTER_BOUND('',#7311,.T.);
#4384=FACE_OUTER_BOUND('',#7312,.T.);
#4385=FACE_OUTER_BOUND('',#7313,.T.);
#4386=FACE_OUTER_BOUND('',#7314,.T.);
#4387=FACE_OUTER_BOUND('',#7315,.T.);
#4388=FACE_OUTER_BOUND('',#7316,.T.);
#4389=FACE_OUTER_BOUND('',#7317,.T.);
#4390=FACE_OUTER_BOUND('',#7318,.T.);
#4391=FACE_OUTER_BOUND('',#7319,.T.);
#4392=FACE_OUTER_BOUND('',#7320,.T.);
#4393=FACE_OUTER_BOUND('',#7321,.T.);
#4394=FACE_OUTER_BOUND('',#7322,.T.);
#4395=FACE_OUTER_BOUND('',#7323,.T.);
#4396=FACE_OUTER_BOUND('',#7324,.T.);
#4397=FACE_OUTER_BOUND('',#7325,.T.);
#4398=FACE_OUTER_BOUND('',#7326,.T.);
#4399=FACE_OUTER_BOUND('',#7327,.T.);
#4400=FACE_OUTER_BOUND('',#7328,.T.);
#4401=FACE_OUTER_BOUND('',#7329,.T.);
#4402=FACE_OUTER_BOUND('',#7330,.T.);
#4403=FACE_OUTER_BOUND('',#7331,.T.);
#4404=FACE_OUTER_BOUND('',#7332,.T.);
#4405=FACE_OUTER_BOUND('',#7333,.T.);
#4406=FACE_OUTER_BOUND('',#7334,.T.);
#4407=FACE_OUTER_BOUND('',#7335,.T.);
#4408=FACE_OUTER_BOUND('',#7336,.T.);
#4409=FACE_OUTER_BOUND('',#7337,.T.);
#4410=FACE_OUTER_BOUND('',#7338,.T.);
#4411=FACE_OUTER_BOUND('',#7339,.T.);
#4412=FACE_OUTER_BOUND('',#7340,.T.);
#4413=FACE_OUTER_BOUND('',#7341,.T.);
#4414=FACE_OUTER_BOUND('',#7342,.T.);
#4415=FACE_OUTER_BOUND('',#7343,.T.);
#4416=FACE_OUTER_BOUND('',#7344,.T.);
#4417=FACE_OUTER_BOUND('',#7345,.T.);
#4418=FACE_OUTER_BOUND('',#7346,.T.);
#4419=FACE_OUTER_BOUND('',#7347,.T.);
#4420=FACE_OUTER_BOUND('',#7348,.T.);
#4421=FACE_OUTER_BOUND('',#7349,.T.);
#4422=FACE_OUTER_BOUND('',#7350,.T.);
#4423=FACE_OUTER_BOUND('',#7351,.T.);
#4424=FACE_OUTER_BOUND('',#7352,.T.);
#4425=FACE_OUTER_BOUND('',#7353,.T.);
#4426=FACE_OUTER_BOUND('',#7354,.T.);
#4427=FACE_OUTER_BOUND('',#7355,.T.);
#4428=FACE_OUTER_BOUND('',#7356,.T.);
#4429=FACE_OUTER_BOUND('',#7357,.T.);
#4430=FACE_OUTER_BOUND('',#7358,.T.);
#4431=FACE_OUTER_BOUND('',#7359,.T.);
#4432=FACE_OUTER_BOUND('',#7360,.T.);
#4433=FACE_OUTER_BOUND('',#7361,.T.);
#4434=FACE_OUTER_BOUND('',#7362,.T.);
#4435=FACE_OUTER_BOUND('',#7363,.T.);
#4436=FACE_OUTER_BOUND('',#7364,.T.);
#4437=FACE_OUTER_BOUND('',#7365,.T.);
#4438=FACE_OUTER_BOUND('',#7366,.T.);
#4439=FACE_OUTER_BOUND('',#7367,.T.);
#4440=FACE_OUTER_BOUND('',#7368,.T.);
#4441=FACE_OUTER_BOUND('',#7369,.T.);
#4442=FACE_OUTER_BOUND('',#7370,.T.);
#4443=FACE_OUTER_BOUND('',#7371,.T.);
#4444=FACE_OUTER_BOUND('',#7372,.T.);
#4445=FACE_OUTER_BOUND('',#7373,.T.);
#4446=FACE_OUTER_BOUND('',#7374,.T.);
#4447=FACE_OUTER_BOUND('',#7375,.T.);
#4448=FACE_OUTER_BOUND('',#7376,.T.);
#4449=FACE_OUTER_BOUND('',#7377,.T.);
#4450=FACE_OUTER_BOUND('',#7378,.T.);
#4451=FACE_OUTER_BOUND('',#7379,.T.);
#4452=FACE_OUTER_BOUND('',#7380,.T.);
#4453=FACE_OUTER_BOUND('',#7381,.T.);
#4454=FACE_OUTER_BOUND('',#7382,.T.);
#4455=FACE_OUTER_BOUND('',#7383,.T.);
#4456=FACE_OUTER_BOUND('',#7384,.T.);
#4457=FACE_OUTER_BOUND('',#7385,.T.);
#4458=FACE_OUTER_BOUND('',#7386,.T.);
#4459=FACE_OUTER_BOUND('',#7387,.T.);
#4460=FACE_OUTER_BOUND('',#7388,.T.);
#4461=FACE_OUTER_BOUND('',#7389,.T.);
#4462=FACE_OUTER_BOUND('',#7390,.T.);
#4463=FACE_OUTER_BOUND('',#7391,.T.);
#4464=FACE_OUTER_BOUND('',#7392,.T.);
#4465=FACE_OUTER_BOUND('',#7393,.T.);
#4466=FACE_OUTER_BOUND('',#7394,.T.);
#4467=FACE_OUTER_BOUND('',#7395,.T.);
#4468=FACE_OUTER_BOUND('',#7396,.T.);
#4469=FACE_OUTER_BOUND('',#7397,.T.);
#4470=FACE_OUTER_BOUND('',#7398,.T.);
#4471=FACE_OUTER_BOUND('',#7399,.T.);
#4472=FACE_OUTER_BOUND('',#7400,.T.);
#4473=FACE_OUTER_BOUND('',#7401,.T.);
#4474=FACE_OUTER_BOUND('',#7402,.T.);
#4475=FACE_OUTER_BOUND('',#7403,.T.);
#4476=FACE_OUTER_BOUND('',#7404,.T.);
#4477=FACE_OUTER_BOUND('',#7405,.T.);
#4478=FACE_OUTER_BOUND('',#7406,.T.);
#4479=FACE_OUTER_BOUND('',#7407,.T.);
#4480=FACE_OUTER_BOUND('',#7408,.T.);
#4481=FACE_OUTER_BOUND('',#7409,.T.);
#4482=FACE_OUTER_BOUND('',#7410,.T.);
#4483=FACE_OUTER_BOUND('',#7411,.T.);
#4484=FACE_OUTER_BOUND('',#7412,.T.);
#4485=FACE_OUTER_BOUND('',#7413,.T.);
#4486=FACE_OUTER_BOUND('',#7414,.T.);
#4487=FACE_OUTER_BOUND('',#7415,.T.);
#4488=FACE_OUTER_BOUND('',#7416,.T.);
#4489=FACE_OUTER_BOUND('',#7417,.T.);
#4490=FACE_OUTER_BOUND('',#7418,.T.);
#4491=FACE_OUTER_BOUND('',#7419,.T.);
#4492=FACE_OUTER_BOUND('',#7420,.T.);
#4493=FACE_OUTER_BOUND('',#7421,.T.);
#4494=FACE_OUTER_BOUND('',#7422,.T.);
#4495=FACE_OUTER_BOUND('',#7423,.T.);
#4496=FACE_OUTER_BOUND('',#7424,.T.);
#4497=FACE_OUTER_BOUND('',#7425,.T.);
#4498=FACE_OUTER_BOUND('',#7426,.T.);
#4499=FACE_OUTER_BOUND('',#7427,.T.);
#4500=FACE_OUTER_BOUND('',#7428,.T.);
#4501=FACE_OUTER_BOUND('',#7429,.T.);
#4502=FACE_OUTER_BOUND('',#7430,.T.);
#4503=FACE_OUTER_BOUND('',#7431,.T.);
#4504=FACE_OUTER_BOUND('',#7432,.T.);
#4505=FACE_OUTER_BOUND('',#7433,.T.);
#4506=FACE_OUTER_BOUND('',#7434,.T.);
#4507=FACE_OUTER_BOUND('',#7435,.T.);
#4508=FACE_OUTER_BOUND('',#7436,.T.);
#4509=FACE_OUTER_BOUND('',#7437,.T.);
#4510=FACE_OUTER_BOUND('',#7438,.T.);
#4511=FACE_OUTER_BOUND('',#7439,.T.);
#4512=FACE_OUTER_BOUND('',#7440,.T.);
#4513=FACE_OUTER_BOUND('',#7441,.T.);
#4514=FACE_OUTER_BOUND('',#7442,.T.);
#4515=FACE_OUTER_BOUND('',#7443,.T.);
#4516=FACE_OUTER_BOUND('',#7444,.T.);
#4517=FACE_OUTER_BOUND('',#7445,.T.);
#4518=FACE_OUTER_BOUND('',#7446,.T.);
#4519=FACE_OUTER_BOUND('',#7447,.T.);
#4520=FACE_OUTER_BOUND('',#7448,.T.);
#4521=FACE_OUTER_BOUND('',#7449,.T.);
#4522=FACE_OUTER_BOUND('',#7450,.T.);
#4523=FACE_OUTER_BOUND('',#7451,.T.);
#4524=FACE_OUTER_BOUND('',#7452,.T.);
#4525=FACE_OUTER_BOUND('',#7453,.T.);
#4526=FACE_OUTER_BOUND('',#7454,.T.);
#4527=FACE_OUTER_BOUND('',#7455,.T.);
#4528=FACE_OUTER_BOUND('',#7456,.T.);
#4529=FACE_OUTER_BOUND('',#7457,.T.);
#4530=FACE_OUTER_BOUND('',#7458,.T.);
#4531=FACE_OUTER_BOUND('',#7459,.T.);
#4532=FACE_OUTER_BOUND('',#7460,.T.);
#4533=FACE_OUTER_BOUND('',#7461,.T.);
#4534=FACE_OUTER_BOUND('',#7462,.T.);
#4535=FACE_OUTER_BOUND('',#7463,.T.);
#4536=FACE_OUTER_BOUND('',#7464,.T.);
#4537=FACE_OUTER_BOUND('',#7465,.T.);
#4538=FACE_OUTER_BOUND('',#7466,.T.);
#4539=FACE_OUTER_BOUND('',#7467,.T.);
#4540=FACE_OUTER_BOUND('',#7468,.T.);
#4541=FACE_OUTER_BOUND('',#7469,.T.);
#4542=FACE_OUTER_BOUND('',#7470,.T.);
#4543=FACE_OUTER_BOUND('',#7471,.T.);
#4544=FACE_OUTER_BOUND('',#7472,.T.);
#4545=FACE_OUTER_BOUND('',#7473,.T.);
#4546=FACE_OUTER_BOUND('',#7474,.T.);
#4547=FACE_OUTER_BOUND('',#7475,.T.);
#4548=FACE_OUTER_BOUND('',#7476,.T.);
#4549=FACE_OUTER_BOUND('',#7477,.T.);
#4550=FACE_OUTER_BOUND('',#7478,.T.);
#4551=FACE_OUTER_BOUND('',#7479,.T.);
#4552=FACE_OUTER_BOUND('',#7480,.T.);
#4553=FACE_OUTER_BOUND('',#7481,.T.);
#4554=FACE_OUTER_BOUND('',#7482,.T.);
#4555=FACE_OUTER_BOUND('',#7483,.T.);
#4556=FACE_OUTER_BOUND('',#7484,.T.);
#4557=FACE_OUTER_BOUND('',#7485,.T.);
#4558=FACE_OUTER_BOUND('',#7486,.T.);
#4559=FACE_OUTER_BOUND('',#7487,.T.);
#4560=FACE_OUTER_BOUND('',#7488,.T.);
#4561=FACE_OUTER_BOUND('',#7489,.T.);
#4562=FACE_OUTER_BOUND('',#7490,.T.);
#4563=FACE_OUTER_BOUND('',#7491,.T.);
#4564=FACE_OUTER_BOUND('',#7492,.T.);
#4565=FACE_OUTER_BOUND('',#7493,.T.);
#4566=FACE_OUTER_BOUND('',#7494,.T.);
#4567=FACE_OUTER_BOUND('',#7495,.T.);
#4568=FACE_OUTER_BOUND('',#7496,.T.);
#4569=FACE_OUTER_BOUND('',#7497,.T.);
#4570=FACE_OUTER_BOUND('',#7498,.T.);
#4571=FACE_OUTER_BOUND('',#7499,.T.);
#4572=FACE_OUTER_BOUND('',#7500,.T.);
#4573=FACE_OUTER_BOUND('',#7501,.T.);
#4574=FACE_OUTER_BOUND('',#7502,.T.);
#4575=FACE_OUTER_BOUND('',#7503,.T.);
#4576=FACE_OUTER_BOUND('',#7504,.T.);
#4577=FACE_OUTER_BOUND('',#7505,.T.);
#4578=FACE_OUTER_BOUND('',#7506,.T.);
#4579=FACE_OUTER_BOUND('',#7507,.T.);
#4580=FACE_OUTER_BOUND('',#7508,.T.);
#4581=FACE_OUTER_BOUND('',#7509,.T.);
#4582=FACE_OUTER_BOUND('',#7510,.T.);
#4583=FACE_OUTER_BOUND('',#7511,.T.);
#4584=FACE_OUTER_BOUND('',#7512,.T.);
#4585=FACE_OUTER_BOUND('',#7513,.T.);
#4586=FACE_OUTER_BOUND('',#7514,.T.);
#4587=FACE_OUTER_BOUND('',#7515,.T.);
#4588=FACE_OUTER_BOUND('',#7516,.T.);
#4589=FACE_OUTER_BOUND('',#7517,.T.);
#4590=FACE_OUTER_BOUND('',#7518,.T.);
#4591=FACE_OUTER_BOUND('',#7519,.T.);
#4592=FACE_OUTER_BOUND('',#7520,.T.);
#4593=FACE_OUTER_BOUND('',#7521,.T.);
#4594=FACE_OUTER_BOUND('',#7522,.T.);
#4595=FACE_OUTER_BOUND('',#7523,.T.);
#4596=FACE_OUTER_BOUND('',#7524,.T.);
#4597=FACE_OUTER_BOUND('',#7525,.T.);
#4598=FACE_OUTER_BOUND('',#7526,.T.);
#4599=FACE_OUTER_BOUND('',#7527,.T.);
#4600=FACE_OUTER_BOUND('',#7528,.T.);
#4601=FACE_OUTER_BOUND('',#7529,.T.);
#4602=FACE_OUTER_BOUND('',#7530,.T.);
#4603=FACE_OUTER_BOUND('',#7531,.T.);
#4604=FACE_OUTER_BOUND('',#7532,.T.);
#4605=FACE_OUTER_BOUND('',#7533,.T.);
#4606=FACE_OUTER_BOUND('',#7534,.T.);
#4607=FACE_OUTER_BOUND('',#7535,.T.);
#4608=FACE_OUTER_BOUND('',#7536,.T.);
#4609=FACE_OUTER_BOUND('',#7537,.T.);
#4610=FACE_OUTER_BOUND('',#7538,.T.);
#4611=FACE_OUTER_BOUND('',#7539,.T.);
#4612=FACE_OUTER_BOUND('',#7540,.T.);
#4613=FACE_OUTER_BOUND('',#7541,.T.);
#4614=FACE_OUTER_BOUND('',#7542,.T.);
#4615=FACE_OUTER_BOUND('',#7543,.T.);
#4616=FACE_OUTER_BOUND('',#7544,.T.);
#4617=FACE_OUTER_BOUND('',#7545,.T.);
#4618=FACE_OUTER_BOUND('',#7546,.T.);
#4619=FACE_OUTER_BOUND('',#7547,.T.);
#4620=FACE_OUTER_BOUND('',#7548,.T.);
#4621=FACE_OUTER_BOUND('',#7549,.T.);
#4622=FACE_OUTER_BOUND('',#7550,.T.);
#4623=FACE_OUTER_BOUND('',#7551,.T.);
#4624=FACE_OUTER_BOUND('',#7552,.T.);
#4625=FACE_OUTER_BOUND('',#7553,.T.);
#4626=FACE_OUTER_BOUND('',#7554,.T.);
#4627=FACE_OUTER_BOUND('',#7555,.T.);
#4628=FACE_OUTER_BOUND('',#7556,.T.);
#4629=FACE_OUTER_BOUND('',#7557,.T.);
#4630=FACE_OUTER_BOUND('',#7558,.T.);
#4631=FACE_OUTER_BOUND('',#7559,.T.);
#4632=FACE_OUTER_BOUND('',#7560,.T.);
#4633=FACE_OUTER_BOUND('',#7561,.T.);
#4634=FACE_OUTER_BOUND('',#7562,.T.);
#4635=FACE_OUTER_BOUND('',#7563,.T.);
#4636=FACE_OUTER_BOUND('',#7564,.T.);
#4637=FACE_OUTER_BOUND('',#7565,.T.);
#4638=FACE_OUTER_BOUND('',#7566,.T.);
#4639=FACE_OUTER_BOUND('',#7567,.T.);
#4640=FACE_OUTER_BOUND('',#7568,.T.);
#4641=FACE_OUTER_BOUND('',#7569,.T.);
#4642=FACE_OUTER_BOUND('',#7570,.T.);
#4643=FACE_OUTER_BOUND('',#7571,.T.);
#4644=FACE_OUTER_BOUND('',#7572,.T.);
#4645=FACE_OUTER_BOUND('',#7573,.T.);
#4646=FACE_OUTER_BOUND('',#7574,.T.);
#4647=FACE_OUTER_BOUND('',#7575,.T.);
#4648=FACE_OUTER_BOUND('',#7576,.T.);
#4649=FACE_OUTER_BOUND('',#7577,.T.);
#4650=FACE_OUTER_BOUND('',#7578,.T.);
#4651=FACE_OUTER_BOUND('',#7579,.T.);
#4652=FACE_OUTER_BOUND('',#7580,.T.);
#4653=FACE_OUTER_BOUND('',#7581,.T.);
#4654=FACE_OUTER_BOUND('',#7582,.T.);
#4655=FACE_OUTER_BOUND('',#7583,.T.);
#4656=FACE_OUTER_BOUND('',#7584,.T.);
#4657=FACE_OUTER_BOUND('',#7585,.T.);
#4658=FACE_OUTER_BOUND('',#7586,.T.);
#4659=FACE_OUTER_BOUND('',#7587,.T.);
#4660=FACE_OUTER_BOUND('',#7588,.T.);
#4661=FACE_OUTER_BOUND('',#7589,.T.);
#4662=FACE_OUTER_BOUND('',#7590,.T.);
#4663=FACE_OUTER_BOUND('',#7591,.T.);
#4664=FACE_OUTER_BOUND('',#7592,.T.);
#4665=FACE_OUTER_BOUND('',#7593,.T.);
#4666=FACE_OUTER_BOUND('',#7594,.T.);
#4667=FACE_OUTER_BOUND('',#7595,.T.);
#4668=FACE_OUTER_BOUND('',#7596,.T.);
#4669=FACE_OUTER_BOUND('',#7597,.T.);
#4670=FACE_OUTER_BOUND('',#7598,.T.);
#4671=FACE_OUTER_BOUND('',#7599,.T.);
#4672=FACE_OUTER_BOUND('',#7600,.T.);
#4673=FACE_OUTER_BOUND('',#7601,.T.);
#4674=FACE_OUTER_BOUND('',#7602,.T.);
#4675=FACE_OUTER_BOUND('',#7603,.T.);
#4676=FACE_OUTER_BOUND('',#7604,.T.);
#4677=FACE_OUTER_BOUND('',#7605,.T.);
#4678=FACE_OUTER_BOUND('',#7606,.T.);
#4679=FACE_OUTER_BOUND('',#7607,.T.);
#4680=FACE_OUTER_BOUND('',#7608,.T.);
#4681=FACE_OUTER_BOUND('',#7609,.T.);
#4682=FACE_OUTER_BOUND('',#7610,.T.);
#4683=FACE_OUTER_BOUND('',#7611,.T.);
#4684=FACE_OUTER_BOUND('',#7612,.T.);
#4685=FACE_OUTER_BOUND('',#7613,.T.);
#4686=FACE_OUTER_BOUND('',#7614,.T.);
#4687=FACE_OUTER_BOUND('',#7615,.T.);
#4688=FACE_OUTER_BOUND('',#7616,.T.);
#4689=FACE_OUTER_BOUND('',#7617,.T.);
#4690=FACE_OUTER_BOUND('',#7618,.T.);
#4691=FACE_OUTER_BOUND('',#7619,.T.);
#4692=FACE_OUTER_BOUND('',#7620,.T.);
#4693=FACE_OUTER_BOUND('',#7621,.T.);
#4694=FACE_OUTER_BOUND('',#7622,.T.);
#4695=FACE_OUTER_BOUND('',#7623,.T.);
#4696=FACE_OUTER_BOUND('',#7624,.T.);
#4697=FACE_OUTER_BOUND('',#7625,.T.);
#4698=FACE_OUTER_BOUND('',#7626,.T.);
#4699=FACE_OUTER_BOUND('',#7627,.T.);
#4700=FACE_OUTER_BOUND('',#7628,.T.);
#4701=FACE_OUTER_BOUND('',#7629,.T.);
#4702=FACE_OUTER_BOUND('',#7630,.T.);
#4703=FACE_OUTER_BOUND('',#7631,.T.);
#4704=FACE_OUTER_BOUND('',#7632,.T.);
#4705=FACE_OUTER_BOUND('',#7633,.T.);
#4706=FACE_OUTER_BOUND('',#7634,.T.);
#4707=FACE_OUTER_BOUND('',#7635,.T.);
#4708=FACE_OUTER_BOUND('',#7636,.T.);
#4709=FACE_OUTER_BOUND('',#7637,.T.);
#4710=FACE_OUTER_BOUND('',#7638,.T.);
#4711=FACE_OUTER_BOUND('',#7639,.T.);
#4712=FACE_OUTER_BOUND('',#7640,.T.);
#4713=FACE_OUTER_BOUND('',#7641,.T.);
#4714=FACE_OUTER_BOUND('',#7642,.T.);
#4715=FACE_OUTER_BOUND('',#7643,.T.);
#4716=FACE_OUTER_BOUND('',#7644,.T.);
#4717=FACE_OUTER_BOUND('',#7645,.T.);
#4718=FACE_OUTER_BOUND('',#7646,.T.);
#4719=FACE_OUTER_BOUND('',#7647,.T.);
#4720=FACE_OUTER_BOUND('',#7648,.T.);
#4721=FACE_OUTER_BOUND('',#7649,.T.);
#4722=FACE_OUTER_BOUND('',#7650,.T.);
#4723=FACE_OUTER_BOUND('',#7651,.T.);
#4724=FACE_OUTER_BOUND('',#7652,.T.);
#4725=FACE_OUTER_BOUND('',#7653,.T.);
#4726=FACE_OUTER_BOUND('',#7654,.T.);
#4727=FACE_OUTER_BOUND('',#7655,.T.);
#4728=FACE_OUTER_BOUND('',#7656,.T.);
#4729=FACE_OUTER_BOUND('',#7657,.T.);
#4730=FACE_OUTER_BOUND('',#7658,.T.);
#4731=FACE_OUTER_BOUND('',#7659,.T.);
#4732=FACE_OUTER_BOUND('',#7660,.T.);
#4733=FACE_OUTER_BOUND('',#7661,.T.);
#4734=FACE_OUTER_BOUND('',#7662,.T.);
#4735=FACE_OUTER_BOUND('',#7663,.T.);
#4736=FACE_OUTER_BOUND('',#7664,.T.);
#4737=FACE_OUTER_BOUND('',#7665,.T.);
#4738=FACE_OUTER_BOUND('',#7666,.T.);
#4739=FACE_OUTER_BOUND('',#7667,.T.);
#4740=FACE_OUTER_BOUND('',#7668,.T.);
#4741=FACE_OUTER_BOUND('',#7669,.T.);
#4742=FACE_OUTER_BOUND('',#7670,.T.);
#4743=FACE_OUTER_BOUND('',#7671,.T.);
#4744=FACE_OUTER_BOUND('',#7672,.T.);
#4745=FACE_OUTER_BOUND('',#7673,.T.);
#4746=FACE_OUTER_BOUND('',#7674,.T.);
#4747=FACE_OUTER_BOUND('',#7675,.T.);
#4748=FACE_OUTER_BOUND('',#7676,.T.);
#4749=FACE_OUTER_BOUND('',#7677,.T.);
#4750=FACE_OUTER_BOUND('',#7678,.T.);
#4751=FACE_OUTER_BOUND('',#7679,.T.);
#4752=FACE_OUTER_BOUND('',#7680,.T.);
#4753=FACE_OUTER_BOUND('',#7681,.T.);
#4754=FACE_OUTER_BOUND('',#7682,.T.);
#4755=FACE_OUTER_BOUND('',#7683,.T.);
#4756=FACE_OUTER_BOUND('',#7684,.T.);
#4757=FACE_OUTER_BOUND('',#7685,.T.);
#4758=FACE_OUTER_BOUND('',#7686,.T.);
#4759=FACE_OUTER_BOUND('',#7687,.T.);
#4760=FACE_OUTER_BOUND('',#7688,.T.);
#4761=FACE_OUTER_BOUND('',#7689,.T.);
#4762=FACE_OUTER_BOUND('',#7690,.T.);
#4763=FACE_OUTER_BOUND('',#7691,.T.);
#4764=FACE_OUTER_BOUND('',#7692,.T.);
#4765=FACE_OUTER_BOUND('',#7693,.T.);
#4766=FACE_OUTER_BOUND('',#7694,.T.);
#4767=FACE_OUTER_BOUND('',#7695,.T.);
#4768=FACE_OUTER_BOUND('',#7696,.T.);
#4769=FACE_OUTER_BOUND('',#7697,.T.);
#4770=FACE_OUTER_BOUND('',#7698,.T.);
#4771=FACE_OUTER_BOUND('',#7699,.T.);
#4772=FACE_OUTER_BOUND('',#7700,.T.);
#4773=FACE_OUTER_BOUND('',#7701,.T.);
#4774=FACE_OUTER_BOUND('',#7702,.T.);
#4775=FACE_OUTER_BOUND('',#7703,.T.);
#4776=FACE_OUTER_BOUND('',#7704,.T.);
#4777=FACE_OUTER_BOUND('',#7705,.T.);
#4778=FACE_OUTER_BOUND('',#7706,.T.);
#4779=FACE_OUTER_BOUND('',#7707,.T.);
#4780=FACE_OUTER_BOUND('',#7708,.T.);
#4781=FACE_OUTER_BOUND('',#7709,.T.);
#4782=FACE_OUTER_BOUND('',#7710,.T.);
#4783=FACE_OUTER_BOUND('',#7711,.T.);
#4784=FACE_OUTER_BOUND('',#7712,.T.);
#4785=FACE_OUTER_BOUND('',#7713,.T.);
#4786=FACE_OUTER_BOUND('',#7714,.T.);
#4787=FACE_OUTER_BOUND('',#7715,.T.);
#4788=FACE_OUTER_BOUND('',#7716,.T.);
#4789=FACE_OUTER_BOUND('',#7717,.T.);
#4790=FACE_OUTER_BOUND('',#7718,.T.);
#4791=FACE_OUTER_BOUND('',#7719,.T.);
#4792=FACE_OUTER_BOUND('',#7720,.T.);
#4793=FACE_OUTER_BOUND('',#7721,.T.);
#4794=FACE_OUTER_BOUND('',#7722,.T.);
#4795=FACE_OUTER_BOUND('',#7723,.T.);
#4796=FACE_OUTER_BOUND('',#7724,.T.);
#4797=FACE_OUTER_BOUND('',#7725,.T.);
#4798=FACE_OUTER_BOUND('',#7726,.T.);
#4799=FACE_OUTER_BOUND('',#7727,.T.);
#4800=FACE_OUTER_BOUND('',#7728,.T.);
#4801=FACE_OUTER_BOUND('',#7729,.T.);
#4802=FACE_OUTER_BOUND('',#7730,.T.);
#4803=FACE_OUTER_BOUND('',#7731,.T.);
#4804=FACE_OUTER_BOUND('',#7732,.T.);
#4805=FACE_OUTER_BOUND('',#7733,.T.);
#4806=FACE_OUTER_BOUND('',#7734,.T.);
#4807=FACE_OUTER_BOUND('',#7735,.T.);
#4808=FACE_OUTER_BOUND('',#7736,.T.);
#4809=FACE_OUTER_BOUND('',#7737,.T.);
#4810=FACE_OUTER_BOUND('',#7738,.T.);
#4811=FACE_OUTER_BOUND('',#7739,.T.);
#4812=FACE_OUTER_BOUND('',#7740,.T.);
#4813=FACE_OUTER_BOUND('',#7741,.T.);
#4814=FACE_OUTER_BOUND('',#7742,.T.);
#4815=FACE_OUTER_BOUND('',#7743,.T.);
#4816=FACE_OUTER_BOUND('',#7744,.T.);
#4817=FACE_OUTER_BOUND('',#7745,.T.);
#4818=FACE_OUTER_BOUND('',#7746,.T.);
#4819=FACE_OUTER_BOUND('',#7747,.T.);
#4820=FACE_OUTER_BOUND('',#7748,.T.);
#4821=FACE_OUTER_BOUND('',#7749,.T.);
#4822=FACE_OUTER_BOUND('',#7750,.T.);
#4823=FACE_OUTER_BOUND('',#7751,.T.);
#4824=FACE_OUTER_BOUND('',#7752,.T.);
#4825=FACE_OUTER_BOUND('',#7753,.T.);
#4826=FACE_OUTER_BOUND('',#7754,.T.);
#4827=FACE_OUTER_BOUND('',#7755,.T.);
#4828=FACE_OUTER_BOUND('',#7756,.T.);
#4829=FACE_OUTER_BOUND('',#7757,.T.);
#4830=FACE_OUTER_BOUND('',#7758,.T.);
#4831=FACE_OUTER_BOUND('',#7759,.T.);
#4832=FACE_OUTER_BOUND('',#7760,.T.);
#4833=FACE_OUTER_BOUND('',#7761,.T.);
#4834=FACE_OUTER_BOUND('',#7762,.T.);
#4835=FACE_OUTER_BOUND('',#7763,.T.);
#4836=FACE_OUTER_BOUND('',#7764,.T.);
#4837=FACE_OUTER_BOUND('',#7765,.T.);
#4838=FACE_OUTER_BOUND('',#7766,.T.);
#4839=FACE_OUTER_BOUND('',#7767,.T.);
#4840=FACE_OUTER_BOUND('',#7768,.T.);
#4841=FACE_OUTER_BOUND('',#7769,.T.);
#4842=FACE_OUTER_BOUND('',#7770,.T.);
#4843=FACE_OUTER_BOUND('',#7771,.T.);
#4844=FACE_OUTER_BOUND('',#7772,.T.);
#4845=FACE_OUTER_BOUND('',#7773,.T.);
#4846=FACE_OUTER_BOUND('',#7774,.T.);
#4847=FACE_OUTER_BOUND('',#7775,.T.);
#4848=FACE_OUTER_BOUND('',#7776,.T.);
#4849=FACE_OUTER_BOUND('',#7777,.T.);
#4850=FACE_OUTER_BOUND('',#7778,.T.);
#4851=FACE_OUTER_BOUND('',#7779,.T.);
#4852=FACE_OUTER_BOUND('',#7780,.T.);
#4853=FACE_OUTER_BOUND('',#7781,.T.);
#4854=FACE_OUTER_BOUND('',#7782,.T.);
#4855=FACE_OUTER_BOUND('',#7783,.T.);
#4856=FACE_OUTER_BOUND('',#7784,.T.);
#4857=FACE_OUTER_BOUND('',#7785,.T.);
#4858=FACE_OUTER_BOUND('',#7786,.T.);
#4859=FACE_OUTER_BOUND('',#7787,.T.);
#4860=FACE_OUTER_BOUND('',#7788,.T.);
#4861=FACE_OUTER_BOUND('',#7789,.T.);
#4862=FACE_OUTER_BOUND('',#7790,.T.);
#4863=FACE_OUTER_BOUND('',#7791,.T.);
#4864=FACE_OUTER_BOUND('',#7792,.T.);
#4865=FACE_OUTER_BOUND('',#7793,.T.);
#4866=FACE_OUTER_BOUND('',#7794,.T.);
#4867=FACE_OUTER_BOUND('',#7795,.T.);
#4868=FACE_OUTER_BOUND('',#7796,.T.);
#4869=FACE_OUTER_BOUND('',#7797,.T.);
#4870=FACE_OUTER_BOUND('',#7798,.T.);
#4871=FACE_OUTER_BOUND('',#7799,.T.);
#4872=FACE_OUTER_BOUND('',#7800,.T.);
#4873=FACE_OUTER_BOUND('',#7801,.T.);
#4874=FACE_OUTER_BOUND('',#7802,.T.);
#4875=FACE_OUTER_BOUND('',#7803,.T.);
#4876=FACE_OUTER_BOUND('',#7804,.T.);
#4877=FACE_OUTER_BOUND('',#7805,.T.);
#4878=FACE_OUTER_BOUND('',#7806,.T.);
#4879=FACE_OUTER_BOUND('',#7807,.T.);
#4880=FACE_OUTER_BOUND('',#7808,.T.);
#4881=FACE_OUTER_BOUND('',#7809,.T.);
#4882=FACE_OUTER_BOUND('',#7810,.T.);
#4883=FACE_OUTER_BOUND('',#7811,.T.);
#4884=FACE_OUTER_BOUND('',#7812,.T.);
#4885=FACE_OUTER_BOUND('',#7813,.T.);
#4886=FACE_OUTER_BOUND('',#7814,.T.);
#4887=FACE_OUTER_BOUND('',#7815,.T.);
#4888=FACE_OUTER_BOUND('',#7816,.T.);
#4889=FACE_OUTER_BOUND('',#7817,.T.);
#4890=FACE_OUTER_BOUND('',#7818,.T.);
#4891=FACE_OUTER_BOUND('',#7819,.T.);
#4892=FACE_OUTER_BOUND('',#7820,.T.);
#4893=FACE_OUTER_BOUND('',#7821,.T.);
#4894=FACE_OUTER_BOUND('',#7822,.T.);
#4895=FACE_OUTER_BOUND('',#7823,.T.);
#4896=FACE_OUTER_BOUND('',#7824,.T.);
#4897=FACE_OUTER_BOUND('',#7825,.T.);
#4898=FACE_OUTER_BOUND('',#7826,.T.);
#4899=FACE_OUTER_BOUND('',#7827,.T.);
#4900=FACE_OUTER_BOUND('',#7828,.T.);
#4901=FACE_OUTER_BOUND('',#7829,.T.);
#4902=FACE_OUTER_BOUND('',#7830,.T.);
#4903=FACE_OUTER_BOUND('',#7831,.T.);
#4904=FACE_OUTER_BOUND('',#7832,.T.);
#4905=FACE_OUTER_BOUND('',#7833,.T.);
#4906=FACE_OUTER_BOUND('',#7834,.T.);
#4907=FACE_OUTER_BOUND('',#7835,.T.);
#4908=FACE_OUTER_BOUND('',#7836,.T.);
#4909=FACE_OUTER_BOUND('',#7837,.T.);
#4910=FACE_OUTER_BOUND('',#7838,.T.);
#4911=FACE_OUTER_BOUND('',#7839,.T.);
#4912=FACE_OUTER_BOUND('',#7840,.T.);
#4913=FACE_OUTER_BOUND('',#7841,.T.);
#4914=FACE_OUTER_BOUND('',#7842,.T.);
#4915=FACE_OUTER_BOUND('',#7843,.T.);
#4916=FACE_OUTER_BOUND('',#7844,.T.);
#4917=FACE_OUTER_BOUND('',#7845,.T.);
#4918=FACE_OUTER_BOUND('',#7846,.T.);
#4919=FACE_OUTER_BOUND('',#7847,.T.);
#4920=FACE_OUTER_BOUND('',#7848,.T.);
#4921=FACE_OUTER_BOUND('',#7849,.T.);
#4922=FACE_OUTER_BOUND('',#7850,.T.);
#4923=FACE_OUTER_BOUND('',#7851,.T.);
#4924=FACE_OUTER_BOUND('',#7852,.T.);
#4925=FACE_OUTER_BOUND('',#7853,.T.);
#4926=FACE_OUTER_BOUND('',#7854,.T.);
#4927=FACE_OUTER_BOUND('',#7855,.T.);
#4928=FACE_OUTER_BOUND('',#7856,.T.);
#4929=FACE_OUTER_BOUND('',#7857,.T.);
#4930=FACE_OUTER_BOUND('',#7858,.T.);
#4931=FACE_OUTER_BOUND('',#7859,.T.);
#4932=FACE_OUTER_BOUND('',#7860,.T.);
#4933=FACE_OUTER_BOUND('',#7861,.T.);
#4934=FACE_OUTER_BOUND('',#7862,.T.);
#4935=FACE_OUTER_BOUND('',#7863,.T.);
#4936=FACE_OUTER_BOUND('',#7864,.T.);
#4937=FACE_OUTER_BOUND('',#7865,.T.);
#4938=FACE_OUTER_BOUND('',#7866,.T.);
#4939=FACE_OUTER_BOUND('',#7867,.T.);
#4940=FACE_OUTER_BOUND('',#7868,.T.);
#4941=FACE_OUTER_BOUND('',#7869,.T.);
#4942=FACE_OUTER_BOUND('',#7870,.T.);
#4943=FACE_OUTER_BOUND('',#7871,.T.);
#4944=FACE_OUTER_BOUND('',#7872,.T.);
#4945=FACE_OUTER_BOUND('',#7873,.T.);
#4946=FACE_OUTER_BOUND('',#7874,.T.);
#4947=FACE_OUTER_BOUND('',#7875,.T.);
#4948=FACE_OUTER_BOUND('',#7876,.T.);
#4949=FACE_OUTER_BOUND('',#7877,.T.);
#4950=FACE_OUTER_BOUND('',#7878,.T.);
#4951=FACE_OUTER_BOUND('',#7879,.T.);
#4952=FACE_OUTER_BOUND('',#7880,.T.);
#4953=FACE_OUTER_BOUND('',#7881,.T.);
#4954=FACE_OUTER_BOUND('',#7882,.T.);
#4955=FACE_OUTER_BOUND('',#7883,.T.);
#4956=FACE_OUTER_BOUND('',#7884,.T.);
#4957=FACE_OUTER_BOUND('',#7885,.T.);
#4958=FACE_OUTER_BOUND('',#7886,.T.);
#4959=FACE_OUTER_BOUND('',#7887,.T.);
#4960=FACE_OUTER_BOUND('',#7888,.T.);
#4961=FACE_OUTER_BOUND('',#7889,.T.);
#4962=FACE_OUTER_BOUND('',#7890,.T.);
#4963=FACE_OUTER_BOUND('',#7891,.T.);
#4964=FACE_OUTER_BOUND('',#7892,.T.);
#4965=FACE_OUTER_BOUND('',#7893,.T.);
#4966=FACE_OUTER_BOUND('',#7894,.T.);
#4967=FACE_OUTER_BOUND('',#7895,.T.);
#4968=FACE_OUTER_BOUND('',#7896,.T.);
#4969=FACE_OUTER_BOUND('',#7897,.T.);
#4970=FACE_OUTER_BOUND('',#7898,.T.);
#4971=FACE_OUTER_BOUND('',#7899,.T.);
#4972=FACE_OUTER_BOUND('',#7900,.T.);
#4973=FACE_OUTER_BOUND('',#7901,.T.);
#4974=FACE_OUTER_BOUND('',#7902,.T.);
#4975=FACE_OUTER_BOUND('',#7903,.T.);
#4976=FACE_OUTER_BOUND('',#7904,.T.);
#4977=FACE_OUTER_BOUND('',#7905,.T.);
#4978=FACE_OUTER_BOUND('',#7906,.T.);
#4979=FACE_OUTER_BOUND('',#7907,.T.);
#4980=FACE_OUTER_BOUND('',#7908,.T.);
#4981=FACE_OUTER_BOUND('',#7909,.T.);
#4982=FACE_OUTER_BOUND('',#7910,.T.);
#4983=FACE_OUTER_BOUND('',#7911,.T.);
#4984=FACE_OUTER_BOUND('',#7912,.T.);
#4985=FACE_OUTER_BOUND('',#7913,.T.);
#4986=FACE_OUTER_BOUND('',#7914,.T.);
#4987=FACE_OUTER_BOUND('',#7915,.T.);
#4988=FACE_OUTER_BOUND('',#7916,.T.);
#4989=FACE_OUTER_BOUND('',#7917,.T.);
#4990=FACE_OUTER_BOUND('',#7918,.T.);
#4991=FACE_OUTER_BOUND('',#7919,.T.);
#4992=FACE_OUTER_BOUND('',#7920,.T.);
#4993=FACE_OUTER_BOUND('',#7921,.T.);
#4994=FACE_OUTER_BOUND('',#7922,.T.);
#4995=FACE_OUTER_BOUND('',#7923,.T.);
#4996=FACE_OUTER_BOUND('',#7924,.T.);
#4997=FACE_OUTER_BOUND('',#7925,.T.);
#4998=FACE_OUTER_BOUND('',#7926,.T.);
#4999=FACE_OUTER_BOUND('',#7927,.T.);
#5000=FACE_OUTER_BOUND('',#7928,.T.);
#5001=FACE_OUTER_BOUND('',#7929,.T.);
#5002=FACE_OUTER_BOUND('',#7930,.T.);
#5003=FACE_OUTER_BOUND('',#7931,.T.);
#5004=FACE_OUTER_BOUND('',#7932,.T.);
#5005=FACE_OUTER_BOUND('',#7933,.T.);
#5006=FACE_OUTER_BOUND('',#7934,.T.);
#5007=FACE_OUTER_BOUND('',#7935,.T.);
#5008=FACE_OUTER_BOUND('',#7936,.T.);
#5009=FACE_OUTER_BOUND('',#7937,.T.);
#5010=FACE_OUTER_BOUND('',#7938,.T.);
#5011=FACE_OUTER_BOUND('',#7939,.T.);
#5012=FACE_OUTER_BOUND('',#7940,.T.);
#5013=FACE_OUTER_BOUND('',#7941,.T.);
#5014=FACE_OUTER_BOUND('',#7942,.T.);
#5015=FACE_OUTER_BOUND('',#7943,.T.);
#5016=FACE_OUTER_BOUND('',#7944,.T.);
#5017=FACE_OUTER_BOUND('',#7945,.T.);
#5018=FACE_OUTER_BOUND('',#7946,.T.);
#5019=FACE_OUTER_BOUND('',#7947,.T.);
#5020=FACE_OUTER_BOUND('',#7948,.T.);
#5021=FACE_OUTER_BOUND('',#7949,.T.);
#5022=FACE_OUTER_BOUND('',#7950,.T.);
#5023=FACE_OUTER_BOUND('',#7951,.T.);
#5024=FACE_OUTER_BOUND('',#7952,.T.);
#5025=FACE_OUTER_BOUND('',#7953,.T.);
#5026=FACE_OUTER_BOUND('',#7954,.T.);
#5027=FACE_OUTER_BOUND('',#7955,.T.);
#5028=FACE_OUTER_BOUND('',#7956,.T.);
#5029=FACE_OUTER_BOUND('',#7957,.T.);
#5030=FACE_OUTER_BOUND('',#7958,.T.);
#5031=FACE_OUTER_BOUND('',#7959,.T.);
#5032=FACE_OUTER_BOUND('',#7960,.T.);
#5033=FACE_OUTER_BOUND('',#7961,.T.);
#5034=FACE_OUTER_BOUND('',#7962,.T.);
#5035=FACE_OUTER_BOUND('',#7963,.T.);
#5036=FACE_OUTER_BOUND('',#7964,.T.);
#5037=FACE_OUTER_BOUND('',#7965,.T.);
#5038=FACE_OUTER_BOUND('',#7966,.T.);
#5039=FACE_OUTER_BOUND('',#7967,.T.);
#5040=FACE_OUTER_BOUND('',#7968,.T.);
#5041=FACE_OUTER_BOUND('',#7969,.T.);
#5042=FACE_OUTER_BOUND('',#7970,.T.);
#5043=FACE_OUTER_BOUND('',#7971,.T.);
#5044=FACE_OUTER_BOUND('',#7972,.T.);
#5045=FACE_OUTER_BOUND('',#7973,.T.);
#5046=FACE_OUTER_BOUND('',#7974,.T.);
#5047=FACE_OUTER_BOUND('',#7975,.T.);
#5048=FACE_OUTER_BOUND('',#7976,.T.);
#5049=FACE_OUTER_BOUND('',#7977,.T.);
#5050=FACE_OUTER_BOUND('',#7978,.T.);
#5051=FACE_OUTER_BOUND('',#7979,.T.);
#5052=FACE_OUTER_BOUND('',#7980,.T.);
#5053=FACE_OUTER_BOUND('',#7981,.T.);
#5054=FACE_OUTER_BOUND('',#7982,.T.);
#5055=FACE_OUTER_BOUND('',#7983,.T.);
#5056=FACE_OUTER_BOUND('',#7984,.T.);
#5057=FACE_OUTER_BOUND('',#7985,.T.);
#5058=FACE_OUTER_BOUND('',#7986,.T.);
#5059=FACE_OUTER_BOUND('',#7987,.T.);
#5060=FACE_OUTER_BOUND('',#7988,.T.);
#5061=FACE_OUTER_BOUND('',#7989,.T.);
#5062=FACE_OUTER_BOUND('',#7990,.T.);
#5063=FACE_OUTER_BOUND('',#7991,.T.);
#5064=FACE_OUTER_BOUND('',#7992,.T.);
#5065=FACE_OUTER_BOUND('',#7993,.T.);
#5066=FACE_OUTER_BOUND('',#7994,.T.);
#5067=FACE_OUTER_BOUND('',#7995,.T.);
#5068=FACE_OUTER_BOUND('',#7996,.T.);
#5069=FACE_OUTER_BOUND('',#7997,.T.);
#5070=FACE_OUTER_BOUND('',#7998,.T.);
#5071=FACE_OUTER_BOUND('',#7999,.T.);
#5072=FACE_OUTER_BOUND('',#8000,.T.);
#5073=FACE_OUTER_BOUND('',#8001,.T.);
#5074=FACE_OUTER_BOUND('',#8002,.T.);
#5075=FACE_OUTER_BOUND('',#8003,.T.);
#5076=FACE_OUTER_BOUND('',#8004,.T.);
#5077=FACE_OUTER_BOUND('',#8005,.T.);
#5078=FACE_OUTER_BOUND('',#8006,.T.);
#5079=FACE_OUTER_BOUND('',#8007,.T.);
#5080=FACE_OUTER_BOUND('',#8008,.T.);
#5081=FACE_OUTER_BOUND('',#8009,.T.);
#5082=FACE_OUTER_BOUND('',#8010,.T.);
#5083=FACE_OUTER_BOUND('',#8011,.T.);
#5084=FACE_OUTER_BOUND('',#8012,.T.);
#5085=FACE_OUTER_BOUND('',#8013,.T.);
#5086=FACE_OUTER_BOUND('',#8014,.T.);
#5087=FACE_OUTER_BOUND('',#8015,.T.);
#5088=FACE_OUTER_BOUND('',#8016,.T.);
#5089=FACE_OUTER_BOUND('',#8017,.T.);
#5090=FACE_OUTER_BOUND('',#8018,.T.);
#5091=FACE_OUTER_BOUND('',#8019,.T.);
#5092=FACE_OUTER_BOUND('',#8020,.T.);
#5093=FACE_OUTER_BOUND('',#8021,.T.);
#5094=FACE_OUTER_BOUND('',#8022,.T.);
#5095=FACE_OUTER_BOUND('',#8023,.T.);
#5096=FACE_OUTER_BOUND('',#8024,.T.);
#5097=FACE_OUTER_BOUND('',#8025,.T.);
#5098=FACE_OUTER_BOUND('',#8026,.T.);
#5099=FACE_OUTER_BOUND('',#8027,.T.);
#5100=FACE_OUTER_BOUND('',#8028,.T.);
#5101=FACE_OUTER_BOUND('',#8029,.T.);
#5102=FACE_OUTER_BOUND('',#8030,.T.);
#5103=FACE_OUTER_BOUND('',#8031,.T.);
#5104=FACE_OUTER_BOUND('',#8032,.T.);
#5105=FACE_OUTER_BOUND('',#8033,.T.);
#5106=FACE_OUTER_BOUND('',#8034,.T.);
#5107=FACE_OUTER_BOUND('',#8035,.T.);
#5108=FACE_OUTER_BOUND('',#8036,.T.);
#5109=FACE_OUTER_BOUND('',#8037,.T.);
#5110=FACE_OUTER_BOUND('',#8038,.T.);
#5111=FACE_OUTER_BOUND('',#8039,.T.);
#5112=FACE_OUTER_BOUND('',#8040,.T.);
#5113=FACE_OUTER_BOUND('',#8041,.T.);
#5114=FACE_OUTER_BOUND('',#8042,.T.);
#5115=FACE_OUTER_BOUND('',#8043,.T.);
#5116=FACE_OUTER_BOUND('',#8044,.T.);
#5117=FACE_OUTER_BOUND('',#8045,.T.);
#5118=FACE_OUTER_BOUND('',#8046,.T.);
#5119=FACE_OUTER_BOUND('',#8047,.T.);
#5120=FACE_OUTER_BOUND('',#8048,.T.);
#5121=FACE_OUTER_BOUND('',#8049,.T.);
#5122=FACE_OUTER_BOUND('',#8050,.T.);
#5123=FACE_OUTER_BOUND('',#8051,.T.);
#5124=FACE_OUTER_BOUND('',#8052,.T.);
#5125=FACE_OUTER_BOUND('',#8053,.T.);
#5126=FACE_OUTER_BOUND('',#8054,.T.);
#5127=FACE_OUTER_BOUND('',#8055,.T.);
#5128=FACE_OUTER_BOUND('',#8056,.T.);
#5129=FACE_OUTER_BOUND('',#8057,.T.);
#5130=FACE_OUTER_BOUND('',#8058,.T.);
#5131=FACE_OUTER_BOUND('',#8059,.T.);
#5132=FACE_OUTER_BOUND('',#8060,.T.);
#5133=FACE_OUTER_BOUND('',#8061,.T.);
#5134=FACE_OUTER_BOUND('',#8062,.T.);
#5135=FACE_OUTER_BOUND('',#8063,.T.);
#5136=FACE_OUTER_BOUND('',#8064,.T.);
#5137=FACE_OUTER_BOUND('',#8065,.T.);
#5138=FACE_OUTER_BOUND('',#8066,.T.);
#5139=FACE_OUTER_BOUND('',#8067,.T.);
#5140=FACE_OUTER_BOUND('',#8068,.T.);
#5141=FACE_OUTER_BOUND('',#8069,.T.);
#5142=FACE_OUTER_BOUND('',#8070,.T.);
#5143=FACE_OUTER_BOUND('',#8071,.T.);
#5144=FACE_OUTER_BOUND('',#8072,.T.);
#5145=FACE_OUTER_BOUND('',#8073,.T.);
#5146=FACE_OUTER_BOUND('',#8074,.T.);
#5147=FACE_OUTER_BOUND('',#8075,.T.);
#5148=FACE_OUTER_BOUND('',#8076,.T.);
#5149=FACE_OUTER_BOUND('',#8077,.T.);
#5150=FACE_OUTER_BOUND('',#8078,.T.);
#5151=FACE_OUTER_BOUND('',#8079,.T.);
#5152=FACE_OUTER_BOUND('',#8080,.T.);
#5153=FACE_OUTER_BOUND('',#8081,.T.);
#5154=FACE_OUTER_BOUND('',#8082,.T.);
#5155=FACE_OUTER_BOUND('',#8083,.T.);
#5156=FACE_OUTER_BOUND('',#8084,.T.);
#5157=FACE_OUTER_BOUND('',#8085,.T.);
#5158=FACE_OUTER_BOUND('',#8086,.T.);
#5159=FACE_OUTER_BOUND('',#8087,.T.);
#5160=FACE_OUTER_BOUND('',#8088,.T.);
#5161=FACE_OUTER_BOUND('',#8089,.T.);
#5162=FACE_OUTER_BOUND('',#8090,.T.);
#5163=FACE_OUTER_BOUND('',#8091,.T.);
#5164=FACE_OUTER_BOUND('',#8092,.T.);
#5165=FACE_OUTER_BOUND('',#8093,.T.);
#5166=FACE_OUTER_BOUND('',#8094,.T.);
#5167=FACE_OUTER_BOUND('',#8095,.T.);
#5168=FACE_OUTER_BOUND('',#8096,.T.);
#5169=FACE_OUTER_BOUND('',#8097,.T.);
#5170=FACE_OUTER_BOUND('',#8098,.T.);
#5171=FACE_OUTER_BOUND('',#8099,.T.);
#5172=FACE_OUTER_BOUND('',#8100,.T.);
#5173=FACE_OUTER_BOUND('',#8101,.T.);
#5174=FACE_OUTER_BOUND('',#8102,.T.);
#5175=FACE_OUTER_BOUND('',#8103,.T.);
#5176=FACE_OUTER_BOUND('',#8104,.T.);
#5177=FACE_OUTER_BOUND('',#8105,.T.);
#5178=FACE_OUTER_BOUND('',#8106,.T.);
#5179=FACE_OUTER_BOUND('',#8107,.T.);
#5180=FACE_OUTER_BOUND('',#8108,.T.);
#5181=FACE_OUTER_BOUND('',#8109,.T.);
#5182=FACE_OUTER_BOUND('',#8110,.T.);
#5183=FACE_OUTER_BOUND('',#8111,.T.);
#5184=FACE_OUTER_BOUND('',#8112,.T.);
#5185=FACE_OUTER_BOUND('',#8113,.T.);
#5186=FACE_OUTER_BOUND('',#8114,.T.);
#5187=FACE_OUTER_BOUND('',#8115,.T.);
#5188=FACE_OUTER_BOUND('',#8116,.T.);
#5189=FACE_OUTER_BOUND('',#8117,.T.);
#5190=FACE_OUTER_BOUND('',#8118,.T.);
#5191=FACE_OUTER_BOUND('',#8119,.T.);
#5192=FACE_OUTER_BOUND('',#8120,.T.);
#5193=FACE_OUTER_BOUND('',#8121,.T.);
#5194=FACE_OUTER_BOUND('',#8122,.T.);
#5195=FACE_OUTER_BOUND('',#8123,.T.);
#5196=FACE_OUTER_BOUND('',#8124,.T.);
#5197=FACE_OUTER_BOUND('',#8125,.T.);
#5198=FACE_OUTER_BOUND('',#8126,.T.);
#5199=FACE_OUTER_BOUND('',#8127,.T.);
#5200=FACE_OUTER_BOUND('',#8128,.T.);
#5201=FACE_OUTER_BOUND('',#8129,.T.);
#5202=FACE_OUTER_BOUND('',#8130,.T.);
#5203=FACE_OUTER_BOUND('',#8131,.T.);
#5204=FACE_OUTER_BOUND('',#8132,.T.);
#5205=FACE_OUTER_BOUND('',#8133,.T.);
#5206=FACE_OUTER_BOUND('',#8134,.T.);
#5207=FACE_OUTER_BOUND('',#8135,.T.);
#5208=FACE_OUTER_BOUND('',#8136,.T.);
#5209=FACE_OUTER_BOUND('',#8137,.T.);
#5210=FACE_OUTER_BOUND('',#8138,.T.);
#5211=FACE_OUTER_BOUND('',#8139,.T.);
#5212=FACE_OUTER_BOUND('',#8140,.T.);
#5213=FACE_OUTER_BOUND('',#8141,.T.);
#5214=FACE_OUTER_BOUND('',#8142,.T.);
#5215=FACE_OUTER_BOUND('',#8143,.T.);
#5216=FACE_OUTER_BOUND('',#8144,.T.);
#5217=FACE_OUTER_BOUND('',#8145,.T.);
#5218=FACE_OUTER_BOUND('',#8146,.T.);
#5219=FACE_OUTER_BOUND('',#8147,.T.);
#5220=FACE_OUTER_BOUND('',#8148,.T.);
#5221=FACE_OUTER_BOUND('',#8149,.T.);
#5222=FACE_OUTER_BOUND('',#8150,.T.);
#5223=FACE_OUTER_BOUND('',#8151,.T.);
#5224=FACE_OUTER_BOUND('',#8152,.T.);
#5225=FACE_OUTER_BOUND('',#8153,.T.);
#5226=FACE_OUTER_BOUND('',#8154,.T.);
#5227=FACE_OUTER_BOUND('',#8155,.T.);
#5228=FACE_OUTER_BOUND('',#8156,.T.);
#5229=FACE_OUTER_BOUND('',#8157,.T.);
#5230=FACE_OUTER_BOUND('',#8158,.T.);
#5231=FACE_OUTER_BOUND('',#8159,.T.);
#5232=FACE_OUTER_BOUND('',#8160,.T.);
#5233=FACE_OUTER_BOUND('',#8161,.T.);
#5234=FACE_OUTER_BOUND('',#8162,.T.);
#5235=FACE_OUTER_BOUND('',#8163,.T.);
#5236=FACE_OUTER_BOUND('',#8164,.T.);
#5237=FACE_OUTER_BOUND('',#8165,.T.);
#5238=FACE_OUTER_BOUND('',#8166,.T.);
#5239=FACE_OUTER_BOUND('',#8167,.T.);
#5240=FACE_OUTER_BOUND('',#8168,.T.);
#5241=FACE_OUTER_BOUND('',#8169,.T.);
#5242=FACE_OUTER_BOUND('',#8170,.T.);
#5243=FACE_OUTER_BOUND('',#8171,.T.);
#5244=FACE_OUTER_BOUND('',#8172,.T.);
#5245=FACE_OUTER_BOUND('',#8173,.T.);
#5246=FACE_OUTER_BOUND('',#8174,.T.);
#5247=FACE_OUTER_BOUND('',#8175,.T.);
#5248=FACE_OUTER_BOUND('',#8177,.T.);
#5249=FACE_OUTER_BOUND('',#8178,.T.);
#5250=FACE_OUTER_BOUND('',#8179,.T.);
#5251=FACE_OUTER_BOUND('',#8180,.T.);
#5252=FACE_OUTER_BOUND('',#8181,.T.);
#5253=FACE_OUTER_BOUND('',#8182,.T.);
#5254=FACE_OUTER_BOUND('',#8183,.T.);
#5255=FACE_OUTER_BOUND('',#8184,.T.);
#5256=FACE_OUTER_BOUND('',#8185,.T.);
#5257=FACE_OUTER_BOUND('',#8186,.T.);
#5258=FACE_OUTER_BOUND('',#8187,.T.);
#5259=FACE_OUTER_BOUND('',#8188,.T.);
#5260=FACE_OUTER_BOUND('',#8189,.T.);
#5261=FACE_OUTER_BOUND('',#8190,.T.);
#5262=FACE_OUTER_BOUND('',#8191,.T.);
#5263=FACE_OUTER_BOUND('',#8192,.T.);
#5264=FACE_OUTER_BOUND('',#8193,.T.);
#5265=FACE_OUTER_BOUND('',#8194,.T.);
#5266=FACE_OUTER_BOUND('',#8195,.T.);
#5267=FACE_OUTER_BOUND('',#8196,.T.);
#5268=FACE_OUTER_BOUND('',#8197,.T.);
#5269=FACE_OUTER_BOUND('',#8198,.T.);
#5270=FACE_OUTER_BOUND('',#8199,.T.);
#5271=FACE_OUTER_BOUND('',#8200,.T.);
#5272=FACE_OUTER_BOUND('',#8201,.T.);
#5273=FACE_OUTER_BOUND('',#8202,.T.);
#5274=FACE_OUTER_BOUND('',#8203,.T.);
#5275=FACE_OUTER_BOUND('',#8204,.T.);
#5276=FACE_OUTER_BOUND('',#8205,.T.);
#5277=FACE_OUTER_BOUND('',#8206,.T.);
#5278=FACE_OUTER_BOUND('',#8207,.T.);
#5279=FACE_OUTER_BOUND('',#8208,.T.);
#5280=FACE_OUTER_BOUND('',#8209,.T.);
#5281=FACE_OUTER_BOUND('',#8210,.T.);
#5282=FACE_OUTER_BOUND('',#8211,.T.);
#5283=FACE_OUTER_BOUND('',#8212,.T.);
#5284=FACE_OUTER_BOUND('',#8213,.T.);
#5285=FACE_OUTER_BOUND('',#8214,.T.);
#5286=FACE_OUTER_BOUND('',#8215,.T.);
#5287=FACE_OUTER_BOUND('',#8216,.T.);
#5288=FACE_OUTER_BOUND('',#8217,.T.);
#5289=FACE_OUTER_BOUND('',#8218,.T.);
#5290=FACE_OUTER_BOUND('',#8219,.T.);
#5291=FACE_OUTER_BOUND('',#8220,.T.);
#5292=FACE_OUTER_BOUND('',#8221,.T.);
#5293=FACE_OUTER_BOUND('',#8222,.T.);
#5294=FACE_OUTER_BOUND('',#8223,.T.);
#5295=FACE_OUTER_BOUND('',#8224,.T.);
#5296=FACE_OUTER_BOUND('',#8225,.T.);
#5297=FACE_OUTER_BOUND('',#8226,.T.);
#5298=FACE_OUTER_BOUND('',#8227,.T.);
#5299=FACE_OUTER_BOUND('',#8228,.T.);
#5300=FACE_OUTER_BOUND('',#8229,.T.);
#5301=FACE_OUTER_BOUND('',#8230,.T.);
#5302=FACE_OUTER_BOUND('',#8231,.T.);
#5303=FACE_OUTER_BOUND('',#8232,.T.);
#5304=FACE_OUTER_BOUND('',#8233,.T.);
#5305=FACE_OUTER_BOUND('',#8234,.T.);
#5306=FACE_OUTER_BOUND('',#8235,.T.);
#5307=FACE_OUTER_BOUND('',#8236,.T.);
#5308=FACE_OUTER_BOUND('',#8237,.T.);
#5309=FACE_OUTER_BOUND('',#8238,.T.);
#5310=FACE_OUTER_BOUND('',#8239,.T.);
#5311=FACE_OUTER_BOUND('',#8240,.T.);
#5312=FACE_OUTER_BOUND('',#8241,.T.);
#5313=FACE_OUTER_BOUND('',#8242,.T.);
#5314=FACE_OUTER_BOUND('',#8243,.T.);
#5315=FACE_OUTER_BOUND('',#8244,.T.);
#5316=FACE_OUTER_BOUND('',#8245,.T.);
#5317=FACE_OUTER_BOUND('',#8246,.T.);
#5318=FACE_OUTER_BOUND('',#8247,.T.);
#5319=FACE_OUTER_BOUND('',#8248,.T.);
#5320=FACE_OUTER_BOUND('',#8249,.T.);
#5321=FACE_OUTER_BOUND('',#8250,.T.);
#5322=FACE_OUTER_BOUND('',#8251,.T.);
#5323=FACE_OUTER_BOUND('',#8252,.T.);
#5324=FACE_OUTER_BOUND('',#8253,.T.);
#5325=FACE_OUTER_BOUND('',#8254,.T.);
#5326=FACE_OUTER_BOUND('',#8255,.T.);
#5327=FACE_OUTER_BOUND('',#8256,.T.);
#5328=FACE_OUTER_BOUND('',#8257,.T.);
#5329=FACE_OUTER_BOUND('',#8258,.T.);
#5330=FACE_OUTER_BOUND('',#8259,.T.);
#5331=FACE_OUTER_BOUND('',#8260,.T.);
#5332=FACE_OUTER_BOUND('',#8261,.T.);
#5333=FACE_OUTER_BOUND('',#8262,.T.);
#5334=FACE_OUTER_BOUND('',#8263,.T.);
#5335=FACE_OUTER_BOUND('',#8264,.T.);
#5336=FACE_OUTER_BOUND('',#8265,.T.);
#5337=FACE_OUTER_BOUND('',#8266,.T.);
#5338=FACE_OUTER_BOUND('',#8267,.T.);
#5339=FACE_OUTER_BOUND('',#8268,.T.);
#5340=FACE_OUTER_BOUND('',#8269,.T.);
#5341=FACE_OUTER_BOUND('',#8270,.T.);
#5342=FACE_OUTER_BOUND('',#8271,.T.);
#5343=FACE_OUTER_BOUND('',#8272,.T.);
#5344=FACE_OUTER_BOUND('',#8273,.T.);
#5345=FACE_OUTER_BOUND('',#8274,.T.);
#5346=FACE_OUTER_BOUND('',#8275,.T.);
#5347=FACE_OUTER_BOUND('',#8276,.T.);
#5348=FACE_OUTER_BOUND('',#8277,.T.);
#5349=FACE_OUTER_BOUND('',#8278,.T.);
#5350=FACE_OUTER_BOUND('',#8279,.T.);
#5351=FACE_OUTER_BOUND('',#8280,.T.);
#5352=FACE_OUTER_BOUND('',#8281,.T.);
#5353=FACE_OUTER_BOUND('',#8282,.T.);
#5354=FACE_OUTER_BOUND('',#8283,.T.);
#5355=FACE_OUTER_BOUND('',#8284,.T.);
#5356=FACE_OUTER_BOUND('',#8285,.T.);
#5357=FACE_OUTER_BOUND('',#8286,.T.);
#5358=FACE_OUTER_BOUND('',#8287,.T.);
#5359=FACE_OUTER_BOUND('',#8288,.T.);
#5360=FACE_OUTER_BOUND('',#8289,.T.);
#5361=FACE_OUTER_BOUND('',#8290,.T.);
#5362=FACE_OUTER_BOUND('',#8291,.T.);
#5363=FACE_OUTER_BOUND('',#8292,.T.);
#5364=FACE_OUTER_BOUND('',#8293,.T.);
#5365=FACE_OUTER_BOUND('',#8294,.T.);
#5366=FACE_OUTER_BOUND('',#8295,.T.);
#5367=FACE_OUTER_BOUND('',#8296,.T.);
#5368=FACE_OUTER_BOUND('',#8297,.T.);
#5369=FACE_OUTER_BOUND('',#8298,.T.);
#5370=FACE_OUTER_BOUND('',#8299,.T.);
#5371=FACE_OUTER_BOUND('',#8300,.T.);
#5372=FACE_OUTER_BOUND('',#8301,.T.);
#5373=FACE_OUTER_BOUND('',#8302,.T.);
#5374=FACE_OUTER_BOUND('',#8303,.T.);
#5375=FACE_OUTER_BOUND('',#8304,.T.);
#5376=FACE_OUTER_BOUND('',#8305,.T.);
#5377=FACE_OUTER_BOUND('',#8306,.T.);
#5378=FACE_OUTER_BOUND('',#8307,.T.);
#5379=FACE_OUTER_BOUND('',#8308,.T.);
#5380=FACE_OUTER_BOUND('',#8309,.T.);
#5381=FACE_OUTER_BOUND('',#8310,.T.);
#5382=FACE_OUTER_BOUND('',#8311,.T.);
#5383=FACE_OUTER_BOUND('',#8312,.T.);
#5384=FACE_OUTER_BOUND('',#8313,.T.);
#5385=FACE_OUTER_BOUND('',#8314,.T.);
#5386=FACE_OUTER_BOUND('',#8315,.T.);
#5387=FACE_OUTER_BOUND('',#8316,.T.);
#5388=FACE_OUTER_BOUND('',#8317,.T.);
#5389=FACE_OUTER_BOUND('',#8318,.T.);
#5390=FACE_OUTER_BOUND('',#8319,.T.);
#5391=FACE_OUTER_BOUND('',#8320,.T.);
#5392=FACE_OUTER_BOUND('',#8321,.T.);
#5393=FACE_OUTER_BOUND('',#8322,.T.);
#5394=FACE_OUTER_BOUND('',#8323,.T.);
#5395=FACE_OUTER_BOUND('',#8324,.T.);
#5396=FACE_OUTER_BOUND('',#8325,.T.);
#5397=FACE_OUTER_BOUND('',#8326,.T.);
#5398=FACE_OUTER_BOUND('',#8327,.T.);
#5399=FACE_OUTER_BOUND('',#8328,.T.);
#5400=FACE_OUTER_BOUND('',#8329,.T.);
#5401=FACE_OUTER_BOUND('',#8330,.T.);
#5402=FACE_OUTER_BOUND('',#8331,.T.);
#5403=FACE_OUTER_BOUND('',#8332,.T.);
#5404=FACE_OUTER_BOUND('',#8333,.T.);
#5405=FACE_OUTER_BOUND('',#8334,.T.);
#5406=FACE_OUTER_BOUND('',#8335,.T.);
#5407=FACE_OUTER_BOUND('',#8336,.T.);
#5408=FACE_OUTER_BOUND('',#8337,.T.);
#5409=FACE_OUTER_BOUND('',#8338,.T.);
#5410=FACE_OUTER_BOUND('',#8339,.T.);
#5411=FACE_OUTER_BOUND('',#8340,.T.);
#5412=FACE_OUTER_BOUND('',#8341,.T.);
#5413=FACE_OUTER_BOUND('',#8342,.T.);
#5414=FACE_OUTER_BOUND('',#8343,.T.);
#5415=FACE_OUTER_BOUND('',#8344,.T.);
#5416=FACE_OUTER_BOUND('',#8345,.T.);
#5417=FACE_OUTER_BOUND('',#8346,.T.);
#5418=FACE_OUTER_BOUND('',#8347,.T.);
#5419=FACE_OUTER_BOUND('',#8348,.T.);
#5420=FACE_OUTER_BOUND('',#8349,.T.);
#5421=FACE_OUTER_BOUND('',#8350,.T.);
#5422=FACE_OUTER_BOUND('',#8351,.T.);
#5423=FACE_OUTER_BOUND('',#8352,.T.);
#5424=FACE_OUTER_BOUND('',#8353,.T.);
#5425=FACE_OUTER_BOUND('',#8354,.T.);
#5426=FACE_OUTER_BOUND('',#8355,.T.);
#5427=FACE_OUTER_BOUND('',#8356,.T.);
#5428=FACE_OUTER_BOUND('',#8357,.T.);
#5429=FACE_OUTER_BOUND('',#8358,.T.);
#5430=FACE_OUTER_BOUND('',#8359,.T.);
#5431=FACE_OUTER_BOUND('',#8360,.T.);
#5432=FACE_OUTER_BOUND('',#8361,.T.);
#5433=FACE_OUTER_BOUND('',#8362,.T.);
#5434=FACE_OUTER_BOUND('',#8363,.T.);
#5435=FACE_OUTER_BOUND('',#8364,.T.);
#5436=FACE_OUTER_BOUND('',#8365,.T.);
#5437=FACE_OUTER_BOUND('',#8366,.T.);
#5438=FACE_OUTER_BOUND('',#8367,.T.);
#5439=FACE_OUTER_BOUND('',#8368,.T.);
#5440=FACE_OUTER_BOUND('',#8369,.T.);
#5441=FACE_OUTER_BOUND('',#8370,.T.);
#5442=FACE_OUTER_BOUND('',#8371,.T.);
#5443=FACE_OUTER_BOUND('',#8372,.T.);
#5444=FACE_OUTER_BOUND('',#8373,.T.);
#5445=FACE_OUTER_BOUND('',#8374,.T.);
#5446=FACE_OUTER_BOUND('',#8375,.T.);
#5447=FACE_OUTER_BOUND('',#8376,.T.);
#5448=FACE_OUTER_BOUND('',#8377,.T.);
#5449=FACE_OUTER_BOUND('',#8378,.T.);
#5450=FACE_OUTER_BOUND('',#8379,.T.);
#5451=FACE_OUTER_BOUND('',#8380,.T.);
#5452=FACE_OUTER_BOUND('',#8381,.T.);
#5453=FACE_OUTER_BOUND('',#8382,.T.);
#5454=FACE_OUTER_BOUND('',#8383,.T.);
#5455=FACE_OUTER_BOUND('',#8384,.T.);
#5456=FACE_OUTER_BOUND('',#8385,.T.);
#5457=FACE_OUTER_BOUND('',#8386,.T.);
#5458=FACE_OUTER_BOUND('',#8387,.T.);
#5459=FACE_OUTER_BOUND('',#8388,.T.);
#5460=FACE_OUTER_BOUND('',#8389,.T.);
#5461=FACE_OUTER_BOUND('',#8390,.T.);
#5462=FACE_OUTER_BOUND('',#8391,.T.);
#5463=FACE_OUTER_BOUND('',#8392,.T.);
#5464=FACE_OUTER_BOUND('',#8393,.T.);
#5465=FACE_OUTER_BOUND('',#8394,.T.);
#5466=FACE_OUTER_BOUND('',#8395,.T.);
#5467=FACE_OUTER_BOUND('',#8396,.T.);
#5468=FACE_OUTER_BOUND('',#8397,.T.);
#5469=FACE_OUTER_BOUND('',#8398,.T.);
#5470=FACE_OUTER_BOUND('',#8399,.T.);
#5471=FACE_OUTER_BOUND('',#8400,.T.);
#5472=FACE_OUTER_BOUND('',#8401,.T.);
#5473=FACE_OUTER_BOUND('',#8402,.T.);
#5474=FACE_OUTER_BOUND('',#8403,.T.);
#5475=FACE_OUTER_BOUND('',#8404,.T.);
#5476=FACE_OUTER_BOUND('',#8405,.T.);
#5477=FACE_OUTER_BOUND('',#8406,.T.);
#5478=FACE_OUTER_BOUND('',#8407,.T.);
#5479=FACE_OUTER_BOUND('',#8408,.T.);
#5480=FACE_OUTER_BOUND('',#8409,.T.);
#5481=FACE_OUTER_BOUND('',#8410,.T.);
#5482=FACE_OUTER_BOUND('',#8411,.T.);
#5483=FACE_OUTER_BOUND('',#8412,.T.);
#5484=FACE_OUTER_BOUND('',#8413,.T.);
#5485=FACE_OUTER_BOUND('',#8414,.T.);
#5486=FACE_OUTER_BOUND('',#8415,.T.);
#5487=FACE_OUTER_BOUND('',#8416,.T.);
#5488=FACE_OUTER_BOUND('',#8417,.T.);
#5489=FACE_OUTER_BOUND('',#8418,.T.);
#5490=FACE_OUTER_BOUND('',#8419,.T.);
#5491=FACE_OUTER_BOUND('',#8420,.T.);
#5492=FACE_OUTER_BOUND('',#8421,.T.);
#5493=FACE_OUTER_BOUND('',#8422,.T.);
#5494=FACE_OUTER_BOUND('',#8423,.T.);
#5495=FACE_OUTER_BOUND('',#8424,.T.);
#5496=FACE_OUTER_BOUND('',#8425,.T.);
#5497=FACE_OUTER_BOUND('',#8426,.T.);
#5498=FACE_OUTER_BOUND('',#8427,.T.);
#5499=FACE_OUTER_BOUND('',#8428,.T.);
#5500=FACE_OUTER_BOUND('',#8429,.T.);
#5501=FACE_OUTER_BOUND('',#8430,.T.);
#5502=FACE_OUTER_BOUND('',#8431,.T.);
#5503=FACE_OUTER_BOUND('',#8432,.T.);
#5504=FACE_OUTER_BOUND('',#8433,.T.);
#5505=FACE_OUTER_BOUND('',#8434,.T.);
#5506=FACE_OUTER_BOUND('',#8435,.T.);
#5507=FACE_OUTER_BOUND('',#8436,.T.);
#5508=FACE_OUTER_BOUND('',#8437,.T.);
#5509=FACE_OUTER_BOUND('',#8438,.T.);
#5510=FACE_OUTER_BOUND('',#8439,.T.);
#5511=FACE_OUTER_BOUND('',#8440,.T.);
#5512=FACE_OUTER_BOUND('',#8441,.T.);
#5513=FACE_OUTER_BOUND('',#8442,.T.);
#5514=FACE_OUTER_BOUND('',#8443,.T.);
#5515=FACE_OUTER_BOUND('',#8444,.T.);
#5516=FACE_OUTER_BOUND('',#8445,.T.);
#5517=FACE_OUTER_BOUND('',#8446,.T.);
#5518=FACE_OUTER_BOUND('',#8447,.T.);
#5519=FACE_OUTER_BOUND('',#8448,.T.);
#5520=FACE_OUTER_BOUND('',#8449,.T.);
#5521=FACE_OUTER_BOUND('',#8450,.T.);
#5522=FACE_OUTER_BOUND('',#8451,.T.);
#5523=FACE_OUTER_BOUND('',#8452,.T.);
#5524=FACE_OUTER_BOUND('',#8453,.T.);
#5525=FACE_OUTER_BOUND('',#8454,.T.);
#5526=FACE_OUTER_BOUND('',#8455,.T.);
#5527=FACE_OUTER_BOUND('',#8456,.T.);
#5528=FACE_OUTER_BOUND('',#8457,.T.);
#5529=FACE_OUTER_BOUND('',#8458,.T.);
#5530=FACE_OUTER_BOUND('',#8459,.T.);
#5531=FACE_OUTER_BOUND('',#8460,.T.);
#5532=FACE_OUTER_BOUND('',#8461,.T.);
#5533=FACE_OUTER_BOUND('',#8462,.T.);
#5534=FACE_OUTER_BOUND('',#8463,.T.);
#5535=FACE_OUTER_BOUND('',#8464,.T.);
#5536=FACE_OUTER_BOUND('',#8465,.T.);
#5537=FACE_OUTER_BOUND('',#8466,.T.);
#5538=FACE_OUTER_BOUND('',#8467,.T.);
#5539=FACE_OUTER_BOUND('',#8468,.T.);
#5540=FACE_OUTER_BOUND('',#8469,.T.);
#5541=FACE_OUTER_BOUND('',#8470,.T.);
#5542=FACE_OUTER_BOUND('',#8471,.T.);
#5543=FACE_OUTER_BOUND('',#8472,.T.);
#5544=FACE_OUTER_BOUND('',#8473,.T.);
#5545=FACE_OUTER_BOUND('',#8474,.T.);
#5546=FACE_OUTER_BOUND('',#8475,.T.);
#5547=FACE_OUTER_BOUND('',#8476,.T.);
#5548=FACE_OUTER_BOUND('',#8477,.T.);
#5549=FACE_OUTER_BOUND('',#8478,.T.);
#5550=FACE_OUTER_BOUND('',#8479,.T.);
#5551=FACE_OUTER_BOUND('',#8480,.T.);
#5552=FACE_OUTER_BOUND('',#8481,.T.);
#5553=FACE_OUTER_BOUND('',#8482,.T.);
#5554=FACE_OUTER_BOUND('',#8483,.T.);
#5555=FACE_OUTER_BOUND('',#8484,.T.);
#5556=FACE_OUTER_BOUND('',#8485,.T.);
#5557=FACE_OUTER_BOUND('',#8486,.T.);
#5558=FACE_OUTER_BOUND('',#8487,.T.);
#5559=FACE_OUTER_BOUND('',#8488,.T.);
#5560=FACE_OUTER_BOUND('',#8489,.T.);
#5561=FACE_OUTER_BOUND('',#8490,.T.);
#5562=FACE_OUTER_BOUND('',#8491,.T.);
#5563=FACE_OUTER_BOUND('',#8492,.T.);
#5564=FACE_OUTER_BOUND('',#8493,.T.);
#5565=FACE_OUTER_BOUND('',#8494,.T.);
#5566=FACE_OUTER_BOUND('',#8495,.T.);
#5567=FACE_OUTER_BOUND('',#8496,.T.);
#5568=FACE_OUTER_BOUND('',#8497,.T.);
#5569=FACE_OUTER_BOUND('',#8498,.T.);
#5570=FACE_OUTER_BOUND('',#8499,.T.);
#5571=FACE_OUTER_BOUND('',#8500,.T.);
#5572=FACE_OUTER_BOUND('',#8501,.T.);
#5573=FACE_OUTER_BOUND('',#8502,.T.);
#5574=FACE_OUTER_BOUND('',#8503,.T.);
#5575=FACE_OUTER_BOUND('',#8504,.T.);
#5576=FACE_OUTER_BOUND('',#8505,.T.);
#5577=FACE_OUTER_BOUND('',#8506,.T.);
#5578=FACE_OUTER_BOUND('',#8507,.T.);
#5579=FACE_OUTER_BOUND('',#8508,.T.);
#5580=FACE_OUTER_BOUND('',#8509,.T.);
#5581=FACE_OUTER_BOUND('',#8510,.T.);
#5582=FACE_OUTER_BOUND('',#8511,.T.);
#5583=FACE_OUTER_BOUND('',#8512,.T.);
#5584=FACE_OUTER_BOUND('',#8513,.T.);
#5585=FACE_OUTER_BOUND('',#8514,.T.);
#5586=FACE_OUTER_BOUND('',#8515,.T.);
#5587=FACE_OUTER_BOUND('',#8516,.T.);
#5588=FACE_OUTER_BOUND('',#8517,.T.);
#5589=FACE_OUTER_BOUND('',#8518,.T.);
#5590=FACE_OUTER_BOUND('',#8519,.T.);
#5591=FACE_OUTER_BOUND('',#8520,.T.);
#5592=FACE_OUTER_BOUND('',#8521,.T.);
#5593=FACE_OUTER_BOUND('',#8522,.T.);
#5594=FACE_OUTER_BOUND('',#8523,.T.);
#5595=FACE_OUTER_BOUND('',#8524,.T.);
#5596=FACE_OUTER_BOUND('',#8525,.T.);
#5597=FACE_OUTER_BOUND('',#8526,.T.);
#5598=FACE_OUTER_BOUND('',#8527,.T.);
#5599=FACE_OUTER_BOUND('',#8528,.T.);
#5600=FACE_OUTER_BOUND('',#8529,.T.);
#5601=FACE_OUTER_BOUND('',#8530,.T.);
#5602=FACE_OUTER_BOUND('',#8531,.T.);
#5603=FACE_OUTER_BOUND('',#8532,.T.);
#5604=FACE_OUTER_BOUND('',#8533,.T.);
#5605=FACE_OUTER_BOUND('',#8534,.T.);
#5606=FACE_OUTER_BOUND('',#8535,.T.);
#5607=FACE_OUTER_BOUND('',#8536,.T.);
#5608=FACE_OUTER_BOUND('',#8537,.T.);
#5609=FACE_OUTER_BOUND('',#8538,.T.);
#5610=FACE_OUTER_BOUND('',#8539,.T.);
#5611=FACE_OUTER_BOUND('',#8540,.T.);
#5612=FACE_OUTER_BOUND('',#8541,.T.);
#5613=FACE_OUTER_BOUND('',#8542,.T.);
#5614=FACE_OUTER_BOUND('',#8543,.T.);
#5615=FACE_OUTER_BOUND('',#8544,.T.);
#5616=FACE_OUTER_BOUND('',#8545,.T.);
#5617=FACE_OUTER_BOUND('',#8546,.T.);
#5618=FACE_OUTER_BOUND('',#8547,.T.);
#5619=FACE_OUTER_BOUND('',#8548,.T.);
#5620=FACE_OUTER_BOUND('',#8549,.T.);
#5621=FACE_OUTER_BOUND('',#8550,.T.);
#5622=FACE_OUTER_BOUND('',#8551,.T.);
#5623=FACE_OUTER_BOUND('',#8552,.T.);
#5624=FACE_OUTER_BOUND('',#8553,.T.);
#5625=FACE_OUTER_BOUND('',#8554,.T.);
#5626=FACE_OUTER_BOUND('',#8555,.T.);
#5627=FACE_OUTER_BOUND('',#8556,.T.);
#5628=FACE_OUTER_BOUND('',#8557,.T.);
#5629=FACE_OUTER_BOUND('',#8558,.T.);
#5630=FACE_OUTER_BOUND('',#8559,.T.);
#5631=FACE_OUTER_BOUND('',#8560,.T.);
#5632=FACE_OUTER_BOUND('',#8561,.T.);
#5633=FACE_OUTER_BOUND('',#8562,.T.);
#5634=FACE_OUTER_BOUND('',#8563,.T.);
#5635=FACE_OUTER_BOUND('',#8564,.T.);
#5636=FACE_OUTER_BOUND('',#8565,.T.);
#5637=FACE_OUTER_BOUND('',#8566,.T.);
#5638=FACE_OUTER_BOUND('',#8567,.T.);
#5639=FACE_OUTER_BOUND('',#8568,.T.);
#5640=FACE_OUTER_BOUND('',#8569,.T.);
#5641=FACE_OUTER_BOUND('',#8570,.T.);
#5642=FACE_OUTER_BOUND('',#8571,.T.);
#5643=FACE_OUTER_BOUND('',#8572,.T.);
#5644=FACE_OUTER_BOUND('',#8573,.T.);
#5645=FACE_OUTER_BOUND('',#8574,.T.);
#5646=FACE_OUTER_BOUND('',#8575,.T.);
#5647=FACE_OUTER_BOUND('',#8576,.T.);
#5648=FACE_OUTER_BOUND('',#8577,.T.);
#5649=FACE_OUTER_BOUND('',#8578,.T.);
#5650=FACE_OUTER_BOUND('',#8579,.T.);
#5651=FACE_OUTER_BOUND('',#8580,.T.);
#5652=FACE_OUTER_BOUND('',#8581,.T.);
#5653=FACE_OUTER_BOUND('',#8582,.T.);
#5654=FACE_OUTER_BOUND('',#8583,.T.);
#5655=FACE_OUTER_BOUND('',#8584,.T.);
#5656=FACE_OUTER_BOUND('',#8585,.T.);
#5657=FACE_OUTER_BOUND('',#8586,.T.);
#5658=FACE_OUTER_BOUND('',#8587,.T.);
#5659=FACE_OUTER_BOUND('',#8588,.T.);
#5660=FACE_OUTER_BOUND('',#8589,.T.);
#5661=FACE_OUTER_BOUND('',#8590,.T.);
#5662=FACE_OUTER_BOUND('',#8591,.T.);
#5663=FACE_OUTER_BOUND('',#8592,.T.);
#5664=FACE_OUTER_BOUND('',#8593,.T.);
#5665=FACE_OUTER_BOUND('',#8594,.T.);
#5666=FACE_OUTER_BOUND('',#8595,.T.);
#5667=FACE_OUTER_BOUND('',#8596,.T.);
#5668=FACE_OUTER_BOUND('',#8597,.T.);
#5669=FACE_OUTER_BOUND('',#8598,.T.);
#5670=FACE_OUTER_BOUND('',#8599,.T.);
#5671=FACE_OUTER_BOUND('',#8600,.T.);
#5672=FACE_OUTER_BOUND('',#8601,.T.);
#5673=FACE_OUTER_BOUND('',#8602,.T.);
#5674=FACE_OUTER_BOUND('',#8603,.T.);
#5675=FACE_OUTER_BOUND('',#8604,.T.);
#5676=FACE_OUTER_BOUND('',#8605,.T.);
#5677=FACE_OUTER_BOUND('',#8606,.T.);
#5678=FACE_OUTER_BOUND('',#8607,.T.);
#5679=FACE_OUTER_BOUND('',#8608,.T.);
#5680=FACE_OUTER_BOUND('',#8609,.T.);
#5681=FACE_OUTER_BOUND('',#8610,.T.);
#5682=FACE_OUTER_BOUND('',#8611,.T.);
#5683=FACE_OUTER_BOUND('',#8612,.T.);
#5684=FACE_OUTER_BOUND('',#8613,.T.);
#5685=FACE_OUTER_BOUND('',#8614,.T.);
#5686=FACE_OUTER_BOUND('',#8615,.T.);
#5687=FACE_OUTER_BOUND('',#8616,.T.);
#5688=FACE_OUTER_BOUND('',#8617,.T.);
#5689=FACE_OUTER_BOUND('',#8618,.T.);
#5690=FACE_OUTER_BOUND('',#8619,.T.);
#5691=FACE_OUTER_BOUND('',#8620,.T.);
#5692=FACE_OUTER_BOUND('',#8621,.T.);
#5693=FACE_OUTER_BOUND('',#8622,.T.);
#5694=FACE_OUTER_BOUND('',#8623,.T.);
#5695=FACE_OUTER_BOUND('',#8624,.T.);
#5696=FACE_OUTER_BOUND('',#8625,.T.);
#5697=FACE_OUTER_BOUND('',#8626,.T.);
#5698=FACE_OUTER_BOUND('',#8627,.T.);
#5699=FACE_OUTER_BOUND('',#8628,.T.);
#5700=FACE_OUTER_BOUND('',#8629,.T.);
#5701=FACE_OUTER_BOUND('',#8630,.T.);
#5702=FACE_OUTER_BOUND('',#8631,.T.);
#5703=FACE_OUTER_BOUND('',#8632,.T.);
#5704=FACE_OUTER_BOUND('',#8633,.T.);
#5705=FACE_OUTER_BOUND('',#8634,.T.);
#5706=FACE_OUTER_BOUND('',#8635,.T.);
#5707=FACE_OUTER_BOUND('',#8636,.T.);
#5708=FACE_OUTER_BOUND('',#8637,.T.);
#5709=FACE_OUTER_BOUND('',#8638,.T.);
#5710=FACE_OUTER_BOUND('',#8639,.T.);
#5711=FACE_OUTER_BOUND('',#8640,.T.);
#5712=FACE_OUTER_BOUND('',#8641,.T.);
#5713=FACE_OUTER_BOUND('',#8642,.T.);
#5714=FACE_OUTER_BOUND('',#8643,.T.);
#5715=FACE_OUTER_BOUND('',#8644,.T.);
#5716=FACE_OUTER_BOUND('',#8645,.T.);
#5717=FACE_OUTER_BOUND('',#8646,.T.);
#5718=FACE_OUTER_BOUND('',#8647,.T.);
#5719=FACE_OUTER_BOUND('',#8648,.T.);
#5720=FACE_OUTER_BOUND('',#8649,.T.);
#5721=FACE_OUTER_BOUND('',#8650,.T.);
#5722=FACE_OUTER_BOUND('',#8651,.T.);
#5723=FACE_OUTER_BOUND('',#8652,.T.);
#5724=FACE_OUTER_BOUND('',#8653,.T.);
#5725=FACE_OUTER_BOUND('',#8654,.T.);
#5726=FACE_OUTER_BOUND('',#8655,.T.);
#5727=FACE_OUTER_BOUND('',#8656,.T.);
#5728=FACE_OUTER_BOUND('',#8657,.T.);
#5729=FACE_OUTER_BOUND('',#8658,.T.);
#5730=FACE_OUTER_BOUND('',#8659,.T.);
#5731=FACE_OUTER_BOUND('',#8660,.T.);
#5732=FACE_OUTER_BOUND('',#8661,.T.);
#5733=FACE_OUTER_BOUND('',#8662,.T.);
#5734=FACE_OUTER_BOUND('',#8663,.T.);
#5735=FACE_OUTER_BOUND('',#8664,.T.);
#5736=FACE_OUTER_BOUND('',#8665,.T.);
#5737=FACE_OUTER_BOUND('',#8666,.T.);
#5738=FACE_OUTER_BOUND('',#8667,.T.);
#5739=FACE_OUTER_BOUND('',#8668,.T.);
#5740=FACE_OUTER_BOUND('',#8669,.T.);
#5741=FACE_OUTER_BOUND('',#8670,.T.);
#5742=FACE_OUTER_BOUND('',#8671,.T.);
#5743=FACE_OUTER_BOUND('',#8672,.T.);
#5744=FACE_OUTER_BOUND('',#8673,.T.);
#5745=FACE_OUTER_BOUND('',#8674,.T.);
#5746=FACE_OUTER_BOUND('',#8675,.T.);
#5747=FACE_OUTER_BOUND('',#8676,.T.);
#5748=FACE_OUTER_BOUND('',#8677,.T.);
#5749=FACE_OUTER_BOUND('',#8678,.T.);
#5750=FACE_OUTER_BOUND('',#8679,.T.);
#5751=FACE_OUTER_BOUND('',#8680,.T.);
#5752=FACE_OUTER_BOUND('',#8681,.T.);
#5753=FACE_OUTER_BOUND('',#8682,.T.);
#5754=FACE_OUTER_BOUND('',#8683,.T.);
#5755=FACE_OUTER_BOUND('',#8684,.T.);
#5756=FACE_OUTER_BOUND('',#8685,.T.);
#5757=FACE_OUTER_BOUND('',#8686,.T.);
#5758=FACE_OUTER_BOUND('',#8687,.T.);
#5759=FACE_OUTER_BOUND('',#8688,.T.);
#5760=FACE_OUTER_BOUND('',#8689,.T.);
#5761=FACE_OUTER_BOUND('',#8690,.T.);
#5762=FACE_OUTER_BOUND('',#8691,.T.);
#5763=FACE_OUTER_BOUND('',#8692,.T.);
#5764=FACE_OUTER_BOUND('',#8693,.T.);
#5765=FACE_OUTER_BOUND('',#8694,.T.);
#5766=FACE_OUTER_BOUND('',#8695,.T.);
#5767=FACE_OUTER_BOUND('',#8696,.T.);
#5768=FACE_OUTER_BOUND('',#8697,.T.);
#5769=FACE_OUTER_BOUND('',#8698,.T.);
#5770=FACE_OUTER_BOUND('',#8699,.T.);
#5771=FACE_OUTER_BOUND('',#8700,.T.);
#5772=FACE_OUTER_BOUND('',#8701,.T.);
#5773=FACE_OUTER_BOUND('',#8702,.T.);
#5774=FACE_OUTER_BOUND('',#8703,.T.);
#5775=FACE_OUTER_BOUND('',#8704,.T.);
#5776=FACE_OUTER_BOUND('',#8705,.T.);
#5777=FACE_OUTER_BOUND('',#8706,.T.);
#5778=FACE_OUTER_BOUND('',#8707,.T.);
#5779=FACE_OUTER_BOUND('',#8708,.T.);
#5780=FACE_OUTER_BOUND('',#8709,.T.);
#5781=FACE_OUTER_BOUND('',#8710,.T.);
#5782=FACE_OUTER_BOUND('',#8711,.T.);
#5783=FACE_OUTER_BOUND('',#8712,.T.);
#5784=FACE_OUTER_BOUND('',#8713,.T.);
#5785=FACE_OUTER_BOUND('',#8714,.T.);
#5786=FACE_OUTER_BOUND('',#8715,.T.);
#5787=FACE_OUTER_BOUND('',#8716,.T.);
#5788=FACE_OUTER_BOUND('',#8717,.T.);
#5789=FACE_OUTER_BOUND('',#8718,.T.);
#5790=FACE_OUTER_BOUND('',#8719,.T.);
#5791=FACE_OUTER_BOUND('',#8720,.T.);
#5792=FACE_OUTER_BOUND('',#8721,.T.);
#5793=FACE_OUTER_BOUND('',#8722,.T.);
#5794=FACE_OUTER_BOUND('',#8723,.T.);
#5795=FACE_OUTER_BOUND('',#8724,.T.);
#5796=FACE_OUTER_BOUND('',#8725,.T.);
#5797=FACE_OUTER_BOUND('',#8726,.T.);
#5798=FACE_OUTER_BOUND('',#8727,.T.);
#5799=FACE_OUTER_BOUND('',#8728,.T.);
#5800=FACE_OUTER_BOUND('',#8729,.T.);
#5801=FACE_OUTER_BOUND('',#8730,.T.);
#5802=FACE_OUTER_BOUND('',#8731,.T.);
#5803=FACE_OUTER_BOUND('',#8732,.T.);
#5804=FACE_OUTER_BOUND('',#8733,.T.);
#5805=FACE_OUTER_BOUND('',#8734,.T.);
#5806=FACE_OUTER_BOUND('',#8735,.T.);
#5807=FACE_OUTER_BOUND('',#8736,.T.);
#5808=FACE_OUTER_BOUND('',#8737,.T.);
#5809=FACE_OUTER_BOUND('',#8738,.T.);
#5810=FACE_OUTER_BOUND('',#8739,.T.);
#5811=FACE_OUTER_BOUND('',#8740,.T.);
#5812=FACE_OUTER_BOUND('',#8741,.T.);
#5813=FACE_OUTER_BOUND('',#8742,.T.);
#5814=FACE_OUTER_BOUND('',#8743,.T.);
#5815=FACE_OUTER_BOUND('',#8744,.T.);
#5816=FACE_OUTER_BOUND('',#8745,.T.);
#5817=FACE_OUTER_BOUND('',#8746,.T.);
#5818=FACE_OUTER_BOUND('',#8747,.T.);
#5819=FACE_OUTER_BOUND('',#8748,.T.);
#5820=FACE_OUTER_BOUND('',#8749,.T.);
#5821=FACE_OUTER_BOUND('',#8750,.T.);
#5822=FACE_OUTER_BOUND('',#8751,.T.);
#5823=FACE_OUTER_BOUND('',#8752,.T.);
#5824=FACE_OUTER_BOUND('',#8753,.T.);
#5825=FACE_OUTER_BOUND('',#8754,.T.);
#5826=FACE_OUTER_BOUND('',#8755,.T.);
#5827=FACE_OUTER_BOUND('',#8756,.T.);
#5828=FACE_OUTER_BOUND('',#8757,.T.);
#5829=FACE_OUTER_BOUND('',#8758,.T.);
#5830=FACE_OUTER_BOUND('',#8759,.T.);
#5831=FACE_OUTER_BOUND('',#8760,.T.);
#5832=FACE_OUTER_BOUND('',#8761,.T.);
#5833=FACE_OUTER_BOUND('',#8762,.T.);
#5834=FACE_OUTER_BOUND('',#8763,.T.);
#5835=FACE_OUTER_BOUND('',#8764,.T.);
#5836=FACE_OUTER_BOUND('',#8765,.T.);
#5837=FACE_OUTER_BOUND('',#8766,.T.);
#5838=FACE_OUTER_BOUND('',#8767,.T.);
#5839=FACE_OUTER_BOUND('',#8768,.T.);
#5840=FACE_OUTER_BOUND('',#8769,.T.);
#5841=FACE_OUTER_BOUND('',#8770,.T.);
#5842=FACE_OUTER_BOUND('',#8771,.T.);
#5843=FACE_OUTER_BOUND('',#8772,.T.);
#5844=FACE_OUTER_BOUND('',#8773,.T.);
#5845=FACE_OUTER_BOUND('',#8774,.T.);
#5846=FACE_OUTER_BOUND('',#8775,.T.);
#5847=FACE_OUTER_BOUND('',#8776,.T.);
#5848=FACE_OUTER_BOUND('',#8777,.T.);
#5849=FACE_OUTER_BOUND('',#8778,.T.);
#5850=FACE_OUTER_BOUND('',#8779,.T.);
#5851=FACE_OUTER_BOUND('',#8780,.T.);
#5852=FACE_OUTER_BOUND('',#8781,.T.);
#5853=FACE_OUTER_BOUND('',#8782,.T.);
#5854=FACE_OUTER_BOUND('',#8783,.T.);
#5855=FACE_OUTER_BOUND('',#8784,.T.);
#5856=FACE_OUTER_BOUND('',#8785,.T.);
#5857=FACE_OUTER_BOUND('',#8786,.T.);
#5858=FACE_OUTER_BOUND('',#8787,.T.);
#5859=FACE_OUTER_BOUND('',#8788,.T.);
#5860=FACE_OUTER_BOUND('',#8789,.T.);
#5861=FACE_OUTER_BOUND('',#8790,.T.);
#5862=FACE_OUTER_BOUND('',#8791,.T.);
#5863=FACE_OUTER_BOUND('',#8792,.T.);
#5864=FACE_OUTER_BOUND('',#8793,.T.);
#5865=FACE_OUTER_BOUND('',#8794,.T.);
#5866=FACE_OUTER_BOUND('',#8795,.T.);
#5867=FACE_OUTER_BOUND('',#8796,.T.);
#5868=FACE_OUTER_BOUND('',#8797,.T.);
#5869=FACE_OUTER_BOUND('',#8798,.T.);
#5870=FACE_OUTER_BOUND('',#8799,.T.);
#5871=FACE_OUTER_BOUND('',#8800,.T.);
#5872=FACE_OUTER_BOUND('',#8801,.T.);
#5873=FACE_OUTER_BOUND('',#8802,.T.);
#5874=FACE_OUTER_BOUND('',#8803,.T.);
#5875=FACE_OUTER_BOUND('',#8804,.T.);
#5876=FACE_OUTER_BOUND('',#8805,.T.);
#5877=FACE_OUTER_BOUND('',#8806,.T.);
#5878=FACE_OUTER_BOUND('',#8807,.T.);
#5879=FACE_OUTER_BOUND('',#8808,.T.);
#5880=FACE_OUTER_BOUND('',#8809,.T.);
#5881=FACE_OUTER_BOUND('',#8810,.T.);
#5882=FACE_OUTER_BOUND('',#8811,.T.);
#5883=FACE_OUTER_BOUND('',#8812,.T.);
#5884=FACE_OUTER_BOUND('',#8813,.T.);
#5885=FACE_OUTER_BOUND('',#8814,.T.);
#5886=FACE_OUTER_BOUND('',#8815,.T.);
#5887=FACE_OUTER_BOUND('',#8816,.T.);
#5888=FACE_OUTER_BOUND('',#8817,.T.);
#5889=FACE_OUTER_BOUND('',#8818,.T.);
#5890=FACE_OUTER_BOUND('',#8819,.T.);
#5891=FACE_OUTER_BOUND('',#8820,.T.);
#5892=FACE_OUTER_BOUND('',#8821,.T.);
#5893=FACE_OUTER_BOUND('',#8822,.T.);
#5894=FACE_OUTER_BOUND('',#8823,.T.);
#5895=FACE_OUTER_BOUND('',#8824,.T.);
#5896=FACE_OUTER_BOUND('',#8825,.T.);
#5897=FACE_OUTER_BOUND('',#8826,.T.);
#5898=FACE_OUTER_BOUND('',#8827,.T.);
#5899=FACE_OUTER_BOUND('',#8828,.T.);
#5900=FACE_OUTER_BOUND('',#8829,.T.);
#5901=FACE_OUTER_BOUND('',#8830,.T.);
#5902=FACE_OUTER_BOUND('',#8831,.T.);
#5903=FACE_OUTER_BOUND('',#8832,.T.);
#5904=FACE_OUTER_BOUND('',#8833,.T.);
#5905=FACE_OUTER_BOUND('',#8834,.T.);
#5906=FACE_OUTER_BOUND('',#8835,.T.);
#5907=FACE_OUTER_BOUND('',#8836,.T.);
#5908=FACE_OUTER_BOUND('',#8837,.T.);
#5909=FACE_OUTER_BOUND('',#8838,.T.);
#5910=FACE_OUTER_BOUND('',#8839,.T.);
#5911=FACE_OUTER_BOUND('',#8840,.T.);
#5912=FACE_OUTER_BOUND('',#8841,.T.);
#5913=FACE_OUTER_BOUND('',#8842,.T.);
#5914=FACE_OUTER_BOUND('',#8843,.T.);
#5915=FACE_OUTER_BOUND('',#8844,.T.);
#5916=FACE_OUTER_BOUND('',#8845,.T.);
#5917=FACE_OUTER_BOUND('',#8846,.T.);
#5918=FACE_OUTER_BOUND('',#8847,.T.);
#5919=FACE_OUTER_BOUND('',#8848,.T.);
#5920=FACE_OUTER_BOUND('',#8849,.T.);
#5921=FACE_OUTER_BOUND('',#8850,.T.);
#5922=FACE_OUTER_BOUND('',#8851,.T.);
#5923=FACE_OUTER_BOUND('',#8852,.T.);
#5924=FACE_OUTER_BOUND('',#8853,.T.);
#5925=FACE_OUTER_BOUND('',#8854,.T.);
#5926=FACE_OUTER_BOUND('',#8855,.T.);
#5927=FACE_OUTER_BOUND('',#8856,.T.);
#5928=FACE_OUTER_BOUND('',#8857,.T.);
#5929=FACE_OUTER_BOUND('',#8858,.T.);
#5930=FACE_OUTER_BOUND('',#8859,.T.);
#5931=FACE_OUTER_BOUND('',#8860,.T.);
#5932=FACE_OUTER_BOUND('',#8861,.T.);
#5933=FACE_OUTER_BOUND('',#8862,.T.);
#5934=FACE_OUTER_BOUND('',#8863,.T.);
#5935=FACE_OUTER_BOUND('',#8864,.T.);
#5936=FACE_OUTER_BOUND('',#8865,.T.);
#5937=FACE_OUTER_BOUND('',#8866,.T.);
#5938=FACE_OUTER_BOUND('',#8867,.T.);
#5939=FACE_OUTER_BOUND('',#8868,.T.);
#5940=FACE_OUTER_BOUND('',#8869,.T.);
#5941=FACE_OUTER_BOUND('',#8870,.T.);
#5942=FACE_OUTER_BOUND('',#8871,.T.);
#5943=FACE_OUTER_BOUND('',#8872,.T.);
#5944=FACE_OUTER_BOUND('',#8873,.T.);
#5945=FACE_OUTER_BOUND('',#8874,.T.);
#5946=FACE_OUTER_BOUND('',#8875,.T.);
#5947=FACE_OUTER_BOUND('',#8876,.T.);
#5948=FACE_OUTER_BOUND('',#8877,.T.);
#5949=FACE_OUTER_BOUND('',#8878,.T.);
#5950=FACE_OUTER_BOUND('',#8879,.T.);
#5951=FACE_OUTER_BOUND('',#8880,.T.);
#5952=FACE_OUTER_BOUND('',#8881,.T.);
#5953=FACE_OUTER_BOUND('',#8882,.T.);
#5954=FACE_OUTER_BOUND('',#8883,.T.);
#5955=FACE_OUTER_BOUND('',#8884,.T.);
#5956=FACE_OUTER_BOUND('',#8885,.T.);
#5957=FACE_OUTER_BOUND('',#8886,.T.);
#5958=FACE_OUTER_BOUND('',#8887,.T.);
#5959=FACE_OUTER_BOUND('',#8888,.T.);
#5960=FACE_OUTER_BOUND('',#8889,.T.);
#5961=FACE_OUTER_BOUND('',#8890,.T.);
#5962=FACE_OUTER_BOUND('',#8891,.T.);
#5963=FACE_OUTER_BOUND('',#8892,.T.);
#5964=FACE_OUTER_BOUND('',#8893,.T.);
#5965=FACE_OUTER_BOUND('',#8894,.T.);
#5966=FACE_OUTER_BOUND('',#8895,.T.);
#5967=FACE_OUTER_BOUND('',#8896,.T.);
#5968=FACE_OUTER_BOUND('',#8897,.T.);
#5969=FACE_OUTER_BOUND('',#8898,.T.);
#5970=FACE_OUTER_BOUND('',#8899,.T.);
#5971=FACE_OUTER_BOUND('',#8900,.T.);
#5972=FACE_OUTER_BOUND('',#8901,.T.);
#5973=FACE_OUTER_BOUND('',#8902,.T.);
#5974=FACE_OUTER_BOUND('',#8903,.T.);
#5975=FACE_OUTER_BOUND('',#8904,.T.);
#5976=FACE_OUTER_BOUND('',#8905,.T.);
#5977=FACE_OUTER_BOUND('',#8906,.T.);
#5978=FACE_OUTER_BOUND('',#8907,.T.);
#5979=FACE_OUTER_BOUND('',#8908,.T.);
#5980=FACE_OUTER_BOUND('',#8909,.T.);
#5981=FACE_OUTER_BOUND('',#8910,.T.);
#5982=FACE_OUTER_BOUND('',#8911,.T.);
#5983=FACE_OUTER_BOUND('',#8912,.T.);
#5984=FACE_OUTER_BOUND('',#8913,.T.);
#5985=FACE_OUTER_BOUND('',#8914,.T.);
#5986=FACE_OUTER_BOUND('',#8915,.T.);
#5987=FACE_OUTER_BOUND('',#8916,.T.);
#5988=FACE_OUTER_BOUND('',#8917,.T.);
#5989=FACE_OUTER_BOUND('',#8918,.T.);
#5990=FACE_OUTER_BOUND('',#8919,.T.);
#5991=FACE_OUTER_BOUND('',#8920,.T.);
#5992=FACE_OUTER_BOUND('',#8921,.T.);
#5993=FACE_OUTER_BOUND('',#8922,.T.);
#5994=FACE_OUTER_BOUND('',#8923,.T.);
#5995=FACE_OUTER_BOUND('',#8924,.T.);
#5996=FACE_OUTER_BOUND('',#8925,.T.);
#5997=FACE_OUTER_BOUND('',#8926,.T.);
#5998=FACE_OUTER_BOUND('',#8927,.T.);
#5999=FACE_OUTER_BOUND('',#8928,.T.);
#6000=FACE_OUTER_BOUND('',#8929,.T.);
#6001=FACE_OUTER_BOUND('',#8930,.T.);
#6002=FACE_OUTER_BOUND('',#8931,.T.);
#6003=FACE_OUTER_BOUND('',#8932,.T.);
#6004=FACE_OUTER_BOUND('',#8933,.T.);
#6005=FACE_OUTER_BOUND('',#8934,.T.);
#6006=FACE_OUTER_BOUND('',#8935,.T.);
#6007=FACE_OUTER_BOUND('',#8936,.T.);
#6008=FACE_OUTER_BOUND('',#8937,.T.);
#6009=FACE_OUTER_BOUND('',#8938,.T.);
#6010=FACE_OUTER_BOUND('',#8939,.T.);
#6011=FACE_OUTER_BOUND('',#8940,.T.);
#6012=FACE_OUTER_BOUND('',#8941,.T.);
#6013=FACE_OUTER_BOUND('',#8942,.T.);
#6014=FACE_OUTER_BOUND('',#8943,.T.);
#6015=FACE_OUTER_BOUND('',#8944,.T.);
#6016=FACE_OUTER_BOUND('',#8945,.T.);
#6017=FACE_OUTER_BOUND('',#8946,.T.);
#6018=FACE_OUTER_BOUND('',#8947,.T.);
#6019=FACE_OUTER_BOUND('',#8948,.T.);
#6020=FACE_OUTER_BOUND('',#8949,.T.);
#6021=FACE_OUTER_BOUND('',#8950,.T.);
#6022=FACE_OUTER_BOUND('',#8951,.T.);
#6023=FACE_OUTER_BOUND('',#8952,.T.);
#6024=FACE_OUTER_BOUND('',#8953,.T.);
#6025=FACE_OUTER_BOUND('',#8954,.T.);
#6026=FACE_OUTER_BOUND('',#8955,.T.);
#6027=FACE_OUTER_BOUND('',#8956,.T.);
#6028=FACE_OUTER_BOUND('',#8957,.T.);
#6029=FACE_OUTER_BOUND('',#8958,.T.);
#6030=FACE_OUTER_BOUND('',#8959,.T.);
#6031=FACE_OUTER_BOUND('',#8960,.T.);
#6032=FACE_OUTER_BOUND('',#8961,.T.);
#6033=FACE_OUTER_BOUND('',#8962,.T.);
#6034=FACE_OUTER_BOUND('',#8963,.T.);
#6035=FACE_OUTER_BOUND('',#8964,.T.);
#6036=FACE_OUTER_BOUND('',#8965,.T.);
#6037=FACE_OUTER_BOUND('',#8966,.T.);
#6038=FACE_OUTER_BOUND('',#8967,.T.);
#6039=FACE_OUTER_BOUND('',#8968,.T.);
#6040=FACE_OUTER_BOUND('',#8969,.T.);
#6041=FACE_OUTER_BOUND('',#8970,.T.);
#6042=FACE_OUTER_BOUND('',#8971,.T.);
#6043=FACE_OUTER_BOUND('',#8972,.T.);
#6044=FACE_OUTER_BOUND('',#8973,.T.);
#6045=FACE_OUTER_BOUND('',#8974,.T.);
#6046=FACE_OUTER_BOUND('',#8975,.T.);
#6047=FACE_OUTER_BOUND('',#8976,.T.);
#6048=FACE_OUTER_BOUND('',#8977,.T.);
#6049=FACE_OUTER_BOUND('',#8978,.T.);
#6050=FACE_OUTER_BOUND('',#8979,.T.);
#6051=FACE_OUTER_BOUND('',#8980,.T.);
#6052=FACE_OUTER_BOUND('',#8981,.T.);
#6053=FACE_OUTER_BOUND('',#8982,.T.);
#6054=FACE_OUTER_BOUND('',#8983,.T.);
#6055=FACE_OUTER_BOUND('',#8984,.T.);
#6056=FACE_OUTER_BOUND('',#8985,.T.);
#6057=FACE_OUTER_BOUND('',#8986,.T.);
#6058=FACE_OUTER_BOUND('',#8987,.T.);
#6059=FACE_OUTER_BOUND('',#8988,.T.);
#6060=FACE_OUTER_BOUND('',#8989,.T.);
#6061=FACE_OUTER_BOUND('',#8990,.T.);
#6062=FACE_OUTER_BOUND('',#8991,.T.);
#6063=FACE_OUTER_BOUND('',#8992,.T.);
#6064=FACE_OUTER_BOUND('',#8993,.T.);
#6065=FACE_OUTER_BOUND('',#8994,.T.);
#6066=FACE_OUTER_BOUND('',#8995,.T.);
#6067=FACE_OUTER_BOUND('',#8996,.T.);
#6068=FACE_OUTER_BOUND('',#8997,.T.);
#6069=FACE_OUTER_BOUND('',#8998,.T.);
#6070=FACE_OUTER_BOUND('',#8999,.T.);
#6071=FACE_OUTER_BOUND('',#9000,.T.);
#6072=FACE_OUTER_BOUND('',#9001,.T.);
#6073=FACE_OUTER_BOUND('',#9002,.T.);
#6074=FACE_OUTER_BOUND('',#9003,.T.);
#6075=FACE_OUTER_BOUND('',#9004,.T.);
#6076=FACE_OUTER_BOUND('',#9005,.T.);
#6077=FACE_OUTER_BOUND('',#9006,.T.);
#6078=FACE_OUTER_BOUND('',#9007,.T.);
#6079=FACE_OUTER_BOUND('',#9008,.T.);
#6080=FACE_OUTER_BOUND('',#9009,.T.);
#6081=FACE_OUTER_BOUND('',#9010,.T.);
#6082=FACE_OUTER_BOUND('',#9011,.T.);
#6083=FACE_OUTER_BOUND('',#9012,.T.);
#6084=FACE_OUTER_BOUND('',#9013,.T.);
#6085=FACE_OUTER_BOUND('',#9014,.T.);
#6086=FACE_OUTER_BOUND('',#9015,.T.);
#6087=FACE_OUTER_BOUND('',#9016,.T.);
#6088=FACE_OUTER_BOUND('',#9017,.T.);
#6089=FACE_OUTER_BOUND('',#9018,.T.);
#6090=FACE_OUTER_BOUND('',#9019,.T.);
#6091=FACE_OUTER_BOUND('',#9020,.T.);
#6092=FACE_OUTER_BOUND('',#9021,.T.);
#6093=FACE_OUTER_BOUND('',#9022,.T.);
#6094=FACE_OUTER_BOUND('',#9023,.T.);
#6095=FACE_OUTER_BOUND('',#9024,.T.);
#6096=FACE_OUTER_BOUND('',#9025,.T.);
#6097=FACE_OUTER_BOUND('',#9026,.T.);
#6098=FACE_OUTER_BOUND('',#9027,.T.);
#6099=FACE_OUTER_BOUND('',#9028,.T.);
#6100=FACE_OUTER_BOUND('',#9029,.T.);
#6101=FACE_OUTER_BOUND('',#9030,.T.);
#6102=FACE_OUTER_BOUND('',#9031,.T.);
#6103=FACE_OUTER_BOUND('',#9032,.T.);
#6104=FACE_OUTER_BOUND('',#9033,.T.);
#6105=FACE_OUTER_BOUND('',#9034,.T.);
#6106=FACE_OUTER_BOUND('',#9035,.T.);
#6107=FACE_OUTER_BOUND('',#9036,.T.);
#6108=FACE_OUTER_BOUND('',#9037,.T.);
#6109=FACE_OUTER_BOUND('',#9038,.T.);
#6110=FACE_OUTER_BOUND('',#9039,.T.);
#6111=FACE_OUTER_BOUND('',#9040,.T.);
#6112=FACE_OUTER_BOUND('',#9041,.T.);
#6113=FACE_OUTER_BOUND('',#9042,.T.);
#6114=FACE_OUTER_BOUND('',#9043,.T.);
#6115=FACE_OUTER_BOUND('',#9044,.T.);
#6116=FACE_OUTER_BOUND('',#9045,.T.);
#6117=FACE_OUTER_BOUND('',#9046,.T.);
#6118=FACE_OUTER_BOUND('',#9047,.T.);
#6119=FACE_OUTER_BOUND('',#9048,.T.);
#6120=FACE_OUTER_BOUND('',#9049,.T.);
#6121=FACE_OUTER_BOUND('',#9050,.T.);
#6122=FACE_OUTER_BOUND('',#9051,.T.);
#6123=FACE_OUTER_BOUND('',#9052,.T.);
#6124=FACE_OUTER_BOUND('',#9053,.T.);
#6125=FACE_OUTER_BOUND('',#9054,.T.);
#6126=FACE_OUTER_BOUND('',#9055,.T.);
#6127=FACE_OUTER_BOUND('',#9056,.T.);
#6128=FACE_OUTER_BOUND('',#9057,.T.);
#6129=FACE_OUTER_BOUND('',#9058,.T.);
#6130=FACE_OUTER_BOUND('',#9059,.T.);
#6131=FACE_OUTER_BOUND('',#9060,.T.);
#6132=FACE_OUTER_BOUND('',#9061,.T.);
#6133=FACE_OUTER_BOUND('',#9062,.T.);
#6134=FACE_OUTER_BOUND('',#9063,.T.);
#6135=FACE_OUTER_BOUND('',#9064,.T.);
#6136=FACE_OUTER_BOUND('',#9065,.T.);
#6137=FACE_OUTER_BOUND('',#9066,.T.);
#6138=FACE_OUTER_BOUND('',#9067,.T.);
#6139=FACE_OUTER_BOUND('',#9068,.T.);
#6140=FACE_OUTER_BOUND('',#9069,.T.);
#6141=FACE_OUTER_BOUND('',#9070,.T.);
#6142=FACE_OUTER_BOUND('',#9071,.T.);
#6143=FACE_OUTER_BOUND('',#9072,.T.);
#6144=FACE_OUTER_BOUND('',#9073,.T.);
#6145=FACE_OUTER_BOUND('',#9074,.T.);
#6146=FACE_OUTER_BOUND('',#9075,.T.);
#6147=FACE_OUTER_BOUND('',#9076,.T.);
#6148=FACE_OUTER_BOUND('',#9077,.T.);
#6149=FACE_OUTER_BOUND('',#9078,.T.);
#6150=FACE_OUTER_BOUND('',#9079,.T.);
#6151=FACE_OUTER_BOUND('',#9080,.T.);
#6152=FACE_OUTER_BOUND('',#9081,.T.);
#6153=FACE_OUTER_BOUND('',#9082,.T.);
#6154=FACE_OUTER_BOUND('',#9083,.T.);
#6155=FACE_OUTER_BOUND('',#9084,.T.);
#6156=FACE_OUTER_BOUND('',#9085,.T.);
#6157=FACE_OUTER_BOUND('',#9086,.T.);
#6158=FACE_OUTER_BOUND('',#9087,.T.);
#6159=FACE_OUTER_BOUND('',#9088,.T.);
#6160=FACE_OUTER_BOUND('',#9089,.T.);
#6161=FACE_OUTER_BOUND('',#9090,.T.);
#6162=FACE_OUTER_BOUND('',#9091,.T.);
#6163=FACE_OUTER_BOUND('',#9092,.T.);
#6164=FACE_OUTER_BOUND('',#9093,.T.);
#6165=FACE_OUTER_BOUND('',#9094,.T.);
#6166=FACE_OUTER_BOUND('',#9095,.T.);
#6167=FACE_OUTER_BOUND('',#9096,.T.);
#6168=FACE_OUTER_BOUND('',#9097,.T.);
#6169=FACE_OUTER_BOUND('',#9098,.T.);
#6170=FACE_OUTER_BOUND('',#9099,.T.);
#6171=FACE_OUTER_BOUND('',#9100,.T.);
#6172=FACE_OUTER_BOUND('',#9101,.T.);
#6173=FACE_OUTER_BOUND('',#9102,.T.);
#6174=FACE_OUTER_BOUND('',#9103,.T.);
#6175=FACE_OUTER_BOUND('',#9104,.T.);
#6176=FACE_OUTER_BOUND('',#9105,.T.);
#6177=FACE_OUTER_BOUND('',#9106,.T.);
#6178=FACE_OUTER_BOUND('',#9107,.T.);
#6179=FACE_OUTER_BOUND('',#9108,.T.);
#6180=FACE_OUTER_BOUND('',#9109,.T.);
#6181=FACE_OUTER_BOUND('',#9110,.T.);
#6182=FACE_OUTER_BOUND('',#9111,.T.);
#6183=FACE_OUTER_BOUND('',#9112,.T.);
#6184=FACE_OUTER_BOUND('',#9113,.T.);
#6185=FACE_OUTER_BOUND('',#9114,.T.);
#6186=FACE_OUTER_BOUND('',#9115,.T.);
#6187=FACE_OUTER_BOUND('',#9116,.T.);
#6188=FACE_OUTER_BOUND('',#9117,.T.);
#6189=FACE_OUTER_BOUND('',#9118,.T.);
#6190=FACE_OUTER_BOUND('',#9119,.T.);
#6191=FACE_OUTER_BOUND('',#9120,.T.);
#6192=FACE_OUTER_BOUND('',#9121,.T.);
#6193=FACE_OUTER_BOUND('',#9122,.T.);
#6194=FACE_OUTER_BOUND('',#9123,.T.);
#6195=FACE_OUTER_BOUND('',#9124,.T.);
#6196=FACE_OUTER_BOUND('',#9125,.T.);
#6197=FACE_OUTER_BOUND('',#9126,.T.);
#6198=FACE_OUTER_BOUND('',#9127,.T.);
#6199=FACE_OUTER_BOUND('',#9128,.T.);
#6200=FACE_OUTER_BOUND('',#9129,.T.);
#6201=FACE_OUTER_BOUND('',#9130,.T.);
#6202=FACE_OUTER_BOUND('',#9131,.T.);
#6203=FACE_OUTER_BOUND('',#9132,.T.);
#6204=FACE_OUTER_BOUND('',#9133,.T.);
#6205=FACE_OUTER_BOUND('',#9134,.T.);
#6206=FACE_OUTER_BOUND('',#9135,.T.);
#6207=FACE_OUTER_BOUND('',#9136,.T.);
#6208=FACE_OUTER_BOUND('',#9137,.T.);
#6209=FACE_OUTER_BOUND('',#9138,.T.);
#6210=FACE_OUTER_BOUND('',#9139,.T.);
#6211=FACE_OUTER_BOUND('',#9140,.T.);
#6212=FACE_OUTER_BOUND('',#9141,.T.);
#6213=FACE_OUTER_BOUND('',#9142,.T.);
#6214=FACE_OUTER_BOUND('',#9143,.T.);
#6215=FACE_OUTER_BOUND('',#9144,.T.);
#6216=FACE_OUTER_BOUND('',#9145,.T.);
#6217=FACE_OUTER_BOUND('',#9146,.T.);
#6218=FACE_OUTER_BOUND('',#9147,.T.);
#6219=FACE_OUTER_BOUND('',#9148,.T.);
#6220=FACE_OUTER_BOUND('',#9149,.T.);
#6221=FACE_OUTER_BOUND('',#9150,.T.);
#6222=FACE_OUTER_BOUND('',#9151,.T.);
#6223=FACE_OUTER_BOUND('',#9152,.T.);
#6224=FACE_OUTER_BOUND('',#9153,.T.);
#6225=FACE_OUTER_BOUND('',#9154,.T.);
#6226=FACE_OUTER_BOUND('',#9155,.T.);
#6227=FACE_OUTER_BOUND('',#9156,.T.);
#6228=FACE_OUTER_BOUND('',#9157,.T.);
#6229=FACE_OUTER_BOUND('',#9158,.T.);
#6230=FACE_OUTER_BOUND('',#9159,.T.);
#6231=FACE_OUTER_BOUND('',#9160,.T.);
#6232=FACE_OUTER_BOUND('',#9161,.T.);
#6233=FACE_OUTER_BOUND('',#9162,.T.);
#6234=FACE_OUTER_BOUND('',#9163,.T.);
#6235=FACE_OUTER_BOUND('',#9164,.T.);
#6236=FACE_OUTER_BOUND('',#9165,.T.);
#6237=FACE_OUTER_BOUND('',#9166,.T.);
#6238=FACE_OUTER_BOUND('',#9167,.T.);
#6239=FACE_OUTER_BOUND('',#9168,.T.);
#6240=FACE_OUTER_BOUND('',#9169,.T.);
#6241=FACE_OUTER_BOUND('',#9170,.T.);
#6242=FACE_OUTER_BOUND('',#9171,.T.);
#6243=FACE_OUTER_BOUND('',#9172,.T.);
#6244=FACE_OUTER_BOUND('',#9173,.T.);
#6245=FACE_OUTER_BOUND('',#9174,.T.);
#6246=FACE_OUTER_BOUND('',#9175,.T.);
#6247=FACE_OUTER_BOUND('',#9176,.T.);
#6248=FACE_OUTER_BOUND('',#9177,.T.);
#6249=FACE_OUTER_BOUND('',#9178,.T.);
#6250=FACE_OUTER_BOUND('',#9179,.T.);
#6251=FACE_OUTER_BOUND('',#9180,.T.);
#6252=FACE_OUTER_BOUND('',#9181,.T.);
#6253=FACE_OUTER_BOUND('',#9182,.T.);
#6254=FACE_OUTER_BOUND('',#9183,.T.);
#6255=FACE_OUTER_BOUND('',#9184,.T.);
#6256=FACE_OUTER_BOUND('',#9185,.T.);
#6257=FACE_OUTER_BOUND('',#9186,.T.);
#6258=FACE_OUTER_BOUND('',#9187,.T.);
#6259=FACE_OUTER_BOUND('',#9188,.T.);
#6260=FACE_OUTER_BOUND('',#9189,.T.);
#6261=FACE_OUTER_BOUND('',#9190,.T.);
#6262=FACE_OUTER_BOUND('',#9191,.T.);
#6263=FACE_OUTER_BOUND('',#9192,.T.);
#6264=FACE_OUTER_BOUND('',#9193,.T.);
#6265=FACE_OUTER_BOUND('',#9194,.T.);
#6266=FACE_OUTER_BOUND('',#9195,.T.);
#6267=FACE_OUTER_BOUND('',#9196,.T.);
#6268=FACE_OUTER_BOUND('',#9197,.T.);
#6269=FACE_OUTER_BOUND('',#9198,.T.);
#6270=FACE_OUTER_BOUND('',#9199,.T.);
#6271=FACE_OUTER_BOUND('',#9200,.T.);
#6272=FACE_OUTER_BOUND('',#9201,.T.);
#6273=FACE_OUTER_BOUND('',#9202,.T.);
#6274=FACE_OUTER_BOUND('',#9203,.T.);
#6275=FACE_OUTER_BOUND('',#9204,.T.);
#6276=FACE_OUTER_BOUND('',#9205,.T.);
#6277=FACE_OUTER_BOUND('',#9206,.T.);
#6278=FACE_OUTER_BOUND('',#9207,.T.);
#6279=FACE_OUTER_BOUND('',#9208,.T.);
#6280=FACE_OUTER_BOUND('',#9209,.T.);
#6281=FACE_OUTER_BOUND('',#9210,.T.);
#6282=FACE_OUTER_BOUND('',#9211,.T.);
#6283=FACE_OUTER_BOUND('',#9212,.T.);
#6284=FACE_OUTER_BOUND('',#9213,.T.);
#6285=FACE_OUTER_BOUND('',#9214,.T.);
#6286=FACE_OUTER_BOUND('',#9215,.T.);
#6287=FACE_OUTER_BOUND('',#9216,.T.);
#6288=FACE_OUTER_BOUND('',#9217,.T.);
#6289=FACE_OUTER_BOUND('',#9218,.T.);
#6290=FACE_OUTER_BOUND('',#9219,.T.);
#6291=FACE_OUTER_BOUND('',#9220,.T.);
#6292=FACE_OUTER_BOUND('',#9221,.T.);
#6293=FACE_OUTER_BOUND('',#9222,.T.);
#6294=FACE_OUTER_BOUND('',#9223,.T.);
#6295=FACE_OUTER_BOUND('',#9224,.T.);
#6296=FACE_OUTER_BOUND('',#9225,.T.);
#6297=FACE_OUTER_BOUND('',#9226,.T.);
#6298=FACE_OUTER_BOUND('',#9227,.T.);
#6299=FACE_OUTER_BOUND('',#9228,.T.);
#6300=FACE_OUTER_BOUND('',#9229,.T.);
#6301=FACE_OUTER_BOUND('',#9230,.T.);
#6302=FACE_OUTER_BOUND('',#9231,.T.);
#6303=FACE_OUTER_BOUND('',#9232,.T.);
#6304=FACE_OUTER_BOUND('',#9233,.T.);
#6305=FACE_OUTER_BOUND('',#9234,.T.);
#6306=FACE_OUTER_BOUND('',#9235,.T.);
#6307=FACE_OUTER_BOUND('',#9236,.T.);
#6308=FACE_OUTER_BOUND('',#9237,.T.);
#6309=FACE_OUTER_BOUND('',#9238,.T.);
#6310=FACE_OUTER_BOUND('',#9239,.T.);
#6311=FACE_OUTER_BOUND('',#9240,.T.);
#6312=FACE_OUTER_BOUND('',#9241,.T.);
#6313=FACE_OUTER_BOUND('',#9242,.T.);
#6314=FACE_OUTER_BOUND('',#9243,.T.);
#6315=FACE_OUTER_BOUND('',#9244,.T.);
#6316=FACE_OUTER_BOUND('',#9245,.T.);
#6317=FACE_OUTER_BOUND('',#9246,.T.);
#6318=FACE_OUTER_BOUND('',#9247,.T.);
#6319=FACE_OUTER_BOUND('',#9248,.T.);
#6320=FACE_OUTER_BOUND('',#9249,.T.);
#6321=FACE_OUTER_BOUND('',#9250,.T.);
#6322=FACE_OUTER_BOUND('',#9251,.T.);
#6323=FACE_OUTER_BOUND('',#9252,.T.);
#6324=FACE_OUTER_BOUND('',#9253,.T.);
#6325=FACE_OUTER_BOUND('',#9254,.T.);
#6326=FACE_OUTER_BOUND('',#9255,.T.);
#6327=FACE_OUTER_BOUND('',#9256,.T.);
#6328=FACE_OUTER_BOUND('',#9257,.T.);
#6329=FACE_OUTER_BOUND('',#9258,.T.);
#6330=FACE_OUTER_BOUND('',#9259,.T.);
#6331=FACE_OUTER_BOUND('',#9260,.T.);
#6332=FACE_OUTER_BOUND('',#9261,.T.);
#6333=FACE_OUTER_BOUND('',#9262,.T.);
#6334=FACE_OUTER_BOUND('',#9263,.T.);
#6335=FACE_OUTER_BOUND('',#9264,.T.);
#6336=FACE_OUTER_BOUND('',#9265,.T.);
#6337=FACE_OUTER_BOUND('',#9266,.T.);
#6338=FACE_OUTER_BOUND('',#9267,.T.);
#6339=FACE_OUTER_BOUND('',#9268,.T.);
#6340=FACE_OUTER_BOUND('',#9269,.T.);
#6341=FACE_OUTER_BOUND('',#9270,.T.);
#6342=FACE_OUTER_BOUND('',#9271,.T.);
#6343=FACE_OUTER_BOUND('',#9272,.T.);
#6344=FACE_OUTER_BOUND('',#9273,.T.);
#6345=FACE_OUTER_BOUND('',#9274,.T.);
#6346=FACE_OUTER_BOUND('',#9275,.T.);
#6347=FACE_OUTER_BOUND('',#9276,.T.);
#6348=FACE_OUTER_BOUND('',#9277,.T.);
#6349=FACE_OUTER_BOUND('',#9278,.T.);
#6350=FACE_OUTER_BOUND('',#9279,.T.);
#6351=FACE_OUTER_BOUND('',#9280,.T.);
#6352=FACE_OUTER_BOUND('',#9281,.T.);
#6353=FACE_OUTER_BOUND('',#9282,.T.);
#6354=FACE_OUTER_BOUND('',#9283,.T.);
#6355=FACE_OUTER_BOUND('',#9284,.T.);
#6356=FACE_OUTER_BOUND('',#9285,.T.);
#6357=FACE_OUTER_BOUND('',#9286,.T.);
#6358=FACE_OUTER_BOUND('',#9287,.T.);
#6359=FACE_OUTER_BOUND('',#9288,.T.);
#6360=FACE_OUTER_BOUND('',#9289,.T.);
#6361=FACE_OUTER_BOUND('',#9290,.T.);
#6362=FACE_OUTER_BOUND('',#9291,.T.);
#6363=FACE_OUTER_BOUND('',#9292,.T.);
#6364=FACE_OUTER_BOUND('',#9293,.T.);
#6365=FACE_OUTER_BOUND('',#9294,.T.);
#6366=FACE_OUTER_BOUND('',#9295,.T.);
#6367=FACE_OUTER_BOUND('',#9296,.T.);
#6368=FACE_OUTER_BOUND('',#9297,.T.);
#6369=FACE_OUTER_BOUND('',#9298,.T.);
#6370=FACE_OUTER_BOUND('',#9299,.T.);
#6371=FACE_OUTER_BOUND('',#9300,.T.);
#6372=FACE_OUTER_BOUND('',#9301,.T.);
#6373=FACE_OUTER_BOUND('',#9302,.T.);
#6374=FACE_OUTER_BOUND('',#9303,.T.);
#6375=FACE_OUTER_BOUND('',#9304,.T.);
#6376=FACE_OUTER_BOUND('',#9305,.T.);
#6377=FACE_OUTER_BOUND('',#9306,.T.);
#6378=FACE_OUTER_BOUND('',#9307,.T.);
#6379=FACE_OUTER_BOUND('',#9308,.T.);
#6380=FACE_OUTER_BOUND('',#9309,.T.);
#6381=FACE_OUTER_BOUND('',#9310,.T.);
#6382=FACE_OUTER_BOUND('',#9311,.T.);
#6383=FACE_OUTER_BOUND('',#9312,.T.);
#6384=FACE_OUTER_BOUND('',#9313,.T.);
#6385=FACE_OUTER_BOUND('',#9314,.T.);
#6386=FACE_OUTER_BOUND('',#9315,.T.);
#6387=FACE_OUTER_BOUND('',#9316,.T.);
#6388=FACE_OUTER_BOUND('',#9317,.T.);
#6389=FACE_OUTER_BOUND('',#9318,.T.);
#6390=FACE_OUTER_BOUND('',#9319,.T.);
#6391=FACE_OUTER_BOUND('',#9320,.T.);
#6392=FACE_OUTER_BOUND('',#9321,.T.);
#6393=FACE_OUTER_BOUND('',#9322,.T.);
#6394=FACE_OUTER_BOUND('',#9323,.T.);
#6395=FACE_OUTER_BOUND('',#9324,.T.);
#6396=FACE_OUTER_BOUND('',#9325,.T.);
#6397=FACE_OUTER_BOUND('',#9326,.T.);
#6398=FACE_OUTER_BOUND('',#9327,.T.);
#6399=FACE_OUTER_BOUND('',#9328,.T.);
#6400=FACE_OUTER_BOUND('',#9329,.T.);
#6401=FACE_OUTER_BOUND('',#9330,.T.);
#6402=FACE_OUTER_BOUND('',#9331,.T.);
#6403=FACE_OUTER_BOUND('',#9333,.T.);
#6404=FACE_OUTER_BOUND('',#9335,.T.);
#6405=FACE_OUTER_BOUND('',#9337,.T.);
#6406=FACE_OUTER_BOUND('',#9338,.T.);
#6407=FACE_OUTER_BOUND('',#9339,.T.);
#6408=FACE_OUTER_BOUND('',#9341,.T.);
#6409=FACE_OUTER_BOUND('',#9343,.T.);
#6410=FACE_OUTER_BOUND('',#9344,.T.);
#6411=FACE_OUTER_BOUND('',#9345,.T.);
#6412=FACE_OUTER_BOUND('',#9346,.T.);
#6413=FACE_OUTER_BOUND('',#9347,.T.);
#6414=FACE_OUTER_BOUND('',#9348,.T.);
#6415=FACE_OUTER_BOUND('',#9349,.T.);
#6416=FACE_OUTER_BOUND('',#9350,.T.);
#6417=FACE_OUTER_BOUND('',#9351,.T.);
#6418=FACE_OUTER_BOUND('',#9352,.T.);
#6419=FACE_OUTER_BOUND('',#9353,.T.);
#6420=FACE_OUTER_BOUND('',#9354,.T.);
#6421=FACE_OUTER_BOUND('',#9355,.T.);
#6422=FACE_OUTER_BOUND('',#9356,.T.);
#6423=FACE_OUTER_BOUND('',#9357,.T.);
#6424=FACE_OUTER_BOUND('',#9358,.T.);
#6425=FACE_OUTER_BOUND('',#9359,.T.);
#6426=FACE_OUTER_BOUND('',#9360,.T.);
#6427=FACE_OUTER_BOUND('',#9361,.T.);
#6428=FACE_OUTER_BOUND('',#9362,.T.);
#6429=FACE_OUTER_BOUND('',#9363,.T.);
#6430=FACE_OUTER_BOUND('',#9364,.T.);
#6431=FACE_OUTER_BOUND('',#9365,.T.);
#6432=FACE_OUTER_BOUND('',#9366,.T.);
#6433=FACE_OUTER_BOUND('',#9367,.T.);
#6434=FACE_OUTER_BOUND('',#9368,.T.);
#6435=FACE_OUTER_BOUND('',#9369,.T.);
#6436=FACE_OUTER_BOUND('',#9370,.T.);
#6437=FACE_OUTER_BOUND('',#9371,.T.);
#6438=FACE_OUTER_BOUND('',#9372,.T.);
#6439=FACE_OUTER_BOUND('',#9373,.T.);
#6440=FACE_OUTER_BOUND('',#9374,.T.);
#6441=FACE_OUTER_BOUND('',#9375,.T.);
#6442=FACE_OUTER_BOUND('',#9376,.T.);
#6443=FACE_OUTER_BOUND('',#9377,.T.);
#6444=FACE_OUTER_BOUND('',#9378,.T.);
#6445=FACE_OUTER_BOUND('',#9379,.T.);
#6446=FACE_OUTER_BOUND('',#9380,.T.);
#6447=FACE_OUTER_BOUND('',#9381,.T.);
#6448=FACE_OUTER_BOUND('',#9382,.T.);
#6449=FACE_OUTER_BOUND('',#9383,.T.);
#6450=FACE_OUTER_BOUND('',#9384,.T.);
#6451=FACE_OUTER_BOUND('',#9385,.T.);
#6452=FACE_OUTER_BOUND('',#9386,.T.);
#6453=FACE_OUTER_BOUND('',#9387,.T.);
#6454=FACE_OUTER_BOUND('',#9388,.T.);
#6455=FACE_OUTER_BOUND('',#9389,.T.);
#6456=FACE_OUTER_BOUND('',#9390,.T.);
#6457=FACE_OUTER_BOUND('',#9391,.T.);
#6458=FACE_OUTER_BOUND('',#9392,.T.);
#6459=FACE_OUTER_BOUND('',#9393,.T.);
#6460=FACE_OUTER_BOUND('',#9394,.T.);
#6461=FACE_OUTER_BOUND('',#9395,.T.);
#6462=FACE_OUTER_BOUND('',#9396,.T.);
#6463=FACE_OUTER_BOUND('',#9397,.T.);
#6464=FACE_OUTER_BOUND('',#9398,.T.);
#6465=FACE_OUTER_BOUND('',#9400,.T.);
#6466=FACE_OUTER_BOUND('',#9402,.T.);
#6467=FACE_OUTER_BOUND('',#9404,.T.);
#6468=FACE_OUTER_BOUND('',#9406,.T.);
#6469=FACE_OUTER_BOUND('',#9407,.T.);
#6470=FACE_OUTER_BOUND('',#9408,.T.);
#6471=FACE_OUTER_BOUND('',#9409,.T.);
#6472=FACE_OUTER_BOUND('',#9410,.T.);
#6473=FACE_OUTER_BOUND('',#9411,.T.);
#6474=FACE_OUTER_BOUND('',#9412,.T.);
#6475=FACE_OUTER_BOUND('',#9413,.T.);
#6476=FACE_OUTER_BOUND('',#9414,.T.);
#6477=FACE_OUTER_BOUND('',#9415,.T.);
#6478=FACE_OUTER_BOUND('',#9416,.T.);
#6479=FACE_OUTER_BOUND('',#9417,.T.);
#6480=FACE_OUTER_BOUND('',#9418,.T.);
#6481=FACE_OUTER_BOUND('',#9419,.T.);
#6482=FACE_OUTER_BOUND('',#9420,.T.);
#6483=FACE_OUTER_BOUND('',#9421,.T.);
#6484=FACE_OUTER_BOUND('',#9422,.T.);
#6485=FACE_OUTER_BOUND('',#9423,.T.);
#6486=FACE_OUTER_BOUND('',#9424,.T.);
#6487=FACE_OUTER_BOUND('',#9425,.T.);
#6488=FACE_OUTER_BOUND('',#9426,.T.);
#6489=FACE_OUTER_BOUND('',#9427,.T.);
#6490=FACE_OUTER_BOUND('',#9428,.T.);
#6491=FACE_OUTER_BOUND('',#9429,.T.);
#6492=FACE_OUTER_BOUND('',#9430,.T.);
#6493=FACE_OUTER_BOUND('',#9431,.T.);
#6494=FACE_OUTER_BOUND('',#9432,.T.);
#6495=FACE_OUTER_BOUND('',#9433,.T.);
#6496=FACE_OUTER_BOUND('',#9434,.T.);
#6497=FACE_OUTER_BOUND('',#9435,.T.);
#6498=FACE_OUTER_BOUND('',#9436,.T.);
#6499=FACE_OUTER_BOUND('',#9437,.T.);
#6500=FACE_OUTER_BOUND('',#9438,.T.);
#6501=FACE_OUTER_BOUND('',#9439,.T.);
#6502=FACE_OUTER_BOUND('',#9440,.T.);
#6503=FACE_OUTER_BOUND('',#9441,.T.);
#6504=FACE_OUTER_BOUND('',#9442,.T.);
#6505=FACE_OUTER_BOUND('',#9443,.T.);
#6506=FACE_OUTER_BOUND('',#9444,.T.);
#6507=FACE_OUTER_BOUND('',#9445,.T.);
#6508=FACE_OUTER_BOUND('',#9446,.T.);
#6509=FACE_OUTER_BOUND('',#9447,.T.);
#6510=FACE_OUTER_BOUND('',#9448,.T.);
#6511=FACE_OUTER_BOUND('',#9449,.T.);
#6512=FACE_OUTER_BOUND('',#9450,.T.);
#6513=FACE_OUTER_BOUND('',#9451,.T.);
#6514=FACE_OUTER_BOUND('',#9452,.T.);
#6515=FACE_OUTER_BOUND('',#9453,.T.);
#6516=FACE_OUTER_BOUND('',#9454,.T.);
#6517=FACE_OUTER_BOUND('',#9455,.T.);
#6518=FACE_OUTER_BOUND('',#9456,.T.);
#6519=FACE_OUTER_BOUND('',#9457,.T.);
#6520=FACE_OUTER_BOUND('',#9458,.T.);
#6521=FACE_OUTER_BOUND('',#9459,.T.);
#6522=FACE_OUTER_BOUND('',#9460,.T.);
#6523=FACE_OUTER_BOUND('',#9461,.T.);
#6524=FACE_OUTER_BOUND('',#9462,.T.);
#6525=FACE_OUTER_BOUND('',#9463,.T.);
#6526=FACE_OUTER_BOUND('',#9464,.T.);
#6527=FACE_OUTER_BOUND('',#9465,.T.);
#6528=FACE_OUTER_BOUND('',#9466,.T.);
#6529=FACE_OUTER_BOUND('',#9467,.T.);
#6530=FACE_OUTER_BOUND('',#9468,.T.);
#6531=FACE_OUTER_BOUND('',#9469,.T.);
#6532=FACE_OUTER_BOUND('',#9470,.T.);
#6533=FACE_OUTER_BOUND('',#9471,.T.);
#6534=FACE_OUTER_BOUND('',#9472,.T.);
#6535=FACE_OUTER_BOUND('',#9473,.T.);
#6536=FACE_OUTER_BOUND('',#9474,.T.);
#6537=FACE_OUTER_BOUND('',#9475,.T.);
#6538=FACE_OUTER_BOUND('',#9476,.T.);
#6539=FACE_OUTER_BOUND('',#9477,.T.);
#6540=FACE_OUTER_BOUND('',#9478,.T.);
#6541=FACE_OUTER_BOUND('',#9479,.T.);
#6542=FACE_OUTER_BOUND('',#9480,.T.);
#6543=FACE_OUTER_BOUND('',#9481,.T.);
#6544=FACE_OUTER_BOUND('',#9482,.T.);
#6545=FACE_OUTER_BOUND('',#9483,.T.);
#6546=FACE_OUTER_BOUND('',#9484,.T.);
#6547=FACE_OUTER_BOUND('',#9485,.T.);
#6548=FACE_OUTER_BOUND('',#9486,.T.);
#6549=FACE_OUTER_BOUND('',#9487,.T.);
#6550=FACE_OUTER_BOUND('',#9488,.T.);
#6551=FACE_OUTER_BOUND('',#9489,.T.);
#6552=FACE_OUTER_BOUND('',#9490,.T.);
#6553=FACE_OUTER_BOUND('',#9491,.T.);
#6554=FACE_OUTER_BOUND('',#9492,.T.);
#6555=FACE_OUTER_BOUND('',#9493,.T.);
#6556=FACE_OUTER_BOUND('',#9494,.T.);
#6557=FACE_OUTER_BOUND('',#9495,.T.);
#6558=FACE_OUTER_BOUND('',#9496,.T.);
#6559=FACE_OUTER_BOUND('',#9497,.T.);
#6560=FACE_OUTER_BOUND('',#9498,.T.);
#6561=FACE_OUTER_BOUND('',#9499,.T.);
#6562=FACE_OUTER_BOUND('',#9500,.T.);
#6563=FACE_OUTER_BOUND('',#9501,.T.);
#6564=FACE_OUTER_BOUND('',#9502,.T.);
#6565=FACE_OUTER_BOUND('',#9503,.T.);
#6566=FACE_OUTER_BOUND('',#9504,.T.);
#6567=FACE_OUTER_BOUND('',#9505,.T.);
#6568=FACE_OUTER_BOUND('',#9506,.T.);
#6569=FACE_OUTER_BOUND('',#9507,.T.);
#6570=FACE_OUTER_BOUND('',#9508,.T.);
#6571=FACE_OUTER_BOUND('',#9509,.T.);
#6572=FACE_OUTER_BOUND('',#9510,.T.);
#6573=FACE_OUTER_BOUND('',#9511,.T.);
#6574=FACE_OUTER_BOUND('',#9513,.T.);
#6575=FACE_OUTER_BOUND('',#9514,.T.);
#6576=FACE_OUTER_BOUND('',#9515,.T.);
#6577=FACE_OUTER_BOUND('',#9517,.T.);
#6578=FACE_OUTER_BOUND('',#9518,.T.);
#6579=FACE_OUTER_BOUND('',#9519,.T.);
#6580=FACE_OUTER_BOUND('',#9520,.T.);
#6581=FACE_OUTER_BOUND('',#9521,.T.);
#6582=FACE_OUTER_BOUND('',#9522,.T.);
#6583=FACE_OUTER_BOUND('',#9523,.T.);
#6584=FACE_OUTER_BOUND('',#9524,.T.);
#6585=FACE_OUTER_BOUND('',#9525,.T.);
#6586=FACE_OUTER_BOUND('',#9526,.T.);
#6587=FACE_OUTER_BOUND('',#9527,.T.);
#6588=FACE_OUTER_BOUND('',#9528,.T.);
#6589=FACE_OUTER_BOUND('',#9529,.T.);
#6590=FACE_OUTER_BOUND('',#9530,.T.);
#6591=FACE_OUTER_BOUND('',#9531,.T.);
#6592=FACE_OUTER_BOUND('',#9532,.T.);
#6593=FACE_OUTER_BOUND('',#9533,.T.);
#6594=FACE_OUTER_BOUND('',#9534,.T.);
#6595=FACE_OUTER_BOUND('',#9535,.T.);
#6596=FACE_OUTER_BOUND('',#9536,.T.);
#6597=FACE_OUTER_BOUND('',#9537,.T.);
#6598=FACE_OUTER_BOUND('',#9538,.T.);
#6599=FACE_OUTER_BOUND('',#9539,.T.);
#6600=FACE_OUTER_BOUND('',#9540,.T.);
#6601=FACE_OUTER_BOUND('',#9541,.T.);
#6602=FACE_OUTER_BOUND('',#9546,.T.);
#6603=FACE_OUTER_BOUND('',#9553,.T.);
#6604=FACE_OUTER_BOUND('',#9554,.T.);
#6605=FACE_OUTER_BOUND('',#9555,.T.);
#6606=FACE_OUTER_BOUND('',#9556,.T.);
#6607=FACE_OUTER_BOUND('',#9558,.T.);
#6608=FACE_OUTER_BOUND('',#9559,.T.);
#6609=FACE_OUTER_BOUND('',#9560,.T.);
#6610=FACE_OUTER_BOUND('',#9561,.T.);
#6611=FACE_OUTER_BOUND('',#9562,.T.);
#6612=FACE_OUTER_BOUND('',#9564,.T.);
#6613=FACE_OUTER_BOUND('',#9565,.T.);
#6614=FACE_OUTER_BOUND('',#9566,.T.);
#6615=FACE_OUTER_BOUND('',#9567,.T.);
#6616=FACE_OUTER_BOUND('',#9568,.T.);
#6617=FACE_OUTER_BOUND('',#9569,.T.);
#6618=FACE_OUTER_BOUND('',#9570,.T.);
#6619=FACE_OUTER_BOUND('',#9571,.T.);
#6620=FACE_OUTER_BOUND('',#9572,.T.);
#6621=FACE_OUTER_BOUND('',#9574,.T.);
#6622=FACE_OUTER_BOUND('',#9576,.T.);
#6623=FACE_OUTER_BOUND('',#9578,.T.);
#6624=FACE_OUTER_BOUND('',#9579,.T.);
#6625=FACE_OUTER_BOUND('',#9580,.T.);
#6626=FACE_OUTER_BOUND('',#9581,.T.);
#6627=FACE_OUTER_BOUND('',#9582,.T.);
#6628=FACE_OUTER_BOUND('',#9583,.T.);
#6629=FACE_OUTER_BOUND('',#9584,.T.);
#6630=FACE_OUTER_BOUND('',#9585,.T.);
#6631=FACE_OUTER_BOUND('',#9586,.T.);
#6632=FACE_OUTER_BOUND('',#9587,.T.);
#6633=FACE_OUTER_BOUND('',#9588,.T.);
#6634=FACE_OUTER_BOUND('',#9589,.T.);
#6635=FACE_OUTER_BOUND('',#9590,.T.);
#6636=FACE_OUTER_BOUND('',#9591,.T.);
#6637=FACE_OUTER_BOUND('',#9592,.T.);
#6638=FACE_OUTER_BOUND('',#9593,.T.);
#6639=FACE_OUTER_BOUND('',#9594,.T.);
#6640=FACE_OUTER_BOUND('',#9595,.T.);
#6641=FACE_OUTER_BOUND('',#9596,.T.);
#6642=FACE_OUTER_BOUND('',#9597,.T.);
#6643=FACE_OUTER_BOUND('',#9598,.T.);
#6644=FACE_OUTER_BOUND('',#9599,.T.);
#6645=FACE_OUTER_BOUND('',#9600,.T.);
#6646=FACE_OUTER_BOUND('',#9601,.T.);
#6647=FACE_OUTER_BOUND('',#9602,.T.);
#6648=FACE_OUTER_BOUND('',#9603,.T.);
#6649=FACE_OUTER_BOUND('',#9604,.T.);
#6650=FACE_OUTER_BOUND('',#9605,.T.);
#6651=FACE_OUTER_BOUND('',#9606,.T.);
#6652=FACE_OUTER_BOUND('',#9608,.T.);
#6653=FACE_OUTER_BOUND('',#9609,.T.);
#6654=FACE_OUTER_BOUND('',#9610,.T.);
#6655=FACE_OUTER_BOUND('',#9611,.T.);
#6656=FACE_OUTER_BOUND('',#9612,.T.);
#6657=FACE_OUTER_BOUND('',#9613,.T.);
#6658=FACE_OUTER_BOUND('',#9614,.T.);
#6659=FACE_OUTER_BOUND('',#9615,.T.);
#6660=FACE_OUTER_BOUND('',#9616,.T.);
#6661=FACE_OUTER_BOUND('',#9617,.T.);
#6662=FACE_OUTER_BOUND('',#9618,.T.);
#6663=FACE_OUTER_BOUND('',#9619,.T.);
#6664=FACE_OUTER_BOUND('',#9620,.T.);
#6665=FACE_OUTER_BOUND('',#9621,.T.);
#6666=FACE_OUTER_BOUND('',#9622,.T.);
#6667=FACE_OUTER_BOUND('',#9623,.T.);
#6668=FACE_OUTER_BOUND('',#9624,.T.);
#6669=FACE_OUTER_BOUND('',#9625,.T.);
#6670=FACE_OUTER_BOUND('',#9626,.T.);
#6671=FACE_OUTER_BOUND('',#9627,.T.);
#6672=FACE_OUTER_BOUND('',#9628,.T.);
#6673=FACE_OUTER_BOUND('',#9629,.T.);
#6674=FACE_OUTER_BOUND('',#9630,.T.);
#6675=FACE_OUTER_BOUND('',#9631,.T.);
#6676=FACE_OUTER_BOUND('',#9632,.T.);
#6677=FACE_OUTER_BOUND('',#9634,.T.);
#6678=FACE_OUTER_BOUND('',#9635,.T.);
#6679=FACE_OUTER_BOUND('',#9636,.T.);
#6680=FACE_OUTER_BOUND('',#9637,.T.);
#6681=FACE_OUTER_BOUND('',#9638,.T.);
#6682=EDGE_LOOP('',(#28122,#28123,#28124,#28125));
#6683=EDGE_LOOP('',(#28126,#28127,#28128,#28129));
#6684=EDGE_LOOP('',(#28130));
#6685=EDGE_LOOP('',(#28131));
#6686=EDGE_LOOP('',(#28132));
#6687=EDGE_LOOP('',(#28133));
#6688=EDGE_LOOP('',(#28134,#28135,#28136,#28137,#28138));
#6689=EDGE_LOOP('',(#28139,#28140));
#6690=EDGE_LOOP('',(#28141));
#6691=EDGE_LOOP('',(#28142,#28143,#28144,#28145));
#6692=EDGE_LOOP('',(#28146,#28147,#28148,#28149));
#6693=EDGE_LOOP('',(#28150));
#6694=EDGE_LOOP('',(#28151));
#6695=EDGE_LOOP('',(#28152,#28153,#28154,#28155,#28156,#28157));
#6696=EDGE_LOOP('',(#28158,#28159,#28160));
#6697=EDGE_LOOP('',(#28161));
#6698=EDGE_LOOP('',(#28162,#28163));
#6699=EDGE_LOOP('',(#28164,#28165,#28166,#28167));
#6700=EDGE_LOOP('',(#28168,#28169,#28170,#28171));
#6701=EDGE_LOOP('',(#28172,#28173,#28174,#28175,#28176,#28177));
#6702=EDGE_LOOP('',(#28178,#28179,#28180,#28181));
#6703=EDGE_LOOP('',(#28182,#28183,#28184,#28185));
#6704=EDGE_LOOP('',(#28186,#28187,#28188,#28189));
#6705=EDGE_LOOP('',(#28190,#28191,#28192,#28193));
#6706=EDGE_LOOP('',(#28194,#28195,#28196,#28197,#28198,#28199));
#6707=EDGE_LOOP('',(#28200,#28201,#28202,#28203));
#6708=EDGE_LOOP('',(#28204,#28205,#28206,#28207,#28208,#28209));
#6709=EDGE_LOOP('',(#28210,#28211,#28212,#28213,#28214));
#6710=EDGE_LOOP('',(#28215,#28216,#28217,#28218,#28219));
#6711=EDGE_LOOP('',(#28220,#28221,#28222,#28223,#28224,#28225));
#6712=EDGE_LOOP('',(#28226,#28227,#28228,#28229,#28230,#28231));
#6713=EDGE_LOOP('',(#28232,#28233,#28234,#28235));
#6714=EDGE_LOOP('',(#28236,#28237,#28238,#28239));
#6715=EDGE_LOOP('',(#28240,#28241,#28242,#28243));
#6716=EDGE_LOOP('',(#28244,#28245,#28246,#28247));
#6717=EDGE_LOOP('',(#28248,#28249,#28250,#28251));
#6718=EDGE_LOOP('',(#28252,#28253,#28254,#28255));
#6719=EDGE_LOOP('',(#28256,#28257,#28258,#28259));
#6720=EDGE_LOOP('',(#28260,#28261,#28262,#28263));
#6721=EDGE_LOOP('',(#28264,#28265,#28266,#28267));
#6722=EDGE_LOOP('',(#28268,#28269,#28270,#28271,#28272,#28273,#28274,#28275,
#28276,#28277,#28278,#28279,#28280,#28281,#28282,#28283,#28284,#28285,#28286,
#28287,#28288,#28289,#28290,#28291,#28292,#28293,#28294,#28295,#28296,#28297,
#28298,#28299,#28300,#28301,#28302,#28303,#28304,#28305,#28306,#28307,#28308,
#28309,#28310,#28311,#28312,#28313,#28314,#28315,#28316,#28317,#28318,#28319,
#28320,#28321,#28322,#28323,#28324,#28325,#28326,#28327,#28328,#28329,#28330,
#28331,#28332,#28333,#28334,#28335,#28336,#28337,#28338,#28339,#28340,#28341,
#28342,#28343,#28344,#28345,#28346,#28347,#28348,#28349,#28350,#28351,#28352,
#28353,#28354,#28355,#28356,#28357,#28358,#28359,#28360,#28361,#28362,#28363,
#28364,#28365,#28366,#28367,#28368,#28369,#28370,#28371,#28372,#28373,#28374,
#28375,#28376,#28377,#28378,#28379,#28380,#28381,#28382,#28383,#28384,#28385,
#28386,#28387,#28388,#28389,#28390,#28391,#28392,#28393,#28394,#28395,#28396,
#28397,#28398,#28399,#28400,#28401,#28402,#28403,#28404,#28405,#28406,#28407,
#28408,#28409,#28410,#28411,#28412,#28413,#28414,#28415,#28416,#28417,#28418,
#28419,#28420,#28421,#28422,#28423,#28424,#28425,#28426,#28427,#28428,#28429,
#28430,#28431,#28432,#28433,#28434,#28435,#28436,#28437,#28438,#28439,#28440,
#28441,#28442,#28443,#28444,#28445,#28446,#28447,#28448,#28449,#28450,#28451,
#28452,#28453,#28454,#28455,#28456,#28457,#28458,#28459,#28460,#28461,#28462,
#28463,#28464,#28465,#28466,#28467,#28468,#28469,#28470,#28471));
#6723=EDGE_LOOP('',(#28472,#28473,#28474,#28475,#28476,#28477,#28478,#28479,
#28480,#28481,#28482,#28483,#28484,#28485,#28486,#28487,#28488,#28489,#28490,
#28491,#28492,#28493,#28494,#28495,#28496,#28497,#28498,#28499,#28500,#28501,
#28502,#28503,#28504,#28505,#28506,#28507,#28508,#28509,#28510,#28511,#28512,
#28513,#28514,#28515,#28516,#28517,#28518,#28519,#28520,#28521,#28522,#28523,
#28524,#28525,#28526,#28527,#28528,#28529,#28530,#28531,#28532,#28533,#28534,
#28535,#28536,#28537,#28538,#28539,#28540,#28541,#28542,#28543,#28544,#28545,
#28546,#28547,#28548,#28549,#28550,#28551,#28552,#28553,#28554,#28555,#28556,
#28557,#28558,#28559,#28560,#28561,#28562,#28563,#28564,#28565,#28566,#28567,
#28568,#28569,#28570,#28571,#28572,#28573,#28574,#28575,#28576,#28577,#28578,
#28579,#28580,#28581,#28582,#28583,#28584,#28585,#28586,#28587,#28588,#28589,
#28590,#28591,#28592,#28593,#28594,#28595,#28596,#28597,#28598,#28599,#28600,
#28601,#28602,#28603,#28604,#28605,#28606,#28607,#28608,#28609,#28610,#28611,
#28612,#28613,#28614,#28615,#28616,#28617,#28618,#28619,#28620,#28621,#28622,
#28623,#28624,#28625,#28626,#28627,#28628,#28629,#28630,#28631,#28632,#28633,
#28634,#28635,#28636,#28637,#28638,#28639,#28640,#28641,#28642,#28643,#28644,
#28645,#28646,#28647,#28648,#28649,#28650,#28651,#28652,#28653,#28654,#28655,
#28656,#28657,#28658,#28659,#28660,#28661,#28662,#28663,#28664,#28665,#28666,
#28667,#28668,#28669,#28670,#28671,#28672,#28673,#28674,#28675,#28676,#28677,
#28678,#28679,#28680,#28681,#28682,#28683,#28684,#28685,#28686,#28687,#28688,
#28689,#28690,#28691,#28692,#28693,#28694,#28695,#28696,#28697,#28698,#28699,
#28700,#28701,#28702,#28703,#28704,#28705,#28706,#28707,#28708,#28709,#28710,
#28711,#28712,#28713,#28714,#28715,#28716,#28717,#28718,#28719,#28720,#28721,
#28722,#28723,#28724,#28725,#28726,#28727,#28728,#28729,#28730,#28731,#28732,
#28733,#28734,#28735,#28736,#28737,#28738,#28739,#28740,#28741,#28742,#28743,
#28744,#28745,#28746,#28747,#28748,#28749,#28750,#28751,#28752,#28753,#28754,
#28755,#28756,#28757,#28758,#28759,#28760,#28761,#28762,#28763,#28764,#28765,
#28766,#28767,#28768,#28769,#28770,#28771,#28772,#28773,#28774,#28775));
#6724=EDGE_LOOP('',(#28776,#28777,#28778,#28779,#28780,#28781));
#6725=EDGE_LOOP('',(#28782,#28783,#28784,#28785));
#6726=EDGE_LOOP('',(#28786,#28787,#28788,#28789,#28790,#28791));
#6727=EDGE_LOOP('',(#28792,#28793,#28794,#28795,#28796,#28797));
#6728=EDGE_LOOP('',(#28798,#28799,#28800,#28801));
#6729=EDGE_LOOP('',(#28802,#28803,#28804,#28805));
#6730=EDGE_LOOP('',(#28806,#28807,#28808,#28809));
#6731=EDGE_LOOP('',(#28810,#28811,#28812,#28813));
#6732=EDGE_LOOP('',(#28814,#28815,#28816));
#6733=EDGE_LOOP('',(#28817,#28818,#28819,#28820));
#6734=EDGE_LOOP('',(#28821,#28822,#28823,#28824));
#6735=EDGE_LOOP('',(#28825,#28826,#28827,#28828,#28829,#28830));
#6736=EDGE_LOOP('',(#28831,#28832,#28833,#28834,#28835,#28836));
#6737=EDGE_LOOP('',(#28837,#28838,#28839,#28840));
#6738=EDGE_LOOP('',(#28841,#28842,#28843,#28844));
#6739=EDGE_LOOP('',(#28845,#28846,#28847,#28848));
#6740=EDGE_LOOP('',(#28849,#28850,#28851,#28852));
#6741=EDGE_LOOP('',(#28853,#28854,#28855,#28856));
#6742=EDGE_LOOP('',(#28857,#28858,#28859,#28860));
#6743=EDGE_LOOP('',(#28861,#28862,#28863,#28864,#28865,#28866));
#6744=EDGE_LOOP('',(#28867,#28868,#28869,#28870,#28871,#28872));
#6745=EDGE_LOOP('',(#28873,#28874,#28875,#28876));
#6746=EDGE_LOOP('',(#28877,#28878,#28879,#28880));
#6747=EDGE_LOOP('',(#28881,#28882,#28883,#28884));
#6748=EDGE_LOOP('',(#28885,#28886,#28887,#28888));
#6749=EDGE_LOOP('',(#28889,#28890,#28891,#28892));
#6750=EDGE_LOOP('',(#28893,#28894,#28895,#28896));
#6751=EDGE_LOOP('',(#28897,#28898,#28899,#28900,#28901,#28902));
#6752=EDGE_LOOP('',(#28903,#28904,#28905,#28906,#28907,#28908));
#6753=EDGE_LOOP('',(#28909,#28910,#28911,#28912));
#6754=EDGE_LOOP('',(#28913,#28914,#28915,#28916));
#6755=EDGE_LOOP('',(#28917,#28918,#28919,#28920));
#6756=EDGE_LOOP('',(#28921,#28922,#28923,#28924));
#6757=EDGE_LOOP('',(#28925,#28926,#28927,#28928));
#6758=EDGE_LOOP('',(#28929,#28930,#28931,#28932));
#6759=EDGE_LOOP('',(#28933,#28934,#28935,#28936,#28937,#28938));
#6760=EDGE_LOOP('',(#28939,#28940,#28941,#28942,#28943,#28944));
#6761=EDGE_LOOP('',(#28945,#28946,#28947,#28948));
#6762=EDGE_LOOP('',(#28949,#28950,#28951,#28952));
#6763=EDGE_LOOP('',(#28953,#28954,#28955,#28956));
#6764=EDGE_LOOP('',(#28957,#28958,#28959,#28960));
#6765=EDGE_LOOP('',(#28961,#28962,#28963,#28964));
#6766=EDGE_LOOP('',(#28965,#28966,#28967,#28968));
#6767=EDGE_LOOP('',(#28969,#28970,#28971,#28972,#28973,#28974));
#6768=EDGE_LOOP('',(#28975,#28976,#28977,#28978,#28979,#28980));
#6769=EDGE_LOOP('',(#28981,#28982,#28983,#28984));
#6770=EDGE_LOOP('',(#28985,#28986,#28987,#28988));
#6771=EDGE_LOOP('',(#28989,#28990,#28991,#28992));
#6772=EDGE_LOOP('',(#28993,#28994,#28995,#28996));
#6773=EDGE_LOOP('',(#28997,#28998,#28999,#29000));
#6774=EDGE_LOOP('',(#29001,#29002,#29003,#29004));
#6775=EDGE_LOOP('',(#29005,#29006,#29007,#29008,#29009,#29010));
#6776=EDGE_LOOP('',(#29011,#29012,#29013));
#6777=EDGE_LOOP('',(#29014,#29015,#29016,#29017));
#6778=EDGE_LOOP('',(#29018,#29019,#29020,#29021));
#6779=EDGE_LOOP('',(#29022,#29023,#29024,#29025,#29026,#29027));
#6780=EDGE_LOOP('',(#29028,#29029,#29030,#29031));
#6781=EDGE_LOOP('',(#29032,#29033,#29034,#29035));
#6782=EDGE_LOOP('',(#29036,#29037,#29038,#29039,#29040,#29041));
#6783=EDGE_LOOP('',(#29042,#29043,#29044,#29045));
#6784=EDGE_LOOP('',(#29046,#29047,#29048));
#6785=EDGE_LOOP('',(#29049,#29050,#29051,#29052));
#6786=EDGE_LOOP('',(#29053,#29054,#29055,#29056,#29057,#29058));
#6787=EDGE_LOOP('',(#29059,#29060,#29061,#29062));
#6788=EDGE_LOOP('',(#29063,#29064,#29065,#29066));
#6789=EDGE_LOOP('',(#29067,#29068,#29069,#29070));
#6790=EDGE_LOOP('',(#29071,#29072,#29073,#29074));
#6791=EDGE_LOOP('',(#29075,#29076,#29077,#29078,#29079,#29080));
#6792=EDGE_LOOP('',(#29081,#29082,#29083,#29084));
#6793=EDGE_LOOP('',(#29085,#29086,#29087,#29088));
#6794=EDGE_LOOP('',(#29089,#29090,#29091,#29092));
#6795=EDGE_LOOP('',(#29093,#29094,#29095,#29096,#29097,#29098));
#6796=EDGE_LOOP('',(#29099,#29100,#29101,#29102));
#6797=EDGE_LOOP('',(#29103,#29104,#29105,#29106));
#6798=EDGE_LOOP('',(#29107,#29108,#29109,#29110));
#6799=EDGE_LOOP('',(#29111,#29112,#29113,#29114,#29115,#29116));
#6800=EDGE_LOOP('',(#29117,#29118,#29119,#29120));
#6801=EDGE_LOOP('',(#29121,#29122,#29123,#29124));
#6802=EDGE_LOOP('',(#29125,#29126,#29127,#29128));
#6803=EDGE_LOOP('',(#29129,#29130,#29131,#29132,#29133,#29134));
#6804=EDGE_LOOP('',(#29135,#29136,#29137,#29138));
#6805=EDGE_LOOP('',(#29139,#29140,#29141,#29142));
#6806=EDGE_LOOP('',(#29143,#29144,#29145,#29146));
#6807=EDGE_LOOP('',(#29147,#29148,#29149));
#6808=EDGE_LOOP('',(#29150,#29151,#29152,#29153,#29154,#29155));
#6809=EDGE_LOOP('',(#29156,#29157,#29158,#29159));
#6810=EDGE_LOOP('',(#29160,#29161,#29162,#29163));
#6811=EDGE_LOOP('',(#29164,#29165,#29166,#29167,#29168,#29169));
#6812=EDGE_LOOP('',(#29170,#29171,#29172,#29173));
#6813=EDGE_LOOP('',(#29174,#29175,#29176));
#6814=EDGE_LOOP('',(#29177,#29178,#29179,#29180));
#6815=EDGE_LOOP('',(#29181,#29182,#29183,#29184));
#6816=EDGE_LOOP('',(#29185,#29186,#29187,#29188,#29189,#29190));
#6817=EDGE_LOOP('',(#29191,#29192,#29193,#29194));
#6818=EDGE_LOOP('',(#29195,#29196,#29197,#29198));
#6819=EDGE_LOOP('',(#29199,#29200,#29201,#29202,#29203,#29204));
#6820=EDGE_LOOP('',(#29205,#29206,#29207,#29208));
#6821=EDGE_LOOP('',(#29209,#29210,#29211,#29212));
#6822=EDGE_LOOP('',(#29213,#29214,#29215,#29216));
#6823=EDGE_LOOP('',(#29217,#29218,#29219,#29220));
#6824=EDGE_LOOP('',(#29221,#29222,#29223,#29224,#29225,#29226));
#6825=EDGE_LOOP('',(#29227,#29228,#29229,#29230));
#6826=EDGE_LOOP('',(#29231,#29232,#29233,#29234));
#6827=EDGE_LOOP('',(#29235,#29236,#29237,#29238));
#6828=EDGE_LOOP('',(#29239,#29240,#29241,#29242,#29243,#29244));
#6829=EDGE_LOOP('',(#29245,#29246,#29247,#29248));
#6830=EDGE_LOOP('',(#29249,#29250,#29251,#29252));
#6831=EDGE_LOOP('',(#29253,#29254,#29255,#29256));
#6832=EDGE_LOOP('',(#29257,#29258,#29259,#29260,#29261,#29262));
#6833=EDGE_LOOP('',(#29263,#29264,#29265,#29266));
#6834=EDGE_LOOP('',(#29267,#29268,#29269,#29270));
#6835=EDGE_LOOP('',(#29271,#29272,#29273,#29274));
#6836=EDGE_LOOP('',(#29275,#29276,#29277));
#6837=EDGE_LOOP('',(#29278,#29279,#29280,#29281,#29282,#29283));
#6838=EDGE_LOOP('',(#29284,#29285,#29286,#29287));
#6839=EDGE_LOOP('',(#29288,#29289,#29290,#29291));
#6840=EDGE_LOOP('',(#29292,#29293,#29294,#29295,#29296,#29297));
#6841=EDGE_LOOP('',(#29298,#29299,#29300,#29301));
#6842=EDGE_LOOP('',(#29302,#29303,#29304));
#6843=EDGE_LOOP('',(#29305,#29306,#29307,#29308));
#6844=EDGE_LOOP('',(#29309,#29310,#29311,#29312));
#6845=EDGE_LOOP('',(#29313,#29314,#29315,#29316,#29317,#29318));
#6846=EDGE_LOOP('',(#29319,#29320,#29321,#29322));
#6847=EDGE_LOOP('',(#29323,#29324,#29325,#29326));
#6848=EDGE_LOOP('',(#29327,#29328,#29329,#29330));
#6849=EDGE_LOOP('',(#29331,#29332,#29333,#29334,#29335,#29336));
#6850=EDGE_LOOP('',(#29337,#29338,#29339,#29340));
#6851=EDGE_LOOP('',(#29341,#29342,#29343,#29344));
#6852=EDGE_LOOP('',(#29345,#29346,#29347,#29348,#29349,#29350));
#6853=EDGE_LOOP('',(#29351,#29352,#29353,#29354));
#6854=EDGE_LOOP('',(#29355,#29356,#29357,#29358));
#6855=EDGE_LOOP('',(#29359,#29360,#29361,#29362));
#6856=EDGE_LOOP('',(#29363,#29364,#29365,#29366));
#6857=EDGE_LOOP('',(#29367,#29368,#29369,#29370,#29371,#29372));
#6858=EDGE_LOOP('',(#29373,#29374,#29375,#29376));
#6859=EDGE_LOOP('',(#29377,#29378,#29379,#29380));
#6860=EDGE_LOOP('',(#29381,#29382,#29383,#29384));
#6861=EDGE_LOOP('',(#29385,#29386,#29387,#29388,#29389,#29390));
#6862=EDGE_LOOP('',(#29391,#29392,#29393,#29394));
#6863=EDGE_LOOP('',(#29395,#29396,#29397,#29398));
#6864=EDGE_LOOP('',(#29399,#29400,#29401,#29402));
#6865=EDGE_LOOP('',(#29403,#29404,#29405));
#6866=EDGE_LOOP('',(#29406,#29407,#29408,#29409,#29410,#29411));
#6867=EDGE_LOOP('',(#29412,#29413,#29414,#29415));
#6868=EDGE_LOOP('',(#29416,#29417,#29418,#29419));
#6869=EDGE_LOOP('',(#29420,#29421,#29422,#29423,#29424,#29425));
#6870=EDGE_LOOP('',(#29426,#29427,#29428,#29429));
#6871=EDGE_LOOP('',(#29430,#29431,#29432));
#6872=EDGE_LOOP('',(#29433,#29434,#29435,#29436));
#6873=EDGE_LOOP('',(#29437,#29438,#29439,#29440));
#6874=EDGE_LOOP('',(#29441,#29442,#29443,#29444,#29445,#29446));
#6875=EDGE_LOOP('',(#29447,#29448,#29449,#29450));
#6876=EDGE_LOOP('',(#29451,#29452,#29453,#29454));
#6877=EDGE_LOOP('',(#29455,#29456,#29457,#29458));
#6878=EDGE_LOOP('',(#29459,#29460,#29461,#29462,#29463,#29464));
#6879=EDGE_LOOP('',(#29465,#29466,#29467,#29468));
#6880=EDGE_LOOP('',(#29469,#29470,#29471,#29472));
#6881=EDGE_LOOP('',(#29473,#29474,#29475,#29476));
#6882=EDGE_LOOP('',(#29477,#29478,#29479,#29480,#29481,#29482));
#6883=EDGE_LOOP('',(#29483,#29484,#29485,#29486));
#6884=EDGE_LOOP('',(#29487,#29488,#29489,#29490));
#6885=EDGE_LOOP('',(#29491,#29492,#29493,#29494,#29495,#29496));
#6886=EDGE_LOOP('',(#29497,#29498,#29499,#29500));
#6887=EDGE_LOOP('',(#29501,#29502,#29503,#29504));
#6888=EDGE_LOOP('',(#29505,#29506,#29507,#29508));
#6889=EDGE_LOOP('',(#29509,#29510,#29511,#29512));
#6890=EDGE_LOOP('',(#29513,#29514,#29515,#29516,#29517,#29518));
#6891=EDGE_LOOP('',(#29519,#29520,#29521,#29522));
#6892=EDGE_LOOP('',(#29523,#29524,#29525,#29526));
#6893=EDGE_LOOP('',(#29527,#29528,#29529,#29530));
#6894=EDGE_LOOP('',(#29531,#29532,#29533));
#6895=EDGE_LOOP('',(#29534,#29535,#29536,#29537,#29538,#29539));
#6896=EDGE_LOOP('',(#29540,#29541,#29542,#29543));
#6897=EDGE_LOOP('',(#29544,#29545,#29546,#29547));
#6898=EDGE_LOOP('',(#29548,#29549,#29550,#29551,#29552,#29553));
#6899=EDGE_LOOP('',(#29554,#29555,#29556,#29557));
#6900=EDGE_LOOP('',(#29558,#29559,#29560));
#6901=EDGE_LOOP('',(#29561,#29562,#29563,#29564));
#6902=EDGE_LOOP('',(#29565,#29566,#29567,#29568));
#6903=EDGE_LOOP('',(#29569,#29570,#29571,#29572,#29573,#29574));
#6904=EDGE_LOOP('',(#29575,#29576,#29577,#29578));
#6905=EDGE_LOOP('',(#29579,#29580,#29581,#29582));
#6906=EDGE_LOOP('',(#29583,#29584,#29585,#29586));
#6907=EDGE_LOOP('',(#29587,#29588,#29589,#29590,#29591,#29592));
#6908=EDGE_LOOP('',(#29593,#29594,#29595,#29596));
#6909=EDGE_LOOP('',(#29597,#29598,#29599,#29600));
#6910=EDGE_LOOP('',(#29601,#29602,#29603,#29604));
#6911=EDGE_LOOP('',(#29605,#29606,#29607,#29608,#29609,#29610));
#6912=EDGE_LOOP('',(#29611,#29612,#29613,#29614));
#6913=EDGE_LOOP('',(#29615,#29616,#29617,#29618));
#6914=EDGE_LOOP('',(#29619,#29620,#29621,#29622));
#6915=EDGE_LOOP('',(#29623,#29624,#29625,#29626,#29627,#29628));
#6916=EDGE_LOOP('',(#29629,#29630,#29631,#29632));
#6917=EDGE_LOOP('',(#29633,#29634,#29635,#29636));
#6918=EDGE_LOOP('',(#29637,#29638,#29639,#29640,#29641,#29642));
#6919=EDGE_LOOP('',(#29643,#29644,#29645,#29646));
#6920=EDGE_LOOP('',(#29647,#29648,#29649,#29650));
#6921=EDGE_LOOP('',(#29651,#29652,#29653,#29654));
#6922=EDGE_LOOP('',(#29655,#29656,#29657,#29658));
#6923=EDGE_LOOP('',(#29659,#29660,#29661));
#6924=EDGE_LOOP('',(#29662,#29663,#29664,#29665,#29666,#29667));
#6925=EDGE_LOOP('',(#29668,#29669,#29670,#29671));
#6926=EDGE_LOOP('',(#29672,#29673,#29674,#29675));
#6927=EDGE_LOOP('',(#29676,#29677,#29678,#29679,#29680,#29681));
#6928=EDGE_LOOP('',(#29682,#29683,#29684,#29685));
#6929=EDGE_LOOP('',(#29686,#29687,#29688));
#6930=EDGE_LOOP('',(#29689,#29690,#29691,#29692));
#6931=EDGE_LOOP('',(#29693,#29694,#29695,#29696));
#6932=EDGE_LOOP('',(#29697,#29698,#29699,#29700,#29701,#29702));
#6933=EDGE_LOOP('',(#29703,#29704,#29705,#29706));
#6934=EDGE_LOOP('',(#29707,#29708,#29709,#29710));
#6935=EDGE_LOOP('',(#29711,#29712,#29713,#29714));
#6936=EDGE_LOOP('',(#29715,#29716,#29717,#29718,#29719,#29720));
#6937=EDGE_LOOP('',(#29721,#29722,#29723,#29724));
#6938=EDGE_LOOP('',(#29725,#29726,#29727,#29728));
#6939=EDGE_LOOP('',(#29729,#29730,#29731,#29732));
#6940=EDGE_LOOP('',(#29733,#29734,#29735,#29736,#29737,#29738));
#6941=EDGE_LOOP('',(#29739,#29740,#29741,#29742));
#6942=EDGE_LOOP('',(#29743,#29744,#29745,#29746));
#6943=EDGE_LOOP('',(#29747,#29748,#29749,#29750));
#6944=EDGE_LOOP('',(#29751,#29752,#29753,#29754,#29755,#29756));
#6945=EDGE_LOOP('',(#29757,#29758,#29759,#29760));
#6946=EDGE_LOOP('',(#29761,#29762,#29763,#29764));
#6947=EDGE_LOOP('',(#29765,#29766,#29767,#29768));
#6948=EDGE_LOOP('',(#29769,#29770,#29771,#29772,#29773,#29774));
#6949=EDGE_LOOP('',(#29775,#29776,#29777,#29778));
#6950=EDGE_LOOP('',(#29779,#29780,#29781,#29782));
#6951=EDGE_LOOP('',(#29783,#29784,#29785,#29786));
#6952=EDGE_LOOP('',(#29787,#29788,#29789));
#6953=EDGE_LOOP('',(#29790,#29791,#29792,#29793,#29794,#29795));
#6954=EDGE_LOOP('',(#29796,#29797,#29798,#29799));
#6955=EDGE_LOOP('',(#29800,#29801,#29802,#29803));
#6956=EDGE_LOOP('',(#29804,#29805,#29806,#29807,#29808,#29809));
#6957=EDGE_LOOP('',(#29810,#29811,#29812,#29813));
#6958=EDGE_LOOP('',(#29814,#29815,#29816));
#6959=EDGE_LOOP('',(#29817,#29818,#29819,#29820));
#6960=EDGE_LOOP('',(#29821,#29822,#29823,#29824));
#6961=EDGE_LOOP('',(#29825,#29826,#29827,#29828,#29829,#29830));
#6962=EDGE_LOOP('',(#29831,#29832,#29833,#29834));
#6963=EDGE_LOOP('',(#29835,#29836,#29837,#29838));
#6964=EDGE_LOOP('',(#29839,#29840,#29841,#29842));
#6965=EDGE_LOOP('',(#29843,#29844,#29845,#29846,#29847,#29848));
#6966=EDGE_LOOP('',(#29849,#29850,#29851,#29852));
#6967=EDGE_LOOP('',(#29853,#29854,#29855,#29856));
#6968=EDGE_LOOP('',(#29857,#29858,#29859,#29860));
#6969=EDGE_LOOP('',(#29861,#29862,#29863,#29864,#29865,#29866));
#6970=EDGE_LOOP('',(#29867,#29868,#29869,#29870));
#6971=EDGE_LOOP('',(#29871,#29872,#29873,#29874));
#6972=EDGE_LOOP('',(#29875,#29876,#29877,#29878));
#6973=EDGE_LOOP('',(#29879,#29880,#29881,#29882,#29883,#29884));
#6974=EDGE_LOOP('',(#29885,#29886,#29887,#29888));
#6975=EDGE_LOOP('',(#29889,#29890,#29891,#29892));
#6976=EDGE_LOOP('',(#29893,#29894,#29895,#29896));
#6977=EDGE_LOOP('',(#29897,#29898,#29899,#29900,#29901,#29902));
#6978=EDGE_LOOP('',(#29903,#29904,#29905,#29906));
#6979=EDGE_LOOP('',(#29907,#29908,#29909,#29910));
#6980=EDGE_LOOP('',(#29911,#29912,#29913,#29914));
#6981=EDGE_LOOP('',(#29915,#29916,#29917));
#6982=EDGE_LOOP('',(#29918,#29919,#29920,#29921,#29922,#29923));
#6983=EDGE_LOOP('',(#29924,#29925,#29926,#29927));
#6984=EDGE_LOOP('',(#29928,#29929,#29930,#29931));
#6985=EDGE_LOOP('',(#29932,#29933,#29934,#29935,#29936,#29937));
#6986=EDGE_LOOP('',(#29938,#29939,#29940,#29941));
#6987=EDGE_LOOP('',(#29942,#29943,#29944));
#6988=EDGE_LOOP('',(#29945,#29946,#29947,#29948));
#6989=EDGE_LOOP('',(#29949,#29950,#29951,#29952));
#6990=EDGE_LOOP('',(#29953,#29954,#29955,#29956,#29957,#29958));
#6991=EDGE_LOOP('',(#29959,#29960,#29961,#29962));
#6992=EDGE_LOOP('',(#29963,#29964,#29965,#29966));
#6993=EDGE_LOOP('',(#29967,#29968,#29969,#29970));
#6994=EDGE_LOOP('',(#29971,#29972,#29973,#29974,#29975,#29976));
#6995=EDGE_LOOP('',(#29977,#29978,#29979,#29980));
#6996=EDGE_LOOP('',(#29981,#29982,#29983,#29984));
#6997=EDGE_LOOP('',(#29985,#29986,#29987,#29988));
#6998=EDGE_LOOP('',(#29989,#29990,#29991,#29992,#29993,#29994));
#6999=EDGE_LOOP('',(#29995,#29996,#29997,#29998));
#7000=EDGE_LOOP('',(#29999,#30000,#30001,#30002));
#7001=EDGE_LOOP('',(#30003,#30004,#30005,#30006));
#7002=EDGE_LOOP('',(#30007,#30008,#30009,#30010,#30011,#30012));
#7003=EDGE_LOOP('',(#30013,#30014,#30015,#30016));
#7004=EDGE_LOOP('',(#30017,#30018,#30019,#30020));
#7005=EDGE_LOOP('',(#30021,#30022,#30023,#30024));
#7006=EDGE_LOOP('',(#30025,#30026,#30027,#30028,#30029,#30030));
#7007=EDGE_LOOP('',(#30031,#30032,#30033,#30034));
#7008=EDGE_LOOP('',(#30035,#30036,#30037,#30038));
#7009=EDGE_LOOP('',(#30039,#30040,#30041,#30042));
#7010=EDGE_LOOP('',(#30043,#30044,#30045));
#7011=EDGE_LOOP('',(#30046,#30047,#30048,#30049,#30050,#30051));
#7012=EDGE_LOOP('',(#30052,#30053,#30054,#30055));
#7013=EDGE_LOOP('',(#30056,#30057,#30058,#30059));
#7014=EDGE_LOOP('',(#30060,#30061,#30062,#30063,#30064,#30065));
#7015=EDGE_LOOP('',(#30066,#30067,#30068,#30069));
#7016=EDGE_LOOP('',(#30070,#30071,#30072));
#7017=EDGE_LOOP('',(#30073,#30074,#30075,#30076));
#7018=EDGE_LOOP('',(#30077,#30078,#30079,#30080));
#7019=EDGE_LOOP('',(#30081,#30082,#30083,#30084,#30085,#30086));
#7020=EDGE_LOOP('',(#30087,#30088,#30089,#30090));
#7021=EDGE_LOOP('',(#30091,#30092,#30093,#30094));
#7022=EDGE_LOOP('',(#30095,#30096,#30097,#30098));
#7023=EDGE_LOOP('',(#30099,#30100,#30101,#30102,#30103,#30104));
#7024=EDGE_LOOP('',(#30105,#30106,#30107,#30108));
#7025=EDGE_LOOP('',(#30109,#30110,#30111,#30112));
#7026=EDGE_LOOP('',(#30113,#30114,#30115,#30116));
#7027=EDGE_LOOP('',(#30117,#30118,#30119,#30120,#30121,#30122));
#7028=EDGE_LOOP('',(#30123,#30124,#30125,#30126));
#7029=EDGE_LOOP('',(#30127,#30128,#30129,#30130));
#7030=EDGE_LOOP('',(#30131,#30132,#30133,#30134));
#7031=EDGE_LOOP('',(#30135,#30136,#30137,#30138,#30139,#30140));
#7032=EDGE_LOOP('',(#30141,#30142,#30143,#30144));
#7033=EDGE_LOOP('',(#30145,#30146,#30147,#30148));
#7034=EDGE_LOOP('',(#30149,#30150,#30151,#30152));
#7035=EDGE_LOOP('',(#30153,#30154,#30155,#30156,#30157,#30158));
#7036=EDGE_LOOP('',(#30159,#30160,#30161,#30162));
#7037=EDGE_LOOP('',(#30163,#30164,#30165,#30166));
#7038=EDGE_LOOP('',(#30167,#30168,#30169,#30170));
#7039=EDGE_LOOP('',(#30171,#30172,#30173));
#7040=EDGE_LOOP('',(#30174,#30175,#30176,#30177,#30178,#30179));
#7041=EDGE_LOOP('',(#30180,#30181,#30182,#30183));
#7042=EDGE_LOOP('',(#30184,#30185,#30186,#30187));
#7043=EDGE_LOOP('',(#30188,#30189,#30190,#30191,#30192,#30193));
#7044=EDGE_LOOP('',(#30194,#30195,#30196,#30197));
#7045=EDGE_LOOP('',(#30198,#30199,#30200));
#7046=EDGE_LOOP('',(#30201,#30202,#30203,#30204));
#7047=EDGE_LOOP('',(#30205,#30206,#30207,#30208));
#7048=EDGE_LOOP('',(#30209,#30210,#30211,#30212,#30213,#30214));
#7049=EDGE_LOOP('',(#30215,#30216,#30217,#30218));
#7050=EDGE_LOOP('',(#30219,#30220,#30221,#30222));
#7051=EDGE_LOOP('',(#30223,#30224,#30225,#30226));
#7052=EDGE_LOOP('',(#30227,#30228,#30229,#30230,#30231,#30232));
#7053=EDGE_LOOP('',(#30233,#30234,#30235,#30236));
#7054=EDGE_LOOP('',(#30237,#30238,#30239,#30240));
#7055=EDGE_LOOP('',(#30241,#30242,#30243,#30244));
#7056=EDGE_LOOP('',(#30245,#30246,#30247,#30248,#30249,#30250));
#7057=EDGE_LOOP('',(#30251,#30252,#30253,#30254));
#7058=EDGE_LOOP('',(#30255,#30256,#30257,#30258));
#7059=EDGE_LOOP('',(#30259,#30260,#30261,#30262));
#7060=EDGE_LOOP('',(#30263,#30264,#30265,#30266,#30267,#30268));
#7061=EDGE_LOOP('',(#30269,#30270,#30271,#30272));
#7062=EDGE_LOOP('',(#30273,#30274,#30275,#30276));
#7063=EDGE_LOOP('',(#30277,#30278,#30279,#30280));
#7064=EDGE_LOOP('',(#30281,#30282,#30283,#30284,#30285,#30286));
#7065=EDGE_LOOP('',(#30287,#30288,#30289,#30290));
#7066=EDGE_LOOP('',(#30291,#30292,#30293,#30294));
#7067=EDGE_LOOP('',(#30295,#30296,#30297,#30298));
#7068=EDGE_LOOP('',(#30299,#30300,#30301));
#7069=EDGE_LOOP('',(#30302,#30303,#30304,#30305,#30306,#30307));
#7070=EDGE_LOOP('',(#30308,#30309,#30310,#30311));
#7071=EDGE_LOOP('',(#30312,#30313,#30314,#30315));
#7072=EDGE_LOOP('',(#30316,#30317,#30318,#30319,#30320,#30321));
#7073=EDGE_LOOP('',(#30322,#30323,#30324,#30325));
#7074=EDGE_LOOP('',(#30326,#30327,#30328));
#7075=EDGE_LOOP('',(#30329,#30330,#30331,#30332));
#7076=EDGE_LOOP('',(#30333,#30334,#30335,#30336));
#7077=EDGE_LOOP('',(#30337,#30338,#30339,#30340,#30341,#30342));
#7078=EDGE_LOOP('',(#30343,#30344,#30345,#30346));
#7079=EDGE_LOOP('',(#30347,#30348,#30349,#30350));
#7080=EDGE_LOOP('',(#30351,#30352,#30353,#30354));
#7081=EDGE_LOOP('',(#30355,#30356,#30357,#30358,#30359,#30360));
#7082=EDGE_LOOP('',(#30361,#30362,#30363,#30364));
#7083=EDGE_LOOP('',(#30365,#30366,#30367,#30368));
#7084=EDGE_LOOP('',(#30369,#30370,#30371,#30372));
#7085=EDGE_LOOP('',(#30373,#30374,#30375,#30376,#30377,#30378));
#7086=EDGE_LOOP('',(#30379,#30380,#30381,#30382));
#7087=EDGE_LOOP('',(#30383,#30384,#30385,#30386));
#7088=EDGE_LOOP('',(#30387,#30388,#30389,#30390));
#7089=EDGE_LOOP('',(#30391,#30392,#30393,#30394,#30395,#30396));
#7090=EDGE_LOOP('',(#30397,#30398,#30399,#30400));
#7091=EDGE_LOOP('',(#30401,#30402,#30403,#30404));
#7092=EDGE_LOOP('',(#30405,#30406,#30407,#30408));
#7093=EDGE_LOOP('',(#30409,#30410,#30411,#30412,#30413,#30414));
#7094=EDGE_LOOP('',(#30415,#30416,#30417,#30418));
#7095=EDGE_LOOP('',(#30419,#30420,#30421,#30422));
#7096=EDGE_LOOP('',(#30423,#30424,#30425,#30426));
#7097=EDGE_LOOP('',(#30427,#30428,#30429));
#7098=EDGE_LOOP('',(#30430,#30431,#30432,#30433,#30434,#30435));
#7099=EDGE_LOOP('',(#30436,#30437,#30438,#30439));
#7100=EDGE_LOOP('',(#30440,#30441,#30442,#30443));
#7101=EDGE_LOOP('',(#30444,#30445,#30446,#30447,#30448,#30449));
#7102=EDGE_LOOP('',(#30450,#30451,#30452,#30453));
#7103=EDGE_LOOP('',(#30454,#30455,#30456));
#7104=EDGE_LOOP('',(#30457,#30458,#30459,#30460));
#7105=EDGE_LOOP('',(#30461,#30462,#30463,#30464));
#7106=EDGE_LOOP('',(#30465,#30466,#30467,#30468,#30469,#30470));
#7107=EDGE_LOOP('',(#30471,#30472,#30473,#30474));
#7108=EDGE_LOOP('',(#30475,#30476,#30477,#30478));
#7109=EDGE_LOOP('',(#30479,#30480,#30481,#30482));
#7110=EDGE_LOOP('',(#30483,#30484,#30485,#30486,#30487,#30488));
#7111=EDGE_LOOP('',(#30489,#30490,#30491,#30492));
#7112=EDGE_LOOP('',(#30493,#30494,#30495,#30496));
#7113=EDGE_LOOP('',(#30497,#30498,#30499,#30500));
#7114=EDGE_LOOP('',(#30501,#30502,#30503,#30504,#30505,#30506));
#7115=EDGE_LOOP('',(#30507,#30508,#30509,#30510));
#7116=EDGE_LOOP('',(#30511,#30512,#30513,#30514));
#7117=EDGE_LOOP('',(#30515,#30516,#30517,#30518));
#7118=EDGE_LOOP('',(#30519,#30520,#30521,#30522,#30523,#30524));
#7119=EDGE_LOOP('',(#30525,#30526,#30527,#30528));
#7120=EDGE_LOOP('',(#30529,#30530,#30531,#30532));
#7121=EDGE_LOOP('',(#30533,#30534,#30535,#30536));
#7122=EDGE_LOOP('',(#30537,#30538,#30539,#30540,#30541,#30542));
#7123=EDGE_LOOP('',(#30543,#30544,#30545,#30546));
#7124=EDGE_LOOP('',(#30547,#30548,#30549,#30550));
#7125=EDGE_LOOP('',(#30551,#30552,#30553,#30554));
#7126=EDGE_LOOP('',(#30555,#30556,#30557));
#7127=EDGE_LOOP('',(#30558,#30559,#30560,#30561,#30562,#30563));
#7128=EDGE_LOOP('',(#30564,#30565,#30566,#30567));
#7129=EDGE_LOOP('',(#30568,#30569,#30570,#30571));
#7130=EDGE_LOOP('',(#30572,#30573,#30574,#30575,#30576,#30577));
#7131=EDGE_LOOP('',(#30578,#30579,#30580,#30581));
#7132=EDGE_LOOP('',(#30582,#30583,#30584));
#7133=EDGE_LOOP('',(#30585,#30586,#30587,#30588));
#7134=EDGE_LOOP('',(#30589,#30590,#30591,#30592));
#7135=EDGE_LOOP('',(#30593,#30594,#30595,#30596,#30597,#30598));
#7136=EDGE_LOOP('',(#30599,#30600,#30601,#30602));
#7137=EDGE_LOOP('',(#30603,#30604,#30605,#30606));
#7138=EDGE_LOOP('',(#30607,#30608,#30609,#30610));
#7139=EDGE_LOOP('',(#30611,#30612,#30613,#30614,#30615,#30616));
#7140=EDGE_LOOP('',(#30617,#30618,#30619,#30620));
#7141=EDGE_LOOP('',(#30621,#30622,#30623,#30624));
#7142=EDGE_LOOP('',(#30625,#30626,#30627,#30628));
#7143=EDGE_LOOP('',(#30629,#30630,#30631,#30632,#30633,#30634));
#7144=EDGE_LOOP('',(#30635,#30636,#30637,#30638));
#7145=EDGE_LOOP('',(#30639,#30640,#30641,#30642));
#7146=EDGE_LOOP('',(#30643,#30644,#30645,#30646));
#7147=EDGE_LOOP('',(#30647,#30648,#30649,#30650,#30651,#30652));
#7148=EDGE_LOOP('',(#30653,#30654,#30655,#30656));
#7149=EDGE_LOOP('',(#30657,#30658,#30659,#30660));
#7150=EDGE_LOOP('',(#30661,#30662,#30663,#30664));
#7151=EDGE_LOOP('',(#30665,#30666,#30667,#30668,#30669,#30670));
#7152=EDGE_LOOP('',(#30671,#30672,#30673,#30674));
#7153=EDGE_LOOP('',(#30675,#30676,#30677,#30678));
#7154=EDGE_LOOP('',(#30679,#30680,#30681,#30682));
#7155=EDGE_LOOP('',(#30683,#30684,#30685));
#7156=EDGE_LOOP('',(#30686,#30687,#30688,#30689,#30690,#30691));
#7157=EDGE_LOOP('',(#30692,#30693,#30694,#30695));
#7158=EDGE_LOOP('',(#30696,#30697,#30698,#30699));
#7159=EDGE_LOOP('',(#30700,#30701,#30702,#30703,#30704,#30705));
#7160=EDGE_LOOP('',(#30706,#30707,#30708,#30709));
#7161=EDGE_LOOP('',(#30710,#30711,#30712));
#7162=EDGE_LOOP('',(#30713,#30714,#30715,#30716));
#7163=EDGE_LOOP('',(#30717,#30718,#30719,#30720));
#7164=EDGE_LOOP('',(#30721,#30722,#30723,#30724,#30725,#30726));
#7165=EDGE_LOOP('',(#30727,#30728,#30729,#30730));
#7166=EDGE_LOOP('',(#30731,#30732,#30733,#30734));
#7167=EDGE_LOOP('',(#30735,#30736,#30737,#30738));
#7168=EDGE_LOOP('',(#30739,#30740,#30741,#30742,#30743,#30744));
#7169=EDGE_LOOP('',(#30745,#30746,#30747,#30748));
#7170=EDGE_LOOP('',(#30749,#30750,#30751,#30752));
#7171=EDGE_LOOP('',(#30753,#30754,#30755,#30756));
#7172=EDGE_LOOP('',(#30757,#30758,#30759,#30760,#30761,#30762));
#7173=EDGE_LOOP('',(#30763,#30764,#30765,#30766));
#7174=EDGE_LOOP('',(#30767,#30768,#30769,#30770));
#7175=EDGE_LOOP('',(#30771,#30772,#30773,#30774));
#7176=EDGE_LOOP('',(#30775,#30776,#30777,#30778,#30779,#30780));
#7177=EDGE_LOOP('',(#30781,#30782,#30783,#30784));
#7178=EDGE_LOOP('',(#30785,#30786,#30787,#30788));
#7179=EDGE_LOOP('',(#30789,#30790,#30791,#30792));
#7180=EDGE_LOOP('',(#30793,#30794,#30795,#30796,#30797,#30798));
#7181=EDGE_LOOP('',(#30799,#30800,#30801,#30802));
#7182=EDGE_LOOP('',(#30803,#30804,#30805,#30806));
#7183=EDGE_LOOP('',(#30807,#30808,#30809,#30810));
#7184=EDGE_LOOP('',(#30811,#30812,#30813));
#7185=EDGE_LOOP('',(#30814,#30815,#30816,#30817,#30818,#30819));
#7186=EDGE_LOOP('',(#30820,#30821,#30822,#30823));
#7187=EDGE_LOOP('',(#30824,#30825,#30826,#30827));
#7188=EDGE_LOOP('',(#30828,#30829,#30830,#30831,#30832,#30833));
#7189=EDGE_LOOP('',(#30834,#30835,#30836,#30837));
#7190=EDGE_LOOP('',(#30838,#30839,#30840));
#7191=EDGE_LOOP('',(#30841,#30842,#30843,#30844));
#7192=EDGE_LOOP('',(#30845,#30846,#30847,#30848));
#7193=EDGE_LOOP('',(#30849,#30850,#30851,#30852,#30853,#30854));
#7194=EDGE_LOOP('',(#30855,#30856,#30857,#30858));
#7195=EDGE_LOOP('',(#30859,#30860,#30861,#30862));
#7196=EDGE_LOOP('',(#30863,#30864,#30865,#30866));
#7197=EDGE_LOOP('',(#30867,#30868,#30869,#30870,#30871,#30872));
#7198=EDGE_LOOP('',(#30873,#30874,#30875,#30876));
#7199=EDGE_LOOP('',(#30877,#30878,#30879,#30880));
#7200=EDGE_LOOP('',(#30881,#30882,#30883,#30884));
#7201=EDGE_LOOP('',(#30885,#30886,#30887,#30888,#30889,#30890));
#7202=EDGE_LOOP('',(#30891,#30892,#30893,#30894));
#7203=EDGE_LOOP('',(#30895,#30896,#30897,#30898));
#7204=EDGE_LOOP('',(#30899,#30900,#30901,#30902));
#7205=EDGE_LOOP('',(#30903,#30904,#30905,#30906,#30907,#30908));
#7206=EDGE_LOOP('',(#30909,#30910,#30911,#30912));
#7207=EDGE_LOOP('',(#30913,#30914,#30915,#30916));
#7208=EDGE_LOOP('',(#30917,#30918,#30919,#30920));
#7209=EDGE_LOOP('',(#30921,#30922,#30923,#30924,#30925,#30926));
#7210=EDGE_LOOP('',(#30927,#30928,#30929,#30930));
#7211=EDGE_LOOP('',(#30931,#30932,#30933,#30934));
#7212=EDGE_LOOP('',(#30935,#30936,#30937,#30938));
#7213=EDGE_LOOP('',(#30939,#30940,#30941));
#7214=EDGE_LOOP('',(#30942,#30943,#30944,#30945,#30946,#30947));
#7215=EDGE_LOOP('',(#30948,#30949,#30950,#30951));
#7216=EDGE_LOOP('',(#30952,#30953,#30954,#30955));
#7217=EDGE_LOOP('',(#30956,#30957,#30958,#30959,#30960,#30961));
#7218=EDGE_LOOP('',(#30962,#30963,#30964,#30965));
#7219=EDGE_LOOP('',(#30966,#30967,#30968));
#7220=EDGE_LOOP('',(#30969,#30970,#30971,#30972));
#7221=EDGE_LOOP('',(#30973,#30974,#30975,#30976));
#7222=EDGE_LOOP('',(#30977,#30978,#30979,#30980,#30981,#30982));
#7223=EDGE_LOOP('',(#30983,#30984,#30985,#30986));
#7224=EDGE_LOOP('',(#30987,#30988,#30989,#30990));
#7225=EDGE_LOOP('',(#30991,#30992,#30993,#30994));
#7226=EDGE_LOOP('',(#30995,#30996,#30997,#30998,#30999,#31000));
#7227=EDGE_LOOP('',(#31001,#31002,#31003,#31004));
#7228=EDGE_LOOP('',(#31005,#31006,#31007,#31008));
#7229=EDGE_LOOP('',(#31009,#31010,#31011,#31012));
#7230=EDGE_LOOP('',(#31013,#31014,#31015,#31016,#31017,#31018));
#7231=EDGE_LOOP('',(#31019,#31020,#31021,#31022));
#7232=EDGE_LOOP('',(#31023,#31024,#31025,#31026));
#7233=EDGE_LOOP('',(#31027,#31028,#31029,#31030));
#7234=EDGE_LOOP('',(#31031,#31032,#31033,#31034,#31035,#31036));
#7235=EDGE_LOOP('',(#31037,#31038,#31039,#31040));
#7236=EDGE_LOOP('',(#31041,#31042,#31043,#31044));
#7237=EDGE_LOOP('',(#31045,#31046,#31047,#31048));
#7238=EDGE_LOOP('',(#31049,#31050,#31051,#31052,#31053,#31054));
#7239=EDGE_LOOP('',(#31055,#31056,#31057,#31058));
#7240=EDGE_LOOP('',(#31059,#31060,#31061,#31062));
#7241=EDGE_LOOP('',(#31063,#31064,#31065,#31066));
#7242=EDGE_LOOP('',(#31067,#31068,#31069));
#7243=EDGE_LOOP('',(#31070,#31071,#31072,#31073,#31074,#31075));
#7244=EDGE_LOOP('',(#31076,#31077,#31078,#31079));
#7245=EDGE_LOOP('',(#31080,#31081,#31082,#31083));
#7246=EDGE_LOOP('',(#31084,#31085,#31086,#31087,#31088,#31089));
#7247=EDGE_LOOP('',(#31090,#31091,#31092,#31093));
#7248=EDGE_LOOP('',(#31094,#31095,#31096));
#7249=EDGE_LOOP('',(#31097,#31098,#31099,#31100));
#7250=EDGE_LOOP('',(#31101,#31102,#31103,#31104));
#7251=EDGE_LOOP('',(#31105,#31106,#31107,#31108,#31109,#31110));
#7252=EDGE_LOOP('',(#31111,#31112,#31113,#31114));
#7253=EDGE_LOOP('',(#31115,#31116,#31117,#31118));
#7254=EDGE_LOOP('',(#31119,#31120,#31121,#31122));
#7255=EDGE_LOOP('',(#31123,#31124,#31125,#31126,#31127,#31128));
#7256=EDGE_LOOP('',(#31129,#31130,#31131,#31132));
#7257=EDGE_LOOP('',(#31133,#31134,#31135,#31136));
#7258=EDGE_LOOP('',(#31137,#31138,#31139,#31140));
#7259=EDGE_LOOP('',(#31141,#31142,#31143,#31144,#31145,#31146));
#7260=EDGE_LOOP('',(#31147,#31148,#31149,#31150));
#7261=EDGE_LOOP('',(#31151,#31152,#31153,#31154));
#7262=EDGE_LOOP('',(#31155,#31156,#31157,#31158));
#7263=EDGE_LOOP('',(#31159,#31160,#31161,#31162,#31163,#31164));
#7264=EDGE_LOOP('',(#31165,#31166,#31167,#31168));
#7265=EDGE_LOOP('',(#31169,#31170,#31171,#31172));
#7266=EDGE_LOOP('',(#31173,#31174,#31175,#31176));
#7267=EDGE_LOOP('',(#31177,#31178,#31179,#31180,#31181,#31182));
#7268=EDGE_LOOP('',(#31183,#31184,#31185,#31186));
#7269=EDGE_LOOP('',(#31187,#31188,#31189,#31190));
#7270=EDGE_LOOP('',(#31191,#31192,#31193,#31194));
#7271=EDGE_LOOP('',(#31195,#31196,#31197));
#7272=EDGE_LOOP('',(#31198,#31199,#31200,#31201,#31202,#31203));
#7273=EDGE_LOOP('',(#31204,#31205,#31206,#31207));
#7274=EDGE_LOOP('',(#31208,#31209,#31210,#31211));
#7275=EDGE_LOOP('',(#31212,#31213,#31214,#31215,#31216,#31217));
#7276=EDGE_LOOP('',(#31218,#31219,#31220,#31221));
#7277=EDGE_LOOP('',(#31222,#31223,#31224));
#7278=EDGE_LOOP('',(#31225,#31226,#31227,#31228));
#7279=EDGE_LOOP('',(#31229,#31230,#31231,#31232));
#7280=EDGE_LOOP('',(#31233,#31234,#31235,#31236,#31237,#31238));
#7281=EDGE_LOOP('',(#31239,#31240,#31241,#31242));
#7282=EDGE_LOOP('',(#31243,#31244,#31245,#31246));
#7283=EDGE_LOOP('',(#31247,#31248,#31249,#31250));
#7284=EDGE_LOOP('',(#31251,#31252,#31253,#31254,#31255,#31256));
#7285=EDGE_LOOP('',(#31257,#31258,#31259,#31260));
#7286=EDGE_LOOP('',(#31261,#31262,#31263,#31264));
#7287=EDGE_LOOP('',(#31265,#31266,#31267,#31268));
#7288=EDGE_LOOP('',(#31269,#31270,#31271,#31272,#31273,#31274));
#7289=EDGE_LOOP('',(#31275,#31276,#31277,#31278));
#7290=EDGE_LOOP('',(#31279,#31280,#31281,#31282));
#7291=EDGE_LOOP('',(#31283,#31284,#31285,#31286));
#7292=EDGE_LOOP('',(#31287,#31288,#31289,#31290,#31291,#31292));
#7293=EDGE_LOOP('',(#31293,#31294,#31295,#31296));
#7294=EDGE_LOOP('',(#31297,#31298,#31299,#31300));
#7295=EDGE_LOOP('',(#31301,#31302,#31303,#31304));
#7296=EDGE_LOOP('',(#31305,#31306,#31307,#31308,#31309,#31310));
#7297=EDGE_LOOP('',(#31311,#31312,#31313,#31314));
#7298=EDGE_LOOP('',(#31315,#31316,#31317,#31318));
#7299=EDGE_LOOP('',(#31319,#31320,#31321,#31322));
#7300=EDGE_LOOP('',(#31323,#31324,#31325));
#7301=EDGE_LOOP('',(#31326,#31327,#31328,#31329,#31330,#31331));
#7302=EDGE_LOOP('',(#31332,#31333,#31334,#31335));
#7303=EDGE_LOOP('',(#31336,#31337,#31338,#31339));
#7304=EDGE_LOOP('',(#31340,#31341,#31342,#31343,#31344,#31345));
#7305=EDGE_LOOP('',(#31346,#31347,#31348,#31349));
#7306=EDGE_LOOP('',(#31350,#31351,#31352));
#7307=EDGE_LOOP('',(#31353,#31354,#31355,#31356));
#7308=EDGE_LOOP('',(#31357,#31358,#31359,#31360));
#7309=EDGE_LOOP('',(#31361,#31362,#31363,#31364,#31365,#31366));
#7310=EDGE_LOOP('',(#31367,#31368,#31369,#31370));
#7311=EDGE_LOOP('',(#31371,#31372,#31373,#31374));
#7312=EDGE_LOOP('',(#31375,#31376,#31377,#31378));
#7313=EDGE_LOOP('',(#31379,#31380,#31381,#31382,#31383,#31384));
#7314=EDGE_LOOP('',(#31385,#31386,#31387,#31388));
#7315=EDGE_LOOP('',(#31389,#31390,#31391,#31392));
#7316=EDGE_LOOP('',(#31393,#31394,#31395,#31396));
#7317=EDGE_LOOP('',(#31397,#31398,#31399,#31400,#31401,#31402));
#7318=EDGE_LOOP('',(#31403,#31404,#31405,#31406));
#7319=EDGE_LOOP('',(#31407,#31408,#31409,#31410));
#7320=EDGE_LOOP('',(#31411,#31412,#31413,#31414));
#7321=EDGE_LOOP('',(#31415,#31416,#31417,#31418,#31419,#31420));
#7322=EDGE_LOOP('',(#31421,#31422,#31423,#31424));
#7323=EDGE_LOOP('',(#31425,#31426,#31427,#31428));
#7324=EDGE_LOOP('',(#31429,#31430,#31431,#31432));
#7325=EDGE_LOOP('',(#31433,#31434,#31435,#31436,#31437,#31438));
#7326=EDGE_LOOP('',(#31439,#31440,#31441,#31442));
#7327=EDGE_LOOP('',(#31443,#31444,#31445,#31446));
#7328=EDGE_LOOP('',(#31447,#31448,#31449,#31450));
#7329=EDGE_LOOP('',(#31451,#31452,#31453));
#7330=EDGE_LOOP('',(#31454,#31455,#31456,#31457,#31458,#31459));
#7331=EDGE_LOOP('',(#31460,#31461,#31462,#31463));
#7332=EDGE_LOOP('',(#31464,#31465,#31466,#31467));
#7333=EDGE_LOOP('',(#31468,#31469,#31470,#31471,#31472,#31473));
#7334=EDGE_LOOP('',(#31474,#31475,#31476,#31477));
#7335=EDGE_LOOP('',(#31478,#31479,#31480));
#7336=EDGE_LOOP('',(#31481,#31482,#31483,#31484));
#7337=EDGE_LOOP('',(#31485,#31486,#31487,#31488));
#7338=EDGE_LOOP('',(#31489,#31490,#31491,#31492,#31493,#31494));
#7339=EDGE_LOOP('',(#31495,#31496,#31497,#31498));
#7340=EDGE_LOOP('',(#31499,#31500,#31501,#31502));
#7341=EDGE_LOOP('',(#31503,#31504,#31505,#31506));
#7342=EDGE_LOOP('',(#31507,#31508,#31509,#31510,#31511,#31512));
#7343=EDGE_LOOP('',(#31513,#31514,#31515,#31516));
#7344=EDGE_LOOP('',(#31517,#31518,#31519,#31520));
#7345=EDGE_LOOP('',(#31521,#31522,#31523,#31524));
#7346=EDGE_LOOP('',(#31525,#31526,#31527,#31528,#31529,#31530));
#7347=EDGE_LOOP('',(#31531,#31532,#31533,#31534));
#7348=EDGE_LOOP('',(#31535,#31536,#31537,#31538));
#7349=EDGE_LOOP('',(#31539,#31540,#31541,#31542));
#7350=EDGE_LOOP('',(#31543,#31544,#31545,#31546,#31547,#31548));
#7351=EDGE_LOOP('',(#31549,#31550,#31551,#31552));
#7352=EDGE_LOOP('',(#31553,#31554,#31555,#31556));
#7353=EDGE_LOOP('',(#31557,#31558,#31559,#31560));
#7354=EDGE_LOOP('',(#31561,#31562,#31563,#31564,#31565,#31566));
#7355=EDGE_LOOP('',(#31567,#31568,#31569,#31570));
#7356=EDGE_LOOP('',(#31571,#31572,#31573,#31574));
#7357=EDGE_LOOP('',(#31575,#31576,#31577,#31578));
#7358=EDGE_LOOP('',(#31579,#31580,#31581));
#7359=EDGE_LOOP('',(#31582,#31583,#31584,#31585,#31586,#31587));
#7360=EDGE_LOOP('',(#31588,#31589,#31590,#31591));
#7361=EDGE_LOOP('',(#31592,#31593,#31594,#31595));
#7362=EDGE_LOOP('',(#31596,#31597,#31598,#31599,#31600,#31601));
#7363=EDGE_LOOP('',(#31602,#31603,#31604,#31605));
#7364=EDGE_LOOP('',(#31606,#31607,#31608));
#7365=EDGE_LOOP('',(#31609,#31610,#31611,#31612));
#7366=EDGE_LOOP('',(#31613,#31614,#31615,#31616));
#7367=EDGE_LOOP('',(#31617,#31618,#31619,#31620,#31621,#31622));
#7368=EDGE_LOOP('',(#31623,#31624,#31625,#31626));
#7369=EDGE_LOOP('',(#31627,#31628,#31629,#31630));
#7370=EDGE_LOOP('',(#31631,#31632,#31633,#31634));
#7371=EDGE_LOOP('',(#31635,#31636,#31637,#31638,#31639,#31640));
#7372=EDGE_LOOP('',(#31641,#31642,#31643,#31644));
#7373=EDGE_LOOP('',(#31645,#31646,#31647,#31648));
#7374=EDGE_LOOP('',(#31649,#31650,#31651,#31652));
#7375=EDGE_LOOP('',(#31653,#31654,#31655,#31656,#31657,#31658));
#7376=EDGE_LOOP('',(#31659,#31660,#31661,#31662));
#7377=EDGE_LOOP('',(#31663,#31664,#31665,#31666));
#7378=EDGE_LOOP('',(#31667,#31668,#31669,#31670));
#7379=EDGE_LOOP('',(#31671,#31672,#31673,#31674,#31675,#31676));
#7380=EDGE_LOOP('',(#31677,#31678,#31679,#31680));
#7381=EDGE_LOOP('',(#31681,#31682,#31683,#31684));
#7382=EDGE_LOOP('',(#31685,#31686,#31687,#31688));
#7383=EDGE_LOOP('',(#31689,#31690,#31691,#31692,#31693,#31694));
#7384=EDGE_LOOP('',(#31695,#31696,#31697,#31698));
#7385=EDGE_LOOP('',(#31699,#31700,#31701,#31702));
#7386=EDGE_LOOP('',(#31703,#31704,#31705,#31706));
#7387=EDGE_LOOP('',(#31707,#31708,#31709));
#7388=EDGE_LOOP('',(#31710,#31711,#31712,#31713,#31714,#31715));
#7389=EDGE_LOOP('',(#31716,#31717,#31718,#31719));
#7390=EDGE_LOOP('',(#31720,#31721,#31722,#31723));
#7391=EDGE_LOOP('',(#31724,#31725,#31726,#31727,#31728,#31729));
#7392=EDGE_LOOP('',(#31730,#31731,#31732,#31733));
#7393=EDGE_LOOP('',(#31734,#31735,#31736));
#7394=EDGE_LOOP('',(#31737,#31738,#31739,#31740));
#7395=EDGE_LOOP('',(#31741,#31742,#31743,#31744));
#7396=EDGE_LOOP('',(#31745,#31746,#31747,#31748,#31749,#31750));
#7397=EDGE_LOOP('',(#31751,#31752,#31753,#31754));
#7398=EDGE_LOOP('',(#31755,#31756,#31757,#31758));
#7399=EDGE_LOOP('',(#31759,#31760,#31761,#31762));
#7400=EDGE_LOOP('',(#31763,#31764,#31765,#31766,#31767,#31768));
#7401=EDGE_LOOP('',(#31769,#31770,#31771,#31772));
#7402=EDGE_LOOP('',(#31773,#31774,#31775,#31776));
#7403=EDGE_LOOP('',(#31777,#31778,#31779,#31780));
#7404=EDGE_LOOP('',(#31781,#31782,#31783,#31784,#31785,#31786));
#7405=EDGE_LOOP('',(#31787,#31788,#31789,#31790));
#7406=EDGE_LOOP('',(#31791,#31792,#31793,#31794));
#7407=EDGE_LOOP('',(#31795,#31796,#31797,#31798));
#7408=EDGE_LOOP('',(#31799,#31800,#31801,#31802,#31803,#31804));
#7409=EDGE_LOOP('',(#31805,#31806,#31807,#31808));
#7410=EDGE_LOOP('',(#31809,#31810,#31811,#31812));
#7411=EDGE_LOOP('',(#31813,#31814,#31815,#31816));
#7412=EDGE_LOOP('',(#31817,#31818,#31819,#31820,#31821,#31822));
#7413=EDGE_LOOP('',(#31823,#31824,#31825,#31826));
#7414=EDGE_LOOP('',(#31827,#31828,#31829,#31830));
#7415=EDGE_LOOP('',(#31831,#31832,#31833,#31834));
#7416=EDGE_LOOP('',(#31835,#31836,#31837));
#7417=EDGE_LOOP('',(#31838,#31839,#31840,#31841,#31842,#31843));
#7418=EDGE_LOOP('',(#31844,#31845,#31846,#31847));
#7419=EDGE_LOOP('',(#31848,#31849,#31850,#31851));
#7420=EDGE_LOOP('',(#31852,#31853,#31854,#31855,#31856,#31857));
#7421=EDGE_LOOP('',(#31858,#31859,#31860,#31861));
#7422=EDGE_LOOP('',(#31862,#31863,#31864));
#7423=EDGE_LOOP('',(#31865,#31866,#31867,#31868));
#7424=EDGE_LOOP('',(#31869,#31870,#31871,#31872));
#7425=EDGE_LOOP('',(#31873,#31874,#31875,#31876,#31877,#31878));
#7426=EDGE_LOOP('',(#31879,#31880,#31881,#31882));
#7427=EDGE_LOOP('',(#31883,#31884,#31885,#31886));
#7428=EDGE_LOOP('',(#31887,#31888,#31889,#31890));
#7429=EDGE_LOOP('',(#31891,#31892,#31893,#31894,#31895,#31896));
#7430=EDGE_LOOP('',(#31897,#31898,#31899,#31900));
#7431=EDGE_LOOP('',(#31901,#31902,#31903,#31904));
#7432=EDGE_LOOP('',(#31905,#31906,#31907,#31908));
#7433=EDGE_LOOP('',(#31909,#31910,#31911,#31912,#31913,#31914));
#7434=EDGE_LOOP('',(#31915,#31916,#31917,#31918));
#7435=EDGE_LOOP('',(#31919,#31920,#31921,#31922));
#7436=EDGE_LOOP('',(#31923,#31924,#31925,#31926));
#7437=EDGE_LOOP('',(#31927,#31928,#31929,#31930,#31931,#31932));
#7438=EDGE_LOOP('',(#31933,#31934,#31935,#31936));
#7439=EDGE_LOOP('',(#31937,#31938,#31939,#31940));
#7440=EDGE_LOOP('',(#31941,#31942,#31943,#31944));
#7441=EDGE_LOOP('',(#31945,#31946,#31947,#31948,#31949,#31950));
#7442=EDGE_LOOP('',(#31951,#31952,#31953,#31954));
#7443=EDGE_LOOP('',(#31955,#31956,#31957,#31958));
#7444=EDGE_LOOP('',(#31959,#31960,#31961,#31962));
#7445=EDGE_LOOP('',(#31963,#31964,#31965));
#7446=EDGE_LOOP('',(#31966,#31967,#31968,#31969,#31970,#31971));
#7447=EDGE_LOOP('',(#31972,#31973,#31974,#31975));
#7448=EDGE_LOOP('',(#31976,#31977,#31978,#31979));
#7449=EDGE_LOOP('',(#31980,#31981,#31982,#31983,#31984,#31985));
#7450=EDGE_LOOP('',(#31986,#31987,#31988,#31989));
#7451=EDGE_LOOP('',(#31990,#31991,#31992));
#7452=EDGE_LOOP('',(#31993,#31994,#31995,#31996));
#7453=EDGE_LOOP('',(#31997,#31998,#31999,#32000));
#7454=EDGE_LOOP('',(#32001,#32002,#32003,#32004,#32005,#32006));
#7455=EDGE_LOOP('',(#32007,#32008,#32009,#32010));
#7456=EDGE_LOOP('',(#32011,#32012,#32013,#32014));
#7457=EDGE_LOOP('',(#32015,#32016,#32017,#32018));
#7458=EDGE_LOOP('',(#32019,#32020,#32021,#32022,#32023,#32024));
#7459=EDGE_LOOP('',(#32025,#32026,#32027,#32028));
#7460=EDGE_LOOP('',(#32029,#32030,#32031,#32032));
#7461=EDGE_LOOP('',(#32033,#32034,#32035,#32036));
#7462=EDGE_LOOP('',(#32037,#32038,#32039,#32040,#32041,#32042));
#7463=EDGE_LOOP('',(#32043,#32044,#32045,#32046));
#7464=EDGE_LOOP('',(#32047,#32048,#32049,#32050));
#7465=EDGE_LOOP('',(#32051,#32052,#32053,#32054));
#7466=EDGE_LOOP('',(#32055,#32056,#32057,#32058,#32059,#32060));
#7467=EDGE_LOOP('',(#32061,#32062,#32063,#32064));
#7468=EDGE_LOOP('',(#32065,#32066,#32067,#32068));
#7469=EDGE_LOOP('',(#32069,#32070,#32071,#32072));
#7470=EDGE_LOOP('',(#32073,#32074,#32075,#32076,#32077,#32078));
#7471=EDGE_LOOP('',(#32079,#32080,#32081,#32082));
#7472=EDGE_LOOP('',(#32083,#32084,#32085,#32086));
#7473=EDGE_LOOP('',(#32087,#32088,#32089,#32090));
#7474=EDGE_LOOP('',(#32091,#32092,#32093));
#7475=EDGE_LOOP('',(#32094,#32095,#32096,#32097,#32098,#32099));
#7476=EDGE_LOOP('',(#32100,#32101,#32102,#32103));
#7477=EDGE_LOOP('',(#32104,#32105,#32106,#32107));
#7478=EDGE_LOOP('',(#32108,#32109,#32110,#32111,#32112,#32113));
#7479=EDGE_LOOP('',(#32114,#32115,#32116,#32117));
#7480=EDGE_LOOP('',(#32118,#32119,#32120));
#7481=EDGE_LOOP('',(#32121,#32122,#32123,#32124));
#7482=EDGE_LOOP('',(#32125,#32126,#32127,#32128));
#7483=EDGE_LOOP('',(#32129,#32130,#32131,#32132,#32133,#32134));
#7484=EDGE_LOOP('',(#32135,#32136,#32137,#32138));
#7485=EDGE_LOOP('',(#32139,#32140,#32141,#32142));
#7486=EDGE_LOOP('',(#32143,#32144,#32145,#32146));
#7487=EDGE_LOOP('',(#32147,#32148,#32149,#32150,#32151,#32152));
#7488=EDGE_LOOP('',(#32153,#32154,#32155,#32156));
#7489=EDGE_LOOP('',(#32157,#32158,#32159,#32160));
#7490=EDGE_LOOP('',(#32161,#32162,#32163,#32164));
#7491=EDGE_LOOP('',(#32165,#32166,#32167,#32168,#32169,#32170));
#7492=EDGE_LOOP('',(#32171,#32172,#32173,#32174));
#7493=EDGE_LOOP('',(#32175,#32176,#32177,#32178));
#7494=EDGE_LOOP('',(#32179,#32180,#32181,#32182));
#7495=EDGE_LOOP('',(#32183,#32184,#32185,#32186,#32187,#32188));
#7496=EDGE_LOOP('',(#32189,#32190,#32191,#32192));
#7497=EDGE_LOOP('',(#32193,#32194,#32195,#32196));
#7498=EDGE_LOOP('',(#32197,#32198,#32199,#32200));
#7499=EDGE_LOOP('',(#32201,#32202,#32203,#32204,#32205,#32206));
#7500=EDGE_LOOP('',(#32207,#32208,#32209,#32210));
#7501=EDGE_LOOP('',(#32211,#32212,#32213,#32214));
#7502=EDGE_LOOP('',(#32215,#32216,#32217,#32218));
#7503=EDGE_LOOP('',(#32219,#32220,#32221));
#7504=EDGE_LOOP('',(#32222,#32223,#32224,#32225,#32226,#32227));
#7505=EDGE_LOOP('',(#32228,#32229,#32230,#32231));
#7506=EDGE_LOOP('',(#32232,#32233,#32234,#32235));
#7507=EDGE_LOOP('',(#32236,#32237,#32238,#32239,#32240,#32241));
#7508=EDGE_LOOP('',(#32242,#32243,#32244,#32245));
#7509=EDGE_LOOP('',(#32246,#32247,#32248));
#7510=EDGE_LOOP('',(#32249,#32250,#32251,#32252));
#7511=EDGE_LOOP('',(#32253,#32254,#32255,#32256));
#7512=EDGE_LOOP('',(#32257,#32258,#32259,#32260,#32261,#32262));
#7513=EDGE_LOOP('',(#32263,#32264,#32265,#32266));
#7514=EDGE_LOOP('',(#32267,#32268,#32269,#32270));
#7515=EDGE_LOOP('',(#32271,#32272,#32273,#32274));
#7516=EDGE_LOOP('',(#32275,#32276,#32277,#32278,#32279,#32280));
#7517=EDGE_LOOP('',(#32281,#32282,#32283,#32284));
#7518=EDGE_LOOP('',(#32285,#32286,#32287,#32288));
#7519=EDGE_LOOP('',(#32289,#32290,#32291,#32292));
#7520=EDGE_LOOP('',(#32293,#32294,#32295,#32296,#32297,#32298));
#7521=EDGE_LOOP('',(#32299,#32300,#32301,#32302));
#7522=EDGE_LOOP('',(#32303,#32304,#32305,#32306));
#7523=EDGE_LOOP('',(#32307,#32308,#32309,#32310));
#7524=EDGE_LOOP('',(#32311,#32312,#32313,#32314,#32315,#32316));
#7525=EDGE_LOOP('',(#32317,#32318,#32319,#32320));
#7526=EDGE_LOOP('',(#32321,#32322,#32323,#32324));
#7527=EDGE_LOOP('',(#32325,#32326,#32327,#32328));
#7528=EDGE_LOOP('',(#32329,#32330,#32331,#32332,#32333,#32334));
#7529=EDGE_LOOP('',(#32335,#32336,#32337,#32338));
#7530=EDGE_LOOP('',(#32339,#32340,#32341,#32342));
#7531=EDGE_LOOP('',(#32343,#32344,#32345,#32346));
#7532=EDGE_LOOP('',(#32347,#32348,#32349));
#7533=EDGE_LOOP('',(#32350,#32351,#32352,#32353,#32354,#32355));
#7534=EDGE_LOOP('',(#32356,#32357,#32358,#32359));
#7535=EDGE_LOOP('',(#32360,#32361,#32362,#32363));
#7536=EDGE_LOOP('',(#32364,#32365,#32366,#32367,#32368,#32369));
#7537=EDGE_LOOP('',(#32370,#32371,#32372,#32373));
#7538=EDGE_LOOP('',(#32374,#32375,#32376));
#7539=EDGE_LOOP('',(#32377,#32378,#32379,#32380));
#7540=EDGE_LOOP('',(#32381,#32382,#32383,#32384));
#7541=EDGE_LOOP('',(#32385,#32386,#32387,#32388,#32389,#32390));
#7542=EDGE_LOOP('',(#32391,#32392,#32393,#32394));
#7543=EDGE_LOOP('',(#32395,#32396,#32397,#32398));
#7544=EDGE_LOOP('',(#32399,#32400,#32401,#32402));
#7545=EDGE_LOOP('',(#32403,#32404,#32405,#32406,#32407,#32408));
#7546=EDGE_LOOP('',(#32409,#32410,#32411,#32412));
#7547=EDGE_LOOP('',(#32413,#32414,#32415,#32416));
#7548=EDGE_LOOP('',(#32417,#32418,#32419,#32420));
#7549=EDGE_LOOP('',(#32421,#32422,#32423,#32424,#32425,#32426));
#7550=EDGE_LOOP('',(#32427,#32428,#32429,#32430));
#7551=EDGE_LOOP('',(#32431,#32432,#32433,#32434));
#7552=EDGE_LOOP('',(#32435,#32436,#32437,#32438));
#7553=EDGE_LOOP('',(#32439,#32440,#32441,#32442,#32443,#32444));
#7554=EDGE_LOOP('',(#32445,#32446,#32447,#32448));
#7555=EDGE_LOOP('',(#32449,#32450,#32451,#32452));
#7556=EDGE_LOOP('',(#32453,#32454,#32455,#32456));
#7557=EDGE_LOOP('',(#32457,#32458,#32459,#32460,#32461,#32462));
#7558=EDGE_LOOP('',(#32463,#32464,#32465,#32466));
#7559=EDGE_LOOP('',(#32467,#32468,#32469,#32470));
#7560=EDGE_LOOP('',(#32471,#32472,#32473,#32474));
#7561=EDGE_LOOP('',(#32475,#32476,#32477));
#7562=EDGE_LOOP('',(#32478,#32479,#32480,#32481,#32482,#32483));
#7563=EDGE_LOOP('',(#32484,#32485,#32486,#32487));
#7564=EDGE_LOOP('',(#32488,#32489,#32490,#32491));
#7565=EDGE_LOOP('',(#32492,#32493,#32494,#32495,#32496,#32497));
#7566=EDGE_LOOP('',(#32498,#32499,#32500,#32501));
#7567=EDGE_LOOP('',(#32502,#32503,#32504));
#7568=EDGE_LOOP('',(#32505,#32506,#32507,#32508));
#7569=EDGE_LOOP('',(#32509,#32510,#32511,#32512));
#7570=EDGE_LOOP('',(#32513,#32514,#32515,#32516,#32517,#32518));
#7571=EDGE_LOOP('',(#32519,#32520,#32521,#32522));
#7572=EDGE_LOOP('',(#32523,#32524,#32525,#32526));
#7573=EDGE_LOOP('',(#32527,#32528,#32529,#32530));
#7574=EDGE_LOOP('',(#32531,#32532,#32533,#32534,#32535,#32536));
#7575=EDGE_LOOP('',(#32537,#32538,#32539,#32540));
#7576=EDGE_LOOP('',(#32541,#32542,#32543,#32544));
#7577=EDGE_LOOP('',(#32545,#32546,#32547,#32548));
#7578=EDGE_LOOP('',(#32549,#32550,#32551,#32552,#32553,#32554));
#7579=EDGE_LOOP('',(#32555,#32556,#32557,#32558));
#7580=EDGE_LOOP('',(#32559,#32560,#32561,#32562));
#7581=EDGE_LOOP('',(#32563,#32564,#32565,#32566));
#7582=EDGE_LOOP('',(#32567,#32568,#32569,#32570,#32571,#32572));
#7583=EDGE_LOOP('',(#32573,#32574,#32575,#32576));
#7584=EDGE_LOOP('',(#32577,#32578,#32579,#32580));
#7585=EDGE_LOOP('',(#32581,#32582,#32583,#32584));
#7586=EDGE_LOOP('',(#32585,#32586,#32587,#32588,#32589,#32590));
#7587=EDGE_LOOP('',(#32591,#32592,#32593,#32594));
#7588=EDGE_LOOP('',(#32595,#32596,#32597,#32598));
#7589=EDGE_LOOP('',(#32599,#32600,#32601,#32602));
#7590=EDGE_LOOP('',(#32603,#32604,#32605));
#7591=EDGE_LOOP('',(#32606,#32607,#32608,#32609,#32610,#32611));
#7592=EDGE_LOOP('',(#32612,#32613,#32614,#32615));
#7593=EDGE_LOOP('',(#32616,#32617,#32618,#32619));
#7594=EDGE_LOOP('',(#32620,#32621,#32622,#32623,#32624,#32625));
#7595=EDGE_LOOP('',(#32626,#32627,#32628,#32629));
#7596=EDGE_LOOP('',(#32630,#32631,#32632));
#7597=EDGE_LOOP('',(#32633,#32634,#32635,#32636));
#7598=EDGE_LOOP('',(#32637,#32638,#32639,#32640));
#7599=EDGE_LOOP('',(#32641,#32642,#32643,#32644,#32645,#32646));
#7600=EDGE_LOOP('',(#32647,#32648,#32649,#32650));
#7601=EDGE_LOOP('',(#32651,#32652,#32653,#32654));
#7602=EDGE_LOOP('',(#32655,#32656,#32657,#32658));
#7603=EDGE_LOOP('',(#32659,#32660,#32661,#32662,#32663,#32664));
#7604=EDGE_LOOP('',(#32665,#32666,#32667,#32668));
#7605=EDGE_LOOP('',(#32669,#32670,#32671,#32672));
#7606=EDGE_LOOP('',(#32673,#32674,#32675,#32676));
#7607=EDGE_LOOP('',(#32677,#32678,#32679,#32680,#32681,#32682));
#7608=EDGE_LOOP('',(#32683,#32684,#32685,#32686));
#7609=EDGE_LOOP('',(#32687,#32688,#32689,#32690));
#7610=EDGE_LOOP('',(#32691,#32692,#32693,#32694));
#7611=EDGE_LOOP('',(#32695,#32696,#32697,#32698,#32699,#32700));
#7612=EDGE_LOOP('',(#32701,#32702,#32703,#32704));
#7613=EDGE_LOOP('',(#32705,#32706,#32707,#32708));
#7614=EDGE_LOOP('',(#32709,#32710,#32711,#32712));
#7615=EDGE_LOOP('',(#32713,#32714,#32715,#32716,#32717,#32718));
#7616=EDGE_LOOP('',(#32719,#32720,#32721,#32722));
#7617=EDGE_LOOP('',(#32723,#32724,#32725,#32726));
#7618=EDGE_LOOP('',(#32727,#32728,#32729,#32730));
#7619=EDGE_LOOP('',(#32731,#32732,#32733));
#7620=EDGE_LOOP('',(#32734,#32735,#32736,#32737,#32738,#32739));
#7621=EDGE_LOOP('',(#32740,#32741,#32742,#32743));
#7622=EDGE_LOOP('',(#32744,#32745,#32746,#32747));
#7623=EDGE_LOOP('',(#32748,#32749,#32750,#32751,#32752,#32753));
#7624=EDGE_LOOP('',(#32754,#32755,#32756,#32757));
#7625=EDGE_LOOP('',(#32758,#32759,#32760));
#7626=EDGE_LOOP('',(#32761,#32762,#32763,#32764));
#7627=EDGE_LOOP('',(#32765,#32766,#32767,#32768));
#7628=EDGE_LOOP('',(#32769,#32770,#32771,#32772,#32773,#32774));
#7629=EDGE_LOOP('',(#32775,#32776,#32777,#32778));
#7630=EDGE_LOOP('',(#32779,#32780,#32781,#32782));
#7631=EDGE_LOOP('',(#32783,#32784,#32785,#32786));
#7632=EDGE_LOOP('',(#32787,#32788,#32789,#32790,#32791,#32792));
#7633=EDGE_LOOP('',(#32793,#32794,#32795,#32796));
#7634=EDGE_LOOP('',(#32797,#32798,#32799,#32800));
#7635=EDGE_LOOP('',(#32801,#32802,#32803,#32804));
#7636=EDGE_LOOP('',(#32805,#32806,#32807,#32808,#32809,#32810));
#7637=EDGE_LOOP('',(#32811,#32812,#32813,#32814));
#7638=EDGE_LOOP('',(#32815,#32816,#32817,#32818));
#7639=EDGE_LOOP('',(#32819,#32820,#32821,#32822));
#7640=EDGE_LOOP('',(#32823,#32824,#32825,#32826,#32827,#32828));
#7641=EDGE_LOOP('',(#32829,#32830,#32831,#32832));
#7642=EDGE_LOOP('',(#32833,#32834,#32835,#32836));
#7643=EDGE_LOOP('',(#32837,#32838,#32839,#32840));
#7644=EDGE_LOOP('',(#32841,#32842,#32843,#32844,#32845,#32846));
#7645=EDGE_LOOP('',(#32847,#32848,#32849,#32850));
#7646=EDGE_LOOP('',(#32851,#32852,#32853,#32854));
#7647=EDGE_LOOP('',(#32855,#32856,#32857,#32858));
#7648=EDGE_LOOP('',(#32859,#32860,#32861));
#7649=EDGE_LOOP('',(#32862,#32863,#32864,#32865,#32866,#32867));
#7650=EDGE_LOOP('',(#32868,#32869,#32870,#32871));
#7651=EDGE_LOOP('',(#32872,#32873,#32874,#32875));
#7652=EDGE_LOOP('',(#32876,#32877,#32878,#32879,#32880,#32881));
#7653=EDGE_LOOP('',(#32882,#32883,#32884,#32885));
#7654=EDGE_LOOP('',(#32886,#32887,#32888));
#7655=EDGE_LOOP('',(#32889,#32890,#32891,#32892));
#7656=EDGE_LOOP('',(#32893,#32894,#32895,#32896));
#7657=EDGE_LOOP('',(#32897,#32898,#32899,#32900,#32901,#32902));
#7658=EDGE_LOOP('',(#32903,#32904,#32905,#32906));
#7659=EDGE_LOOP('',(#32907,#32908,#32909,#32910));
#7660=EDGE_LOOP('',(#32911,#32912,#32913,#32914));
#7661=EDGE_LOOP('',(#32915,#32916,#32917,#32918,#32919,#32920));
#7662=EDGE_LOOP('',(#32921,#32922,#32923,#32924));
#7663=EDGE_LOOP('',(#32925,#32926,#32927,#32928));
#7664=EDGE_LOOP('',(#32929,#32930,#32931,#32932));
#7665=EDGE_LOOP('',(#32933,#32934,#32935,#32936,#32937,#32938));
#7666=EDGE_LOOP('',(#32939,#32940,#32941,#32942));
#7667=EDGE_LOOP('',(#32943,#32944,#32945,#32946));
#7668=EDGE_LOOP('',(#32947,#32948,#32949,#32950));
#7669=EDGE_LOOP('',(#32951,#32952,#32953,#32954,#32955,#32956));
#7670=EDGE_LOOP('',(#32957,#32958,#32959,#32960));
#7671=EDGE_LOOP('',(#32961,#32962,#32963,#32964));
#7672=EDGE_LOOP('',(#32965,#32966,#32967,#32968));
#7673=EDGE_LOOP('',(#32969,#32970,#32971,#32972,#32973,#32974));
#7674=EDGE_LOOP('',(#32975,#32976,#32977,#32978));
#7675=EDGE_LOOP('',(#32979,#32980,#32981,#32982));
#7676=EDGE_LOOP('',(#32983,#32984,#32985,#32986));
#7677=EDGE_LOOP('',(#32987,#32988,#32989));
#7678=EDGE_LOOP('',(#32990,#32991,#32992,#32993,#32994,#32995));
#7679=EDGE_LOOP('',(#32996,#32997,#32998,#32999));
#7680=EDGE_LOOP('',(#33000,#33001,#33002,#33003));
#7681=EDGE_LOOP('',(#33004,#33005,#33006,#33007,#33008,#33009));
#7682=EDGE_LOOP('',(#33010,#33011,#33012,#33013));
#7683=EDGE_LOOP('',(#33014,#33015,#33016));
#7684=EDGE_LOOP('',(#33017,#33018,#33019,#33020));
#7685=EDGE_LOOP('',(#33021,#33022,#33023,#33024));
#7686=EDGE_LOOP('',(#33025,#33026,#33027,#33028,#33029,#33030));
#7687=EDGE_LOOP('',(#33031,#33032,#33033,#33034));
#7688=EDGE_LOOP('',(#33035,#33036,#33037,#33038));
#7689=EDGE_LOOP('',(#33039,#33040,#33041,#33042));
#7690=EDGE_LOOP('',(#33043,#33044,#33045,#33046,#33047,#33048));
#7691=EDGE_LOOP('',(#33049,#33050,#33051,#33052));
#7692=EDGE_LOOP('',(#33053,#33054,#33055,#33056));
#7693=EDGE_LOOP('',(#33057,#33058,#33059,#33060));
#7694=EDGE_LOOP('',(#33061,#33062,#33063,#33064,#33065,#33066));
#7695=EDGE_LOOP('',(#33067,#33068,#33069,#33070));
#7696=EDGE_LOOP('',(#33071,#33072,#33073,#33074));
#7697=EDGE_LOOP('',(#33075,#33076,#33077,#33078));
#7698=EDGE_LOOP('',(#33079,#33080,#33081,#33082,#33083,#33084));
#7699=EDGE_LOOP('',(#33085,#33086,#33087,#33088));
#7700=EDGE_LOOP('',(#33089,#33090,#33091,#33092));
#7701=EDGE_LOOP('',(#33093,#33094,#33095,#33096));
#7702=EDGE_LOOP('',(#33097,#33098,#33099,#33100,#33101,#33102));
#7703=EDGE_LOOP('',(#33103,#33104,#33105,#33106));
#7704=EDGE_LOOP('',(#33107,#33108,#33109,#33110));
#7705=EDGE_LOOP('',(#33111,#33112,#33113,#33114));
#7706=EDGE_LOOP('',(#33115,#33116,#33117));
#7707=EDGE_LOOP('',(#33118,#33119,#33120,#33121,#33122,#33123));
#7708=EDGE_LOOP('',(#33124,#33125,#33126,#33127));
#7709=EDGE_LOOP('',(#33128,#33129,#33130,#33131));
#7710=EDGE_LOOP('',(#33132,#33133,#33134,#33135,#33136,#33137));
#7711=EDGE_LOOP('',(#33138,#33139,#33140,#33141));
#7712=EDGE_LOOP('',(#33142,#33143,#33144));
#7713=EDGE_LOOP('',(#33145,#33146,#33147,#33148));
#7714=EDGE_LOOP('',(#33149,#33150,#33151,#33152));
#7715=EDGE_LOOP('',(#33153,#33154,#33155,#33156,#33157,#33158));
#7716=EDGE_LOOP('',(#33159,#33160,#33161,#33162));
#7717=EDGE_LOOP('',(#33163,#33164,#33165,#33166));
#7718=EDGE_LOOP('',(#33167,#33168,#33169,#33170));
#7719=EDGE_LOOP('',(#33171,#33172,#33173,#33174,#33175,#33176));
#7720=EDGE_LOOP('',(#33177,#33178,#33179,#33180));
#7721=EDGE_LOOP('',(#33181,#33182,#33183,#33184));
#7722=EDGE_LOOP('',(#33185,#33186,#33187,#33188));
#7723=EDGE_LOOP('',(#33189,#33190,#33191,#33192,#33193,#33194));
#7724=EDGE_LOOP('',(#33195,#33196,#33197,#33198));
#7725=EDGE_LOOP('',(#33199,#33200,#33201,#33202));
#7726=EDGE_LOOP('',(#33203,#33204,#33205,#33206));
#7727=EDGE_LOOP('',(#33207,#33208,#33209,#33210,#33211,#33212));
#7728=EDGE_LOOP('',(#33213,#33214,#33215,#33216));
#7729=EDGE_LOOP('',(#33217,#33218,#33219,#33220));
#7730=EDGE_LOOP('',(#33221,#33222,#33223,#33224));
#7731=EDGE_LOOP('',(#33225,#33226,#33227,#33228,#33229,#33230));
#7732=EDGE_LOOP('',(#33231,#33232,#33233,#33234));
#7733=EDGE_LOOP('',(#33235,#33236,#33237,#33238));
#7734=EDGE_LOOP('',(#33239,#33240,#33241,#33242));
#7735=EDGE_LOOP('',(#33243,#33244,#33245));
#7736=EDGE_LOOP('',(#33246,#33247,#33248,#33249,#33250,#33251));
#7737=EDGE_LOOP('',(#33252,#33253,#33254,#33255));
#7738=EDGE_LOOP('',(#33256,#33257,#33258,#33259));
#7739=EDGE_LOOP('',(#33260,#33261,#33262,#33263,#33264,#33265));
#7740=EDGE_LOOP('',(#33266,#33267,#33268,#33269));
#7741=EDGE_LOOP('',(#33270,#33271,#33272));
#7742=EDGE_LOOP('',(#33273,#33274,#33275,#33276));
#7743=EDGE_LOOP('',(#33277,#33278,#33279,#33280));
#7744=EDGE_LOOP('',(#33281,#33282,#33283,#33284,#33285,#33286));
#7745=EDGE_LOOP('',(#33287,#33288,#33289,#33290));
#7746=EDGE_LOOP('',(#33291,#33292,#33293,#33294));
#7747=EDGE_LOOP('',(#33295,#33296,#33297,#33298));
#7748=EDGE_LOOP('',(#33299,#33300,#33301,#33302,#33303,#33304));
#7749=EDGE_LOOP('',(#33305,#33306,#33307,#33308));
#7750=EDGE_LOOP('',(#33309,#33310,#33311,#33312));
#7751=EDGE_LOOP('',(#33313,#33314,#33315,#33316));
#7752=EDGE_LOOP('',(#33317,#33318,#33319,#33320,#33321,#33322));
#7753=EDGE_LOOP('',(#33323,#33324,#33325,#33326));
#7754=EDGE_LOOP('',(#33327,#33328,#33329,#33330));
#7755=EDGE_LOOP('',(#33331,#33332,#33333,#33334));
#7756=EDGE_LOOP('',(#33335,#33336,#33337,#33338,#33339,#33340));
#7757=EDGE_LOOP('',(#33341,#33342,#33343,#33344));
#7758=EDGE_LOOP('',(#33345,#33346,#33347,#33348));
#7759=EDGE_LOOP('',(#33349,#33350,#33351,#33352));
#7760=EDGE_LOOP('',(#33353,#33354,#33355,#33356,#33357,#33358));
#7761=EDGE_LOOP('',(#33359,#33360,#33361,#33362));
#7762=EDGE_LOOP('',(#33363,#33364,#33365,#33366));
#7763=EDGE_LOOP('',(#33367,#33368,#33369,#33370));
#7764=EDGE_LOOP('',(#33371,#33372,#33373));
#7765=EDGE_LOOP('',(#33374,#33375,#33376,#33377,#33378,#33379));
#7766=EDGE_LOOP('',(#33380,#33381,#33382,#33383));
#7767=EDGE_LOOP('',(#33384,#33385,#33386,#33387));
#7768=EDGE_LOOP('',(#33388,#33389,#33390,#33391,#33392,#33393));
#7769=EDGE_LOOP('',(#33394,#33395,#33396,#33397));
#7770=EDGE_LOOP('',(#33398,#33399,#33400));
#7771=EDGE_LOOP('',(#33401,#33402,#33403,#33404));
#7772=EDGE_LOOP('',(#33405,#33406,#33407,#33408));
#7773=EDGE_LOOP('',(#33409,#33410,#33411,#33412,#33413,#33414));
#7774=EDGE_LOOP('',(#33415,#33416,#33417,#33418));
#7775=EDGE_LOOP('',(#33419,#33420,#33421,#33422));
#7776=EDGE_LOOP('',(#33423,#33424,#33425,#33426));
#7777=EDGE_LOOP('',(#33427,#33428,#33429,#33430,#33431,#33432));
#7778=EDGE_LOOP('',(#33433,#33434,#33435,#33436));
#7779=EDGE_LOOP('',(#33437,#33438,#33439,#33440));
#7780=EDGE_LOOP('',(#33441,#33442,#33443,#33444));
#7781=EDGE_LOOP('',(#33445,#33446,#33447,#33448,#33449,#33450));
#7782=EDGE_LOOP('',(#33451,#33452,#33453,#33454));
#7783=EDGE_LOOP('',(#33455,#33456,#33457,#33458));
#7784=EDGE_LOOP('',(#33459,#33460,#33461,#33462));
#7785=EDGE_LOOP('',(#33463,#33464,#33465,#33466,#33467,#33468));
#7786=EDGE_LOOP('',(#33469,#33470,#33471,#33472));
#7787=EDGE_LOOP('',(#33473,#33474,#33475,#33476));
#7788=EDGE_LOOP('',(#33477,#33478,#33479,#33480));
#7789=EDGE_LOOP('',(#33481,#33482,#33483,#33484,#33485,#33486));
#7790=EDGE_LOOP('',(#33487,#33488,#33489,#33490));
#7791=EDGE_LOOP('',(#33491,#33492,#33493,#33494));
#7792=EDGE_LOOP('',(#33495,#33496,#33497,#33498));
#7793=EDGE_LOOP('',(#33499,#33500,#33501));
#7794=EDGE_LOOP('',(#33502,#33503,#33504,#33505,#33506,#33507));
#7795=EDGE_LOOP('',(#33508,#33509,#33510,#33511));
#7796=EDGE_LOOP('',(#33512,#33513,#33514,#33515));
#7797=EDGE_LOOP('',(#33516,#33517,#33518,#33519,#33520,#33521));
#7798=EDGE_LOOP('',(#33522,#33523,#33524,#33525));
#7799=EDGE_LOOP('',(#33526,#33527,#33528));
#7800=EDGE_LOOP('',(#33529,#33530,#33531,#33532));
#7801=EDGE_LOOP('',(#33533,#33534,#33535,#33536));
#7802=EDGE_LOOP('',(#33537,#33538,#33539,#33540,#33541,#33542));
#7803=EDGE_LOOP('',(#33543,#33544,#33545,#33546));
#7804=EDGE_LOOP('',(#33547,#33548,#33549,#33550));
#7805=EDGE_LOOP('',(#33551,#33552,#33553,#33554));
#7806=EDGE_LOOP('',(#33555,#33556,#33557,#33558,#33559,#33560));
#7807=EDGE_LOOP('',(#33561,#33562,#33563,#33564));
#7808=EDGE_LOOP('',(#33565,#33566,#33567,#33568));
#7809=EDGE_LOOP('',(#33569,#33570,#33571,#33572));
#7810=EDGE_LOOP('',(#33573,#33574,#33575,#33576,#33577,#33578));
#7811=EDGE_LOOP('',(#33579,#33580,#33581,#33582));
#7812=EDGE_LOOP('',(#33583,#33584,#33585,#33586));
#7813=EDGE_LOOP('',(#33587,#33588,#33589,#33590));
#7814=EDGE_LOOP('',(#33591,#33592,#33593,#33594,#33595,#33596));
#7815=EDGE_LOOP('',(#33597,#33598,#33599,#33600));
#7816=EDGE_LOOP('',(#33601,#33602,#33603,#33604));
#7817=EDGE_LOOP('',(#33605,#33606,#33607,#33608));
#7818=EDGE_LOOP('',(#33609,#33610,#33611,#33612,#33613,#33614));
#7819=EDGE_LOOP('',(#33615,#33616,#33617,#33618));
#7820=EDGE_LOOP('',(#33619,#33620,#33621,#33622));
#7821=EDGE_LOOP('',(#33623,#33624,#33625,#33626));
#7822=EDGE_LOOP('',(#33627,#33628,#33629));
#7823=EDGE_LOOP('',(#33630,#33631,#33632,#33633,#33634,#33635));
#7824=EDGE_LOOP('',(#33636,#33637,#33638,#33639));
#7825=EDGE_LOOP('',(#33640,#33641,#33642,#33643));
#7826=EDGE_LOOP('',(#33644,#33645,#33646,#33647,#33648,#33649));
#7827=EDGE_LOOP('',(#33650,#33651,#33652,#33653));
#7828=EDGE_LOOP('',(#33654,#33655,#33656));
#7829=EDGE_LOOP('',(#33657,#33658,#33659,#33660));
#7830=EDGE_LOOP('',(#33661,#33662,#33663,#33664));
#7831=EDGE_LOOP('',(#33665,#33666,#33667,#33668,#33669,#33670));
#7832=EDGE_LOOP('',(#33671,#33672,#33673,#33674));
#7833=EDGE_LOOP('',(#33675,#33676,#33677,#33678));
#7834=EDGE_LOOP('',(#33679,#33680,#33681,#33682));
#7835=EDGE_LOOP('',(#33683,#33684,#33685,#33686,#33687,#33688));
#7836=EDGE_LOOP('',(#33689,#33690,#33691,#33692));
#7837=EDGE_LOOP('',(#33693,#33694,#33695,#33696));
#7838=EDGE_LOOP('',(#33697,#33698,#33699,#33700));
#7839=EDGE_LOOP('',(#33701,#33702,#33703,#33704,#33705,#33706));
#7840=EDGE_LOOP('',(#33707,#33708,#33709,#33710));
#7841=EDGE_LOOP('',(#33711,#33712,#33713,#33714));
#7842=EDGE_LOOP('',(#33715,#33716,#33717,#33718));
#7843=EDGE_LOOP('',(#33719,#33720,#33721,#33722,#33723,#33724));
#7844=EDGE_LOOP('',(#33725,#33726,#33727,#33728));
#7845=EDGE_LOOP('',(#33729,#33730,#33731,#33732));
#7846=EDGE_LOOP('',(#33733,#33734,#33735,#33736));
#7847=EDGE_LOOP('',(#33737,#33738,#33739,#33740,#33741,#33742));
#7848=EDGE_LOOP('',(#33743,#33744,#33745,#33746));
#7849=EDGE_LOOP('',(#33747,#33748,#33749,#33750));
#7850=EDGE_LOOP('',(#33751,#33752,#33753,#33754));
#7851=EDGE_LOOP('',(#33755,#33756,#33757));
#7852=EDGE_LOOP('',(#33758,#33759,#33760,#33761,#33762,#33763));
#7853=EDGE_LOOP('',(#33764,#33765,#33766,#33767));
#7854=EDGE_LOOP('',(#33768,#33769,#33770,#33771));
#7855=EDGE_LOOP('',(#33772,#33773,#33774,#33775,#33776,#33777));
#7856=EDGE_LOOP('',(#33778,#33779,#33780,#33781));
#7857=EDGE_LOOP('',(#33782,#33783,#33784));
#7858=EDGE_LOOP('',(#33785,#33786,#33787,#33788));
#7859=EDGE_LOOP('',(#33789,#33790,#33791,#33792));
#7860=EDGE_LOOP('',(#33793,#33794,#33795,#33796,#33797,#33798));
#7861=EDGE_LOOP('',(#33799,#33800,#33801,#33802));
#7862=EDGE_LOOP('',(#33803,#33804,#33805,#33806));
#7863=EDGE_LOOP('',(#33807,#33808,#33809,#33810));
#7864=EDGE_LOOP('',(#33811,#33812,#33813,#33814,#33815,#33816));
#7865=EDGE_LOOP('',(#33817,#33818,#33819,#33820));
#7866=EDGE_LOOP('',(#33821,#33822,#33823,#33824));
#7867=EDGE_LOOP('',(#33825,#33826,#33827,#33828));
#7868=EDGE_LOOP('',(#33829,#33830,#33831,#33832,#33833,#33834));
#7869=EDGE_LOOP('',(#33835,#33836,#33837,#33838));
#7870=EDGE_LOOP('',(#33839,#33840,#33841,#33842));
#7871=EDGE_LOOP('',(#33843,#33844,#33845,#33846));
#7872=EDGE_LOOP('',(#33847,#33848,#33849,#33850,#33851,#33852));
#7873=EDGE_LOOP('',(#33853,#33854,#33855,#33856));
#7874=EDGE_LOOP('',(#33857,#33858,#33859,#33860));
#7875=EDGE_LOOP('',(#33861,#33862,#33863,#33864));
#7876=EDGE_LOOP('',(#33865,#33866,#33867,#33868,#33869,#33870));
#7877=EDGE_LOOP('',(#33871,#33872,#33873,#33874));
#7878=EDGE_LOOP('',(#33875,#33876,#33877,#33878));
#7879=EDGE_LOOP('',(#33879,#33880,#33881,#33882));
#7880=EDGE_LOOP('',(#33883,#33884,#33885));
#7881=EDGE_LOOP('',(#33886,#33887,#33888,#33889,#33890,#33891));
#7882=EDGE_LOOP('',(#33892,#33893,#33894,#33895));
#7883=EDGE_LOOP('',(#33896,#33897,#33898,#33899));
#7884=EDGE_LOOP('',(#33900,#33901,#33902,#33903,#33904,#33905));
#7885=EDGE_LOOP('',(#33906,#33907,#33908,#33909));
#7886=EDGE_LOOP('',(#33910,#33911,#33912));
#7887=EDGE_LOOP('',(#33913,#33914,#33915,#33916));
#7888=EDGE_LOOP('',(#33917,#33918,#33919,#33920));
#7889=EDGE_LOOP('',(#33921,#33922,#33923,#33924,#33925,#33926));
#7890=EDGE_LOOP('',(#33927,#33928,#33929,#33930));
#7891=EDGE_LOOP('',(#33931,#33932,#33933,#33934));
#7892=EDGE_LOOP('',(#33935,#33936,#33937,#33938));
#7893=EDGE_LOOP('',(#33939,#33940,#33941,#33942,#33943,#33944));
#7894=EDGE_LOOP('',(#33945,#33946,#33947,#33948));
#7895=EDGE_LOOP('',(#33949,#33950,#33951,#33952));
#7896=EDGE_LOOP('',(#33953,#33954,#33955,#33956));
#7897=EDGE_LOOP('',(#33957,#33958,#33959,#33960,#33961,#33962));
#7898=EDGE_LOOP('',(#33963,#33964,#33965,#33966));
#7899=EDGE_LOOP('',(#33967,#33968,#33969,#33970));
#7900=EDGE_LOOP('',(#33971,#33972,#33973,#33974));
#7901=EDGE_LOOP('',(#33975,#33976,#33977,#33978,#33979,#33980));
#7902=EDGE_LOOP('',(#33981,#33982,#33983,#33984));
#7903=EDGE_LOOP('',(#33985,#33986,#33987,#33988));
#7904=EDGE_LOOP('',(#33989,#33990,#33991,#33992));
#7905=EDGE_LOOP('',(#33993,#33994,#33995,#33996,#33997,#33998));
#7906=EDGE_LOOP('',(#33999,#34000,#34001,#34002));
#7907=EDGE_LOOP('',(#34003,#34004,#34005,#34006));
#7908=EDGE_LOOP('',(#34007,#34008,#34009,#34010));
#7909=EDGE_LOOP('',(#34011,#34012,#34013));
#7910=EDGE_LOOP('',(#34014,#34015,#34016,#34017,#34018,#34019));
#7911=EDGE_LOOP('',(#34020,#34021,#34022,#34023));
#7912=EDGE_LOOP('',(#34024,#34025,#34026,#34027));
#7913=EDGE_LOOP('',(#34028,#34029,#34030,#34031,#34032,#34033));
#7914=EDGE_LOOP('',(#34034,#34035,#34036,#34037));
#7915=EDGE_LOOP('',(#34038,#34039,#34040));
#7916=EDGE_LOOP('',(#34041,#34042,#34043,#34044));
#7917=EDGE_LOOP('',(#34045,#34046,#34047,#34048));
#7918=EDGE_LOOP('',(#34049,#34050,#34051,#34052,#34053,#34054));
#7919=EDGE_LOOP('',(#34055,#34056,#34057,#34058));
#7920=EDGE_LOOP('',(#34059,#34060,#34061,#34062));
#7921=EDGE_LOOP('',(#34063,#34064,#34065,#34066));
#7922=EDGE_LOOP('',(#34067,#34068,#34069,#34070,#34071,#34072));
#7923=EDGE_LOOP('',(#34073,#34074,#34075,#34076));
#7924=EDGE_LOOP('',(#34077,#34078,#34079,#34080));
#7925=EDGE_LOOP('',(#34081,#34082,#34083,#34084));
#7926=EDGE_LOOP('',(#34085,#34086,#34087,#34088,#34089,#34090));
#7927=EDGE_LOOP('',(#34091,#34092,#34093,#34094));
#7928=EDGE_LOOP('',(#34095,#34096,#34097,#34098));
#7929=EDGE_LOOP('',(#34099,#34100,#34101,#34102));
#7930=EDGE_LOOP('',(#34103,#34104,#34105,#34106,#34107,#34108));
#7931=EDGE_LOOP('',(#34109,#34110,#34111,#34112));
#7932=EDGE_LOOP('',(#34113,#34114,#34115,#34116));
#7933=EDGE_LOOP('',(#34117,#34118,#34119,#34120));
#7934=EDGE_LOOP('',(#34121,#34122,#34123,#34124,#34125,#34126));
#7935=EDGE_LOOP('',(#34127,#34128,#34129,#34130));
#7936=EDGE_LOOP('',(#34131,#34132,#34133,#34134));
#7937=EDGE_LOOP('',(#34135,#34136,#34137,#34138));
#7938=EDGE_LOOP('',(#34139,#34140,#34141));
#7939=EDGE_LOOP('',(#34142,#34143,#34144,#34145,#34146,#34147));
#7940=EDGE_LOOP('',(#34148,#34149,#34150,#34151));
#7941=EDGE_LOOP('',(#34152,#34153,#34154,#34155));
#7942=EDGE_LOOP('',(#34156,#34157,#34158,#34159,#34160,#34161));
#7943=EDGE_LOOP('',(#34162,#34163,#34164,#34165));
#7944=EDGE_LOOP('',(#34166,#34167,#34168));
#7945=EDGE_LOOP('',(#34169,#34170,#34171,#34172));
#7946=EDGE_LOOP('',(#34173,#34174,#34175,#34176));
#7947=EDGE_LOOP('',(#34177,#34178,#34179,#34180,#34181,#34182));
#7948=EDGE_LOOP('',(#34183,#34184,#34185,#34186));
#7949=EDGE_LOOP('',(#34187,#34188,#34189,#34190));
#7950=EDGE_LOOP('',(#34191,#34192,#34193,#34194));
#7951=EDGE_LOOP('',(#34195,#34196,#34197,#34198,#34199,#34200));
#7952=EDGE_LOOP('',(#34201,#34202,#34203,#34204));
#7953=EDGE_LOOP('',(#34205,#34206,#34207,#34208));
#7954=EDGE_LOOP('',(#34209,#34210,#34211,#34212));
#7955=EDGE_LOOP('',(#34213,#34214,#34215,#34216,#34217,#34218));
#7956=EDGE_LOOP('',(#34219,#34220,#34221,#34222));
#7957=EDGE_LOOP('',(#34223,#34224,#34225,#34226));
#7958=EDGE_LOOP('',(#34227,#34228,#34229,#34230));
#7959=EDGE_LOOP('',(#34231,#34232,#34233,#34234,#34235,#34236));
#7960=EDGE_LOOP('',(#34237,#34238,#34239,#34240));
#7961=EDGE_LOOP('',(#34241,#34242,#34243,#34244));
#7962=EDGE_LOOP('',(#34245,#34246,#34247,#34248));
#7963=EDGE_LOOP('',(#34249,#34250,#34251,#34252,#34253,#34254));
#7964=EDGE_LOOP('',(#34255,#34256,#34257,#34258));
#7965=EDGE_LOOP('',(#34259,#34260,#34261,#34262));
#7966=EDGE_LOOP('',(#34263,#34264,#34265,#34266));
#7967=EDGE_LOOP('',(#34267,#34268,#34269));
#7968=EDGE_LOOP('',(#34270,#34271,#34272,#34273,#34274,#34275));
#7969=EDGE_LOOP('',(#34276,#34277,#34278,#34279));
#7970=EDGE_LOOP('',(#34280,#34281,#34282,#34283));
#7971=EDGE_LOOP('',(#34284,#34285,#34286,#34287,#34288,#34289));
#7972=EDGE_LOOP('',(#34290,#34291,#34292,#34293));
#7973=EDGE_LOOP('',(#34294,#34295,#34296));
#7974=EDGE_LOOP('',(#34297,#34298,#34299,#34300));
#7975=EDGE_LOOP('',(#34301,#34302,#34303,#34304));
#7976=EDGE_LOOP('',(#34305,#34306,#34307,#34308,#34309,#34310));
#7977=EDGE_LOOP('',(#34311,#34312,#34313,#34314));
#7978=EDGE_LOOP('',(#34315,#34316,#34317,#34318));
#7979=EDGE_LOOP('',(#34319,#34320,#34321,#34322));
#7980=EDGE_LOOP('',(#34323,#34324,#34325,#34326,#34327,#34328));
#7981=EDGE_LOOP('',(#34329,#34330,#34331,#34332));
#7982=EDGE_LOOP('',(#34333,#34334,#34335,#34336));
#7983=EDGE_LOOP('',(#34337,#34338,#34339,#34340));
#7984=EDGE_LOOP('',(#34341,#34342,#34343,#34344,#34345,#34346));
#7985=EDGE_LOOP('',(#34347,#34348,#34349,#34350));
#7986=EDGE_LOOP('',(#34351,#34352,#34353,#34354));
#7987=EDGE_LOOP('',(#34355,#34356,#34357,#34358));
#7988=EDGE_LOOP('',(#34359,#34360,#34361,#34362,#34363,#34364));
#7989=EDGE_LOOP('',(#34365,#34366,#34367,#34368));
#7990=EDGE_LOOP('',(#34369,#34370,#34371,#34372));
#7991=EDGE_LOOP('',(#34373,#34374,#34375,#34376));
#7992=EDGE_LOOP('',(#34377,#34378,#34379,#34380,#34381,#34382));
#7993=EDGE_LOOP('',(#34383,#34384,#34385,#34386));
#7994=EDGE_LOOP('',(#34387,#34388,#34389,#34390));
#7995=EDGE_LOOP('',(#34391,#34392,#34393,#34394));
#7996=EDGE_LOOP('',(#34395,#34396,#34397));
#7997=EDGE_LOOP('',(#34398,#34399,#34400,#34401));
#7998=EDGE_LOOP('',(#34402,#34403,#34404,#34405,#34406,#34407));
#7999=EDGE_LOOP('',(#34408,#34409,#34410,#34411));
#8000=EDGE_LOOP('',(#34412,#34413,#34414,#34415,#34416,#34417));
#8001=EDGE_LOOP('',(#34418,#34419,#34420,#34421));
#8002=EDGE_LOOP('',(#34422,#34423,#34424));
#8003=EDGE_LOOP('',(#34425,#34426,#34427,#34428));
#8004=EDGE_LOOP('',(#34429,#34430,#34431,#34432));
#8005=EDGE_LOOP('',(#34433,#34434,#34435,#34436,#34437,#34438));
#8006=EDGE_LOOP('',(#34439,#34440,#34441,#34442));
#8007=EDGE_LOOP('',(#34443,#34444,#34445,#34446));
#8008=EDGE_LOOP('',(#34447,#34448,#34449,#34450));
#8009=EDGE_LOOP('',(#34451,#34452,#34453,#34454,#34455,#34456));
#8010=EDGE_LOOP('',(#34457,#34458,#34459,#34460));
#8011=EDGE_LOOP('',(#34461,#34462,#34463,#34464));
#8012=EDGE_LOOP('',(#34465,#34466,#34467,#34468));
#8013=EDGE_LOOP('',(#34469,#34470,#34471,#34472,#34473,#34474));
#8014=EDGE_LOOP('',(#34475,#34476,#34477,#34478));
#8015=EDGE_LOOP('',(#34479,#34480,#34481,#34482));
#8016=EDGE_LOOP('',(#34483,#34484,#34485,#34486));
#8017=EDGE_LOOP('',(#34487,#34488,#34489,#34490,#34491,#34492));
#8018=EDGE_LOOP('',(#34493,#34494,#34495,#34496));
#8019=EDGE_LOOP('',(#34497,#34498,#34499,#34500));
#8020=EDGE_LOOP('',(#34501,#34502,#34503,#34504));
#8021=EDGE_LOOP('',(#34505,#34506,#34507,#34508,#34509,#34510));
#8022=EDGE_LOOP('',(#34511,#34512,#34513,#34514));
#8023=EDGE_LOOP('',(#34515,#34516,#34517,#34518));
#8024=EDGE_LOOP('',(#34519,#34520,#34521,#34522));
#8025=EDGE_LOOP('',(#34523,#34524,#34525));
#8026=EDGE_LOOP('',(#34526,#34527,#34528,#34529));
#8027=EDGE_LOOP('',(#34530,#34531,#34532,#34533));
#8028=EDGE_LOOP('',(#34534,#34535,#34536,#34537,#34538,#34539));
#8029=EDGE_LOOP('',(#34540,#34541,#34542,#34543));
#8030=EDGE_LOOP('',(#34544,#34545,#34546,#34547,#34548,#34549));
#8031=EDGE_LOOP('',(#34550,#34551,#34552,#34553));
#8032=EDGE_LOOP('',(#34554,#34555,#34556));
#8033=EDGE_LOOP('',(#34557,#34558,#34559,#34560));
#8034=EDGE_LOOP('',(#34561,#34562,#34563,#34564,#34565,#34566));
#8035=EDGE_LOOP('',(#34567,#34568,#34569,#34570));
#8036=EDGE_LOOP('',(#34571,#34572,#34573,#34574));
#8037=EDGE_LOOP('',(#34575,#34576,#34577,#34578));
#8038=EDGE_LOOP('',(#34579,#34580,#34581,#34582,#34583,#34584));
#8039=EDGE_LOOP('',(#34585,#34586,#34587,#34588));
#8040=EDGE_LOOP('',(#34589,#34590,#34591,#34592));
#8041=EDGE_LOOP('',(#34593,#34594,#34595,#34596));
#8042=EDGE_LOOP('',(#34597,#34598,#34599,#34600,#34601,#34602));
#8043=EDGE_LOOP('',(#34603,#34604,#34605,#34606));
#8044=EDGE_LOOP('',(#34607,#34608,#34609,#34610));
#8045=EDGE_LOOP('',(#34611,#34612,#34613,#34614));
#8046=EDGE_LOOP('',(#34615,#34616,#34617,#34618,#34619,#34620));
#8047=EDGE_LOOP('',(#34621,#34622,#34623,#34624));
#8048=EDGE_LOOP('',(#34625,#34626,#34627,#34628));
#8049=EDGE_LOOP('',(#34629,#34630,#34631,#34632));
#8050=EDGE_LOOP('',(#34633,#34634,#34635,#34636,#34637,#34638));
#8051=EDGE_LOOP('',(#34639,#34640,#34641,#34642));
#8052=EDGE_LOOP('',(#34643,#34644,#34645,#34646));
#8053=EDGE_LOOP('',(#34647,#34648,#34649,#34650));
#8054=EDGE_LOOP('',(#34651,#34652,#34653));
#8055=EDGE_LOOP('',(#34654,#34655,#34656,#34657));
#8056=EDGE_LOOP('',(#34658,#34659,#34660,#34661));
#8057=EDGE_LOOP('',(#34662,#34663,#34664,#34665));
#8058=EDGE_LOOP('',(#34666,#34667,#34668,#34669,#34670,#34671));
#8059=EDGE_LOOP('',(#34672,#34673,#34674,#34675));
#8060=EDGE_LOOP('',(#34676,#34677,#34678));
#8061=EDGE_LOOP('',(#34679,#34680,#34681,#34682));
#8062=EDGE_LOOP('',(#34683,#34684,#34685,#34686,#34687,#34688));
#8063=EDGE_LOOP('',(#34689,#34690,#34691,#34692));
#8064=EDGE_LOOP('',(#34693,#34694,#34695,#34696));
#8065=EDGE_LOOP('',(#34697,#34698,#34699,#34700,#34701,#34702));
#8066=EDGE_LOOP('',(#34703,#34704,#34705,#34706));
#8067=EDGE_LOOP('',(#34707,#34708,#34709,#34710));
#8068=EDGE_LOOP('',(#34711,#34712,#34713,#34714,#34715,#34716));
#8069=EDGE_LOOP('',(#34717,#34718,#34719,#34720));
#8070=EDGE_LOOP('',(#34721,#34722,#34723,#34724));
#8071=EDGE_LOOP('',(#34725,#34726,#34727,#34728,#34729,#34730));
#8072=EDGE_LOOP('',(#34731,#34732,#34733,#34734));
#8073=EDGE_LOOP('',(#34735,#34736,#34737,#34738));
#8074=EDGE_LOOP('',(#34739,#34740,#34741,#34742));
#8075=EDGE_LOOP('',(#34743,#34744,#34745,#34746,#34747,#34748));
#8076=EDGE_LOOP('',(#34749,#34750,#34751,#34752));
#8077=EDGE_LOOP('',(#34753,#34754,#34755,#34756));
#8078=EDGE_LOOP('',(#34757,#34758,#34759,#34760));
#8079=EDGE_LOOP('',(#34761,#34762,#34763,#34764,#34765,#34766));
#8080=EDGE_LOOP('',(#34767,#34768,#34769,#34770));
#8081=EDGE_LOOP('',(#34771,#34772,#34773,#34774));
#8082=EDGE_LOOP('',(#34775,#34776,#34777,#34778));
#8083=EDGE_LOOP('',(#34779,#34780,#34781));
#8084=EDGE_LOOP('',(#34782,#34783,#34784,#34785));
#8085=EDGE_LOOP('',(#34786,#34787,#34788,#34789));
#8086=EDGE_LOOP('',(#34790,#34791,#34792,#34793));
#8087=EDGE_LOOP('',(#34794,#34795,#34796,#34797));
#8088=EDGE_LOOP('',(#34798,#34799,#34800,#34801,#34802,#34803));
#8089=EDGE_LOOP('',(#34804,#34805,#34806,#34807));
#8090=EDGE_LOOP('',(#34808,#34809,#34810,#34811));
#8091=EDGE_LOOP('',(#34812,#34813,#34814,#34815,#34816,#34817));
#8092=EDGE_LOOP('',(#34818,#34819,#34820,#34821));
#8093=EDGE_LOOP('',(#34822,#34823,#34824,#34825));
#8094=EDGE_LOOP('',(#34826,#34827,#34828,#34829,#34830,#34831));
#8095=EDGE_LOOP('',(#34832,#34833,#34834,#34835));
#8096=EDGE_LOOP('',(#34836,#34837,#34838,#34839));
#8097=EDGE_LOOP('',(#34840,#34841,#34842,#34843,#34844,#34845));
#8098=EDGE_LOOP('',(#34846,#34847,#34848,#34849));
#8099=EDGE_LOOP('',(#34850,#34851,#34852,#34853,#34854,#34855));
#8100=EDGE_LOOP('',(#34856,#34857,#34858,#34859));
#8101=EDGE_LOOP('',(#34860,#34861,#34862));
#8102=EDGE_LOOP('',(#34863,#34864,#34865,#34866));
#8103=EDGE_LOOP('',(#34867,#34868,#34869,#34870));
#8104=EDGE_LOOP('',(#34871,#34872,#34873,#34874,#34875,#34876));
#8105=EDGE_LOOP('',(#34877,#34878,#34879,#34880));
#8106=EDGE_LOOP('',(#34881,#34882,#34883,#34884));
#8107=EDGE_LOOP('',(#34885,#34886,#34887,#34888));
#8108=EDGE_LOOP('',(#34889,#34890,#34891,#34892,#34893,#34894));
#8109=EDGE_LOOP('',(#34895,#34896,#34897,#34898));
#8110=EDGE_LOOP('',(#34899,#34900,#34901,#34902));
#8111=EDGE_LOOP('',(#34903,#34904,#34905,#34906));
#8112=EDGE_LOOP('',(#34907,#34908,#34909));
#8113=EDGE_LOOP('',(#34910,#34911,#34912,#34913));
#8114=EDGE_LOOP('',(#34914,#34915,#34916,#34917));
#8115=EDGE_LOOP('',(#34918,#34919,#34920,#34921));
#8116=EDGE_LOOP('',(#34922,#34923,#34924,#34925));
#8117=EDGE_LOOP('',(#34926,#34927,#34928,#34929));
#8118=EDGE_LOOP('',(#34930,#34931,#34932,#34933,#34934,#34935));
#8119=EDGE_LOOP('',(#34936,#34937,#34938,#34939));
#8120=EDGE_LOOP('',(#34940,#34941,#34942,#34943));
#8121=EDGE_LOOP('',(#34944,#34945,#34946,#34947,#34948,#34949));
#8122=EDGE_LOOP('',(#34950,#34951,#34952,#34953));
#8123=EDGE_LOOP('',(#34954,#34955,#34956,#34957));
#8124=EDGE_LOOP('',(#34958,#34959,#34960,#34961,#34962,#34963));
#8125=EDGE_LOOP('',(#34964,#34965,#34966,#34967));
#8126=EDGE_LOOP('',(#34968,#34969,#34970,#34971));
#8127=EDGE_LOOP('',(#34972,#34973,#34974,#34975,#34976,#34977));
#8128=EDGE_LOOP('',(#34978,#34979,#34980,#34981));
#8129=EDGE_LOOP('',(#34982,#34983,#34984,#34985,#34986,#34987));
#8130=EDGE_LOOP('',(#34988,#34989,#34990,#34991));
#8131=EDGE_LOOP('',(#34992,#34993,#34994));
#8132=EDGE_LOOP('',(#34995,#34996,#34997,#34998));
#8133=EDGE_LOOP('',(#34999,#35000,#35001,#35002,#35003,#35004));
#8134=EDGE_LOOP('',(#35005,#35006,#35007,#35008));
#8135=EDGE_LOOP('',(#35009,#35010,#35011,#35012));
#8136=EDGE_LOOP('',(#35013,#35014,#35015,#35016));
#8137=EDGE_LOOP('',(#35017,#35018,#35019,#35020,#35021,#35022));
#8138=EDGE_LOOP('',(#35023,#35024,#35025,#35026));
#8139=EDGE_LOOP('',(#35027,#35028,#35029,#35030));
#8140=EDGE_LOOP('',(#35031,#35032,#35033,#35034));
#8141=EDGE_LOOP('',(#35035,#35036,#35037));
#8142=EDGE_LOOP('',(#35038,#35039,#35040,#35041));
#8143=EDGE_LOOP('',(#35042,#35043,#35044,#35045));
#8144=EDGE_LOOP('',(#35046,#35047,#35048,#35049));
#8145=EDGE_LOOP('',(#35050,#35051,#35052,#35053));
#8146=EDGE_LOOP('',(#35054,#35055,#35056,#35057));
#8147=EDGE_LOOP('',(#35058,#35059,#35060,#35061));
#8148=EDGE_LOOP('',(#35062,#35063,#35064,#35065,#35066,#35067));
#8149=EDGE_LOOP('',(#35068,#35069,#35070,#35071));
#8150=EDGE_LOOP('',(#35072,#35073,#35074,#35075));
#8151=EDGE_LOOP('',(#35076,#35077,#35078,#35079,#35080,#35081));
#8152=EDGE_LOOP('',(#35082,#35083,#35084,#35085));
#8153=EDGE_LOOP('',(#35086,#35087,#35088,#35089));
#8154=EDGE_LOOP('',(#35090,#35091,#35092,#35093,#35094,#35095));
#8155=EDGE_LOOP('',(#35096,#35097,#35098,#35099));
#8156=EDGE_LOOP('',(#35100,#35101,#35102,#35103));
#8157=EDGE_LOOP('',(#35104,#35105,#35106,#35107,#35108,#35109));
#8158=EDGE_LOOP('',(#35110,#35111,#35112,#35113));
#8159=EDGE_LOOP('',(#35114,#35115,#35116,#35117,#35118,#35119));
#8160=EDGE_LOOP('',(#35120,#35121,#35122,#35123));
#8161=EDGE_LOOP('',(#35124,#35125,#35126));
#8162=EDGE_LOOP('',(#35127,#35128,#35129,#35130));
#8163=EDGE_LOOP('',(#35131,#35132,#35133,#35134,#35135,#35136));
#8164=EDGE_LOOP('',(#35137,#35138,#35139,#35140));
#8165=EDGE_LOOP('',(#35141,#35142,#35143,#35144));
#8166=EDGE_LOOP('',(#35145,#35146,#35147,#35148,#35149,#35150));
#8167=EDGE_LOOP('',(#35151,#35152,#35153,#35154));
#8168=EDGE_LOOP('',(#35155,#35156,#35157,#35158));
#8169=EDGE_LOOP('',(#35159,#35160,#35161,#35162));
#8170=EDGE_LOOP('',(#35163,#35164,#35165));
#8171=EDGE_LOOP('',(#35166,#35167,#35168,#35169));
#8172=EDGE_LOOP('',(#35170,#35171,#35172));
#8173=EDGE_LOOP('',(#35173,#35174,#35175));
#8174=EDGE_LOOP('',(#35176));
#8175=EDGE_LOOP('',(#35177));
#8176=EDGE_LOOP('',(#35178));
#8177=EDGE_LOOP('',(#35179));
#8178=EDGE_LOOP('',(#35180,#35181,#35182,#35183));
#8179=EDGE_LOOP('',(#35184,#35185,#35186,#35187));
#8180=EDGE_LOOP('',(#35188,#35189,#35190,#35191,#35192,#35193));
#8181=EDGE_LOOP('',(#35194,#35195,#35196,#35197));
#8182=EDGE_LOOP('',(#35198,#35199,#35200,#35201));
#8183=EDGE_LOOP('',(#35202,#35203,#35204,#35205,#35206,#35207));
#8184=EDGE_LOOP('',(#35208,#35209,#35210,#35211));
#8185=EDGE_LOOP('',(#35212,#35213,#35214,#35215));
#8186=EDGE_LOOP('',(#35216,#35217,#35218,#35219,#35220,#35221));
#8187=EDGE_LOOP('',(#35222,#35223,#35224,#35225));
#8188=EDGE_LOOP('',(#35226,#35227,#35228,#35229));
#8189=EDGE_LOOP('',(#35230,#35231,#35232,#35233,#35234,#35235));
#8190=EDGE_LOOP('',(#35236,#35237,#35238,#35239));
#8191=EDGE_LOOP('',(#35240,#35241,#35242));
#8192=EDGE_LOOP('',(#35243,#35244,#35245,#35246,#35247,#35248));
#8193=EDGE_LOOP('',(#35249,#35250,#35251));
#8194=EDGE_LOOP('',(#35252,#35253,#35254,#35255));
#8195=EDGE_LOOP('',(#35256,#35257,#35258,#35259));
#8196=EDGE_LOOP('',(#35260,#35261,#35262,#35263));
#8197=EDGE_LOOP('',(#35264,#35265,#35266,#35267,#35268,#35269));
#8198=EDGE_LOOP('',(#35270,#35271,#35272,#35273,#35274,#35275));
#8199=EDGE_LOOP('',(#35276,#35277,#35278,#35279));
#8200=EDGE_LOOP('',(#35280,#35281,#35282,#35283));
#8201=EDGE_LOOP('',(#35284,#35285,#35286));
#8202=EDGE_LOOP('',(#35287,#35288,#35289,#35290));
#8203=EDGE_LOOP('',(#35291,#35292,#35293,#35294));
#8204=EDGE_LOOP('',(#35295,#35296,#35297,#35298));
#8205=EDGE_LOOP('',(#35299,#35300,#35301,#35302,#35303,#35304));
#8206=EDGE_LOOP('',(#35305,#35306,#35307,#35308));
#8207=EDGE_LOOP('',(#35309,#35310,#35311,#35312));
#8208=EDGE_LOOP('',(#35313,#35314,#35315,#35316,#35317,#35318));
#8209=EDGE_LOOP('',(#35319,#35320,#35321,#35322));
#8210=EDGE_LOOP('',(#35323,#35324,#35325,#35326));
#8211=EDGE_LOOP('',(#35327,#35328,#35329,#35330,#35331,#35332));
#8212=EDGE_LOOP('',(#35333,#35334,#35335,#35336));
#8213=EDGE_LOOP('',(#35337,#35338,#35339,#35340));
#8214=EDGE_LOOP('',(#35341,#35342,#35343,#35344,#35345,#35346));
#8215=EDGE_LOOP('',(#35347,#35348,#35349,#35350));
#8216=EDGE_LOOP('',(#35351,#35352,#35353));
#8217=EDGE_LOOP('',(#35354,#35355,#35356,#35357,#35358,#35359,#35360));
#8218=EDGE_LOOP('',(#35361,#35362,#35363,#35364));
#8219=EDGE_LOOP('',(#35365,#35366,#35367,#35368));
#8220=EDGE_LOOP('',(#35369,#35370,#35371,#35372,#35373,#35374));
#8221=EDGE_LOOP('',(#35375,#35376,#35377,#35378,#35379,#35380));
#8222=EDGE_LOOP('',(#35381,#35382,#35383,#35384));
#8223=EDGE_LOOP('',(#35385,#35386,#35387,#35388));
#8224=EDGE_LOOP('',(#35389,#35390,#35391));
#8225=EDGE_LOOP('',(#35392,#35393,#35394,#35395));
#8226=EDGE_LOOP('',(#35396,#35397,#35398,#35399));
#8227=EDGE_LOOP('',(#35400,#35401,#35402,#35403));
#8228=EDGE_LOOP('',(#35404,#35405,#35406,#35407,#35408,#35409));
#8229=EDGE_LOOP('',(#35410,#35411,#35412,#35413));
#8230=EDGE_LOOP('',(#35414,#35415,#35416,#35417));
#8231=EDGE_LOOP('',(#35418,#35419,#35420,#35421,#35422,#35423));
#8232=EDGE_LOOP('',(#35424,#35425,#35426,#35427));
#8233=EDGE_LOOP('',(#35428,#35429,#35430,#35431));
#8234=EDGE_LOOP('',(#35432,#35433,#35434,#35435,#35436,#35437));
#8235=EDGE_LOOP('',(#35438,#35439,#35440,#35441));
#8236=EDGE_LOOP('',(#35442,#35443,#35444,#35445));
#8237=EDGE_LOOP('',(#35446,#35447,#35448,#35449,#35450,#35451));
#8238=EDGE_LOOP('',(#35452,#35453,#35454,#35455));
#8239=EDGE_LOOP('',(#35456,#35457,#35458));
#8240=EDGE_LOOP('',(#35459,#35460,#35461,#35462,#35463,#35464));
#8241=EDGE_LOOP('',(#35465,#35466,#35467,#35468));
#8242=EDGE_LOOP('',(#35469,#35470,#35471,#35472));
#8243=EDGE_LOOP('',(#35473,#35474,#35475,#35476,#35477,#35478));
#8244=EDGE_LOOP('',(#35479,#35480,#35481,#35482,#35483,#35484));
#8245=EDGE_LOOP('',(#35485,#35486,#35487,#35488));
#8246=EDGE_LOOP('',(#35489,#35490,#35491,#35492));
#8247=EDGE_LOOP('',(#35493,#35494,#35495));
#8248=EDGE_LOOP('',(#35496,#35497,#35498,#35499));
#8249=EDGE_LOOP('',(#35500,#35501,#35502,#35503));
#8250=EDGE_LOOP('',(#35504,#35505,#35506,#35507));
#8251=EDGE_LOOP('',(#35508,#35509,#35510,#35511,#35512,#35513));
#8252=EDGE_LOOP('',(#35514,#35515,#35516,#35517));
#8253=EDGE_LOOP('',(#35518,#35519,#35520,#35521));
#8254=EDGE_LOOP('',(#35522,#35523,#35524,#35525,#35526,#35527));
#8255=EDGE_LOOP('',(#35528,#35529,#35530,#35531));
#8256=EDGE_LOOP('',(#35532,#35533,#35534,#35535));
#8257=EDGE_LOOP('',(#35536,#35537,#35538,#35539,#35540,#35541));
#8258=EDGE_LOOP('',(#35542,#35543,#35544,#35545));
#8259=EDGE_LOOP('',(#35546,#35547,#35548,#35549));
#8260=EDGE_LOOP('',(#35550,#35551,#35552,#35553,#35554,#35555));
#8261=EDGE_LOOP('',(#35556,#35557,#35558,#35559));
#8262=EDGE_LOOP('',(#35560,#35561,#35562));
#8263=EDGE_LOOP('',(#35563,#35564,#35565,#35566,#35567,#35568));
#8264=EDGE_LOOP('',(#35569,#35570,#35571,#35572));
#8265=EDGE_LOOP('',(#35573,#35574,#35575,#35576));
#8266=EDGE_LOOP('',(#35577,#35578,#35579,#35580,#35581,#35582));
#8267=EDGE_LOOP('',(#35583,#35584,#35585,#35586,#35587,#35588));
#8268=EDGE_LOOP('',(#35589,#35590,#35591,#35592));
#8269=EDGE_LOOP('',(#35593,#35594,#35595,#35596));
#8270=EDGE_LOOP('',(#35597,#35598,#35599));
#8271=EDGE_LOOP('',(#35600,#35601,#35602,#35603));
#8272=EDGE_LOOP('',(#35604,#35605,#35606,#35607));
#8273=EDGE_LOOP('',(#35608,#35609,#35610,#35611));
#8274=EDGE_LOOP('',(#35612,#35613,#35614,#35615,#35616,#35617));
#8275=EDGE_LOOP('',(#35618,#35619,#35620,#35621));
#8276=EDGE_LOOP('',(#35622,#35623,#35624,#35625));
#8277=EDGE_LOOP('',(#35626,#35627,#35628,#35629,#35630,#35631));
#8278=EDGE_LOOP('',(#35632,#35633,#35634,#35635));
#8279=EDGE_LOOP('',(#35636,#35637,#35638,#35639));
#8280=EDGE_LOOP('',(#35640,#35641,#35642,#35643,#35644,#35645));
#8281=EDGE_LOOP('',(#35646,#35647,#35648,#35649));
#8282=EDGE_LOOP('',(#35650,#35651,#35652,#35653));
#8283=EDGE_LOOP('',(#35654,#35655,#35656,#35657,#35658,#35659));
#8284=EDGE_LOOP('',(#35660,#35661,#35662,#35663));
#8285=EDGE_LOOP('',(#35664,#35665,#35666,#35667,#35668,#35669));
#8286=EDGE_LOOP('',(#35670,#35671,#35672));
#8287=EDGE_LOOP('',(#35673,#35674,#35675,#35676));
#8288=EDGE_LOOP('',(#35677,#35678,#35679,#35680));
#8289=EDGE_LOOP('',(#35681,#35682,#35683,#35684,#35685,#35686));
#8290=EDGE_LOOP('',(#35687,#35688,#35689,#35690,#35691,#35692));
#8291=EDGE_LOOP('',(#35693,#35694,#35695,#35696));
#8292=EDGE_LOOP('',(#35697,#35698,#35699,#35700));
#8293=EDGE_LOOP('',(#35701,#35702,#35703));
#8294=EDGE_LOOP('',(#35704,#35705,#35706,#35707));
#8295=EDGE_LOOP('',(#35708,#35709,#35710,#35711));
#8296=EDGE_LOOP('',(#35712,#35713,#35714,#35715));
#8297=EDGE_LOOP('',(#35716,#35717,#35718,#35719,#35720,#35721));
#8298=EDGE_LOOP('',(#35722,#35723,#35724,#35725));
#8299=EDGE_LOOP('',(#35726,#35727,#35728,#35729));
#8300=EDGE_LOOP('',(#35730,#35731,#35732,#35733,#35734,#35735));
#8301=EDGE_LOOP('',(#35736,#35737,#35738,#35739));
#8302=EDGE_LOOP('',(#35740,#35741,#35742,#35743));
#8303=EDGE_LOOP('',(#35744,#35745,#35746,#35747,#35748,#35749));
#8304=EDGE_LOOP('',(#35750,#35751,#35752,#35753));
#8305=EDGE_LOOP('',(#35754,#35755,#35756,#35757));
#8306=EDGE_LOOP('',(#35758,#35759,#35760,#35761,#35762,#35763));
#8307=EDGE_LOOP('',(#35764,#35765,#35766,#35767));
#8308=EDGE_LOOP('',(#35768,#35769,#35770,#35771));
#8309=EDGE_LOOP('',(#35772,#35773,#35774,#35775,#35776,#35777));
#8310=EDGE_LOOP('',(#35778,#35779,#35780,#35781));
#8311=EDGE_LOOP('',(#35782,#35783,#35784,#35785));
#8312=EDGE_LOOP('',(#35786,#35787,#35788,#35789,#35790,#35791));
#8313=EDGE_LOOP('',(#35792,#35793,#35794,#35795,#35796,#35797));
#8314=EDGE_LOOP('',(#35798,#35799,#35800,#35801));
#8315=EDGE_LOOP('',(#35802,#35803,#35804));
#8316=EDGE_LOOP('',(#35805,#35806,#35807));
#8317=EDGE_LOOP('',(#35808,#35809,#35810,#35811));
#8318=EDGE_LOOP('',(#35812,#35813,#35814,#35815));
#8319=EDGE_LOOP('',(#35816,#35817,#35818,#35819));
#8320=EDGE_LOOP('',(#35820,#35821,#35822,#35823,#35824,#35825));
#8321=EDGE_LOOP('',(#35826,#35827,#35828,#35829));
#8322=EDGE_LOOP('',(#35830,#35831,#35832,#35833));
#8323=EDGE_LOOP('',(#35834,#35835,#35836,#35837,#35838,#35839));
#8324=EDGE_LOOP('',(#35840,#35841,#35842,#35843));
#8325=EDGE_LOOP('',(#35844,#35845,#35846,#35847));
#8326=EDGE_LOOP('',(#35848,#35849,#35850,#35851,#35852,#35853));
#8327=EDGE_LOOP('',(#35854,#35855,#35856,#35857));
#8328=EDGE_LOOP('',(#35858,#35859,#35860,#35861));
#8329=EDGE_LOOP('',(#35862,#35863,#35864,#35865,#35866,#35867));
#8330=EDGE_LOOP('',(#35868,#35869,#35870,#35871));
#8331=EDGE_LOOP('',(#35872,#35873,#35874,#35875));
#8332=EDGE_LOOP('',(#35876,#35877,#35878,#35879,#35880,#35881));
#8333=EDGE_LOOP('',(#35882,#35883,#35884,#35885));
#8334=EDGE_LOOP('',(#35886,#35887,#35888,#35889));
#8335=EDGE_LOOP('',(#35890,#35891,#35892,#35893,#35894,#35895));
#8336=EDGE_LOOP('',(#35896,#35897,#35898,#35899,#35900,#35901));
#8337=EDGE_LOOP('',(#35902,#35903,#35904,#35905));
#8338=EDGE_LOOP('',(#35906,#35907,#35908));
#8339=EDGE_LOOP('',(#35909,#35910,#35911));
#8340=EDGE_LOOP('',(#35912,#35913,#35914,#35915));
#8341=EDGE_LOOP('',(#35916,#35917,#35918,#35919));
#8342=EDGE_LOOP('',(#35920,#35921,#35922,#35923));
#8343=EDGE_LOOP('',(#35924,#35925,#35926,#35927,#35928,#35929));
#8344=EDGE_LOOP('',(#35930,#35931,#35932,#35933));
#8345=EDGE_LOOP('',(#35934,#35935,#35936,#35937));
#8346=EDGE_LOOP('',(#35938,#35939,#35940,#35941,#35942,#35943));
#8347=EDGE_LOOP('',(#35944,#35945,#35946,#35947));
#8348=EDGE_LOOP('',(#35948,#35949,#35950,#35951));
#8349=EDGE_LOOP('',(#35952,#35953,#35954,#35955,#35956,#35957));
#8350=EDGE_LOOP('',(#35958,#35959,#35960,#35961));
#8351=EDGE_LOOP('',(#35962,#35963,#35964,#35965));
#8352=EDGE_LOOP('',(#35966,#35967,#35968,#35969,#35970,#35971));
#8353=EDGE_LOOP('',(#35972,#35973,#35974,#35975));
#8354=EDGE_LOOP('',(#35976,#35977,#35978,#35979));
#8355=EDGE_LOOP('',(#35980,#35981,#35982,#35983,#35984,#35985));
#8356=EDGE_LOOP('',(#35986,#35987,#35988,#35989));
#8357=EDGE_LOOP('',(#35990,#35991,#35992,#35993));
#8358=EDGE_LOOP('',(#35994,#35995,#35996,#35997,#35998,#35999));
#8359=EDGE_LOOP('',(#36000,#36001,#36002,#36003,#36004,#36005));
#8360=EDGE_LOOP('',(#36006,#36007,#36008,#36009));
#8361=EDGE_LOOP('',(#36010,#36011,#36012));
#8362=EDGE_LOOP('',(#36013,#36014,#36015));
#8363=EDGE_LOOP('',(#36016,#36017,#36018,#36019));
#8364=EDGE_LOOP('',(#36020,#36021,#36022,#36023));
#8365=EDGE_LOOP('',(#36024,#36025,#36026,#36027));
#8366=EDGE_LOOP('',(#36028,#36029,#36030,#36031,#36032,#36033));
#8367=EDGE_LOOP('',(#36034,#36035,#36036,#36037));
#8368=EDGE_LOOP('',(#36038,#36039,#36040,#36041));
#8369=EDGE_LOOP('',(#36042,#36043,#36044,#36045,#36046,#36047));
#8370=EDGE_LOOP('',(#36048,#36049,#36050,#36051));
#8371=EDGE_LOOP('',(#36052,#36053,#36054,#36055));
#8372=EDGE_LOOP('',(#36056,#36057,#36058,#36059,#36060,#36061));
#8373=EDGE_LOOP('',(#36062,#36063,#36064,#36065));
#8374=EDGE_LOOP('',(#36066,#36067,#36068,#36069));
#8375=EDGE_LOOP('',(#36070,#36071,#36072,#36073,#36074,#36075));
#8376=EDGE_LOOP('',(#36076,#36077,#36078,#36079));
#8377=EDGE_LOOP('',(#36080,#36081,#36082,#36083));
#8378=EDGE_LOOP('',(#36084,#36085,#36086,#36087,#36088,#36089));
#8379=EDGE_LOOP('',(#36090,#36091,#36092,#36093));
#8380=EDGE_LOOP('',(#36094,#36095,#36096,#36097));
#8381=EDGE_LOOP('',(#36098,#36099,#36100,#36101,#36102,#36103));
#8382=EDGE_LOOP('',(#36104,#36105,#36106,#36107,#36108,#36109));
#8383=EDGE_LOOP('',(#36110,#36111,#36112,#36113));
#8384=EDGE_LOOP('',(#36114,#36115,#36116));
#8385=EDGE_LOOP('',(#36117,#36118,#36119));
#8386=EDGE_LOOP('',(#36120,#36121,#36122,#36123));
#8387=EDGE_LOOP('',(#36124,#36125,#36126,#36127));
#8388=EDGE_LOOP('',(#36128,#36129,#36130,#36131));
#8389=EDGE_LOOP('',(#36132,#36133,#36134,#36135,#36136,#36137));
#8390=EDGE_LOOP('',(#36138,#36139,#36140,#36141));
#8391=EDGE_LOOP('',(#36142,#36143,#36144,#36145));
#8392=EDGE_LOOP('',(#36146,#36147,#36148,#36149,#36150,#36151));
#8393=EDGE_LOOP('',(#36152,#36153,#36154,#36155));
#8394=EDGE_LOOP('',(#36156,#36157,#36158,#36159));
#8395=EDGE_LOOP('',(#36160,#36161,#36162,#36163,#36164,#36165));
#8396=EDGE_LOOP('',(#36166,#36167,#36168,#36169));
#8397=EDGE_LOOP('',(#36170,#36171,#36172,#36173));
#8398=EDGE_LOOP('',(#36174,#36175,#36176,#36177,#36178,#36179));
#8399=EDGE_LOOP('',(#36180,#36181,#36182,#36183));
#8400=EDGE_LOOP('',(#36184,#36185,#36186,#36187));
#8401=EDGE_LOOP('',(#36188,#36189,#36190,#36191,#36192,#36193));
#8402=EDGE_LOOP('',(#36194,#36195,#36196,#36197));
#8403=EDGE_LOOP('',(#36198,#36199,#36200,#36201));
#8404=EDGE_LOOP('',(#36202,#36203,#36204,#36205,#36206,#36207));
#8405=EDGE_LOOP('',(#36208,#36209,#36210,#36211,#36212,#36213));
#8406=EDGE_LOOP('',(#36214,#36215,#36216,#36217));
#8407=EDGE_LOOP('',(#36218,#36219,#36220));
#8408=EDGE_LOOP('',(#36221,#36222,#36223));
#8409=EDGE_LOOP('',(#36224,#36225,#36226,#36227));
#8410=EDGE_LOOP('',(#36228,#36229,#36230,#36231));
#8411=EDGE_LOOP('',(#36232,#36233,#36234,#36235));
#8412=EDGE_LOOP('',(#36236,#36237,#36238,#36239,#36240,#36241));
#8413=EDGE_LOOP('',(#36242,#36243,#36244,#36245));
#8414=EDGE_LOOP('',(#36246,#36247,#36248,#36249));
#8415=EDGE_LOOP('',(#36250,#36251,#36252,#36253,#36254,#36255));
#8416=EDGE_LOOP('',(#36256,#36257,#36258,#36259));
#8417=EDGE_LOOP('',(#36260,#36261,#36262,#36263));
#8418=EDGE_LOOP('',(#36264,#36265,#36266,#36267,#36268,#36269));
#8419=EDGE_LOOP('',(#36270,#36271,#36272,#36273));
#8420=EDGE_LOOP('',(#36274,#36275,#36276,#36277));
#8421=EDGE_LOOP('',(#36278,#36279,#36280,#36281,#36282,#36283));
#8422=EDGE_LOOP('',(#36284,#36285,#36286,#36287));
#8423=EDGE_LOOP('',(#36288,#36289,#36290,#36291));
#8424=EDGE_LOOP('',(#36292,#36293,#36294,#36295,#36296,#36297));
#8425=EDGE_LOOP('',(#36298,#36299,#36300,#36301));
#8426=EDGE_LOOP('',(#36302,#36303,#36304,#36305));
#8427=EDGE_LOOP('',(#36306,#36307,#36308,#36309,#36310,#36311));
#8428=EDGE_LOOP('',(#36312,#36313,#36314,#36315,#36316,#36317));
#8429=EDGE_LOOP('',(#36318,#36319,#36320,#36321));
#8430=EDGE_LOOP('',(#36322,#36323,#36324));
#8431=EDGE_LOOP('',(#36325,#36326,#36327));
#8432=EDGE_LOOP('',(#36328,#36329,#36330,#36331));
#8433=EDGE_LOOP('',(#36332,#36333,#36334,#36335));
#8434=EDGE_LOOP('',(#36336,#36337,#36338,#36339));
#8435=EDGE_LOOP('',(#36340,#36341,#36342,#36343,#36344,#36345));
#8436=EDGE_LOOP('',(#36346,#36347,#36348,#36349));
#8437=EDGE_LOOP('',(#36350,#36351,#36352,#36353));
#8438=EDGE_LOOP('',(#36354,#36355,#36356,#36357,#36358,#36359));
#8439=EDGE_LOOP('',(#36360,#36361,#36362,#36363));
#8440=EDGE_LOOP('',(#36364,#36365,#36366,#36367));
#8441=EDGE_LOOP('',(#36368,#36369,#36370,#36371,#36372,#36373));
#8442=EDGE_LOOP('',(#36374,#36375,#36376,#36377));
#8443=EDGE_LOOP('',(#36378,#36379,#36380,#36381));
#8444=EDGE_LOOP('',(#36382,#36383,#36384,#36385,#36386,#36387));
#8445=EDGE_LOOP('',(#36388,#36389,#36390,#36391));
#8446=EDGE_LOOP('',(#36392,#36393,#36394,#36395));
#8447=EDGE_LOOP('',(#36396,#36397,#36398,#36399,#36400,#36401));
#8448=EDGE_LOOP('',(#36402,#36403,#36404,#36405));
#8449=EDGE_LOOP('',(#36406,#36407,#36408,#36409));
#8450=EDGE_LOOP('',(#36410,#36411,#36412,#36413,#36414,#36415));
#8451=EDGE_LOOP('',(#36416,#36417,#36418,#36419,#36420,#36421));
#8452=EDGE_LOOP('',(#36422,#36423,#36424,#36425));
#8453=EDGE_LOOP('',(#36426,#36427,#36428));
#8454=EDGE_LOOP('',(#36429,#36430,#36431));
#8455=EDGE_LOOP('',(#36432,#36433,#36434,#36435));
#8456=EDGE_LOOP('',(#36436,#36437,#36438,#36439));
#8457=EDGE_LOOP('',(#36440,#36441,#36442,#36443));
#8458=EDGE_LOOP('',(#36444,#36445,#36446,#36447,#36448,#36449));
#8459=EDGE_LOOP('',(#36450,#36451,#36452,#36453));
#8460=EDGE_LOOP('',(#36454,#36455,#36456,#36457));
#8461=EDGE_LOOP('',(#36458,#36459,#36460,#36461,#36462,#36463));
#8462=EDGE_LOOP('',(#36464,#36465,#36466,#36467));
#8463=EDGE_LOOP('',(#36468,#36469,#36470,#36471));
#8464=EDGE_LOOP('',(#36472,#36473,#36474,#36475,#36476,#36477));
#8465=EDGE_LOOP('',(#36478,#36479,#36480,#36481));
#8466=EDGE_LOOP('',(#36482,#36483,#36484,#36485));
#8467=EDGE_LOOP('',(#36486,#36487,#36488,#36489,#36490,#36491));
#8468=EDGE_LOOP('',(#36492,#36493,#36494,#36495));
#8469=EDGE_LOOP('',(#36496,#36497,#36498,#36499));
#8470=EDGE_LOOP('',(#36500,#36501,#36502,#36503,#36504,#36505));
#8471=EDGE_LOOP('',(#36506,#36507,#36508,#36509));
#8472=EDGE_LOOP('',(#36510,#36511,#36512,#36513));
#8473=EDGE_LOOP('',(#36514,#36515,#36516,#36517,#36518,#36519));
#8474=EDGE_LOOP('',(#36520,#36521,#36522,#36523,#36524,#36525));
#8475=EDGE_LOOP('',(#36526,#36527,#36528,#36529));
#8476=EDGE_LOOP('',(#36530,#36531,#36532));
#8477=EDGE_LOOP('',(#36533,#36534,#36535));
#8478=EDGE_LOOP('',(#36536,#36537,#36538,#36539));
#8479=EDGE_LOOP('',(#36540,#36541,#36542,#36543));
#8480=EDGE_LOOP('',(#36544,#36545,#36546,#36547));
#8481=EDGE_LOOP('',(#36548,#36549,#36550,#36551,#36552,#36553));
#8482=EDGE_LOOP('',(#36554,#36555,#36556,#36557));
#8483=EDGE_LOOP('',(#36558,#36559,#36560,#36561));
#8484=EDGE_LOOP('',(#36562,#36563,#36564,#36565,#36566,#36567));
#8485=EDGE_LOOP('',(#36568,#36569,#36570,#36571));
#8486=EDGE_LOOP('',(#36572,#36573,#36574,#36575));
#8487=EDGE_LOOP('',(#36576,#36577,#36578,#36579,#36580,#36581));
#8488=EDGE_LOOP('',(#36582,#36583,#36584,#36585));
#8489=EDGE_LOOP('',(#36586,#36587,#36588,#36589));
#8490=EDGE_LOOP('',(#36590,#36591,#36592,#36593,#36594,#36595));
#8491=EDGE_LOOP('',(#36596,#36597,#36598,#36599));
#8492=EDGE_LOOP('',(#36600,#36601,#36602,#36603));
#8493=EDGE_LOOP('',(#36604,#36605,#36606,#36607,#36608,#36609));
#8494=EDGE_LOOP('',(#36610,#36611,#36612,#36613));
#8495=EDGE_LOOP('',(#36614,#36615,#36616,#36617));
#8496=EDGE_LOOP('',(#36618,#36619,#36620,#36621,#36622,#36623));
#8497=EDGE_LOOP('',(#36624,#36625,#36626,#36627,#36628,#36629));
#8498=EDGE_LOOP('',(#36630,#36631,#36632,#36633));
#8499=EDGE_LOOP('',(#36634,#36635,#36636));
#8500=EDGE_LOOP('',(#36637,#36638,#36639));
#8501=EDGE_LOOP('',(#36640,#36641,#36642,#36643));
#8502=EDGE_LOOP('',(#36644,#36645,#36646,#36647));
#8503=EDGE_LOOP('',(#36648,#36649,#36650,#36651));
#8504=EDGE_LOOP('',(#36652,#36653,#36654,#36655,#36656,#36657));
#8505=EDGE_LOOP('',(#36658,#36659,#36660,#36661));
#8506=EDGE_LOOP('',(#36662,#36663,#36664,#36665));
#8507=EDGE_LOOP('',(#36666,#36667,#36668,#36669,#36670,#36671));
#8508=EDGE_LOOP('',(#36672,#36673,#36674,#36675));
#8509=EDGE_LOOP('',(#36676,#36677,#36678,#36679));
#8510=EDGE_LOOP('',(#36680,#36681,#36682,#36683,#36684,#36685));
#8511=EDGE_LOOP('',(#36686,#36687,#36688,#36689));
#8512=EDGE_LOOP('',(#36690,#36691,#36692,#36693));
#8513=EDGE_LOOP('',(#36694,#36695,#36696,#36697,#36698,#36699));
#8514=EDGE_LOOP('',(#36700,#36701,#36702,#36703));
#8515=EDGE_LOOP('',(#36704,#36705,#36706,#36707));
#8516=EDGE_LOOP('',(#36708,#36709,#36710,#36711,#36712,#36713));
#8517=EDGE_LOOP('',(#36714,#36715,#36716,#36717));
#8518=EDGE_LOOP('',(#36718,#36719,#36720,#36721));
#8519=EDGE_LOOP('',(#36722,#36723,#36724,#36725,#36726,#36727));
#8520=EDGE_LOOP('',(#36728,#36729,#36730,#36731,#36732,#36733));
#8521=EDGE_LOOP('',(#36734,#36735,#36736,#36737));
#8522=EDGE_LOOP('',(#36738,#36739,#36740));
#8523=EDGE_LOOP('',(#36741,#36742,#36743));
#8524=EDGE_LOOP('',(#36744,#36745,#36746,#36747));
#8525=EDGE_LOOP('',(#36748,#36749,#36750,#36751));
#8526=EDGE_LOOP('',(#36752,#36753,#36754,#36755));
#8527=EDGE_LOOP('',(#36756,#36757,#36758,#36759,#36760,#36761));
#8528=EDGE_LOOP('',(#36762,#36763,#36764,#36765));
#8529=EDGE_LOOP('',(#36766,#36767,#36768,#36769));
#8530=EDGE_LOOP('',(#36770,#36771,#36772,#36773,#36774,#36775));
#8531=EDGE_LOOP('',(#36776,#36777,#36778,#36779));
#8532=EDGE_LOOP('',(#36780,#36781,#36782,#36783));
#8533=EDGE_LOOP('',(#36784,#36785,#36786,#36787,#36788,#36789));
#8534=EDGE_LOOP('',(#36790,#36791,#36792,#36793));
#8535=EDGE_LOOP('',(#36794,#36795,#36796,#36797));
#8536=EDGE_LOOP('',(#36798,#36799,#36800,#36801,#36802,#36803));
#8537=EDGE_LOOP('',(#36804,#36805,#36806,#36807));
#8538=EDGE_LOOP('',(#36808,#36809,#36810,#36811));
#8539=EDGE_LOOP('',(#36812,#36813,#36814,#36815,#36816,#36817));
#8540=EDGE_LOOP('',(#36818,#36819,#36820,#36821));
#8541=EDGE_LOOP('',(#36822,#36823,#36824,#36825));
#8542=EDGE_LOOP('',(#36826,#36827,#36828,#36829,#36830,#36831));
#8543=EDGE_LOOP('',(#36832,#36833,#36834,#36835,#36836,#36837));
#8544=EDGE_LOOP('',(#36838,#36839,#36840,#36841));
#8545=EDGE_LOOP('',(#36842,#36843,#36844));
#8546=EDGE_LOOP('',(#36845,#36846,#36847));
#8547=EDGE_LOOP('',(#36848,#36849,#36850,#36851));
#8548=EDGE_LOOP('',(#36852,#36853,#36854,#36855));
#8549=EDGE_LOOP('',(#36856,#36857,#36858,#36859));
#8550=EDGE_LOOP('',(#36860,#36861,#36862,#36863,#36864,#36865));
#8551=EDGE_LOOP('',(#36866,#36867,#36868,#36869));
#8552=EDGE_LOOP('',(#36870,#36871,#36872,#36873));
#8553=EDGE_LOOP('',(#36874,#36875,#36876,#36877,#36878,#36879));
#8554=EDGE_LOOP('',(#36880,#36881,#36882,#36883));
#8555=EDGE_LOOP('',(#36884,#36885,#36886,#36887));
#8556=EDGE_LOOP('',(#36888,#36889,#36890,#36891,#36892,#36893));
#8557=EDGE_LOOP('',(#36894,#36895,#36896,#36897));
#8558=EDGE_LOOP('',(#36898,#36899,#36900,#36901));
#8559=EDGE_LOOP('',(#36902,#36903,#36904,#36905,#36906,#36907));
#8560=EDGE_LOOP('',(#36908,#36909,#36910,#36911));
#8561=EDGE_LOOP('',(#36912,#36913,#36914,#36915));
#8562=EDGE_LOOP('',(#36916,#36917,#36918,#36919,#36920,#36921));
#8563=EDGE_LOOP('',(#36922,#36923,#36924,#36925));
#8564=EDGE_LOOP('',(#36926,#36927,#36928,#36929));
#8565=EDGE_LOOP('',(#36930,#36931,#36932,#36933,#36934,#36935));
#8566=EDGE_LOOP('',(#36936,#36937,#36938,#36939,#36940,#36941));
#8567=EDGE_LOOP('',(#36942,#36943,#36944,#36945));
#8568=EDGE_LOOP('',(#36946,#36947,#36948));
#8569=EDGE_LOOP('',(#36949,#36950,#36951));
#8570=EDGE_LOOP('',(#36952,#36953,#36954,#36955));
#8571=EDGE_LOOP('',(#36956,#36957,#36958,#36959));
#8572=EDGE_LOOP('',(#36960,#36961,#36962,#36963));
#8573=EDGE_LOOP('',(#36964,#36965,#36966,#36967,#36968,#36969));
#8574=EDGE_LOOP('',(#36970,#36971,#36972,#36973));
#8575=EDGE_LOOP('',(#36974,#36975,#36976,#36977));
#8576=EDGE_LOOP('',(#36978,#36979,#36980,#36981,#36982,#36983));
#8577=EDGE_LOOP('',(#36984,#36985,#36986,#36987));
#8578=EDGE_LOOP('',(#36988,#36989,#36990,#36991));
#8579=EDGE_LOOP('',(#36992,#36993,#36994,#36995,#36996,#36997));
#8580=EDGE_LOOP('',(#36998,#36999,#37000,#37001));
#8581=EDGE_LOOP('',(#37002,#37003,#37004,#37005));
#8582=EDGE_LOOP('',(#37006,#37007,#37008,#37009,#37010,#37011));
#8583=EDGE_LOOP('',(#37012,#37013,#37014,#37015));
#8584=EDGE_LOOP('',(#37016,#37017,#37018,#37019));
#8585=EDGE_LOOP('',(#37020,#37021,#37022,#37023,#37024,#37025));
#8586=EDGE_LOOP('',(#37026,#37027,#37028,#37029));
#8587=EDGE_LOOP('',(#37030,#37031,#37032,#37033));
#8588=EDGE_LOOP('',(#37034,#37035,#37036,#37037,#37038,#37039));
#8589=EDGE_LOOP('',(#37040,#37041,#37042,#37043,#37044,#37045));
#8590=EDGE_LOOP('',(#37046,#37047,#37048,#37049));
#8591=EDGE_LOOP('',(#37050,#37051,#37052));
#8592=EDGE_LOOP('',(#37053,#37054,#37055));
#8593=EDGE_LOOP('',(#37056,#37057,#37058,#37059));
#8594=EDGE_LOOP('',(#37060,#37061,#37062,#37063));
#8595=EDGE_LOOP('',(#37064,#37065,#37066,#37067));
#8596=EDGE_LOOP('',(#37068,#37069,#37070,#37071,#37072,#37073));
#8597=EDGE_LOOP('',(#37074,#37075,#37076,#37077));
#8598=EDGE_LOOP('',(#37078,#37079,#37080,#37081));
#8599=EDGE_LOOP('',(#37082,#37083,#37084,#37085,#37086,#37087));
#8600=EDGE_LOOP('',(#37088,#37089,#37090,#37091));
#8601=EDGE_LOOP('',(#37092,#37093,#37094,#37095));
#8602=EDGE_LOOP('',(#37096,#37097,#37098,#37099,#37100,#37101));
#8603=EDGE_LOOP('',(#37102,#37103,#37104,#37105));
#8604=EDGE_LOOP('',(#37106,#37107,#37108,#37109));
#8605=EDGE_LOOP('',(#37110,#37111,#37112,#37113,#37114,#37115));
#8606=EDGE_LOOP('',(#37116,#37117,#37118,#37119));
#8607=EDGE_LOOP('',(#37120,#37121,#37122,#37123));
#8608=EDGE_LOOP('',(#37124,#37125,#37126,#37127,#37128,#37129));
#8609=EDGE_LOOP('',(#37130,#37131,#37132,#37133));
#8610=EDGE_LOOP('',(#37134,#37135,#37136,#37137));
#8611=EDGE_LOOP('',(#37138,#37139,#37140,#37141,#37142,#37143));
#8612=EDGE_LOOP('',(#37144,#37145,#37146,#37147,#37148,#37149));
#8613=EDGE_LOOP('',(#37150,#37151,#37152,#37153));
#8614=EDGE_LOOP('',(#37154,#37155,#37156));
#8615=EDGE_LOOP('',(#37157,#37158,#37159));
#8616=EDGE_LOOP('',(#37160,#37161,#37162,#37163));
#8617=EDGE_LOOP('',(#37164,#37165,#37166,#37167));
#8618=EDGE_LOOP('',(#37168,#37169,#37170,#37171));
#8619=EDGE_LOOP('',(#37172,#37173,#37174,#37175,#37176,#37177));
#8620=EDGE_LOOP('',(#37178,#37179,#37180,#37181));
#8621=EDGE_LOOP('',(#37182,#37183,#37184,#37185));
#8622=EDGE_LOOP('',(#37186,#37187,#37188,#37189,#37190,#37191));
#8623=EDGE_LOOP('',(#37192,#37193,#37194,#37195));
#8624=EDGE_LOOP('',(#37196,#37197,#37198,#37199));
#8625=EDGE_LOOP('',(#37200,#37201,#37202,#37203,#37204,#37205));
#8626=EDGE_LOOP('',(#37206,#37207,#37208,#37209));
#8627=EDGE_LOOP('',(#37210,#37211,#37212,#37213));
#8628=EDGE_LOOP('',(#37214,#37215,#37216,#37217,#37218,#37219));
#8629=EDGE_LOOP('',(#37220,#37221,#37222,#37223));
#8630=EDGE_LOOP('',(#37224,#37225,#37226,#37227));
#8631=EDGE_LOOP('',(#37228,#37229,#37230,#37231,#37232,#37233));
#8632=EDGE_LOOP('',(#37234,#37235,#37236,#37237));
#8633=EDGE_LOOP('',(#37238,#37239,#37240,#37241));
#8634=EDGE_LOOP('',(#37242,#37243,#37244,#37245,#37246,#37247));
#8635=EDGE_LOOP('',(#37248,#37249,#37250,#37251,#37252,#37253));
#8636=EDGE_LOOP('',(#37254,#37255,#37256,#37257));
#8637=EDGE_LOOP('',(#37258,#37259,#37260));
#8638=EDGE_LOOP('',(#37261,#37262,#37263));
#8639=EDGE_LOOP('',(#37264,#37265,#37266,#37267));
#8640=EDGE_LOOP('',(#37268,#37269,#37270,#37271));
#8641=EDGE_LOOP('',(#37272,#37273,#37274,#37275));
#8642=EDGE_LOOP('',(#37276,#37277,#37278,#37279,#37280,#37281));
#8643=EDGE_LOOP('',(#37282,#37283,#37284,#37285));
#8644=EDGE_LOOP('',(#37286,#37287,#37288,#37289));
#8645=EDGE_LOOP('',(#37290,#37291,#37292,#37293,#37294,#37295));
#8646=EDGE_LOOP('',(#37296,#37297,#37298,#37299));
#8647=EDGE_LOOP('',(#37300,#37301,#37302,#37303));
#8648=EDGE_LOOP('',(#37304,#37305,#37306,#37307,#37308,#37309));
#8649=EDGE_LOOP('',(#37310,#37311,#37312,#37313));
#8650=EDGE_LOOP('',(#37314,#37315,#37316,#37317));
#8651=EDGE_LOOP('',(#37318,#37319,#37320,#37321,#37322,#37323));
#8652=EDGE_LOOP('',(#37324,#37325,#37326,#37327));
#8653=EDGE_LOOP('',(#37328,#37329,#37330,#37331));
#8654=EDGE_LOOP('',(#37332,#37333,#37334,#37335,#37336,#37337));
#8655=EDGE_LOOP('',(#37338,#37339,#37340,#37341));
#8656=EDGE_LOOP('',(#37342,#37343,#37344,#37345));
#8657=EDGE_LOOP('',(#37346,#37347,#37348,#37349,#37350,#37351));
#8658=EDGE_LOOP('',(#37352,#37353,#37354,#37355,#37356,#37357));
#8659=EDGE_LOOP('',(#37358,#37359,#37360,#37361));
#8660=EDGE_LOOP('',(#37362,#37363,#37364));
#8661=EDGE_LOOP('',(#37365,#37366,#37367));
#8662=EDGE_LOOP('',(#37368,#37369,#37370,#37371));
#8663=EDGE_LOOP('',(#37372,#37373,#37374,#37375));
#8664=EDGE_LOOP('',(#37376,#37377,#37378,#37379));
#8665=EDGE_LOOP('',(#37380,#37381,#37382,#37383,#37384,#37385));
#8666=EDGE_LOOP('',(#37386,#37387,#37388,#37389));
#8667=EDGE_LOOP('',(#37390,#37391,#37392,#37393));
#8668=EDGE_LOOP('',(#37394,#37395,#37396,#37397,#37398,#37399));
#8669=EDGE_LOOP('',(#37400,#37401,#37402,#37403));
#8670=EDGE_LOOP('',(#37404,#37405,#37406,#37407));
#8671=EDGE_LOOP('',(#37408,#37409,#37410,#37411,#37412,#37413));
#8672=EDGE_LOOP('',(#37414,#37415,#37416,#37417));
#8673=EDGE_LOOP('',(#37418,#37419,#37420,#37421));
#8674=EDGE_LOOP('',(#37422,#37423,#37424,#37425,#37426,#37427));
#8675=EDGE_LOOP('',(#37428,#37429,#37430,#37431));
#8676=EDGE_LOOP('',(#37432,#37433,#37434,#37435));
#8677=EDGE_LOOP('',(#37436,#37437,#37438,#37439,#37440,#37441));
#8678=EDGE_LOOP('',(#37442,#37443,#37444,#37445));
#8679=EDGE_LOOP('',(#37446,#37447,#37448,#37449));
#8680=EDGE_LOOP('',(#37450,#37451,#37452,#37453,#37454,#37455));
#8681=EDGE_LOOP('',(#37456,#37457,#37458,#37459,#37460,#37461));
#8682=EDGE_LOOP('',(#37462,#37463,#37464,#37465));
#8683=EDGE_LOOP('',(#37466,#37467,#37468));
#8684=EDGE_LOOP('',(#37469,#37470,#37471));
#8685=EDGE_LOOP('',(#37472,#37473,#37474,#37475));
#8686=EDGE_LOOP('',(#37476,#37477,#37478,#37479));
#8687=EDGE_LOOP('',(#37480,#37481,#37482,#37483));
#8688=EDGE_LOOP('',(#37484,#37485,#37486,#37487,#37488,#37489));
#8689=EDGE_LOOP('',(#37490,#37491,#37492,#37493));
#8690=EDGE_LOOP('',(#37494,#37495,#37496,#37497));
#8691=EDGE_LOOP('',(#37498,#37499,#37500,#37501,#37502,#37503));
#8692=EDGE_LOOP('',(#37504,#37505,#37506,#37507));
#8693=EDGE_LOOP('',(#37508,#37509,#37510,#37511));
#8694=EDGE_LOOP('',(#37512,#37513,#37514,#37515,#37516,#37517));
#8695=EDGE_LOOP('',(#37518,#37519,#37520,#37521));
#8696=EDGE_LOOP('',(#37522,#37523,#37524,#37525));
#8697=EDGE_LOOP('',(#37526,#37527,#37528,#37529,#37530,#37531));
#8698=EDGE_LOOP('',(#37532,#37533,#37534,#37535));
#8699=EDGE_LOOP('',(#37536,#37537,#37538,#37539));
#8700=EDGE_LOOP('',(#37540,#37541,#37542,#37543,#37544,#37545));
#8701=EDGE_LOOP('',(#37546,#37547,#37548,#37549));
#8702=EDGE_LOOP('',(#37550,#37551,#37552,#37553));
#8703=EDGE_LOOP('',(#37554,#37555,#37556,#37557,#37558,#37559));
#8704=EDGE_LOOP('',(#37560,#37561,#37562,#37563,#37564,#37565));
#8705=EDGE_LOOP('',(#37566,#37567,#37568,#37569));
#8706=EDGE_LOOP('',(#37570,#37571,#37572));
#8707=EDGE_LOOP('',(#37573,#37574,#37575));
#8708=EDGE_LOOP('',(#37576,#37577,#37578,#37579));
#8709=EDGE_LOOP('',(#37580,#37581,#37582,#37583));
#8710=EDGE_LOOP('',(#37584,#37585,#37586,#37587,#37588));
#8711=EDGE_LOOP('',(#37589,#37590,#37591,#37592,#37593,#37594));
#8712=EDGE_LOOP('',(#37595,#37596,#37597,#37598));
#8713=EDGE_LOOP('',(#37599,#37600,#37601,#37602));
#8714=EDGE_LOOP('',(#37603,#37604,#37605,#37606,#37607,#37608));
#8715=EDGE_LOOP('',(#37609,#37610,#37611,#37612));
#8716=EDGE_LOOP('',(#37613,#37614,#37615,#37616));
#8717=EDGE_LOOP('',(#37617,#37618,#37619,#37620,#37621,#37622));
#8718=EDGE_LOOP('',(#37623,#37624,#37625,#37626));
#8719=EDGE_LOOP('',(#37627,#37628,#37629,#37630));
#8720=EDGE_LOOP('',(#37631,#37632,#37633,#37634,#37635,#37636));
#8721=EDGE_LOOP('',(#37637,#37638,#37639,#37640));
#8722=EDGE_LOOP('',(#37641,#37642,#37643,#37644));
#8723=EDGE_LOOP('',(#37645,#37646,#37647,#37648,#37649,#37650));
#8724=EDGE_LOOP('',(#37651,#37652,#37653,#37654));
#8725=EDGE_LOOP('',(#37655,#37656,#37657,#37658));
#8726=EDGE_LOOP('',(#37659,#37660,#37661,#37662,#37663,#37664));
#8727=EDGE_LOOP('',(#37665,#37666,#37667,#37668,#37669,#37670));
#8728=EDGE_LOOP('',(#37671,#37672,#37673,#37674));
#8729=EDGE_LOOP('',(#37675,#37676,#37677));
#8730=EDGE_LOOP('',(#37678,#37679,#37680));
#8731=EDGE_LOOP('',(#37681,#37682,#37683,#37684));
#8732=EDGE_LOOP('',(#37685,#37686,#37687,#37688));
#8733=EDGE_LOOP('',(#37689,#37690,#37691,#37692));
#8734=EDGE_LOOP('',(#37693,#37694,#37695,#37696,#37697,#37698));
#8735=EDGE_LOOP('',(#37699,#37700,#37701,#37702));
#8736=EDGE_LOOP('',(#37703,#37704,#37705,#37706));
#8737=EDGE_LOOP('',(#37707,#37708,#37709,#37710,#37711,#37712));
#8738=EDGE_LOOP('',(#37713,#37714,#37715,#37716));
#8739=EDGE_LOOP('',(#37717,#37718,#37719,#37720));
#8740=EDGE_LOOP('',(#37721,#37722,#37723,#37724,#37725,#37726));
#8741=EDGE_LOOP('',(#37727,#37728,#37729,#37730));
#8742=EDGE_LOOP('',(#37731,#37732,#37733,#37734));
#8743=EDGE_LOOP('',(#37735,#37736,#37737,#37738,#37739,#37740));
#8744=EDGE_LOOP('',(#37741,#37742,#37743,#37744));
#8745=EDGE_LOOP('',(#37745,#37746,#37747,#37748));
#8746=EDGE_LOOP('',(#37749,#37750,#37751,#37752,#37753,#37754));
#8747=EDGE_LOOP('',(#37755,#37756,#37757,#37758));
#8748=EDGE_LOOP('',(#37759,#37760,#37761,#37762));
#8749=EDGE_LOOP('',(#37763,#37764,#37765,#37766,#37767,#37768));
#8750=EDGE_LOOP('',(#37769,#37770,#37771,#37772,#37773,#37774));
#8751=EDGE_LOOP('',(#37775,#37776,#37777,#37778));
#8752=EDGE_LOOP('',(#37779,#37780,#37781));
#8753=EDGE_LOOP('',(#37782,#37783,#37784));
#8754=EDGE_LOOP('',(#37785,#37786,#37787,#37788));
#8755=EDGE_LOOP('',(#37789,#37790,#37791,#37792));
#8756=EDGE_LOOP('',(#37793,#37794,#37795,#37796));
#8757=EDGE_LOOP('',(#37797,#37798,#37799,#37800,#37801,#37802));
#8758=EDGE_LOOP('',(#37803,#37804,#37805,#37806));
#8759=EDGE_LOOP('',(#37807,#37808,#37809,#37810));
#8760=EDGE_LOOP('',(#37811,#37812,#37813,#37814,#37815,#37816));
#8761=EDGE_LOOP('',(#37817,#37818,#37819,#37820));
#8762=EDGE_LOOP('',(#37821,#37822,#37823,#37824));
#8763=EDGE_LOOP('',(#37825,#37826,#37827,#37828,#37829,#37830));
#8764=EDGE_LOOP('',(#37831,#37832,#37833,#37834));
#8765=EDGE_LOOP('',(#37835,#37836,#37837,#37838));
#8766=EDGE_LOOP('',(#37839,#37840,#37841,#37842,#37843,#37844));
#8767=EDGE_LOOP('',(#37845,#37846,#37847,#37848));
#8768=EDGE_LOOP('',(#37849,#37850,#37851,#37852));
#8769=EDGE_LOOP('',(#37853,#37854,#37855,#37856,#37857,#37858));
#8770=EDGE_LOOP('',(#37859,#37860,#37861,#37862));
#8771=EDGE_LOOP('',(#37863,#37864,#37865,#37866));
#8772=EDGE_LOOP('',(#37867,#37868,#37869,#37870,#37871,#37872));
#8773=EDGE_LOOP('',(#37873,#37874,#37875,#37876,#37877,#37878));
#8774=EDGE_LOOP('',(#37879,#37880,#37881,#37882));
#8775=EDGE_LOOP('',(#37883,#37884,#37885));
#8776=EDGE_LOOP('',(#37886,#37887,#37888));
#8777=EDGE_LOOP('',(#37889,#37890,#37891,#37892));
#8778=EDGE_LOOP('',(#37893,#37894,#37895,#37896));
#8779=EDGE_LOOP('',(#37897,#37898,#37899,#37900));
#8780=EDGE_LOOP('',(#37901,#37902,#37903,#37904,#37905,#37906));
#8781=EDGE_LOOP('',(#37907,#37908,#37909,#37910));
#8782=EDGE_LOOP('',(#37911,#37912,#37913,#37914));
#8783=EDGE_LOOP('',(#37915,#37916,#37917,#37918,#37919,#37920));
#8784=EDGE_LOOP('',(#37921,#37922,#37923,#37924));
#8785=EDGE_LOOP('',(#37925,#37926,#37927,#37928));
#8786=EDGE_LOOP('',(#37929,#37930,#37931,#37932,#37933,#37934));
#8787=EDGE_LOOP('',(#37935,#37936,#37937,#37938));
#8788=EDGE_LOOP('',(#37939,#37940,#37941,#37942));
#8789=EDGE_LOOP('',(#37943,#37944,#37945,#37946,#37947,#37948));
#8790=EDGE_LOOP('',(#37949,#37950,#37951,#37952));
#8791=EDGE_LOOP('',(#37953,#37954,#37955,#37956));
#8792=EDGE_LOOP('',(#37957,#37958,#37959,#37960,#37961,#37962));
#8793=EDGE_LOOP('',(#37963,#37964,#37965,#37966));
#8794=EDGE_LOOP('',(#37967,#37968,#37969,#37970));
#8795=EDGE_LOOP('',(#37971,#37972,#37973,#37974,#37975,#37976));
#8796=EDGE_LOOP('',(#37977,#37978,#37979,#37980,#37981,#37982));
#8797=EDGE_LOOP('',(#37983,#37984,#37985,#37986));
#8798=EDGE_LOOP('',(#37987,#37988,#37989));
#8799=EDGE_LOOP('',(#37990,#37991,#37992));
#8800=EDGE_LOOP('',(#37993,#37994,#37995,#37996));
#8801=EDGE_LOOP('',(#37997,#37998,#37999,#38000));
#8802=EDGE_LOOP('',(#38001,#38002,#38003,#38004));
#8803=EDGE_LOOP('',(#38005,#38006,#38007,#38008,#38009,#38010));
#8804=EDGE_LOOP('',(#38011,#38012,#38013,#38014));
#8805=EDGE_LOOP('',(#38015,#38016,#38017,#38018));
#8806=EDGE_LOOP('',(#38019,#38020,#38021,#38022,#38023,#38024));
#8807=EDGE_LOOP('',(#38025,#38026,#38027,#38028));
#8808=EDGE_LOOP('',(#38029,#38030,#38031,#38032));
#8809=EDGE_LOOP('',(#38033,#38034,#38035,#38036,#38037,#38038));
#8810=EDGE_LOOP('',(#38039,#38040,#38041,#38042));
#8811=EDGE_LOOP('',(#38043,#38044,#38045,#38046));
#8812=EDGE_LOOP('',(#38047,#38048,#38049,#38050,#38051,#38052));
#8813=EDGE_LOOP('',(#38053,#38054,#38055,#38056));
#8814=EDGE_LOOP('',(#38057,#38058,#38059,#38060));
#8815=EDGE_LOOP('',(#38061,#38062,#38063,#38064,#38065,#38066));
#8816=EDGE_LOOP('',(#38067,#38068,#38069,#38070));
#8817=EDGE_LOOP('',(#38071,#38072,#38073,#38074));
#8818=EDGE_LOOP('',(#38075,#38076,#38077,#38078,#38079,#38080));
#8819=EDGE_LOOP('',(#38081,#38082,#38083,#38084,#38085,#38086));
#8820=EDGE_LOOP('',(#38087,#38088,#38089,#38090));
#8821=EDGE_LOOP('',(#38091,#38092,#38093));
#8822=EDGE_LOOP('',(#38094,#38095,#38096));
#8823=EDGE_LOOP('',(#38097,#38098,#38099,#38100));
#8824=EDGE_LOOP('',(#38101,#38102,#38103,#38104));
#8825=EDGE_LOOP('',(#38105,#38106,#38107,#38108));
#8826=EDGE_LOOP('',(#38109,#38110,#38111,#38112,#38113,#38114));
#8827=EDGE_LOOP('',(#38115,#38116,#38117,#38118));
#8828=EDGE_LOOP('',(#38119,#38120,#38121,#38122));
#8829=EDGE_LOOP('',(#38123,#38124,#38125,#38126,#38127,#38128));
#8830=EDGE_LOOP('',(#38129,#38130,#38131,#38132));
#8831=EDGE_LOOP('',(#38133,#38134,#38135,#38136));
#8832=EDGE_LOOP('',(#38137,#38138,#38139,#38140,#38141,#38142));
#8833=EDGE_LOOP('',(#38143,#38144,#38145,#38146));
#8834=EDGE_LOOP('',(#38147,#38148,#38149,#38150));
#8835=EDGE_LOOP('',(#38151,#38152,#38153,#38154,#38155,#38156));
#8836=EDGE_LOOP('',(#38157,#38158,#38159,#38160));
#8837=EDGE_LOOP('',(#38161,#38162,#38163,#38164));
#8838=EDGE_LOOP('',(#38165,#38166,#38167,#38168,#38169,#38170));
#8839=EDGE_LOOP('',(#38171,#38172,#38173,#38174));
#8840=EDGE_LOOP('',(#38175,#38176,#38177,#38178));
#8841=EDGE_LOOP('',(#38179,#38180,#38181,#38182,#38183,#38184));
#8842=EDGE_LOOP('',(#38185,#38186,#38187,#38188,#38189,#38190));
#8843=EDGE_LOOP('',(#38191,#38192,#38193,#38194));
#8844=EDGE_LOOP('',(#38195,#38196,#38197));
#8845=EDGE_LOOP('',(#38198,#38199,#38200));
#8846=EDGE_LOOP('',(#38201,#38202,#38203,#38204));
#8847=EDGE_LOOP('',(#38205,#38206,#38207,#38208));
#8848=EDGE_LOOP('',(#38209,#38210,#38211,#38212));
#8849=EDGE_LOOP('',(#38213,#38214,#38215,#38216,#38217,#38218));
#8850=EDGE_LOOP('',(#38219,#38220,#38221,#38222));
#8851=EDGE_LOOP('',(#38223,#38224,#38225,#38226));
#8852=EDGE_LOOP('',(#38227,#38228,#38229,#38230,#38231,#38232));
#8853=EDGE_LOOP('',(#38233,#38234,#38235,#38236));
#8854=EDGE_LOOP('',(#38237,#38238,#38239,#38240));
#8855=EDGE_LOOP('',(#38241,#38242,#38243,#38244,#38245,#38246));
#8856=EDGE_LOOP('',(#38247,#38248,#38249,#38250));
#8857=EDGE_LOOP('',(#38251,#38252,#38253,#38254));
#8858=EDGE_LOOP('',(#38255,#38256,#38257,#38258,#38259,#38260));
#8859=EDGE_LOOP('',(#38261,#38262,#38263,#38264));
#8860=EDGE_LOOP('',(#38265,#38266,#38267,#38268));
#8861=EDGE_LOOP('',(#38269,#38270,#38271,#38272,#38273,#38274));
#8862=EDGE_LOOP('',(#38275,#38276,#38277,#38278));
#8863=EDGE_LOOP('',(#38279,#38280,#38281,#38282));
#8864=EDGE_LOOP('',(#38283,#38284,#38285,#38286,#38287,#38288));
#8865=EDGE_LOOP('',(#38289,#38290,#38291,#38292,#38293,#38294));
#8866=EDGE_LOOP('',(#38295,#38296,#38297,#38298));
#8867=EDGE_LOOP('',(#38299,#38300,#38301));
#8868=EDGE_LOOP('',(#38302,#38303,#38304));
#8869=EDGE_LOOP('',(#38305,#38306,#38307,#38308));
#8870=EDGE_LOOP('',(#38309,#38310,#38311,#38312));
#8871=EDGE_LOOP('',(#38313,#38314,#38315,#38316));
#8872=EDGE_LOOP('',(#38317,#38318,#38319,#38320,#38321,#38322));
#8873=EDGE_LOOP('',(#38323,#38324,#38325,#38326));
#8874=EDGE_LOOP('',(#38327,#38328,#38329,#38330));
#8875=EDGE_LOOP('',(#38331,#38332,#38333,#38334,#38335,#38336));
#8876=EDGE_LOOP('',(#38337,#38338,#38339,#38340));
#8877=EDGE_LOOP('',(#38341,#38342,#38343,#38344));
#8878=EDGE_LOOP('',(#38345,#38346,#38347,#38348,#38349,#38350));
#8879=EDGE_LOOP('',(#38351,#38352,#38353,#38354));
#8880=EDGE_LOOP('',(#38355,#38356,#38357,#38358));
#8881=EDGE_LOOP('',(#38359,#38360,#38361,#38362,#38363,#38364));
#8882=EDGE_LOOP('',(#38365,#38366,#38367,#38368));
#8883=EDGE_LOOP('',(#38369,#38370,#38371,#38372));
#8884=EDGE_LOOP('',(#38373,#38374,#38375,#38376,#38377,#38378));
#8885=EDGE_LOOP('',(#38379,#38380,#38381,#38382));
#8886=EDGE_LOOP('',(#38383,#38384,#38385,#38386));
#8887=EDGE_LOOP('',(#38387,#38388,#38389,#38390,#38391,#38392));
#8888=EDGE_LOOP('',(#38393,#38394,#38395,#38396,#38397,#38398));
#8889=EDGE_LOOP('',(#38399,#38400,#38401,#38402));
#8890=EDGE_LOOP('',(#38403,#38404,#38405));
#8891=EDGE_LOOP('',(#38406,#38407,#38408));
#8892=EDGE_LOOP('',(#38409,#38410,#38411,#38412));
#8893=EDGE_LOOP('',(#38413,#38414,#38415,#38416));
#8894=EDGE_LOOP('',(#38417,#38418,#38419,#38420));
#8895=EDGE_LOOP('',(#38421,#38422,#38423,#38424,#38425,#38426));
#8896=EDGE_LOOP('',(#38427,#38428,#38429,#38430));
#8897=EDGE_LOOP('',(#38431,#38432,#38433,#38434));
#8898=EDGE_LOOP('',(#38435,#38436,#38437,#38438,#38439,#38440));
#8899=EDGE_LOOP('',(#38441,#38442,#38443,#38444));
#8900=EDGE_LOOP('',(#38445,#38446,#38447,#38448));
#8901=EDGE_LOOP('',(#38449,#38450,#38451,#38452,#38453,#38454));
#8902=EDGE_LOOP('',(#38455,#38456,#38457,#38458));
#8903=EDGE_LOOP('',(#38459,#38460,#38461,#38462));
#8904=EDGE_LOOP('',(#38463,#38464,#38465,#38466,#38467,#38468));
#8905=EDGE_LOOP('',(#38469,#38470,#38471,#38472));
#8906=EDGE_LOOP('',(#38473,#38474,#38475,#38476));
#8907=EDGE_LOOP('',(#38477,#38478,#38479,#38480,#38481,#38482));
#8908=EDGE_LOOP('',(#38483,#38484,#38485,#38486));
#8909=EDGE_LOOP('',(#38487,#38488,#38489,#38490));
#8910=EDGE_LOOP('',(#38491,#38492,#38493,#38494,#38495,#38496));
#8911=EDGE_LOOP('',(#38497,#38498,#38499,#38500,#38501,#38502));
#8912=EDGE_LOOP('',(#38503,#38504,#38505,#38506));
#8913=EDGE_LOOP('',(#38507,#38508,#38509));
#8914=EDGE_LOOP('',(#38510,#38511,#38512));
#8915=EDGE_LOOP('',(#38513,#38514,#38515,#38516));
#8916=EDGE_LOOP('',(#38517,#38518,#38519,#38520));
#8917=EDGE_LOOP('',(#38521,#38522,#38523,#38524));
#8918=EDGE_LOOP('',(#38525,#38526,#38527,#38528,#38529,#38530));
#8919=EDGE_LOOP('',(#38531,#38532,#38533,#38534));
#8920=EDGE_LOOP('',(#38535,#38536,#38537,#38538));
#8921=EDGE_LOOP('',(#38539,#38540,#38541,#38542,#38543,#38544));
#8922=EDGE_LOOP('',(#38545,#38546,#38547,#38548));
#8923=EDGE_LOOP('',(#38549,#38550,#38551,#38552));
#8924=EDGE_LOOP('',(#38553,#38554,#38555,#38556,#38557,#38558));
#8925=EDGE_LOOP('',(#38559,#38560,#38561,#38562));
#8926=EDGE_LOOP('',(#38563,#38564,#38565,#38566));
#8927=EDGE_LOOP('',(#38567,#38568,#38569,#38570,#38571,#38572));
#8928=EDGE_LOOP('',(#38573,#38574,#38575,#38576));
#8929=EDGE_LOOP('',(#38577,#38578,#38579,#38580));
#8930=EDGE_LOOP('',(#38581,#38582,#38583,#38584,#38585,#38586));
#8931=EDGE_LOOP('',(#38587,#38588,#38589,#38590));
#8932=EDGE_LOOP('',(#38591,#38592,#38593,#38594));
#8933=EDGE_LOOP('',(#38595,#38596,#38597,#38598,#38599,#38600));
#8934=EDGE_LOOP('',(#38601,#38602,#38603,#38604,#38605,#38606));
#8935=EDGE_LOOP('',(#38607,#38608,#38609,#38610));
#8936=EDGE_LOOP('',(#38611,#38612,#38613));
#8937=EDGE_LOOP('',(#38614,#38615,#38616));
#8938=EDGE_LOOP('',(#38617,#38618,#38619,#38620));
#8939=EDGE_LOOP('',(#38621,#38622,#38623,#38624));
#8940=EDGE_LOOP('',(#38625,#38626,#38627,#38628));
#8941=EDGE_LOOP('',(#38629,#38630,#38631,#38632,#38633,#38634));
#8942=EDGE_LOOP('',(#38635,#38636,#38637,#38638));
#8943=EDGE_LOOP('',(#38639,#38640,#38641,#38642));
#8944=EDGE_LOOP('',(#38643,#38644,#38645,#38646,#38647,#38648));
#8945=EDGE_LOOP('',(#38649,#38650,#38651,#38652));
#8946=EDGE_LOOP('',(#38653,#38654,#38655,#38656));
#8947=EDGE_LOOP('',(#38657,#38658,#38659,#38660,#38661,#38662));
#8948=EDGE_LOOP('',(#38663,#38664,#38665,#38666));
#8949=EDGE_LOOP('',(#38667,#38668,#38669,#38670));
#8950=EDGE_LOOP('',(#38671,#38672,#38673,#38674,#38675,#38676));
#8951=EDGE_LOOP('',(#38677,#38678,#38679,#38680));
#8952=EDGE_LOOP('',(#38681,#38682,#38683,#38684));
#8953=EDGE_LOOP('',(#38685,#38686,#38687,#38688,#38689,#38690));
#8954=EDGE_LOOP('',(#38691,#38692,#38693,#38694));
#8955=EDGE_LOOP('',(#38695,#38696,#38697,#38698));
#8956=EDGE_LOOP('',(#38699,#38700,#38701,#38702,#38703,#38704));
#8957=EDGE_LOOP('',(#38705,#38706,#38707,#38708,#38709,#38710));
#8958=EDGE_LOOP('',(#38711,#38712,#38713,#38714));
#8959=EDGE_LOOP('',(#38715,#38716,#38717));
#8960=EDGE_LOOP('',(#38718,#38719,#38720));
#8961=EDGE_LOOP('',(#38721,#38722,#38723,#38724));
#8962=EDGE_LOOP('',(#38725,#38726,#38727,#38728));
#8963=EDGE_LOOP('',(#38729,#38730,#38731,#38732));
#8964=EDGE_LOOP('',(#38733,#38734,#38735,#38736,#38737,#38738));
#8965=EDGE_LOOP('',(#38739,#38740,#38741,#38742));
#8966=EDGE_LOOP('',(#38743,#38744,#38745,#38746));
#8967=EDGE_LOOP('',(#38747,#38748,#38749,#38750,#38751,#38752));
#8968=EDGE_LOOP('',(#38753,#38754,#38755,#38756));
#8969=EDGE_LOOP('',(#38757,#38758,#38759,#38760));
#8970=EDGE_LOOP('',(#38761,#38762,#38763,#38764,#38765,#38766));
#8971=EDGE_LOOP('',(#38767,#38768,#38769,#38770));
#8972=EDGE_LOOP('',(#38771,#38772,#38773,#38774));
#8973=EDGE_LOOP('',(#38775,#38776,#38777,#38778,#38779,#38780));
#8974=EDGE_LOOP('',(#38781,#38782,#38783,#38784));
#8975=EDGE_LOOP('',(#38785,#38786,#38787,#38788));
#8976=EDGE_LOOP('',(#38789,#38790,#38791,#38792,#38793,#38794));
#8977=EDGE_LOOP('',(#38795,#38796,#38797,#38798));
#8978=EDGE_LOOP('',(#38799,#38800,#38801,#38802));
#8979=EDGE_LOOP('',(#38803,#38804,#38805,#38806,#38807,#38808));
#8980=EDGE_LOOP('',(#38809,#38810,#38811,#38812,#38813,#38814));
#8981=EDGE_LOOP('',(#38815,#38816,#38817,#38818));
#8982=EDGE_LOOP('',(#38819,#38820,#38821));
#8983=EDGE_LOOP('',(#38822,#38823,#38824));
#8984=EDGE_LOOP('',(#38825,#38826,#38827,#38828));
#8985=EDGE_LOOP('',(#38829,#38830,#38831,#38832));
#8986=EDGE_LOOP('',(#38833,#38834,#38835,#38836));
#8987=EDGE_LOOP('',(#38837,#38838,#38839,#38840,#38841,#38842));
#8988=EDGE_LOOP('',(#38843,#38844,#38845,#38846));
#8989=EDGE_LOOP('',(#38847,#38848,#38849,#38850));
#8990=EDGE_LOOP('',(#38851,#38852,#38853,#38854,#38855,#38856));
#8991=EDGE_LOOP('',(#38857,#38858,#38859,#38860));
#8992=EDGE_LOOP('',(#38861,#38862,#38863,#38864));
#8993=EDGE_LOOP('',(#38865,#38866,#38867,#38868,#38869,#38870));
#8994=EDGE_LOOP('',(#38871,#38872,#38873,#38874));
#8995=EDGE_LOOP('',(#38875,#38876,#38877,#38878));
#8996=EDGE_LOOP('',(#38879,#38880,#38881,#38882,#38883,#38884));
#8997=EDGE_LOOP('',(#38885,#38886,#38887,#38888));
#8998=EDGE_LOOP('',(#38889,#38890,#38891,#38892));
#8999=EDGE_LOOP('',(#38893,#38894,#38895,#38896,#38897,#38898));
#9000=EDGE_LOOP('',(#38899,#38900,#38901,#38902));
#9001=EDGE_LOOP('',(#38903,#38904,#38905,#38906));
#9002=EDGE_LOOP('',(#38907,#38908,#38909,#38910,#38911,#38912));
#9003=EDGE_LOOP('',(#38913,#38914,#38915,#38916,#38917,#38918));
#9004=EDGE_LOOP('',(#38919,#38920,#38921,#38922));
#9005=EDGE_LOOP('',(#38923,#38924,#38925));
#9006=EDGE_LOOP('',(#38926,#38927,#38928));
#9007=EDGE_LOOP('',(#38929,#38930,#38931,#38932));
#9008=EDGE_LOOP('',(#38933,#38934,#38935,#38936));
#9009=EDGE_LOOP('',(#38937,#38938,#38939,#38940));
#9010=EDGE_LOOP('',(#38941,#38942,#38943,#38944,#38945,#38946));
#9011=EDGE_LOOP('',(#38947,#38948,#38949,#38950));
#9012=EDGE_LOOP('',(#38951,#38952,#38953,#38954));
#9013=EDGE_LOOP('',(#38955,#38956,#38957,#38958,#38959,#38960));
#9014=EDGE_LOOP('',(#38961,#38962,#38963,#38964));
#9015=EDGE_LOOP('',(#38965,#38966,#38967,#38968));
#9016=EDGE_LOOP('',(#38969,#38970,#38971,#38972,#38973,#38974));
#9017=EDGE_LOOP('',(#38975,#38976,#38977,#38978));
#9018=EDGE_LOOP('',(#38979,#38980,#38981,#38982));
#9019=EDGE_LOOP('',(#38983,#38984,#38985,#38986,#38987,#38988));
#9020=EDGE_LOOP('',(#38989,#38990,#38991,#38992));
#9021=EDGE_LOOP('',(#38993,#38994,#38995,#38996));
#9022=EDGE_LOOP('',(#38997,#38998,#38999,#39000,#39001,#39002));
#9023=EDGE_LOOP('',(#39003,#39004,#39005,#39006));
#9024=EDGE_LOOP('',(#39007,#39008,#39009,#39010));
#9025=EDGE_LOOP('',(#39011,#39012,#39013,#39014,#39015,#39016));
#9026=EDGE_LOOP('',(#39017,#39018,#39019,#39020,#39021,#39022));
#9027=EDGE_LOOP('',(#39023,#39024,#39025,#39026));
#9028=EDGE_LOOP('',(#39027,#39028,#39029));
#9029=EDGE_LOOP('',(#39030,#39031,#39032));
#9030=EDGE_LOOP('',(#39033,#39034,#39035,#39036));
#9031=EDGE_LOOP('',(#39037,#39038,#39039,#39040));
#9032=EDGE_LOOP('',(#39041,#39042,#39043,#39044));
#9033=EDGE_LOOP('',(#39045,#39046,#39047,#39048,#39049,#39050));
#9034=EDGE_LOOP('',(#39051,#39052,#39053,#39054));
#9035=EDGE_LOOP('',(#39055,#39056,#39057,#39058));
#9036=EDGE_LOOP('',(#39059,#39060,#39061,#39062,#39063,#39064));
#9037=EDGE_LOOP('',(#39065,#39066,#39067,#39068));
#9038=EDGE_LOOP('',(#39069,#39070,#39071,#39072));
#9039=EDGE_LOOP('',(#39073,#39074,#39075,#39076,#39077,#39078));
#9040=EDGE_LOOP('',(#39079,#39080,#39081,#39082));
#9041=EDGE_LOOP('',(#39083,#39084,#39085,#39086));
#9042=EDGE_LOOP('',(#39087,#39088,#39089,#39090,#39091,#39092));
#9043=EDGE_LOOP('',(#39093,#39094,#39095,#39096));
#9044=EDGE_LOOP('',(#39097,#39098,#39099,#39100));
#9045=EDGE_LOOP('',(#39101,#39102,#39103,#39104,#39105,#39106));
#9046=EDGE_LOOP('',(#39107,#39108,#39109,#39110));
#9047=EDGE_LOOP('',(#39111,#39112,#39113,#39114));
#9048=EDGE_LOOP('',(#39115,#39116,#39117,#39118,#39119,#39120));
#9049=EDGE_LOOP('',(#39121,#39122,#39123,#39124,#39125,#39126));
#9050=EDGE_LOOP('',(#39127,#39128,#39129,#39130));
#9051=EDGE_LOOP('',(#39131,#39132,#39133));
#9052=EDGE_LOOP('',(#39134,#39135,#39136));
#9053=EDGE_LOOP('',(#39137,#39138,#39139,#39140));
#9054=EDGE_LOOP('',(#39141,#39142,#39143,#39144));
#9055=EDGE_LOOP('',(#39145,#39146,#39147,#39148));
#9056=EDGE_LOOP('',(#39149,#39150,#39151,#39152,#39153,#39154));
#9057=EDGE_LOOP('',(#39155,#39156,#39157,#39158));
#9058=EDGE_LOOP('',(#39159,#39160,#39161,#39162));
#9059=EDGE_LOOP('',(#39163,#39164,#39165,#39166,#39167,#39168));
#9060=EDGE_LOOP('',(#39169,#39170,#39171,#39172));
#9061=EDGE_LOOP('',(#39173,#39174,#39175,#39176));
#9062=EDGE_LOOP('',(#39177,#39178,#39179,#39180,#39181,#39182));
#9063=EDGE_LOOP('',(#39183,#39184,#39185,#39186));
#9064=EDGE_LOOP('',(#39187,#39188,#39189,#39190));
#9065=EDGE_LOOP('',(#39191,#39192,#39193,#39194,#39195,#39196));
#9066=EDGE_LOOP('',(#39197,#39198,#39199,#39200));
#9067=EDGE_LOOP('',(#39201,#39202,#39203,#39204));
#9068=EDGE_LOOP('',(#39205,#39206,#39207,#39208,#39209,#39210));
#9069=EDGE_LOOP('',(#39211,#39212,#39213,#39214));
#9070=EDGE_LOOP('',(#39215,#39216,#39217,#39218));
#9071=EDGE_LOOP('',(#39219,#39220,#39221,#39222,#39223,#39224));
#9072=EDGE_LOOP('',(#39225,#39226,#39227,#39228,#39229,#39230));
#9073=EDGE_LOOP('',(#39231,#39232,#39233,#39234));
#9074=EDGE_LOOP('',(#39235,#39236,#39237));
#9075=EDGE_LOOP('',(#39238,#39239,#39240));
#9076=EDGE_LOOP('',(#39241,#39242,#39243,#39244));
#9077=EDGE_LOOP('',(#39245,#39246,#39247,#39248));
#9078=EDGE_LOOP('',(#39249,#39250,#39251,#39252));
#9079=EDGE_LOOP('',(#39253,#39254,#39255,#39256,#39257,#39258));
#9080=EDGE_LOOP('',(#39259,#39260,#39261,#39262));
#9081=EDGE_LOOP('',(#39263,#39264,#39265,#39266));
#9082=EDGE_LOOP('',(#39267,#39268,#39269,#39270,#39271,#39272));
#9083=EDGE_LOOP('',(#39273,#39274,#39275,#39276));
#9084=EDGE_LOOP('',(#39277,#39278,#39279,#39280));
#9085=EDGE_LOOP('',(#39281,#39282,#39283,#39284,#39285,#39286));
#9086=EDGE_LOOP('',(#39287,#39288,#39289,#39290));
#9087=EDGE_LOOP('',(#39291,#39292,#39293,#39294));
#9088=EDGE_LOOP('',(#39295,#39296,#39297,#39298,#39299,#39300));
#9089=EDGE_LOOP('',(#39301,#39302,#39303,#39304));
#9090=EDGE_LOOP('',(#39305,#39306,#39307,#39308));
#9091=EDGE_LOOP('',(#39309,#39310,#39311,#39312,#39313,#39314));
#9092=EDGE_LOOP('',(#39315,#39316,#39317,#39318));
#9093=EDGE_LOOP('',(#39319,#39320,#39321,#39322));
#9094=EDGE_LOOP('',(#39323,#39324,#39325,#39326,#39327,#39328));
#9095=EDGE_LOOP('',(#39329,#39330,#39331,#39332,#39333,#39334));
#9096=EDGE_LOOP('',(#39335,#39336,#39337,#39338));
#9097=EDGE_LOOP('',(#39339,#39340,#39341));
#9098=EDGE_LOOP('',(#39342,#39343,#39344));
#9099=EDGE_LOOP('',(#39345,#39346,#39347,#39348));
#9100=EDGE_LOOP('',(#39349,#39350,#39351,#39352));
#9101=EDGE_LOOP('',(#39353,#39354,#39355,#39356));
#9102=EDGE_LOOP('',(#39357,#39358,#39359,#39360,#39361,#39362));
#9103=EDGE_LOOP('',(#39363,#39364,#39365,#39366));
#9104=EDGE_LOOP('',(#39367,#39368,#39369,#39370));
#9105=EDGE_LOOP('',(#39371,#39372,#39373,#39374,#39375,#39376));
#9106=EDGE_LOOP('',(#39377,#39378,#39379,#39380));
#9107=EDGE_LOOP('',(#39381,#39382,#39383,#39384));
#9108=EDGE_LOOP('',(#39385,#39386,#39387,#39388,#39389,#39390));
#9109=EDGE_LOOP('',(#39391,#39392,#39393,#39394));
#9110=EDGE_LOOP('',(#39395,#39396,#39397,#39398));
#9111=EDGE_LOOP('',(#39399,#39400,#39401,#39402,#39403,#39404));
#9112=EDGE_LOOP('',(#39405,#39406,#39407,#39408));
#9113=EDGE_LOOP('',(#39409,#39410,#39411,#39412));
#9114=EDGE_LOOP('',(#39413,#39414,#39415,#39416,#39417,#39418));
#9115=EDGE_LOOP('',(#39419,#39420,#39421,#39422));
#9116=EDGE_LOOP('',(#39423,#39424,#39425,#39426));
#9117=EDGE_LOOP('',(#39427,#39428,#39429,#39430,#39431,#39432));
#9118=EDGE_LOOP('',(#39433,#39434,#39435,#39436,#39437,#39438));
#9119=EDGE_LOOP('',(#39439,#39440,#39441,#39442));
#9120=EDGE_LOOP('',(#39443,#39444,#39445));
#9121=EDGE_LOOP('',(#39446,#39447,#39448));
#9122=EDGE_LOOP('',(#39449,#39450,#39451,#39452));
#9123=EDGE_LOOP('',(#39453,#39454,#39455,#39456));
#9124=EDGE_LOOP('',(#39457,#39458,#39459,#39460));
#9125=EDGE_LOOP('',(#39461,#39462,#39463,#39464,#39465,#39466));
#9126=EDGE_LOOP('',(#39467,#39468,#39469,#39470));
#9127=EDGE_LOOP('',(#39471,#39472,#39473,#39474));
#9128=EDGE_LOOP('',(#39475,#39476,#39477,#39478,#39479,#39480));
#9129=EDGE_LOOP('',(#39481,#39482,#39483,#39484));
#9130=EDGE_LOOP('',(#39485,#39486,#39487,#39488));
#9131=EDGE_LOOP('',(#39489,#39490,#39491,#39492,#39493,#39494));
#9132=EDGE_LOOP('',(#39495,#39496,#39497,#39498));
#9133=EDGE_LOOP('',(#39499,#39500,#39501,#39502));
#9134=EDGE_LOOP('',(#39503,#39504,#39505,#39506,#39507,#39508));
#9135=EDGE_LOOP('',(#39509,#39510,#39511,#39512));
#9136=EDGE_LOOP('',(#39513,#39514,#39515,#39516));
#9137=EDGE_LOOP('',(#39517,#39518,#39519,#39520,#39521,#39522));
#9138=EDGE_LOOP('',(#39523,#39524,#39525,#39526));
#9139=EDGE_LOOP('',(#39527,#39528,#39529,#39530));
#9140=EDGE_LOOP('',(#39531,#39532,#39533,#39534,#39535,#39536));
#9141=EDGE_LOOP('',(#39537,#39538,#39539,#39540,#39541,#39542));
#9142=EDGE_LOOP('',(#39543,#39544,#39545,#39546));
#9143=EDGE_LOOP('',(#39547,#39548,#39549));
#9144=EDGE_LOOP('',(#39550,#39551,#39552));
#9145=EDGE_LOOP('',(#39553,#39554,#39555,#39556));
#9146=EDGE_LOOP('',(#39557,#39558,#39559,#39560));
#9147=EDGE_LOOP('',(#39561,#39562,#39563,#39564));
#9148=EDGE_LOOP('',(#39565,#39566,#39567,#39568,#39569,#39570));
#9149=EDGE_LOOP('',(#39571,#39572,#39573,#39574));
#9150=EDGE_LOOP('',(#39575,#39576,#39577,#39578));
#9151=EDGE_LOOP('',(#39579,#39580,#39581,#39582,#39583,#39584));
#9152=EDGE_LOOP('',(#39585,#39586,#39587,#39588));
#9153=EDGE_LOOP('',(#39589,#39590,#39591,#39592));
#9154=EDGE_LOOP('',(#39593,#39594,#39595,#39596,#39597,#39598));
#9155=EDGE_LOOP('',(#39599,#39600,#39601,#39602));
#9156=EDGE_LOOP('',(#39603,#39604,#39605,#39606));
#9157=EDGE_LOOP('',(#39607,#39608,#39609,#39610,#39611,#39612));
#9158=EDGE_LOOP('',(#39613,#39614,#39615,#39616));
#9159=EDGE_LOOP('',(#39617,#39618,#39619,#39620));
#9160=EDGE_LOOP('',(#39621,#39622,#39623,#39624,#39625,#39626));
#9161=EDGE_LOOP('',(#39627,#39628,#39629,#39630));
#9162=EDGE_LOOP('',(#39631,#39632,#39633,#39634));
#9163=EDGE_LOOP('',(#39635,#39636,#39637,#39638,#39639,#39640));
#9164=EDGE_LOOP('',(#39641,#39642,#39643,#39644,#39645,#39646));
#9165=EDGE_LOOP('',(#39647,#39648,#39649,#39650));
#9166=EDGE_LOOP('',(#39651,#39652,#39653));
#9167=EDGE_LOOP('',(#39654,#39655,#39656,#39657));
#9168=EDGE_LOOP('',(#39658,#39659,#39660,#39661));
#9169=EDGE_LOOP('',(#39662,#39663,#39664,#39665,#39666,#39667));
#9170=EDGE_LOOP('',(#39668,#39669,#39670));
#9171=EDGE_LOOP('',(#39671,#39672,#39673,#39674));
#9172=EDGE_LOOP('',(#39675,#39676,#39677,#39678));
#9173=EDGE_LOOP('',(#39679,#39680,#39681,#39682));
#9174=EDGE_LOOP('',(#39683,#39684,#39685,#39686,#39687,#39688));
#9175=EDGE_LOOP('',(#39689,#39690,#39691,#39692));
#9176=EDGE_LOOP('',(#39693,#39694,#39695,#39696));
#9177=EDGE_LOOP('',(#39697,#39698,#39699,#39700,#39701,#39702));
#9178=EDGE_LOOP('',(#39703,#39704,#39705,#39706));
#9179=EDGE_LOOP('',(#39707,#39708,#39709,#39710));
#9180=EDGE_LOOP('',(#39711,#39712,#39713,#39714,#39715,#39716));
#9181=EDGE_LOOP('',(#39717,#39718,#39719,#39720));
#9182=EDGE_LOOP('',(#39721,#39722,#39723,#39724));
#9183=EDGE_LOOP('',(#39725,#39726,#39727,#39728,#39729,#39730));
#9184=EDGE_LOOP('',(#39731,#39732,#39733,#39734));
#9185=EDGE_LOOP('',(#39735,#39736,#39737,#39738));
#9186=EDGE_LOOP('',(#39739,#39740,#39741,#39742,#39743,#39744));
#9187=EDGE_LOOP('',(#39745,#39746,#39747,#39748,#39749,#39750));
#9188=EDGE_LOOP('',(#39751,#39752,#39753,#39754));
#9189=EDGE_LOOP('',(#39755,#39756,#39757));
#9190=EDGE_LOOP('',(#39758,#39759,#39760));
#9191=EDGE_LOOP('',(#39761,#39762,#39763,#39764));
#9192=EDGE_LOOP('',(#39765,#39766,#39767,#39768));
#9193=EDGE_LOOP('',(#39769,#39770,#39771,#39772));
#9194=EDGE_LOOP('',(#39773,#39774,#39775,#39776,#39777,#39778));
#9195=EDGE_LOOP('',(#39779,#39780,#39781,#39782));
#9196=EDGE_LOOP('',(#39783,#39784,#39785,#39786));
#9197=EDGE_LOOP('',(#39787,#39788,#39789,#39790,#39791,#39792));
#9198=EDGE_LOOP('',(#39793,#39794,#39795,#39796));
#9199=EDGE_LOOP('',(#39797,#39798,#39799,#39800));
#9200=EDGE_LOOP('',(#39801,#39802,#39803,#39804,#39805,#39806));
#9201=EDGE_LOOP('',(#39807,#39808,#39809,#39810));
#9202=EDGE_LOOP('',(#39811,#39812,#39813,#39814));
#9203=EDGE_LOOP('',(#39815,#39816,#39817,#39818,#39819,#39820));
#9204=EDGE_LOOP('',(#39821,#39822,#39823,#39824));
#9205=EDGE_LOOP('',(#39825,#39826,#39827,#39828));
#9206=EDGE_LOOP('',(#39829,#39830,#39831,#39832,#39833,#39834));
#9207=EDGE_LOOP('',(#39835,#39836,#39837,#39838));
#9208=EDGE_LOOP('',(#39839,#39840,#39841,#39842));
#9209=EDGE_LOOP('',(#39843,#39844,#39845,#39846,#39847,#39848));
#9210=EDGE_LOOP('',(#39849,#39850,#39851,#39852,#39853,#39854));
#9211=EDGE_LOOP('',(#39855,#39856,#39857,#39858));
#9212=EDGE_LOOP('',(#39859,#39860,#39861));
#9213=EDGE_LOOP('',(#39862,#39863,#39864));
#9214=EDGE_LOOP('',(#39865,#39866,#39867,#39868));
#9215=EDGE_LOOP('',(#39869,#39870,#39871,#39872));
#9216=EDGE_LOOP('',(#39873,#39874,#39875,#39876));
#9217=EDGE_LOOP('',(#39877,#39878,#39879,#39880,#39881,#39882));
#9218=EDGE_LOOP('',(#39883,#39884,#39885,#39886));
#9219=EDGE_LOOP('',(#39887,#39888,#39889,#39890));
#9220=EDGE_LOOP('',(#39891,#39892,#39893,#39894,#39895,#39896));
#9221=EDGE_LOOP('',(#39897,#39898,#39899,#39900));
#9222=EDGE_LOOP('',(#39901,#39902,#39903,#39904));
#9223=EDGE_LOOP('',(#39905,#39906,#39907,#39908,#39909,#39910));
#9224=EDGE_LOOP('',(#39911,#39912,#39913,#39914));
#9225=EDGE_LOOP('',(#39915,#39916,#39917,#39918));
#9226=EDGE_LOOP('',(#39919,#39920,#39921,#39922,#39923,#39924));
#9227=EDGE_LOOP('',(#39925,#39926,#39927,#39928));
#9228=EDGE_LOOP('',(#39929,#39930,#39931,#39932));
#9229=EDGE_LOOP('',(#39933,#39934,#39935,#39936,#39937,#39938));
#9230=EDGE_LOOP('',(#39939,#39940,#39941,#39942));
#9231=EDGE_LOOP('',(#39943,#39944,#39945,#39946));
#9232=EDGE_LOOP('',(#39947,#39948,#39949,#39950,#39951,#39952));
#9233=EDGE_LOOP('',(#39953,#39954,#39955,#39956,#39957,#39958));
#9234=EDGE_LOOP('',(#39959,#39960,#39961,#39962));
#9235=EDGE_LOOP('',(#39963,#39964,#39965));
#9236=EDGE_LOOP('',(#39966,#39967,#39968));
#9237=EDGE_LOOP('',(#39969,#39970,#39971,#39972));
#9238=EDGE_LOOP('',(#39973,#39974,#39975,#39976));
#9239=EDGE_LOOP('',(#39977,#39978,#39979,#39980));
#9240=EDGE_LOOP('',(#39981,#39982,#39983,#39984,#39985,#39986));
#9241=EDGE_LOOP('',(#39987,#39988,#39989,#39990));
#9242=EDGE_LOOP('',(#39991,#39992,#39993,#39994));
#9243=EDGE_LOOP('',(#39995,#39996,#39997,#39998,#39999,#40000));
#9244=EDGE_LOOP('',(#40001,#40002,#40003,#40004));
#9245=EDGE_LOOP('',(#40005,#40006,#40007,#40008));
#9246=EDGE_LOOP('',(#40009,#40010,#40011,#40012,#40013,#40014));
#9247=EDGE_LOOP('',(#40015,#40016,#40017,#40018));
#9248=EDGE_LOOP('',(#40019,#40020,#40021,#40022));
#9249=EDGE_LOOP('',(#40023,#40024,#40025,#40026,#40027,#40028));
#9250=EDGE_LOOP('',(#40029,#40030,#40031,#40032));
#9251=EDGE_LOOP('',(#40033,#40034,#40035,#40036));
#9252=EDGE_LOOP('',(#40037,#40038,#40039,#40040,#40041,#40042));
#9253=EDGE_LOOP('',(#40043,#40044,#40045,#40046));
#9254=EDGE_LOOP('',(#40047,#40048,#40049,#40050));
#9255=EDGE_LOOP('',(#40051,#40052,#40053,#40054,#40055,#40056));
#9256=EDGE_LOOP('',(#40057,#40058,#40059,#40060,#40061,#40062));
#9257=EDGE_LOOP('',(#40063,#40064,#40065,#40066));
#9258=EDGE_LOOP('',(#40067,#40068,#40069));
#9259=EDGE_LOOP('',(#40070,#40071,#40072));
#9260=EDGE_LOOP('',(#40073,#40074,#40075,#40076));
#9261=EDGE_LOOP('',(#40077,#40078,#40079,#40080));
#9262=EDGE_LOOP('',(#40081,#40082,#40083,#40084));
#9263=EDGE_LOOP('',(#40085,#40086,#40087,#40088,#40089,#40090));
#9264=EDGE_LOOP('',(#40091,#40092,#40093,#40094));
#9265=EDGE_LOOP('',(#40095,#40096,#40097,#40098));
#9266=EDGE_LOOP('',(#40099,#40100,#40101,#40102,#40103,#40104));
#9267=EDGE_LOOP('',(#40105,#40106,#40107,#40108));
#9268=EDGE_LOOP('',(#40109,#40110,#40111,#40112));
#9269=EDGE_LOOP('',(#40113,#40114,#40115,#40116,#40117,#40118));
#9270=EDGE_LOOP('',(#40119,#40120,#40121,#40122));
#9271=EDGE_LOOP('',(#40123,#40124,#40125,#40126));
#9272=EDGE_LOOP('',(#40127,#40128,#40129,#40130,#40131,#40132));
#9273=EDGE_LOOP('',(#40133,#40134,#40135,#40136));
#9274=EDGE_LOOP('',(#40137,#40138,#40139,#40140));
#9275=EDGE_LOOP('',(#40141,#40142,#40143,#40144,#40145,#40146));
#9276=EDGE_LOOP('',(#40147,#40148,#40149,#40150));
#9277=EDGE_LOOP('',(#40151,#40152,#40153,#40154));
#9278=EDGE_LOOP('',(#40155,#40156,#40157,#40158,#40159,#40160));
#9279=EDGE_LOOP('',(#40161,#40162,#40163,#40164,#40165,#40166));
#9280=EDGE_LOOP('',(#40167,#40168,#40169,#40170));
#9281=EDGE_LOOP('',(#40171,#40172,#40173));
#9282=EDGE_LOOP('',(#40174,#40175,#40176));
#9283=EDGE_LOOP('',(#40177,#40178,#40179,#40180));
#9284=EDGE_LOOP('',(#40181,#40182,#40183,#40184));
#9285=EDGE_LOOP('',(#40185,#40186,#40187,#40188));
#9286=EDGE_LOOP('',(#40189,#40190,#40191,#40192,#40193,#40194));
#9287=EDGE_LOOP('',(#40195,#40196,#40197,#40198));
#9288=EDGE_LOOP('',(#40199,#40200,#40201,#40202));
#9289=EDGE_LOOP('',(#40203,#40204,#40205,#40206,#40207,#40208));
#9290=EDGE_LOOP('',(#40209,#40210,#40211,#40212));
#9291=EDGE_LOOP('',(#40213,#40214,#40215,#40216));
#9292=EDGE_LOOP('',(#40217,#40218,#40219,#40220,#40221,#40222));
#9293=EDGE_LOOP('',(#40223,#40224,#40225,#40226));
#9294=EDGE_LOOP('',(#40227,#40228,#40229,#40230));
#9295=EDGE_LOOP('',(#40231,#40232,#40233,#40234,#40235,#40236));
#9296=EDGE_LOOP('',(#40237,#40238,#40239,#40240));
#9297=EDGE_LOOP('',(#40241,#40242,#40243,#40244));
#9298=EDGE_LOOP('',(#40245,#40246,#40247,#40248,#40249,#40250));
#9299=EDGE_LOOP('',(#40251,#40252,#40253,#40254));
#9300=EDGE_LOOP('',(#40255,#40256,#40257,#40258));
#9301=EDGE_LOOP('',(#40259,#40260,#40261,#40262,#40263,#40264));
#9302=EDGE_LOOP('',(#40265,#40266,#40267,#40268,#40269,#40270));
#9303=EDGE_LOOP('',(#40271,#40272,#40273,#40274));
#9304=EDGE_LOOP('',(#40275,#40276,#40277));
#9305=EDGE_LOOP('',(#40278,#40279,#40280));
#9306=EDGE_LOOP('',(#40281,#40282,#40283,#40284));
#9307=EDGE_LOOP('',(#40285,#40286,#40287,#40288));
#9308=EDGE_LOOP('',(#40289,#40290,#40291,#40292));
#9309=EDGE_LOOP('',(#40293,#40294,#40295,#40296,#40297,#40298));
#9310=EDGE_LOOP('',(#40299,#40300,#40301,#40302));
#9311=EDGE_LOOP('',(#40303,#40304,#40305,#40306));
#9312=EDGE_LOOP('',(#40307,#40308,#40309,#40310,#40311,#40312));
#9313=EDGE_LOOP('',(#40313,#40314,#40315,#40316));
#9314=EDGE_LOOP('',(#40317,#40318,#40319,#40320));
#9315=EDGE_LOOP('',(#40321,#40322,#40323,#40324,#40325,#40326));
#9316=EDGE_LOOP('',(#40327,#40328,#40329,#40330));
#9317=EDGE_LOOP('',(#40331,#40332,#40333,#40334));
#9318=EDGE_LOOP('',(#40335,#40336,#40337,#40338,#40339,#40340));
#9319=EDGE_LOOP('',(#40341,#40342,#40343,#40344));
#9320=EDGE_LOOP('',(#40345,#40346,#40347,#40348));
#9321=EDGE_LOOP('',(#40349,#40350,#40351,#40352,#40353,#40354));
#9322=EDGE_LOOP('',(#40355,#40356,#40357,#40358));
#9323=EDGE_LOOP('',(#40359,#40360,#40361,#40362));
#9324=EDGE_LOOP('',(#40363,#40364,#40365,#40366,#40367,#40368));
#9325=EDGE_LOOP('',(#40369,#40370,#40371,#40372,#40373,#40374));
#9326=EDGE_LOOP('',(#40375,#40376,#40377,#40378));
#9327=EDGE_LOOP('',(#40379,#40380,#40381));
#9328=EDGE_LOOP('',(#40382,#40383,#40384,#40385));
#9329=EDGE_LOOP('',(#40386,#40387,#40388,#40389));
#9330=EDGE_LOOP('',(#40390,#40391,#40392,#40393));
#9331=EDGE_LOOP('',(#40394));
#9332=EDGE_LOOP('',(#40395));
#9333=EDGE_LOOP('',(#40396));
#9334=EDGE_LOOP('',(#40397));
#9335=EDGE_LOOP('',(#40398));
#9336=EDGE_LOOP('',(#40399));
#9337=EDGE_LOOP('',(#40400,#40401,#40402,#40403));
#9338=EDGE_LOOP('',(#40404,#40405,#40406,#40407));
#9339=EDGE_LOOP('',(#40408));
#9340=EDGE_LOOP('',(#40409));
#9341=EDGE_LOOP('',(#40410));
#9342=EDGE_LOOP('',(#40411));
#9343=EDGE_LOOP('',(#40412,#40413,#40414,#40415));
#9344=EDGE_LOOP('',(#40416,#40417,#40418,#40419));
#9345=EDGE_LOOP('',(#40420,#40421,#40422,#40423));
#9346=EDGE_LOOP('',(#40424,#40425,#40426,#40427));
#9347=EDGE_LOOP('',(#40428,#40429,#40430,#40431));
#9348=EDGE_LOOP('',(#40432,#40433,#40434,#40435));
#9349=EDGE_LOOP('',(#40436,#40437,#40438,#40439));
#9350=EDGE_LOOP('',(#40440,#40441,#40442,#40443));
#9351=EDGE_LOOP('',(#40444,#40445,#40446,#40447));
#9352=EDGE_LOOP('',(#40448,#40449,#40450,#40451));
#9353=EDGE_LOOP('',(#40452,#40453,#40454,#40455));
#9354=EDGE_LOOP('',(#40456,#40457,#40458,#40459));
#9355=EDGE_LOOP('',(#40460,#40461,#40462,#40463));
#9356=EDGE_LOOP('',(#40464,#40465,#40466,#40467));
#9357=EDGE_LOOP('',(#40468,#40469,#40470,#40471));
#9358=EDGE_LOOP('',(#40472,#40473,#40474,#40475));
#9359=EDGE_LOOP('',(#40476,#40477,#40478,#40479));
#9360=EDGE_LOOP('',(#40480,#40481,#40482,#40483));
#9361=EDGE_LOOP('',(#40484,#40485,#40486,#40487));
#9362=EDGE_LOOP('',(#40488,#40489,#40490,#40491));
#9363=EDGE_LOOP('',(#40492,#40493,#40494,#40495));
#9364=EDGE_LOOP('',(#40496,#40497,#40498,#40499));
#9365=EDGE_LOOP('',(#40500,#40501,#40502,#40503));
#9366=EDGE_LOOP('',(#40504,#40505,#40506,#40507));
#9367=EDGE_LOOP('',(#40508,#40509,#40510,#40511));
#9368=EDGE_LOOP('',(#40512,#40513,#40514,#40515));
#9369=EDGE_LOOP('',(#40516,#40517,#40518,#40519));
#9370=EDGE_LOOP('',(#40520,#40521,#40522,#40523));
#9371=EDGE_LOOP('',(#40524,#40525,#40526,#40527));
#9372=EDGE_LOOP('',(#40528,#40529,#40530,#40531));
#9373=EDGE_LOOP('',(#40532,#40533,#40534,#40535));
#9374=EDGE_LOOP('',(#40536,#40537,#40538,#40539));
#9375=EDGE_LOOP('',(#40540,#40541,#40542,#40543));
#9376=EDGE_LOOP('',(#40544,#40545,#40546,#40547));
#9377=EDGE_LOOP('',(#40548,#40549,#40550,#40551));
#9378=EDGE_LOOP('',(#40552,#40553,#40554,#40555));
#9379=EDGE_LOOP('',(#40556,#40557,#40558,#40559));
#9380=EDGE_LOOP('',(#40560,#40561,#40562,#40563));
#9381=EDGE_LOOP('',(#40564,#40565,#40566,#40567));
#9382=EDGE_LOOP('',(#40568,#40569,#40570,#40571));
#9383=EDGE_LOOP('',(#40572,#40573,#40574,#40575));
#9384=EDGE_LOOP('',(#40576,#40577,#40578,#40579));
#9385=EDGE_LOOP('',(#40580,#40581,#40582,#40583));
#9386=EDGE_LOOP('',(#40584,#40585,#40586,#40587));
#9387=EDGE_LOOP('',(#40588,#40589,#40590,#40591));
#9388=EDGE_LOOP('',(#40592,#40593,#40594,#40595));
#9389=EDGE_LOOP('',(#40596,#40597,#40598,#40599));
#9390=EDGE_LOOP('',(#40600,#40601,#40602,#40603));
#9391=EDGE_LOOP('',(#40604,#40605,#40606,#40607));
#9392=EDGE_LOOP('',(#40608,#40609,#40610,#40611));
#9393=EDGE_LOOP('',(#40612,#40613,#40614,#40615));
#9394=EDGE_LOOP('',(#40616,#40617,#40618,#40619));
#9395=EDGE_LOOP('',(#40620,#40621,#40622,#40623));
#9396=EDGE_LOOP('',(#40624,#40625,#40626,#40627));
#9397=EDGE_LOOP('',(#40628,#40629,#40630,#40631));
#9398=EDGE_LOOP('',(#40632,#40633,#40634,#40635,#40636,#40637,#40638,#40639,
#40640,#40641,#40642,#40643,#40644,#40645,#40646,#40647,#40648,#40649,#40650,
#40651,#40652,#40653,#40654,#40655,#40656,#40657,#40658,#40659,#40660,#40661,
#40662,#40663,#40664,#40665,#40666,#40667,#40668,#40669,#40670,#40671,#40672,
#40673,#40674,#40675,#40676,#40677,#40678,#40679,#40680,#40681,#40682,#40683,
#40684,#40685,#40686,#40687,#40688,#40689,#40690,#40691,#40692,#40693,#40694,
#40695,#40696,#40697,#40698,#40699,#40700,#40701,#40702,#40703,#40704,#40705,
#40706,#40707,#40708,#40709,#40710,#40711,#40712,#40713,#40714,#40715,#40716,
#40717,#40718,#40719,#40720,#40721,#40722,#40723,#40724,#40725,#40726,#40727,
#40728,#40729,#40730,#40731,#40732,#40733,#40734,#40735,#40736,#40737,#40738,
#40739,#40740,#40741,#40742,#40743,#40744,#40745,#40746,#40747,#40748,#40749,
#40750,#40751,#40752,#40753,#40754,#40755,#40756,#40757,#40758,#40759,#40760,
#40761,#40762,#40763,#40764,#40765,#40766,#40767,#40768,#40769,#40770,#40771,
#40772,#40773,#40774,#40775,#40776,#40777,#40778,#40779,#40780,#40781,#40782,
#40783,#40784));
#9399=EDGE_LOOP('',(#40785));
#9400=EDGE_LOOP('',(#40786,#40787,#40788,#40789,#40790,#40791,#40792,#40793,
#40794,#40795,#40796,#40797,#40798,#40799,#40800,#40801,#40802,#40803,#40804,
#40805,#40806,#40807,#40808,#40809,#40810,#40811,#40812,#40813,#40814,#40815,
#40816,#40817,#40818,#40819,#40820,#40821,#40822,#40823,#40824,#40825,#40826,
#40827,#40828,#40829,#40830,#40831,#40832,#40833,#40834,#40835,#40836,#40837,
#40838,#40839,#40840,#40841,#40842,#40843,#40844,#40845,#40846,#40847,#40848,
#40849,#40850,#40851,#40852,#40853,#40854,#40855,#40856,#40857,#40858,#40859,
#40860,#40861,#40862,#40863,#40864,#40865,#40866,#40867,#40868,#40869,#40870,
#40871,#40872,#40873,#40874,#40875,#40876,#40877,#40878,#40879,#40880,#40881,
#40882,#40883,#40884,#40885,#40886,#40887,#40888,#40889,#40890,#40891,#40892,
#40893,#40894,#40895,#40896,#40897,#40898,#40899,#40900,#40901,#40902,#40903,
#40904,#40905,#40906,#40907,#40908,#40909,#40910,#40911,#40912,#40913,#40914,
#40915,#40916,#40917,#40918,#40919,#40920,#40921,#40922,#40923,#40924,#40925,
#40926,#40927,#40928,#40929,#40930,#40931,#40932,#40933,#40934,#40935,#40936,
#40937,#40938));
#9401=EDGE_LOOP('',(#40939));
#9402=EDGE_LOOP('',(#40940));
#9403=EDGE_LOOP('',(#40941));
#9404=EDGE_LOOP('',(#40942));
#9405=EDGE_LOOP('',(#40943));
#9406=EDGE_LOOP('',(#40944));
#9407=EDGE_LOOP('',(#40945));
#9408=EDGE_LOOP('',(#40946,#40947,#40948,#40949));
#9409=EDGE_LOOP('',(#40950,#40951,#40952,#40953));
#9410=EDGE_LOOP('',(#40954,#40955,#40956,#40957));
#9411=EDGE_LOOP('',(#40958,#40959,#40960,#40961));
#9412=EDGE_LOOP('',(#40962,#40963,#40964,#40965));
#9413=EDGE_LOOP('',(#40966,#40967,#40968,#40969));
#9414=EDGE_LOOP('',(#40970,#40971,#40972,#40973));
#9415=EDGE_LOOP('',(#40974,#40975,#40976,#40977));
#9416=EDGE_LOOP('',(#40978,#40979,#40980,#40981));
#9417=EDGE_LOOP('',(#40982,#40983,#40984,#40985));
#9418=EDGE_LOOP('',(#40986,#40987,#40988,#40989));
#9419=EDGE_LOOP('',(#40990,#40991,#40992,#40993));
#9420=EDGE_LOOP('',(#40994,#40995,#40996,#40997));
#9421=EDGE_LOOP('',(#40998,#40999,#41000,#41001));
#9422=EDGE_LOOP('',(#41002,#41003,#41004,#41005));
#9423=EDGE_LOOP('',(#41006,#41007,#41008,#41009));
#9424=EDGE_LOOP('',(#41010,#41011,#41012,#41013));
#9425=EDGE_LOOP('',(#41014,#41015,#41016,#41017));
#9426=EDGE_LOOP('',(#41018,#41019,#41020,#41021));
#9427=EDGE_LOOP('',(#41022,#41023,#41024,#41025));
#9428=EDGE_LOOP('',(#41026,#41027,#41028,#41029));
#9429=EDGE_LOOP('',(#41030,#41031,#41032,#41033));
#9430=EDGE_LOOP('',(#41034,#41035,#41036,#41037));
#9431=EDGE_LOOP('',(#41038,#41039,#41040,#41041));
#9432=EDGE_LOOP('',(#41042,#41043,#41044,#41045));
#9433=EDGE_LOOP('',(#41046,#41047,#41048,#41049));
#9434=EDGE_LOOP('',(#41050,#41051,#41052,#41053));
#9435=EDGE_LOOP('',(#41054,#41055,#41056,#41057));
#9436=EDGE_LOOP('',(#41058,#41059,#41060,#41061));
#9437=EDGE_LOOP('',(#41062,#41063,#41064,#41065));
#9438=EDGE_LOOP('',(#41066,#41067,#41068,#41069));
#9439=EDGE_LOOP('',(#41070,#41071,#41072,#41073));
#9440=EDGE_LOOP('',(#41074,#41075,#41076,#41077));
#9441=EDGE_LOOP('',(#41078,#41079,#41080,#41081));
#9442=EDGE_LOOP('',(#41082,#41083,#41084,#41085));
#9443=EDGE_LOOP('',(#41086,#41087,#41088,#41089));
#9444=EDGE_LOOP('',(#41090,#41091,#41092,#41093));
#9445=EDGE_LOOP('',(#41094,#41095,#41096,#41097));
#9446=EDGE_LOOP('',(#41098,#41099,#41100,#41101));
#9447=EDGE_LOOP('',(#41102,#41103,#41104,#41105));
#9448=EDGE_LOOP('',(#41106,#41107,#41108,#41109));
#9449=EDGE_LOOP('',(#41110,#41111,#41112,#41113));
#9450=EDGE_LOOP('',(#41114,#41115,#41116,#41117));
#9451=EDGE_LOOP('',(#41118,#41119,#41120,#41121));
#9452=EDGE_LOOP('',(#41122,#41123,#41124,#41125));
#9453=EDGE_LOOP('',(#41126,#41127,#41128,#41129));
#9454=EDGE_LOOP('',(#41130,#41131,#41132,#41133));
#9455=EDGE_LOOP('',(#41134,#41135,#41136,#41137));
#9456=EDGE_LOOP('',(#41138,#41139,#41140,#41141));
#9457=EDGE_LOOP('',(#41142,#41143,#41144,#41145));
#9458=EDGE_LOOP('',(#41146,#41147,#41148,#41149));
#9459=EDGE_LOOP('',(#41150,#41151,#41152,#41153));
#9460=EDGE_LOOP('',(#41154,#41155,#41156,#41157));
#9461=EDGE_LOOP('',(#41158,#41159,#41160,#41161));
#9462=EDGE_LOOP('',(#41162,#41163,#41164,#41165));
#9463=EDGE_LOOP('',(#41166,#41167,#41168,#41169));
#9464=EDGE_LOOP('',(#41170,#41171,#41172,#41173));
#9465=EDGE_LOOP('',(#41174,#41175,#41176,#41177));
#9466=EDGE_LOOP('',(#41178,#41179,#41180,#41181));
#9467=EDGE_LOOP('',(#41182,#41183,#41184,#41185));
#9468=EDGE_LOOP('',(#41186,#41187,#41188,#41189));
#9469=EDGE_LOOP('',(#41190,#41191,#41192,#41193));
#9470=EDGE_LOOP('',(#41194,#41195,#41196,#41197));
#9471=EDGE_LOOP('',(#41198,#41199,#41200,#41201));
#9472=EDGE_LOOP('',(#41202,#41203,#41204,#41205));
#9473=EDGE_LOOP('',(#41206,#41207,#41208,#41209));
#9474=EDGE_LOOP('',(#41210,#41211,#41212,#41213));
#9475=EDGE_LOOP('',(#41214,#41215,#41216,#41217));
#9476=EDGE_LOOP('',(#41218,#41219,#41220,#41221));
#9477=EDGE_LOOP('',(#41222,#41223,#41224,#41225));
#9478=EDGE_LOOP('',(#41226,#41227,#41228,#41229));
#9479=EDGE_LOOP('',(#41230,#41231,#41232,#41233));
#9480=EDGE_LOOP('',(#41234,#41235,#41236,#41237));
#9481=EDGE_LOOP('',(#41238,#41239,#41240,#41241));
#9482=EDGE_LOOP('',(#41242,#41243,#41244,#41245));
#9483=EDGE_LOOP('',(#41246,#41247,#41248,#41249));
#9484=EDGE_LOOP('',(#41250,#41251,#41252,#41253));
#9485=EDGE_LOOP('',(#41254,#41255,#41256,#41257));
#9486=EDGE_LOOP('',(#41258,#41259,#41260,#41261));
#9487=EDGE_LOOP('',(#41262,#41263,#41264,#41265));
#9488=EDGE_LOOP('',(#41266,#41267,#41268,#41269));
#9489=EDGE_LOOP('',(#41270,#41271,#41272,#41273));
#9490=EDGE_LOOP('',(#41274,#41275,#41276,#41277));
#9491=EDGE_LOOP('',(#41278,#41279,#41280,#41281));
#9492=EDGE_LOOP('',(#41282,#41283,#41284,#41285));
#9493=EDGE_LOOP('',(#41286,#41287,#41288,#41289));
#9494=EDGE_LOOP('',(#41290,#41291,#41292,#41293));
#9495=EDGE_LOOP('',(#41294,#41295,#41296,#41297));
#9496=EDGE_LOOP('',(#41298,#41299,#41300,#41301));
#9497=EDGE_LOOP('',(#41302,#41303,#41304,#41305));
#9498=EDGE_LOOP('',(#41306,#41307,#41308,#41309));
#9499=EDGE_LOOP('',(#41310,#41311,#41312,#41313));
#9500=EDGE_LOOP('',(#41314,#41315,#41316,#41317));
#9501=EDGE_LOOP('',(#41318,#41319,#41320,#41321));
#9502=EDGE_LOOP('',(#41322,#41323,#41324,#41325));
#9503=EDGE_LOOP('',(#41326,#41327,#41328,#41329));
#9504=EDGE_LOOP('',(#41330,#41331,#41332,#41333));
#9505=EDGE_LOOP('',(#41334,#41335,#41336,#41337));
#9506=EDGE_LOOP('',(#41338,#41339,#41340,#41341));
#9507=EDGE_LOOP('',(#41342,#41343,#41344,#41345));
#9508=EDGE_LOOP('',(#41346,#41347,#41348,#41349));
#9509=EDGE_LOOP('',(#41350,#41351,#41352,#41353));
#9510=EDGE_LOOP('',(#41354,#41355,#41356,#41357,#41358,#41359,#41360,#41361,
#41362,#41363,#41364,#41365));
#9511=EDGE_LOOP('',(#41366,#41367,#41368,#41369));
#9512=EDGE_LOOP('',(#41370));
#9513=EDGE_LOOP('',(#41371,#41372,#41373,#41374));
#9514=EDGE_LOOP('',(#41375,#41376,#41377,#41378));
#9515=EDGE_LOOP('',(#41379,#41380,#41381,#41382));
#9516=EDGE_LOOP('',(#41383));
#9517=EDGE_LOOP('',(#41384,#41385,#41386,#41387,#41388,#41389,#41390,#41391,
#41392));
#9518=EDGE_LOOP('',(#41393,#41394,#41395,#41396));
#9519=EDGE_LOOP('',(#41397,#41398,#41399,#41400));
#9520=EDGE_LOOP('',(#41401,#41402,#41403,#41404));
#9521=EDGE_LOOP('',(#41405,#41406,#41407,#41408,#41409,#41410));
#9522=EDGE_LOOP('',(#41411,#41412,#41413,#41414));
#9523=EDGE_LOOP('',(#41415,#41416,#41417,#41418));
#9524=EDGE_LOOP('',(#41419,#41420,#41421,#41422));
#9525=EDGE_LOOP('',(#41423,#41424,#41425,#41426));
#9526=EDGE_LOOP('',(#41427,#41428,#41429,#41430,#41431,#41432,#41433,#41434,
#41435,#41436));
#9527=EDGE_LOOP('',(#41437,#41438,#41439,#41440));
#9528=EDGE_LOOP('',(#41441,#41442,#41443,#41444,#41445,#41446,#41447,#41448));
#9529=EDGE_LOOP('',(#41449,#41450,#41451,#41452,#41453,#41454,#41455,#41456));
#9530=EDGE_LOOP('',(#41457,#41458,#41459,#41460));
#9531=EDGE_LOOP('',(#41461,#41462,#41463,#41464,#41465,#41466,#41467,#41468,
#41469));
#9532=EDGE_LOOP('',(#41470,#41471,#41472,#41473,#41474,#41475,#41476,#41477,
#41478,#41479,#41480,#41481,#41482,#41483,#41484));
#9533=EDGE_LOOP('',(#41485,#41486,#41487,#41488,#41489,#41490));
#9534=EDGE_LOOP('',(#41491,#41492,#41493,#41494,#41495));
#9535=EDGE_LOOP('',(#41496,#41497,#41498,#41499));
#9536=EDGE_LOOP('',(#41500,#41501,#41502,#41503,#41504,#41505,#41506,#41507,
#41508,#41509,#41510,#41511,#41512));
#9537=EDGE_LOOP('',(#41513,#41514,#41515,#41516,#41517,#41518));
#9538=EDGE_LOOP('',(#41519,#41520,#41521,#41522,#41523));
#9539=EDGE_LOOP('',(#41524,#41525,#41526,#41527));
#9540=EDGE_LOOP('',(#41528,#41529,#41530,#41531,#41532,#41533));
#9541=EDGE_LOOP('',(#41534,#41535,#41536,#41537,#41538,#41539,#41540,#41541));
#9542=EDGE_LOOP('',(#41542,#41543,#41544,#41545,#41546,#41547,#41548,#41549));
#9543=EDGE_LOOP('',(#41550));
#9544=EDGE_LOOP('',(#41551));
#9545=EDGE_LOOP('',(#41552));
#9546=EDGE_LOOP('',(#41553,#41554,#41555,#41556,#41557,#41558,#41559,#41560,
#41561,#41562,#41563,#41564,#41565,#41566,#41567,#41568,#41569,#41570,#41571,
#41572,#41573,#41574,#41575,#41576,#41577,#41578,#41579,#41580,#41581,#41582,
#41583,#41584,#41585,#41586,#41587));
#9547=EDGE_LOOP('',(#41588));
#9548=EDGE_LOOP('',(#41589));
#9549=EDGE_LOOP('',(#41590));
#9550=EDGE_LOOP('',(#41591));
#9551=EDGE_LOOP('',(#41592));
#9552=EDGE_LOOP('',(#41593));
#9553=EDGE_LOOP('',(#41594,#41595,#41596,#41597));
#9554=EDGE_LOOP('',(#41598,#41599,#41600,#41601,#41602,#41603,#41604,#41605,
#41606,#41607));
#9555=EDGE_LOOP('',(#41608,#41609,#41610,#41611));
#9556=EDGE_LOOP('',(#41612,#41613,#41614,#41615,#41616,#41617,#41618,#41619,
#41620,#41621));
#9557=EDGE_LOOP('',(#41622));
#9558=EDGE_LOOP('',(#41623,#41624,#41625,#41626,#41627));
#9559=EDGE_LOOP('',(#41628,#41629,#41630,#41631,#41632,#41633));
#9560=EDGE_LOOP('',(#41634,#41635,#41636,#41637));
#9561=EDGE_LOOP('',(#41638,#41639,#41640,#41641));
#9562=EDGE_LOOP('',(#41642,#41643,#41644,#41645));
#9563=EDGE_LOOP('',(#41646));
#9564=EDGE_LOOP('',(#41647,#41648,#41649,#41650));
#9565=EDGE_LOOP('',(#41651,#41652,#41653,#41654));
#9566=EDGE_LOOP('',(#41655,#41656,#41657,#41658));
#9567=EDGE_LOOP('',(#41659,#41660,#41661,#41662));
#9568=EDGE_LOOP('',(#41663,#41664,#41665,#41666));
#9569=EDGE_LOOP('',(#41667,#41668,#41669,#41670,#41671));
#9570=EDGE_LOOP('',(#41672,#41673,#41674,#41675));
#9571=EDGE_LOOP('',(#41676,#41677,#41678,#41679,#41680));
#9572=EDGE_LOOP('',(#41681));
#9573=EDGE_LOOP('',(#41682));
#9574=EDGE_LOOP('',(#41683));
#9575=EDGE_LOOP('',(#41684));
#9576=EDGE_LOOP('',(#41685));
#9577=EDGE_LOOP('',(#41686));
#9578=EDGE_LOOP('',(#41687,#41688,#41689,#41690,#41691,#41692,#41693));
#9579=EDGE_LOOP('',(#41694,#41695,#41696,#41697));
#9580=EDGE_LOOP('',(#41698,#41699,#41700,#41701));
#9581=EDGE_LOOP('',(#41702,#41703,#41704,#41705));
#9582=EDGE_LOOP('',(#41706,#41707,#41708,#41709));
#9583=EDGE_LOOP('',(#41710,#41711,#41712,#41713));
#9584=EDGE_LOOP('',(#41714,#41715,#41716,#41717,#41718,#41719));
#9585=EDGE_LOOP('',(#41720,#41721,#41722,#41723));
#9586=EDGE_LOOP('',(#41724,#41725,#41726,#41727,#41728,#41729,#41730,#41731,
#41732,#41733,#41734,#41735,#41736,#41737,#41738));
#9587=EDGE_LOOP('',(#41739,#41740,#41741,#41742));
#9588=EDGE_LOOP('',(#41743,#41744,#41745,#41746));
#9589=EDGE_LOOP('',(#41747,#41748,#41749,#41750));
#9590=EDGE_LOOP('',(#41751,#41752,#41753,#41754));
#9591=EDGE_LOOP('',(#41755,#41756,#41757,#41758));
#9592=EDGE_LOOP('',(#41759,#41760,#41761,#41762));
#9593=EDGE_LOOP('',(#41763,#41764,#41765,#41766,#41767));
#9594=EDGE_LOOP('',(#41768,#41769,#41770,#41771));
#9595=EDGE_LOOP('',(#41772,#41773,#41774,#41775,#41776,#41777,#41778));
#9596=EDGE_LOOP('',(#41779,#41780,#41781,#41782));
#9597=EDGE_LOOP('',(#41783,#41784,#41785,#41786));
#9598=EDGE_LOOP('',(#41787,#41788,#41789,#41790));
#9599=EDGE_LOOP('',(#41791,#41792,#41793,#41794));
#9600=EDGE_LOOP('',(#41795,#41796,#41797,#41798));
#9601=EDGE_LOOP('',(#41799,#41800,#41801,#41802));
#9602=EDGE_LOOP('',(#41803,#41804,#41805,#41806,#41807,#41808,#41809,#41810));
#9603=EDGE_LOOP('',(#41811,#41812,#41813,#41814));
#9604=EDGE_LOOP('',(#41815));
#9605=EDGE_LOOP('',(#41816,#41817,#41818,#41819));
#9606=EDGE_LOOP('',(#41820));
#9607=EDGE_LOOP('',(#41821));
#9608=EDGE_LOOP('',(#41822));
#9609=EDGE_LOOP('',(#41823));
#9610=EDGE_LOOP('',(#41824,#41825,#41826,#41827));
#9611=EDGE_LOOP('',(#41828,#41829,#41830,#41831));
#9612=EDGE_LOOP('',(#41832,#41833,#41834,#41835));
#9613=EDGE_LOOP('',(#41836,#41837,#41838,#41839));
#9614=EDGE_LOOP('',(#41840,#41841,#41842,#41843));
#9615=EDGE_LOOP('',(#41844,#41845,#41846,#41847));
#9616=EDGE_LOOP('',(#41848,#41849,#41850,#41851));
#9617=EDGE_LOOP('',(#41852,#41853,#41854,#41855));
#9618=EDGE_LOOP('',(#41856,#41857,#41858,#41859,#41860,#41861,#41862,#41863));
#9619=EDGE_LOOP('',(#41864,#41865,#41866,#41867));
#9620=EDGE_LOOP('',(#41868,#41869,#41870,#41871,#41872,#41873,#41874));
#9621=EDGE_LOOP('',(#41875,#41876,#41877,#41878,#41879,#41880,#41881,#41882));
#9622=EDGE_LOOP('',(#41883,#41884,#41885,#41886));
#9623=EDGE_LOOP('',(#41887,#41888,#41889,#41890,#41891,#41892,#41893,#41894,
#41895,#41896,#41897,#41898));
#9624=EDGE_LOOP('',(#41899,#41900,#41901,#41902,#41903));
#9625=EDGE_LOOP('',(#41904,#41905,#41906,#41907,#41908));
#9626=EDGE_LOOP('',(#41909,#41910,#41911,#41912));
#9627=EDGE_LOOP('',(#41913,#41914,#41915));
#9628=EDGE_LOOP('',(#41916,#41917,#41918,#41919));
#9629=EDGE_LOOP('',(#41920,#41921,#41922,#41923));
#9630=EDGE_LOOP('',(#41924,#41925,#41926,#41927,#41928,#41929));
#9631=EDGE_LOOP('',(#41930,#41931,#41932,#41933,#41934,#41935));
#9632=EDGE_LOOP('',(#41936));
#9633=EDGE_LOOP('',(#41937));
#9634=EDGE_LOOP('',(#41938,#41939,#41940,#41941,#41942));
#9635=EDGE_LOOP('',(#41943,#41944,#41945,#41946));
#9636=EDGE_LOOP('',(#41947,#41948,#41949,#41950,#41951));
#9637=EDGE_LOOP('',(#41952,#41953,#41954,#41955));
#9638=EDGE_LOOP('',(#41956,#41957,#41958,#41959));
#9639=LINE('',#61802,#11623);
#9640=LINE('',#61808,#11624);
#9641=LINE('',#63374,#11625);
#9642=LINE('',#63383,#11626);
#9643=LINE('',#63416,#11627);
#9644=LINE('',#63425,#11628);
#9645=LINE('',#63428,#11629);
#9646=LINE('',#63434,#11630);
#9647=LINE('',#63437,#11631);
#9648=LINE('',#63440,#11632);
#9649=LINE('',#63442,#11633);
#9650=LINE('',#63444,#11634);
#9651=LINE('',#63446,#11635);
#9652=LINE('',#63447,#11636);
#9653=LINE('',#63449,#11637);
#9654=LINE('',#63452,#11638);
#9655=LINE('',#63457,#11639);
#9656=LINE('',#63461,#11640);
#9657=LINE('',#63463,#11641);
#9658=LINE('',#63464,#11642);
#9659=LINE('',#63467,#11643);
#9660=LINE('',#63469,#11644);
#9661=LINE('',#63470,#11645);
#9662=LINE('',#63474,#11646);
#9663=LINE('',#63476,#11647);
#9664=LINE('',#63478,#11648);
#9665=LINE('',#63480,#11649);
#9666=LINE('',#63482,#11650);
#9667=LINE('',#63483,#11651);
#9668=LINE('',#63485,#11652);
#9669=LINE('',#63488,#11653);
#9670=LINE('',#63491,#11654);
#9671=LINE('',#63492,#11655);
#9672=LINE('',#63494,#11656);
#9673=LINE('',#63495,#11657);
#9674=LINE('',#63498,#11658);
#9675=LINE('',#63499,#11659);
#9676=LINE('',#63502,#11660);
#9677=LINE('',#63503,#11661);
#9678=LINE('',#63505,#11662);
#9679=LINE('',#63507,#11663);
#9680=LINE('',#63509,#11664);
#9681=LINE('',#63510,#11665);
#9682=LINE('',#63514,#11666);
#9683=LINE('',#63516,#11667);
#9684=LINE('',#63518,#11668);
#9685=LINE('',#63520,#11669);
#9686=LINE('',#63527,#11670);
#9687=LINE('',#63539,#11671);
#9688=LINE('',#64446,#11672);
#9689=LINE('',#65232,#11673);
#9690=LINE('',#65258,#11674);
#9691=LINE('',#65271,#11675);
#9692=LINE('',#65276,#11676);
#9693=LINE('',#65296,#11677);
#9694=LINE('',#65325,#11678);
#9695=LINE('',#65343,#11679);
#9696=LINE('',#65374,#11680);
#9697=LINE('',#65410,#11681);
#9698=LINE('',#65415,#11682);
#9699=LINE('',#65430,#11683);
#9700=LINE('',#65435,#11684);
#9701=LINE('',#65452,#11685);
#9702=LINE('',#65481,#11686);
#9703=LINE('',#65500,#11687);
#9704=LINE('',#65511,#11688);
#9705=LINE('',#65566,#11689);
#9706=LINE('',#65571,#11690);
#9707=LINE('',#65583,#11691);
#9708=LINE('',#65588,#11692);
#9709=LINE('',#65605,#11693);
#9710=LINE('',#65634,#11694);
#9711=LINE('',#65664,#11695);
#9712=LINE('',#65675,#11696);
#9713=LINE('',#65713,#11697);
#9714=LINE('',#65718,#11698);
#9715=LINE('',#65739,#11699);
#9716=LINE('',#65757,#11700);
#9717=LINE('',#65774,#11701);
#9718=LINE('',#65803,#11702);
#9719=LINE('',#65829,#11703);
#9720=LINE('',#65841,#11704);
#9721=LINE('',#65894,#11705);
#9722=LINE('',#65899,#11706);
#9723=LINE('',#65914,#11707);
#9724=LINE('',#65919,#11708);
#9725=LINE('',#65936,#11709);
#9726=LINE('',#65965,#11710);
#9727=LINE('',#65991,#11711);
#9728=LINE('',#66009,#11712);
#9729=LINE('',#66045,#11713);
#9730=LINE('',#66050,#11714);
#9731=LINE('',#66072,#11715);
#9732=LINE('',#66077,#11716);
#9733=LINE('',#66094,#11717);
#9734=LINE('',#66123,#11718);
#9735=LINE('',#66141,#11719);
#9736=LINE('',#66159,#11720);
#9737=LINE('',#66178,#11721);
#9738=LINE('',#66194,#11722);
#9739=LINE('',#66199,#11723);
#9740=LINE('',#66224,#11724);
#9741=LINE('',#66241,#11725);
#9742=LINE('',#66273,#11726);
#9743=LINE('',#66299,#11727);
#9744=LINE('',#66317,#11728);
#9745=LINE('',#66322,#11729);
#9746=LINE('',#66339,#11730);
#9747=LINE('',#66373,#11731);
#9748=LINE('',#66388,#11732);
#9749=LINE('',#66393,#11733);
#9750=LINE('',#66412,#11734);
#9751=LINE('',#66435,#11735);
#9752=LINE('',#66481,#11736);
#9753=LINE('',#66486,#11737);
#9754=LINE('',#66503,#11738);
#9755=LINE('',#66539,#11739);
#9756=LINE('',#66562,#11740);
#9757=LINE('',#66567,#11741);
#9758=LINE('',#66584,#11742);
#9759=LINE('',#66609,#11743);
#9760=LINE('',#66637,#11744);
#9761=LINE('',#66642,#11745);
#9762=LINE('',#66659,#11746);
#9763=LINE('',#66691,#11747);
#9764=LINE('',#66715,#11748);
#9765=LINE('',#66720,#11749);
#9766=LINE('',#66737,#11750);
#9767=LINE('',#66761,#11751);
#9768=LINE('',#66765,#11752);
#9769=LINE('',#66799,#11753);
#9770=LINE('',#66825,#11754);
#9771=LINE('',#66843,#11755);
#9772=LINE('',#66848,#11756);
#9773=LINE('',#66865,#11757);
#9774=LINE('',#66899,#11758);
#9775=LINE('',#66920,#11759);
#9776=LINE('',#66925,#11760);
#9777=LINE('',#66942,#11761);
#9778=LINE('',#66967,#11762);
#9779=LINE('',#67001,#11763);
#9780=LINE('',#67006,#11764);
#9781=LINE('',#67036,#11765);
#9782=LINE('',#67059,#11766);
#9783=LINE('',#67091,#11767);
#9784=LINE('',#67096,#11768);
#9785=LINE('',#67113,#11769);
#9786=LINE('',#67138,#11770);
#9787=LINE('',#67166,#11771);
#9788=LINE('',#67171,#11772);
#9789=LINE('',#67188,#11773);
#9790=LINE('',#67213,#11774);
#9791=LINE('',#67237,#11775);
#9792=LINE('',#67242,#11776);
#9793=LINE('',#67259,#11777);
#9794=LINE('',#67283,#11778);
#9795=LINE('',#67287,#11779);
#9796=LINE('',#67321,#11780);
#9797=LINE('',#67347,#11781);
#9798=LINE('',#67365,#11782);
#9799=LINE('',#67370,#11783);
#9800=LINE('',#67387,#11784);
#9801=LINE('',#67421,#11785);
#9802=LINE('',#67442,#11786);
#9803=LINE('',#67447,#11787);
#9804=LINE('',#67464,#11788);
#9805=LINE('',#67489,#11789);
#9806=LINE('',#67529,#11790);
#9807=LINE('',#67534,#11791);
#9808=LINE('',#67551,#11792);
#9809=LINE('',#67587,#11793);
#9810=LINE('',#67602,#11794);
#9811=LINE('',#67607,#11795);
#9812=LINE('',#67626,#11796);
#9813=LINE('',#67654,#11797);
#9814=LINE('',#67688,#11798);
#9815=LINE('',#67693,#11799);
#9816=LINE('',#67710,#11800);
#9817=LINE('',#67735,#11801);
#9818=LINE('',#67756,#11802);
#9819=LINE('',#67761,#11803);
#9820=LINE('',#67778,#11804);
#9821=LINE('',#67795,#11805);
#9822=LINE('',#67799,#11806);
#9823=LINE('',#67833,#11807);
#9824=LINE('',#67859,#11808);
#9825=LINE('',#67877,#11809);
#9826=LINE('',#67882,#11810);
#9827=LINE('',#67899,#11811);
#9828=LINE('',#67933,#11812);
#9829=LINE('',#67954,#11813);
#9830=LINE('',#67959,#11814);
#9831=LINE('',#67976,#11815);
#9832=LINE('',#68001,#11816);
#9833=LINE('',#68041,#11817);
#9834=LINE('',#68046,#11818);
#9835=LINE('',#68063,#11819);
#9836=LINE('',#68099,#11820);
#9837=LINE('',#68125,#11821);
#9838=LINE('',#68130,#11822);
#9839=LINE('',#68147,#11823);
#9840=LINE('',#68172,#11824);
#9841=LINE('',#68194,#11825);
#9842=LINE('',#68199,#11826);
#9843=LINE('',#68218,#11827);
#9844=LINE('',#68241,#11828);
#9845=LINE('',#68268,#11829);
#9846=LINE('',#68273,#11830);
#9847=LINE('',#68290,#11831);
#9848=LINE('',#68307,#11832);
#9849=LINE('',#68311,#11833);
#9850=LINE('',#68345,#11834);
#9851=LINE('',#68371,#11835);
#9852=LINE('',#68389,#11836);
#9853=LINE('',#68394,#11837);
#9854=LINE('',#68411,#11838);
#9855=LINE('',#68445,#11839);
#9856=LINE('',#68466,#11840);
#9857=LINE('',#68471,#11841);
#9858=LINE('',#68488,#11842);
#9859=LINE('',#68513,#11843);
#9860=LINE('',#68553,#11844);
#9861=LINE('',#68558,#11845);
#9862=LINE('',#68575,#11846);
#9863=LINE('',#68611,#11847);
#9864=LINE('',#68637,#11848);
#9865=LINE('',#68642,#11849);
#9866=LINE('',#68659,#11850);
#9867=LINE('',#68684,#11851);
#9868=LINE('',#68712,#11852);
#9869=LINE('',#68717,#11853);
#9870=LINE('',#68734,#11854);
#9871=LINE('',#68759,#11855);
#9872=LINE('',#68777,#11856);
#9873=LINE('',#68782,#11857);
#9874=LINE('',#68793,#11858);
#9875=LINE('',#68816,#11859);
#9876=LINE('',#68826,#11860);
#9877=LINE('',#68860,#11861);
#9878=LINE('',#68886,#11862);
#9879=LINE('',#68904,#11863);
#9880=LINE('',#68909,#11864);
#9881=LINE('',#68926,#11865);
#9882=LINE('',#68960,#11866);
#9883=LINE('',#68981,#11867);
#9884=LINE('',#68986,#11868);
#9885=LINE('',#69003,#11869);
#9886=LINE('',#69028,#11870);
#9887=LINE('',#69068,#11871);
#9888=LINE('',#69073,#11872);
#9889=LINE('',#69090,#11873);
#9890=LINE('',#69126,#11874);
#9891=LINE('',#69152,#11875);
#9892=LINE('',#69157,#11876);
#9893=LINE('',#69174,#11877);
#9894=LINE('',#69199,#11878);
#9895=LINE('',#69227,#11879);
#9896=LINE('',#69232,#11880);
#9897=LINE('',#69249,#11881);
#9898=LINE('',#69274,#11882);
#9899=LINE('',#69298,#11883);
#9900=LINE('',#69303,#11884);
#9901=LINE('',#69320,#11885);
#9902=LINE('',#69337,#11886);
#9903=LINE('',#69341,#11887);
#9904=LINE('',#69375,#11888);
#9905=LINE('',#69401,#11889);
#9906=LINE('',#69419,#11890);
#9907=LINE('',#69424,#11891);
#9908=LINE('',#69441,#11892);
#9909=LINE('',#69475,#11893);
#9910=LINE('',#69496,#11894);
#9911=LINE('',#69501,#11895);
#9912=LINE('',#69518,#11896);
#9913=LINE('',#69543,#11897);
#9914=LINE('',#69583,#11898);
#9915=LINE('',#69588,#11899);
#9916=LINE('',#69605,#11900);
#9917=LINE('',#69641,#11901);
#9918=LINE('',#69667,#11902);
#9919=LINE('',#69672,#11903);
#9920=LINE('',#69689,#11904);
#9921=LINE('',#69714,#11905);
#9922=LINE('',#69742,#11906);
#9923=LINE('',#69747,#11907);
#9924=LINE('',#69764,#11908);
#9925=LINE('',#69789,#11909);
#9926=LINE('',#69813,#11910);
#9927=LINE('',#69818,#11911);
#9928=LINE('',#69835,#11912);
#9929=LINE('',#69852,#11913);
#9930=LINE('',#69856,#11914);
#9931=LINE('',#69890,#11915);
#9932=LINE('',#69916,#11916);
#9933=LINE('',#69934,#11917);
#9934=LINE('',#69939,#11918);
#9935=LINE('',#69956,#11919);
#9936=LINE('',#69990,#11920);
#9937=LINE('',#70011,#11921);
#9938=LINE('',#70016,#11922);
#9939=LINE('',#70033,#11923);
#9940=LINE('',#70058,#11924);
#9941=LINE('',#70098,#11925);
#9942=LINE('',#70103,#11926);
#9943=LINE('',#70120,#11927);
#9944=LINE('',#70156,#11928);
#9945=LINE('',#70182,#11929);
#9946=LINE('',#70187,#11930);
#9947=LINE('',#70204,#11931);
#9948=LINE('',#70229,#11932);
#9949=LINE('',#70257,#11933);
#9950=LINE('',#70262,#11934);
#9951=LINE('',#70279,#11935);
#9952=LINE('',#70304,#11936);
#9953=LINE('',#70328,#11937);
#9954=LINE('',#70333,#11938);
#9955=LINE('',#70350,#11939);
#9956=LINE('',#70367,#11940);
#9957=LINE('',#70371,#11941);
#9958=LINE('',#70405,#11942);
#9959=LINE('',#70431,#11943);
#9960=LINE('',#70449,#11944);
#9961=LINE('',#70454,#11945);
#9962=LINE('',#70471,#11946);
#9963=LINE('',#70505,#11947);
#9964=LINE('',#70526,#11948);
#9965=LINE('',#70531,#11949);
#9966=LINE('',#70548,#11950);
#9967=LINE('',#70573,#11951);
#9968=LINE('',#70613,#11952);
#9969=LINE('',#70618,#11953);
#9970=LINE('',#70635,#11954);
#9971=LINE('',#70671,#11955);
#9972=LINE('',#70697,#11956);
#9973=LINE('',#70702,#11957);
#9974=LINE('',#70719,#11958);
#9975=LINE('',#70744,#11959);
#9976=LINE('',#70772,#11960);
#9977=LINE('',#70777,#11961);
#9978=LINE('',#70794,#11962);
#9979=LINE('',#70819,#11963);
#9980=LINE('',#70843,#11964);
#9981=LINE('',#70848,#11965);
#9982=LINE('',#70865,#11966);
#9983=LINE('',#70882,#11967);
#9984=LINE('',#70886,#11968);
#9985=LINE('',#70920,#11969);
#9986=LINE('',#70946,#11970);
#9987=LINE('',#70964,#11971);
#9988=LINE('',#70969,#11972);
#9989=LINE('',#70986,#11973);
#9990=LINE('',#71020,#11974);
#9991=LINE('',#71041,#11975);
#9992=LINE('',#71046,#11976);
#9993=LINE('',#71063,#11977);
#9994=LINE('',#71088,#11978);
#9995=LINE('',#71128,#11979);
#9996=LINE('',#71133,#11980);
#9997=LINE('',#71150,#11981);
#9998=LINE('',#71186,#11982);
#9999=LINE('',#71212,#11983);
#10000=LINE('',#71217,#11984);
#10001=LINE('',#71234,#11985);
#10002=LINE('',#71259,#11986);
#10003=LINE('',#71287,#11987);
#10004=LINE('',#71292,#11988);
#10005=LINE('',#71309,#11989);
#10006=LINE('',#71334,#11990);
#10007=LINE('',#71358,#11991);
#10008=LINE('',#71363,#11992);
#10009=LINE('',#71380,#11993);
#10010=LINE('',#71397,#11994);
#10011=LINE('',#71401,#11995);
#10012=LINE('',#71435,#11996);
#10013=LINE('',#71461,#11997);
#10014=LINE('',#71479,#11998);
#10015=LINE('',#71484,#11999);
#10016=LINE('',#71501,#12000);
#10017=LINE('',#71535,#12001);
#10018=LINE('',#71556,#12002);
#10019=LINE('',#71561,#12003);
#10020=LINE('',#71578,#12004);
#10021=LINE('',#71603,#12005);
#10022=LINE('',#71643,#12006);
#10023=LINE('',#71648,#12007);
#10024=LINE('',#71665,#12008);
#10025=LINE('',#71701,#12009);
#10026=LINE('',#71727,#12010);
#10027=LINE('',#71732,#12011);
#10028=LINE('',#71749,#12012);
#10029=LINE('',#71774,#12013);
#10030=LINE('',#71802,#12014);
#10031=LINE('',#71807,#12015);
#10032=LINE('',#71824,#12016);
#10033=LINE('',#71849,#12017);
#10034=LINE('',#71873,#12018);
#10035=LINE('',#71878,#12019);
#10036=LINE('',#71895,#12020);
#10037=LINE('',#71912,#12021);
#10038=LINE('',#71916,#12022);
#10039=LINE('',#71950,#12023);
#10040=LINE('',#71976,#12024);
#10041=LINE('',#71994,#12025);
#10042=LINE('',#71999,#12026);
#10043=LINE('',#72016,#12027);
#10044=LINE('',#72050,#12028);
#10045=LINE('',#72071,#12029);
#10046=LINE('',#72076,#12030);
#10047=LINE('',#72093,#12031);
#10048=LINE('',#72118,#12032);
#10049=LINE('',#72158,#12033);
#10050=LINE('',#72163,#12034);
#10051=LINE('',#72180,#12035);
#10052=LINE('',#72216,#12036);
#10053=LINE('',#72242,#12037);
#10054=LINE('',#72247,#12038);
#10055=LINE('',#72264,#12039);
#10056=LINE('',#72289,#12040);
#10057=LINE('',#72317,#12041);
#10058=LINE('',#72322,#12042);
#10059=LINE('',#72339,#12043);
#10060=LINE('',#72364,#12044);
#10061=LINE('',#72388,#12045);
#10062=LINE('',#72393,#12046);
#10063=LINE('',#72410,#12047);
#10064=LINE('',#72427,#12048);
#10065=LINE('',#72431,#12049);
#10066=LINE('',#72465,#12050);
#10067=LINE('',#72491,#12051);
#10068=LINE('',#72509,#12052);
#10069=LINE('',#72514,#12053);
#10070=LINE('',#72531,#12054);
#10071=LINE('',#72565,#12055);
#10072=LINE('',#72586,#12056);
#10073=LINE('',#72591,#12057);
#10074=LINE('',#72608,#12058);
#10075=LINE('',#72633,#12059);
#10076=LINE('',#72673,#12060);
#10077=LINE('',#72678,#12061);
#10078=LINE('',#72695,#12062);
#10079=LINE('',#72731,#12063);
#10080=LINE('',#72757,#12064);
#10081=LINE('',#72762,#12065);
#10082=LINE('',#72779,#12066);
#10083=LINE('',#72804,#12067);
#10084=LINE('',#72832,#12068);
#10085=LINE('',#72837,#12069);
#10086=LINE('',#72854,#12070);
#10087=LINE('',#72879,#12071);
#10088=LINE('',#72903,#12072);
#10089=LINE('',#72908,#12073);
#10090=LINE('',#72925,#12074);
#10091=LINE('',#72942,#12075);
#10092=LINE('',#72946,#12076);
#10093=LINE('',#72980,#12077);
#10094=LINE('',#73006,#12078);
#10095=LINE('',#73024,#12079);
#10096=LINE('',#73029,#12080);
#10097=LINE('',#73046,#12081);
#10098=LINE('',#73080,#12082);
#10099=LINE('',#73098,#12083);
#10100=LINE('',#73103,#12084);
#10101=LINE('',#73120,#12085);
#10102=LINE('',#73152,#12086);
#10103=LINE('',#73192,#12087);
#10104=LINE('',#73197,#12088);
#10105=LINE('',#73214,#12089);
#10106=LINE('',#73250,#12090);
#10107=LINE('',#73276,#12091);
#10108=LINE('',#73281,#12092);
#10109=LINE('',#73298,#12093);
#10110=LINE('',#73323,#12094);
#10111=LINE('',#73351,#12095);
#10112=LINE('',#73356,#12096);
#10113=LINE('',#73373,#12097);
#10114=LINE('',#73398,#12098);
#10115=LINE('',#73422,#12099);
#10116=LINE('',#73427,#12100);
#10117=LINE('',#73444,#12101);
#10118=LINE('',#73461,#12102);
#10119=LINE('',#73465,#12103);
#10120=LINE('',#73499,#12104);
#10121=LINE('',#73525,#12105);
#10122=LINE('',#73543,#12106);
#10123=LINE('',#73548,#12107);
#10124=LINE('',#73565,#12108);
#10125=LINE('',#73599,#12109);
#10126=LINE('',#73620,#12110);
#10127=LINE('',#73625,#12111);
#10128=LINE('',#73642,#12112);
#10129=LINE('',#73667,#12113);
#10130=LINE('',#73707,#12114);
#10131=LINE('',#73712,#12115);
#10132=LINE('',#73729,#12116);
#10133=LINE('',#73765,#12117);
#10134=LINE('',#73791,#12118);
#10135=LINE('',#73796,#12119);
#10136=LINE('',#73813,#12120);
#10137=LINE('',#73838,#12121);
#10138=LINE('',#73866,#12122);
#10139=LINE('',#73871,#12123);
#10140=LINE('',#73888,#12124);
#10141=LINE('',#73913,#12125);
#10142=LINE('',#73937,#12126);
#10143=LINE('',#73942,#12127);
#10144=LINE('',#73959,#12128);
#10145=LINE('',#73976,#12129);
#10146=LINE('',#73980,#12130);
#10147=LINE('',#74014,#12131);
#10148=LINE('',#74040,#12132);
#10149=LINE('',#74058,#12133);
#10150=LINE('',#74063,#12134);
#10151=LINE('',#74080,#12135);
#10152=LINE('',#74114,#12136);
#10153=LINE('',#74135,#12137);
#10154=LINE('',#74140,#12138);
#10155=LINE('',#74157,#12139);
#10156=LINE('',#74182,#12140);
#10157=LINE('',#74222,#12141);
#10158=LINE('',#74227,#12142);
#10159=LINE('',#74244,#12143);
#10160=LINE('',#74280,#12144);
#10161=LINE('',#74306,#12145);
#10162=LINE('',#74311,#12146);
#10163=LINE('',#74328,#12147);
#10164=LINE('',#74353,#12148);
#10165=LINE('',#74381,#12149);
#10166=LINE('',#74386,#12150);
#10167=LINE('',#74403,#12151);
#10168=LINE('',#74428,#12152);
#10169=LINE('',#74452,#12153);
#10170=LINE('',#74457,#12154);
#10171=LINE('',#74474,#12155);
#10172=LINE('',#74491,#12156);
#10173=LINE('',#74495,#12157);
#10174=LINE('',#74529,#12158);
#10175=LINE('',#74555,#12159);
#10176=LINE('',#74573,#12160);
#10177=LINE('',#74578,#12161);
#10178=LINE('',#74595,#12162);
#10179=LINE('',#74629,#12163);
#10180=LINE('',#74650,#12164);
#10181=LINE('',#74655,#12165);
#10182=LINE('',#74672,#12166);
#10183=LINE('',#74697,#12167);
#10184=LINE('',#74737,#12168);
#10185=LINE('',#74742,#12169);
#10186=LINE('',#74759,#12170);
#10187=LINE('',#74795,#12171);
#10188=LINE('',#74821,#12172);
#10189=LINE('',#74826,#12173);
#10190=LINE('',#74843,#12174);
#10191=LINE('',#74868,#12175);
#10192=LINE('',#74896,#12176);
#10193=LINE('',#74901,#12177);
#10194=LINE('',#74918,#12178);
#10195=LINE('',#74943,#12179);
#10196=LINE('',#74967,#12180);
#10197=LINE('',#74972,#12181);
#10198=LINE('',#74989,#12182);
#10199=LINE('',#75006,#12183);
#10200=LINE('',#75010,#12184);
#10201=LINE('',#75044,#12185);
#10202=LINE('',#75070,#12186);
#10203=LINE('',#75088,#12187);
#10204=LINE('',#75093,#12188);
#10205=LINE('',#75110,#12189);
#10206=LINE('',#75144,#12190);
#10207=LINE('',#75165,#12191);
#10208=LINE('',#75170,#12192);
#10209=LINE('',#75187,#12193);
#10210=LINE('',#75212,#12194);
#10211=LINE('',#75252,#12195);
#10212=LINE('',#75257,#12196);
#10213=LINE('',#75274,#12197);
#10214=LINE('',#75310,#12198);
#10215=LINE('',#75336,#12199);
#10216=LINE('',#75341,#12200);
#10217=LINE('',#75358,#12201);
#10218=LINE('',#75383,#12202);
#10219=LINE('',#75411,#12203);
#10220=LINE('',#75416,#12204);
#10221=LINE('',#75433,#12205);
#10222=LINE('',#75458,#12206);
#10223=LINE('',#75482,#12207);
#10224=LINE('',#75487,#12208);
#10225=LINE('',#75504,#12209);
#10226=LINE('',#75521,#12210);
#10227=LINE('',#75525,#12211);
#10228=LINE('',#75559,#12212);
#10229=LINE('',#75585,#12213);
#10230=LINE('',#75603,#12214);
#10231=LINE('',#75608,#12215);
#10232=LINE('',#75625,#12216);
#10233=LINE('',#75659,#12217);
#10234=LINE('',#75677,#12218);
#10235=LINE('',#75682,#12219);
#10236=LINE('',#75699,#12220);
#10237=LINE('',#75731,#12221);
#10238=LINE('',#75771,#12222);
#10239=LINE('',#75776,#12223);
#10240=LINE('',#75793,#12224);
#10241=LINE('',#75829,#12225);
#10242=LINE('',#75855,#12226);
#10243=LINE('',#75860,#12227);
#10244=LINE('',#75877,#12228);
#10245=LINE('',#75902,#12229);
#10246=LINE('',#75930,#12230);
#10247=LINE('',#75935,#12231);
#10248=LINE('',#75952,#12232);
#10249=LINE('',#75977,#12233);
#10250=LINE('',#76001,#12234);
#10251=LINE('',#76006,#12235);
#10252=LINE('',#76023,#12236);
#10253=LINE('',#76040,#12237);
#10254=LINE('',#76044,#12238);
#10255=LINE('',#76078,#12239);
#10256=LINE('',#76104,#12240);
#10257=LINE('',#76122,#12241);
#10258=LINE('',#76127,#12242);
#10259=LINE('',#76144,#12243);
#10260=LINE('',#76178,#12244);
#10261=LINE('',#76199,#12245);
#10262=LINE('',#76204,#12246);
#10263=LINE('',#76221,#12247);
#10264=LINE('',#76246,#12248);
#10265=LINE('',#76285,#12249);
#10266=LINE('',#76290,#12250);
#10267=LINE('',#76307,#12251);
#10268=LINE('',#76338,#12252);
#10269=LINE('',#76364,#12253);
#10270=LINE('',#76369,#12254);
#10271=LINE('',#76386,#12255);
#10272=LINE('',#76411,#12256);
#10273=LINE('',#76439,#12257);
#10274=LINE('',#76444,#12258);
#10275=LINE('',#76461,#12259);
#10276=LINE('',#76486,#12260);
#10277=LINE('',#76510,#12261);
#10278=LINE('',#76515,#12262);
#10279=LINE('',#76532,#12263);
#10280=LINE('',#76549,#12264);
#10281=LINE('',#76553,#12265);
#10282=LINE('',#76587,#12266);
#10283=LINE('',#76613,#12267);
#10284=LINE('',#76631,#12268);
#10285=LINE('',#76636,#12269);
#10286=LINE('',#76653,#12270);
#10287=LINE('',#76687,#12271);
#10288=LINE('',#76705,#12272);
#10289=LINE('',#76710,#12273);
#10290=LINE('',#76727,#12274);
#10291=LINE('',#76759,#12275);
#10292=LINE('',#76799,#12276);
#10293=LINE('',#76804,#12277);
#10294=LINE('',#76821,#12278);
#10295=LINE('',#76857,#12279);
#10296=LINE('',#76880,#12280);
#10297=LINE('',#76885,#12281);
#10298=LINE('',#76902,#12282);
#10299=LINE('',#76934,#12283);
#10300=LINE('',#76962,#12284);
#10301=LINE('',#76967,#12285);
#10302=LINE('',#76984,#12286);
#10303=LINE('',#77009,#12287);
#10304=LINE('',#77033,#12288);
#10305=LINE('',#77038,#12289);
#10306=LINE('',#77055,#12290);
#10307=LINE('',#77072,#12291);
#10308=LINE('',#77076,#12292);
#10309=LINE('',#77110,#12293);
#10310=LINE('',#77136,#12294);
#10311=LINE('',#77154,#12295);
#10312=LINE('',#77159,#12296);
#10313=LINE('',#77176,#12297);
#10314=LINE('',#77210,#12298);
#10315=LINE('',#77231,#12299);
#10316=LINE('',#77236,#12300);
#10317=LINE('',#77253,#12301);
#10318=LINE('',#77278,#12302);
#10319=LINE('',#77318,#12303);
#10320=LINE('',#77323,#12304);
#10321=LINE('',#77340,#12305);
#10322=LINE('',#77376,#12306);
#10323=LINE('',#77402,#12307);
#10324=LINE('',#77407,#12308);
#10325=LINE('',#77424,#12309);
#10326=LINE('',#77449,#12310);
#10327=LINE('',#77477,#12311);
#10328=LINE('',#77482,#12312);
#10329=LINE('',#77499,#12313);
#10330=LINE('',#77531,#12314);
#10331=LINE('',#77555,#12315);
#10332=LINE('',#77560,#12316);
#10333=LINE('',#77577,#12317);
#10334=LINE('',#77594,#12318);
#10335=LINE('',#77598,#12319);
#10336=LINE('',#77632,#12320);
#10337=LINE('',#77658,#12321);
#10338=LINE('',#77676,#12322);
#10339=LINE('',#77681,#12323);
#10340=LINE('',#77698,#12324);
#10341=LINE('',#77732,#12325);
#10342=LINE('',#77753,#12326);
#10343=LINE('',#77758,#12327);
#10344=LINE('',#77775,#12328);
#10345=LINE('',#77800,#12329);
#10346=LINE('',#77840,#12330);
#10347=LINE('',#77845,#12331);
#10348=LINE('',#77862,#12332);
#10349=LINE('',#77898,#12333);
#10350=LINE('',#77924,#12334);
#10351=LINE('',#77929,#12335);
#10352=LINE('',#77946,#12336);
#10353=LINE('',#77971,#12337);
#10354=LINE('',#77999,#12338);
#10355=LINE('',#78004,#12339);
#10356=LINE('',#78021,#12340);
#10357=LINE('',#78046,#12341);
#10358=LINE('',#78067,#12342);
#10359=LINE('',#78072,#12343);
#10360=LINE('',#78089,#12344);
#10361=LINE('',#78113,#12345);
#10362=LINE('',#78117,#12346);
#10363=LINE('',#78151,#12347);
#10364=LINE('',#78177,#12348);
#10365=LINE('',#78195,#12349);
#10366=LINE('',#78200,#12350);
#10367=LINE('',#78217,#12351);
#10368=LINE('',#78251,#12352);
#10369=LINE('',#78272,#12353);
#10370=LINE('',#78277,#12354);
#10371=LINE('',#78294,#12355);
#10372=LINE('',#78319,#12356);
#10373=LINE('',#78359,#12357);
#10374=LINE('',#78364,#12358);
#10375=LINE('',#78381,#12359);
#10376=LINE('',#78417,#12360);
#10377=LINE('',#78443,#12361);
#10378=LINE('',#78448,#12362);
#10379=LINE('',#78465,#12363);
#10380=LINE('',#78490,#12364);
#10381=LINE('',#78518,#12365);
#10382=LINE('',#78523,#12366);
#10383=LINE('',#78540,#12367);
#10384=LINE('',#78565,#12368);
#10385=LINE('',#78589,#12369);
#10386=LINE('',#78594,#12370);
#10387=LINE('',#78611,#12371);
#10388=LINE('',#78628,#12372);
#10389=LINE('',#78632,#12373);
#10390=LINE('',#78666,#12374);
#10391=LINE('',#78692,#12375);
#10392=LINE('',#78710,#12376);
#10393=LINE('',#78715,#12377);
#10394=LINE('',#78732,#12378);
#10395=LINE('',#78766,#12379);
#10396=LINE('',#78787,#12380);
#10397=LINE('',#78792,#12381);
#10398=LINE('',#78809,#12382);
#10399=LINE('',#78834,#12383);
#10400=LINE('',#78874,#12384);
#10401=LINE('',#78879,#12385);
#10402=LINE('',#78896,#12386);
#10403=LINE('',#78932,#12387);
#10404=LINE('',#78958,#12388);
#10405=LINE('',#78963,#12389);
#10406=LINE('',#78980,#12390);
#10407=LINE('',#79005,#12391);
#10408=LINE('',#79033,#12392);
#10409=LINE('',#79038,#12393);
#10410=LINE('',#79055,#12394);
#10411=LINE('',#79080,#12395);
#10412=LINE('',#79104,#12396);
#10413=LINE('',#79109,#12397);
#10414=LINE('',#79126,#12398);
#10415=LINE('',#79143,#12399);
#10416=LINE('',#79147,#12400);
#10417=LINE('',#79181,#12401);
#10418=LINE('',#79207,#12402);
#10419=LINE('',#79225,#12403);
#10420=LINE('',#79230,#12404);
#10421=LINE('',#79247,#12405);
#10422=LINE('',#79281,#12406);
#10423=LINE('',#79302,#12407);
#10424=LINE('',#79307,#12408);
#10425=LINE('',#79324,#12409);
#10426=LINE('',#79349,#12410);
#10427=LINE('',#79389,#12411);
#10428=LINE('',#79394,#12412);
#10429=LINE('',#79411,#12413);
#10430=LINE('',#79447,#12414);
#10431=LINE('',#79473,#12415);
#10432=LINE('',#79478,#12416);
#10433=LINE('',#79495,#12417);
#10434=LINE('',#79520,#12418);
#10435=LINE('',#79548,#12419);
#10436=LINE('',#79553,#12420);
#10437=LINE('',#79570,#12421);
#10438=LINE('',#79595,#12422);
#10439=LINE('',#79619,#12423);
#10440=LINE('',#79624,#12424);
#10441=LINE('',#79641,#12425);
#10442=LINE('',#79658,#12426);
#10443=LINE('',#79662,#12427);
#10444=LINE('',#79696,#12428);
#10445=LINE('',#79722,#12429);
#10446=LINE('',#79740,#12430);
#10447=LINE('',#79745,#12431);
#10448=LINE('',#79762,#12432);
#10449=LINE('',#79796,#12433);
#10450=LINE('',#79817,#12434);
#10451=LINE('',#79822,#12435);
#10452=LINE('',#79839,#12436);
#10453=LINE('',#79864,#12437);
#10454=LINE('',#79904,#12438);
#10455=LINE('',#79909,#12439);
#10456=LINE('',#79926,#12440);
#10457=LINE('',#79962,#12441);
#10458=LINE('',#79988,#12442);
#10459=LINE('',#79993,#12443);
#10460=LINE('',#80010,#12444);
#10461=LINE('',#80035,#12445);
#10462=LINE('',#80063,#12446);
#10463=LINE('',#80068,#12447);
#10464=LINE('',#80085,#12448);
#10465=LINE('',#80110,#12449);
#10466=LINE('',#80134,#12450);
#10467=LINE('',#80139,#12451);
#10468=LINE('',#80156,#12452);
#10469=LINE('',#80173,#12453);
#10470=LINE('',#80177,#12454);
#10471=LINE('',#80211,#12455);
#10472=LINE('',#80237,#12456);
#10473=LINE('',#80255,#12457);
#10474=LINE('',#80260,#12458);
#10475=LINE('',#80277,#12459);
#10476=LINE('',#80311,#12460);
#10477=LINE('',#80332,#12461);
#10478=LINE('',#80337,#12462);
#10479=LINE('',#80354,#12463);
#10480=LINE('',#80379,#12464);
#10481=LINE('',#80419,#12465);
#10482=LINE('',#80424,#12466);
#10483=LINE('',#80441,#12467);
#10484=LINE('',#80477,#12468);
#10485=LINE('',#80503,#12469);
#10486=LINE('',#80508,#12470);
#10487=LINE('',#80525,#12471);
#10488=LINE('',#80550,#12472);
#10489=LINE('',#80578,#12473);
#10490=LINE('',#80583,#12474);
#10491=LINE('',#80600,#12475);
#10492=LINE('',#80625,#12476);
#10493=LINE('',#80649,#12477);
#10494=LINE('',#80654,#12478);
#10495=LINE('',#80671,#12479);
#10496=LINE('',#80688,#12480);
#10497=LINE('',#80692,#12481);
#10498=LINE('',#80726,#12482);
#10499=LINE('',#80752,#12483);
#10500=LINE('',#80770,#12484);
#10501=LINE('',#80775,#12485);
#10502=LINE('',#80792,#12486);
#10503=LINE('',#80826,#12487);
#10504=LINE('',#80847,#12488);
#10505=LINE('',#80852,#12489);
#10506=LINE('',#80869,#12490);
#10507=LINE('',#80894,#12491);
#10508=LINE('',#80934,#12492);
#10509=LINE('',#80939,#12493);
#10510=LINE('',#80956,#12494);
#10511=LINE('',#80992,#12495);
#10512=LINE('',#81018,#12496);
#10513=LINE('',#81023,#12497);
#10514=LINE('',#81040,#12498);
#10515=LINE('',#81065,#12499);
#10516=LINE('',#81093,#12500);
#10517=LINE('',#81098,#12501);
#10518=LINE('',#81115,#12502);
#10519=LINE('',#81140,#12503);
#10520=LINE('',#81164,#12504);
#10521=LINE('',#81169,#12505);
#10522=LINE('',#81186,#12506);
#10523=LINE('',#81203,#12507);
#10524=LINE('',#81207,#12508);
#10525=LINE('',#81241,#12509);
#10526=LINE('',#81267,#12510);
#10527=LINE('',#81285,#12511);
#10528=LINE('',#81290,#12512);
#10529=LINE('',#81307,#12513);
#10530=LINE('',#81341,#12514);
#10531=LINE('',#81359,#12515);
#10532=LINE('',#81364,#12516);
#10533=LINE('',#81381,#12517);
#10534=LINE('',#81413,#12518);
#10535=LINE('',#81453,#12519);
#10536=LINE('',#81458,#12520);
#10537=LINE('',#81475,#12521);
#10538=LINE('',#81511,#12522);
#10539=LINE('',#81537,#12523);
#10540=LINE('',#81542,#12524);
#10541=LINE('',#81559,#12525);
#10542=LINE('',#81584,#12526);
#10543=LINE('',#81612,#12527);
#10544=LINE('',#81617,#12528);
#10545=LINE('',#81634,#12529);
#10546=LINE('',#81659,#12530);
#10547=LINE('',#81683,#12531);
#10548=LINE('',#81688,#12532);
#10549=LINE('',#81705,#12533);
#10550=LINE('',#81722,#12534);
#10551=LINE('',#81726,#12535);
#10552=LINE('',#81760,#12536);
#10553=LINE('',#81786,#12537);
#10554=LINE('',#81804,#12538);
#10555=LINE('',#81809,#12539);
#10556=LINE('',#81826,#12540);
#10557=LINE('',#81860,#12541);
#10558=LINE('',#81881,#12542);
#10559=LINE('',#81886,#12543);
#10560=LINE('',#81903,#12544);
#10561=LINE('',#81928,#12545);
#10562=LINE('',#81967,#12546);
#10563=LINE('',#81972,#12547);
#10564=LINE('',#81989,#12548);
#10565=LINE('',#82020,#12549);
#10566=LINE('',#82046,#12550);
#10567=LINE('',#82051,#12551);
#10568=LINE('',#82068,#12552);
#10569=LINE('',#82093,#12553);
#10570=LINE('',#82121,#12554);
#10571=LINE('',#82126,#12555);
#10572=LINE('',#82143,#12556);
#10573=LINE('',#82168,#12557);
#10574=LINE('',#82192,#12558);
#10575=LINE('',#82197,#12559);
#10576=LINE('',#82214,#12560);
#10577=LINE('',#82231,#12561);
#10578=LINE('',#82235,#12562);
#10579=LINE('',#82269,#12563);
#10580=LINE('',#82295,#12564);
#10581=LINE('',#82313,#12565);
#10582=LINE('',#82318,#12566);
#10583=LINE('',#82335,#12567);
#10584=LINE('',#82369,#12568);
#10585=LINE('',#82390,#12569);
#10586=LINE('',#82395,#12570);
#10587=LINE('',#82412,#12571);
#10588=LINE('',#82437,#12572);
#10589=LINE('',#82477,#12573);
#10590=LINE('',#82482,#12574);
#10591=LINE('',#82499,#12575);
#10592=LINE('',#82535,#12576);
#10593=LINE('',#82558,#12577);
#10594=LINE('',#82563,#12578);
#10595=LINE('',#82580,#12579);
#10596=LINE('',#82612,#12580);
#10597=LINE('',#82640,#12581);
#10598=LINE('',#82645,#12582);
#10599=LINE('',#82662,#12583);
#10600=LINE('',#82687,#12584);
#10601=LINE('',#82711,#12585);
#10602=LINE('',#82716,#12586);
#10603=LINE('',#82733,#12587);
#10604=LINE('',#82750,#12588);
#10605=LINE('',#82754,#12589);
#10606=LINE('',#82788,#12590);
#10607=LINE('',#82814,#12591);
#10608=LINE('',#82832,#12592);
#10609=LINE('',#82837,#12593);
#10610=LINE('',#82854,#12594);
#10611=LINE('',#82888,#12595);
#10612=LINE('',#82909,#12596);
#10613=LINE('',#82914,#12597);
#10614=LINE('',#82931,#12598);
#10615=LINE('',#82956,#12599);
#10616=LINE('',#82996,#12600);
#10617=LINE('',#83001,#12601);
#10618=LINE('',#83018,#12602);
#10619=LINE('',#83054,#12603);
#10620=LINE('',#83080,#12604);
#10621=LINE('',#83085,#12605);
#10622=LINE('',#83102,#12606);
#10623=LINE('',#83127,#12607);
#10624=LINE('',#83155,#12608);
#10625=LINE('',#83160,#12609);
#10626=LINE('',#83177,#12610);
#10627=LINE('',#83209,#12611);
#10628=LINE('',#83233,#12612);
#10629=LINE('',#83238,#12613);
#10630=LINE('',#83255,#12614);
#10631=LINE('',#83272,#12615);
#10632=LINE('',#83276,#12616);
#10633=LINE('',#83310,#12617);
#10634=LINE('',#83336,#12618);
#10635=LINE('',#83354,#12619);
#10636=LINE('',#83359,#12620);
#10637=LINE('',#83376,#12621);
#10638=LINE('',#83410,#12622);
#10639=LINE('',#83431,#12623);
#10640=LINE('',#83436,#12624);
#10641=LINE('',#83453,#12625);
#10642=LINE('',#83478,#12626);
#10643=LINE('',#83518,#12627);
#10644=LINE('',#83523,#12628);
#10645=LINE('',#83540,#12629);
#10646=LINE('',#83576,#12630);
#10647=LINE('',#83602,#12631);
#10648=LINE('',#83607,#12632);
#10649=LINE('',#83624,#12633);
#10650=LINE('',#83649,#12634);
#10651=LINE('',#83677,#12635);
#10652=LINE('',#83682,#12636);
#10653=LINE('',#83699,#12637);
#10654=LINE('',#83724,#12638);
#10655=LINE('',#83745,#12639);
#10656=LINE('',#83750,#12640);
#10657=LINE('',#83767,#12641);
#10658=LINE('',#83791,#12642);
#10659=LINE('',#83795,#12643);
#10660=LINE('',#83829,#12644);
#10661=LINE('',#83855,#12645);
#10662=LINE('',#83873,#12646);
#10663=LINE('',#83878,#12647);
#10664=LINE('',#83895,#12648);
#10665=LINE('',#83929,#12649);
#10666=LINE('',#83950,#12650);
#10667=LINE('',#83955,#12651);
#10668=LINE('',#83972,#12652);
#10669=LINE('',#83997,#12653);
#10670=LINE('',#84037,#12654);
#10671=LINE('',#84042,#12655);
#10672=LINE('',#84059,#12656);
#10673=LINE('',#84095,#12657);
#10674=LINE('',#84121,#12658);
#10675=LINE('',#84126,#12659);
#10676=LINE('',#84143,#12660);
#10677=LINE('',#84168,#12661);
#10678=LINE('',#84196,#12662);
#10679=LINE('',#84201,#12663);
#10680=LINE('',#84218,#12664);
#10681=LINE('',#84243,#12665);
#10682=LINE('',#84267,#12666);
#10683=LINE('',#84272,#12667);
#10684=LINE('',#84289,#12668);
#10685=LINE('',#84306,#12669);
#10686=LINE('',#84310,#12670);
#10687=LINE('',#84344,#12671);
#10688=LINE('',#84370,#12672);
#10689=LINE('',#84388,#12673);
#10690=LINE('',#84393,#12674);
#10691=LINE('',#84410,#12675);
#10692=LINE('',#84444,#12676);
#10693=LINE('',#84465,#12677);
#10694=LINE('',#84470,#12678);
#10695=LINE('',#84487,#12679);
#10696=LINE('',#84512,#12680);
#10697=LINE('',#84552,#12681);
#10698=LINE('',#84557,#12682);
#10699=LINE('',#84574,#12683);
#10700=LINE('',#84610,#12684);
#10701=LINE('',#84636,#12685);
#10702=LINE('',#84641,#12686);
#10703=LINE('',#84658,#12687);
#10704=LINE('',#84683,#12688);
#10705=LINE('',#84711,#12689);
#10706=LINE('',#84716,#12690);
#10707=LINE('',#84733,#12691);
#10708=LINE('',#84758,#12692);
#10709=LINE('',#84782,#12693);
#10710=LINE('',#84787,#12694);
#10711=LINE('',#84804,#12695);
#10712=LINE('',#84821,#12696);
#10713=LINE('',#84825,#12697);
#10714=LINE('',#84859,#12698);
#10715=LINE('',#84885,#12699);
#10716=LINE('',#84903,#12700);
#10717=LINE('',#84908,#12701);
#10718=LINE('',#84925,#12702);
#10719=LINE('',#84959,#12703);
#10720=LINE('',#84980,#12704);
#10721=LINE('',#84985,#12705);
#10722=LINE('',#85002,#12706);
#10723=LINE('',#85027,#12707);
#10724=LINE('',#85067,#12708);
#10725=LINE('',#85072,#12709);
#10726=LINE('',#85089,#12710);
#10727=LINE('',#85125,#12711);
#10728=LINE('',#85151,#12712);
#10729=LINE('',#85156,#12713);
#10730=LINE('',#85173,#12714);
#10731=LINE('',#85198,#12715);
#10732=LINE('',#85226,#12716);
#10733=LINE('',#85231,#12717);
#10734=LINE('',#85248,#12718);
#10735=LINE('',#85273,#12719);
#10736=LINE('',#85297,#12720);
#10737=LINE('',#85302,#12721);
#10738=LINE('',#85319,#12722);
#10739=LINE('',#85336,#12723);
#10740=LINE('',#85340,#12724);
#10741=LINE('',#85374,#12725);
#10742=LINE('',#85400,#12726);
#10743=LINE('',#85418,#12727);
#10744=LINE('',#85423,#12728);
#10745=LINE('',#85440,#12729);
#10746=LINE('',#85474,#12730);
#10747=LINE('',#85495,#12731);
#10748=LINE('',#85500,#12732);
#10749=LINE('',#85517,#12733);
#10750=LINE('',#85542,#12734);
#10751=LINE('',#85582,#12735);
#10752=LINE('',#85587,#12736);
#10753=LINE('',#85604,#12737);
#10754=LINE('',#85640,#12738);
#10755=LINE('',#85666,#12739);
#10756=LINE('',#85671,#12740);
#10757=LINE('',#85688,#12741);
#10758=LINE('',#85713,#12742);
#10759=LINE('',#85741,#12743);
#10760=LINE('',#85746,#12744);
#10761=LINE('',#85763,#12745);
#10762=LINE('',#85788,#12746);
#10763=LINE('',#85812,#12747);
#10764=LINE('',#85817,#12748);
#10765=LINE('',#85834,#12749);
#10766=LINE('',#85851,#12750);
#10767=LINE('',#85855,#12751);
#10768=LINE('',#85889,#12752);
#10769=LINE('',#85915,#12753);
#10770=LINE('',#85933,#12754);
#10771=LINE('',#85938,#12755);
#10772=LINE('',#85955,#12756);
#10773=LINE('',#85989,#12757);
#10774=LINE('',#86010,#12758);
#10775=LINE('',#86015,#12759);
#10776=LINE('',#86032,#12760);
#10777=LINE('',#86057,#12761);
#10778=LINE('',#86097,#12762);
#10779=LINE('',#86102,#12763);
#10780=LINE('',#86119,#12764);
#10781=LINE('',#86155,#12765);
#10782=LINE('',#86181,#12766);
#10783=LINE('',#86186,#12767);
#10784=LINE('',#86203,#12768);
#10785=LINE('',#86228,#12769);
#10786=LINE('',#86256,#12770);
#10787=LINE('',#86261,#12771);
#10788=LINE('',#86278,#12772);
#10789=LINE('',#86303,#12773);
#10790=LINE('',#86327,#12774);
#10791=LINE('',#86332,#12775);
#10792=LINE('',#86349,#12776);
#10793=LINE('',#86366,#12777);
#10794=LINE('',#86370,#12778);
#10795=LINE('',#86404,#12779);
#10796=LINE('',#86430,#12780);
#10797=LINE('',#86448,#12781);
#10798=LINE('',#86453,#12782);
#10799=LINE('',#86470,#12783);
#10800=LINE('',#86504,#12784);
#10801=LINE('',#86525,#12785);
#10802=LINE('',#86530,#12786);
#10803=LINE('',#86547,#12787);
#10804=LINE('',#86572,#12788);
#10805=LINE('',#86612,#12789);
#10806=LINE('',#86617,#12790);
#10807=LINE('',#86634,#12791);
#10808=LINE('',#86670,#12792);
#10809=LINE('',#86696,#12793);
#10810=LINE('',#86701,#12794);
#10811=LINE('',#86718,#12795);
#10812=LINE('',#86743,#12796);
#10813=LINE('',#86771,#12797);
#10814=LINE('',#86776,#12798);
#10815=LINE('',#86793,#12799);
#10816=LINE('',#86818,#12800);
#10817=LINE('',#86842,#12801);
#10818=LINE('',#86847,#12802);
#10819=LINE('',#86864,#12803);
#10820=LINE('',#86881,#12804);
#10821=LINE('',#86885,#12805);
#10822=LINE('',#86919,#12806);
#10823=LINE('',#86945,#12807);
#10824=LINE('',#86963,#12808);
#10825=LINE('',#86968,#12809);
#10826=LINE('',#86985,#12810);
#10827=LINE('',#87019,#12811);
#10828=LINE('',#87040,#12812);
#10829=LINE('',#87045,#12813);
#10830=LINE('',#87062,#12814);
#10831=LINE('',#87087,#12815);
#10832=LINE('',#87127,#12816);
#10833=LINE('',#87132,#12817);
#10834=LINE('',#87149,#12818);
#10835=LINE('',#87185,#12819);
#10836=LINE('',#87211,#12820);
#10837=LINE('',#87216,#12821);
#10838=LINE('',#87233,#12822);
#10839=LINE('',#87258,#12823);
#10840=LINE('',#87286,#12824);
#10841=LINE('',#87291,#12825);
#10842=LINE('',#87308,#12826);
#10843=LINE('',#87333,#12827);
#10844=LINE('',#87357,#12828);
#10845=LINE('',#87362,#12829);
#10846=LINE('',#87379,#12830);
#10847=LINE('',#87396,#12831);
#10848=LINE('',#87400,#12832);
#10849=LINE('',#87434,#12833);
#10850=LINE('',#87460,#12834);
#10851=LINE('',#87478,#12835);
#10852=LINE('',#87483,#12836);
#10853=LINE('',#87500,#12837);
#10854=LINE('',#87534,#12838);
#10855=LINE('',#87555,#12839);
#10856=LINE('',#87560,#12840);
#10857=LINE('',#87577,#12841);
#10858=LINE('',#87602,#12842);
#10859=LINE('',#87642,#12843);
#10860=LINE('',#87647,#12844);
#10861=LINE('',#87664,#12845);
#10862=LINE('',#87700,#12846);
#10863=LINE('',#87726,#12847);
#10864=LINE('',#87731,#12848);
#10865=LINE('',#87748,#12849);
#10866=LINE('',#87773,#12850);
#10867=LINE('',#87801,#12851);
#10868=LINE('',#87806,#12852);
#10869=LINE('',#87823,#12853);
#10870=LINE('',#87848,#12854);
#10871=LINE('',#87872,#12855);
#10872=LINE('',#87877,#12856);
#10873=LINE('',#87894,#12857);
#10874=LINE('',#87911,#12858);
#10875=LINE('',#87915,#12859);
#10876=LINE('',#87958,#12860);
#10877=LINE('',#87981,#12861);
#10878=LINE('',#87993,#12862);
#10879=LINE('',#87998,#12863);
#10880=LINE('',#88015,#12864);
#10881=LINE('',#88049,#12865);
#10882=LINE('',#88070,#12866);
#10883=LINE('',#88075,#12867);
#10884=LINE('',#88092,#12868);
#10885=LINE('',#88117,#12869);
#10886=LINE('',#88157,#12870);
#10887=LINE('',#88162,#12871);
#10888=LINE('',#88179,#12872);
#10889=LINE('',#88215,#12873);
#10890=LINE('',#88241,#12874);
#10891=LINE('',#88246,#12875);
#10892=LINE('',#88263,#12876);
#10893=LINE('',#88288,#12877);
#10894=LINE('',#88316,#12878);
#10895=LINE('',#88321,#12879);
#10896=LINE('',#88338,#12880);
#10897=LINE('',#88363,#12881);
#10898=LINE('',#88387,#12882);
#10899=LINE('',#88392,#12883);
#10900=LINE('',#88409,#12884);
#10901=LINE('',#88426,#12885);
#10902=LINE('',#88430,#12886);
#10903=LINE('',#88482,#12887);
#10904=LINE('',#88505,#12888);
#10905=LINE('',#88520,#12889);
#10906=LINE('',#88525,#12890);
#10907=LINE('',#88542,#12891);
#10908=LINE('',#88573,#12892);
#10909=LINE('',#88585,#12893);
#10910=LINE('',#88590,#12894);
#10911=LINE('',#88607,#12895);
#10912=LINE('',#88639,#12896);
#10913=LINE('',#88679,#12897);
#10914=LINE('',#88684,#12898);
#10915=LINE('',#88701,#12899);
#10916=LINE('',#88737,#12900);
#10917=LINE('',#88763,#12901);
#10918=LINE('',#88768,#12902);
#10919=LINE('',#88785,#12903);
#10920=LINE('',#88810,#12904);
#10921=LINE('',#88838,#12905);
#10922=LINE('',#88843,#12906);
#10923=LINE('',#88860,#12907);
#10924=LINE('',#88885,#12908);
#10925=LINE('',#88909,#12909);
#10926=LINE('',#88914,#12910);
#10927=LINE('',#88931,#12911);
#10928=LINE('',#88948,#12912);
#10929=LINE('',#88952,#12913);
#10930=LINE('',#88994,#12914);
#10931=LINE('',#88999,#12915);
#10932=LINE('',#89016,#12916);
#10933=LINE('',#89047,#12917);
#10934=LINE('',#89065,#12918);
#10935=LINE('',#89070,#12919);
#10936=LINE('',#89087,#12920);
#10937=LINE('',#89109,#12921);
#10938=LINE('',#89142,#12922);
#10939=LINE('',#89147,#12923);
#10940=LINE('',#89164,#12924);
#10941=LINE('',#89195,#12925);
#10942=LINE('',#89219,#12926);
#10943=LINE('',#89242,#12927);
#10944=LINE('',#89268,#12928);
#10945=LINE('',#89273,#12929);
#10946=LINE('',#89290,#12930);
#10947=LINE('',#89315,#12931);
#10948=LINE('',#89343,#12932);
#10949=LINE('',#89348,#12933);
#10950=LINE('',#89365,#12934);
#10951=LINE('',#89390,#12935);
#10952=LINE('',#89414,#12936);
#10953=LINE('',#89419,#12937);
#10954=LINE('',#89436,#12938);
#10955=LINE('',#89453,#12939);
#10956=LINE('',#89457,#12940);
#10957=LINE('',#89518,#12941);
#10958=LINE('',#89523,#12942);
#10959=LINE('',#89540,#12943);
#10960=LINE('',#89569,#12944);
#10961=LINE('',#89608,#12945);
#10962=LINE('',#89613,#12946);
#10963=LINE('',#89630,#12947);
#10964=LINE('',#89658,#12948);
#10965=LINE('',#89670,#12949);
#10966=LINE('',#89675,#12950);
#10967=LINE('',#89692,#12951);
#10968=LINE('',#89724,#12952);
#10969=LINE('',#89748,#12953);
#10970=LINE('',#89771,#12954);
#10971=LINE('',#89789,#12955);
#10972=LINE('',#89794,#12956);
#10973=LINE('',#89811,#12957);
#10974=LINE('',#89842,#12958);
#10975=LINE('',#89870,#12959);
#10976=LINE('',#89875,#12960);
#10977=LINE('',#89892,#12961);
#10978=LINE('',#89917,#12962);
#10979=LINE('',#89941,#12963);
#10980=LINE('',#89946,#12964);
#10981=LINE('',#89963,#12965);
#10982=LINE('',#89980,#12966);
#10983=LINE('',#89984,#12967);
#10984=LINE('',#90075,#12968);
#10985=LINE('',#90080,#12969);
#10986=LINE('',#90097,#12970);
#10987=LINE('',#90120,#12971);
#10988=LINE('',#90138,#12972);
#10989=LINE('',#90143,#12973);
#10990=LINE('',#90160,#12974);
#10991=LINE('',#90182,#12975);
#10992=LINE('',#90204,#12976);
#10993=LINE('',#90209,#12977);
#10994=LINE('',#90226,#12978);
#10995=LINE('',#90258,#12979);
#10996=LINE('',#90289,#12980);
#10997=LINE('',#90305,#12981);
#10998=LINE('',#90323,#12982);
#10999=LINE('',#90328,#12983);
#11000=LINE('',#90345,#12984);
#11001=LINE('',#90376,#12985);
#11002=LINE('',#90394,#12986);
#11003=LINE('',#90399,#12987);
#11004=LINE('',#90416,#12988);
#11005=LINE('',#90438,#12989);
#11006=LINE('',#90462,#12990);
#11007=LINE('',#90467,#12991);
#11008=LINE('',#90484,#12992);
#11009=LINE('',#90501,#12993);
#11010=LINE('',#90505,#12994);
#11011=LINE('',#90584,#12995);
#11012=LINE('',#90588,#12996);
#11013=LINE('',#90605,#12997);
#11014=LINE('',#90634,#12998);
#11015=LINE('',#90652,#12999);
#11016=LINE('',#90656,#13000);
#11017=LINE('',#90673,#13001);
#11018=LINE('',#90695,#13002);
#11019=LINE('',#90710,#13003);
#11020=LINE('',#90715,#13004);
#11021=LINE('',#90732,#13005);
#11022=LINE('',#90756,#13006);
#11023=LINE('',#90779,#13007);
#11024=LINE('',#90795,#13008);
#11025=LINE('',#90810,#13009);
#11026=LINE('',#90814,#13010);
#11027=LINE('',#90831,#13011);
#11028=LINE('',#90855,#13012);
#11029=LINE('',#90873,#13013);
#11030=LINE('',#90877,#13014);
#11031=LINE('',#90894,#13015);
#11032=LINE('',#90916,#13016);
#11033=LINE('',#90955,#13017);
#11034=LINE('',#90959,#13018);
#11035=LINE('',#90976,#13019);
#11036=LINE('',#91004,#13020);
#11037=LINE('',#91008,#13021);
#11038=LINE('',#91015,#13022);
#11039=LINE('',#106229,#13023);
#11040=LINE('',#106235,#13024);
#11041=LINE('',#106241,#13025);
#11042=LINE('',#106251,#13026);
#11043=LINE('',#106257,#13027);
#11044=LINE('',#106266,#13028);
#11045=LINE('',#106272,#13029);
#11046=LINE('',#106278,#13030);
#11047=LINE('',#106284,#13031);
#11048=LINE('',#106289,#13032);
#11049=LINE('',#106293,#13033);
#11050=LINE('',#106298,#13034);
#11051=LINE('',#106302,#13035);
#11052=LINE('',#106307,#13036);
#11053=LINE('',#106311,#13037);
#11054=LINE('',#106316,#13038);
#11055=LINE('',#106320,#13039);
#11056=LINE('',#106325,#13040);
#11057=LINE('',#106329,#13041);
#11058=LINE('',#106334,#13042);
#11059=LINE('',#106338,#13043);
#11060=LINE('',#106343,#13044);
#11061=LINE('',#106347,#13045);
#11062=LINE('',#106352,#13046);
#11063=LINE('',#106356,#13047);
#11064=LINE('',#106361,#13048);
#11065=LINE('',#106365,#13049);
#11066=LINE('',#106370,#13050);
#11067=LINE('',#106374,#13051);
#11068=LINE('',#106379,#13052);
#11069=LINE('',#106383,#13053);
#11070=LINE('',#106388,#13054);
#11071=LINE('',#106392,#13055);
#11072=LINE('',#106397,#13056);
#11073=LINE('',#106401,#13057);
#11074=LINE('',#106406,#13058);
#11075=LINE('',#106410,#13059);
#11076=LINE('',#106415,#13060);
#11077=LINE('',#106419,#13061);
#11078=LINE('',#106424,#13062);
#11079=LINE('',#106428,#13063);
#11080=LINE('',#106433,#13064);
#11081=LINE('',#106437,#13065);
#11082=LINE('',#106442,#13066);
#11083=LINE('',#106446,#13067);
#11084=LINE('',#106451,#13068);
#11085=LINE('',#106455,#13069);
#11086=LINE('',#106460,#13070);
#11087=LINE('',#106464,#13071);
#11088=LINE('',#106469,#13072);
#11089=LINE('',#106473,#13073);
#11090=LINE('',#106478,#13074);
#11091=LINE('',#106482,#13075);
#11092=LINE('',#106487,#13076);
#11093=LINE('',#106491,#13077);
#11094=LINE('',#106496,#13078);
#11095=LINE('',#106500,#13079);
#11096=LINE('',#106505,#13080);
#11097=LINE('',#106509,#13081);
#11098=LINE('',#106514,#13082);
#11099=LINE('',#106518,#13083);
#11100=LINE('',#106523,#13084);
#11101=LINE('',#106527,#13085);
#11102=LINE('',#106532,#13086);
#11103=LINE('',#106536,#13087);
#11104=LINE('',#106541,#13088);
#11105=LINE('',#106545,#13089);
#11106=LINE('',#106550,#13090);
#11107=LINE('',#106554,#13091);
#11108=LINE('',#106559,#13092);
#11109=LINE('',#106563,#13093);
#11110=LINE('',#106568,#13094);
#11111=LINE('',#106572,#13095);
#11112=LINE('',#106577,#13096);
#11113=LINE('',#106581,#13097);
#11114=LINE('',#106586,#13098);
#11115=LINE('',#106590,#13099);
#11116=LINE('',#106595,#13100);
#11117=LINE('',#106599,#13101);
#11118=LINE('',#106604,#13102);
#11119=LINE('',#106608,#13103);
#11120=LINE('',#106613,#13104);
#11121=LINE('',#106617,#13105);
#11122=LINE('',#106622,#13106);
#11123=LINE('',#106626,#13107);
#11124=LINE('',#106631,#13108);
#11125=LINE('',#106635,#13109);
#11126=LINE('',#106640,#13110);
#11127=LINE('',#106644,#13111);
#11128=LINE('',#106649,#13112);
#11129=LINE('',#106653,#13113);
#11130=LINE('',#106658,#13114);
#11131=LINE('',#106662,#13115);
#11132=LINE('',#106667,#13116);
#11133=LINE('',#106671,#13117);
#11134=LINE('',#106676,#13118);
#11135=LINE('',#106680,#13119);
#11136=LINE('',#106685,#13120);
#11137=LINE('',#106689,#13121);
#11138=LINE('',#106694,#13122);
#11139=LINE('',#106698,#13123);
#11140=LINE('',#106703,#13124);
#11141=LINE('',#106707,#13125);
#11142=LINE('',#106712,#13126);
#11143=LINE('',#106716,#13127);
#11144=LINE('',#106721,#13128);
#11145=LINE('',#106725,#13129);
#11146=LINE('',#106730,#13130);
#11147=LINE('',#106734,#13131);
#11148=LINE('',#106739,#13132);
#11149=LINE('',#106743,#13133);
#11150=LINE('',#106747,#13134);
#11151=LINE('',#106748,#13135);
#11152=LINE('',#106750,#13136);
#11153=LINE('',#106751,#13137);
#11154=LINE('',#106753,#13138);
#11155=LINE('',#106754,#13139);
#11156=LINE('',#106756,#13140);
#11157=LINE('',#106757,#13141);
#11158=LINE('',#106759,#13142);
#11159=LINE('',#106760,#13143);
#11160=LINE('',#106762,#13144);
#11161=LINE('',#106763,#13145);
#11162=LINE('',#106765,#13146);
#11163=LINE('',#106766,#13147);
#11164=LINE('',#106768,#13148);
#11165=LINE('',#106769,#13149);
#11166=LINE('',#106771,#13150);
#11167=LINE('',#106772,#13151);
#11168=LINE('',#106774,#13152);
#11169=LINE('',#106775,#13153);
#11170=LINE('',#106777,#13154);
#11171=LINE('',#106778,#13155);
#11172=LINE('',#106780,#13156);
#11173=LINE('',#106781,#13157);
#11174=LINE('',#106783,#13158);
#11175=LINE('',#106784,#13159);
#11176=LINE('',#106786,#13160);
#11177=LINE('',#106787,#13161);
#11178=LINE('',#106789,#13162);
#11179=LINE('',#106790,#13163);
#11180=LINE('',#106792,#13164);
#11181=LINE('',#106793,#13165);
#11182=LINE('',#106795,#13166);
#11183=LINE('',#106796,#13167);
#11184=LINE('',#106798,#13168);
#11185=LINE('',#106799,#13169);
#11186=LINE('',#106801,#13170);
#11187=LINE('',#106802,#13171);
#11188=LINE('',#106804,#13172);
#11189=LINE('',#106805,#13173);
#11190=LINE('',#106807,#13174);
#11191=LINE('',#106808,#13175);
#11192=LINE('',#106810,#13176);
#11193=LINE('',#106811,#13177);
#11194=LINE('',#106813,#13178);
#11195=LINE('',#106814,#13179);
#11196=LINE('',#106816,#13180);
#11197=LINE('',#106817,#13181);
#11198=LINE('',#106819,#13182);
#11199=LINE('',#106820,#13183);
#11200=LINE('',#106822,#13184);
#11201=LINE('',#106823,#13185);
#11202=LINE('',#106825,#13186);
#11203=LINE('',#106826,#13187);
#11204=LINE('',#106828,#13188);
#11205=LINE('',#106829,#13189);
#11206=LINE('',#106831,#13190);
#11207=LINE('',#106832,#13191);
#11208=LINE('',#106834,#13192);
#11209=LINE('',#106835,#13193);
#11210=LINE('',#106837,#13194);
#11211=LINE('',#106838,#13195);
#11212=LINE('',#106840,#13196);
#11213=LINE('',#106841,#13197);
#11214=LINE('',#106843,#13198);
#11215=LINE('',#106844,#13199);
#11216=LINE('',#106846,#13200);
#11217=LINE('',#106847,#13201);
#11218=LINE('',#106849,#13202);
#11219=LINE('',#106850,#13203);
#11220=LINE('',#106852,#13204);
#11221=LINE('',#106853,#13205);
#11222=LINE('',#106855,#13206);
#11223=LINE('',#106856,#13207);
#11224=LINE('',#106858,#13208);
#11225=LINE('',#106859,#13209);
#11226=LINE('',#106861,#13210);
#11227=LINE('',#106862,#13211);
#11228=LINE('',#106864,#13212);
#11229=LINE('',#106865,#13213);
#11230=LINE('',#106867,#13214);
#11231=LINE('',#106868,#13215);
#11232=LINE('',#106870,#13216);
#11233=LINE('',#106871,#13217);
#11234=LINE('',#106873,#13218);
#11235=LINE('',#106874,#13219);
#11236=LINE('',#106876,#13220);
#11237=LINE('',#106877,#13221);
#11238=LINE('',#106879,#13222);
#11239=LINE('',#106880,#13223);
#11240=LINE('',#106882,#13224);
#11241=LINE('',#106883,#13225);
#11242=LINE('',#106885,#13226);
#11243=LINE('',#106886,#13227);
#11244=LINE('',#106888,#13228);
#11245=LINE('',#106889,#13229);
#11246=LINE('',#106891,#13230);
#11247=LINE('',#106892,#13231);
#11248=LINE('',#106894,#13232);
#11249=LINE('',#106895,#13233);
#11250=LINE('',#106897,#13234);
#11251=LINE('',#106898,#13235);
#11252=LINE('',#106901,#13236);
#11253=LINE('',#106902,#13237);
#11254=LINE('',#106904,#13238);
#11255=LINE('',#106905,#13239);
#11256=LINE('',#106907,#13240);
#11257=LINE('',#106908,#13241);
#11258=LINE('',#106910,#13242);
#11259=LINE('',#106911,#13243);
#11260=LINE('',#106913,#13244);
#11261=LINE('',#106914,#13245);
#11262=LINE('',#106916,#13246);
#11263=LINE('',#106917,#13247);
#11264=LINE('',#106919,#13248);
#11265=LINE('',#106920,#13249);
#11266=LINE('',#106922,#13250);
#11267=LINE('',#106923,#13251);
#11268=LINE('',#106925,#13252);
#11269=LINE('',#106926,#13253);
#11270=LINE('',#106928,#13254);
#11271=LINE('',#106929,#13255);
#11272=LINE('',#106931,#13256);
#11273=LINE('',#106932,#13257);
#11274=LINE('',#106934,#13258);
#11275=LINE('',#106935,#13259);
#11276=LINE('',#106937,#13260);
#11277=LINE('',#106938,#13261);
#11278=LINE('',#106940,#13262);
#11279=LINE('',#106941,#13263);
#11280=LINE('',#106943,#13264);
#11281=LINE('',#106944,#13265);
#11282=LINE('',#106946,#13266);
#11283=LINE('',#106947,#13267);
#11284=LINE('',#106949,#13268);
#11285=LINE('',#106950,#13269);
#11286=LINE('',#106952,#13270);
#11287=LINE('',#106953,#13271);
#11288=LINE('',#106955,#13272);
#11289=LINE('',#106956,#13273);
#11290=LINE('',#106958,#13274);
#11291=LINE('',#106959,#13275);
#11292=LINE('',#106961,#13276);
#11293=LINE('',#106962,#13277);
#11294=LINE('',#106964,#13278);
#11295=LINE('',#106965,#13279);
#11296=LINE('',#106967,#13280);
#11297=LINE('',#106968,#13281);
#11298=LINE('',#106970,#13282);
#11299=LINE('',#106971,#13283);
#11300=LINE('',#106973,#13284);
#11301=LINE('',#106974,#13285);
#11302=LINE('',#106976,#13286);
#11303=LINE('',#106977,#13287);
#11304=LINE('',#106979,#13288);
#11305=LINE('',#106980,#13289);
#11306=LINE('',#106982,#13290);
#11307=LINE('',#106983,#13291);
#11308=LINE('',#106985,#13292);
#11309=LINE('',#106986,#13293);
#11310=LINE('',#106988,#13294);
#11311=LINE('',#106989,#13295);
#11312=LINE('',#106991,#13296);
#11313=LINE('',#106992,#13297);
#11314=LINE('',#106994,#13298);
#11315=LINE('',#106995,#13299);
#11316=LINE('',#106997,#13300);
#11317=LINE('',#106998,#13301);
#11318=LINE('',#107000,#13302);
#11319=LINE('',#107001,#13303);
#11320=LINE('',#107003,#13304);
#11321=LINE('',#107004,#13305);
#11322=LINE('',#107006,#13306);
#11323=LINE('',#107007,#13307);
#11324=LINE('',#107009,#13308);
#11325=LINE('',#107010,#13309);
#11326=LINE('',#107012,#13310);
#11327=LINE('',#107013,#13311);
#11328=LINE('',#107015,#13312);
#11329=LINE('',#107016,#13313);
#11330=LINE('',#107018,#13314);
#11331=LINE('',#107019,#13315);
#11332=LINE('',#107021,#13316);
#11333=LINE('',#107022,#13317);
#11334=LINE('',#107024,#13318);
#11335=LINE('',#107025,#13319);
#11336=LINE('',#107027,#13320);
#11337=LINE('',#107028,#13321);
#11338=LINE('',#107030,#13322);
#11339=LINE('',#107031,#13323);
#11340=LINE('',#107033,#13324);
#11341=LINE('',#107034,#13325);
#11342=LINE('',#107036,#13326);
#11343=LINE('',#107037,#13327);
#11344=LINE('',#107039,#13328);
#11345=LINE('',#107040,#13329);
#11346=LINE('',#107042,#13330);
#11347=LINE('',#107043,#13331);
#11348=LINE('',#107045,#13332);
#11349=LINE('',#107046,#13333);
#11350=LINE('',#107048,#13334);
#11351=LINE('',#107049,#13335);
#11352=LINE('',#107051,#13336);
#11353=LINE('',#107052,#13337);
#11354=LINE('',#107058,#13338);
#11355=LINE('',#107061,#13339);
#11356=LINE('',#107064,#13340);
#11357=LINE('',#107067,#13341);
#11358=LINE('',#107070,#13342);
#11359=LINE('',#107073,#13343);
#11360=LINE('',#107076,#13344);
#11361=LINE('',#107079,#13345);
#11362=LINE('',#107082,#13346);
#11363=LINE('',#107085,#13347);
#11364=LINE('',#107088,#13348);
#11365=LINE('',#107091,#13349);
#11366=LINE('',#107094,#13350);
#11367=LINE('',#107097,#13351);
#11368=LINE('',#107100,#13352);
#11369=LINE('',#107103,#13353);
#11370=LINE('',#107106,#13354);
#11371=LINE('',#107109,#13355);
#11372=LINE('',#107112,#13356);
#11373=LINE('',#107115,#13357);
#11374=LINE('',#107118,#13358);
#11375=LINE('',#107121,#13359);
#11376=LINE('',#107124,#13360);
#11377=LINE('',#107127,#13361);
#11378=LINE('',#107130,#13362);
#11379=LINE('',#107133,#13363);
#11380=LINE('',#107136,#13364);
#11381=LINE('',#107139,#13365);
#11382=LINE('',#107142,#13366);
#11383=LINE('',#107145,#13367);
#11384=LINE('',#107148,#13368);
#11385=LINE('',#107151,#13369);
#11386=LINE('',#107154,#13370);
#11387=LINE('',#107157,#13371);
#11388=LINE('',#107160,#13372);
#11389=LINE('',#107163,#13373);
#11390=LINE('',#107166,#13374);
#11391=LINE('',#107169,#13375);
#11392=LINE('',#107172,#13376);
#11393=LINE('',#107175,#13377);
#11394=LINE('',#107178,#13378);
#11395=LINE('',#107181,#13379);
#11396=LINE('',#107184,#13380);
#11397=LINE('',#107187,#13381);
#11398=LINE('',#107190,#13382);
#11399=LINE('',#107193,#13383);
#11400=LINE('',#107196,#13384);
#11401=LINE('',#107199,#13385);
#11402=LINE('',#107202,#13386);
#11403=LINE('',#107205,#13387);
#11404=LINE('',#107208,#13388);
#11405=LINE('',#107215,#13389);
#11406=LINE('',#107219,#13390);
#11407=LINE('',#107223,#13391);
#11408=LINE('',#107228,#13392);
#11409=LINE('',#107234,#13393);
#11410=LINE('',#107283,#13394);
#11411=LINE('',#107290,#13395);
#11412=LINE('',#107293,#13396);
#11413=LINE('',#107298,#13397);
#11414=LINE('',#107305,#13398);
#11415=LINE('',#107332,#13399);
#11416=LINE('',#107338,#13400);
#11417=LINE('',#107345,#13401);
#11418=LINE('',#107348,#13402);
#11419=LINE('',#107354,#13403);
#11420=LINE('',#107358,#13404);
#11421=LINE('',#107361,#13405);
#11422=LINE('',#107366,#13406);
#11423=LINE('',#107372,#13407);
#11424=LINE('',#107378,#13408);
#11425=LINE('',#107384,#13409);
#11426=LINE('',#107390,#13410);
#11427=LINE('',#107394,#13411);
#11428=LINE('',#107398,#13412);
#11429=LINE('',#107400,#13413);
#11430=LINE('',#107405,#13414);
#11431=LINE('',#107409,#13415);
#11432=LINE('',#107412,#13416);
#11433=LINE('',#107415,#13417);
#11434=LINE('',#107421,#13418);
#11435=LINE('',#107426,#13419);
#11436=LINE('',#107429,#13420);
#11437=LINE('',#107433,#13421);
#11438=LINE('',#107435,#13422);
#11439=LINE('',#107437,#13423);
#11440=LINE('',#107438,#13424);
#11441=LINE('',#107442,#13425);
#11442=LINE('',#107446,#13426);
#11443=LINE('',#107450,#13427);
#11444=LINE('',#107455,#13428);
#11445=LINE('',#107458,#13429);
#11446=LINE('',#107460,#13430);
#11447=LINE('',#107464,#13431);
#11448=LINE('',#107466,#13432);
#11449=LINE('',#107468,#13433);
#11450=LINE('',#107470,#13434);
#11451=LINE('',#107471,#13435);
#11452=LINE('',#107472,#13436);
#11453=LINE('',#107476,#13437);
#11454=LINE('',#107478,#13438);
#11455=LINE('',#107479,#13439);
#11456=LINE('',#107480,#13440);
#11457=LINE('',#107481,#13441);
#11458=LINE('',#107485,#13442);
#11459=LINE('',#107487,#13443);
#11460=LINE('',#107488,#13444);
#11461=LINE('',#107490,#13445);
#11462=LINE('',#107491,#13446);
#11463=LINE('',#107495,#13447);
#11464=LINE('',#107497,#13448);
#11465=LINE('',#107499,#13449);
#11466=LINE('',#107500,#13450);
#11467=LINE('',#107504,#13451);
#11468=LINE('',#107508,#13452);
#11469=LINE('',#107512,#13453);
#11470=LINE('',#107516,#13454);
#11471=LINE('',#107522,#13455);
#11472=LINE('',#107528,#13456);
#11473=LINE('',#107531,#13457);
#11474=LINE('',#107533,#13458);
#11475=LINE('',#107534,#13459);
#11476=LINE('',#107538,#13460);
#11477=LINE('',#107540,#13461);
#11478=LINE('',#107542,#13462);
#11479=LINE('',#107544,#13463);
#11480=LINE('',#107546,#13464);
#11481=LINE('',#107547,#13465);
#11482=LINE('',#107551,#13466);
#11483=LINE('',#107553,#13467);
#11484=LINE('',#107555,#13468);
#11485=LINE('',#107557,#13469);
#11486=LINE('',#107559,#13470);
#11487=LINE('',#107561,#13471);
#11488=LINE('',#107563,#13472);
#11489=LINE('',#107564,#13473);
#11490=LINE('',#107567,#13474);
#11491=LINE('',#107569,#13475);
#11492=LINE('',#107571,#13476);
#11493=LINE('',#107573,#13477);
#11494=LINE('',#107575,#13478);
#11495=LINE('',#107577,#13479);
#11496=LINE('',#107579,#13480);
#11497=LINE('',#107580,#13481);
#11498=LINE('',#107583,#13482);
#11499=LINE('',#107585,#13483);
#11500=LINE('',#107587,#13484);
#11501=LINE('',#107589,#13485);
#11502=LINE('',#107591,#13486);
#11503=LINE('',#107593,#13487);
#11504=LINE('',#107595,#13488);
#11505=LINE('',#107597,#13489);
#11506=LINE('',#107599,#13490);
#11507=LINE('',#107603,#13491);
#11508=LINE('',#107607,#13492);
#11509=LINE('',#107611,#13493);
#11510=LINE('',#107613,#13494);
#11511=LINE('',#107615,#13495);
#11512=LINE('',#107619,#13496);
#11513=LINE('',#107623,#13497);
#11514=LINE('',#107626,#13498);
#11515=LINE('',#107628,#13499);
#11516=LINE('',#107632,#13500);
#11517=LINE('',#107637,#13501);
#11518=LINE('',#107639,#13502);
#11519=LINE('',#107640,#13503);
#11520=LINE('',#107642,#13504);
#11521=LINE('',#107643,#13505);
#11522=LINE('',#107645,#13506);
#11523=LINE('',#107646,#13507);
#11524=LINE('',#107647,#13508);
#11525=LINE('',#107651,#13509);
#11526=LINE('',#107652,#13510);
#11527=LINE('',#107653,#13511);
#11528=LINE('',#107655,#13512);
#11529=LINE('',#107656,#13513);
#11530=LINE('',#107658,#13514);
#11531=LINE('',#107659,#13515);
#11532=LINE('',#107661,#13516);
#11533=LINE('',#107662,#13517);
#11534=LINE('',#107665,#13518);
#11535=LINE('',#107667,#13519);
#11536=LINE('',#107668,#13520);
#11537=LINE('',#107670,#13521);
#11538=LINE('',#107672,#13522);
#11539=LINE('',#107673,#13523);
#11540=LINE('',#107676,#13524);
#11541=LINE('',#107677,#13525);
#11542=LINE('',#107680,#13526);
#11543=LINE('',#107681,#13527);
#11544=LINE('',#107683,#13528);
#11545=LINE('',#107685,#13529);
#11546=LINE('',#107686,#13530);
#11547=LINE('',#107688,#13531);
#11548=LINE('',#107690,#13532);
#11549=LINE('',#107692,#13533);
#11550=LINE('',#107694,#13534);
#11551=LINE('',#107696,#13535);
#11552=LINE('',#107698,#13536);
#11553=LINE('',#107704,#13537);
#11554=LINE('',#107706,#13538);
#11555=LINE('',#107707,#13539);
#11556=LINE('',#107710,#13540);
#11557=LINE('',#107714,#13541);
#11558=LINE('',#107715,#13542);
#11559=LINE('',#107718,#13543);
#11560=LINE('',#107722,#13544);
#11561=LINE('',#107723,#13545);
#11562=LINE('',#107726,#13546);
#11563=LINE('',#107730,#13547);
#11564=LINE('',#107731,#13548);
#11565=LINE('',#107734,#13549);
#11566=LINE('',#107737,#13550);
#11567=LINE('',#107738,#13551);
#11568=LINE('',#107743,#13552);
#11569=LINE('',#107744,#13553);
#11570=LINE('',#107748,#13554);
#11571=LINE('',#107751,#13555);
#11572=LINE('',#107752,#13556);
#11573=LINE('',#107758,#13557);
#11574=LINE('',#107759,#13558);
#11575=LINE('',#107760,#13559);
#11576=LINE('',#107764,#13560);
#11577=LINE('',#107765,#13561);
#11578=LINE('',#107766,#13562);
#11579=LINE('',#107768,#13563);
#11580=LINE('',#107770,#13564);
#11581=LINE('',#107771,#13565);
#11582=LINE('',#107772,#13566);
#11583=LINE('',#107774,#13567);
#11584=LINE('',#107776,#13568);
#11585=LINE('',#107778,#13569);
#11586=LINE('',#107780,#13570);
#11587=LINE('',#107782,#13571);
#11588=LINE('',#107789,#13572);
#11589=LINE('',#107795,#13573);
#11590=LINE('',#107797,#13574);
#11591=LINE('',#107798,#13575);
#11592=LINE('',#107801,#13576);
#11593=LINE('',#107802,#13577);
#11594=LINE('',#107805,#13578);
#11595=LINE('',#107806,#13579);
#11596=LINE('',#107809,#13580);
#11597=LINE('',#107810,#13581);
#11598=LINE('',#107813,#13582);
#11599=LINE('',#107814,#13583);
#11600=LINE('',#107817,#13584);
#11601=LINE('',#107818,#13585);
#11602=LINE('',#107821,#13586);
#11603=LINE('',#107822,#13587);
#11604=LINE('',#107824,#13588);
#11605=LINE('',#107831,#13589);
#11606=LINE('',#107833,#13590);
#11607=LINE('',#107835,#13591);
#11608=LINE('',#107837,#13592);
#11609=LINE('',#107838,#13593);
#11610=LINE('',#107843,#13594);
#11611=LINE('',#107844,#13595);
#11612=LINE('',#107848,#13596);
#11613=LINE('',#107851,#13597);
#11614=LINE('',#107852,#13598);
#11615=LINE('',#107854,#13599);
#11616=LINE('',#107857,#13600);
#11617=LINE('',#107864,#13601);
#11618=LINE('',#107865,#13602);
#11619=LINE('',#107870,#13603);
#11620=LINE('',#107871,#13604);
#11621=LINE('',#107873,#13605);
#11622=LINE('',#107874,#13606);
#11623=VECTOR('',#50384,0.0015);
#11624=VECTOR('',#50391,0.004);
#11625=VECTOR('',#50416,0.0015);
#11626=VECTOR('',#50429,0.0025);
#11627=VECTOR('',#50436,1.);
#11628=VECTOR('',#50447,1.);
#11629=VECTOR('',#50450,1.);
#11630=VECTOR('',#50455,1.);
#11631=VECTOR('',#50458,1.);
#11632=VECTOR('',#50461,1.);
#11633=VECTOR('',#50462,1.);
#11634=VECTOR('',#50463,1.);
#11635=VECTOR('',#50464,1.);
#11636=VECTOR('',#50465,1.);
#11637=VECTOR('',#50466,1.);
#11638=VECTOR('',#50469,1.);
#11639=VECTOR('',#50474,1.);
#11640=VECTOR('',#50479,1.);
#11641=VECTOR('',#50480,1.);
#11642=VECTOR('',#50481,1.);
#11643=VECTOR('',#50484,1.);
#11644=VECTOR('',#50485,1.);
#11645=VECTOR('',#50486,1.);
#11646=VECTOR('',#50489,1.);
#11647=VECTOR('',#50490,1.);
#11648=VECTOR('',#50491,1.);
#11649=VECTOR('',#50492,1.);
#11650=VECTOR('',#50493,1.);
#11651=VECTOR('',#50494,1.);
#11652=VECTOR('',#50495,1.);
#11653=VECTOR('',#50498,1.);
#11654=VECTOR('',#50501,1.);
#11655=VECTOR('',#50502,1.);
#11656=VECTOR('',#50503,1.);
#11657=VECTOR('',#50504,1.);
#11658=VECTOR('',#50507,1.);
#11659=VECTOR('',#50508,1.);
#11660=VECTOR('',#50511,1.);
#11661=VECTOR('',#50512,1.);
#11662=VECTOR('',#50515,1.);
#11663=VECTOR('',#50518,1.);
#11664=VECTOR('',#50521,1.);
#11665=VECTOR('',#50522,1.);
#11666=VECTOR('',#50529,1.);
#11667=VECTOR('',#50532,1.);
#11668=VECTOR('',#50535,1.);
#11669=VECTOR('',#50538,1.);
#11670=VECTOR('',#50547,0.0015);
#11671=VECTOR('',#50552,0.006);
#11672=VECTOR('',#50757,0.0055);
#11673=VECTOR('',#51264,1.);
#11674=VECTOR('',#51267,1.);
#11675=VECTOR('',#51272,0.999999999999999);
#11676=VECTOR('',#51277,1.);
#11677=VECTOR('',#51280,1.);
#11678=VECTOR('',#51287,1.);
#11679=VECTOR('',#51288,1.);
#11680=VECTOR('',#51299,1.);
#11681=VECTOR('',#51324,1.);
#11682=VECTOR('',#51329,1.);
#11683=VECTOR('',#51334,1.);
#11684=VECTOR('',#51339,1.);
#11685=VECTOR('',#51340,1.);
#11686=VECTOR('',#51341,0.999999999999999);
#11687=VECTOR('',#51344,1.);
#11688=VECTOR('',#51345,1.);
#11689=VECTOR('',#51364,1.);
#11690=VECTOR('',#51369,1.);
#11691=VECTOR('',#51374,1.);
#11692=VECTOR('',#51379,1.);
#11693=VECTOR('',#51380,0.999999999999999);
#11694=VECTOR('',#51381,1.);
#11695=VECTOR('',#51382,1.);
#11696=VECTOR('',#51383,1.);
#11697=VECTOR('',#51404,1.);
#11698=VECTOR('',#51409,1.);
#11699=VECTOR('',#51414,1.);
#11700=VECTOR('',#51415,1.);
#11701=VECTOR('',#51416,1.);
#11702=VECTOR('',#51417,1.);
#11703=VECTOR('',#51420,1.);
#11704=VECTOR('',#51421,1.);
#11705=VECTOR('',#51440,1.);
#11706=VECTOR('',#51445,1.);
#11707=VECTOR('',#51450,1.);
#11708=VECTOR('',#51455,1.);
#11709=VECTOR('',#51456,1.);
#11710=VECTOR('',#51457,1.);
#11711=VECTOR('',#51460,1.);
#11712=VECTOR('',#51461,1.);
#11713=VECTOR('',#51484,1.);
#11714=VECTOR('',#51489,0.01);
#11715=VECTOR('',#51494,1.);
#11716=VECTOR('',#51499,1.);
#11717=VECTOR('',#51500,1.);
#11718=VECTOR('',#51501,1.);
#11719=VECTOR('',#51504,0.01);
#11720=VECTOR('',#51505,1.);
#11721=VECTOR('',#51520,0.01);
#11722=VECTOR('',#51527,0.01);
#11723=VECTOR('',#51532,1.);
#11724=VECTOR('',#51537,1.);
#11725=VECTOR('',#51538,0.01);
#11726=VECTOR('',#51547,1.);
#11727=VECTOR('',#51550,1.);
#11728=VECTOR('',#51563,1.);
#11729=VECTOR('',#51568,1.);
#11730=VECTOR('',#51569,1.);
#11731=VECTOR('',#51576,1.);
#11732=VECTOR('',#51581,1.);
#11733=VECTOR('',#51586,1.);
#11734=VECTOR('',#51589,1.);
#11735=VECTOR('',#51598,1.);
#11736=VECTOR('',#51607,1.);
#11737=VECTOR('',#51612,1.);
#11738=VECTOR('',#51613,1.);
#11739=VECTOR('',#51614,1.);
#11740=VECTOR('',#51625,1.);
#11741=VECTOR('',#51630,1.);
#11742=VECTOR('',#51631,1.);
#11743=VECTOR('',#51634,1.);
#11744=VECTOR('',#51647,1.);
#11745=VECTOR('',#51652,1.);
#11746=VECTOR('',#51653,1.);
#11747=VECTOR('',#51656,1.);
#11748=VECTOR('',#51669,1.);
#11749=VECTOR('',#51674,0.01);
#11750=VECTOR('',#51675,1.);
#11751=VECTOR('',#51678,0.01);
#11752=VECTOR('',#51683,0.01);
#11753=VECTOR('',#51696,1.);
#11754=VECTOR('',#51699,1.);
#11755=VECTOR('',#51712,1.);
#11756=VECTOR('',#51717,1.);
#11757=VECTOR('',#51718,1.);
#11758=VECTOR('',#51725,1.);
#11759=VECTOR('',#51738,0.999999999999999);
#11760=VECTOR('',#51743,1.);
#11761=VECTOR('',#51744,1.);
#11762=VECTOR('',#51747,1.);
#11763=VECTOR('',#51748,1.);
#11764=VECTOR('',#51753,1.);
#11765=VECTOR('',#51754,1.);
#11766=VECTOR('',#51763,1.);
#11767=VECTOR('',#51774,1.);
#11768=VECTOR('',#51779,1.);
#11769=VECTOR('',#51780,1.);
#11770=VECTOR('',#51783,1.);
#11771=VECTOR('',#51796,1.);
#11772=VECTOR('',#51801,1.);
#11773=VECTOR('',#51802,1.);
#11774=VECTOR('',#51805,1.);
#11775=VECTOR('',#51818,1.);
#11776=VECTOR('',#51823,0.01);
#11777=VECTOR('',#51824,1.);
#11778=VECTOR('',#51827,0.01);
#11779=VECTOR('',#51832,0.01);
#11780=VECTOR('',#51845,1.);
#11781=VECTOR('',#51848,1.);
#11782=VECTOR('',#51861,1.);
#11783=VECTOR('',#51866,1.);
#11784=VECTOR('',#51867,1.);
#11785=VECTOR('',#51874,1.);
#11786=VECTOR('',#51887,1.);
#11787=VECTOR('',#51892,1.);
#11788=VECTOR('',#51893,1.);
#11789=VECTOR('',#51896,1.);
#11790=VECTOR('',#51905,1.);
#11791=VECTOR('',#51910,1.);
#11792=VECTOR('',#51911,1.);
#11793=VECTOR('',#51912,1.);
#11794=VECTOR('',#51917,1.);
#11795=VECTOR('',#51922,1.);
#11796=VECTOR('',#51925,1.);
#11797=VECTOR('',#51932,1.);
#11798=VECTOR('',#51945,1.);
#11799=VECTOR('',#51950,1.);
#11800=VECTOR('',#51951,1.);
#11801=VECTOR('',#51954,1.);
#11802=VECTOR('',#51967,1.);
#11803=VECTOR('',#51972,0.01);
#11804=VECTOR('',#51973,1.);
#11805=VECTOR('',#51976,0.01);
#11806=VECTOR('',#51981,0.01);
#11807=VECTOR('',#51994,1.);
#11808=VECTOR('',#51997,1.);
#11809=VECTOR('',#52010,1.);
#11810=VECTOR('',#52015,1.);
#11811=VECTOR('',#52016,1.);
#11812=VECTOR('',#52023,1.);
#11813=VECTOR('',#52036,1.);
#11814=VECTOR('',#52041,1.);
#11815=VECTOR('',#52042,1.);
#11816=VECTOR('',#52045,1.);
#11817=VECTOR('',#52054,1.);
#11818=VECTOR('',#52059,1.);
#11819=VECTOR('',#52060,1.);
#11820=VECTOR('',#52061,1.);
#11821=VECTOR('',#52072,1.);
#11822=VECTOR('',#52077,1.);
#11823=VECTOR('',#52078,1.);
#11824=VECTOR('',#52081,1.);
#11825=VECTOR('',#52086,1.);
#11826=VECTOR('',#52091,1.);
#11827=VECTOR('',#52094,1.);
#11828=VECTOR('',#52103,1.);
#11829=VECTOR('',#52116,0.999999999999999);
#11830=VECTOR('',#52121,0.01);
#11831=VECTOR('',#52122,1.);
#11832=VECTOR('',#52125,0.01);
#11833=VECTOR('',#52130,0.01);
#11834=VECTOR('',#52143,1.);
#11835=VECTOR('',#52146,1.);
#11836=VECTOR('',#52159,1.);
#11837=VECTOR('',#52164,1.);
#11838=VECTOR('',#52165,1.);
#11839=VECTOR('',#52172,1.);
#11840=VECTOR('',#52185,1.);
#11841=VECTOR('',#52190,1.);
#11842=VECTOR('',#52191,1.);
#11843=VECTOR('',#52194,1.);
#11844=VECTOR('',#52203,1.);
#11845=VECTOR('',#52208,1.);
#11846=VECTOR('',#52209,1.);
#11847=VECTOR('',#52210,1.);
#11848=VECTOR('',#52221,1.);
#11849=VECTOR('',#52226,1.);
#11850=VECTOR('',#52227,1.);
#11851=VECTOR('',#52230,1.);
#11852=VECTOR('',#52243,1.);
#11853=VECTOR('',#52248,1.);
#11854=VECTOR('',#52249,1.);
#11855=VECTOR('',#52252,1.);
#11856=VECTOR('',#52257,1.);
#11857=VECTOR('',#52262,0.01);
#11858=VECTOR('',#52265,0.01);
#11859=VECTOR('',#52274,1.);
#11860=VECTOR('',#52279,0.01);
#11861=VECTOR('',#52292,1.);
#11862=VECTOR('',#52295,1.);
#11863=VECTOR('',#52308,1.);
#11864=VECTOR('',#52313,1.);
#11865=VECTOR('',#52314,1.);
#11866=VECTOR('',#52321,1.);
#11867=VECTOR('',#52334,1.);
#11868=VECTOR('',#52339,1.);
#11869=VECTOR('',#52340,1.);
#11870=VECTOR('',#52343,1.);
#11871=VECTOR('',#52352,1.);
#11872=VECTOR('',#52357,1.);
#11873=VECTOR('',#52358,1.);
#11874=VECTOR('',#52359,1.);
#11875=VECTOR('',#52370,1.);
#11876=VECTOR('',#52375,1.);
#11877=VECTOR('',#52376,1.);
#11878=VECTOR('',#52379,1.);
#11879=VECTOR('',#52392,0.999999999999998);
#11880=VECTOR('',#52397,1.);
#11881=VECTOR('',#52398,1.);
#11882=VECTOR('',#52401,1.);
#11883=VECTOR('',#52414,1.);
#11884=VECTOR('',#52419,0.01);
#11885=VECTOR('',#52420,1.);
#11886=VECTOR('',#52423,0.01);
#11887=VECTOR('',#52428,0.01);
#11888=VECTOR('',#52441,1.);
#11889=VECTOR('',#52444,1.);
#11890=VECTOR('',#52457,1.);
#11891=VECTOR('',#52462,1.);
#11892=VECTOR('',#52463,1.);
#11893=VECTOR('',#52470,1.);
#11894=VECTOR('',#52483,1.);
#11895=VECTOR('',#52488,1.);
#11896=VECTOR('',#52489,1.);
#11897=VECTOR('',#52492,1.);
#11898=VECTOR('',#52501,1.);
#11899=VECTOR('',#52506,1.);
#11900=VECTOR('',#52507,1.);
#11901=VECTOR('',#52508,1.);
#11902=VECTOR('',#52519,1.);
#11903=VECTOR('',#52524,1.);
#11904=VECTOR('',#52525,1.);
#11905=VECTOR('',#52528,1.);
#11906=VECTOR('',#52541,1.);
#11907=VECTOR('',#52546,1.);
#11908=VECTOR('',#52547,1.);
#11909=VECTOR('',#52550,1.);
#11910=VECTOR('',#52563,1.);
#11911=VECTOR('',#52568,0.01);
#11912=VECTOR('',#52569,1.);
#11913=VECTOR('',#52572,0.01);
#11914=VECTOR('',#52577,0.01);
#11915=VECTOR('',#52590,1.);
#11916=VECTOR('',#52593,1.);
#11917=VECTOR('',#52606,1.);
#11918=VECTOR('',#52611,1.);
#11919=VECTOR('',#52612,1.);
#11920=VECTOR('',#52619,1.);
#11921=VECTOR('',#52632,1.);
#11922=VECTOR('',#52637,1.);
#11923=VECTOR('',#52638,1.);
#11924=VECTOR('',#52641,1.);
#11925=VECTOR('',#52650,1.);
#11926=VECTOR('',#52655,1.);
#11927=VECTOR('',#52656,1.);
#11928=VECTOR('',#52657,1.);
#11929=VECTOR('',#52668,1.);
#11930=VECTOR('',#52673,1.);
#11931=VECTOR('',#52674,1.);
#11932=VECTOR('',#52677,1.);
#11933=VECTOR('',#52690,1.);
#11934=VECTOR('',#52695,1.);
#11935=VECTOR('',#52696,1.);
#11936=VECTOR('',#52699,1.);
#11937=VECTOR('',#52712,1.);
#11938=VECTOR('',#52717,0.01);
#11939=VECTOR('',#52718,1.);
#11940=VECTOR('',#52721,0.01);
#11941=VECTOR('',#52726,0.01);
#11942=VECTOR('',#52739,1.);
#11943=VECTOR('',#52742,1.);
#11944=VECTOR('',#52755,1.);
#11945=VECTOR('',#52760,1.);
#11946=VECTOR('',#52761,1.);
#11947=VECTOR('',#52768,1.);
#11948=VECTOR('',#52781,1.);
#11949=VECTOR('',#52786,1.);
#11950=VECTOR('',#52787,1.);
#11951=VECTOR('',#52790,1.);
#11952=VECTOR('',#52799,1.);
#11953=VECTOR('',#52804,1.);
#11954=VECTOR('',#52805,1.);
#11955=VECTOR('',#52806,1.);
#11956=VECTOR('',#52817,1.);
#11957=VECTOR('',#52822,0.999999999999999);
#11958=VECTOR('',#52823,1.);
#11959=VECTOR('',#52826,1.);
#11960=VECTOR('',#52839,1.);
#11961=VECTOR('',#52844,1.);
#11962=VECTOR('',#52845,1.);
#11963=VECTOR('',#52848,1.);
#11964=VECTOR('',#52861,1.);
#11965=VECTOR('',#52866,0.01);
#11966=VECTOR('',#52867,1.);
#11967=VECTOR('',#52870,0.01);
#11968=VECTOR('',#52875,0.01);
#11969=VECTOR('',#52888,1.);
#11970=VECTOR('',#52891,1.);
#11971=VECTOR('',#52904,1.);
#11972=VECTOR('',#52909,1.);
#11973=VECTOR('',#52910,1.);
#11974=VECTOR('',#52917,1.);
#11975=VECTOR('',#52930,1.);
#11976=VECTOR('',#52935,1.);
#11977=VECTOR('',#52936,1.);
#11978=VECTOR('',#52939,1.);
#11979=VECTOR('',#52948,1.);
#11980=VECTOR('',#52953,1.);
#11981=VECTOR('',#52954,1.);
#11982=VECTOR('',#52955,1.);
#11983=VECTOR('',#52966,1.);
#11984=VECTOR('',#52971,1.);
#11985=VECTOR('',#52972,1.);
#11986=VECTOR('',#52975,1.);
#11987=VECTOR('',#52988,1.);
#11988=VECTOR('',#52993,1.);
#11989=VECTOR('',#52994,1.);
#11990=VECTOR('',#52997,1.);
#11991=VECTOR('',#53010,0.999999999999999);
#11992=VECTOR('',#53015,0.01);
#11993=VECTOR('',#53016,1.);
#11994=VECTOR('',#53019,0.01);
#11995=VECTOR('',#53024,0.01);
#11996=VECTOR('',#53037,1.);
#11997=VECTOR('',#53040,1.);
#11998=VECTOR('',#53053,1.);
#11999=VECTOR('',#53058,1.);
#12000=VECTOR('',#53059,1.);
#12001=VECTOR('',#53066,1.);
#12002=VECTOR('',#53079,1.);
#12003=VECTOR('',#53084,0.999999999999999);
#12004=VECTOR('',#53085,1.);
#12005=VECTOR('',#53088,1.);
#12006=VECTOR('',#53097,1.);
#12007=VECTOR('',#53102,1.);
#12008=VECTOR('',#53103,1.);
#12009=VECTOR('',#53104,1.);
#12010=VECTOR('',#53115,1.);
#12011=VECTOR('',#53120,1.);
#12012=VECTOR('',#53121,1.);
#12013=VECTOR('',#53124,1.);
#12014=VECTOR('',#53137,1.);
#12015=VECTOR('',#53142,1.);
#12016=VECTOR('',#53143,1.);
#12017=VECTOR('',#53146,1.);
#12018=VECTOR('',#53159,1.);
#12019=VECTOR('',#53164,0.01);
#12020=VECTOR('',#53165,1.);
#12021=VECTOR('',#53168,0.01);
#12022=VECTOR('',#53173,0.01);
#12023=VECTOR('',#53186,1.);
#12024=VECTOR('',#53189,1.);
#12025=VECTOR('',#53202,1.);
#12026=VECTOR('',#53207,1.);
#12027=VECTOR('',#53208,1.);
#12028=VECTOR('',#53215,1.);
#12029=VECTOR('',#53228,1.);
#12030=VECTOR('',#53233,1.);
#12031=VECTOR('',#53234,1.);
#12032=VECTOR('',#53237,1.);
#12033=VECTOR('',#53246,1.);
#12034=VECTOR('',#53251,1.);
#12035=VECTOR('',#53252,1.);
#12036=VECTOR('',#53253,1.);
#12037=VECTOR('',#53264,1.);
#12038=VECTOR('',#53269,0.999999999999999);
#12039=VECTOR('',#53270,1.);
#12040=VECTOR('',#53273,1.);
#12041=VECTOR('',#53286,1.);
#12042=VECTOR('',#53291,1.);
#12043=VECTOR('',#53292,1.);
#12044=VECTOR('',#53295,1.);
#12045=VECTOR('',#53308,1.);
#12046=VECTOR('',#53313,0.01);
#12047=VECTOR('',#53314,1.);
#12048=VECTOR('',#53317,0.01);
#12049=VECTOR('',#53322,0.01);
#12050=VECTOR('',#53335,1.);
#12051=VECTOR('',#53338,1.);
#12052=VECTOR('',#53351,1.);
#12053=VECTOR('',#53356,1.);
#12054=VECTOR('',#53357,1.);
#12055=VECTOR('',#53364,1.);
#12056=VECTOR('',#53377,1.);
#12057=VECTOR('',#53382,1.);
#12058=VECTOR('',#53383,1.);
#12059=VECTOR('',#53386,1.);
#12060=VECTOR('',#53395,1.);
#12061=VECTOR('',#53400,1.);
#12062=VECTOR('',#53401,1.);
#12063=VECTOR('',#53402,1.);
#12064=VECTOR('',#53413,1.);
#12065=VECTOR('',#53418,1.);
#12066=VECTOR('',#53419,1.);
#12067=VECTOR('',#53422,1.);
#12068=VECTOR('',#53435,1.);
#12069=VECTOR('',#53440,1.);
#12070=VECTOR('',#53441,1.);
#12071=VECTOR('',#53444,1.);
#12072=VECTOR('',#53457,1.);
#12073=VECTOR('',#53462,0.01);
#12074=VECTOR('',#53463,1.);
#12075=VECTOR('',#53466,0.01);
#12076=VECTOR('',#53471,0.01);
#12077=VECTOR('',#53484,1.);
#12078=VECTOR('',#53487,1.);
#12079=VECTOR('',#53500,1.);
#12080=VECTOR('',#53505,1.);
#12081=VECTOR('',#53506,1.);
#12082=VECTOR('',#53513,1.);
#12083=VECTOR('',#53526,1.);
#12084=VECTOR('',#53531,1.);
#12085=VECTOR('',#53532,1.);
#12086=VECTOR('',#53535,1.);
#12087=VECTOR('',#53544,1.);
#12088=VECTOR('',#53549,1.);
#12089=VECTOR('',#53550,1.);
#12090=VECTOR('',#53551,0.999999999999999);
#12091=VECTOR('',#53562,1.);
#12092=VECTOR('',#53567,1.);
#12093=VECTOR('',#53568,1.);
#12094=VECTOR('',#53571,1.);
#12095=VECTOR('',#53584,1.);
#12096=VECTOR('',#53589,1.);
#12097=VECTOR('',#53590,1.);
#12098=VECTOR('',#53593,1.);
#12099=VECTOR('',#53606,1.);
#12100=VECTOR('',#53611,0.01);
#12101=VECTOR('',#53612,1.);
#12102=VECTOR('',#53615,0.01);
#12103=VECTOR('',#53620,0.01);
#12104=VECTOR('',#53633,1.);
#12105=VECTOR('',#53636,1.);
#12106=VECTOR('',#53649,1.);
#12107=VECTOR('',#53654,1.);
#12108=VECTOR('',#53655,1.);
#12109=VECTOR('',#53662,1.);
#12110=VECTOR('',#53675,1.);
#12111=VECTOR('',#53680,1.);
#12112=VECTOR('',#53681,1.);
#12113=VECTOR('',#53684,1.);
#12114=VECTOR('',#53693,1.);
#12115=VECTOR('',#53698,1.);
#12116=VECTOR('',#53699,1.);
#12117=VECTOR('',#53700,1.);
#12118=VECTOR('',#53711,1.);
#12119=VECTOR('',#53716,1.);
#12120=VECTOR('',#53717,1.);
#12121=VECTOR('',#53720,1.);
#12122=VECTOR('',#53733,1.);
#12123=VECTOR('',#53738,1.);
#12124=VECTOR('',#53739,1.);
#12125=VECTOR('',#53742,1.);
#12126=VECTOR('',#53755,1.);
#12127=VECTOR('',#53760,0.01);
#12128=VECTOR('',#53761,1.);
#12129=VECTOR('',#53764,0.01);
#12130=VECTOR('',#53769,0.01);
#12131=VECTOR('',#53782,1.);
#12132=VECTOR('',#53785,1.);
#12133=VECTOR('',#53798,1.);
#12134=VECTOR('',#53803,1.);
#12135=VECTOR('',#53804,1.);
#12136=VECTOR('',#53811,1.);
#12137=VECTOR('',#53824,1.);
#12138=VECTOR('',#53829,1.);
#12139=VECTOR('',#53830,1.);
#12140=VECTOR('',#53833,1.);
#12141=VECTOR('',#53842,1.);
#12142=VECTOR('',#53847,1.);
#12143=VECTOR('',#53848,1.);
#12144=VECTOR('',#53849,1.);
#12145=VECTOR('',#53860,1.);
#12146=VECTOR('',#53865,1.);
#12147=VECTOR('',#53866,1.);
#12148=VECTOR('',#53869,1.);
#12149=VECTOR('',#53882,1.);
#12150=VECTOR('',#53887,1.);
#12151=VECTOR('',#53888,1.);
#12152=VECTOR('',#53891,1.);
#12153=VECTOR('',#53904,1.);
#12154=VECTOR('',#53909,0.01);
#12155=VECTOR('',#53910,1.);
#12156=VECTOR('',#53913,0.01);
#12157=VECTOR('',#53918,0.01);
#12158=VECTOR('',#53931,1.);
#12159=VECTOR('',#53934,1.);
#12160=VECTOR('',#53947,1.);
#12161=VECTOR('',#53952,1.);
#12162=VECTOR('',#53953,1.);
#12163=VECTOR('',#53960,1.);
#12164=VECTOR('',#53973,1.);
#12165=VECTOR('',#53978,1.);
#12166=VECTOR('',#53979,0.999999999999999);
#12167=VECTOR('',#53982,1.);
#12168=VECTOR('',#53991,1.);
#12169=VECTOR('',#53996,1.);
#12170=VECTOR('',#53997,1.);
#12171=VECTOR('',#53998,1.);
#12172=VECTOR('',#54009,1.);
#12173=VECTOR('',#54014,1.);
#12174=VECTOR('',#54015,1.);
#12175=VECTOR('',#54018,1.);
#12176=VECTOR('',#54031,1.);
#12177=VECTOR('',#54036,1.);
#12178=VECTOR('',#54037,1.);
#12179=VECTOR('',#54040,1.);
#12180=VECTOR('',#54053,0.999999999999999);
#12181=VECTOR('',#54058,0.01);
#12182=VECTOR('',#54059,1.);
#12183=VECTOR('',#54062,0.01);
#12184=VECTOR('',#54067,0.01);
#12185=VECTOR('',#54080,1.);
#12186=VECTOR('',#54083,1.);
#12187=VECTOR('',#54096,1.);
#12188=VECTOR('',#54101,1.);
#12189=VECTOR('',#54102,0.999999999999999);
#12190=VECTOR('',#54109,1.);
#12191=VECTOR('',#54122,1.);
#12192=VECTOR('',#54127,1.);
#12193=VECTOR('',#54128,1.);
#12194=VECTOR('',#54131,1.);
#12195=VECTOR('',#54140,1.);
#12196=VECTOR('',#54145,1.);
#12197=VECTOR('',#54146,1.);
#12198=VECTOR('',#54147,1.);
#12199=VECTOR('',#54158,1.);
#12200=VECTOR('',#54163,1.);
#12201=VECTOR('',#54164,1.);
#12202=VECTOR('',#54167,1.);
#12203=VECTOR('',#54180,0.999999999999999);
#12204=VECTOR('',#54185,0.999999999999998);
#12205=VECTOR('',#54186,1.);
#12206=VECTOR('',#54189,1.);
#12207=VECTOR('',#54202,1.);
#12208=VECTOR('',#54207,0.01);
#12209=VECTOR('',#54208,1.);
#12210=VECTOR('',#54211,0.01);
#12211=VECTOR('',#54216,0.01);
#12212=VECTOR('',#54229,1.);
#12213=VECTOR('',#54232,1.);
#12214=VECTOR('',#54245,1.);
#12215=VECTOR('',#54250,1.);
#12216=VECTOR('',#54251,1.);
#12217=VECTOR('',#54258,1.);
#12218=VECTOR('',#54271,1.);
#12219=VECTOR('',#54276,0.999999999999998);
#12220=VECTOR('',#54277,1.);
#12221=VECTOR('',#54280,1.);
#12222=VECTOR('',#54289,1.);
#12223=VECTOR('',#54294,1.);
#12224=VECTOR('',#54295,1.);
#12225=VECTOR('',#54296,1.);
#12226=VECTOR('',#54307,1.);
#12227=VECTOR('',#54312,1.);
#12228=VECTOR('',#54313,1.);
#12229=VECTOR('',#54316,1.);
#12230=VECTOR('',#54329,1.);
#12231=VECTOR('',#54334,1.);
#12232=VECTOR('',#54335,1.);
#12233=VECTOR('',#54338,1.);
#12234=VECTOR('',#54351,1.);
#12235=VECTOR('',#54356,0.00999999999999998);
#12236=VECTOR('',#54357,1.);
#12237=VECTOR('',#54360,0.01);
#12238=VECTOR('',#54365,0.01);
#12239=VECTOR('',#54378,1.);
#12240=VECTOR('',#54381,1.);
#12241=VECTOR('',#54394,1.);
#12242=VECTOR('',#54399,1.);
#12243=VECTOR('',#54400,1.);
#12244=VECTOR('',#54407,0.999999999999999);
#12245=VECTOR('',#54420,1.);
#12246=VECTOR('',#54425,1.);
#12247=VECTOR('',#54426,1.);
#12248=VECTOR('',#54429,1.);
#12249=VECTOR('',#54438,1.);
#12250=VECTOR('',#54443,1.);
#12251=VECTOR('',#54444,1.);
#12252=VECTOR('',#54445,1.);
#12253=VECTOR('',#54456,1.);
#12254=VECTOR('',#54461,1.);
#12255=VECTOR('',#54462,1.);
#12256=VECTOR('',#54465,1.);
#12257=VECTOR('',#54478,1.);
#12258=VECTOR('',#54483,1.);
#12259=VECTOR('',#54484,1.);
#12260=VECTOR('',#54487,1.);
#12261=VECTOR('',#54500,1.);
#12262=VECTOR('',#54505,0.01);
#12263=VECTOR('',#54506,1.);
#12264=VECTOR('',#54509,0.01);
#12265=VECTOR('',#54514,0.01);
#12266=VECTOR('',#54527,1.);
#12267=VECTOR('',#54530,1.);
#12268=VECTOR('',#54543,1.);
#12269=VECTOR('',#54548,1.);
#12270=VECTOR('',#54549,1.);
#12271=VECTOR('',#54556,1.);
#12272=VECTOR('',#54569,1.);
#12273=VECTOR('',#54574,1.);
#12274=VECTOR('',#54575,1.);
#12275=VECTOR('',#54578,1.);
#12276=VECTOR('',#54587,1.);
#12277=VECTOR('',#54592,1.);
#12278=VECTOR('',#54593,1.);
#12279=VECTOR('',#54594,1.);
#12280=VECTOR('',#54605,1.);
#12281=VECTOR('',#54610,1.);
#12282=VECTOR('',#54611,1.);
#12283=VECTOR('',#54614,1.);
#12284=VECTOR('',#54627,1.);
#12285=VECTOR('',#54632,0.999999999999999);
#12286=VECTOR('',#54633,1.);
#12287=VECTOR('',#54636,1.);
#12288=VECTOR('',#54649,1.);
#12289=VECTOR('',#54654,0.01);
#12290=VECTOR('',#54655,1.);
#12291=VECTOR('',#54658,0.01);
#12292=VECTOR('',#54663,0.01);
#12293=VECTOR('',#54676,1.);
#12294=VECTOR('',#54679,1.);
#12295=VECTOR('',#54692,1.);
#12296=VECTOR('',#54697,1.);
#12297=VECTOR('',#54698,1.);
#12298=VECTOR('',#54705,1.);
#12299=VECTOR('',#54718,1.);
#12300=VECTOR('',#54723,1.);
#12301=VECTOR('',#54724,1.);
#12302=VECTOR('',#54727,1.);
#12303=VECTOR('',#54736,1.);
#12304=VECTOR('',#54741,1.);
#12305=VECTOR('',#54742,1.);
#12306=VECTOR('',#54743,1.);
#12307=VECTOR('',#54754,1.);
#12308=VECTOR('',#54759,1.);
#12309=VECTOR('',#54760,0.999999999999999);
#12310=VECTOR('',#54763,1.);
#12311=VECTOR('',#54776,1.);
#12312=VECTOR('',#54781,1.);
#12313=VECTOR('',#54782,1.);
#12314=VECTOR('',#54785,1.);
#12315=VECTOR('',#54798,1.);
#12316=VECTOR('',#54803,0.01);
#12317=VECTOR('',#54804,1.);
#12318=VECTOR('',#54807,0.01);
#12319=VECTOR('',#54812,0.01);
#12320=VECTOR('',#54825,1.);
#12321=VECTOR('',#54828,1.);
#12322=VECTOR('',#54841,1.);
#12323=VECTOR('',#54846,1.);
#12324=VECTOR('',#54847,1.);
#12325=VECTOR('',#54854,1.);
#12326=VECTOR('',#54867,1.);
#12327=VECTOR('',#54872,1.);
#12328=VECTOR('',#54873,1.);
#12329=VECTOR('',#54876,1.);
#12330=VECTOR('',#54885,1.);
#12331=VECTOR('',#54890,1.);
#12332=VECTOR('',#54891,1.);
#12333=VECTOR('',#54892,1.);
#12334=VECTOR('',#54903,1.);
#12335=VECTOR('',#54908,1.);
#12336=VECTOR('',#54909,1.);
#12337=VECTOR('',#54912,1.);
#12338=VECTOR('',#54925,1.);
#12339=VECTOR('',#54930,1.);
#12340=VECTOR('',#54931,1.);
#12341=VECTOR('',#54934,1.);
#12342=VECTOR('',#54947,1.);
#12343=VECTOR('',#54952,0.01);
#12344=VECTOR('',#54953,1.);
#12345=VECTOR('',#54956,0.01);
#12346=VECTOR('',#54961,0.01);
#12347=VECTOR('',#54974,1.);
#12348=VECTOR('',#54977,1.);
#12349=VECTOR('',#54990,1.);
#12350=VECTOR('',#54995,1.);
#12351=VECTOR('',#54996,1.);
#12352=VECTOR('',#55003,1.);
#12353=VECTOR('',#55016,1.);
#12354=VECTOR('',#55021,1.);
#12355=VECTOR('',#55022,1.);
#12356=VECTOR('',#55025,1.);
#12357=VECTOR('',#55034,1.);
#12358=VECTOR('',#55039,1.);
#12359=VECTOR('',#55040,1.);
#12360=VECTOR('',#55041,1.);
#12361=VECTOR('',#55052,1.);
#12362=VECTOR('',#55057,1.);
#12363=VECTOR('',#55058,1.);
#12364=VECTOR('',#55061,1.);
#12365=VECTOR('',#55074,1.);
#12366=VECTOR('',#55079,1.);
#12367=VECTOR('',#55080,1.);
#12368=VECTOR('',#55083,1.);
#12369=VECTOR('',#55096,1.);
#12370=VECTOR('',#55101,0.01);
#12371=VECTOR('',#55102,1.);
#12372=VECTOR('',#55105,0.01);
#12373=VECTOR('',#55110,0.01);
#12374=VECTOR('',#55123,1.);
#12375=VECTOR('',#55126,1.);
#12376=VECTOR('',#55139,1.);
#12377=VECTOR('',#55144,1.);
#12378=VECTOR('',#55145,1.);
#12379=VECTOR('',#55152,1.);
#12380=VECTOR('',#55165,1.);
#12381=VECTOR('',#55170,1.);
#12382=VECTOR('',#55171,1.);
#12383=VECTOR('',#55174,1.);
#12384=VECTOR('',#55183,1.);
#12385=VECTOR('',#55188,1.);
#12386=VECTOR('',#55189,1.);
#12387=VECTOR('',#55190,1.);
#12388=VECTOR('',#55201,1.);
#12389=VECTOR('',#55206,1.);
#12390=VECTOR('',#55207,1.);
#12391=VECTOR('',#55210,1.);
#12392=VECTOR('',#55223,1.);
#12393=VECTOR('',#55228,1.);
#12394=VECTOR('',#55229,1.);
#12395=VECTOR('',#55232,1.);
#12396=VECTOR('',#55245,1.);
#12397=VECTOR('',#55250,0.01);
#12398=VECTOR('',#55251,1.);
#12399=VECTOR('',#55254,0.01);
#12400=VECTOR('',#55259,0.01);
#12401=VECTOR('',#55272,1.);
#12402=VECTOR('',#55275,1.);
#12403=VECTOR('',#55288,1.);
#12404=VECTOR('',#55293,1.);
#12405=VECTOR('',#55294,1.);
#12406=VECTOR('',#55301,1.);
#12407=VECTOR('',#55314,1.);
#12408=VECTOR('',#55319,1.);
#12409=VECTOR('',#55320,1.);
#12410=VECTOR('',#55323,1.);
#12411=VECTOR('',#55332,1.);
#12412=VECTOR('',#55337,1.);
#12413=VECTOR('',#55338,1.);
#12414=VECTOR('',#55339,1.);
#12415=VECTOR('',#55350,1.);
#12416=VECTOR('',#55355,1.);
#12417=VECTOR('',#55356,1.);
#12418=VECTOR('',#55359,1.);
#12419=VECTOR('',#55372,1.);
#12420=VECTOR('',#55377,1.);
#12421=VECTOR('',#55378,1.);
#12422=VECTOR('',#55381,1.);
#12423=VECTOR('',#55394,1.);
#12424=VECTOR('',#55399,0.01);
#12425=VECTOR('',#55400,1.);
#12426=VECTOR('',#55403,0.01);
#12427=VECTOR('',#55408,0.01);
#12428=VECTOR('',#55421,1.);
#12429=VECTOR('',#55424,1.);
#12430=VECTOR('',#55437,1.);
#12431=VECTOR('',#55442,1.);
#12432=VECTOR('',#55443,1.);
#12433=VECTOR('',#55450,1.);
#12434=VECTOR('',#55463,1.);
#12435=VECTOR('',#55468,1.);
#12436=VECTOR('',#55469,1.);
#12437=VECTOR('',#55472,1.);
#12438=VECTOR('',#55481,1.);
#12439=VECTOR('',#55486,0.999999999999999);
#12440=VECTOR('',#55487,1.);
#12441=VECTOR('',#55488,1.);
#12442=VECTOR('',#55499,1.);
#12443=VECTOR('',#55504,1.);
#12444=VECTOR('',#55505,1.);
#12445=VECTOR('',#55508,1.);
#12446=VECTOR('',#55521,1.);
#12447=VECTOR('',#55526,1.);
#12448=VECTOR('',#55527,1.);
#12449=VECTOR('',#55530,1.);
#12450=VECTOR('',#55543,0.999999999999998);
#12451=VECTOR('',#55548,0.01);
#12452=VECTOR('',#55549,1.);
#12453=VECTOR('',#55552,0.01);
#12454=VECTOR('',#55557,0.01);
#12455=VECTOR('',#55570,1.);
#12456=VECTOR('',#55573,1.);
#12457=VECTOR('',#55586,1.);
#12458=VECTOR('',#55591,1.);
#12459=VECTOR('',#55592,1.);
#12460=VECTOR('',#55599,1.);
#12461=VECTOR('',#55612,1.);
#12462=VECTOR('',#55617,1.);
#12463=VECTOR('',#55618,1.);
#12464=VECTOR('',#55621,1.);
#12465=VECTOR('',#55630,1.);
#12466=VECTOR('',#55635,1.);
#12467=VECTOR('',#55636,1.);
#12468=VECTOR('',#55637,1.);
#12469=VECTOR('',#55648,1.);
#12470=VECTOR('',#55653,1.);
#12471=VECTOR('',#55654,1.);
#12472=VECTOR('',#55657,1.);
#12473=VECTOR('',#55670,1.);
#12474=VECTOR('',#55675,0.999999999999999);
#12475=VECTOR('',#55676,1.);
#12476=VECTOR('',#55679,1.);
#12477=VECTOR('',#55692,1.);
#12478=VECTOR('',#55697,0.01);
#12479=VECTOR('',#55698,1.);
#12480=VECTOR('',#55701,0.01);
#12481=VECTOR('',#55706,0.01);
#12482=VECTOR('',#55719,1.);
#12483=VECTOR('',#55722,1.);
#12484=VECTOR('',#55735,0.999999999999998);
#12485=VECTOR('',#55740,1.);
#12486=VECTOR('',#55741,1.);
#12487=VECTOR('',#55748,1.);
#12488=VECTOR('',#55761,1.);
#12489=VECTOR('',#55766,1.);
#12490=VECTOR('',#55767,1.);
#12491=VECTOR('',#55770,1.);
#12492=VECTOR('',#55779,1.);
#12493=VECTOR('',#55784,1.);
#12494=VECTOR('',#55785,1.);
#12495=VECTOR('',#55786,1.);
#12496=VECTOR('',#55797,1.);
#12497=VECTOR('',#55802,1.);
#12498=VECTOR('',#55803,1.);
#12499=VECTOR('',#55806,1.);
#12500=VECTOR('',#55819,1.);
#12501=VECTOR('',#55824,1.);
#12502=VECTOR('',#55825,1.);
#12503=VECTOR('',#55828,1.);
#12504=VECTOR('',#55841,1.);
#12505=VECTOR('',#55846,0.01);
#12506=VECTOR('',#55847,1.);
#12507=VECTOR('',#55850,0.01);
#12508=VECTOR('',#55855,0.01);
#12509=VECTOR('',#55868,1.);
#12510=VECTOR('',#55871,1.);
#12511=VECTOR('',#55884,1.);
#12512=VECTOR('',#55889,1.);
#12513=VECTOR('',#55890,1.);
#12514=VECTOR('',#55897,1.);
#12515=VECTOR('',#55910,1.);
#12516=VECTOR('',#55915,1.);
#12517=VECTOR('',#55916,1.);
#12518=VECTOR('',#55919,1.);
#12519=VECTOR('',#55928,1.);
#12520=VECTOR('',#55933,1.);
#12521=VECTOR('',#55934,1.);
#12522=VECTOR('',#55935,1.);
#12523=VECTOR('',#55946,1.);
#12524=VECTOR('',#55951,1.);
#12525=VECTOR('',#55952,1.);
#12526=VECTOR('',#55955,1.);
#12527=VECTOR('',#55968,1.);
#12528=VECTOR('',#55973,1.);
#12529=VECTOR('',#55974,1.);
#12530=VECTOR('',#55977,1.);
#12531=VECTOR('',#55990,1.);
#12532=VECTOR('',#55995,0.01);
#12533=VECTOR('',#55996,1.);
#12534=VECTOR('',#55999,0.01);
#12535=VECTOR('',#56004,0.01);
#12536=VECTOR('',#56017,1.);
#12537=VECTOR('',#56020,1.);
#12538=VECTOR('',#56033,1.);
#12539=VECTOR('',#56038,1.);
#12540=VECTOR('',#56039,1.);
#12541=VECTOR('',#56046,1.);
#12542=VECTOR('',#56059,1.);
#12543=VECTOR('',#56064,1.);
#12544=VECTOR('',#56065,1.);
#12545=VECTOR('',#56068,1.);
#12546=VECTOR('',#56077,1.);
#12547=VECTOR('',#56082,1.);
#12548=VECTOR('',#56083,1.);
#12549=VECTOR('',#56084,1.);
#12550=VECTOR('',#56095,1.);
#12551=VECTOR('',#56100,1.);
#12552=VECTOR('',#56101,1.);
#12553=VECTOR('',#56104,1.);
#12554=VECTOR('',#56117,0.999999999999998);
#12555=VECTOR('',#56122,1.);
#12556=VECTOR('',#56123,1.);
#12557=VECTOR('',#56126,1.);
#12558=VECTOR('',#56139,1.);
#12559=VECTOR('',#56144,0.01);
#12560=VECTOR('',#56145,1.);
#12561=VECTOR('',#56148,0.01);
#12562=VECTOR('',#56153,0.01);
#12563=VECTOR('',#56166,1.);
#12564=VECTOR('',#56169,1.);
#12565=VECTOR('',#56182,1.);
#12566=VECTOR('',#56187,1.);
#12567=VECTOR('',#56188,1.);
#12568=VECTOR('',#56195,1.);
#12569=VECTOR('',#56208,1.);
#12570=VECTOR('',#56213,1.);
#12571=VECTOR('',#56214,1.);
#12572=VECTOR('',#56217,1.);
#12573=VECTOR('',#56226,1.);
#12574=VECTOR('',#56231,1.);
#12575=VECTOR('',#56232,0.999999999999999);
#12576=VECTOR('',#56233,1.);
#12577=VECTOR('',#56244,1.);
#12578=VECTOR('',#56249,1.);
#12579=VECTOR('',#56250,1.);
#12580=VECTOR('',#56253,1.);
#12581=VECTOR('',#56266,1.);
#12582=VECTOR('',#56271,1.);
#12583=VECTOR('',#56272,1.);
#12584=VECTOR('',#56275,1.);
#12585=VECTOR('',#56288,1.);
#12586=VECTOR('',#56293,0.01);
#12587=VECTOR('',#56294,1.);
#12588=VECTOR('',#56297,0.01);
#12589=VECTOR('',#56302,0.01);
#12590=VECTOR('',#56315,1.);
#12591=VECTOR('',#56318,1.);
#12592=VECTOR('',#56331,1.);
#12593=VECTOR('',#56336,0.999999999999999);
#12594=VECTOR('',#56337,1.);
#12595=VECTOR('',#56344,1.);
#12596=VECTOR('',#56357,1.);
#12597=VECTOR('',#56362,1.);
#12598=VECTOR('',#56363,1.);
#12599=VECTOR('',#56366,1.);
#12600=VECTOR('',#56375,1.);
#12601=VECTOR('',#56380,1.);
#12602=VECTOR('',#56381,1.);
#12603=VECTOR('',#56382,1.);
#12604=VECTOR('',#56393,1.);
#12605=VECTOR('',#56398,1.);
#12606=VECTOR('',#56399,1.);
#12607=VECTOR('',#56402,1.);
#12608=VECTOR('',#56415,1.);
#12609=VECTOR('',#56420,0.999999999999998);
#12610=VECTOR('',#56421,1.);
#12611=VECTOR('',#56424,1.);
#12612=VECTOR('',#56437,1.);
#12613=VECTOR('',#56442,0.01);
#12614=VECTOR('',#56443,1.);
#12615=VECTOR('',#56446,0.01);
#12616=VECTOR('',#56451,0.01);
#12617=VECTOR('',#56464,1.);
#12618=VECTOR('',#56467,1.);
#12619=VECTOR('',#56480,1.);
#12620=VECTOR('',#56485,1.);
#12621=VECTOR('',#56486,1.);
#12622=VECTOR('',#56493,1.);
#12623=VECTOR('',#56506,1.);
#12624=VECTOR('',#56511,1.);
#12625=VECTOR('',#56512,1.);
#12626=VECTOR('',#56515,1.);
#12627=VECTOR('',#56524,1.);
#12628=VECTOR('',#56529,1.);
#12629=VECTOR('',#56530,1.);
#12630=VECTOR('',#56531,1.);
#12631=VECTOR('',#56542,1.);
#12632=VECTOR('',#56547,1.);
#12633=VECTOR('',#56548,1.);
#12634=VECTOR('',#56551,1.);
#12635=VECTOR('',#56564,1.);
#12636=VECTOR('',#56569,1.);
#12637=VECTOR('',#56570,1.);
#12638=VECTOR('',#56573,1.);
#12639=VECTOR('',#56586,1.);
#12640=VECTOR('',#56591,0.01);
#12641=VECTOR('',#56592,1.);
#12642=VECTOR('',#56595,0.01);
#12643=VECTOR('',#56600,0.01);
#12644=VECTOR('',#56613,1.);
#12645=VECTOR('',#56616,1.);
#12646=VECTOR('',#56629,1.);
#12647=VECTOR('',#56634,1.);
#12648=VECTOR('',#56635,1.);
#12649=VECTOR('',#56642,1.);
#12650=VECTOR('',#56655,1.);
#12651=VECTOR('',#56660,1.);
#12652=VECTOR('',#56661,1.);
#12653=VECTOR('',#56664,1.);
#12654=VECTOR('',#56673,1.);
#12655=VECTOR('',#56678,1.);
#12656=VECTOR('',#56679,1.);
#12657=VECTOR('',#56680,1.);
#12658=VECTOR('',#56691,1.);
#12659=VECTOR('',#56696,1.);
#12660=VECTOR('',#56697,1.);
#12661=VECTOR('',#56700,1.);
#12662=VECTOR('',#56713,1.);
#12663=VECTOR('',#56718,1.);
#12664=VECTOR('',#56719,1.);
#12665=VECTOR('',#56722,1.);
#12666=VECTOR('',#56735,1.);
#12667=VECTOR('',#56740,0.01);
#12668=VECTOR('',#56741,1.);
#12669=VECTOR('',#56744,0.01);
#12670=VECTOR('',#56749,0.01);
#12671=VECTOR('',#56762,1.);
#12672=VECTOR('',#56765,1.);
#12673=VECTOR('',#56778,1.);
#12674=VECTOR('',#56783,1.);
#12675=VECTOR('',#56784,1.);
#12676=VECTOR('',#56791,1.);
#12677=VECTOR('',#56804,1.);
#12678=VECTOR('',#56809,1.);
#12679=VECTOR('',#56810,1.);
#12680=VECTOR('',#56813,1.);
#12681=VECTOR('',#56822,1.);
#12682=VECTOR('',#56827,1.);
#12683=VECTOR('',#56828,1.);
#12684=VECTOR('',#56829,1.);
#12685=VECTOR('',#56840,1.);
#12686=VECTOR('',#56845,1.);
#12687=VECTOR('',#56846,1.);
#12688=VECTOR('',#56849,1.);
#12689=VECTOR('',#56862,1.);
#12690=VECTOR('',#56867,1.);
#12691=VECTOR('',#56868,1.);
#12692=VECTOR('',#56871,1.);
#12693=VECTOR('',#56884,1.);
#12694=VECTOR('',#56889,0.01);
#12695=VECTOR('',#56890,1.);
#12696=VECTOR('',#56893,0.01);
#12697=VECTOR('',#56898,0.01);
#12698=VECTOR('',#56911,1.);
#12699=VECTOR('',#56914,1.);
#12700=VECTOR('',#56927,1.);
#12701=VECTOR('',#56932,1.);
#12702=VECTOR('',#56933,1.);
#12703=VECTOR('',#56940,1.);
#12704=VECTOR('',#56953,1.);
#12705=VECTOR('',#56958,1.);
#12706=VECTOR('',#56959,1.);
#12707=VECTOR('',#56962,1.);
#12708=VECTOR('',#56971,1.);
#12709=VECTOR('',#56976,1.);
#12710=VECTOR('',#56977,1.);
#12711=VECTOR('',#56978,1.);
#12712=VECTOR('',#56989,1.);
#12713=VECTOR('',#56994,1.);
#12714=VECTOR('',#56995,1.);
#12715=VECTOR('',#56998,1.);
#12716=VECTOR('',#57011,1.);
#12717=VECTOR('',#57016,1.);
#12718=VECTOR('',#57017,1.);
#12719=VECTOR('',#57020,1.);
#12720=VECTOR('',#57033,1.);
#12721=VECTOR('',#57038,0.01);
#12722=VECTOR('',#57039,1.);
#12723=VECTOR('',#57042,0.01);
#12724=VECTOR('',#57047,0.01);
#12725=VECTOR('',#57060,1.);
#12726=VECTOR('',#57063,1.);
#12727=VECTOR('',#57076,1.);
#12728=VECTOR('',#57081,1.);
#12729=VECTOR('',#57082,1.);
#12730=VECTOR('',#57089,1.);
#12731=VECTOR('',#57102,1.);
#12732=VECTOR('',#57107,0.999999999999999);
#12733=VECTOR('',#57108,1.);
#12734=VECTOR('',#57111,1.);
#12735=VECTOR('',#57120,1.);
#12736=VECTOR('',#57125,1.);
#12737=VECTOR('',#57126,1.);
#12738=VECTOR('',#57127,1.);
#12739=VECTOR('',#57138,1.);
#12740=VECTOR('',#57143,1.);
#12741=VECTOR('',#57144,1.);
#12742=VECTOR('',#57147,1.);
#12743=VECTOR('',#57160,1.);
#12744=VECTOR('',#57165,1.);
#12745=VECTOR('',#57166,1.);
#12746=VECTOR('',#57169,1.);
#12747=VECTOR('',#57182,1.);
#12748=VECTOR('',#57187,0.01);
#12749=VECTOR('',#57188,1.);
#12750=VECTOR('',#57191,0.01);
#12751=VECTOR('',#57196,0.01);
#12752=VECTOR('',#57209,1.);
#12753=VECTOR('',#57212,1.);
#12754=VECTOR('',#57225,1.);
#12755=VECTOR('',#57230,1.);
#12756=VECTOR('',#57231,1.);
#12757=VECTOR('',#57238,1.);
#12758=VECTOR('',#57251,1.);
#12759=VECTOR('',#57256,1.);
#12760=VECTOR('',#57257,1.);
#12761=VECTOR('',#57260,1.);
#12762=VECTOR('',#57269,1.);
#12763=VECTOR('',#57274,1.);
#12764=VECTOR('',#57275,1.);
#12765=VECTOR('',#57276,1.);
#12766=VECTOR('',#57287,1.);
#12767=VECTOR('',#57292,1.);
#12768=VECTOR('',#57293,1.);
#12769=VECTOR('',#57296,1.);
#12770=VECTOR('',#57309,1.);
#12771=VECTOR('',#57314,1.);
#12772=VECTOR('',#57315,1.);
#12773=VECTOR('',#57318,1.);
#12774=VECTOR('',#57331,1.);
#12775=VECTOR('',#57336,0.01);
#12776=VECTOR('',#57337,1.);
#12777=VECTOR('',#57340,0.01);
#12778=VECTOR('',#57345,0.01);
#12779=VECTOR('',#57358,1.);
#12780=VECTOR('',#57361,1.);
#12781=VECTOR('',#57374,0.999999999999998);
#12782=VECTOR('',#57379,1.);
#12783=VECTOR('',#57380,1.);
#12784=VECTOR('',#57387,1.);
#12785=VECTOR('',#57400,1.);
#12786=VECTOR('',#57405,1.);
#12787=VECTOR('',#57406,1.);
#12788=VECTOR('',#57409,1.);
#12789=VECTOR('',#57418,1.);
#12790=VECTOR('',#57423,1.);
#12791=VECTOR('',#57424,1.);
#12792=VECTOR('',#57425,1.);
#12793=VECTOR('',#57436,1.);
#12794=VECTOR('',#57441,1.);
#12795=VECTOR('',#57442,0.999999999999999);
#12796=VECTOR('',#57445,1.);
#12797=VECTOR('',#57458,1.);
#12798=VECTOR('',#57463,1.);
#12799=VECTOR('',#57464,1.);
#12800=VECTOR('',#57467,1.);
#12801=VECTOR('',#57480,1.);
#12802=VECTOR('',#57485,0.01);
#12803=VECTOR('',#57486,1.);
#12804=VECTOR('',#57489,0.01);
#12805=VECTOR('',#57494,0.01);
#12806=VECTOR('',#57507,1.);
#12807=VECTOR('',#57510,1.);
#12808=VECTOR('',#57523,1.);
#12809=VECTOR('',#57528,1.);
#12810=VECTOR('',#57529,1.);
#12811=VECTOR('',#57536,1.);
#12812=VECTOR('',#57549,1.);
#12813=VECTOR('',#57554,1.);
#12814=VECTOR('',#57555,1.);
#12815=VECTOR('',#57558,1.);
#12816=VECTOR('',#57567,1.);
#12817=VECTOR('',#57572,1.);
#12818=VECTOR('',#57573,1.);
#12819=VECTOR('',#57574,1.);
#12820=VECTOR('',#57585,1.);
#12821=VECTOR('',#57590,1.);
#12822=VECTOR('',#57591,1.);
#12823=VECTOR('',#57594,1.);
#12824=VECTOR('',#57607,1.);
#12825=VECTOR('',#57612,1.);
#12826=VECTOR('',#57613,1.);
#12827=VECTOR('',#57616,1.);
#12828=VECTOR('',#57629,1.);
#12829=VECTOR('',#57634,0.01);
#12830=VECTOR('',#57635,1.);
#12831=VECTOR('',#57638,0.01);
#12832=VECTOR('',#57643,0.01);
#12833=VECTOR('',#57656,1.);
#12834=VECTOR('',#57659,1.);
#12835=VECTOR('',#57672,1.);
#12836=VECTOR('',#57677,1.);
#12837=VECTOR('',#57678,1.);
#12838=VECTOR('',#57685,1.);
#12839=VECTOR('',#57698,1.);
#12840=VECTOR('',#57703,1.);
#12841=VECTOR('',#57704,1.);
#12842=VECTOR('',#57707,1.);
#12843=VECTOR('',#57716,0.999999999999999);
#12844=VECTOR('',#57721,1.);
#12845=VECTOR('',#57722,1.);
#12846=VECTOR('',#57723,1.);
#12847=VECTOR('',#57734,1.);
#12848=VECTOR('',#57739,1.);
#12849=VECTOR('',#57740,1.);
#12850=VECTOR('',#57743,1.);
#12851=VECTOR('',#57756,1.);
#12852=VECTOR('',#57761,1.);
#12853=VECTOR('',#57762,1.);
#12854=VECTOR('',#57765,1.);
#12855=VECTOR('',#57778,1.);
#12856=VECTOR('',#57783,0.01);
#12857=VECTOR('',#57784,1.);
#12858=VECTOR('',#57787,0.01);
#12859=VECTOR('',#57792,0.01);
#12860=VECTOR('',#57815,1.);
#12861=VECTOR('',#57816,1.);
#12862=VECTOR('',#57821,1.);
#12863=VECTOR('',#57826,0.999999999999998);
#12864=VECTOR('',#57827,1.);
#12865=VECTOR('',#57834,1.);
#12866=VECTOR('',#57847,1.);
#12867=VECTOR('',#57852,1.);
#12868=VECTOR('',#57853,1.);
#12869=VECTOR('',#57856,1.);
#12870=VECTOR('',#57865,1.);
#12871=VECTOR('',#57870,1.);
#12872=VECTOR('',#57871,1.);
#12873=VECTOR('',#57872,1.);
#12874=VECTOR('',#57883,1.);
#12875=VECTOR('',#57888,1.);
#12876=VECTOR('',#57889,1.);
#12877=VECTOR('',#57892,1.);
#12878=VECTOR('',#57905,1.);
#12879=VECTOR('',#57910,1.);
#12880=VECTOR('',#57911,1.);
#12881=VECTOR('',#57914,1.);
#12882=VECTOR('',#57927,1.);
#12883=VECTOR('',#57932,0.01);
#12884=VECTOR('',#57933,1.);
#12885=VECTOR('',#57936,0.01);
#12886=VECTOR('',#57941,0.01);
#12887=VECTOR('',#57974,1.);
#12888=VECTOR('',#57975,1.);
#12889=VECTOR('',#57980,1.);
#12890=VECTOR('',#57985,1.);
#12891=VECTOR('',#57986,1.);
#12892=VECTOR('',#57991,1.);
#12893=VECTOR('',#57996,1.);
#12894=VECTOR('',#58001,1.);
#12895=VECTOR('',#58002,1.);
#12896=VECTOR('',#58005,1.);
#12897=VECTOR('',#58014,1.);
#12898=VECTOR('',#58019,1.);
#12899=VECTOR('',#58020,1.);
#12900=VECTOR('',#58021,1.);
#12901=VECTOR('',#58032,1.);
#12902=VECTOR('',#58037,1.);
#12903=VECTOR('',#58038,1.);
#12904=VECTOR('',#58041,1.);
#12905=VECTOR('',#58054,1.);
#12906=VECTOR('',#58059,1.);
#12907=VECTOR('',#58060,1.);
#12908=VECTOR('',#58063,1.);
#12909=VECTOR('',#58076,1.);
#12910=VECTOR('',#58081,0.01);
#12911=VECTOR('',#58082,1.);
#12912=VECTOR('',#58085,0.01);
#12913=VECTOR('',#58090,0.01);
#12914=VECTOR('',#58131,1.);
#12915=VECTOR('',#58136,1.);
#12916=VECTOR('',#58137,1.);
#12917=VECTOR('',#58142,1.);
#12918=VECTOR('',#58147,1.);
#12919=VECTOR('',#58152,1.);
#12920=VECTOR('',#58153,1.);
#12921=VECTOR('',#58154,1.);
#12922=VECTOR('',#58155,1.);
#12923=VECTOR('',#58160,1.);
#12924=VECTOR('',#58161,1.);
#12925=VECTOR('',#58162,1.);
#12926=VECTOR('',#58169,1.);
#12927=VECTOR('',#58170,1.);
#12928=VECTOR('',#58181,1.);
#12929=VECTOR('',#58186,1.);
#12930=VECTOR('',#58187,1.);
#12931=VECTOR('',#58190,1.);
#12932=VECTOR('',#58203,1.);
#12933=VECTOR('',#58208,1.);
#12934=VECTOR('',#58209,1.);
#12935=VECTOR('',#58212,1.);
#12936=VECTOR('',#58225,1.);
#12937=VECTOR('',#58230,0.01);
#12938=VECTOR('',#58231,1.);
#12939=VECTOR('',#58234,0.01);
#12940=VECTOR('',#58239,0.01);
#12941=VECTOR('',#58286,1.);
#12942=VECTOR('',#58291,1.);
#12943=VECTOR('',#58292,1.);
#12944=VECTOR('',#58293,1.);
#12945=VECTOR('',#58294,0.999999999999999);
#12946=VECTOR('',#58299,1.);
#12947=VECTOR('',#58300,1.);
#12948=VECTOR('',#58301,1.);
#12949=VECTOR('',#58306,1.);
#12950=VECTOR('',#58311,0.999999999999999);
#12951=VECTOR('',#58312,1.);
#12952=VECTOR('',#58315,1.);
#12953=VECTOR('',#58322,0.999999999999999);
#12954=VECTOR('',#58323,1.);
#12955=VECTOR('',#58328,1.);
#12956=VECTOR('',#58333,1.);
#12957=VECTOR('',#58334,1.);
#12958=VECTOR('',#58339,1.);
#12959=VECTOR('',#58352,1.);
#12960=VECTOR('',#58357,1.);
#12961=VECTOR('',#58358,1.);
#12962=VECTOR('',#58361,1.);
#12963=VECTOR('',#58374,1.);
#12964=VECTOR('',#58379,0.01);
#12965=VECTOR('',#58380,1.);
#12966=VECTOR('',#58383,0.01);
#12967=VECTOR('',#58388,0.01);
#12968=VECTOR('',#58441,1.);
#12969=VECTOR('',#58446,1.);
#12970=VECTOR('',#58447,1.);
#12971=VECTOR('',#58448,1.);
#12972=VECTOR('',#58453,1.);
#12973=VECTOR('',#58458,0.999999999999999);
#12974=VECTOR('',#58459,1.);
#12975=VECTOR('',#58460,1.);
#12976=VECTOR('',#58465,1.);
#12977=VECTOR('',#58470,1.);
#12978=VECTOR('',#58471,1.);
#12979=VECTOR('',#58474,1.);
#12980=VECTOR('',#58481,1.);
#12981=VECTOR('',#58482,1.);
#12982=VECTOR('',#58487,1.);
#12983=VECTOR('',#58492,1.);
#12984=VECTOR('',#58493,1.);
#12985=VECTOR('',#58498,1.);
#12986=VECTOR('',#58503,1.);
#12987=VECTOR('',#58508,1.);
#12988=VECTOR('',#58509,1.);
#12989=VECTOR('',#58510,1.);
#12990=VECTOR('',#58523,1.);
#12991=VECTOR('',#58528,0.01);
#12992=VECTOR('',#58529,1.);
#12993=VECTOR('',#58532,0.01);
#12994=VECTOR('',#58537,0.01);
#12995=VECTOR('',#58604,1.);
#12996=VECTOR('',#58609,1.);
#12997=VECTOR('',#58610,1.);
#12998=VECTOR('',#58611,1.);
#12999=VECTOR('',#58616,1.);
#13000=VECTOR('',#58621,1.);
#13001=VECTOR('',#58622,1.);
#13002=VECTOR('',#58623,1.);
#13003=VECTOR('',#58628,1.);
#13004=VECTOR('',#58633,0.01);
#13005=VECTOR('',#58634,1.);
#13006=VECTOR('',#58637,0.01);
#13007=VECTOR('',#58644,1.);
#13008=VECTOR('',#58645,1.);
#13009=VECTOR('',#58650,1.);
#13010=VECTOR('',#58655,1.);
#13011=VECTOR('',#58656,1.);
#13012=VECTOR('',#58661,1.);
#13013=VECTOR('',#58666,1.);
#13014=VECTOR('',#58671,1.);
#13015=VECTOR('',#58672,1.);
#13016=VECTOR('',#58673,1.);
#13017=VECTOR('',#58674,1.);
#13018=VECTOR('',#58679,1.);
#13019=VECTOR('',#58680,1.);
#13020=VECTOR('',#58681,1.);
#13021=VECTOR('',#58686,0.01);
#13022=VECTOR('',#58697,0.01);
#13023=VECTOR('',#60220,0.002);
#13024=VECTOR('',#60227,0.00525);
#13025=VECTOR('',#60234,0.0043952301441823);
#13026=VECTOR('',#60249,0.002);
#13027=VECTOR('',#60256,0.00525);
#13028=VECTOR('',#60269,0.004);
#13029=VECTOR('',#60276,0.005825);
#13030=VECTOR('',#60283,0.010875);
#13031=VECTOR('',#60290,0.010875);
#13032=VECTOR('',#60295,1.);
#13033=VECTOR('',#60298,1.);
#13034=VECTOR('',#60303,1.);
#13035=VECTOR('',#60306,1.);
#13036=VECTOR('',#60311,1.);
#13037=VECTOR('',#60314,1.);
#13038=VECTOR('',#60319,1.);
#13039=VECTOR('',#60322,1.);
#13040=VECTOR('',#60327,1.);
#13041=VECTOR('',#60330,1.);
#13042=VECTOR('',#60335,1.);
#13043=VECTOR('',#60338,1.);
#13044=VECTOR('',#60343,1.);
#13045=VECTOR('',#60346,1.);
#13046=VECTOR('',#60351,1.);
#13047=VECTOR('',#60354,1.);
#13048=VECTOR('',#60359,1.);
#13049=VECTOR('',#60362,1.);
#13050=VECTOR('',#60367,1.);
#13051=VECTOR('',#60370,1.);
#13052=VECTOR('',#60375,1.);
#13053=VECTOR('',#60378,1.);
#13054=VECTOR('',#60383,1.);
#13055=VECTOR('',#60386,1.);
#13056=VECTOR('',#60391,1.);
#13057=VECTOR('',#60394,1.);
#13058=VECTOR('',#60399,1.);
#13059=VECTOR('',#60402,1.);
#13060=VECTOR('',#60407,1.);
#13061=VECTOR('',#60410,1.);
#13062=VECTOR('',#60415,1.);
#13063=VECTOR('',#60418,1.);
#13064=VECTOR('',#60423,1.);
#13065=VECTOR('',#60426,1.);
#13066=VECTOR('',#60431,1.);
#13067=VECTOR('',#60434,1.);
#13068=VECTOR('',#60439,1.);
#13069=VECTOR('',#60442,1.);
#13070=VECTOR('',#60447,1.);
#13071=VECTOR('',#60450,1.);
#13072=VECTOR('',#60455,1.);
#13073=VECTOR('',#60458,1.);
#13074=VECTOR('',#60463,1.);
#13075=VECTOR('',#60466,1.);
#13076=VECTOR('',#60471,1.);
#13077=VECTOR('',#60474,1.);
#13078=VECTOR('',#60479,1.);
#13079=VECTOR('',#60482,1.);
#13080=VECTOR('',#60487,1.);
#13081=VECTOR('',#60490,1.);
#13082=VECTOR('',#60495,1.);
#13083=VECTOR('',#60498,1.);
#13084=VECTOR('',#60503,1.);
#13085=VECTOR('',#60506,1.);
#13086=VECTOR('',#60511,1.);
#13087=VECTOR('',#60514,1.);
#13088=VECTOR('',#60519,1.);
#13089=VECTOR('',#60522,1.);
#13090=VECTOR('',#60527,1.);
#13091=VECTOR('',#60530,1.);
#13092=VECTOR('',#60535,1.);
#13093=VECTOR('',#60538,1.);
#13094=VECTOR('',#60543,1.);
#13095=VECTOR('',#60546,1.);
#13096=VECTOR('',#60551,1.);
#13097=VECTOR('',#60554,1.);
#13098=VECTOR('',#60559,1.);
#13099=VECTOR('',#60562,1.);
#13100=VECTOR('',#60567,1.);
#13101=VECTOR('',#60570,1.);
#13102=VECTOR('',#60575,1.);
#13103=VECTOR('',#60578,1.);
#13104=VECTOR('',#60583,1.);
#13105=VECTOR('',#60586,1.);
#13106=VECTOR('',#60591,1.);
#13107=VECTOR('',#60594,1.);
#13108=VECTOR('',#60599,1.);
#13109=VECTOR('',#60602,1.);
#13110=VECTOR('',#60607,1.);
#13111=VECTOR('',#60610,1.);
#13112=VECTOR('',#60615,1.);
#13113=VECTOR('',#60618,1.);
#13114=VECTOR('',#60623,1.);
#13115=VECTOR('',#60626,1.);
#13116=VECTOR('',#60631,1.);
#13117=VECTOR('',#60634,1.);
#13118=VECTOR('',#60639,1.);
#13119=VECTOR('',#60642,1.);
#13120=VECTOR('',#60647,1.);
#13121=VECTOR('',#60650,1.);
#13122=VECTOR('',#60655,1.);
#13123=VECTOR('',#60658,1.);
#13124=VECTOR('',#60663,1.);
#13125=VECTOR('',#60666,1.);
#13126=VECTOR('',#60671,1.);
#13127=VECTOR('',#60674,1.);
#13128=VECTOR('',#60679,1.);
#13129=VECTOR('',#60682,1.);
#13130=VECTOR('',#60687,1.);
#13131=VECTOR('',#60690,1.);
#13132=VECTOR('',#60695,1.);
#13133=VECTOR('',#60698,1.);
#13134=VECTOR('',#60703,1.);
#13135=VECTOR('',#60704,1.);
#13136=VECTOR('',#60705,1.);
#13137=VECTOR('',#60706,1.);
#13138=VECTOR('',#60707,1.);
#13139=VECTOR('',#60708,1.);
#13140=VECTOR('',#60709,1.);
#13141=VECTOR('',#60710,1.);
#13142=VECTOR('',#60711,1.);
#13143=VECTOR('',#60712,1.);
#13144=VECTOR('',#60713,1.);
#13145=VECTOR('',#60714,1.);
#13146=VECTOR('',#60715,1.);
#13147=VECTOR('',#60716,1.);
#13148=VECTOR('',#60717,1.);
#13149=VECTOR('',#60718,1.);
#13150=VECTOR('',#60719,1.);
#13151=VECTOR('',#60720,1.);
#13152=VECTOR('',#60721,1.);
#13153=VECTOR('',#60722,1.);
#13154=VECTOR('',#60723,1.);
#13155=VECTOR('',#60724,1.);
#13156=VECTOR('',#60725,1.);
#13157=VECTOR('',#60726,1.);
#13158=VECTOR('',#60727,1.);
#13159=VECTOR('',#60728,1.);
#13160=VECTOR('',#60729,1.);
#13161=VECTOR('',#60730,1.);
#13162=VECTOR('',#60731,1.);
#13163=VECTOR('',#60732,1.);
#13164=VECTOR('',#60733,1.);
#13165=VECTOR('',#60734,1.);
#13166=VECTOR('',#60735,1.);
#13167=VECTOR('',#60736,1.);
#13168=VECTOR('',#60737,1.);
#13169=VECTOR('',#60738,1.);
#13170=VECTOR('',#60739,1.);
#13171=VECTOR('',#60740,1.);
#13172=VECTOR('',#60741,1.);
#13173=VECTOR('',#60742,1.);
#13174=VECTOR('',#60743,1.);
#13175=VECTOR('',#60744,1.);
#13176=VECTOR('',#60745,1.);
#13177=VECTOR('',#60746,1.);
#13178=VECTOR('',#60747,1.);
#13179=VECTOR('',#60748,1.);
#13180=VECTOR('',#60749,1.);
#13181=VECTOR('',#60750,1.);
#13182=VECTOR('',#60751,1.);
#13183=VECTOR('',#60752,1.);
#13184=VECTOR('',#60753,1.);
#13185=VECTOR('',#60754,1.);
#13186=VECTOR('',#60755,1.);
#13187=VECTOR('',#60756,1.);
#13188=VECTOR('',#60757,1.);
#13189=VECTOR('',#60758,1.);
#13190=VECTOR('',#60759,1.);
#13191=VECTOR('',#60760,1.);
#13192=VECTOR('',#60761,1.);
#13193=VECTOR('',#60762,1.);
#13194=VECTOR('',#60763,1.);
#13195=VECTOR('',#60764,1.);
#13196=VECTOR('',#60765,1.);
#13197=VECTOR('',#60766,1.);
#13198=VECTOR('',#60767,1.);
#13199=VECTOR('',#60768,1.);
#13200=VECTOR('',#60769,1.);
#13201=VECTOR('',#60770,1.);
#13202=VECTOR('',#60771,1.);
#13203=VECTOR('',#60772,1.);
#13204=VECTOR('',#60773,1.);
#13205=VECTOR('',#60774,1.);
#13206=VECTOR('',#60775,1.);
#13207=VECTOR('',#60776,1.);
#13208=VECTOR('',#60777,1.);
#13209=VECTOR('',#60778,1.);
#13210=VECTOR('',#60779,1.);
#13211=VECTOR('',#60780,1.);
#13212=VECTOR('',#60781,1.);
#13213=VECTOR('',#60782,1.);
#13214=VECTOR('',#60783,1.);
#13215=VECTOR('',#60784,1.);
#13216=VECTOR('',#60785,1.);
#13217=VECTOR('',#60786,1.);
#13218=VECTOR('',#60787,1.);
#13219=VECTOR('',#60788,1.);
#13220=VECTOR('',#60789,1.);
#13221=VECTOR('',#60790,0.999999999999998);
#13222=VECTOR('',#60791,1.);
#13223=VECTOR('',#60792,1.);
#13224=VECTOR('',#60793,1.);
#13225=VECTOR('',#60794,1.);
#13226=VECTOR('',#60795,1.);
#13227=VECTOR('',#60796,1.);
#13228=VECTOR('',#60797,1.);
#13229=VECTOR('',#60798,1.);
#13230=VECTOR('',#60799,1.);
#13231=VECTOR('',#60800,1.);
#13232=VECTOR('',#60801,1.);
#13233=VECTOR('',#60802,1.);
#13234=VECTOR('',#60803,1.);
#13235=VECTOR('',#60804,1.);
#13236=VECTOR('',#60807,1.);
#13237=VECTOR('',#60808,1.);
#13238=VECTOR('',#60809,1.);
#13239=VECTOR('',#60810,1.);
#13240=VECTOR('',#60811,1.);
#13241=VECTOR('',#60812,1.);
#13242=VECTOR('',#60813,1.);
#13243=VECTOR('',#60814,1.);
#13244=VECTOR('',#60815,1.);
#13245=VECTOR('',#60816,1.);
#13246=VECTOR('',#60817,1.);
#13247=VECTOR('',#60818,1.);
#13248=VECTOR('',#60819,1.);
#13249=VECTOR('',#60820,1.);
#13250=VECTOR('',#60821,1.);
#13251=VECTOR('',#60822,1.);
#13252=VECTOR('',#60823,0.999999999999998);
#13253=VECTOR('',#60824,1.);
#13254=VECTOR('',#60825,1.);
#13255=VECTOR('',#60826,1.);
#13256=VECTOR('',#60827,1.);
#13257=VECTOR('',#60828,1.);
#13258=VECTOR('',#60829,1.);
#13259=VECTOR('',#60830,1.);
#13260=VECTOR('',#60831,1.);
#13261=VECTOR('',#60832,1.);
#13262=VECTOR('',#60833,1.);
#13263=VECTOR('',#60834,1.);
#13264=VECTOR('',#60835,1.);
#13265=VECTOR('',#60836,1.);
#13266=VECTOR('',#60837,1.);
#13267=VECTOR('',#60838,1.);
#13268=VECTOR('',#60839,1.);
#13269=VECTOR('',#60840,1.);
#13270=VECTOR('',#60841,1.);
#13271=VECTOR('',#60842,1.);
#13272=VECTOR('',#60843,1.);
#13273=VECTOR('',#60844,1.);
#13274=VECTOR('',#60845,1.);
#13275=VECTOR('',#60846,1.);
#13276=VECTOR('',#60847,1.);
#13277=VECTOR('',#60848,1.);
#13278=VECTOR('',#60849,1.);
#13279=VECTOR('',#60850,1.);
#13280=VECTOR('',#60851,1.);
#13281=VECTOR('',#60852,1.);
#13282=VECTOR('',#60853,1.);
#13283=VECTOR('',#60854,1.);
#13284=VECTOR('',#60855,1.);
#13285=VECTOR('',#60856,1.);
#13286=VECTOR('',#60857,1.);
#13287=VECTOR('',#60858,1.);
#13288=VECTOR('',#60859,1.);
#13289=VECTOR('',#60860,1.);
#13290=VECTOR('',#60861,1.);
#13291=VECTOR('',#60862,1.);
#13292=VECTOR('',#60863,1.);
#13293=VECTOR('',#60864,1.);
#13294=VECTOR('',#60865,1.);
#13295=VECTOR('',#60866,1.);
#13296=VECTOR('',#60867,1.);
#13297=VECTOR('',#60868,1.);
#13298=VECTOR('',#60869,1.);
#13299=VECTOR('',#60870,1.);
#13300=VECTOR('',#60871,1.);
#13301=VECTOR('',#60872,1.);
#13302=VECTOR('',#60873,1.);
#13303=VECTOR('',#60874,1.);
#13304=VECTOR('',#60875,1.);
#13305=VECTOR('',#60876,1.);
#13306=VECTOR('',#60877,1.);
#13307=VECTOR('',#60878,1.);
#13308=VECTOR('',#60879,1.);
#13309=VECTOR('',#60880,1.);
#13310=VECTOR('',#60881,1.);
#13311=VECTOR('',#60882,1.);
#13312=VECTOR('',#60883,1.);
#13313=VECTOR('',#60884,1.);
#13314=VECTOR('',#60885,1.);
#13315=VECTOR('',#60886,1.);
#13316=VECTOR('',#60887,1.);
#13317=VECTOR('',#60888,1.);
#13318=VECTOR('',#60889,1.);
#13319=VECTOR('',#60890,1.);
#13320=VECTOR('',#60891,1.);
#13321=VECTOR('',#60892,1.);
#13322=VECTOR('',#60893,1.);
#13323=VECTOR('',#60894,1.);
#13324=VECTOR('',#60895,1.);
#13325=VECTOR('',#60896,1.);
#13326=VECTOR('',#60897,1.);
#13327=VECTOR('',#60898,1.);
#13328=VECTOR('',#60899,1.);
#13329=VECTOR('',#60900,1.);
#13330=VECTOR('',#60901,1.);
#13331=VECTOR('',#60902,1.);
#13332=VECTOR('',#60903,1.);
#13333=VECTOR('',#60904,1.);
#13334=VECTOR('',#60905,1.);
#13335=VECTOR('',#60906,1.);
#13336=VECTOR('',#60907,1.);
#13337=VECTOR('',#60908,1.);
#13338=VECTOR('',#60919,1.);
#13339=VECTOR('',#60924,1.);
#13340=VECTOR('',#60929,1.);
#13341=VECTOR('',#60934,1.);
#13342=VECTOR('',#60939,1.);
#13343=VECTOR('',#60944,1.);
#13344=VECTOR('',#60949,1.);
#13345=VECTOR('',#60954,1.);
#13346=VECTOR('',#60959,1.);
#13347=VECTOR('',#60964,1.);
#13348=VECTOR('',#60969,1.);
#13349=VECTOR('',#60974,1.);
#13350=VECTOR('',#60979,1.);
#13351=VECTOR('',#60984,1.);
#13352=VECTOR('',#60989,1.);
#13353=VECTOR('',#60994,1.);
#13354=VECTOR('',#60999,1.);
#13355=VECTOR('',#61004,1.);
#13356=VECTOR('',#61009,1.);
#13357=VECTOR('',#61014,1.);
#13358=VECTOR('',#61019,1.);
#13359=VECTOR('',#61024,1.);
#13360=VECTOR('',#61029,1.);
#13361=VECTOR('',#61034,1.);
#13362=VECTOR('',#61039,1.);
#13363=VECTOR('',#61044,1.);
#13364=VECTOR('',#61049,1.);
#13365=VECTOR('',#61054,1.);
#13366=VECTOR('',#61059,1.);
#13367=VECTOR('',#61064,1.);
#13368=VECTOR('',#61069,1.);
#13369=VECTOR('',#61074,1.);
#13370=VECTOR('',#61079,1.);
#13371=VECTOR('',#61084,1.);
#13372=VECTOR('',#61089,1.);
#13373=VECTOR('',#61094,1.);
#13374=VECTOR('',#61099,1.);
#13375=VECTOR('',#61104,1.);
#13376=VECTOR('',#61109,1.);
#13377=VECTOR('',#61114,1.);
#13378=VECTOR('',#61119,1.);
#13379=VECTOR('',#61124,1.);
#13380=VECTOR('',#61129,1.);
#13381=VECTOR('',#61134,1.);
#13382=VECTOR('',#61139,1.);
#13383=VECTOR('',#61144,1.);
#13384=VECTOR('',#61149,1.);
#13385=VECTOR('',#61154,1.);
#13386=VECTOR('',#61159,1.);
#13387=VECTOR('',#61164,1.);
#13388=VECTOR('',#61169,1.);
#13389=VECTOR('',#61178,0.008);
#13390=VECTOR('',#61181,1.);
#13391=VECTOR('',#61184,0.008);
#13392=VECTOR('',#61189,1.);
#13393=VECTOR('',#61196,0.002125);
#13394=VECTOR('',#61203,0.003);
#13395=VECTOR('',#61210,1.);
#13396=VECTOR('',#61213,1.);
#13397=VECTOR('',#61218,0.0025);
#13398=VECTOR('',#61225,0.005875);
#13399=VECTOR('',#61236,0.01125);
#13400=VECTOR('',#61243,0.0015);
#13401=VECTOR('',#61250,1.);
#13402=VECTOR('',#61253,1.);
#13403=VECTOR('',#61258,1.);
#13404=VECTOR('',#61261,1.);
#13405=VECTOR('',#61264,1.);
#13406=VECTOR('',#61269,0.002825);
#13407=VECTOR('',#61276,0.002825);
#13408=VECTOR('',#61283,0.002825);
#13409=VECTOR('',#61290,0.0016);
#13410=VECTOR('',#61297,0.0016);
#13411=VECTOR('',#61300,1.);
#13412=VECTOR('',#61303,0.0016);
#13413=VECTOR('',#61306,1.);
#13414=VECTOR('',#61311,0.0016);
#13415=VECTOR('',#61316,0.0059);
#13416=VECTOR('',#61319,1.);
#13417=VECTOR('',#61322,1.);
#13418=VECTOR('',#61327,1.);
#13419=VECTOR('',#61332,1.);
#13420=VECTOR('',#61335,1.);
#13421=VECTOR('',#61338,1.);
#13422=VECTOR('',#61339,1.);
#13423=VECTOR('',#61340,1.);
#13424=VECTOR('',#61341,1.);
#13425=VECTOR('',#61344,1.);
#13426=VECTOR('',#61347,1.);
#13427=VECTOR('',#61350,1.);
#13428=VECTOR('',#61357,1.);
#13429=VECTOR('',#61360,1.);
#13430=VECTOR('',#61361,1.);
#13431=VECTOR('',#61364,1.);
#13432=VECTOR('',#61365,1.);
#13433=VECTOR('',#61366,1.);
#13434=VECTOR('',#61367,1.);
#13435=VECTOR('',#61368,1.);
#13436=VECTOR('',#61369,1.);
#13437=VECTOR('',#61372,1.);
#13438=VECTOR('',#61373,1.);
#13439=VECTOR('',#61374,1.);
#13440=VECTOR('',#61375,1.);
#13441=VECTOR('',#61376,1.);
#13442=VECTOR('',#61379,1.);
#13443=VECTOR('',#61380,1.);
#13444=VECTOR('',#61381,1.);
#13445=VECTOR('',#61382,1.);
#13446=VECTOR('',#61383,1.);
#13447=VECTOR('',#61386,1.);
#13448=VECTOR('',#61387,1.);
#13449=VECTOR('',#61388,1.);
#13450=VECTOR('',#61389,1.);
#13451=VECTOR('',#61394,1.);
#13452=VECTOR('',#61397,1.);
#13453=VECTOR('',#61400,1.);
#13454=VECTOR('',#61403,1.);
#13455=VECTOR('',#61410,1.);
#13456=VECTOR('',#61419,1.);
#13457=VECTOR('',#61422,1.);
#13458=VECTOR('',#61423,1.);
#13459=VECTOR('',#61424,1.);
#13460=VECTOR('',#61427,1.);
#13461=VECTOR('',#61428,1.);
#13462=VECTOR('',#61429,1.);
#13463=VECTOR('',#61430,1.);
#13464=VECTOR('',#61431,1.);
#13465=VECTOR('',#61432,1.);
#13466=VECTOR('',#61435,1.);
#13467=VECTOR('',#61436,1.);
#13468=VECTOR('',#61437,1.);
#13469=VECTOR('',#61438,1.);
#13470=VECTOR('',#61439,1.);
#13471=VECTOR('',#61440,1.);
#13472=VECTOR('',#61441,1.);
#13473=VECTOR('',#61442,1.);
#13474=VECTOR('',#61443,1.);
#13475=VECTOR('',#61444,1.);
#13476=VECTOR('',#61445,1.);
#13477=VECTOR('',#61446,1.);
#13478=VECTOR('',#61447,1.);
#13479=VECTOR('',#61448,1.);
#13480=VECTOR('',#61449,1.);
#13481=VECTOR('',#61450,1.);
#13482=VECTOR('',#61453,1.);
#13483=VECTOR('',#61454,1.);
#13484=VECTOR('',#61455,1.);
#13485=VECTOR('',#61456,1.);
#13486=VECTOR('',#61457,1.);
#13487=VECTOR('',#61458,1.);
#13488=VECTOR('',#61459,1.);
#13489=VECTOR('',#61460,1.);
#13490=VECTOR('',#61461,1.);
#13491=VECTOR('',#61464,1.);
#13492=VECTOR('',#61467,1.);
#13493=VECTOR('',#61470,1.);
#13494=VECTOR('',#61471,1.);
#13495=VECTOR('',#61472,1.);
#13496=VECTOR('',#61475,1.);
#13497=VECTOR('',#61478,1.);
#13498=VECTOR('',#61481,1.);
#13499=VECTOR('',#61482,1.);
#13500=VECTOR('',#61485,1.);
#13501=VECTOR('',#61492,1.);
#13502=VECTOR('',#61493,1.);
#13503=VECTOR('',#61494,1.);
#13504=VECTOR('',#61497,1.);
#13505=VECTOR('',#61498,1.);
#13506=VECTOR('',#61499,1.);
#13507=VECTOR('',#61500,1.);
#13508=VECTOR('',#61501,1.);
#13509=VECTOR('',#61504,1.);
#13510=VECTOR('',#61505,1.);
#13511=VECTOR('',#61506,1.);
#13512=VECTOR('',#61509,1.);
#13513=VECTOR('',#61510,1.);
#13514=VECTOR('',#61511,1.);
#13515=VECTOR('',#61512,1.);
#13516=VECTOR('',#61513,1.);
#13517=VECTOR('',#61514,1.);
#13518=VECTOR('',#61517,1.);
#13519=VECTOR('',#61518,1.);
#13520=VECTOR('',#61519,1.);
#13521=VECTOR('',#61522,1.);
#13522=VECTOR('',#61523,1.);
#13523=VECTOR('',#61524,1.);
#13524=VECTOR('',#61527,1.);
#13525=VECTOR('',#61528,1.);
#13526=VECTOR('',#61531,1.);
#13527=VECTOR('',#61532,1.);
#13528=VECTOR('',#61535,1.);
#13529=VECTOR('',#61538,1.);
#13530=VECTOR('',#61539,1.);
#13531=VECTOR('',#61542,1.);
#13532=VECTOR('',#61545,1.);
#13533=VECTOR('',#61548,1.);
#13534=VECTOR('',#61551,1.);
#13535=VECTOR('',#61554,1.);
#13536=VECTOR('',#61557,1.);
#13537=VECTOR('',#61568,1.);
#13538=VECTOR('',#61569,1.);
#13539=VECTOR('',#61570,1.);
#13540=VECTOR('',#61573,1.);
#13541=VECTOR('',#61578,1.);
#13542=VECTOR('',#61579,1.);
#13543=VECTOR('',#61582,1.);
#13544=VECTOR('',#61587,1.);
#13545=VECTOR('',#61588,1.);
#13546=VECTOR('',#61591,1.);
#13547=VECTOR('',#61596,1.);
#13548=VECTOR('',#61597,1.);
#13549=VECTOR('',#61600,1.);
#13550=VECTOR('',#61605,1.);
#13551=VECTOR('',#61606,1.);
#13552=VECTOR('',#61613,1.);
#13553=VECTOR('',#61614,1.);
#13554=VECTOR('',#61619,1.);
#13555=VECTOR('',#61622,1.);
#13556=VECTOR('',#61623,1.);
#13557=VECTOR('',#61630,1.);
#13558=VECTOR('',#61631,1.);
#13559=VECTOR('',#61632,1.);
#13560=VECTOR('',#61635,1.);
#13561=VECTOR('',#61636,1.);
#13562=VECTOR('',#61637,1.);
#13563=VECTOR('',#61640,1.);
#13564=VECTOR('',#61641,1.);
#13565=VECTOR('',#61642,1.);
#13566=VECTOR('',#61643,1.);
#13567=VECTOR('',#61646,1.);
#13568=VECTOR('',#61649,1.);
#13569=VECTOR('',#61652,1.);
#13570=VECTOR('',#61655,1.);
#13571=VECTOR('',#61658,1.);
#13572=VECTOR('',#61671,1.);
#13573=VECTOR('',#61680,1.);
#13574=VECTOR('',#61681,1.);
#13575=VECTOR('',#61682,1.);
#13576=VECTOR('',#61685,1.);
#13577=VECTOR('',#61686,1.);
#13578=VECTOR('',#61689,1.);
#13579=VECTOR('',#61690,1.);
#13580=VECTOR('',#61693,1.);
#13581=VECTOR('',#61694,1.);
#13582=VECTOR('',#61697,1.);
#13583=VECTOR('',#61698,1.);
#13584=VECTOR('',#61701,1.);
#13585=VECTOR('',#61702,1.);
#13586=VECTOR('',#61705,1.);
#13587=VECTOR('',#61706,1.);
#13588=VECTOR('',#61709,1.);
#13589=VECTOR('',#61720,1.);
#13590=VECTOR('',#61721,1.);
#13591=VECTOR('',#61722,1.);
#13592=VECTOR('',#61723,1.);
#13593=VECTOR('',#61724,1.);
#13594=VECTOR('',#61731,1.);
#13595=VECTOR('',#61732,1.);
#13596=VECTOR('',#61739,1.);
#13597=VECTOR('',#61742,1.);
#13598=VECTOR('',#61743,1.);
#13599=VECTOR('',#61746,1.);
#13600=VECTOR('',#61751,1.);
#13601=VECTOR('',#61760,1.);
#13602=VECTOR('',#61761,1.);
#13603=VECTOR('',#61766,1.);
#13604=VECTOR('',#61767,1.);
#13605=VECTOR('',#61770,1.);
#13606=VECTOR('',#61771,1.);
#13607=CIRCLE('',#45661,0.00150000000001001);
#13608=CIRCLE('',#45662,0.00150000000001001);
#13609=CIRCLE('',#45664,0.00400000000001001);
#13610=CIRCLE('',#45665,0.00400000000001001);
#13611=CIRCLE('',#45673,0.00100000000001);
#13612=CIRCLE('',#45674,0.0005);
#13613=CIRCLE('',#45675,0.00150000000001);
#13614=CIRCLE('',#45677,0.00150000000001);
#13615=CIRCLE('',#45682,0.00250000000001001);
#13616=CIRCLE('',#45683,0.00250000000001001);
#13617=CIRCLE('',#45684,0.00250000000001001);
#13618=CIRCLE('',#45690,0.00175000000001001);
#13619=CIRCLE('',#45691,0.00175000000001001);
#13620=CIRCLE('',#45693,0.00450000000001);
#13621=CIRCLE('',#45694,0.00450000000001);
#13622=CIRCLE('',#45696,0.00175000000001001);
#13623=CIRCLE('',#45703,0.00175000000001001);
#13624=CIRCLE('',#45719,0.00150000000001001);
#13625=CIRCLE('',#45720,0.00150000000001001);
#13626=CIRCLE('',#45722,0.00550000000001001);
#13627=CIRCLE('',#45723,0.0101999634198228);
#13628=CIRCLE('',#45724,0.00961011190536243);
#13629=CIRCLE('',#45725,0.010199963424716);
#13630=CIRCLE('',#45726,0.00961011190549176);
#13631=CIRCLE('',#45727,0.010199963406456);
#13632=CIRCLE('',#45728,0.0096101119054614);
#13633=CIRCLE('',#45729,0.0101999634077649);
#13634=CIRCLE('',#45730,0.00961011190527579);
#13635=CIRCLE('',#45731,0.0101999634686637);
#13636=CIRCLE('',#45732,0.00961011190568892);
#13637=CIRCLE('',#45733,0.010199963468495);
#13638=CIRCLE('',#45734,0.0096101119055966);
#13639=CIRCLE('',#45735,0.0101999634692665);
#13640=CIRCLE('',#45736,0.0096101119055853);
#13641=CIRCLE('',#45737,0.010199963406071);
#13642=CIRCLE('',#45738,0.00961011190544941);
#13643=CIRCLE('',#45739,0.0101999634685094);
#13644=CIRCLE('',#45740,0.00961011190559131);
#13645=CIRCLE('',#45741,0.0101999634061418);
#13646=CIRCLE('',#45742,0.00961011190556026);
#13647=CIRCLE('',#45743,0.0101999634122045);
#13648=CIRCLE('',#45744,0.00961011190565787);
#13649=CIRCLE('',#45745,0.0101999634683188);
#13650=CIRCLE('',#45746,0.00961011190573388);
#13651=CIRCLE('',#45747,0.010199963468478);
#13652=CIRCLE('',#45748,0.00961011190561557);
#13653=CIRCLE('',#45749,0.010199963468907);
#13654=CIRCLE('',#45750,0.00961011190548147);
#13655=CIRCLE('',#45751,0.0101999634060557);
#13656=CIRCLE('',#45752,0.00961011190541856);
#13657=CIRCLE('',#45753,0.0101999634064124);
#13658=CIRCLE('',#45754,0.00961011190591087);
#13659=CIRCLE('',#45755,0.0101999634061439);
#13660=CIRCLE('',#45756,0.00961011190542911);
#13661=CIRCLE('',#45757,0.0101999634689394);
#13662=CIRCLE('',#45758,0.00961011190529722);
#13663=CIRCLE('',#45759,0.0101999634686951);
#13664=CIRCLE('',#45760,0.00961011190550351);
#13665=CIRCLE('',#45761,0.0101999634689749);
#13666=CIRCLE('',#45762,0.0096101119053556);
#13667=CIRCLE('',#45763,0.0101999634535387);
#13668=CIRCLE('',#45764,0.00961011190563452);
#13669=CIRCLE('',#45765,0.010199963468864);
#13670=CIRCLE('',#45766,0.00961011190551607);
#13671=CIRCLE('',#45767,0.0101999634130628);
#13672=CIRCLE('',#45768,0.00961011190524368);
#13673=CIRCLE('',#45769,0.0101999634342632);
#13674=CIRCLE('',#45770,0.00961011190543232);
#13675=CIRCLE('',#45771,0.0101999634059357);
#13676=CIRCLE('',#45772,0.00961011190551928);
#13677=CIRCLE('',#45773,0.0101999634691664);
#13678=CIRCLE('',#45774,0.00961011257877421);
#13679=CIRCLE('',#45775,0.0101999634074436);
#13680=CIRCLE('',#45776,0.00961011257877713);
#13681=CIRCLE('',#45777,0.0101999634064149);
#13682=CIRCLE('',#45778,0.00961011190539081);
#13683=CIRCLE('',#45779,0.0101999634680358);
#13684=CIRCLE('',#45780,0.00961011190545386);
#13685=CIRCLE('',#45781,0.0101999634383056);
#13686=CIRCLE('',#45782,0.00961011190542872);
#13687=CIRCLE('',#45783,0.0101999634686043);
#13688=CIRCLE('',#45784,0.00961011190523193);
#13689=CIRCLE('',#45785,0.0101999634688037);
#13690=CIRCLE('',#45786,0.00961011190527582);
#13691=CIRCLE('',#45787,0.0101999634682683);
#13692=CIRCLE('',#45788,0.00961011190538962);
#13693=CIRCLE('',#45789,0.010199963406837);
#13694=CIRCLE('',#45790,0.00961011190522354);
#13695=CIRCLE('',#45791,0.0101999634066951);
#13696=CIRCLE('',#45792,0.00961011190518779);
#13697=CIRCLE('',#45793,0.0101999634687797);
#13698=CIRCLE('',#45794,0.0096101119054408);
#13699=CIRCLE('',#45795,0.0101999634124819);
#13700=CIRCLE('',#45796,0.00961011190539864);
#13701=CIRCLE('',#45797,0.0101999634688732);
#13702=CIRCLE('',#45798,0.00961011190543064);
#13703=CIRCLE('',#45799,0.0101999634686598);
#13704=CIRCLE('',#45800,0.00961011190546885);
#13705=CIRCLE('',#45801,0.0101999634685102);
#13706=CIRCLE('',#45802,0.00961011190533588);
#13707=CIRCLE('',#45803,0.0101999634689061);
#13708=CIRCLE('',#45804,0.00961011190537567);
#13709=CIRCLE('',#45805,0.010199963468622);
#13710=CIRCLE('',#45806,0.00961011190512478);
#13711=CIRCLE('',#45807,0.0101999634685834);
#13712=CIRCLE('',#45808,0.00961011190557325);
#13713=CIRCLE('',#45809,0.0101999634135171);
#13714=CIRCLE('',#45810,0.00961011190532499);
#13715=CIRCLE('',#45811,0.0101999634144479);
#13716=CIRCLE('',#45812,0.00961011190541419);
#13717=CIRCLE('',#45813,0.0101999634682382);
#13718=CIRCLE('',#45814,0.00961011190539613);
#13719=CIRCLE('',#45815,0.010199963468837);
#13720=CIRCLE('',#45816,0.0096101119055694);
#13721=CIRCLE('',#45817,0.0101999634070027);
#13722=CIRCLE('',#45818,0.00961011257882628);
#13723=CIRCLE('',#45819,0.0101999634068588);
#13724=CIRCLE('',#45820,0.00961011190535638);
#13725=CIRCLE('',#45821,0.0101999634058789);
#13726=CIRCLE('',#45822,0.00961011190522167);
#13727=CIRCLE('',#45824,0.00550000000000999);
#13728=CIRCLE('',#45825,0.0102493166482249);
#13729=CIRCLE('',#45826,0.0053246973266101);
#13730=CIRCLE('',#45827,0.00475546947659179);
#13731=CIRCLE('',#45828,0.00648603628634445);
#13732=CIRCLE('',#45829,0.0102493166718611);
#13733=CIRCLE('',#45830,0.0102493166487836);
#13734=CIRCLE('',#45831,0.00532469732665603);
#13735=CIRCLE('',#45832,0.00475546947669687);
#13736=CIRCLE('',#45833,0.00648603628675515);
#13737=CIRCLE('',#45834,0.0102493166715216);
#13738=CIRCLE('',#45835,0.0102493166104809);
#13739=CIRCLE('',#45836,0.00532469732652641);
#13740=CIRCLE('',#45837,0.00475546947650176);
#13741=CIRCLE('',#45838,0.00648603628632398);
#13742=CIRCLE('',#45839,0.0102493166719252);
#13743=CIRCLE('',#45840,0.0102493166009724);
#13744=CIRCLE('',#45841,0.00532469721575116);
#13745=CIRCLE('',#45842,0.00475546947660697);
#13746=CIRCLE('',#45843,0.00648603622544307);
#13747=CIRCLE('',#45844,0.0102493166717213);
#13748=CIRCLE('',#45845,0.010249316648423);
#13749=CIRCLE('',#45846,0.00532469732666842);
#13750=CIRCLE('',#45847,0.00475546947669352);
#13751=CIRCLE('',#45848,0.00648603628637552);
#13752=CIRCLE('',#45849,0.0102493166245638);
#13753=CIRCLE('',#45850,0.0102493166005703);
#13754=CIRCLE('',#45851,0.0053246973264583);
#13755=CIRCLE('',#45852,0.00475546947661744);
#13756=CIRCLE('',#45853,0.00648603622472093);
#13757=CIRCLE('',#45854,0.0102493166718273);
#13758=CIRCLE('',#45855,0.0102493166425282);
#13759=CIRCLE('',#45856,0.0053246973263111);
#13760=CIRCLE('',#45857,0.00475546947674408);
#13761=CIRCLE('',#45858,0.00648603628642182);
#13762=CIRCLE('',#45859,0.0102493166722208);
#13763=CIRCLE('',#45860,0.0102493166480392);
#13764=CIRCLE('',#45861,0.00532469732662197);
#13765=CIRCLE('',#45862,0.00475546947672397);
#13766=CIRCLE('',#45863,0.00648603622510153);
#13767=CIRCLE('',#45864,0.0102493166712224);
#13768=CIRCLE('',#45865,0.0102493166012379);
#13769=CIRCLE('',#45866,0.00532469732691152);
#13770=CIRCLE('',#45867,0.00475546947675362);
#13771=CIRCLE('',#45868,0.00648603628632466);
#13772=CIRCLE('',#45869,0.0102493166716241);
#13773=CIRCLE('',#45870,0.0102493166479186);
#13774=CIRCLE('',#45871,0.00532469732665895);
#13775=CIRCLE('',#45872,0.00475546947660793);
#13776=CIRCLE('',#45873,0.00648603628636125);
#13777=CIRCLE('',#45874,0.0102493166710006);
#13778=CIRCLE('',#45875,0.0102493166008836);
#13779=CIRCLE('',#45876,0.00532469732698949);
#13780=CIRCLE('',#45877,0.004755469476696);
#13781=CIRCLE('',#45878,0.00648603628639426);
#13782=CIRCLE('',#45879,0.0102493166718501);
#13783=CIRCLE('',#45880,0.0102493166025515);
#13784=CIRCLE('',#45881,0.00532469732649169);
#13785=CIRCLE('',#45882,0.00475546947661964);
#13786=CIRCLE('',#45883,0.00648603628593725);
#13787=CIRCLE('',#45884,0.0102493166238904);
#13788=CIRCLE('',#45885,0.0102493166011681);
#13789=CIRCLE('',#45886,0.00532469732651491);
#13790=CIRCLE('',#45887,0.00475546947656947);
#13791=CIRCLE('',#45888,0.00648603628638922);
#13792=CIRCLE('',#45889,0.0102493166717296);
#13793=CIRCLE('',#45890,0.0102493166477823);
#13794=CIRCLE('',#45891,0.00532469732669679);
#13795=CIRCLE('',#45892,0.0047554694767808);
#13796=CIRCLE('',#45893,0.0064860362863431);
#13797=CIRCLE('',#45894,0.0102493166250233);
#13798=CIRCLE('',#45895,0.0102493166054584);
#13799=CIRCLE('',#45896,0.00532469714696864);
#13800=CIRCLE('',#45897,0.00475546947657628);
#13801=CIRCLE('',#45898,0.00648603628645712);
#13802=CIRCLE('',#45899,0.0102493166243565);
#13803=CIRCLE('',#45900,0.0102493166004352);
#13804=CIRCLE('',#45901,0.00532469719186945);
#13805=CIRCLE('',#45902,0.00475546947659521);
#13806=CIRCLE('',#45903,0.00648603622541537);
#13807=CIRCLE('',#45904,0.0102493166714882);
#13808=CIRCLE('',#45905,0.0102493166051678);
#13809=CIRCLE('',#45906,0.00532469732704207);
#13810=CIRCLE('',#45907,0.00475546947651806);
#13811=CIRCLE('',#45908,0.00648603628635028);
#13812=CIRCLE('',#45909,0.0102493166241683);
#13813=CIRCLE('',#45910,0.0102493166050561);
#13814=CIRCLE('',#45911,0.00532469732762967);
#13815=CIRCLE('',#45912,0.00475546947641074);
#13816=CIRCLE('',#45913,0.00648603628667914);
#13817=CIRCLE('',#45914,0.0102493166242875);
#13818=CIRCLE('',#45915,0.0102493166003182);
#13819=CIRCLE('',#45916,0.00532469732627292);
#13820=CIRCLE('',#45917,0.00475546947642505);
#13821=CIRCLE('',#45918,0.00648603628637591);
#13822=CIRCLE('',#45919,0.01024931662477);
#13823=CIRCLE('',#45920,0.0102493166012571);
#13824=CIRCLE('',#45921,0.00532469732746319);
#13825=CIRCLE('',#45922,0.00475546947649367);
#13826=CIRCLE('',#45923,0.00648603628630755);
#13827=CIRCLE('',#45924,0.0102493166718604);
#13828=CIRCLE('',#45925,0.0102493166484345);
#13829=CIRCLE('',#45926,0.00532469732665917);
#13830=CIRCLE('',#45927,0.00475546947633255);
#13831=CIRCLE('',#45928,0.0064860362254672);
#13832=CIRCLE('',#45929,0.0102493166247972);
#13833=CIRCLE('',#45930,0.0102493166483869);
#13834=CIRCLE('',#45931,0.00532469732679201);
#13835=CIRCLE('',#45932,0.00475546947631373);
#13836=CIRCLE('',#45933,0.0064860362863926);
#13837=CIRCLE('',#45934,0.0102493166720589);
#13838=CIRCLE('',#45935,0.0102493166714337);
#13839=CIRCLE('',#45936,0.00532469722681492);
#13840=CIRCLE('',#45937,0.0047554694764722);
#13841=CIRCLE('',#45938,0.0064860362862893);
#13842=CIRCLE('',#45939,0.0102493166242712);
#13843=CIRCLE('',#45940,0.0102493166052055);
#13844=CIRCLE('',#45941,0.00532469736046863);
#13845=CIRCLE('',#45942,0.00475546947651302);
#13846=CIRCLE('',#45943,0.00648603629473408);
#13847=CIRCLE('',#45944,0.0102493166288082);
#13848=CIRCLE('',#45945,0.0102493166484294);
#13849=CIRCLE('',#45946,0.00532469732671263);
#13850=CIRCLE('',#45947,0.00475546947665501);
#13851=CIRCLE('',#45948,0.0064860362944419);
#13852=CIRCLE('',#45949,0.0102496495656366);
#13853=CIRCLE('',#45950,0.0102493166480359);
#13854=CIRCLE('',#45951,0.00532469732665437);
#13855=CIRCLE('',#45952,0.00475546947623826);
#13856=CIRCLE('',#45953,0.00648603628674945);
#13857=CIRCLE('',#45954,0.0102493166717214);
#13858=CIRCLE('',#45955,0.0102493166485119);
#13859=CIRCLE('',#45956,0.00532469732678191);
#13860=CIRCLE('',#45957,0.00475546947640079);
#13861=CIRCLE('',#45958,0.00648603628633778);
#13862=CIRCLE('',#45959,0.0102493166239895);
#13863=CIRCLE('',#45960,0.0102493166330884);
#13864=CIRCLE('',#45961,0.00532469732685707);
#13865=CIRCLE('',#45962,0.00475546947639237);
#13866=CIRCLE('',#45963,0.00648603628599675);
#13867=CIRCLE('',#45964,0.0102493166297343);
#13868=CIRCLE('',#45965,0.0102493166013718);
#13869=CIRCLE('',#45966,0.00532469732648639);
#13870=CIRCLE('',#45967,0.00475546947668858);
#13871=CIRCLE('',#45968,0.00648603623363353);
#13872=CIRCLE('',#45969,0.0102493166243019);
#13873=CIRCLE('',#45970,0.0102493166717791);
#13874=CIRCLE('',#45971,0.00532469733008092);
#13875=CIRCLE('',#45972,0.00475546947645808);
#13876=CIRCLE('',#45973,0.00648603628640931);
#13877=CIRCLE('',#45974,0.0102493166719781);
#13878=CIRCLE('',#45975,0.010249316648395);
#13879=CIRCLE('',#45976,0.005324697326878);
#13880=CIRCLE('',#45977,0.00475546947653182);
#13881=CIRCLE('',#45978,0.00648603628598081);
#13882=CIRCLE('',#45979,0.0102493166237232);
#13883=CIRCLE('',#45980,0.0102493166023052);
#13884=CIRCLE('',#45981,0.0053246973266947);
#13885=CIRCLE('',#45982,0.00475546947629264);
#13886=CIRCLE('',#45983,0.00648603628636186);
#13887=CIRCLE('',#45984,0.0102493166717635);
#13888=CIRCLE('',#45985,0.0102493166479927);
#13889=CIRCLE('',#45986,0.00532469732661717);
#13890=CIRCLE('',#45987,0.0047554694764501);
#13891=CIRCLE('',#45988,0.00648603628640458);
#13892=CIRCLE('',#45989,0.0102493166719148);
#13893=CIRCLE('',#45990,0.0102493166007194);
#13894=CIRCLE('',#45991,0.00532469732664688);
#13895=CIRCLE('',#45992,0.00475546947636627);
#13896=CIRCLE('',#45993,0.00648603622475047);
#13897=CIRCLE('',#45994,0.0102493166241635);
#13898=CIRCLE('',#45995,0.0102493166052413);
#13899=CIRCLE('',#45996,0.00532469732675286);
#13900=CIRCLE('',#45997,0.00475546947649013);
#13901=CIRCLE('',#45998,0.00648603628639659);
#13902=CIRCLE('',#45999,0.0102493166716537);
#13903=CIRCLE('',#46000,0.0102493166482303);
#13904=CIRCLE('',#46001,0.0053246973262865);
#13905=CIRCLE('',#46002,0.00475546947630579);
#13906=CIRCLE('',#46003,0.00648603622505416);
#13907=CIRCLE('',#46004,0.0102493166239091);
#13908=CIRCLE('',#46005,0.0102493166478681);
#13909=CIRCLE('',#46006,0.00532469732668171);
#13910=CIRCLE('',#46007,0.00475546947629698);
#13911=CIRCLE('',#46008,0.00648603622531174);
#13912=CIRCLE('',#46009,0.0102493166240524);
#13913=CIRCLE('',#46010,0.0102493166479907);
#13914=CIRCLE('',#46011,0.0053246973267911);
#13915=CIRCLE('',#46012,0.00475546947628155);
#13916=CIRCLE('',#46013,0.00648603628643135);
#13917=CIRCLE('',#46014,0.0102493166717961);
#13918=CIRCLE('',#46015,0.0102493166481149);
#13919=CIRCLE('',#46016,0.00532469732675658);
#13920=CIRCLE('',#46017,0.00475546947656979);
#13921=CIRCLE('',#46018,0.00648603628637084);
#13922=CIRCLE('',#46019,0.0102493166494609);
#13923=CIRCLE('',#46020,0.0102493166022047);
#13924=CIRCLE('',#46021,0.00532469732677744);
#13925=CIRCLE('',#46022,0.00475546947636188);
#13926=CIRCLE('',#46023,0.00648603628633145);
#13927=CIRCLE('',#46024,0.0102493166241846);
#13928=CIRCLE('',#46025,0.0102493166181535);
#13929=CIRCLE('',#46026,0.0053246971466303);
#13930=CIRCLE('',#46027,0.00475546947635082);
#13931=CIRCLE('',#46028,0.00648603628599);
#13932=CIRCLE('',#46029,0.0102493166246586);
#13933=CIRCLE('',#46030,0.0102493166006857);
#13934=CIRCLE('',#46031,0.00532469732601802);
#13935=CIRCLE('',#46032,0.00475546947642643);
#13936=CIRCLE('',#46033,0.00648603628591527);
#13937=CIRCLE('',#46034,0.0102493166716824);
#13938=CIRCLE('',#46035,0.0102493166441937);
#13939=CIRCLE('',#46036,0.00532469732637081);
#13940=CIRCLE('',#46037,0.0047554694765186);
#13941=CIRCLE('',#46038,0.00648603628632817);
#13942=CIRCLE('',#46039,0.0102493166241877);
#13943=CIRCLE('',#46040,0.0102493166338346);
#13944=CIRCLE('',#46041,0.00532469732662526);
#13945=CIRCLE('',#46042,0.00475546947642523);
#13946=CIRCLE('',#46043,0.00648603628644076);
#13947=CIRCLE('',#46044,0.0102493166242875);
#13948=CIRCLE('',#46045,0.0102493166008074);
#13949=CIRCLE('',#46046,0.00532469732655984);
#13950=CIRCLE('',#46047,0.00475546947646747);
#13951=CIRCLE('',#46048,0.00648603628642339);
#13952=CIRCLE('',#46049,0.0102493166386258);
#13953=CIRCLE('',#46050,0.0102493166015152);
#13954=CIRCLE('',#46051,0.00532469732729442);
#13955=CIRCLE('',#46052,0.0047554694765978);
#13956=CIRCLE('',#46053,0.00648603628666572);
#13957=CIRCLE('',#46054,0.0102493166713575);
#13958=CIRCLE('',#46055,0.0102493166001166);
#13959=CIRCLE('',#46056,0.00532469732654698);
#13960=CIRCLE('',#46057,0.00475546947657245);
#13961=CIRCLE('',#46058,0.00648603628626377);
#13962=CIRCLE('',#46059,0.0102493166244758);
#13963=CIRCLE('',#46060,0.0102493166486952);
#13964=CIRCLE('',#46061,0.00532469732693619);
#13965=CIRCLE('',#46062,0.00475546947644521);
#13966=CIRCLE('',#46063,0.00648603628674011);
#13967=CIRCLE('',#46064,0.010249316671993);
#13968=CIRCLE('',#46065,0.0102493166001336);
#13969=CIRCLE('',#46066,0.00532469732673807);
#13970=CIRCLE('',#46067,0.00475546947659657);
#13971=CIRCLE('',#46068,0.00648603628634253);
#13972=CIRCLE('',#46069,0.0102493166245827);
#13973=CIRCLE('',#46070,0.0102493166485861);
#13974=CIRCLE('',#46071,0.00532469732688642);
#13975=CIRCLE('',#46072,0.00475546947650669);
#13976=CIRCLE('',#46073,0.00648603628629632);
#13977=CIRCLE('',#46074,0.0167157066785444);
#13978=CIRCLE('',#46075,0.0109625450112925);
#13979=CIRCLE('',#46077,0.0165541458345315);
#13980=CIRCLE('',#46078,0.0168110399842234);
#13981=CIRCLE('',#46079,0.0110459668039187);
#13982=CIRCLE('',#46080,0.0167928000137521);
#13983=CIRCLE('',#46081,0.0110624552741157);
#13984=CIRCLE('',#46083,0.0167157066790098);
#13985=CIRCLE('',#46084,0.010962545020111);
#13986=CIRCLE('',#46085,0.0166052621069394);
#13987=CIRCLE('',#46086,0.016554145912157);
#13988=CIRCLE('',#46088,0.016557944649642);
#13989=CIRCLE('',#46089,0.0165541496597369);
#13990=CIRCLE('',#46090,0.0165579409211877);
#13991=CIRCLE('',#46094,0.0166048023975909);
#13992=CIRCLE('',#46095,0.0166052658421244);
#13993=CIRCLE('',#46096,0.0166047988011243);
#13994=CIRCLE('',#46098,0.0165579409681659);
#13995=CIRCLE('',#46099,0.016557944360907);
#13996=CIRCLE('',#46100,0.0165541492774108);
#13997=CIRCLE('',#46101,0.0167731971567229);
#13998=CIRCLE('',#46102,0.0110573244852915);
#13999=CIRCLE('',#46103,0.0168013216994734);
#14000=CIRCLE('',#46104,0.0110316530748901);
#14001=CIRCLE('',#46105,0.0167928000125642);
#14002=CIRCLE('',#46106,0.0110624552748644);
#14003=CIRCLE('',#46107,0.0168110399833315);
#14004=CIRCLE('',#46108,0.011045966807248);
#14005=CIRCLE('',#46109,0.0165310254138195);
#14006=CIRCLE('',#46110,0.016605262361828);
#14007=CIRCLE('',#46112,0.0165263187395066);
#14008=CIRCLE('',#46113,0.016531029156974);
#14009=CIRCLE('',#46114,0.0165263151375714);
#14010=CIRCLE('',#46116,0.0166047989403509);
#14011=CIRCLE('',#46117,0.0166048024058239);
#14012=CIRCLE('',#46118,0.0166052659708717);
#14013=CIRCLE('',#46119,0.0166775856851178);
#14014=CIRCLE('',#46120,0.0109205691229868);
#14015=CIRCLE('',#46121,0.0168013216990798);
#14016=CIRCLE('',#46122,0.0110316530724368);
#14017=CIRCLE('',#46123,0.0167731941324261);
#14018=CIRCLE('',#46124,0.0110573150837526);
#14019=CIRCLE('',#46125,0.0165310252579689);
#14020=CIRCLE('',#46127,0.0164211205749457);
#14021=CIRCLE('',#46128,0.0164211166382376);
#14022=CIRCLE('',#46130,0.0165263140892247);
#14023=CIRCLE('',#46131,0.016526317515756);
#14024=CIRCLE('',#46132,0.0165310292173529);
#14025=CIRCLE('',#46133,0.0167388235410816);
#14026=CIRCLE('',#46134,0.0109676133194785);
#14027=CIRCLE('',#46135,0.0166825658002112);
#14028=CIRCLE('',#46136,0.011019447276401);
#14029=CIRCLE('',#46137,0.0166775856847206);
#14030=CIRCLE('',#46138,0.0109205691226522);
#14031=CIRCLE('',#46139,0.0165701550626842);
#14032=CIRCLE('',#46141,0.0165733022770367);
#14033=CIRCLE('',#46142,0.0165701587329592);
#14034=CIRCLE('',#46143,0.0165732980302487);
#14035=CIRCLE('',#46145,0.0164211167233465);
#14036=CIRCLE('',#46146,0.016421120810035);
#14037=CIRCLE('',#46147,0.0168141206455738);
#14038=CIRCLE('',#46148,0.0110535372551865);
#14039=CIRCLE('',#46149,0.0168028432283268);
#14040=CIRCLE('',#46150,0.0110635670224663);
#14041=CIRCLE('',#46151,0.0166825658000333);
#14042=CIRCLE('',#46152,0.0110194472775248);
#14043=CIRCLE('',#46153,0.0167388244010463);
#14044=CIRCLE('',#46154,0.0109676127118324);
#14045=CIRCLE('',#46155,0.016601990891616);
#14046=CIRCLE('',#46156,0.0165701584781876);
#14047=CIRCLE('',#46158,0.0166008671691556);
#14048=CIRCLE('',#46159,0.016601990770559);
#14049=CIRCLE('',#46160,0.016600866394852);
#14050=CIRCLE('',#46162,0.0165732944442546);
#14051=CIRCLE('',#46163,0.0165732946042444);
#14052=CIRCLE('',#46164,0.0165701587076333);
#14053=CIRCLE('',#46165,0.0167577810051783);
#14054=CIRCLE('',#46166,0.01105120005134);
#14055=CIRCLE('',#46167,0.0167907391087188);
#14056=CIRCLE('',#46168,0.0110190981868938);
#14057=CIRCLE('',#46169,0.0168028429615406);
#14058=CIRCLE('',#46170,0.0110635670194223);
#14059=CIRCLE('',#46171,0.0168141206274235);
#14060=CIRCLE('',#46172,0.0110535372956647);
#14061=CIRCLE('',#46173,0.00665874948993467);
#14062=CIRCLE('',#46174,0.0166019908649283);
#14063=CIRCLE('',#46176,0.0166008673107098);
#14064=CIRCLE('',#46177,0.016600867411406);
#14065=CIRCLE('',#46178,0.0166019908993219);
#14066=CIRCLE('',#46182,0.0167907391088827);
#14067=CIRCLE('',#46183,0.0110190981864188);
#14068=CIRCLE('',#46184,0.0167577810055165);
#14069=CIRCLE('',#46185,0.0110511996786626);
#14070=CIRCLE('',#46188,0.00665874807859034);
#14071=CIRCLE('',#46189,0.0167157066782481);
#14072=CIRCLE('',#46190,0.0109625450129288);
#14073=CIRCLE('',#46192,0.0165541458650858);
#14074=CIRCLE('',#46194,0.0165579447496526);
#14075=CIRCLE('',#46195,0.0165541495550316);
#14076=CIRCLE('',#46196,0.0165579407230662);
#14077=CIRCLE('',#46197,0.0168110399843813);
#14078=CIRCLE('',#46198,0.0110459668052798);
#14079=CIRCLE('',#46199,0.0167928000139607);
#14080=CIRCLE('',#46200,0.011062455274128);
#14081=CIRCLE('',#46203,0.0166052623896179);
#14082=CIRCLE('',#46204,0.0167731971566023);
#14083=CIRCLE('',#46205,0.0110573244863002);
#14084=CIRCLE('',#46206,0.0168013216994758);
#14085=CIRCLE('',#46207,0.0110316530728458);
#14086=CIRCLE('',#46208,0.0165310255530965);
#14087=CIRCLE('',#46210,0.0166048020948578);
#14088=CIRCLE('',#46211,0.0166052658282088);
#14089=CIRCLE('',#46212,0.0166047987187429);
#14090=CIRCLE('',#46214,0.0165263176787315);
#14091=CIRCLE('',#46215,0.0165310292102148);
#14092=CIRCLE('',#46216,0.0165263141083913);
#14093=CIRCLE('',#46217,0.0166775856847837);
#14094=CIRCLE('',#46218,0.01092056912188);
#14095=CIRCLE('',#46220,0.0164211204563653);
#14096=CIRCLE('',#46221,0.0164211165490995);
#14097=CIRCLE('',#46222,0.0167388248040795);
#14098=CIRCLE('',#46223,0.0109676124292381);
#14099=CIRCLE('',#46224,0.0166825658003758);
#14100=CIRCLE('',#46225,0.0110194472778358);
#14101=CIRCLE('',#46226,0.0165701550024346);
#14102=CIRCLE('',#46228,0.0165733020496899);
#14103=CIRCLE('',#46229,0.0165701586099358);
#14104=CIRCLE('',#46230,0.0165732979706372);
#14105=CIRCLE('',#46231,0.0168141206457996);
#14106=CIRCLE('',#46232,0.0110535372520998);
#14107=CIRCLE('',#46233,0.0168028429612458);
#14108=CIRCLE('',#46234,0.0110635670226642);
#14109=CIRCLE('',#46235,0.0166019908703622);
#14110=CIRCLE('',#46237,0.0166008745056209);
#14111=CIRCLE('',#46238,0.0166019945478856);
#14112=CIRCLE('',#46239,0.0166008708537231);
#14113=CIRCLE('',#46240,0.0167570839933584);
#14114=CIRCLE('',#46241,0.0110512000528469);
#14115=CIRCLE('',#46242,0.0167907391092656);
#14116=CIRCLE('',#46243,0.0110190981844322);
#14117=CIRCLE('',#46244,0.00665874948996591);
#14118=CIRCLE('',#46250,0.0167157066788449);
#14119=CIRCLE('',#46251,0.0109625450157349);
#14120=CIRCLE('',#46253,0.0165541456612475);
#14121=CIRCLE('',#46255,0.016557944529206);
#14122=CIRCLE('',#46256,0.0165541495662002);
#14123=CIRCLE('',#46257,0.0165579404686478);
#14124=CIRCLE('',#46258,0.0168110399833158);
#14125=CIRCLE('',#46259,0.0110459668058598);
#14126=CIRCLE('',#46260,0.0167928000133157);
#14127=CIRCLE('',#46261,0.0110624552757788);
#14128=CIRCLE('',#46264,0.0166052622563343);
#14129=CIRCLE('',#46266,0.0166048019880859);
#14130=CIRCLE('',#46267,0.016605265693657);
#14131=CIRCLE('',#46268,0.0166047985415224);
#14132=CIRCLE('',#46269,0.016773197157004);
#14133=CIRCLE('',#46270,0.0110573244844948);
#14134=CIRCLE('',#46271,0.0168013217003487);
#14135=CIRCLE('',#46272,0.0110316530741932);
#14136=CIRCLE('',#46273,0.016531025536569);
#14137=CIRCLE('',#46274,0.016677585684276);
#14138=CIRCLE('',#46275,0.010920569120958);
#14139=CIRCLE('',#46277,0.0165263177240885);
#14140=CIRCLE('',#46278,0.0165310290137369);
#14141=CIRCLE('',#46279,0.0165263140293687);
#14142=CIRCLE('',#46281,0.0164211203137004);
#14143=CIRCLE('',#46282,0.0164211163601858);
#14144=CIRCLE('',#46283,0.0167388248040086);
#14145=CIRCLE('',#46284,0.0109676124278852);
#14146=CIRCLE('',#46285,0.0166825658000735);
#14147=CIRCLE('',#46286,0.0110194472744378);
#14148=CIRCLE('',#46287,0.01657015489151);
#14149=CIRCLE('',#46289,0.0165733019052232);
#14150=CIRCLE('',#46290,0.0165701584063188);
#14151=CIRCLE('',#46291,0.0165732978847224);
#14152=CIRCLE('',#46292,0.0168141206460675);
#14153=CIRCLE('',#46293,0.0110535372543768);
#14154=CIRCLE('',#46294,0.0168028429612253);
#14155=CIRCLE('',#46295,0.0110635670207699);
#14156=CIRCLE('',#46296,0.0166019908452381);
#14157=CIRCLE('',#46298,0.0166008745510226);
#14158=CIRCLE('',#46299,0.0166019945379808);
#14159=CIRCLE('',#46300,0.0166008707896187);
#14160=CIRCLE('',#46301,0.0167570839934763);
#14161=CIRCLE('',#46302,0.0110511996765818);
#14162=CIRCLE('',#46303,0.0167907391089836);
#14163=CIRCLE('',#46304,0.011019098183272);
#14164=CIRCLE('',#46305,0.00665874807858906);
#14165=CIRCLE('',#46311,0.0167157066783153);
#14166=CIRCLE('',#46312,0.0109625450148706);
#14167=CIRCLE('',#46314,0.0165541457136845);
#14168=CIRCLE('',#46316,0.0165579445181912);
#14169=CIRCLE('',#46317,0.0165541494994364);
#14170=CIRCLE('',#46318,0.0165579404832497);
#14171=CIRCLE('',#46319,0.0168110399843214);
#14172=CIRCLE('',#46320,0.0110459668049122);
#14173=CIRCLE('',#46321,0.0167928000136182);
#14174=CIRCLE('',#46322,0.0110624552755236);
#14175=CIRCLE('',#46325,0.0166052620429394);
#14176=CIRCLE('',#46327,0.0166048019728615);
#14177=CIRCLE('',#46328,0.0166052654892367);
#14178=CIRCLE('',#46329,0.016604798338537);
#14179=CIRCLE('',#46330,0.0167731971568726);
#14180=CIRCLE('',#46331,0.0110573244857002);
#14181=CIRCLE('',#46332,0.0168013216997007);
#14182=CIRCLE('',#46333,0.0110316530729538);
#14183=CIRCLE('',#46334,0.0165310253681436);
#14184=CIRCLE('',#46336,0.016526317656267);
#14185=CIRCLE('',#46337,0.0165310290197966);
#14186=CIRCLE('',#46338,0.016526313977243);
#14187=CIRCLE('',#46339,0.0166775856850731);
#14188=CIRCLE('',#46340,0.0109205691226483);
#14189=CIRCLE('',#46341,0.0167388248041618);
#14190=CIRCLE('',#46342,0.0109676124265561);
#14191=CIRCLE('',#46343,0.0166825658007631);
#14192=CIRCLE('',#46344,0.0110194472758072);
#14193=CIRCLE('',#46345,0.0165701549483552);
#14194=CIRCLE('',#46347,0.016421120963718);
#14195=CIRCLE('',#46348,0.0164211172523543);
#14196=CIRCLE('',#46350,0.0165733019619278);
#14197=CIRCLE('',#46351,0.0165701584484713);
#14198=CIRCLE('',#46352,0.0165732979233713);
#14199=CIRCLE('',#46353,0.0168141206459143);
#14200=CIRCLE('',#46354,0.0110535372553736);
#14201=CIRCLE('',#46355,0.0168028429611379);
#14202=CIRCLE('',#46356,0.0110635670204192);
#14203=CIRCLE('',#46357,0.01660199084655);
#14204=CIRCLE('',#46359,0.0166008740135834);
#14205=CIRCLE('',#46360,0.0166019943862027);
#14206=CIRCLE('',#46361,0.0166008706679157);
#14207=CIRCLE('',#46362,0.0167571840016751);
#14208=CIRCLE('',#46363,0.0110511996779237);
#14209=CIRCLE('',#46364,0.0167907391086096);
#14210=CIRCLE('',#46365,0.0110190981845606);
#14211=CIRCLE('',#46366,0.00665874807872191);
#14212=CIRCLE('',#46372,0.0167157066787399);
#14213=CIRCLE('',#46373,0.0109625450172281);
#14214=CIRCLE('',#46375,0.016554145863149);
#14215=CIRCLE('',#46377,0.0165579443223679);
#14216=CIRCLE('',#46378,0.0165541494393283);
#14217=CIRCLE('',#46379,0.0165579404080053);
#14218=CIRCLE('',#46380,0.0168110399831297);
#14219=CIRCLE('',#46381,0.0110459668041232);
#14220=CIRCLE('',#46382,0.0167928000133307);
#14221=CIRCLE('',#46383,0.0110624552729397);
#14222=CIRCLE('',#46386,0.0166052621959235);
#14223=CIRCLE('',#46388,0.0166048017987275);
#14224=CIRCLE('',#46389,0.0166052655757444);
#14225=CIRCLE('',#46390,0.0166047982632794);
#14226=CIRCLE('',#46391,0.0167731971567896);
#14227=CIRCLE('',#46392,0.0110573244857354);
#14228=CIRCLE('',#46393,0.0168013216998883);
#14229=CIRCLE('',#46394,0.0110316530750987);
#14230=CIRCLE('',#46395,0.0165310254000604);
#14231=CIRCLE('',#46397,0.0165263173244825);
#14232=CIRCLE('',#46398,0.016531029121176);
#14233=CIRCLE('',#46399,0.016526313649102);
#14234=CIRCLE('',#46400,0.0166775856846902);
#14235=CIRCLE('',#46401,0.0109205691217964);
#14236=CIRCLE('',#46403,0.0164211208389438);
#14237=CIRCLE('',#46404,0.0164211169206929);
#14238=CIRCLE('',#46405,0.0167388235414725);
#14239=CIRCLE('',#46406,0.0109676133176049);
#14240=CIRCLE('',#46407,0.0166825658009187);
#14241=CIRCLE('',#46408,0.0110194472773788);
#14242=CIRCLE('',#46409,0.01657015512772);
#14243=CIRCLE('',#46410,0.0168141206463138);
#14244=CIRCLE('',#46411,0.0110535372541819);
#14245=CIRCLE('',#46412,0.0168028429613);
#14246=CIRCLE('',#46413,0.0110635670202627);
#14247=CIRCLE('',#46414,0.0166019908518525);
#14248=CIRCLE('',#46416,0.0165733014219288);
#14249=CIRCLE('',#46417,0.0165701585380017);
#14250=CIRCLE('',#46418,0.0165732976051541);
#14251=CIRCLE('',#46420,0.0166008740668358);
#14252=CIRCLE('',#46421,0.016601994282197);
#14253=CIRCLE('',#46422,0.0166008706697224);
#14254=CIRCLE('',#46423,0.0167571840017961);
#14255=CIRCLE('',#46424,0.0110511996801296);
#14256=CIRCLE('',#46425,0.0167907401351506);
#14257=CIRCLE('',#46426,0.0110190981852389);
#14258=CIRCLE('',#46427,0.00665874808269402);
#14259=CIRCLE('',#46433,0.0167157066787735);
#14260=CIRCLE('',#46434,0.0109625450086395);
#14261=CIRCLE('',#46436,0.0165541457433777);
#14262=CIRCLE('',#46438,0.0165579439802928);
#14263=CIRCLE('',#46439,0.016554149180976);
#14264=CIRCLE('',#46440,0.0165579403754774);
#14265=CIRCLE('',#46441,0.0168110399834262);
#14266=CIRCLE('',#46442,0.0110459668053105);
#14267=CIRCLE('',#46443,0.0167928000135676);
#14268=CIRCLE('',#46444,0.0110624552748488);
#14269=CIRCLE('',#46447,0.0166052621504435);
#14270=CIRCLE('',#46449,0.0166048016472146);
#14271=CIRCLE('',#46450,0.0166052654283215);
#14272=CIRCLE('',#46451,0.0166047981204781);
#14273=CIRCLE('',#46452,0.0167731971565139);
#14274=CIRCLE('',#46453,0.0110573244859286);
#14275=CIRCLE('',#46454,0.0168013216996024);
#14276=CIRCLE('',#46455,0.0110316530737568);
#14277=CIRCLE('',#46456,0.0165310253926076);
#14278=CIRCLE('',#46458,0.0165263173436374);
#14279=CIRCLE('',#46459,0.0165310288225687);
#14280=CIRCLE('',#46460,0.0165263139459922);
#14281=CIRCLE('',#46461,0.0166775856845203);
#14282=CIRCLE('',#46462,0.0109205691218795);
#14283=CIRCLE('',#46464,0.016421120591577);
#14284=CIRCLE('',#46465,0.0164211170893945);
#14285=CIRCLE('',#46466,0.0167388248044872);
#14286=CIRCLE('',#46467,0.0109676124278148);
#14287=CIRCLE('',#46468,0.0166825658003588);
#14288=CIRCLE('',#46469,0.0110194472751782);
#14289=CIRCLE('',#46470,0.0165701550372275);
#14290=CIRCLE('',#46472,0.016573301534994);
#14291=CIRCLE('',#46473,0.0165701582749609);
#14292=CIRCLE('',#46474,0.0165732975210063);
#14293=CIRCLE('',#46475,0.0168141206462113);
#14294=CIRCLE('',#46476,0.011053537257143);
#14295=CIRCLE('',#46477,0.016802842961573);
#14296=CIRCLE('',#46478,0.0110635670197482);
#14297=CIRCLE('',#46479,0.0166019907560126);
#14298=CIRCLE('',#46480,0.0167571840018051);
#14299=CIRCLE('',#46481,0.0110511996746033);
#14300=CIRCLE('',#46482,0.0167907391147266);
#14301=CIRCLE('',#46483,0.0110190981801841);
#14302=CIRCLE('',#46484,0.00665874807845964);
#14303=CIRCLE('',#46486,0.0166008736798517);
#14304=CIRCLE('',#46487,0.0166019943376052);
#14305=CIRCLE('',#46488,0.0166008704639832);
#14306=CIRCLE('',#46494,0.0167157066787271);
#14307=CIRCLE('',#46495,0.0109625450155126);
#14308=CIRCLE('',#46497,0.0165541457593406);
#14309=CIRCLE('',#46499,0.0165579439133504);
#14310=CIRCLE('',#46500,0.016554149284651);
#14311=CIRCLE('',#46501,0.0165579402711089);
#14312=CIRCLE('',#46502,0.0168110399834225);
#14313=CIRCLE('',#46503,0.0110459668054873);
#14314=CIRCLE('',#46504,0.0167928000134005);
#14315=CIRCLE('',#46505,0.0110624552730069);
#14316=CIRCLE('',#46508,0.0166052623894506);
#14317=CIRCLE('',#46510,0.0166048012956226);
#14318=CIRCLE('',#46511,0.0166052652614101);
#14319=CIRCLE('',#46512,0.0166047979814454);
#14320=CIRCLE('',#46513,0.016773197156408);
#14321=CIRCLE('',#46514,0.011057324485339);
#14322=CIRCLE('',#46515,0.0168013216999789);
#14323=CIRCLE('',#46516,0.0110316530746973);
#14324=CIRCLE('',#46517,0.0165310254083766);
#14325=CIRCLE('',#46519,0.0165263171113626);
#14326=CIRCLE('',#46520,0.0165310288164899);
#14327=CIRCLE('',#46521,0.016526313804532);
#14328=CIRCLE('',#46522,0.0166775856843033);
#14329=CIRCLE('',#46523,0.0109205691207937);
#14330=CIRCLE('',#46525,0.0164211206244058);
#14331=CIRCLE('',#46526,0.0164211168117424);
#14332=CIRCLE('',#46527,0.0167388248044568);
#14333=CIRCLE('',#46528,0.0109676124300459);
#14334=CIRCLE('',#46529,0.0166825658003417);
#14335=CIRCLE('',#46530,0.0110194472761544);
#14336=CIRCLE('',#46531,0.0165701550713745);
#14337=CIRCLE('',#46533,0.0165733013649083);
#14338=CIRCLE('',#46534,0.0165701582459345);
#14339=CIRCLE('',#46535,0.0165732975853571);
#14340=CIRCLE('',#46536,0.0168141206461695);
#14341=CIRCLE('',#46537,0.0110535372551713);
#14342=CIRCLE('',#46538,0.0168028429611972);
#14343=CIRCLE('',#46539,0.0110635670196212);
#14344=CIRCLE('',#46540,0.0166019906622895);
#14345=CIRCLE('',#46542,0.0166008736566399);
#14346=CIRCLE('',#46543,0.0166019942352781);
#14347=CIRCLE('',#46544,0.0166008704873754);
#14348=CIRCLE('',#46545,0.0167571840019032);
#14349=CIRCLE('',#46546,0.0110511996781316);
#14350=CIRCLE('',#46547,0.0167907391094546);
#14351=CIRCLE('',#46548,0.0110190981863504);
#14352=CIRCLE('',#46549,0.00665874807845054);
#14353=CIRCLE('',#46555,0.0167157066788714);
#14354=CIRCLE('',#46556,0.0109625450156485);
#14355=CIRCLE('',#46558,0.0165541458403176);
#14356=CIRCLE('',#46560,0.0165579438000108);
#14357=CIRCLE('',#46561,0.0165541491923771);
#14358=CIRCLE('',#46562,0.0165579401565676);
#14359=CIRCLE('',#46563,0.0168110399837841);
#14360=CIRCLE('',#46564,0.01104596680535);
#14361=CIRCLE('',#46565,0.0167928000135096);
#14362=CIRCLE('',#46566,0.0110624552742451);
#14363=CIRCLE('',#46569,0.0166052623307736);
#14364=CIRCLE('',#46571,0.0166048011321904);
#14365=CIRCLE('',#46572,0.0166052652850872);
#14366=CIRCLE('',#46573,0.0166047979680738);
#14367=CIRCLE('',#46574,0.0167731971565765);
#14368=CIRCLE('',#46575,0.0110573244859317);
#14369=CIRCLE('',#46576,0.0168013216998573);
#14370=CIRCLE('',#46577,0.0110316530736586);
#14371=CIRCLE('',#46578,0.0165310254666878);
#14372=CIRCLE('',#46580,0.0165263168519717);
#14373=CIRCLE('',#46581,0.0165310286498186);
#14374=CIRCLE('',#46582,0.0165263136882871);
#14375=CIRCLE('',#46583,0.0166775856847044);
#14376=CIRCLE('',#46584,0.0109205691215522);
#14377=CIRCLE('',#46586,0.0164211204165485);
#14378=CIRCLE('',#46587,0.01642111702004);
#14379=CIRCLE('',#46588,0.0167388248040759);
#14380=CIRCLE('',#46589,0.010967612429176);
#14381=CIRCLE('',#46590,0.0166825658002452);
#14382=CIRCLE('',#46591,0.0110194472759032);
#14383=CIRCLE('',#46592,0.0165701549294572);
#14384=CIRCLE('',#46594,0.0165733010869347);
#14385=CIRCLE('',#46595,0.0165701581404128);
#14386=CIRCLE('',#46596,0.0165732974129815);
#14387=CIRCLE('',#46597,0.0168141206456206);
#14388=CIRCLE('',#46598,0.0110535372554596);
#14389=CIRCLE('',#46599,0.016802842961168);
#14390=CIRCLE('',#46600,0.0110635670198317);
#14391=CIRCLE('',#46601,0.0166019909206233);
#14392=CIRCLE('',#46603,0.0166008736960907);
#14393=CIRCLE('',#46604,0.0166019942659323);
#14394=CIRCLE('',#46605,0.0166008703795521);
#14395=CIRCLE('',#46606,0.0167571840017354);
#14396=CIRCLE('',#46607,0.0110511996746513);
#14397=CIRCLE('',#46608,0.016790739109306);
#14398=CIRCLE('',#46609,0.0110190981849237);
#14399=CIRCLE('',#46610,0.00665874807849537);
#14400=CIRCLE('',#46616,0.0167157066788494);
#14401=CIRCLE('',#46617,0.0109625450144348);
#14402=CIRCLE('',#46619,0.0165541457392142);
#14403=CIRCLE('',#46621,0.0165579435275741);
#14404=CIRCLE('',#46622,0.0165541490391494);
#14405=CIRCLE('',#46623,0.01655794009905);
#14406=CIRCLE('',#46624,0.0168110399836772);
#14407=CIRCLE('',#46625,0.0110459668047881);
#14408=CIRCLE('',#46626,0.0167928000132441);
#14409=CIRCLE('',#46627,0.011062455274256);
#14410=CIRCLE('',#46630,0.0166052622859872);
#14411=CIRCLE('',#46632,0.0166048011030158);
#14412=CIRCLE('',#46633,0.016605265295473);
#14413=CIRCLE('',#46634,0.0166047979887019);
#14414=CIRCLE('',#46635,0.0167731971568965);
#14415=CIRCLE('',#46636,0.0110573244855055);
#14416=CIRCLE('',#46637,0.0168013216999169);
#14417=CIRCLE('',#46638,0.0110316530742442);
#14418=CIRCLE('',#46639,0.0165310254614906);
#14419=CIRCLE('',#46641,0.0165263165791028);
#14420=CIRCLE('',#46642,0.0165310285681001);
#14421=CIRCLE('',#46643,0.01652631359464);
#14422=CIRCLE('',#46644,0.0166775856846869);
#14423=CIRCLE('',#46645,0.0109205691221241);
#14424=CIRCLE('',#46647,0.0164211201277747);
#14425=CIRCLE('',#46648,0.0164211167583284);
#14426=CIRCLE('',#46649,0.0167388248042462);
#14427=CIRCLE('',#46650,0.010967612427505);
#14428=CIRCLE('',#46651,0.0166825658003648);
#14429=CIRCLE('',#46652,0.0110194472768145);
#14430=CIRCLE('',#46653,0.0165701550156401);
#14431=CIRCLE('',#46655,0.016573300951402);
#14432=CIRCLE('',#46656,0.0165701580778124);
#14433=CIRCLE('',#46657,0.0165732974503698);
#14434=CIRCLE('',#46658,0.0168141206459052);
#14435=CIRCLE('',#46659,0.0110535372556727);
#14436=CIRCLE('',#46660,0.0168028429610878);
#14437=CIRCLE('',#46661,0.0110635670209691);
#14438=CIRCLE('',#46662,0.0166019907928354);
#14439=CIRCLE('',#46664,0.0166008734712458);
#14440=CIRCLE('',#46665,0.0166019940729384);
#14441=CIRCLE('',#46666,0.0166008703331209);
#14442=CIRCLE('',#46667,0.0167571840018693);
#14443=CIRCLE('',#46668,0.0110511996747374);
#14444=CIRCLE('',#46669,0.0167907391089814);
#14445=CIRCLE('',#46670,0.0110190981862152);
#14446=CIRCLE('',#46671,0.0066587480786164);
#14447=CIRCLE('',#46677,0.0167157066788542);
#14448=CIRCLE('',#46678,0.010962545014382);
#14449=CIRCLE('',#46680,0.0165541458107732);
#14450=CIRCLE('',#46682,0.01655794340933);
#14451=CIRCLE('',#46683,0.0165541490562889);
#14452=CIRCLE('',#46684,0.0165579399946687);
#14453=CIRCLE('',#46685,0.0168110399835196);
#14454=CIRCLE('',#46686,0.0110459668056131);
#14455=CIRCLE('',#46687,0.0167928000130259);
#14456=CIRCLE('',#46688,0.0110624552743332);
#14457=CIRCLE('',#46691,0.0166052623067422);
#14458=CIRCLE('',#46693,0.0166048008214679);
#14459=CIRCLE('',#46694,0.0166052651212716);
#14460=CIRCLE('',#46695,0.0166047978286768);
#14461=CIRCLE('',#46696,0.0167731971563245);
#14462=CIRCLE('',#46697,0.0110573244853286);
#14463=CIRCLE('',#46698,0.0168013216997433);
#14464=CIRCLE('',#46699,0.0110316530741568);
#14465=CIRCLE('',#46700,0.0165310254486529);
#14466=CIRCLE('',#46702,0.0165263165711203);
#14467=CIRCLE('',#46703,0.0165310285556837);
#14468=CIRCLE('',#46704,0.0165263135008287);
#14469=CIRCLE('',#46705,0.016677585684674);
#14470=CIRCLE('',#46706,0.0109205691216249);
#14471=CIRCLE('',#46708,0.016421119933082);
#14472=CIRCLE('',#46709,0.0164211167102725);
#14473=CIRCLE('',#46710,0.0167388248042328);
#14474=CIRCLE('',#46711,0.0109676124278834);
#14475=CIRCLE('',#46712,0.016682565800226);
#14476=CIRCLE('',#46713,0.0110194472759658);
#14477=CIRCLE('',#46714,0.0165701548739711);
#14478=CIRCLE('',#46716,0.0165733007123841);
#14479=CIRCLE('',#46717,0.0165701579072542);
#14480=CIRCLE('',#46718,0.0165732973056387);
#14481=CIRCLE('',#46719,0.0168141206272229);
#14482=CIRCLE('',#46720,0.0110535372947043);
#14483=CIRCLE('',#46721,0.0168028429611657);
#14484=CIRCLE('',#46722,0.0110635670203127);
#14485=CIRCLE('',#46723,0.0166019907732245);
#14486=CIRCLE('',#46725,0.0166008734031971);
#14487=CIRCLE('',#46726,0.0166019940334412);
#14488=CIRCLE('',#46727,0.0166008701570932);
#14489=CIRCLE('',#46728,0.0167571840017254);
#14490=CIRCLE('',#46729,0.0110511996794246);
#14491=CIRCLE('',#46730,0.0167907391086331);
#14492=CIRCLE('',#46731,0.0110190981843864);
#14493=CIRCLE('',#46732,0.00665874807867345);
#14494=CIRCLE('',#46738,0.0167157066786842);
#14495=CIRCLE('',#46739,0.0109625450142564);
#14496=CIRCLE('',#46741,0.016554145839149);
#14497=CIRCLE('',#46743,0.0165579433023043);
#14498=CIRCLE('',#46744,0.016554148987948);
#14499=CIRCLE('',#46745,0.0165579399145523);
#14500=CIRCLE('',#46746,0.0168110399836963);
#14501=CIRCLE('',#46747,0.0110459668052039);
#14502=CIRCLE('',#46748,0.0167928000132366);
#14503=CIRCLE('',#46749,0.011062455274358);
#14504=CIRCLE('',#46752,0.016605262351716);
#14505=CIRCLE('',#46754,0.0166048007004478);
#14506=CIRCLE('',#46755,0.0166052650989619);
#14507=CIRCLE('',#46756,0.0166047977419434);
#14508=CIRCLE('',#46757,0.0167731971563632);
#14509=CIRCLE('',#46758,0.011057324485821);
#14510=CIRCLE('',#46759,0.0168013216996036);
#14511=CIRCLE('',#46760,0.01103165307418);
#14512=CIRCLE('',#46761,0.01653102540833);
#14513=CIRCLE('',#46763,0.0165263163781144);
#14514=CIRCLE('',#46764,0.0165310283781746);
#14515=CIRCLE('',#46765,0.0165263134035609);
#14516=CIRCLE('',#46766,0.0166775856847597);
#14517=CIRCLE('',#46767,0.0109205691216858);
#14518=CIRCLE('',#46769,0.0164211197695146);
#14519=CIRCLE('',#46770,0.0164211166578231);
#14520=CIRCLE('',#46771,0.0167388248042642);
#14521=CIRCLE('',#46772,0.0109676124290397);
#14522=CIRCLE('',#46773,0.0166825658005341);
#14523=CIRCLE('',#46774,0.0110194472766462);
#14524=CIRCLE('',#46775,0.0165701549958441);
#14525=CIRCLE('',#46777,0.0165733005409841);
#14526=CIRCLE('',#46778,0.0165701578815627);
#14527=CIRCLE('',#46779,0.016573297179401);
#14528=CIRCLE('',#46780,0.0168141205746601);
#14529=CIRCLE('',#46781,0.0110535374113562);
#14530=CIRCLE('',#46782,0.0168028429611159);
#14531=CIRCLE('',#46783,0.0110635670203989);
#14532=CIRCLE('',#46784,0.0166019907645692);
#14533=CIRCLE('',#46786,0.0166008731501757);
#14534=CIRCLE('',#46787,0.0166019938578661);
#14535=CIRCLE('',#46788,0.0166008700795619);
#14536=CIRCLE('',#46789,0.0167571840018104);
#14537=CIRCLE('',#46790,0.0110511996752243);
#14538=CIRCLE('',#46791,0.0167907391089732);
#14539=CIRCLE('',#46792,0.0110190981849284);
#14540=CIRCLE('',#46793,0.00665874807864357);
#14541=CIRCLE('',#46799,0.016715706679058);
#14542=CIRCLE('',#46800,0.0109625450134028);
#14543=CIRCLE('',#46802,0.0165541457916914);
#14544=CIRCLE('',#46804,0.0165579430656142);
#14545=CIRCLE('',#46805,0.0165541488951878);
#14546=CIRCLE('',#46806,0.016557939800831);
#14547=CIRCLE('',#46807,0.0168110399835283);
#14548=CIRCLE('',#46808,0.0110459668053988);
#14549=CIRCLE('',#46809,0.0167928000128959);
#14550=CIRCLE('',#46810,0.0110624552746248);
#14551=CIRCLE('',#46813,0.0166052621808357);
#14552=CIRCLE('',#46815,0.0166048005591929);
#14553=CIRCLE('',#46816,0.0166052650439038);
#14554=CIRCLE('',#46817,0.0166047976643043);
#14555=CIRCLE('',#46818,0.0167731983501938);
#14556=CIRCLE('',#46819,0.011057328194232);
#14557=CIRCLE('',#46820,0.0168013216996613);
#14558=CIRCLE('',#46821,0.0110316530736681);
#14559=CIRCLE('',#46822,0.0165310254746411);
#14560=CIRCLE('',#46824,0.0165263162138977);
#14561=CIRCLE('',#46825,0.0165310283187957);
#14562=CIRCLE('',#46826,0.016526313348087);
#14563=CIRCLE('',#46827,0.0166775856844355);
#14564=CIRCLE('',#46828,0.0109205691220054);
#14565=CIRCLE('',#46830,0.0164211195586707);
#14566=CIRCLE('',#46831,0.0164211165641859);
#14567=CIRCLE('',#46832,0.0167388244016766);
#14568=CIRCLE('',#46833,0.0109676127118461);
#14569=CIRCLE('',#46834,0.0166825658004541);
#14570=CIRCLE('',#46835,0.0110194472760805);
#14571=CIRCLE('',#46836,0.0165701549651593);
#14572=CIRCLE('',#46838,0.0165733004050165);
#14573=CIRCLE('',#46839,0.0165701577605721);
#14574=CIRCLE('',#46840,0.0165732971634873);
#14575=CIRCLE('',#46841,0.0168141206270518);
#14576=CIRCLE('',#46842,0.0110535372968108);
#14577=CIRCLE('',#46843,0.016802842961495);
#14578=CIRCLE('',#46844,0.0110635670201626);
#14579=CIRCLE('',#46845,0.0166019908199673);
#14580=CIRCLE('',#46847,0.0166008730003544);
#14581=CIRCLE('',#46848,0.0166019937860896);
#14582=CIRCLE('',#46849,0.0166008699897132);
#14583=CIRCLE('',#46850,0.0167571840016942);
#14584=CIRCLE('',#46851,0.0110511996751948);
#14585=CIRCLE('',#46852,0.0167907391086622);
#14586=CIRCLE('',#46853,0.0110190981851049);
#14587=CIRCLE('',#46854,0.00665874807858149);
#14588=CIRCLE('',#46860,0.0167157066789418);
#14589=CIRCLE('',#46861,0.0109625450120428);
#14590=CIRCLE('',#46863,0.0165541458124077);
#14591=CIRCLE('',#46865,0.0165579429181672);
#14592=CIRCLE('',#46866,0.0165541488045164);
#14593=CIRCLE('',#46867,0.0165579397757552);
#14594=CIRCLE('',#46868,0.016811039983842);
#14595=CIRCLE('',#46869,0.0110459668054937);
#14596=CIRCLE('',#46870,0.0167928000132036);
#14597=CIRCLE('',#46871,0.0110624552742704);
#14598=CIRCLE('',#46874,0.016605262184445);
#14599=CIRCLE('',#46876,0.0166048003609683);
#14600=CIRCLE('',#46877,0.0166052649419975);
#14601=CIRCLE('',#46878,0.0166047976138641);
#14602=CIRCLE('',#46879,0.0167731971563786);
#14603=CIRCLE('',#46880,0.0110573244859619);
#14604=CIRCLE('',#46881,0.0168013216995128);
#14605=CIRCLE('',#46882,0.0110316530734511);
#14606=CIRCLE('',#46883,0.0165310254124807);
#14607=CIRCLE('',#46885,0.0165263161039668);
#14608=CIRCLE('',#46886,0.0165310282256654);
#14609=CIRCLE('',#46887,0.0165263132667817);
#14610=CIRCLE('',#46888,0.0166775856848087);
#14611=CIRCLE('',#46889,0.0109205691216089);
#14612=CIRCLE('',#46891,0.0164211194140629);
#14613=CIRCLE('',#46892,0.0164211164742805);
#14614=CIRCLE('',#46893,0.0167388235415256);
#14615=CIRCLE('',#46894,0.0109676133181102);
#14616=CIRCLE('',#46895,0.0166825658003835);
#14617=CIRCLE('',#46896,0.0110194472759929);
#14618=CIRCLE('',#46897,0.0165701550060228);
#14619=CIRCLE('',#46899,0.0165733002568834);
#14620=CIRCLE('',#46900,0.0165701577318853);
#14621=CIRCLE('',#46901,0.0165732970574261);
#14622=CIRCLE('',#46902,0.0168141206458311);
#14623=CIRCLE('',#46903,0.0110535372534871);
#14624=CIRCLE('',#46904,0.0168028429615044);
#14625=CIRCLE('',#46905,0.0110635670200074);
#14626=CIRCLE('',#46906,0.0166019907981289);
#14627=CIRCLE('',#46908,0.0166008728515721);
#14628=CIRCLE('',#46909,0.016601993743918);
#14629=CIRCLE('',#46910,0.01660086994767);
#14630=CIRCLE('',#46911,0.0167571840017539);
#14631=CIRCLE('',#46912,0.0110511996747717);
#14632=CIRCLE('',#46913,0.016790739109151);
#14633=CIRCLE('',#46914,0.011019098184771);
#14634=CIRCLE('',#46915,0.00665874807852504);
#14635=CIRCLE('',#46921,0.016715706679042);
#14636=CIRCLE('',#46922,0.0109625450121176);
#14637=CIRCLE('',#46924,0.0165541458179537);
#14638=CIRCLE('',#46926,0.0165579428661948);
#14639=CIRCLE('',#46927,0.0165541488386055);
#14640=CIRCLE('',#46928,0.0165579396627073);
#14641=CIRCLE('',#46929,0.0168110399837985);
#14642=CIRCLE('',#46930,0.0110459668053948);
#14643=CIRCLE('',#46931,0.016792800013335);
#14644=CIRCLE('',#46932,0.0110624552740833);
#14645=CIRCLE('',#46935,0.016605262299189);
#14646=CIRCLE('',#46937,0.016604800193468);
#14647=CIRCLE('',#46938,0.0166052648195743);
#14648=CIRCLE('',#46939,0.0166047975317367);
#14649=CIRCLE('',#46940,0.0167731971566556);
#14650=CIRCLE('',#46941,0.0110573244856772);
#14651=CIRCLE('',#46942,0.0168013216995712);
#14652=CIRCLE('',#46943,0.0110316530743037);
#14653=CIRCLE('',#46944,0.0165310254920278);
#14654=CIRCLE('',#46946,0.016526315910392);
#14655=CIRCLE('',#46947,0.016531028181923);
#14656=CIRCLE('',#46948,0.0165263132269298);
#14657=CIRCLE('',#46949,0.0166775856844546);
#14658=CIRCLE('',#46950,0.0109205691225738);
#14659=CIRCLE('',#46952,0.0164211193103871);
#14660=CIRCLE('',#46953,0.0164211163289822);
#14661=CIRCLE('',#46954,0.016738824804311);
#14662=CIRCLE('',#46955,0.0109676124277876);
#14663=CIRCLE('',#46956,0.0166825658006998);
#14664=CIRCLE('',#46957,0.0110194472765826);
#14665=CIRCLE('',#46958,0.0165701550441626);
#14666=CIRCLE('',#46960,0.016573300064543);
#14667=CIRCLE('',#46961,0.0165701576417903);
#14668=CIRCLE('',#46962,0.0165732970357012);
#14669=CIRCLE('',#46963,0.0168141206457594);
#14670=CIRCLE('',#46964,0.0110535372561457);
#14671=CIRCLE('',#46965,0.0168028429613552);
#14672=CIRCLE('',#46966,0.0110635670203864);
#14673=CIRCLE('',#46967,0.0166019907852403);
#14674=CIRCLE('',#46969,0.0166008726533189);
#14675=CIRCLE('',#46970,0.0166019936781065);
#14676=CIRCLE('',#46971,0.0166008698380475);
#14677=CIRCLE('',#46972,0.0167571840015755);
#14678=CIRCLE('',#46973,0.0110512000527843);
#14679=CIRCLE('',#46974,0.0167907391090083);
#14680=CIRCLE('',#46975,0.0110190981853154);
#14681=CIRCLE('',#46976,0.00665874948998041);
#14682=CIRCLE('',#46982,0.0167157066789768);
#14683=CIRCLE('',#46983,0.0109625450124528);
#14684=CIRCLE('',#46985,0.0165541458153592);
#14685=CIRCLE('',#46987,0.0165579426819535);
#14686=CIRCLE('',#46988,0.0165541486417264);
#14687=CIRCLE('',#46989,0.0165579395870733);
#14688=CIRCLE('',#46990,0.0168110399838875);
#14689=CIRCLE('',#46991,0.0110459668057296);
#14690=CIRCLE('',#46992,0.0167928000131379);
#14691=CIRCLE('',#46993,0.0110624552743193);
#14692=CIRCLE('',#46996,0.016605262379085);
#14693=CIRCLE('',#46998,0.0166048001267036);
#14694=CIRCLE('',#46999,0.0166052648636375);
#14695=CIRCLE('',#47000,0.0166047974056641);
#14696=CIRCLE('',#47001,0.0167731941322786);
#14697=CIRCLE('',#47002,0.011057315084616);
#14698=CIRCLE('',#47003,0.0168013216997332);
#14699=CIRCLE('',#47004,0.0110316530734077);
#14700=CIRCLE('',#47005,0.0165310255275055);
#14701=CIRCLE('',#47007,0.0165263158442697);
#14702=CIRCLE('',#47008,0.0165310280287164);
#14703=CIRCLE('',#47009,0.0165263130706467);
#14704=CIRCLE('',#47010,0.0166775856847185);
#14705=CIRCLE('',#47011,0.0109205691218712);
#14706=CIRCLE('',#47013,0.0164211191001963);
#14707=CIRCLE('',#47014,0.0164211163212165);
#14708=CIRCLE('',#47015,0.0167388235414893);
#14709=CIRCLE('',#47016,0.0109676133206887);
#14710=CIRCLE('',#47017,0.0166825658000383);
#14711=CIRCLE('',#47018,0.0110194472761275);
#14712=CIRCLE('',#47019,0.0165701550641018);
#14713=CIRCLE('',#47021,0.016573299955908);
#14714=CIRCLE('',#47022,0.0165701575707523);
#14715=CIRCLE('',#47023,0.0165732969049596);
#14716=CIRCLE('',#47024,0.0168141206460598);
#14717=CIRCLE('',#47025,0.0110535372557423);
#14718=CIRCLE('',#47026,0.0168028429616789);
#14719=CIRCLE('',#47027,0.0110635670200694);
#14720=CIRCLE('',#47028,0.0166019907372786);
#14721=CIRCLE('',#47030,0.0166008724580541);
#14722=CIRCLE('',#47031,0.0166019935357958);
#14723=CIRCLE('',#47032,0.0166008697383443);
#14724=CIRCLE('',#47033,0.0167571840016023);
#14725=CIRCLE('',#47034,0.0110512000530287);
#14726=CIRCLE('',#47035,0.0167907391088295);
#14727=CIRCLE('',#47036,0.0110190981855165);
#14728=CIRCLE('',#47037,0.00665874948993921);
#14729=CIRCLE('',#47043,0.0167157066789882);
#14730=CIRCLE('',#47044,0.0109625450150047);
#14731=CIRCLE('',#47046,0.0165541458574325);
#14732=CIRCLE('',#47048,0.016557942526337);
#14733=CIRCLE('',#47049,0.0165541486090743);
#14734=CIRCLE('',#47050,0.0165579394753156);
#14735=CIRCLE('',#47051,0.0168110399838102);
#14736=CIRCLE('',#47052,0.0110459668051484);
#14737=CIRCLE('',#47053,0.0167928000130372);
#14738=CIRCLE('',#47054,0.0110624552742874);
#14739=CIRCLE('',#47057,0.0166052623608482);
#14740=CIRCLE('',#47059,0.0166047998884685);
#14741=CIRCLE('',#47060,0.0166052647263381);
#14742=CIRCLE('',#47061,0.0166047973426093);
#14743=CIRCLE('',#47062,0.0167731971565137);
#14744=CIRCLE('',#47063,0.011057324485952);
#14745=CIRCLE('',#47064,0.0168013216994156);
#14746=CIRCLE('',#47065,0.011031653073398);
#14747=CIRCLE('',#47066,0.0165310255032138);
#14748=CIRCLE('',#47068,0.0165263157542874);
#14749=CIRCLE('',#47069,0.016531027963222);
#14750=CIRCLE('',#47070,0.0165263130548289);
#14751=CIRCLE('',#47071,0.0166775856847766);
#14752=CIRCLE('',#47072,0.0109205691221087);
#14753=CIRCLE('',#47074,0.0164211189896864);
#14754=CIRCLE('',#47075,0.0164211161722232);
#14755=CIRCLE('',#47076,0.0167388248043622);
#14756=CIRCLE('',#47077,0.0109676124277629);
#14757=CIRCLE('',#47078,0.0166825658002222);
#14758=CIRCLE('',#47079,0.0110194472759779);
#14759=CIRCLE('',#47080,0.0165701550303073);
#14760=CIRCLE('',#47082,0.0165732997875192);
#14761=CIRCLE('',#47083,0.0165701574824665);
#14762=CIRCLE('',#47084,0.0165732968390795);
#14763=CIRCLE('',#47085,0.0168141206456921);
#14764=CIRCLE('',#47086,0.011053537253665);
#14765=CIRCLE('',#47087,0.0168028429613703);
#14766=CIRCLE('',#47088,0.0110635670200615);
#14767=CIRCLE('',#47089,0.0166019907613543);
#14768=CIRCLE('',#47091,0.0166008723040521);
#14769=CIRCLE('',#47092,0.0166019935105866);
#14770=CIRCLE('',#47093,0.0166008696361459);
#14771=CIRCLE('',#47094,0.016757184001689);
#14772=CIRCLE('',#47095,0.011051199674271);
#14773=CIRCLE('',#47096,0.0167907391089668);
#14774=CIRCLE('',#47097,0.0110190981851912);
#14775=CIRCLE('',#47098,0.00665874807851366);
#14776=CIRCLE('',#47104,0.0167157066787324);
#14777=CIRCLE('',#47105,0.0109625450149831);
#14778=CIRCLE('',#47107,0.0165541458174054);
#14779=CIRCLE('',#47109,0.0165579423489387);
#14780=CIRCLE('',#47110,0.0165541485712035);
#14781=CIRCLE('',#47111,0.0165579393901184);
#14782=CIRCLE('',#47112,0.0168110399833972);
#14783=CIRCLE('',#47113,0.0110459668042894);
#14784=CIRCLE('',#47114,0.0167928000130159);
#14785=CIRCLE('',#47115,0.0110624552742632);
#14786=CIRCLE('',#47118,0.0166052622705376);
#14787=CIRCLE('',#47120,0.0166047997474789);
#14788=CIRCLE('',#47121,0.0166052646439818);
#14789=CIRCLE('',#47122,0.0166047971632048);
#14790=CIRCLE('',#47123,0.0167731971566282);
#14791=CIRCLE('',#47124,0.0110573244865126);
#14792=CIRCLE('',#47125,0.0168013216993064);
#14793=CIRCLE('',#47126,0.0110316530755126);
#14794=CIRCLE('',#47127,0.0165310255575995);
#14795=CIRCLE('',#47129,0.0165263155511315);
#14796=CIRCLE('',#47130,0.0165310280119525);
#14797=CIRCLE('',#47131,0.0165263129783182);
#14798=CIRCLE('',#47132,0.0166775856846212);
#14799=CIRCLE('',#47133,0.0109205691222008);
#14800=CIRCLE('',#47135,0.0164211188655515);
#14801=CIRCLE('',#47136,0.0164211160635202);
#14802=CIRCLE('',#47137,0.0167388248043554);
#14803=CIRCLE('',#47138,0.0109676124277361);
#14804=CIRCLE('',#47139,0.0166825658003021);
#14805=CIRCLE('',#47140,0.011019447276877);
#14806=CIRCLE('',#47141,0.0165701549917329);
#14807=CIRCLE('',#47143,0.0165732995310219);
#14808=CIRCLE('',#47144,0.0165701573426138);
#14809=CIRCLE('',#47145,0.0165732967230516);
#14810=CIRCLE('',#47146,0.0168141206453851);
#14811=CIRCLE('',#47147,0.011053537253855);
#14812=CIRCLE('',#47148,0.0168028429613918);
#14813=CIRCLE('',#47149,0.0110635670201788);
#14814=CIRCLE('',#47150,0.016601990699506);
#14815=CIRCLE('',#47152,0.0166008721089114);
#14816=CIRCLE('',#47153,0.0166019934077686);
#14817=CIRCLE('',#47154,0.0166008695465524);
#14818=CIRCLE('',#47155,0.0167571840016732);
#14819=CIRCLE('',#47156,0.011051199674904);
#14820=CIRCLE('',#47157,0.0167907391085881);
#14821=CIRCLE('',#47158,0.0110190981861391);
#14822=CIRCLE('',#47159,0.00665874807863435);
#14823=CIRCLE('',#47165,0.0167157066789665);
#14824=CIRCLE('',#47166,0.0109625450168683);
#14825=CIRCLE('',#47168,0.0165541458960314);
#14826=CIRCLE('',#47170,0.0165579424243726);
#14827=CIRCLE('',#47171,0.0165541486047321);
#14828=CIRCLE('',#47172,0.0165579395243273);
#14829=CIRCLE('',#47173,0.0168110399840367);
#14830=CIRCLE('',#47174,0.0110459668047921);
#14831=CIRCLE('',#47175,0.0167928000131094);
#14832=CIRCLE('',#47176,0.0110624552733874);
#14833=CIRCLE('',#47179,0.0166052624151451);
#14834=CIRCLE('',#47181,0.0166047997039492);
#14835=CIRCLE('',#47182,0.0166052646301021);
#14836=CIRCLE('',#47183,0.0166047971334831);
#14837=CIRCLE('',#47184,0.0167731971565164);
#14838=CIRCLE('',#47185,0.0110573244858054);
#14839=CIRCLE('',#47186,0.0168013216993822);
#14840=CIRCLE('',#47187,0.0110316530729965);
#14841=CIRCLE('',#47188,0.01653102537938);
#14842=CIRCLE('',#47190,0.0165263154516607);
#14843=CIRCLE('',#47191,0.0165310277099439);
#14844=CIRCLE('',#47192,0.0165263127670499);
#14845=CIRCLE('',#47193,0.016677585684748);
#14846=CIRCLE('',#47194,0.0109205691220697);
#14847=CIRCLE('',#47196,0.01642111861694);
#14848=CIRCLE('',#47197,0.0164211160383969);
#14849=CIRCLE('',#47198,0.0167388248040173);
#14850=CIRCLE('',#47199,0.0109676124293361);
#14851=CIRCLE('',#47200,0.0166825658006657);
#14852=CIRCLE('',#47201,0.0110194472766751);
#14853=CIRCLE('',#47202,0.016570155060932);
#14854=CIRCLE('',#47204,0.0165732995806975);
#14855=CIRCLE('',#47205,0.0165701573868749);
#14856=CIRCLE('',#47206,0.0165732966694879);
#14857=CIRCLE('',#47207,0.0168141206458845);
#14858=CIRCLE('',#47208,0.0110535372544796);
#14859=CIRCLE('',#47209,0.0168028429614423);
#14860=CIRCLE('',#47210,0.0110635670200312);
#14861=CIRCLE('',#47211,0.0166019907852894);
#14862=CIRCLE('',#47213,0.0166008721177798);
#14863=CIRCLE('',#47214,0.016601993410395);
#14864=CIRCLE('',#47215,0.0166008694719737);
#14865=CIRCLE('',#47216,0.0167571840017142);
#14866=CIRCLE('',#47217,0.0110511996802703);
#14867=CIRCLE('',#47218,0.0167907391087389);
#14868=CIRCLE('',#47219,0.0110190981851166);
#14869=CIRCLE('',#47220,0.00665874808274784);
#14870=CIRCLE('',#47226,0.016715706679209);
#14871=CIRCLE('',#47227,0.0109625450128583);
#14872=CIRCLE('',#47229,0.0165541458902804);
#14873=CIRCLE('',#47231,0.0165579419073244);
#14874=CIRCLE('',#47232,0.0165541485288617);
#14875=CIRCLE('',#47233,0.0165579392048);
#14876=CIRCLE('',#47234,0.0168110399835751);
#14877=CIRCLE('',#47235,0.0110459668060784);
#14878=CIRCLE('',#47236,0.016792800012697);
#14879=CIRCLE('',#47237,0.0110624552745184);
#14880=CIRCLE('',#47240,0.0166052624316687);
#14881=CIRCLE('',#47242,0.0166047995343761);
#14882=CIRCLE('',#47243,0.0166052644243831);
#14883=CIRCLE('',#47244,0.0166047970554349);
#14884=CIRCLE('',#47245,0.0167731971566083);
#14885=CIRCLE('',#47246,0.0110573244837942);
#14886=CIRCLE('',#47247,0.0168013216994279);
#14887=CIRCLE('',#47248,0.0110316530744061);
#14888=CIRCLE('',#47249,0.0165310256090931);
#14889=CIRCLE('',#47251,0.0165263151740798);
#14890=CIRCLE('',#47252,0.0165310277948519);
#14891=CIRCLE('',#47253,0.0165263129250178);
#14892=CIRCLE('',#47254,0.0166775856848588);
#14893=CIRCLE('',#47255,0.0109205691212204);
#14894=CIRCLE('',#47257,0.0164211185950565);
#14895=CIRCLE('',#47258,0.0164211159847808);
#14896=CIRCLE('',#47259,0.0167388248045614);
#14897=CIRCLE('',#47260,0.0109676124270857);
#14898=CIRCLE('',#47261,0.0166825658002627);
#14899=CIRCLE('',#47262,0.0110194472759807);
#14900=CIRCLE('',#47263,0.016570155040469);
#14901=CIRCLE('',#47265,0.0165732993554859);
#14902=CIRCLE('',#47266,0.0165701572968777);
#14903=CIRCLE('',#47267,0.0165732965929683);
#14904=CIRCLE('',#47268,0.0168141206459158);
#14905=CIRCLE('',#47269,0.0110535372569532);
#14906=CIRCLE('',#47270,0.016802842961278);
#14907=CIRCLE('',#47271,0.011063567019422);
#14908=CIRCLE('',#47272,0.0166019907597247);
#14909=CIRCLE('',#47274,0.01660087193563);
#14910=CIRCLE('',#47275,0.0166019931914076);
#14911=CIRCLE('',#47276,0.0166008694194318);
#14912=CIRCLE('',#47277,0.0167571840016429);
#14913=CIRCLE('',#47278,0.0110511996751358);
#14914=CIRCLE('',#47279,0.0167907391090019);
#14915=CIRCLE('',#47280,0.0110190981850566);
#14916=CIRCLE('',#47281,0.00665874808271733);
#14917=CIRCLE('',#47287,0.0167157066786898);
#14918=CIRCLE('',#47288,0.0109625450140703);
#14919=CIRCLE('',#47290,0.0165541457088435);
#14920=CIRCLE('',#47292,0.0165579419209612);
#14921=CIRCLE('',#47293,0.0165541485096187);
#14922=CIRCLE('',#47294,0.0165579394649361);
#14923=CIRCLE('',#47295,0.0168110399840163);
#14924=CIRCLE('',#47296,0.0110459668046887);
#14925=CIRCLE('',#47297,0.0167928000131629);
#14926=CIRCLE('',#47298,0.0110624552738361);
#14927=CIRCLE('',#47301,0.0166052623317775);
#14928=CIRCLE('',#47303,0.0166047993749498);
#14929=CIRCLE('',#47304,0.0166052644755989);
#14930=CIRCLE('',#47305,0.0166047969454479);
#14931=CIRCLE('',#47306,0.0167731941325696);
#14932=CIRCLE('',#47307,0.0110573150844451);
#14933=CIRCLE('',#47308,0.0168013216993458);
#14934=CIRCLE('',#47309,0.011031653074156);
#14935=CIRCLE('',#47310,0.0165310256288537);
#14936=CIRCLE('',#47312,0.0165263150151698);
#14937=CIRCLE('',#47313,0.0165310275145087);
#14938=CIRCLE('',#47314,0.016526312778801);
#14939=CIRCLE('',#47315,0.0166775856842448);
#14940=CIRCLE('',#47316,0.0109205691234822);
#14941=CIRCLE('',#47318,0.0164211183560543);
#14942=CIRCLE('',#47319,0.0164211160009157);
#14943=CIRCLE('',#47320,0.0167388235414568);
#14944=CIRCLE('',#47321,0.0109676133201212);
#14945=CIRCLE('',#47322,0.016682565800537);
#14946=CIRCLE('',#47323,0.0110194472762134);
#14947=CIRCLE('',#47324,0.0165701548825087);
#14948=CIRCLE('',#47326,0.0165732991360922);
#14949=CIRCLE('',#47327,0.0165701570900863);
#14950=CIRCLE('',#47328,0.0165732967225825);
#14951=CIRCLE('',#47329,0.016814120645603);
#14952=CIRCLE('',#47330,0.01105353725617);
#14953=CIRCLE('',#47331,0.0168028429620497);
#14954=CIRCLE('',#47332,0.0110635670191861);
#14955=CIRCLE('',#47333,0.0166019907656715);
#14956=CIRCLE('',#47335,0.0166008718074278);
#14957=CIRCLE('',#47336,0.0166019931546632);
#14958=CIRCLE('',#47337,0.0166008693989611);
#14959=CIRCLE('',#47338,0.016757184001536);
#14960=CIRCLE('',#47339,0.011051199674654);
#14961=CIRCLE('',#47340,0.0167907391090067);
#14962=CIRCLE('',#47341,0.0110190981853047);
#14963=CIRCLE('',#47342,0.00665874807851997);
#14964=CIRCLE('',#47348,0.016715706679377);
#14965=CIRCLE('',#47349,0.0109625450099256);
#14966=CIRCLE('',#47351,0.0165541456677397);
#14967=CIRCLE('',#47353,0.0165579417570842);
#14968=CIRCLE('',#47354,0.0165541482253256);
#14969=CIRCLE('',#47355,0.0165579391842505);
#14970=CIRCLE('',#47356,0.0168110399838653);
#14971=CIRCLE('',#47357,0.011045966806135);
#14972=CIRCLE('',#47358,0.0167928000128381);
#14973=CIRCLE('',#47359,0.0110624552737996);
#14974=CIRCLE('',#47362,0.0166052622330066);
#14975=CIRCLE('',#47364,0.0166047990110056);
#14976=CIRCLE('',#47365,0.016605264397152);
#14977=CIRCLE('',#47366,0.0166047967671889);
#14978=CIRCLE('',#47367,0.0167731971567163);
#14979=CIRCLE('',#47368,0.0110573244864769);
#14980=CIRCLE('',#47369,0.0168013216997017);
#14981=CIRCLE('',#47370,0.0110316530730052);
#14982=CIRCLE('',#47371,0.0165310253924406);
#14983=CIRCLE('',#47373,0.0165263148442778);
#14984=CIRCLE('',#47374,0.0165310274387597);
#14985=CIRCLE('',#47375,0.0165263127470437);
#14986=CIRCLE('',#47376,0.016677585684615);
#14987=CIRCLE('',#47377,0.0109205691231124);
#14988=CIRCLE('',#47379,0.0164211182503939);
#14989=CIRCLE('',#47380,0.01642111586262);
#14990=CIRCLE('',#47381,0.0167388235416579);
#14991=CIRCLE('',#47382,0.0109676133205617);
#14992=CIRCLE('',#47383,0.0166825658001667);
#14993=CIRCLE('',#47384,0.0110194472749627);
#14994=CIRCLE('',#47385,0.016570155031964);
#14995=CIRCLE('',#47387,0.0165732988903193);
#14996=CIRCLE('',#47388,0.0165701570326878);
#14997=CIRCLE('',#47389,0.0165732964484296);
#14998=CIRCLE('',#47390,0.0168141206453718);
#14999=CIRCLE('',#47391,0.0110535372569656);
#15000=CIRCLE('',#47392,0.0168028429610742);
#15001=CIRCLE('',#47393,0.0110635670206168);
#15002=CIRCLE('',#47394,0.0166019908598596);
#15003=CIRCLE('',#47396,0.0166008716102798);
#15004=CIRCLE('',#47397,0.0166019931695136);
#15005=CIRCLE('',#47398,0.0166008692496937);
#15006=CIRCLE('',#47399,0.0167571840016719);
#15007=CIRCLE('',#47400,0.011051199674668);
#15008=CIRCLE('',#47401,0.0167907391088039);
#15009=CIRCLE('',#47402,0.0110190981857932);
#15010=CIRCLE('',#47403,0.00665874807867338);
#15011=CIRCLE('',#47409,0.0167157066790264);
#15012=CIRCLE('',#47410,0.0109625450122563);
#15013=CIRCLE('',#47412,0.0165541459279617);
#15014=CIRCLE('',#47414,0.0165579415750164);
#15015=CIRCLE('',#47415,0.0165541483771701);
#15016=CIRCLE('',#47416,0.0165579391484975);
#15017=CIRCLE('',#47417,0.0168110399833571);
#15018=CIRCLE('',#47418,0.0110459668047138);
#15019=CIRCLE('',#47419,0.0167928000136081);
#15020=CIRCLE('',#47420,0.0110624552749001);
#15021=CIRCLE('',#47423,0.0166052623945908);
#15022=CIRCLE('',#47425,0.0166047990219055);
#15023=CIRCLE('',#47426,0.0166052642669552);
#15024=CIRCLE('',#47427,0.0166047967670206);
#15025=CIRCLE('',#47428,0.0167731941320866);
#15026=CIRCLE('',#47429,0.0110573150842326);
#15027=CIRCLE('',#47430,0.0168013216996376);
#15028=CIRCLE('',#47431,0.0110316530743853);
#15029=CIRCLE('',#47432,0.0165310255787377);
#15030=CIRCLE('',#47434,0.0165263146387248);
#15031=CIRCLE('',#47435,0.0165310275016277);
#15032=CIRCLE('',#47436,0.0165263127901589);
#15033=CIRCLE('',#47437,0.0166775856845433);
#15034=CIRCLE('',#47438,0.0109205691215517);
#15035=CIRCLE('',#47440,0.0164211177556893);
#15036=CIRCLE('',#47441,0.0164211158516326);
#15037=CIRCLE('',#47442,0.0167388235420917);
#15038=CIRCLE('',#47443,0.0109676133174696);
#15039=CIRCLE('',#47444,0.0166825658003095);
#15040=CIRCLE('',#47445,0.0110194472756285);
#15041=CIRCLE('',#47446,0.0165701551070582);
#15042=CIRCLE('',#47448,0.0165732988655155);
#15043=CIRCLE('',#47449,0.0165701569487744);
#15044=CIRCLE('',#47450,0.0165732963152157);
#15045=CIRCLE('',#47451,0.016814120627371);
#15046=CIRCLE('',#47452,0.011053537295479);
#15047=CIRCLE('',#47453,0.0168028429613983);
#15048=CIRCLE('',#47454,0.0110635670202091);
#15049=CIRCLE('',#47455,0.0166019907132379);
#15050=CIRCLE('',#47457,0.0166008713632373);
#15051=CIRCLE('',#47458,0.0166019930618939);
#15052=CIRCLE('',#47459,0.0166008693209907);
#15053=CIRCLE('',#47460,0.0167571840018115);
#15054=CIRCLE('',#47461,0.0110511996753908);
#15055=CIRCLE('',#47462,0.0167907391084152);
#15056=CIRCLE('',#47463,0.0110190981848113);
#15057=CIRCLE('',#47464,0.00665874807856962);
#15058=CIRCLE('',#47470,0.0167157066795252);
#15059=CIRCLE('',#47471,0.0109625450105399);
#15060=CIRCLE('',#47473,0.0165541458488985);
#15061=CIRCLE('',#47475,0.0165579414961178);
#15062=CIRCLE('',#47476,0.016554148203893);
#15063=CIRCLE('',#47477,0.0165579390888471);
#15064=CIRCLE('',#47478,0.016811039983394);
#15065=CIRCLE('',#47479,0.0110459668054207);
#15066=CIRCLE('',#47480,0.0167928000126915);
#15067=CIRCLE('',#47481,0.0110624552731583);
#15068=CIRCLE('',#47484,0.0166052623744163);
#15069=CIRCLE('',#47486,0.0166047989081871);
#15070=CIRCLE('',#47487,0.0166052641204778);
#15071=CIRCLE('',#47488,0.0166047967765761);
#15072=CIRCLE('',#47489,0.0167731971564122);
#15073=CIRCLE('',#47490,0.0110573244848604);
#15074=CIRCLE('',#47491,0.0168013216996565);
#15075=CIRCLE('',#47492,0.0110316530728958);
#15076=CIRCLE('',#47493,0.016531025437288);
#15077=CIRCLE('',#47495,0.0165263146554168);
#15078=CIRCLE('',#47496,0.0165310275404691);
#15079=CIRCLE('',#47497,0.0165263124377282);
#15080=CIRCLE('',#47498,0.0166775856846072);
#15081=CIRCLE('',#47499,0.0109205691214054);
#15082=CIRCLE('',#47501,0.0164211179394138);
#15083=CIRCLE('',#47502,0.0164211156339015);
#15084=CIRCLE('',#47503,0.0167388248040325);
#15085=CIRCLE('',#47504,0.0109676124287069);
#15086=CIRCLE('',#47505,0.0166825658000452);
#15087=CIRCLE('',#47506,0.0110194472757815);
#15088=CIRCLE('',#47507,0.0165701549775579);
#15089=CIRCLE('',#47509,0.0165732987883178);
#15090=CIRCLE('',#47510,0.0165701570277774);
#15091=CIRCLE('',#47511,0.0165732961623271);
#15092=CIRCLE('',#47512,0.016814120626826);
#15093=CIRCLE('',#47513,0.0110535372950808);
#15094=CIRCLE('',#47514,0.0168028429613692);
#15095=CIRCLE('',#47515,0.0110635670209873);
#15096=CIRCLE('',#47516,0.0166019907930465);
#15097=CIRCLE('',#47518,0.0166008712589892);
#15098=CIRCLE('',#47519,0.0166019928145345);
#15099=CIRCLE('',#47520,0.0166008692132377);
#15100=CIRCLE('',#47521,0.0167571840016013);
#15101=CIRCLE('',#47522,0.0110511996738178);
#15102=CIRCLE('',#47523,0.01679073910861);
#15103=CIRCLE('',#47524,0.0110190981842078);
#15104=CIRCLE('',#47525,0.00665874807848039);
#15105=CIRCLE('',#47531,0.0167157066795619);
#15106=CIRCLE('',#47532,0.0109625450129655);
#15107=CIRCLE('',#47534,0.0165541457243246);
#15108=CIRCLE('',#47536,0.0165579412106767);
#15109=CIRCLE('',#47537,0.0165541482558227);
#15110=CIRCLE('',#47538,0.0165579386921517);
#15111=CIRCLE('',#47539,0.0168110399838667);
#15112=CIRCLE('',#47540,0.0110459668055425);
#15113=CIRCLE('',#47541,0.0167928000128198);
#15114=CIRCLE('',#47542,0.0110624552748793);
#15115=CIRCLE('',#47545,0.0166052622059834);
#15116=CIRCLE('',#47547,0.016604798651343);
#15117=CIRCLE('',#47548,0.0166052642067028);
#15118=CIRCLE('',#47549,0.0166047966805386);
#15119=CIRCLE('',#47550,0.0167731971562434);
#15120=CIRCLE('',#47551,0.0110573244854881);
#15121=CIRCLE('',#47552,0.0168013216999379);
#15122=CIRCLE('',#47553,0.0110316530754383);
#15123=CIRCLE('',#47554,0.0165310255164065);
#15124=CIRCLE('',#47556,0.0165263144958598);
#15125=CIRCLE('',#47557,0.0165310272807434);
#15126=CIRCLE('',#47558,0.0165263123171155);
#15127=CIRCLE('',#47559,0.0166775856848886);
#15128=CIRCLE('',#47560,0.0109205691224704);
#15129=CIRCLE('',#47562,0.0164211176536645);
#15130=CIRCLE('',#47563,0.0164211156591293);
#15131=CIRCLE('',#47564,0.0167388244022555);
#15132=CIRCLE('',#47565,0.0109676127120857);
#15133=CIRCLE('',#47566,0.0166825658003426);
#15134=CIRCLE('',#47567,0.0110194472767055);
#15135=CIRCLE('',#47568,0.0165701550072313);
#15136=CIRCLE('',#47570,0.0165732986276967);
#15137=CIRCLE('',#47571,0.0165701568562288);
#15138=CIRCLE('',#47572,0.0165732962912302);
#15139=CIRCLE('',#47573,0.0168141206268075);
#15140=CIRCLE('',#47574,0.0110535372934106);
#15141=CIRCLE('',#47575,0.0168028429615418);
#15142=CIRCLE('',#47576,0.0110635670205629);
#15143=CIRCLE('',#47577,0.0166019906012785);
#15144=CIRCLE('',#47579,0.0166008713097932);
#15145=CIRCLE('',#47580,0.0166019929578284);
#15146=CIRCLE('',#47581,0.0166008690696432);
#15147=CIRCLE('',#47582,0.016757781005222);
#15148=CIRCLE('',#47583,0.0110511996751157);
#15149=CIRCLE('',#47584,0.0167907391087404);
#15150=CIRCLE('',#47585,0.0110190981859409);
#15151=CIRCLE('',#47586,0.00665874807854453);
#15152=CIRCLE('',#47592,0.0167157066788644);
#15153=CIRCLE('',#47593,0.0109625450154754);
#15154=CIRCLE('',#47595,0.016554146073238);
#15155=CIRCLE('',#47597,0.0165579411825587);
#15156=CIRCLE('',#47598,0.0165541481365723);
#15157=CIRCLE('',#47599,0.0165579388524576);
#15158=CIRCLE('',#47600,0.0168110399839204);
#15159=CIRCLE('',#47601,0.0110459668037209);
#15160=CIRCLE('',#47602,0.0167928000128627);
#15161=CIRCLE('',#47603,0.0110624552745945);
#15162=CIRCLE('',#47606,0.0166052623891851);
#15163=CIRCLE('',#47608,0.0166047984747976);
#15164=CIRCLE('',#47609,0.0166052639005878);
#15165=CIRCLE('',#47610,0.0166047965284398);
#15166=CIRCLE('',#47611,0.0167731983504133);
#15167=CIRCLE('',#47612,0.0110573281940185);
#15168=CIRCLE('',#47613,0.0168013216993258);
#15169=CIRCLE('',#47614,0.0110316530733178);
#15170=CIRCLE('',#47615,0.0165310256300649);
#15171=CIRCLE('',#47617,0.0165263143157291);
#15172=CIRCLE('',#47618,0.0165310273691108);
#15173=CIRCLE('',#47619,0.0165263125268229);
#15174=CIRCLE('',#47620,0.0166775856847163);
#15175=CIRCLE('',#47621,0.0109205691211382);
#15176=CIRCLE('',#47623,0.0164211175690923);
#15177=CIRCLE('',#47624,0.0164211156634918);
#15178=CIRCLE('',#47625,0.016738824402298);
#15179=CIRCLE('',#47626,0.0109676127131101);
#15180=CIRCLE('',#47627,0.0166825658003235);
#15181=CIRCLE('',#47628,0.0110194472769563);
#15182=CIRCLE('',#47629,0.0165701551403399);
#15183=CIRCLE('',#47631,0.0165732983967805);
#15184=CIRCLE('',#47632,0.0165701565626166);
#15185=CIRCLE('',#47633,0.0165732960775949);
#15186=CIRCLE('',#47634,0.0168141206266248);
#15187=CIRCLE('',#47635,0.0110535372955402);
#15188=CIRCLE('',#47636,0.0168028429610133);
#15189=CIRCLE('',#47637,0.0110635670199097);
#15190=CIRCLE('',#47638,0.0166019906551576);
#15191=CIRCLE('',#47640,0.0166008708466768);
#15192=CIRCLE('',#47641,0.0166019927018465);
#15193=CIRCLE('',#47642,0.0166008689412734);
#15194=CIRCLE('',#47643,0.016757184001705);
#15195=CIRCLE('',#47644,0.0110511996761176);
#15196=CIRCLE('',#47645,0.016790739109215);
#15197=CIRCLE('',#47646,0.011019098184434);
#15198=CIRCLE('',#47647,0.0066587480828286);
#15199=CIRCLE('',#47653,0.0167157066790089);
#15200=CIRCLE('',#47654,0.0109625450117604);
#15201=CIRCLE('',#47656,0.0165541457909729);
#15202=CIRCLE('',#47658,0.016557940910524);
#15203=CIRCLE('',#47659,0.0165541480837066);
#15204=CIRCLE('',#47660,0.0165579387559605);
#15205=CIRCLE('',#47661,0.0168110399839677);
#15206=CIRCLE('',#47662,0.0110459668065405);
#15207=CIRCLE('',#47663,0.0167928000131899);
#15208=CIRCLE('',#47664,0.0110624552729814);
#15209=CIRCLE('',#47667,0.0166052623997871);
#15210=CIRCLE('',#47669,0.0166047984590974);
#15211=CIRCLE('',#47670,0.0166052638884078);
#15212=CIRCLE('',#47671,0.0166047966615301);
#15213=CIRCLE('',#47672,0.0167731971561139);
#15214=CIRCLE('',#47673,0.0110573244858449);
#15215=CIRCLE('',#47674,0.0168013216993788);
#15216=CIRCLE('',#47675,0.0110316530767841);
#15217=CIRCLE('',#47676,0.0165310255307904);
#15218=CIRCLE('',#47678,0.0165263141351347);
#15219=CIRCLE('',#47679,0.0165310269859533);
#15220=CIRCLE('',#47680,0.0165263124289528);
#15221=CIRCLE('',#47681,0.0166775856839762);
#15222=CIRCLE('',#47682,0.0109205691225622);
#15223=CIRCLE('',#47684,0.0164211174216821);
#15224=CIRCLE('',#47685,0.0164211152287567);
#15225=CIRCLE('',#47686,0.0167388248049001);
#15226=CIRCLE('',#47687,0.0109676124289856);
#15227=CIRCLE('',#47688,0.0166825658005866);
#15228=CIRCLE('',#47689,0.0110194472755798);
#15229=CIRCLE('',#47690,0.0165701552119444);
#15230=CIRCLE('',#47692,0.0165732982632728);
#15231=CIRCLE('',#47693,0.016570156637561);
#15232=CIRCLE('',#47694,0.0165732960426156);
#15233=CIRCLE('',#47695,0.0168141205742218);
#15234=CIRCLE('',#47696,0.011053537412211);
#15235=CIRCLE('',#47697,0.0168028429618933);
#15236=CIRCLE('',#47698,0.0110635670201166);
#15237=CIRCLE('',#47699,0.0166019906886142);
#15238=CIRCLE('',#47701,0.0166008709183064);
#15239=CIRCLE('',#47702,0.0166019926437347);
#15240=CIRCLE('',#47703,0.0166008689366435);
#15241=CIRCLE('',#47704,0.0167571840014403);
#15242=CIRCLE('',#47705,0.0110512000530764);
#15243=CIRCLE('',#47706,0.0167907391089602);
#15244=CIRCLE('',#47707,0.0110190981855417);
#15245=CIRCLE('',#47708,0.00665874948987581);
#15246=CIRCLE('',#47714,0.0167157066787763);
#15247=CIRCLE('',#47715,0.0109625450161231);
#15248=CIRCLE('',#47717,0.0165541458013739);
#15249=CIRCLE('',#47719,0.0165579408335849);
#15250=CIRCLE('',#47720,0.0165541479190511);
#15251=CIRCLE('',#47721,0.0165579387335229);
#15252=CIRCLE('',#47722,0.0168110399839455);
#15253=CIRCLE('',#47723,0.0110459668054762);
#15254=CIRCLE('',#47724,0.0167928000127178);
#15255=CIRCLE('',#47725,0.0110624552735594);
#15256=CIRCLE('',#47728,0.0166052624219195);
#15257=CIRCLE('',#47730,0.0166047982868483);
#15258=CIRCLE('',#47731,0.0166052639548341);
#15259=CIRCLE('',#47732,0.0166047965522661);
#15260=CIRCLE('',#47733,0.0167731971567446);
#15261=CIRCLE('',#47734,0.0110573244853783);
#15262=CIRCLE('',#47735,0.0168013216992766);
#15263=CIRCLE('',#47736,0.0110316530731178);
#15264=CIRCLE('',#47737,0.0165310254682502);
#15265=CIRCLE('',#47739,0.0165263139662139);
#15266=CIRCLE('',#47740,0.0165310273029044);
#15267=CIRCLE('',#47741,0.0165263122502954);
#15268=CIRCLE('',#47742,0.0166775856841097);
#15269=CIRCLE('',#47743,0.0109205691214897);
#15270=CIRCLE('',#47745,0.0164211170610155);
#15271=CIRCLE('',#47746,0.0164211153185495);
#15272=CIRCLE('',#47747,0.0167388248045554);
#15273=CIRCLE('',#47748,0.0109676124278452);
#15274=CIRCLE('',#47749,0.0166825658004723);
#15275=CIRCLE('',#47750,0.0110194472759086);
#15276=CIRCLE('',#47751,0.0165701549486484);
#15277=CIRCLE('',#47753,0.0165732980341184);
#15278=CIRCLE('',#47754,0.0165701566511404);
#15279=CIRCLE('',#47755,0.0165732959899662);
#15280=CIRCLE('',#47756,0.0168141206453934);
#15281=CIRCLE('',#47757,0.0110535372533032);
#15282=CIRCLE('',#47758,0.0168028429606526);
#15283=CIRCLE('',#47759,0.0110635670195936);
#15284=CIRCLE('',#47760,0.0166019908025361);
#15285=CIRCLE('',#47762,0.0166008705740594);
#15286=CIRCLE('',#47763,0.0166019925677242);
#15287=CIRCLE('',#47764,0.0166008688871382);
#15288=CIRCLE('',#47765,0.0167571840018058);
#15289=CIRCLE('',#47766,0.0110512000569864);
#15290=CIRCLE('',#47767,0.0167907391092407);
#15291=CIRCLE('',#47768,0.0110190981863241);
#15292=CIRCLE('',#47769,0.00665874948993972);
#15293=CIRCLE('',#47775,0.0167157066786719);
#15294=CIRCLE('',#47776,0.0109625450160374);
#15295=CIRCLE('',#47778,0.0165541458229972);
#15296=CIRCLE('',#47780,0.0165579405587508);
#15297=CIRCLE('',#47781,0.0165541479749883);
#15298=CIRCLE('',#47782,0.0165579385078735);
#15299=CIRCLE('',#47783,0.0168110399838372);
#15300=CIRCLE('',#47784,0.0110459668048916);
#15301=CIRCLE('',#47785,0.0167928000129713);
#15302=CIRCLE('',#47786,0.0110624552756187);
#15303=CIRCLE('',#47789,0.0166052622979043);
#15304=CIRCLE('',#47791,0.0166047980078517);
#15305=CIRCLE('',#47792,0.0166052637458812);
#15306=CIRCLE('',#47793,0.016604796546177);
#15307=CIRCLE('',#47794,0.0167731971562877);
#15308=CIRCLE('',#47795,0.0110573244849338);
#15309=CIRCLE('',#47796,0.0168013216991658);
#15310=CIRCLE('',#47797,0.011031653076038);
#15311=CIRCLE('',#47798,0.0165310254980791);
#15312=CIRCLE('',#47800,0.016526313867048);
#15313=CIRCLE('',#47801,0.0165310270047356);
#15314=CIRCLE('',#47802,0.0165263124988837);
#15315=CIRCLE('',#47803,0.0166775856851045);
#15316=CIRCLE('',#47804,0.01092056912089);
#15317=CIRCLE('',#47806,0.0164211169494706);
#15318=CIRCLE('',#47807,0.0164211152668151);
#15319=CIRCLE('',#47808,0.0167388248044777);
#15320=CIRCLE('',#47809,0.0109676124279146);
#15321=CIRCLE('',#47810,0.016682565800564);
#15322=CIRCLE('',#47811,0.0110194472766535);
#15323=CIRCLE('',#47812,0.0165701548917864);
#15324=CIRCLE('',#47814,0.0165732978045151);
#15325=CIRCLE('',#47815,0.0165701564472872);
#15326=CIRCLE('',#47816,0.0165732957486762);
#15327=CIRCLE('',#47817,0.0168141206453714);
#15328=CIRCLE('',#47818,0.0110535372567067);
#15329=CIRCLE('',#47819,0.0168028429617165);
#15330=CIRCLE('',#47820,0.0110635670195438);
#15331=CIRCLE('',#47821,0.0166019906461126);
#15332=CIRCLE('',#47823,0.0166008704437203);
#15333=CIRCLE('',#47824,0.0166019927691166);
#15334=CIRCLE('',#47825,0.016600868870716);
#15335=CIRCLE('',#47826,0.0167571840013951);
#15336=CIRCLE('',#47827,0.0110511996790365);
#15337=CIRCLE('',#47828,0.016790739108159);
#15338=CIRCLE('',#47829,0.0110190981859346);
#15339=CIRCLE('',#47830,0.00665874807865914);
#15340=CIRCLE('',#47836,0.0167157066790517);
#15341=CIRCLE('',#47837,0.0109625450109347);
#15342=CIRCLE('',#47839,0.0165541458621187);
#15343=CIRCLE('',#47841,0.0165579404282209);
#15344=CIRCLE('',#47842,0.0165541478979011);
#15345=CIRCLE('',#47843,0.016557938488688);
#15346=CIRCLE('',#47844,0.01681103998369);
#15347=CIRCLE('',#47845,0.0110459668054687);
#15348=CIRCLE('',#47846,0.0167928000124603);
#15349=CIRCLE('',#47847,0.0110624552742697);
#15350=CIRCLE('',#47850,0.0166052623411055);
#15351=CIRCLE('',#47852,0.0166047979258038);
#15352=CIRCLE('',#47853,0.0166052638195381);
#15353=CIRCLE('',#47854,0.016604796415447);
#15354=CIRCLE('',#47855,0.016773197156601);
#15355=CIRCLE('',#47856,0.0110573244864894);
#15356=CIRCLE('',#47857,0.0168013216997676);
#15357=CIRCLE('',#47858,0.0110316530752986);
#15358=CIRCLE('',#47859,0.0165310253501258);
#15359=CIRCLE('',#47861,0.0165263137831181);
#15360=CIRCLE('',#47862,0.0165310270138886);
#15361=CIRCLE('',#47863,0.0165263123403775);
#15362=CIRCLE('',#47864,0.0166775856843488);
#15363=CIRCLE('',#47865,0.0109205691222831);
#15364=CIRCLE('',#47867,0.0164211168538974);
#15365=CIRCLE('',#47868,0.0164211151504863);
#15366=CIRCLE('',#47869,0.0167388235417016);
#15367=CIRCLE('',#47870,0.0109676133178113);
#15368=CIRCLE('',#47871,0.0166825658009599);
#15369=CIRCLE('',#47872,0.0110194472770996);
#15370=CIRCLE('',#47873,0.0165701548115593);
#15371=CIRCLE('',#47875,0.01657329760585);
#15372=CIRCLE('',#47876,0.016570156674166);
#15373=CIRCLE('',#47877,0.0165732958903677);
#15374=CIRCLE('',#47878,0.0168141206461625);
#15375=CIRCLE('',#47879,0.0110535372541906);
#15376=CIRCLE('',#47880,0.0168028429615073);
#15377=CIRCLE('',#47881,0.0110635670195637);
#15378=CIRCLE('',#47882,0.0166019906026257);
#15379=CIRCLE('',#47884,0.0166008702318525);
#15380=CIRCLE('',#47885,0.0166019925762392);
#15381=CIRCLE('',#47886,0.0166008685776365);
#15382=CIRCLE('',#47887,0.0167571840015236);
#15383=CIRCLE('',#47888,0.0110511996751507);
#15384=CIRCLE('',#47889,0.0167907391088176);
#15385=CIRCLE('',#47890,0.0110190981854031);
#15386=CIRCLE('',#47891,0.00665874807872873);
#15387=CIRCLE('',#47897,0.0167157066787157);
#15388=CIRCLE('',#47898,0.0109625450142858);
#15389=CIRCLE('',#47900,0.0165541457909352);
#15390=CIRCLE('',#47902,0.0165579402781184);
#15391=CIRCLE('',#47903,0.0165541477545415);
#15392=CIRCLE('',#47904,0.016557938424068);
#15393=CIRCLE('',#47905,0.0168110399836047);
#15394=CIRCLE('',#47906,0.0110459668051156);
#15395=CIRCLE('',#47907,0.0167928000128988);
#15396=CIRCLE('',#47908,0.0110624552738703);
#15397=CIRCLE('',#47911,0.0166052624109867);
#15398=CIRCLE('',#47913,0.0166047977841876);
#15399=CIRCLE('',#47914,0.0166052636354893);
#15400=CIRCLE('',#47915,0.0166047962325927);
#15401=CIRCLE('',#47916,0.0167731971560594);
#15402=CIRCLE('',#47917,0.0110573244858153);
#15403=CIRCLE('',#47918,0.0168013216994829);
#15404=CIRCLE('',#47919,0.0110316530742135);
#15405=CIRCLE('',#47920,0.0165310254867642);
#15406=CIRCLE('',#47922,0.0165263134594726);
#15407=CIRCLE('',#47923,0.0165310267542607);
#15408=CIRCLE('',#47924,0.0165263119891698);
#15409=CIRCLE('',#47925,0.0166775856848237);
#15410=CIRCLE('',#47926,0.0109205691213332);
#15411=CIRCLE('',#47928,0.0164211167562658);
#15412=CIRCLE('',#47929,0.0164211150069546);
#15413=CIRCLE('',#47930,0.0167388248040529);
#15414=CIRCLE('',#47931,0.0109676124294812);
#15415=CIRCLE('',#47932,0.0166825658009133);
#15416=CIRCLE('',#47933,0.0110194472761536);
#15417=CIRCLE('',#47934,0.0165701548909676);
#15418=CIRCLE('',#47936,0.0165732976153206);
#15419=CIRCLE('',#47937,0.0165701563546957);
#15420=CIRCLE('',#47938,0.0165732959810528);
#15421=CIRCLE('',#47939,0.0168141206457686);
#15422=CIRCLE('',#47940,0.0110535372541688);
#15423=CIRCLE('',#47941,0.0168028429613712);
#15424=CIRCLE('',#47942,0.011063567020347);
#15425=CIRCLE('',#47943,0.0166019905963711);
#15426=CIRCLE('',#47945,0.0166008702286165);
#15427=CIRCLE('',#47946,0.016601992541578);
#15428=CIRCLE('',#47947,0.0166008686459998);
#15429=CIRCLE('',#47948,0.016757184001533);
#15430=CIRCLE('',#47949,0.0110511996795091);
#15431=CIRCLE('',#47950,0.016790739108611);
#15432=CIRCLE('',#47951,0.0110190981835215);
#15433=CIRCLE('',#47952,0.00665874807857607);
#15434=CIRCLE('',#47958,0.0167157066788821);
#15435=CIRCLE('',#47959,0.0109625450166771);
#15436=CIRCLE('',#47961,0.0165541458400344);
#15437=CIRCLE('',#47963,0.0165579399865424);
#15438=CIRCLE('',#47964,0.0165541474848087);
#15439=CIRCLE('',#47965,0.0165579382754252);
#15440=CIRCLE('',#47966,0.0168110399835032);
#15441=CIRCLE('',#47967,0.0110459668042796);
#15442=CIRCLE('',#47968,0.0167928000129298);
#15443=CIRCLE('',#47969,0.0110624552747411);
#15444=CIRCLE('',#47972,0.0166052624204165);
#15445=CIRCLE('',#47974,0.0166047975298572);
#15446=CIRCLE('',#47975,0.0166052635696027);
#15447=CIRCLE('',#47976,0.0166047961541093);
#15448=CIRCLE('',#47977,0.0167731941320965);
#15449=CIRCLE('',#47978,0.0110573150844861);
#15450=CIRCLE('',#47979,0.0168013216988545);
#15451=CIRCLE('',#47980,0.0110316530737055);
#15452=CIRCLE('',#47981,0.01653102561324);
#15453=CIRCLE('',#47983,0.0165263134535438);
#15454=CIRCLE('',#47984,0.0165310266894553);
#15455=CIRCLE('',#47985,0.0165263119606172);
#15456=CIRCLE('',#47986,0.016677585684666);
#15457=CIRCLE('',#47987,0.0109205691211641);
#15458=CIRCLE('',#47989,0.0164211164846049);
#15459=CIRCLE('',#47990,0.0164211149742223);
#15460=CIRCLE('',#47991,0.0167388248041252);
#15461=CIRCLE('',#47992,0.0109676124298911);
#15462=CIRCLE('',#47993,0.0166825658006233);
#15463=CIRCLE('',#47994,0.0110194472786196);
#15464=CIRCLE('',#47995,0.016570155027543);
#15465=CIRCLE('',#47997,0.0165732973038302);
#15466=CIRCLE('',#47998,0.0165701565528539);
#15467=CIRCLE('',#47999,0.0165732957936516);
#15468=CIRCLE('',#48000,0.0168141205743096);
#15469=CIRCLE('',#48001,0.0110535374095543);
#15470=CIRCLE('',#48002,0.0168028429616262);
#15471=CIRCLE('',#48003,0.0110635670192313);
#15472=CIRCLE('',#48004,0.0166019907953388);
#15473=CIRCLE('',#48006,0.0166008699165455);
#15474=CIRCLE('',#48007,0.0166019924266547);
#15475=CIRCLE('',#48008,0.0166008685549454);
#15476=CIRCLE('',#48009,0.0167571840015528);
#15477=CIRCLE('',#48010,0.0110511996804726);
#15478=CIRCLE('',#48011,0.0167907391088268);
#15479=CIRCLE('',#48012,0.0110190981846686);
#15480=CIRCLE('',#48013,0.00665874807857608);
#15481=CIRCLE('',#48019,0.0167157066791692);
#15482=CIRCLE('',#48020,0.0109625450124005);
#15483=CIRCLE('',#48022,0.0165541458563792);
#15484=CIRCLE('',#48024,0.0165579398708296);
#15485=CIRCLE('',#48025,0.016554147259951);
#15486=CIRCLE('',#48026,0.0165579381717781);
#15487=CIRCLE('',#48027,0.0168110399835602);
#15488=CIRCLE('',#48028,0.0110459668058413);
#15489=CIRCLE('',#48029,0.0167928000130561);
#15490=CIRCLE('',#48030,0.0110624552745106);
#15491=CIRCLE('',#48033,0.0166052621606994);
#15492=CIRCLE('',#48035,0.0166047975523418);
#15493=CIRCLE('',#48036,0.0166052634410576);
#15494=CIRCLE('',#48037,0.0166047961237714);
#15495=CIRCLE('',#48038,0.0167731971564195);
#15496=CIRCLE('',#48039,0.0110573244853963);
#15497=CIRCLE('',#48040,0.0168013216996777);
#15498=CIRCLE('',#48041,0.0110316530737103);
#15499=CIRCLE('',#48042,0.0165310255839058);
#15500=CIRCLE('',#48044,0.0165263131899507);
#15501=CIRCLE('',#48045,0.0165310267138344);
#15502=CIRCLE('',#48046,0.0165263117828695);
#15503=CIRCLE('',#48047,0.0166775856839844);
#15504=CIRCLE('',#48048,0.010920569122766);
#15505=CIRCLE('',#48050,0.0164211163471286);
#15506=CIRCLE('',#48051,0.0164211148702252);
#15507=CIRCLE('',#48052,0.0167388248043213);
#15508=CIRCLE('',#48053,0.010967612427291);
#15509=CIRCLE('',#48054,0.0166825658003235);
#15510=CIRCLE('',#48055,0.0110194472750709);
#15511=CIRCLE('',#48056,0.0165701549840473);
#15512=CIRCLE('',#48058,0.0165732971979771);
#15513=CIRCLE('',#48059,0.0165701563441456);
#15514=CIRCLE('',#48060,0.016573295686663);
#15515=CIRCLE('',#48061,0.0168141206459555);
#15516=CIRCLE('',#48062,0.01105353725616);
#15517=CIRCLE('',#48063,0.0168028429614426);
#15518=CIRCLE('',#48064,0.0110635670200517);
#15519=CIRCLE('',#48065,0.0166019908585466);
#15520=CIRCLE('',#48067,0.0166008697863184);
#15521=CIRCLE('',#48068,0.0166019923320812);
#15522=CIRCLE('',#48069,0.0166008684816235);
#15523=CIRCLE('',#48070,0.0167571840014785);
#15524=CIRCLE('',#48071,0.0110511996761483);
#15525=CIRCLE('',#48072,0.0167907391088928);
#15526=CIRCLE('',#48073,0.0110190981840285);
#15527=CIRCLE('',#48074,0.00665874807855417);
#15528=CIRCLE('',#48080,0.0167157066790624);
#15529=CIRCLE('',#48081,0.0109625450150895);
#15530=CIRCLE('',#48083,0.0165541458221566);
#15531=CIRCLE('',#48085,0.0165579397651312);
#15532=CIRCLE('',#48086,0.0165541473401467);
#15533=CIRCLE('',#48087,0.0165579381811266);
#15534=CIRCLE('',#48088,0.016811039983551);
#15535=CIRCLE('',#48089,0.0110459668053132);
#15536=CIRCLE('',#48090,0.0167928000130745);
#15537=CIRCLE('',#48091,0.0110624552748131);
#15538=CIRCLE('',#48094,0.016605262299557);
#15539=CIRCLE('',#48096,0.0166047972767696);
#15540=CIRCLE('',#48097,0.016605263291903);
#15541=CIRCLE('',#48098,0.01660479606158);
#15542=CIRCLE('',#48099,0.0167731971567289);
#15543=CIRCLE('',#48100,0.0110573244852766);
#15544=CIRCLE('',#48101,0.0168013216995077);
#15545=CIRCLE('',#48102,0.0110316530736745);
#15546=CIRCLE('',#48103,0.0165310253844543);
#15547=CIRCLE('',#48105,0.0165263132517026);
#15548=CIRCLE('',#48106,0.0165310266599294);
#15549=CIRCLE('',#48107,0.01652631182441);
#15550=CIRCLE('',#48108,0.0166775856846773);
#15551=CIRCLE('',#48109,0.0109205691231875);
#15552=CIRCLE('',#48111,0.0164211161921942);
#15553=CIRCLE('',#48112,0.0164211148656089);
#15554=CIRCLE('',#48113,0.0167388248043935);
#15555=CIRCLE('',#48114,0.0109676124288808);
#15556=CIRCLE('',#48115,0.016682565800743);
#15557=CIRCLE('',#48116,0.0110194472768691);
#15558=CIRCLE('',#48117,0.0165701549825662);
#15559=CIRCLE('',#48119,0.0165732970168302);
#15560=CIRCLE('',#48120,0.016570156277062);
#15561=CIRCLE('',#48121,0.0165732954740135);
#15562=CIRCLE('',#48122,0.0168141205745554);
#15563=CIRCLE('',#48123,0.0110535374087421);
#15564=CIRCLE('',#48124,0.0168028429610667);
#15565=CIRCLE('',#48125,0.0110635670195058);
#15566=CIRCLE('',#48126,0.0166019907129225);
#15567=CIRCLE('',#48128,0.0166008698804845);
#15568=CIRCLE('',#48129,0.016601992082684);
#15569=CIRCLE('',#48130,0.0166008685783328);
#15570=CIRCLE('',#48131,0.0167571840014611);
#15571=CIRCLE('',#48132,0.0110511996805999);
#15572=CIRCLE('',#48133,0.0167907391091645);
#15573=CIRCLE('',#48134,0.0110190981845518);
#15574=CIRCLE('',#48135,0.00665874808267189);
#15575=CIRCLE('',#48141,0.016715706678982);
#15576=CIRCLE('',#48142,0.0109625450123671);
#15577=CIRCLE('',#48144,0.0165541458429362);
#15578=CIRCLE('',#48146,0.0165579396121371);
#15579=CIRCLE('',#48147,0.0165541473073873);
#15580=CIRCLE('',#48148,0.0165579381287537);
#15581=CIRCLE('',#48149,0.0168110399837888);
#15582=CIRCLE('',#48150,0.0110459668050407);
#15583=CIRCLE('',#48151,0.0167928000131913);
#15584=CIRCLE('',#48152,0.0110624552739991);
#15585=CIRCLE('',#48155,0.0166052623178069);
#15586=CIRCLE('',#48157,0.0166047971419355);
#15587=CIRCLE('',#48158,0.0166052632661251);
#15588=CIRCLE('',#48159,0.0166047959270355);
#15589=CIRCLE('',#48160,0.0167731971565613);
#15590=CIRCLE('',#48161,0.0110573244865064);
#15591=CIRCLE('',#48162,0.0168013216995224);
#15592=CIRCLE('',#48163,0.0110316530744794);
#15593=CIRCLE('',#48164,0.0165310255747975);
#15594=CIRCLE('',#48166,0.0165263129036402);
#15595=CIRCLE('',#48167,0.0165310265276423);
#15596=CIRCLE('',#48168,0.0165263117199402);
#15597=CIRCLE('',#48169,0.0166775856847219);
#15598=CIRCLE('',#48170,0.010920569121723);
#15599=CIRCLE('',#48172,0.016421116098934);
#15600=CIRCLE('',#48173,0.0164211148099697);
#15601=CIRCLE('',#48174,0.0167388248042058);
#15602=CIRCLE('',#48175,0.0109676124285651);
#15603=CIRCLE('',#48176,0.0166825658005706);
#15604=CIRCLE('',#48177,0.0110194472756133);
#15605=CIRCLE('',#48178,0.0165701550852875);
#15606=CIRCLE('',#48180,0.0165732968920231);
#15607=CIRCLE('',#48181,0.0165701561472083);
#15608=CIRCLE('',#48182,0.0165732954569517);
#15609=CIRCLE('',#48183,0.0168141206459413);
#15610=CIRCLE('',#48184,0.0110535372534566);
#15611=CIRCLE('',#48185,0.0168028429612771);
#15612=CIRCLE('',#48186,0.0110635670198656);
#15613=CIRCLE('',#48187,0.0166019908312719);
#15614=CIRCLE('',#48189,0.0166008696419111);
#15615=CIRCLE('',#48190,0.0166019921364906);
#15616=CIRCLE('',#48191,0.0166008683378502);
#15617=CIRCLE('',#48192,0.0167571840016696);
#15618=CIRCLE('',#48193,0.0110511996786392);
#15619=CIRCLE('',#48194,0.0167907391087163);
#15620=CIRCLE('',#48195,0.0110190981851326);
#15621=CIRCLE('',#48196,0.00665874807863192);
#15622=CIRCLE('',#48202,0.0167157066786652);
#15623=CIRCLE('',#48203,0.01096254501372);
#15624=CIRCLE('',#48205,0.0165541458428756);
#15625=CIRCLE('',#48207,0.0165579395212262);
#15626=CIRCLE('',#48208,0.0165541472262184);
#15627=CIRCLE('',#48209,0.0165579380173231);
#15628=CIRCLE('',#48210,0.0168110399836305);
#15629=CIRCLE('',#48211,0.0110459668053802);
#15630=CIRCLE('',#48212,0.0167928000132902);
#15631=CIRCLE('',#48213,0.0110624552750508);
#15632=CIRCLE('',#48216,0.0166052622985171);
#15633=CIRCLE('',#48218,0.0166047969953593);
#15634=CIRCLE('',#48219,0.0166052632596361);
#15635=CIRCLE('',#48220,0.0166047958844994);
#15636=CIRCLE('',#48221,0.0167731971564568);
#15637=CIRCLE('',#48222,0.0110573244851529);
#15638=CIRCLE('',#48223,0.0168013216996);
#15639=CIRCLE('',#48224,0.0110316530734903);
#15640=CIRCLE('',#48225,0.016531025524901);
#15641=CIRCLE('',#48227,0.0165263128517349);
#15642=CIRCLE('',#48228,0.0165310265016073);
#15643=CIRCLE('',#48229,0.0165263115872939);
#15644=CIRCLE('',#48230,0.0166775856845724);
#15645=CIRCLE('',#48231,0.0109205691219406);
#15646=CIRCLE('',#48233,0.0164211159073852);
#15647=CIRCLE('',#48234,0.0164211147625774);
#15648=CIRCLE('',#48235,0.0167388235417366);
#15649=CIRCLE('',#48236,0.0109676133178607);
#15650=CIRCLE('',#48237,0.0166825658004808);
#15651=CIRCLE('',#48238,0.0110194472764579);
#15652=CIRCLE('',#48239,0.0165701550086192);
#15653=CIRCLE('',#48241,0.0165732968106716);
#15654=CIRCLE('',#48242,0.0165701560854755);
#15655=CIRCLE('',#48243,0.0165732953410207);
#15656=CIRCLE('',#48244,0.0168141206272819);
#15657=CIRCLE('',#48245,0.0110535372938326);
#15658=CIRCLE('',#48246,0.0168028429616766);
#15659=CIRCLE('',#48247,0.0110635670196207);
#15660=CIRCLE('',#48248,0.0166019908311988);
#15661=CIRCLE('',#48250,0.016600869402183);
#15662=CIRCLE('',#48251,0.0166019920672427);
#15663=CIRCLE('',#48252,0.0166008681241324);
#15664=CIRCLE('',#48253,0.0167577810054763);
#15665=CIRCLE('',#48254,0.011051199676122);
#15666=CIRCLE('',#48255,0.0167907391087387);
#15667=CIRCLE('',#48256,0.0110190981854095);
#15668=CIRCLE('',#48257,0.00665874808266081);
#15669=CIRCLE('',#48263,0.0167157066785781);
#15670=CIRCLE('',#48264,0.0109625450129892);
#15671=CIRCLE('',#48266,0.0165541458625202);
#15672=CIRCLE('',#48268,0.0165579392760386);
#15673=CIRCLE('',#48269,0.0165541470496618);
#15674=CIRCLE('',#48270,0.0165579379144359);
#15675=CIRCLE('',#48271,0.0168110399834894);
#15676=CIRCLE('',#48272,0.0110459668055838);
#15677=CIRCLE('',#48273,0.0167928000130272);
#15678=CIRCLE('',#48274,0.0110624552745341);
#15679=CIRCLE('',#48277,0.0166052622900365);
#15680=CIRCLE('',#48279,0.016604796869262);
#15681=CIRCLE('',#48280,0.0166052631782005);
#15682=CIRCLE('',#48281,0.0166047958522747);
#15683=CIRCLE('',#48282,0.0167731971564835);
#15684=CIRCLE('',#48283,0.011057324485878);
#15685=CIRCLE('',#48284,0.0168013216995648);
#15686=CIRCLE('',#48285,0.0110316530741046);
#15687=CIRCLE('',#48286,0.0165310254682413);
#15688=CIRCLE('',#48288,0.0165263126814153);
#15689=CIRCLE('',#48289,0.0165310264424974);
#15690=CIRCLE('',#48290,0.0165263115926201);
#15691=CIRCLE('',#48291,0.0166775856846586);
#15692=CIRCLE('',#48292,0.0109205691217816);
#15693=CIRCLE('',#48294,0.0164211156962373);
#15694=CIRCLE('',#48295,0.0164211145902099);
#15695=CIRCLE('',#48296,0.0167388248044593);
#15696=CIRCLE('',#48297,0.0109676124272191);
#15697=CIRCLE('',#48298,0.0166825658002918);
#15698=CIRCLE('',#48299,0.0110194472756495);
#15699=CIRCLE('',#48300,0.0165701549805964);
#15700=CIRCLE('',#48302,0.0165732964757245);
#15701=CIRCLE('',#48303,0.016570155993251);
#15702=CIRCLE('',#48304,0.0165732952076342);
#15703=CIRCLE('',#48305,0.0168141206270738);
#15704=CIRCLE('',#48306,0.0110535372948799);
#15705=CIRCLE('',#48307,0.0168028429613149);
#15706=CIRCLE('',#48308,0.0110635670197968);
#15707=CIRCLE('',#48309,0.0166019907856206);
#15708=CIRCLE('',#48311,0.016600869281246);
#15709=CIRCLE('',#48312,0.0166019919750651);
#15710=CIRCLE('',#48313,0.0166008681437444);
#15711=CIRCLE('',#48314,0.0167571840016302);
#15712=CIRCLE('',#48315,0.0110511996784197);
#15713=CIRCLE('',#48316,0.0167907391087342);
#15714=CIRCLE('',#48317,0.0110190981852672);
#15715=CIRCLE('',#48318,0.00665874807857735);
#15716=CIRCLE('',#48324,0.0167157066788082);
#15717=CIRCLE('',#48325,0.0109625450139715);
#15718=CIRCLE('',#48327,0.0165541457528717);
#15719=CIRCLE('',#48329,0.0165579391310576);
#15720=CIRCLE('',#48330,0.0165541470455079);
#15721=CIRCLE('',#48331,0.0165579378864428);
#15722=CIRCLE('',#48332,0.0168110399835194);
#15723=CIRCLE('',#48333,0.0110459668048852);
#15724=CIRCLE('',#48334,0.0167928000131374);
#15725=CIRCLE('',#48335,0.0110624552741263);
#15726=CIRCLE('',#48338,0.0166052623235493);
#15727=CIRCLE('',#48340,0.0166047966343837);
#15728=CIRCLE('',#48341,0.0166052630637473);
#15729=CIRCLE('',#48342,0.0166047956728293);
#15730=CIRCLE('',#48343,0.016773198350099);
#15731=CIRCLE('',#48344,0.0110573281946764);
#15732=CIRCLE('',#48345,0.0168013216995328);
#15733=CIRCLE('',#48346,0.0110316530739007);
#15734=CIRCLE('',#48347,0.0165310254915807);
#15735=CIRCLE('',#48349,0.0165263125359947);
#15736=CIRCLE('',#48350,0.0165310263328488);
#15737=CIRCLE('',#48351,0.0165263115654509);
#15738=CIRCLE('',#48352,0.0166775856846347);
#15739=CIRCLE('',#48353,0.0109205691218874);
#15740=CIRCLE('',#48355,0.0164211155053557);
#15741=CIRCLE('',#48356,0.0164211145217507);
#15742=CIRCLE('',#48357,0.0167388244017953);
#15743=CIRCLE('',#48358,0.0109676127120334);
#15744=CIRCLE('',#48359,0.0166825658004791);
#15745=CIRCLE('',#48360,0.0110194472762198);
#15746=CIRCLE('',#48361,0.0165701550928783);
#15747=CIRCLE('',#48363,0.0165732963879411);
#15748=CIRCLE('',#48364,0.0165701559310954);
#15749=CIRCLE('',#48365,0.016573295223886);
#15750=CIRCLE('',#48366,0.0168141206271986);
#15751=CIRCLE('',#48367,0.0110535372945764);
#15752=CIRCLE('',#48368,0.0168028429614001);
#15753=CIRCLE('',#48369,0.0110635670197259);
#15754=CIRCLE('',#48370,0.0166019908106737);
#15755=CIRCLE('',#48372,0.016600869078043);
#15756=CIRCLE('',#48373,0.0166019918428707);
#15757=CIRCLE('',#48374,0.016600868010713);
#15758=CIRCLE('',#48375,0.0167571840015784);
#15759=CIRCLE('',#48376,0.0110511996800335);
#15760=CIRCLE('',#48377,0.016790739109042);
#15761=CIRCLE('',#48378,0.0110190981854062);
#15762=CIRCLE('',#48379,0.00665874808278241);
#15763=CIRCLE('',#48385,0.0167157066788378);
#15764=CIRCLE('',#48386,0.0109625450137759);
#15765=CIRCLE('',#48388,0.016554145781167);
#15766=CIRCLE('',#48390,0.0165579390814041);
#15767=CIRCLE('',#48391,0.016554146981822);
#15768=CIRCLE('',#48392,0.0165579378221229);
#15769=CIRCLE('',#48393,0.016811039983634);
#15770=CIRCLE('',#48394,0.0110459668055729);
#15771=CIRCLE('',#48395,0.0167928000132035);
#15772=CIRCLE('',#48396,0.0110624552743364);
#15773=CIRCLE('',#48399,0.0166052621326915);
#15774=CIRCLE('',#48401,0.0166047965546541);
#15775=CIRCLE('',#48402,0.0166052629654533);
#15776=CIRCLE('',#48403,0.0166047956448385);
#15777=CIRCLE('',#48404,0.0167731971564053);
#15778=CIRCLE('',#48405,0.0110573244857942);
#15779=CIRCLE('',#48406,0.0168013216995398);
#15780=CIRCLE('',#48407,0.0110316530743371);
#15781=CIRCLE('',#48408,0.0165310254751661);
#15782=CIRCLE('',#48410,0.016526312332431);
#15783=CIRCLE('',#48411,0.0165310263076625);
#15784=CIRCLE('',#48412,0.016526311446041);
#15785=CIRCLE('',#48413,0.0166775856843973);
#15786=CIRCLE('',#48414,0.0109205691218644);
#15787=CIRCLE('',#48416,0.0164211154121946);
#15788=CIRCLE('',#48417,0.016421114517602);
#15789=CIRCLE('',#48418,0.0167388248043828);
#15790=CIRCLE('',#48419,0.0109676124297309);
#15791=CIRCLE('',#48420,0.0166825658004906);
#15792=CIRCLE('',#48421,0.0110194472759386);
#15793=CIRCLE('',#48422,0.0165701549459977);
#15794=CIRCLE('',#48424,0.0165732962478553);
#15795=CIRCLE('',#48425,0.0165701557827074);
#15796=CIRCLE('',#48426,0.0165732950593365);
#15797=CIRCLE('',#48427,0.0168141206459375);
#15798=CIRCLE('',#48428,0.0110535372538286);
#15799=CIRCLE('',#48429,0.0168028429614107);
#15800=CIRCLE('',#48430,0.0110635670204726);
#15801=CIRCLE('',#48431,0.0166019907581878);
#15802=CIRCLE('',#48433,0.0166008689277773);
#15803=CIRCLE('',#48434,0.0166019917505441);
#15804=CIRCLE('',#48435,0.0166008679730606);
#15805=CIRCLE('',#48436,0.0167571840016015);
#15806=CIRCLE('',#48437,0.0110511996782994);
#15807=CIRCLE('',#48438,0.0167907391087864);
#15808=CIRCLE('',#48439,0.0110190981847917);
#15809=CIRCLE('',#48440,0.00665874807856375);
#15810=CIRCLE('',#48446,0.0167157066788102);
#15811=CIRCLE('',#48447,0.0109625450123883);
#15812=CIRCLE('',#48449,0.0165541457930371);
#15813=CIRCLE('',#48451,0.0165579390065225);
#15814=CIRCLE('',#48452,0.0165541470235924);
#15815=CIRCLE('',#48453,0.0165579377120552);
#15816=CIRCLE('',#48454,0.0168110399836019);
#15817=CIRCLE('',#48455,0.0110459668046012);
#15818=CIRCLE('',#48456,0.0167928000133165);
#15819=CIRCLE('',#48457,0.0110624552745342);
#15820=CIRCLE('',#48460,0.0166052623962907);
#15821=CIRCLE('',#48462,0.0166047964871083);
#15822=CIRCLE('',#48463,0.0166052630584548);
#15823=CIRCLE('',#48464,0.0166047955723545);
#15824=CIRCLE('',#48465,0.0167731971564806);
#15825=CIRCLE('',#48466,0.011057324486099);
#15826=CIRCLE('',#48467,0.0168013216996322);
#15827=CIRCLE('',#48468,0.0110316530750212);
#15828=CIRCLE('',#48469,0.0165310254445976);
#15829=CIRCLE('',#48471,0.0165263122162804);
#15830=CIRCLE('',#48472,0.0165310261855289);
#15831=CIRCLE('',#48473,0.0165263113676245);
#15832=CIRCLE('',#48474,0.0166775856844551);
#15833=CIRCLE('',#48475,0.0109205691223334);
#15834=CIRCLE('',#48477,0.0164211151716581);
#15835=CIRCLE('',#48478,0.0164211143291737);
#15836=CIRCLE('',#48479,0.0167388248041972);
#15837=CIRCLE('',#48480,0.0109676124278026);
#15838=CIRCLE('',#48481,0.0166825658002287);
#15839=CIRCLE('',#48482,0.0110194472760281);
#15840=CIRCLE('',#48483,0.0165701549962637);
#15841=CIRCLE('',#48485,0.0165732961308722);
#15842=CIRCLE('',#48486,0.0165701557733917);
#15843=CIRCLE('',#48487,0.016573294988113);
#15844=CIRCLE('',#48488,0.0168141206457764);
#15845=CIRCLE('',#48489,0.0110535372558345);
#15846=CIRCLE('',#48490,0.0168028429614474);
#15847=CIRCLE('',#48491,0.0110635670202249);
#15848=CIRCLE('',#48492,0.0166019907868911);
#15849=CIRCLE('',#48494,0.0166008687725664);
#15850=CIRCLE('',#48495,0.0166019916684501);
#15851=CIRCLE('',#48496,0.0166008679137632);
#15852=CIRCLE('',#48497,0.016757184001683);
#15853=CIRCLE('',#48498,0.0110512000569263);
#15854=CIRCLE('',#48499,0.016790739108977);
#15855=CIRCLE('',#48500,0.0110190981844742);
#15856=CIRCLE('',#48501,0.00665874948999836);
#15857=CIRCLE('',#48507,0.0167157066788402);
#15858=CIRCLE('',#48508,0.0109625450147756);
#15859=CIRCLE('',#48510,0.016554145772189);
#15860=CIRCLE('',#48512,0.0165579387522727);
#15861=CIRCLE('',#48513,0.016554146838596);
#15862=CIRCLE('',#48514,0.0165579376418337);
#15863=CIRCLE('',#48515,0.016811039983612);
#15864=CIRCLE('',#48516,0.0110459668047955);
#15865=CIRCLE('',#48517,0.0167928000134311);
#15866=CIRCLE('',#48518,0.0110624552743749);
#15867=CIRCLE('',#48521,0.0166052623598551);
#15868=CIRCLE('',#48523,0.0166047964320598);
#15869=CIRCLE('',#48524,0.0166052629385756);
#15870=CIRCLE('',#48525,0.0166047955511812);
#15871=CIRCLE('',#48526,0.0167731971563387);
#15872=CIRCLE('',#48527,0.011057324484739);
#15873=CIRCLE('',#48528,0.0168013216997687);
#15874=CIRCLE('',#48529,0.0110316530744769);
#15875=CIRCLE('',#48530,0.0165310254871738);
#15876=CIRCLE('',#48532,0.0165263120948897);
#15877=CIRCLE('',#48533,0.0165310260521502);
#15878=CIRCLE('',#48534,0.016526311314141);
#15879=CIRCLE('',#48535,0.0166775856846251);
#15880=CIRCLE('',#48536,0.0109205691213651);
#15881=CIRCLE('',#48538,0.0164211151214994);
#15882=CIRCLE('',#48539,0.0164211142044887);
#15883=CIRCLE('',#48540,0.0167388248042407);
#15884=CIRCLE('',#48541,0.0109676124279531);
#15885=CIRCLE('',#48542,0.0166825658003064);
#15886=CIRCLE('',#48543,0.0110194472762773);
#15887=CIRCLE('',#48544,0.0165701549300338);
#15888=CIRCLE('',#48546,0.01657329596834);
#15889=CIRCLE('',#48547,0.0165701556722587);
#15890=CIRCLE('',#48548,0.0165732949097595);
#15891=CIRCLE('',#48549,0.0168141206458614);
#15892=CIRCLE('',#48550,0.0110535372562175);
#15893=CIRCLE('',#48551,0.0168028429609649);
#15894=CIRCLE('',#48552,0.0110635670204018);
#15895=CIRCLE('',#48553,0.0166019907899111);
#15896=CIRCLE('',#48555,0.0166008687324912);
#15897=CIRCLE('',#48556,0.0166019915912748);
#15898=CIRCLE('',#48557,0.0166008678302651);
#15899=CIRCLE('',#48558,0.0167571840016815);
#15900=CIRCLE('',#48559,0.0110511996755867);
#15901=CIRCLE('',#48560,0.0167907391091693);
#15902=CIRCLE('',#48561,0.0110190981847612);
#15903=CIRCLE('',#48562,0.00665874808285124);
#15904=CIRCLE('',#48568,0.0167157066788687);
#15905=CIRCLE('',#48569,0.0109625450105235);
#15906=CIRCLE('',#48571,0.0165541458689486);
#15907=CIRCLE('',#48573,0.0165579387376058);
#15908=CIRCLE('',#48574,0.016554146790368);
#15909=CIRCLE('',#48575,0.0165579377385169);
#15910=CIRCLE('',#48576,0.0168110399836123);
#15911=CIRCLE('',#48577,0.0110459668052381);
#15912=CIRCLE('',#48578,0.0167928000134394);
#15913=CIRCLE('',#48579,0.0110624552747778);
#15914=CIRCLE('',#48582,0.0166052622177305);
#15915=CIRCLE('',#48584,0.0166047963821227);
#15916=CIRCLE('',#48585,0.0166052627674726);
#15917=CIRCLE('',#48586,0.0166047954504736);
#15918=CIRCLE('',#48587,0.0167731971567311);
#15919=CIRCLE('',#48588,0.0110573244852228);
#15920=CIRCLE('',#48589,0.0168013217001361);
#15921=CIRCLE('',#48590,0.0110316530738364);
#15922=CIRCLE('',#48591,0.0165310254896641);
#15923=CIRCLE('',#48593,0.0165263120151855);
#15924=CIRCLE('',#48594,0.016531026053535);
#15925=CIRCLE('',#48595,0.0165263111919852);
#15926=CIRCLE('',#48596,0.0166775856847841);
#15927=CIRCLE('',#48597,0.0109205691208038);
#15928=CIRCLE('',#48599,0.0164211150348133);
#15929=CIRCLE('',#48600,0.0164211142243237);
#15930=CIRCLE('',#48601,0.0167388248044049);
#15931=CIRCLE('',#48602,0.010967612429207);
#15932=CIRCLE('',#48603,0.0166825658005772);
#15933=CIRCLE('',#48604,0.011019447276484);
#15934=CIRCLE('',#48605,0.0165701548872828);
#15935=CIRCLE('',#48607,0.0165732958098313);
#15936=CIRCLE('',#48608,0.0165701556355031);
#15937=CIRCLE('',#48609,0.0165732948914799);
#15938=CIRCLE('',#48610,0.016814120646272);
#15939=CIRCLE('',#48611,0.011053537253304);
#15940=CIRCLE('',#48612,0.0168028429611533);
#15941=CIRCLE('',#48613,0.0110635670201188);
#15942=CIRCLE('',#48614,0.0166019907902361);
#15943=CIRCLE('',#48616,0.0166008685032828);
#15944=CIRCLE('',#48617,0.0166019914916695);
#15945=CIRCLE('',#48618,0.016600867649731);
#15946=CIRCLE('',#48619,0.0167571840015815);
#15947=CIRCLE('',#48620,0.011051199679);
#15948=CIRCLE('',#48621,0.0167907391088403);
#15949=CIRCLE('',#48622,0.0110190981841265);
#15950=CIRCLE('',#48623,0.00665874807866852);
#15951=CIRCLE('',#48629,0.0167157066790663);
#15952=CIRCLE('',#48630,0.0109625450116274);
#15953=CIRCLE('',#48632,0.0165541457744851);
#15954=CIRCLE('',#48634,0.0165579387507397);
#15955=CIRCLE('',#48635,0.016554146743131);
#15956=CIRCLE('',#48636,0.0165579377034758);
#15957=CIRCLE('',#48637,0.0168110399838886);
#15958=CIRCLE('',#48638,0.0110459668054311);
#15959=CIRCLE('',#48639,0.0167928000134423);
#15960=CIRCLE('',#48640,0.0110624552738554);
#15961=CIRCLE('',#48643,0.0166052623210084);
#15962=CIRCLE('',#48645,0.0166047962621703);
#15963=CIRCLE('',#48646,0.0166052628393574);
#15964=CIRCLE('',#48647,0.0166047955580633);
#15965=CIRCLE('',#48648,0.0167731971565687);
#15966=CIRCLE('',#48649,0.0110573244856284);
#15967=CIRCLE('',#48650,0.0168013217000599);
#15968=CIRCLE('',#48651,0.0110316530737674);
#15969=CIRCLE('',#48652,0.016531025343733);
#15970=CIRCLE('',#48654,0.0165263119423416);
#15971=CIRCLE('',#48655,0.0165310259885897);
#15972=CIRCLE('',#48656,0.0165263111618812);
#15973=CIRCLE('',#48657,0.0166775856845741);
#15974=CIRCLE('',#48658,0.0109205691218698);
#15975=CIRCLE('',#48660,0.0164211148044813);
#15976=CIRCLE('',#48661,0.0164211140991842);
#15977=CIRCLE('',#48662,0.0167388248044534);
#15978=CIRCLE('',#48663,0.0109676124283774);
#15979=CIRCLE('',#48664,0.0166825658003316);
#15980=CIRCLE('',#48665,0.011019447275932);
#15981=CIRCLE('',#48666,0.0165701549382436);
#15982=CIRCLE('',#48668,0.0165732957156712);
#15983=CIRCLE('',#48669,0.0165701555936647);
#15984=CIRCLE('',#48670,0.0165732948439745);
#15985=CIRCLE('',#48671,0.0168141205747683);
#15986=CIRCLE('',#48672,0.011053537408688);
#15987=CIRCLE('',#48673,0.0168028429614129);
#15988=CIRCLE('',#48674,0.0110635670205279);
#15989=CIRCLE('',#48675,0.0166019907724184);
#15990=CIRCLE('',#48677,0.0166008684458131);
#15991=CIRCLE('',#48678,0.0166019915037999);
#15992=CIRCLE('',#48679,0.0166008675674056);
#15993=CIRCLE('',#48680,0.0167571840019693);
#15994=CIRCLE('',#48681,0.0110511996785788);
#15995=CIRCLE('',#48682,0.0167907391089601);
#15996=CIRCLE('',#48683,0.0110190981854491);
#15997=CIRCLE('',#48684,0.00665874807856069);
#15998=CIRCLE('',#48690,0.016715706678537);
#15999=CIRCLE('',#48691,0.0109625450197299);
#16000=CIRCLE('',#48693,0.016554145832691);
#16001=CIRCLE('',#48695,0.0165579388535833);
#16002=CIRCLE('',#48696,0.0165541468078329);
#16003=CIRCLE('',#48697,0.0165579376714078);
#16004=CIRCLE('',#48698,0.0168110399839155);
#16005=CIRCLE('',#48699,0.0110459668052241);
#16006=CIRCLE('',#48700,0.0167928000135522);
#16007=CIRCLE('',#48701,0.0110624552747427);
#16008=CIRCLE('',#48704,0.0166052622016704);
#16009=CIRCLE('',#48706,0.016604796182051);
#16010=CIRCLE('',#48707,0.0166052627553303);
#16011=CIRCLE('',#48708,0.0166047954861773);
#16012=CIRCLE('',#48709,0.016773197156293);
#16013=CIRCLE('',#48710,0.0110573244845348);
#16014=CIRCLE('',#48711,0.0168013216996969);
#16015=CIRCLE('',#48712,0.0110316530734857);
#16016=CIRCLE('',#48713,0.0165310253971778);
#16017=CIRCLE('',#48715,0.0165263117090146);
#16018=CIRCLE('',#48716,0.0165310260091766);
#16019=CIRCLE('',#48717,0.0165263111336701);
#16020=CIRCLE('',#48718,0.0166775856849231);
#16021=CIRCLE('',#48719,0.0109205691220921);
#16022=CIRCLE('',#48721,0.0164211147379008);
#16023=CIRCLE('',#48722,0.0164211140186072);
#16024=CIRCLE('',#48723,0.0167388248039756);
#16025=CIRCLE('',#48724,0.0109676124295965);
#16026=CIRCLE('',#48725,0.0166825658000704);
#16027=CIRCLE('',#48726,0.0110194472757774);
#16028=CIRCLE('',#48727,0.0165701550589786);
#16029=CIRCLE('',#48729,0.0165732955439304);
#16030=CIRCLE('',#48730,0.0165701554623967);
#16031=CIRCLE('',#48731,0.0165732947607562);
#16032=CIRCLE('',#48732,0.0168141206460369);
#16033=CIRCLE('',#48733,0.0110535372552296);
#16034=CIRCLE('',#48734,0.016802842961279);
#16035=CIRCLE('',#48735,0.0110635670194712);
#16036=CIRCLE('',#48736,0.016601990558003);
#16037=CIRCLE('',#48738,0.0166008682641072);
#16038=CIRCLE('',#48739,0.0166019914886659);
#16039=CIRCLE('',#48740,0.0166008676115602);
#16040=CIRCLE('',#48741,0.0167571840015966);
#16041=CIRCLE('',#48742,0.0110511996789531);
#16042=CIRCLE('',#48743,0.0167907391091812);
#16043=CIRCLE('',#48744,0.0110190981859215);
#16044=CIRCLE('',#48745,0.0066587480786017);
#16045=CIRCLE('',#48752,0.016557938393399);
#16046=CIRCLE('',#48753,0.0165541465800056);
#16047=CIRCLE('',#48754,0.0165541457005333);
#16048=CIRCLE('',#48755,0.0165579375969566);
#16049=CIRCLE('',#48756,0.0167157066784803);
#16050=CIRCLE('',#48757,0.0109625450132406);
#16051=CIRCLE('',#48759,0.0168110399838593);
#16052=CIRCLE('',#48760,0.0110459668052074);
#16053=CIRCLE('',#48761,0.0167928000132456);
#16054=CIRCLE('',#48762,0.0110624552747817);
#16055=CIRCLE('',#48765,0.0166052620204301);
#16056=CIRCLE('',#48767,0.0166047961639415);
#16057=CIRCLE('',#48768,0.0166052628105858);
#16058=CIRCLE('',#48769,0.0166047955823238);
#16059=CIRCLE('',#48770,0.0167731971571948);
#16060=CIRCLE('',#48771,0.0110573244863);
#16061=CIRCLE('',#48772,0.0168013216971416);
#16062=CIRCLE('',#48773,0.0110316530737572);
#16063=CIRCLE('',#48774,0.0165310253747238);
#16064=CIRCLE('',#48776,0.016526312005147);
#16065=CIRCLE('',#48777,0.0165310260705086);
#16066=CIRCLE('',#48778,0.0165263109804035);
#16067=CIRCLE('',#48779,0.0166775856847484);
#16068=CIRCLE('',#48780,0.0109205691222534);
#16069=CIRCLE('',#48782,0.0164211146382283);
#16070=CIRCLE('',#48783,0.0164211139468424);
#16071=CIRCLE('',#48784,0.016738824804484);
#16072=CIRCLE('',#48785,0.0109676124291467);
#16073=CIRCLE('',#48786,0.0166825658004142);
#16074=CIRCLE('',#48787,0.0110194472756397);
#16075=CIRCLE('',#48788,0.016570155142403);
#16076=CIRCLE('',#48790,0.0165732953358236);
#16077=CIRCLE('',#48791,0.0165701555271706);
#16078=CIRCLE('',#48792,0.0165732944523174);
#16079=CIRCLE('',#48793,0.0168141205740459);
#16080=CIRCLE('',#48794,0.011053537408101);
#16081=CIRCLE('',#48795,0.0168028429610983);
#16082=CIRCLE('',#48796,0.0110635670202757);
#16083=CIRCLE('',#48797,0.016601990873592);
#16084=CIRCLE('',#48799,0.0166008681138699);
#16085=CIRCLE('',#48800,0.0166019914981724);
#16086=CIRCLE('',#48801,0.016600867635325);
#16087=CIRCLE('',#48802,0.0167571840016304);
#16088=CIRCLE('',#48803,0.0110511996746034);
#16089=CIRCLE('',#48804,0.0167907391096125);
#16090=CIRCLE('',#48805,0.0110190981856332);
#16091=CIRCLE('',#48806,0.00665874807864147);
#16092=CIRCLE('',#48813,0.0166047962151536);
#16093=CIRCLE('',#48814,0.0166052626736676);
#16094=CIRCLE('',#48815,0.0166052623558693);
#16095=CIRCLE('',#48816,0.0166047953839558);
#16096=CIRCLE('',#48818,0.0165579386710114);
#16097=CIRCLE('',#48819,0.0165541467375174);
#16098=CIRCLE('',#48820,0.0165541458003313);
#16099=CIRCLE('',#48821,0.0165579376502966);
#16100=CIRCLE('',#48822,0.0167157066782624);
#16101=CIRCLE('',#48823,0.0109625450121743);
#16102=CIRCLE('',#48825,0.0168110399837832);
#16103=CIRCLE('',#48826,0.0110459668064786);
#16104=CIRCLE('',#48827,0.0167928000131371);
#16105=CIRCLE('',#48828,0.0110624552742206);
#16106=CIRCLE('',#48831,0.0167731941318447);
#16107=CIRCLE('',#48832,0.0110573150854568);
#16108=CIRCLE('',#48833,0.016801321700207);
#16109=CIRCLE('',#48834,0.0110316530747847);
#16110=CIRCLE('',#48835,0.0165310253466521);
#16111=CIRCLE('',#48837,0.0165263118016029);
#16112=CIRCLE('',#48838,0.0165310260720093);
#16113=CIRCLE('',#48839,0.0165263109786302);
#16114=CIRCLE('',#48840,0.0166775856849412);
#16115=CIRCLE('',#48841,0.0109205691228325);
#16116=CIRCLE('',#48843,0.0164211146258441);
#16117=CIRCLE('',#48844,0.0164211141132704);
#16118=CIRCLE('',#48845,0.0167388248046037);
#16119=CIRCLE('',#48846,0.010967612428738);
#16120=CIRCLE('',#48847,0.0166825658000916);
#16121=CIRCLE('',#48848,0.0110194472760106);
#16122=CIRCLE('',#48849,0.0165701550493577);
#16123=CIRCLE('',#48851,0.0165732951167833);
#16124=CIRCLE('',#48852,0.0165701554481991);
#16125=CIRCLE('',#48853,0.0165732947079051);
#16126=CIRCLE('',#48854,0.0168141206459652);
#16127=CIRCLE('',#48855,0.0110535372533542);
#16128=CIRCLE('',#48856,0.0168028429612053);
#16129=CIRCLE('',#48857,0.011063567020668);
#16130=CIRCLE('',#48858,0.016601990796754);
#16131=CIRCLE('',#48860,0.0166008681495549);
#16132=CIRCLE('',#48861,0.016601991287057);
#16133=CIRCLE('',#48862,0.0166008676670592);
#16134=CIRCLE('',#48863,0.0167571840015897);
#16135=CIRCLE('',#48864,0.0110511996792007);
#16136=CIRCLE('',#48865,0.0167907391090489);
#16137=CIRCLE('',#48866,0.011019098184922);
#16138=CIRCLE('',#48867,0.00665874807852574);
#16139=CIRCLE('',#48874,0.016557937242374);
#16140=CIRCLE('',#48875,0.0165541493793539);
#16141=CIRCLE('',#48876,0.0165541529820997);
#16142=CIRCLE('',#48877,0.0165579410864609);
#16143=CIRCLE('',#48879,0.0165263116215834);
#16144=CIRCLE('',#48880,0.0165310258878028);
#16145=CIRCLE('',#48881,0.0165310253924632);
#16146=CIRCLE('',#48882,0.0165263111348691);
#16147=CIRCLE('',#48884,0.0166047959564872);
#16148=CIRCLE('',#48885,0.0166052625710691);
#16149=CIRCLE('',#48886,0.016605262158595);
#16150=CIRCLE('',#48887,0.0166047955076839);
#16151=CIRCLE('',#48888,0.0168110399834951);
#16152=CIRCLE('',#48889,0.0110459668057758);
#16153=CIRCLE('',#48890,0.0167928000131421);
#16154=CIRCLE('',#48891,0.0110624552741314);
#16155=CIRCLE('',#48894,0.0167731971562018);
#16156=CIRCLE('',#48895,0.011057324484393);
#16157=CIRCLE('',#48896,0.0168013216998445);
#16158=CIRCLE('',#48897,0.0110316530740487);
#16159=CIRCLE('',#48898,0.016677585684157);
#16160=CIRCLE('',#48899,0.0109205691204241);
#16161=CIRCLE('',#48900,0.0167157066790715);
#16162=CIRCLE('',#48901,0.0109625450147775);
#16163=CIRCLE('',#48904,0.0164211142969033);
#16164=CIRCLE('',#48905,0.0164211138522741);
#16165=CIRCLE('',#48906,0.0167388248042754);
#16166=CIRCLE('',#48907,0.0109676124296621);
#16167=CIRCLE('',#48908,0.0166825658001335);
#16168=CIRCLE('',#48909,0.0110194472755734);
#16169=CIRCLE('',#48910,0.016570154969177);
#16170=CIRCLE('',#48912,0.0165732952369211);
#16171=CIRCLE('',#48913,0.0165701552418422);
#16172=CIRCLE('',#48914,0.0165732945809266);
#16173=CIRCLE('',#48915,0.0168141205748277);
#16174=CIRCLE('',#48916,0.0110535374108902);
#16175=CIRCLE('',#48917,0.0168028429609699);
#16176=CIRCLE('',#48918,0.0110635670205065);
#16177=CIRCLE('',#48919,0.0166019908221658);
#16178=CIRCLE('',#48921,0.0166008677448166);
#16179=CIRCLE('',#48922,0.0166019910949407);
#16180=CIRCLE('',#48923,0.0166008676018247);
#16181=CIRCLE('',#48924,0.0167571840016316);
#16182=CIRCLE('',#48925,0.0110511996795116);
#16183=CIRCLE('',#48926,0.0167907391092683);
#16184=CIRCLE('',#48927,0.0110190981847272);
#16185=CIRCLE('',#48928,0.00665874807855451);
#16186=CIRCLE('',#48935,0.0165579455857381);
#16187=CIRCLE('',#48936,0.0165541498437811);
#16188=CIRCLE('',#48937,0.0165541457456698);
#16189=CIRCLE('',#48938,0.0165579408786856);
#16190=CIRCLE('',#48940,0.016604795239985);
#16191=CIRCLE('',#48941,0.0166052660684846);
#16192=CIRCLE('',#48942,0.0166052697732378);
#16193=CIRCLE('',#48943,0.0166047985728746);
#16194=CIRCLE('',#48945,0.016421114122627);
#16195=CIRCLE('',#48946,0.0164211138454056);
#16196=CIRCLE('',#48948,0.0165263119725143);
#16197=CIRCLE('',#48949,0.0165310259092296);
#16198=CIRCLE('',#48950,0.0165310254281581);
#16199=CIRCLE('',#48951,0.0165263110945175);
#16200=CIRCLE('',#48952,0.0167731941324389);
#16201=CIRCLE('',#48953,0.0110573150841859);
#16202=CIRCLE('',#48954,0.0168013216994028);
#16203=CIRCLE('',#48955,0.0110316530738022);
#16204=CIRCLE('',#48956,0.0166775856846015);
#16205=CIRCLE('',#48957,0.0109205691205302);
#16206=CIRCLE('',#48958,0.0167388248039332);
#16207=CIRCLE('',#48959,0.0109676124292315);
#16208=CIRCLE('',#48960,0.0166825658001939);
#16209=CIRCLE('',#48961,0.0110194472762046);
#16210=CIRCLE('',#48962,0.0165701550429815);
#16211=CIRCLE('',#48963,0.0167157066790929);
#16212=CIRCLE('',#48964,0.0109625450184708);
#16213=CIRCLE('',#48966,0.0168110399829948);
#16214=CIRCLE('',#48967,0.0110459668038541);
#16215=CIRCLE('',#48968,0.0167928000131439);
#16216=CIRCLE('',#48969,0.0110624552739188);
#16217=CIRCLE('',#48973,0.0165732949494959);
#16218=CIRCLE('',#48974,0.0165701553102014);
#16219=CIRCLE('',#48975,0.016573294404056);
#16220=CIRCLE('',#48976,0.0168141206275132);
#16221=CIRCLE('',#48977,0.0110535372967461);
#16222=CIRCLE('',#48978,0.0168028429610256);
#16223=CIRCLE('',#48979,0.0110635670189512);
#16224=CIRCLE('',#48980,0.016601990634965);
#16225=CIRCLE('',#48982,0.0166008677966898);
#16226=CIRCLE('',#48983,0.0166019912748291);
#16227=CIRCLE('',#48984,0.0166008673365702);
#16228=CIRCLE('',#48985,0.0167571840017735);
#16229=CIRCLE('',#48986,0.0110511996760864);
#16230=CIRCLE('',#48987,0.016790739108973);
#16231=CIRCLE('',#48988,0.0110190981836151);
#16232=CIRCLE('',#48989,0.006658748078702);
#16233=CIRCLE('',#48996,0.0166048028270532);
#16234=CIRCLE('',#48997,0.0166052661745815);
#16235=CIRCLE('',#48998,0.0166052620760957);
#16236=CIRCLE('',#48999,0.0166047986766637);
#16237=CIRCLE('',#49001,0.0165263107944059);
#16238=CIRCLE('',#49002,0.0165310291800569);
#16239=CIRCLE('',#49003,0.016531033258646);
#16240=CIRCLE('',#49004,0.0165263139561476);
#16241=CIRCLE('',#49006,0.0165579452785632);
#16242=CIRCLE('',#49007,0.0165541498850607);
#16243=CIRCLE('',#49008,0.0165541458961846);
#16244=CIRCLE('',#49009,0.0165579408553482);
#16245=CIRCLE('',#49011,0.0165732946997177);
#16246=CIRCLE('',#49012,0.0165701553210565);
#16247=CIRCLE('',#49013,0.0165701549414162);
#16248=CIRCLE('',#49014,0.0165732941125412);
#16249=CIRCLE('',#49016,0.0164211139334697);
#16250=CIRCLE('',#49017,0.0164211136739296);
#16251=CIRCLE('',#49018,0.0166775856845022);
#16252=CIRCLE('',#49019,0.0109205691229004);
#16253=CIRCLE('',#49020,0.0167388248043908);
#16254=CIRCLE('',#49021,0.0109676124286852);
#16255=CIRCLE('',#49022,0.0166825658001782);
#16256=CIRCLE('',#49023,0.0110194472770084);
#16257=CIRCLE('',#49024,0.0168141206268823);
#16258=CIRCLE('',#49025,0.0110535372941716);
#16259=CIRCLE('',#49026,0.0168028429606942);
#16260=CIRCLE('',#49027,0.0110635670207016);
#16261=CIRCLE('',#49028,0.0166019907542044);
#16262=CIRCLE('',#49029,0.0167157066784153);
#16263=CIRCLE('',#49030,0.0109625450155666);
#16264=CIRCLE('',#49032,0.0168110399837356);
#16265=CIRCLE('',#49033,0.0110459668043168);
#16266=CIRCLE('',#49034,0.0167928000125649);
#16267=CIRCLE('',#49035,0.0110624552757974);
#16268=CIRCLE('',#49038,0.0167731971566166);
#16269=CIRCLE('',#49039,0.0110573244865956);
#16270=CIRCLE('',#49040,0.0168013216996847);
#16271=CIRCLE('',#49041,0.0110316530734883);
#16272=CIRCLE('',#49043,0.016600867675102);
#16273=CIRCLE('',#49044,0.0166019908963819);
#16274=CIRCLE('',#49045,0.0166008673124711);
#16275=CIRCLE('',#49046,0.0167571840015828);
#16276=CIRCLE('',#49047,0.0110511996731572);
#16277=CIRCLE('',#49048,0.0167907391094298);
#16278=CIRCLE('',#49049,0.0110190981840155);
#16279=CIRCLE('',#49050,0.00665874807849252);
#16280=CIRCLE('',#49057,0.0165263179950152);
#16281=CIRCLE('',#49058,0.0165310293667509);
#16282=CIRCLE('',#49059,0.0165310254750887);
#16283=CIRCLE('',#49060,0.0165263142576533);
#16284=CIRCLE('',#49062,0.016421112801567);
#16285=CIRCLE('',#49063,0.0164211129684179);
#16286=CIRCLE('',#49065,0.0166048025454181);
#16287=CIRCLE('',#49066,0.0166052658521807);
#16288=CIRCLE('',#49067,0.0166052623722192);
#16289=CIRCLE('',#49068,0.016604799156512);
#16290=CIRCLE('',#49070,0.0165579450668964);
#16291=CIRCLE('',#49071,0.0165541497704911);
#16292=CIRCLE('',#49072,0.0165541458562401);
#16293=CIRCLE('',#49073,0.0165579409363684);
#16294=CIRCLE('',#49075,0.0166008675583637);
#16295=CIRCLE('',#49076,0.0166019911921346);
#16296=CIRCLE('',#49077,0.0166019909806196);
#16297=CIRCLE('',#49078,0.0166008674180751);
#16298=CIRCLE('',#49080,0.0165732948516365);
#16299=CIRCLE('',#49081,0.0165701549539817);
#16300=CIRCLE('',#49082,0.0165701548215611);
#16301=CIRCLE('',#49083,0.0165732946310353);
#16302=CIRCLE('',#49084,0.0167388235414638);
#16303=CIRCLE('',#49085,0.0109676133208622);
#16304=CIRCLE('',#49086,0.0166825658004335);
#16305=CIRCLE('',#49087,0.0110194472763306);
#16306=CIRCLE('',#49088,0.0168141206269654);
#16307=CIRCLE('',#49089,0.0110535372941354);
#16308=CIRCLE('',#49090,0.0168028429606016);
#16309=CIRCLE('',#49091,0.0110635670210023);
#16310=CIRCLE('',#49092,0.0167577810042491);
#16311=CIRCLE('',#49093,0.0110511996741528);
#16312=CIRCLE('',#49094,0.0167907391083702);
#16313=CIRCLE('',#49095,0.0110190981849621);
#16314=CIRCLE('',#49096,0.00665874807860464);
#16315=CIRCLE('',#49097,0.016715706678561);
#16316=CIRCLE('',#49098,0.0109625450139336);
#16317=CIRCLE('',#49100,0.01681103998381);
#16318=CIRCLE('',#49101,0.0110459668040065);
#16319=CIRCLE('',#49102,0.0167928000129461);
#16320=CIRCLE('',#49103,0.011062455275826);
#16321=CIRCLE('',#49106,0.0167731971564552);
#16322=CIRCLE('',#49107,0.0110573244867307);
#16323=CIRCLE('',#49108,0.0168013217000393);
#16324=CIRCLE('',#49109,0.0110316530743163);
#16325=CIRCLE('',#49110,0.0166775856850414);
#16326=CIRCLE('',#49111,0.0109205691219998);
#16327=CIRCLE('',#49127,0.0167388260783937);
#16328=CIRCLE('',#49128,0.0166825657982655);
#16329=CIRCLE('',#49129,0.016677585688039);
#16330=CIRCLE('',#49130,0.0168013216997719);
#16331=CIRCLE('',#49131,0.0167731941307207);
#16332=CIRCLE('',#49132,0.0167927979163913);
#16333=CIRCLE('',#49133,0.0168110399834981);
#16334=CIRCLE('',#49134,0.0167157066894911);
#16335=CIRCLE('',#49135,0.016669993461729);
#16336=CIRCLE('',#49138,0.016790740140474);
#16337=CIRCLE('',#49139,0.0167556795651006);
#16338=CIRCLE('',#49140,0.0168141206870994);
#16339=CIRCLE('',#49141,0.0168028429614352);
#16340=CIRCLE('',#49144,0.0167907401409518);
#16341=CIRCLE('',#49145,0.0167556795649506);
#16342=CIRCLE('',#49146,0.0166775856879641);
#16343=CIRCLE('',#49147,0.0168013216996554);
#16344=CIRCLE('',#49148,0.0167731941280413);
#16345=CIRCLE('',#49149,0.0167927979156723);
#16346=CIRCLE('',#49150,0.0168110399832801);
#16347=CIRCLE('',#49151,0.0167157066891269);
#16348=CIRCLE('',#49152,0.0166699934626322);
#16349=CIRCLE('',#49153,0.0168028429612061);
#16350=CIRCLE('',#49154,0.0168141206870611);
#16351=CIRCLE('',#49155,0.0167388260793371);
#16352=CIRCLE('',#49156,0.016682565798012);
#16353=CIRCLE('',#49159,0.0167907401408078);
#16354=CIRCLE('',#49160,0.0167556795652516);
#16355=CIRCLE('',#49161,0.0168028429610846);
#16356=CIRCLE('',#49162,0.0168141206870671);
#16357=CIRCLE('',#49163,0.0167731941284153);
#16358=CIRCLE('',#49164,0.0168013216997419);
#16359=CIRCLE('',#49165,0.016792797915505);
#16360=CIRCLE('',#49166,0.0168110399837014);
#16361=CIRCLE('',#49167,0.0167157066890383);
#16362=CIRCLE('',#49168,0.0166699934636628);
#16363=CIRCLE('',#49169,0.0166825657979271);
#16364=CIRCLE('',#49170,0.0167388260780698);
#16365=CIRCLE('',#49171,0.0166775856878139);
#16366=CIRCLE('',#49174,0.0167907401403366);
#16367=CIRCLE('',#49175,0.0167556795651758);
#16368=CIRCLE('',#49176,0.0168028429612437);
#16369=CIRCLE('',#49177,0.016814120686832);
#16370=CIRCLE('',#49178,0.0166825657979198);
#16371=CIRCLE('',#49179,0.0167388260787839);
#16372=CIRCLE('',#49180,0.0168110399833388);
#16373=CIRCLE('',#49181,0.0167927979159865);
#16374=CIRCLE('',#49182,0.0167157066893643);
#16375=CIRCLE('',#49183,0.0166699934636401);
#16376=CIRCLE('',#49184,0.0166775856879577);
#16377=CIRCLE('',#49185,0.0167731941306356);
#16378=CIRCLE('',#49186,0.0168013217000056);
#16379=CIRCLE('',#49189,0.016790740140676);
#16380=CIRCLE('',#49190,0.0167556795647294);
#16381=CIRCLE('',#49191,0.0168028429607678);
#16382=CIRCLE('',#49192,0.016814120686581);
#16383=CIRCLE('',#49193,0.016682565798137);
#16384=CIRCLE('',#49194,0.0167388260784122);
#16385=CIRCLE('',#49195,0.0166775856881153);
#16386=CIRCLE('',#49196,0.0167157066889213);
#16387=CIRCLE('',#49197,0.0166699934634911);
#16388=CIRCLE('',#49198,0.0168013217001458);
#16389=CIRCLE('',#49199,0.0167731941276694);
#16390=CIRCLE('',#49200,0.0168110399835617);
#16391=CIRCLE('',#49201,0.0167927979161373);
#16392=CIRCLE('',#49204,0.0167907401403663);
#16393=CIRCLE('',#49205,0.0167556795645121);
#16394=CIRCLE('',#49206,0.0168028429610977);
#16395=CIRCLE('',#49207,0.0168141206872044);
#16396=CIRCLE('',#49208,0.0166825657978588);
#16397=CIRCLE('',#49209,0.0167388260786764);
#16398=CIRCLE('',#49210,0.0166775856875181);
#16399=CIRCLE('',#49211,0.0168013216997636);
#16400=CIRCLE('',#49212,0.0167731941312831);
#16401=CIRCLE('',#49213,0.0167927979156146);
#16402=CIRCLE('',#49214,0.0168110399829328);
#16403=CIRCLE('',#49215,0.0167157066892931);
#16404=CIRCLE('',#49216,0.0166699934628592);
#16405=CIRCLE('',#49219,0.0167907401406868);
#16406=CIRCLE('',#49220,0.016755679564891);
#16407=CIRCLE('',#49221,0.0168028429609253);
#16408=CIRCLE('',#49222,0.016814120687073);
#16409=CIRCLE('',#49223,0.0166825657976404);
#16410=CIRCLE('',#49224,0.0167388260782794);
#16411=CIRCLE('',#49225,0.0166775856880801);
#16412=CIRCLE('',#49226,0.0168013217001565);
#16413=CIRCLE('',#49227,0.0167731941275393);
#16414=CIRCLE('',#49228,0.0167927979158512);
#16415=CIRCLE('',#49229,0.0168110399828972);
#16416=CIRCLE('',#49230,0.016715706690013);
#16417=CIRCLE('',#49231,0.0166699934626573);
#16418=CIRCLE('',#49234,0.0167907401409215);
#16419=CIRCLE('',#49235,0.0167556795649318);
#16420=CIRCLE('',#49236,0.0168028429612012);
#16421=CIRCLE('',#49237,0.0168141206870639);
#16422=CIRCLE('',#49238,0.0166825657980482);
#16423=CIRCLE('',#49239,0.0167388260785539);
#16424=CIRCLE('',#49240,0.0166775856881294);
#16425=CIRCLE('',#49241,0.0168013217002588);
#16426=CIRCLE('',#49242,0.0167731941275873);
#16427=CIRCLE('',#49243,0.0167927979163074);
#16428=CIRCLE('',#49244,0.0168110399834913);
#16429=CIRCLE('',#49245,0.01671570669022);
#16430=CIRCLE('',#49246,0.0166699934637729);
#16431=CIRCLE('',#49249,0.0167907401408375);
#16432=CIRCLE('',#49250,0.0167556795644563);
#16433=CIRCLE('',#49251,0.0168028429614237);
#16434=CIRCLE('',#49252,0.0168141206867054);
#16435=CIRCLE('',#49253,0.0166825657978822);
#16436=CIRCLE('',#49254,0.0167388260784786);
#16437=CIRCLE('',#49255,0.0166775856882109);
#16438=CIRCLE('',#49256,0.0168013217001937);
#16439=CIRCLE('',#49257,0.0167731941272391);
#16440=CIRCLE('',#49258,0.0167927979160117);
#16441=CIRCLE('',#49259,0.0168110399832238);
#16442=CIRCLE('',#49260,0.0167157066898009);
#16443=CIRCLE('',#49261,0.0166699934627845);
#16444=CIRCLE('',#49264,0.0167907401407062);
#16445=CIRCLE('',#49265,0.0167556795646256);
#16446=CIRCLE('',#49266,0.0168028429611231);
#16447=CIRCLE('',#49267,0.0168141206869206);
#16448=CIRCLE('',#49268,0.0166825657980672);
#16449=CIRCLE('',#49269,0.0167388260784666);
#16450=CIRCLE('',#49270,0.0166775856878968);
#16451=CIRCLE('',#49271,0.0168013217000833);
#16452=CIRCLE('',#49272,0.0167731941274843);
#16453=CIRCLE('',#49273,0.0167927979160231);
#16454=CIRCLE('',#49274,0.0168110399832967);
#16455=CIRCLE('',#49275,0.0167157066900166);
#16456=CIRCLE('',#49276,0.0166699934635313);
#16457=CIRCLE('',#49279,0.0167907401405469);
#16458=CIRCLE('',#49280,0.0167556795646356);
#16459=CIRCLE('',#49281,0.0168028429610838);
#16460=CIRCLE('',#49282,0.0168141206869845);
#16461=CIRCLE('',#49283,0.0166825657980557);
#16462=CIRCLE('',#49284,0.0167388260783001);
#16463=CIRCLE('',#49285,0.0166775856879415);
#16464=CIRCLE('',#49286,0.0168013216996465);
#16465=CIRCLE('',#49287,0.0167731941273415);
#16466=CIRCLE('',#49288,0.0167927979157984);
#16467=CIRCLE('',#49289,0.0168110399832164);
#16468=CIRCLE('',#49290,0.0167157066897016);
#16469=CIRCLE('',#49291,0.0166699934628616);
#16470=CIRCLE('',#49294,0.0167907401405266);
#16471=CIRCLE('',#49295,0.0167556795645506);
#16472=CIRCLE('',#49296,0.0168028429611932);
#16473=CIRCLE('',#49297,0.0168141206868017);
#16474=CIRCLE('',#49298,0.016682565798159);
#16475=CIRCLE('',#49299,0.0167388260783459);
#16476=CIRCLE('',#49300,0.0166775856879777);
#16477=CIRCLE('',#49301,0.0168013216996097);
#16478=CIRCLE('',#49302,0.0167731941274576);
#16479=CIRCLE('',#49303,0.0167927979157949);
#16480=CIRCLE('',#49304,0.0168110399830942);
#16481=CIRCLE('',#49305,0.0167157066896616);
#16482=CIRCLE('',#49306,0.0166699934630128);
#16483=CIRCLE('',#49309,0.0167907401404702);
#16484=CIRCLE('',#49310,0.0167556795647818);
#16485=CIRCLE('',#49311,0.0168028429611256);
#16486=CIRCLE('',#49312,0.0168141206869255);
#16487=CIRCLE('',#49313,0.0166825657979659);
#16488=CIRCLE('',#49314,0.0167388260782657);
#16489=CIRCLE('',#49315,0.0166775856881158);
#16490=CIRCLE('',#49316,0.0168013216998003);
#16491=CIRCLE('',#49317,0.0167731941278287);
#16492=CIRCLE('',#49318,0.0167927979158031);
#16493=CIRCLE('',#49319,0.0168110399831387);
#16494=CIRCLE('',#49320,0.0167157066897092);
#16495=CIRCLE('',#49321,0.0166699934632686);
#16496=CIRCLE('',#49324,0.0167907401404887);
#16497=CIRCLE('',#49325,0.0167556795649006);
#16498=CIRCLE('',#49326,0.0168028429610311);
#16499=CIRCLE('',#49327,0.0168141206867439);
#16500=CIRCLE('',#49328,0.0166825657981543);
#16501=CIRCLE('',#49329,0.0167388260782707);
#16502=CIRCLE('',#49330,0.0166775856879633);
#16503=CIRCLE('',#49331,0.0168013216997165);
#16504=CIRCLE('',#49332,0.0167731941261392);
#16505=CIRCLE('',#49333,0.0167927979157724);
#16506=CIRCLE('',#49334,0.0168110399830984);
#16507=CIRCLE('',#49335,0.0167157066895802);
#16508=CIRCLE('',#49336,0.0166699934630215);
#16509=CIRCLE('',#49339,0.0167907401405266);
#16510=CIRCLE('',#49340,0.0167556795647706);
#16511=CIRCLE('',#49341,0.0168028429610707);
#16512=CIRCLE('',#49342,0.0168141206869169);
#16513=CIRCLE('',#49343,0.0166825657981712);
#16514=CIRCLE('',#49344,0.0167388260781345);
#16515=CIRCLE('',#49345,0.0166775856880515);
#16516=CIRCLE('',#49346,0.0168013216996411);
#16517=CIRCLE('',#49347,0.0167731941277484);
#16518=CIRCLE('',#49348,0.0167927979158021);
#16519=CIRCLE('',#49349,0.0168110399831109);
#16520=CIRCLE('',#49350,0.0167157066894836);
#16521=CIRCLE('',#49351,0.01666999346303);
#16522=CIRCLE('',#49354,0.0167907401402849);
#16523=CIRCLE('',#49355,0.0167556795649538);
#16524=CIRCLE('',#49356,0.0168028429613468);
#16525=CIRCLE('',#49357,0.0168141206865413);
#16526=CIRCLE('',#49358,0.0166825657981593);
#16527=CIRCLE('',#49359,0.0167388260788683);
#16528=CIRCLE('',#49360,0.0166775856882428);
#16529=CIRCLE('',#49361,0.0168013216994228);
#16530=CIRCLE('',#49362,0.016773194127514);
#16531=CIRCLE('',#49363,0.0167927979156933);
#16532=CIRCLE('',#49364,0.0168110399830131);
#16533=CIRCLE('',#49365,0.0167157066897977);
#16534=CIRCLE('',#49366,0.0166699934631597);
#16535=CIRCLE('',#49369,0.0167907401403453);
#16536=CIRCLE('',#49370,0.0167556795646501);
#16537=CIRCLE('',#49371,0.0168028429612447);
#16538=CIRCLE('',#49372,0.0168141206866647);
#16539=CIRCLE('',#49373,0.0166825657980678);
#16540=CIRCLE('',#49374,0.016738826078584);
#16541=CIRCLE('',#49375,0.0166775856878689);
#16542=CIRCLE('',#49376,0.0168013216998913);
#16543=CIRCLE('',#49377,0.0167731941274802);
#16544=CIRCLE('',#49378,0.0167927979155802);
#16545=CIRCLE('',#49379,0.0168110399832431);
#16546=CIRCLE('',#49380,0.0167157066894647);
#16547=CIRCLE('',#49381,0.0166699934627573);
#16548=CIRCLE('',#49384,0.0167907401399346);
#16549=CIRCLE('',#49385,0.016755679564844);
#16550=CIRCLE('',#49386,0.0168028429610995);
#16551=CIRCLE('',#49387,0.0168141206868666);
#16552=CIRCLE('',#49388,0.0166825657982027);
#16553=CIRCLE('',#49389,0.0167388260782498);
#16554=CIRCLE('',#49390,0.0166775856882351);
#16555=CIRCLE('',#49391,0.0168013216997972);
#16556=CIRCLE('',#49392,0.0167731941278249);
#16557=CIRCLE('',#49393,0.0167927979153362);
#16558=CIRCLE('',#49394,0.0168110399829424);
#16559=CIRCLE('',#49395,0.016715706689545);
#16560=CIRCLE('',#49396,0.0166699934633333);
#16561=CIRCLE('',#49399,0.0167907401404065);
#16562=CIRCLE('',#49400,0.0167556795645056);
#16563=CIRCLE('',#49401,0.0168028429610298);
#16564=CIRCLE('',#49402,0.0168141206869512);
#16565=CIRCLE('',#49403,0.0166825657981821);
#16566=CIRCLE('',#49404,0.0167388260779847);
#16567=CIRCLE('',#49405,0.0166775856883076);
#16568=CIRCLE('',#49406,0.0168013217000258);
#16569=CIRCLE('',#49407,0.016773194127048);
#16570=CIRCLE('',#49408,0.0167927979160005);
#16571=CIRCLE('',#49409,0.0168110399829486);
#16572=CIRCLE('',#49410,0.016715706689756);
#16573=CIRCLE('',#49411,0.0166699934628589);
#16574=CIRCLE('',#49414,0.0167907401403316);
#16575=CIRCLE('',#49415,0.0167556795644366);
#16576=CIRCLE('',#49416,0.0168028429610019);
#16577=CIRCLE('',#49417,0.016814120687397);
#16578=CIRCLE('',#49418,0.0166825657985891);
#16579=CIRCLE('',#49419,0.0167388260779154);
#16580=CIRCLE('',#49420,0.0166775856881447);
#16581=CIRCLE('',#49421,0.0168013216997569);
#16582=CIRCLE('',#49422,0.0167731941313463);
#16583=CIRCLE('',#49423,0.0167927979160407);
#16584=CIRCLE('',#49424,0.0168110399828166);
#16585=CIRCLE('',#49425,0.016715706689698);
#16586=CIRCLE('',#49426,0.0166699934624352);
#16587=CIRCLE('',#49429,0.0167907401401542);
#16588=CIRCLE('',#49430,0.0167556795645292);
#16589=CIRCLE('',#49431,0.016802842961176);
#16590=CIRCLE('',#49432,0.016814120686921);
#16591=CIRCLE('',#49433,0.0166825657981214);
#16592=CIRCLE('',#49434,0.0167388260781204);
#16593=CIRCLE('',#49435,0.0166775856878453);
#16594=CIRCLE('',#49436,0.0168013217000734);
#16595=CIRCLE('',#49437,0.0167731941274432);
#16596=CIRCLE('',#49438,0.0167927979156718);
#16597=CIRCLE('',#49439,0.0168110399831377);
#16598=CIRCLE('',#49440,0.0167157066896371);
#16599=CIRCLE('',#49441,0.0166699934621213);
#16600=CIRCLE('',#49444,0.0167907401408063);
#16601=CIRCLE('',#49445,0.0167556795650037);
#16602=CIRCLE('',#49446,0.0168028429611068);
#16603=CIRCLE('',#49447,0.0168141206864774);
#16604=CIRCLE('',#49448,0.0166825657986373);
#16605=CIRCLE('',#49449,0.0167388260793153);
#16606=CIRCLE('',#49450,0.0166775856881973);
#16607=CIRCLE('',#49451,0.0168013216999736);
#16608=CIRCLE('',#49452,0.0167731941279987);
#16609=CIRCLE('',#49453,0.0167927979157798);
#16610=CIRCLE('',#49454,0.0168110399829498);
#16611=CIRCLE('',#49455,0.0167157066894906);
#16612=CIRCLE('',#49456,0.0166699934635282);
#16613=CIRCLE('',#49459,0.0167907401399869);
#16614=CIRCLE('',#49460,0.0167556795645096);
#16615=CIRCLE('',#49461,0.0168028429608607);
#16616=CIRCLE('',#49462,0.0168141206866532);
#16617=CIRCLE('',#49463,0.0166825657986826);
#16618=CIRCLE('',#49464,0.0167388260779909);
#16619=CIRCLE('',#49465,0.0166775856878773);
#16620=CIRCLE('',#49466,0.0168013216998194);
#16621=CIRCLE('',#49467,0.0167731941269337);
#16622=CIRCLE('',#49468,0.0167927979154591);
#16623=CIRCLE('',#49469,0.0168110399830451);
#16624=CIRCLE('',#49470,0.016715706689462);
#16625=CIRCLE('',#49471,0.0166699934625152);
#16626=CIRCLE('',#49474,0.0167907401401331);
#16627=CIRCLE('',#49475,0.0167556795646395);
#16628=CIRCLE('',#49476,0.0168028429616909);
#16629=CIRCLE('',#49477,0.0168141206867984);
#16630=CIRCLE('',#49478,0.0166825657987859);
#16631=CIRCLE('',#49479,0.0167388260782469);
#16632=CIRCLE('',#49480,0.0166775856879888);
#16633=CIRCLE('',#49481,0.0168013216991336);
#16634=CIRCLE('',#49482,0.0167731941268989);
#16635=CIRCLE('',#49483,0.0167927979157023);
#16636=CIRCLE('',#49484,0.0168110399830373);
#16637=CIRCLE('',#49485,0.0167157066891133);
#16638=CIRCLE('',#49486,0.0166699934636415);
#16639=CIRCLE('',#49489,0.0167907401399268);
#16640=CIRCLE('',#49490,0.016755679564799);
#16641=CIRCLE('',#49491,0.0168028429610272);
#16642=CIRCLE('',#49492,0.0168141206865376);
#16643=CIRCLE('',#49493,0.0166825657977261);
#16644=CIRCLE('',#49494,0.0167388260780295);
#16645=CIRCLE('',#49495,0.0166775856882616);
#16646=CIRCLE('',#49496,0.0168013216989463);
#16647=CIRCLE('',#49497,0.016773194127227);
#16648=CIRCLE('',#49498,0.0167927979160616);
#16649=CIRCLE('',#49499,0.0168110399825236);
#16650=CIRCLE('',#49500,0.0167157066891566);
#16651=CIRCLE('',#49501,0.0166699934635826);
#16652=CIRCLE('',#49504,0.0167907401403848);
#16653=CIRCLE('',#49505,0.0167556795649154);
#16654=CIRCLE('',#49506,0.0168028429616512);
#16655=CIRCLE('',#49507,0.0168141206873185);
#16656=CIRCLE('',#49508,0.0166825657986855);
#16657=CIRCLE('',#49509,0.0167388260784559);
#16658=CIRCLE('',#49510,0.0166775856884377);
#16659=CIRCLE('',#49511,0.016801321699798);
#16660=CIRCLE('',#49512,0.0167731941264143);
#16661=CIRCLE('',#49513,0.0167927979155266);
#16662=CIRCLE('',#49514,0.0168110399834553);
#16663=CIRCLE('',#49515,0.0167157066896358);
#16664=CIRCLE('',#49516,0.0166699934627382);
#16665=CIRCLE('',#49519,0.0167907401403515);
#16666=CIRCLE('',#49520,0.0167556795649599);
#16667=CIRCLE('',#49521,0.0168028429606613);
#16668=CIRCLE('',#49522,0.0168141206865821);
#16669=CIRCLE('',#49523,0.016682565798408);
#16670=CIRCLE('',#49524,0.0167388260783537);
#16671=CIRCLE('',#49525,0.0166775856878138);
#16672=CIRCLE('',#49526,0.016801321699649);
#16673=CIRCLE('',#49527,0.0167731941281915);
#16674=CIRCLE('',#49528,0.0167927979157696);
#16675=CIRCLE('',#49529,0.016811039982445);
#16676=CIRCLE('',#49530,0.0167157066896602);
#16677=CIRCLE('',#49531,0.0166699934624107);
#16678=CIRCLE('',#49534,0.0167907401405091);
#16679=CIRCLE('',#49535,0.0167556795648695);
#16680=CIRCLE('',#49536,0.0168028429605574);
#16681=CIRCLE('',#49537,0.0168141206868357);
#16682=CIRCLE('',#49538,0.0166825657984589);
#16683=CIRCLE('',#49539,0.0167388260780524);
#16684=CIRCLE('',#49540,0.0166775856881515);
#16685=CIRCLE('',#49541,0.0168013216994995);
#16686=CIRCLE('',#49542,0.0167731941274536);
#16687=CIRCLE('',#49543,0.016792797915285);
#16688=CIRCLE('',#49544,0.016811039983189);
#16689=CIRCLE('',#49545,0.0167157066899231);
#16690=CIRCLE('',#49546,0.0166699934630661);
#16691=CIRCLE('',#49549,0.016790740140516);
#16692=CIRCLE('',#49550,0.0167556795648152);
#16693=CIRCLE('',#49551,0.0168028429611241);
#16694=CIRCLE('',#49552,0.0168141206865178);
#16695=CIRCLE('',#49553,0.0166825657986247);
#16696=CIRCLE('',#49554,0.0167388260789807);
#16697=CIRCLE('',#49555,0.0166775856883438);
#16698=CIRCLE('',#49556,0.0168013216988337);
#16699=CIRCLE('',#49557,0.0167731941308824);
#16700=CIRCLE('',#49558,0.0167927979151636);
#16701=CIRCLE('',#49559,0.0168110399829744);
#16702=CIRCLE('',#49560,0.0167157066897106);
#16703=CIRCLE('',#49561,0.0166699934627811);
#16704=CIRCLE('',#49564,0.0167907401403223);
#16705=CIRCLE('',#49565,0.0167556795648479);
#16706=CIRCLE('',#49566,0.0168028429613066);
#16707=CIRCLE('',#49567,0.0168141206867935);
#16708=CIRCLE('',#49568,0.016682565798211);
#16709=CIRCLE('',#49569,0.0167388260791185);
#16710=CIRCLE('',#49570,0.0166775856879496);
#16711=CIRCLE('',#49571,0.0168013216997423);
#16712=CIRCLE('',#49572,0.0167731941268201);
#16713=CIRCLE('',#49573,0.0167927979157175);
#16714=CIRCLE('',#49574,0.0168110399830299);
#16715=CIRCLE('',#49575,0.0167157066894611);
#16716=CIRCLE('',#49576,0.0166699934627715);
#16717=CIRCLE('',#49579,0.0167907401406675);
#16718=CIRCLE('',#49580,0.0167556795651135);
#16719=CIRCLE('',#49581,0.0168028429611185);
#16720=CIRCLE('',#49582,0.0168141206868113);
#16721=CIRCLE('',#49583,0.0166825657981354);
#16722=CIRCLE('',#49584,0.016738826078842);
#16723=CIRCLE('',#49585,0.0166775856879909);
#16724=CIRCLE('',#49586,0.0168013216996849);
#16725=CIRCLE('',#49587,0.0167731941309764);
#16726=CIRCLE('',#49588,0.0167927979155125);
#16727=CIRCLE('',#49589,0.0168110399827123);
#16728=CIRCLE('',#49590,0.0167157066899265);
#16729=CIRCLE('',#49591,0.0166699934632962);
#16730=CIRCLE('',#49594,0.0167907401400898);
#16731=CIRCLE('',#49595,0.0167556795648269);
#16732=CIRCLE('',#49596,0.0168028429611803);
#16733=CIRCLE('',#49597,0.0168141206869151);
#16734=CIRCLE('',#49598,0.0166825657981214);
#16735=CIRCLE('',#49599,0.0167388260780384);
#16736=CIRCLE('',#49600,0.0166775856876485);
#16737=CIRCLE('',#49601,0.0168013216999341);
#16738=CIRCLE('',#49602,0.0167731941273188);
#16739=CIRCLE('',#49603,0.0167927979155007);
#16740=CIRCLE('',#49604,0.0168110399830011);
#16741=CIRCLE('',#49605,0.0167157066896642);
#16742=CIRCLE('',#49606,0.0166699934625497);
#16743=CIRCLE('',#49609,0.0167907401400955);
#16744=CIRCLE('',#49610,0.016755679564979);
#16745=CIRCLE('',#49611,0.016802842961219);
#16746=CIRCLE('',#49612,0.0168141206866368);
#16747=CIRCLE('',#49613,0.0166825657982672);
#16748=CIRCLE('',#49614,0.0167388260779614);
#16749=CIRCLE('',#49615,0.0166775856879899);
#16750=CIRCLE('',#49616,0.0168013216996006);
#16751=CIRCLE('',#49617,0.0167731941275982);
#16752=CIRCLE('',#49618,0.0167927979154729);
#16753=CIRCLE('',#49619,0.0168110399826746);
#16754=CIRCLE('',#49620,0.016715706689989);
#16755=CIRCLE('',#49621,0.0166699934626932);
#16756=CIRCLE('',#49624,0.0167907401402084);
#16757=CIRCLE('',#49625,0.0167556795648738);
#16758=CIRCLE('',#49626,0.0168028429612814);
#16759=CIRCLE('',#49627,0.0168141206866302);
#16760=CIRCLE('',#49628,0.016682565798374);
#16761=CIRCLE('',#49629,0.016738826078286);
#16762=CIRCLE('',#49630,0.0166775856882792);
#16763=CIRCLE('',#49631,0.0168013216997163);
#16764=CIRCLE('',#49632,0.0167731941269379);
#16765=CIRCLE('',#49633,0.0167927979155145);
#16766=CIRCLE('',#49634,0.0168110399830661);
#16767=CIRCLE('',#49635,0.0167157066895842);
#16768=CIRCLE('',#49636,0.016669993462965);
#16769=CIRCLE('',#49639,0.0167907401403724);
#16770=CIRCLE('',#49640,0.0167556795647631);
#16771=CIRCLE('',#49641,0.0168028429611403);
#16772=CIRCLE('',#49642,0.0168141206867779);
#16773=CIRCLE('',#49643,0.0166825657980329);
#16774=CIRCLE('',#49644,0.0167388260781292);
#16775=CIRCLE('',#49645,0.0166775856880859);
#16776=CIRCLE('',#49646,0.0168013216996242);
#16777=CIRCLE('',#49647,0.0167731941274905);
#16778=CIRCLE('',#49648,0.0167927979153934);
#16779=CIRCLE('',#49649,0.0168110399830263);
#16780=CIRCLE('',#49650,0.0167157066893938);
#16781=CIRCLE('',#49651,0.016669993463144);
#16782=CIRCLE('',#49654,0.0167907401403581);
#16783=CIRCLE('',#49655,0.0167556795646162);
#16784=CIRCLE('',#49656,0.0168028429611157);
#16785=CIRCLE('',#49657,0.0168141206868219);
#16786=CIRCLE('',#49658,0.0166825657980236);
#16787=CIRCLE('',#49659,0.0167388260788799);
#16788=CIRCLE('',#49660,0.0166775856879766);
#16789=CIRCLE('',#49661,0.0168013216995879);
#16790=CIRCLE('',#49662,0.016773194130988);
#16791=CIRCLE('',#49663,0.016792797915703);
#16792=CIRCLE('',#49664,0.0168110399831045);
#16793=CIRCLE('',#49665,0.0167157066894689);
#16794=CIRCLE('',#49666,0.0166699934630159);
#16795=CIRCLE('',#49669,0.0167907401404635);
#16796=CIRCLE('',#49670,0.0167556795646378);
#16797=CIRCLE('',#49671,0.0168028429611376);
#16798=CIRCLE('',#49672,0.0168141206868429);
#16799=CIRCLE('',#49673,0.0166825657981163);
#16800=CIRCLE('',#49674,0.0167388260782811);
#16801=CIRCLE('',#49675,0.0166775856879326);
#16802=CIRCLE('',#49676,0.0168013216998213);
#16803=CIRCLE('',#49677,0.0167731941273884);
#16804=CIRCLE('',#49678,0.0167927979156772);
#16805=CIRCLE('',#49679,0.0168110399831208);
#16806=CIRCLE('',#49680,0.0167157066895047);
#16807=CIRCLE('',#49681,0.0166699934629633);
#16808=CIRCLE('',#49684,0.0167907401403066);
#16809=CIRCLE('',#49685,0.0167556795646854);
#16810=CIRCLE('',#49686,0.0168028429612024);
#16811=CIRCLE('',#49687,0.0168141206868642);
#16812=CIRCLE('',#49688,0.0166825657981071);
#16813=CIRCLE('',#49689,0.0167388260788764);
#16814=CIRCLE('',#49690,0.0166775856879837);
#16815=CIRCLE('',#49691,0.0168013216997269);
#16816=CIRCLE('',#49692,0.0167731941275909);
#16817=CIRCLE('',#49693,0.01679279791573);
#16818=CIRCLE('',#49694,0.0168110399830354);
#16819=CIRCLE('',#49695,0.0167157066893839);
#16820=CIRCLE('',#49696,0.0166699934630788);
#16821=CIRCLE('',#49699,0.0167907401404595);
#16822=CIRCLE('',#49700,0.0167556795646726);
#16823=CIRCLE('',#49701,0.01680284296134);
#16824=CIRCLE('',#49702,0.0168141206869116);
#16825=CIRCLE('',#49703,0.0166825657980472);
#16826=CIRCLE('',#49704,0.0167388260786423);
#16827=CIRCLE('',#49705,0.0166775856880389);
#16828=CIRCLE('',#49706,0.016801321699758);
#16829=CIRCLE('',#49707,0.0167731941261841);
#16830=CIRCLE('',#49708,0.0167927979157453);
#16831=CIRCLE('',#49709,0.0168110399831073);
#16832=CIRCLE('',#49710,0.0167157066895967);
#16833=CIRCLE('',#49711,0.0166699934629367);
#16834=CIRCLE('',#49714,0.01679074014056);
#16835=CIRCLE('',#49715,0.0167556795644209);
#16836=CIRCLE('',#49716,0.016802842961138);
#16837=CIRCLE('',#49717,0.0168141206869105);
#16838=CIRCLE('',#49718,0.0166825657980409);
#16839=CIRCLE('',#49719,0.0167388260784289);
#16840=CIRCLE('',#49720,0.0166775856880623);
#16841=CIRCLE('',#49721,0.0168013216998352);
#16842=CIRCLE('',#49722,0.0167731941275654);
#16843=CIRCLE('',#49723,0.0167927979156913);
#16844=CIRCLE('',#49724,0.0168110399832004);
#16845=CIRCLE('',#49725,0.0167157066896417);
#16846=CIRCLE('',#49726,0.0166699934631642);
#16847=CIRCLE('',#49729,0.0167907401404596);
#16848=CIRCLE('',#49730,0.0167556795643878);
#16849=CIRCLE('',#49731,0.0168028429611488);
#16850=CIRCLE('',#49732,0.0168141206869211);
#16851=CIRCLE('',#49733,0.0166825657981752);
#16852=CIRCLE('',#49734,0.0167388260781587);
#16853=CIRCLE('',#49735,0.0166775856880192);
#16854=CIRCLE('',#49736,0.0168013216997431);
#16855=CIRCLE('',#49737,0.016773194127811);
#16856=CIRCLE('',#49738,0.0167927979156636);
#16857=CIRCLE('',#49739,0.0168110399832791);
#16858=CIRCLE('',#49740,0.0167157066895083);
#16859=CIRCLE('',#49741,0.0166699934633002);
#16860=CIRCLE('',#49744,0.0167907401407301);
#16861=CIRCLE('',#49745,0.0167556795646886);
#16862=CIRCLE('',#49746,0.0168028429607967);
#16863=CIRCLE('',#49747,0.0168141206869222);
#16864=CIRCLE('',#49748,0.0166825657982171);
#16865=CIRCLE('',#49749,0.0167388260786759);
#16866=CIRCLE('',#49750,0.0166775856879533);
#16867=CIRCLE('',#49751,0.0168013216996623);
#16868=CIRCLE('',#49752,0.0167731941276768);
#16869=CIRCLE('',#49753,0.0167927979160612);
#16870=CIRCLE('',#49754,0.0168110399831404);
#16871=CIRCLE('',#49755,0.0167157066895039);
#16872=CIRCLE('',#49756,0.0166699934630218);
#16873=CIRCLE('',#49759,0.0167907401403511);
#16874=CIRCLE('',#49760,0.016755679564925);
#16875=CIRCLE('',#49761,0.0168028429611863);
#16876=CIRCLE('',#49762,0.0168141206870156);
#16877=CIRCLE('',#49763,0.0166825657983043);
#16878=CIRCLE('',#49764,0.0167388260785622);
#16879=CIRCLE('',#49765,0.0166775856880007);
#16880=CIRCLE('',#49766,0.0168013216997968);
#16881=CIRCLE('',#49767,0.0167731941278823);
#16882=CIRCLE('',#49768,0.0167927979159493);
#16883=CIRCLE('',#49769,0.0168110399835583);
#16884=CIRCLE('',#49770,0.016715706689841);
#16885=CIRCLE('',#49771,0.0166699934630285);
#16886=CIRCLE('',#49772,0.0167907401418377);
#16887=CIRCLE('',#49773,0.0167556795640797);
#16888=CIRCLE('',#49776,0.0168028429612844);
#16889=CIRCLE('',#49777,0.0168141206872066);
#16890=CIRCLE('',#49778,0.0166825657981722);
#16891=CIRCLE('',#49779,0.0167388260782425);
#16892=CIRCLE('',#49780,0.0166775856877683);
#16893=CIRCLE('',#49781,0.0168013216998571);
#16894=CIRCLE('',#49782,0.016773194127473);
#16895=CIRCLE('',#49783,0.016792797915847);
#16896=CIRCLE('',#49784,0.0168110399827025);
#16897=CIRCLE('',#49785,0.0167157066896251);
#16898=CIRCLE('',#49786,0.0166699934631566);
#16899=CIRCLE('',#49789,0.0167907401405);
#16900=CIRCLE('',#49790,0.0167556795643959);
#16901=CIRCLE('',#49791,0.0168028429608355);
#16902=CIRCLE('',#49792,0.0168141206870379);
#16903=CIRCLE('',#49793,0.0166825657980907);
#16904=CIRCLE('',#49794,0.0167388260782623);
#16905=CIRCLE('',#49795,0.0166775856876276);
#16906=CIRCLE('',#49796,0.0168013216998691);
#16907=CIRCLE('',#49797,0.0167731941274095);
#16908=CIRCLE('',#49798,0.0167927979157214);
#16909=CIRCLE('',#49799,0.0168110399835694);
#16910=CIRCLE('',#49800,0.0167157066893231);
#16911=CIRCLE('',#49801,0.0166699934625659);
#16912=CIRCLE('',#49804,0.0167907401407283);
#16913=CIRCLE('',#49805,0.0167556795645328);
#16914=CIRCLE('',#49806,0.0168028429606754);
#16915=CIRCLE('',#49807,0.0168141206867869);
#16916=CIRCLE('',#49808,0.016682565797981);
#16917=CIRCLE('',#49809,0.0167388260789757);
#16918=CIRCLE('',#49810,0.0166775856879619);
#16919=CIRCLE('',#49811,0.0168013217004705);
#16920=CIRCLE('',#49812,0.0167731941274059);
#16921=CIRCLE('',#49813,0.0167927979162409);
#16922=CIRCLE('',#49814,0.0168110399829851);
#16923=CIRCLE('',#49815,0.0167157066898108);
#16924=CIRCLE('',#49816,0.0166699934630458);
#16925=CIRCLE('',#49819,0.0167907401412662);
#16926=CIRCLE('',#49820,0.0167556795648169);
#16927=CIRCLE('',#49821,0.0168028429607998);
#16928=CIRCLE('',#49822,0.0168141206873158);
#16929=CIRCLE('',#49823,0.0166825657978841);
#16930=CIRCLE('',#49824,0.0167388260784621);
#16931=CIRCLE('',#49825,0.0166775856881556);
#16932=CIRCLE('',#49826,0.0168013217001323);
#16933=CIRCLE('',#49827,0.0167731941280479);
#16934=CIRCLE('',#49828,0.0167927979162208);
#16935=CIRCLE('',#49829,0.016811039983661);
#16936=CIRCLE('',#49830,0.0167157066894465);
#16937=CIRCLE('',#49831,0.016669993463765);
#16938=CIRCLE('',#49834,0.0167907401410194);
#16939=CIRCLE('',#49835,0.0167556795644157);
#16940=CIRCLE('',#49836,0.0168028429605724);
#16941=CIRCLE('',#49837,0.0168141206871603);
#16942=CIRCLE('',#49838,0.016682565797517);
#16943=CIRCLE('',#49839,0.0167388260786104);
#16944=CIRCLE('',#49840,0.0166775856879752);
#16945=CIRCLE('',#49841,0.0168013216999819);
#16946=CIRCLE('',#49842,0.0167731941273484);
#16947=CIRCLE('',#49843,0.0167927979161244);
#16948=CIRCLE('',#49844,0.0168110399832073);
#16949=CIRCLE('',#49845,0.0167157066895601);
#16950=CIRCLE('',#49846,0.0166699934631375);
#16951=CIRCLE('',#49849,0.0167907401403971);
#16952=CIRCLE('',#49850,0.016755679564564);
#16953=CIRCLE('',#49851,0.0168028429616715);
#16954=CIRCLE('',#49852,0.0168141206866833);
#16955=CIRCLE('',#49853,0.0166825657981775);
#16956=CIRCLE('',#49854,0.0167388260789031);
#16957=CIRCLE('',#49855,0.0166775856879953);
#16958=CIRCLE('',#49856,0.016801321700032);
#16959=CIRCLE('',#49857,0.0167731941275527);
#16960=CIRCLE('',#49858,0.0167927979159458);
#16961=CIRCLE('',#49859,0.0168110399835324);
#16962=CIRCLE('',#49860,0.016715706689142);
#16963=CIRCLE('',#49861,0.0166699934637507);
#16964=CIRCLE('',#49864,0.0167907401408317);
#16965=CIRCLE('',#49865,0.0167556795649818);
#16966=CIRCLE('',#49866,0.0168028429617713);
#16967=CIRCLE('',#49867,0.0168141206868476);
#16968=CIRCLE('',#49868,0.0166825657982996);
#16969=CIRCLE('',#49869,0.0167388260788473);
#16970=CIRCLE('',#49870,0.0166775856876856);
#16971=CIRCLE('',#49871,0.0168013217002675);
#16972=CIRCLE('',#49872,0.0167731941280441);
#16973=CIRCLE('',#49873,0.0167927979160106);
#16974=CIRCLE('',#49874,0.0168110399831407);
#16975=CIRCLE('',#49875,0.0167157066898652);
#16976=CIRCLE('',#49876,0.0166699934632956);
#16977=CIRCLE('',#49879,0.00200000000001);
#16978=CIRCLE('',#49880,0.00200000000001);
#16979=CIRCLE('',#49882,0.00525000000001);
#16980=CIRCLE('',#49883,0.00525000000001);
#16981=CIRCLE('',#49885,0.00439523014419231);
#16982=CIRCLE('',#49886,0.00439523014419231);
#16983=CIRCLE('',#49892,0.00200000000001);
#16984=CIRCLE('',#49893,0.00200000000001);
#16985=CIRCLE('',#49895,0.00525000000001);
#16986=CIRCLE('',#49896,0.00525000000001);
#16987=CIRCLE('',#49901,0.00400000000001);
#16988=CIRCLE('',#49902,0.00400000000001);
#16989=CIRCLE('',#49904,0.00582500000001);
#16990=CIRCLE('',#49905,0.00582500000001);
#16991=CIRCLE('',#49907,0.01087500000001);
#16992=CIRCLE('',#49908,0.01087500000001);
#16993=CIRCLE('',#49910,0.01087500000001);
#16994=CIRCLE('',#49911,0.01087500000001);
#16995=CIRCLE('',#49913,0.01350000000001);
#16996=CIRCLE('',#49914,0.01350000000001);
#16997=CIRCLE('',#49916,0.01350000000001);
#16998=CIRCLE('',#49917,0.01350000000001);
#16999=CIRCLE('',#49919,0.01350000000001);
#17000=CIRCLE('',#49920,0.01350000000001);
#17001=CIRCLE('',#49922,0.01350000000001);
#17002=CIRCLE('',#49923,0.01350000000001);
#17003=CIRCLE('',#49925,0.01350000000001);
#17004=CIRCLE('',#49926,0.01350000000001);
#17005=CIRCLE('',#49928,0.01350000000001);
#17006=CIRCLE('',#49929,0.01350000000001);
#17007=CIRCLE('',#49931,0.01350000000001);
#17008=CIRCLE('',#49932,0.01350000000001);
#17009=CIRCLE('',#49934,0.01350000000001);
#17010=CIRCLE('',#49935,0.01350000000001);
#17011=CIRCLE('',#49937,0.01350000000001);
#17012=CIRCLE('',#49938,0.01350000000001);
#17013=CIRCLE('',#49940,0.01350000000001);
#17014=CIRCLE('',#49941,0.01350000000001);
#17015=CIRCLE('',#49943,0.01350000000001);
#17016=CIRCLE('',#49944,0.01350000000001);
#17017=CIRCLE('',#49946,0.01350000000001);
#17018=CIRCLE('',#49947,0.01350000000001);
#17019=CIRCLE('',#49949,0.01350000000001);
#17020=CIRCLE('',#49950,0.01350000000001);
#17021=CIRCLE('',#49952,0.01350000000001);
#17022=CIRCLE('',#49953,0.01350000000001);
#17023=CIRCLE('',#49955,0.01350000000001);
#17024=CIRCLE('',#49956,0.01350000000001);
#17025=CIRCLE('',#49958,0.01350000000001);
#17026=CIRCLE('',#49959,0.01350000000001);
#17027=CIRCLE('',#49961,0.01350000000001);
#17028=CIRCLE('',#49962,0.01350000000001);
#17029=CIRCLE('',#49964,0.01350000000001);
#17030=CIRCLE('',#49965,0.01350000000001);
#17031=CIRCLE('',#49967,0.01350000000001);
#17032=CIRCLE('',#49968,0.01350000000001);
#17033=CIRCLE('',#49970,0.01350000000001);
#17034=CIRCLE('',#49971,0.01350000000001);
#17035=CIRCLE('',#49973,0.01350000000001);
#17036=CIRCLE('',#49974,0.01350000000001);
#17037=CIRCLE('',#49976,0.01350000000001);
#17038=CIRCLE('',#49977,0.01350000000001);
#17039=CIRCLE('',#49979,0.01350000000001);
#17040=CIRCLE('',#49980,0.01350000000001);
#17041=CIRCLE('',#49982,0.01350000000001);
#17042=CIRCLE('',#49983,0.01350000000001);
#17043=CIRCLE('',#49985,0.01350000000001);
#17044=CIRCLE('',#49986,0.01350000000001);
#17045=CIRCLE('',#49988,0.01350000000001);
#17046=CIRCLE('',#49989,0.01350000000001);
#17047=CIRCLE('',#49991,0.01350000000001);
#17048=CIRCLE('',#49992,0.01350000000001);
#17049=CIRCLE('',#49994,0.01350000000001);
#17050=CIRCLE('',#49995,0.01350000000001);
#17051=CIRCLE('',#49997,0.01350000000001);
#17052=CIRCLE('',#49998,0.01350000000001);
#17053=CIRCLE('',#50000,0.01350000000001);
#17054=CIRCLE('',#50001,0.01350000000001);
#17055=CIRCLE('',#50003,0.01350000000001);
#17056=CIRCLE('',#50004,0.01350000000001);
#17057=CIRCLE('',#50006,0.01350000000001);
#17058=CIRCLE('',#50007,0.01350000000001);
#17059=CIRCLE('',#50009,0.01350000000001);
#17060=CIRCLE('',#50010,0.01350000000001);
#17061=CIRCLE('',#50012,0.01350000000001);
#17062=CIRCLE('',#50013,0.01350000000001);
#17063=CIRCLE('',#50015,0.01350000000001);
#17064=CIRCLE('',#50016,0.01350000000001);
#17065=CIRCLE('',#50018,0.01350000000001);
#17066=CIRCLE('',#50019,0.01350000000001);
#17067=CIRCLE('',#50021,0.01350000000001);
#17068=CIRCLE('',#50022,0.01350000000001);
#17069=CIRCLE('',#50024,0.01350000000001);
#17070=CIRCLE('',#50025,0.01350000000001);
#17071=CIRCLE('',#50027,0.01350000000001);
#17072=CIRCLE('',#50028,0.01350000000001);
#17073=CIRCLE('',#50030,0.01350000000001);
#17074=CIRCLE('',#50031,0.01350000000001);
#17075=CIRCLE('',#50033,0.01350000000001);
#17076=CIRCLE('',#50034,0.01350000000001);
#17077=CIRCLE('',#50036,0.01350000000001);
#17078=CIRCLE('',#50037,0.01350000000001);
#17079=CIRCLE('',#50039,0.01350000000001);
#17080=CIRCLE('',#50040,0.01350000000001);
#17081=CIRCLE('',#50042,0.01350000000001);
#17082=CIRCLE('',#50043,0.01350000000001);
#17083=CIRCLE('',#50045,0.01350000000001);
#17084=CIRCLE('',#50046,0.01350000000001);
#17085=CIRCLE('',#50048,0.01350000000001);
#17086=CIRCLE('',#50049,0.01350000000001);
#17087=CIRCLE('',#50051,0.01350000000001);
#17088=CIRCLE('',#50052,0.01350000000001);
#17089=CIRCLE('',#50054,0.01350000000001);
#17090=CIRCLE('',#50055,0.01350000000001);
#17091=CIRCLE('',#50057,0.01350000000001);
#17092=CIRCLE('',#50058,0.01350000000001);
#17093=CIRCLE('',#50060,0.01350000000001);
#17094=CIRCLE('',#50061,0.01350000000001);
#17095=CIRCLE('',#50063,0.01350000000001);
#17096=CIRCLE('',#50064,0.01350000000001);
#17097=CIRCLE('',#50175,0.00800000000000999);
#17098=CIRCLE('',#50176,0.00800000000000999);
#17099=CIRCLE('',#50177,0.00800000000000999);
#17100=CIRCLE('',#50178,0.00800000000000999);
#17101=CIRCLE('',#50179,0.00800000000000999);
#17102=CIRCLE('',#50180,0.00800000000000999);
#17103=CIRCLE('',#50182,0.00212500000001);
#17104=CIRCLE('',#50183,0.00212500000001);
#17105=CIRCLE('',#50185,0.00300000000001);
#17106=CIRCLE('',#50186,0.00300000000001);
#17107=CIRCLE('',#50188,0.00500000000001);
#17108=CIRCLE('',#50189,0.00500000000001);
#17109=CIRCLE('',#50191,0.00250000000001);
#17110=CIRCLE('',#50192,0.00250000000001);
#17111=CIRCLE('',#50194,0.01012500000001);
#17112=CIRCLE('',#50195,0.01125000000001);
#17113=CIRCLE('',#50196,0.01012500000001);
#17114=CIRCLE('',#50197,0.00590000000001);
#17115=CIRCLE('',#50198,0.00590000000001);
#17116=CIRCLE('',#50200,0.01125000000001);
#17117=CIRCLE('',#50202,0.00150000000001);
#17118=CIRCLE('',#50203,0.00150000000001);
#17119=CIRCLE('',#50205,0.00360000000001);
#17120=CIRCLE('',#50206,0.00360000000001);
#17121=CIRCLE('',#50208,0.00370000000001);
#17122=CIRCLE('',#50209,0.00370000000001);
#17123=CIRCLE('',#50210,0.00370000000001);
#17124=CIRCLE('',#50212,0.00282500000001);
#17125=CIRCLE('',#50213,0.00282500000001);
#17126=CIRCLE('',#50215,0.00282500000001);
#17127=CIRCLE('',#50216,0.00282500000001);
#17128=CIRCLE('',#50218,0.00282500000001);
#17129=CIRCLE('',#50219,0.00282500000001);
#17130=CIRCLE('',#50221,0.00160000000001);
#17131=CIRCLE('',#50222,0.00160000000001);
#17132=CIRCLE('',#50224,0.00160000000001);
#17133=CIRCLE('',#50225,0.00160000000001);
#17134=CIRCLE('',#50226,0.00160000000001);
#17135=CIRCLE('',#50227,0.00160000000001);
#17136=CIRCLE('',#50229,0.00160000000001);
#17137=CIRCLE('',#50230,0.00160000000001);
#17138=CIRCLE('',#50232,0.00590000000001);
#17139=CIRCLE('',#50233,0.00590000000001);
#17140=CIRCLE('',#50235,0.01350000000001);
#17141=CIRCLE('',#50236,0.01350000000001);
#17142=CIRCLE('',#50237,0.01350000000001);
#17143=CIRCLE('',#50238,0.01350000000001);
#17144=CIRCLE('',#50241,0.01400000000001);
#17145=CIRCLE('',#50242,0.01400000000001);
#17146=CIRCLE('',#50243,0.01400000000001);
#17147=CIRCLE('',#50244,0.01400000000001);
#17148=CIRCLE('',#50246,0.01400000000001);
#17149=CIRCLE('',#50247,0.01400000000001);
#17150=CIRCLE('',#50252,0.01565000000001);
#17151=CIRCLE('',#50253,0.00650498845855181);
#17152=CIRCLE('',#50254,0.00525000000001);
#17153=CIRCLE('',#50255,0.00500000000001);
#17154=CIRCLE('',#50256,0.01565000000001);
#17155=CIRCLE('',#50257,0.01350000000001);
#17156=CIRCLE('',#50259,0.01350000000001);
#17157=CIRCLE('',#50260,0.01350000000001);
#17158=CIRCLE('',#50262,0.01400000000001);
#17159=CIRCLE('',#50267,0.00400000000001);
#17160=CIRCLE('',#50268,0.00725000000001);
#17161=CIRCLE('',#50269,0.00300000000001001);
#17162=CIRCLE('',#50270,0.00500000000001);
#17163=CIRCLE('',#50271,0.00525000000001);
#17164=CIRCLE('',#50272,0.00650498845855181);
#17165=CIRCLE('',#50273,0.00370000000001);
#17166=CIRCLE('',#50274,0.00370000000001);
#17167=CIRCLE('',#50275,0.00360000000001);
#17168=CIRCLE('',#50298,0.00300000000001001);
#17169=CIRCLE('',#50301,0.00725000000001);
#17170=CIRCLE('',#50304,0.00400000000001);
#17171=CIRCLE('',#50307,0.01400000000001);
#17172=CIRCLE('',#50313,0.00370000000001);
#17173=CIRCLE('',#50316,0.00370000000001);
#17174=CIRCLE('',#50328,0.00360000000001);
#17175=CIRCLE('',#50344,0.01565000000001);
#17176=CIRCLE('',#50348,0.01565000000001);
#17177=CIRCLE('',#50360,0.00600000000001);
#17178=CIRCLE('',#50362,0.00600000000001);
#17179=VERTEX_POINT('',#61799);
#17180=VERTEX_POINT('',#61801);
#17181=VERTEX_POINT('',#61805);
#17182=VERTEX_POINT('',#61807);
#17183=VERTEX_POINT('',#63073);
#17184=VERTEX_POINT('',#63157);
#17185=VERTEX_POINT('',#63274);
#17186=VERTEX_POINT('',#63367);
#17187=VERTEX_POINT('',#63369);
#17188=VERTEX_POINT('',#63373);
#17189=VERTEX_POINT('',#63380);
#17190=VERTEX_POINT('',#63382);
#17191=VERTEX_POINT('',#63384);
#17192=VERTEX_POINT('',#63386);
#17193=VERTEX_POINT('',#63421);
#17194=VERTEX_POINT('',#63422);
#17195=VERTEX_POINT('',#63424);
#17196=VERTEX_POINT('',#63426);
#17197=VERTEX_POINT('',#63430);
#17198=VERTEX_POINT('',#63431);
#17199=VERTEX_POINT('',#63433);
#17200=VERTEX_POINT('',#63435);
#17201=VERTEX_POINT('',#63439);
#17202=VERTEX_POINT('',#63441);
#17203=VERTEX_POINT('',#63443);
#17204=VERTEX_POINT('',#63445);
#17205=VERTEX_POINT('',#63448);
#17206=VERTEX_POINT('',#63450);
#17207=VERTEX_POINT('',#63454);
#17208=VERTEX_POINT('',#63456);
#17209=VERTEX_POINT('',#63460);
#17210=VERTEX_POINT('',#63462);
#17211=VERTEX_POINT('',#63466);
#17212=VERTEX_POINT('',#63468);
#17213=VERTEX_POINT('',#63472);
#17214=VERTEX_POINT('',#63473);
#17215=VERTEX_POINT('',#63475);
#17216=VERTEX_POINT('',#63477);
#17217=VERTEX_POINT('',#63479);
#17218=VERTEX_POINT('',#63481);
#17219=VERTEX_POINT('',#63484);
#17220=VERTEX_POINT('',#63486);
#17221=VERTEX_POINT('',#63490);
#17222=VERTEX_POINT('',#63493);
#17223=VERTEX_POINT('',#63497);
#17224=VERTEX_POINT('',#63501);
#17225=VERTEX_POINT('',#63524);
#17226=VERTEX_POINT('',#63526);
#17227=VERTEX_POINT('',#63530);
#17228=VERTEX_POINT('',#63531);
#17229=VERTEX_POINT('',#63538);
#17230=VERTEX_POINT('',#63541);
#17231=VERTEX_POINT('',#63546);
#17232=VERTEX_POINT('',#63548);
#17233=VERTEX_POINT('',#63550);
#17234=VERTEX_POINT('',#63557);
#17235=VERTEX_POINT('',#63564);
#17236=VERTEX_POINT('',#63566);
#17237=VERTEX_POINT('',#63568);
#17238=VERTEX_POINT('',#63575);
#17239=VERTEX_POINT('',#63582);
#17240=VERTEX_POINT('',#63584);
#17241=VERTEX_POINT('',#63586);
#17242=VERTEX_POINT('',#63593);
#17243=VERTEX_POINT('',#63600);
#17244=VERTEX_POINT('',#63602);
#17245=VERTEX_POINT('',#63604);
#17246=VERTEX_POINT('',#63611);
#17247=VERTEX_POINT('',#63618);
#17248=VERTEX_POINT('',#63620);
#17249=VERTEX_POINT('',#63622);
#17250=VERTEX_POINT('',#63629);
#17251=VERTEX_POINT('',#63636);
#17252=VERTEX_POINT('',#63638);
#17253=VERTEX_POINT('',#63640);
#17254=VERTEX_POINT('',#63647);
#17255=VERTEX_POINT('',#63654);
#17256=VERTEX_POINT('',#63656);
#17257=VERTEX_POINT('',#63658);
#17258=VERTEX_POINT('',#63665);
#17259=VERTEX_POINT('',#63672);
#17260=VERTEX_POINT('',#63674);
#17261=VERTEX_POINT('',#63676);
#17262=VERTEX_POINT('',#63683);
#17263=VERTEX_POINT('',#63690);
#17264=VERTEX_POINT('',#63692);
#17265=VERTEX_POINT('',#63694);
#17266=VERTEX_POINT('',#63701);
#17267=VERTEX_POINT('',#63708);
#17268=VERTEX_POINT('',#63710);
#17269=VERTEX_POINT('',#63712);
#17270=VERTEX_POINT('',#63719);
#17271=VERTEX_POINT('',#63726);
#17272=VERTEX_POINT('',#63728);
#17273=VERTEX_POINT('',#63730);
#17274=VERTEX_POINT('',#63737);
#17275=VERTEX_POINT('',#63744);
#17276=VERTEX_POINT('',#63746);
#17277=VERTEX_POINT('',#63748);
#17278=VERTEX_POINT('',#63755);
#17279=VERTEX_POINT('',#63762);
#17280=VERTEX_POINT('',#63764);
#17281=VERTEX_POINT('',#63766);
#17282=VERTEX_POINT('',#63773);
#17283=VERTEX_POINT('',#63780);
#17284=VERTEX_POINT('',#63782);
#17285=VERTEX_POINT('',#63784);
#17286=VERTEX_POINT('',#63791);
#17287=VERTEX_POINT('',#63798);
#17288=VERTEX_POINT('',#63800);
#17289=VERTEX_POINT('',#63802);
#17290=VERTEX_POINT('',#63809);
#17291=VERTEX_POINT('',#63816);
#17292=VERTEX_POINT('',#63818);
#17293=VERTEX_POINT('',#63820);
#17294=VERTEX_POINT('',#63827);
#17295=VERTEX_POINT('',#63834);
#17296=VERTEX_POINT('',#63836);
#17297=VERTEX_POINT('',#63838);
#17298=VERTEX_POINT('',#63845);
#17299=VERTEX_POINT('',#63852);
#17300=VERTEX_POINT('',#63854);
#17301=VERTEX_POINT('',#63856);
#17302=VERTEX_POINT('',#63863);
#17303=VERTEX_POINT('',#63870);
#17304=VERTEX_POINT('',#63872);
#17305=VERTEX_POINT('',#63874);
#17306=VERTEX_POINT('',#63881);
#17307=VERTEX_POINT('',#63888);
#17308=VERTEX_POINT('',#63890);
#17309=VERTEX_POINT('',#63892);
#17310=VERTEX_POINT('',#63899);
#17311=VERTEX_POINT('',#63906);
#17312=VERTEX_POINT('',#63908);
#17313=VERTEX_POINT('',#63910);
#17314=VERTEX_POINT('',#63917);
#17315=VERTEX_POINT('',#63924);
#17316=VERTEX_POINT('',#63926);
#17317=VERTEX_POINT('',#63928);
#17318=VERTEX_POINT('',#63935);
#17319=VERTEX_POINT('',#63942);
#17320=VERTEX_POINT('',#63944);
#17321=VERTEX_POINT('',#63946);
#17322=VERTEX_POINT('',#63953);
#17323=VERTEX_POINT('',#63960);
#17324=VERTEX_POINT('',#63962);
#17325=VERTEX_POINT('',#63964);
#17326=VERTEX_POINT('',#63971);
#17327=VERTEX_POINT('',#63978);
#17328=VERTEX_POINT('',#63980);
#17329=VERTEX_POINT('',#63982);
#17330=VERTEX_POINT('',#63989);
#17331=VERTEX_POINT('',#63996);
#17332=VERTEX_POINT('',#63998);
#17333=VERTEX_POINT('',#64000);
#17334=VERTEX_POINT('',#64007);
#17335=VERTEX_POINT('',#64014);
#17336=VERTEX_POINT('',#64016);
#17337=VERTEX_POINT('',#64018);
#17338=VERTEX_POINT('',#64025);
#17339=VERTEX_POINT('',#64032);
#17340=VERTEX_POINT('',#64034);
#17341=VERTEX_POINT('',#64036);
#17342=VERTEX_POINT('',#64043);
#17343=VERTEX_POINT('',#64050);
#17344=VERTEX_POINT('',#64052);
#17345=VERTEX_POINT('',#64054);
#17346=VERTEX_POINT('',#64061);
#17347=VERTEX_POINT('',#64068);
#17348=VERTEX_POINT('',#64070);
#17349=VERTEX_POINT('',#64072);
#17350=VERTEX_POINT('',#64079);
#17351=VERTEX_POINT('',#64086);
#17352=VERTEX_POINT('',#64088);
#17353=VERTEX_POINT('',#64090);
#17354=VERTEX_POINT('',#64097);
#17355=VERTEX_POINT('',#64104);
#17356=VERTEX_POINT('',#64106);
#17357=VERTEX_POINT('',#64108);
#17358=VERTEX_POINT('',#64115);
#17359=VERTEX_POINT('',#64122);
#17360=VERTEX_POINT('',#64124);
#17361=VERTEX_POINT('',#64126);
#17362=VERTEX_POINT('',#64133);
#17363=VERTEX_POINT('',#64140);
#17364=VERTEX_POINT('',#64142);
#17365=VERTEX_POINT('',#64144);
#17366=VERTEX_POINT('',#64151);
#17367=VERTEX_POINT('',#64158);
#17368=VERTEX_POINT('',#64160);
#17369=VERTEX_POINT('',#64162);
#17370=VERTEX_POINT('',#64169);
#17371=VERTEX_POINT('',#64176);
#17372=VERTEX_POINT('',#64178);
#17373=VERTEX_POINT('',#64180);
#17374=VERTEX_POINT('',#64187);
#17375=VERTEX_POINT('',#64194);
#17376=VERTEX_POINT('',#64196);
#17377=VERTEX_POINT('',#64198);
#17378=VERTEX_POINT('',#64205);
#17379=VERTEX_POINT('',#64212);
#17380=VERTEX_POINT('',#64214);
#17381=VERTEX_POINT('',#64216);
#17382=VERTEX_POINT('',#64223);
#17383=VERTEX_POINT('',#64230);
#17384=VERTEX_POINT('',#64232);
#17385=VERTEX_POINT('',#64234);
#17386=VERTEX_POINT('',#64241);
#17387=VERTEX_POINT('',#64248);
#17388=VERTEX_POINT('',#64250);
#17389=VERTEX_POINT('',#64252);
#17390=VERTEX_POINT('',#64259);
#17391=VERTEX_POINT('',#64266);
#17392=VERTEX_POINT('',#64268);
#17393=VERTEX_POINT('',#64270);
#17394=VERTEX_POINT('',#64277);
#17395=VERTEX_POINT('',#64284);
#17396=VERTEX_POINT('',#64286);
#17397=VERTEX_POINT('',#64288);
#17398=VERTEX_POINT('',#64295);
#17399=VERTEX_POINT('',#64302);
#17400=VERTEX_POINT('',#64304);
#17401=VERTEX_POINT('',#64306);
#17402=VERTEX_POINT('',#64313);
#17403=VERTEX_POINT('',#64320);
#17404=VERTEX_POINT('',#64322);
#17405=VERTEX_POINT('',#64324);
#17406=VERTEX_POINT('',#64331);
#17407=VERTEX_POINT('',#64338);
#17408=VERTEX_POINT('',#64340);
#17409=VERTEX_POINT('',#64342);
#17410=VERTEX_POINT('',#64349);
#17411=VERTEX_POINT('',#64356);
#17412=VERTEX_POINT('',#64358);
#17413=VERTEX_POINT('',#64360);
#17414=VERTEX_POINT('',#64367);
#17415=VERTEX_POINT('',#64374);
#17416=VERTEX_POINT('',#64376);
#17417=VERTEX_POINT('',#64378);
#17418=VERTEX_POINT('',#64385);
#17419=VERTEX_POINT('',#64392);
#17420=VERTEX_POINT('',#64394);
#17421=VERTEX_POINT('',#64396);
#17422=VERTEX_POINT('',#64403);
#17423=VERTEX_POINT('',#64410);
#17424=VERTEX_POINT('',#64412);
#17425=VERTEX_POINT('',#64414);
#17426=VERTEX_POINT('',#64421);
#17427=VERTEX_POINT('',#64428);
#17428=VERTEX_POINT('',#64430);
#17429=VERTEX_POINT('',#64439);
#17430=VERTEX_POINT('',#64440);
#17431=VERTEX_POINT('',#64445);
#17432=VERTEX_POINT('',#64448);
#17433=VERTEX_POINT('',#64455);
#17434=VERTEX_POINT('',#64457);
#17435=VERTEX_POINT('',#64459);
#17436=VERTEX_POINT('',#64461);
#17437=VERTEX_POINT('',#64463);
#17438=VERTEX_POINT('',#64468);
#17439=VERTEX_POINT('',#64470);
#17440=VERTEX_POINT('',#64472);
#17441=VERTEX_POINT('',#64474);
#17442=VERTEX_POINT('',#64476);
#17443=VERTEX_POINT('',#64478);
#17444=VERTEX_POINT('',#64483);
#17445=VERTEX_POINT('',#64485);
#17446=VERTEX_POINT('',#64487);
#17447=VERTEX_POINT('',#64489);
#17448=VERTEX_POINT('',#64491);
#17449=VERTEX_POINT('',#64493);
#17450=VERTEX_POINT('',#64498);
#17451=VERTEX_POINT('',#64500);
#17452=VERTEX_POINT('',#64502);
#17453=VERTEX_POINT('',#64504);
#17454=VERTEX_POINT('',#64506);
#17455=VERTEX_POINT('',#64508);
#17456=VERTEX_POINT('',#64513);
#17457=VERTEX_POINT('',#64515);
#17458=VERTEX_POINT('',#64517);
#17459=VERTEX_POINT('',#64519);
#17460=VERTEX_POINT('',#64521);
#17461=VERTEX_POINT('',#64523);
#17462=VERTEX_POINT('',#64528);
#17463=VERTEX_POINT('',#64530);
#17464=VERTEX_POINT('',#64532);
#17465=VERTEX_POINT('',#64534);
#17466=VERTEX_POINT('',#64536);
#17467=VERTEX_POINT('',#64538);
#17468=VERTEX_POINT('',#64543);
#17469=VERTEX_POINT('',#64545);
#17470=VERTEX_POINT('',#64547);
#17471=VERTEX_POINT('',#64549);
#17472=VERTEX_POINT('',#64551);
#17473=VERTEX_POINT('',#64553);
#17474=VERTEX_POINT('',#64558);
#17475=VERTEX_POINT('',#64560);
#17476=VERTEX_POINT('',#64562);
#17477=VERTEX_POINT('',#64564);
#17478=VERTEX_POINT('',#64566);
#17479=VERTEX_POINT('',#64568);
#17480=VERTEX_POINT('',#64573);
#17481=VERTEX_POINT('',#64575);
#17482=VERTEX_POINT('',#64577);
#17483=VERTEX_POINT('',#64579);
#17484=VERTEX_POINT('',#64581);
#17485=VERTEX_POINT('',#64583);
#17486=VERTEX_POINT('',#64588);
#17487=VERTEX_POINT('',#64590);
#17488=VERTEX_POINT('',#64592);
#17489=VERTEX_POINT('',#64594);
#17490=VERTEX_POINT('',#64596);
#17491=VERTEX_POINT('',#64598);
#17492=VERTEX_POINT('',#64603);
#17493=VERTEX_POINT('',#64605);
#17494=VERTEX_POINT('',#64607);
#17495=VERTEX_POINT('',#64609);
#17496=VERTEX_POINT('',#64611);
#17497=VERTEX_POINT('',#64613);
#17498=VERTEX_POINT('',#64618);
#17499=VERTEX_POINT('',#64620);
#17500=VERTEX_POINT('',#64622);
#17501=VERTEX_POINT('',#64624);
#17502=VERTEX_POINT('',#64626);
#17503=VERTEX_POINT('',#64628);
#17504=VERTEX_POINT('',#64633);
#17505=VERTEX_POINT('',#64635);
#17506=VERTEX_POINT('',#64637);
#17507=VERTEX_POINT('',#64639);
#17508=VERTEX_POINT('',#64641);
#17509=VERTEX_POINT('',#64643);
#17510=VERTEX_POINT('',#64648);
#17511=VERTEX_POINT('',#64650);
#17512=VERTEX_POINT('',#64652);
#17513=VERTEX_POINT('',#64654);
#17514=VERTEX_POINT('',#64656);
#17515=VERTEX_POINT('',#64658);
#17516=VERTEX_POINT('',#64663);
#17517=VERTEX_POINT('',#64665);
#17518=VERTEX_POINT('',#64667);
#17519=VERTEX_POINT('',#64669);
#17520=VERTEX_POINT('',#64671);
#17521=VERTEX_POINT('',#64673);
#17522=VERTEX_POINT('',#64678);
#17523=VERTEX_POINT('',#64680);
#17524=VERTEX_POINT('',#64682);
#17525=VERTEX_POINT('',#64684);
#17526=VERTEX_POINT('',#64686);
#17527=VERTEX_POINT('',#64688);
#17528=VERTEX_POINT('',#64693);
#17529=VERTEX_POINT('',#64695);
#17530=VERTEX_POINT('',#64697);
#17531=VERTEX_POINT('',#64699);
#17532=VERTEX_POINT('',#64701);
#17533=VERTEX_POINT('',#64703);
#17534=VERTEX_POINT('',#64708);
#17535=VERTEX_POINT('',#64710);
#17536=VERTEX_POINT('',#64712);
#17537=VERTEX_POINT('',#64714);
#17538=VERTEX_POINT('',#64716);
#17539=VERTEX_POINT('',#64718);
#17540=VERTEX_POINT('',#64723);
#17541=VERTEX_POINT('',#64725);
#17542=VERTEX_POINT('',#64727);
#17543=VERTEX_POINT('',#64729);
#17544=VERTEX_POINT('',#64731);
#17545=VERTEX_POINT('',#64733);
#17546=VERTEX_POINT('',#64738);
#17547=VERTEX_POINT('',#64740);
#17548=VERTEX_POINT('',#64742);
#17549=VERTEX_POINT('',#64744);
#17550=VERTEX_POINT('',#64746);
#17551=VERTEX_POINT('',#64748);
#17552=VERTEX_POINT('',#64753);
#17553=VERTEX_POINT('',#64755);
#17554=VERTEX_POINT('',#64757);
#17555=VERTEX_POINT('',#64759);
#17556=VERTEX_POINT('',#64761);
#17557=VERTEX_POINT('',#64763);
#17558=VERTEX_POINT('',#64768);
#17559=VERTEX_POINT('',#64770);
#17560=VERTEX_POINT('',#64772);
#17561=VERTEX_POINT('',#64774);
#17562=VERTEX_POINT('',#64776);
#17563=VERTEX_POINT('',#64778);
#17564=VERTEX_POINT('',#64783);
#17565=VERTEX_POINT('',#64785);
#17566=VERTEX_POINT('',#64787);
#17567=VERTEX_POINT('',#64789);
#17568=VERTEX_POINT('',#64791);
#17569=VERTEX_POINT('',#64793);
#17570=VERTEX_POINT('',#64798);
#17571=VERTEX_POINT('',#64800);
#17572=VERTEX_POINT('',#64802);
#17573=VERTEX_POINT('',#64804);
#17574=VERTEX_POINT('',#64806);
#17575=VERTEX_POINT('',#64808);
#17576=VERTEX_POINT('',#64813);
#17577=VERTEX_POINT('',#64815);
#17578=VERTEX_POINT('',#64817);
#17579=VERTEX_POINT('',#64819);
#17580=VERTEX_POINT('',#64821);
#17581=VERTEX_POINT('',#64823);
#17582=VERTEX_POINT('',#64828);
#17583=VERTEX_POINT('',#64830);
#17584=VERTEX_POINT('',#64832);
#17585=VERTEX_POINT('',#64834);
#17586=VERTEX_POINT('',#64836);
#17587=VERTEX_POINT('',#64838);
#17588=VERTEX_POINT('',#64843);
#17589=VERTEX_POINT('',#64845);
#17590=VERTEX_POINT('',#64847);
#17591=VERTEX_POINT('',#64849);
#17592=VERTEX_POINT('',#64851);
#17593=VERTEX_POINT('',#64853);
#17594=VERTEX_POINT('',#64858);
#17595=VERTEX_POINT('',#64860);
#17596=VERTEX_POINT('',#64862);
#17597=VERTEX_POINT('',#64864);
#17598=VERTEX_POINT('',#64866);
#17599=VERTEX_POINT('',#64868);
#17600=VERTEX_POINT('',#64873);
#17601=VERTEX_POINT('',#64875);
#17602=VERTEX_POINT('',#64877);
#17603=VERTEX_POINT('',#64879);
#17604=VERTEX_POINT('',#64881);
#17605=VERTEX_POINT('',#64883);
#17606=VERTEX_POINT('',#64888);
#17607=VERTEX_POINT('',#64890);
#17608=VERTEX_POINT('',#64892);
#17609=VERTEX_POINT('',#64894);
#17610=VERTEX_POINT('',#64896);
#17611=VERTEX_POINT('',#64898);
#17612=VERTEX_POINT('',#64903);
#17613=VERTEX_POINT('',#64905);
#17614=VERTEX_POINT('',#64907);
#17615=VERTEX_POINT('',#64909);
#17616=VERTEX_POINT('',#64911);
#17617=VERTEX_POINT('',#64913);
#17618=VERTEX_POINT('',#64918);
#17619=VERTEX_POINT('',#64920);
#17620=VERTEX_POINT('',#64922);
#17621=VERTEX_POINT('',#64924);
#17622=VERTEX_POINT('',#64926);
#17623=VERTEX_POINT('',#64928);
#17624=VERTEX_POINT('',#64933);
#17625=VERTEX_POINT('',#64935);
#17626=VERTEX_POINT('',#64937);
#17627=VERTEX_POINT('',#64939);
#17628=VERTEX_POINT('',#64941);
#17629=VERTEX_POINT('',#64943);
#17630=VERTEX_POINT('',#64948);
#17631=VERTEX_POINT('',#64950);
#17632=VERTEX_POINT('',#64952);
#17633=VERTEX_POINT('',#64954);
#17634=VERTEX_POINT('',#64956);
#17635=VERTEX_POINT('',#64958);
#17636=VERTEX_POINT('',#64963);
#17637=VERTEX_POINT('',#64965);
#17638=VERTEX_POINT('',#64967);
#17639=VERTEX_POINT('',#64969);
#17640=VERTEX_POINT('',#64971);
#17641=VERTEX_POINT('',#64973);
#17642=VERTEX_POINT('',#64978);
#17643=VERTEX_POINT('',#64980);
#17644=VERTEX_POINT('',#64982);
#17645=VERTEX_POINT('',#64984);
#17646=VERTEX_POINT('',#64986);
#17647=VERTEX_POINT('',#64988);
#17648=VERTEX_POINT('',#64993);
#17649=VERTEX_POINT('',#64995);
#17650=VERTEX_POINT('',#64997);
#17651=VERTEX_POINT('',#64999);
#17652=VERTEX_POINT('',#65001);
#17653=VERTEX_POINT('',#65003);
#17654=VERTEX_POINT('',#65008);
#17655=VERTEX_POINT('',#65010);
#17656=VERTEX_POINT('',#65012);
#17657=VERTEX_POINT('',#65014);
#17658=VERTEX_POINT('',#65016);
#17659=VERTEX_POINT('',#65018);
#17660=VERTEX_POINT('',#65023);
#17661=VERTEX_POINT('',#65025);
#17662=VERTEX_POINT('',#65027);
#17663=VERTEX_POINT('',#65029);
#17664=VERTEX_POINT('',#65031);
#17665=VERTEX_POINT('',#65033);
#17666=VERTEX_POINT('',#65038);
#17667=VERTEX_POINT('',#65040);
#17668=VERTEX_POINT('',#65042);
#17669=VERTEX_POINT('',#65044);
#17670=VERTEX_POINT('',#65046);
#17671=VERTEX_POINT('',#65048);
#17672=VERTEX_POINT('',#65053);
#17673=VERTEX_POINT('',#65055);
#17674=VERTEX_POINT('',#65057);
#17675=VERTEX_POINT('',#65059);
#17676=VERTEX_POINT('',#65061);
#17677=VERTEX_POINT('',#65063);
#17678=VERTEX_POINT('',#65068);
#17679=VERTEX_POINT('',#65070);
#17680=VERTEX_POINT('',#65072);
#17681=VERTEX_POINT('',#65074);
#17682=VERTEX_POINT('',#65076);
#17683=VERTEX_POINT('',#65078);
#17684=VERTEX_POINT('',#65083);
#17685=VERTEX_POINT('',#65085);
#17686=VERTEX_POINT('',#65087);
#17687=VERTEX_POINT('',#65089);
#17688=VERTEX_POINT('',#65091);
#17689=VERTEX_POINT('',#65093);
#17690=VERTEX_POINT('',#65098);
#17691=VERTEX_POINT('',#65100);
#17692=VERTEX_POINT('',#65102);
#17693=VERTEX_POINT('',#65104);
#17694=VERTEX_POINT('',#65106);
#17695=VERTEX_POINT('',#65108);
#17696=VERTEX_POINT('',#65113);
#17697=VERTEX_POINT('',#65115);
#17698=VERTEX_POINT('',#65117);
#17699=VERTEX_POINT('',#65119);
#17700=VERTEX_POINT('',#65121);
#17701=VERTEX_POINT('',#65123);
#17702=VERTEX_POINT('',#65128);
#17703=VERTEX_POINT('',#65130);
#17704=VERTEX_POINT('',#65132);
#17705=VERTEX_POINT('',#65134);
#17706=VERTEX_POINT('',#65136);
#17707=VERTEX_POINT('',#65138);
#17708=VERTEX_POINT('',#65143);
#17709=VERTEX_POINT('',#65145);
#17710=VERTEX_POINT('',#65147);
#17711=VERTEX_POINT('',#65149);
#17712=VERTEX_POINT('',#65151);
#17713=VERTEX_POINT('',#65153);
#17714=VERTEX_POINT('',#65158);
#17715=VERTEX_POINT('',#65160);
#17716=VERTEX_POINT('',#65162);
#17717=VERTEX_POINT('',#65164);
#17718=VERTEX_POINT('',#65166);
#17719=VERTEX_POINT('',#65168);
#17720=VERTEX_POINT('',#65173);
#17721=VERTEX_POINT('',#65175);
#17722=VERTEX_POINT('',#65177);
#17723=VERTEX_POINT('',#65179);
#17724=VERTEX_POINT('',#65181);
#17725=VERTEX_POINT('',#65183);
#17726=VERTEX_POINT('',#65188);
#17727=VERTEX_POINT('',#65190);
#17728=VERTEX_POINT('',#65192);
#17729=VERTEX_POINT('',#65194);
#17730=VERTEX_POINT('',#65196);
#17731=VERTEX_POINT('',#65218);
#17732=VERTEX_POINT('',#65219);
#17733=VERTEX_POINT('',#65222);
#17734=VERTEX_POINT('',#65230);
#17735=VERTEX_POINT('',#65249);
#17736=VERTEX_POINT('',#65250);
#17737=VERTEX_POINT('',#65265);
#17738=VERTEX_POINT('',#65266);
#17739=VERTEX_POINT('',#65268);
#17740=VERTEX_POINT('',#65270);
#17741=VERTEX_POINT('',#65272);
#17742=VERTEX_POINT('',#65274);
#17743=VERTEX_POINT('',#65286);
#17744=VERTEX_POINT('',#65295);
#17745=VERTEX_POINT('',#65297);
#17746=VERTEX_POINT('',#65316);
#17747=VERTEX_POINT('',#65317);
#17748=VERTEX_POINT('',#65342);
#17749=VERTEX_POINT('',#65344);
#17750=VERTEX_POINT('',#65353);
#17751=VERTEX_POINT('',#65354);
#17752=VERTEX_POINT('',#65384);
#17753=VERTEX_POINT('',#65385);
#17754=VERTEX_POINT('',#65390);
#17755=VERTEX_POINT('',#65392);
#17756=VERTEX_POINT('',#65404);
#17757=VERTEX_POINT('',#65405);
#17758=VERTEX_POINT('',#65407);
#17759=VERTEX_POINT('',#65409);
#17760=VERTEX_POINT('',#65411);
#17761=VERTEX_POINT('',#65413);
#17762=VERTEX_POINT('',#65425);
#17763=VERTEX_POINT('',#65426);
#17764=VERTEX_POINT('',#65429);
#17765=VERTEX_POINT('',#65431);
#17766=VERTEX_POINT('',#65433);
#17767=VERTEX_POINT('',#65491);
#17768=VERTEX_POINT('',#65492);
#17769=VERTEX_POINT('',#65510);
#17770=VERTEX_POINT('',#65512);
#17771=VERTEX_POINT('',#65521);
#17772=VERTEX_POINT('',#65522);
#17773=VERTEX_POINT('',#65527);
#17774=VERTEX_POINT('',#65529);
#17775=VERTEX_POINT('',#65547);
#17776=VERTEX_POINT('',#65548);
#17777=VERTEX_POINT('',#65556);
#17778=VERTEX_POINT('',#65565);
#17779=VERTEX_POINT('',#65567);
#17780=VERTEX_POINT('',#65569);
#17781=VERTEX_POINT('',#65578);
#17782=VERTEX_POINT('',#65579);
#17783=VERTEX_POINT('',#65582);
#17784=VERTEX_POINT('',#65584);
#17785=VERTEX_POINT('',#65586);
#17786=VERTEX_POINT('',#65650);
#17787=VERTEX_POINT('',#65651);
#17788=VERTEX_POINT('',#65674);
#17789=VERTEX_POINT('',#65676);
#17790=VERTEX_POINT('',#65685);
#17791=VERTEX_POINT('',#65686);
#17792=VERTEX_POINT('',#65696);
#17793=VERTEX_POINT('',#65698);
#17794=VERTEX_POINT('',#65707);
#17795=VERTEX_POINT('',#65708);
#17796=VERTEX_POINT('',#65710);
#17797=VERTEX_POINT('',#65712);
#17798=VERTEX_POINT('',#65714);
#17799=VERTEX_POINT('',#65716);
#17800=VERTEX_POINT('',#65734);
#17801=VERTEX_POINT('',#65735);
#17802=VERTEX_POINT('',#65738);
#17803=VERTEX_POINT('',#65740);
#17804=VERTEX_POINT('',#65748);
#17805=VERTEX_POINT('',#65820);
#17806=VERTEX_POINT('',#65821);
#17807=VERTEX_POINT('',#65840);
#17808=VERTEX_POINT('',#65842);
#17809=VERTEX_POINT('',#65856);
#17810=VERTEX_POINT('',#65857);
#17811=VERTEX_POINT('',#65862);
#17812=VERTEX_POINT('',#65864);
#17813=VERTEX_POINT('',#65888);
#17814=VERTEX_POINT('',#65889);
#17815=VERTEX_POINT('',#65891);
#17816=VERTEX_POINT('',#65893);
#17817=VERTEX_POINT('',#65895);
#17818=VERTEX_POINT('',#65897);
#17819=VERTEX_POINT('',#65909);
#17820=VERTEX_POINT('',#65910);
#17821=VERTEX_POINT('',#65913);
#17822=VERTEX_POINT('',#65915);
#17823=VERTEX_POINT('',#65917);
#17824=VERTEX_POINT('',#65982);
#17825=VERTEX_POINT('',#65983);
#17826=VERTEX_POINT('',#66008);
#17827=VERTEX_POINT('',#66010);
#17828=VERTEX_POINT('',#66019);
#17829=VERTEX_POINT('',#66020);
#17830=VERTEX_POINT('',#66025);
#17831=VERTEX_POINT('',#66027);
#17832=VERTEX_POINT('',#66039);
#17833=VERTEX_POINT('',#66040);
#17834=VERTEX_POINT('',#66042);
#17835=VERTEX_POINT('',#66044);
#17836=VERTEX_POINT('',#66046);
#17837=VERTEX_POINT('',#66048);
#17838=VERTEX_POINT('',#66067);
#17839=VERTEX_POINT('',#66068);
#17840=VERTEX_POINT('',#66071);
#17841=VERTEX_POINT('',#66073);
#17842=VERTEX_POINT('',#66075);
#17843=VERTEX_POINT('',#66158);
#17844=VERTEX_POINT('',#66160);
#17845=VERTEX_POINT('',#66169);
#17846=VERTEX_POINT('',#66171);
#17847=VERTEX_POINT('',#66175);
#17848=VERTEX_POINT('',#66177);
#17849=VERTEX_POINT('',#66189);
#17850=VERTEX_POINT('',#66190);
#17851=VERTEX_POINT('',#66193);
#17852=VERTEX_POINT('',#66195);
#17853=VERTEX_POINT('',#66197);
#17854=VERTEX_POINT('',#66259);
#17855=VERTEX_POINT('',#66260);
#17856=VERTEX_POINT('',#66263);
#17857=VERTEX_POINT('',#66271);
#17858=VERTEX_POINT('',#66290);
#17859=VERTEX_POINT('',#66291);
#17860=VERTEX_POINT('',#66301);
#17861=VERTEX_POINT('',#66302);
#17862=VERTEX_POINT('',#66312);
#17863=VERTEX_POINT('',#66313);
#17864=VERTEX_POINT('',#66316);
#17865=VERTEX_POINT('',#66318);
#17866=VERTEX_POINT('',#66320);
#17867=VERTEX_POINT('',#66364);
#17868=VERTEX_POINT('',#66365);
#17869=VERTEX_POINT('',#66383);
#17870=VERTEX_POINT('',#66384);
#17871=VERTEX_POINT('',#66387);
#17872=VERTEX_POINT('',#66389);
#17873=VERTEX_POINT('',#66391);
#17874=VERTEX_POINT('',#66403);
#17875=VERTEX_POINT('',#66404);
#17876=VERTEX_POINT('',#66414);
#17877=VERTEX_POINT('',#66415);
#17878=VERTEX_POINT('',#66443);
#17879=VERTEX_POINT('',#66444);
#17880=VERTEX_POINT('',#66463);
#17881=VERTEX_POINT('',#66464);
#17882=VERTEX_POINT('',#66480);
#17883=VERTEX_POINT('',#66482);
#17884=VERTEX_POINT('',#66484);
#17885=VERTEX_POINT('',#66525);
#17886=VERTEX_POINT('',#66526);
#17887=VERTEX_POINT('',#66541);
#17888=VERTEX_POINT('',#66542);
#17889=VERTEX_POINT('',#66557);
#17890=VERTEX_POINT('',#66558);
#17891=VERTEX_POINT('',#66561);
#17892=VERTEX_POINT('',#66563);
#17893=VERTEX_POINT('',#66565);
#17894=VERTEX_POINT('',#66600);
#17895=VERTEX_POINT('',#66601);
#17896=VERTEX_POINT('',#66611);
#17897=VERTEX_POINT('',#66612);
#17898=VERTEX_POINT('',#66632);
#17899=VERTEX_POINT('',#66633);
#17900=VERTEX_POINT('',#66636);
#17901=VERTEX_POINT('',#66638);
#17902=VERTEX_POINT('',#66640);
#17903=VERTEX_POINT('',#66682);
#17904=VERTEX_POINT('',#66683);
#17905=VERTEX_POINT('',#66693);
#17906=VERTEX_POINT('',#66694);
#17907=VERTEX_POINT('',#66710);
#17908=VERTEX_POINT('',#66711);
#17909=VERTEX_POINT('',#66714);
#17910=VERTEX_POINT('',#66716);
#17911=VERTEX_POINT('',#66718);
#17912=VERTEX_POINT('',#66764);
#17913=VERTEX_POINT('',#66785);
#17914=VERTEX_POINT('',#66786);
#17915=VERTEX_POINT('',#66789);
#17916=VERTEX_POINT('',#66797);
#17917=VERTEX_POINT('',#66816);
#17918=VERTEX_POINT('',#66817);
#17919=VERTEX_POINT('',#66827);
#17920=VERTEX_POINT('',#66828);
#17921=VERTEX_POINT('',#66838);
#17922=VERTEX_POINT('',#66839);
#17923=VERTEX_POINT('',#66842);
#17924=VERTEX_POINT('',#66844);
#17925=VERTEX_POINT('',#66846);
#17926=VERTEX_POINT('',#66890);
#17927=VERTEX_POINT('',#66891);
#17928=VERTEX_POINT('',#66901);
#17929=VERTEX_POINT('',#66902);
#17930=VERTEX_POINT('',#66915);
#17931=VERTEX_POINT('',#66916);
#17932=VERTEX_POINT('',#66919);
#17933=VERTEX_POINT('',#66921);
#17934=VERTEX_POINT('',#66923);
#17935=VERTEX_POINT('',#66958);
#17936=VERTEX_POINT('',#66959);
#17937=VERTEX_POINT('',#66983);
#17938=VERTEX_POINT('',#66984);
#17939=VERTEX_POINT('',#67000);
#17940=VERTEX_POINT('',#67002);
#17941=VERTEX_POINT('',#67004);
#17942=VERTEX_POINT('',#67022);
#17943=VERTEX_POINT('',#67023);
#17944=VERTEX_POINT('',#67038);
#17945=VERTEX_POINT('',#67039);
#17946=VERTEX_POINT('',#67067);
#17947=VERTEX_POINT('',#67068);
#17948=VERTEX_POINT('',#67086);
#17949=VERTEX_POINT('',#67087);
#17950=VERTEX_POINT('',#67090);
#17951=VERTEX_POINT('',#67092);
#17952=VERTEX_POINT('',#67094);
#17953=VERTEX_POINT('',#67129);
#17954=VERTEX_POINT('',#67130);
#17955=VERTEX_POINT('',#67140);
#17956=VERTEX_POINT('',#67141);
#17957=VERTEX_POINT('',#67161);
#17958=VERTEX_POINT('',#67162);
#17959=VERTEX_POINT('',#67165);
#17960=VERTEX_POINT('',#67167);
#17961=VERTEX_POINT('',#67169);
#17962=VERTEX_POINT('',#67204);
#17963=VERTEX_POINT('',#67205);
#17964=VERTEX_POINT('',#67215);
#17965=VERTEX_POINT('',#67216);
#17966=VERTEX_POINT('',#67232);
#17967=VERTEX_POINT('',#67233);
#17968=VERTEX_POINT('',#67236);
#17969=VERTEX_POINT('',#67238);
#17970=VERTEX_POINT('',#67240);
#17971=VERTEX_POINT('',#67286);
#17972=VERTEX_POINT('',#67307);
#17973=VERTEX_POINT('',#67308);
#17974=VERTEX_POINT('',#67311);
#17975=VERTEX_POINT('',#67319);
#17976=VERTEX_POINT('',#67338);
#17977=VERTEX_POINT('',#67339);
#17978=VERTEX_POINT('',#67349);
#17979=VERTEX_POINT('',#67350);
#17980=VERTEX_POINT('',#67360);
#17981=VERTEX_POINT('',#67361);
#17982=VERTEX_POINT('',#67364);
#17983=VERTEX_POINT('',#67366);
#17984=VERTEX_POINT('',#67368);
#17985=VERTEX_POINT('',#67412);
#17986=VERTEX_POINT('',#67413);
#17987=VERTEX_POINT('',#67423);
#17988=VERTEX_POINT('',#67424);
#17989=VERTEX_POINT('',#67437);
#17990=VERTEX_POINT('',#67438);
#17991=VERTEX_POINT('',#67441);
#17992=VERTEX_POINT('',#67443);
#17993=VERTEX_POINT('',#67445);
#17994=VERTEX_POINT('',#67480);
#17995=VERTEX_POINT('',#67481);
#17996=VERTEX_POINT('',#67491);
#17997=VERTEX_POINT('',#67492);
#17998=VERTEX_POINT('',#67511);
#17999=VERTEX_POINT('',#67512);
#18000=VERTEX_POINT('',#67528);
#18001=VERTEX_POINT('',#67530);
#18002=VERTEX_POINT('',#67532);
#18003=VERTEX_POINT('',#67573);
#18004=VERTEX_POINT('',#67574);
#18005=VERTEX_POINT('',#67597);
#18006=VERTEX_POINT('',#67598);
#18007=VERTEX_POINT('',#67601);
#18008=VERTEX_POINT('',#67603);
#18009=VERTEX_POINT('',#67605);
#18010=VERTEX_POINT('',#67617);
#18011=VERTEX_POINT('',#67618);
#18012=VERTEX_POINT('',#67628);
#18013=VERTEX_POINT('',#67629);
#18014=VERTEX_POINT('',#67662);
#18015=VERTEX_POINT('',#67663);
#18016=VERTEX_POINT('',#67683);
#18017=VERTEX_POINT('',#67684);
#18018=VERTEX_POINT('',#67687);
#18019=VERTEX_POINT('',#67689);
#18020=VERTEX_POINT('',#67691);
#18021=VERTEX_POINT('',#67726);
#18022=VERTEX_POINT('',#67727);
#18023=VERTEX_POINT('',#67737);
#18024=VERTEX_POINT('',#67738);
#18025=VERTEX_POINT('',#67751);
#18026=VERTEX_POINT('',#67752);
#18027=VERTEX_POINT('',#67755);
#18028=VERTEX_POINT('',#67757);
#18029=VERTEX_POINT('',#67759);
#18030=VERTEX_POINT('',#67798);
#18031=VERTEX_POINT('',#67819);
#18032=VERTEX_POINT('',#67820);
#18033=VERTEX_POINT('',#67823);
#18034=VERTEX_POINT('',#67831);
#18035=VERTEX_POINT('',#67850);
#18036=VERTEX_POINT('',#67851);
#18037=VERTEX_POINT('',#67861);
#18038=VERTEX_POINT('',#67862);
#18039=VERTEX_POINT('',#67872);
#18040=VERTEX_POINT('',#67873);
#18041=VERTEX_POINT('',#67876);
#18042=VERTEX_POINT('',#67878);
#18043=VERTEX_POINT('',#67880);
#18044=VERTEX_POINT('',#67924);
#18045=VERTEX_POINT('',#67925);
#18046=VERTEX_POINT('',#67935);
#18047=VERTEX_POINT('',#67936);
#18048=VERTEX_POINT('',#67949);
#18049=VERTEX_POINT('',#67950);
#18050=VERTEX_POINT('',#67953);
#18051=VERTEX_POINT('',#67955);
#18052=VERTEX_POINT('',#67957);
#18053=VERTEX_POINT('',#67992);
#18054=VERTEX_POINT('',#67993);
#18055=VERTEX_POINT('',#68003);
#18056=VERTEX_POINT('',#68004);
#18057=VERTEX_POINT('',#68023);
#18058=VERTEX_POINT('',#68024);
#18059=VERTEX_POINT('',#68040);
#18060=VERTEX_POINT('',#68042);
#18061=VERTEX_POINT('',#68044);
#18062=VERTEX_POINT('',#68085);
#18063=VERTEX_POINT('',#68086);
#18064=VERTEX_POINT('',#68101);
#18065=VERTEX_POINT('',#68102);
#18066=VERTEX_POINT('',#68120);
#18067=VERTEX_POINT('',#68121);
#18068=VERTEX_POINT('',#68124);
#18069=VERTEX_POINT('',#68126);
#18070=VERTEX_POINT('',#68128);
#18071=VERTEX_POINT('',#68163);
#18072=VERTEX_POINT('',#68164);
#18073=VERTEX_POINT('',#68189);
#18074=VERTEX_POINT('',#68190);
#18075=VERTEX_POINT('',#68193);
#18076=VERTEX_POINT('',#68195);
#18077=VERTEX_POINT('',#68197);
#18078=VERTEX_POINT('',#68209);
#18079=VERTEX_POINT('',#68210);
#18080=VERTEX_POINT('',#68220);
#18081=VERTEX_POINT('',#68221);
#18082=VERTEX_POINT('',#68249);
#18083=VERTEX_POINT('',#68250);
#18084=VERTEX_POINT('',#68263);
#18085=VERTEX_POINT('',#68264);
#18086=VERTEX_POINT('',#68267);
#18087=VERTEX_POINT('',#68269);
#18088=VERTEX_POINT('',#68271);
#18089=VERTEX_POINT('',#68310);
#18090=VERTEX_POINT('',#68331);
#18091=VERTEX_POINT('',#68332);
#18092=VERTEX_POINT('',#68335);
#18093=VERTEX_POINT('',#68343);
#18094=VERTEX_POINT('',#68362);
#18095=VERTEX_POINT('',#68363);
#18096=VERTEX_POINT('',#68373);
#18097=VERTEX_POINT('',#68374);
#18098=VERTEX_POINT('',#68384);
#18099=VERTEX_POINT('',#68385);
#18100=VERTEX_POINT('',#68388);
#18101=VERTEX_POINT('',#68390);
#18102=VERTEX_POINT('',#68392);
#18103=VERTEX_POINT('',#68436);
#18104=VERTEX_POINT('',#68437);
#18105=VERTEX_POINT('',#68447);
#18106=VERTEX_POINT('',#68448);
#18107=VERTEX_POINT('',#68461);
#18108=VERTEX_POINT('',#68462);
#18109=VERTEX_POINT('',#68465);
#18110=VERTEX_POINT('',#68467);
#18111=VERTEX_POINT('',#68469);
#18112=VERTEX_POINT('',#68504);
#18113=VERTEX_POINT('',#68505);
#18114=VERTEX_POINT('',#68515);
#18115=VERTEX_POINT('',#68516);
#18116=VERTEX_POINT('',#68535);
#18117=VERTEX_POINT('',#68536);
#18118=VERTEX_POINT('',#68552);
#18119=VERTEX_POINT('',#68554);
#18120=VERTEX_POINT('',#68556);
#18121=VERTEX_POINT('',#68597);
#18122=VERTEX_POINT('',#68598);
#18123=VERTEX_POINT('',#68613);
#18124=VERTEX_POINT('',#68614);
#18125=VERTEX_POINT('',#68632);
#18126=VERTEX_POINT('',#68633);
#18127=VERTEX_POINT('',#68636);
#18128=VERTEX_POINT('',#68638);
#18129=VERTEX_POINT('',#68640);
#18130=VERTEX_POINT('',#68675);
#18131=VERTEX_POINT('',#68676);
#18132=VERTEX_POINT('',#68686);
#18133=VERTEX_POINT('',#68687);
#18134=VERTEX_POINT('',#68707);
#18135=VERTEX_POINT('',#68708);
#18136=VERTEX_POINT('',#68711);
#18137=VERTEX_POINT('',#68713);
#18138=VERTEX_POINT('',#68715);
#18139=VERTEX_POINT('',#68750);
#18140=VERTEX_POINT('',#68751);
#18141=VERTEX_POINT('',#68772);
#18142=VERTEX_POINT('',#68773);
#18143=VERTEX_POINT('',#68776);
#18144=VERTEX_POINT('',#68778);
#18145=VERTEX_POINT('',#68780);
#18146=VERTEX_POINT('',#68795);
#18147=VERTEX_POINT('',#68796);
#18148=VERTEX_POINT('',#68825);
#18149=VERTEX_POINT('',#68846);
#18150=VERTEX_POINT('',#68847);
#18151=VERTEX_POINT('',#68850);
#18152=VERTEX_POINT('',#68858);
#18153=VERTEX_POINT('',#68877);
#18154=VERTEX_POINT('',#68878);
#18155=VERTEX_POINT('',#68888);
#18156=VERTEX_POINT('',#68889);
#18157=VERTEX_POINT('',#68899);
#18158=VERTEX_POINT('',#68900);
#18159=VERTEX_POINT('',#68903);
#18160=VERTEX_POINT('',#68905);
#18161=VERTEX_POINT('',#68907);
#18162=VERTEX_POINT('',#68951);
#18163=VERTEX_POINT('',#68952);
#18164=VERTEX_POINT('',#68962);
#18165=VERTEX_POINT('',#68963);
#18166=VERTEX_POINT('',#68976);
#18167=VERTEX_POINT('',#68977);
#18168=VERTEX_POINT('',#68980);
#18169=VERTEX_POINT('',#68982);
#18170=VERTEX_POINT('',#68984);
#18171=VERTEX_POINT('',#69019);
#18172=VERTEX_POINT('',#69020);
#18173=VERTEX_POINT('',#69030);
#18174=VERTEX_POINT('',#69031);
#18175=VERTEX_POINT('',#69050);
#18176=VERTEX_POINT('',#69051);
#18177=VERTEX_POINT('',#69067);
#18178=VERTEX_POINT('',#69069);
#18179=VERTEX_POINT('',#69071);
#18180=VERTEX_POINT('',#69112);
#18181=VERTEX_POINT('',#69113);
#18182=VERTEX_POINT('',#69128);
#18183=VERTEX_POINT('',#69129);
#18184=VERTEX_POINT('',#69147);
#18185=VERTEX_POINT('',#69148);
#18186=VERTEX_POINT('',#69151);
#18187=VERTEX_POINT('',#69153);
#18188=VERTEX_POINT('',#69155);
#18189=VERTEX_POINT('',#69190);
#18190=VERTEX_POINT('',#69191);
#18191=VERTEX_POINT('',#69201);
#18192=VERTEX_POINT('',#69202);
#18193=VERTEX_POINT('',#69222);
#18194=VERTEX_POINT('',#69223);
#18195=VERTEX_POINT('',#69226);
#18196=VERTEX_POINT('',#69228);
#18197=VERTEX_POINT('',#69230);
#18198=VERTEX_POINT('',#69265);
#18199=VERTEX_POINT('',#69266);
#18200=VERTEX_POINT('',#69276);
#18201=VERTEX_POINT('',#69277);
#18202=VERTEX_POINT('',#69293);
#18203=VERTEX_POINT('',#69294);
#18204=VERTEX_POINT('',#69297);
#18205=VERTEX_POINT('',#69299);
#18206=VERTEX_POINT('',#69301);
#18207=VERTEX_POINT('',#69340);
#18208=VERTEX_POINT('',#69361);
#18209=VERTEX_POINT('',#69362);
#18210=VERTEX_POINT('',#69365);
#18211=VERTEX_POINT('',#69373);
#18212=VERTEX_POINT('',#69392);
#18213=VERTEX_POINT('',#69393);
#18214=VERTEX_POINT('',#69403);
#18215=VERTEX_POINT('',#69404);
#18216=VERTEX_POINT('',#69414);
#18217=VERTEX_POINT('',#69415);
#18218=VERTEX_POINT('',#69418);
#18219=VERTEX_POINT('',#69420);
#18220=VERTEX_POINT('',#69422);
#18221=VERTEX_POINT('',#69466);
#18222=VERTEX_POINT('',#69467);
#18223=VERTEX_POINT('',#69477);
#18224=VERTEX_POINT('',#69478);
#18225=VERTEX_POINT('',#69491);
#18226=VERTEX_POINT('',#69492);
#18227=VERTEX_POINT('',#69495);
#18228=VERTEX_POINT('',#69497);
#18229=VERTEX_POINT('',#69499);
#18230=VERTEX_POINT('',#69534);
#18231=VERTEX_POINT('',#69535);
#18232=VERTEX_POINT('',#69545);
#18233=VERTEX_POINT('',#69546);
#18234=VERTEX_POINT('',#69565);
#18235=VERTEX_POINT('',#69566);
#18236=VERTEX_POINT('',#69582);
#18237=VERTEX_POINT('',#69584);
#18238=VERTEX_POINT('',#69586);
#18239=VERTEX_POINT('',#69627);
#18240=VERTEX_POINT('',#69628);
#18241=VERTEX_POINT('',#69643);
#18242=VERTEX_POINT('',#69644);
#18243=VERTEX_POINT('',#69662);
#18244=VERTEX_POINT('',#69663);
#18245=VERTEX_POINT('',#69666);
#18246=VERTEX_POINT('',#69668);
#18247=VERTEX_POINT('',#69670);
#18248=VERTEX_POINT('',#69705);
#18249=VERTEX_POINT('',#69706);
#18250=VERTEX_POINT('',#69716);
#18251=VERTEX_POINT('',#69717);
#18252=VERTEX_POINT('',#69737);
#18253=VERTEX_POINT('',#69738);
#18254=VERTEX_POINT('',#69741);
#18255=VERTEX_POINT('',#69743);
#18256=VERTEX_POINT('',#69745);
#18257=VERTEX_POINT('',#69780);
#18258=VERTEX_POINT('',#69781);
#18259=VERTEX_POINT('',#69791);
#18260=VERTEX_POINT('',#69792);
#18261=VERTEX_POINT('',#69808);
#18262=VERTEX_POINT('',#69809);
#18263=VERTEX_POINT('',#69812);
#18264=VERTEX_POINT('',#69814);
#18265=VERTEX_POINT('',#69816);
#18266=VERTEX_POINT('',#69855);
#18267=VERTEX_POINT('',#69876);
#18268=VERTEX_POINT('',#69877);
#18269=VERTEX_POINT('',#69880);
#18270=VERTEX_POINT('',#69888);
#18271=VERTEX_POINT('',#69907);
#18272=VERTEX_POINT('',#69908);
#18273=VERTEX_POINT('',#69918);
#18274=VERTEX_POINT('',#69919);
#18275=VERTEX_POINT('',#69929);
#18276=VERTEX_POINT('',#69930);
#18277=VERTEX_POINT('',#69933);
#18278=VERTEX_POINT('',#69935);
#18279=VERTEX_POINT('',#69937);
#18280=VERTEX_POINT('',#69981);
#18281=VERTEX_POINT('',#69982);
#18282=VERTEX_POINT('',#69992);
#18283=VERTEX_POINT('',#69993);
#18284=VERTEX_POINT('',#70006);
#18285=VERTEX_POINT('',#70007);
#18286=VERTEX_POINT('',#70010);
#18287=VERTEX_POINT('',#70012);
#18288=VERTEX_POINT('',#70014);
#18289=VERTEX_POINT('',#70049);
#18290=VERTEX_POINT('',#70050);
#18291=VERTEX_POINT('',#70060);
#18292=VERTEX_POINT('',#70061);
#18293=VERTEX_POINT('',#70080);
#18294=VERTEX_POINT('',#70081);
#18295=VERTEX_POINT('',#70097);
#18296=VERTEX_POINT('',#70099);
#18297=VERTEX_POINT('',#70101);
#18298=VERTEX_POINT('',#70142);
#18299=VERTEX_POINT('',#70143);
#18300=VERTEX_POINT('',#70158);
#18301=VERTEX_POINT('',#70159);
#18302=VERTEX_POINT('',#70177);
#18303=VERTEX_POINT('',#70178);
#18304=VERTEX_POINT('',#70181);
#18305=VERTEX_POINT('',#70183);
#18306=VERTEX_POINT('',#70185);
#18307=VERTEX_POINT('',#70220);
#18308=VERTEX_POINT('',#70221);
#18309=VERTEX_POINT('',#70231);
#18310=VERTEX_POINT('',#70232);
#18311=VERTEX_POINT('',#70252);
#18312=VERTEX_POINT('',#70253);
#18313=VERTEX_POINT('',#70256);
#18314=VERTEX_POINT('',#70258);
#18315=VERTEX_POINT('',#70260);
#18316=VERTEX_POINT('',#70295);
#18317=VERTEX_POINT('',#70296);
#18318=VERTEX_POINT('',#70306);
#18319=VERTEX_POINT('',#70307);
#18320=VERTEX_POINT('',#70323);
#18321=VERTEX_POINT('',#70324);
#18322=VERTEX_POINT('',#70327);
#18323=VERTEX_POINT('',#70329);
#18324=VERTEX_POINT('',#70331);
#18325=VERTEX_POINT('',#70370);
#18326=VERTEX_POINT('',#70391);
#18327=VERTEX_POINT('',#70392);
#18328=VERTEX_POINT('',#70395);
#18329=VERTEX_POINT('',#70403);
#18330=VERTEX_POINT('',#70422);
#18331=VERTEX_POINT('',#70423);
#18332=VERTEX_POINT('',#70433);
#18333=VERTEX_POINT('',#70434);
#18334=VERTEX_POINT('',#70444);
#18335=VERTEX_POINT('',#70445);
#18336=VERTEX_POINT('',#70448);
#18337=VERTEX_POINT('',#70450);
#18338=VERTEX_POINT('',#70452);
#18339=VERTEX_POINT('',#70496);
#18340=VERTEX_POINT('',#70497);
#18341=VERTEX_POINT('',#70507);
#18342=VERTEX_POINT('',#70508);
#18343=VERTEX_POINT('',#70521);
#18344=VERTEX_POINT('',#70522);
#18345=VERTEX_POINT('',#70525);
#18346=VERTEX_POINT('',#70527);
#18347=VERTEX_POINT('',#70529);
#18348=VERTEX_POINT('',#70564);
#18349=VERTEX_POINT('',#70565);
#18350=VERTEX_POINT('',#70575);
#18351=VERTEX_POINT('',#70576);
#18352=VERTEX_POINT('',#70595);
#18353=VERTEX_POINT('',#70596);
#18354=VERTEX_POINT('',#70612);
#18355=VERTEX_POINT('',#70614);
#18356=VERTEX_POINT('',#70616);
#18357=VERTEX_POINT('',#70657);
#18358=VERTEX_POINT('',#70658);
#18359=VERTEX_POINT('',#70673);
#18360=VERTEX_POINT('',#70674);
#18361=VERTEX_POINT('',#70692);
#18362=VERTEX_POINT('',#70693);
#18363=VERTEX_POINT('',#70696);
#18364=VERTEX_POINT('',#70698);
#18365=VERTEX_POINT('',#70700);
#18366=VERTEX_POINT('',#70735);
#18367=VERTEX_POINT('',#70736);
#18368=VERTEX_POINT('',#70746);
#18369=VERTEX_POINT('',#70747);
#18370=VERTEX_POINT('',#70767);
#18371=VERTEX_POINT('',#70768);
#18372=VERTEX_POINT('',#70771);
#18373=VERTEX_POINT('',#70773);
#18374=VERTEX_POINT('',#70775);
#18375=VERTEX_POINT('',#70810);
#18376=VERTEX_POINT('',#70811);
#18377=VERTEX_POINT('',#70821);
#18378=VERTEX_POINT('',#70822);
#18379=VERTEX_POINT('',#70838);
#18380=VERTEX_POINT('',#70839);
#18381=VERTEX_POINT('',#70842);
#18382=VERTEX_POINT('',#70844);
#18383=VERTEX_POINT('',#70846);
#18384=VERTEX_POINT('',#70885);
#18385=VERTEX_POINT('',#70906);
#18386=VERTEX_POINT('',#70907);
#18387=VERTEX_POINT('',#70910);
#18388=VERTEX_POINT('',#70918);
#18389=VERTEX_POINT('',#70937);
#18390=VERTEX_POINT('',#70938);
#18391=VERTEX_POINT('',#70948);
#18392=VERTEX_POINT('',#70949);
#18393=VERTEX_POINT('',#70959);
#18394=VERTEX_POINT('',#70960);
#18395=VERTEX_POINT('',#70963);
#18396=VERTEX_POINT('',#70965);
#18397=VERTEX_POINT('',#70967);
#18398=VERTEX_POINT('',#71011);
#18399=VERTEX_POINT('',#71012);
#18400=VERTEX_POINT('',#71022);
#18401=VERTEX_POINT('',#71023);
#18402=VERTEX_POINT('',#71036);
#18403=VERTEX_POINT('',#71037);
#18404=VERTEX_POINT('',#71040);
#18405=VERTEX_POINT('',#71042);
#18406=VERTEX_POINT('',#71044);
#18407=VERTEX_POINT('',#71079);
#18408=VERTEX_POINT('',#71080);
#18409=VERTEX_POINT('',#71090);
#18410=VERTEX_POINT('',#71091);
#18411=VERTEX_POINT('',#71110);
#18412=VERTEX_POINT('',#71111);
#18413=VERTEX_POINT('',#71127);
#18414=VERTEX_POINT('',#71129);
#18415=VERTEX_POINT('',#71131);
#18416=VERTEX_POINT('',#71172);
#18417=VERTEX_POINT('',#71173);
#18418=VERTEX_POINT('',#71188);
#18419=VERTEX_POINT('',#71189);
#18420=VERTEX_POINT('',#71207);
#18421=VERTEX_POINT('',#71208);
#18422=VERTEX_POINT('',#71211);
#18423=VERTEX_POINT('',#71213);
#18424=VERTEX_POINT('',#71215);
#18425=VERTEX_POINT('',#71250);
#18426=VERTEX_POINT('',#71251);
#18427=VERTEX_POINT('',#71261);
#18428=VERTEX_POINT('',#71262);
#18429=VERTEX_POINT('',#71282);
#18430=VERTEX_POINT('',#71283);
#18431=VERTEX_POINT('',#71286);
#18432=VERTEX_POINT('',#71288);
#18433=VERTEX_POINT('',#71290);
#18434=VERTEX_POINT('',#71325);
#18435=VERTEX_POINT('',#71326);
#18436=VERTEX_POINT('',#71336);
#18437=VERTEX_POINT('',#71337);
#18438=VERTEX_POINT('',#71353);
#18439=VERTEX_POINT('',#71354);
#18440=VERTEX_POINT('',#71357);
#18441=VERTEX_POINT('',#71359);
#18442=VERTEX_POINT('',#71361);
#18443=VERTEX_POINT('',#71400);
#18444=VERTEX_POINT('',#71421);
#18445=VERTEX_POINT('',#71422);
#18446=VERTEX_POINT('',#71425);
#18447=VERTEX_POINT('',#71433);
#18448=VERTEX_POINT('',#71452);
#18449=VERTEX_POINT('',#71453);
#18450=VERTEX_POINT('',#71463);
#18451=VERTEX_POINT('',#71464);
#18452=VERTEX_POINT('',#71474);
#18453=VERTEX_POINT('',#71475);
#18454=VERTEX_POINT('',#71478);
#18455=VERTEX_POINT('',#71480);
#18456=VERTEX_POINT('',#71482);
#18457=VERTEX_POINT('',#71526);
#18458=VERTEX_POINT('',#71527);
#18459=VERTEX_POINT('',#71537);
#18460=VERTEX_POINT('',#71538);
#18461=VERTEX_POINT('',#71551);
#18462=VERTEX_POINT('',#71552);
#18463=VERTEX_POINT('',#71555);
#18464=VERTEX_POINT('',#71557);
#18465=VERTEX_POINT('',#71559);
#18466=VERTEX_POINT('',#71594);
#18467=VERTEX_POINT('',#71595);
#18468=VERTEX_POINT('',#71605);
#18469=VERTEX_POINT('',#71606);
#18470=VERTEX_POINT('',#71625);
#18471=VERTEX_POINT('',#71626);
#18472=VERTEX_POINT('',#71642);
#18473=VERTEX_POINT('',#71644);
#18474=VERTEX_POINT('',#71646);
#18475=VERTEX_POINT('',#71687);
#18476=VERTEX_POINT('',#71688);
#18477=VERTEX_POINT('',#71703);
#18478=VERTEX_POINT('',#71704);
#18479=VERTEX_POINT('',#71722);
#18480=VERTEX_POINT('',#71723);
#18481=VERTEX_POINT('',#71726);
#18482=VERTEX_POINT('',#71728);
#18483=VERTEX_POINT('',#71730);
#18484=VERTEX_POINT('',#71765);
#18485=VERTEX_POINT('',#71766);
#18486=VERTEX_POINT('',#71776);
#18487=VERTEX_POINT('',#71777);
#18488=VERTEX_POINT('',#71797);
#18489=VERTEX_POINT('',#71798);
#18490=VERTEX_POINT('',#71801);
#18491=VERTEX_POINT('',#71803);
#18492=VERTEX_POINT('',#71805);
#18493=VERTEX_POINT('',#71840);
#18494=VERTEX_POINT('',#71841);
#18495=VERTEX_POINT('',#71851);
#18496=VERTEX_POINT('',#71852);
#18497=VERTEX_POINT('',#71868);
#18498=VERTEX_POINT('',#71869);
#18499=VERTEX_POINT('',#71872);
#18500=VERTEX_POINT('',#71874);
#18501=VERTEX_POINT('',#71876);
#18502=VERTEX_POINT('',#71915);
#18503=VERTEX_POINT('',#71936);
#18504=VERTEX_POINT('',#71937);
#18505=VERTEX_POINT('',#71940);
#18506=VERTEX_POINT('',#71948);
#18507=VERTEX_POINT('',#71967);
#18508=VERTEX_POINT('',#71968);
#18509=VERTEX_POINT('',#71978);
#18510=VERTEX_POINT('',#71979);
#18511=VERTEX_POINT('',#71989);
#18512=VERTEX_POINT('',#71990);
#18513=VERTEX_POINT('',#71993);
#18514=VERTEX_POINT('',#71995);
#18515=VERTEX_POINT('',#71997);
#18516=VERTEX_POINT('',#72041);
#18517=VERTEX_POINT('',#72042);
#18518=VERTEX_POINT('',#72052);
#18519=VERTEX_POINT('',#72053);
#18520=VERTEX_POINT('',#72066);
#18521=VERTEX_POINT('',#72067);
#18522=VERTEX_POINT('',#72070);
#18523=VERTEX_POINT('',#72072);
#18524=VERTEX_POINT('',#72074);
#18525=VERTEX_POINT('',#72109);
#18526=VERTEX_POINT('',#72110);
#18527=VERTEX_POINT('',#72120);
#18528=VERTEX_POINT('',#72121);
#18529=VERTEX_POINT('',#72140);
#18530=VERTEX_POINT('',#72141);
#18531=VERTEX_POINT('',#72157);
#18532=VERTEX_POINT('',#72159);
#18533=VERTEX_POINT('',#72161);
#18534=VERTEX_POINT('',#72202);
#18535=VERTEX_POINT('',#72203);
#18536=VERTEX_POINT('',#72218);
#18537=VERTEX_POINT('',#72219);
#18538=VERTEX_POINT('',#72237);
#18539=VERTEX_POINT('',#72238);
#18540=VERTEX_POINT('',#72241);
#18541=VERTEX_POINT('',#72243);
#18542=VERTEX_POINT('',#72245);
#18543=VERTEX_POINT('',#72280);
#18544=VERTEX_POINT('',#72281);
#18545=VERTEX_POINT('',#72291);
#18546=VERTEX_POINT('',#72292);
#18547=VERTEX_POINT('',#72312);
#18548=VERTEX_POINT('',#72313);
#18549=VERTEX_POINT('',#72316);
#18550=VERTEX_POINT('',#72318);
#18551=VERTEX_POINT('',#72320);
#18552=VERTEX_POINT('',#72355);
#18553=VERTEX_POINT('',#72356);
#18554=VERTEX_POINT('',#72366);
#18555=VERTEX_POINT('',#72367);
#18556=VERTEX_POINT('',#72383);
#18557=VERTEX_POINT('',#72384);
#18558=VERTEX_POINT('',#72387);
#18559=VERTEX_POINT('',#72389);
#18560=VERTEX_POINT('',#72391);
#18561=VERTEX_POINT('',#72430);
#18562=VERTEX_POINT('',#72451);
#18563=VERTEX_POINT('',#72452);
#18564=VERTEX_POINT('',#72455);
#18565=VERTEX_POINT('',#72463);
#18566=VERTEX_POINT('',#72482);
#18567=VERTEX_POINT('',#72483);
#18568=VERTEX_POINT('',#72493);
#18569=VERTEX_POINT('',#72494);
#18570=VERTEX_POINT('',#72504);
#18571=VERTEX_POINT('',#72505);
#18572=VERTEX_POINT('',#72508);
#18573=VERTEX_POINT('',#72510);
#18574=VERTEX_POINT('',#72512);
#18575=VERTEX_POINT('',#72556);
#18576=VERTEX_POINT('',#72557);
#18577=VERTEX_POINT('',#72567);
#18578=VERTEX_POINT('',#72568);
#18579=VERTEX_POINT('',#72581);
#18580=VERTEX_POINT('',#72582);
#18581=VERTEX_POINT('',#72585);
#18582=VERTEX_POINT('',#72587);
#18583=VERTEX_POINT('',#72589);
#18584=VERTEX_POINT('',#72624);
#18585=VERTEX_POINT('',#72625);
#18586=VERTEX_POINT('',#72635);
#18587=VERTEX_POINT('',#72636);
#18588=VERTEX_POINT('',#72655);
#18589=VERTEX_POINT('',#72656);
#18590=VERTEX_POINT('',#72672);
#18591=VERTEX_POINT('',#72674);
#18592=VERTEX_POINT('',#72676);
#18593=VERTEX_POINT('',#72717);
#18594=VERTEX_POINT('',#72718);
#18595=VERTEX_POINT('',#72733);
#18596=VERTEX_POINT('',#72734);
#18597=VERTEX_POINT('',#72752);
#18598=VERTEX_POINT('',#72753);
#18599=VERTEX_POINT('',#72756);
#18600=VERTEX_POINT('',#72758);
#18601=VERTEX_POINT('',#72760);
#18602=VERTEX_POINT('',#72795);
#18603=VERTEX_POINT('',#72796);
#18604=VERTEX_POINT('',#72806);
#18605=VERTEX_POINT('',#72807);
#18606=VERTEX_POINT('',#72827);
#18607=VERTEX_POINT('',#72828);
#18608=VERTEX_POINT('',#72831);
#18609=VERTEX_POINT('',#72833);
#18610=VERTEX_POINT('',#72835);
#18611=VERTEX_POINT('',#72870);
#18612=VERTEX_POINT('',#72871);
#18613=VERTEX_POINT('',#72881);
#18614=VERTEX_POINT('',#72882);
#18615=VERTEX_POINT('',#72898);
#18616=VERTEX_POINT('',#72899);
#18617=VERTEX_POINT('',#72902);
#18618=VERTEX_POINT('',#72904);
#18619=VERTEX_POINT('',#72906);
#18620=VERTEX_POINT('',#72945);
#18621=VERTEX_POINT('',#72966);
#18622=VERTEX_POINT('',#72967);
#18623=VERTEX_POINT('',#72970);
#18624=VERTEX_POINT('',#72978);
#18625=VERTEX_POINT('',#72997);
#18626=VERTEX_POINT('',#72998);
#18627=VERTEX_POINT('',#73008);
#18628=VERTEX_POINT('',#73009);
#18629=VERTEX_POINT('',#73019);
#18630=VERTEX_POINT('',#73020);
#18631=VERTEX_POINT('',#73023);
#18632=VERTEX_POINT('',#73025);
#18633=VERTEX_POINT('',#73027);
#18634=VERTEX_POINT('',#73071);
#18635=VERTEX_POINT('',#73072);
#18636=VERTEX_POINT('',#73082);
#18637=VERTEX_POINT('',#73083);
#18638=VERTEX_POINT('',#73093);
#18639=VERTEX_POINT('',#73094);
#18640=VERTEX_POINT('',#73097);
#18641=VERTEX_POINT('',#73099);
#18642=VERTEX_POINT('',#73101);
#18643=VERTEX_POINT('',#73143);
#18644=VERTEX_POINT('',#73144);
#18645=VERTEX_POINT('',#73154);
#18646=VERTEX_POINT('',#73155);
#18647=VERTEX_POINT('',#73174);
#18648=VERTEX_POINT('',#73175);
#18649=VERTEX_POINT('',#73191);
#18650=VERTEX_POINT('',#73193);
#18651=VERTEX_POINT('',#73195);
#18652=VERTEX_POINT('',#73236);
#18653=VERTEX_POINT('',#73237);
#18654=VERTEX_POINT('',#73252);
#18655=VERTEX_POINT('',#73253);
#18656=VERTEX_POINT('',#73271);
#18657=VERTEX_POINT('',#73272);
#18658=VERTEX_POINT('',#73275);
#18659=VERTEX_POINT('',#73277);
#18660=VERTEX_POINT('',#73279);
#18661=VERTEX_POINT('',#73314);
#18662=VERTEX_POINT('',#73315);
#18663=VERTEX_POINT('',#73325);
#18664=VERTEX_POINT('',#73326);
#18665=VERTEX_POINT('',#73346);
#18666=VERTEX_POINT('',#73347);
#18667=VERTEX_POINT('',#73350);
#18668=VERTEX_POINT('',#73352);
#18669=VERTEX_POINT('',#73354);
#18670=VERTEX_POINT('',#73389);
#18671=VERTEX_POINT('',#73390);
#18672=VERTEX_POINT('',#73400);
#18673=VERTEX_POINT('',#73401);
#18674=VERTEX_POINT('',#73417);
#18675=VERTEX_POINT('',#73418);
#18676=VERTEX_POINT('',#73421);
#18677=VERTEX_POINT('',#73423);
#18678=VERTEX_POINT('',#73425);
#18679=VERTEX_POINT('',#73464);
#18680=VERTEX_POINT('',#73485);
#18681=VERTEX_POINT('',#73486);
#18682=VERTEX_POINT('',#73489);
#18683=VERTEX_POINT('',#73497);
#18684=VERTEX_POINT('',#73516);
#18685=VERTEX_POINT('',#73517);
#18686=VERTEX_POINT('',#73527);
#18687=VERTEX_POINT('',#73528);
#18688=VERTEX_POINT('',#73538);
#18689=VERTEX_POINT('',#73539);
#18690=VERTEX_POINT('',#73542);
#18691=VERTEX_POINT('',#73544);
#18692=VERTEX_POINT('',#73546);
#18693=VERTEX_POINT('',#73590);
#18694=VERTEX_POINT('',#73591);
#18695=VERTEX_POINT('',#73601);
#18696=VERTEX_POINT('',#73602);
#18697=VERTEX_POINT('',#73615);
#18698=VERTEX_POINT('',#73616);
#18699=VERTEX_POINT('',#73619);
#18700=VERTEX_POINT('',#73621);
#18701=VERTEX_POINT('',#73623);
#18702=VERTEX_POINT('',#73658);
#18703=VERTEX_POINT('',#73659);
#18704=VERTEX_POINT('',#73669);
#18705=VERTEX_POINT('',#73670);
#18706=VERTEX_POINT('',#73689);
#18707=VERTEX_POINT('',#73690);
#18708=VERTEX_POINT('',#73706);
#18709=VERTEX_POINT('',#73708);
#18710=VERTEX_POINT('',#73710);
#18711=VERTEX_POINT('',#73751);
#18712=VERTEX_POINT('',#73752);
#18713=VERTEX_POINT('',#73767);
#18714=VERTEX_POINT('',#73768);
#18715=VERTEX_POINT('',#73786);
#18716=VERTEX_POINT('',#73787);
#18717=VERTEX_POINT('',#73790);
#18718=VERTEX_POINT('',#73792);
#18719=VERTEX_POINT('',#73794);
#18720=VERTEX_POINT('',#73829);
#18721=VERTEX_POINT('',#73830);
#18722=VERTEX_POINT('',#73840);
#18723=VERTEX_POINT('',#73841);
#18724=VERTEX_POINT('',#73861);
#18725=VERTEX_POINT('',#73862);
#18726=VERTEX_POINT('',#73865);
#18727=VERTEX_POINT('',#73867);
#18728=VERTEX_POINT('',#73869);
#18729=VERTEX_POINT('',#73904);
#18730=VERTEX_POINT('',#73905);
#18731=VERTEX_POINT('',#73915);
#18732=VERTEX_POINT('',#73916);
#18733=VERTEX_POINT('',#73932);
#18734=VERTEX_POINT('',#73933);
#18735=VERTEX_POINT('',#73936);
#18736=VERTEX_POINT('',#73938);
#18737=VERTEX_POINT('',#73940);
#18738=VERTEX_POINT('',#73979);
#18739=VERTEX_POINT('',#74000);
#18740=VERTEX_POINT('',#74001);
#18741=VERTEX_POINT('',#74004);
#18742=VERTEX_POINT('',#74012);
#18743=VERTEX_POINT('',#74031);
#18744=VERTEX_POINT('',#74032);
#18745=VERTEX_POINT('',#74042);
#18746=VERTEX_POINT('',#74043);
#18747=VERTEX_POINT('',#74053);
#18748=VERTEX_POINT('',#74054);
#18749=VERTEX_POINT('',#74057);
#18750=VERTEX_POINT('',#74059);
#18751=VERTEX_POINT('',#74061);
#18752=VERTEX_POINT('',#74105);
#18753=VERTEX_POINT('',#74106);
#18754=VERTEX_POINT('',#74116);
#18755=VERTEX_POINT('',#74117);
#18756=VERTEX_POINT('',#74130);
#18757=VERTEX_POINT('',#74131);
#18758=VERTEX_POINT('',#74134);
#18759=VERTEX_POINT('',#74136);
#18760=VERTEX_POINT('',#74138);
#18761=VERTEX_POINT('',#74173);
#18762=VERTEX_POINT('',#74174);
#18763=VERTEX_POINT('',#74184);
#18764=VERTEX_POINT('',#74185);
#18765=VERTEX_POINT('',#74204);
#18766=VERTEX_POINT('',#74205);
#18767=VERTEX_POINT('',#74221);
#18768=VERTEX_POINT('',#74223);
#18769=VERTEX_POINT('',#74225);
#18770=VERTEX_POINT('',#74266);
#18771=VERTEX_POINT('',#74267);
#18772=VERTEX_POINT('',#74282);
#18773=VERTEX_POINT('',#74283);
#18774=VERTEX_POINT('',#74301);
#18775=VERTEX_POINT('',#74302);
#18776=VERTEX_POINT('',#74305);
#18777=VERTEX_POINT('',#74307);
#18778=VERTEX_POINT('',#74309);
#18779=VERTEX_POINT('',#74344);
#18780=VERTEX_POINT('',#74345);
#18781=VERTEX_POINT('',#74355);
#18782=VERTEX_POINT('',#74356);
#18783=VERTEX_POINT('',#74376);
#18784=VERTEX_POINT('',#74377);
#18785=VERTEX_POINT('',#74380);
#18786=VERTEX_POINT('',#74382);
#18787=VERTEX_POINT('',#74384);
#18788=VERTEX_POINT('',#74419);
#18789=VERTEX_POINT('',#74420);
#18790=VERTEX_POINT('',#74430);
#18791=VERTEX_POINT('',#74431);
#18792=VERTEX_POINT('',#74447);
#18793=VERTEX_POINT('',#74448);
#18794=VERTEX_POINT('',#74451);
#18795=VERTEX_POINT('',#74453);
#18796=VERTEX_POINT('',#74455);
#18797=VERTEX_POINT('',#74494);
#18798=VERTEX_POINT('',#74515);
#18799=VERTEX_POINT('',#74516);
#18800=VERTEX_POINT('',#74519);
#18801=VERTEX_POINT('',#74527);
#18802=VERTEX_POINT('',#74546);
#18803=VERTEX_POINT('',#74547);
#18804=VERTEX_POINT('',#74557);
#18805=VERTEX_POINT('',#74558);
#18806=VERTEX_POINT('',#74568);
#18807=VERTEX_POINT('',#74569);
#18808=VERTEX_POINT('',#74572);
#18809=VERTEX_POINT('',#74574);
#18810=VERTEX_POINT('',#74576);
#18811=VERTEX_POINT('',#74620);
#18812=VERTEX_POINT('',#74621);
#18813=VERTEX_POINT('',#74631);
#18814=VERTEX_POINT('',#74632);
#18815=VERTEX_POINT('',#74645);
#18816=VERTEX_POINT('',#74646);
#18817=VERTEX_POINT('',#74649);
#18818=VERTEX_POINT('',#74651);
#18819=VERTEX_POINT('',#74653);
#18820=VERTEX_POINT('',#74688);
#18821=VERTEX_POINT('',#74689);
#18822=VERTEX_POINT('',#74699);
#18823=VERTEX_POINT('',#74700);
#18824=VERTEX_POINT('',#74719);
#18825=VERTEX_POINT('',#74720);
#18826=VERTEX_POINT('',#74736);
#18827=VERTEX_POINT('',#74738);
#18828=VERTEX_POINT('',#74740);
#18829=VERTEX_POINT('',#74781);
#18830=VERTEX_POINT('',#74782);
#18831=VERTEX_POINT('',#74797);
#18832=VERTEX_POINT('',#74798);
#18833=VERTEX_POINT('',#74816);
#18834=VERTEX_POINT('',#74817);
#18835=VERTEX_POINT('',#74820);
#18836=VERTEX_POINT('',#74822);
#18837=VERTEX_POINT('',#74824);
#18838=VERTEX_POINT('',#74859);
#18839=VERTEX_POINT('',#74860);
#18840=VERTEX_POINT('',#74870);
#18841=VERTEX_POINT('',#74871);
#18842=VERTEX_POINT('',#74891);
#18843=VERTEX_POINT('',#74892);
#18844=VERTEX_POINT('',#74895);
#18845=VERTEX_POINT('',#74897);
#18846=VERTEX_POINT('',#74899);
#18847=VERTEX_POINT('',#74934);
#18848=VERTEX_POINT('',#74935);
#18849=VERTEX_POINT('',#74945);
#18850=VERTEX_POINT('',#74946);
#18851=VERTEX_POINT('',#74962);
#18852=VERTEX_POINT('',#74963);
#18853=VERTEX_POINT('',#74966);
#18854=VERTEX_POINT('',#74968);
#18855=VERTEX_POINT('',#74970);
#18856=VERTEX_POINT('',#75009);
#18857=VERTEX_POINT('',#75030);
#18858=VERTEX_POINT('',#75031);
#18859=VERTEX_POINT('',#75034);
#18860=VERTEX_POINT('',#75042);
#18861=VERTEX_POINT('',#75061);
#18862=VERTEX_POINT('',#75062);
#18863=VERTEX_POINT('',#75072);
#18864=VERTEX_POINT('',#75073);
#18865=VERTEX_POINT('',#75083);
#18866=VERTEX_POINT('',#75084);
#18867=VERTEX_POINT('',#75087);
#18868=VERTEX_POINT('',#75089);
#18869=VERTEX_POINT('',#75091);
#18870=VERTEX_POINT('',#75135);
#18871=VERTEX_POINT('',#75136);
#18872=VERTEX_POINT('',#75146);
#18873=VERTEX_POINT('',#75147);
#18874=VERTEX_POINT('',#75160);
#18875=VERTEX_POINT('',#75161);
#18876=VERTEX_POINT('',#75164);
#18877=VERTEX_POINT('',#75166);
#18878=VERTEX_POINT('',#75168);
#18879=VERTEX_POINT('',#75203);
#18880=VERTEX_POINT('',#75204);
#18881=VERTEX_POINT('',#75214);
#18882=VERTEX_POINT('',#75215);
#18883=VERTEX_POINT('',#75234);
#18884=VERTEX_POINT('',#75235);
#18885=VERTEX_POINT('',#75251);
#18886=VERTEX_POINT('',#75253);
#18887=VERTEX_POINT('',#75255);
#18888=VERTEX_POINT('',#75296);
#18889=VERTEX_POINT('',#75297);
#18890=VERTEX_POINT('',#75312);
#18891=VERTEX_POINT('',#75313);
#18892=VERTEX_POINT('',#75331);
#18893=VERTEX_POINT('',#75332);
#18894=VERTEX_POINT('',#75335);
#18895=VERTEX_POINT('',#75337);
#18896=VERTEX_POINT('',#75339);
#18897=VERTEX_POINT('',#75374);
#18898=VERTEX_POINT('',#75375);
#18899=VERTEX_POINT('',#75385);
#18900=VERTEX_POINT('',#75386);
#18901=VERTEX_POINT('',#75406);
#18902=VERTEX_POINT('',#75407);
#18903=VERTEX_POINT('',#75410);
#18904=VERTEX_POINT('',#75412);
#18905=VERTEX_POINT('',#75414);
#18906=VERTEX_POINT('',#75449);
#18907=VERTEX_POINT('',#75450);
#18908=VERTEX_POINT('',#75460);
#18909=VERTEX_POINT('',#75461);
#18910=VERTEX_POINT('',#75477);
#18911=VERTEX_POINT('',#75478);
#18912=VERTEX_POINT('',#75481);
#18913=VERTEX_POINT('',#75483);
#18914=VERTEX_POINT('',#75485);
#18915=VERTEX_POINT('',#75524);
#18916=VERTEX_POINT('',#75545);
#18917=VERTEX_POINT('',#75546);
#18918=VERTEX_POINT('',#75549);
#18919=VERTEX_POINT('',#75557);
#18920=VERTEX_POINT('',#75576);
#18921=VERTEX_POINT('',#75577);
#18922=VERTEX_POINT('',#75587);
#18923=VERTEX_POINT('',#75588);
#18924=VERTEX_POINT('',#75598);
#18925=VERTEX_POINT('',#75599);
#18926=VERTEX_POINT('',#75602);
#18927=VERTEX_POINT('',#75604);
#18928=VERTEX_POINT('',#75606);
#18929=VERTEX_POINT('',#75650);
#18930=VERTEX_POINT('',#75651);
#18931=VERTEX_POINT('',#75661);
#18932=VERTEX_POINT('',#75662);
#18933=VERTEX_POINT('',#75672);
#18934=VERTEX_POINT('',#75673);
#18935=VERTEX_POINT('',#75676);
#18936=VERTEX_POINT('',#75678);
#18937=VERTEX_POINT('',#75680);
#18938=VERTEX_POINT('',#75722);
#18939=VERTEX_POINT('',#75723);
#18940=VERTEX_POINT('',#75733);
#18941=VERTEX_POINT('',#75734);
#18942=VERTEX_POINT('',#75753);
#18943=VERTEX_POINT('',#75754);
#18944=VERTEX_POINT('',#75770);
#18945=VERTEX_POINT('',#75772);
#18946=VERTEX_POINT('',#75774);
#18947=VERTEX_POINT('',#75815);
#18948=VERTEX_POINT('',#75816);
#18949=VERTEX_POINT('',#75831);
#18950=VERTEX_POINT('',#75832);
#18951=VERTEX_POINT('',#75850);
#18952=VERTEX_POINT('',#75851);
#18953=VERTEX_POINT('',#75854);
#18954=VERTEX_POINT('',#75856);
#18955=VERTEX_POINT('',#75858);
#18956=VERTEX_POINT('',#75893);
#18957=VERTEX_POINT('',#75894);
#18958=VERTEX_POINT('',#75904);
#18959=VERTEX_POINT('',#75905);
#18960=VERTEX_POINT('',#75925);
#18961=VERTEX_POINT('',#75926);
#18962=VERTEX_POINT('',#75929);
#18963=VERTEX_POINT('',#75931);
#18964=VERTEX_POINT('',#75933);
#18965=VERTEX_POINT('',#75968);
#18966=VERTEX_POINT('',#75969);
#18967=VERTEX_POINT('',#75979);
#18968=VERTEX_POINT('',#75980);
#18969=VERTEX_POINT('',#75996);
#18970=VERTEX_POINT('',#75997);
#18971=VERTEX_POINT('',#76000);
#18972=VERTEX_POINT('',#76002);
#18973=VERTEX_POINT('',#76004);
#18974=VERTEX_POINT('',#76043);
#18975=VERTEX_POINT('',#76064);
#18976=VERTEX_POINT('',#76065);
#18977=VERTEX_POINT('',#76068);
#18978=VERTEX_POINT('',#76076);
#18979=VERTEX_POINT('',#76095);
#18980=VERTEX_POINT('',#76096);
#18981=VERTEX_POINT('',#76106);
#18982=VERTEX_POINT('',#76107);
#18983=VERTEX_POINT('',#76117);
#18984=VERTEX_POINT('',#76118);
#18985=VERTEX_POINT('',#76121);
#18986=VERTEX_POINT('',#76123);
#18987=VERTEX_POINT('',#76125);
#18988=VERTEX_POINT('',#76169);
#18989=VERTEX_POINT('',#76170);
#18990=VERTEX_POINT('',#76180);
#18991=VERTEX_POINT('',#76181);
#18992=VERTEX_POINT('',#76194);
#18993=VERTEX_POINT('',#76195);
#18994=VERTEX_POINT('',#76198);
#18995=VERTEX_POINT('',#76200);
#18996=VERTEX_POINT('',#76202);
#18997=VERTEX_POINT('',#76237);
#18998=VERTEX_POINT('',#76238);
#18999=VERTEX_POINT('',#76248);
#19000=VERTEX_POINT('',#76249);
#19001=VERTEX_POINT('',#76269);
#19002=VERTEX_POINT('',#76270);
#19003=VERTEX_POINT('',#76284);
#19004=VERTEX_POINT('',#76286);
#19005=VERTEX_POINT('',#76288);
#19006=VERTEX_POINT('',#76324);
#19007=VERTEX_POINT('',#76325);
#19008=VERTEX_POINT('',#76340);
#19009=VERTEX_POINT('',#76341);
#19010=VERTEX_POINT('',#76359);
#19011=VERTEX_POINT('',#76360);
#19012=VERTEX_POINT('',#76363);
#19013=VERTEX_POINT('',#76365);
#19014=VERTEX_POINT('',#76367);
#19015=VERTEX_POINT('',#76402);
#19016=VERTEX_POINT('',#76403);
#19017=VERTEX_POINT('',#76413);
#19018=VERTEX_POINT('',#76414);
#19019=VERTEX_POINT('',#76434);
#19020=VERTEX_POINT('',#76435);
#19021=VERTEX_POINT('',#76438);
#19022=VERTEX_POINT('',#76440);
#19023=VERTEX_POINT('',#76442);
#19024=VERTEX_POINT('',#76477);
#19025=VERTEX_POINT('',#76478);
#19026=VERTEX_POINT('',#76488);
#19027=VERTEX_POINT('',#76489);
#19028=VERTEX_POINT('',#76505);
#19029=VERTEX_POINT('',#76506);
#19030=VERTEX_POINT('',#76509);
#19031=VERTEX_POINT('',#76511);
#19032=VERTEX_POINT('',#76513);
#19033=VERTEX_POINT('',#76552);
#19034=VERTEX_POINT('',#76573);
#19035=VERTEX_POINT('',#76574);
#19036=VERTEX_POINT('',#76577);
#19037=VERTEX_POINT('',#76585);
#19038=VERTEX_POINT('',#76604);
#19039=VERTEX_POINT('',#76605);
#19040=VERTEX_POINT('',#76615);
#19041=VERTEX_POINT('',#76616);
#19042=VERTEX_POINT('',#76626);
#19043=VERTEX_POINT('',#76627);
#19044=VERTEX_POINT('',#76630);
#19045=VERTEX_POINT('',#76632);
#19046=VERTEX_POINT('',#76634);
#19047=VERTEX_POINT('',#76678);
#19048=VERTEX_POINT('',#76679);
#19049=VERTEX_POINT('',#76689);
#19050=VERTEX_POINT('',#76690);
#19051=VERTEX_POINT('',#76700);
#19052=VERTEX_POINT('',#76701);
#19053=VERTEX_POINT('',#76704);
#19054=VERTEX_POINT('',#76706);
#19055=VERTEX_POINT('',#76708);
#19056=VERTEX_POINT('',#76750);
#19057=VERTEX_POINT('',#76751);
#19058=VERTEX_POINT('',#76761);
#19059=VERTEX_POINT('',#76762);
#19060=VERTEX_POINT('',#76781);
#19061=VERTEX_POINT('',#76782);
#19062=VERTEX_POINT('',#76798);
#19063=VERTEX_POINT('',#76800);
#19064=VERTEX_POINT('',#76802);
#19065=VERTEX_POINT('',#76843);
#19066=VERTEX_POINT('',#76844);
#19067=VERTEX_POINT('',#76859);
#19068=VERTEX_POINT('',#76860);
#19069=VERTEX_POINT('',#76875);
#19070=VERTEX_POINT('',#76876);
#19071=VERTEX_POINT('',#76879);
#19072=VERTEX_POINT('',#76881);
#19073=VERTEX_POINT('',#76883);
#19074=VERTEX_POINT('',#76925);
#19075=VERTEX_POINT('',#76926);
#19076=VERTEX_POINT('',#76936);
#19077=VERTEX_POINT('',#76937);
#19078=VERTEX_POINT('',#76957);
#19079=VERTEX_POINT('',#76958);
#19080=VERTEX_POINT('',#76961);
#19081=VERTEX_POINT('',#76963);
#19082=VERTEX_POINT('',#76965);
#19083=VERTEX_POINT('',#77000);
#19084=VERTEX_POINT('',#77001);
#19085=VERTEX_POINT('',#77011);
#19086=VERTEX_POINT('',#77012);
#19087=VERTEX_POINT('',#77028);
#19088=VERTEX_POINT('',#77029);
#19089=VERTEX_POINT('',#77032);
#19090=VERTEX_POINT('',#77034);
#19091=VERTEX_POINT('',#77036);
#19092=VERTEX_POINT('',#77075);
#19093=VERTEX_POINT('',#77096);
#19094=VERTEX_POINT('',#77097);
#19095=VERTEX_POINT('',#77100);
#19096=VERTEX_POINT('',#77108);
#19097=VERTEX_POINT('',#77127);
#19098=VERTEX_POINT('',#77128);
#19099=VERTEX_POINT('',#77138);
#19100=VERTEX_POINT('',#77139);
#19101=VERTEX_POINT('',#77149);
#19102=VERTEX_POINT('',#77150);
#19103=VERTEX_POINT('',#77153);
#19104=VERTEX_POINT('',#77155);
#19105=VERTEX_POINT('',#77157);
#19106=VERTEX_POINT('',#77201);
#19107=VERTEX_POINT('',#77202);
#19108=VERTEX_POINT('',#77212);
#19109=VERTEX_POINT('',#77213);
#19110=VERTEX_POINT('',#77226);
#19111=VERTEX_POINT('',#77227);
#19112=VERTEX_POINT('',#77230);
#19113=VERTEX_POINT('',#77232);
#19114=VERTEX_POINT('',#77234);
#19115=VERTEX_POINT('',#77269);
#19116=VERTEX_POINT('',#77270);
#19117=VERTEX_POINT('',#77280);
#19118=VERTEX_POINT('',#77281);
#19119=VERTEX_POINT('',#77300);
#19120=VERTEX_POINT('',#77301);
#19121=VERTEX_POINT('',#77317);
#19122=VERTEX_POINT('',#77319);
#19123=VERTEX_POINT('',#77321);
#19124=VERTEX_POINT('',#77362);
#19125=VERTEX_POINT('',#77363);
#19126=VERTEX_POINT('',#77378);
#19127=VERTEX_POINT('',#77379);
#19128=VERTEX_POINT('',#77397);
#19129=VERTEX_POINT('',#77398);
#19130=VERTEX_POINT('',#77401);
#19131=VERTEX_POINT('',#77403);
#19132=VERTEX_POINT('',#77405);
#19133=VERTEX_POINT('',#77440);
#19134=VERTEX_POINT('',#77441);
#19135=VERTEX_POINT('',#77451);
#19136=VERTEX_POINT('',#77452);
#19137=VERTEX_POINT('',#77472);
#19138=VERTEX_POINT('',#77473);
#19139=VERTEX_POINT('',#77476);
#19140=VERTEX_POINT('',#77478);
#19141=VERTEX_POINT('',#77480);
#19142=VERTEX_POINT('',#77522);
#19143=VERTEX_POINT('',#77523);
#19144=VERTEX_POINT('',#77533);
#19145=VERTEX_POINT('',#77534);
#19146=VERTEX_POINT('',#77550);
#19147=VERTEX_POINT('',#77551);
#19148=VERTEX_POINT('',#77554);
#19149=VERTEX_POINT('',#77556);
#19150=VERTEX_POINT('',#77558);
#19151=VERTEX_POINT('',#77597);
#19152=VERTEX_POINT('',#77618);
#19153=VERTEX_POINT('',#77619);
#19154=VERTEX_POINT('',#77622);
#19155=VERTEX_POINT('',#77630);
#19156=VERTEX_POINT('',#77649);
#19157=VERTEX_POINT('',#77650);
#19158=VERTEX_POINT('',#77660);
#19159=VERTEX_POINT('',#77661);
#19160=VERTEX_POINT('',#77671);
#19161=VERTEX_POINT('',#77672);
#19162=VERTEX_POINT('',#77675);
#19163=VERTEX_POINT('',#77677);
#19164=VERTEX_POINT('',#77679);
#19165=VERTEX_POINT('',#77723);
#19166=VERTEX_POINT('',#77724);
#19167=VERTEX_POINT('',#77734);
#19168=VERTEX_POINT('',#77735);
#19169=VERTEX_POINT('',#77748);
#19170=VERTEX_POINT('',#77749);
#19171=VERTEX_POINT('',#77752);
#19172=VERTEX_POINT('',#77754);
#19173=VERTEX_POINT('',#77756);
#19174=VERTEX_POINT('',#77791);
#19175=VERTEX_POINT('',#77792);
#19176=VERTEX_POINT('',#77802);
#19177=VERTEX_POINT('',#77803);
#19178=VERTEX_POINT('',#77822);
#19179=VERTEX_POINT('',#77823);
#19180=VERTEX_POINT('',#77839);
#19181=VERTEX_POINT('',#77841);
#19182=VERTEX_POINT('',#77843);
#19183=VERTEX_POINT('',#77884);
#19184=VERTEX_POINT('',#77885);
#19185=VERTEX_POINT('',#77900);
#19186=VERTEX_POINT('',#77901);
#19187=VERTEX_POINT('',#77919);
#19188=VERTEX_POINT('',#77920);
#19189=VERTEX_POINT('',#77923);
#19190=VERTEX_POINT('',#77925);
#19191=VERTEX_POINT('',#77927);
#19192=VERTEX_POINT('',#77962);
#19193=VERTEX_POINT('',#77963);
#19194=VERTEX_POINT('',#77973);
#19195=VERTEX_POINT('',#77974);
#19196=VERTEX_POINT('',#77994);
#19197=VERTEX_POINT('',#77995);
#19198=VERTEX_POINT('',#77998);
#19199=VERTEX_POINT('',#78000);
#19200=VERTEX_POINT('',#78002);
#19201=VERTEX_POINT('',#78037);
#19202=VERTEX_POINT('',#78038);
#19203=VERTEX_POINT('',#78048);
#19204=VERTEX_POINT('',#78049);
#19205=VERTEX_POINT('',#78062);
#19206=VERTEX_POINT('',#78063);
#19207=VERTEX_POINT('',#78066);
#19208=VERTEX_POINT('',#78068);
#19209=VERTEX_POINT('',#78070);
#19210=VERTEX_POINT('',#78116);
#19211=VERTEX_POINT('',#78137);
#19212=VERTEX_POINT('',#78138);
#19213=VERTEX_POINT('',#78141);
#19214=VERTEX_POINT('',#78149);
#19215=VERTEX_POINT('',#78168);
#19216=VERTEX_POINT('',#78169);
#19217=VERTEX_POINT('',#78179);
#19218=VERTEX_POINT('',#78180);
#19219=VERTEX_POINT('',#78190);
#19220=VERTEX_POINT('',#78191);
#19221=VERTEX_POINT('',#78194);
#19222=VERTEX_POINT('',#78196);
#19223=VERTEX_POINT('',#78198);
#19224=VERTEX_POINT('',#78242);
#19225=VERTEX_POINT('',#78243);
#19226=VERTEX_POINT('',#78253);
#19227=VERTEX_POINT('',#78254);
#19228=VERTEX_POINT('',#78267);
#19229=VERTEX_POINT('',#78268);
#19230=VERTEX_POINT('',#78271);
#19231=VERTEX_POINT('',#78273);
#19232=VERTEX_POINT('',#78275);
#19233=VERTEX_POINT('',#78310);
#19234=VERTEX_POINT('',#78311);
#19235=VERTEX_POINT('',#78321);
#19236=VERTEX_POINT('',#78322);
#19237=VERTEX_POINT('',#78341);
#19238=VERTEX_POINT('',#78342);
#19239=VERTEX_POINT('',#78358);
#19240=VERTEX_POINT('',#78360);
#19241=VERTEX_POINT('',#78362);
#19242=VERTEX_POINT('',#78403);
#19243=VERTEX_POINT('',#78404);
#19244=VERTEX_POINT('',#78419);
#19245=VERTEX_POINT('',#78420);
#19246=VERTEX_POINT('',#78438);
#19247=VERTEX_POINT('',#78439);
#19248=VERTEX_POINT('',#78442);
#19249=VERTEX_POINT('',#78444);
#19250=VERTEX_POINT('',#78446);
#19251=VERTEX_POINT('',#78481);
#19252=VERTEX_POINT('',#78482);
#19253=VERTEX_POINT('',#78492);
#19254=VERTEX_POINT('',#78493);
#19255=VERTEX_POINT('',#78513);
#19256=VERTEX_POINT('',#78514);
#19257=VERTEX_POINT('',#78517);
#19258=VERTEX_POINT('',#78519);
#19259=VERTEX_POINT('',#78521);
#19260=VERTEX_POINT('',#78556);
#19261=VERTEX_POINT('',#78557);
#19262=VERTEX_POINT('',#78567);
#19263=VERTEX_POINT('',#78568);
#19264=VERTEX_POINT('',#78584);
#19265=VERTEX_POINT('',#78585);
#19266=VERTEX_POINT('',#78588);
#19267=VERTEX_POINT('',#78590);
#19268=VERTEX_POINT('',#78592);
#19269=VERTEX_POINT('',#78631);
#19270=VERTEX_POINT('',#78652);
#19271=VERTEX_POINT('',#78653);
#19272=VERTEX_POINT('',#78656);
#19273=VERTEX_POINT('',#78664);
#19274=VERTEX_POINT('',#78683);
#19275=VERTEX_POINT('',#78684);
#19276=VERTEX_POINT('',#78694);
#19277=VERTEX_POINT('',#78695);
#19278=VERTEX_POINT('',#78705);
#19279=VERTEX_POINT('',#78706);
#19280=VERTEX_POINT('',#78709);
#19281=VERTEX_POINT('',#78711);
#19282=VERTEX_POINT('',#78713);
#19283=VERTEX_POINT('',#78757);
#19284=VERTEX_POINT('',#78758);
#19285=VERTEX_POINT('',#78768);
#19286=VERTEX_POINT('',#78769);
#19287=VERTEX_POINT('',#78782);
#19288=VERTEX_POINT('',#78783);
#19289=VERTEX_POINT('',#78786);
#19290=VERTEX_POINT('',#78788);
#19291=VERTEX_POINT('',#78790);
#19292=VERTEX_POINT('',#78825);
#19293=VERTEX_POINT('',#78826);
#19294=VERTEX_POINT('',#78836);
#19295=VERTEX_POINT('',#78837);
#19296=VERTEX_POINT('',#78856);
#19297=VERTEX_POINT('',#78857);
#19298=VERTEX_POINT('',#78873);
#19299=VERTEX_POINT('',#78875);
#19300=VERTEX_POINT('',#78877);
#19301=VERTEX_POINT('',#78918);
#19302=VERTEX_POINT('',#78919);
#19303=VERTEX_POINT('',#78934);
#19304=VERTEX_POINT('',#78935);
#19305=VERTEX_POINT('',#78953);
#19306=VERTEX_POINT('',#78954);
#19307=VERTEX_POINT('',#78957);
#19308=VERTEX_POINT('',#78959);
#19309=VERTEX_POINT('',#78961);
#19310=VERTEX_POINT('',#78996);
#19311=VERTEX_POINT('',#78997);
#19312=VERTEX_POINT('',#79007);
#19313=VERTEX_POINT('',#79008);
#19314=VERTEX_POINT('',#79028);
#19315=VERTEX_POINT('',#79029);
#19316=VERTEX_POINT('',#79032);
#19317=VERTEX_POINT('',#79034);
#19318=VERTEX_POINT('',#79036);
#19319=VERTEX_POINT('',#79071);
#19320=VERTEX_POINT('',#79072);
#19321=VERTEX_POINT('',#79082);
#19322=VERTEX_POINT('',#79083);
#19323=VERTEX_POINT('',#79099);
#19324=VERTEX_POINT('',#79100);
#19325=VERTEX_POINT('',#79103);
#19326=VERTEX_POINT('',#79105);
#19327=VERTEX_POINT('',#79107);
#19328=VERTEX_POINT('',#79146);
#19329=VERTEX_POINT('',#79167);
#19330=VERTEX_POINT('',#79168);
#19331=VERTEX_POINT('',#79171);
#19332=VERTEX_POINT('',#79179);
#19333=VERTEX_POINT('',#79198);
#19334=VERTEX_POINT('',#79199);
#19335=VERTEX_POINT('',#79209);
#19336=VERTEX_POINT('',#79210);
#19337=VERTEX_POINT('',#79220);
#19338=VERTEX_POINT('',#79221);
#19339=VERTEX_POINT('',#79224);
#19340=VERTEX_POINT('',#79226);
#19341=VERTEX_POINT('',#79228);
#19342=VERTEX_POINT('',#79272);
#19343=VERTEX_POINT('',#79273);
#19344=VERTEX_POINT('',#79283);
#19345=VERTEX_POINT('',#79284);
#19346=VERTEX_POINT('',#79297);
#19347=VERTEX_POINT('',#79298);
#19348=VERTEX_POINT('',#79301);
#19349=VERTEX_POINT('',#79303);
#19350=VERTEX_POINT('',#79305);
#19351=VERTEX_POINT('',#79340);
#19352=VERTEX_POINT('',#79341);
#19353=VERTEX_POINT('',#79351);
#19354=VERTEX_POINT('',#79352);
#19355=VERTEX_POINT('',#79371);
#19356=VERTEX_POINT('',#79372);
#19357=VERTEX_POINT('',#79388);
#19358=VERTEX_POINT('',#79390);
#19359=VERTEX_POINT('',#79392);
#19360=VERTEX_POINT('',#79433);
#19361=VERTEX_POINT('',#79434);
#19362=VERTEX_POINT('',#79449);
#19363=VERTEX_POINT('',#79450);
#19364=VERTEX_POINT('',#79468);
#19365=VERTEX_POINT('',#79469);
#19366=VERTEX_POINT('',#79472);
#19367=VERTEX_POINT('',#79474);
#19368=VERTEX_POINT('',#79476);
#19369=VERTEX_POINT('',#79511);
#19370=VERTEX_POINT('',#79512);
#19371=VERTEX_POINT('',#79522);
#19372=VERTEX_POINT('',#79523);
#19373=VERTEX_POINT('',#79543);
#19374=VERTEX_POINT('',#79544);
#19375=VERTEX_POINT('',#79547);
#19376=VERTEX_POINT('',#79549);
#19377=VERTEX_POINT('',#79551);
#19378=VERTEX_POINT('',#79586);
#19379=VERTEX_POINT('',#79587);
#19380=VERTEX_POINT('',#79597);
#19381=VERTEX_POINT('',#79598);
#19382=VERTEX_POINT('',#79614);
#19383=VERTEX_POINT('',#79615);
#19384=VERTEX_POINT('',#79618);
#19385=VERTEX_POINT('',#79620);
#19386=VERTEX_POINT('',#79622);
#19387=VERTEX_POINT('',#79661);
#19388=VERTEX_POINT('',#79682);
#19389=VERTEX_POINT('',#79683);
#19390=VERTEX_POINT('',#79686);
#19391=VERTEX_POINT('',#79694);
#19392=VERTEX_POINT('',#79713);
#19393=VERTEX_POINT('',#79714);
#19394=VERTEX_POINT('',#79724);
#19395=VERTEX_POINT('',#79725);
#19396=VERTEX_POINT('',#79735);
#19397=VERTEX_POINT('',#79736);
#19398=VERTEX_POINT('',#79739);
#19399=VERTEX_POINT('',#79741);
#19400=VERTEX_POINT('',#79743);
#19401=VERTEX_POINT('',#79787);
#19402=VERTEX_POINT('',#79788);
#19403=VERTEX_POINT('',#79798);
#19404=VERTEX_POINT('',#79799);
#19405=VERTEX_POINT('',#79812);
#19406=VERTEX_POINT('',#79813);
#19407=VERTEX_POINT('',#79816);
#19408=VERTEX_POINT('',#79818);
#19409=VERTEX_POINT('',#79820);
#19410=VERTEX_POINT('',#79855);
#19411=VERTEX_POINT('',#79856);
#19412=VERTEX_POINT('',#79866);
#19413=VERTEX_POINT('',#79867);
#19414=VERTEX_POINT('',#79886);
#19415=VERTEX_POINT('',#79887);
#19416=VERTEX_POINT('',#79903);
#19417=VERTEX_POINT('',#79905);
#19418=VERTEX_POINT('',#79907);
#19419=VERTEX_POINT('',#79948);
#19420=VERTEX_POINT('',#79949);
#19421=VERTEX_POINT('',#79964);
#19422=VERTEX_POINT('',#79965);
#19423=VERTEX_POINT('',#79983);
#19424=VERTEX_POINT('',#79984);
#19425=VERTEX_POINT('',#79987);
#19426=VERTEX_POINT('',#79989);
#19427=VERTEX_POINT('',#79991);
#19428=VERTEX_POINT('',#80026);
#19429=VERTEX_POINT('',#80027);
#19430=VERTEX_POINT('',#80037);
#19431=VERTEX_POINT('',#80038);
#19432=VERTEX_POINT('',#80058);
#19433=VERTEX_POINT('',#80059);
#19434=VERTEX_POINT('',#80062);
#19435=VERTEX_POINT('',#80064);
#19436=VERTEX_POINT('',#80066);
#19437=VERTEX_POINT('',#80101);
#19438=VERTEX_POINT('',#80102);
#19439=VERTEX_POINT('',#80112);
#19440=VERTEX_POINT('',#80113);
#19441=VERTEX_POINT('',#80129);
#19442=VERTEX_POINT('',#80130);
#19443=VERTEX_POINT('',#80133);
#19444=VERTEX_POINT('',#80135);
#19445=VERTEX_POINT('',#80137);
#19446=VERTEX_POINT('',#80176);
#19447=VERTEX_POINT('',#80197);
#19448=VERTEX_POINT('',#80198);
#19449=VERTEX_POINT('',#80201);
#19450=VERTEX_POINT('',#80209);
#19451=VERTEX_POINT('',#80228);
#19452=VERTEX_POINT('',#80229);
#19453=VERTEX_POINT('',#80239);
#19454=VERTEX_POINT('',#80240);
#19455=VERTEX_POINT('',#80250);
#19456=VERTEX_POINT('',#80251);
#19457=VERTEX_POINT('',#80254);
#19458=VERTEX_POINT('',#80256);
#19459=VERTEX_POINT('',#80258);
#19460=VERTEX_POINT('',#80302);
#19461=VERTEX_POINT('',#80303);
#19462=VERTEX_POINT('',#80313);
#19463=VERTEX_POINT('',#80314);
#19464=VERTEX_POINT('',#80327);
#19465=VERTEX_POINT('',#80328);
#19466=VERTEX_POINT('',#80331);
#19467=VERTEX_POINT('',#80333);
#19468=VERTEX_POINT('',#80335);
#19469=VERTEX_POINT('',#80370);
#19470=VERTEX_POINT('',#80371);
#19471=VERTEX_POINT('',#80381);
#19472=VERTEX_POINT('',#80382);
#19473=VERTEX_POINT('',#80401);
#19474=VERTEX_POINT('',#80402);
#19475=VERTEX_POINT('',#80418);
#19476=VERTEX_POINT('',#80420);
#19477=VERTEX_POINT('',#80422);
#19478=VERTEX_POINT('',#80463);
#19479=VERTEX_POINT('',#80464);
#19480=VERTEX_POINT('',#80479);
#19481=VERTEX_POINT('',#80480);
#19482=VERTEX_POINT('',#80498);
#19483=VERTEX_POINT('',#80499);
#19484=VERTEX_POINT('',#80502);
#19485=VERTEX_POINT('',#80504);
#19486=VERTEX_POINT('',#80506);
#19487=VERTEX_POINT('',#80541);
#19488=VERTEX_POINT('',#80542);
#19489=VERTEX_POINT('',#80552);
#19490=VERTEX_POINT('',#80553);
#19491=VERTEX_POINT('',#80573);
#19492=VERTEX_POINT('',#80574);
#19493=VERTEX_POINT('',#80577);
#19494=VERTEX_POINT('',#80579);
#19495=VERTEX_POINT('',#80581);
#19496=VERTEX_POINT('',#80616);
#19497=VERTEX_POINT('',#80617);
#19498=VERTEX_POINT('',#80627);
#19499=VERTEX_POINT('',#80628);
#19500=VERTEX_POINT('',#80644);
#19501=VERTEX_POINT('',#80645);
#19502=VERTEX_POINT('',#80648);
#19503=VERTEX_POINT('',#80650);
#19504=VERTEX_POINT('',#80652);
#19505=VERTEX_POINT('',#80691);
#19506=VERTEX_POINT('',#80712);
#19507=VERTEX_POINT('',#80713);
#19508=VERTEX_POINT('',#80716);
#19509=VERTEX_POINT('',#80724);
#19510=VERTEX_POINT('',#80743);
#19511=VERTEX_POINT('',#80744);
#19512=VERTEX_POINT('',#80754);
#19513=VERTEX_POINT('',#80755);
#19514=VERTEX_POINT('',#80765);
#19515=VERTEX_POINT('',#80766);
#19516=VERTEX_POINT('',#80769);
#19517=VERTEX_POINT('',#80771);
#19518=VERTEX_POINT('',#80773);
#19519=VERTEX_POINT('',#80817);
#19520=VERTEX_POINT('',#80818);
#19521=VERTEX_POINT('',#80828);
#19522=VERTEX_POINT('',#80829);
#19523=VERTEX_POINT('',#80842);
#19524=VERTEX_POINT('',#80843);
#19525=VERTEX_POINT('',#80846);
#19526=VERTEX_POINT('',#80848);
#19527=VERTEX_POINT('',#80850);
#19528=VERTEX_POINT('',#80885);
#19529=VERTEX_POINT('',#80886);
#19530=VERTEX_POINT('',#80896);
#19531=VERTEX_POINT('',#80897);
#19532=VERTEX_POINT('',#80916);
#19533=VERTEX_POINT('',#80917);
#19534=VERTEX_POINT('',#80933);
#19535=VERTEX_POINT('',#80935);
#19536=VERTEX_POINT('',#80937);
#19537=VERTEX_POINT('',#80978);
#19538=VERTEX_POINT('',#80979);
#19539=VERTEX_POINT('',#80994);
#19540=VERTEX_POINT('',#80995);
#19541=VERTEX_POINT('',#81013);
#19542=VERTEX_POINT('',#81014);
#19543=VERTEX_POINT('',#81017);
#19544=VERTEX_POINT('',#81019);
#19545=VERTEX_POINT('',#81021);
#19546=VERTEX_POINT('',#81056);
#19547=VERTEX_POINT('',#81057);
#19548=VERTEX_POINT('',#81067);
#19549=VERTEX_POINT('',#81068);
#19550=VERTEX_POINT('',#81088);
#19551=VERTEX_POINT('',#81089);
#19552=VERTEX_POINT('',#81092);
#19553=VERTEX_POINT('',#81094);
#19554=VERTEX_POINT('',#81096);
#19555=VERTEX_POINT('',#81131);
#19556=VERTEX_POINT('',#81132);
#19557=VERTEX_POINT('',#81142);
#19558=VERTEX_POINT('',#81143);
#19559=VERTEX_POINT('',#81159);
#19560=VERTEX_POINT('',#81160);
#19561=VERTEX_POINT('',#81163);
#19562=VERTEX_POINT('',#81165);
#19563=VERTEX_POINT('',#81167);
#19564=VERTEX_POINT('',#81206);
#19565=VERTEX_POINT('',#81227);
#19566=VERTEX_POINT('',#81228);
#19567=VERTEX_POINT('',#81231);
#19568=VERTEX_POINT('',#81239);
#19569=VERTEX_POINT('',#81258);
#19570=VERTEX_POINT('',#81259);
#19571=VERTEX_POINT('',#81269);
#19572=VERTEX_POINT('',#81270);
#19573=VERTEX_POINT('',#81280);
#19574=VERTEX_POINT('',#81281);
#19575=VERTEX_POINT('',#81284);
#19576=VERTEX_POINT('',#81286);
#19577=VERTEX_POINT('',#81288);
#19578=VERTEX_POINT('',#81332);
#19579=VERTEX_POINT('',#81333);
#19580=VERTEX_POINT('',#81343);
#19581=VERTEX_POINT('',#81344);
#19582=VERTEX_POINT('',#81354);
#19583=VERTEX_POINT('',#81355);
#19584=VERTEX_POINT('',#81358);
#19585=VERTEX_POINT('',#81360);
#19586=VERTEX_POINT('',#81362);
#19587=VERTEX_POINT('',#81404);
#19588=VERTEX_POINT('',#81405);
#19589=VERTEX_POINT('',#81415);
#19590=VERTEX_POINT('',#81416);
#19591=VERTEX_POINT('',#81435);
#19592=VERTEX_POINT('',#81436);
#19593=VERTEX_POINT('',#81452);
#19594=VERTEX_POINT('',#81454);
#19595=VERTEX_POINT('',#81456);
#19596=VERTEX_POINT('',#81497);
#19597=VERTEX_POINT('',#81498);
#19598=VERTEX_POINT('',#81513);
#19599=VERTEX_POINT('',#81514);
#19600=VERTEX_POINT('',#81532);
#19601=VERTEX_POINT('',#81533);
#19602=VERTEX_POINT('',#81536);
#19603=VERTEX_POINT('',#81538);
#19604=VERTEX_POINT('',#81540);
#19605=VERTEX_POINT('',#81575);
#19606=VERTEX_POINT('',#81576);
#19607=VERTEX_POINT('',#81586);
#19608=VERTEX_POINT('',#81587);
#19609=VERTEX_POINT('',#81607);
#19610=VERTEX_POINT('',#81608);
#19611=VERTEX_POINT('',#81611);
#19612=VERTEX_POINT('',#81613);
#19613=VERTEX_POINT('',#81615);
#19614=VERTEX_POINT('',#81650);
#19615=VERTEX_POINT('',#81651);
#19616=VERTEX_POINT('',#81661);
#19617=VERTEX_POINT('',#81662);
#19618=VERTEX_POINT('',#81678);
#19619=VERTEX_POINT('',#81679);
#19620=VERTEX_POINT('',#81682);
#19621=VERTEX_POINT('',#81684);
#19622=VERTEX_POINT('',#81686);
#19623=VERTEX_POINT('',#81725);
#19624=VERTEX_POINT('',#81746);
#19625=VERTEX_POINT('',#81747);
#19626=VERTEX_POINT('',#81750);
#19627=VERTEX_POINT('',#81758);
#19628=VERTEX_POINT('',#81777);
#19629=VERTEX_POINT('',#81778);
#19630=VERTEX_POINT('',#81788);
#19631=VERTEX_POINT('',#81789);
#19632=VERTEX_POINT('',#81799);
#19633=VERTEX_POINT('',#81800);
#19634=VERTEX_POINT('',#81803);
#19635=VERTEX_POINT('',#81805);
#19636=VERTEX_POINT('',#81807);
#19637=VERTEX_POINT('',#81851);
#19638=VERTEX_POINT('',#81852);
#19639=VERTEX_POINT('',#81862);
#19640=VERTEX_POINT('',#81863);
#19641=VERTEX_POINT('',#81876);
#19642=VERTEX_POINT('',#81877);
#19643=VERTEX_POINT('',#81880);
#19644=VERTEX_POINT('',#81882);
#19645=VERTEX_POINT('',#81884);
#19646=VERTEX_POINT('',#81919);
#19647=VERTEX_POINT('',#81920);
#19648=VERTEX_POINT('',#81930);
#19649=VERTEX_POINT('',#81931);
#19650=VERTEX_POINT('',#81951);
#19651=VERTEX_POINT('',#81952);
#19652=VERTEX_POINT('',#81966);
#19653=VERTEX_POINT('',#81968);
#19654=VERTEX_POINT('',#81970);
#19655=VERTEX_POINT('',#82006);
#19656=VERTEX_POINT('',#82007);
#19657=VERTEX_POINT('',#82022);
#19658=VERTEX_POINT('',#82023);
#19659=VERTEX_POINT('',#82041);
#19660=VERTEX_POINT('',#82042);
#19661=VERTEX_POINT('',#82045);
#19662=VERTEX_POINT('',#82047);
#19663=VERTEX_POINT('',#82049);
#19664=VERTEX_POINT('',#82084);
#19665=VERTEX_POINT('',#82085);
#19666=VERTEX_POINT('',#82095);
#19667=VERTEX_POINT('',#82096);
#19668=VERTEX_POINT('',#82116);
#19669=VERTEX_POINT('',#82117);
#19670=VERTEX_POINT('',#82120);
#19671=VERTEX_POINT('',#82122);
#19672=VERTEX_POINT('',#82124);
#19673=VERTEX_POINT('',#82159);
#19674=VERTEX_POINT('',#82160);
#19675=VERTEX_POINT('',#82170);
#19676=VERTEX_POINT('',#82171);
#19677=VERTEX_POINT('',#82187);
#19678=VERTEX_POINT('',#82188);
#19679=VERTEX_POINT('',#82191);
#19680=VERTEX_POINT('',#82193);
#19681=VERTEX_POINT('',#82195);
#19682=VERTEX_POINT('',#82234);
#19683=VERTEX_POINT('',#82255);
#19684=VERTEX_POINT('',#82256);
#19685=VERTEX_POINT('',#82259);
#19686=VERTEX_POINT('',#82267);
#19687=VERTEX_POINT('',#82286);
#19688=VERTEX_POINT('',#82287);
#19689=VERTEX_POINT('',#82297);
#19690=VERTEX_POINT('',#82298);
#19691=VERTEX_POINT('',#82308);
#19692=VERTEX_POINT('',#82309);
#19693=VERTEX_POINT('',#82312);
#19694=VERTEX_POINT('',#82314);
#19695=VERTEX_POINT('',#82316);
#19696=VERTEX_POINT('',#82360);
#19697=VERTEX_POINT('',#82361);
#19698=VERTEX_POINT('',#82371);
#19699=VERTEX_POINT('',#82372);
#19700=VERTEX_POINT('',#82385);
#19701=VERTEX_POINT('',#82386);
#19702=VERTEX_POINT('',#82389);
#19703=VERTEX_POINT('',#82391);
#19704=VERTEX_POINT('',#82393);
#19705=VERTEX_POINT('',#82428);
#19706=VERTEX_POINT('',#82429);
#19707=VERTEX_POINT('',#82439);
#19708=VERTEX_POINT('',#82440);
#19709=VERTEX_POINT('',#82459);
#19710=VERTEX_POINT('',#82460);
#19711=VERTEX_POINT('',#82476);
#19712=VERTEX_POINT('',#82478);
#19713=VERTEX_POINT('',#82480);
#19714=VERTEX_POINT('',#82521);
#19715=VERTEX_POINT('',#82522);
#19716=VERTEX_POINT('',#82537);
#19717=VERTEX_POINT('',#82538);
#19718=VERTEX_POINT('',#82553);
#19719=VERTEX_POINT('',#82554);
#19720=VERTEX_POINT('',#82557);
#19721=VERTEX_POINT('',#82559);
#19722=VERTEX_POINT('',#82561);
#19723=VERTEX_POINT('',#82603);
#19724=VERTEX_POINT('',#82604);
#19725=VERTEX_POINT('',#82614);
#19726=VERTEX_POINT('',#82615);
#19727=VERTEX_POINT('',#82635);
#19728=VERTEX_POINT('',#82636);
#19729=VERTEX_POINT('',#82639);
#19730=VERTEX_POINT('',#82641);
#19731=VERTEX_POINT('',#82643);
#19732=VERTEX_POINT('',#82678);
#19733=VERTEX_POINT('',#82679);
#19734=VERTEX_POINT('',#82689);
#19735=VERTEX_POINT('',#82690);
#19736=VERTEX_POINT('',#82706);
#19737=VERTEX_POINT('',#82707);
#19738=VERTEX_POINT('',#82710);
#19739=VERTEX_POINT('',#82712);
#19740=VERTEX_POINT('',#82714);
#19741=VERTEX_POINT('',#82753);
#19742=VERTEX_POINT('',#82774);
#19743=VERTEX_POINT('',#82775);
#19744=VERTEX_POINT('',#82778);
#19745=VERTEX_POINT('',#82786);
#19746=VERTEX_POINT('',#82805);
#19747=VERTEX_POINT('',#82806);
#19748=VERTEX_POINT('',#82816);
#19749=VERTEX_POINT('',#82817);
#19750=VERTEX_POINT('',#82827);
#19751=VERTEX_POINT('',#82828);
#19752=VERTEX_POINT('',#82831);
#19753=VERTEX_POINT('',#82833);
#19754=VERTEX_POINT('',#82835);
#19755=VERTEX_POINT('',#82879);
#19756=VERTEX_POINT('',#82880);
#19757=VERTEX_POINT('',#82890);
#19758=VERTEX_POINT('',#82891);
#19759=VERTEX_POINT('',#82904);
#19760=VERTEX_POINT('',#82905);
#19761=VERTEX_POINT('',#82908);
#19762=VERTEX_POINT('',#82910);
#19763=VERTEX_POINT('',#82912);
#19764=VERTEX_POINT('',#82947);
#19765=VERTEX_POINT('',#82948);
#19766=VERTEX_POINT('',#82958);
#19767=VERTEX_POINT('',#82959);
#19768=VERTEX_POINT('',#82978);
#19769=VERTEX_POINT('',#82979);
#19770=VERTEX_POINT('',#82995);
#19771=VERTEX_POINT('',#82997);
#19772=VERTEX_POINT('',#82999);
#19773=VERTEX_POINT('',#83040);
#19774=VERTEX_POINT('',#83041);
#19775=VERTEX_POINT('',#83056);
#19776=VERTEX_POINT('',#83057);
#19777=VERTEX_POINT('',#83075);
#19778=VERTEX_POINT('',#83076);
#19779=VERTEX_POINT('',#83079);
#19780=VERTEX_POINT('',#83081);
#19781=VERTEX_POINT('',#83083);
#19782=VERTEX_POINT('',#83118);
#19783=VERTEX_POINT('',#83119);
#19784=VERTEX_POINT('',#83129);
#19785=VERTEX_POINT('',#83130);
#19786=VERTEX_POINT('',#83150);
#19787=VERTEX_POINT('',#83151);
#19788=VERTEX_POINT('',#83154);
#19789=VERTEX_POINT('',#83156);
#19790=VERTEX_POINT('',#83158);
#19791=VERTEX_POINT('',#83200);
#19792=VERTEX_POINT('',#83201);
#19793=VERTEX_POINT('',#83211);
#19794=VERTEX_POINT('',#83212);
#19795=VERTEX_POINT('',#83228);
#19796=VERTEX_POINT('',#83229);
#19797=VERTEX_POINT('',#83232);
#19798=VERTEX_POINT('',#83234);
#19799=VERTEX_POINT('',#83236);
#19800=VERTEX_POINT('',#83275);
#19801=VERTEX_POINT('',#83296);
#19802=VERTEX_POINT('',#83297);
#19803=VERTEX_POINT('',#83300);
#19804=VERTEX_POINT('',#83308);
#19805=VERTEX_POINT('',#83327);
#19806=VERTEX_POINT('',#83328);
#19807=VERTEX_POINT('',#83338);
#19808=VERTEX_POINT('',#83339);
#19809=VERTEX_POINT('',#83349);
#19810=VERTEX_POINT('',#83350);
#19811=VERTEX_POINT('',#83353);
#19812=VERTEX_POINT('',#83355);
#19813=VERTEX_POINT('',#83357);
#19814=VERTEX_POINT('',#83401);
#19815=VERTEX_POINT('',#83402);
#19816=VERTEX_POINT('',#83412);
#19817=VERTEX_POINT('',#83413);
#19818=VERTEX_POINT('',#83426);
#19819=VERTEX_POINT('',#83427);
#19820=VERTEX_POINT('',#83430);
#19821=VERTEX_POINT('',#83432);
#19822=VERTEX_POINT('',#83434);
#19823=VERTEX_POINT('',#83469);
#19824=VERTEX_POINT('',#83470);
#19825=VERTEX_POINT('',#83480);
#19826=VERTEX_POINT('',#83481);
#19827=VERTEX_POINT('',#83500);
#19828=VERTEX_POINT('',#83501);
#19829=VERTEX_POINT('',#83517);
#19830=VERTEX_POINT('',#83519);
#19831=VERTEX_POINT('',#83521);
#19832=VERTEX_POINT('',#83562);
#19833=VERTEX_POINT('',#83563);
#19834=VERTEX_POINT('',#83578);
#19835=VERTEX_POINT('',#83579);
#19836=VERTEX_POINT('',#83597);
#19837=VERTEX_POINT('',#83598);
#19838=VERTEX_POINT('',#83601);
#19839=VERTEX_POINT('',#83603);
#19840=VERTEX_POINT('',#83605);
#19841=VERTEX_POINT('',#83640);
#19842=VERTEX_POINT('',#83641);
#19843=VERTEX_POINT('',#83651);
#19844=VERTEX_POINT('',#83652);
#19845=VERTEX_POINT('',#83672);
#19846=VERTEX_POINT('',#83673);
#19847=VERTEX_POINT('',#83676);
#19848=VERTEX_POINT('',#83678);
#19849=VERTEX_POINT('',#83680);
#19850=VERTEX_POINT('',#83715);
#19851=VERTEX_POINT('',#83716);
#19852=VERTEX_POINT('',#83726);
#19853=VERTEX_POINT('',#83727);
#19854=VERTEX_POINT('',#83740);
#19855=VERTEX_POINT('',#83741);
#19856=VERTEX_POINT('',#83744);
#19857=VERTEX_POINT('',#83746);
#19858=VERTEX_POINT('',#83748);
#19859=VERTEX_POINT('',#83794);
#19860=VERTEX_POINT('',#83815);
#19861=VERTEX_POINT('',#83816);
#19862=VERTEX_POINT('',#83819);
#19863=VERTEX_POINT('',#83827);
#19864=VERTEX_POINT('',#83846);
#19865=VERTEX_POINT('',#83847);
#19866=VERTEX_POINT('',#83857);
#19867=VERTEX_POINT('',#83858);
#19868=VERTEX_POINT('',#83868);
#19869=VERTEX_POINT('',#83869);
#19870=VERTEX_POINT('',#83872);
#19871=VERTEX_POINT('',#83874);
#19872=VERTEX_POINT('',#83876);
#19873=VERTEX_POINT('',#83920);
#19874=VERTEX_POINT('',#83921);
#19875=VERTEX_POINT('',#83931);
#19876=VERTEX_POINT('',#83932);
#19877=VERTEX_POINT('',#83945);
#19878=VERTEX_POINT('',#83946);
#19879=VERTEX_POINT('',#83949);
#19880=VERTEX_POINT('',#83951);
#19881=VERTEX_POINT('',#83953);
#19882=VERTEX_POINT('',#83988);
#19883=VERTEX_POINT('',#83989);
#19884=VERTEX_POINT('',#83999);
#19885=VERTEX_POINT('',#84000);
#19886=VERTEX_POINT('',#84019);
#19887=VERTEX_POINT('',#84020);
#19888=VERTEX_POINT('',#84036);
#19889=VERTEX_POINT('',#84038);
#19890=VERTEX_POINT('',#84040);
#19891=VERTEX_POINT('',#84081);
#19892=VERTEX_POINT('',#84082);
#19893=VERTEX_POINT('',#84097);
#19894=VERTEX_POINT('',#84098);
#19895=VERTEX_POINT('',#84116);
#19896=VERTEX_POINT('',#84117);
#19897=VERTEX_POINT('',#84120);
#19898=VERTEX_POINT('',#84122);
#19899=VERTEX_POINT('',#84124);
#19900=VERTEX_POINT('',#84159);
#19901=VERTEX_POINT('',#84160);
#19902=VERTEX_POINT('',#84170);
#19903=VERTEX_POINT('',#84171);
#19904=VERTEX_POINT('',#84191);
#19905=VERTEX_POINT('',#84192);
#19906=VERTEX_POINT('',#84195);
#19907=VERTEX_POINT('',#84197);
#19908=VERTEX_POINT('',#84199);
#19909=VERTEX_POINT('',#84234);
#19910=VERTEX_POINT('',#84235);
#19911=VERTEX_POINT('',#84245);
#19912=VERTEX_POINT('',#84246);
#19913=VERTEX_POINT('',#84262);
#19914=VERTEX_POINT('',#84263);
#19915=VERTEX_POINT('',#84266);
#19916=VERTEX_POINT('',#84268);
#19917=VERTEX_POINT('',#84270);
#19918=VERTEX_POINT('',#84309);
#19919=VERTEX_POINT('',#84330);
#19920=VERTEX_POINT('',#84331);
#19921=VERTEX_POINT('',#84334);
#19922=VERTEX_POINT('',#84342);
#19923=VERTEX_POINT('',#84361);
#19924=VERTEX_POINT('',#84362);
#19925=VERTEX_POINT('',#84372);
#19926=VERTEX_POINT('',#84373);
#19927=VERTEX_POINT('',#84383);
#19928=VERTEX_POINT('',#84384);
#19929=VERTEX_POINT('',#84387);
#19930=VERTEX_POINT('',#84389);
#19931=VERTEX_POINT('',#84391);
#19932=VERTEX_POINT('',#84435);
#19933=VERTEX_POINT('',#84436);
#19934=VERTEX_POINT('',#84446);
#19935=VERTEX_POINT('',#84447);
#19936=VERTEX_POINT('',#84460);
#19937=VERTEX_POINT('',#84461);
#19938=VERTEX_POINT('',#84464);
#19939=VERTEX_POINT('',#84466);
#19940=VERTEX_POINT('',#84468);
#19941=VERTEX_POINT('',#84503);
#19942=VERTEX_POINT('',#84504);
#19943=VERTEX_POINT('',#84514);
#19944=VERTEX_POINT('',#84515);
#19945=VERTEX_POINT('',#84534);
#19946=VERTEX_POINT('',#84535);
#19947=VERTEX_POINT('',#84551);
#19948=VERTEX_POINT('',#84553);
#19949=VERTEX_POINT('',#84555);
#19950=VERTEX_POINT('',#84596);
#19951=VERTEX_POINT('',#84597);
#19952=VERTEX_POINT('',#84612);
#19953=VERTEX_POINT('',#84613);
#19954=VERTEX_POINT('',#84631);
#19955=VERTEX_POINT('',#84632);
#19956=VERTEX_POINT('',#84635);
#19957=VERTEX_POINT('',#84637);
#19958=VERTEX_POINT('',#84639);
#19959=VERTEX_POINT('',#84674);
#19960=VERTEX_POINT('',#84675);
#19961=VERTEX_POINT('',#84685);
#19962=VERTEX_POINT('',#84686);
#19963=VERTEX_POINT('',#84706);
#19964=VERTEX_POINT('',#84707);
#19965=VERTEX_POINT('',#84710);
#19966=VERTEX_POINT('',#84712);
#19967=VERTEX_POINT('',#84714);
#19968=VERTEX_POINT('',#84749);
#19969=VERTEX_POINT('',#84750);
#19970=VERTEX_POINT('',#84760);
#19971=VERTEX_POINT('',#84761);
#19972=VERTEX_POINT('',#84777);
#19973=VERTEX_POINT('',#84778);
#19974=VERTEX_POINT('',#84781);
#19975=VERTEX_POINT('',#84783);
#19976=VERTEX_POINT('',#84785);
#19977=VERTEX_POINT('',#84824);
#19978=VERTEX_POINT('',#84845);
#19979=VERTEX_POINT('',#84846);
#19980=VERTEX_POINT('',#84849);
#19981=VERTEX_POINT('',#84857);
#19982=VERTEX_POINT('',#84876);
#19983=VERTEX_POINT('',#84877);
#19984=VERTEX_POINT('',#84887);
#19985=VERTEX_POINT('',#84888);
#19986=VERTEX_POINT('',#84898);
#19987=VERTEX_POINT('',#84899);
#19988=VERTEX_POINT('',#84902);
#19989=VERTEX_POINT('',#84904);
#19990=VERTEX_POINT('',#84906);
#19991=VERTEX_POINT('',#84950);
#19992=VERTEX_POINT('',#84951);
#19993=VERTEX_POINT('',#84961);
#19994=VERTEX_POINT('',#84962);
#19995=VERTEX_POINT('',#84975);
#19996=VERTEX_POINT('',#84976);
#19997=VERTEX_POINT('',#84979);
#19998=VERTEX_POINT('',#84981);
#19999=VERTEX_POINT('',#84983);
#20000=VERTEX_POINT('',#85018);
#20001=VERTEX_POINT('',#85019);
#20002=VERTEX_POINT('',#85029);
#20003=VERTEX_POINT('',#85030);
#20004=VERTEX_POINT('',#85049);
#20005=VERTEX_POINT('',#85050);
#20006=VERTEX_POINT('',#85066);
#20007=VERTEX_POINT('',#85068);
#20008=VERTEX_POINT('',#85070);
#20009=VERTEX_POINT('',#85111);
#20010=VERTEX_POINT('',#85112);
#20011=VERTEX_POINT('',#85127);
#20012=VERTEX_POINT('',#85128);
#20013=VERTEX_POINT('',#85146);
#20014=VERTEX_POINT('',#85147);
#20015=VERTEX_POINT('',#85150);
#20016=VERTEX_POINT('',#85152);
#20017=VERTEX_POINT('',#85154);
#20018=VERTEX_POINT('',#85189);
#20019=VERTEX_POINT('',#85190);
#20020=VERTEX_POINT('',#85200);
#20021=VERTEX_POINT('',#85201);
#20022=VERTEX_POINT('',#85221);
#20023=VERTEX_POINT('',#85222);
#20024=VERTEX_POINT('',#85225);
#20025=VERTEX_POINT('',#85227);
#20026=VERTEX_POINT('',#85229);
#20027=VERTEX_POINT('',#85264);
#20028=VERTEX_POINT('',#85265);
#20029=VERTEX_POINT('',#85275);
#20030=VERTEX_POINT('',#85276);
#20031=VERTEX_POINT('',#85292);
#20032=VERTEX_POINT('',#85293);
#20033=VERTEX_POINT('',#85296);
#20034=VERTEX_POINT('',#85298);
#20035=VERTEX_POINT('',#85300);
#20036=VERTEX_POINT('',#85339);
#20037=VERTEX_POINT('',#85360);
#20038=VERTEX_POINT('',#85361);
#20039=VERTEX_POINT('',#85364);
#20040=VERTEX_POINT('',#85372);
#20041=VERTEX_POINT('',#85391);
#20042=VERTEX_POINT('',#85392);
#20043=VERTEX_POINT('',#85402);
#20044=VERTEX_POINT('',#85403);
#20045=VERTEX_POINT('',#85413);
#20046=VERTEX_POINT('',#85414);
#20047=VERTEX_POINT('',#85417);
#20048=VERTEX_POINT('',#85419);
#20049=VERTEX_POINT('',#85421);
#20050=VERTEX_POINT('',#85465);
#20051=VERTEX_POINT('',#85466);
#20052=VERTEX_POINT('',#85476);
#20053=VERTEX_POINT('',#85477);
#20054=VERTEX_POINT('',#85490);
#20055=VERTEX_POINT('',#85491);
#20056=VERTEX_POINT('',#85494);
#20057=VERTEX_POINT('',#85496);
#20058=VERTEX_POINT('',#85498);
#20059=VERTEX_POINT('',#85533);
#20060=VERTEX_POINT('',#85534);
#20061=VERTEX_POINT('',#85544);
#20062=VERTEX_POINT('',#85545);
#20063=VERTEX_POINT('',#85564);
#20064=VERTEX_POINT('',#85565);
#20065=VERTEX_POINT('',#85581);
#20066=VERTEX_POINT('',#85583);
#20067=VERTEX_POINT('',#85585);
#20068=VERTEX_POINT('',#85626);
#20069=VERTEX_POINT('',#85627);
#20070=VERTEX_POINT('',#85642);
#20071=VERTEX_POINT('',#85643);
#20072=VERTEX_POINT('',#85661);
#20073=VERTEX_POINT('',#85662);
#20074=VERTEX_POINT('',#85665);
#20075=VERTEX_POINT('',#85667);
#20076=VERTEX_POINT('',#85669);
#20077=VERTEX_POINT('',#85704);
#20078=VERTEX_POINT('',#85705);
#20079=VERTEX_POINT('',#85715);
#20080=VERTEX_POINT('',#85716);
#20081=VERTEX_POINT('',#85736);
#20082=VERTEX_POINT('',#85737);
#20083=VERTEX_POINT('',#85740);
#20084=VERTEX_POINT('',#85742);
#20085=VERTEX_POINT('',#85744);
#20086=VERTEX_POINT('',#85779);
#20087=VERTEX_POINT('',#85780);
#20088=VERTEX_POINT('',#85790);
#20089=VERTEX_POINT('',#85791);
#20090=VERTEX_POINT('',#85807);
#20091=VERTEX_POINT('',#85808);
#20092=VERTEX_POINT('',#85811);
#20093=VERTEX_POINT('',#85813);
#20094=VERTEX_POINT('',#85815);
#20095=VERTEX_POINT('',#85854);
#20096=VERTEX_POINT('',#85875);
#20097=VERTEX_POINT('',#85876);
#20098=VERTEX_POINT('',#85879);
#20099=VERTEX_POINT('',#85887);
#20100=VERTEX_POINT('',#85906);
#20101=VERTEX_POINT('',#85907);
#20102=VERTEX_POINT('',#85917);
#20103=VERTEX_POINT('',#85918);
#20104=VERTEX_POINT('',#85928);
#20105=VERTEX_POINT('',#85929);
#20106=VERTEX_POINT('',#85932);
#20107=VERTEX_POINT('',#85934);
#20108=VERTEX_POINT('',#85936);
#20109=VERTEX_POINT('',#85980);
#20110=VERTEX_POINT('',#85981);
#20111=VERTEX_POINT('',#85991);
#20112=VERTEX_POINT('',#85992);
#20113=VERTEX_POINT('',#86005);
#20114=VERTEX_POINT('',#86006);
#20115=VERTEX_POINT('',#86009);
#20116=VERTEX_POINT('',#86011);
#20117=VERTEX_POINT('',#86013);
#20118=VERTEX_POINT('',#86048);
#20119=VERTEX_POINT('',#86049);
#20120=VERTEX_POINT('',#86059);
#20121=VERTEX_POINT('',#86060);
#20122=VERTEX_POINT('',#86079);
#20123=VERTEX_POINT('',#86080);
#20124=VERTEX_POINT('',#86096);
#20125=VERTEX_POINT('',#86098);
#20126=VERTEX_POINT('',#86100);
#20127=VERTEX_POINT('',#86141);
#20128=VERTEX_POINT('',#86142);
#20129=VERTEX_POINT('',#86157);
#20130=VERTEX_POINT('',#86158);
#20131=VERTEX_POINT('',#86176);
#20132=VERTEX_POINT('',#86177);
#20133=VERTEX_POINT('',#86180);
#20134=VERTEX_POINT('',#86182);
#20135=VERTEX_POINT('',#86184);
#20136=VERTEX_POINT('',#86219);
#20137=VERTEX_POINT('',#86220);
#20138=VERTEX_POINT('',#86230);
#20139=VERTEX_POINT('',#86231);
#20140=VERTEX_POINT('',#86251);
#20141=VERTEX_POINT('',#86252);
#20142=VERTEX_POINT('',#86255);
#20143=VERTEX_POINT('',#86257);
#20144=VERTEX_POINT('',#86259);
#20145=VERTEX_POINT('',#86294);
#20146=VERTEX_POINT('',#86295);
#20147=VERTEX_POINT('',#86305);
#20148=VERTEX_POINT('',#86306);
#20149=VERTEX_POINT('',#86322);
#20150=VERTEX_POINT('',#86323);
#20151=VERTEX_POINT('',#86326);
#20152=VERTEX_POINT('',#86328);
#20153=VERTEX_POINT('',#86330);
#20154=VERTEX_POINT('',#86369);
#20155=VERTEX_POINT('',#86390);
#20156=VERTEX_POINT('',#86391);
#20157=VERTEX_POINT('',#86394);
#20158=VERTEX_POINT('',#86402);
#20159=VERTEX_POINT('',#86421);
#20160=VERTEX_POINT('',#86422);
#20161=VERTEX_POINT('',#86432);
#20162=VERTEX_POINT('',#86433);
#20163=VERTEX_POINT('',#86443);
#20164=VERTEX_POINT('',#86444);
#20165=VERTEX_POINT('',#86447);
#20166=VERTEX_POINT('',#86449);
#20167=VERTEX_POINT('',#86451);
#20168=VERTEX_POINT('',#86495);
#20169=VERTEX_POINT('',#86496);
#20170=VERTEX_POINT('',#86506);
#20171=VERTEX_POINT('',#86507);
#20172=VERTEX_POINT('',#86520);
#20173=VERTEX_POINT('',#86521);
#20174=VERTEX_POINT('',#86524);
#20175=VERTEX_POINT('',#86526);
#20176=VERTEX_POINT('',#86528);
#20177=VERTEX_POINT('',#86563);
#20178=VERTEX_POINT('',#86564);
#20179=VERTEX_POINT('',#86574);
#20180=VERTEX_POINT('',#86575);
#20181=VERTEX_POINT('',#86594);
#20182=VERTEX_POINT('',#86595);
#20183=VERTEX_POINT('',#86611);
#20184=VERTEX_POINT('',#86613);
#20185=VERTEX_POINT('',#86615);
#20186=VERTEX_POINT('',#86656);
#20187=VERTEX_POINT('',#86657);
#20188=VERTEX_POINT('',#86672);
#20189=VERTEX_POINT('',#86673);
#20190=VERTEX_POINT('',#86691);
#20191=VERTEX_POINT('',#86692);
#20192=VERTEX_POINT('',#86695);
#20193=VERTEX_POINT('',#86697);
#20194=VERTEX_POINT('',#86699);
#20195=VERTEX_POINT('',#86734);
#20196=VERTEX_POINT('',#86735);
#20197=VERTEX_POINT('',#86745);
#20198=VERTEX_POINT('',#86746);
#20199=VERTEX_POINT('',#86766);
#20200=VERTEX_POINT('',#86767);
#20201=VERTEX_POINT('',#86770);
#20202=VERTEX_POINT('',#86772);
#20203=VERTEX_POINT('',#86774);
#20204=VERTEX_POINT('',#86809);
#20205=VERTEX_POINT('',#86810);
#20206=VERTEX_POINT('',#86820);
#20207=VERTEX_POINT('',#86821);
#20208=VERTEX_POINT('',#86837);
#20209=VERTEX_POINT('',#86838);
#20210=VERTEX_POINT('',#86841);
#20211=VERTEX_POINT('',#86843);
#20212=VERTEX_POINT('',#86845);
#20213=VERTEX_POINT('',#86884);
#20214=VERTEX_POINT('',#86905);
#20215=VERTEX_POINT('',#86906);
#20216=VERTEX_POINT('',#86909);
#20217=VERTEX_POINT('',#86917);
#20218=VERTEX_POINT('',#86936);
#20219=VERTEX_POINT('',#86937);
#20220=VERTEX_POINT('',#86947);
#20221=VERTEX_POINT('',#86948);
#20222=VERTEX_POINT('',#86958);
#20223=VERTEX_POINT('',#86959);
#20224=VERTEX_POINT('',#86962);
#20225=VERTEX_POINT('',#86964);
#20226=VERTEX_POINT('',#86966);
#20227=VERTEX_POINT('',#87010);
#20228=VERTEX_POINT('',#87011);
#20229=VERTEX_POINT('',#87021);
#20230=VERTEX_POINT('',#87022);
#20231=VERTEX_POINT('',#87035);
#20232=VERTEX_POINT('',#87036);
#20233=VERTEX_POINT('',#87039);
#20234=VERTEX_POINT('',#87041);
#20235=VERTEX_POINT('',#87043);
#20236=VERTEX_POINT('',#87078);
#20237=VERTEX_POINT('',#87079);
#20238=VERTEX_POINT('',#87089);
#20239=VERTEX_POINT('',#87090);
#20240=VERTEX_POINT('',#87109);
#20241=VERTEX_POINT('',#87110);
#20242=VERTEX_POINT('',#87126);
#20243=VERTEX_POINT('',#87128);
#20244=VERTEX_POINT('',#87130);
#20245=VERTEX_POINT('',#87171);
#20246=VERTEX_POINT('',#87172);
#20247=VERTEX_POINT('',#87187);
#20248=VERTEX_POINT('',#87188);
#20249=VERTEX_POINT('',#87206);
#20250=VERTEX_POINT('',#87207);
#20251=VERTEX_POINT('',#87210);
#20252=VERTEX_POINT('',#87212);
#20253=VERTEX_POINT('',#87214);
#20254=VERTEX_POINT('',#87249);
#20255=VERTEX_POINT('',#87250);
#20256=VERTEX_POINT('',#87260);
#20257=VERTEX_POINT('',#87261);
#20258=VERTEX_POINT('',#87281);
#20259=VERTEX_POINT('',#87282);
#20260=VERTEX_POINT('',#87285);
#20261=VERTEX_POINT('',#87287);
#20262=VERTEX_POINT('',#87289);
#20263=VERTEX_POINT('',#87324);
#20264=VERTEX_POINT('',#87325);
#20265=VERTEX_POINT('',#87335);
#20266=VERTEX_POINT('',#87336);
#20267=VERTEX_POINT('',#87352);
#20268=VERTEX_POINT('',#87353);
#20269=VERTEX_POINT('',#87356);
#20270=VERTEX_POINT('',#87358);
#20271=VERTEX_POINT('',#87360);
#20272=VERTEX_POINT('',#87399);
#20273=VERTEX_POINT('',#87420);
#20274=VERTEX_POINT('',#87421);
#20275=VERTEX_POINT('',#87424);
#20276=VERTEX_POINT('',#87432);
#20277=VERTEX_POINT('',#87451);
#20278=VERTEX_POINT('',#87452);
#20279=VERTEX_POINT('',#87462);
#20280=VERTEX_POINT('',#87463);
#20281=VERTEX_POINT('',#87473);
#20282=VERTEX_POINT('',#87474);
#20283=VERTEX_POINT('',#87477);
#20284=VERTEX_POINT('',#87479);
#20285=VERTEX_POINT('',#87481);
#20286=VERTEX_POINT('',#87525);
#20287=VERTEX_POINT('',#87526);
#20288=VERTEX_POINT('',#87536);
#20289=VERTEX_POINT('',#87537);
#20290=VERTEX_POINT('',#87550);
#20291=VERTEX_POINT('',#87551);
#20292=VERTEX_POINT('',#87554);
#20293=VERTEX_POINT('',#87556);
#20294=VERTEX_POINT('',#87558);
#20295=VERTEX_POINT('',#87593);
#20296=VERTEX_POINT('',#87594);
#20297=VERTEX_POINT('',#87604);
#20298=VERTEX_POINT('',#87605);
#20299=VERTEX_POINT('',#87624);
#20300=VERTEX_POINT('',#87625);
#20301=VERTEX_POINT('',#87641);
#20302=VERTEX_POINT('',#87643);
#20303=VERTEX_POINT('',#87645);
#20304=VERTEX_POINT('',#87686);
#20305=VERTEX_POINT('',#87687);
#20306=VERTEX_POINT('',#87702);
#20307=VERTEX_POINT('',#87703);
#20308=VERTEX_POINT('',#87721);
#20309=VERTEX_POINT('',#87722);
#20310=VERTEX_POINT('',#87725);
#20311=VERTEX_POINT('',#87727);
#20312=VERTEX_POINT('',#87729);
#20313=VERTEX_POINT('',#87764);
#20314=VERTEX_POINT('',#87765);
#20315=VERTEX_POINT('',#87775);
#20316=VERTEX_POINT('',#87776);
#20317=VERTEX_POINT('',#87796);
#20318=VERTEX_POINT('',#87797);
#20319=VERTEX_POINT('',#87800);
#20320=VERTEX_POINT('',#87802);
#20321=VERTEX_POINT('',#87804);
#20322=VERTEX_POINT('',#87839);
#20323=VERTEX_POINT('',#87840);
#20324=VERTEX_POINT('',#87850);
#20325=VERTEX_POINT('',#87851);
#20326=VERTEX_POINT('',#87867);
#20327=VERTEX_POINT('',#87868);
#20328=VERTEX_POINT('',#87871);
#20329=VERTEX_POINT('',#87873);
#20330=VERTEX_POINT('',#87875);
#20331=VERTEX_POINT('',#87914);
#20332=VERTEX_POINT('',#87920);
#20333=VERTEX_POINT('',#87921);
#20334=VERTEX_POINT('',#87923);
#20335=VERTEX_POINT('',#87925);
#20336=VERTEX_POINT('',#87944);
#20337=VERTEX_POINT('',#87945);
#20338=VERTEX_POINT('',#87948);
#20339=VERTEX_POINT('',#87956);
#20340=VERTEX_POINT('',#87988);
#20341=VERTEX_POINT('',#87989);
#20342=VERTEX_POINT('',#87992);
#20343=VERTEX_POINT('',#87994);
#20344=VERTEX_POINT('',#87996);
#20345=VERTEX_POINT('',#88040);
#20346=VERTEX_POINT('',#88041);
#20347=VERTEX_POINT('',#88051);
#20348=VERTEX_POINT('',#88052);
#20349=VERTEX_POINT('',#88065);
#20350=VERTEX_POINT('',#88066);
#20351=VERTEX_POINT('',#88069);
#20352=VERTEX_POINT('',#88071);
#20353=VERTEX_POINT('',#88073);
#20354=VERTEX_POINT('',#88108);
#20355=VERTEX_POINT('',#88109);
#20356=VERTEX_POINT('',#88119);
#20357=VERTEX_POINT('',#88120);
#20358=VERTEX_POINT('',#88139);
#20359=VERTEX_POINT('',#88140);
#20360=VERTEX_POINT('',#88156);
#20361=VERTEX_POINT('',#88158);
#20362=VERTEX_POINT('',#88160);
#20363=VERTEX_POINT('',#88201);
#20364=VERTEX_POINT('',#88202);
#20365=VERTEX_POINT('',#88217);
#20366=VERTEX_POINT('',#88218);
#20367=VERTEX_POINT('',#88236);
#20368=VERTEX_POINT('',#88237);
#20369=VERTEX_POINT('',#88240);
#20370=VERTEX_POINT('',#88242);
#20371=VERTEX_POINT('',#88244);
#20372=VERTEX_POINT('',#88279);
#20373=VERTEX_POINT('',#88280);
#20374=VERTEX_POINT('',#88290);
#20375=VERTEX_POINT('',#88291);
#20376=VERTEX_POINT('',#88311);
#20377=VERTEX_POINT('',#88312);
#20378=VERTEX_POINT('',#88315);
#20379=VERTEX_POINT('',#88317);
#20380=VERTEX_POINT('',#88319);
#20381=VERTEX_POINT('',#88354);
#20382=VERTEX_POINT('',#88355);
#20383=VERTEX_POINT('',#88365);
#20384=VERTEX_POINT('',#88366);
#20385=VERTEX_POINT('',#88382);
#20386=VERTEX_POINT('',#88383);
#20387=VERTEX_POINT('',#88386);
#20388=VERTEX_POINT('',#88388);
#20389=VERTEX_POINT('',#88390);
#20390=VERTEX_POINT('',#88429);
#20391=VERTEX_POINT('',#88435);
#20392=VERTEX_POINT('',#88436);
#20393=VERTEX_POINT('',#88438);
#20394=VERTEX_POINT('',#88440);
#20395=VERTEX_POINT('',#88444);
#20396=VERTEX_POINT('',#88445);
#20397=VERTEX_POINT('',#88447);
#20398=VERTEX_POINT('',#88449);
#20399=VERTEX_POINT('',#88468);
#20400=VERTEX_POINT('',#88469);
#20401=VERTEX_POINT('',#88472);
#20402=VERTEX_POINT('',#88480);
#20403=VERTEX_POINT('',#88515);
#20404=VERTEX_POINT('',#88516);
#20405=VERTEX_POINT('',#88519);
#20406=VERTEX_POINT('',#88521);
#20407=VERTEX_POINT('',#88523);
#20408=VERTEX_POINT('',#88580);
#20409=VERTEX_POINT('',#88581);
#20410=VERTEX_POINT('',#88584);
#20411=VERTEX_POINT('',#88586);
#20412=VERTEX_POINT('',#88588);
#20413=VERTEX_POINT('',#88630);
#20414=VERTEX_POINT('',#88631);
#20415=VERTEX_POINT('',#88641);
#20416=VERTEX_POINT('',#88642);
#20417=VERTEX_POINT('',#88661);
#20418=VERTEX_POINT('',#88662);
#20419=VERTEX_POINT('',#88678);
#20420=VERTEX_POINT('',#88680);
#20421=VERTEX_POINT('',#88682);
#20422=VERTEX_POINT('',#88723);
#20423=VERTEX_POINT('',#88724);
#20424=VERTEX_POINT('',#88739);
#20425=VERTEX_POINT('',#88740);
#20426=VERTEX_POINT('',#88758);
#20427=VERTEX_POINT('',#88759);
#20428=VERTEX_POINT('',#88762);
#20429=VERTEX_POINT('',#88764);
#20430=VERTEX_POINT('',#88766);
#20431=VERTEX_POINT('',#88801);
#20432=VERTEX_POINT('',#88802);
#20433=VERTEX_POINT('',#88812);
#20434=VERTEX_POINT('',#88813);
#20435=VERTEX_POINT('',#88833);
#20436=VERTEX_POINT('',#88834);
#20437=VERTEX_POINT('',#88837);
#20438=VERTEX_POINT('',#88839);
#20439=VERTEX_POINT('',#88841);
#20440=VERTEX_POINT('',#88876);
#20441=VERTEX_POINT('',#88877);
#20442=VERTEX_POINT('',#88887);
#20443=VERTEX_POINT('',#88888);
#20444=VERTEX_POINT('',#88904);
#20445=VERTEX_POINT('',#88905);
#20446=VERTEX_POINT('',#88908);
#20447=VERTEX_POINT('',#88910);
#20448=VERTEX_POINT('',#88912);
#20449=VERTEX_POINT('',#88951);
#20450=VERTEX_POINT('',#88957);
#20451=VERTEX_POINT('',#88958);
#20452=VERTEX_POINT('',#88960);
#20453=VERTEX_POINT('',#88962);
#20454=VERTEX_POINT('',#88966);
#20455=VERTEX_POINT('',#88967);
#20456=VERTEX_POINT('',#88969);
#20457=VERTEX_POINT('',#88971);
#20458=VERTEX_POINT('',#88975);
#20459=VERTEX_POINT('',#88976);
#20460=VERTEX_POINT('',#88978);
#20461=VERTEX_POINT('',#88980);
#20462=VERTEX_POINT('',#88989);
#20463=VERTEX_POINT('',#88990);
#20464=VERTEX_POINT('',#88993);
#20465=VERTEX_POINT('',#88995);
#20466=VERTEX_POINT('',#88997);
#20467=VERTEX_POINT('',#89060);
#20468=VERTEX_POINT('',#89061);
#20469=VERTEX_POINT('',#89064);
#20470=VERTEX_POINT('',#89066);
#20471=VERTEX_POINT('',#89068);
#20472=VERTEX_POINT('',#89126);
#20473=VERTEX_POINT('',#89127);
#20474=VERTEX_POINT('',#89141);
#20475=VERTEX_POINT('',#89143);
#20476=VERTEX_POINT('',#89145);
#20477=VERTEX_POINT('',#89181);
#20478=VERTEX_POINT('',#89182);
#20479=VERTEX_POINT('',#89205);
#20480=VERTEX_POINT('',#89206);
#20481=VERTEX_POINT('',#89209);
#20482=VERTEX_POINT('',#89217);
#20483=VERTEX_POINT('',#89244);
#20484=VERTEX_POINT('',#89245);
#20485=VERTEX_POINT('',#89263);
#20486=VERTEX_POINT('',#89264);
#20487=VERTEX_POINT('',#89267);
#20488=VERTEX_POINT('',#89269);
#20489=VERTEX_POINT('',#89271);
#20490=VERTEX_POINT('',#89306);
#20491=VERTEX_POINT('',#89307);
#20492=VERTEX_POINT('',#89317);
#20493=VERTEX_POINT('',#89318);
#20494=VERTEX_POINT('',#89338);
#20495=VERTEX_POINT('',#89339);
#20496=VERTEX_POINT('',#89342);
#20497=VERTEX_POINT('',#89344);
#20498=VERTEX_POINT('',#89346);
#20499=VERTEX_POINT('',#89381);
#20500=VERTEX_POINT('',#89382);
#20501=VERTEX_POINT('',#89392);
#20502=VERTEX_POINT('',#89393);
#20503=VERTEX_POINT('',#89409);
#20504=VERTEX_POINT('',#89410);
#20505=VERTEX_POINT('',#89413);
#20506=VERTEX_POINT('',#89415);
#20507=VERTEX_POINT('',#89417);
#20508=VERTEX_POINT('',#89456);
#20509=VERTEX_POINT('',#89462);
#20510=VERTEX_POINT('',#89463);
#20511=VERTEX_POINT('',#89465);
#20512=VERTEX_POINT('',#89467);
#20513=VERTEX_POINT('',#89471);
#20514=VERTEX_POINT('',#89472);
#20515=VERTEX_POINT('',#89474);
#20516=VERTEX_POINT('',#89476);
#20517=VERTEX_POINT('',#89480);
#20518=VERTEX_POINT('',#89481);
#20519=VERTEX_POINT('',#89483);
#20520=VERTEX_POINT('',#89490);
#20521=VERTEX_POINT('',#89499);
#20522=VERTEX_POINT('',#89500);
#20523=VERTEX_POINT('',#89502);
#20524=VERTEX_POINT('',#89504);
#20525=VERTEX_POINT('',#89513);
#20526=VERTEX_POINT('',#89514);
#20527=VERTEX_POINT('',#89517);
#20528=VERTEX_POINT('',#89519);
#20529=VERTEX_POINT('',#89521);
#20530=VERTEX_POINT('',#89590);
#20531=VERTEX_POINT('',#89591);
#20532=VERTEX_POINT('',#89607);
#20533=VERTEX_POINT('',#89609);
#20534=VERTEX_POINT('',#89611);
#20535=VERTEX_POINT('',#89665);
#20536=VERTEX_POINT('',#89666);
#20537=VERTEX_POINT('',#89669);
#20538=VERTEX_POINT('',#89671);
#20539=VERTEX_POINT('',#89673);
#20540=VERTEX_POINT('',#89715);
#20541=VERTEX_POINT('',#89716);
#20542=VERTEX_POINT('',#89734);
#20543=VERTEX_POINT('',#89735);
#20544=VERTEX_POINT('',#89738);
#20545=VERTEX_POINT('',#89746);
#20546=VERTEX_POINT('',#89784);
#20547=VERTEX_POINT('',#89785);
#20548=VERTEX_POINT('',#89788);
#20549=VERTEX_POINT('',#89790);
#20550=VERTEX_POINT('',#89792);
#20551=VERTEX_POINT('',#89844);
#20552=VERTEX_POINT('',#89845);
#20553=VERTEX_POINT('',#89865);
#20554=VERTEX_POINT('',#89866);
#20555=VERTEX_POINT('',#89869);
#20556=VERTEX_POINT('',#89871);
#20557=VERTEX_POINT('',#89873);
#20558=VERTEX_POINT('',#89908);
#20559=VERTEX_POINT('',#89909);
#20560=VERTEX_POINT('',#89919);
#20561=VERTEX_POINT('',#89920);
#20562=VERTEX_POINT('',#89936);
#20563=VERTEX_POINT('',#89937);
#20564=VERTEX_POINT('',#89940);
#20565=VERTEX_POINT('',#89942);
#20566=VERTEX_POINT('',#89944);
#20567=VERTEX_POINT('',#89983);
#20568=VERTEX_POINT('',#89989);
#20569=VERTEX_POINT('',#89990);
#20570=VERTEX_POINT('',#89992);
#20571=VERTEX_POINT('',#89994);
#20572=VERTEX_POINT('',#89998);
#20573=VERTEX_POINT('',#89999);
#20574=VERTEX_POINT('',#90001);
#20575=VERTEX_POINT('',#90003);
#20576=VERTEX_POINT('',#90007);
#20577=VERTEX_POINT('',#90008);
#20578=VERTEX_POINT('',#90010);
#20579=VERTEX_POINT('',#90012);
#20580=VERTEX_POINT('',#90016);
#20581=VERTEX_POINT('',#90017);
#20582=VERTEX_POINT('',#90019);
#20583=VERTEX_POINT('',#90021);
#20584=VERTEX_POINT('',#90025);
#20585=VERTEX_POINT('',#90026);
#20586=VERTEX_POINT('',#90028);
#20587=VERTEX_POINT('',#90035);
#20588=VERTEX_POINT('',#90059);
#20589=VERTEX_POINT('',#90060);
#20590=VERTEX_POINT('',#90074);
#20591=VERTEX_POINT('',#90076);
#20592=VERTEX_POINT('',#90078);
#20593=VERTEX_POINT('',#90133);
#20594=VERTEX_POINT('',#90134);
#20595=VERTEX_POINT('',#90137);
#20596=VERTEX_POINT('',#90139);
#20597=VERTEX_POINT('',#90141);
#20598=VERTEX_POINT('',#90199);
#20599=VERTEX_POINT('',#90200);
#20600=VERTEX_POINT('',#90203);
#20601=VERTEX_POINT('',#90205);
#20602=VERTEX_POINT('',#90207);
#20603=VERTEX_POINT('',#90249);
#20604=VERTEX_POINT('',#90250);
#20605=VERTEX_POINT('',#90275);
#20606=VERTEX_POINT('',#90276);
#20607=VERTEX_POINT('',#90279);
#20608=VERTEX_POINT('',#90287);
#20609=VERTEX_POINT('',#90318);
#20610=VERTEX_POINT('',#90319);
#20611=VERTEX_POINT('',#90322);
#20612=VERTEX_POINT('',#90324);
#20613=VERTEX_POINT('',#90326);
#20614=VERTEX_POINT('',#90389);
#20615=VERTEX_POINT('',#90390);
#20616=VERTEX_POINT('',#90393);
#20617=VERTEX_POINT('',#90395);
#20618=VERTEX_POINT('',#90397);
#20619=VERTEX_POINT('',#90440);
#20620=VERTEX_POINT('',#90441);
#20621=VERTEX_POINT('',#90457);
#20622=VERTEX_POINT('',#90458);
#20623=VERTEX_POINT('',#90461);
#20624=VERTEX_POINT('',#90463);
#20625=VERTEX_POINT('',#90465);
#20626=VERTEX_POINT('',#90504);
#20627=VERTEX_POINT('',#90510);
#20628=VERTEX_POINT('',#90511);
#20629=VERTEX_POINT('',#90513);
#20630=VERTEX_POINT('',#90515);
#20631=VERTEX_POINT('',#90519);
#20632=VERTEX_POINT('',#90520);
#20633=VERTEX_POINT('',#90522);
#20634=VERTEX_POINT('',#90529);
#20635=VERTEX_POINT('',#90538);
#20636=VERTEX_POINT('',#90539);
#20637=VERTEX_POINT('',#90541);
#20638=VERTEX_POINT('',#90543);
#20639=VERTEX_POINT('',#90547);
#20640=VERTEX_POINT('',#90548);
#20641=VERTEX_POINT('',#90550);
#20642=VERTEX_POINT('',#90552);
#20643=VERTEX_POINT('',#90556);
#20644=VERTEX_POINT('',#90557);
#20645=VERTEX_POINT('',#90559);
#20646=VERTEX_POINT('',#90561);
#20647=VERTEX_POINT('',#90565);
#20648=VERTEX_POINT('',#90566);
#20649=VERTEX_POINT('',#90568);
#20650=VERTEX_POINT('',#90570);
#20651=VERTEX_POINT('',#90579);
#20652=VERTEX_POINT('',#90580);
#20653=VERTEX_POINT('',#90583);
#20654=VERTEX_POINT('',#90585);
#20655=VERTEX_POINT('',#90647);
#20656=VERTEX_POINT('',#90648);
#20657=VERTEX_POINT('',#90651);
#20658=VERTEX_POINT('',#90653);
#20659=VERTEX_POINT('',#90705);
#20660=VERTEX_POINT('',#90706);
#20661=VERTEX_POINT('',#90709);
#20662=VERTEX_POINT('',#90711);
#20663=VERTEX_POINT('',#90713);
#20664=VERTEX_POINT('',#90766);
#20665=VERTEX_POINT('',#90767);
#20666=VERTEX_POINT('',#90770);
#20667=VERTEX_POINT('',#90805);
#20668=VERTEX_POINT('',#90806);
#20669=VERTEX_POINT('',#90809);
#20670=VERTEX_POINT('',#90811);
#20671=VERTEX_POINT('',#90868);
#20672=VERTEX_POINT('',#90869);
#20673=VERTEX_POINT('',#90872);
#20674=VERTEX_POINT('',#90874);
#20675=VERTEX_POINT('',#90937);
#20676=VERTEX_POINT('',#90938);
#20677=VERTEX_POINT('',#90954);
#20678=VERTEX_POINT('',#90956);
#20679=VERTEX_POINT('',#91007);
#20680=VERTEX_POINT('',#91014);
#20681=VERTEX_POINT('',#106226);
#20682=VERTEX_POINT('',#106228);
#20683=VERTEX_POINT('',#106232);
#20684=VERTEX_POINT('',#106234);
#20685=VERTEX_POINT('',#106238);
#20686=VERTEX_POINT('',#106240);
#20687=VERTEX_POINT('',#106248);
#20688=VERTEX_POINT('',#106250);
#20689=VERTEX_POINT('',#106254);
#20690=VERTEX_POINT('',#106256);
#20691=VERTEX_POINT('',#106263);
#20692=VERTEX_POINT('',#106265);
#20693=VERTEX_POINT('',#106269);
#20694=VERTEX_POINT('',#106271);
#20695=VERTEX_POINT('',#106275);
#20696=VERTEX_POINT('',#106277);
#20697=VERTEX_POINT('',#106281);
#20698=VERTEX_POINT('',#106283);
#20699=VERTEX_POINT('',#106287);
#20700=VERTEX_POINT('',#106288);
#20701=VERTEX_POINT('',#106290);
#20702=VERTEX_POINT('',#106292);
#20703=VERTEX_POINT('',#106296);
#20704=VERTEX_POINT('',#106297);
#20705=VERTEX_POINT('',#106299);
#20706=VERTEX_POINT('',#106301);
#20707=VERTEX_POINT('',#106305);
#20708=VERTEX_POINT('',#106306);
#20709=VERTEX_POINT('',#106308);
#20710=VERTEX_POINT('',#106310);
#20711=VERTEX_POINT('',#106314);
#20712=VERTEX_POINT('',#106315);
#20713=VERTEX_POINT('',#106317);
#20714=VERTEX_POINT('',#106319);
#20715=VERTEX_POINT('',#106323);
#20716=VERTEX_POINT('',#106324);
#20717=VERTEX_POINT('',#106326);
#20718=VERTEX_POINT('',#106328);
#20719=VERTEX_POINT('',#106332);
#20720=VERTEX_POINT('',#106333);
#20721=VERTEX_POINT('',#106335);
#20722=VERTEX_POINT('',#106337);
#20723=VERTEX_POINT('',#106341);
#20724=VERTEX_POINT('',#106342);
#20725=VERTEX_POINT('',#106344);
#20726=VERTEX_POINT('',#106346);
#20727=VERTEX_POINT('',#106350);
#20728=VERTEX_POINT('',#106351);
#20729=VERTEX_POINT('',#106353);
#20730=VERTEX_POINT('',#106355);
#20731=VERTEX_POINT('',#106359);
#20732=VERTEX_POINT('',#106360);
#20733=VERTEX_POINT('',#106362);
#20734=VERTEX_POINT('',#106364);
#20735=VERTEX_POINT('',#106368);
#20736=VERTEX_POINT('',#106369);
#20737=VERTEX_POINT('',#106371);
#20738=VERTEX_POINT('',#106373);
#20739=VERTEX_POINT('',#106377);
#20740=VERTEX_POINT('',#106378);
#20741=VERTEX_POINT('',#106380);
#20742=VERTEX_POINT('',#106382);
#20743=VERTEX_POINT('',#106386);
#20744=VERTEX_POINT('',#106387);
#20745=VERTEX_POINT('',#106389);
#20746=VERTEX_POINT('',#106391);
#20747=VERTEX_POINT('',#106395);
#20748=VERTEX_POINT('',#106396);
#20749=VERTEX_POINT('',#106398);
#20750=VERTEX_POINT('',#106400);
#20751=VERTEX_POINT('',#106404);
#20752=VERTEX_POINT('',#106405);
#20753=VERTEX_POINT('',#106407);
#20754=VERTEX_POINT('',#106409);
#20755=VERTEX_POINT('',#106413);
#20756=VERTEX_POINT('',#106414);
#20757=VERTEX_POINT('',#106416);
#20758=VERTEX_POINT('',#106418);
#20759=VERTEX_POINT('',#106422);
#20760=VERTEX_POINT('',#106423);
#20761=VERTEX_POINT('',#106425);
#20762=VERTEX_POINT('',#106427);
#20763=VERTEX_POINT('',#106431);
#20764=VERTEX_POINT('',#106432);
#20765=VERTEX_POINT('',#106434);
#20766=VERTEX_POINT('',#106436);
#20767=VERTEX_POINT('',#106440);
#20768=VERTEX_POINT('',#106441);
#20769=VERTEX_POINT('',#106443);
#20770=VERTEX_POINT('',#106445);
#20771=VERTEX_POINT('',#106449);
#20772=VERTEX_POINT('',#106450);
#20773=VERTEX_POINT('',#106452);
#20774=VERTEX_POINT('',#106454);
#20775=VERTEX_POINT('',#106458);
#20776=VERTEX_POINT('',#106459);
#20777=VERTEX_POINT('',#106461);
#20778=VERTEX_POINT('',#106463);
#20779=VERTEX_POINT('',#106467);
#20780=VERTEX_POINT('',#106468);
#20781=VERTEX_POINT('',#106470);
#20782=VERTEX_POINT('',#106472);
#20783=VERTEX_POINT('',#106476);
#20784=VERTEX_POINT('',#106477);
#20785=VERTEX_POINT('',#106479);
#20786=VERTEX_POINT('',#106481);
#20787=VERTEX_POINT('',#106485);
#20788=VERTEX_POINT('',#106486);
#20789=VERTEX_POINT('',#106488);
#20790=VERTEX_POINT('',#106490);
#20791=VERTEX_POINT('',#106494);
#20792=VERTEX_POINT('',#106495);
#20793=VERTEX_POINT('',#106497);
#20794=VERTEX_POINT('',#106499);
#20795=VERTEX_POINT('',#106503);
#20796=VERTEX_POINT('',#106504);
#20797=VERTEX_POINT('',#106506);
#20798=VERTEX_POINT('',#106508);
#20799=VERTEX_POINT('',#106512);
#20800=VERTEX_POINT('',#106513);
#20801=VERTEX_POINT('',#106515);
#20802=VERTEX_POINT('',#106517);
#20803=VERTEX_POINT('',#106521);
#20804=VERTEX_POINT('',#106522);
#20805=VERTEX_POINT('',#106524);
#20806=VERTEX_POINT('',#106526);
#20807=VERTEX_POINT('',#106530);
#20808=VERTEX_POINT('',#106531);
#20809=VERTEX_POINT('',#106533);
#20810=VERTEX_POINT('',#106535);
#20811=VERTEX_POINT('',#106539);
#20812=VERTEX_POINT('',#106540);
#20813=VERTEX_POINT('',#106542);
#20814=VERTEX_POINT('',#106544);
#20815=VERTEX_POINT('',#106548);
#20816=VERTEX_POINT('',#106549);
#20817=VERTEX_POINT('',#106551);
#20818=VERTEX_POINT('',#106553);
#20819=VERTEX_POINT('',#106557);
#20820=VERTEX_POINT('',#106558);
#20821=VERTEX_POINT('',#106560);
#20822=VERTEX_POINT('',#106562);
#20823=VERTEX_POINT('',#106566);
#20824=VERTEX_POINT('',#106567);
#20825=VERTEX_POINT('',#106569);
#20826=VERTEX_POINT('',#106571);
#20827=VERTEX_POINT('',#106575);
#20828=VERTEX_POINT('',#106576);
#20829=VERTEX_POINT('',#106578);
#20830=VERTEX_POINT('',#106580);
#20831=VERTEX_POINT('',#106584);
#20832=VERTEX_POINT('',#106585);
#20833=VERTEX_POINT('',#106587);
#20834=VERTEX_POINT('',#106589);
#20835=VERTEX_POINT('',#106593);
#20836=VERTEX_POINT('',#106594);
#20837=VERTEX_POINT('',#106596);
#20838=VERTEX_POINT('',#106598);
#20839=VERTEX_POINT('',#106602);
#20840=VERTEX_POINT('',#106603);
#20841=VERTEX_POINT('',#106605);
#20842=VERTEX_POINT('',#106607);
#20843=VERTEX_POINT('',#106611);
#20844=VERTEX_POINT('',#106612);
#20845=VERTEX_POINT('',#106614);
#20846=VERTEX_POINT('',#106616);
#20847=VERTEX_POINT('',#106620);
#20848=VERTEX_POINT('',#106621);
#20849=VERTEX_POINT('',#106623);
#20850=VERTEX_POINT('',#106625);
#20851=VERTEX_POINT('',#106629);
#20852=VERTEX_POINT('',#106630);
#20853=VERTEX_POINT('',#106632);
#20854=VERTEX_POINT('',#106634);
#20855=VERTEX_POINT('',#106638);
#20856=VERTEX_POINT('',#106639);
#20857=VERTEX_POINT('',#106641);
#20858=VERTEX_POINT('',#106643);
#20859=VERTEX_POINT('',#106647);
#20860=VERTEX_POINT('',#106648);
#20861=VERTEX_POINT('',#106650);
#20862=VERTEX_POINT('',#106652);
#20863=VERTEX_POINT('',#106656);
#20864=VERTEX_POINT('',#106657);
#20865=VERTEX_POINT('',#106659);
#20866=VERTEX_POINT('',#106661);
#20867=VERTEX_POINT('',#106665);
#20868=VERTEX_POINT('',#106666);
#20869=VERTEX_POINT('',#106668);
#20870=VERTEX_POINT('',#106670);
#20871=VERTEX_POINT('',#106674);
#20872=VERTEX_POINT('',#106675);
#20873=VERTEX_POINT('',#106677);
#20874=VERTEX_POINT('',#106679);
#20875=VERTEX_POINT('',#106683);
#20876=VERTEX_POINT('',#106684);
#20877=VERTEX_POINT('',#106686);
#20878=VERTEX_POINT('',#106688);
#20879=VERTEX_POINT('',#106692);
#20880=VERTEX_POINT('',#106693);
#20881=VERTEX_POINT('',#106695);
#20882=VERTEX_POINT('',#106697);
#20883=VERTEX_POINT('',#106701);
#20884=VERTEX_POINT('',#106702);
#20885=VERTEX_POINT('',#106704);
#20886=VERTEX_POINT('',#106706);
#20887=VERTEX_POINT('',#106710);
#20888=VERTEX_POINT('',#106711);
#20889=VERTEX_POINT('',#106713);
#20890=VERTEX_POINT('',#106715);
#20891=VERTEX_POINT('',#106719);
#20892=VERTEX_POINT('',#106720);
#20893=VERTEX_POINT('',#106722);
#20894=VERTEX_POINT('',#106724);
#20895=VERTEX_POINT('',#106728);
#20896=VERTEX_POINT('',#106729);
#20897=VERTEX_POINT('',#106731);
#20898=VERTEX_POINT('',#106733);
#20899=VERTEX_POINT('',#106737);
#20900=VERTEX_POINT('',#106738);
#20901=VERTEX_POINT('',#106740);
#20902=VERTEX_POINT('',#106742);
#20903=VERTEX_POINT('',#106746);
#20904=VERTEX_POINT('',#106749);
#20905=VERTEX_POINT('',#106752);
#20906=VERTEX_POINT('',#106755);
#20907=VERTEX_POINT('',#106758);
#20908=VERTEX_POINT('',#106761);
#20909=VERTEX_POINT('',#106764);
#20910=VERTEX_POINT('',#106767);
#20911=VERTEX_POINT('',#106770);
#20912=VERTEX_POINT('',#106773);
#20913=VERTEX_POINT('',#106776);
#20914=VERTEX_POINT('',#106779);
#20915=VERTEX_POINT('',#106782);
#20916=VERTEX_POINT('',#106785);
#20917=VERTEX_POINT('',#106788);
#20918=VERTEX_POINT('',#106791);
#20919=VERTEX_POINT('',#106794);
#20920=VERTEX_POINT('',#106797);
#20921=VERTEX_POINT('',#106800);
#20922=VERTEX_POINT('',#106803);
#20923=VERTEX_POINT('',#106806);
#20924=VERTEX_POINT('',#106809);
#20925=VERTEX_POINT('',#106812);
#20926=VERTEX_POINT('',#106815);
#20927=VERTEX_POINT('',#106818);
#20928=VERTEX_POINT('',#106821);
#20929=VERTEX_POINT('',#106824);
#20930=VERTEX_POINT('',#106827);
#20931=VERTEX_POINT('',#106830);
#20932=VERTEX_POINT('',#106833);
#20933=VERTEX_POINT('',#106836);
#20934=VERTEX_POINT('',#106839);
#20935=VERTEX_POINT('',#106842);
#20936=VERTEX_POINT('',#106845);
#20937=VERTEX_POINT('',#106848);
#20938=VERTEX_POINT('',#106851);
#20939=VERTEX_POINT('',#106854);
#20940=VERTEX_POINT('',#106857);
#20941=VERTEX_POINT('',#106860);
#20942=VERTEX_POINT('',#106863);
#20943=VERTEX_POINT('',#106866);
#20944=VERTEX_POINT('',#106869);
#20945=VERTEX_POINT('',#106872);
#20946=VERTEX_POINT('',#106875);
#20947=VERTEX_POINT('',#106878);
#20948=VERTEX_POINT('',#106881);
#20949=VERTEX_POINT('',#106884);
#20950=VERTEX_POINT('',#106887);
#20951=VERTEX_POINT('',#106890);
#20952=VERTEX_POINT('',#106893);
#20953=VERTEX_POINT('',#106896);
#20954=VERTEX_POINT('',#106900);
#20955=VERTEX_POINT('',#106903);
#20956=VERTEX_POINT('',#106906);
#20957=VERTEX_POINT('',#106909);
#20958=VERTEX_POINT('',#106912);
#20959=VERTEX_POINT('',#106915);
#20960=VERTEX_POINT('',#106918);
#20961=VERTEX_POINT('',#106921);
#20962=VERTEX_POINT('',#106924);
#20963=VERTEX_POINT('',#106927);
#20964=VERTEX_POINT('',#106930);
#20965=VERTEX_POINT('',#106933);
#20966=VERTEX_POINT('',#106936);
#20967=VERTEX_POINT('',#106939);
#20968=VERTEX_POINT('',#106942);
#20969=VERTEX_POINT('',#106945);
#20970=VERTEX_POINT('',#106948);
#20971=VERTEX_POINT('',#106951);
#20972=VERTEX_POINT('',#106954);
#20973=VERTEX_POINT('',#106957);
#20974=VERTEX_POINT('',#106960);
#20975=VERTEX_POINT('',#106963);
#20976=VERTEX_POINT('',#106966);
#20977=VERTEX_POINT('',#106969);
#20978=VERTEX_POINT('',#106972);
#20979=VERTEX_POINT('',#106975);
#20980=VERTEX_POINT('',#106978);
#20981=VERTEX_POINT('',#106981);
#20982=VERTEX_POINT('',#106984);
#20983=VERTEX_POINT('',#106987);
#20984=VERTEX_POINT('',#106990);
#20985=VERTEX_POINT('',#106993);
#20986=VERTEX_POINT('',#106996);
#20987=VERTEX_POINT('',#106999);
#20988=VERTEX_POINT('',#107002);
#20989=VERTEX_POINT('',#107005);
#20990=VERTEX_POINT('',#107008);
#20991=VERTEX_POINT('',#107011);
#20992=VERTEX_POINT('',#107014);
#20993=VERTEX_POINT('',#107017);
#20994=VERTEX_POINT('',#107020);
#20995=VERTEX_POINT('',#107023);
#20996=VERTEX_POINT('',#107026);
#20997=VERTEX_POINT('',#107029);
#20998=VERTEX_POINT('',#107032);
#20999=VERTEX_POINT('',#107035);
#21000=VERTEX_POINT('',#107038);
#21001=VERTEX_POINT('',#107041);
#21002=VERTEX_POINT('',#107044);
#21003=VERTEX_POINT('',#107047);
#21004=VERTEX_POINT('',#107050);
#21005=VERTEX_POINT('',#107212);
#21006=VERTEX_POINT('',#107214);
#21007=VERTEX_POINT('',#107216);
#21008=VERTEX_POINT('',#107218);
#21009=VERTEX_POINT('',#107220);
#21010=VERTEX_POINT('',#107222);
#21011=VERTEX_POINT('',#107225);
#21012=VERTEX_POINT('',#107227);
#21013=VERTEX_POINT('',#107231);
#21014=VERTEX_POINT('',#107233);
#21015=VERTEX_POINT('',#107236);
#21016=VERTEX_POINT('',#107280);
#21017=VERTEX_POINT('',#107282);
#21018=VERTEX_POINT('',#107286);
#21019=VERTEX_POINT('',#107287);
#21020=VERTEX_POINT('',#107289);
#21021=VERTEX_POINT('',#107291);
#21022=VERTEX_POINT('',#107295);
#21023=VERTEX_POINT('',#107297);
#21024=VERTEX_POINT('',#107301);
#21025=VERTEX_POINT('',#107302);
#21026=VERTEX_POINT('',#107304);
#21027=VERTEX_POINT('',#107307);
#21028=VERTEX_POINT('',#107309);
#21029=VERTEX_POINT('',#107318);
#21030=VERTEX_POINT('',#107320);
#21031=VERTEX_POINT('',#107331);
#21032=VERTEX_POINT('',#107335);
#21033=VERTEX_POINT('',#107337);
#21034=VERTEX_POINT('',#107341);
#21035=VERTEX_POINT('',#107342);
#21036=VERTEX_POINT('',#107344);
#21037=VERTEX_POINT('',#107346);
#21038=VERTEX_POINT('',#107350);
#21039=VERTEX_POINT('',#107351);
#21040=VERTEX_POINT('',#107353);
#21041=VERTEX_POINT('',#107355);
#21042=VERTEX_POINT('',#107357);
#21043=VERTEX_POINT('',#107359);
#21044=VERTEX_POINT('',#107363);
#21045=VERTEX_POINT('',#107365);
#21046=VERTEX_POINT('',#107369);
#21047=VERTEX_POINT('',#107371);
#21048=VERTEX_POINT('',#107375);
#21049=VERTEX_POINT('',#107377);
#21050=VERTEX_POINT('',#107381);
#21051=VERTEX_POINT('',#107383);
#21052=VERTEX_POINT('',#107387);
#21053=VERTEX_POINT('',#107389);
#21054=VERTEX_POINT('',#107391);
#21055=VERTEX_POINT('',#107393);
#21056=VERTEX_POINT('',#107395);
#21057=VERTEX_POINT('',#107397);
#21058=VERTEX_POINT('',#107402);
#21059=VERTEX_POINT('',#107404);
#21060=VERTEX_POINT('',#107408);
#21061=VERTEX_POINT('',#107411);
#21062=VERTEX_POINT('',#107413);
#21063=VERTEX_POINT('',#107417);
#21064=VERTEX_POINT('',#107418);
#21065=VERTEX_POINT('',#107420);
#21066=VERTEX_POINT('',#107423);
#21067=VERTEX_POINT('',#107425);
#21068=VERTEX_POINT('',#107427);
#21069=VERTEX_POINT('',#107431);
#21070=VERTEX_POINT('',#107432);
#21071=VERTEX_POINT('',#107434);
#21072=VERTEX_POINT('',#107436);
#21073=VERTEX_POINT('',#107440);
#21074=VERTEX_POINT('',#107441);
#21075=VERTEX_POINT('',#107443);
#21076=VERTEX_POINT('',#107445);
#21077=VERTEX_POINT('',#107447);
#21078=VERTEX_POINT('',#107449);
#21079=VERTEX_POINT('',#107454);
#21080=VERTEX_POINT('',#107456);
#21081=VERTEX_POINT('',#107459);
#21082=VERTEX_POINT('',#107461);
#21083=VERTEX_POINT('',#107463);
#21084=VERTEX_POINT('',#107465);
#21085=VERTEX_POINT('',#107467);
#21086=VERTEX_POINT('',#107469);
#21087=VERTEX_POINT('',#107474);
#21088=VERTEX_POINT('',#107475);
#21089=VERTEX_POINT('',#107477);
#21090=VERTEX_POINT('',#107483);
#21091=VERTEX_POINT('',#107484);
#21092=VERTEX_POINT('',#107486);
#21093=VERTEX_POINT('',#107489);
#21094=VERTEX_POINT('',#107493);
#21095=VERTEX_POINT('',#107494);
#21096=VERTEX_POINT('',#107496);
#21097=VERTEX_POINT('',#107498);
#21098=VERTEX_POINT('',#107503);
#21099=VERTEX_POINT('',#107505);
#21100=VERTEX_POINT('',#107507);
#21101=VERTEX_POINT('',#107509);
#21102=VERTEX_POINT('',#107511);
#21103=VERTEX_POINT('',#107513);
#21104=VERTEX_POINT('',#107515);
#21105=VERTEX_POINT('',#107517);
#21106=VERTEX_POINT('',#107521);
#21107=VERTEX_POINT('',#107526);
#21108=VERTEX_POINT('',#107530);
#21109=VERTEX_POINT('',#107532);
#21110=VERTEX_POINT('',#107536);
#21111=VERTEX_POINT('',#107537);
#21112=VERTEX_POINT('',#107539);
#21113=VERTEX_POINT('',#107541);
#21114=VERTEX_POINT('',#107543);
#21115=VERTEX_POINT('',#107545);
#21116=VERTEX_POINT('',#107549);
#21117=VERTEX_POINT('',#107550);
#21118=VERTEX_POINT('',#107552);
#21119=VERTEX_POINT('',#107554);
#21120=VERTEX_POINT('',#107556);
#21121=VERTEX_POINT('',#107558);
#21122=VERTEX_POINT('',#107560);
#21123=VERTEX_POINT('',#107562);
#21124=VERTEX_POINT('',#107565);
#21125=VERTEX_POINT('',#107566);
#21126=VERTEX_POINT('',#107568);
#21127=VERTEX_POINT('',#107570);
#21128=VERTEX_POINT('',#107572);
#21129=VERTEX_POINT('',#107574);
#21130=VERTEX_POINT('',#107576);
#21131=VERTEX_POINT('',#107578);
#21132=VERTEX_POINT('',#107582);
#21133=VERTEX_POINT('',#107584);
#21134=VERTEX_POINT('',#107586);
#21135=VERTEX_POINT('',#107588);
#21136=VERTEX_POINT('',#107590);
#21137=VERTEX_POINT('',#107592);
#21138=VERTEX_POINT('',#107594);
#21139=VERTEX_POINT('',#107596);
#21140=VERTEX_POINT('',#107598);
#21141=VERTEX_POINT('',#107600);
#21142=VERTEX_POINT('',#107602);
#21143=VERTEX_POINT('',#107604);
#21144=VERTEX_POINT('',#107606);
#21145=VERTEX_POINT('',#107608);
#21146=VERTEX_POINT('',#107610);
#21147=VERTEX_POINT('',#107612);
#21148=VERTEX_POINT('',#107614);
#21149=VERTEX_POINT('',#107616);
#21150=VERTEX_POINT('',#107618);
#21151=VERTEX_POINT('',#107620);
#21152=VERTEX_POINT('',#107622);
#21153=VERTEX_POINT('',#107624);
#21154=VERTEX_POINT('',#107627);
#21155=VERTEX_POINT('',#107629);
#21156=VERTEX_POINT('',#107631);
#21157=VERTEX_POINT('',#107636);
#21158=VERTEX_POINT('',#107638);
#21159=VERTEX_POINT('',#107644);
#21160=VERTEX_POINT('',#107649);
#21161=VERTEX_POINT('',#107650);
#21162=VERTEX_POINT('',#107657);
#21163=VERTEX_POINT('',#107660);
#21164=VERTEX_POINT('',#107664);
#21165=VERTEX_POINT('',#107666);
#21166=VERTEX_POINT('',#107671);
#21167=VERTEX_POINT('',#107675);
#21168=VERTEX_POINT('',#107679);
#21169=VERTEX_POINT('',#107705);
#21170=VERTEX_POINT('',#107709);
#21171=VERTEX_POINT('',#107713);
#21172=VERTEX_POINT('',#107717);
#21173=VERTEX_POINT('',#107721);
#21174=VERTEX_POINT('',#107725);
#21175=VERTEX_POINT('',#107729);
#21176=VERTEX_POINT('',#107733);
#21177=VERTEX_POINT('',#107742);
#21178=VERTEX_POINT('',#107746);
#21179=VERTEX_POINT('',#107750);
#21180=VERTEX_POINT('',#107756);
#21181=VERTEX_POINT('',#107757);
#21182=VERTEX_POINT('',#107762);
#21183=VERTEX_POINT('',#107763);
#21184=VERTEX_POINT('',#107769);
#21185=VERTEX_POINT('',#107794);
#21186=VERTEX_POINT('',#107796);
#21187=VERTEX_POINT('',#107800);
#21188=VERTEX_POINT('',#107804);
#21189=VERTEX_POINT('',#107808);
#21190=VERTEX_POINT('',#107812);
#21191=VERTEX_POINT('',#107816);
#21192=VERTEX_POINT('',#107820);
#21193=VERTEX_POINT('',#107830);
#21194=VERTEX_POINT('',#107832);
#21195=VERTEX_POINT('',#107834);
#21196=VERTEX_POINT('',#107836);
#21197=VERTEX_POINT('',#107842);
#21198=VERTEX_POINT('',#107850);
#21199=VERTEX_POINT('',#107861);
#21200=VERTEX_POINT('',#107862);
#21201=VERTEX_POINT('',#107867);
#21202=VERTEX_POINT('',#107868);
#21203=EDGE_CURVE('',#17179,#17179,#13607,.T.);
#21204=EDGE_CURVE('',#17179,#17180,#9639,.T.);
#21205=EDGE_CURVE('',#17180,#17180,#13608,.T.);
#21206=EDGE_CURVE('',#17181,#17181,#13609,.T.);
#21207=EDGE_CURVE('',#17181,#17182,#9640,.T.);
#21208=EDGE_CURVE('',#17182,#17182,#13610,.T.);
#21209=EDGE_CURVE('',#17183,#17183,#1137,.F.);
#21210=EDGE_CURVE('',#17183,#17184,#1138,.T.);
#21211=EDGE_CURVE('',#17184,#17185,#1139,.F.);
#21212=EDGE_CURVE('',#17185,#17184,#1140,.F.);
#21213=EDGE_CURVE('',#17186,#17186,#13611,.T.);
#21214=EDGE_CURVE('',#17186,#17187,#13612,.T.);
#21215=EDGE_CURVE('',#17187,#17187,#13613,.T.);
#21216=EDGE_CURVE('',#17187,#17188,#9641,.T.);
#21217=EDGE_CURVE('',#17188,#17188,#13614,.T.);
#21218=EDGE_CURVE('',#17189,#17189,#13615,.T.);
#21219=EDGE_CURVE('',#17189,#17190,#9642,.T.);
#21220=EDGE_CURVE('',#17190,#17191,#13616,.T.);
#21221=EDGE_CURVE('',#17192,#17191,#1141,.F.);
#21222=EDGE_CURVE('',#17192,#17190,#13617,.T.);
#21223=EDGE_CURVE('',#17192,#17191,#9643,.T.);
#21224=EDGE_CURVE('',#17193,#17194,#13618,.T.);
#21225=EDGE_CURVE('',#17194,#17195,#9644,.T.);
#21226=EDGE_CURVE('',#17195,#17196,#13619,.T.);
#21227=EDGE_CURVE('',#17193,#17196,#9645,.T.);
#21228=EDGE_CURVE('',#17197,#17198,#13620,.T.);
#21229=EDGE_CURVE('',#17197,#17199,#9646,.T.);
#21230=EDGE_CURVE('',#17199,#17200,#13621,.T.);
#21231=EDGE_CURVE('',#17198,#17200,#9647,.T.);
#21232=EDGE_CURVE('',#17200,#17201,#9648,.T.);
#21233=EDGE_CURVE('',#17202,#17201,#9649,.T.);
#21234=EDGE_CURVE('',#17203,#17202,#9650,.T.);
#21235=EDGE_CURVE('',#17204,#17203,#9651,.T.);
#21236=EDGE_CURVE('',#17198,#17204,#9652,.T.);
#21237=EDGE_CURVE('',#17205,#17193,#9653,.T.);
#21238=EDGE_CURVE('',#17206,#17205,#13622,.T.);
#21239=EDGE_CURVE('',#17194,#17206,#9654,.T.);
#21240=EDGE_CURVE('',#17202,#17207,#884,.T.);
#21241=EDGE_CURVE('',#17208,#17207,#9655,.T.);
#21242=EDGE_CURVE('',#17208,#17203,#885,.T.);
#21243=EDGE_CURVE('',#17207,#17209,#9656,.T.);
#21244=EDGE_CURVE('',#17210,#17209,#9657,.T.);
#21245=EDGE_CURVE('',#17210,#17208,#9658,.T.);
#21246=EDGE_CURVE('',#17209,#17211,#9659,.T.);
#21247=EDGE_CURVE('',#17211,#17212,#9660,.T.);
#21248=EDGE_CURVE('',#17210,#17212,#9661,.T.);
#21249=EDGE_CURVE('',#17213,#17214,#9662,.T.);
#21250=EDGE_CURVE('',#17214,#17215,#9663,.T.);
#21251=EDGE_CURVE('',#17216,#17215,#9664,.T.);
#21252=EDGE_CURVE('',#17216,#17217,#9665,.T.);
#21253=EDGE_CURVE('',#17217,#17218,#9666,.T.);
#21254=EDGE_CURVE('',#17218,#17213,#9667,.T.);
#21255=EDGE_CURVE('',#17219,#17195,#9668,.T.);
#21256=EDGE_CURVE('',#17220,#17219,#13623,.T.);
#21257=EDGE_CURVE('',#17196,#17220,#9669,.T.);
#21258=EDGE_CURVE('',#17215,#17221,#9670,.T.);
#21259=EDGE_CURVE('',#17221,#17199,#9671,.T.);
#21260=EDGE_CURVE('',#17222,#17197,#9672,.T.);
#21261=EDGE_CURVE('',#17222,#17216,#9673,.T.);
#21262=EDGE_CURVE('',#17204,#17223,#9674,.T.);
#21263=EDGE_CURVE('',#17223,#17222,#9675,.T.);
#21264=EDGE_CURVE('',#17221,#17224,#9676,.T.);
#21265=EDGE_CURVE('',#17201,#17224,#9677,.T.);
#21266=EDGE_CURVE('',#17224,#17211,#9678,.T.);
#21267=EDGE_CURVE('',#17212,#17223,#9679,.T.);
#21268=EDGE_CURVE('',#17205,#17220,#9680,.T.);
#21269=EDGE_CURVE('',#17206,#17219,#9681,.T.);
#21270=EDGE_CURVE('',#17217,#17223,#9682,.T.);
#21271=EDGE_CURVE('',#17218,#17212,#9683,.T.);
#21272=EDGE_CURVE('',#17213,#17211,#9684,.T.);
#21273=EDGE_CURVE('',#17214,#17224,#9685,.T.);
#21274=EDGE_CURVE('',#17225,#17225,#13624,.T.);
#21275=EDGE_CURVE('',#17225,#17226,#9686,.T.);
#21276=EDGE_CURVE('',#17226,#17226,#13625,.T.);
#21277=EDGE_CURVE('',#17227,#17228,#1142,.F.);
#21278=EDGE_CURVE('',#17228,#17229,#9687,.T.);
#21279=EDGE_CURVE('',#17229,#17229,#13626,.T.);
#21280=EDGE_CURVE('',#17228,#17230,#1143,.F.);
#21281=EDGE_CURVE('',#17230,#17231,#13627,.T.);
#21282=EDGE_CURVE('',#17231,#17232,#13628,.T.);
#21283=EDGE_CURVE('',#17232,#17233,#1144,.T.);
#21284=EDGE_CURVE('',#17233,#17234,#1145,.T.);
#21285=EDGE_CURVE('',#17234,#17235,#13629,.T.);
#21286=EDGE_CURVE('',#17235,#17236,#13630,.T.);
#21287=EDGE_CURVE('',#17236,#17237,#1146,.T.);
#21288=EDGE_CURVE('',#17237,#17238,#1147,.T.);
#21289=EDGE_CURVE('',#17238,#17239,#13631,.T.);
#21290=EDGE_CURVE('',#17239,#17240,#13632,.T.);
#21291=EDGE_CURVE('',#17240,#17241,#1148,.T.);
#21292=EDGE_CURVE('',#17241,#17242,#1149,.T.);
#21293=EDGE_CURVE('',#17242,#17243,#13633,.T.);
#21294=EDGE_CURVE('',#17243,#17244,#13634,.T.);
#21295=EDGE_CURVE('',#17244,#17245,#1150,.T.);
#21296=EDGE_CURVE('',#17245,#17246,#1151,.T.);
#21297=EDGE_CURVE('',#17246,#17247,#13635,.T.);
#21298=EDGE_CURVE('',#17247,#17248,#13636,.T.);
#21299=EDGE_CURVE('',#17248,#17249,#1152,.T.);
#21300=EDGE_CURVE('',#17249,#17250,#1153,.T.);
#21301=EDGE_CURVE('',#17250,#17251,#13637,.T.);
#21302=EDGE_CURVE('',#17251,#17252,#13638,.T.);
#21303=EDGE_CURVE('',#17252,#17253,#1154,.T.);
#21304=EDGE_CURVE('',#17253,#17254,#1155,.T.);
#21305=EDGE_CURVE('',#17254,#17255,#13639,.T.);
#21306=EDGE_CURVE('',#17255,#17256,#13640,.T.);
#21307=EDGE_CURVE('',#17256,#17257,#1156,.T.);
#21308=EDGE_CURVE('',#17257,#17258,#1157,.T.);
#21309=EDGE_CURVE('',#17258,#17259,#13641,.T.);
#21310=EDGE_CURVE('',#17259,#17260,#13642,.T.);
#21311=EDGE_CURVE('',#17260,#17261,#1158,.T.);
#21312=EDGE_CURVE('',#17261,#17262,#1159,.T.);
#21313=EDGE_CURVE('',#17262,#17263,#13643,.T.);
#21314=EDGE_CURVE('',#17263,#17264,#13644,.T.);
#21315=EDGE_CURVE('',#17264,#17265,#1160,.T.);
#21316=EDGE_CURVE('',#17265,#17266,#1161,.T.);
#21317=EDGE_CURVE('',#17266,#17267,#13645,.T.);
#21318=EDGE_CURVE('',#17267,#17268,#13646,.T.);
#21319=EDGE_CURVE('',#17268,#17269,#1162,.T.);
#21320=EDGE_CURVE('',#17269,#17270,#1163,.T.);
#21321=EDGE_CURVE('',#17270,#17271,#13647,.T.);
#21322=EDGE_CURVE('',#17271,#17272,#13648,.T.);
#21323=EDGE_CURVE('',#17272,#17273,#1164,.T.);
#21324=EDGE_CURVE('',#17273,#17274,#1165,.T.);
#21325=EDGE_CURVE('',#17274,#17275,#13649,.T.);
#21326=EDGE_CURVE('',#17275,#17276,#13650,.T.);
#21327=EDGE_CURVE('',#17276,#17277,#1166,.T.);
#21328=EDGE_CURVE('',#17277,#17278,#1167,.T.);
#21329=EDGE_CURVE('',#17278,#17279,#13651,.T.);
#21330=EDGE_CURVE('',#17279,#17280,#13652,.T.);
#21331=EDGE_CURVE('',#17280,#17281,#1168,.T.);
#21332=EDGE_CURVE('',#17281,#17282,#1169,.T.);
#21333=EDGE_CURVE('',#17282,#17283,#13653,.T.);
#21334=EDGE_CURVE('',#17283,#17284,#13654,.T.);
#21335=EDGE_CURVE('',#17284,#17285,#1170,.T.);
#21336=EDGE_CURVE('',#17285,#17286,#1171,.T.);
#21337=EDGE_CURVE('',#17286,#17287,#13655,.T.);
#21338=EDGE_CURVE('',#17287,#17288,#13656,.T.);
#21339=EDGE_CURVE('',#17288,#17289,#1172,.T.);
#21340=EDGE_CURVE('',#17289,#17290,#1173,.T.);
#21341=EDGE_CURVE('',#17290,#17291,#13657,.T.);
#21342=EDGE_CURVE('',#17291,#17292,#13658,.T.);
#21343=EDGE_CURVE('',#17292,#17293,#1174,.T.);
#21344=EDGE_CURVE('',#17293,#17294,#1175,.T.);
#21345=EDGE_CURVE('',#17294,#17295,#13659,.T.);
#21346=EDGE_CURVE('',#17295,#17296,#13660,.T.);
#21347=EDGE_CURVE('',#17296,#17297,#1176,.T.);
#21348=EDGE_CURVE('',#17297,#17298,#1177,.T.);
#21349=EDGE_CURVE('',#17298,#17299,#13661,.T.);
#21350=EDGE_CURVE('',#17299,#17300,#13662,.T.);
#21351=EDGE_CURVE('',#17300,#17301,#1178,.T.);
#21352=EDGE_CURVE('',#17301,#17302,#1179,.T.);
#21353=EDGE_CURVE('',#17302,#17303,#13663,.T.);
#21354=EDGE_CURVE('',#17303,#17304,#13664,.T.);
#21355=EDGE_CURVE('',#17304,#17305,#1180,.T.);
#21356=EDGE_CURVE('',#17305,#17306,#1181,.T.);
#21357=EDGE_CURVE('',#17306,#17307,#13665,.T.);
#21358=EDGE_CURVE('',#17307,#17308,#13666,.T.);
#21359=EDGE_CURVE('',#17308,#17309,#1182,.T.);
#21360=EDGE_CURVE('',#17309,#17310,#1183,.T.);
#21361=EDGE_CURVE('',#17310,#17311,#13667,.T.);
#21362=EDGE_CURVE('',#17311,#17312,#13668,.T.);
#21363=EDGE_CURVE('',#17312,#17313,#1184,.T.);
#21364=EDGE_CURVE('',#17313,#17314,#1185,.T.);
#21365=EDGE_CURVE('',#17314,#17315,#13669,.T.);
#21366=EDGE_CURVE('',#17315,#17316,#13670,.T.);
#21367=EDGE_CURVE('',#17316,#17317,#1186,.T.);
#21368=EDGE_CURVE('',#17317,#17318,#1187,.T.);
#21369=EDGE_CURVE('',#17318,#17319,#13671,.T.);
#21370=EDGE_CURVE('',#17319,#17320,#13672,.T.);
#21371=EDGE_CURVE('',#17320,#17321,#1188,.T.);
#21372=EDGE_CURVE('',#17321,#17322,#1189,.T.);
#21373=EDGE_CURVE('',#17322,#17323,#13673,.T.);
#21374=EDGE_CURVE('',#17323,#17324,#13674,.T.);
#21375=EDGE_CURVE('',#17324,#17325,#1190,.T.);
#21376=EDGE_CURVE('',#17325,#17326,#1191,.T.);
#21377=EDGE_CURVE('',#17326,#17327,#13675,.T.);
#21378=EDGE_CURVE('',#17327,#17328,#13676,.T.);
#21379=EDGE_CURVE('',#17328,#17329,#1192,.T.);
#21380=EDGE_CURVE('',#17329,#17330,#1193,.T.);
#21381=EDGE_CURVE('',#17330,#17331,#13677,.T.);
#21382=EDGE_CURVE('',#17331,#17332,#13678,.T.);
#21383=EDGE_CURVE('',#17332,#17333,#1194,.T.);
#21384=EDGE_CURVE('',#17333,#17334,#1195,.T.);
#21385=EDGE_CURVE('',#17334,#17335,#13679,.T.);
#21386=EDGE_CURVE('',#17335,#17336,#13680,.T.);
#21387=EDGE_CURVE('',#17336,#17337,#1196,.T.);
#21388=EDGE_CURVE('',#17337,#17338,#1197,.T.);
#21389=EDGE_CURVE('',#17338,#17339,#13681,.T.);
#21390=EDGE_CURVE('',#17339,#17340,#13682,.T.);
#21391=EDGE_CURVE('',#17340,#17341,#1198,.T.);
#21392=EDGE_CURVE('',#17341,#17342,#1199,.T.);
#21393=EDGE_CURVE('',#17342,#17343,#13683,.T.);
#21394=EDGE_CURVE('',#17343,#17344,#13684,.T.);
#21395=EDGE_CURVE('',#17344,#17345,#1200,.T.);
#21396=EDGE_CURVE('',#17345,#17346,#1201,.T.);
#21397=EDGE_CURVE('',#17346,#17347,#13685,.T.);
#21398=EDGE_CURVE('',#17347,#17348,#13686,.T.);
#21399=EDGE_CURVE('',#17348,#17349,#1202,.T.);
#21400=EDGE_CURVE('',#17349,#17350,#1203,.T.);
#21401=EDGE_CURVE('',#17350,#17351,#13687,.T.);
#21402=EDGE_CURVE('',#17351,#17352,#13688,.T.);
#21403=EDGE_CURVE('',#17352,#17353,#1204,.T.);
#21404=EDGE_CURVE('',#17353,#17354,#1205,.T.);
#21405=EDGE_CURVE('',#17354,#17355,#13689,.T.);
#21406=EDGE_CURVE('',#17355,#17356,#13690,.T.);
#21407=EDGE_CURVE('',#17356,#17357,#1206,.T.);
#21408=EDGE_CURVE('',#17357,#17358,#1207,.T.);
#21409=EDGE_CURVE('',#17358,#17359,#13691,.T.);
#21410=EDGE_CURVE('',#17359,#17360,#13692,.T.);
#21411=EDGE_CURVE('',#17360,#17361,#1208,.T.);
#21412=EDGE_CURVE('',#17361,#17362,#1209,.T.);
#21413=EDGE_CURVE('',#17362,#17363,#13693,.T.);
#21414=EDGE_CURVE('',#17363,#17364,#13694,.T.);
#21415=EDGE_CURVE('',#17364,#17365,#1210,.T.);
#21416=EDGE_CURVE('',#17365,#17366,#1211,.T.);
#21417=EDGE_CURVE('',#17366,#17367,#13695,.T.);
#21418=EDGE_CURVE('',#17367,#17368,#13696,.T.);
#21419=EDGE_CURVE('',#17368,#17369,#1212,.T.);
#21420=EDGE_CURVE('',#17369,#17370,#1213,.T.);
#21421=EDGE_CURVE('',#17370,#17371,#13697,.T.);
#21422=EDGE_CURVE('',#17371,#17372,#13698,.T.);
#21423=EDGE_CURVE('',#17372,#17373,#1214,.T.);
#21424=EDGE_CURVE('',#17373,#17374,#1215,.T.);
#21425=EDGE_CURVE('',#17374,#17375,#13699,.T.);
#21426=EDGE_CURVE('',#17375,#17376,#13700,.T.);
#21427=EDGE_CURVE('',#17376,#17377,#1216,.T.);
#21428=EDGE_CURVE('',#17377,#17378,#1217,.T.);
#21429=EDGE_CURVE('',#17378,#17379,#13701,.T.);
#21430=EDGE_CURVE('',#17379,#17380,#13702,.T.);
#21431=EDGE_CURVE('',#17380,#17381,#1218,.T.);
#21432=EDGE_CURVE('',#17381,#17382,#1219,.T.);
#21433=EDGE_CURVE('',#17382,#17383,#13703,.T.);
#21434=EDGE_CURVE('',#17383,#17384,#13704,.T.);
#21435=EDGE_CURVE('',#17384,#17385,#1220,.T.);
#21436=EDGE_CURVE('',#17385,#17386,#1221,.T.);
#21437=EDGE_CURVE('',#17386,#17387,#13705,.T.);
#21438=EDGE_CURVE('',#17387,#17388,#13706,.T.);
#21439=EDGE_CURVE('',#17388,#17389,#1222,.T.);
#21440=EDGE_CURVE('',#17389,#17390,#1223,.T.);
#21441=EDGE_CURVE('',#17390,#17391,#13707,.T.);
#21442=EDGE_CURVE('',#17391,#17392,#13708,.T.);
#21443=EDGE_CURVE('',#17392,#17393,#1224,.T.);
#21444=EDGE_CURVE('',#17393,#17394,#1225,.T.);
#21445=EDGE_CURVE('',#17394,#17395,#13709,.T.);
#21446=EDGE_CURVE('',#17395,#17396,#13710,.T.);
#21447=EDGE_CURVE('',#17396,#17397,#1226,.T.);
#21448=EDGE_CURVE('',#17397,#17398,#1227,.T.);
#21449=EDGE_CURVE('',#17398,#17399,#13711,.T.);
#21450=EDGE_CURVE('',#17399,#17400,#13712,.T.);
#21451=EDGE_CURVE('',#17400,#17401,#1228,.T.);
#21452=EDGE_CURVE('',#17401,#17402,#1229,.T.);
#21453=EDGE_CURVE('',#17402,#17403,#13713,.T.);
#21454=EDGE_CURVE('',#17403,#17404,#13714,.T.);
#21455=EDGE_CURVE('',#17404,#17405,#1230,.T.);
#21456=EDGE_CURVE('',#17405,#17406,#1231,.T.);
#21457=EDGE_CURVE('',#17406,#17407,#13715,.T.);
#21458=EDGE_CURVE('',#17407,#17408,#13716,.T.);
#21459=EDGE_CURVE('',#17408,#17409,#1232,.T.);
#21460=EDGE_CURVE('',#17409,#17410,#1233,.T.);
#21461=EDGE_CURVE('',#17410,#17411,#13717,.T.);
#21462=EDGE_CURVE('',#17411,#17412,#13718,.T.);
#21463=EDGE_CURVE('',#17412,#17413,#1234,.T.);
#21464=EDGE_CURVE('',#17413,#17414,#1235,.T.);
#21465=EDGE_CURVE('',#17414,#17415,#13719,.T.);
#21466=EDGE_CURVE('',#17415,#17416,#13720,.T.);
#21467=EDGE_CURVE('',#17416,#17417,#1236,.T.);
#21468=EDGE_CURVE('',#17417,#17418,#1237,.T.);
#21469=EDGE_CURVE('',#17418,#17419,#13721,.T.);
#21470=EDGE_CURVE('',#17419,#17420,#13722,.T.);
#21471=EDGE_CURVE('',#17420,#17421,#1238,.T.);
#21472=EDGE_CURVE('',#17421,#17422,#1239,.T.);
#21473=EDGE_CURVE('',#17422,#17423,#13723,.T.);
#21474=EDGE_CURVE('',#17423,#17424,#13724,.T.);
#21475=EDGE_CURVE('',#17424,#17425,#1240,.T.);
#21476=EDGE_CURVE('',#17425,#17426,#1241,.T.);
#21477=EDGE_CURVE('',#17426,#17427,#13725,.T.);
#21478=EDGE_CURVE('',#17427,#17428,#13726,.T.);
#21479=EDGE_CURVE('',#17428,#17227,#1242,.T.);
#21480=EDGE_CURVE('',#17429,#17430,#1243,.F.);
#21481=EDGE_CURVE('',#17430,#17431,#9688,.T.);
#21482=EDGE_CURVE('',#17431,#17431,#13727,.T.);
#21483=EDGE_CURVE('',#17430,#17432,#1244,.F.);
#21484=EDGE_CURVE('',#17432,#17433,#13728,.T.);
#21485=EDGE_CURVE('',#17433,#17434,#13729,.T.);
#21486=EDGE_CURVE('',#17434,#17435,#13730,.T.);
#21487=EDGE_CURVE('',#17435,#17436,#13731,.T.);
#21488=EDGE_CURVE('',#17436,#17437,#1245,.T.);
#21489=EDGE_CURVE('',#17437,#17438,#13732,.T.);
#21490=EDGE_CURVE('',#17438,#17439,#13733,.T.);
#21491=EDGE_CURVE('',#17439,#17440,#13734,.T.);
#21492=EDGE_CURVE('',#17440,#17441,#13735,.T.);
#21493=EDGE_CURVE('',#17441,#17442,#13736,.T.);
#21494=EDGE_CURVE('',#17442,#17443,#1246,.T.);
#21495=EDGE_CURVE('',#17443,#17444,#13737,.T.);
#21496=EDGE_CURVE('',#17444,#17445,#13738,.T.);
#21497=EDGE_CURVE('',#17445,#17446,#13739,.T.);
#21498=EDGE_CURVE('',#17446,#17447,#13740,.T.);
#21499=EDGE_CURVE('',#17447,#17448,#13741,.T.);
#21500=EDGE_CURVE('',#17448,#17449,#1247,.T.);
#21501=EDGE_CURVE('',#17449,#17450,#13742,.T.);
#21502=EDGE_CURVE('',#17450,#17451,#13743,.T.);
#21503=EDGE_CURVE('',#17451,#17452,#13744,.T.);
#21504=EDGE_CURVE('',#17452,#17453,#13745,.T.);
#21505=EDGE_CURVE('',#17453,#17454,#13746,.T.);
#21506=EDGE_CURVE('',#17454,#17455,#1248,.T.);
#21507=EDGE_CURVE('',#17455,#17456,#13747,.T.);
#21508=EDGE_CURVE('',#17456,#17457,#13748,.T.);
#21509=EDGE_CURVE('',#17457,#17458,#13749,.T.);
#21510=EDGE_CURVE('',#17458,#17459,#13750,.T.);
#21511=EDGE_CURVE('',#17459,#17460,#13751,.T.);
#21512=EDGE_CURVE('',#17460,#17461,#1249,.T.);
#21513=EDGE_CURVE('',#17461,#17462,#13752,.T.);
#21514=EDGE_CURVE('',#17462,#17463,#13753,.T.);
#21515=EDGE_CURVE('',#17463,#17464,#13754,.T.);
#21516=EDGE_CURVE('',#17464,#17465,#13755,.T.);
#21517=EDGE_CURVE('',#17465,#17466,#13756,.T.);
#21518=EDGE_CURVE('',#17466,#17467,#1250,.T.);
#21519=EDGE_CURVE('',#17467,#17468,#13757,.T.);
#21520=EDGE_CURVE('',#17468,#17469,#13758,.T.);
#21521=EDGE_CURVE('',#17469,#17470,#13759,.T.);
#21522=EDGE_CURVE('',#17470,#17471,#13760,.T.);
#21523=EDGE_CURVE('',#17471,#17472,#13761,.T.);
#21524=EDGE_CURVE('',#17472,#17473,#1251,.T.);
#21525=EDGE_CURVE('',#17473,#17474,#13762,.T.);
#21526=EDGE_CURVE('',#17474,#17475,#13763,.T.);
#21527=EDGE_CURVE('',#17475,#17476,#13764,.T.);
#21528=EDGE_CURVE('',#17476,#17477,#13765,.T.);
#21529=EDGE_CURVE('',#17477,#17478,#13766,.T.);
#21530=EDGE_CURVE('',#17478,#17479,#1252,.T.);
#21531=EDGE_CURVE('',#17479,#17480,#13767,.T.);
#21532=EDGE_CURVE('',#17480,#17481,#13768,.T.);
#21533=EDGE_CURVE('',#17481,#17482,#13769,.T.);
#21534=EDGE_CURVE('',#17482,#17483,#13770,.T.);
#21535=EDGE_CURVE('',#17483,#17484,#13771,.T.);
#21536=EDGE_CURVE('',#17484,#17485,#1253,.T.);
#21537=EDGE_CURVE('',#17485,#17486,#13772,.T.);
#21538=EDGE_CURVE('',#17486,#17487,#13773,.T.);
#21539=EDGE_CURVE('',#17487,#17488,#13774,.T.);
#21540=EDGE_CURVE('',#17488,#17489,#13775,.T.);
#21541=EDGE_CURVE('',#17489,#17490,#13776,.T.);
#21542=EDGE_CURVE('',#17490,#17491,#1254,.T.);
#21543=EDGE_CURVE('',#17491,#17492,#13777,.T.);
#21544=EDGE_CURVE('',#17492,#17493,#13778,.T.);
#21545=EDGE_CURVE('',#17493,#17494,#13779,.T.);
#21546=EDGE_CURVE('',#17494,#17495,#13780,.T.);
#21547=EDGE_CURVE('',#17495,#17496,#13781,.T.);
#21548=EDGE_CURVE('',#17496,#17497,#1255,.T.);
#21549=EDGE_CURVE('',#17497,#17498,#13782,.T.);
#21550=EDGE_CURVE('',#17498,#17499,#13783,.T.);
#21551=EDGE_CURVE('',#17499,#17500,#13784,.T.);
#21552=EDGE_CURVE('',#17500,#17501,#13785,.T.);
#21553=EDGE_CURVE('',#17501,#17502,#13786,.T.);
#21554=EDGE_CURVE('',#17502,#17503,#1256,.T.);
#21555=EDGE_CURVE('',#17503,#17504,#13787,.T.);
#21556=EDGE_CURVE('',#17504,#17505,#13788,.T.);
#21557=EDGE_CURVE('',#17505,#17506,#13789,.T.);
#21558=EDGE_CURVE('',#17506,#17507,#13790,.T.);
#21559=EDGE_CURVE('',#17507,#17508,#13791,.T.);
#21560=EDGE_CURVE('',#17508,#17509,#1257,.T.);
#21561=EDGE_CURVE('',#17509,#17510,#13792,.T.);
#21562=EDGE_CURVE('',#17510,#17511,#13793,.T.);
#21563=EDGE_CURVE('',#17511,#17512,#13794,.T.);
#21564=EDGE_CURVE('',#17512,#17513,#13795,.T.);
#21565=EDGE_CURVE('',#17513,#17514,#13796,.T.);
#21566=EDGE_CURVE('',#17514,#17515,#1258,.T.);
#21567=EDGE_CURVE('',#17515,#17516,#13797,.T.);
#21568=EDGE_CURVE('',#17516,#17517,#13798,.T.);
#21569=EDGE_CURVE('',#17517,#17518,#13799,.T.);
#21570=EDGE_CURVE('',#17518,#17519,#13800,.T.);
#21571=EDGE_CURVE('',#17519,#17520,#13801,.T.);
#21572=EDGE_CURVE('',#17520,#17521,#1259,.T.);
#21573=EDGE_CURVE('',#17521,#17522,#13802,.T.);
#21574=EDGE_CURVE('',#17522,#17523,#13803,.T.);
#21575=EDGE_CURVE('',#17523,#17524,#13804,.T.);
#21576=EDGE_CURVE('',#17524,#17525,#13805,.T.);
#21577=EDGE_CURVE('',#17525,#17526,#13806,.T.);
#21578=EDGE_CURVE('',#17526,#17527,#1260,.T.);
#21579=EDGE_CURVE('',#17527,#17528,#13807,.T.);
#21580=EDGE_CURVE('',#17528,#17529,#13808,.T.);
#21581=EDGE_CURVE('',#17529,#17530,#13809,.T.);
#21582=EDGE_CURVE('',#17530,#17531,#13810,.T.);
#21583=EDGE_CURVE('',#17531,#17532,#13811,.T.);
#21584=EDGE_CURVE('',#17532,#17533,#1261,.T.);
#21585=EDGE_CURVE('',#17533,#17534,#13812,.T.);
#21586=EDGE_CURVE('',#17534,#17535,#13813,.T.);
#21587=EDGE_CURVE('',#17535,#17536,#13814,.T.);
#21588=EDGE_CURVE('',#17536,#17537,#13815,.T.);
#21589=EDGE_CURVE('',#17537,#17538,#13816,.T.);
#21590=EDGE_CURVE('',#17538,#17539,#1262,.T.);
#21591=EDGE_CURVE('',#17539,#17540,#13817,.T.);
#21592=EDGE_CURVE('',#17540,#17541,#13818,.T.);
#21593=EDGE_CURVE('',#17541,#17542,#13819,.T.);
#21594=EDGE_CURVE('',#17542,#17543,#13820,.T.);
#21595=EDGE_CURVE('',#17543,#17544,#13821,.T.);
#21596=EDGE_CURVE('',#17544,#17545,#1263,.T.);
#21597=EDGE_CURVE('',#17545,#17546,#13822,.T.);
#21598=EDGE_CURVE('',#17546,#17547,#13823,.T.);
#21599=EDGE_CURVE('',#17547,#17548,#13824,.T.);
#21600=EDGE_CURVE('',#17548,#17549,#13825,.T.);
#21601=EDGE_CURVE('',#17549,#17550,#13826,.T.);
#21602=EDGE_CURVE('',#17550,#17551,#1264,.T.);
#21603=EDGE_CURVE('',#17551,#17552,#13827,.T.);
#21604=EDGE_CURVE('',#17552,#17553,#13828,.T.);
#21605=EDGE_CURVE('',#17553,#17554,#13829,.T.);
#21606=EDGE_CURVE('',#17554,#17555,#13830,.T.);
#21607=EDGE_CURVE('',#17555,#17556,#13831,.T.);
#21608=EDGE_CURVE('',#17556,#17557,#1265,.T.);
#21609=EDGE_CURVE('',#17557,#17558,#13832,.T.);
#21610=EDGE_CURVE('',#17558,#17559,#13833,.T.);
#21611=EDGE_CURVE('',#17559,#17560,#13834,.T.);
#21612=EDGE_CURVE('',#17560,#17561,#13835,.T.);
#21613=EDGE_CURVE('',#17561,#17562,#13836,.T.);
#21614=EDGE_CURVE('',#17562,#17563,#1266,.T.);
#21615=EDGE_CURVE('',#17563,#17564,#13837,.T.);
#21616=EDGE_CURVE('',#17564,#17565,#13838,.T.);
#21617=EDGE_CURVE('',#17565,#17566,#13839,.T.);
#21618=EDGE_CURVE('',#17566,#17567,#13840,.T.);
#21619=EDGE_CURVE('',#17567,#17568,#13841,.T.);
#21620=EDGE_CURVE('',#17568,#17569,#1267,.T.);
#21621=EDGE_CURVE('',#17569,#17570,#13842,.T.);
#21622=EDGE_CURVE('',#17570,#17571,#13843,.T.);
#21623=EDGE_CURVE('',#17571,#17572,#13844,.T.);
#21624=EDGE_CURVE('',#17572,#17573,#13845,.T.);
#21625=EDGE_CURVE('',#17573,#17574,#13846,.T.);
#21626=EDGE_CURVE('',#17574,#17575,#1268,.T.);
#21627=EDGE_CURVE('',#17575,#17576,#13847,.T.);
#21628=EDGE_CURVE('',#17576,#17577,#13848,.T.);
#21629=EDGE_CURVE('',#17577,#17578,#13849,.T.);
#21630=EDGE_CURVE('',#17578,#17579,#13850,.T.);
#21631=EDGE_CURVE('',#17579,#17580,#13851,.T.);
#21632=EDGE_CURVE('',#17580,#17581,#1269,.T.);
#21633=EDGE_CURVE('',#17581,#17582,#13852,.T.);
#21634=EDGE_CURVE('',#17582,#17583,#13853,.T.);
#21635=EDGE_CURVE('',#17583,#17584,#13854,.T.);
#21636=EDGE_CURVE('',#17584,#17585,#13855,.T.);
#21637=EDGE_CURVE('',#17585,#17586,#13856,.T.);
#21638=EDGE_CURVE('',#17586,#17587,#1270,.T.);
#21639=EDGE_CURVE('',#17587,#17588,#13857,.T.);
#21640=EDGE_CURVE('',#17588,#17589,#13858,.T.);
#21641=EDGE_CURVE('',#17589,#17590,#13859,.T.);
#21642=EDGE_CURVE('',#17590,#17591,#13860,.T.);
#21643=EDGE_CURVE('',#17591,#17592,#13861,.T.);
#21644=EDGE_CURVE('',#17592,#17593,#1271,.T.);
#21645=EDGE_CURVE('',#17593,#17594,#13862,.T.);
#21646=EDGE_CURVE('',#17594,#17595,#13863,.T.);
#21647=EDGE_CURVE('',#17595,#17596,#13864,.T.);
#21648=EDGE_CURVE('',#17596,#17597,#13865,.T.);
#21649=EDGE_CURVE('',#17597,#17598,#13866,.T.);
#21650=EDGE_CURVE('',#17598,#17599,#1272,.T.);
#21651=EDGE_CURVE('',#17599,#17600,#13867,.T.);
#21652=EDGE_CURVE('',#17600,#17601,#13868,.T.);
#21653=EDGE_CURVE('',#17601,#17602,#13869,.T.);
#21654=EDGE_CURVE('',#17602,#17603,#13870,.T.);
#21655=EDGE_CURVE('',#17603,#17604,#13871,.T.);
#21656=EDGE_CURVE('',#17604,#17605,#1273,.T.);
#21657=EDGE_CURVE('',#17605,#17606,#13872,.T.);
#21658=EDGE_CURVE('',#17606,#17607,#13873,.T.);
#21659=EDGE_CURVE('',#17607,#17608,#13874,.T.);
#21660=EDGE_CURVE('',#17608,#17609,#13875,.T.);
#21661=EDGE_CURVE('',#17609,#17610,#13876,.T.);
#21662=EDGE_CURVE('',#17610,#17611,#1274,.T.);
#21663=EDGE_CURVE('',#17611,#17612,#13877,.T.);
#21664=EDGE_CURVE('',#17612,#17613,#13878,.T.);
#21665=EDGE_CURVE('',#17613,#17614,#13879,.T.);
#21666=EDGE_CURVE('',#17614,#17615,#13880,.T.);
#21667=EDGE_CURVE('',#17615,#17616,#13881,.T.);
#21668=EDGE_CURVE('',#17616,#17617,#1275,.T.);
#21669=EDGE_CURVE('',#17617,#17618,#13882,.T.);
#21670=EDGE_CURVE('',#17618,#17619,#13883,.T.);
#21671=EDGE_CURVE('',#17619,#17620,#13884,.T.);
#21672=EDGE_CURVE('',#17620,#17621,#13885,.T.);
#21673=EDGE_CURVE('',#17621,#17622,#13886,.T.);
#21674=EDGE_CURVE('',#17622,#17623,#1276,.T.);
#21675=EDGE_CURVE('',#17623,#17624,#13887,.T.);
#21676=EDGE_CURVE('',#17624,#17625,#13888,.T.);
#21677=EDGE_CURVE('',#17625,#17626,#13889,.T.);
#21678=EDGE_CURVE('',#17626,#17627,#13890,.T.);
#21679=EDGE_CURVE('',#17627,#17628,#13891,.T.);
#21680=EDGE_CURVE('',#17628,#17629,#1277,.T.);
#21681=EDGE_CURVE('',#17629,#17630,#13892,.T.);
#21682=EDGE_CURVE('',#17630,#17631,#13893,.T.);
#21683=EDGE_CURVE('',#17631,#17632,#13894,.T.);
#21684=EDGE_CURVE('',#17632,#17633,#13895,.T.);
#21685=EDGE_CURVE('',#17633,#17634,#13896,.T.);
#21686=EDGE_CURVE('',#17634,#17635,#1278,.T.);
#21687=EDGE_CURVE('',#17635,#17636,#13897,.T.);
#21688=EDGE_CURVE('',#17636,#17637,#13898,.T.);
#21689=EDGE_CURVE('',#17637,#17638,#13899,.T.);
#21690=EDGE_CURVE('',#17638,#17639,#13900,.T.);
#21691=EDGE_CURVE('',#17639,#17640,#13901,.T.);
#21692=EDGE_CURVE('',#17640,#17641,#1279,.T.);
#21693=EDGE_CURVE('',#17641,#17642,#13902,.T.);
#21694=EDGE_CURVE('',#17642,#17643,#13903,.T.);
#21695=EDGE_CURVE('',#17643,#17644,#13904,.T.);
#21696=EDGE_CURVE('',#17644,#17645,#13905,.T.);
#21697=EDGE_CURVE('',#17645,#17646,#13906,.T.);
#21698=EDGE_CURVE('',#17646,#17647,#1280,.T.);
#21699=EDGE_CURVE('',#17647,#17648,#13907,.T.);
#21700=EDGE_CURVE('',#17648,#17649,#13908,.T.);
#21701=EDGE_CURVE('',#17649,#17650,#13909,.T.);
#21702=EDGE_CURVE('',#17650,#17651,#13910,.T.);
#21703=EDGE_CURVE('',#17651,#17652,#13911,.T.);
#21704=EDGE_CURVE('',#17652,#17653,#1281,.T.);
#21705=EDGE_CURVE('',#17653,#17654,#13912,.T.);
#21706=EDGE_CURVE('',#17654,#17655,#13913,.T.);
#21707=EDGE_CURVE('',#17655,#17656,#13914,.T.);
#21708=EDGE_CURVE('',#17656,#17657,#13915,.T.);
#21709=EDGE_CURVE('',#17657,#17658,#13916,.T.);
#21710=EDGE_CURVE('',#17658,#17659,#1282,.T.);
#21711=EDGE_CURVE('',#17659,#17660,#13917,.T.);
#21712=EDGE_CURVE('',#17660,#17661,#13918,.T.);
#21713=EDGE_CURVE('',#17661,#17662,#13919,.T.);
#21714=EDGE_CURVE('',#17662,#17663,#13920,.T.);
#21715=EDGE_CURVE('',#17663,#17664,#13921,.T.);
#21716=EDGE_CURVE('',#17664,#17665,#1283,.T.);
#21717=EDGE_CURVE('',#17665,#17666,#13922,.T.);
#21718=EDGE_CURVE('',#17666,#17667,#13923,.T.);
#21719=EDGE_CURVE('',#17667,#17668,#13924,.T.);
#21720=EDGE_CURVE('',#17668,#17669,#13925,.T.);
#21721=EDGE_CURVE('',#17669,#17670,#13926,.T.);
#21722=EDGE_CURVE('',#17670,#17671,#1284,.T.);
#21723=EDGE_CURVE('',#17671,#17672,#13927,.T.);
#21724=EDGE_CURVE('',#17672,#17673,#13928,.T.);
#21725=EDGE_CURVE('',#17673,#17674,#13929,.T.);
#21726=EDGE_CURVE('',#17674,#17675,#13930,.T.);
#21727=EDGE_CURVE('',#17675,#17676,#13931,.T.);
#21728=EDGE_CURVE('',#17676,#17677,#1285,.T.);
#21729=EDGE_CURVE('',#17677,#17678,#13932,.T.);
#21730=EDGE_CURVE('',#17678,#17679,#13933,.T.);
#21731=EDGE_CURVE('',#17679,#17680,#13934,.T.);
#21732=EDGE_CURVE('',#17680,#17681,#13935,.T.);
#21733=EDGE_CURVE('',#17681,#17682,#13936,.T.);
#21734=EDGE_CURVE('',#17682,#17683,#1286,.T.);
#21735=EDGE_CURVE('',#17683,#17684,#13937,.T.);
#21736=EDGE_CURVE('',#17684,#17685,#13938,.T.);
#21737=EDGE_CURVE('',#17685,#17686,#13939,.T.);
#21738=EDGE_CURVE('',#17686,#17687,#13940,.T.);
#21739=EDGE_CURVE('',#17687,#17688,#13941,.T.);
#21740=EDGE_CURVE('',#17688,#17689,#1287,.T.);
#21741=EDGE_CURVE('',#17689,#17690,#13942,.T.);
#21742=EDGE_CURVE('',#17690,#17691,#13943,.T.);
#21743=EDGE_CURVE('',#17691,#17692,#13944,.T.);
#21744=EDGE_CURVE('',#17692,#17693,#13945,.T.);
#21745=EDGE_CURVE('',#17693,#17694,#13946,.T.);
#21746=EDGE_CURVE('',#17694,#17695,#1288,.T.);
#21747=EDGE_CURVE('',#17695,#17696,#13947,.T.);
#21748=EDGE_CURVE('',#17696,#17697,#13948,.T.);
#21749=EDGE_CURVE('',#17697,#17698,#13949,.T.);
#21750=EDGE_CURVE('',#17698,#17699,#13950,.T.);
#21751=EDGE_CURVE('',#17699,#17700,#13951,.T.);
#21752=EDGE_CURVE('',#17700,#17701,#1289,.T.);
#21753=EDGE_CURVE('',#17701,#17702,#13952,.T.);
#21754=EDGE_CURVE('',#17702,#17703,#13953,.T.);
#21755=EDGE_CURVE('',#17703,#17704,#13954,.T.);
#21756=EDGE_CURVE('',#17704,#17705,#13955,.T.);
#21757=EDGE_CURVE('',#17705,#17706,#13956,.T.);
#21758=EDGE_CURVE('',#17706,#17707,#1290,.T.);
#21759=EDGE_CURVE('',#17707,#17708,#13957,.T.);
#21760=EDGE_CURVE('',#17708,#17709,#13958,.T.);
#21761=EDGE_CURVE('',#17709,#17710,#13959,.T.);
#21762=EDGE_CURVE('',#17710,#17711,#13960,.T.);
#21763=EDGE_CURVE('',#17711,#17712,#13961,.T.);
#21764=EDGE_CURVE('',#17712,#17713,#1291,.T.);
#21765=EDGE_CURVE('',#17713,#17714,#13962,.T.);
#21766=EDGE_CURVE('',#17714,#17715,#13963,.T.);
#21767=EDGE_CURVE('',#17715,#17716,#13964,.T.);
#21768=EDGE_CURVE('',#17716,#17717,#13965,.T.);
#21769=EDGE_CURVE('',#17717,#17718,#13966,.T.);
#21770=EDGE_CURVE('',#17718,#17719,#1292,.T.);
#21771=EDGE_CURVE('',#17719,#17720,#13967,.T.);
#21772=EDGE_CURVE('',#17720,#17721,#13968,.T.);
#21773=EDGE_CURVE('',#17721,#17722,#13969,.T.);
#21774=EDGE_CURVE('',#17722,#17723,#13970,.T.);
#21775=EDGE_CURVE('',#17723,#17724,#13971,.T.);
#21776=EDGE_CURVE('',#17724,#17725,#1293,.T.);
#21777=EDGE_CURVE('',#17725,#17726,#13972,.T.);
#21778=EDGE_CURVE('',#17726,#17727,#13973,.T.);
#21779=EDGE_CURVE('',#17727,#17728,#13974,.T.);
#21780=EDGE_CURVE('',#17728,#17729,#13975,.T.);
#21781=EDGE_CURVE('',#17729,#17730,#13976,.T.);
#21782=EDGE_CURVE('',#17730,#17429,#1294,.T.);
#21783=EDGE_CURVE('',#17731,#17732,#13977,.T.);
#21784=EDGE_CURVE('',#17732,#17421,#13978,.T.);
#21785=EDGE_CURVE('',#17733,#17420,#1295,.T.);
#21786=EDGE_CURVE('',#17733,#17734,#886,.T.);
#21787=EDGE_CURVE('',#17734,#17731,#9689,.T.);
#21788=EDGE_CURVE('',#17735,#17736,#13979,.T.);
#21789=EDGE_CURVE('',#17735,#17732,#1296,.T.);
#21790=EDGE_CURVE('',#17731,#17736,#9690,.T.);
#21791=EDGE_CURVE('',#17737,#17738,#13980,.T.);
#21792=EDGE_CURVE('',#17738,#17739,#13981,.T.);
#21793=EDGE_CURVE('',#17739,#17740,#9691,.T.);
#21794=EDGE_CURVE('',#17741,#17740,#13982,.T.);
#21795=EDGE_CURVE('',#17741,#17742,#13983,.T.);
#21796=EDGE_CURVE('',#17742,#17737,#9692,.T.);
#21797=EDGE_CURVE('',#17743,#17424,#1297,.T.);
#21798=EDGE_CURVE('',#17743,#17739,#887,.T.);
#21799=EDGE_CURVE('',#17739,#17744,#9693,.T.);
#21800=EDGE_CURVE('',#17744,#17745,#13984,.T.);
#21801=EDGE_CURVE('',#17745,#17425,#13985,.T.);
#21802=EDGE_CURVE('',#17746,#17747,#13986,.T.);
#21803=EDGE_CURVE('',#17746,#17738,#1298,.T.);
#21804=EDGE_CURVE('',#17737,#17747,#9694,.T.);
#21805=EDGE_CURVE('',#17744,#17748,#9695,.T.);
#21806=EDGE_CURVE('',#17749,#17748,#13987,.T.);
#21807=EDGE_CURVE('',#17749,#17745,#1299,.T.);
#21808=EDGE_CURVE('',#17750,#17751,#13988,.T.);
#21809=EDGE_CURVE('',#17751,#17735,#13989,.T.);
#21810=EDGE_CURVE('',#17736,#17750,#13990,.T.);
#21811=EDGE_CURVE('',#17740,#17751,#9696,.T.);
#21812=EDGE_CURVE('',#17750,#17741,#1300,.T.);
#21813=EDGE_CURVE('',#17423,#17743,#888,.T.);
#21814=EDGE_CURVE('',#17752,#17753,#13991,.T.);
#21815=EDGE_CURVE('',#17753,#17746,#13992,.T.);
#21816=EDGE_CURVE('',#17747,#17752,#13993,.T.);
#21817=EDGE_CURVE('',#17748,#17754,#13994,.T.);
#21818=EDGE_CURVE('',#17754,#17755,#13995,.T.);
#21819=EDGE_CURVE('',#17755,#17749,#13996,.T.);
#21820=EDGE_CURVE('',#17756,#17757,#13997,.T.);
#21821=EDGE_CURVE('',#17757,#17758,#13998,.T.);
#21822=EDGE_CURVE('',#17758,#17759,#9697,.T.);
#21823=EDGE_CURVE('',#17760,#17759,#13999,.T.);
#21824=EDGE_CURVE('',#17760,#17761,#14000,.T.);
#21825=EDGE_CURVE('',#17761,#17756,#9698,.T.);
#21826=EDGE_CURVE('',#17762,#17763,#14001,.T.);
#21827=EDGE_CURVE('',#17762,#17758,#14002,.T.);
#21828=EDGE_CURVE('',#17758,#17764,#9699,.T.);
#21829=EDGE_CURVE('',#17764,#17765,#14003,.T.);
#21830=EDGE_CURVE('',#17765,#17766,#14004,.T.);
#21831=EDGE_CURVE('',#17766,#17763,#9700,.T.);
#21832=EDGE_CURVE('',#17759,#17753,#9701,.T.);
#21833=EDGE_CURVE('',#17752,#17760,#1301,.T.);
#21834=EDGE_CURVE('',#17754,#17762,#1302,.T.);
#21835=EDGE_CURVE('',#17763,#17755,#9702,.T.);
#21836=EDGE_CURVE('',#17767,#17768,#14005,.T.);
#21837=EDGE_CURVE('',#17767,#17757,#1303,.T.);
#21838=EDGE_CURVE('',#17756,#17768,#9703,.T.);
#21839=EDGE_CURVE('',#17764,#17769,#9704,.T.);
#21840=EDGE_CURVE('',#17770,#17769,#14006,.T.);
#21841=EDGE_CURVE('',#17770,#17765,#1304,.T.);
#21842=EDGE_CURVE('',#17771,#17772,#14007,.T.);
#21843=EDGE_CURVE('',#17772,#17767,#14008,.T.);
#21844=EDGE_CURVE('',#17768,#17771,#14009,.T.);
#21845=EDGE_CURVE('',#17769,#17773,#14010,.T.);
#21846=EDGE_CURVE('',#17773,#17774,#14011,.T.);
#21847=EDGE_CURVE('',#17774,#17770,#14012,.T.);
#21848=EDGE_CURVE('',#17775,#17776,#1305,.T.);
#21849=EDGE_CURVE('',#17776,#17777,#1306,.T.);
#21850=EDGE_CURVE('',#17777,#17778,#9705,.T.);
#21851=EDGE_CURVE('',#17779,#17778,#14013,.T.);
#21852=EDGE_CURVE('',#17779,#17780,#14014,.T.);
#21853=EDGE_CURVE('',#17780,#17775,#9706,.T.);
#21854=EDGE_CURVE('',#17781,#17782,#14015,.T.);
#21855=EDGE_CURVE('',#17781,#17777,#14016,.T.);
#21856=EDGE_CURVE('',#17777,#17783,#9707,.T.);
#21857=EDGE_CURVE('',#17783,#17784,#14017,.T.);
#21858=EDGE_CURVE('',#17784,#17785,#14018,.T.);
#21859=EDGE_CURVE('',#17785,#17782,#9708,.T.);
#21860=EDGE_CURVE('',#17778,#17772,#9709,.T.);
#21861=EDGE_CURVE('',#17771,#17779,#1307,.T.);
#21862=EDGE_CURVE('',#17773,#17781,#1308,.T.);
#21863=EDGE_CURVE('',#17782,#17774,#9710,.T.);
#21864=EDGE_CURVE('',#17786,#17787,#1309,.T.);
#21865=EDGE_CURVE('',#17786,#17776,#1310,.T.);
#21866=EDGE_CURVE('',#17775,#17787,#9711,.T.);
#21867=EDGE_CURVE('',#17783,#17788,#9712,.T.);
#21868=EDGE_CURVE('',#17789,#17788,#14019,.T.);
#21869=EDGE_CURVE('',#17789,#17784,#1311,.T.);
#21870=EDGE_CURVE('',#17790,#17791,#14020,.T.);
#21871=EDGE_CURVE('',#17791,#17786,#1312,.T.);
#21872=EDGE_CURVE('',#17787,#17790,#14021,.T.);
#21873=EDGE_CURVE('',#17788,#17792,#14022,.T.);
#21874=EDGE_CURVE('',#17792,#17793,#14023,.T.);
#21875=EDGE_CURVE('',#17793,#17789,#14024,.T.);
#21876=EDGE_CURVE('',#17794,#17795,#14025,.T.);
#21877=EDGE_CURVE('',#17795,#17796,#14026,.T.);
#21878=EDGE_CURVE('',#17796,#17797,#9713,.T.);
#21879=EDGE_CURVE('',#17798,#17797,#14027,.T.);
#21880=EDGE_CURVE('',#17798,#17799,#14028,.T.);
#21881=EDGE_CURVE('',#17799,#17794,#9714,.T.);
#21882=EDGE_CURVE('',#17800,#17801,#14029,.T.);
#21883=EDGE_CURVE('',#17800,#17796,#14030,.T.);
#21884=EDGE_CURVE('',#17796,#17802,#9715,.T.);
#21885=EDGE_CURVE('',#17802,#17803,#1313,.T.);
#21886=EDGE_CURVE('',#17803,#17804,#1314,.T.);
#21887=EDGE_CURVE('',#17804,#17801,#9716,.T.);
#21888=EDGE_CURVE('',#17797,#17791,#9717,.T.);
#21889=EDGE_CURVE('',#17790,#17798,#1315,.T.);
#21890=EDGE_CURVE('',#17792,#17800,#1316,.T.);
#21891=EDGE_CURVE('',#17801,#17793,#9718,.T.);
#21892=EDGE_CURVE('',#17805,#17806,#14031,.T.);
#21893=EDGE_CURVE('',#17805,#17795,#1317,.T.);
#21894=EDGE_CURVE('',#17794,#17806,#9719,.T.);
#21895=EDGE_CURVE('',#17802,#17807,#9720,.T.);
#21896=EDGE_CURVE('',#17808,#17807,#1318,.T.);
#21897=EDGE_CURVE('',#17808,#17803,#1319,.T.);
#21898=EDGE_CURVE('',#17809,#17810,#14032,.T.);
#21899=EDGE_CURVE('',#17810,#17805,#14033,.T.);
#21900=EDGE_CURVE('',#17806,#17809,#14034,.T.);
#21901=EDGE_CURVE('',#17807,#17811,#14035,.T.);
#21902=EDGE_CURVE('',#17811,#17812,#14036,.T.);
#21903=EDGE_CURVE('',#17812,#17808,#1320,.T.);
#21904=EDGE_CURVE('',#17813,#17814,#14037,.T.);
#21905=EDGE_CURVE('',#17814,#17815,#14038,.T.);
#21906=EDGE_CURVE('',#17815,#17816,#9721,.T.);
#21907=EDGE_CURVE('',#17817,#17816,#14039,.T.);
#21908=EDGE_CURVE('',#17817,#17818,#14040,.T.);
#21909=EDGE_CURVE('',#17818,#17813,#9722,.T.);
#21910=EDGE_CURVE('',#17819,#17820,#14041,.T.);
#21911=EDGE_CURVE('',#17819,#17815,#14042,.T.);
#21912=EDGE_CURVE('',#17815,#17821,#9723,.T.);
#21913=EDGE_CURVE('',#17821,#17822,#14043,.T.);
#21914=EDGE_CURVE('',#17822,#17823,#14044,.T.);
#21915=EDGE_CURVE('',#17823,#17820,#9724,.T.);
#21916=EDGE_CURVE('',#17816,#17810,#9725,.T.);
#21917=EDGE_CURVE('',#17809,#17817,#1321,.T.);
#21918=EDGE_CURVE('',#17811,#17819,#1322,.T.);
#21919=EDGE_CURVE('',#17820,#17812,#9726,.T.);
#21920=EDGE_CURVE('',#17824,#17825,#14045,.T.);
#21921=EDGE_CURVE('',#17824,#17814,#1323,.T.);
#21922=EDGE_CURVE('',#17813,#17825,#9727,.T.);
#21923=EDGE_CURVE('',#17821,#17826,#9728,.T.);
#21924=EDGE_CURVE('',#17827,#17826,#14046,.T.);
#21925=EDGE_CURVE('',#17827,#17822,#1324,.T.);
#21926=EDGE_CURVE('',#17828,#17829,#14047,.T.);
#21927=EDGE_CURVE('',#17829,#17824,#14048,.T.);
#21928=EDGE_CURVE('',#17825,#17828,#14049,.T.);
#21929=EDGE_CURVE('',#17826,#17830,#14050,.T.);
#21930=EDGE_CURVE('',#17830,#17831,#14051,.T.);
#21931=EDGE_CURVE('',#17831,#17827,#14052,.T.);
#21932=EDGE_CURVE('',#17832,#17833,#14053,.T.);
#21933=EDGE_CURVE('',#17833,#17834,#14054,.T.);
#21934=EDGE_CURVE('',#17834,#17835,#9729,.T.);
#21935=EDGE_CURVE('',#17836,#17835,#14055,.T.);
#21936=EDGE_CURVE('',#17836,#17837,#14056,.T.);
#21937=EDGE_CURVE('',#17837,#17832,#9730,.F.);
#21938=EDGE_CURVE('',#17838,#17839,#14057,.T.);
#21939=EDGE_CURVE('',#17838,#17834,#14058,.T.);
#21940=EDGE_CURVE('',#17834,#17840,#9731,.T.);
#21941=EDGE_CURVE('',#17840,#17841,#14059,.T.);
#21942=EDGE_CURVE('',#17841,#17842,#14060,.T.);
#21943=EDGE_CURVE('',#17842,#17839,#9732,.T.);
#21944=EDGE_CURVE('',#17835,#17829,#9733,.T.);
#21945=EDGE_CURVE('',#17828,#17836,#1325,.T.);
#21946=EDGE_CURVE('',#17830,#17838,#1326,.T.);
#21947=EDGE_CURVE('',#17839,#17831,#9734,.T.);
#21948=EDGE_CURVE('',#17576,#17833,#14061,.T.);
#21949=EDGE_CURVE('',#17832,#17577,#9735,.F.);
#21950=EDGE_CURVE('',#17840,#17843,#9736,.T.);
#21951=EDGE_CURVE('',#17844,#17843,#14062,.T.);
#21952=EDGE_CURVE('',#17844,#17841,#1327,.T.);
#21953=EDGE_CURVE('',#17843,#17845,#14063,.T.);
#21954=EDGE_CURVE('',#17845,#17846,#14064,.T.);
#21955=EDGE_CURVE('',#17846,#17844,#14065,.T.);
#21956=EDGE_CURVE('',#17573,#17847,#889,.T.);
#21957=EDGE_CURVE('',#17847,#17848,#9737,.T.);
#21958=EDGE_CURVE('',#17574,#17848,#890,.T.);
#21959=EDGE_CURVE('',#17849,#17850,#14066,.T.);
#21960=EDGE_CURVE('',#17849,#17847,#14067,.T.);
#21961=EDGE_CURVE('',#17847,#17851,#9738,.F.);
#21962=EDGE_CURVE('',#17851,#17852,#14068,.T.);
#21963=EDGE_CURVE('',#17852,#17853,#14069,.T.);
#21964=EDGE_CURVE('',#17853,#17850,#9739,.T.);
#21965=EDGE_CURVE('',#17848,#17575,#891,.T.);
#21966=EDGE_CURVE('',#17845,#17849,#1328,.T.);
#21967=EDGE_CURVE('',#17850,#17846,#9740,.T.);
#21968=EDGE_CURVE('',#17851,#17571,#9741,.F.);
#21969=EDGE_CURVE('',#17570,#17852,#14070,.T.);
#21970=EDGE_CURVE('',#17854,#17855,#14071,.T.);
#21971=EDGE_CURVE('',#17855,#17417,#14072,.T.);
#21972=EDGE_CURVE('',#17856,#17416,#1329,.T.);
#21973=EDGE_CURVE('',#17856,#17857,#892,.T.);
#21974=EDGE_CURVE('',#17857,#17854,#9742,.T.);
#21975=EDGE_CURVE('',#17858,#17859,#14073,.T.);
#21976=EDGE_CURVE('',#17858,#17855,#1330,.T.);
#21977=EDGE_CURVE('',#17854,#17859,#9743,.T.);
#21978=EDGE_CURVE('',#17860,#17861,#14074,.T.);
#21979=EDGE_CURVE('',#17861,#17858,#14075,.T.);
#21980=EDGE_CURVE('',#17859,#17860,#14076,.T.);
#21981=EDGE_CURVE('',#17862,#17863,#14077,.T.);
#21982=EDGE_CURVE('',#17863,#17734,#14078,.T.);
#21983=EDGE_CURVE('',#17734,#17864,#9744,.T.);
#21984=EDGE_CURVE('',#17865,#17864,#14079,.T.);
#21985=EDGE_CURVE('',#17865,#17866,#14080,.T.);
#21986=EDGE_CURVE('',#17866,#17862,#9745,.T.);
#21987=EDGE_CURVE('',#17864,#17861,#9746,.T.);
#21988=EDGE_CURVE('',#17860,#17865,#1331,.T.);
#21989=EDGE_CURVE('',#17419,#17733,#893,.T.);
#21990=EDGE_CURVE('',#17867,#17868,#14081,.T.);
#21991=EDGE_CURVE('',#17867,#17863,#1332,.T.);
#21992=EDGE_CURVE('',#17862,#17868,#9747,.T.);
#21993=EDGE_CURVE('',#17869,#17870,#14082,.T.);
#21994=EDGE_CURVE('',#17870,#17742,#14083,.T.);
#21995=EDGE_CURVE('',#17742,#17871,#9748,.T.);
#21996=EDGE_CURVE('',#17872,#17871,#14084,.T.);
#21997=EDGE_CURVE('',#17872,#17873,#14085,.T.);
#21998=EDGE_CURVE('',#17873,#17869,#9749,.T.);
#21999=EDGE_CURVE('',#17874,#17875,#14086,.T.);
#22000=EDGE_CURVE('',#17874,#17870,#1333,.T.);
#22001=EDGE_CURVE('',#17869,#17875,#9750,.T.);
#22002=EDGE_CURVE('',#17876,#17877,#14087,.T.);
#22003=EDGE_CURVE('',#17877,#17867,#14088,.T.);
#22004=EDGE_CURVE('',#17868,#17876,#14089,.T.);
#22005=EDGE_CURVE('',#17871,#17877,#9751,.T.);
#22006=EDGE_CURVE('',#17876,#17872,#1334,.T.);
#22007=EDGE_CURVE('',#17878,#17879,#14090,.T.);
#22008=EDGE_CURVE('',#17879,#17874,#14091,.T.);
#22009=EDGE_CURVE('',#17875,#17878,#14092,.T.);
#22010=EDGE_CURVE('',#17880,#17881,#1335,.T.);
#22011=EDGE_CURVE('',#17881,#17761,#1336,.T.);
#22012=EDGE_CURVE('',#17761,#17882,#9752,.T.);
#22013=EDGE_CURVE('',#17883,#17882,#14093,.T.);
#22014=EDGE_CURVE('',#17883,#17884,#14094,.T.);
#22015=EDGE_CURVE('',#17884,#17880,#9753,.T.);
#22016=EDGE_CURVE('',#17882,#17879,#9754,.T.);
#22017=EDGE_CURVE('',#17878,#17883,#1337,.T.);
#22018=EDGE_CURVE('',#17885,#17886,#1338,.T.);
#22019=EDGE_CURVE('',#17885,#17881,#1339,.T.);
#22020=EDGE_CURVE('',#17880,#17886,#9755,.T.);
#22021=EDGE_CURVE('',#17887,#17888,#14095,.T.);
#22022=EDGE_CURVE('',#17888,#17885,#1340,.T.);
#22023=EDGE_CURVE('',#17886,#17887,#14096,.T.);
#22024=EDGE_CURVE('',#17889,#17890,#14097,.T.);
#22025=EDGE_CURVE('',#17890,#17780,#14098,.T.);
#22026=EDGE_CURVE('',#17780,#17891,#9756,.T.);
#22027=EDGE_CURVE('',#17892,#17891,#14099,.T.);
#22028=EDGE_CURVE('',#17892,#17893,#14100,.T.);
#22029=EDGE_CURVE('',#17893,#17889,#9757,.T.);
#22030=EDGE_CURVE('',#17891,#17888,#9758,.T.);
#22031=EDGE_CURVE('',#17887,#17892,#1341,.T.);
#22032=EDGE_CURVE('',#17894,#17895,#14101,.T.);
#22033=EDGE_CURVE('',#17894,#17890,#1342,.T.);
#22034=EDGE_CURVE('',#17889,#17895,#9759,.T.);
#22035=EDGE_CURVE('',#17896,#17897,#14102,.T.);
#22036=EDGE_CURVE('',#17897,#17894,#14103,.T.);
#22037=EDGE_CURVE('',#17895,#17896,#14104,.T.);
#22038=EDGE_CURVE('',#17898,#17899,#14105,.T.);
#22039=EDGE_CURVE('',#17899,#17799,#14106,.T.);
#22040=EDGE_CURVE('',#17799,#17900,#9760,.T.);
#22041=EDGE_CURVE('',#17901,#17900,#14107,.T.);
#22042=EDGE_CURVE('',#17901,#17902,#14108,.T.);
#22043=EDGE_CURVE('',#17902,#17898,#9761,.T.);
#22044=EDGE_CURVE('',#17900,#17897,#9762,.T.);
#22045=EDGE_CURVE('',#17896,#17901,#1343,.T.);
#22046=EDGE_CURVE('',#17903,#17904,#14109,.T.);
#22047=EDGE_CURVE('',#17903,#17899,#1344,.T.);
#22048=EDGE_CURVE('',#17898,#17904,#9763,.T.);
#22049=EDGE_CURVE('',#17905,#17906,#14110,.T.);
#22050=EDGE_CURVE('',#17906,#17903,#14111,.T.);
#22051=EDGE_CURVE('',#17904,#17905,#14112,.T.);
#22052=EDGE_CURVE('',#17907,#17908,#14113,.T.);
#22053=EDGE_CURVE('',#17908,#17818,#14114,.T.);
#22054=EDGE_CURVE('',#17818,#17909,#9764,.T.);
#22055=EDGE_CURVE('',#17910,#17909,#14115,.T.);
#22056=EDGE_CURVE('',#17910,#17911,#14116,.T.);
#22057=EDGE_CURVE('',#17911,#17907,#9765,.F.);
#22058=EDGE_CURVE('',#17909,#17906,#9766,.T.);
#22059=EDGE_CURVE('',#17905,#17910,#1345,.T.);
#22060=EDGE_CURVE('',#17582,#17908,#14117,.T.);
#22061=EDGE_CURVE('',#17907,#17583,#9767,.F.);
#22062=EDGE_CURVE('',#17579,#17837,#894,.T.);
#22063=EDGE_CURVE('',#17837,#17912,#9768,.T.);
#22064=EDGE_CURVE('',#17580,#17912,#895,.T.);
#22065=EDGE_CURVE('',#17912,#17581,#896,.T.);
#22066=EDGE_CURVE('',#17913,#17914,#14118,.T.);
#22067=EDGE_CURVE('',#17914,#17413,#14119,.T.);
#22068=EDGE_CURVE('',#17915,#17412,#1346,.T.);
#22069=EDGE_CURVE('',#17915,#17916,#897,.T.);
#22070=EDGE_CURVE('',#17916,#17913,#9769,.T.);
#22071=EDGE_CURVE('',#17917,#17918,#14120,.T.);
#22072=EDGE_CURVE('',#17917,#17914,#1347,.T.);
#22073=EDGE_CURVE('',#17913,#17918,#9770,.T.);
#22074=EDGE_CURVE('',#17919,#17920,#14121,.T.);
#22075=EDGE_CURVE('',#17920,#17917,#14122,.T.);
#22076=EDGE_CURVE('',#17918,#17919,#14123,.T.);
#22077=EDGE_CURVE('',#17921,#17922,#14124,.T.);
#22078=EDGE_CURVE('',#17922,#17857,#14125,.T.);
#22079=EDGE_CURVE('',#17857,#17923,#9771,.T.);
#22080=EDGE_CURVE('',#17924,#17923,#14126,.T.);
#22081=EDGE_CURVE('',#17924,#17925,#14127,.T.);
#22082=EDGE_CURVE('',#17925,#17921,#9772,.T.);
#22083=EDGE_CURVE('',#17923,#17920,#9773,.T.);
#22084=EDGE_CURVE('',#17919,#17924,#1348,.T.);
#22085=EDGE_CURVE('',#17415,#17856,#898,.T.);
#22086=EDGE_CURVE('',#17926,#17927,#14128,.T.);
#22087=EDGE_CURVE('',#17926,#17922,#1349,.T.);
#22088=EDGE_CURVE('',#17921,#17927,#9774,.T.);
#22089=EDGE_CURVE('',#17928,#17929,#14129,.T.);
#22090=EDGE_CURVE('',#17929,#17926,#14130,.T.);
#22091=EDGE_CURVE('',#17927,#17928,#14131,.T.);
#22092=EDGE_CURVE('',#17930,#17931,#14132,.T.);
#22093=EDGE_CURVE('',#17931,#17866,#14133,.T.);
#22094=EDGE_CURVE('',#17866,#17932,#9775,.T.);
#22095=EDGE_CURVE('',#17933,#17932,#14134,.T.);
#22096=EDGE_CURVE('',#17933,#17934,#14135,.T.);
#22097=EDGE_CURVE('',#17934,#17930,#9776,.T.);
#22098=EDGE_CURVE('',#17932,#17929,#9777,.T.);
#22099=EDGE_CURVE('',#17928,#17933,#1350,.T.);
#22100=EDGE_CURVE('',#17935,#17936,#14136,.T.);
#22101=EDGE_CURVE('',#17935,#17931,#1351,.T.);
#22102=EDGE_CURVE('',#17930,#17936,#9778,.T.);
#22103=EDGE_CURVE('',#17937,#17938,#1352,.T.);
#22104=EDGE_CURVE('',#17938,#17873,#1353,.T.);
#22105=EDGE_CURVE('',#17873,#17939,#9779,.T.);
#22106=EDGE_CURVE('',#17940,#17939,#14137,.T.);
#22107=EDGE_CURVE('',#17940,#17941,#14138,.T.);
#22108=EDGE_CURVE('',#17941,#17937,#9780,.T.);
#22109=EDGE_CURVE('',#17942,#17943,#1354,.T.);
#22110=EDGE_CURVE('',#17942,#17938,#1355,.T.);
#22111=EDGE_CURVE('',#17937,#17943,#9781,.T.);
#22112=EDGE_CURVE('',#17944,#17945,#14139,.T.);
#22113=EDGE_CURVE('',#17945,#17935,#14140,.T.);
#22114=EDGE_CURVE('',#17936,#17944,#14141,.T.);
#22115=EDGE_CURVE('',#17939,#17945,#9782,.T.);
#22116=EDGE_CURVE('',#17944,#17940,#1356,.T.);
#22117=EDGE_CURVE('',#17946,#17947,#14142,.T.);
#22118=EDGE_CURVE('',#17947,#17942,#1357,.T.);
#22119=EDGE_CURVE('',#17943,#17946,#14143,.T.);
#22120=EDGE_CURVE('',#17948,#17949,#14144,.T.);
#22121=EDGE_CURVE('',#17949,#17884,#14145,.T.);
#22122=EDGE_CURVE('',#17884,#17950,#9783,.T.);
#22123=EDGE_CURVE('',#17951,#17950,#14146,.T.);
#22124=EDGE_CURVE('',#17951,#17952,#14147,.T.);
#22125=EDGE_CURVE('',#17952,#17948,#9784,.T.);
#22126=EDGE_CURVE('',#17950,#17947,#9785,.T.);
#22127=EDGE_CURVE('',#17946,#17951,#1358,.T.);
#22128=EDGE_CURVE('',#17953,#17954,#14148,.T.);
#22129=EDGE_CURVE('',#17953,#17949,#1359,.T.);
#22130=EDGE_CURVE('',#17948,#17954,#9786,.T.);
#22131=EDGE_CURVE('',#17955,#17956,#14149,.T.);
#22132=EDGE_CURVE('',#17956,#17953,#14150,.T.);
#22133=EDGE_CURVE('',#17954,#17955,#14151,.T.);
#22134=EDGE_CURVE('',#17957,#17958,#14152,.T.);
#22135=EDGE_CURVE('',#17958,#17893,#14153,.T.);
#22136=EDGE_CURVE('',#17893,#17959,#9787,.T.);
#22137=EDGE_CURVE('',#17960,#17959,#14154,.T.);
#22138=EDGE_CURVE('',#17960,#17961,#14155,.T.);
#22139=EDGE_CURVE('',#17961,#17957,#9788,.T.);
#22140=EDGE_CURVE('',#17959,#17956,#9789,.T.);
#22141=EDGE_CURVE('',#17955,#17960,#1360,.T.);
#22142=EDGE_CURVE('',#17962,#17963,#14156,.T.);
#22143=EDGE_CURVE('',#17962,#17958,#1361,.T.);
#22144=EDGE_CURVE('',#17957,#17963,#9790,.T.);
#22145=EDGE_CURVE('',#17964,#17965,#14157,.T.);
#22146=EDGE_CURVE('',#17965,#17962,#14158,.T.);
#22147=EDGE_CURVE('',#17963,#17964,#14159,.T.);
#22148=EDGE_CURVE('',#17966,#17967,#14160,.T.);
#22149=EDGE_CURVE('',#17967,#17902,#14161,.T.);
#22150=EDGE_CURVE('',#17902,#17968,#9791,.T.);
#22151=EDGE_CURVE('',#17969,#17968,#14162,.T.);
#22152=EDGE_CURVE('',#17969,#17970,#14163,.T.);
#22153=EDGE_CURVE('',#17970,#17966,#9792,.F.);
#22154=EDGE_CURVE('',#17968,#17965,#9793,.T.);
#22155=EDGE_CURVE('',#17964,#17969,#1362,.T.);
#22156=EDGE_CURVE('',#17588,#17967,#14164,.T.);
#22157=EDGE_CURVE('',#17966,#17589,#9794,.F.);
#22158=EDGE_CURVE('',#17585,#17911,#899,.T.);
#22159=EDGE_CURVE('',#17911,#17971,#9795,.T.);
#22160=EDGE_CURVE('',#17586,#17971,#900,.T.);
#22161=EDGE_CURVE('',#17971,#17587,#901,.T.);
#22162=EDGE_CURVE('',#17972,#17973,#14165,.T.);
#22163=EDGE_CURVE('',#17973,#17409,#14166,.T.);
#22164=EDGE_CURVE('',#17974,#17408,#1363,.T.);
#22165=EDGE_CURVE('',#17974,#17975,#902,.T.);
#22166=EDGE_CURVE('',#17975,#17972,#9796,.T.);
#22167=EDGE_CURVE('',#17976,#17977,#14167,.T.);
#22168=EDGE_CURVE('',#17976,#17973,#1364,.T.);
#22169=EDGE_CURVE('',#17972,#17977,#9797,.T.);
#22170=EDGE_CURVE('',#17978,#17979,#14168,.T.);
#22171=EDGE_CURVE('',#17979,#17976,#14169,.T.);
#22172=EDGE_CURVE('',#17977,#17978,#14170,.T.);
#22173=EDGE_CURVE('',#17980,#17981,#14171,.T.);
#22174=EDGE_CURVE('',#17981,#17916,#14172,.T.);
#22175=EDGE_CURVE('',#17916,#17982,#9798,.T.);
#22176=EDGE_CURVE('',#17983,#17982,#14173,.T.);
#22177=EDGE_CURVE('',#17983,#17984,#14174,.T.);
#22178=EDGE_CURVE('',#17984,#17980,#9799,.T.);
#22179=EDGE_CURVE('',#17982,#17979,#9800,.T.);
#22180=EDGE_CURVE('',#17978,#17983,#1365,.T.);
#22181=EDGE_CURVE('',#17411,#17915,#903,.T.);
#22182=EDGE_CURVE('',#17985,#17986,#14175,.T.);
#22183=EDGE_CURVE('',#17985,#17981,#1366,.T.);
#22184=EDGE_CURVE('',#17980,#17986,#9801,.T.);
#22185=EDGE_CURVE('',#17987,#17988,#14176,.T.);
#22186=EDGE_CURVE('',#17988,#17985,#14177,.T.);
#22187=EDGE_CURVE('',#17986,#17987,#14178,.T.);
#22188=EDGE_CURVE('',#17989,#17990,#14179,.T.);
#22189=EDGE_CURVE('',#17990,#17925,#14180,.T.);
#22190=EDGE_CURVE('',#17925,#17991,#9802,.T.);
#22191=EDGE_CURVE('',#17992,#17991,#14181,.T.);
#22192=EDGE_CURVE('',#17992,#17993,#14182,.T.);
#22193=EDGE_CURVE('',#17993,#17989,#9803,.T.);
#22194=EDGE_CURVE('',#17991,#17988,#9804,.T.);
#22195=EDGE_CURVE('',#17987,#17992,#1367,.T.);
#22196=EDGE_CURVE('',#17994,#17995,#14183,.T.);
#22197=EDGE_CURVE('',#17994,#17990,#1368,.T.);
#22198=EDGE_CURVE('',#17989,#17995,#9805,.T.);
#22199=EDGE_CURVE('',#17996,#17997,#14184,.T.);
#22200=EDGE_CURVE('',#17997,#17994,#14185,.T.);
#22201=EDGE_CURVE('',#17995,#17996,#14186,.T.);
#22202=EDGE_CURVE('',#17998,#17999,#1369,.T.);
#22203=EDGE_CURVE('',#17999,#17934,#1370,.T.);
#22204=EDGE_CURVE('',#17934,#18000,#9806,.T.);
#22205=EDGE_CURVE('',#18001,#18000,#14187,.T.);
#22206=EDGE_CURVE('',#18001,#18002,#14188,.T.);
#22207=EDGE_CURVE('',#18002,#17998,#9807,.T.);
#22208=EDGE_CURVE('',#18000,#17997,#9808,.T.);
#22209=EDGE_CURVE('',#17996,#18001,#1371,.T.);
#22210=EDGE_CURVE('',#18003,#18004,#1372,.T.);
#22211=EDGE_CURVE('',#18003,#17999,#1373,.T.);
#22212=EDGE_CURVE('',#17998,#18004,#9809,.T.);
#22213=EDGE_CURVE('',#18005,#18006,#14189,.T.);
#22214=EDGE_CURVE('',#18006,#17941,#14190,.T.);
#22215=EDGE_CURVE('',#17941,#18007,#9810,.T.);
#22216=EDGE_CURVE('',#18008,#18007,#14191,.T.);
#22217=EDGE_CURVE('',#18008,#18009,#14192,.T.);
#22218=EDGE_CURVE('',#18009,#18005,#9811,.T.);
#22219=EDGE_CURVE('',#18010,#18011,#14193,.T.);
#22220=EDGE_CURVE('',#18010,#18006,#1374,.T.);
#22221=EDGE_CURVE('',#18005,#18011,#9812,.T.);
#22222=EDGE_CURVE('',#18012,#18013,#14194,.T.);
#22223=EDGE_CURVE('',#18013,#18003,#1375,.T.);
#22224=EDGE_CURVE('',#18004,#18012,#14195,.T.);
#22225=EDGE_CURVE('',#18007,#18013,#9813,.T.);
#22226=EDGE_CURVE('',#18012,#18008,#1376,.T.);
#22227=EDGE_CURVE('',#18014,#18015,#14196,.T.);
#22228=EDGE_CURVE('',#18015,#18010,#14197,.T.);
#22229=EDGE_CURVE('',#18011,#18014,#14198,.T.);
#22230=EDGE_CURVE('',#18016,#18017,#14199,.T.);
#22231=EDGE_CURVE('',#18017,#17952,#14200,.T.);
#22232=EDGE_CURVE('',#17952,#18018,#9814,.T.);
#22233=EDGE_CURVE('',#18019,#18018,#14201,.T.);
#22234=EDGE_CURVE('',#18019,#18020,#14202,.T.);
#22235=EDGE_CURVE('',#18020,#18016,#9815,.T.);
#22236=EDGE_CURVE('',#18018,#18015,#9816,.T.);
#22237=EDGE_CURVE('',#18014,#18019,#1377,.T.);
#22238=EDGE_CURVE('',#18021,#18022,#14203,.T.);
#22239=EDGE_CURVE('',#18021,#18017,#1378,.T.);
#22240=EDGE_CURVE('',#18016,#18022,#9817,.T.);
#22241=EDGE_CURVE('',#18023,#18024,#14204,.T.);
#22242=EDGE_CURVE('',#18024,#18021,#14205,.T.);
#22243=EDGE_CURVE('',#18022,#18023,#14206,.T.);
#22244=EDGE_CURVE('',#18025,#18026,#14207,.T.);
#22245=EDGE_CURVE('',#18026,#17961,#14208,.T.);
#22246=EDGE_CURVE('',#17961,#18027,#9818,.T.);
#22247=EDGE_CURVE('',#18028,#18027,#14209,.T.);
#22248=EDGE_CURVE('',#18028,#18029,#14210,.T.);
#22249=EDGE_CURVE('',#18029,#18025,#9819,.F.);
#22250=EDGE_CURVE('',#18027,#18024,#9820,.T.);
#22251=EDGE_CURVE('',#18023,#18028,#1379,.T.);
#22252=EDGE_CURVE('',#17594,#18026,#14211,.T.);
#22253=EDGE_CURVE('',#18025,#17595,#9821,.F.);
#22254=EDGE_CURVE('',#17591,#17970,#904,.T.);
#22255=EDGE_CURVE('',#17970,#18030,#9822,.T.);
#22256=EDGE_CURVE('',#17592,#18030,#905,.T.);
#22257=EDGE_CURVE('',#18030,#17593,#906,.T.);
#22258=EDGE_CURVE('',#18031,#18032,#14212,.T.);
#22259=EDGE_CURVE('',#18032,#17405,#14213,.T.);
#22260=EDGE_CURVE('',#18033,#17404,#1380,.T.);
#22261=EDGE_CURVE('',#18033,#18034,#907,.T.);
#22262=EDGE_CURVE('',#18034,#18031,#9823,.T.);
#22263=EDGE_CURVE('',#18035,#18036,#14214,.T.);
#22264=EDGE_CURVE('',#18035,#18032,#1381,.T.);
#22265=EDGE_CURVE('',#18031,#18036,#9824,.T.);
#22266=EDGE_CURVE('',#18037,#18038,#14215,.T.);
#22267=EDGE_CURVE('',#18038,#18035,#14216,.T.);
#22268=EDGE_CURVE('',#18036,#18037,#14217,.T.);
#22269=EDGE_CURVE('',#18039,#18040,#14218,.T.);
#22270=EDGE_CURVE('',#18040,#17975,#14219,.T.);
#22271=EDGE_CURVE('',#17975,#18041,#9825,.T.);
#22272=EDGE_CURVE('',#18042,#18041,#14220,.T.);
#22273=EDGE_CURVE('',#18042,#18043,#14221,.T.);
#22274=EDGE_CURVE('',#18043,#18039,#9826,.T.);
#22275=EDGE_CURVE('',#18041,#18038,#9827,.T.);
#22276=EDGE_CURVE('',#18037,#18042,#1382,.T.);
#22277=EDGE_CURVE('',#17407,#17974,#908,.T.);
#22278=EDGE_CURVE('',#18044,#18045,#14222,.T.);
#22279=EDGE_CURVE('',#18044,#18040,#1383,.T.);
#22280=EDGE_CURVE('',#18039,#18045,#9828,.T.);
#22281=EDGE_CURVE('',#18046,#18047,#14223,.T.);
#22282=EDGE_CURVE('',#18047,#18044,#14224,.T.);
#22283=EDGE_CURVE('',#18045,#18046,#14225,.T.);
#22284=EDGE_CURVE('',#18048,#18049,#14226,.T.);
#22285=EDGE_CURVE('',#18049,#17984,#14227,.T.);
#22286=EDGE_CURVE('',#17984,#18050,#9829,.T.);
#22287=EDGE_CURVE('',#18051,#18050,#14228,.T.);
#22288=EDGE_CURVE('',#18051,#18052,#14229,.T.);
#22289=EDGE_CURVE('',#18052,#18048,#9830,.T.);
#22290=EDGE_CURVE('',#18050,#18047,#9831,.T.);
#22291=EDGE_CURVE('',#18046,#18051,#1384,.T.);
#22292=EDGE_CURVE('',#18053,#18054,#14230,.T.);
#22293=EDGE_CURVE('',#18053,#18049,#1385,.T.);
#22294=EDGE_CURVE('',#18048,#18054,#9832,.T.);
#22295=EDGE_CURVE('',#18055,#18056,#14231,.T.);
#22296=EDGE_CURVE('',#18056,#18053,#14232,.T.);
#22297=EDGE_CURVE('',#18054,#18055,#14233,.T.);
#22298=EDGE_CURVE('',#18057,#18058,#1386,.T.);
#22299=EDGE_CURVE('',#18058,#17993,#1387,.T.);
#22300=EDGE_CURVE('',#17993,#18059,#9833,.T.);
#22301=EDGE_CURVE('',#18060,#18059,#14234,.T.);
#22302=EDGE_CURVE('',#18060,#18061,#14235,.T.);
#22303=EDGE_CURVE('',#18061,#18057,#9834,.T.);
#22304=EDGE_CURVE('',#18059,#18056,#9835,.T.);
#22305=EDGE_CURVE('',#18055,#18060,#1388,.T.);
#22306=EDGE_CURVE('',#18062,#18063,#1389,.T.);
#22307=EDGE_CURVE('',#18062,#18058,#1390,.T.);
#22308=EDGE_CURVE('',#18057,#18063,#9836,.T.);
#22309=EDGE_CURVE('',#18064,#18065,#14236,.T.);
#22310=EDGE_CURVE('',#18065,#18062,#1391,.T.);
#22311=EDGE_CURVE('',#18063,#18064,#14237,.T.);
#22312=EDGE_CURVE('',#18066,#18067,#14238,.T.);
#22313=EDGE_CURVE('',#18067,#18002,#14239,.T.);
#22314=EDGE_CURVE('',#18002,#18068,#9837,.T.);
#22315=EDGE_CURVE('',#18069,#18068,#14240,.T.);
#22316=EDGE_CURVE('',#18069,#18070,#14241,.T.);
#22317=EDGE_CURVE('',#18070,#18066,#9838,.T.);
#22318=EDGE_CURVE('',#18068,#18065,#9839,.T.);
#22319=EDGE_CURVE('',#18064,#18069,#1392,.T.);
#22320=EDGE_CURVE('',#18071,#18072,#14242,.T.);
#22321=EDGE_CURVE('',#18071,#18067,#1393,.T.);
#22322=EDGE_CURVE('',#18066,#18072,#9840,.T.);
#22323=EDGE_CURVE('',#18073,#18074,#14243,.T.);
#22324=EDGE_CURVE('',#18074,#18009,#14244,.T.);
#22325=EDGE_CURVE('',#18009,#18075,#9841,.T.);
#22326=EDGE_CURVE('',#18076,#18075,#14245,.T.);
#22327=EDGE_CURVE('',#18076,#18077,#14246,.T.);
#22328=EDGE_CURVE('',#18077,#18073,#9842,.T.);
#22329=EDGE_CURVE('',#18078,#18079,#14247,.T.);
#22330=EDGE_CURVE('',#18078,#18074,#1394,.T.);
#22331=EDGE_CURVE('',#18073,#18079,#9843,.T.);
#22332=EDGE_CURVE('',#18080,#18081,#14248,.T.);
#22333=EDGE_CURVE('',#18081,#18071,#14249,.T.);
#22334=EDGE_CURVE('',#18072,#18080,#14250,.T.);
#22335=EDGE_CURVE('',#18075,#18081,#9844,.T.);
#22336=EDGE_CURVE('',#18080,#18076,#1395,.T.);
#22337=EDGE_CURVE('',#18082,#18083,#14251,.T.);
#22338=EDGE_CURVE('',#18083,#18078,#14252,.T.);
#22339=EDGE_CURVE('',#18079,#18082,#14253,.T.);
#22340=EDGE_CURVE('',#18084,#18085,#14254,.T.);
#22341=EDGE_CURVE('',#18085,#18020,#14255,.T.);
#22342=EDGE_CURVE('',#18020,#18086,#9845,.T.);
#22343=EDGE_CURVE('',#18087,#18086,#14256,.T.);
#22344=EDGE_CURVE('',#18087,#18088,#14257,.T.);
#22345=EDGE_CURVE('',#18088,#18084,#9846,.F.);
#22346=EDGE_CURVE('',#18086,#18083,#9847,.T.);
#22347=EDGE_CURVE('',#18082,#18087,#1396,.T.);
#22348=EDGE_CURVE('',#17600,#18085,#14258,.T.);
#22349=EDGE_CURVE('',#18084,#17601,#9848,.F.);
#22350=EDGE_CURVE('',#17597,#18029,#909,.T.);
#22351=EDGE_CURVE('',#18029,#18089,#9849,.T.);
#22352=EDGE_CURVE('',#17598,#18089,#910,.T.);
#22353=EDGE_CURVE('',#18089,#17599,#911,.T.);
#22354=EDGE_CURVE('',#18090,#18091,#14259,.T.);
#22355=EDGE_CURVE('',#18091,#17401,#14260,.T.);
#22356=EDGE_CURVE('',#18092,#17400,#1397,.T.);
#22357=EDGE_CURVE('',#18092,#18093,#912,.T.);
#22358=EDGE_CURVE('',#18093,#18090,#9850,.T.);
#22359=EDGE_CURVE('',#18094,#18095,#14261,.T.);
#22360=EDGE_CURVE('',#18094,#18091,#1398,.T.);
#22361=EDGE_CURVE('',#18090,#18095,#9851,.T.);
#22362=EDGE_CURVE('',#18096,#18097,#14262,.T.);
#22363=EDGE_CURVE('',#18097,#18094,#14263,.T.);
#22364=EDGE_CURVE('',#18095,#18096,#14264,.T.);
#22365=EDGE_CURVE('',#18098,#18099,#14265,.T.);
#22366=EDGE_CURVE('',#18099,#18034,#14266,.T.);
#22367=EDGE_CURVE('',#18034,#18100,#9852,.T.);
#22368=EDGE_CURVE('',#18101,#18100,#14267,.T.);
#22369=EDGE_CURVE('',#18101,#18102,#14268,.T.);
#22370=EDGE_CURVE('',#18102,#18098,#9853,.T.);
#22371=EDGE_CURVE('',#18100,#18097,#9854,.T.);
#22372=EDGE_CURVE('',#18096,#18101,#1399,.T.);
#22373=EDGE_CURVE('',#17403,#18033,#913,.T.);
#22374=EDGE_CURVE('',#18103,#18104,#14269,.T.);
#22375=EDGE_CURVE('',#18103,#18099,#1400,.T.);
#22376=EDGE_CURVE('',#18098,#18104,#9855,.T.);
#22377=EDGE_CURVE('',#18105,#18106,#14270,.T.);
#22378=EDGE_CURVE('',#18106,#18103,#14271,.T.);
#22379=EDGE_CURVE('',#18104,#18105,#14272,.T.);
#22380=EDGE_CURVE('',#18107,#18108,#14273,.T.);
#22381=EDGE_CURVE('',#18108,#18043,#14274,.T.);
#22382=EDGE_CURVE('',#18043,#18109,#9856,.T.);
#22383=EDGE_CURVE('',#18110,#18109,#14275,.T.);
#22384=EDGE_CURVE('',#18110,#18111,#14276,.T.);
#22385=EDGE_CURVE('',#18111,#18107,#9857,.T.);
#22386=EDGE_CURVE('',#18109,#18106,#9858,.T.);
#22387=EDGE_CURVE('',#18105,#18110,#1401,.T.);
#22388=EDGE_CURVE('',#18112,#18113,#14277,.T.);
#22389=EDGE_CURVE('',#18112,#18108,#1402,.T.);
#22390=EDGE_CURVE('',#18107,#18113,#9859,.T.);
#22391=EDGE_CURVE('',#18114,#18115,#14278,.T.);
#22392=EDGE_CURVE('',#18115,#18112,#14279,.T.);
#22393=EDGE_CURVE('',#18113,#18114,#14280,.T.);
#22394=EDGE_CURVE('',#18116,#18117,#1403,.T.);
#22395=EDGE_CURVE('',#18117,#18052,#1404,.T.);
#22396=EDGE_CURVE('',#18052,#18118,#9860,.T.);
#22397=EDGE_CURVE('',#18119,#18118,#14281,.T.);
#22398=EDGE_CURVE('',#18119,#18120,#14282,.T.);
#22399=EDGE_CURVE('',#18120,#18116,#9861,.T.);
#22400=EDGE_CURVE('',#18118,#18115,#9862,.T.);
#22401=EDGE_CURVE('',#18114,#18119,#1405,.T.);
#22402=EDGE_CURVE('',#18121,#18122,#1406,.T.);
#22403=EDGE_CURVE('',#18121,#18117,#1407,.T.);
#22404=EDGE_CURVE('',#18116,#18122,#9863,.T.);
#22405=EDGE_CURVE('',#18123,#18124,#14283,.T.);
#22406=EDGE_CURVE('',#18124,#18121,#1408,.T.);
#22407=EDGE_CURVE('',#18122,#18123,#14284,.T.);
#22408=EDGE_CURVE('',#18125,#18126,#14285,.T.);
#22409=EDGE_CURVE('',#18126,#18061,#14286,.T.);
#22410=EDGE_CURVE('',#18061,#18127,#9864,.T.);
#22411=EDGE_CURVE('',#18128,#18127,#14287,.T.);
#22412=EDGE_CURVE('',#18128,#18129,#14288,.T.);
#22413=EDGE_CURVE('',#18129,#18125,#9865,.T.);
#22414=EDGE_CURVE('',#18127,#18124,#9866,.T.);
#22415=EDGE_CURVE('',#18123,#18128,#1409,.T.);
#22416=EDGE_CURVE('',#18130,#18131,#14289,.T.);
#22417=EDGE_CURVE('',#18130,#18126,#1410,.T.);
#22418=EDGE_CURVE('',#18125,#18131,#9867,.T.);
#22419=EDGE_CURVE('',#18132,#18133,#14290,.T.);
#22420=EDGE_CURVE('',#18133,#18130,#14291,.T.);
#22421=EDGE_CURVE('',#18131,#18132,#14292,.T.);
#22422=EDGE_CURVE('',#18134,#18135,#14293,.T.);
#22423=EDGE_CURVE('',#18135,#18070,#14294,.T.);
#22424=EDGE_CURVE('',#18070,#18136,#9868,.T.);
#22425=EDGE_CURVE('',#18137,#18136,#14295,.T.);
#22426=EDGE_CURVE('',#18137,#18138,#14296,.T.);
#22427=EDGE_CURVE('',#18138,#18134,#9869,.T.);
#22428=EDGE_CURVE('',#18136,#18133,#9870,.T.);
#22429=EDGE_CURVE('',#18132,#18137,#1411,.T.);
#22430=EDGE_CURVE('',#18139,#18140,#14297,.T.);
#22431=EDGE_CURVE('',#18139,#18135,#1412,.T.);
#22432=EDGE_CURVE('',#18134,#18140,#9871,.T.);
#22433=EDGE_CURVE('',#18141,#18142,#14298,.T.);
#22434=EDGE_CURVE('',#18142,#18077,#14299,.T.);
#22435=EDGE_CURVE('',#18077,#18143,#9872,.T.);
#22436=EDGE_CURVE('',#18144,#18143,#14300,.T.);
#22437=EDGE_CURVE('',#18144,#18145,#14301,.T.);
#22438=EDGE_CURVE('',#18145,#18141,#9873,.F.);
#22439=EDGE_CURVE('',#17606,#18142,#14302,.T.);
#22440=EDGE_CURVE('',#18141,#17607,#9874,.F.);
#22441=EDGE_CURVE('',#18146,#18147,#14303,.T.);
#22442=EDGE_CURVE('',#18147,#18139,#14304,.T.);
#22443=EDGE_CURVE('',#18140,#18146,#14305,.T.);
#22444=EDGE_CURVE('',#18143,#18147,#9875,.T.);
#22445=EDGE_CURVE('',#18146,#18144,#1413,.T.);
#22446=EDGE_CURVE('',#17603,#18088,#914,.T.);
#22447=EDGE_CURVE('',#18088,#18148,#9876,.T.);
#22448=EDGE_CURVE('',#17604,#18148,#915,.T.);
#22449=EDGE_CURVE('',#18148,#17605,#916,.T.);
#22450=EDGE_CURVE('',#18149,#18150,#14306,.T.);
#22451=EDGE_CURVE('',#18150,#17397,#14307,.T.);
#22452=EDGE_CURVE('',#18151,#17396,#1414,.T.);
#22453=EDGE_CURVE('',#18151,#18152,#917,.T.);
#22454=EDGE_CURVE('',#18152,#18149,#9877,.T.);
#22455=EDGE_CURVE('',#18153,#18154,#14308,.T.);
#22456=EDGE_CURVE('',#18153,#18150,#1415,.T.);
#22457=EDGE_CURVE('',#18149,#18154,#9878,.T.);
#22458=EDGE_CURVE('',#18155,#18156,#14309,.T.);
#22459=EDGE_CURVE('',#18156,#18153,#14310,.T.);
#22460=EDGE_CURVE('',#18154,#18155,#14311,.T.);
#22461=EDGE_CURVE('',#18157,#18158,#14312,.T.);
#22462=EDGE_CURVE('',#18158,#18093,#14313,.T.);
#22463=EDGE_CURVE('',#18093,#18159,#9879,.T.);
#22464=EDGE_CURVE('',#18160,#18159,#14314,.T.);
#22465=EDGE_CURVE('',#18160,#18161,#14315,.T.);
#22466=EDGE_CURVE('',#18161,#18157,#9880,.T.);
#22467=EDGE_CURVE('',#18159,#18156,#9881,.T.);
#22468=EDGE_CURVE('',#18155,#18160,#1416,.T.);
#22469=EDGE_CURVE('',#17399,#18092,#918,.T.);
#22470=EDGE_CURVE('',#18162,#18163,#14316,.T.);
#22471=EDGE_CURVE('',#18162,#18158,#1417,.T.);
#22472=EDGE_CURVE('',#18157,#18163,#9882,.T.);
#22473=EDGE_CURVE('',#18164,#18165,#14317,.T.);
#22474=EDGE_CURVE('',#18165,#18162,#14318,.T.);
#22475=EDGE_CURVE('',#18163,#18164,#14319,.T.);
#22476=EDGE_CURVE('',#18166,#18167,#14320,.T.);
#22477=EDGE_CURVE('',#18167,#18102,#14321,.T.);
#22478=EDGE_CURVE('',#18102,#18168,#9883,.T.);
#22479=EDGE_CURVE('',#18169,#18168,#14322,.T.);
#22480=EDGE_CURVE('',#18169,#18170,#14323,.T.);
#22481=EDGE_CURVE('',#18170,#18166,#9884,.T.);
#22482=EDGE_CURVE('',#18168,#18165,#9885,.T.);
#22483=EDGE_CURVE('',#18164,#18169,#1418,.T.);
#22484=EDGE_CURVE('',#18171,#18172,#14324,.T.);
#22485=EDGE_CURVE('',#18171,#18167,#1419,.T.);
#22486=EDGE_CURVE('',#18166,#18172,#9886,.T.);
#22487=EDGE_CURVE('',#18173,#18174,#14325,.T.);
#22488=EDGE_CURVE('',#18174,#18171,#14326,.T.);
#22489=EDGE_CURVE('',#18172,#18173,#14327,.T.);
#22490=EDGE_CURVE('',#18175,#18176,#1420,.T.);
#22491=EDGE_CURVE('',#18176,#18111,#1421,.T.);
#22492=EDGE_CURVE('',#18111,#18177,#9887,.T.);
#22493=EDGE_CURVE('',#18178,#18177,#14328,.T.);
#22494=EDGE_CURVE('',#18178,#18179,#14329,.T.);
#22495=EDGE_CURVE('',#18179,#18175,#9888,.T.);
#22496=EDGE_CURVE('',#18177,#18174,#9889,.T.);
#22497=EDGE_CURVE('',#18173,#18178,#1422,.T.);
#22498=EDGE_CURVE('',#18180,#18181,#1423,.T.);
#22499=EDGE_CURVE('',#18180,#18176,#1424,.T.);
#22500=EDGE_CURVE('',#18175,#18181,#9890,.T.);
#22501=EDGE_CURVE('',#18182,#18183,#14330,.T.);
#22502=EDGE_CURVE('',#18183,#18180,#1425,.T.);
#22503=EDGE_CURVE('',#18181,#18182,#14331,.T.);
#22504=EDGE_CURVE('',#18184,#18185,#14332,.T.);
#22505=EDGE_CURVE('',#18185,#18120,#14333,.T.);
#22506=EDGE_CURVE('',#18120,#18186,#9891,.T.);
#22507=EDGE_CURVE('',#18187,#18186,#14334,.T.);
#22508=EDGE_CURVE('',#18187,#18188,#14335,.T.);
#22509=EDGE_CURVE('',#18188,#18184,#9892,.T.);
#22510=EDGE_CURVE('',#18186,#18183,#9893,.T.);
#22511=EDGE_CURVE('',#18182,#18187,#1426,.T.);
#22512=EDGE_CURVE('',#18189,#18190,#14336,.T.);
#22513=EDGE_CURVE('',#18189,#18185,#1427,.T.);
#22514=EDGE_CURVE('',#18184,#18190,#9894,.T.);
#22515=EDGE_CURVE('',#18191,#18192,#14337,.T.);
#22516=EDGE_CURVE('',#18192,#18189,#14338,.T.);
#22517=EDGE_CURVE('',#18190,#18191,#14339,.T.);
#22518=EDGE_CURVE('',#18193,#18194,#14340,.T.);
#22519=EDGE_CURVE('',#18194,#18129,#14341,.T.);
#22520=EDGE_CURVE('',#18129,#18195,#9895,.T.);
#22521=EDGE_CURVE('',#18196,#18195,#14342,.T.);
#22522=EDGE_CURVE('',#18196,#18197,#14343,.T.);
#22523=EDGE_CURVE('',#18197,#18193,#9896,.T.);
#22524=EDGE_CURVE('',#18195,#18192,#9897,.T.);
#22525=EDGE_CURVE('',#18191,#18196,#1428,.T.);
#22526=EDGE_CURVE('',#18198,#18199,#14344,.T.);
#22527=EDGE_CURVE('',#18198,#18194,#1429,.T.);
#22528=EDGE_CURVE('',#18193,#18199,#9898,.T.);
#22529=EDGE_CURVE('',#18200,#18201,#14345,.T.);
#22530=EDGE_CURVE('',#18201,#18198,#14346,.T.);
#22531=EDGE_CURVE('',#18199,#18200,#14347,.T.);
#22532=EDGE_CURVE('',#18202,#18203,#14348,.T.);
#22533=EDGE_CURVE('',#18203,#18138,#14349,.T.);
#22534=EDGE_CURVE('',#18138,#18204,#9899,.T.);
#22535=EDGE_CURVE('',#18205,#18204,#14350,.T.);
#22536=EDGE_CURVE('',#18205,#18206,#14351,.T.);
#22537=EDGE_CURVE('',#18206,#18202,#9900,.F.);
#22538=EDGE_CURVE('',#18204,#18201,#9901,.T.);
#22539=EDGE_CURVE('',#18200,#18205,#1430,.T.);
#22540=EDGE_CURVE('',#17612,#18203,#14352,.T.);
#22541=EDGE_CURVE('',#18202,#17613,#9902,.F.);
#22542=EDGE_CURVE('',#17609,#18145,#919,.T.);
#22543=EDGE_CURVE('',#18145,#18207,#9903,.T.);
#22544=EDGE_CURVE('',#17610,#18207,#920,.T.);
#22545=EDGE_CURVE('',#18207,#17611,#921,.T.);
#22546=EDGE_CURVE('',#18208,#18209,#14353,.T.);
#22547=EDGE_CURVE('',#18209,#17393,#14354,.T.);
#22548=EDGE_CURVE('',#18210,#17392,#1431,.T.);
#22549=EDGE_CURVE('',#18210,#18211,#922,.T.);
#22550=EDGE_CURVE('',#18211,#18208,#9904,.T.);
#22551=EDGE_CURVE('',#18212,#18213,#14355,.T.);
#22552=EDGE_CURVE('',#18212,#18209,#1432,.T.);
#22553=EDGE_CURVE('',#18208,#18213,#9905,.T.);
#22554=EDGE_CURVE('',#18214,#18215,#14356,.T.);
#22555=EDGE_CURVE('',#18215,#18212,#14357,.T.);
#22556=EDGE_CURVE('',#18213,#18214,#14358,.T.);
#22557=EDGE_CURVE('',#18216,#18217,#14359,.T.);
#22558=EDGE_CURVE('',#18217,#18152,#14360,.T.);
#22559=EDGE_CURVE('',#18152,#18218,#9906,.T.);
#22560=EDGE_CURVE('',#18219,#18218,#14361,.T.);
#22561=EDGE_CURVE('',#18219,#18220,#14362,.T.);
#22562=EDGE_CURVE('',#18220,#18216,#9907,.T.);
#22563=EDGE_CURVE('',#18218,#18215,#9908,.T.);
#22564=EDGE_CURVE('',#18214,#18219,#1433,.T.);
#22565=EDGE_CURVE('',#17395,#18151,#923,.T.);
#22566=EDGE_CURVE('',#18221,#18222,#14363,.T.);
#22567=EDGE_CURVE('',#18221,#18217,#1434,.T.);
#22568=EDGE_CURVE('',#18216,#18222,#9909,.T.);
#22569=EDGE_CURVE('',#18223,#18224,#14364,.T.);
#22570=EDGE_CURVE('',#18224,#18221,#14365,.T.);
#22571=EDGE_CURVE('',#18222,#18223,#14366,.T.);
#22572=EDGE_CURVE('',#18225,#18226,#14367,.T.);
#22573=EDGE_CURVE('',#18226,#18161,#14368,.T.);
#22574=EDGE_CURVE('',#18161,#18227,#9910,.T.);
#22575=EDGE_CURVE('',#18228,#18227,#14369,.T.);
#22576=EDGE_CURVE('',#18228,#18229,#14370,.T.);
#22577=EDGE_CURVE('',#18229,#18225,#9911,.T.);
#22578=EDGE_CURVE('',#18227,#18224,#9912,.T.);
#22579=EDGE_CURVE('',#18223,#18228,#1435,.T.);
#22580=EDGE_CURVE('',#18230,#18231,#14371,.T.);
#22581=EDGE_CURVE('',#18230,#18226,#1436,.T.);
#22582=EDGE_CURVE('',#18225,#18231,#9913,.T.);
#22583=EDGE_CURVE('',#18232,#18233,#14372,.T.);
#22584=EDGE_CURVE('',#18233,#18230,#14373,.T.);
#22585=EDGE_CURVE('',#18231,#18232,#14374,.T.);
#22586=EDGE_CURVE('',#18234,#18235,#1437,.T.);
#22587=EDGE_CURVE('',#18235,#18170,#1438,.T.);
#22588=EDGE_CURVE('',#18170,#18236,#9914,.T.);
#22589=EDGE_CURVE('',#18237,#18236,#14375,.T.);
#22590=EDGE_CURVE('',#18237,#18238,#14376,.T.);
#22591=EDGE_CURVE('',#18238,#18234,#9915,.T.);
#22592=EDGE_CURVE('',#18236,#18233,#9916,.T.);
#22593=EDGE_CURVE('',#18232,#18237,#1439,.T.);
#22594=EDGE_CURVE('',#18239,#18240,#1440,.T.);
#22595=EDGE_CURVE('',#18239,#18235,#1441,.T.);
#22596=EDGE_CURVE('',#18234,#18240,#9917,.T.);
#22597=EDGE_CURVE('',#18241,#18242,#14377,.T.);
#22598=EDGE_CURVE('',#18242,#18239,#1442,.T.);
#22599=EDGE_CURVE('',#18240,#18241,#14378,.T.);
#22600=EDGE_CURVE('',#18243,#18244,#14379,.T.);
#22601=EDGE_CURVE('',#18244,#18179,#14380,.T.);
#22602=EDGE_CURVE('',#18179,#18245,#9918,.T.);
#22603=EDGE_CURVE('',#18246,#18245,#14381,.T.);
#22604=EDGE_CURVE('',#18246,#18247,#14382,.T.);
#22605=EDGE_CURVE('',#18247,#18243,#9919,.T.);
#22606=EDGE_CURVE('',#18245,#18242,#9920,.T.);
#22607=EDGE_CURVE('',#18241,#18246,#1443,.T.);
#22608=EDGE_CURVE('',#18248,#18249,#14383,.T.);
#22609=EDGE_CURVE('',#18248,#18244,#1444,.T.);
#22610=EDGE_CURVE('',#18243,#18249,#9921,.T.);
#22611=EDGE_CURVE('',#18250,#18251,#14384,.T.);
#22612=EDGE_CURVE('',#18251,#18248,#14385,.T.);
#22613=EDGE_CURVE('',#18249,#18250,#14386,.T.);
#22614=EDGE_CURVE('',#18252,#18253,#14387,.T.);
#22615=EDGE_CURVE('',#18253,#18188,#14388,.T.);
#22616=EDGE_CURVE('',#18188,#18254,#9922,.T.);
#22617=EDGE_CURVE('',#18255,#18254,#14389,.T.);
#22618=EDGE_CURVE('',#18255,#18256,#14390,.T.);
#22619=EDGE_CURVE('',#18256,#18252,#9923,.T.);
#22620=EDGE_CURVE('',#18254,#18251,#9924,.T.);
#22621=EDGE_CURVE('',#18250,#18255,#1445,.T.);
#22622=EDGE_CURVE('',#18257,#18258,#14391,.T.);
#22623=EDGE_CURVE('',#18257,#18253,#1446,.T.);
#22624=EDGE_CURVE('',#18252,#18258,#9925,.T.);
#22625=EDGE_CURVE('',#18259,#18260,#14392,.T.);
#22626=EDGE_CURVE('',#18260,#18257,#14393,.T.);
#22627=EDGE_CURVE('',#18258,#18259,#14394,.T.);
#22628=EDGE_CURVE('',#18261,#18262,#14395,.T.);
#22629=EDGE_CURVE('',#18262,#18197,#14396,.T.);
#22630=EDGE_CURVE('',#18197,#18263,#9926,.T.);
#22631=EDGE_CURVE('',#18264,#18263,#14397,.T.);
#22632=EDGE_CURVE('',#18264,#18265,#14398,.T.);
#22633=EDGE_CURVE('',#18265,#18261,#9927,.F.);
#22634=EDGE_CURVE('',#18263,#18260,#9928,.T.);
#22635=EDGE_CURVE('',#18259,#18264,#1447,.T.);
#22636=EDGE_CURVE('',#17618,#18262,#14399,.T.);
#22637=EDGE_CURVE('',#18261,#17619,#9929,.F.);
#22638=EDGE_CURVE('',#17615,#18206,#924,.T.);
#22639=EDGE_CURVE('',#18206,#18266,#9930,.T.);
#22640=EDGE_CURVE('',#17616,#18266,#925,.T.);
#22641=EDGE_CURVE('',#18266,#17617,#926,.T.);
#22642=EDGE_CURVE('',#18267,#18268,#14400,.T.);
#22643=EDGE_CURVE('',#18268,#17389,#14401,.T.);
#22644=EDGE_CURVE('',#18269,#17388,#1448,.T.);
#22645=EDGE_CURVE('',#18269,#18270,#927,.T.);
#22646=EDGE_CURVE('',#18270,#18267,#9931,.T.);
#22647=EDGE_CURVE('',#18271,#18272,#14402,.T.);
#22648=EDGE_CURVE('',#18271,#18268,#1449,.T.);
#22649=EDGE_CURVE('',#18267,#18272,#9932,.T.);
#22650=EDGE_CURVE('',#18273,#18274,#14403,.T.);
#22651=EDGE_CURVE('',#18274,#18271,#14404,.T.);
#22652=EDGE_CURVE('',#18272,#18273,#14405,.T.);
#22653=EDGE_CURVE('',#18275,#18276,#14406,.T.);
#22654=EDGE_CURVE('',#18276,#18211,#14407,.T.);
#22655=EDGE_CURVE('',#18211,#18277,#9933,.T.);
#22656=EDGE_CURVE('',#18278,#18277,#14408,.T.);
#22657=EDGE_CURVE('',#18278,#18279,#14409,.T.);
#22658=EDGE_CURVE('',#18279,#18275,#9934,.T.);
#22659=EDGE_CURVE('',#18277,#18274,#9935,.T.);
#22660=EDGE_CURVE('',#18273,#18278,#1450,.T.);
#22661=EDGE_CURVE('',#17391,#18210,#928,.T.);
#22662=EDGE_CURVE('',#18280,#18281,#14410,.T.);
#22663=EDGE_CURVE('',#18280,#18276,#1451,.T.);
#22664=EDGE_CURVE('',#18275,#18281,#9936,.T.);
#22665=EDGE_CURVE('',#18282,#18283,#14411,.T.);
#22666=EDGE_CURVE('',#18283,#18280,#14412,.T.);
#22667=EDGE_CURVE('',#18281,#18282,#14413,.T.);
#22668=EDGE_CURVE('',#18284,#18285,#14414,.T.);
#22669=EDGE_CURVE('',#18285,#18220,#14415,.T.);
#22670=EDGE_CURVE('',#18220,#18286,#9937,.T.);
#22671=EDGE_CURVE('',#18287,#18286,#14416,.T.);
#22672=EDGE_CURVE('',#18287,#18288,#14417,.T.);
#22673=EDGE_CURVE('',#18288,#18284,#9938,.T.);
#22674=EDGE_CURVE('',#18286,#18283,#9939,.T.);
#22675=EDGE_CURVE('',#18282,#18287,#1452,.T.);
#22676=EDGE_CURVE('',#18289,#18290,#14418,.T.);
#22677=EDGE_CURVE('',#18289,#18285,#1453,.T.);
#22678=EDGE_CURVE('',#18284,#18290,#9940,.T.);
#22679=EDGE_CURVE('',#18291,#18292,#14419,.T.);
#22680=EDGE_CURVE('',#18292,#18289,#14420,.T.);
#22681=EDGE_CURVE('',#18290,#18291,#14421,.T.);
#22682=EDGE_CURVE('',#18293,#18294,#1454,.T.);
#22683=EDGE_CURVE('',#18294,#18229,#1455,.T.);
#22684=EDGE_CURVE('',#18229,#18295,#9941,.T.);
#22685=EDGE_CURVE('',#18296,#18295,#14422,.T.);
#22686=EDGE_CURVE('',#18296,#18297,#14423,.T.);
#22687=EDGE_CURVE('',#18297,#18293,#9942,.T.);
#22688=EDGE_CURVE('',#18295,#18292,#9943,.T.);
#22689=EDGE_CURVE('',#18291,#18296,#1456,.T.);
#22690=EDGE_CURVE('',#18298,#18299,#1457,.T.);
#22691=EDGE_CURVE('',#18298,#18294,#1458,.T.);
#22692=EDGE_CURVE('',#18293,#18299,#9944,.T.);
#22693=EDGE_CURVE('',#18300,#18301,#14424,.T.);
#22694=EDGE_CURVE('',#18301,#18298,#1459,.T.);
#22695=EDGE_CURVE('',#18299,#18300,#14425,.T.);
#22696=EDGE_CURVE('',#18302,#18303,#14426,.T.);
#22697=EDGE_CURVE('',#18303,#18238,#14427,.T.);
#22698=EDGE_CURVE('',#18238,#18304,#9945,.T.);
#22699=EDGE_CURVE('',#18305,#18304,#14428,.T.);
#22700=EDGE_CURVE('',#18305,#18306,#14429,.T.);
#22701=EDGE_CURVE('',#18306,#18302,#9946,.T.);
#22702=EDGE_CURVE('',#18304,#18301,#9947,.T.);
#22703=EDGE_CURVE('',#18300,#18305,#1460,.T.);
#22704=EDGE_CURVE('',#18307,#18308,#14430,.T.);
#22705=EDGE_CURVE('',#18307,#18303,#1461,.T.);
#22706=EDGE_CURVE('',#18302,#18308,#9948,.T.);
#22707=EDGE_CURVE('',#18309,#18310,#14431,.T.);
#22708=EDGE_CURVE('',#18310,#18307,#14432,.T.);
#22709=EDGE_CURVE('',#18308,#18309,#14433,.T.);
#22710=EDGE_CURVE('',#18311,#18312,#14434,.T.);
#22711=EDGE_CURVE('',#18312,#18247,#14435,.T.);
#22712=EDGE_CURVE('',#18247,#18313,#9949,.T.);
#22713=EDGE_CURVE('',#18314,#18313,#14436,.T.);
#22714=EDGE_CURVE('',#18314,#18315,#14437,.T.);
#22715=EDGE_CURVE('',#18315,#18311,#9950,.T.);
#22716=EDGE_CURVE('',#18313,#18310,#9951,.T.);
#22717=EDGE_CURVE('',#18309,#18314,#1462,.T.);
#22718=EDGE_CURVE('',#18316,#18317,#14438,.T.);
#22719=EDGE_CURVE('',#18316,#18312,#1463,.T.);
#22720=EDGE_CURVE('',#18311,#18317,#9952,.T.);
#22721=EDGE_CURVE('',#18318,#18319,#14439,.T.);
#22722=EDGE_CURVE('',#18319,#18316,#14440,.T.);
#22723=EDGE_CURVE('',#18317,#18318,#14441,.T.);
#22724=EDGE_CURVE('',#18320,#18321,#14442,.T.);
#22725=EDGE_CURVE('',#18321,#18256,#14443,.T.);
#22726=EDGE_CURVE('',#18256,#18322,#9953,.T.);
#22727=EDGE_CURVE('',#18323,#18322,#14444,.T.);
#22728=EDGE_CURVE('',#18323,#18324,#14445,.T.);
#22729=EDGE_CURVE('',#18324,#18320,#9954,.F.);
#22730=EDGE_CURVE('',#18322,#18319,#9955,.T.);
#22731=EDGE_CURVE('',#18318,#18323,#1464,.T.);
#22732=EDGE_CURVE('',#17624,#18321,#14446,.T.);
#22733=EDGE_CURVE('',#18320,#17625,#9956,.F.);
#22734=EDGE_CURVE('',#17621,#18265,#929,.T.);
#22735=EDGE_CURVE('',#18265,#18325,#9957,.T.);
#22736=EDGE_CURVE('',#17622,#18325,#930,.T.);
#22737=EDGE_CURVE('',#18325,#17623,#931,.T.);
#22738=EDGE_CURVE('',#18326,#18327,#14447,.T.);
#22739=EDGE_CURVE('',#18327,#17385,#14448,.T.);
#22740=EDGE_CURVE('',#18328,#17384,#1465,.T.);
#22741=EDGE_CURVE('',#18328,#18329,#932,.T.);
#22742=EDGE_CURVE('',#18329,#18326,#9958,.T.);
#22743=EDGE_CURVE('',#18330,#18331,#14449,.T.);
#22744=EDGE_CURVE('',#18330,#18327,#1466,.T.);
#22745=EDGE_CURVE('',#18326,#18331,#9959,.T.);
#22746=EDGE_CURVE('',#18332,#18333,#14450,.T.);
#22747=EDGE_CURVE('',#18333,#18330,#14451,.T.);
#22748=EDGE_CURVE('',#18331,#18332,#14452,.T.);
#22749=EDGE_CURVE('',#18334,#18335,#14453,.T.);
#22750=EDGE_CURVE('',#18335,#18270,#14454,.T.);
#22751=EDGE_CURVE('',#18270,#18336,#9960,.T.);
#22752=EDGE_CURVE('',#18337,#18336,#14455,.T.);
#22753=EDGE_CURVE('',#18337,#18338,#14456,.T.);
#22754=EDGE_CURVE('',#18338,#18334,#9961,.T.);
#22755=EDGE_CURVE('',#18336,#18333,#9962,.T.);
#22756=EDGE_CURVE('',#18332,#18337,#1467,.T.);
#22757=EDGE_CURVE('',#17387,#18269,#933,.T.);
#22758=EDGE_CURVE('',#18339,#18340,#14457,.T.);
#22759=EDGE_CURVE('',#18339,#18335,#1468,.T.);
#22760=EDGE_CURVE('',#18334,#18340,#9963,.T.);
#22761=EDGE_CURVE('',#18341,#18342,#14458,.T.);
#22762=EDGE_CURVE('',#18342,#18339,#14459,.T.);
#22763=EDGE_CURVE('',#18340,#18341,#14460,.T.);
#22764=EDGE_CURVE('',#18343,#18344,#14461,.T.);
#22765=EDGE_CURVE('',#18344,#18279,#14462,.T.);
#22766=EDGE_CURVE('',#18279,#18345,#9964,.T.);
#22767=EDGE_CURVE('',#18346,#18345,#14463,.T.);
#22768=EDGE_CURVE('',#18346,#18347,#14464,.T.);
#22769=EDGE_CURVE('',#18347,#18343,#9965,.T.);
#22770=EDGE_CURVE('',#18345,#18342,#9966,.T.);
#22771=EDGE_CURVE('',#18341,#18346,#1469,.T.);
#22772=EDGE_CURVE('',#18348,#18349,#14465,.T.);
#22773=EDGE_CURVE('',#18348,#18344,#1470,.T.);
#22774=EDGE_CURVE('',#18343,#18349,#9967,.T.);
#22775=EDGE_CURVE('',#18350,#18351,#14466,.T.);
#22776=EDGE_CURVE('',#18351,#18348,#14467,.T.);
#22777=EDGE_CURVE('',#18349,#18350,#14468,.T.);
#22778=EDGE_CURVE('',#18352,#18353,#1471,.T.);
#22779=EDGE_CURVE('',#18353,#18288,#1472,.T.);
#22780=EDGE_CURVE('',#18288,#18354,#9968,.T.);
#22781=EDGE_CURVE('',#18355,#18354,#14469,.T.);
#22782=EDGE_CURVE('',#18355,#18356,#14470,.T.);
#22783=EDGE_CURVE('',#18356,#18352,#9969,.T.);
#22784=EDGE_CURVE('',#18354,#18351,#9970,.T.);
#22785=EDGE_CURVE('',#18350,#18355,#1473,.T.);
#22786=EDGE_CURVE('',#18357,#18358,#1474,.T.);
#22787=EDGE_CURVE('',#18357,#18353,#1475,.T.);
#22788=EDGE_CURVE('',#18352,#18358,#9971,.T.);
#22789=EDGE_CURVE('',#18359,#18360,#14471,.T.);
#22790=EDGE_CURVE('',#18360,#18357,#1476,.T.);
#22791=EDGE_CURVE('',#18358,#18359,#14472,.T.);
#22792=EDGE_CURVE('',#18361,#18362,#14473,.T.);
#22793=EDGE_CURVE('',#18362,#18297,#14474,.T.);
#22794=EDGE_CURVE('',#18297,#18363,#9972,.T.);
#22795=EDGE_CURVE('',#18364,#18363,#14475,.T.);
#22796=EDGE_CURVE('',#18364,#18365,#14476,.T.);
#22797=EDGE_CURVE('',#18365,#18361,#9973,.T.);
#22798=EDGE_CURVE('',#18363,#18360,#9974,.T.);
#22799=EDGE_CURVE('',#18359,#18364,#1477,.T.);
#22800=EDGE_CURVE('',#18366,#18367,#14477,.T.);
#22801=EDGE_CURVE('',#18366,#18362,#1478,.T.);
#22802=EDGE_CURVE('',#18361,#18367,#9975,.T.);
#22803=EDGE_CURVE('',#18368,#18369,#14478,.T.);
#22804=EDGE_CURVE('',#18369,#18366,#14479,.T.);
#22805=EDGE_CURVE('',#18367,#18368,#14480,.T.);
#22806=EDGE_CURVE('',#18370,#18371,#14481,.T.);
#22807=EDGE_CURVE('',#18371,#18306,#14482,.T.);
#22808=EDGE_CURVE('',#18306,#18372,#9976,.T.);
#22809=EDGE_CURVE('',#18373,#18372,#14483,.T.);
#22810=EDGE_CURVE('',#18373,#18374,#14484,.T.);
#22811=EDGE_CURVE('',#18374,#18370,#9977,.T.);
#22812=EDGE_CURVE('',#18372,#18369,#9978,.T.);
#22813=EDGE_CURVE('',#18368,#18373,#1479,.T.);
#22814=EDGE_CURVE('',#18375,#18376,#14485,.T.);
#22815=EDGE_CURVE('',#18375,#18371,#1480,.T.);
#22816=EDGE_CURVE('',#18370,#18376,#9979,.T.);
#22817=EDGE_CURVE('',#18377,#18378,#14486,.T.);
#22818=EDGE_CURVE('',#18378,#18375,#14487,.T.);
#22819=EDGE_CURVE('',#18376,#18377,#14488,.T.);
#22820=EDGE_CURVE('',#18379,#18380,#14489,.T.);
#22821=EDGE_CURVE('',#18380,#18315,#14490,.T.);
#22822=EDGE_CURVE('',#18315,#18381,#9980,.T.);
#22823=EDGE_CURVE('',#18382,#18381,#14491,.T.);
#22824=EDGE_CURVE('',#18382,#18383,#14492,.T.);
#22825=EDGE_CURVE('',#18383,#18379,#9981,.F.);
#22826=EDGE_CURVE('',#18381,#18378,#9982,.T.);
#22827=EDGE_CURVE('',#18377,#18382,#1481,.T.);
#22828=EDGE_CURVE('',#17630,#18380,#14493,.T.);
#22829=EDGE_CURVE('',#18379,#17631,#9983,.F.);
#22830=EDGE_CURVE('',#17627,#18324,#934,.T.);
#22831=EDGE_CURVE('',#18324,#18384,#9984,.T.);
#22832=EDGE_CURVE('',#17628,#18384,#935,.T.);
#22833=EDGE_CURVE('',#18384,#17629,#936,.T.);
#22834=EDGE_CURVE('',#18385,#18386,#14494,.T.);
#22835=EDGE_CURVE('',#18386,#17381,#14495,.T.);
#22836=EDGE_CURVE('',#18387,#17380,#1482,.T.);
#22837=EDGE_CURVE('',#18387,#18388,#937,.T.);
#22838=EDGE_CURVE('',#18388,#18385,#9985,.T.);
#22839=EDGE_CURVE('',#18389,#18390,#14496,.T.);
#22840=EDGE_CURVE('',#18389,#18386,#1483,.T.);
#22841=EDGE_CURVE('',#18385,#18390,#9986,.T.);
#22842=EDGE_CURVE('',#18391,#18392,#14497,.T.);
#22843=EDGE_CURVE('',#18392,#18389,#14498,.T.);
#22844=EDGE_CURVE('',#18390,#18391,#14499,.T.);
#22845=EDGE_CURVE('',#18393,#18394,#14500,.T.);
#22846=EDGE_CURVE('',#18394,#18329,#14501,.T.);
#22847=EDGE_CURVE('',#18329,#18395,#9987,.T.);
#22848=EDGE_CURVE('',#18396,#18395,#14502,.T.);
#22849=EDGE_CURVE('',#18396,#18397,#14503,.T.);
#22850=EDGE_CURVE('',#18397,#18393,#9988,.T.);
#22851=EDGE_CURVE('',#18395,#18392,#9989,.T.);
#22852=EDGE_CURVE('',#18391,#18396,#1484,.T.);
#22853=EDGE_CURVE('',#17383,#18328,#938,.T.);
#22854=EDGE_CURVE('',#18398,#18399,#14504,.T.);
#22855=EDGE_CURVE('',#18398,#18394,#1485,.T.);
#22856=EDGE_CURVE('',#18393,#18399,#9990,.T.);
#22857=EDGE_CURVE('',#18400,#18401,#14505,.T.);
#22858=EDGE_CURVE('',#18401,#18398,#14506,.T.);
#22859=EDGE_CURVE('',#18399,#18400,#14507,.T.);
#22860=EDGE_CURVE('',#18402,#18403,#14508,.T.);
#22861=EDGE_CURVE('',#18403,#18338,#14509,.T.);
#22862=EDGE_CURVE('',#18338,#18404,#9991,.T.);
#22863=EDGE_CURVE('',#18405,#18404,#14510,.T.);
#22864=EDGE_CURVE('',#18405,#18406,#14511,.T.);
#22865=EDGE_CURVE('',#18406,#18402,#9992,.T.);
#22866=EDGE_CURVE('',#18404,#18401,#9993,.T.);
#22867=EDGE_CURVE('',#18400,#18405,#1486,.T.);
#22868=EDGE_CURVE('',#18407,#18408,#14512,.T.);
#22869=EDGE_CURVE('',#18407,#18403,#1487,.T.);
#22870=EDGE_CURVE('',#18402,#18408,#9994,.T.);
#22871=EDGE_CURVE('',#18409,#18410,#14513,.T.);
#22872=EDGE_CURVE('',#18410,#18407,#14514,.T.);
#22873=EDGE_CURVE('',#18408,#18409,#14515,.T.);
#22874=EDGE_CURVE('',#18411,#18412,#1488,.T.);
#22875=EDGE_CURVE('',#18412,#18347,#1489,.T.);
#22876=EDGE_CURVE('',#18347,#18413,#9995,.T.);
#22877=EDGE_CURVE('',#18414,#18413,#14516,.T.);
#22878=EDGE_CURVE('',#18414,#18415,#14517,.T.);
#22879=EDGE_CURVE('',#18415,#18411,#9996,.T.);
#22880=EDGE_CURVE('',#18413,#18410,#9997,.T.);
#22881=EDGE_CURVE('',#18409,#18414,#1490,.T.);
#22882=EDGE_CURVE('',#18416,#18417,#1491,.T.);
#22883=EDGE_CURVE('',#18416,#18412,#1492,.T.);
#22884=EDGE_CURVE('',#18411,#18417,#9998,.T.);
#22885=EDGE_CURVE('',#18418,#18419,#14518,.T.);
#22886=EDGE_CURVE('',#18419,#18416,#1493,.T.);
#22887=EDGE_CURVE('',#18417,#18418,#14519,.T.);
#22888=EDGE_CURVE('',#18420,#18421,#14520,.T.);
#22889=EDGE_CURVE('',#18421,#18356,#14521,.T.);
#22890=EDGE_CURVE('',#18356,#18422,#9999,.T.);
#22891=EDGE_CURVE('',#18423,#18422,#14522,.T.);
#22892=EDGE_CURVE('',#18423,#18424,#14523,.T.);
#22893=EDGE_CURVE('',#18424,#18420,#10000,.T.);
#22894=EDGE_CURVE('',#18422,#18419,#10001,.T.);
#22895=EDGE_CURVE('',#18418,#18423,#1494,.T.);
#22896=EDGE_CURVE('',#18425,#18426,#14524,.T.);
#22897=EDGE_CURVE('',#18425,#18421,#1495,.T.);
#22898=EDGE_CURVE('',#18420,#18426,#10002,.T.);
#22899=EDGE_CURVE('',#18427,#18428,#14525,.T.);
#22900=EDGE_CURVE('',#18428,#18425,#14526,.T.);
#22901=EDGE_CURVE('',#18426,#18427,#14527,.T.);
#22902=EDGE_CURVE('',#18429,#18430,#14528,.T.);
#22903=EDGE_CURVE('',#18430,#18365,#14529,.T.);
#22904=EDGE_CURVE('',#18365,#18431,#10003,.T.);
#22905=EDGE_CURVE('',#18432,#18431,#14530,.T.);
#22906=EDGE_CURVE('',#18432,#18433,#14531,.T.);
#22907=EDGE_CURVE('',#18433,#18429,#10004,.T.);
#22908=EDGE_CURVE('',#18431,#18428,#10005,.T.);
#22909=EDGE_CURVE('',#18427,#18432,#1496,.T.);
#22910=EDGE_CURVE('',#18434,#18435,#14532,.T.);
#22911=EDGE_CURVE('',#18434,#18430,#1497,.T.);
#22912=EDGE_CURVE('',#18429,#18435,#10006,.T.);
#22913=EDGE_CURVE('',#18436,#18437,#14533,.T.);
#22914=EDGE_CURVE('',#18437,#18434,#14534,.T.);
#22915=EDGE_CURVE('',#18435,#18436,#14535,.T.);
#22916=EDGE_CURVE('',#18438,#18439,#14536,.T.);
#22917=EDGE_CURVE('',#18439,#18374,#14537,.T.);
#22918=EDGE_CURVE('',#18374,#18440,#10007,.T.);
#22919=EDGE_CURVE('',#18441,#18440,#14538,.T.);
#22920=EDGE_CURVE('',#18441,#18442,#14539,.T.);
#22921=EDGE_CURVE('',#18442,#18438,#10008,.F.);
#22922=EDGE_CURVE('',#18440,#18437,#10009,.T.);
#22923=EDGE_CURVE('',#18436,#18441,#1498,.T.);
#22924=EDGE_CURVE('',#17636,#18439,#14540,.T.);
#22925=EDGE_CURVE('',#18438,#17637,#10010,.F.);
#22926=EDGE_CURVE('',#17633,#18383,#939,.T.);
#22927=EDGE_CURVE('',#18383,#18443,#10011,.T.);
#22928=EDGE_CURVE('',#17634,#18443,#940,.T.);
#22929=EDGE_CURVE('',#18443,#17635,#941,.T.);
#22930=EDGE_CURVE('',#18444,#18445,#14541,.T.);
#22931=EDGE_CURVE('',#18445,#17377,#14542,.T.);
#22932=EDGE_CURVE('',#18446,#17376,#1499,.T.);
#22933=EDGE_CURVE('',#18446,#18447,#942,.T.);
#22934=EDGE_CURVE('',#18447,#18444,#10012,.T.);
#22935=EDGE_CURVE('',#18448,#18449,#14543,.T.);
#22936=EDGE_CURVE('',#18448,#18445,#1500,.T.);
#22937=EDGE_CURVE('',#18444,#18449,#10013,.T.);
#22938=EDGE_CURVE('',#18450,#18451,#14544,.T.);
#22939=EDGE_CURVE('',#18451,#18448,#14545,.T.);
#22940=EDGE_CURVE('',#18449,#18450,#14546,.T.);
#22941=EDGE_CURVE('',#18452,#18453,#14547,.T.);
#22942=EDGE_CURVE('',#18453,#18388,#14548,.T.);
#22943=EDGE_CURVE('',#18388,#18454,#10014,.T.);
#22944=EDGE_CURVE('',#18455,#18454,#14549,.T.);
#22945=EDGE_CURVE('',#18455,#18456,#14550,.T.);
#22946=EDGE_CURVE('',#18456,#18452,#10015,.T.);
#22947=EDGE_CURVE('',#18454,#18451,#10016,.T.);
#22948=EDGE_CURVE('',#18450,#18455,#1501,.T.);
#22949=EDGE_CURVE('',#17379,#18387,#943,.T.);
#22950=EDGE_CURVE('',#18457,#18458,#14551,.T.);
#22951=EDGE_CURVE('',#18457,#18453,#1502,.T.);
#22952=EDGE_CURVE('',#18452,#18458,#10017,.T.);
#22953=EDGE_CURVE('',#18459,#18460,#14552,.T.);
#22954=EDGE_CURVE('',#18460,#18457,#14553,.T.);
#22955=EDGE_CURVE('',#18458,#18459,#14554,.T.);
#22956=EDGE_CURVE('',#18461,#18462,#14555,.T.);
#22957=EDGE_CURVE('',#18462,#18397,#14556,.T.);
#22958=EDGE_CURVE('',#18397,#18463,#10018,.T.);
#22959=EDGE_CURVE('',#18464,#18463,#14557,.T.);
#22960=EDGE_CURVE('',#18464,#18465,#14558,.T.);
#22961=EDGE_CURVE('',#18465,#18461,#10019,.T.);
#22962=EDGE_CURVE('',#18463,#18460,#10020,.T.);
#22963=EDGE_CURVE('',#18459,#18464,#1503,.T.);
#22964=EDGE_CURVE('',#18466,#18467,#14559,.T.);
#22965=EDGE_CURVE('',#18466,#18462,#1504,.T.);
#22966=EDGE_CURVE('',#18461,#18467,#10021,.T.);
#22967=EDGE_CURVE('',#18468,#18469,#14560,.T.);
#22968=EDGE_CURVE('',#18469,#18466,#14561,.T.);
#22969=EDGE_CURVE('',#18467,#18468,#14562,.T.);
#22970=EDGE_CURVE('',#18470,#18471,#1505,.T.);
#22971=EDGE_CURVE('',#18471,#18406,#1506,.T.);
#22972=EDGE_CURVE('',#18406,#18472,#10022,.T.);
#22973=EDGE_CURVE('',#18473,#18472,#14563,.T.);
#22974=EDGE_CURVE('',#18473,#18474,#14564,.T.);
#22975=EDGE_CURVE('',#18474,#18470,#10023,.T.);
#22976=EDGE_CURVE('',#18472,#18469,#10024,.T.);
#22977=EDGE_CURVE('',#18468,#18473,#1507,.T.);
#22978=EDGE_CURVE('',#18475,#18476,#1508,.T.);
#22979=EDGE_CURVE('',#18475,#18471,#1509,.T.);
#22980=EDGE_CURVE('',#18470,#18476,#10025,.T.);
#22981=EDGE_CURVE('',#18477,#18478,#14565,.T.);
#22982=EDGE_CURVE('',#18478,#18475,#1510,.T.);
#22983=EDGE_CURVE('',#18476,#18477,#14566,.T.);
#22984=EDGE_CURVE('',#18479,#18480,#14567,.T.);
#22985=EDGE_CURVE('',#18480,#18415,#14568,.T.);
#22986=EDGE_CURVE('',#18415,#18481,#10026,.T.);
#22987=EDGE_CURVE('',#18482,#18481,#14569,.T.);
#22988=EDGE_CURVE('',#18482,#18483,#14570,.T.);
#22989=EDGE_CURVE('',#18483,#18479,#10027,.T.);
#22990=EDGE_CURVE('',#18481,#18478,#10028,.T.);
#22991=EDGE_CURVE('',#18477,#18482,#1511,.T.);
#22992=EDGE_CURVE('',#18484,#18485,#14571,.T.);
#22993=EDGE_CURVE('',#18484,#18480,#1512,.T.);
#22994=EDGE_CURVE('',#18479,#18485,#10029,.T.);
#22995=EDGE_CURVE('',#18486,#18487,#14572,.T.);
#22996=EDGE_CURVE('',#18487,#18484,#14573,.T.);
#22997=EDGE_CURVE('',#18485,#18486,#14574,.T.);
#22998=EDGE_CURVE('',#18488,#18489,#14575,.T.);
#22999=EDGE_CURVE('',#18489,#18424,#14576,.T.);
#23000=EDGE_CURVE('',#18424,#18490,#10030,.T.);
#23001=EDGE_CURVE('',#18491,#18490,#14577,.T.);
#23002=EDGE_CURVE('',#18491,#18492,#14578,.T.);
#23003=EDGE_CURVE('',#18492,#18488,#10031,.T.);
#23004=EDGE_CURVE('',#18490,#18487,#10032,.T.);
#23005=EDGE_CURVE('',#18486,#18491,#1513,.T.);
#23006=EDGE_CURVE('',#18493,#18494,#14579,.T.);
#23007=EDGE_CURVE('',#18493,#18489,#1514,.T.);
#23008=EDGE_CURVE('',#18488,#18494,#10033,.T.);
#23009=EDGE_CURVE('',#18495,#18496,#14580,.T.);
#23010=EDGE_CURVE('',#18496,#18493,#14581,.T.);
#23011=EDGE_CURVE('',#18494,#18495,#14582,.T.);
#23012=EDGE_CURVE('',#18497,#18498,#14583,.T.);
#23013=EDGE_CURVE('',#18498,#18433,#14584,.T.);
#23014=EDGE_CURVE('',#18433,#18499,#10034,.T.);
#23015=EDGE_CURVE('',#18500,#18499,#14585,.T.);
#23016=EDGE_CURVE('',#18500,#18501,#14586,.T.);
#23017=EDGE_CURVE('',#18501,#18497,#10035,.F.);
#23018=EDGE_CURVE('',#18499,#18496,#10036,.T.);
#23019=EDGE_CURVE('',#18495,#18500,#1515,.T.);
#23020=EDGE_CURVE('',#17642,#18498,#14587,.T.);
#23021=EDGE_CURVE('',#18497,#17643,#10037,.F.);
#23022=EDGE_CURVE('',#17639,#18442,#944,.T.);
#23023=EDGE_CURVE('',#18442,#18502,#10038,.T.);
#23024=EDGE_CURVE('',#17640,#18502,#945,.T.);
#23025=EDGE_CURVE('',#18502,#17641,#946,.T.);
#23026=EDGE_CURVE('',#18503,#18504,#14588,.T.);
#23027=EDGE_CURVE('',#18504,#17373,#14589,.T.);
#23028=EDGE_CURVE('',#18505,#17372,#1516,.T.);
#23029=EDGE_CURVE('',#18505,#18506,#947,.T.);
#23030=EDGE_CURVE('',#18506,#18503,#10039,.T.);
#23031=EDGE_CURVE('',#18507,#18508,#14590,.T.);
#23032=EDGE_CURVE('',#18507,#18504,#1517,.T.);
#23033=EDGE_CURVE('',#18503,#18508,#10040,.T.);
#23034=EDGE_CURVE('',#18509,#18510,#14591,.T.);
#23035=EDGE_CURVE('',#18510,#18507,#14592,.T.);
#23036=EDGE_CURVE('',#18508,#18509,#14593,.T.);
#23037=EDGE_CURVE('',#18511,#18512,#14594,.T.);
#23038=EDGE_CURVE('',#18512,#18447,#14595,.T.);
#23039=EDGE_CURVE('',#18447,#18513,#10041,.T.);
#23040=EDGE_CURVE('',#18514,#18513,#14596,.T.);
#23041=EDGE_CURVE('',#18514,#18515,#14597,.T.);
#23042=EDGE_CURVE('',#18515,#18511,#10042,.T.);
#23043=EDGE_CURVE('',#18513,#18510,#10043,.T.);
#23044=EDGE_CURVE('',#18509,#18514,#1518,.T.);
#23045=EDGE_CURVE('',#17375,#18446,#948,.T.);
#23046=EDGE_CURVE('',#18516,#18517,#14598,.T.);
#23047=EDGE_CURVE('',#18516,#18512,#1519,.T.);
#23048=EDGE_CURVE('',#18511,#18517,#10044,.T.);
#23049=EDGE_CURVE('',#18518,#18519,#14599,.T.);
#23050=EDGE_CURVE('',#18519,#18516,#14600,.T.);
#23051=EDGE_CURVE('',#18517,#18518,#14601,.T.);
#23052=EDGE_CURVE('',#18520,#18521,#14602,.T.);
#23053=EDGE_CURVE('',#18521,#18456,#14603,.T.);
#23054=EDGE_CURVE('',#18456,#18522,#10045,.T.);
#23055=EDGE_CURVE('',#18523,#18522,#14604,.T.);
#23056=EDGE_CURVE('',#18523,#18524,#14605,.T.);
#23057=EDGE_CURVE('',#18524,#18520,#10046,.T.);
#23058=EDGE_CURVE('',#18522,#18519,#10047,.T.);
#23059=EDGE_CURVE('',#18518,#18523,#1520,.T.);
#23060=EDGE_CURVE('',#18525,#18526,#14606,.T.);
#23061=EDGE_CURVE('',#18525,#18521,#1521,.T.);
#23062=EDGE_CURVE('',#18520,#18526,#10048,.T.);
#23063=EDGE_CURVE('',#18527,#18528,#14607,.T.);
#23064=EDGE_CURVE('',#18528,#18525,#14608,.T.);
#23065=EDGE_CURVE('',#18526,#18527,#14609,.T.);
#23066=EDGE_CURVE('',#18529,#18530,#1522,.T.);
#23067=EDGE_CURVE('',#18530,#18465,#1523,.T.);
#23068=EDGE_CURVE('',#18465,#18531,#10049,.T.);
#23069=EDGE_CURVE('',#18532,#18531,#14610,.T.);
#23070=EDGE_CURVE('',#18532,#18533,#14611,.T.);
#23071=EDGE_CURVE('',#18533,#18529,#10050,.T.);
#23072=EDGE_CURVE('',#18531,#18528,#10051,.T.);
#23073=EDGE_CURVE('',#18527,#18532,#1524,.T.);
#23074=EDGE_CURVE('',#18534,#18535,#1525,.T.);
#23075=EDGE_CURVE('',#18534,#18530,#1526,.T.);
#23076=EDGE_CURVE('',#18529,#18535,#10052,.T.);
#23077=EDGE_CURVE('',#18536,#18537,#14612,.T.);
#23078=EDGE_CURVE('',#18537,#18534,#1527,.T.);
#23079=EDGE_CURVE('',#18535,#18536,#14613,.T.);
#23080=EDGE_CURVE('',#18538,#18539,#14614,.T.);
#23081=EDGE_CURVE('',#18539,#18474,#14615,.T.);
#23082=EDGE_CURVE('',#18474,#18540,#10053,.T.);
#23083=EDGE_CURVE('',#18541,#18540,#14616,.T.);
#23084=EDGE_CURVE('',#18541,#18542,#14617,.T.);
#23085=EDGE_CURVE('',#18542,#18538,#10054,.T.);
#23086=EDGE_CURVE('',#18540,#18537,#10055,.T.);
#23087=EDGE_CURVE('',#18536,#18541,#1528,.T.);
#23088=EDGE_CURVE('',#18543,#18544,#14618,.T.);
#23089=EDGE_CURVE('',#18543,#18539,#1529,.T.);
#23090=EDGE_CURVE('',#18538,#18544,#10056,.T.);
#23091=EDGE_CURVE('',#18545,#18546,#14619,.T.);
#23092=EDGE_CURVE('',#18546,#18543,#14620,.T.);
#23093=EDGE_CURVE('',#18544,#18545,#14621,.T.);
#23094=EDGE_CURVE('',#18547,#18548,#14622,.T.);
#23095=EDGE_CURVE('',#18548,#18483,#14623,.T.);
#23096=EDGE_CURVE('',#18483,#18549,#10057,.T.);
#23097=EDGE_CURVE('',#18550,#18549,#14624,.T.);
#23098=EDGE_CURVE('',#18550,#18551,#14625,.T.);
#23099=EDGE_CURVE('',#18551,#18547,#10058,.T.);
#23100=EDGE_CURVE('',#18549,#18546,#10059,.T.);
#23101=EDGE_CURVE('',#18545,#18550,#1530,.T.);
#23102=EDGE_CURVE('',#18552,#18553,#14626,.T.);
#23103=EDGE_CURVE('',#18552,#18548,#1531,.T.);
#23104=EDGE_CURVE('',#18547,#18553,#10060,.T.);
#23105=EDGE_CURVE('',#18554,#18555,#14627,.T.);
#23106=EDGE_CURVE('',#18555,#18552,#14628,.T.);
#23107=EDGE_CURVE('',#18553,#18554,#14629,.T.);
#23108=EDGE_CURVE('',#18556,#18557,#14630,.T.);
#23109=EDGE_CURVE('',#18557,#18492,#14631,.T.);
#23110=EDGE_CURVE('',#18492,#18558,#10061,.T.);
#23111=EDGE_CURVE('',#18559,#18558,#14632,.T.);
#23112=EDGE_CURVE('',#18559,#18560,#14633,.T.);
#23113=EDGE_CURVE('',#18560,#18556,#10062,.F.);
#23114=EDGE_CURVE('',#18558,#18555,#10063,.T.);
#23115=EDGE_CURVE('',#18554,#18559,#1532,.T.);
#23116=EDGE_CURVE('',#17648,#18557,#14634,.T.);
#23117=EDGE_CURVE('',#18556,#17649,#10064,.F.);
#23118=EDGE_CURVE('',#17645,#18501,#949,.T.);
#23119=EDGE_CURVE('',#18501,#18561,#10065,.T.);
#23120=EDGE_CURVE('',#17646,#18561,#950,.T.);
#23121=EDGE_CURVE('',#18561,#17647,#951,.T.);
#23122=EDGE_CURVE('',#18562,#18563,#14635,.T.);
#23123=EDGE_CURVE('',#18563,#17369,#14636,.T.);
#23124=EDGE_CURVE('',#18564,#17368,#1533,.T.);
#23125=EDGE_CURVE('',#18564,#18565,#952,.T.);
#23126=EDGE_CURVE('',#18565,#18562,#10066,.T.);
#23127=EDGE_CURVE('',#18566,#18567,#14637,.T.);
#23128=EDGE_CURVE('',#18566,#18563,#1534,.T.);
#23129=EDGE_CURVE('',#18562,#18567,#10067,.T.);
#23130=EDGE_CURVE('',#18568,#18569,#14638,.T.);
#23131=EDGE_CURVE('',#18569,#18566,#14639,.T.);
#23132=EDGE_CURVE('',#18567,#18568,#14640,.T.);
#23133=EDGE_CURVE('',#18570,#18571,#14641,.T.);
#23134=EDGE_CURVE('',#18571,#18506,#14642,.T.);
#23135=EDGE_CURVE('',#18506,#18572,#10068,.T.);
#23136=EDGE_CURVE('',#18573,#18572,#14643,.T.);
#23137=EDGE_CURVE('',#18573,#18574,#14644,.T.);
#23138=EDGE_CURVE('',#18574,#18570,#10069,.T.);
#23139=EDGE_CURVE('',#18572,#18569,#10070,.T.);
#23140=EDGE_CURVE('',#18568,#18573,#1535,.T.);
#23141=EDGE_CURVE('',#17371,#18505,#953,.T.);
#23142=EDGE_CURVE('',#18575,#18576,#14645,.T.);
#23143=EDGE_CURVE('',#18575,#18571,#1536,.T.);
#23144=EDGE_CURVE('',#18570,#18576,#10071,.T.);
#23145=EDGE_CURVE('',#18577,#18578,#14646,.T.);
#23146=EDGE_CURVE('',#18578,#18575,#14647,.T.);
#23147=EDGE_CURVE('',#18576,#18577,#14648,.T.);
#23148=EDGE_CURVE('',#18579,#18580,#14649,.T.);
#23149=EDGE_CURVE('',#18580,#18515,#14650,.T.);
#23150=EDGE_CURVE('',#18515,#18581,#10072,.T.);
#23151=EDGE_CURVE('',#18582,#18581,#14651,.T.);
#23152=EDGE_CURVE('',#18582,#18583,#14652,.T.);
#23153=EDGE_CURVE('',#18583,#18579,#10073,.T.);
#23154=EDGE_CURVE('',#18581,#18578,#10074,.T.);
#23155=EDGE_CURVE('',#18577,#18582,#1537,.T.);
#23156=EDGE_CURVE('',#18584,#18585,#14653,.T.);
#23157=EDGE_CURVE('',#18584,#18580,#1538,.T.);
#23158=EDGE_CURVE('',#18579,#18585,#10075,.T.);
#23159=EDGE_CURVE('',#18586,#18587,#14654,.T.);
#23160=EDGE_CURVE('',#18587,#18584,#14655,.T.);
#23161=EDGE_CURVE('',#18585,#18586,#14656,.T.);
#23162=EDGE_CURVE('',#18588,#18589,#1539,.T.);
#23163=EDGE_CURVE('',#18589,#18524,#1540,.T.);
#23164=EDGE_CURVE('',#18524,#18590,#10076,.T.);
#23165=EDGE_CURVE('',#18591,#18590,#14657,.T.);
#23166=EDGE_CURVE('',#18591,#18592,#14658,.T.);
#23167=EDGE_CURVE('',#18592,#18588,#10077,.T.);
#23168=EDGE_CURVE('',#18590,#18587,#10078,.T.);
#23169=EDGE_CURVE('',#18586,#18591,#1541,.T.);
#23170=EDGE_CURVE('',#18593,#18594,#1542,.T.);
#23171=EDGE_CURVE('',#18593,#18589,#1543,.T.);
#23172=EDGE_CURVE('',#18588,#18594,#10079,.T.);
#23173=EDGE_CURVE('',#18595,#18596,#14659,.T.);
#23174=EDGE_CURVE('',#18596,#18593,#1544,.T.);
#23175=EDGE_CURVE('',#18594,#18595,#14660,.T.);
#23176=EDGE_CURVE('',#18597,#18598,#14661,.T.);
#23177=EDGE_CURVE('',#18598,#18533,#14662,.T.);
#23178=EDGE_CURVE('',#18533,#18599,#10080,.T.);
#23179=EDGE_CURVE('',#18600,#18599,#14663,.T.);
#23180=EDGE_CURVE('',#18600,#18601,#14664,.T.);
#23181=EDGE_CURVE('',#18601,#18597,#10081,.T.);
#23182=EDGE_CURVE('',#18599,#18596,#10082,.T.);
#23183=EDGE_CURVE('',#18595,#18600,#1545,.T.);
#23184=EDGE_CURVE('',#18602,#18603,#14665,.T.);
#23185=EDGE_CURVE('',#18602,#18598,#1546,.T.);
#23186=EDGE_CURVE('',#18597,#18603,#10083,.T.);
#23187=EDGE_CURVE('',#18604,#18605,#14666,.T.);
#23188=EDGE_CURVE('',#18605,#18602,#14667,.T.);
#23189=EDGE_CURVE('',#18603,#18604,#14668,.T.);
#23190=EDGE_CURVE('',#18606,#18607,#14669,.T.);
#23191=EDGE_CURVE('',#18607,#18542,#14670,.T.);
#23192=EDGE_CURVE('',#18542,#18608,#10084,.T.);
#23193=EDGE_CURVE('',#18609,#18608,#14671,.T.);
#23194=EDGE_CURVE('',#18609,#18610,#14672,.T.);
#23195=EDGE_CURVE('',#18610,#18606,#10085,.T.);
#23196=EDGE_CURVE('',#18608,#18605,#10086,.T.);
#23197=EDGE_CURVE('',#18604,#18609,#1547,.T.);
#23198=EDGE_CURVE('',#18611,#18612,#14673,.T.);
#23199=EDGE_CURVE('',#18611,#18607,#1548,.T.);
#23200=EDGE_CURVE('',#18606,#18612,#10087,.T.);
#23201=EDGE_CURVE('',#18613,#18614,#14674,.T.);
#23202=EDGE_CURVE('',#18614,#18611,#14675,.T.);
#23203=EDGE_CURVE('',#18612,#18613,#14676,.T.);
#23204=EDGE_CURVE('',#18615,#18616,#14677,.T.);
#23205=EDGE_CURVE('',#18616,#18551,#14678,.T.);
#23206=EDGE_CURVE('',#18551,#18617,#10088,.T.);
#23207=EDGE_CURVE('',#18618,#18617,#14679,.T.);
#23208=EDGE_CURVE('',#18618,#18619,#14680,.T.);
#23209=EDGE_CURVE('',#18619,#18615,#10089,.F.);
#23210=EDGE_CURVE('',#18617,#18614,#10090,.T.);
#23211=EDGE_CURVE('',#18613,#18618,#1549,.T.);
#23212=EDGE_CURVE('',#17654,#18616,#14681,.T.);
#23213=EDGE_CURVE('',#18615,#17655,#10091,.F.);
#23214=EDGE_CURVE('',#17651,#18560,#954,.T.);
#23215=EDGE_CURVE('',#18560,#18620,#10092,.T.);
#23216=EDGE_CURVE('',#17652,#18620,#955,.T.);
#23217=EDGE_CURVE('',#18620,#17653,#956,.T.);
#23218=EDGE_CURVE('',#18621,#18622,#14682,.T.);
#23219=EDGE_CURVE('',#18622,#17365,#14683,.T.);
#23220=EDGE_CURVE('',#18623,#17364,#1550,.T.);
#23221=EDGE_CURVE('',#18623,#18624,#957,.T.);
#23222=EDGE_CURVE('',#18624,#18621,#10093,.T.);
#23223=EDGE_CURVE('',#18625,#18626,#14684,.T.);
#23224=EDGE_CURVE('',#18625,#18622,#1551,.T.);
#23225=EDGE_CURVE('',#18621,#18626,#10094,.T.);
#23226=EDGE_CURVE('',#18627,#18628,#14685,.T.);
#23227=EDGE_CURVE('',#18628,#18625,#14686,.T.);
#23228=EDGE_CURVE('',#18626,#18627,#14687,.T.);
#23229=EDGE_CURVE('',#18629,#18630,#14688,.T.);
#23230=EDGE_CURVE('',#18630,#18565,#14689,.T.);
#23231=EDGE_CURVE('',#18565,#18631,#10095,.T.);
#23232=EDGE_CURVE('',#18632,#18631,#14690,.T.);
#23233=EDGE_CURVE('',#18632,#18633,#14691,.T.);
#23234=EDGE_CURVE('',#18633,#18629,#10096,.T.);
#23235=EDGE_CURVE('',#18631,#18628,#10097,.T.);
#23236=EDGE_CURVE('',#18627,#18632,#1552,.T.);
#23237=EDGE_CURVE('',#17367,#18564,#958,.T.);
#23238=EDGE_CURVE('',#18634,#18635,#14692,.T.);
#23239=EDGE_CURVE('',#18634,#18630,#1553,.T.);
#23240=EDGE_CURVE('',#18629,#18635,#10098,.T.);
#23241=EDGE_CURVE('',#18636,#18637,#14693,.T.);
#23242=EDGE_CURVE('',#18637,#18634,#14694,.T.);
#23243=EDGE_CURVE('',#18635,#18636,#14695,.T.);
#23244=EDGE_CURVE('',#18638,#18639,#14696,.T.);
#23245=EDGE_CURVE('',#18639,#18574,#14697,.T.);
#23246=EDGE_CURVE('',#18574,#18640,#10099,.T.);
#23247=EDGE_CURVE('',#18641,#18640,#14698,.T.);
#23248=EDGE_CURVE('',#18641,#18642,#14699,.T.);
#23249=EDGE_CURVE('',#18642,#18638,#10100,.T.);
#23250=EDGE_CURVE('',#18640,#18637,#10101,.T.);
#23251=EDGE_CURVE('',#18636,#18641,#1554,.T.);
#23252=EDGE_CURVE('',#18643,#18644,#14700,.T.);
#23253=EDGE_CURVE('',#18643,#18639,#1555,.T.);
#23254=EDGE_CURVE('',#18638,#18644,#10102,.T.);
#23255=EDGE_CURVE('',#18645,#18646,#14701,.T.);
#23256=EDGE_CURVE('',#18646,#18643,#14702,.T.);
#23257=EDGE_CURVE('',#18644,#18645,#14703,.T.);
#23258=EDGE_CURVE('',#18647,#18648,#1556,.T.);
#23259=EDGE_CURVE('',#18648,#18583,#1557,.T.);
#23260=EDGE_CURVE('',#18583,#18649,#10103,.T.);
#23261=EDGE_CURVE('',#18650,#18649,#14704,.T.);
#23262=EDGE_CURVE('',#18650,#18651,#14705,.T.);
#23263=EDGE_CURVE('',#18651,#18647,#10104,.T.);
#23264=EDGE_CURVE('',#18649,#18646,#10105,.T.);
#23265=EDGE_CURVE('',#18645,#18650,#1558,.T.);
#23266=EDGE_CURVE('',#18652,#18653,#1559,.T.);
#23267=EDGE_CURVE('',#18652,#18648,#1560,.T.);
#23268=EDGE_CURVE('',#18647,#18653,#10106,.T.);
#23269=EDGE_CURVE('',#18654,#18655,#14706,.T.);
#23270=EDGE_CURVE('',#18655,#18652,#1561,.T.);
#23271=EDGE_CURVE('',#18653,#18654,#14707,.T.);
#23272=EDGE_CURVE('',#18656,#18657,#14708,.T.);
#23273=EDGE_CURVE('',#18657,#18592,#14709,.T.);
#23274=EDGE_CURVE('',#18592,#18658,#10107,.T.);
#23275=EDGE_CURVE('',#18659,#18658,#14710,.T.);
#23276=EDGE_CURVE('',#18659,#18660,#14711,.T.);
#23277=EDGE_CURVE('',#18660,#18656,#10108,.T.);
#23278=EDGE_CURVE('',#18658,#18655,#10109,.T.);
#23279=EDGE_CURVE('',#18654,#18659,#1562,.T.);
#23280=EDGE_CURVE('',#18661,#18662,#14712,.T.);
#23281=EDGE_CURVE('',#18661,#18657,#1563,.T.);
#23282=EDGE_CURVE('',#18656,#18662,#10110,.T.);
#23283=EDGE_CURVE('',#18663,#18664,#14713,.T.);
#23284=EDGE_CURVE('',#18664,#18661,#14714,.T.);
#23285=EDGE_CURVE('',#18662,#18663,#14715,.T.);
#23286=EDGE_CURVE('',#18665,#18666,#14716,.T.);
#23287=EDGE_CURVE('',#18666,#18601,#14717,.T.);
#23288=EDGE_CURVE('',#18601,#18667,#10111,.T.);
#23289=EDGE_CURVE('',#18668,#18667,#14718,.T.);
#23290=EDGE_CURVE('',#18668,#18669,#14719,.T.);
#23291=EDGE_CURVE('',#18669,#18665,#10112,.T.);
#23292=EDGE_CURVE('',#18667,#18664,#10113,.T.);
#23293=EDGE_CURVE('',#18663,#18668,#1564,.T.);
#23294=EDGE_CURVE('',#18670,#18671,#14720,.T.);
#23295=EDGE_CURVE('',#18670,#18666,#1565,.T.);
#23296=EDGE_CURVE('',#18665,#18671,#10114,.T.);
#23297=EDGE_CURVE('',#18672,#18673,#14721,.T.);
#23298=EDGE_CURVE('',#18673,#18670,#14722,.T.);
#23299=EDGE_CURVE('',#18671,#18672,#14723,.T.);
#23300=EDGE_CURVE('',#18674,#18675,#14724,.T.);
#23301=EDGE_CURVE('',#18675,#18610,#14725,.T.);
#23302=EDGE_CURVE('',#18610,#18676,#10115,.T.);
#23303=EDGE_CURVE('',#18677,#18676,#14726,.T.);
#23304=EDGE_CURVE('',#18677,#18678,#14727,.T.);
#23305=EDGE_CURVE('',#18678,#18674,#10116,.F.);
#23306=EDGE_CURVE('',#18676,#18673,#10117,.T.);
#23307=EDGE_CURVE('',#18672,#18677,#1566,.T.);
#23308=EDGE_CURVE('',#17660,#18675,#14728,.T.);
#23309=EDGE_CURVE('',#18674,#17661,#10118,.F.);
#23310=EDGE_CURVE('',#17657,#18619,#959,.T.);
#23311=EDGE_CURVE('',#18619,#18679,#10119,.T.);
#23312=EDGE_CURVE('',#17658,#18679,#960,.T.);
#23313=EDGE_CURVE('',#18679,#17659,#961,.T.);
#23314=EDGE_CURVE('',#18680,#18681,#14729,.T.);
#23315=EDGE_CURVE('',#18681,#17361,#14730,.T.);
#23316=EDGE_CURVE('',#18682,#17360,#1567,.T.);
#23317=EDGE_CURVE('',#18682,#18683,#962,.T.);
#23318=EDGE_CURVE('',#18683,#18680,#10120,.T.);
#23319=EDGE_CURVE('',#18684,#18685,#14731,.T.);
#23320=EDGE_CURVE('',#18684,#18681,#1568,.T.);
#23321=EDGE_CURVE('',#18680,#18685,#10121,.T.);
#23322=EDGE_CURVE('',#18686,#18687,#14732,.T.);
#23323=EDGE_CURVE('',#18687,#18684,#14733,.T.);
#23324=EDGE_CURVE('',#18685,#18686,#14734,.T.);
#23325=EDGE_CURVE('',#18688,#18689,#14735,.T.);
#23326=EDGE_CURVE('',#18689,#18624,#14736,.T.);
#23327=EDGE_CURVE('',#18624,#18690,#10122,.T.);
#23328=EDGE_CURVE('',#18691,#18690,#14737,.T.);
#23329=EDGE_CURVE('',#18691,#18692,#14738,.T.);
#23330=EDGE_CURVE('',#18692,#18688,#10123,.T.);
#23331=EDGE_CURVE('',#18690,#18687,#10124,.T.);
#23332=EDGE_CURVE('',#18686,#18691,#1569,.T.);
#23333=EDGE_CURVE('',#17363,#18623,#963,.T.);
#23334=EDGE_CURVE('',#18693,#18694,#14739,.T.);
#23335=EDGE_CURVE('',#18693,#18689,#1570,.T.);
#23336=EDGE_CURVE('',#18688,#18694,#10125,.T.);
#23337=EDGE_CURVE('',#18695,#18696,#14740,.T.);
#23338=EDGE_CURVE('',#18696,#18693,#14741,.T.);
#23339=EDGE_CURVE('',#18694,#18695,#14742,.T.);
#23340=EDGE_CURVE('',#18697,#18698,#14743,.T.);
#23341=EDGE_CURVE('',#18698,#18633,#14744,.T.);
#23342=EDGE_CURVE('',#18633,#18699,#10126,.T.);
#23343=EDGE_CURVE('',#18700,#18699,#14745,.T.);
#23344=EDGE_CURVE('',#18700,#18701,#14746,.T.);
#23345=EDGE_CURVE('',#18701,#18697,#10127,.T.);
#23346=EDGE_CURVE('',#18699,#18696,#10128,.T.);
#23347=EDGE_CURVE('',#18695,#18700,#1571,.T.);
#23348=EDGE_CURVE('',#18702,#18703,#14747,.T.);
#23349=EDGE_CURVE('',#18702,#18698,#1572,.T.);
#23350=EDGE_CURVE('',#18697,#18703,#10129,.T.);
#23351=EDGE_CURVE('',#18704,#18705,#14748,.T.);
#23352=EDGE_CURVE('',#18705,#18702,#14749,.T.);
#23353=EDGE_CURVE('',#18703,#18704,#14750,.T.);
#23354=EDGE_CURVE('',#18706,#18707,#1573,.T.);
#23355=EDGE_CURVE('',#18707,#18642,#1574,.T.);
#23356=EDGE_CURVE('',#18642,#18708,#10130,.T.);
#23357=EDGE_CURVE('',#18709,#18708,#14751,.T.);
#23358=EDGE_CURVE('',#18709,#18710,#14752,.T.);
#23359=EDGE_CURVE('',#18710,#18706,#10131,.T.);
#23360=EDGE_CURVE('',#18708,#18705,#10132,.T.);
#23361=EDGE_CURVE('',#18704,#18709,#1575,.T.);
#23362=EDGE_CURVE('',#18711,#18712,#1576,.T.);
#23363=EDGE_CURVE('',#18711,#18707,#1577,.T.);
#23364=EDGE_CURVE('',#18706,#18712,#10133,.T.);
#23365=EDGE_CURVE('',#18713,#18714,#14753,.T.);
#23366=EDGE_CURVE('',#18714,#18711,#1578,.T.);
#23367=EDGE_CURVE('',#18712,#18713,#14754,.T.);
#23368=EDGE_CURVE('',#18715,#18716,#14755,.T.);
#23369=EDGE_CURVE('',#18716,#18651,#14756,.T.);
#23370=EDGE_CURVE('',#18651,#18717,#10134,.T.);
#23371=EDGE_CURVE('',#18718,#18717,#14757,.T.);
#23372=EDGE_CURVE('',#18718,#18719,#14758,.T.);
#23373=EDGE_CURVE('',#18719,#18715,#10135,.T.);
#23374=EDGE_CURVE('',#18717,#18714,#10136,.T.);
#23375=EDGE_CURVE('',#18713,#18718,#1579,.T.);
#23376=EDGE_CURVE('',#18720,#18721,#14759,.T.);
#23377=EDGE_CURVE('',#18720,#18716,#1580,.T.);
#23378=EDGE_CURVE('',#18715,#18721,#10137,.T.);
#23379=EDGE_CURVE('',#18722,#18723,#14760,.T.);
#23380=EDGE_CURVE('',#18723,#18720,#14761,.T.);
#23381=EDGE_CURVE('',#18721,#18722,#14762,.T.);
#23382=EDGE_CURVE('',#18724,#18725,#14763,.T.);
#23383=EDGE_CURVE('',#18725,#18660,#14764,.T.);
#23384=EDGE_CURVE('',#18660,#18726,#10138,.T.);
#23385=EDGE_CURVE('',#18727,#18726,#14765,.T.);
#23386=EDGE_CURVE('',#18727,#18728,#14766,.T.);
#23387=EDGE_CURVE('',#18728,#18724,#10139,.T.);
#23388=EDGE_CURVE('',#18726,#18723,#10140,.T.);
#23389=EDGE_CURVE('',#18722,#18727,#1581,.T.);
#23390=EDGE_CURVE('',#18729,#18730,#14767,.T.);
#23391=EDGE_CURVE('',#18729,#18725,#1582,.T.);
#23392=EDGE_CURVE('',#18724,#18730,#10141,.T.);
#23393=EDGE_CURVE('',#18731,#18732,#14768,.T.);
#23394=EDGE_CURVE('',#18732,#18729,#14769,.T.);
#23395=EDGE_CURVE('',#18730,#18731,#14770,.T.);
#23396=EDGE_CURVE('',#18733,#18734,#14771,.T.);
#23397=EDGE_CURVE('',#18734,#18669,#14772,.T.);
#23398=EDGE_CURVE('',#18669,#18735,#10142,.T.);
#23399=EDGE_CURVE('',#18736,#18735,#14773,.T.);
#23400=EDGE_CURVE('',#18736,#18737,#14774,.T.);
#23401=EDGE_CURVE('',#18737,#18733,#10143,.F.);
#23402=EDGE_CURVE('',#18735,#18732,#10144,.T.);
#23403=EDGE_CURVE('',#18731,#18736,#1583,.T.);
#23404=EDGE_CURVE('',#17666,#18734,#14775,.T.);
#23405=EDGE_CURVE('',#18733,#17667,#10145,.F.);
#23406=EDGE_CURVE('',#17663,#18678,#964,.T.);
#23407=EDGE_CURVE('',#18678,#18738,#10146,.T.);
#23408=EDGE_CURVE('',#17664,#18738,#965,.T.);
#23409=EDGE_CURVE('',#18738,#17665,#966,.T.);
#23410=EDGE_CURVE('',#18739,#18740,#14776,.T.);
#23411=EDGE_CURVE('',#18740,#17357,#14777,.T.);
#23412=EDGE_CURVE('',#18741,#17356,#1584,.T.);
#23413=EDGE_CURVE('',#18741,#18742,#967,.T.);
#23414=EDGE_CURVE('',#18742,#18739,#10147,.T.);
#23415=EDGE_CURVE('',#18743,#18744,#14778,.T.);
#23416=EDGE_CURVE('',#18743,#18740,#1585,.T.);
#23417=EDGE_CURVE('',#18739,#18744,#10148,.T.);
#23418=EDGE_CURVE('',#18745,#18746,#14779,.T.);
#23419=EDGE_CURVE('',#18746,#18743,#14780,.T.);
#23420=EDGE_CURVE('',#18744,#18745,#14781,.T.);
#23421=EDGE_CURVE('',#18747,#18748,#14782,.T.);
#23422=EDGE_CURVE('',#18748,#18683,#14783,.T.);
#23423=EDGE_CURVE('',#18683,#18749,#10149,.T.);
#23424=EDGE_CURVE('',#18750,#18749,#14784,.T.);
#23425=EDGE_CURVE('',#18750,#18751,#14785,.T.);
#23426=EDGE_CURVE('',#18751,#18747,#10150,.T.);
#23427=EDGE_CURVE('',#18749,#18746,#10151,.T.);
#23428=EDGE_CURVE('',#18745,#18750,#1586,.T.);
#23429=EDGE_CURVE('',#17359,#18682,#968,.T.);
#23430=EDGE_CURVE('',#18752,#18753,#14786,.T.);
#23431=EDGE_CURVE('',#18752,#18748,#1587,.T.);
#23432=EDGE_CURVE('',#18747,#18753,#10152,.T.);
#23433=EDGE_CURVE('',#18754,#18755,#14787,.T.);
#23434=EDGE_CURVE('',#18755,#18752,#14788,.T.);
#23435=EDGE_CURVE('',#18753,#18754,#14789,.T.);
#23436=EDGE_CURVE('',#18756,#18757,#14790,.T.);
#23437=EDGE_CURVE('',#18757,#18692,#14791,.T.);
#23438=EDGE_CURVE('',#18692,#18758,#10153,.T.);
#23439=EDGE_CURVE('',#18759,#18758,#14792,.T.);
#23440=EDGE_CURVE('',#18759,#18760,#14793,.T.);
#23441=EDGE_CURVE('',#18760,#18756,#10154,.T.);
#23442=EDGE_CURVE('',#18758,#18755,#10155,.T.);
#23443=EDGE_CURVE('',#18754,#18759,#1588,.T.);
#23444=EDGE_CURVE('',#18761,#18762,#14794,.T.);
#23445=EDGE_CURVE('',#18761,#18757,#1589,.T.);
#23446=EDGE_CURVE('',#18756,#18762,#10156,.T.);
#23447=EDGE_CURVE('',#18763,#18764,#14795,.T.);
#23448=EDGE_CURVE('',#18764,#18761,#14796,.T.);
#23449=EDGE_CURVE('',#18762,#18763,#14797,.T.);
#23450=EDGE_CURVE('',#18765,#18766,#1590,.T.);
#23451=EDGE_CURVE('',#18766,#18701,#1591,.T.);
#23452=EDGE_CURVE('',#18701,#18767,#10157,.T.);
#23453=EDGE_CURVE('',#18768,#18767,#14798,.T.);
#23454=EDGE_CURVE('',#18768,#18769,#14799,.T.);
#23455=EDGE_CURVE('',#18769,#18765,#10158,.T.);
#23456=EDGE_CURVE('',#18767,#18764,#10159,.T.);
#23457=EDGE_CURVE('',#18763,#18768,#1592,.T.);
#23458=EDGE_CURVE('',#18770,#18771,#1593,.T.);
#23459=EDGE_CURVE('',#18770,#18766,#1594,.T.);
#23460=EDGE_CURVE('',#18765,#18771,#10160,.T.);
#23461=EDGE_CURVE('',#18772,#18773,#14800,.T.);
#23462=EDGE_CURVE('',#18773,#18770,#1595,.T.);
#23463=EDGE_CURVE('',#18771,#18772,#14801,.T.);
#23464=EDGE_CURVE('',#18774,#18775,#14802,.T.);
#23465=EDGE_CURVE('',#18775,#18710,#14803,.T.);
#23466=EDGE_CURVE('',#18710,#18776,#10161,.T.);
#23467=EDGE_CURVE('',#18777,#18776,#14804,.T.);
#23468=EDGE_CURVE('',#18777,#18778,#14805,.T.);
#23469=EDGE_CURVE('',#18778,#18774,#10162,.T.);
#23470=EDGE_CURVE('',#18776,#18773,#10163,.T.);
#23471=EDGE_CURVE('',#18772,#18777,#1596,.T.);
#23472=EDGE_CURVE('',#18779,#18780,#14806,.T.);
#23473=EDGE_CURVE('',#18779,#18775,#1597,.T.);
#23474=EDGE_CURVE('',#18774,#18780,#10164,.T.);
#23475=EDGE_CURVE('',#18781,#18782,#14807,.T.);
#23476=EDGE_CURVE('',#18782,#18779,#14808,.T.);
#23477=EDGE_CURVE('',#18780,#18781,#14809,.T.);
#23478=EDGE_CURVE('',#18783,#18784,#14810,.T.);
#23479=EDGE_CURVE('',#18784,#18719,#14811,.T.);
#23480=EDGE_CURVE('',#18719,#18785,#10165,.T.);
#23481=EDGE_CURVE('',#18786,#18785,#14812,.T.);
#23482=EDGE_CURVE('',#18786,#18787,#14813,.T.);
#23483=EDGE_CURVE('',#18787,#18783,#10166,.T.);
#23484=EDGE_CURVE('',#18785,#18782,#10167,.T.);
#23485=EDGE_CURVE('',#18781,#18786,#1598,.T.);
#23486=EDGE_CURVE('',#18788,#18789,#14814,.T.);
#23487=EDGE_CURVE('',#18788,#18784,#1599,.T.);
#23488=EDGE_CURVE('',#18783,#18789,#10168,.T.);
#23489=EDGE_CURVE('',#18790,#18791,#14815,.T.);
#23490=EDGE_CURVE('',#18791,#18788,#14816,.T.);
#23491=EDGE_CURVE('',#18789,#18790,#14817,.T.);
#23492=EDGE_CURVE('',#18792,#18793,#14818,.T.);
#23493=EDGE_CURVE('',#18793,#18728,#14819,.T.);
#23494=EDGE_CURVE('',#18728,#18794,#10169,.T.);
#23495=EDGE_CURVE('',#18795,#18794,#14820,.T.);
#23496=EDGE_CURVE('',#18795,#18796,#14821,.T.);
#23497=EDGE_CURVE('',#18796,#18792,#10170,.F.);
#23498=EDGE_CURVE('',#18794,#18791,#10171,.T.);
#23499=EDGE_CURVE('',#18790,#18795,#1600,.T.);
#23500=EDGE_CURVE('',#17672,#18793,#14822,.T.);
#23501=EDGE_CURVE('',#18792,#17673,#10172,.F.);
#23502=EDGE_CURVE('',#17669,#18737,#969,.T.);
#23503=EDGE_CURVE('',#18737,#18797,#10173,.T.);
#23504=EDGE_CURVE('',#17670,#18797,#970,.T.);
#23505=EDGE_CURVE('',#18797,#17671,#971,.T.);
#23506=EDGE_CURVE('',#18798,#18799,#14823,.T.);
#23507=EDGE_CURVE('',#18799,#17353,#14824,.T.);
#23508=EDGE_CURVE('',#18800,#17352,#1601,.T.);
#23509=EDGE_CURVE('',#18800,#18801,#972,.T.);
#23510=EDGE_CURVE('',#18801,#18798,#10174,.T.);
#23511=EDGE_CURVE('',#18802,#18803,#14825,.T.);
#23512=EDGE_CURVE('',#18802,#18799,#1602,.T.);
#23513=EDGE_CURVE('',#18798,#18803,#10175,.T.);
#23514=EDGE_CURVE('',#18804,#18805,#14826,.T.);
#23515=EDGE_CURVE('',#18805,#18802,#14827,.T.);
#23516=EDGE_CURVE('',#18803,#18804,#14828,.T.);
#23517=EDGE_CURVE('',#18806,#18807,#14829,.T.);
#23518=EDGE_CURVE('',#18807,#18742,#14830,.T.);
#23519=EDGE_CURVE('',#18742,#18808,#10176,.T.);
#23520=EDGE_CURVE('',#18809,#18808,#14831,.T.);
#23521=EDGE_CURVE('',#18809,#18810,#14832,.T.);
#23522=EDGE_CURVE('',#18810,#18806,#10177,.T.);
#23523=EDGE_CURVE('',#18808,#18805,#10178,.T.);
#23524=EDGE_CURVE('',#18804,#18809,#1603,.T.);
#23525=EDGE_CURVE('',#17355,#18741,#973,.T.);
#23526=EDGE_CURVE('',#18811,#18812,#14833,.T.);
#23527=EDGE_CURVE('',#18811,#18807,#1604,.T.);
#23528=EDGE_CURVE('',#18806,#18812,#10179,.T.);
#23529=EDGE_CURVE('',#18813,#18814,#14834,.T.);
#23530=EDGE_CURVE('',#18814,#18811,#14835,.T.);
#23531=EDGE_CURVE('',#18812,#18813,#14836,.T.);
#23532=EDGE_CURVE('',#18815,#18816,#14837,.T.);
#23533=EDGE_CURVE('',#18816,#18751,#14838,.T.);
#23534=EDGE_CURVE('',#18751,#18817,#10180,.T.);
#23535=EDGE_CURVE('',#18818,#18817,#14839,.T.);
#23536=EDGE_CURVE('',#18818,#18819,#14840,.T.);
#23537=EDGE_CURVE('',#18819,#18815,#10181,.T.);
#23538=EDGE_CURVE('',#18817,#18814,#10182,.T.);
#23539=EDGE_CURVE('',#18813,#18818,#1605,.T.);
#23540=EDGE_CURVE('',#18820,#18821,#14841,.T.);
#23541=EDGE_CURVE('',#18820,#18816,#1606,.T.);
#23542=EDGE_CURVE('',#18815,#18821,#10183,.T.);
#23543=EDGE_CURVE('',#18822,#18823,#14842,.T.);
#23544=EDGE_CURVE('',#18823,#18820,#14843,.T.);
#23545=EDGE_CURVE('',#18821,#18822,#14844,.T.);
#23546=EDGE_CURVE('',#18824,#18825,#1607,.T.);
#23547=EDGE_CURVE('',#18825,#18760,#1608,.T.);
#23548=EDGE_CURVE('',#18760,#18826,#10184,.T.);
#23549=EDGE_CURVE('',#18827,#18826,#14845,.T.);
#23550=EDGE_CURVE('',#18827,#18828,#14846,.T.);
#23551=EDGE_CURVE('',#18828,#18824,#10185,.T.);
#23552=EDGE_CURVE('',#18826,#18823,#10186,.T.);
#23553=EDGE_CURVE('',#18822,#18827,#1609,.T.);
#23554=EDGE_CURVE('',#18829,#18830,#1610,.T.);
#23555=EDGE_CURVE('',#18829,#18825,#1611,.T.);
#23556=EDGE_CURVE('',#18824,#18830,#10187,.T.);
#23557=EDGE_CURVE('',#18831,#18832,#14847,.T.);
#23558=EDGE_CURVE('',#18832,#18829,#1612,.T.);
#23559=EDGE_CURVE('',#18830,#18831,#14848,.T.);
#23560=EDGE_CURVE('',#18833,#18834,#14849,.T.);
#23561=EDGE_CURVE('',#18834,#18769,#14850,.T.);
#23562=EDGE_CURVE('',#18769,#18835,#10188,.T.);
#23563=EDGE_CURVE('',#18836,#18835,#14851,.T.);
#23564=EDGE_CURVE('',#18836,#18837,#14852,.T.);
#23565=EDGE_CURVE('',#18837,#18833,#10189,.T.);
#23566=EDGE_CURVE('',#18835,#18832,#10190,.T.);
#23567=EDGE_CURVE('',#18831,#18836,#1613,.T.);
#23568=EDGE_CURVE('',#18838,#18839,#14853,.T.);
#23569=EDGE_CURVE('',#18838,#18834,#1614,.T.);
#23570=EDGE_CURVE('',#18833,#18839,#10191,.T.);
#23571=EDGE_CURVE('',#18840,#18841,#14854,.T.);
#23572=EDGE_CURVE('',#18841,#18838,#14855,.T.);
#23573=EDGE_CURVE('',#18839,#18840,#14856,.T.);
#23574=EDGE_CURVE('',#18842,#18843,#14857,.T.);
#23575=EDGE_CURVE('',#18843,#18778,#14858,.T.);
#23576=EDGE_CURVE('',#18778,#18844,#10192,.T.);
#23577=EDGE_CURVE('',#18845,#18844,#14859,.T.);
#23578=EDGE_CURVE('',#18845,#18846,#14860,.T.);
#23579=EDGE_CURVE('',#18846,#18842,#10193,.T.);
#23580=EDGE_CURVE('',#18844,#18841,#10194,.T.);
#23581=EDGE_CURVE('',#18840,#18845,#1615,.T.);
#23582=EDGE_CURVE('',#18847,#18848,#14861,.T.);
#23583=EDGE_CURVE('',#18847,#18843,#1616,.T.);
#23584=EDGE_CURVE('',#18842,#18848,#10195,.T.);
#23585=EDGE_CURVE('',#18849,#18850,#14862,.T.);
#23586=EDGE_CURVE('',#18850,#18847,#14863,.T.);
#23587=EDGE_CURVE('',#18848,#18849,#14864,.T.);
#23588=EDGE_CURVE('',#18851,#18852,#14865,.T.);
#23589=EDGE_CURVE('',#18852,#18787,#14866,.T.);
#23590=EDGE_CURVE('',#18787,#18853,#10196,.T.);
#23591=EDGE_CURVE('',#18854,#18853,#14867,.T.);
#23592=EDGE_CURVE('',#18854,#18855,#14868,.T.);
#23593=EDGE_CURVE('',#18855,#18851,#10197,.F.);
#23594=EDGE_CURVE('',#18853,#18850,#10198,.T.);
#23595=EDGE_CURVE('',#18849,#18854,#1617,.T.);
#23596=EDGE_CURVE('',#17678,#18852,#14869,.T.);
#23597=EDGE_CURVE('',#18851,#17679,#10199,.F.);
#23598=EDGE_CURVE('',#17675,#18796,#974,.T.);
#23599=EDGE_CURVE('',#18796,#18856,#10200,.T.);
#23600=EDGE_CURVE('',#17676,#18856,#975,.T.);
#23601=EDGE_CURVE('',#18856,#17677,#976,.T.);
#23602=EDGE_CURVE('',#18857,#18858,#14870,.T.);
#23603=EDGE_CURVE('',#18858,#17349,#14871,.T.);
#23604=EDGE_CURVE('',#18859,#17348,#1618,.T.);
#23605=EDGE_CURVE('',#18859,#18860,#977,.T.);
#23606=EDGE_CURVE('',#18860,#18857,#10201,.T.);
#23607=EDGE_CURVE('',#18861,#18862,#14872,.T.);
#23608=EDGE_CURVE('',#18861,#18858,#1619,.T.);
#23609=EDGE_CURVE('',#18857,#18862,#10202,.T.);
#23610=EDGE_CURVE('',#18863,#18864,#14873,.T.);
#23611=EDGE_CURVE('',#18864,#18861,#14874,.T.);
#23612=EDGE_CURVE('',#18862,#18863,#14875,.T.);
#23613=EDGE_CURVE('',#18865,#18866,#14876,.T.);
#23614=EDGE_CURVE('',#18866,#18801,#14877,.T.);
#23615=EDGE_CURVE('',#18801,#18867,#10203,.T.);
#23616=EDGE_CURVE('',#18868,#18867,#14878,.T.);
#23617=EDGE_CURVE('',#18868,#18869,#14879,.T.);
#23618=EDGE_CURVE('',#18869,#18865,#10204,.T.);
#23619=EDGE_CURVE('',#18867,#18864,#10205,.T.);
#23620=EDGE_CURVE('',#18863,#18868,#1620,.T.);
#23621=EDGE_CURVE('',#17351,#18800,#978,.T.);
#23622=EDGE_CURVE('',#18870,#18871,#14880,.T.);
#23623=EDGE_CURVE('',#18870,#18866,#1621,.T.);
#23624=EDGE_CURVE('',#18865,#18871,#10206,.T.);
#23625=EDGE_CURVE('',#18872,#18873,#14881,.T.);
#23626=EDGE_CURVE('',#18873,#18870,#14882,.T.);
#23627=EDGE_CURVE('',#18871,#18872,#14883,.T.);
#23628=EDGE_CURVE('',#18874,#18875,#14884,.T.);
#23629=EDGE_CURVE('',#18875,#18810,#14885,.T.);
#23630=EDGE_CURVE('',#18810,#18876,#10207,.T.);
#23631=EDGE_CURVE('',#18877,#18876,#14886,.T.);
#23632=EDGE_CURVE('',#18877,#18878,#14887,.T.);
#23633=EDGE_CURVE('',#18878,#18874,#10208,.T.);
#23634=EDGE_CURVE('',#18876,#18873,#10209,.T.);
#23635=EDGE_CURVE('',#18872,#18877,#1622,.T.);
#23636=EDGE_CURVE('',#18879,#18880,#14888,.T.);
#23637=EDGE_CURVE('',#18879,#18875,#1623,.T.);
#23638=EDGE_CURVE('',#18874,#18880,#10210,.T.);
#23639=EDGE_CURVE('',#18881,#18882,#14889,.T.);
#23640=EDGE_CURVE('',#18882,#18879,#14890,.T.);
#23641=EDGE_CURVE('',#18880,#18881,#14891,.T.);
#23642=EDGE_CURVE('',#18883,#18884,#1624,.T.);
#23643=EDGE_CURVE('',#18884,#18819,#1625,.T.);
#23644=EDGE_CURVE('',#18819,#18885,#10211,.T.);
#23645=EDGE_CURVE('',#18886,#18885,#14892,.T.);
#23646=EDGE_CURVE('',#18886,#18887,#14893,.T.);
#23647=EDGE_CURVE('',#18887,#18883,#10212,.T.);
#23648=EDGE_CURVE('',#18885,#18882,#10213,.T.);
#23649=EDGE_CURVE('',#18881,#18886,#1626,.T.);
#23650=EDGE_CURVE('',#18888,#18889,#1627,.T.);
#23651=EDGE_CURVE('',#18888,#18884,#1628,.T.);
#23652=EDGE_CURVE('',#18883,#18889,#10214,.T.);
#23653=EDGE_CURVE('',#18890,#18891,#14894,.T.);
#23654=EDGE_CURVE('',#18891,#18888,#1629,.T.);
#23655=EDGE_CURVE('',#18889,#18890,#14895,.T.);
#23656=EDGE_CURVE('',#18892,#18893,#14896,.T.);
#23657=EDGE_CURVE('',#18893,#18828,#14897,.T.);
#23658=EDGE_CURVE('',#18828,#18894,#10215,.T.);
#23659=EDGE_CURVE('',#18895,#18894,#14898,.T.);
#23660=EDGE_CURVE('',#18895,#18896,#14899,.T.);
#23661=EDGE_CURVE('',#18896,#18892,#10216,.T.);
#23662=EDGE_CURVE('',#18894,#18891,#10217,.T.);
#23663=EDGE_CURVE('',#18890,#18895,#1630,.T.);
#23664=EDGE_CURVE('',#18897,#18898,#14900,.T.);
#23665=EDGE_CURVE('',#18897,#18893,#1631,.T.);
#23666=EDGE_CURVE('',#18892,#18898,#10218,.T.);
#23667=EDGE_CURVE('',#18899,#18900,#14901,.T.);
#23668=EDGE_CURVE('',#18900,#18897,#14902,.T.);
#23669=EDGE_CURVE('',#18898,#18899,#14903,.T.);
#23670=EDGE_CURVE('',#18901,#18902,#14904,.T.);
#23671=EDGE_CURVE('',#18902,#18837,#14905,.T.);
#23672=EDGE_CURVE('',#18837,#18903,#10219,.T.);
#23673=EDGE_CURVE('',#18904,#18903,#14906,.T.);
#23674=EDGE_CURVE('',#18904,#18905,#14907,.T.);
#23675=EDGE_CURVE('',#18905,#18901,#10220,.T.);
#23676=EDGE_CURVE('',#18903,#18900,#10221,.T.);
#23677=EDGE_CURVE('',#18899,#18904,#1632,.T.);
#23678=EDGE_CURVE('',#18906,#18907,#14908,.T.);
#23679=EDGE_CURVE('',#18906,#18902,#1633,.T.);
#23680=EDGE_CURVE('',#18901,#18907,#10222,.T.);
#23681=EDGE_CURVE('',#18908,#18909,#14909,.T.);
#23682=EDGE_CURVE('',#18909,#18906,#14910,.T.);
#23683=EDGE_CURVE('',#18907,#18908,#14911,.T.);
#23684=EDGE_CURVE('',#18910,#18911,#14912,.T.);
#23685=EDGE_CURVE('',#18911,#18846,#14913,.T.);
#23686=EDGE_CURVE('',#18846,#18912,#10223,.T.);
#23687=EDGE_CURVE('',#18913,#18912,#14914,.T.);
#23688=EDGE_CURVE('',#18913,#18914,#14915,.T.);
#23689=EDGE_CURVE('',#18914,#18910,#10224,.F.);
#23690=EDGE_CURVE('',#18912,#18909,#10225,.T.);
#23691=EDGE_CURVE('',#18908,#18913,#1634,.T.);
#23692=EDGE_CURVE('',#17684,#18911,#14916,.T.);
#23693=EDGE_CURVE('',#18910,#17685,#10226,.F.);
#23694=EDGE_CURVE('',#17681,#18855,#979,.T.);
#23695=EDGE_CURVE('',#18855,#18915,#10227,.T.);
#23696=EDGE_CURVE('',#17682,#18915,#980,.T.);
#23697=EDGE_CURVE('',#18915,#17683,#981,.T.);
#23698=EDGE_CURVE('',#18916,#18917,#14917,.T.);
#23699=EDGE_CURVE('',#18917,#17345,#14918,.T.);
#23700=EDGE_CURVE('',#18918,#17344,#1635,.T.);
#23701=EDGE_CURVE('',#18918,#18919,#982,.T.);
#23702=EDGE_CURVE('',#18919,#18916,#10228,.T.);
#23703=EDGE_CURVE('',#18920,#18921,#14919,.T.);
#23704=EDGE_CURVE('',#18920,#18917,#1636,.T.);
#23705=EDGE_CURVE('',#18916,#18921,#10229,.T.);
#23706=EDGE_CURVE('',#18922,#18923,#14920,.T.);
#23707=EDGE_CURVE('',#18923,#18920,#14921,.T.);
#23708=EDGE_CURVE('',#18921,#18922,#14922,.T.);
#23709=EDGE_CURVE('',#18924,#18925,#14923,.T.);
#23710=EDGE_CURVE('',#18925,#18860,#14924,.T.);
#23711=EDGE_CURVE('',#18860,#18926,#10230,.T.);
#23712=EDGE_CURVE('',#18927,#18926,#14925,.T.);
#23713=EDGE_CURVE('',#18927,#18928,#14926,.T.);
#23714=EDGE_CURVE('',#18928,#18924,#10231,.T.);
#23715=EDGE_CURVE('',#18926,#18923,#10232,.T.);
#23716=EDGE_CURVE('',#18922,#18927,#1637,.T.);
#23717=EDGE_CURVE('',#17347,#18859,#983,.T.);
#23718=EDGE_CURVE('',#18929,#18930,#14927,.T.);
#23719=EDGE_CURVE('',#18929,#18925,#1638,.T.);
#23720=EDGE_CURVE('',#18924,#18930,#10233,.T.);
#23721=EDGE_CURVE('',#18931,#18932,#14928,.T.);
#23722=EDGE_CURVE('',#18932,#18929,#14929,.T.);
#23723=EDGE_CURVE('',#18930,#18931,#14930,.T.);
#23724=EDGE_CURVE('',#18933,#18934,#14931,.T.);
#23725=EDGE_CURVE('',#18934,#18869,#14932,.T.);
#23726=EDGE_CURVE('',#18869,#18935,#10234,.T.);
#23727=EDGE_CURVE('',#18936,#18935,#14933,.T.);
#23728=EDGE_CURVE('',#18936,#18937,#14934,.T.);
#23729=EDGE_CURVE('',#18937,#18933,#10235,.T.);
#23730=EDGE_CURVE('',#18935,#18932,#10236,.T.);
#23731=EDGE_CURVE('',#18931,#18936,#1639,.T.);
#23732=EDGE_CURVE('',#18938,#18939,#14935,.T.);
#23733=EDGE_CURVE('',#18938,#18934,#1640,.T.);
#23734=EDGE_CURVE('',#18933,#18939,#10237,.T.);
#23735=EDGE_CURVE('',#18940,#18941,#14936,.T.);
#23736=EDGE_CURVE('',#18941,#18938,#14937,.T.);
#23737=EDGE_CURVE('',#18939,#18940,#14938,.T.);
#23738=EDGE_CURVE('',#18942,#18943,#1641,.T.);
#23739=EDGE_CURVE('',#18943,#18878,#1642,.T.);
#23740=EDGE_CURVE('',#18878,#18944,#10238,.T.);
#23741=EDGE_CURVE('',#18945,#18944,#14939,.T.);
#23742=EDGE_CURVE('',#18945,#18946,#14940,.T.);
#23743=EDGE_CURVE('',#18946,#18942,#10239,.T.);
#23744=EDGE_CURVE('',#18944,#18941,#10240,.T.);
#23745=EDGE_CURVE('',#18940,#18945,#1643,.T.);
#23746=EDGE_CURVE('',#18947,#18948,#1644,.T.);
#23747=EDGE_CURVE('',#18947,#18943,#1645,.T.);
#23748=EDGE_CURVE('',#18942,#18948,#10241,.T.);
#23749=EDGE_CURVE('',#18949,#18950,#14941,.T.);
#23750=EDGE_CURVE('',#18950,#18947,#1646,.T.);
#23751=EDGE_CURVE('',#18948,#18949,#14942,.T.);
#23752=EDGE_CURVE('',#18951,#18952,#14943,.T.);
#23753=EDGE_CURVE('',#18952,#18887,#14944,.T.);
#23754=EDGE_CURVE('',#18887,#18953,#10242,.T.);
#23755=EDGE_CURVE('',#18954,#18953,#14945,.T.);
#23756=EDGE_CURVE('',#18954,#18955,#14946,.T.);
#23757=EDGE_CURVE('',#18955,#18951,#10243,.T.);
#23758=EDGE_CURVE('',#18953,#18950,#10244,.T.);
#23759=EDGE_CURVE('',#18949,#18954,#1647,.T.);
#23760=EDGE_CURVE('',#18956,#18957,#14947,.T.);
#23761=EDGE_CURVE('',#18956,#18952,#1648,.T.);
#23762=EDGE_CURVE('',#18951,#18957,#10245,.T.);
#23763=EDGE_CURVE('',#18958,#18959,#14948,.T.);
#23764=EDGE_CURVE('',#18959,#18956,#14949,.T.);
#23765=EDGE_CURVE('',#18957,#18958,#14950,.T.);
#23766=EDGE_CURVE('',#18960,#18961,#14951,.T.);
#23767=EDGE_CURVE('',#18961,#18896,#14952,.T.);
#23768=EDGE_CURVE('',#18896,#18962,#10246,.T.);
#23769=EDGE_CURVE('',#18963,#18962,#14953,.T.);
#23770=EDGE_CURVE('',#18963,#18964,#14954,.T.);
#23771=EDGE_CURVE('',#18964,#18960,#10247,.T.);
#23772=EDGE_CURVE('',#18962,#18959,#10248,.T.);
#23773=EDGE_CURVE('',#18958,#18963,#1649,.T.);
#23774=EDGE_CURVE('',#18965,#18966,#14955,.T.);
#23775=EDGE_CURVE('',#18965,#18961,#1650,.T.);
#23776=EDGE_CURVE('',#18960,#18966,#10249,.T.);
#23777=EDGE_CURVE('',#18967,#18968,#14956,.T.);
#23778=EDGE_CURVE('',#18968,#18965,#14957,.T.);
#23779=EDGE_CURVE('',#18966,#18967,#14958,.T.);
#23780=EDGE_CURVE('',#18969,#18970,#14959,.T.);
#23781=EDGE_CURVE('',#18970,#18905,#14960,.T.);
#23782=EDGE_CURVE('',#18905,#18971,#10250,.T.);
#23783=EDGE_CURVE('',#18972,#18971,#14961,.T.);
#23784=EDGE_CURVE('',#18972,#18973,#14962,.T.);
#23785=EDGE_CURVE('',#18973,#18969,#10251,.F.);
#23786=EDGE_CURVE('',#18971,#18968,#10252,.T.);
#23787=EDGE_CURVE('',#18967,#18972,#1651,.T.);
#23788=EDGE_CURVE('',#17690,#18970,#14963,.T.);
#23789=EDGE_CURVE('',#18969,#17691,#10253,.F.);
#23790=EDGE_CURVE('',#17687,#18914,#984,.T.);
#23791=EDGE_CURVE('',#18914,#18974,#10254,.T.);
#23792=EDGE_CURVE('',#17688,#18974,#985,.T.);
#23793=EDGE_CURVE('',#18974,#17689,#986,.T.);
#23794=EDGE_CURVE('',#18975,#18976,#14964,.T.);
#23795=EDGE_CURVE('',#18976,#17341,#14965,.T.);
#23796=EDGE_CURVE('',#18977,#17340,#1652,.T.);
#23797=EDGE_CURVE('',#18977,#18978,#987,.T.);
#23798=EDGE_CURVE('',#18978,#18975,#10255,.T.);
#23799=EDGE_CURVE('',#18979,#18980,#14966,.T.);
#23800=EDGE_CURVE('',#18979,#18976,#1653,.T.);
#23801=EDGE_CURVE('',#18975,#18980,#10256,.T.);
#23802=EDGE_CURVE('',#18981,#18982,#14967,.T.);
#23803=EDGE_CURVE('',#18982,#18979,#14968,.T.);
#23804=EDGE_CURVE('',#18980,#18981,#14969,.T.);
#23805=EDGE_CURVE('',#18983,#18984,#14970,.T.);
#23806=EDGE_CURVE('',#18984,#18919,#14971,.T.);
#23807=EDGE_CURVE('',#18919,#18985,#10257,.T.);
#23808=EDGE_CURVE('',#18986,#18985,#14972,.T.);
#23809=EDGE_CURVE('',#18986,#18987,#14973,.T.);
#23810=EDGE_CURVE('',#18987,#18983,#10258,.T.);
#23811=EDGE_CURVE('',#18985,#18982,#10259,.T.);
#23812=EDGE_CURVE('',#18981,#18986,#1654,.T.);
#23813=EDGE_CURVE('',#17343,#18918,#988,.T.);
#23814=EDGE_CURVE('',#18988,#18989,#14974,.T.);
#23815=EDGE_CURVE('',#18988,#18984,#1655,.T.);
#23816=EDGE_CURVE('',#18983,#18989,#10260,.T.);
#23817=EDGE_CURVE('',#18990,#18991,#14975,.T.);
#23818=EDGE_CURVE('',#18991,#18988,#14976,.T.);
#23819=EDGE_CURVE('',#18989,#18990,#14977,.T.);
#23820=EDGE_CURVE('',#18992,#18993,#14978,.T.);
#23821=EDGE_CURVE('',#18993,#18928,#14979,.T.);
#23822=EDGE_CURVE('',#18928,#18994,#10261,.T.);
#23823=EDGE_CURVE('',#18995,#18994,#14980,.T.);
#23824=EDGE_CURVE('',#18995,#18996,#14981,.T.);
#23825=EDGE_CURVE('',#18996,#18992,#10262,.T.);
#23826=EDGE_CURVE('',#18994,#18991,#10263,.T.);
#23827=EDGE_CURVE('',#18990,#18995,#1656,.T.);
#23828=EDGE_CURVE('',#18997,#18998,#14982,.T.);
#23829=EDGE_CURVE('',#18997,#18993,#1657,.T.);
#23830=EDGE_CURVE('',#18992,#18998,#10264,.T.);
#23831=EDGE_CURVE('',#18999,#19000,#14983,.T.);
#23832=EDGE_CURVE('',#19000,#18997,#14984,.T.);
#23833=EDGE_CURVE('',#18998,#18999,#14985,.T.);
#23834=EDGE_CURVE('',#19001,#19002,#1658,.T.);
#23835=EDGE_CURVE('',#19002,#18937,#1659,.T.);
#23836=EDGE_CURVE('',#18937,#19003,#10265,.T.);
#23837=EDGE_CURVE('',#19004,#19003,#14986,.T.);
#23838=EDGE_CURVE('',#19004,#19005,#14987,.T.);
#23839=EDGE_CURVE('',#19005,#19001,#10266,.T.);
#23840=EDGE_CURVE('',#19003,#19000,#10267,.T.);
#23841=EDGE_CURVE('',#18999,#19004,#1660,.T.);
#23842=EDGE_CURVE('',#19006,#19007,#1661,.T.);
#23843=EDGE_CURVE('',#19006,#19002,#1662,.T.);
#23844=EDGE_CURVE('',#19001,#19007,#10268,.T.);
#23845=EDGE_CURVE('',#19008,#19009,#14988,.T.);
#23846=EDGE_CURVE('',#19009,#19006,#1663,.T.);
#23847=EDGE_CURVE('',#19007,#19008,#14989,.T.);
#23848=EDGE_CURVE('',#19010,#19011,#14990,.T.);
#23849=EDGE_CURVE('',#19011,#18946,#14991,.T.);
#23850=EDGE_CURVE('',#18946,#19012,#10269,.T.);
#23851=EDGE_CURVE('',#19013,#19012,#14992,.T.);
#23852=EDGE_CURVE('',#19013,#19014,#14993,.T.);
#23853=EDGE_CURVE('',#19014,#19010,#10270,.T.);
#23854=EDGE_CURVE('',#19012,#19009,#10271,.T.);
#23855=EDGE_CURVE('',#19008,#19013,#1664,.T.);
#23856=EDGE_CURVE('',#19015,#19016,#14994,.T.);
#23857=EDGE_CURVE('',#19015,#19011,#1665,.T.);
#23858=EDGE_CURVE('',#19010,#19016,#10272,.T.);
#23859=EDGE_CURVE('',#19017,#19018,#14995,.T.);
#23860=EDGE_CURVE('',#19018,#19015,#14996,.T.);
#23861=EDGE_CURVE('',#19016,#19017,#14997,.T.);
#23862=EDGE_CURVE('',#19019,#19020,#14998,.T.);
#23863=EDGE_CURVE('',#19020,#18955,#14999,.T.);
#23864=EDGE_CURVE('',#18955,#19021,#10273,.T.);
#23865=EDGE_CURVE('',#19022,#19021,#15000,.T.);
#23866=EDGE_CURVE('',#19022,#19023,#15001,.T.);
#23867=EDGE_CURVE('',#19023,#19019,#10274,.T.);
#23868=EDGE_CURVE('',#19021,#19018,#10275,.T.);
#23869=EDGE_CURVE('',#19017,#19022,#1666,.T.);
#23870=EDGE_CURVE('',#19024,#19025,#15002,.T.);
#23871=EDGE_CURVE('',#19024,#19020,#1667,.T.);
#23872=EDGE_CURVE('',#19019,#19025,#10276,.T.);
#23873=EDGE_CURVE('',#19026,#19027,#15003,.T.);
#23874=EDGE_CURVE('',#19027,#19024,#15004,.T.);
#23875=EDGE_CURVE('',#19025,#19026,#15005,.T.);
#23876=EDGE_CURVE('',#19028,#19029,#15006,.T.);
#23877=EDGE_CURVE('',#19029,#18964,#15007,.T.);
#23878=EDGE_CURVE('',#18964,#19030,#10277,.T.);
#23879=EDGE_CURVE('',#19031,#19030,#15008,.T.);
#23880=EDGE_CURVE('',#19031,#19032,#15009,.T.);
#23881=EDGE_CURVE('',#19032,#19028,#10278,.F.);
#23882=EDGE_CURVE('',#19030,#19027,#10279,.T.);
#23883=EDGE_CURVE('',#19026,#19031,#1668,.T.);
#23884=EDGE_CURVE('',#17696,#19029,#15010,.T.);
#23885=EDGE_CURVE('',#19028,#17697,#10280,.F.);
#23886=EDGE_CURVE('',#17693,#18973,#989,.T.);
#23887=EDGE_CURVE('',#18973,#19033,#10281,.T.);
#23888=EDGE_CURVE('',#17694,#19033,#990,.T.);
#23889=EDGE_CURVE('',#19033,#17695,#991,.T.);
#23890=EDGE_CURVE('',#19034,#19035,#15011,.T.);
#23891=EDGE_CURVE('',#19035,#17337,#15012,.T.);
#23892=EDGE_CURVE('',#19036,#17336,#1669,.T.);
#23893=EDGE_CURVE('',#19036,#19037,#992,.T.);
#23894=EDGE_CURVE('',#19037,#19034,#10282,.T.);
#23895=EDGE_CURVE('',#19038,#19039,#15013,.T.);
#23896=EDGE_CURVE('',#19038,#19035,#1670,.T.);
#23897=EDGE_CURVE('',#19034,#19039,#10283,.T.);
#23898=EDGE_CURVE('',#19040,#19041,#15014,.T.);
#23899=EDGE_CURVE('',#19041,#19038,#15015,.T.);
#23900=EDGE_CURVE('',#19039,#19040,#15016,.T.);
#23901=EDGE_CURVE('',#19042,#19043,#15017,.T.);
#23902=EDGE_CURVE('',#19043,#18978,#15018,.T.);
#23903=EDGE_CURVE('',#18978,#19044,#10284,.T.);
#23904=EDGE_CURVE('',#19045,#19044,#15019,.T.);
#23905=EDGE_CURVE('',#19045,#19046,#15020,.T.);
#23906=EDGE_CURVE('',#19046,#19042,#10285,.T.);
#23907=EDGE_CURVE('',#19044,#19041,#10286,.T.);
#23908=EDGE_CURVE('',#19040,#19045,#1671,.T.);
#23909=EDGE_CURVE('',#17339,#18977,#993,.T.);
#23910=EDGE_CURVE('',#19047,#19048,#15021,.T.);
#23911=EDGE_CURVE('',#19047,#19043,#1672,.T.);
#23912=EDGE_CURVE('',#19042,#19048,#10287,.T.);
#23913=EDGE_CURVE('',#19049,#19050,#15022,.T.);
#23914=EDGE_CURVE('',#19050,#19047,#15023,.T.);
#23915=EDGE_CURVE('',#19048,#19049,#15024,.T.);
#23916=EDGE_CURVE('',#19051,#19052,#15025,.T.);
#23917=EDGE_CURVE('',#19052,#18987,#15026,.T.);
#23918=EDGE_CURVE('',#18987,#19053,#10288,.T.);
#23919=EDGE_CURVE('',#19054,#19053,#15027,.T.);
#23920=EDGE_CURVE('',#19054,#19055,#15028,.T.);
#23921=EDGE_CURVE('',#19055,#19051,#10289,.T.);
#23922=EDGE_CURVE('',#19053,#19050,#10290,.T.);
#23923=EDGE_CURVE('',#19049,#19054,#1673,.T.);
#23924=EDGE_CURVE('',#19056,#19057,#15029,.T.);
#23925=EDGE_CURVE('',#19056,#19052,#1674,.T.);
#23926=EDGE_CURVE('',#19051,#19057,#10291,.T.);
#23927=EDGE_CURVE('',#19058,#19059,#15030,.T.);
#23928=EDGE_CURVE('',#19059,#19056,#15031,.T.);
#23929=EDGE_CURVE('',#19057,#19058,#15032,.T.);
#23930=EDGE_CURVE('',#19060,#19061,#1675,.T.);
#23931=EDGE_CURVE('',#19061,#18996,#1676,.T.);
#23932=EDGE_CURVE('',#18996,#19062,#10292,.T.);
#23933=EDGE_CURVE('',#19063,#19062,#15033,.T.);
#23934=EDGE_CURVE('',#19063,#19064,#15034,.T.);
#23935=EDGE_CURVE('',#19064,#19060,#10293,.T.);
#23936=EDGE_CURVE('',#19062,#19059,#10294,.T.);
#23937=EDGE_CURVE('',#19058,#19063,#1677,.T.);
#23938=EDGE_CURVE('',#19065,#19066,#1678,.T.);
#23939=EDGE_CURVE('',#19065,#19061,#1679,.T.);
#23940=EDGE_CURVE('',#19060,#19066,#10295,.T.);
#23941=EDGE_CURVE('',#19067,#19068,#15035,.T.);
#23942=EDGE_CURVE('',#19068,#19065,#1680,.T.);
#23943=EDGE_CURVE('',#19066,#19067,#15036,.T.);
#23944=EDGE_CURVE('',#19069,#19070,#15037,.T.);
#23945=EDGE_CURVE('',#19070,#19005,#15038,.T.);
#23946=EDGE_CURVE('',#19005,#19071,#10296,.T.);
#23947=EDGE_CURVE('',#19072,#19071,#15039,.T.);
#23948=EDGE_CURVE('',#19072,#19073,#15040,.T.);
#23949=EDGE_CURVE('',#19073,#19069,#10297,.T.);
#23950=EDGE_CURVE('',#19071,#19068,#10298,.T.);
#23951=EDGE_CURVE('',#19067,#19072,#1681,.T.);
#23952=EDGE_CURVE('',#19074,#19075,#15041,.T.);
#23953=EDGE_CURVE('',#19074,#19070,#1682,.T.);
#23954=EDGE_CURVE('',#19069,#19075,#10299,.T.);
#23955=EDGE_CURVE('',#19076,#19077,#15042,.T.);
#23956=EDGE_CURVE('',#19077,#19074,#15043,.T.);
#23957=EDGE_CURVE('',#19075,#19076,#15044,.T.);
#23958=EDGE_CURVE('',#19078,#19079,#15045,.T.);
#23959=EDGE_CURVE('',#19079,#19014,#15046,.T.);
#23960=EDGE_CURVE('',#19014,#19080,#10300,.T.);
#23961=EDGE_CURVE('',#19081,#19080,#15047,.T.);
#23962=EDGE_CURVE('',#19081,#19082,#15048,.T.);
#23963=EDGE_CURVE('',#19082,#19078,#10301,.T.);
#23964=EDGE_CURVE('',#19080,#19077,#10302,.T.);
#23965=EDGE_CURVE('',#19076,#19081,#1683,.T.);
#23966=EDGE_CURVE('',#19083,#19084,#15049,.T.);
#23967=EDGE_CURVE('',#19083,#19079,#1684,.T.);
#23968=EDGE_CURVE('',#19078,#19084,#10303,.T.);
#23969=EDGE_CURVE('',#19085,#19086,#15050,.T.);
#23970=EDGE_CURVE('',#19086,#19083,#15051,.T.);
#23971=EDGE_CURVE('',#19084,#19085,#15052,.T.);
#23972=EDGE_CURVE('',#19087,#19088,#15053,.T.);
#23973=EDGE_CURVE('',#19088,#19023,#15054,.T.);
#23974=EDGE_CURVE('',#19023,#19089,#10304,.T.);
#23975=EDGE_CURVE('',#19090,#19089,#15055,.T.);
#23976=EDGE_CURVE('',#19090,#19091,#15056,.T.);
#23977=EDGE_CURVE('',#19091,#19087,#10305,.F.);
#23978=EDGE_CURVE('',#19089,#19086,#10306,.T.);
#23979=EDGE_CURVE('',#19085,#19090,#1685,.T.);
#23980=EDGE_CURVE('',#17702,#19088,#15057,.T.);
#23981=EDGE_CURVE('',#19087,#17703,#10307,.F.);
#23982=EDGE_CURVE('',#17699,#19032,#994,.T.);
#23983=EDGE_CURVE('',#19032,#19092,#10308,.T.);
#23984=EDGE_CURVE('',#17700,#19092,#995,.T.);
#23985=EDGE_CURVE('',#19092,#17701,#996,.T.);
#23986=EDGE_CURVE('',#19093,#19094,#15058,.T.);
#23987=EDGE_CURVE('',#19094,#17333,#15059,.T.);
#23988=EDGE_CURVE('',#19095,#17332,#1686,.T.);
#23989=EDGE_CURVE('',#19095,#19096,#997,.T.);
#23990=EDGE_CURVE('',#19096,#19093,#10309,.T.);
#23991=EDGE_CURVE('',#19097,#19098,#15060,.T.);
#23992=EDGE_CURVE('',#19097,#19094,#1687,.T.);
#23993=EDGE_CURVE('',#19093,#19098,#10310,.T.);
#23994=EDGE_CURVE('',#19099,#19100,#15061,.T.);
#23995=EDGE_CURVE('',#19100,#19097,#15062,.T.);
#23996=EDGE_CURVE('',#19098,#19099,#15063,.T.);
#23997=EDGE_CURVE('',#19101,#19102,#15064,.T.);
#23998=EDGE_CURVE('',#19102,#19037,#15065,.T.);
#23999=EDGE_CURVE('',#19037,#19103,#10311,.T.);
#24000=EDGE_CURVE('',#19104,#19103,#15066,.T.);
#24001=EDGE_CURVE('',#19104,#19105,#15067,.T.);
#24002=EDGE_CURVE('',#19105,#19101,#10312,.T.);
#24003=EDGE_CURVE('',#19103,#19100,#10313,.T.);
#24004=EDGE_CURVE('',#19099,#19104,#1688,.T.);
#24005=EDGE_CURVE('',#17335,#19036,#998,.T.);
#24006=EDGE_CURVE('',#19106,#19107,#15068,.T.);
#24007=EDGE_CURVE('',#19106,#19102,#1689,.T.);
#24008=EDGE_CURVE('',#19101,#19107,#10314,.T.);
#24009=EDGE_CURVE('',#19108,#19109,#15069,.T.);
#24010=EDGE_CURVE('',#19109,#19106,#15070,.T.);
#24011=EDGE_CURVE('',#19107,#19108,#15071,.T.);
#24012=EDGE_CURVE('',#19110,#19111,#15072,.T.);
#24013=EDGE_CURVE('',#19111,#19046,#15073,.T.);
#24014=EDGE_CURVE('',#19046,#19112,#10315,.T.);
#24015=EDGE_CURVE('',#19113,#19112,#15074,.T.);
#24016=EDGE_CURVE('',#19113,#19114,#15075,.T.);
#24017=EDGE_CURVE('',#19114,#19110,#10316,.T.);
#24018=EDGE_CURVE('',#19112,#19109,#10317,.T.);
#24019=EDGE_CURVE('',#19108,#19113,#1690,.T.);
#24020=EDGE_CURVE('',#19115,#19116,#15076,.T.);
#24021=EDGE_CURVE('',#19115,#19111,#1691,.T.);
#24022=EDGE_CURVE('',#19110,#19116,#10318,.T.);
#24023=EDGE_CURVE('',#19117,#19118,#15077,.T.);
#24024=EDGE_CURVE('',#19118,#19115,#15078,.T.);
#24025=EDGE_CURVE('',#19116,#19117,#15079,.T.);
#24026=EDGE_CURVE('',#19119,#19120,#1692,.T.);
#24027=EDGE_CURVE('',#19120,#19055,#1693,.T.);
#24028=EDGE_CURVE('',#19055,#19121,#10319,.T.);
#24029=EDGE_CURVE('',#19122,#19121,#15080,.T.);
#24030=EDGE_CURVE('',#19122,#19123,#15081,.T.);
#24031=EDGE_CURVE('',#19123,#19119,#10320,.T.);
#24032=EDGE_CURVE('',#19121,#19118,#10321,.T.);
#24033=EDGE_CURVE('',#19117,#19122,#1694,.T.);
#24034=EDGE_CURVE('',#19124,#19125,#1695,.T.);
#24035=EDGE_CURVE('',#19124,#19120,#1696,.T.);
#24036=EDGE_CURVE('',#19119,#19125,#10322,.T.);
#24037=EDGE_CURVE('',#19126,#19127,#15082,.T.);
#24038=EDGE_CURVE('',#19127,#19124,#1697,.T.);
#24039=EDGE_CURVE('',#19125,#19126,#15083,.T.);
#24040=EDGE_CURVE('',#19128,#19129,#15084,.T.);
#24041=EDGE_CURVE('',#19129,#19064,#15085,.T.);
#24042=EDGE_CURVE('',#19064,#19130,#10323,.T.);
#24043=EDGE_CURVE('',#19131,#19130,#15086,.T.);
#24044=EDGE_CURVE('',#19131,#19132,#15087,.T.);
#24045=EDGE_CURVE('',#19132,#19128,#10324,.T.);
#24046=EDGE_CURVE('',#19130,#19127,#10325,.T.);
#24047=EDGE_CURVE('',#19126,#19131,#1698,.T.);
#24048=EDGE_CURVE('',#19133,#19134,#15088,.T.);
#24049=EDGE_CURVE('',#19133,#19129,#1699,.T.);
#24050=EDGE_CURVE('',#19128,#19134,#10326,.T.);
#24051=EDGE_CURVE('',#19135,#19136,#15089,.T.);
#24052=EDGE_CURVE('',#19136,#19133,#15090,.T.);
#24053=EDGE_CURVE('',#19134,#19135,#15091,.T.);
#24054=EDGE_CURVE('',#19137,#19138,#15092,.T.);
#24055=EDGE_CURVE('',#19138,#19073,#15093,.T.);
#24056=EDGE_CURVE('',#19073,#19139,#10327,.T.);
#24057=EDGE_CURVE('',#19140,#19139,#15094,.T.);
#24058=EDGE_CURVE('',#19140,#19141,#15095,.T.);
#24059=EDGE_CURVE('',#19141,#19137,#10328,.T.);
#24060=EDGE_CURVE('',#19139,#19136,#10329,.T.);
#24061=EDGE_CURVE('',#19135,#19140,#1700,.T.);
#24062=EDGE_CURVE('',#19142,#19143,#15096,.T.);
#24063=EDGE_CURVE('',#19142,#19138,#1701,.T.);
#24064=EDGE_CURVE('',#19137,#19143,#10330,.T.);
#24065=EDGE_CURVE('',#19144,#19145,#15097,.T.);
#24066=EDGE_CURVE('',#19145,#19142,#15098,.T.);
#24067=EDGE_CURVE('',#19143,#19144,#15099,.T.);
#24068=EDGE_CURVE('',#19146,#19147,#15100,.T.);
#24069=EDGE_CURVE('',#19147,#19082,#15101,.T.);
#24070=EDGE_CURVE('',#19082,#19148,#10331,.T.);
#24071=EDGE_CURVE('',#19149,#19148,#15102,.T.);
#24072=EDGE_CURVE('',#19149,#19150,#15103,.T.);
#24073=EDGE_CURVE('',#19150,#19146,#10332,.F.);
#24074=EDGE_CURVE('',#19148,#19145,#10333,.T.);
#24075=EDGE_CURVE('',#19144,#19149,#1702,.T.);
#24076=EDGE_CURVE('',#17708,#19147,#15104,.T.);
#24077=EDGE_CURVE('',#19146,#17709,#10334,.F.);
#24078=EDGE_CURVE('',#17705,#19091,#999,.T.);
#24079=EDGE_CURVE('',#19091,#19151,#10335,.T.);
#24080=EDGE_CURVE('',#17706,#19151,#1000,.T.);
#24081=EDGE_CURVE('',#19151,#17707,#1001,.T.);
#24082=EDGE_CURVE('',#19152,#19153,#15105,.T.);
#24083=EDGE_CURVE('',#19153,#17329,#15106,.T.);
#24084=EDGE_CURVE('',#19154,#17328,#1703,.T.);
#24085=EDGE_CURVE('',#19154,#19155,#1002,.T.);
#24086=EDGE_CURVE('',#19155,#19152,#10336,.T.);
#24087=EDGE_CURVE('',#19156,#19157,#15107,.T.);
#24088=EDGE_CURVE('',#19156,#19153,#1704,.T.);
#24089=EDGE_CURVE('',#19152,#19157,#10337,.T.);
#24090=EDGE_CURVE('',#19158,#19159,#15108,.T.);
#24091=EDGE_CURVE('',#19159,#19156,#15109,.T.);
#24092=EDGE_CURVE('',#19157,#19158,#15110,.T.);
#24093=EDGE_CURVE('',#19160,#19161,#15111,.T.);
#24094=EDGE_CURVE('',#19161,#19096,#15112,.T.);
#24095=EDGE_CURVE('',#19096,#19162,#10338,.T.);
#24096=EDGE_CURVE('',#19163,#19162,#15113,.T.);
#24097=EDGE_CURVE('',#19163,#19164,#15114,.T.);
#24098=EDGE_CURVE('',#19164,#19160,#10339,.T.);
#24099=EDGE_CURVE('',#19162,#19159,#10340,.T.);
#24100=EDGE_CURVE('',#19158,#19163,#1705,.T.);
#24101=EDGE_CURVE('',#17331,#19095,#1003,.T.);
#24102=EDGE_CURVE('',#19165,#19166,#15115,.T.);
#24103=EDGE_CURVE('',#19165,#19161,#1706,.T.);
#24104=EDGE_CURVE('',#19160,#19166,#10341,.T.);
#24105=EDGE_CURVE('',#19167,#19168,#15116,.T.);
#24106=EDGE_CURVE('',#19168,#19165,#15117,.T.);
#24107=EDGE_CURVE('',#19166,#19167,#15118,.T.);
#24108=EDGE_CURVE('',#19169,#19170,#15119,.T.);
#24109=EDGE_CURVE('',#19170,#19105,#15120,.T.);
#24110=EDGE_CURVE('',#19105,#19171,#10342,.T.);
#24111=EDGE_CURVE('',#19172,#19171,#15121,.T.);
#24112=EDGE_CURVE('',#19172,#19173,#15122,.T.);
#24113=EDGE_CURVE('',#19173,#19169,#10343,.T.);
#24114=EDGE_CURVE('',#19171,#19168,#10344,.T.);
#24115=EDGE_CURVE('',#19167,#19172,#1707,.T.);
#24116=EDGE_CURVE('',#19174,#19175,#15123,.T.);
#24117=EDGE_CURVE('',#19174,#19170,#1708,.T.);
#24118=EDGE_CURVE('',#19169,#19175,#10345,.T.);
#24119=EDGE_CURVE('',#19176,#19177,#15124,.T.);
#24120=EDGE_CURVE('',#19177,#19174,#15125,.T.);
#24121=EDGE_CURVE('',#19175,#19176,#15126,.T.);
#24122=EDGE_CURVE('',#19178,#19179,#1709,.T.);
#24123=EDGE_CURVE('',#19179,#19114,#1710,.T.);
#24124=EDGE_CURVE('',#19114,#19180,#10346,.T.);
#24125=EDGE_CURVE('',#19181,#19180,#15127,.T.);
#24126=EDGE_CURVE('',#19181,#19182,#15128,.T.);
#24127=EDGE_CURVE('',#19182,#19178,#10347,.T.);
#24128=EDGE_CURVE('',#19180,#19177,#10348,.T.);
#24129=EDGE_CURVE('',#19176,#19181,#1711,.T.);
#24130=EDGE_CURVE('',#19183,#19184,#1712,.T.);
#24131=EDGE_CURVE('',#19183,#19179,#1713,.T.);
#24132=EDGE_CURVE('',#19178,#19184,#10349,.T.);
#24133=EDGE_CURVE('',#19185,#19186,#15129,.T.);
#24134=EDGE_CURVE('',#19186,#19183,#1714,.T.);
#24135=EDGE_CURVE('',#19184,#19185,#15130,.T.);
#24136=EDGE_CURVE('',#19187,#19188,#15131,.T.);
#24137=EDGE_CURVE('',#19188,#19123,#15132,.T.);
#24138=EDGE_CURVE('',#19123,#19189,#10350,.T.);
#24139=EDGE_CURVE('',#19190,#19189,#15133,.T.);
#24140=EDGE_CURVE('',#19190,#19191,#15134,.T.);
#24141=EDGE_CURVE('',#19191,#19187,#10351,.T.);
#24142=EDGE_CURVE('',#19189,#19186,#10352,.T.);
#24143=EDGE_CURVE('',#19185,#19190,#1715,.T.);
#24144=EDGE_CURVE('',#19192,#19193,#15135,.T.);
#24145=EDGE_CURVE('',#19192,#19188,#1716,.T.);
#24146=EDGE_CURVE('',#19187,#19193,#10353,.T.);
#24147=EDGE_CURVE('',#19194,#19195,#15136,.T.);
#24148=EDGE_CURVE('',#19195,#19192,#15137,.T.);
#24149=EDGE_CURVE('',#19193,#19194,#15138,.T.);
#24150=EDGE_CURVE('',#19196,#19197,#15139,.T.);
#24151=EDGE_CURVE('',#19197,#19132,#15140,.T.);
#24152=EDGE_CURVE('',#19132,#19198,#10354,.T.);
#24153=EDGE_CURVE('',#19199,#19198,#15141,.T.);
#24154=EDGE_CURVE('',#19199,#19200,#15142,.T.);
#24155=EDGE_CURVE('',#19200,#19196,#10355,.T.);
#24156=EDGE_CURVE('',#19198,#19195,#10356,.T.);
#24157=EDGE_CURVE('',#19194,#19199,#1717,.T.);
#24158=EDGE_CURVE('',#19201,#19202,#15143,.T.);
#24159=EDGE_CURVE('',#19201,#19197,#1718,.T.);
#24160=EDGE_CURVE('',#19196,#19202,#10357,.T.);
#24161=EDGE_CURVE('',#19203,#19204,#15144,.T.);
#24162=EDGE_CURVE('',#19204,#19201,#15145,.T.);
#24163=EDGE_CURVE('',#19202,#19203,#15146,.T.);
#24164=EDGE_CURVE('',#19205,#19206,#15147,.T.);
#24165=EDGE_CURVE('',#19206,#19141,#15148,.T.);
#24166=EDGE_CURVE('',#19141,#19207,#10358,.T.);
#24167=EDGE_CURVE('',#19208,#19207,#15149,.T.);
#24168=EDGE_CURVE('',#19208,#19209,#15150,.T.);
#24169=EDGE_CURVE('',#19209,#19205,#10359,.F.);
#24170=EDGE_CURVE('',#19207,#19204,#10360,.T.);
#24171=EDGE_CURVE('',#19203,#19208,#1719,.T.);
#24172=EDGE_CURVE('',#17714,#19206,#15151,.T.);
#24173=EDGE_CURVE('',#19205,#17715,#10361,.F.);
#24174=EDGE_CURVE('',#17711,#19150,#1004,.T.);
#24175=EDGE_CURVE('',#19150,#19210,#10362,.T.);
#24176=EDGE_CURVE('',#17712,#19210,#1005,.T.);
#24177=EDGE_CURVE('',#19210,#17713,#1006,.T.);
#24178=EDGE_CURVE('',#19211,#19212,#15152,.T.);
#24179=EDGE_CURVE('',#19212,#17325,#15153,.T.);
#24180=EDGE_CURVE('',#19213,#17324,#1720,.T.);
#24181=EDGE_CURVE('',#19213,#19214,#1007,.T.);
#24182=EDGE_CURVE('',#19214,#19211,#10363,.T.);
#24183=EDGE_CURVE('',#19215,#19216,#15154,.T.);
#24184=EDGE_CURVE('',#19215,#19212,#1721,.T.);
#24185=EDGE_CURVE('',#19211,#19216,#10364,.T.);
#24186=EDGE_CURVE('',#19217,#19218,#15155,.T.);
#24187=EDGE_CURVE('',#19218,#19215,#15156,.T.);
#24188=EDGE_CURVE('',#19216,#19217,#15157,.T.);
#24189=EDGE_CURVE('',#19219,#19220,#15158,.T.);
#24190=EDGE_CURVE('',#19220,#19155,#15159,.T.);
#24191=EDGE_CURVE('',#19155,#19221,#10365,.T.);
#24192=EDGE_CURVE('',#19222,#19221,#15160,.T.);
#24193=EDGE_CURVE('',#19222,#19223,#15161,.T.);
#24194=EDGE_CURVE('',#19223,#19219,#10366,.T.);
#24195=EDGE_CURVE('',#19221,#19218,#10367,.T.);
#24196=EDGE_CURVE('',#19217,#19222,#1722,.T.);
#24197=EDGE_CURVE('',#17327,#19154,#1008,.T.);
#24198=EDGE_CURVE('',#19224,#19225,#15162,.T.);
#24199=EDGE_CURVE('',#19224,#19220,#1723,.T.);
#24200=EDGE_CURVE('',#19219,#19225,#10368,.T.);
#24201=EDGE_CURVE('',#19226,#19227,#15163,.T.);
#24202=EDGE_CURVE('',#19227,#19224,#15164,.T.);
#24203=EDGE_CURVE('',#19225,#19226,#15165,.T.);
#24204=EDGE_CURVE('',#19228,#19229,#15166,.T.);
#24205=EDGE_CURVE('',#19229,#19164,#15167,.T.);
#24206=EDGE_CURVE('',#19164,#19230,#10369,.T.);
#24207=EDGE_CURVE('',#19231,#19230,#15168,.T.);
#24208=EDGE_CURVE('',#19231,#19232,#15169,.T.);
#24209=EDGE_CURVE('',#19232,#19228,#10370,.T.);
#24210=EDGE_CURVE('',#19230,#19227,#10371,.T.);
#24211=EDGE_CURVE('',#19226,#19231,#1724,.T.);
#24212=EDGE_CURVE('',#19233,#19234,#15170,.T.);
#24213=EDGE_CURVE('',#19233,#19229,#1725,.T.);
#24214=EDGE_CURVE('',#19228,#19234,#10372,.T.);
#24215=EDGE_CURVE('',#19235,#19236,#15171,.T.);
#24216=EDGE_CURVE('',#19236,#19233,#15172,.T.);
#24217=EDGE_CURVE('',#19234,#19235,#15173,.T.);
#24218=EDGE_CURVE('',#19237,#19238,#1726,.T.);
#24219=EDGE_CURVE('',#19238,#19173,#1727,.T.);
#24220=EDGE_CURVE('',#19173,#19239,#10373,.T.);
#24221=EDGE_CURVE('',#19240,#19239,#15174,.T.);
#24222=EDGE_CURVE('',#19240,#19241,#15175,.T.);
#24223=EDGE_CURVE('',#19241,#19237,#10374,.T.);
#24224=EDGE_CURVE('',#19239,#19236,#10375,.T.);
#24225=EDGE_CURVE('',#19235,#19240,#1728,.T.);
#24226=EDGE_CURVE('',#19242,#19243,#1729,.T.);
#24227=EDGE_CURVE('',#19242,#19238,#1730,.T.);
#24228=EDGE_CURVE('',#19237,#19243,#10376,.T.);
#24229=EDGE_CURVE('',#19244,#19245,#15176,.T.);
#24230=EDGE_CURVE('',#19245,#19242,#1731,.T.);
#24231=EDGE_CURVE('',#19243,#19244,#15177,.T.);
#24232=EDGE_CURVE('',#19246,#19247,#15178,.T.);
#24233=EDGE_CURVE('',#19247,#19182,#15179,.T.);
#24234=EDGE_CURVE('',#19182,#19248,#10377,.T.);
#24235=EDGE_CURVE('',#19249,#19248,#15180,.T.);
#24236=EDGE_CURVE('',#19249,#19250,#15181,.T.);
#24237=EDGE_CURVE('',#19250,#19246,#10378,.T.);
#24238=EDGE_CURVE('',#19248,#19245,#10379,.T.);
#24239=EDGE_CURVE('',#19244,#19249,#1732,.T.);
#24240=EDGE_CURVE('',#19251,#19252,#15182,.T.);
#24241=EDGE_CURVE('',#19251,#19247,#1733,.T.);
#24242=EDGE_CURVE('',#19246,#19252,#10380,.T.);
#24243=EDGE_CURVE('',#19253,#19254,#15183,.T.);
#24244=EDGE_CURVE('',#19254,#19251,#15184,.T.);
#24245=EDGE_CURVE('',#19252,#19253,#15185,.T.);
#24246=EDGE_CURVE('',#19255,#19256,#15186,.T.);
#24247=EDGE_CURVE('',#19256,#19191,#15187,.T.);
#24248=EDGE_CURVE('',#19191,#19257,#10381,.T.);
#24249=EDGE_CURVE('',#19258,#19257,#15188,.T.);
#24250=EDGE_CURVE('',#19258,#19259,#15189,.T.);
#24251=EDGE_CURVE('',#19259,#19255,#10382,.T.);
#24252=EDGE_CURVE('',#19257,#19254,#10383,.T.);
#24253=EDGE_CURVE('',#19253,#19258,#1734,.T.);
#24254=EDGE_CURVE('',#19260,#19261,#15190,.T.);
#24255=EDGE_CURVE('',#19260,#19256,#1735,.T.);
#24256=EDGE_CURVE('',#19255,#19261,#10384,.T.);
#24257=EDGE_CURVE('',#19262,#19263,#15191,.T.);
#24258=EDGE_CURVE('',#19263,#19260,#15192,.T.);
#24259=EDGE_CURVE('',#19261,#19262,#15193,.T.);
#24260=EDGE_CURVE('',#19264,#19265,#15194,.T.);
#24261=EDGE_CURVE('',#19265,#19200,#15195,.T.);
#24262=EDGE_CURVE('',#19200,#19266,#10385,.T.);
#24263=EDGE_CURVE('',#19267,#19266,#15196,.T.);
#24264=EDGE_CURVE('',#19267,#19268,#15197,.T.);
#24265=EDGE_CURVE('',#19268,#19264,#10386,.F.);
#24266=EDGE_CURVE('',#19266,#19263,#10387,.T.);
#24267=EDGE_CURVE('',#19262,#19267,#1736,.T.);
#24268=EDGE_CURVE('',#17720,#19265,#15198,.T.);
#24269=EDGE_CURVE('',#19264,#17721,#10388,.F.);
#24270=EDGE_CURVE('',#17717,#19209,#1009,.T.);
#24271=EDGE_CURVE('',#19209,#19269,#10389,.T.);
#24272=EDGE_CURVE('',#17718,#19269,#1010,.T.);
#24273=EDGE_CURVE('',#19269,#17719,#1011,.T.);
#24274=EDGE_CURVE('',#19270,#19271,#15199,.T.);
#24275=EDGE_CURVE('',#19271,#17321,#15200,.T.);
#24276=EDGE_CURVE('',#19272,#17320,#1737,.T.);
#24277=EDGE_CURVE('',#19272,#19273,#1012,.T.);
#24278=EDGE_CURVE('',#19273,#19270,#10390,.T.);
#24279=EDGE_CURVE('',#19274,#19275,#15201,.T.);
#24280=EDGE_CURVE('',#19274,#19271,#1738,.T.);
#24281=EDGE_CURVE('',#19270,#19275,#10391,.T.);
#24282=EDGE_CURVE('',#19276,#19277,#15202,.T.);
#24283=EDGE_CURVE('',#19277,#19274,#15203,.T.);
#24284=EDGE_CURVE('',#19275,#19276,#15204,.T.);
#24285=EDGE_CURVE('',#19278,#19279,#15205,.T.);
#24286=EDGE_CURVE('',#19279,#19214,#15206,.T.);
#24287=EDGE_CURVE('',#19214,#19280,#10392,.T.);
#24288=EDGE_CURVE('',#19281,#19280,#15207,.T.);
#24289=EDGE_CURVE('',#19281,#19282,#15208,.T.);
#24290=EDGE_CURVE('',#19282,#19278,#10393,.T.);
#24291=EDGE_CURVE('',#19280,#19277,#10394,.T.);
#24292=EDGE_CURVE('',#19276,#19281,#1739,.T.);
#24293=EDGE_CURVE('',#17323,#19213,#1013,.T.);
#24294=EDGE_CURVE('',#19283,#19284,#15209,.T.);
#24295=EDGE_CURVE('',#19283,#19279,#1740,.T.);
#24296=EDGE_CURVE('',#19278,#19284,#10395,.T.);
#24297=EDGE_CURVE('',#19285,#19286,#15210,.T.);
#24298=EDGE_CURVE('',#19286,#19283,#15211,.T.);
#24299=EDGE_CURVE('',#19284,#19285,#15212,.T.);
#24300=EDGE_CURVE('',#19287,#19288,#15213,.T.);
#24301=EDGE_CURVE('',#19288,#19223,#15214,.T.);
#24302=EDGE_CURVE('',#19223,#19289,#10396,.T.);
#24303=EDGE_CURVE('',#19290,#19289,#15215,.T.);
#24304=EDGE_CURVE('',#19290,#19291,#15216,.T.);
#24305=EDGE_CURVE('',#19291,#19287,#10397,.T.);
#24306=EDGE_CURVE('',#19289,#19286,#10398,.T.);
#24307=EDGE_CURVE('',#19285,#19290,#1741,.T.);
#24308=EDGE_CURVE('',#19292,#19293,#15217,.T.);
#24309=EDGE_CURVE('',#19292,#19288,#1742,.T.);
#24310=EDGE_CURVE('',#19287,#19293,#10399,.T.);
#24311=EDGE_CURVE('',#19294,#19295,#15218,.T.);
#24312=EDGE_CURVE('',#19295,#19292,#15219,.T.);
#24313=EDGE_CURVE('',#19293,#19294,#15220,.T.);
#24314=EDGE_CURVE('',#19296,#19297,#1743,.T.);
#24315=EDGE_CURVE('',#19297,#19232,#1744,.T.);
#24316=EDGE_CURVE('',#19232,#19298,#10400,.T.);
#24317=EDGE_CURVE('',#19299,#19298,#15221,.T.);
#24318=EDGE_CURVE('',#19299,#19300,#15222,.T.);
#24319=EDGE_CURVE('',#19300,#19296,#10401,.T.);
#24320=EDGE_CURVE('',#19298,#19295,#10402,.T.);
#24321=EDGE_CURVE('',#19294,#19299,#1745,.T.);
#24322=EDGE_CURVE('',#19301,#19302,#1746,.T.);
#24323=EDGE_CURVE('',#19301,#19297,#1747,.T.);
#24324=EDGE_CURVE('',#19296,#19302,#10403,.T.);
#24325=EDGE_CURVE('',#19303,#19304,#15223,.T.);
#24326=EDGE_CURVE('',#19304,#19301,#1748,.T.);
#24327=EDGE_CURVE('',#19302,#19303,#15224,.T.);
#24328=EDGE_CURVE('',#19305,#19306,#15225,.T.);
#24329=EDGE_CURVE('',#19306,#19241,#15226,.T.);
#24330=EDGE_CURVE('',#19241,#19307,#10404,.T.);
#24331=EDGE_CURVE('',#19308,#19307,#15227,.T.);
#24332=EDGE_CURVE('',#19308,#19309,#15228,.T.);
#24333=EDGE_CURVE('',#19309,#19305,#10405,.T.);
#24334=EDGE_CURVE('',#19307,#19304,#10406,.T.);
#24335=EDGE_CURVE('',#19303,#19308,#1749,.T.);
#24336=EDGE_CURVE('',#19310,#19311,#15229,.T.);
#24337=EDGE_CURVE('',#19310,#19306,#1750,.T.);
#24338=EDGE_CURVE('',#19305,#19311,#10407,.T.);
#24339=EDGE_CURVE('',#19312,#19313,#15230,.T.);
#24340=EDGE_CURVE('',#19313,#19310,#15231,.T.);
#24341=EDGE_CURVE('',#19311,#19312,#15232,.T.);
#24342=EDGE_CURVE('',#19314,#19315,#15233,.T.);
#24343=EDGE_CURVE('',#19315,#19250,#15234,.T.);
#24344=EDGE_CURVE('',#19250,#19316,#10408,.T.);
#24345=EDGE_CURVE('',#19317,#19316,#15235,.T.);
#24346=EDGE_CURVE('',#19317,#19318,#15236,.T.);
#24347=EDGE_CURVE('',#19318,#19314,#10409,.T.);
#24348=EDGE_CURVE('',#19316,#19313,#10410,.T.);
#24349=EDGE_CURVE('',#19312,#19317,#1751,.T.);
#24350=EDGE_CURVE('',#19319,#19320,#15237,.T.);
#24351=EDGE_CURVE('',#19319,#19315,#1752,.T.);
#24352=EDGE_CURVE('',#19314,#19320,#10411,.T.);
#24353=EDGE_CURVE('',#19321,#19322,#15238,.T.);
#24354=EDGE_CURVE('',#19322,#19319,#15239,.T.);
#24355=EDGE_CURVE('',#19320,#19321,#15240,.T.);
#24356=EDGE_CURVE('',#19323,#19324,#15241,.T.);
#24357=EDGE_CURVE('',#19324,#19259,#15242,.T.);
#24358=EDGE_CURVE('',#19259,#19325,#10412,.T.);
#24359=EDGE_CURVE('',#19326,#19325,#15243,.T.);
#24360=EDGE_CURVE('',#19326,#19327,#15244,.T.);
#24361=EDGE_CURVE('',#19327,#19323,#10413,.F.);
#24362=EDGE_CURVE('',#19325,#19322,#10414,.T.);
#24363=EDGE_CURVE('',#19321,#19326,#1753,.T.);
#24364=EDGE_CURVE('',#17726,#19324,#15245,.T.);
#24365=EDGE_CURVE('',#19323,#17727,#10415,.F.);
#24366=EDGE_CURVE('',#17723,#19268,#1014,.T.);
#24367=EDGE_CURVE('',#19268,#19328,#10416,.T.);
#24368=EDGE_CURVE('',#17724,#19328,#1015,.T.);
#24369=EDGE_CURVE('',#19328,#17725,#1016,.T.);
#24370=EDGE_CURVE('',#19329,#19330,#15246,.T.);
#24371=EDGE_CURVE('',#19330,#17317,#15247,.T.);
#24372=EDGE_CURVE('',#19331,#17316,#1754,.T.);
#24373=EDGE_CURVE('',#19331,#19332,#1017,.T.);
#24374=EDGE_CURVE('',#19332,#19329,#10417,.T.);
#24375=EDGE_CURVE('',#19333,#19334,#15248,.T.);
#24376=EDGE_CURVE('',#19333,#19330,#1755,.T.);
#24377=EDGE_CURVE('',#19329,#19334,#10418,.T.);
#24378=EDGE_CURVE('',#19335,#19336,#15249,.T.);
#24379=EDGE_CURVE('',#19336,#19333,#15250,.T.);
#24380=EDGE_CURVE('',#19334,#19335,#15251,.T.);
#24381=EDGE_CURVE('',#19337,#19338,#15252,.T.);
#24382=EDGE_CURVE('',#19338,#19273,#15253,.T.);
#24383=EDGE_CURVE('',#19273,#19339,#10419,.T.);
#24384=EDGE_CURVE('',#19340,#19339,#15254,.T.);
#24385=EDGE_CURVE('',#19340,#19341,#15255,.T.);
#24386=EDGE_CURVE('',#19341,#19337,#10420,.T.);
#24387=EDGE_CURVE('',#19339,#19336,#10421,.T.);
#24388=EDGE_CURVE('',#19335,#19340,#1756,.T.);
#24389=EDGE_CURVE('',#17319,#19272,#1018,.T.);
#24390=EDGE_CURVE('',#19342,#19343,#15256,.T.);
#24391=EDGE_CURVE('',#19342,#19338,#1757,.T.);
#24392=EDGE_CURVE('',#19337,#19343,#10422,.T.);
#24393=EDGE_CURVE('',#19344,#19345,#15257,.T.);
#24394=EDGE_CURVE('',#19345,#19342,#15258,.T.);
#24395=EDGE_CURVE('',#19343,#19344,#15259,.T.);
#24396=EDGE_CURVE('',#19346,#19347,#15260,.T.);
#24397=EDGE_CURVE('',#19347,#19282,#15261,.T.);
#24398=EDGE_CURVE('',#19282,#19348,#10423,.T.);
#24399=EDGE_CURVE('',#19349,#19348,#15262,.T.);
#24400=EDGE_CURVE('',#19349,#19350,#15263,.T.);
#24401=EDGE_CURVE('',#19350,#19346,#10424,.T.);
#24402=EDGE_CURVE('',#19348,#19345,#10425,.T.);
#24403=EDGE_CURVE('',#19344,#19349,#1758,.T.);
#24404=EDGE_CURVE('',#19351,#19352,#15264,.T.);
#24405=EDGE_CURVE('',#19351,#19347,#1759,.T.);
#24406=EDGE_CURVE('',#19346,#19352,#10426,.T.);
#24407=EDGE_CURVE('',#19353,#19354,#15265,.T.);
#24408=EDGE_CURVE('',#19354,#19351,#15266,.T.);
#24409=EDGE_CURVE('',#19352,#19353,#15267,.T.);
#24410=EDGE_CURVE('',#19355,#19356,#1760,.T.);
#24411=EDGE_CURVE('',#19356,#19291,#1761,.T.);
#24412=EDGE_CURVE('',#19291,#19357,#10427,.T.);
#24413=EDGE_CURVE('',#19358,#19357,#15268,.T.);
#24414=EDGE_CURVE('',#19358,#19359,#15269,.T.);
#24415=EDGE_CURVE('',#19359,#19355,#10428,.T.);
#24416=EDGE_CURVE('',#19357,#19354,#10429,.T.);
#24417=EDGE_CURVE('',#19353,#19358,#1762,.T.);
#24418=EDGE_CURVE('',#19360,#19361,#1763,.T.);
#24419=EDGE_CURVE('',#19360,#19356,#1764,.T.);
#24420=EDGE_CURVE('',#19355,#19361,#10430,.T.);
#24421=EDGE_CURVE('',#19362,#19363,#15270,.T.);
#24422=EDGE_CURVE('',#19363,#19360,#1765,.T.);
#24423=EDGE_CURVE('',#19361,#19362,#15271,.T.);
#24424=EDGE_CURVE('',#19364,#19365,#15272,.T.);
#24425=EDGE_CURVE('',#19365,#19300,#15273,.T.);
#24426=EDGE_CURVE('',#19300,#19366,#10431,.T.);
#24427=EDGE_CURVE('',#19367,#19366,#15274,.T.);
#24428=EDGE_CURVE('',#19367,#19368,#15275,.T.);
#24429=EDGE_CURVE('',#19368,#19364,#10432,.T.);
#24430=EDGE_CURVE('',#19366,#19363,#10433,.T.);
#24431=EDGE_CURVE('',#19362,#19367,#1766,.T.);
#24432=EDGE_CURVE('',#19369,#19370,#15276,.T.);
#24433=EDGE_CURVE('',#19369,#19365,#1767,.T.);
#24434=EDGE_CURVE('',#19364,#19370,#10434,.T.);
#24435=EDGE_CURVE('',#19371,#19372,#15277,.T.);
#24436=EDGE_CURVE('',#19372,#19369,#15278,.T.);
#24437=EDGE_CURVE('',#19370,#19371,#15279,.T.);
#24438=EDGE_CURVE('',#19373,#19374,#15280,.T.);
#24439=EDGE_CURVE('',#19374,#19309,#15281,.T.);
#24440=EDGE_CURVE('',#19309,#19375,#10435,.T.);
#24441=EDGE_CURVE('',#19376,#19375,#15282,.T.);
#24442=EDGE_CURVE('',#19376,#19377,#15283,.T.);
#24443=EDGE_CURVE('',#19377,#19373,#10436,.T.);
#24444=EDGE_CURVE('',#19375,#19372,#10437,.T.);
#24445=EDGE_CURVE('',#19371,#19376,#1768,.T.);
#24446=EDGE_CURVE('',#19378,#19379,#15284,.T.);
#24447=EDGE_CURVE('',#19378,#19374,#1769,.T.);
#24448=EDGE_CURVE('',#19373,#19379,#10438,.T.);
#24449=EDGE_CURVE('',#19380,#19381,#15285,.T.);
#24450=EDGE_CURVE('',#19381,#19378,#15286,.T.);
#24451=EDGE_CURVE('',#19379,#19380,#15287,.T.);
#24452=EDGE_CURVE('',#19382,#19383,#15288,.T.);
#24453=EDGE_CURVE('',#19383,#19318,#15289,.T.);
#24454=EDGE_CURVE('',#19318,#19384,#10439,.T.);
#24455=EDGE_CURVE('',#19385,#19384,#15290,.T.);
#24456=EDGE_CURVE('',#19385,#19386,#15291,.T.);
#24457=EDGE_CURVE('',#19386,#19382,#10440,.F.);
#24458=EDGE_CURVE('',#19384,#19381,#10441,.T.);
#24459=EDGE_CURVE('',#19380,#19385,#1770,.T.);
#24460=EDGE_CURVE('',#17432,#19383,#15292,.T.);
#24461=EDGE_CURVE('',#19382,#17433,#10442,.F.);
#24462=EDGE_CURVE('',#17729,#19327,#1019,.T.);
#24463=EDGE_CURVE('',#19327,#19387,#10443,.T.);
#24464=EDGE_CURVE('',#17730,#19387,#1020,.T.);
#24465=EDGE_CURVE('',#19387,#17429,#1021,.T.);
#24466=EDGE_CURVE('',#19388,#19389,#15293,.T.);
#24467=EDGE_CURVE('',#19389,#17313,#15294,.T.);
#24468=EDGE_CURVE('',#19390,#17312,#1771,.T.);
#24469=EDGE_CURVE('',#19390,#19391,#1022,.T.);
#24470=EDGE_CURVE('',#19391,#19388,#10444,.T.);
#24471=EDGE_CURVE('',#19392,#19393,#15295,.T.);
#24472=EDGE_CURVE('',#19392,#19389,#1772,.T.);
#24473=EDGE_CURVE('',#19388,#19393,#10445,.T.);
#24474=EDGE_CURVE('',#19394,#19395,#15296,.T.);
#24475=EDGE_CURVE('',#19395,#19392,#15297,.T.);
#24476=EDGE_CURVE('',#19393,#19394,#15298,.T.);
#24477=EDGE_CURVE('',#19396,#19397,#15299,.T.);
#24478=EDGE_CURVE('',#19397,#19332,#15300,.T.);
#24479=EDGE_CURVE('',#19332,#19398,#10446,.T.);
#24480=EDGE_CURVE('',#19399,#19398,#15301,.T.);
#24481=EDGE_CURVE('',#19399,#19400,#15302,.T.);
#24482=EDGE_CURVE('',#19400,#19396,#10447,.T.);
#24483=EDGE_CURVE('',#19398,#19395,#10448,.T.);
#24484=EDGE_CURVE('',#19394,#19399,#1773,.T.);
#24485=EDGE_CURVE('',#17315,#19331,#1023,.T.);
#24486=EDGE_CURVE('',#19401,#19402,#15303,.T.);
#24487=EDGE_CURVE('',#19401,#19397,#1774,.T.);
#24488=EDGE_CURVE('',#19396,#19402,#10449,.T.);
#24489=EDGE_CURVE('',#19403,#19404,#15304,.T.);
#24490=EDGE_CURVE('',#19404,#19401,#15305,.T.);
#24491=EDGE_CURVE('',#19402,#19403,#15306,.T.);
#24492=EDGE_CURVE('',#19405,#19406,#15307,.T.);
#24493=EDGE_CURVE('',#19406,#19341,#15308,.T.);
#24494=EDGE_CURVE('',#19341,#19407,#10450,.T.);
#24495=EDGE_CURVE('',#19408,#19407,#15309,.T.);
#24496=EDGE_CURVE('',#19408,#19409,#15310,.T.);
#24497=EDGE_CURVE('',#19409,#19405,#10451,.T.);
#24498=EDGE_CURVE('',#19407,#19404,#10452,.T.);
#24499=EDGE_CURVE('',#19403,#19408,#1775,.T.);
#24500=EDGE_CURVE('',#19410,#19411,#15311,.T.);
#24501=EDGE_CURVE('',#19410,#19406,#1776,.T.);
#24502=EDGE_CURVE('',#19405,#19411,#10453,.T.);
#24503=EDGE_CURVE('',#19412,#19413,#15312,.T.);
#24504=EDGE_CURVE('',#19413,#19410,#15313,.T.);
#24505=EDGE_CURVE('',#19411,#19412,#15314,.T.);
#24506=EDGE_CURVE('',#19414,#19415,#1777,.T.);
#24507=EDGE_CURVE('',#19415,#19350,#1778,.T.);
#24508=EDGE_CURVE('',#19350,#19416,#10454,.T.);
#24509=EDGE_CURVE('',#19417,#19416,#15315,.T.);
#24510=EDGE_CURVE('',#19417,#19418,#15316,.T.);
#24511=EDGE_CURVE('',#19418,#19414,#10455,.T.);
#24512=EDGE_CURVE('',#19416,#19413,#10456,.T.);
#24513=EDGE_CURVE('',#19412,#19417,#1779,.T.);
#24514=EDGE_CURVE('',#19419,#19420,#1780,.T.);
#24515=EDGE_CURVE('',#19419,#19415,#1781,.T.);
#24516=EDGE_CURVE('',#19414,#19420,#10457,.T.);
#24517=EDGE_CURVE('',#19421,#19422,#15317,.T.);
#24518=EDGE_CURVE('',#19422,#19419,#1782,.T.);
#24519=EDGE_CURVE('',#19420,#19421,#15318,.T.);
#24520=EDGE_CURVE('',#19423,#19424,#15319,.T.);
#24521=EDGE_CURVE('',#19424,#19359,#15320,.T.);
#24522=EDGE_CURVE('',#19359,#19425,#10458,.T.);
#24523=EDGE_CURVE('',#19426,#19425,#15321,.T.);
#24524=EDGE_CURVE('',#19426,#19427,#15322,.T.);
#24525=EDGE_CURVE('',#19427,#19423,#10459,.T.);
#24526=EDGE_CURVE('',#19425,#19422,#10460,.T.);
#24527=EDGE_CURVE('',#19421,#19426,#1783,.T.);
#24528=EDGE_CURVE('',#19428,#19429,#15323,.T.);
#24529=EDGE_CURVE('',#19428,#19424,#1784,.T.);
#24530=EDGE_CURVE('',#19423,#19429,#10461,.T.);
#24531=EDGE_CURVE('',#19430,#19431,#15324,.T.);
#24532=EDGE_CURVE('',#19431,#19428,#15325,.T.);
#24533=EDGE_CURVE('',#19429,#19430,#15326,.T.);
#24534=EDGE_CURVE('',#19432,#19433,#15327,.T.);
#24535=EDGE_CURVE('',#19433,#19368,#15328,.T.);
#24536=EDGE_CURVE('',#19368,#19434,#10462,.T.);
#24537=EDGE_CURVE('',#19435,#19434,#15329,.T.);
#24538=EDGE_CURVE('',#19435,#19436,#15330,.T.);
#24539=EDGE_CURVE('',#19436,#19432,#10463,.T.);
#24540=EDGE_CURVE('',#19434,#19431,#10464,.T.);
#24541=EDGE_CURVE('',#19430,#19435,#1785,.T.);
#24542=EDGE_CURVE('',#19437,#19438,#15331,.T.);
#24543=EDGE_CURVE('',#19437,#19433,#1786,.T.);
#24544=EDGE_CURVE('',#19432,#19438,#10465,.T.);
#24545=EDGE_CURVE('',#19439,#19440,#15332,.T.);
#24546=EDGE_CURVE('',#19440,#19437,#15333,.T.);
#24547=EDGE_CURVE('',#19438,#19439,#15334,.T.);
#24548=EDGE_CURVE('',#19441,#19442,#15335,.T.);
#24549=EDGE_CURVE('',#19442,#19377,#15336,.T.);
#24550=EDGE_CURVE('',#19377,#19443,#10466,.T.);
#24551=EDGE_CURVE('',#19444,#19443,#15337,.T.);
#24552=EDGE_CURVE('',#19444,#19445,#15338,.T.);
#24553=EDGE_CURVE('',#19445,#19441,#10467,.F.);
#24554=EDGE_CURVE('',#19443,#19440,#10468,.T.);
#24555=EDGE_CURVE('',#19439,#19444,#1787,.T.);
#24556=EDGE_CURVE('',#17438,#19442,#15339,.T.);
#24557=EDGE_CURVE('',#19441,#17439,#10469,.F.);
#24558=EDGE_CURVE('',#17435,#19386,#1024,.T.);
#24559=EDGE_CURVE('',#19386,#19446,#10470,.T.);
#24560=EDGE_CURVE('',#17436,#19446,#1025,.T.);
#24561=EDGE_CURVE('',#19446,#17437,#1026,.T.);
#24562=EDGE_CURVE('',#19447,#19448,#15340,.T.);
#24563=EDGE_CURVE('',#19448,#17309,#15341,.T.);
#24564=EDGE_CURVE('',#19449,#17308,#1788,.T.);
#24565=EDGE_CURVE('',#19449,#19450,#1027,.T.);
#24566=EDGE_CURVE('',#19450,#19447,#10471,.T.);
#24567=EDGE_CURVE('',#19451,#19452,#15342,.T.);
#24568=EDGE_CURVE('',#19451,#19448,#1789,.T.);
#24569=EDGE_CURVE('',#19447,#19452,#10472,.T.);
#24570=EDGE_CURVE('',#19453,#19454,#15343,.T.);
#24571=EDGE_CURVE('',#19454,#19451,#15344,.T.);
#24572=EDGE_CURVE('',#19452,#19453,#15345,.T.);
#24573=EDGE_CURVE('',#19455,#19456,#15346,.T.);
#24574=EDGE_CURVE('',#19456,#19391,#15347,.T.);
#24575=EDGE_CURVE('',#19391,#19457,#10473,.T.);
#24576=EDGE_CURVE('',#19458,#19457,#15348,.T.);
#24577=EDGE_CURVE('',#19458,#19459,#15349,.T.);
#24578=EDGE_CURVE('',#19459,#19455,#10474,.T.);
#24579=EDGE_CURVE('',#19457,#19454,#10475,.T.);
#24580=EDGE_CURVE('',#19453,#19458,#1790,.T.);
#24581=EDGE_CURVE('',#17311,#19390,#1028,.T.);
#24582=EDGE_CURVE('',#19460,#19461,#15350,.T.);
#24583=EDGE_CURVE('',#19460,#19456,#1791,.T.);
#24584=EDGE_CURVE('',#19455,#19461,#10476,.T.);
#24585=EDGE_CURVE('',#19462,#19463,#15351,.T.);
#24586=EDGE_CURVE('',#19463,#19460,#15352,.T.);
#24587=EDGE_CURVE('',#19461,#19462,#15353,.T.);
#24588=EDGE_CURVE('',#19464,#19465,#15354,.T.);
#24589=EDGE_CURVE('',#19465,#19400,#15355,.T.);
#24590=EDGE_CURVE('',#19400,#19466,#10477,.T.);
#24591=EDGE_CURVE('',#19467,#19466,#15356,.T.);
#24592=EDGE_CURVE('',#19467,#19468,#15357,.T.);
#24593=EDGE_CURVE('',#19468,#19464,#10478,.T.);
#24594=EDGE_CURVE('',#19466,#19463,#10479,.T.);
#24595=EDGE_CURVE('',#19462,#19467,#1792,.T.);
#24596=EDGE_CURVE('',#19469,#19470,#15358,.T.);
#24597=EDGE_CURVE('',#19469,#19465,#1793,.T.);
#24598=EDGE_CURVE('',#19464,#19470,#10480,.T.);
#24599=EDGE_CURVE('',#19471,#19472,#15359,.T.);
#24600=EDGE_CURVE('',#19472,#19469,#15360,.T.);
#24601=EDGE_CURVE('',#19470,#19471,#15361,.T.);
#24602=EDGE_CURVE('',#19473,#19474,#1794,.T.);
#24603=EDGE_CURVE('',#19474,#19409,#1795,.T.);
#24604=EDGE_CURVE('',#19409,#19475,#10481,.T.);
#24605=EDGE_CURVE('',#19476,#19475,#15362,.T.);
#24606=EDGE_CURVE('',#19476,#19477,#15363,.T.);
#24607=EDGE_CURVE('',#19477,#19473,#10482,.T.);
#24608=EDGE_CURVE('',#19475,#19472,#10483,.T.);
#24609=EDGE_CURVE('',#19471,#19476,#1796,.T.);
#24610=EDGE_CURVE('',#19478,#19479,#1797,.T.);
#24611=EDGE_CURVE('',#19478,#19474,#1798,.T.);
#24612=EDGE_CURVE('',#19473,#19479,#10484,.T.);
#24613=EDGE_CURVE('',#19480,#19481,#15364,.T.);
#24614=EDGE_CURVE('',#19481,#19478,#1799,.T.);
#24615=EDGE_CURVE('',#19479,#19480,#15365,.T.);
#24616=EDGE_CURVE('',#19482,#19483,#15366,.T.);
#24617=EDGE_CURVE('',#19483,#19418,#15367,.T.);
#24618=EDGE_CURVE('',#19418,#19484,#10485,.T.);
#24619=EDGE_CURVE('',#19485,#19484,#15368,.T.);
#24620=EDGE_CURVE('',#19485,#19486,#15369,.T.);
#24621=EDGE_CURVE('',#19486,#19482,#10486,.T.);
#24622=EDGE_CURVE('',#19484,#19481,#10487,.T.);
#24623=EDGE_CURVE('',#19480,#19485,#1800,.T.);
#24624=EDGE_CURVE('',#19487,#19488,#15370,.T.);
#24625=EDGE_CURVE('',#19487,#19483,#1801,.T.);
#24626=EDGE_CURVE('',#19482,#19488,#10488,.T.);
#24627=EDGE_CURVE('',#19489,#19490,#15371,.T.);
#24628=EDGE_CURVE('',#19490,#19487,#15372,.T.);
#24629=EDGE_CURVE('',#19488,#19489,#15373,.T.);
#24630=EDGE_CURVE('',#19491,#19492,#15374,.T.);
#24631=EDGE_CURVE('',#19492,#19427,#15375,.T.);
#24632=EDGE_CURVE('',#19427,#19493,#10489,.T.);
#24633=EDGE_CURVE('',#19494,#19493,#15376,.T.);
#24634=EDGE_CURVE('',#19494,#19495,#15377,.T.);
#24635=EDGE_CURVE('',#19495,#19491,#10490,.T.);
#24636=EDGE_CURVE('',#19493,#19490,#10491,.T.);
#24637=EDGE_CURVE('',#19489,#19494,#1802,.T.);
#24638=EDGE_CURVE('',#19496,#19497,#15378,.T.);
#24639=EDGE_CURVE('',#19496,#19492,#1803,.T.);
#24640=EDGE_CURVE('',#19491,#19497,#10492,.T.);
#24641=EDGE_CURVE('',#19498,#19499,#15379,.T.);
#24642=EDGE_CURVE('',#19499,#19496,#15380,.T.);
#24643=EDGE_CURVE('',#19497,#19498,#15381,.T.);
#24644=EDGE_CURVE('',#19500,#19501,#15382,.T.);
#24645=EDGE_CURVE('',#19501,#19436,#15383,.T.);
#24646=EDGE_CURVE('',#19436,#19502,#10493,.T.);
#24647=EDGE_CURVE('',#19503,#19502,#15384,.T.);
#24648=EDGE_CURVE('',#19503,#19504,#15385,.T.);
#24649=EDGE_CURVE('',#19504,#19500,#10494,.F.);
#24650=EDGE_CURVE('',#19502,#19499,#10495,.T.);
#24651=EDGE_CURVE('',#19498,#19503,#1804,.T.);
#24652=EDGE_CURVE('',#17444,#19501,#15386,.T.);
#24653=EDGE_CURVE('',#19500,#17445,#10496,.F.);
#24654=EDGE_CURVE('',#17441,#19445,#1029,.T.);
#24655=EDGE_CURVE('',#19445,#19505,#10497,.T.);
#24656=EDGE_CURVE('',#17442,#19505,#1030,.T.);
#24657=EDGE_CURVE('',#19505,#17443,#1031,.T.);
#24658=EDGE_CURVE('',#19506,#19507,#15387,.T.);
#24659=EDGE_CURVE('',#19507,#17305,#15388,.T.);
#24660=EDGE_CURVE('',#19508,#17304,#1805,.T.);
#24661=EDGE_CURVE('',#19508,#19509,#1032,.T.);
#24662=EDGE_CURVE('',#19509,#19506,#10498,.T.);
#24663=EDGE_CURVE('',#19510,#19511,#15389,.T.);
#24664=EDGE_CURVE('',#19510,#19507,#1806,.T.);
#24665=EDGE_CURVE('',#19506,#19511,#10499,.T.);
#24666=EDGE_CURVE('',#19512,#19513,#15390,.T.);
#24667=EDGE_CURVE('',#19513,#19510,#15391,.T.);
#24668=EDGE_CURVE('',#19511,#19512,#15392,.T.);
#24669=EDGE_CURVE('',#19514,#19515,#15393,.T.);
#24670=EDGE_CURVE('',#19515,#19450,#15394,.T.);
#24671=EDGE_CURVE('',#19450,#19516,#10500,.T.);
#24672=EDGE_CURVE('',#19517,#19516,#15395,.T.);
#24673=EDGE_CURVE('',#19517,#19518,#15396,.T.);
#24674=EDGE_CURVE('',#19518,#19514,#10501,.T.);
#24675=EDGE_CURVE('',#19516,#19513,#10502,.T.);
#24676=EDGE_CURVE('',#19512,#19517,#1807,.T.);
#24677=EDGE_CURVE('',#17307,#19449,#1033,.T.);
#24678=EDGE_CURVE('',#19519,#19520,#15397,.T.);
#24679=EDGE_CURVE('',#19519,#19515,#1808,.T.);
#24680=EDGE_CURVE('',#19514,#19520,#10503,.T.);
#24681=EDGE_CURVE('',#19521,#19522,#15398,.T.);
#24682=EDGE_CURVE('',#19522,#19519,#15399,.T.);
#24683=EDGE_CURVE('',#19520,#19521,#15400,.T.);
#24684=EDGE_CURVE('',#19523,#19524,#15401,.T.);
#24685=EDGE_CURVE('',#19524,#19459,#15402,.T.);
#24686=EDGE_CURVE('',#19459,#19525,#10504,.T.);
#24687=EDGE_CURVE('',#19526,#19525,#15403,.T.);
#24688=EDGE_CURVE('',#19526,#19527,#15404,.T.);
#24689=EDGE_CURVE('',#19527,#19523,#10505,.T.);
#24690=EDGE_CURVE('',#19525,#19522,#10506,.T.);
#24691=EDGE_CURVE('',#19521,#19526,#1809,.T.);
#24692=EDGE_CURVE('',#19528,#19529,#15405,.T.);
#24693=EDGE_CURVE('',#19528,#19524,#1810,.T.);
#24694=EDGE_CURVE('',#19523,#19529,#10507,.T.);
#24695=EDGE_CURVE('',#19530,#19531,#15406,.T.);
#24696=EDGE_CURVE('',#19531,#19528,#15407,.T.);
#24697=EDGE_CURVE('',#19529,#19530,#15408,.T.);
#24698=EDGE_CURVE('',#19532,#19533,#1811,.T.);
#24699=EDGE_CURVE('',#19533,#19468,#1812,.T.);
#24700=EDGE_CURVE('',#19468,#19534,#10508,.T.);
#24701=EDGE_CURVE('',#19535,#19534,#15409,.T.);
#24702=EDGE_CURVE('',#19535,#19536,#15410,.T.);
#24703=EDGE_CURVE('',#19536,#19532,#10509,.T.);
#24704=EDGE_CURVE('',#19534,#19531,#10510,.T.);
#24705=EDGE_CURVE('',#19530,#19535,#1813,.T.);
#24706=EDGE_CURVE('',#19537,#19538,#1814,.T.);
#24707=EDGE_CURVE('',#19537,#19533,#1815,.T.);
#24708=EDGE_CURVE('',#19532,#19538,#10511,.T.);
#24709=EDGE_CURVE('',#19539,#19540,#15411,.T.);
#24710=EDGE_CURVE('',#19540,#19537,#1816,.T.);
#24711=EDGE_CURVE('',#19538,#19539,#15412,.T.);
#24712=EDGE_CURVE('',#19541,#19542,#15413,.T.);
#24713=EDGE_CURVE('',#19542,#19477,#15414,.T.);
#24714=EDGE_CURVE('',#19477,#19543,#10512,.T.);
#24715=EDGE_CURVE('',#19544,#19543,#15415,.T.);
#24716=EDGE_CURVE('',#19544,#19545,#15416,.T.);
#24717=EDGE_CURVE('',#19545,#19541,#10513,.T.);
#24718=EDGE_CURVE('',#19543,#19540,#10514,.T.);
#24719=EDGE_CURVE('',#19539,#19544,#1817,.T.);
#24720=EDGE_CURVE('',#19546,#19547,#15417,.T.);
#24721=EDGE_CURVE('',#19546,#19542,#1818,.T.);
#24722=EDGE_CURVE('',#19541,#19547,#10515,.T.);
#24723=EDGE_CURVE('',#19548,#19549,#15418,.T.);
#24724=EDGE_CURVE('',#19549,#19546,#15419,.T.);
#24725=EDGE_CURVE('',#19547,#19548,#15420,.T.);
#24726=EDGE_CURVE('',#19550,#19551,#15421,.T.);
#24727=EDGE_CURVE('',#19551,#19486,#15422,.T.);
#24728=EDGE_CURVE('',#19486,#19552,#10516,.T.);
#24729=EDGE_CURVE('',#19553,#19552,#15423,.T.);
#24730=EDGE_CURVE('',#19553,#19554,#15424,.T.);
#24731=EDGE_CURVE('',#19554,#19550,#10517,.T.);
#24732=EDGE_CURVE('',#19552,#19549,#10518,.T.);
#24733=EDGE_CURVE('',#19548,#19553,#1819,.T.);
#24734=EDGE_CURVE('',#19555,#19556,#15425,.T.);
#24735=EDGE_CURVE('',#19555,#19551,#1820,.T.);
#24736=EDGE_CURVE('',#19550,#19556,#10519,.T.);
#24737=EDGE_CURVE('',#19557,#19558,#15426,.T.);
#24738=EDGE_CURVE('',#19558,#19555,#15427,.T.);
#24739=EDGE_CURVE('',#19556,#19557,#15428,.T.);
#24740=EDGE_CURVE('',#19559,#19560,#15429,.T.);
#24741=EDGE_CURVE('',#19560,#19495,#15430,.T.);
#24742=EDGE_CURVE('',#19495,#19561,#10520,.T.);
#24743=EDGE_CURVE('',#19562,#19561,#15431,.T.);
#24744=EDGE_CURVE('',#19562,#19563,#15432,.T.);
#24745=EDGE_CURVE('',#19563,#19559,#10521,.F.);
#24746=EDGE_CURVE('',#19561,#19558,#10522,.T.);
#24747=EDGE_CURVE('',#19557,#19562,#1821,.T.);
#24748=EDGE_CURVE('',#17450,#19560,#15433,.T.);
#24749=EDGE_CURVE('',#19559,#17451,#10523,.F.);
#24750=EDGE_CURVE('',#17447,#19504,#1034,.T.);
#24751=EDGE_CURVE('',#19504,#19564,#10524,.T.);
#24752=EDGE_CURVE('',#17448,#19564,#1035,.T.);
#24753=EDGE_CURVE('',#19564,#17449,#1036,.T.);
#24754=EDGE_CURVE('',#19565,#19566,#15434,.T.);
#24755=EDGE_CURVE('',#19566,#17301,#15435,.T.);
#24756=EDGE_CURVE('',#19567,#17300,#1822,.T.);
#24757=EDGE_CURVE('',#19567,#19568,#1037,.T.);
#24758=EDGE_CURVE('',#19568,#19565,#10525,.T.);
#24759=EDGE_CURVE('',#19569,#19570,#15436,.T.);
#24760=EDGE_CURVE('',#19569,#19566,#1823,.T.);
#24761=EDGE_CURVE('',#19565,#19570,#10526,.T.);
#24762=EDGE_CURVE('',#19571,#19572,#15437,.T.);
#24763=EDGE_CURVE('',#19572,#19569,#15438,.T.);
#24764=EDGE_CURVE('',#19570,#19571,#15439,.T.);
#24765=EDGE_CURVE('',#19573,#19574,#15440,.T.);
#24766=EDGE_CURVE('',#19574,#19509,#15441,.T.);
#24767=EDGE_CURVE('',#19509,#19575,#10527,.T.);
#24768=EDGE_CURVE('',#19576,#19575,#15442,.T.);
#24769=EDGE_CURVE('',#19576,#19577,#15443,.T.);
#24770=EDGE_CURVE('',#19577,#19573,#10528,.T.);
#24771=EDGE_CURVE('',#19575,#19572,#10529,.T.);
#24772=EDGE_CURVE('',#19571,#19576,#1824,.T.);
#24773=EDGE_CURVE('',#17303,#19508,#1038,.T.);
#24774=EDGE_CURVE('',#19578,#19579,#15444,.T.);
#24775=EDGE_CURVE('',#19578,#19574,#1825,.T.);
#24776=EDGE_CURVE('',#19573,#19579,#10530,.T.);
#24777=EDGE_CURVE('',#19580,#19581,#15445,.T.);
#24778=EDGE_CURVE('',#19581,#19578,#15446,.T.);
#24779=EDGE_CURVE('',#19579,#19580,#15447,.T.);
#24780=EDGE_CURVE('',#19582,#19583,#15448,.T.);
#24781=EDGE_CURVE('',#19583,#19518,#15449,.T.);
#24782=EDGE_CURVE('',#19518,#19584,#10531,.T.);
#24783=EDGE_CURVE('',#19585,#19584,#15450,.T.);
#24784=EDGE_CURVE('',#19585,#19586,#15451,.T.);
#24785=EDGE_CURVE('',#19586,#19582,#10532,.T.);
#24786=EDGE_CURVE('',#19584,#19581,#10533,.T.);
#24787=EDGE_CURVE('',#19580,#19585,#1826,.T.);
#24788=EDGE_CURVE('',#19587,#19588,#15452,.T.);
#24789=EDGE_CURVE('',#19587,#19583,#1827,.T.);
#24790=EDGE_CURVE('',#19582,#19588,#10534,.T.);
#24791=EDGE_CURVE('',#19589,#19590,#15453,.T.);
#24792=EDGE_CURVE('',#19590,#19587,#15454,.T.);
#24793=EDGE_CURVE('',#19588,#19589,#15455,.T.);
#24794=EDGE_CURVE('',#19591,#19592,#1828,.T.);
#24795=EDGE_CURVE('',#19592,#19527,#1829,.T.);
#24796=EDGE_CURVE('',#19527,#19593,#10535,.T.);
#24797=EDGE_CURVE('',#19594,#19593,#15456,.T.);
#24798=EDGE_CURVE('',#19594,#19595,#15457,.T.);
#24799=EDGE_CURVE('',#19595,#19591,#10536,.T.);
#24800=EDGE_CURVE('',#19593,#19590,#10537,.T.);
#24801=EDGE_CURVE('',#19589,#19594,#1830,.T.);
#24802=EDGE_CURVE('',#19596,#19597,#1831,.T.);
#24803=EDGE_CURVE('',#19596,#19592,#1832,.T.);
#24804=EDGE_CURVE('',#19591,#19597,#10538,.T.);
#24805=EDGE_CURVE('',#19598,#19599,#15458,.T.);
#24806=EDGE_CURVE('',#19599,#19596,#1833,.T.);
#24807=EDGE_CURVE('',#19597,#19598,#15459,.T.);
#24808=EDGE_CURVE('',#19600,#19601,#15460,.T.);
#24809=EDGE_CURVE('',#19601,#19536,#15461,.T.);
#24810=EDGE_CURVE('',#19536,#19602,#10539,.T.);
#24811=EDGE_CURVE('',#19603,#19602,#15462,.T.);
#24812=EDGE_CURVE('',#19603,#19604,#15463,.T.);
#24813=EDGE_CURVE('',#19604,#19600,#10540,.T.);
#24814=EDGE_CURVE('',#19602,#19599,#10541,.T.);
#24815=EDGE_CURVE('',#19598,#19603,#1834,.T.);
#24816=EDGE_CURVE('',#19605,#19606,#15464,.T.);
#24817=EDGE_CURVE('',#19605,#19601,#1835,.T.);
#24818=EDGE_CURVE('',#19600,#19606,#10542,.T.);
#24819=EDGE_CURVE('',#19607,#19608,#15465,.T.);
#24820=EDGE_CURVE('',#19608,#19605,#15466,.T.);
#24821=EDGE_CURVE('',#19606,#19607,#15467,.T.);
#24822=EDGE_CURVE('',#19609,#19610,#15468,.T.);
#24823=EDGE_CURVE('',#19610,#19545,#15469,.T.);
#24824=EDGE_CURVE('',#19545,#19611,#10543,.T.);
#24825=EDGE_CURVE('',#19612,#19611,#15470,.T.);
#24826=EDGE_CURVE('',#19612,#19613,#15471,.T.);
#24827=EDGE_CURVE('',#19613,#19609,#10544,.T.);
#24828=EDGE_CURVE('',#19611,#19608,#10545,.T.);
#24829=EDGE_CURVE('',#19607,#19612,#1836,.T.);
#24830=EDGE_CURVE('',#19614,#19615,#15472,.T.);
#24831=EDGE_CURVE('',#19614,#19610,#1837,.T.);
#24832=EDGE_CURVE('',#19609,#19615,#10546,.T.);
#24833=EDGE_CURVE('',#19616,#19617,#15473,.T.);
#24834=EDGE_CURVE('',#19617,#19614,#15474,.T.);
#24835=EDGE_CURVE('',#19615,#19616,#15475,.T.);
#24836=EDGE_CURVE('',#19618,#19619,#15476,.T.);
#24837=EDGE_CURVE('',#19619,#19554,#15477,.T.);
#24838=EDGE_CURVE('',#19554,#19620,#10547,.T.);
#24839=EDGE_CURVE('',#19621,#19620,#15478,.T.);
#24840=EDGE_CURVE('',#19621,#19622,#15479,.T.);
#24841=EDGE_CURVE('',#19622,#19618,#10548,.F.);
#24842=EDGE_CURVE('',#19620,#19617,#10549,.T.);
#24843=EDGE_CURVE('',#19616,#19621,#1838,.T.);
#24844=EDGE_CURVE('',#17456,#19619,#15480,.T.);
#24845=EDGE_CURVE('',#19618,#17457,#10550,.F.);
#24846=EDGE_CURVE('',#17453,#19563,#1039,.T.);
#24847=EDGE_CURVE('',#19563,#19623,#10551,.T.);
#24848=EDGE_CURVE('',#17454,#19623,#1040,.T.);
#24849=EDGE_CURVE('',#19623,#17455,#1041,.T.);
#24850=EDGE_CURVE('',#19624,#19625,#15481,.T.);
#24851=EDGE_CURVE('',#19625,#17297,#15482,.T.);
#24852=EDGE_CURVE('',#19626,#17296,#1839,.T.);
#24853=EDGE_CURVE('',#19626,#19627,#1042,.T.);
#24854=EDGE_CURVE('',#19627,#19624,#10552,.T.);
#24855=EDGE_CURVE('',#19628,#19629,#15483,.T.);
#24856=EDGE_CURVE('',#19628,#19625,#1840,.T.);
#24857=EDGE_CURVE('',#19624,#19629,#10553,.T.);
#24858=EDGE_CURVE('',#19630,#19631,#15484,.T.);
#24859=EDGE_CURVE('',#19631,#19628,#15485,.T.);
#24860=EDGE_CURVE('',#19629,#19630,#15486,.T.);
#24861=EDGE_CURVE('',#19632,#19633,#15487,.T.);
#24862=EDGE_CURVE('',#19633,#19568,#15488,.T.);
#24863=EDGE_CURVE('',#19568,#19634,#10554,.T.);
#24864=EDGE_CURVE('',#19635,#19634,#15489,.T.);
#24865=EDGE_CURVE('',#19635,#19636,#15490,.T.);
#24866=EDGE_CURVE('',#19636,#19632,#10555,.T.);
#24867=EDGE_CURVE('',#19634,#19631,#10556,.T.);
#24868=EDGE_CURVE('',#19630,#19635,#1841,.T.);
#24869=EDGE_CURVE('',#17299,#19567,#1043,.T.);
#24870=EDGE_CURVE('',#19637,#19638,#15491,.T.);
#24871=EDGE_CURVE('',#19637,#19633,#1842,.T.);
#24872=EDGE_CURVE('',#19632,#19638,#10557,.T.);
#24873=EDGE_CURVE('',#19639,#19640,#15492,.T.);
#24874=EDGE_CURVE('',#19640,#19637,#15493,.T.);
#24875=EDGE_CURVE('',#19638,#19639,#15494,.T.);
#24876=EDGE_CURVE('',#19641,#19642,#15495,.T.);
#24877=EDGE_CURVE('',#19642,#19577,#15496,.T.);
#24878=EDGE_CURVE('',#19577,#19643,#10558,.T.);
#24879=EDGE_CURVE('',#19644,#19643,#15497,.T.);
#24880=EDGE_CURVE('',#19644,#19645,#15498,.T.);
#24881=EDGE_CURVE('',#19645,#19641,#10559,.T.);
#24882=EDGE_CURVE('',#19643,#19640,#10560,.T.);
#24883=EDGE_CURVE('',#19639,#19644,#1843,.T.);
#24884=EDGE_CURVE('',#19646,#19647,#15499,.T.);
#24885=EDGE_CURVE('',#19646,#19642,#1844,.T.);
#24886=EDGE_CURVE('',#19641,#19647,#10561,.T.);
#24887=EDGE_CURVE('',#19648,#19649,#15500,.T.);
#24888=EDGE_CURVE('',#19649,#19646,#15501,.T.);
#24889=EDGE_CURVE('',#19647,#19648,#15502,.T.);
#24890=EDGE_CURVE('',#19650,#19651,#1845,.T.);
#24891=EDGE_CURVE('',#19651,#19586,#1846,.T.);
#24892=EDGE_CURVE('',#19586,#19652,#10562,.T.);
#24893=EDGE_CURVE('',#19653,#19652,#15503,.T.);
#24894=EDGE_CURVE('',#19653,#19654,#15504,.T.);
#24895=EDGE_CURVE('',#19654,#19650,#10563,.T.);
#24896=EDGE_CURVE('',#19652,#19649,#10564,.T.);
#24897=EDGE_CURVE('',#19648,#19653,#1847,.T.);
#24898=EDGE_CURVE('',#19655,#19656,#1848,.T.);
#24899=EDGE_CURVE('',#19655,#19651,#1849,.T.);
#24900=EDGE_CURVE('',#19650,#19656,#10565,.T.);
#24901=EDGE_CURVE('',#19657,#19658,#15505,.T.);
#24902=EDGE_CURVE('',#19658,#19655,#1850,.T.);
#24903=EDGE_CURVE('',#19656,#19657,#15506,.T.);
#24904=EDGE_CURVE('',#19659,#19660,#15507,.T.);
#24905=EDGE_CURVE('',#19660,#19595,#15508,.T.);
#24906=EDGE_CURVE('',#19595,#19661,#10566,.T.);
#24907=EDGE_CURVE('',#19662,#19661,#15509,.T.);
#24908=EDGE_CURVE('',#19662,#19663,#15510,.T.);
#24909=EDGE_CURVE('',#19663,#19659,#10567,.T.);
#24910=EDGE_CURVE('',#19661,#19658,#10568,.T.);
#24911=EDGE_CURVE('',#19657,#19662,#1851,.T.);
#24912=EDGE_CURVE('',#19664,#19665,#15511,.T.);
#24913=EDGE_CURVE('',#19664,#19660,#1852,.T.);
#24914=EDGE_CURVE('',#19659,#19665,#10569,.T.);
#24915=EDGE_CURVE('',#19666,#19667,#15512,.T.);
#24916=EDGE_CURVE('',#19667,#19664,#15513,.T.);
#24917=EDGE_CURVE('',#19665,#19666,#15514,.T.);
#24918=EDGE_CURVE('',#19668,#19669,#15515,.T.);
#24919=EDGE_CURVE('',#19669,#19604,#15516,.T.);
#24920=EDGE_CURVE('',#19604,#19670,#10570,.T.);
#24921=EDGE_CURVE('',#19671,#19670,#15517,.T.);
#24922=EDGE_CURVE('',#19671,#19672,#15518,.T.);
#24923=EDGE_CURVE('',#19672,#19668,#10571,.T.);
#24924=EDGE_CURVE('',#19670,#19667,#10572,.T.);
#24925=EDGE_CURVE('',#19666,#19671,#1853,.T.);
#24926=EDGE_CURVE('',#19673,#19674,#15519,.T.);
#24927=EDGE_CURVE('',#19673,#19669,#1854,.T.);
#24928=EDGE_CURVE('',#19668,#19674,#10573,.T.);
#24929=EDGE_CURVE('',#19675,#19676,#15520,.T.);
#24930=EDGE_CURVE('',#19676,#19673,#15521,.T.);
#24931=EDGE_CURVE('',#19674,#19675,#15522,.T.);
#24932=EDGE_CURVE('',#19677,#19678,#15523,.T.);
#24933=EDGE_CURVE('',#19678,#19613,#15524,.T.);
#24934=EDGE_CURVE('',#19613,#19679,#10574,.T.);
#24935=EDGE_CURVE('',#19680,#19679,#15525,.T.);
#24936=EDGE_CURVE('',#19680,#19681,#15526,.T.);
#24937=EDGE_CURVE('',#19681,#19677,#10575,.F.);
#24938=EDGE_CURVE('',#19679,#19676,#10576,.T.);
#24939=EDGE_CURVE('',#19675,#19680,#1855,.T.);
#24940=EDGE_CURVE('',#17462,#19678,#15527,.T.);
#24941=EDGE_CURVE('',#19677,#17463,#10577,.F.);
#24942=EDGE_CURVE('',#17459,#19622,#1044,.T.);
#24943=EDGE_CURVE('',#19622,#19682,#10578,.T.);
#24944=EDGE_CURVE('',#17460,#19682,#1045,.T.);
#24945=EDGE_CURVE('',#19682,#17461,#1046,.T.);
#24946=EDGE_CURVE('',#19683,#19684,#15528,.T.);
#24947=EDGE_CURVE('',#19684,#17293,#15529,.T.);
#24948=EDGE_CURVE('',#19685,#17292,#1856,.T.);
#24949=EDGE_CURVE('',#19685,#19686,#1047,.T.);
#24950=EDGE_CURVE('',#19686,#19683,#10579,.T.);
#24951=EDGE_CURVE('',#19687,#19688,#15530,.T.);
#24952=EDGE_CURVE('',#19687,#19684,#1857,.T.);
#24953=EDGE_CURVE('',#19683,#19688,#10580,.T.);
#24954=EDGE_CURVE('',#19689,#19690,#15531,.T.);
#24955=EDGE_CURVE('',#19690,#19687,#15532,.T.);
#24956=EDGE_CURVE('',#19688,#19689,#15533,.T.);
#24957=EDGE_CURVE('',#19691,#19692,#15534,.T.);
#24958=EDGE_CURVE('',#19692,#19627,#15535,.T.);
#24959=EDGE_CURVE('',#19627,#19693,#10581,.T.);
#24960=EDGE_CURVE('',#19694,#19693,#15536,.T.);
#24961=EDGE_CURVE('',#19694,#19695,#15537,.T.);
#24962=EDGE_CURVE('',#19695,#19691,#10582,.T.);
#24963=EDGE_CURVE('',#19693,#19690,#10583,.T.);
#24964=EDGE_CURVE('',#19689,#19694,#1858,.T.);
#24965=EDGE_CURVE('',#17295,#19626,#1048,.T.);
#24966=EDGE_CURVE('',#19696,#19697,#15538,.T.);
#24967=EDGE_CURVE('',#19696,#19692,#1859,.T.);
#24968=EDGE_CURVE('',#19691,#19697,#10584,.T.);
#24969=EDGE_CURVE('',#19698,#19699,#15539,.T.);
#24970=EDGE_CURVE('',#19699,#19696,#15540,.T.);
#24971=EDGE_CURVE('',#19697,#19698,#15541,.T.);
#24972=EDGE_CURVE('',#19700,#19701,#15542,.T.);
#24973=EDGE_CURVE('',#19701,#19636,#15543,.T.);
#24974=EDGE_CURVE('',#19636,#19702,#10585,.T.);
#24975=EDGE_CURVE('',#19703,#19702,#15544,.T.);
#24976=EDGE_CURVE('',#19703,#19704,#15545,.T.);
#24977=EDGE_CURVE('',#19704,#19700,#10586,.T.);
#24978=EDGE_CURVE('',#19702,#19699,#10587,.T.);
#24979=EDGE_CURVE('',#19698,#19703,#1860,.T.);
#24980=EDGE_CURVE('',#19705,#19706,#15546,.T.);
#24981=EDGE_CURVE('',#19705,#19701,#1861,.T.);
#24982=EDGE_CURVE('',#19700,#19706,#10588,.T.);
#24983=EDGE_CURVE('',#19707,#19708,#15547,.T.);
#24984=EDGE_CURVE('',#19708,#19705,#15548,.T.);
#24985=EDGE_CURVE('',#19706,#19707,#15549,.T.);
#24986=EDGE_CURVE('',#19709,#19710,#1862,.T.);
#24987=EDGE_CURVE('',#19710,#19645,#1863,.T.);
#24988=EDGE_CURVE('',#19645,#19711,#10589,.T.);
#24989=EDGE_CURVE('',#19712,#19711,#15550,.T.);
#24990=EDGE_CURVE('',#19712,#19713,#15551,.T.);
#24991=EDGE_CURVE('',#19713,#19709,#10590,.T.);
#24992=EDGE_CURVE('',#19711,#19708,#10591,.T.);
#24993=EDGE_CURVE('',#19707,#19712,#1864,.T.);
#24994=EDGE_CURVE('',#19714,#19715,#1865,.T.);
#24995=EDGE_CURVE('',#19714,#19710,#1866,.T.);
#24996=EDGE_CURVE('',#19709,#19715,#10592,.T.);
#24997=EDGE_CURVE('',#19716,#19717,#15552,.T.);
#24998=EDGE_CURVE('',#19717,#19714,#1867,.T.);
#24999=EDGE_CURVE('',#19715,#19716,#15553,.T.);
#25000=EDGE_CURVE('',#19718,#19719,#15554,.T.);
#25001=EDGE_CURVE('',#19719,#19654,#15555,.T.);
#25002=EDGE_CURVE('',#19654,#19720,#10593,.T.);
#25003=EDGE_CURVE('',#19721,#19720,#15556,.T.);
#25004=EDGE_CURVE('',#19721,#19722,#15557,.T.);
#25005=EDGE_CURVE('',#19722,#19718,#10594,.T.);
#25006=EDGE_CURVE('',#19720,#19717,#10595,.T.);
#25007=EDGE_CURVE('',#19716,#19721,#1868,.T.);
#25008=EDGE_CURVE('',#19723,#19724,#15558,.T.);
#25009=EDGE_CURVE('',#19723,#19719,#1869,.T.);
#25010=EDGE_CURVE('',#19718,#19724,#10596,.T.);
#25011=EDGE_CURVE('',#19725,#19726,#15559,.T.);
#25012=EDGE_CURVE('',#19726,#19723,#15560,.T.);
#25013=EDGE_CURVE('',#19724,#19725,#15561,.T.);
#25014=EDGE_CURVE('',#19727,#19728,#15562,.T.);
#25015=EDGE_CURVE('',#19728,#19663,#15563,.T.);
#25016=EDGE_CURVE('',#19663,#19729,#10597,.T.);
#25017=EDGE_CURVE('',#19730,#19729,#15564,.T.);
#25018=EDGE_CURVE('',#19730,#19731,#15565,.T.);
#25019=EDGE_CURVE('',#19731,#19727,#10598,.T.);
#25020=EDGE_CURVE('',#19729,#19726,#10599,.T.);
#25021=EDGE_CURVE('',#19725,#19730,#1870,.T.);
#25022=EDGE_CURVE('',#19732,#19733,#15566,.T.);
#25023=EDGE_CURVE('',#19732,#19728,#1871,.T.);
#25024=EDGE_CURVE('',#19727,#19733,#10600,.T.);
#25025=EDGE_CURVE('',#19734,#19735,#15567,.T.);
#25026=EDGE_CURVE('',#19735,#19732,#15568,.T.);
#25027=EDGE_CURVE('',#19733,#19734,#15569,.T.);
#25028=EDGE_CURVE('',#19736,#19737,#15570,.T.);
#25029=EDGE_CURVE('',#19737,#19672,#15571,.T.);
#25030=EDGE_CURVE('',#19672,#19738,#10601,.T.);
#25031=EDGE_CURVE('',#19739,#19738,#15572,.T.);
#25032=EDGE_CURVE('',#19739,#19740,#15573,.T.);
#25033=EDGE_CURVE('',#19740,#19736,#10602,.F.);
#25034=EDGE_CURVE('',#19738,#19735,#10603,.T.);
#25035=EDGE_CURVE('',#19734,#19739,#1872,.T.);
#25036=EDGE_CURVE('',#17468,#19737,#15574,.T.);
#25037=EDGE_CURVE('',#19736,#17469,#10604,.F.);
#25038=EDGE_CURVE('',#17465,#19681,#1049,.T.);
#25039=EDGE_CURVE('',#19681,#19741,#10605,.T.);
#25040=EDGE_CURVE('',#17466,#19741,#1050,.T.);
#25041=EDGE_CURVE('',#19741,#17467,#1051,.T.);
#25042=EDGE_CURVE('',#19742,#19743,#15575,.T.);
#25043=EDGE_CURVE('',#19743,#17289,#15576,.T.);
#25044=EDGE_CURVE('',#19744,#17288,#1873,.T.);
#25045=EDGE_CURVE('',#19744,#19745,#1052,.T.);
#25046=EDGE_CURVE('',#19745,#19742,#10606,.T.);
#25047=EDGE_CURVE('',#19746,#19747,#15577,.T.);
#25048=EDGE_CURVE('',#19746,#19743,#1874,.T.);
#25049=EDGE_CURVE('',#19742,#19747,#10607,.T.);
#25050=EDGE_CURVE('',#19748,#19749,#15578,.T.);
#25051=EDGE_CURVE('',#19749,#19746,#15579,.T.);
#25052=EDGE_CURVE('',#19747,#19748,#15580,.T.);
#25053=EDGE_CURVE('',#19750,#19751,#15581,.T.);
#25054=EDGE_CURVE('',#19751,#19686,#15582,.T.);
#25055=EDGE_CURVE('',#19686,#19752,#10608,.T.);
#25056=EDGE_CURVE('',#19753,#19752,#15583,.T.);
#25057=EDGE_CURVE('',#19753,#19754,#15584,.T.);
#25058=EDGE_CURVE('',#19754,#19750,#10609,.T.);
#25059=EDGE_CURVE('',#19752,#19749,#10610,.T.);
#25060=EDGE_CURVE('',#19748,#19753,#1875,.T.);
#25061=EDGE_CURVE('',#17291,#19685,#1053,.T.);
#25062=EDGE_CURVE('',#19755,#19756,#15585,.T.);
#25063=EDGE_CURVE('',#19755,#19751,#1876,.T.);
#25064=EDGE_CURVE('',#19750,#19756,#10611,.T.);
#25065=EDGE_CURVE('',#19757,#19758,#15586,.T.);
#25066=EDGE_CURVE('',#19758,#19755,#15587,.T.);
#25067=EDGE_CURVE('',#19756,#19757,#15588,.T.);
#25068=EDGE_CURVE('',#19759,#19760,#15589,.T.);
#25069=EDGE_CURVE('',#19760,#19695,#15590,.T.);
#25070=EDGE_CURVE('',#19695,#19761,#10612,.T.);
#25071=EDGE_CURVE('',#19762,#19761,#15591,.T.);
#25072=EDGE_CURVE('',#19762,#19763,#15592,.T.);
#25073=EDGE_CURVE('',#19763,#19759,#10613,.T.);
#25074=EDGE_CURVE('',#19761,#19758,#10614,.T.);
#25075=EDGE_CURVE('',#19757,#19762,#1877,.T.);
#25076=EDGE_CURVE('',#19764,#19765,#15593,.T.);
#25077=EDGE_CURVE('',#19764,#19760,#1878,.T.);
#25078=EDGE_CURVE('',#19759,#19765,#10615,.T.);
#25079=EDGE_CURVE('',#19766,#19767,#15594,.T.);
#25080=EDGE_CURVE('',#19767,#19764,#15595,.T.);
#25081=EDGE_CURVE('',#19765,#19766,#15596,.T.);
#25082=EDGE_CURVE('',#19768,#19769,#1879,.T.);
#25083=EDGE_CURVE('',#19769,#19704,#1880,.T.);
#25084=EDGE_CURVE('',#19704,#19770,#10616,.T.);
#25085=EDGE_CURVE('',#19771,#19770,#15597,.T.);
#25086=EDGE_CURVE('',#19771,#19772,#15598,.T.);
#25087=EDGE_CURVE('',#19772,#19768,#10617,.T.);
#25088=EDGE_CURVE('',#19770,#19767,#10618,.T.);
#25089=EDGE_CURVE('',#19766,#19771,#1881,.T.);
#25090=EDGE_CURVE('',#19773,#19774,#1882,.T.);
#25091=EDGE_CURVE('',#19773,#19769,#1883,.T.);
#25092=EDGE_CURVE('',#19768,#19774,#10619,.T.);
#25093=EDGE_CURVE('',#19775,#19776,#15599,.T.);
#25094=EDGE_CURVE('',#19776,#19773,#1884,.T.);
#25095=EDGE_CURVE('',#19774,#19775,#15600,.T.);
#25096=EDGE_CURVE('',#19777,#19778,#15601,.T.);
#25097=EDGE_CURVE('',#19778,#19713,#15602,.T.);
#25098=EDGE_CURVE('',#19713,#19779,#10620,.T.);
#25099=EDGE_CURVE('',#19780,#19779,#15603,.T.);
#25100=EDGE_CURVE('',#19780,#19781,#15604,.T.);
#25101=EDGE_CURVE('',#19781,#19777,#10621,.T.);
#25102=EDGE_CURVE('',#19779,#19776,#10622,.T.);
#25103=EDGE_CURVE('',#19775,#19780,#1885,.T.);
#25104=EDGE_CURVE('',#19782,#19783,#15605,.T.);
#25105=EDGE_CURVE('',#19782,#19778,#1886,.T.);
#25106=EDGE_CURVE('',#19777,#19783,#10623,.T.);
#25107=EDGE_CURVE('',#19784,#19785,#15606,.T.);
#25108=EDGE_CURVE('',#19785,#19782,#15607,.T.);
#25109=EDGE_CURVE('',#19783,#19784,#15608,.T.);
#25110=EDGE_CURVE('',#19786,#19787,#15609,.T.);
#25111=EDGE_CURVE('',#19787,#19722,#15610,.T.);
#25112=EDGE_CURVE('',#19722,#19788,#10624,.T.);
#25113=EDGE_CURVE('',#19789,#19788,#15611,.T.);
#25114=EDGE_CURVE('',#19789,#19790,#15612,.T.);
#25115=EDGE_CURVE('',#19790,#19786,#10625,.T.);
#25116=EDGE_CURVE('',#19788,#19785,#10626,.T.);
#25117=EDGE_CURVE('',#19784,#19789,#1887,.T.);
#25118=EDGE_CURVE('',#19791,#19792,#15613,.T.);
#25119=EDGE_CURVE('',#19791,#19787,#1888,.T.);
#25120=EDGE_CURVE('',#19786,#19792,#10627,.T.);
#25121=EDGE_CURVE('',#19793,#19794,#15614,.T.);
#25122=EDGE_CURVE('',#19794,#19791,#15615,.T.);
#25123=EDGE_CURVE('',#19792,#19793,#15616,.T.);
#25124=EDGE_CURVE('',#19795,#19796,#15617,.T.);
#25125=EDGE_CURVE('',#19796,#19731,#15618,.T.);
#25126=EDGE_CURVE('',#19731,#19797,#10628,.T.);
#25127=EDGE_CURVE('',#19798,#19797,#15619,.T.);
#25128=EDGE_CURVE('',#19798,#19799,#15620,.T.);
#25129=EDGE_CURVE('',#19799,#19795,#10629,.F.);
#25130=EDGE_CURVE('',#19797,#19794,#10630,.T.);
#25131=EDGE_CURVE('',#19793,#19798,#1889,.T.);
#25132=EDGE_CURVE('',#17474,#19796,#15621,.T.);
#25133=EDGE_CURVE('',#19795,#17475,#10631,.F.);
#25134=EDGE_CURVE('',#17471,#19740,#1054,.T.);
#25135=EDGE_CURVE('',#19740,#19800,#10632,.T.);
#25136=EDGE_CURVE('',#17472,#19800,#1055,.T.);
#25137=EDGE_CURVE('',#19800,#17473,#1056,.T.);
#25138=EDGE_CURVE('',#19801,#19802,#15622,.T.);
#25139=EDGE_CURVE('',#19802,#17285,#15623,.T.);
#25140=EDGE_CURVE('',#19803,#17284,#1890,.T.);
#25141=EDGE_CURVE('',#19803,#19804,#1057,.T.);
#25142=EDGE_CURVE('',#19804,#19801,#10633,.T.);
#25143=EDGE_CURVE('',#19805,#19806,#15624,.T.);
#25144=EDGE_CURVE('',#19805,#19802,#1891,.T.);
#25145=EDGE_CURVE('',#19801,#19806,#10634,.T.);
#25146=EDGE_CURVE('',#19807,#19808,#15625,.T.);
#25147=EDGE_CURVE('',#19808,#19805,#15626,.T.);
#25148=EDGE_CURVE('',#19806,#19807,#15627,.T.);
#25149=EDGE_CURVE('',#19809,#19810,#15628,.T.);
#25150=EDGE_CURVE('',#19810,#19745,#15629,.T.);
#25151=EDGE_CURVE('',#19745,#19811,#10635,.T.);
#25152=EDGE_CURVE('',#19812,#19811,#15630,.T.);
#25153=EDGE_CURVE('',#19812,#19813,#15631,.T.);
#25154=EDGE_CURVE('',#19813,#19809,#10636,.T.);
#25155=EDGE_CURVE('',#19811,#19808,#10637,.T.);
#25156=EDGE_CURVE('',#19807,#19812,#1892,.T.);
#25157=EDGE_CURVE('',#17287,#19744,#1058,.T.);
#25158=EDGE_CURVE('',#19814,#19815,#15632,.T.);
#25159=EDGE_CURVE('',#19814,#19810,#1893,.T.);
#25160=EDGE_CURVE('',#19809,#19815,#10638,.T.);
#25161=EDGE_CURVE('',#19816,#19817,#15633,.T.);
#25162=EDGE_CURVE('',#19817,#19814,#15634,.T.);
#25163=EDGE_CURVE('',#19815,#19816,#15635,.T.);
#25164=EDGE_CURVE('',#19818,#19819,#15636,.T.);
#25165=EDGE_CURVE('',#19819,#19754,#15637,.T.);
#25166=EDGE_CURVE('',#19754,#19820,#10639,.T.);
#25167=EDGE_CURVE('',#19821,#19820,#15638,.T.);
#25168=EDGE_CURVE('',#19821,#19822,#15639,.T.);
#25169=EDGE_CURVE('',#19822,#19818,#10640,.T.);
#25170=EDGE_CURVE('',#19820,#19817,#10641,.T.);
#25171=EDGE_CURVE('',#19816,#19821,#1894,.T.);
#25172=EDGE_CURVE('',#19823,#19824,#15640,.T.);
#25173=EDGE_CURVE('',#19823,#19819,#1895,.T.);
#25174=EDGE_CURVE('',#19818,#19824,#10642,.T.);
#25175=EDGE_CURVE('',#19825,#19826,#15641,.T.);
#25176=EDGE_CURVE('',#19826,#19823,#15642,.T.);
#25177=EDGE_CURVE('',#19824,#19825,#15643,.T.);
#25178=EDGE_CURVE('',#19827,#19828,#1896,.T.);
#25179=EDGE_CURVE('',#19828,#19763,#1897,.T.);
#25180=EDGE_CURVE('',#19763,#19829,#10643,.T.);
#25181=EDGE_CURVE('',#19830,#19829,#15644,.T.);
#25182=EDGE_CURVE('',#19830,#19831,#15645,.T.);
#25183=EDGE_CURVE('',#19831,#19827,#10644,.T.);
#25184=EDGE_CURVE('',#19829,#19826,#10645,.T.);
#25185=EDGE_CURVE('',#19825,#19830,#1898,.T.);
#25186=EDGE_CURVE('',#19832,#19833,#1899,.T.);
#25187=EDGE_CURVE('',#19832,#19828,#1900,.T.);
#25188=EDGE_CURVE('',#19827,#19833,#10646,.T.);
#25189=EDGE_CURVE('',#19834,#19835,#15646,.T.);
#25190=EDGE_CURVE('',#19835,#19832,#1901,.T.);
#25191=EDGE_CURVE('',#19833,#19834,#15647,.T.);
#25192=EDGE_CURVE('',#19836,#19837,#15648,.T.);
#25193=EDGE_CURVE('',#19837,#19772,#15649,.T.);
#25194=EDGE_CURVE('',#19772,#19838,#10647,.T.);
#25195=EDGE_CURVE('',#19839,#19838,#15650,.T.);
#25196=EDGE_CURVE('',#19839,#19840,#15651,.T.);
#25197=EDGE_CURVE('',#19840,#19836,#10648,.T.);
#25198=EDGE_CURVE('',#19838,#19835,#10649,.T.);
#25199=EDGE_CURVE('',#19834,#19839,#1902,.T.);
#25200=EDGE_CURVE('',#19841,#19842,#15652,.T.);
#25201=EDGE_CURVE('',#19841,#19837,#1903,.T.);
#25202=EDGE_CURVE('',#19836,#19842,#10650,.T.);
#25203=EDGE_CURVE('',#19843,#19844,#15653,.T.);
#25204=EDGE_CURVE('',#19844,#19841,#15654,.T.);
#25205=EDGE_CURVE('',#19842,#19843,#15655,.T.);
#25206=EDGE_CURVE('',#19845,#19846,#15656,.T.);
#25207=EDGE_CURVE('',#19846,#19781,#15657,.T.);
#25208=EDGE_CURVE('',#19781,#19847,#10651,.T.);
#25209=EDGE_CURVE('',#19848,#19847,#15658,.T.);
#25210=EDGE_CURVE('',#19848,#19849,#15659,.T.);
#25211=EDGE_CURVE('',#19849,#19845,#10652,.T.);
#25212=EDGE_CURVE('',#19847,#19844,#10653,.T.);
#25213=EDGE_CURVE('',#19843,#19848,#1904,.T.);
#25214=EDGE_CURVE('',#19850,#19851,#15660,.T.);
#25215=EDGE_CURVE('',#19850,#19846,#1905,.T.);
#25216=EDGE_CURVE('',#19845,#19851,#10654,.T.);
#25217=EDGE_CURVE('',#19852,#19853,#15661,.T.);
#25218=EDGE_CURVE('',#19853,#19850,#15662,.T.);
#25219=EDGE_CURVE('',#19851,#19852,#15663,.T.);
#25220=EDGE_CURVE('',#19854,#19855,#15664,.T.);
#25221=EDGE_CURVE('',#19855,#19790,#15665,.T.);
#25222=EDGE_CURVE('',#19790,#19856,#10655,.T.);
#25223=EDGE_CURVE('',#19857,#19856,#15666,.T.);
#25224=EDGE_CURVE('',#19857,#19858,#15667,.T.);
#25225=EDGE_CURVE('',#19858,#19854,#10656,.F.);
#25226=EDGE_CURVE('',#19856,#19853,#10657,.T.);
#25227=EDGE_CURVE('',#19852,#19857,#1906,.T.);
#25228=EDGE_CURVE('',#17480,#19855,#15668,.T.);
#25229=EDGE_CURVE('',#19854,#17481,#10658,.F.);
#25230=EDGE_CURVE('',#17477,#19799,#1059,.T.);
#25231=EDGE_CURVE('',#19799,#19859,#10659,.T.);
#25232=EDGE_CURVE('',#17478,#19859,#1060,.T.);
#25233=EDGE_CURVE('',#19859,#17479,#1061,.T.);
#25234=EDGE_CURVE('',#19860,#19861,#15669,.T.);
#25235=EDGE_CURVE('',#19861,#17281,#15670,.T.);
#25236=EDGE_CURVE('',#19862,#17280,#1907,.T.);
#25237=EDGE_CURVE('',#19862,#19863,#1062,.T.);
#25238=EDGE_CURVE('',#19863,#19860,#10660,.T.);
#25239=EDGE_CURVE('',#19864,#19865,#15671,.T.);
#25240=EDGE_CURVE('',#19864,#19861,#1908,.T.);
#25241=EDGE_CURVE('',#19860,#19865,#10661,.T.);
#25242=EDGE_CURVE('',#19866,#19867,#15672,.T.);
#25243=EDGE_CURVE('',#19867,#19864,#15673,.T.);
#25244=EDGE_CURVE('',#19865,#19866,#15674,.T.);
#25245=EDGE_CURVE('',#19868,#19869,#15675,.T.);
#25246=EDGE_CURVE('',#19869,#19804,#15676,.T.);
#25247=EDGE_CURVE('',#19804,#19870,#10662,.T.);
#25248=EDGE_CURVE('',#19871,#19870,#15677,.T.);
#25249=EDGE_CURVE('',#19871,#19872,#15678,.T.);
#25250=EDGE_CURVE('',#19872,#19868,#10663,.T.);
#25251=EDGE_CURVE('',#19870,#19867,#10664,.T.);
#25252=EDGE_CURVE('',#19866,#19871,#1909,.T.);
#25253=EDGE_CURVE('',#17283,#19803,#1063,.T.);
#25254=EDGE_CURVE('',#19873,#19874,#15679,.T.);
#25255=EDGE_CURVE('',#19873,#19869,#1910,.T.);
#25256=EDGE_CURVE('',#19868,#19874,#10665,.T.);
#25257=EDGE_CURVE('',#19875,#19876,#15680,.T.);
#25258=EDGE_CURVE('',#19876,#19873,#15681,.T.);
#25259=EDGE_CURVE('',#19874,#19875,#15682,.T.);
#25260=EDGE_CURVE('',#19877,#19878,#15683,.T.);
#25261=EDGE_CURVE('',#19878,#19813,#15684,.T.);
#25262=EDGE_CURVE('',#19813,#19879,#10666,.T.);
#25263=EDGE_CURVE('',#19880,#19879,#15685,.T.);
#25264=EDGE_CURVE('',#19880,#19881,#15686,.T.);
#25265=EDGE_CURVE('',#19881,#19877,#10667,.T.);
#25266=EDGE_CURVE('',#19879,#19876,#10668,.T.);
#25267=EDGE_CURVE('',#19875,#19880,#1911,.T.);
#25268=EDGE_CURVE('',#19882,#19883,#15687,.T.);
#25269=EDGE_CURVE('',#19882,#19878,#1912,.T.);
#25270=EDGE_CURVE('',#19877,#19883,#10669,.T.);
#25271=EDGE_CURVE('',#19884,#19885,#15688,.T.);
#25272=EDGE_CURVE('',#19885,#19882,#15689,.T.);
#25273=EDGE_CURVE('',#19883,#19884,#15690,.T.);
#25274=EDGE_CURVE('',#19886,#19887,#1913,.T.);
#25275=EDGE_CURVE('',#19887,#19822,#1914,.T.);
#25276=EDGE_CURVE('',#19822,#19888,#10670,.T.);
#25277=EDGE_CURVE('',#19889,#19888,#15691,.T.);
#25278=EDGE_CURVE('',#19889,#19890,#15692,.T.);
#25279=EDGE_CURVE('',#19890,#19886,#10671,.T.);
#25280=EDGE_CURVE('',#19888,#19885,#10672,.T.);
#25281=EDGE_CURVE('',#19884,#19889,#1915,.T.);
#25282=EDGE_CURVE('',#19891,#19892,#1916,.T.);
#25283=EDGE_CURVE('',#19891,#19887,#1917,.T.);
#25284=EDGE_CURVE('',#19886,#19892,#10673,.T.);
#25285=EDGE_CURVE('',#19893,#19894,#15693,.T.);
#25286=EDGE_CURVE('',#19894,#19891,#1918,.T.);
#25287=EDGE_CURVE('',#19892,#19893,#15694,.T.);
#25288=EDGE_CURVE('',#19895,#19896,#15695,.T.);
#25289=EDGE_CURVE('',#19896,#19831,#15696,.T.);
#25290=EDGE_CURVE('',#19831,#19897,#10674,.T.);
#25291=EDGE_CURVE('',#19898,#19897,#15697,.T.);
#25292=EDGE_CURVE('',#19898,#19899,#15698,.T.);
#25293=EDGE_CURVE('',#19899,#19895,#10675,.T.);
#25294=EDGE_CURVE('',#19897,#19894,#10676,.T.);
#25295=EDGE_CURVE('',#19893,#19898,#1919,.T.);
#25296=EDGE_CURVE('',#19900,#19901,#15699,.T.);
#25297=EDGE_CURVE('',#19900,#19896,#1920,.T.);
#25298=EDGE_CURVE('',#19895,#19901,#10677,.T.);
#25299=EDGE_CURVE('',#19902,#19903,#15700,.T.);
#25300=EDGE_CURVE('',#19903,#19900,#15701,.T.);
#25301=EDGE_CURVE('',#19901,#19902,#15702,.T.);
#25302=EDGE_CURVE('',#19904,#19905,#15703,.T.);
#25303=EDGE_CURVE('',#19905,#19840,#15704,.T.);
#25304=EDGE_CURVE('',#19840,#19906,#10678,.T.);
#25305=EDGE_CURVE('',#19907,#19906,#15705,.T.);
#25306=EDGE_CURVE('',#19907,#19908,#15706,.T.);
#25307=EDGE_CURVE('',#19908,#19904,#10679,.T.);
#25308=EDGE_CURVE('',#19906,#19903,#10680,.T.);
#25309=EDGE_CURVE('',#19902,#19907,#1921,.T.);
#25310=EDGE_CURVE('',#19909,#19910,#15707,.T.);
#25311=EDGE_CURVE('',#19909,#19905,#1922,.T.);
#25312=EDGE_CURVE('',#19904,#19910,#10681,.T.);
#25313=EDGE_CURVE('',#19911,#19912,#15708,.T.);
#25314=EDGE_CURVE('',#19912,#19909,#15709,.T.);
#25315=EDGE_CURVE('',#19910,#19911,#15710,.T.);
#25316=EDGE_CURVE('',#19913,#19914,#15711,.T.);
#25317=EDGE_CURVE('',#19914,#19849,#15712,.T.);
#25318=EDGE_CURVE('',#19849,#19915,#10682,.T.);
#25319=EDGE_CURVE('',#19916,#19915,#15713,.T.);
#25320=EDGE_CURVE('',#19916,#19917,#15714,.T.);
#25321=EDGE_CURVE('',#19917,#19913,#10683,.F.);
#25322=EDGE_CURVE('',#19915,#19912,#10684,.T.);
#25323=EDGE_CURVE('',#19911,#19916,#1923,.T.);
#25324=EDGE_CURVE('',#17486,#19914,#15715,.T.);
#25325=EDGE_CURVE('',#19913,#17487,#10685,.F.);
#25326=EDGE_CURVE('',#17483,#19858,#1064,.T.);
#25327=EDGE_CURVE('',#19858,#19918,#10686,.T.);
#25328=EDGE_CURVE('',#17484,#19918,#1065,.T.);
#25329=EDGE_CURVE('',#19918,#17485,#1066,.T.);
#25330=EDGE_CURVE('',#19919,#19920,#15716,.T.);
#25331=EDGE_CURVE('',#19920,#17277,#15717,.T.);
#25332=EDGE_CURVE('',#19921,#17276,#1924,.T.);
#25333=EDGE_CURVE('',#19921,#19922,#1067,.T.);
#25334=EDGE_CURVE('',#19922,#19919,#10687,.T.);
#25335=EDGE_CURVE('',#19923,#19924,#15718,.T.);
#25336=EDGE_CURVE('',#19923,#19920,#1925,.T.);
#25337=EDGE_CURVE('',#19919,#19924,#10688,.T.);
#25338=EDGE_CURVE('',#19925,#19926,#15719,.T.);
#25339=EDGE_CURVE('',#19926,#19923,#15720,.T.);
#25340=EDGE_CURVE('',#19924,#19925,#15721,.T.);
#25341=EDGE_CURVE('',#19927,#19928,#15722,.T.);
#25342=EDGE_CURVE('',#19928,#19863,#15723,.T.);
#25343=EDGE_CURVE('',#19863,#19929,#10689,.T.);
#25344=EDGE_CURVE('',#19930,#19929,#15724,.T.);
#25345=EDGE_CURVE('',#19930,#19931,#15725,.T.);
#25346=EDGE_CURVE('',#19931,#19927,#10690,.T.);
#25347=EDGE_CURVE('',#19929,#19926,#10691,.T.);
#25348=EDGE_CURVE('',#19925,#19930,#1926,.T.);
#25349=EDGE_CURVE('',#17279,#19862,#1068,.T.);
#25350=EDGE_CURVE('',#19932,#19933,#15726,.T.);
#25351=EDGE_CURVE('',#19932,#19928,#1927,.T.);
#25352=EDGE_CURVE('',#19927,#19933,#10692,.T.);
#25353=EDGE_CURVE('',#19934,#19935,#15727,.T.);
#25354=EDGE_CURVE('',#19935,#19932,#15728,.T.);
#25355=EDGE_CURVE('',#19933,#19934,#15729,.T.);
#25356=EDGE_CURVE('',#19936,#19937,#15730,.T.);
#25357=EDGE_CURVE('',#19937,#19872,#15731,.T.);
#25358=EDGE_CURVE('',#19872,#19938,#10693,.T.);
#25359=EDGE_CURVE('',#19939,#19938,#15732,.T.);
#25360=EDGE_CURVE('',#19939,#19940,#15733,.T.);
#25361=EDGE_CURVE('',#19940,#19936,#10694,.T.);
#25362=EDGE_CURVE('',#19938,#19935,#10695,.T.);
#25363=EDGE_CURVE('',#19934,#19939,#1928,.T.);
#25364=EDGE_CURVE('',#19941,#19942,#15734,.T.);
#25365=EDGE_CURVE('',#19941,#19937,#1929,.T.);
#25366=EDGE_CURVE('',#19936,#19942,#10696,.T.);
#25367=EDGE_CURVE('',#19943,#19944,#15735,.T.);
#25368=EDGE_CURVE('',#19944,#19941,#15736,.T.);
#25369=EDGE_CURVE('',#19942,#19943,#15737,.T.);
#25370=EDGE_CURVE('',#19945,#19946,#1930,.T.);
#25371=EDGE_CURVE('',#19946,#19881,#1931,.T.);
#25372=EDGE_CURVE('',#19881,#19947,#10697,.T.);
#25373=EDGE_CURVE('',#19948,#19947,#15738,.T.);
#25374=EDGE_CURVE('',#19948,#19949,#15739,.T.);
#25375=EDGE_CURVE('',#19949,#19945,#10698,.T.);
#25376=EDGE_CURVE('',#19947,#19944,#10699,.T.);
#25377=EDGE_CURVE('',#19943,#19948,#1932,.T.);
#25378=EDGE_CURVE('',#19950,#19951,#1933,.T.);
#25379=EDGE_CURVE('',#19950,#19946,#1934,.T.);
#25380=EDGE_CURVE('',#19945,#19951,#10700,.T.);
#25381=EDGE_CURVE('',#19952,#19953,#15740,.T.);
#25382=EDGE_CURVE('',#19953,#19950,#1935,.T.);
#25383=EDGE_CURVE('',#19951,#19952,#15741,.T.);
#25384=EDGE_CURVE('',#19954,#19955,#15742,.T.);
#25385=EDGE_CURVE('',#19955,#19890,#15743,.T.);
#25386=EDGE_CURVE('',#19890,#19956,#10701,.T.);
#25387=EDGE_CURVE('',#19957,#19956,#15744,.T.);
#25388=EDGE_CURVE('',#19957,#19958,#15745,.T.);
#25389=EDGE_CURVE('',#19958,#19954,#10702,.T.);
#25390=EDGE_CURVE('',#19956,#19953,#10703,.T.);
#25391=EDGE_CURVE('',#19952,#19957,#1936,.T.);
#25392=EDGE_CURVE('',#19959,#19960,#15746,.T.);
#25393=EDGE_CURVE('',#19959,#19955,#1937,.T.);
#25394=EDGE_CURVE('',#19954,#19960,#10704,.T.);
#25395=EDGE_CURVE('',#19961,#19962,#15747,.T.);
#25396=EDGE_CURVE('',#19962,#19959,#15748,.T.);
#25397=EDGE_CURVE('',#19960,#19961,#15749,.T.);
#25398=EDGE_CURVE('',#19963,#19964,#15750,.T.);
#25399=EDGE_CURVE('',#19964,#19899,#15751,.T.);
#25400=EDGE_CURVE('',#19899,#19965,#10705,.T.);
#25401=EDGE_CURVE('',#19966,#19965,#15752,.T.);
#25402=EDGE_CURVE('',#19966,#19967,#15753,.T.);
#25403=EDGE_CURVE('',#19967,#19963,#10706,.T.);
#25404=EDGE_CURVE('',#19965,#19962,#10707,.T.);
#25405=EDGE_CURVE('',#19961,#19966,#1938,.T.);
#25406=EDGE_CURVE('',#19968,#19969,#15754,.T.);
#25407=EDGE_CURVE('',#19968,#19964,#1939,.T.);
#25408=EDGE_CURVE('',#19963,#19969,#10708,.T.);
#25409=EDGE_CURVE('',#19970,#19971,#15755,.T.);
#25410=EDGE_CURVE('',#19971,#19968,#15756,.T.);
#25411=EDGE_CURVE('',#19969,#19970,#15757,.T.);
#25412=EDGE_CURVE('',#19972,#19973,#15758,.T.);
#25413=EDGE_CURVE('',#19973,#19908,#15759,.T.);
#25414=EDGE_CURVE('',#19908,#19974,#10709,.T.);
#25415=EDGE_CURVE('',#19975,#19974,#15760,.T.);
#25416=EDGE_CURVE('',#19975,#19976,#15761,.T.);
#25417=EDGE_CURVE('',#19976,#19972,#10710,.F.);
#25418=EDGE_CURVE('',#19974,#19971,#10711,.T.);
#25419=EDGE_CURVE('',#19970,#19975,#1940,.T.);
#25420=EDGE_CURVE('',#17492,#19973,#15762,.T.);
#25421=EDGE_CURVE('',#19972,#17493,#10712,.F.);
#25422=EDGE_CURVE('',#17489,#19917,#1069,.T.);
#25423=EDGE_CURVE('',#19917,#19977,#10713,.T.);
#25424=EDGE_CURVE('',#17490,#19977,#1070,.T.);
#25425=EDGE_CURVE('',#19977,#17491,#1071,.T.);
#25426=EDGE_CURVE('',#19978,#19979,#15763,.T.);
#25427=EDGE_CURVE('',#19979,#17273,#15764,.T.);
#25428=EDGE_CURVE('',#19980,#17272,#1941,.T.);
#25429=EDGE_CURVE('',#19980,#19981,#1072,.T.);
#25430=EDGE_CURVE('',#19981,#19978,#10714,.T.);
#25431=EDGE_CURVE('',#19982,#19983,#15765,.T.);
#25432=EDGE_CURVE('',#19982,#19979,#1942,.T.);
#25433=EDGE_CURVE('',#19978,#19983,#10715,.T.);
#25434=EDGE_CURVE('',#19984,#19985,#15766,.T.);
#25435=EDGE_CURVE('',#19985,#19982,#15767,.T.);
#25436=EDGE_CURVE('',#19983,#19984,#15768,.T.);
#25437=EDGE_CURVE('',#19986,#19987,#15769,.T.);
#25438=EDGE_CURVE('',#19987,#19922,#15770,.T.);
#25439=EDGE_CURVE('',#19922,#19988,#10716,.T.);
#25440=EDGE_CURVE('',#19989,#19988,#15771,.T.);
#25441=EDGE_CURVE('',#19989,#19990,#15772,.T.);
#25442=EDGE_CURVE('',#19990,#19986,#10717,.T.);
#25443=EDGE_CURVE('',#19988,#19985,#10718,.T.);
#25444=EDGE_CURVE('',#19984,#19989,#1943,.T.);
#25445=EDGE_CURVE('',#17275,#19921,#1073,.T.);
#25446=EDGE_CURVE('',#19991,#19992,#15773,.T.);
#25447=EDGE_CURVE('',#19991,#19987,#1944,.T.);
#25448=EDGE_CURVE('',#19986,#19992,#10719,.T.);
#25449=EDGE_CURVE('',#19993,#19994,#15774,.T.);
#25450=EDGE_CURVE('',#19994,#19991,#15775,.T.);
#25451=EDGE_CURVE('',#19992,#19993,#15776,.T.);
#25452=EDGE_CURVE('',#19995,#19996,#15777,.T.);
#25453=EDGE_CURVE('',#19996,#19931,#15778,.T.);
#25454=EDGE_CURVE('',#19931,#19997,#10720,.T.);
#25455=EDGE_CURVE('',#19998,#19997,#15779,.T.);
#25456=EDGE_CURVE('',#19998,#19999,#15780,.T.);
#25457=EDGE_CURVE('',#19999,#19995,#10721,.T.);
#25458=EDGE_CURVE('',#19997,#19994,#10722,.T.);
#25459=EDGE_CURVE('',#19993,#19998,#1945,.T.);
#25460=EDGE_CURVE('',#20000,#20001,#15781,.T.);
#25461=EDGE_CURVE('',#20000,#19996,#1946,.T.);
#25462=EDGE_CURVE('',#19995,#20001,#10723,.T.);
#25463=EDGE_CURVE('',#20002,#20003,#15782,.T.);
#25464=EDGE_CURVE('',#20003,#20000,#15783,.T.);
#25465=EDGE_CURVE('',#20001,#20002,#15784,.T.);
#25466=EDGE_CURVE('',#20004,#20005,#1947,.T.);
#25467=EDGE_CURVE('',#20005,#19940,#1948,.T.);
#25468=EDGE_CURVE('',#19940,#20006,#10724,.T.);
#25469=EDGE_CURVE('',#20007,#20006,#15785,.T.);
#25470=EDGE_CURVE('',#20007,#20008,#15786,.T.);
#25471=EDGE_CURVE('',#20008,#20004,#10725,.T.);
#25472=EDGE_CURVE('',#20006,#20003,#10726,.T.);
#25473=EDGE_CURVE('',#20002,#20007,#1949,.T.);
#25474=EDGE_CURVE('',#20009,#20010,#1950,.T.);
#25475=EDGE_CURVE('',#20009,#20005,#1951,.T.);
#25476=EDGE_CURVE('',#20004,#20010,#10727,.T.);
#25477=EDGE_CURVE('',#20011,#20012,#15787,.T.);
#25478=EDGE_CURVE('',#20012,#20009,#1952,.T.);
#25479=EDGE_CURVE('',#20010,#20011,#15788,.T.);
#25480=EDGE_CURVE('',#20013,#20014,#15789,.T.);
#25481=EDGE_CURVE('',#20014,#19949,#15790,.T.);
#25482=EDGE_CURVE('',#19949,#20015,#10728,.T.);
#25483=EDGE_CURVE('',#20016,#20015,#15791,.T.);
#25484=EDGE_CURVE('',#20016,#20017,#15792,.T.);
#25485=EDGE_CURVE('',#20017,#20013,#10729,.T.);
#25486=EDGE_CURVE('',#20015,#20012,#10730,.T.);
#25487=EDGE_CURVE('',#20011,#20016,#1953,.T.);
#25488=EDGE_CURVE('',#20018,#20019,#15793,.T.);
#25489=EDGE_CURVE('',#20018,#20014,#1954,.T.);
#25490=EDGE_CURVE('',#20013,#20019,#10731,.T.);
#25491=EDGE_CURVE('',#20020,#20021,#15794,.T.);
#25492=EDGE_CURVE('',#20021,#20018,#15795,.T.);
#25493=EDGE_CURVE('',#20019,#20020,#15796,.T.);
#25494=EDGE_CURVE('',#20022,#20023,#15797,.T.);
#25495=EDGE_CURVE('',#20023,#19958,#15798,.T.);
#25496=EDGE_CURVE('',#19958,#20024,#10732,.T.);
#25497=EDGE_CURVE('',#20025,#20024,#15799,.T.);
#25498=EDGE_CURVE('',#20025,#20026,#15800,.T.);
#25499=EDGE_CURVE('',#20026,#20022,#10733,.T.);
#25500=EDGE_CURVE('',#20024,#20021,#10734,.T.);
#25501=EDGE_CURVE('',#20020,#20025,#1955,.T.);
#25502=EDGE_CURVE('',#20027,#20028,#15801,.T.);
#25503=EDGE_CURVE('',#20027,#20023,#1956,.T.);
#25504=EDGE_CURVE('',#20022,#20028,#10735,.T.);
#25505=EDGE_CURVE('',#20029,#20030,#15802,.T.);
#25506=EDGE_CURVE('',#20030,#20027,#15803,.T.);
#25507=EDGE_CURVE('',#20028,#20029,#15804,.T.);
#25508=EDGE_CURVE('',#20031,#20032,#15805,.T.);
#25509=EDGE_CURVE('',#20032,#19967,#15806,.T.);
#25510=EDGE_CURVE('',#19967,#20033,#10736,.T.);
#25511=EDGE_CURVE('',#20034,#20033,#15807,.T.);
#25512=EDGE_CURVE('',#20034,#20035,#15808,.T.);
#25513=EDGE_CURVE('',#20035,#20031,#10737,.F.);
#25514=EDGE_CURVE('',#20033,#20030,#10738,.T.);
#25515=EDGE_CURVE('',#20029,#20034,#1957,.T.);
#25516=EDGE_CURVE('',#17498,#20032,#15809,.T.);
#25517=EDGE_CURVE('',#20031,#17499,#10739,.F.);
#25518=EDGE_CURVE('',#17495,#19976,#1074,.T.);
#25519=EDGE_CURVE('',#19976,#20036,#10740,.T.);
#25520=EDGE_CURVE('',#17496,#20036,#1075,.T.);
#25521=EDGE_CURVE('',#20036,#17497,#1076,.T.);
#25522=EDGE_CURVE('',#20037,#20038,#15810,.T.);
#25523=EDGE_CURVE('',#20038,#17269,#15811,.T.);
#25524=EDGE_CURVE('',#20039,#17268,#1958,.T.);
#25525=EDGE_CURVE('',#20039,#20040,#1077,.T.);
#25526=EDGE_CURVE('',#20040,#20037,#10741,.T.);
#25527=EDGE_CURVE('',#20041,#20042,#15812,.T.);
#25528=EDGE_CURVE('',#20041,#20038,#1959,.T.);
#25529=EDGE_CURVE('',#20037,#20042,#10742,.T.);
#25530=EDGE_CURVE('',#20043,#20044,#15813,.T.);
#25531=EDGE_CURVE('',#20044,#20041,#15814,.T.);
#25532=EDGE_CURVE('',#20042,#20043,#15815,.T.);
#25533=EDGE_CURVE('',#20045,#20046,#15816,.T.);
#25534=EDGE_CURVE('',#20046,#19981,#15817,.T.);
#25535=EDGE_CURVE('',#19981,#20047,#10743,.T.);
#25536=EDGE_CURVE('',#20048,#20047,#15818,.T.);
#25537=EDGE_CURVE('',#20048,#20049,#15819,.T.);
#25538=EDGE_CURVE('',#20049,#20045,#10744,.T.);
#25539=EDGE_CURVE('',#20047,#20044,#10745,.T.);
#25540=EDGE_CURVE('',#20043,#20048,#1960,.T.);
#25541=EDGE_CURVE('',#17271,#19980,#1078,.T.);
#25542=EDGE_CURVE('',#20050,#20051,#15820,.T.);
#25543=EDGE_CURVE('',#20050,#20046,#1961,.T.);
#25544=EDGE_CURVE('',#20045,#20051,#10746,.T.);
#25545=EDGE_CURVE('',#20052,#20053,#15821,.T.);
#25546=EDGE_CURVE('',#20053,#20050,#15822,.T.);
#25547=EDGE_CURVE('',#20051,#20052,#15823,.T.);
#25548=EDGE_CURVE('',#20054,#20055,#15824,.T.);
#25549=EDGE_CURVE('',#20055,#19990,#15825,.T.);
#25550=EDGE_CURVE('',#19990,#20056,#10747,.T.);
#25551=EDGE_CURVE('',#20057,#20056,#15826,.T.);
#25552=EDGE_CURVE('',#20057,#20058,#15827,.T.);
#25553=EDGE_CURVE('',#20058,#20054,#10748,.T.);
#25554=EDGE_CURVE('',#20056,#20053,#10749,.T.);
#25555=EDGE_CURVE('',#20052,#20057,#1962,.T.);
#25556=EDGE_CURVE('',#20059,#20060,#15828,.T.);
#25557=EDGE_CURVE('',#20059,#20055,#1963,.T.);
#25558=EDGE_CURVE('',#20054,#20060,#10750,.T.);
#25559=EDGE_CURVE('',#20061,#20062,#15829,.T.);
#25560=EDGE_CURVE('',#20062,#20059,#15830,.T.);
#25561=EDGE_CURVE('',#20060,#20061,#15831,.T.);
#25562=EDGE_CURVE('',#20063,#20064,#1964,.T.);
#25563=EDGE_CURVE('',#20064,#19999,#1965,.T.);
#25564=EDGE_CURVE('',#19999,#20065,#10751,.T.);
#25565=EDGE_CURVE('',#20066,#20065,#15832,.T.);
#25566=EDGE_CURVE('',#20066,#20067,#15833,.T.);
#25567=EDGE_CURVE('',#20067,#20063,#10752,.T.);
#25568=EDGE_CURVE('',#20065,#20062,#10753,.T.);
#25569=EDGE_CURVE('',#20061,#20066,#1966,.T.);
#25570=EDGE_CURVE('',#20068,#20069,#1967,.T.);
#25571=EDGE_CURVE('',#20068,#20064,#1968,.T.);
#25572=EDGE_CURVE('',#20063,#20069,#10754,.T.);
#25573=EDGE_CURVE('',#20070,#20071,#15834,.T.);
#25574=EDGE_CURVE('',#20071,#20068,#1969,.T.);
#25575=EDGE_CURVE('',#20069,#20070,#15835,.T.);
#25576=EDGE_CURVE('',#20072,#20073,#15836,.T.);
#25577=EDGE_CURVE('',#20073,#20008,#15837,.T.);
#25578=EDGE_CURVE('',#20008,#20074,#10755,.T.);
#25579=EDGE_CURVE('',#20075,#20074,#15838,.T.);
#25580=EDGE_CURVE('',#20075,#20076,#15839,.T.);
#25581=EDGE_CURVE('',#20076,#20072,#10756,.T.);
#25582=EDGE_CURVE('',#20074,#20071,#10757,.T.);
#25583=EDGE_CURVE('',#20070,#20075,#1970,.T.);
#25584=EDGE_CURVE('',#20077,#20078,#15840,.T.);
#25585=EDGE_CURVE('',#20077,#20073,#1971,.T.);
#25586=EDGE_CURVE('',#20072,#20078,#10758,.T.);
#25587=EDGE_CURVE('',#20079,#20080,#15841,.T.);
#25588=EDGE_CURVE('',#20080,#20077,#15842,.T.);
#25589=EDGE_CURVE('',#20078,#20079,#15843,.T.);
#25590=EDGE_CURVE('',#20081,#20082,#15844,.T.);
#25591=EDGE_CURVE('',#20082,#20017,#15845,.T.);
#25592=EDGE_CURVE('',#20017,#20083,#10759,.T.);
#25593=EDGE_CURVE('',#20084,#20083,#15846,.T.);
#25594=EDGE_CURVE('',#20084,#20085,#15847,.T.);
#25595=EDGE_CURVE('',#20085,#20081,#10760,.T.);
#25596=EDGE_CURVE('',#20083,#20080,#10761,.T.);
#25597=EDGE_CURVE('',#20079,#20084,#1972,.T.);
#25598=EDGE_CURVE('',#20086,#20087,#15848,.T.);
#25599=EDGE_CURVE('',#20086,#20082,#1973,.T.);
#25600=EDGE_CURVE('',#20081,#20087,#10762,.T.);
#25601=EDGE_CURVE('',#20088,#20089,#15849,.T.);
#25602=EDGE_CURVE('',#20089,#20086,#15850,.T.);
#25603=EDGE_CURVE('',#20087,#20088,#15851,.T.);
#25604=EDGE_CURVE('',#20090,#20091,#15852,.T.);
#25605=EDGE_CURVE('',#20091,#20026,#15853,.T.);
#25606=EDGE_CURVE('',#20026,#20092,#10763,.T.);
#25607=EDGE_CURVE('',#20093,#20092,#15854,.T.);
#25608=EDGE_CURVE('',#20093,#20094,#15855,.T.);
#25609=EDGE_CURVE('',#20094,#20090,#10764,.F.);
#25610=EDGE_CURVE('',#20092,#20089,#10765,.T.);
#25611=EDGE_CURVE('',#20088,#20093,#1974,.T.);
#25612=EDGE_CURVE('',#17504,#20091,#15856,.T.);
#25613=EDGE_CURVE('',#20090,#17505,#10766,.F.);
#25614=EDGE_CURVE('',#17501,#20035,#1079,.T.);
#25615=EDGE_CURVE('',#20035,#20095,#10767,.T.);
#25616=EDGE_CURVE('',#17502,#20095,#1080,.T.);
#25617=EDGE_CURVE('',#20095,#17503,#1081,.T.);
#25618=EDGE_CURVE('',#20096,#20097,#15857,.T.);
#25619=EDGE_CURVE('',#20097,#17265,#15858,.T.);
#25620=EDGE_CURVE('',#20098,#17264,#1975,.T.);
#25621=EDGE_CURVE('',#20098,#20099,#1082,.T.);
#25622=EDGE_CURVE('',#20099,#20096,#10768,.T.);
#25623=EDGE_CURVE('',#20100,#20101,#15859,.T.);
#25624=EDGE_CURVE('',#20100,#20097,#1976,.T.);
#25625=EDGE_CURVE('',#20096,#20101,#10769,.T.);
#25626=EDGE_CURVE('',#20102,#20103,#15860,.T.);
#25627=EDGE_CURVE('',#20103,#20100,#15861,.T.);
#25628=EDGE_CURVE('',#20101,#20102,#15862,.T.);
#25629=EDGE_CURVE('',#20104,#20105,#15863,.T.);
#25630=EDGE_CURVE('',#20105,#20040,#15864,.T.);
#25631=EDGE_CURVE('',#20040,#20106,#10770,.T.);
#25632=EDGE_CURVE('',#20107,#20106,#15865,.T.);
#25633=EDGE_CURVE('',#20107,#20108,#15866,.T.);
#25634=EDGE_CURVE('',#20108,#20104,#10771,.T.);
#25635=EDGE_CURVE('',#20106,#20103,#10772,.T.);
#25636=EDGE_CURVE('',#20102,#20107,#1977,.T.);
#25637=EDGE_CURVE('',#17267,#20039,#1083,.T.);
#25638=EDGE_CURVE('',#20109,#20110,#15867,.T.);
#25639=EDGE_CURVE('',#20109,#20105,#1978,.T.);
#25640=EDGE_CURVE('',#20104,#20110,#10773,.T.);
#25641=EDGE_CURVE('',#20111,#20112,#15868,.T.);
#25642=EDGE_CURVE('',#20112,#20109,#15869,.T.);
#25643=EDGE_CURVE('',#20110,#20111,#15870,.T.);
#25644=EDGE_CURVE('',#20113,#20114,#15871,.T.);
#25645=EDGE_CURVE('',#20114,#20049,#15872,.T.);
#25646=EDGE_CURVE('',#20049,#20115,#10774,.T.);
#25647=EDGE_CURVE('',#20116,#20115,#15873,.T.);
#25648=EDGE_CURVE('',#20116,#20117,#15874,.T.);
#25649=EDGE_CURVE('',#20117,#20113,#10775,.T.);
#25650=EDGE_CURVE('',#20115,#20112,#10776,.T.);
#25651=EDGE_CURVE('',#20111,#20116,#1979,.T.);
#25652=EDGE_CURVE('',#20118,#20119,#15875,.T.);
#25653=EDGE_CURVE('',#20118,#20114,#1980,.T.);
#25654=EDGE_CURVE('',#20113,#20119,#10777,.T.);
#25655=EDGE_CURVE('',#20120,#20121,#15876,.T.);
#25656=EDGE_CURVE('',#20121,#20118,#15877,.T.);
#25657=EDGE_CURVE('',#20119,#20120,#15878,.T.);
#25658=EDGE_CURVE('',#20122,#20123,#1981,.T.);
#25659=EDGE_CURVE('',#20123,#20058,#1982,.T.);
#25660=EDGE_CURVE('',#20058,#20124,#10778,.T.);
#25661=EDGE_CURVE('',#20125,#20124,#15879,.T.);
#25662=EDGE_CURVE('',#20125,#20126,#15880,.T.);
#25663=EDGE_CURVE('',#20126,#20122,#10779,.T.);
#25664=EDGE_CURVE('',#20124,#20121,#10780,.T.);
#25665=EDGE_CURVE('',#20120,#20125,#1983,.T.);
#25666=EDGE_CURVE('',#20127,#20128,#1984,.T.);
#25667=EDGE_CURVE('',#20127,#20123,#1985,.T.);
#25668=EDGE_CURVE('',#20122,#20128,#10781,.T.);
#25669=EDGE_CURVE('',#20129,#20130,#15881,.T.);
#25670=EDGE_CURVE('',#20130,#20127,#1986,.T.);
#25671=EDGE_CURVE('',#20128,#20129,#15882,.T.);
#25672=EDGE_CURVE('',#20131,#20132,#15883,.T.);
#25673=EDGE_CURVE('',#20132,#20067,#15884,.T.);
#25674=EDGE_CURVE('',#20067,#20133,#10782,.T.);
#25675=EDGE_CURVE('',#20134,#20133,#15885,.T.);
#25676=EDGE_CURVE('',#20134,#20135,#15886,.T.);
#25677=EDGE_CURVE('',#20135,#20131,#10783,.T.);
#25678=EDGE_CURVE('',#20133,#20130,#10784,.T.);
#25679=EDGE_CURVE('',#20129,#20134,#1987,.T.);
#25680=EDGE_CURVE('',#20136,#20137,#15887,.T.);
#25681=EDGE_CURVE('',#20136,#20132,#1988,.T.);
#25682=EDGE_CURVE('',#20131,#20137,#10785,.T.);
#25683=EDGE_CURVE('',#20138,#20139,#15888,.T.);
#25684=EDGE_CURVE('',#20139,#20136,#15889,.T.);
#25685=EDGE_CURVE('',#20137,#20138,#15890,.T.);
#25686=EDGE_CURVE('',#20140,#20141,#15891,.T.);
#25687=EDGE_CURVE('',#20141,#20076,#15892,.T.);
#25688=EDGE_CURVE('',#20076,#20142,#10786,.T.);
#25689=EDGE_CURVE('',#20143,#20142,#15893,.T.);
#25690=EDGE_CURVE('',#20143,#20144,#15894,.T.);
#25691=EDGE_CURVE('',#20144,#20140,#10787,.T.);
#25692=EDGE_CURVE('',#20142,#20139,#10788,.T.);
#25693=EDGE_CURVE('',#20138,#20143,#1989,.T.);
#25694=EDGE_CURVE('',#20145,#20146,#15895,.T.);
#25695=EDGE_CURVE('',#20145,#20141,#1990,.T.);
#25696=EDGE_CURVE('',#20140,#20146,#10789,.T.);
#25697=EDGE_CURVE('',#20147,#20148,#15896,.T.);
#25698=EDGE_CURVE('',#20148,#20145,#15897,.T.);
#25699=EDGE_CURVE('',#20146,#20147,#15898,.T.);
#25700=EDGE_CURVE('',#20149,#20150,#15899,.T.);
#25701=EDGE_CURVE('',#20150,#20085,#15900,.T.);
#25702=EDGE_CURVE('',#20085,#20151,#10790,.T.);
#25703=EDGE_CURVE('',#20152,#20151,#15901,.T.);
#25704=EDGE_CURVE('',#20152,#20153,#15902,.T.);
#25705=EDGE_CURVE('',#20153,#20149,#10791,.F.);
#25706=EDGE_CURVE('',#20151,#20148,#10792,.T.);
#25707=EDGE_CURVE('',#20147,#20152,#1991,.T.);
#25708=EDGE_CURVE('',#17510,#20150,#15903,.T.);
#25709=EDGE_CURVE('',#20149,#17511,#10793,.F.);
#25710=EDGE_CURVE('',#17507,#20094,#1084,.T.);
#25711=EDGE_CURVE('',#20094,#20154,#10794,.T.);
#25712=EDGE_CURVE('',#17508,#20154,#1085,.T.);
#25713=EDGE_CURVE('',#20154,#17509,#1086,.T.);
#25714=EDGE_CURVE('',#20155,#20156,#15904,.T.);
#25715=EDGE_CURVE('',#20156,#17261,#15905,.T.);
#25716=EDGE_CURVE('',#20157,#17260,#1992,.T.);
#25717=EDGE_CURVE('',#20157,#20158,#1087,.T.);
#25718=EDGE_CURVE('',#20158,#20155,#10795,.T.);
#25719=EDGE_CURVE('',#20159,#20160,#15906,.T.);
#25720=EDGE_CURVE('',#20159,#20156,#1993,.T.);
#25721=EDGE_CURVE('',#20155,#20160,#10796,.T.);
#25722=EDGE_CURVE('',#20161,#20162,#15907,.T.);
#25723=EDGE_CURVE('',#20162,#20159,#15908,.T.);
#25724=EDGE_CURVE('',#20160,#20161,#15909,.T.);
#25725=EDGE_CURVE('',#20163,#20164,#15910,.T.);
#25726=EDGE_CURVE('',#20164,#20099,#15911,.T.);
#25727=EDGE_CURVE('',#20099,#20165,#10797,.T.);
#25728=EDGE_CURVE('',#20166,#20165,#15912,.T.);
#25729=EDGE_CURVE('',#20166,#20167,#15913,.T.);
#25730=EDGE_CURVE('',#20167,#20163,#10798,.T.);
#25731=EDGE_CURVE('',#20165,#20162,#10799,.T.);
#25732=EDGE_CURVE('',#20161,#20166,#1994,.T.);
#25733=EDGE_CURVE('',#17263,#20098,#1088,.T.);
#25734=EDGE_CURVE('',#20168,#20169,#15914,.T.);
#25735=EDGE_CURVE('',#20168,#20164,#1995,.T.);
#25736=EDGE_CURVE('',#20163,#20169,#10800,.T.);
#25737=EDGE_CURVE('',#20170,#20171,#15915,.T.);
#25738=EDGE_CURVE('',#20171,#20168,#15916,.T.);
#25739=EDGE_CURVE('',#20169,#20170,#15917,.T.);
#25740=EDGE_CURVE('',#20172,#20173,#15918,.T.);
#25741=EDGE_CURVE('',#20173,#20108,#15919,.T.);
#25742=EDGE_CURVE('',#20108,#20174,#10801,.T.);
#25743=EDGE_CURVE('',#20175,#20174,#15920,.T.);
#25744=EDGE_CURVE('',#20175,#20176,#15921,.T.);
#25745=EDGE_CURVE('',#20176,#20172,#10802,.T.);
#25746=EDGE_CURVE('',#20174,#20171,#10803,.T.);
#25747=EDGE_CURVE('',#20170,#20175,#1996,.T.);
#25748=EDGE_CURVE('',#20177,#20178,#15922,.T.);
#25749=EDGE_CURVE('',#20177,#20173,#1997,.T.);
#25750=EDGE_CURVE('',#20172,#20178,#10804,.T.);
#25751=EDGE_CURVE('',#20179,#20180,#15923,.T.);
#25752=EDGE_CURVE('',#20180,#20177,#15924,.T.);
#25753=EDGE_CURVE('',#20178,#20179,#15925,.T.);
#25754=EDGE_CURVE('',#20181,#20182,#1998,.T.);
#25755=EDGE_CURVE('',#20182,#20117,#1999,.T.);
#25756=EDGE_CURVE('',#20117,#20183,#10805,.T.);
#25757=EDGE_CURVE('',#20184,#20183,#15926,.T.);
#25758=EDGE_CURVE('',#20184,#20185,#15927,.T.);
#25759=EDGE_CURVE('',#20185,#20181,#10806,.T.);
#25760=EDGE_CURVE('',#20183,#20180,#10807,.T.);
#25761=EDGE_CURVE('',#20179,#20184,#2000,.T.);
#25762=EDGE_CURVE('',#20186,#20187,#2001,.T.);
#25763=EDGE_CURVE('',#20186,#20182,#2002,.T.);
#25764=EDGE_CURVE('',#20181,#20187,#10808,.T.);
#25765=EDGE_CURVE('',#20188,#20189,#15928,.T.);
#25766=EDGE_CURVE('',#20189,#20186,#2003,.T.);
#25767=EDGE_CURVE('',#20187,#20188,#15929,.T.);
#25768=EDGE_CURVE('',#20190,#20191,#15930,.T.);
#25769=EDGE_CURVE('',#20191,#20126,#15931,.T.);
#25770=EDGE_CURVE('',#20126,#20192,#10809,.T.);
#25771=EDGE_CURVE('',#20193,#20192,#15932,.T.);
#25772=EDGE_CURVE('',#20193,#20194,#15933,.T.);
#25773=EDGE_CURVE('',#20194,#20190,#10810,.T.);
#25774=EDGE_CURVE('',#20192,#20189,#10811,.T.);
#25775=EDGE_CURVE('',#20188,#20193,#2004,.T.);
#25776=EDGE_CURVE('',#20195,#20196,#15934,.T.);
#25777=EDGE_CURVE('',#20195,#20191,#2005,.T.);
#25778=EDGE_CURVE('',#20190,#20196,#10812,.T.);
#25779=EDGE_CURVE('',#20197,#20198,#15935,.T.);
#25780=EDGE_CURVE('',#20198,#20195,#15936,.T.);
#25781=EDGE_CURVE('',#20196,#20197,#15937,.T.);
#25782=EDGE_CURVE('',#20199,#20200,#15938,.T.);
#25783=EDGE_CURVE('',#20200,#20135,#15939,.T.);
#25784=EDGE_CURVE('',#20135,#20201,#10813,.T.);
#25785=EDGE_CURVE('',#20202,#20201,#15940,.T.);
#25786=EDGE_CURVE('',#20202,#20203,#15941,.T.);
#25787=EDGE_CURVE('',#20203,#20199,#10814,.T.);
#25788=EDGE_CURVE('',#20201,#20198,#10815,.T.);
#25789=EDGE_CURVE('',#20197,#20202,#2006,.T.);
#25790=EDGE_CURVE('',#20204,#20205,#15942,.T.);
#25791=EDGE_CURVE('',#20204,#20200,#2007,.T.);
#25792=EDGE_CURVE('',#20199,#20205,#10816,.T.);
#25793=EDGE_CURVE('',#20206,#20207,#15943,.T.);
#25794=EDGE_CURVE('',#20207,#20204,#15944,.T.);
#25795=EDGE_CURVE('',#20205,#20206,#15945,.T.);
#25796=EDGE_CURVE('',#20208,#20209,#15946,.T.);
#25797=EDGE_CURVE('',#20209,#20144,#15947,.T.);
#25798=EDGE_CURVE('',#20144,#20210,#10817,.T.);
#25799=EDGE_CURVE('',#20211,#20210,#15948,.T.);
#25800=EDGE_CURVE('',#20211,#20212,#15949,.T.);
#25801=EDGE_CURVE('',#20212,#20208,#10818,.F.);
#25802=EDGE_CURVE('',#20210,#20207,#10819,.T.);
#25803=EDGE_CURVE('',#20206,#20211,#2008,.T.);
#25804=EDGE_CURVE('',#17516,#20209,#15950,.T.);
#25805=EDGE_CURVE('',#20208,#17517,#10820,.F.);
#25806=EDGE_CURVE('',#17513,#20153,#1089,.T.);
#25807=EDGE_CURVE('',#20153,#20213,#10821,.T.);
#25808=EDGE_CURVE('',#17514,#20213,#1090,.T.);
#25809=EDGE_CURVE('',#20213,#17515,#1091,.T.);
#25810=EDGE_CURVE('',#20214,#20215,#15951,.T.);
#25811=EDGE_CURVE('',#20215,#17257,#15952,.T.);
#25812=EDGE_CURVE('',#20216,#17256,#2009,.T.);
#25813=EDGE_CURVE('',#20216,#20217,#1092,.T.);
#25814=EDGE_CURVE('',#20217,#20214,#10822,.T.);
#25815=EDGE_CURVE('',#20218,#20219,#15953,.T.);
#25816=EDGE_CURVE('',#20218,#20215,#2010,.T.);
#25817=EDGE_CURVE('',#20214,#20219,#10823,.T.);
#25818=EDGE_CURVE('',#20220,#20221,#15954,.T.);
#25819=EDGE_CURVE('',#20221,#20218,#15955,.T.);
#25820=EDGE_CURVE('',#20219,#20220,#15956,.T.);
#25821=EDGE_CURVE('',#20222,#20223,#15957,.T.);
#25822=EDGE_CURVE('',#20223,#20158,#15958,.T.);
#25823=EDGE_CURVE('',#20158,#20224,#10824,.T.);
#25824=EDGE_CURVE('',#20225,#20224,#15959,.T.);
#25825=EDGE_CURVE('',#20225,#20226,#15960,.T.);
#25826=EDGE_CURVE('',#20226,#20222,#10825,.T.);
#25827=EDGE_CURVE('',#20224,#20221,#10826,.T.);
#25828=EDGE_CURVE('',#20220,#20225,#2011,.T.);
#25829=EDGE_CURVE('',#17259,#20157,#1093,.T.);
#25830=EDGE_CURVE('',#20227,#20228,#15961,.T.);
#25831=EDGE_CURVE('',#20227,#20223,#2012,.T.);
#25832=EDGE_CURVE('',#20222,#20228,#10827,.T.);
#25833=EDGE_CURVE('',#20229,#20230,#15962,.T.);
#25834=EDGE_CURVE('',#20230,#20227,#15963,.T.);
#25835=EDGE_CURVE('',#20228,#20229,#15964,.T.);
#25836=EDGE_CURVE('',#20231,#20232,#15965,.T.);
#25837=EDGE_CURVE('',#20232,#20167,#15966,.T.);
#25838=EDGE_CURVE('',#20167,#20233,#10828,.T.);
#25839=EDGE_CURVE('',#20234,#20233,#15967,.T.);
#25840=EDGE_CURVE('',#20234,#20235,#15968,.T.);
#25841=EDGE_CURVE('',#20235,#20231,#10829,.T.);
#25842=EDGE_CURVE('',#20233,#20230,#10830,.T.);
#25843=EDGE_CURVE('',#20229,#20234,#2013,.T.);
#25844=EDGE_CURVE('',#20236,#20237,#15969,.T.);
#25845=EDGE_CURVE('',#20236,#20232,#2014,.T.);
#25846=EDGE_CURVE('',#20231,#20237,#10831,.T.);
#25847=EDGE_CURVE('',#20238,#20239,#15970,.T.);
#25848=EDGE_CURVE('',#20239,#20236,#15971,.T.);
#25849=EDGE_CURVE('',#20237,#20238,#15972,.T.);
#25850=EDGE_CURVE('',#20240,#20241,#2015,.T.);
#25851=EDGE_CURVE('',#20241,#20176,#2016,.T.);
#25852=EDGE_CURVE('',#20176,#20242,#10832,.T.);
#25853=EDGE_CURVE('',#20243,#20242,#15973,.T.);
#25854=EDGE_CURVE('',#20243,#20244,#15974,.T.);
#25855=EDGE_CURVE('',#20244,#20240,#10833,.T.);
#25856=EDGE_CURVE('',#20242,#20239,#10834,.T.);
#25857=EDGE_CURVE('',#20238,#20243,#2017,.T.);
#25858=EDGE_CURVE('',#20245,#20246,#2018,.T.);
#25859=EDGE_CURVE('',#20245,#20241,#2019,.T.);
#25860=EDGE_CURVE('',#20240,#20246,#10835,.T.);
#25861=EDGE_CURVE('',#20247,#20248,#15975,.T.);
#25862=EDGE_CURVE('',#20248,#20245,#2020,.T.);
#25863=EDGE_CURVE('',#20246,#20247,#15976,.T.);
#25864=EDGE_CURVE('',#20249,#20250,#15977,.T.);
#25865=EDGE_CURVE('',#20250,#20185,#15978,.T.);
#25866=EDGE_CURVE('',#20185,#20251,#10836,.T.);
#25867=EDGE_CURVE('',#20252,#20251,#15979,.T.);
#25868=EDGE_CURVE('',#20252,#20253,#15980,.T.);
#25869=EDGE_CURVE('',#20253,#20249,#10837,.T.);
#25870=EDGE_CURVE('',#20251,#20248,#10838,.T.);
#25871=EDGE_CURVE('',#20247,#20252,#2021,.T.);
#25872=EDGE_CURVE('',#20254,#20255,#15981,.T.);
#25873=EDGE_CURVE('',#20254,#20250,#2022,.T.);
#25874=EDGE_CURVE('',#20249,#20255,#10839,.T.);
#25875=EDGE_CURVE('',#20256,#20257,#15982,.T.);
#25876=EDGE_CURVE('',#20257,#20254,#15983,.T.);
#25877=EDGE_CURVE('',#20255,#20256,#15984,.T.);
#25878=EDGE_CURVE('',#20258,#20259,#15985,.T.);
#25879=EDGE_CURVE('',#20259,#20194,#15986,.T.);
#25880=EDGE_CURVE('',#20194,#20260,#10840,.T.);
#25881=EDGE_CURVE('',#20261,#20260,#15987,.T.);
#25882=EDGE_CURVE('',#20261,#20262,#15988,.T.);
#25883=EDGE_CURVE('',#20262,#20258,#10841,.T.);
#25884=EDGE_CURVE('',#20260,#20257,#10842,.T.);
#25885=EDGE_CURVE('',#20256,#20261,#2023,.T.);
#25886=EDGE_CURVE('',#20263,#20264,#15989,.T.);
#25887=EDGE_CURVE('',#20263,#20259,#2024,.T.);
#25888=EDGE_CURVE('',#20258,#20264,#10843,.T.);
#25889=EDGE_CURVE('',#20265,#20266,#15990,.T.);
#25890=EDGE_CURVE('',#20266,#20263,#15991,.T.);
#25891=EDGE_CURVE('',#20264,#20265,#15992,.T.);
#25892=EDGE_CURVE('',#20267,#20268,#15993,.T.);
#25893=EDGE_CURVE('',#20268,#20203,#15994,.T.);
#25894=EDGE_CURVE('',#20203,#20269,#10844,.T.);
#25895=EDGE_CURVE('',#20270,#20269,#15995,.T.);
#25896=EDGE_CURVE('',#20270,#20271,#15996,.T.);
#25897=EDGE_CURVE('',#20271,#20267,#10845,.F.);
#25898=EDGE_CURVE('',#20269,#20266,#10846,.T.);
#25899=EDGE_CURVE('',#20265,#20270,#2025,.T.);
#25900=EDGE_CURVE('',#17522,#20268,#15997,.T.);
#25901=EDGE_CURVE('',#20267,#17523,#10847,.F.);
#25902=EDGE_CURVE('',#17519,#20212,#1094,.T.);
#25903=EDGE_CURVE('',#20212,#20272,#10848,.T.);
#25904=EDGE_CURVE('',#17520,#20272,#1095,.T.);
#25905=EDGE_CURVE('',#20272,#17521,#1096,.T.);
#25906=EDGE_CURVE('',#20273,#20274,#15998,.T.);
#25907=EDGE_CURVE('',#20274,#17253,#15999,.T.);
#25908=EDGE_CURVE('',#20275,#17252,#2026,.T.);
#25909=EDGE_CURVE('',#20275,#20276,#1097,.T.);
#25910=EDGE_CURVE('',#20276,#20273,#10849,.T.);
#25911=EDGE_CURVE('',#20277,#20278,#16000,.T.);
#25912=EDGE_CURVE('',#20277,#20274,#2027,.T.);
#25913=EDGE_CURVE('',#20273,#20278,#10850,.T.);
#25914=EDGE_CURVE('',#20279,#20280,#16001,.T.);
#25915=EDGE_CURVE('',#20280,#20277,#16002,.T.);
#25916=EDGE_CURVE('',#20278,#20279,#16003,.T.);
#25917=EDGE_CURVE('',#20281,#20282,#16004,.T.);
#25918=EDGE_CURVE('',#20282,#20217,#16005,.T.);
#25919=EDGE_CURVE('',#20217,#20283,#10851,.T.);
#25920=EDGE_CURVE('',#20284,#20283,#16006,.T.);
#25921=EDGE_CURVE('',#20284,#20285,#16007,.T.);
#25922=EDGE_CURVE('',#20285,#20281,#10852,.T.);
#25923=EDGE_CURVE('',#20283,#20280,#10853,.T.);
#25924=EDGE_CURVE('',#20279,#20284,#2028,.T.);
#25925=EDGE_CURVE('',#17255,#20216,#1098,.T.);
#25926=EDGE_CURVE('',#20286,#20287,#16008,.T.);
#25927=EDGE_CURVE('',#20286,#20282,#2029,.T.);
#25928=EDGE_CURVE('',#20281,#20287,#10854,.T.);
#25929=EDGE_CURVE('',#20288,#20289,#16009,.T.);
#25930=EDGE_CURVE('',#20289,#20286,#16010,.T.);
#25931=EDGE_CURVE('',#20287,#20288,#16011,.T.);
#25932=EDGE_CURVE('',#20290,#20291,#16012,.T.);
#25933=EDGE_CURVE('',#20291,#20226,#16013,.T.);
#25934=EDGE_CURVE('',#20226,#20292,#10855,.T.);
#25935=EDGE_CURVE('',#20293,#20292,#16014,.T.);
#25936=EDGE_CURVE('',#20293,#20294,#16015,.T.);
#25937=EDGE_CURVE('',#20294,#20290,#10856,.T.);
#25938=EDGE_CURVE('',#20292,#20289,#10857,.T.);
#25939=EDGE_CURVE('',#20288,#20293,#2030,.T.);
#25940=EDGE_CURVE('',#20295,#20296,#16016,.T.);
#25941=EDGE_CURVE('',#20295,#20291,#2031,.T.);
#25942=EDGE_CURVE('',#20290,#20296,#10858,.T.);
#25943=EDGE_CURVE('',#20297,#20298,#16017,.T.);
#25944=EDGE_CURVE('',#20298,#20295,#16018,.T.);
#25945=EDGE_CURVE('',#20296,#20297,#16019,.T.);
#25946=EDGE_CURVE('',#20299,#20300,#2032,.T.);
#25947=EDGE_CURVE('',#20300,#20235,#2033,.T.);
#25948=EDGE_CURVE('',#20235,#20301,#10859,.T.);
#25949=EDGE_CURVE('',#20302,#20301,#16020,.T.);
#25950=EDGE_CURVE('',#20302,#20303,#16021,.T.);
#25951=EDGE_CURVE('',#20303,#20299,#10860,.T.);
#25952=EDGE_CURVE('',#20301,#20298,#10861,.T.);
#25953=EDGE_CURVE('',#20297,#20302,#2034,.T.);
#25954=EDGE_CURVE('',#20304,#20305,#2035,.T.);
#25955=EDGE_CURVE('',#20304,#20300,#2036,.T.);
#25956=EDGE_CURVE('',#20299,#20305,#10862,.T.);
#25957=EDGE_CURVE('',#20306,#20307,#16022,.T.);
#25958=EDGE_CURVE('',#20307,#20304,#2037,.T.);
#25959=EDGE_CURVE('',#20305,#20306,#16023,.T.);
#25960=EDGE_CURVE('',#20308,#20309,#16024,.T.);
#25961=EDGE_CURVE('',#20309,#20244,#16025,.T.);
#25962=EDGE_CURVE('',#20244,#20310,#10863,.T.);
#25963=EDGE_CURVE('',#20311,#20310,#16026,.T.);
#25964=EDGE_CURVE('',#20311,#20312,#16027,.T.);
#25965=EDGE_CURVE('',#20312,#20308,#10864,.T.);
#25966=EDGE_CURVE('',#20310,#20307,#10865,.T.);
#25967=EDGE_CURVE('',#20306,#20311,#2038,.T.);
#25968=EDGE_CURVE('',#20313,#20314,#16028,.T.);
#25969=EDGE_CURVE('',#20313,#20309,#2039,.T.);
#25970=EDGE_CURVE('',#20308,#20314,#10866,.T.);
#25971=EDGE_CURVE('',#20315,#20316,#16029,.T.);
#25972=EDGE_CURVE('',#20316,#20313,#16030,.T.);
#25973=EDGE_CURVE('',#20314,#20315,#16031,.T.);
#25974=EDGE_CURVE('',#20317,#20318,#16032,.T.);
#25975=EDGE_CURVE('',#20318,#20253,#16033,.T.);
#25976=EDGE_CURVE('',#20253,#20319,#10867,.T.);
#25977=EDGE_CURVE('',#20320,#20319,#16034,.T.);
#25978=EDGE_CURVE('',#20320,#20321,#16035,.T.);
#25979=EDGE_CURVE('',#20321,#20317,#10868,.T.);
#25980=EDGE_CURVE('',#20319,#20316,#10869,.T.);
#25981=EDGE_CURVE('',#20315,#20320,#2040,.T.);
#25982=EDGE_CURVE('',#20322,#20323,#16036,.T.);
#25983=EDGE_CURVE('',#20322,#20318,#2041,.T.);
#25984=EDGE_CURVE('',#20317,#20323,#10870,.T.);
#25985=EDGE_CURVE('',#20324,#20325,#16037,.T.);
#25986=EDGE_CURVE('',#20325,#20322,#16038,.T.);
#25987=EDGE_CURVE('',#20323,#20324,#16039,.T.);
#25988=EDGE_CURVE('',#20326,#20327,#16040,.T.);
#25989=EDGE_CURVE('',#20327,#20262,#16041,.T.);
#25990=EDGE_CURVE('',#20262,#20328,#10871,.T.);
#25991=EDGE_CURVE('',#20329,#20328,#16042,.T.);
#25992=EDGE_CURVE('',#20329,#20330,#16043,.T.);
#25993=EDGE_CURVE('',#20330,#20326,#10872,.F.);
#25994=EDGE_CURVE('',#20328,#20325,#10873,.T.);
#25995=EDGE_CURVE('',#20324,#20329,#2042,.T.);
#25996=EDGE_CURVE('',#17528,#20327,#16044,.T.);
#25997=EDGE_CURVE('',#20326,#17529,#10874,.F.);
#25998=EDGE_CURVE('',#17525,#20271,#1099,.T.);
#25999=EDGE_CURVE('',#20271,#20331,#10875,.T.);
#26000=EDGE_CURVE('',#17526,#20331,#1100,.T.);
#26001=EDGE_CURVE('',#20331,#17527,#1101,.T.);
#26002=EDGE_CURVE('',#20332,#20333,#16045,.T.);
#26003=EDGE_CURVE('',#20333,#20334,#16046,.T.);
#26004=EDGE_CURVE('',#20334,#20335,#16047,.T.);
#26005=EDGE_CURVE('',#20335,#20332,#16048,.T.);
#26006=EDGE_CURVE('',#20336,#20337,#16049,.T.);
#26007=EDGE_CURVE('',#20337,#17249,#16050,.T.);
#26008=EDGE_CURVE('',#20338,#17248,#2043,.T.);
#26009=EDGE_CURVE('',#20338,#20339,#1102,.T.);
#26010=EDGE_CURVE('',#20339,#20336,#10876,.T.);
#26011=EDGE_CURVE('',#20334,#20337,#2044,.T.);
#26012=EDGE_CURVE('',#20336,#20335,#10877,.T.);
#26013=EDGE_CURVE('',#20340,#20341,#16051,.T.);
#26014=EDGE_CURVE('',#20341,#20276,#16052,.T.);
#26015=EDGE_CURVE('',#20276,#20342,#10878,.T.);
#26016=EDGE_CURVE('',#20343,#20342,#16053,.T.);
#26017=EDGE_CURVE('',#20343,#20344,#16054,.T.);
#26018=EDGE_CURVE('',#20344,#20340,#10879,.T.);
#26019=EDGE_CURVE('',#20342,#20333,#10880,.T.);
#26020=EDGE_CURVE('',#20332,#20343,#2045,.T.);
#26021=EDGE_CURVE('',#17251,#20275,#1103,.T.);
#26022=EDGE_CURVE('',#20345,#20346,#16055,.T.);
#26023=EDGE_CURVE('',#20345,#20341,#2046,.T.);
#26024=EDGE_CURVE('',#20340,#20346,#10881,.T.);
#26025=EDGE_CURVE('',#20347,#20348,#16056,.T.);
#26026=EDGE_CURVE('',#20348,#20345,#16057,.T.);
#26027=EDGE_CURVE('',#20346,#20347,#16058,.T.);
#26028=EDGE_CURVE('',#20349,#20350,#16059,.T.);
#26029=EDGE_CURVE('',#20350,#20285,#16060,.T.);
#26030=EDGE_CURVE('',#20285,#20351,#10882,.T.);
#26031=EDGE_CURVE('',#20352,#20351,#16061,.T.);
#26032=EDGE_CURVE('',#20352,#20353,#16062,.T.);
#26033=EDGE_CURVE('',#20353,#20349,#10883,.T.);
#26034=EDGE_CURVE('',#20351,#20348,#10884,.T.);
#26035=EDGE_CURVE('',#20347,#20352,#2047,.T.);
#26036=EDGE_CURVE('',#20354,#20355,#16063,.T.);
#26037=EDGE_CURVE('',#20354,#20350,#2048,.T.);
#26038=EDGE_CURVE('',#20349,#20355,#10885,.T.);
#26039=EDGE_CURVE('',#20356,#20357,#16064,.T.);
#26040=EDGE_CURVE('',#20357,#20354,#16065,.T.);
#26041=EDGE_CURVE('',#20355,#20356,#16066,.T.);
#26042=EDGE_CURVE('',#20358,#20359,#2049,.T.);
#26043=EDGE_CURVE('',#20359,#20294,#2050,.T.);
#26044=EDGE_CURVE('',#20294,#20360,#10886,.T.);
#26045=EDGE_CURVE('',#20361,#20360,#16067,.T.);
#26046=EDGE_CURVE('',#20361,#20362,#16068,.T.);
#26047=EDGE_CURVE('',#20362,#20358,#10887,.T.);
#26048=EDGE_CURVE('',#20360,#20357,#10888,.T.);
#26049=EDGE_CURVE('',#20356,#20361,#2051,.T.);
#26050=EDGE_CURVE('',#20363,#20364,#2052,.T.);
#26051=EDGE_CURVE('',#20363,#20359,#2053,.T.);
#26052=EDGE_CURVE('',#20358,#20364,#10889,.T.);
#26053=EDGE_CURVE('',#20365,#20366,#16069,.T.);
#26054=EDGE_CURVE('',#20366,#20363,#2054,.T.);
#26055=EDGE_CURVE('',#20364,#20365,#16070,.T.);
#26056=EDGE_CURVE('',#20367,#20368,#16071,.T.);
#26057=EDGE_CURVE('',#20368,#20303,#16072,.T.);
#26058=EDGE_CURVE('',#20303,#20369,#10890,.T.);
#26059=EDGE_CURVE('',#20370,#20369,#16073,.T.);
#26060=EDGE_CURVE('',#20370,#20371,#16074,.T.);
#26061=EDGE_CURVE('',#20371,#20367,#10891,.T.);
#26062=EDGE_CURVE('',#20369,#20366,#10892,.T.);
#26063=EDGE_CURVE('',#20365,#20370,#2055,.T.);
#26064=EDGE_CURVE('',#20372,#20373,#16075,.T.);
#26065=EDGE_CURVE('',#20372,#20368,#2056,.T.);
#26066=EDGE_CURVE('',#20367,#20373,#10893,.T.);
#26067=EDGE_CURVE('',#20374,#20375,#16076,.T.);
#26068=EDGE_CURVE('',#20375,#20372,#16077,.T.);
#26069=EDGE_CURVE('',#20373,#20374,#16078,.T.);
#26070=EDGE_CURVE('',#20376,#20377,#16079,.T.);
#26071=EDGE_CURVE('',#20377,#20312,#16080,.T.);
#26072=EDGE_CURVE('',#20312,#20378,#10894,.T.);
#26073=EDGE_CURVE('',#20379,#20378,#16081,.T.);
#26074=EDGE_CURVE('',#20379,#20380,#16082,.T.);
#26075=EDGE_CURVE('',#20380,#20376,#10895,.T.);
#26076=EDGE_CURVE('',#20378,#20375,#10896,.T.);
#26077=EDGE_CURVE('',#20374,#20379,#2057,.T.);
#26078=EDGE_CURVE('',#20381,#20382,#16083,.T.);
#26079=EDGE_CURVE('',#20381,#20377,#2058,.T.);
#26080=EDGE_CURVE('',#20376,#20382,#10897,.T.);
#26081=EDGE_CURVE('',#20383,#20384,#16084,.T.);
#26082=EDGE_CURVE('',#20384,#20381,#16085,.T.);
#26083=EDGE_CURVE('',#20382,#20383,#16086,.T.);
#26084=EDGE_CURVE('',#20385,#20386,#16087,.T.);
#26085=EDGE_CURVE('',#20386,#20321,#16088,.T.);
#26086=EDGE_CURVE('',#20321,#20387,#10898,.T.);
#26087=EDGE_CURVE('',#20388,#20387,#16089,.T.);
#26088=EDGE_CURVE('',#20388,#20389,#16090,.T.);
#26089=EDGE_CURVE('',#20389,#20385,#10899,.F.);
#26090=EDGE_CURVE('',#20387,#20384,#10900,.T.);
#26091=EDGE_CURVE('',#20383,#20388,#2059,.T.);
#26092=EDGE_CURVE('',#17534,#20386,#16091,.T.);
#26093=EDGE_CURVE('',#20385,#17535,#10901,.F.);
#26094=EDGE_CURVE('',#17531,#20330,#1104,.T.);
#26095=EDGE_CURVE('',#20330,#20390,#10902,.T.);
#26096=EDGE_CURVE('',#17532,#20390,#1105,.T.);
#26097=EDGE_CURVE('',#20390,#17533,#1106,.T.);
#26098=EDGE_CURVE('',#20391,#20392,#16092,.T.);
#26099=EDGE_CURVE('',#20392,#20393,#16093,.T.);
#26100=EDGE_CURVE('',#20393,#20394,#16094,.T.);
#26101=EDGE_CURVE('',#20394,#20391,#16095,.T.);
#26102=EDGE_CURVE('',#20395,#20396,#16096,.T.);
#26103=EDGE_CURVE('',#20396,#20397,#16097,.T.);
#26104=EDGE_CURVE('',#20397,#20398,#16098,.T.);
#26105=EDGE_CURVE('',#20398,#20395,#16099,.T.);
#26106=EDGE_CURVE('',#20399,#20400,#16100,.T.);
#26107=EDGE_CURVE('',#20400,#17245,#16101,.T.);
#26108=EDGE_CURVE('',#20401,#17244,#2060,.T.);
#26109=EDGE_CURVE('',#20401,#20402,#1107,.T.);
#26110=EDGE_CURVE('',#20402,#20399,#10903,.T.);
#26111=EDGE_CURVE('',#20397,#20400,#2061,.T.);
#26112=EDGE_CURVE('',#20399,#20398,#10904,.T.);
#26113=EDGE_CURVE('',#20403,#20404,#16102,.T.);
#26114=EDGE_CURVE('',#20404,#20339,#16103,.T.);
#26115=EDGE_CURVE('',#20339,#20405,#10905,.T.);
#26116=EDGE_CURVE('',#20406,#20405,#16104,.T.);
#26117=EDGE_CURVE('',#20406,#20407,#16105,.T.);
#26118=EDGE_CURVE('',#20407,#20403,#10906,.T.);
#26119=EDGE_CURVE('',#20405,#20396,#10907,.T.);
#26120=EDGE_CURVE('',#20395,#20406,#2062,.T.);
#26121=EDGE_CURVE('',#17247,#20338,#1108,.T.);
#26122=EDGE_CURVE('',#20393,#20404,#2063,.T.);
#26123=EDGE_CURVE('',#20403,#20394,#10908,.T.);
#26124=EDGE_CURVE('',#20408,#20409,#16106,.T.);
#26125=EDGE_CURVE('',#20409,#20344,#16107,.T.);
#26126=EDGE_CURVE('',#20344,#20410,#10909,.T.);
#26127=EDGE_CURVE('',#20411,#20410,#16108,.T.);
#26128=EDGE_CURVE('',#20411,#20412,#16109,.T.);
#26129=EDGE_CURVE('',#20412,#20408,#10910,.T.);
#26130=EDGE_CURVE('',#20410,#20392,#10911,.T.);
#26131=EDGE_CURVE('',#20391,#20411,#2064,.T.);
#26132=EDGE_CURVE('',#20413,#20414,#16110,.T.);
#26133=EDGE_CURVE('',#20413,#20409,#2065,.T.);
#26134=EDGE_CURVE('',#20408,#20414,#10912,.T.);
#26135=EDGE_CURVE('',#20415,#20416,#16111,.T.);
#26136=EDGE_CURVE('',#20416,#20413,#16112,.T.);
#26137=EDGE_CURVE('',#20414,#20415,#16113,.T.);
#26138=EDGE_CURVE('',#20417,#20418,#2066,.T.);
#26139=EDGE_CURVE('',#20418,#20353,#2067,.T.);
#26140=EDGE_CURVE('',#20353,#20419,#10913,.T.);
#26141=EDGE_CURVE('',#20420,#20419,#16114,.T.);
#26142=EDGE_CURVE('',#20420,#20421,#16115,.T.);
#26143=EDGE_CURVE('',#20421,#20417,#10914,.T.);
#26144=EDGE_CURVE('',#20419,#20416,#10915,.T.);
#26145=EDGE_CURVE('',#20415,#20420,#2068,.T.);
#26146=EDGE_CURVE('',#20422,#20423,#2069,.T.);
#26147=EDGE_CURVE('',#20422,#20418,#2070,.T.);
#26148=EDGE_CURVE('',#20417,#20423,#10916,.T.);
#26149=EDGE_CURVE('',#20424,#20425,#16116,.T.);
#26150=EDGE_CURVE('',#20425,#20422,#2071,.T.);
#26151=EDGE_CURVE('',#20423,#20424,#16117,.T.);
#26152=EDGE_CURVE('',#20426,#20427,#16118,.T.);
#26153=EDGE_CURVE('',#20427,#20362,#16119,.T.);
#26154=EDGE_CURVE('',#20362,#20428,#10917,.T.);
#26155=EDGE_CURVE('',#20429,#20428,#16120,.T.);
#26156=EDGE_CURVE('',#20429,#20430,#16121,.T.);
#26157=EDGE_CURVE('',#20430,#20426,#10918,.T.);
#26158=EDGE_CURVE('',#20428,#20425,#10919,.T.);
#26159=EDGE_CURVE('',#20424,#20429,#2072,.T.);
#26160=EDGE_CURVE('',#20431,#20432,#16122,.T.);
#26161=EDGE_CURVE('',#20431,#20427,#2073,.T.);
#26162=EDGE_CURVE('',#20426,#20432,#10920,.T.);
#26163=EDGE_CURVE('',#20433,#20434,#16123,.T.);
#26164=EDGE_CURVE('',#20434,#20431,#16124,.T.);
#26165=EDGE_CURVE('',#20432,#20433,#16125,.T.);
#26166=EDGE_CURVE('',#20435,#20436,#16126,.T.);
#26167=EDGE_CURVE('',#20436,#20371,#16127,.T.);
#26168=EDGE_CURVE('',#20371,#20437,#10921,.T.);
#26169=EDGE_CURVE('',#20438,#20437,#16128,.T.);
#26170=EDGE_CURVE('',#20438,#20439,#16129,.T.);
#26171=EDGE_CURVE('',#20439,#20435,#10922,.T.);
#26172=EDGE_CURVE('',#20437,#20434,#10923,.T.);
#26173=EDGE_CURVE('',#20433,#20438,#2074,.T.);
#26174=EDGE_CURVE('',#20440,#20441,#16130,.T.);
#26175=EDGE_CURVE('',#20440,#20436,#2075,.T.);
#26176=EDGE_CURVE('',#20435,#20441,#10924,.T.);
#26177=EDGE_CURVE('',#20442,#20443,#16131,.T.);
#26178=EDGE_CURVE('',#20443,#20440,#16132,.T.);
#26179=EDGE_CURVE('',#20441,#20442,#16133,.T.);
#26180=EDGE_CURVE('',#20444,#20445,#16134,.T.);
#26181=EDGE_CURVE('',#20445,#20380,#16135,.T.);
#26182=EDGE_CURVE('',#20380,#20446,#10925,.T.);
#26183=EDGE_CURVE('',#20447,#20446,#16136,.T.);
#26184=EDGE_CURVE('',#20447,#20448,#16137,.T.);
#26185=EDGE_CURVE('',#20448,#20444,#10926,.F.);
#26186=EDGE_CURVE('',#20446,#20443,#10927,.T.);
#26187=EDGE_CURVE('',#20442,#20447,#2076,.T.);
#26188=EDGE_CURVE('',#17540,#20445,#16138,.T.);
#26189=EDGE_CURVE('',#20444,#17541,#10928,.F.);
#26190=EDGE_CURVE('',#17537,#20389,#1109,.T.);
#26191=EDGE_CURVE('',#20389,#20449,#10929,.T.);
#26192=EDGE_CURVE('',#17538,#20449,#1110,.T.);
#26193=EDGE_CURVE('',#20449,#17539,#1111,.T.);
#26194=EDGE_CURVE('',#20450,#20451,#16139,.T.);
#26195=EDGE_CURVE('',#20451,#20452,#16140,.T.);
#26196=EDGE_CURVE('',#20452,#20453,#16141,.T.);
#26197=EDGE_CURVE('',#20453,#20450,#16142,.T.);
#26198=EDGE_CURVE('',#20454,#20455,#16143,.T.);
#26199=EDGE_CURVE('',#20455,#20456,#16144,.T.);
#26200=EDGE_CURVE('',#20456,#20457,#16145,.T.);
#26201=EDGE_CURVE('',#20457,#20454,#16146,.T.);
#26202=EDGE_CURVE('',#20458,#20459,#16147,.T.);
#26203=EDGE_CURVE('',#20459,#20460,#16148,.T.);
#26204=EDGE_CURVE('',#20460,#20461,#16149,.T.);
#26205=EDGE_CURVE('',#20461,#20458,#16150,.T.);
#26206=EDGE_CURVE('',#20462,#20463,#16151,.T.);
#26207=EDGE_CURVE('',#20463,#20402,#16152,.T.);
#26208=EDGE_CURVE('',#20402,#20464,#10930,.T.);
#26209=EDGE_CURVE('',#20465,#20464,#16153,.T.);
#26210=EDGE_CURVE('',#20465,#20466,#16154,.T.);
#26211=EDGE_CURVE('',#20466,#20462,#10931,.T.);
#26212=EDGE_CURVE('',#20464,#20451,#10932,.T.);
#26213=EDGE_CURVE('',#20450,#20465,#2077,.T.);
#26214=EDGE_CURVE('',#17243,#20401,#1112,.T.);
#26215=EDGE_CURVE('',#20460,#20463,#2078,.T.);
#26216=EDGE_CURVE('',#20462,#20461,#10933,.T.);
#26217=EDGE_CURVE('',#20467,#20468,#16155,.T.);
#26218=EDGE_CURVE('',#20468,#20407,#16156,.T.);
#26219=EDGE_CURVE('',#20407,#20469,#10934,.T.);
#26220=EDGE_CURVE('',#20470,#20469,#16157,.T.);
#26221=EDGE_CURVE('',#20470,#20471,#16158,.T.);
#26222=EDGE_CURVE('',#20471,#20467,#10935,.T.);
#26223=EDGE_CURVE('',#20469,#20459,#10936,.T.);
#26224=EDGE_CURVE('',#20458,#20470,#2079,.T.);
#26225=EDGE_CURVE('',#20456,#20468,#2080,.T.);
#26226=EDGE_CURVE('',#20467,#20457,#10937,.T.);
#26227=EDGE_CURVE('',#20472,#20473,#2081,.T.);
#26228=EDGE_CURVE('',#20473,#20412,#2082,.T.);
#26229=EDGE_CURVE('',#20412,#20474,#10938,.T.);
#26230=EDGE_CURVE('',#20475,#20474,#16159,.T.);
#26231=EDGE_CURVE('',#20475,#20476,#16160,.T.);
#26232=EDGE_CURVE('',#20476,#20472,#10939,.T.);
#26233=EDGE_CURVE('',#20474,#20455,#10940,.T.);
#26234=EDGE_CURVE('',#20454,#20475,#2083,.T.);
#26235=EDGE_CURVE('',#20477,#20478,#2084,.T.);
#26236=EDGE_CURVE('',#20477,#20473,#2085,.T.);
#26237=EDGE_CURVE('',#20472,#20478,#10941,.T.);
#26238=EDGE_CURVE('',#20479,#20480,#16161,.T.);
#26239=EDGE_CURVE('',#20480,#17241,#16162,.T.);
#26240=EDGE_CURVE('',#20481,#17240,#2086,.T.);
#26241=EDGE_CURVE('',#20481,#20482,#1113,.T.);
#26242=EDGE_CURVE('',#20482,#20479,#10942,.T.);
#26243=EDGE_CURVE('',#20452,#20480,#2087,.T.);
#26244=EDGE_CURVE('',#20479,#20453,#10943,.T.);
#26245=EDGE_CURVE('',#20483,#20484,#16163,.T.);
#26246=EDGE_CURVE('',#20484,#20477,#2088,.T.);
#26247=EDGE_CURVE('',#20478,#20483,#16164,.T.);
#26248=EDGE_CURVE('',#20485,#20486,#16165,.T.);
#26249=EDGE_CURVE('',#20486,#20421,#16166,.T.);
#26250=EDGE_CURVE('',#20421,#20487,#10944,.T.);
#26251=EDGE_CURVE('',#20488,#20487,#16167,.T.);
#26252=EDGE_CURVE('',#20488,#20489,#16168,.T.);
#26253=EDGE_CURVE('',#20489,#20485,#10945,.T.);
#26254=EDGE_CURVE('',#20487,#20484,#10946,.T.);
#26255=EDGE_CURVE('',#20483,#20488,#2089,.T.);
#26256=EDGE_CURVE('',#20490,#20491,#16169,.T.);
#26257=EDGE_CURVE('',#20490,#20486,#2090,.T.);
#26258=EDGE_CURVE('',#20485,#20491,#10947,.T.);
#26259=EDGE_CURVE('',#20492,#20493,#16170,.T.);
#26260=EDGE_CURVE('',#20493,#20490,#16171,.T.);
#26261=EDGE_CURVE('',#20491,#20492,#16172,.T.);
#26262=EDGE_CURVE('',#20494,#20495,#16173,.T.);
#26263=EDGE_CURVE('',#20495,#20430,#16174,.T.);
#26264=EDGE_CURVE('',#20430,#20496,#10948,.T.);
#26265=EDGE_CURVE('',#20497,#20496,#16175,.T.);
#26266=EDGE_CURVE('',#20497,#20498,#16176,.T.);
#26267=EDGE_CURVE('',#20498,#20494,#10949,.T.);
#26268=EDGE_CURVE('',#20496,#20493,#10950,.T.);
#26269=EDGE_CURVE('',#20492,#20497,#2091,.T.);
#26270=EDGE_CURVE('',#20499,#20500,#16177,.T.);
#26271=EDGE_CURVE('',#20499,#20495,#2092,.T.);
#26272=EDGE_CURVE('',#20494,#20500,#10951,.T.);
#26273=EDGE_CURVE('',#20501,#20502,#16178,.T.);
#26274=EDGE_CURVE('',#20502,#20499,#16179,.T.);
#26275=EDGE_CURVE('',#20500,#20501,#16180,.T.);
#26276=EDGE_CURVE('',#20503,#20504,#16181,.T.);
#26277=EDGE_CURVE('',#20504,#20439,#16182,.T.);
#26278=EDGE_CURVE('',#20439,#20505,#10952,.T.);
#26279=EDGE_CURVE('',#20506,#20505,#16183,.T.);
#26280=EDGE_CURVE('',#20506,#20507,#16184,.T.);
#26281=EDGE_CURVE('',#20507,#20503,#10953,.F.);
#26282=EDGE_CURVE('',#20505,#20502,#10954,.T.);
#26283=EDGE_CURVE('',#20501,#20506,#2093,.T.);
#26284=EDGE_CURVE('',#17546,#20504,#16185,.T.);
#26285=EDGE_CURVE('',#20503,#17547,#10955,.F.);
#26286=EDGE_CURVE('',#17543,#20448,#1114,.T.);
#26287=EDGE_CURVE('',#20448,#20508,#10956,.T.);
#26288=EDGE_CURVE('',#17544,#20508,#1115,.T.);
#26289=EDGE_CURVE('',#20508,#17545,#1116,.T.);
#26290=EDGE_CURVE('',#20509,#20510,#16186,.T.);
#26291=EDGE_CURVE('',#20510,#20511,#16187,.T.);
#26292=EDGE_CURVE('',#20511,#20512,#16188,.T.);
#26293=EDGE_CURVE('',#20512,#20509,#16189,.T.);
#26294=EDGE_CURVE('',#20513,#20514,#16190,.T.);
#26295=EDGE_CURVE('',#20514,#20515,#16191,.T.);
#26296=EDGE_CURVE('',#20515,#20516,#16192,.T.);
#26297=EDGE_CURVE('',#20516,#20513,#16193,.T.);
#26298=EDGE_CURVE('',#20517,#20518,#16194,.T.);
#26299=EDGE_CURVE('',#20518,#20519,#2094,.T.);
#26300=EDGE_CURVE('',#20519,#20520,#2095,.T.);
#26301=EDGE_CURVE('',#20520,#20517,#16195,.T.);
#26302=EDGE_CURVE('',#20521,#20522,#16196,.T.);
#26303=EDGE_CURVE('',#20522,#20523,#16197,.T.);
#26304=EDGE_CURVE('',#20523,#20524,#16198,.T.);
#26305=EDGE_CURVE('',#20524,#20521,#16199,.T.);
#26306=EDGE_CURVE('',#20525,#20526,#16200,.T.);
#26307=EDGE_CURVE('',#20526,#20466,#16201,.T.);
#26308=EDGE_CURVE('',#20466,#20527,#10957,.T.);
#26309=EDGE_CURVE('',#20528,#20527,#16202,.T.);
#26310=EDGE_CURVE('',#20528,#20529,#16203,.T.);
#26311=EDGE_CURVE('',#20529,#20525,#10958,.T.);
#26312=EDGE_CURVE('',#20527,#20514,#10959,.T.);
#26313=EDGE_CURVE('',#20513,#20528,#2096,.T.);
#26314=EDGE_CURVE('',#20523,#20526,#2097,.T.);
#26315=EDGE_CURVE('',#20525,#20524,#10960,.T.);
#26316=EDGE_CURVE('',#20530,#20531,#2098,.T.);
#26317=EDGE_CURVE('',#20531,#20471,#2099,.T.);
#26318=EDGE_CURVE('',#20471,#20532,#10961,.T.);
#26319=EDGE_CURVE('',#20533,#20532,#16204,.T.);
#26320=EDGE_CURVE('',#20533,#20534,#16205,.T.);
#26321=EDGE_CURVE('',#20534,#20530,#10962,.T.);
#26322=EDGE_CURVE('',#20532,#20522,#10963,.T.);
#26323=EDGE_CURVE('',#20521,#20533,#2100,.T.);
#26324=EDGE_CURVE('',#20519,#20531,#2101,.T.);
#26325=EDGE_CURVE('',#20530,#20520,#10964,.T.);
#26326=EDGE_CURVE('',#20535,#20536,#16206,.T.);
#26327=EDGE_CURVE('',#20536,#20476,#16207,.T.);
#26328=EDGE_CURVE('',#20476,#20537,#10965,.T.);
#26329=EDGE_CURVE('',#20538,#20537,#16208,.T.);
#26330=EDGE_CURVE('',#20538,#20539,#16209,.T.);
#26331=EDGE_CURVE('',#20539,#20535,#10966,.T.);
#26332=EDGE_CURVE('',#20537,#20518,#10967,.T.);
#26333=EDGE_CURVE('',#20517,#20538,#2102,.T.);
#26334=EDGE_CURVE('',#20540,#20541,#16210,.T.);
#26335=EDGE_CURVE('',#20540,#20536,#2103,.T.);
#26336=EDGE_CURVE('',#20535,#20541,#10968,.T.);
#26337=EDGE_CURVE('',#20542,#20543,#16211,.T.);
#26338=EDGE_CURVE('',#20543,#17237,#16212,.T.);
#26339=EDGE_CURVE('',#20544,#17236,#2104,.T.);
#26340=EDGE_CURVE('',#20544,#20545,#1117,.T.);
#26341=EDGE_CURVE('',#20545,#20542,#10969,.T.);
#26342=EDGE_CURVE('',#20511,#20543,#2105,.T.);
#26343=EDGE_CURVE('',#20542,#20512,#10970,.T.);
#26344=EDGE_CURVE('',#20546,#20547,#16213,.T.);
#26345=EDGE_CURVE('',#20547,#20482,#16214,.T.);
#26346=EDGE_CURVE('',#20482,#20548,#10971,.T.);
#26347=EDGE_CURVE('',#20549,#20548,#16215,.T.);
#26348=EDGE_CURVE('',#20549,#20550,#16216,.T.);
#26349=EDGE_CURVE('',#20550,#20546,#10972,.T.);
#26350=EDGE_CURVE('',#20548,#20510,#10973,.T.);
#26351=EDGE_CURVE('',#20509,#20549,#2106,.T.);
#26352=EDGE_CURVE('',#17239,#20481,#1118,.T.);
#26353=EDGE_CURVE('',#20515,#20547,#2107,.T.);
#26354=EDGE_CURVE('',#20546,#20516,#10974,.T.);
#26355=EDGE_CURVE('',#20551,#20552,#16217,.T.);
#26356=EDGE_CURVE('',#20552,#20540,#16218,.T.);
#26357=EDGE_CURVE('',#20541,#20551,#16219,.T.);
#26358=EDGE_CURVE('',#20553,#20554,#16220,.T.);
#26359=EDGE_CURVE('',#20554,#20489,#16221,.T.);
#26360=EDGE_CURVE('',#20489,#20555,#10975,.T.);
#26361=EDGE_CURVE('',#20556,#20555,#16222,.T.);
#26362=EDGE_CURVE('',#20556,#20557,#16223,.T.);
#26363=EDGE_CURVE('',#20557,#20553,#10976,.T.);
#26364=EDGE_CURVE('',#20555,#20552,#10977,.T.);
#26365=EDGE_CURVE('',#20551,#20556,#2108,.T.);
#26366=EDGE_CURVE('',#20558,#20559,#16224,.T.);
#26367=EDGE_CURVE('',#20558,#20554,#2109,.T.);
#26368=EDGE_CURVE('',#20553,#20559,#10978,.T.);
#26369=EDGE_CURVE('',#20560,#20561,#16225,.T.);
#26370=EDGE_CURVE('',#20561,#20558,#16226,.T.);
#26371=EDGE_CURVE('',#20559,#20560,#16227,.T.);
#26372=EDGE_CURVE('',#20562,#20563,#16228,.T.);
#26373=EDGE_CURVE('',#20563,#20498,#16229,.T.);
#26374=EDGE_CURVE('',#20498,#20564,#10979,.T.);
#26375=EDGE_CURVE('',#20565,#20564,#16230,.T.);
#26376=EDGE_CURVE('',#20565,#20566,#16231,.T.);
#26377=EDGE_CURVE('',#20566,#20562,#10980,.F.);
#26378=EDGE_CURVE('',#20564,#20561,#10981,.T.);
#26379=EDGE_CURVE('',#20560,#20565,#2110,.T.);
#26380=EDGE_CURVE('',#17552,#20563,#16232,.T.);
#26381=EDGE_CURVE('',#20562,#17553,#10982,.F.);
#26382=EDGE_CURVE('',#17549,#20507,#1119,.T.);
#26383=EDGE_CURVE('',#20507,#20567,#10983,.T.);
#26384=EDGE_CURVE('',#17550,#20567,#1120,.T.);
#26385=EDGE_CURVE('',#20567,#17551,#1121,.T.);
#26386=EDGE_CURVE('',#20568,#20569,#16233,.T.);
#26387=EDGE_CURVE('',#20569,#20570,#16234,.T.);
#26388=EDGE_CURVE('',#20570,#20571,#16235,.T.);
#26389=EDGE_CURVE('',#20571,#20568,#16236,.T.);
#26390=EDGE_CURVE('',#20572,#20573,#16237,.T.);
#26391=EDGE_CURVE('',#20573,#20574,#16238,.T.);
#26392=EDGE_CURVE('',#20574,#20575,#16239,.T.);
#26393=EDGE_CURVE('',#20575,#20572,#16240,.T.);
#26394=EDGE_CURVE('',#20576,#20577,#16241,.T.);
#26395=EDGE_CURVE('',#20577,#20578,#16242,.T.);
#26396=EDGE_CURVE('',#20578,#20579,#16243,.T.);
#26397=EDGE_CURVE('',#20579,#20576,#16244,.T.);
#26398=EDGE_CURVE('',#20580,#20581,#16245,.T.);
#26399=EDGE_CURVE('',#20581,#20582,#16246,.T.);
#26400=EDGE_CURVE('',#20582,#20583,#16247,.T.);
#26401=EDGE_CURVE('',#20583,#20580,#16248,.T.);
#26402=EDGE_CURVE('',#20584,#20585,#16249,.T.);
#26403=EDGE_CURVE('',#20585,#20586,#2111,.T.);
#26404=EDGE_CURVE('',#20586,#20587,#2112,.T.);
#26405=EDGE_CURVE('',#20587,#20584,#16250,.T.);
#26406=EDGE_CURVE('',#20588,#20589,#2113,.T.);
#26407=EDGE_CURVE('',#20589,#20529,#2114,.T.);
#26408=EDGE_CURVE('',#20529,#20590,#10984,.T.);
#26409=EDGE_CURVE('',#20591,#20590,#16251,.T.);
#26410=EDGE_CURVE('',#20591,#20592,#16252,.T.);
#26411=EDGE_CURVE('',#20592,#20588,#10985,.T.);
#26412=EDGE_CURVE('',#20590,#20573,#10986,.T.);
#26413=EDGE_CURVE('',#20572,#20591,#2115,.T.);
#26414=EDGE_CURVE('',#20586,#20589,#2116,.T.);
#26415=EDGE_CURVE('',#20588,#20587,#10987,.T.);
#26416=EDGE_CURVE('',#20593,#20594,#16253,.T.);
#26417=EDGE_CURVE('',#20594,#20534,#16254,.T.);
#26418=EDGE_CURVE('',#20534,#20595,#10988,.T.);
#26419=EDGE_CURVE('',#20596,#20595,#16255,.T.);
#26420=EDGE_CURVE('',#20596,#20597,#16256,.T.);
#26421=EDGE_CURVE('',#20597,#20593,#10989,.T.);
#26422=EDGE_CURVE('',#20595,#20585,#10990,.T.);
#26423=EDGE_CURVE('',#20584,#20596,#2117,.T.);
#26424=EDGE_CURVE('',#20582,#20594,#2118,.T.);
#26425=EDGE_CURVE('',#20593,#20583,#10991,.T.);
#26426=EDGE_CURVE('',#20598,#20599,#16257,.T.);
#26427=EDGE_CURVE('',#20599,#20539,#16258,.T.);
#26428=EDGE_CURVE('',#20539,#20600,#10992,.T.);
#26429=EDGE_CURVE('',#20601,#20600,#16259,.T.);
#26430=EDGE_CURVE('',#20601,#20602,#16260,.T.);
#26431=EDGE_CURVE('',#20602,#20598,#10993,.T.);
#26432=EDGE_CURVE('',#20600,#20581,#10994,.T.);
#26433=EDGE_CURVE('',#20580,#20601,#2119,.T.);
#26434=EDGE_CURVE('',#20603,#20604,#16261,.T.);
#26435=EDGE_CURVE('',#20603,#20599,#2120,.T.);
#26436=EDGE_CURVE('',#20598,#20604,#10995,.T.);
#26437=EDGE_CURVE('',#20605,#20606,#16262,.T.);
#26438=EDGE_CURVE('',#20606,#17233,#16263,.T.);
#26439=EDGE_CURVE('',#20607,#17232,#2121,.T.);
#26440=EDGE_CURVE('',#20607,#20608,#1122,.T.);
#26441=EDGE_CURVE('',#20608,#20605,#10996,.T.);
#26442=EDGE_CURVE('',#20578,#20606,#2122,.T.);
#26443=EDGE_CURVE('',#20605,#20579,#10997,.T.);
#26444=EDGE_CURVE('',#20609,#20610,#16264,.T.);
#26445=EDGE_CURVE('',#20610,#20545,#16265,.T.);
#26446=EDGE_CURVE('',#20545,#20611,#10998,.T.);
#26447=EDGE_CURVE('',#20612,#20611,#16266,.T.);
#26448=EDGE_CURVE('',#20612,#20613,#16267,.T.);
#26449=EDGE_CURVE('',#20613,#20609,#10999,.T.);
#26450=EDGE_CURVE('',#20611,#20577,#11000,.T.);
#26451=EDGE_CURVE('',#20576,#20612,#2123,.T.);
#26452=EDGE_CURVE('',#17235,#20544,#1123,.T.);
#26453=EDGE_CURVE('',#20570,#20610,#2124,.T.);
#26454=EDGE_CURVE('',#20609,#20571,#11001,.T.);
#26455=EDGE_CURVE('',#20614,#20615,#16268,.T.);
#26456=EDGE_CURVE('',#20615,#20550,#16269,.T.);
#26457=EDGE_CURVE('',#20550,#20616,#11002,.T.);
#26458=EDGE_CURVE('',#20617,#20616,#16270,.T.);
#26459=EDGE_CURVE('',#20617,#20618,#16271,.T.);
#26460=EDGE_CURVE('',#20618,#20614,#11003,.T.);
#26461=EDGE_CURVE('',#20616,#20569,#11004,.T.);
#26462=EDGE_CURVE('',#20568,#20617,#2125,.T.);
#26463=EDGE_CURVE('',#20574,#20615,#2126,.T.);
#26464=EDGE_CURVE('',#20614,#20575,#11005,.T.);
#26465=EDGE_CURVE('',#20619,#20620,#16272,.T.);
#26466=EDGE_CURVE('',#20620,#20603,#16273,.T.);
#26467=EDGE_CURVE('',#20604,#20619,#16274,.T.);
#26468=EDGE_CURVE('',#20621,#20622,#16275,.T.);
#26469=EDGE_CURVE('',#20622,#20557,#16276,.T.);
#26470=EDGE_CURVE('',#20557,#20623,#11006,.T.);
#26471=EDGE_CURVE('',#20624,#20623,#16277,.T.);
#26472=EDGE_CURVE('',#20624,#20625,#16278,.T.);
#26473=EDGE_CURVE('',#20625,#20621,#11007,.F.);
#26474=EDGE_CURVE('',#20623,#20620,#11008,.T.);
#26475=EDGE_CURVE('',#20619,#20624,#2127,.T.);
#26476=EDGE_CURVE('',#17558,#20622,#16279,.T.);
#26477=EDGE_CURVE('',#20621,#17559,#11009,.F.);
#26478=EDGE_CURVE('',#17555,#20566,#1124,.T.);
#26479=EDGE_CURVE('',#20566,#20626,#11010,.T.);
#26480=EDGE_CURVE('',#17556,#20626,#1125,.T.);
#26481=EDGE_CURVE('',#20626,#17557,#1126,.T.);
#26482=EDGE_CURVE('',#20627,#20628,#16280,.T.);
#26483=EDGE_CURVE('',#20628,#20629,#16281,.T.);
#26484=EDGE_CURVE('',#20629,#20630,#16282,.T.);
#26485=EDGE_CURVE('',#20630,#20627,#16283,.T.);
#26486=EDGE_CURVE('',#20631,#20632,#16284,.T.);
#26487=EDGE_CURVE('',#20632,#20633,#2128,.T.);
#26488=EDGE_CURVE('',#20633,#20634,#2129,.T.);
#26489=EDGE_CURVE('',#20634,#20631,#16285,.T.);
#26490=EDGE_CURVE('',#20635,#20636,#16286,.T.);
#26491=EDGE_CURVE('',#20636,#20637,#16287,.T.);
#26492=EDGE_CURVE('',#20637,#20638,#16288,.T.);
#26493=EDGE_CURVE('',#20638,#20635,#16289,.T.);
#26494=EDGE_CURVE('',#20639,#20640,#16290,.T.);
#26495=EDGE_CURVE('',#20640,#20641,#16291,.T.);
#26496=EDGE_CURVE('',#20641,#20642,#16292,.T.);
#26497=EDGE_CURVE('',#20642,#20639,#16293,.T.);
#26498=EDGE_CURVE('',#20643,#20644,#16294,.T.);
#26499=EDGE_CURVE('',#20644,#20645,#16295,.T.);
#26500=EDGE_CURVE('',#20645,#20646,#16296,.T.);
#26501=EDGE_CURVE('',#20646,#20643,#16297,.T.);
#26502=EDGE_CURVE('',#20647,#20648,#16298,.T.);
#26503=EDGE_CURVE('',#20648,#20649,#16299,.T.);
#26504=EDGE_CURVE('',#20649,#20650,#16300,.T.);
#26505=EDGE_CURVE('',#20650,#20647,#16301,.T.);
#26506=EDGE_CURVE('',#20651,#20652,#16302,.T.);
#26507=EDGE_CURVE('',#20652,#20592,#16303,.T.);
#26508=EDGE_CURVE('',#20592,#20653,#11011,.T.);
#26509=EDGE_CURVE('',#20654,#20653,#16304,.T.);
#26510=EDGE_CURVE('',#20654,#17842,#16305,.T.);
#26511=EDGE_CURVE('',#17842,#20651,#11012,.T.);
#26512=EDGE_CURVE('',#20653,#20632,#11013,.T.);
#26513=EDGE_CURVE('',#20631,#20654,#2130,.T.);
#26514=EDGE_CURVE('',#20649,#20652,#2131,.T.);
#26515=EDGE_CURVE('',#20651,#20650,#11014,.T.);
#26516=EDGE_CURVE('',#20655,#20656,#16306,.T.);
#26517=EDGE_CURVE('',#20656,#20597,#16307,.T.);
#26518=EDGE_CURVE('',#20597,#20657,#11015,.T.);
#26519=EDGE_CURVE('',#20658,#20657,#16308,.T.);
#26520=EDGE_CURVE('',#20658,#17853,#16309,.T.);
#26521=EDGE_CURVE('',#17853,#20655,#11016,.T.);
#26522=EDGE_CURVE('',#20657,#20648,#11017,.T.);
#26523=EDGE_CURVE('',#20647,#20658,#2132,.T.);
#26524=EDGE_CURVE('',#20645,#20656,#2133,.T.);
#26525=EDGE_CURVE('',#20655,#20646,#11018,.T.);
#26526=EDGE_CURVE('',#20659,#20660,#16310,.T.);
#26527=EDGE_CURVE('',#20660,#20602,#16311,.T.);
#26528=EDGE_CURVE('',#20602,#20661,#11019,.T.);
#26529=EDGE_CURVE('',#20662,#20661,#16312,.T.);
#26530=EDGE_CURVE('',#20662,#20663,#16313,.T.);
#26531=EDGE_CURVE('',#20663,#20659,#11020,.F.);
#26532=EDGE_CURVE('',#20661,#20644,#11021,.T.);
#26533=EDGE_CURVE('',#20643,#20662,#2134,.T.);
#26534=EDGE_CURVE('',#17564,#20660,#16314,.T.);
#26535=EDGE_CURVE('',#20659,#17565,#11022,.F.);
#26536=EDGE_CURVE('',#20664,#20665,#16315,.T.);
#26537=EDGE_CURVE('',#20665,#17227,#16316,.T.);
#26538=EDGE_CURVE('',#20666,#17428,#2135,.T.);
#26539=EDGE_CURVE('',#20666,#17766,#1127,.T.);
#26540=EDGE_CURVE('',#17766,#20664,#11023,.T.);
#26541=EDGE_CURVE('',#20641,#20665,#2136,.T.);
#26542=EDGE_CURVE('',#20664,#20642,#11024,.T.);
#26543=EDGE_CURVE('',#20667,#20668,#16317,.T.);
#26544=EDGE_CURVE('',#20668,#20608,#16318,.T.);
#26545=EDGE_CURVE('',#20608,#20669,#11025,.T.);
#26546=EDGE_CURVE('',#20670,#20669,#16319,.T.);
#26547=EDGE_CURVE('',#20670,#17785,#16320,.T.);
#26548=EDGE_CURVE('',#17785,#20667,#11026,.T.);
#26549=EDGE_CURVE('',#20669,#20640,#11027,.T.);
#26550=EDGE_CURVE('',#20639,#20670,#2137,.T.);
#26551=EDGE_CURVE('',#17231,#20607,#1128,.T.);
#26552=EDGE_CURVE('',#20637,#20668,#2138,.T.);
#26553=EDGE_CURVE('',#20667,#20638,#11028,.T.);
#26554=EDGE_CURVE('',#20671,#20672,#16321,.T.);
#26555=EDGE_CURVE('',#20672,#20613,#16322,.T.);
#26556=EDGE_CURVE('',#20613,#20673,#11029,.T.);
#26557=EDGE_CURVE('',#20674,#20673,#16323,.T.);
#26558=EDGE_CURVE('',#20674,#17804,#16324,.T.);
#26559=EDGE_CURVE('',#17804,#20671,#11030,.T.);
#26560=EDGE_CURVE('',#20673,#20636,#11031,.T.);
#26561=EDGE_CURVE('',#20635,#20674,#2139,.T.);
#26562=EDGE_CURVE('',#20629,#20672,#2140,.T.);
#26563=EDGE_CURVE('',#20671,#20630,#11032,.T.);
#26564=EDGE_CURVE('',#20675,#20676,#2141,.T.);
#26565=EDGE_CURVE('',#20676,#20618,#2142,.T.);
#26566=EDGE_CURVE('',#20618,#20677,#11033,.T.);
#26567=EDGE_CURVE('',#20678,#20677,#16325,.T.);
#26568=EDGE_CURVE('',#20678,#17823,#16326,.T.);
#26569=EDGE_CURVE('',#17823,#20675,#11034,.T.);
#26570=EDGE_CURVE('',#20677,#20628,#11035,.T.);
#26571=EDGE_CURVE('',#20627,#20678,#2143,.T.);
#26572=EDGE_CURVE('',#20633,#20676,#2144,.T.);
#26573=EDGE_CURVE('',#20675,#20634,#11036,.T.);
#26574=EDGE_CURVE('',#17561,#20625,#1129,.T.);
#26575=EDGE_CURVE('',#20625,#20679,#11037,.T.);
#26576=EDGE_CURVE('',#17562,#20679,#1130,.T.);
#26577=EDGE_CURVE('',#20679,#17563,#1131,.T.);
#26578=EDGE_CURVE('',#17567,#20663,#1132,.T.);
#26579=EDGE_CURVE('',#20663,#20680,#11038,.T.);
#26580=EDGE_CURVE('',#17568,#20680,#1133,.T.);
#26581=EDGE_CURVE('',#20680,#17569,#1134,.T.);
#26582=EDGE_CURVE('',#17427,#20666,#1135,.T.);
#26583=EDGE_CURVE('',#17839,#17822,#16327,.T.);
#26584=EDGE_CURVE('',#20654,#20675,#16328,.T.);
#26585=EDGE_CURVE('',#20678,#20671,#16329,.T.);
#26586=EDGE_CURVE('',#17820,#17803,#51,.T.);
#26587=EDGE_CURVE('',#20674,#20667,#16330,.T.);
#26588=EDGE_CURVE('',#17801,#17784,#16331,.T.);
#26589=EDGE_CURVE('',#20670,#20664,#16332,.T.);
#26590=EDGE_CURVE('',#17782,#17765,#16333,.T.);
#26591=EDGE_CURVE('',#17763,#17745,#16334,.T.);
#26592=EDGE_CURVE('',#20666,#17426,#16335,.T.);
#26593=EDGE_CURVE('',#17566,#20659,#2145,.T.);
#26594=EDGE_CURVE('',#20662,#20655,#16336,.T.);
#26595=EDGE_CURVE('',#20680,#17852,#16337,.T.);
#26596=EDGE_CURVE('',#17850,#17841,#16338,.T.);
#26597=EDGE_CURVE('',#20658,#20651,#16339,.T.);
#26598=EDGE_CURVE('',#17560,#20621,#2146,.T.);
#26599=EDGE_CURVE('',#20624,#20598,#16340,.T.);
#26600=EDGE_CURVE('',#20679,#20660,#16341,.T.);
#26601=EDGE_CURVE('',#20653,#20676,#52,.T.);
#26602=EDGE_CURVE('',#20591,#20614,#16342,.T.);
#26603=EDGE_CURVE('',#20617,#20609,#16343,.T.);
#26604=EDGE_CURVE('',#20677,#20672,#16344,.T.);
#26605=EDGE_CURVE('',#20612,#20605,#16345,.T.);
#26606=EDGE_CURVE('',#20673,#20668,#16346,.T.);
#26607=EDGE_CURVE('',#20669,#20665,#16347,.T.);
#26608=EDGE_CURVE('',#20607,#17230,#16348,.T.);
#26609=EDGE_CURVE('',#20601,#20593,#16349,.T.);
#26610=EDGE_CURVE('',#20661,#20656,#16350,.T.);
#26611=EDGE_CURVE('',#20657,#20652,#16351,.T.);
#26612=EDGE_CURVE('',#20596,#20588,#16352,.T.);
#26613=EDGE_CURVE('',#17554,#20562,#2147,.T.);
#26614=EDGE_CURVE('',#20565,#20553,#16353,.T.);
#26615=EDGE_CURVE('',#20626,#20622,#16354,.T.);
#26616=EDGE_CURVE('',#20556,#20535,#16355,.T.);
#26617=EDGE_CURVE('',#20623,#20599,#16356,.T.);
#26618=EDGE_CURVE('',#20590,#20615,#16357,.T.);
#26619=EDGE_CURVE('',#20528,#20546,#16358,.T.);
#26620=EDGE_CURVE('',#20549,#20542,#16359,.T.);
#26621=EDGE_CURVE('',#20616,#20610,#16360,.T.);
#26622=EDGE_CURVE('',#20611,#20606,#16361,.T.);
#26623=EDGE_CURVE('',#20544,#17234,#16362,.T.);
#26624=EDGE_CURVE('',#20538,#20530,#16363,.T.);
#26625=EDGE_CURVE('',#20600,#20594,#16364,.T.);
#26626=EDGE_CURVE('',#20595,#20589,#53,.T.);
#26627=EDGE_CURVE('',#20533,#20525,#16365,.T.);
#26628=EDGE_CURVE('',#17548,#20503,#2148,.T.);
#26629=EDGE_CURVE('',#20506,#20494,#16366,.T.);
#26630=EDGE_CURVE('',#20567,#20563,#16367,.T.);
#26631=EDGE_CURVE('',#20497,#20485,#16368,.T.);
#26632=EDGE_CURVE('',#20564,#20554,#16369,.T.);
#26633=EDGE_CURVE('',#20488,#20472,#16370,.T.);
#26634=EDGE_CURVE('',#20555,#20536,#16371,.T.);
#26635=EDGE_CURVE('',#20527,#20547,#16372,.T.);
#26636=EDGE_CURVE('',#20465,#20479,#16373,.T.);
#26637=EDGE_CURVE('',#20548,#20543,#16374,.T.);
#26638=EDGE_CURVE('',#20481,#17238,#16375,.T.);
#26639=EDGE_CURVE('',#20475,#20467,#16376,.T.);
#26640=EDGE_CURVE('',#20537,#20531,#54,.T.);
#26641=EDGE_CURVE('',#20532,#20526,#16377,.T.);
#26642=EDGE_CURVE('',#20470,#20462,#16378,.T.);
#26643=EDGE_CURVE('',#17542,#20444,#2149,.T.);
#26644=EDGE_CURVE('',#20447,#20435,#16379,.T.);
#26645=EDGE_CURVE('',#20508,#20504,#16380,.T.);
#26646=EDGE_CURVE('',#20438,#20426,#16381,.T.);
#26647=EDGE_CURVE('',#20505,#20495,#16382,.T.);
#26648=EDGE_CURVE('',#20429,#20417,#16383,.T.);
#26649=EDGE_CURVE('',#20496,#20486,#16384,.T.);
#26650=EDGE_CURVE('',#20420,#20408,#16385,.T.);
#26651=EDGE_CURVE('',#20487,#20473,#55,.T.);
#26652=EDGE_CURVE('',#20464,#20480,#16386,.T.);
#26653=EDGE_CURVE('',#20401,#17242,#16387,.T.);
#26654=EDGE_CURVE('',#20411,#20403,#16388,.T.);
#26655=EDGE_CURVE('',#20474,#20468,#16389,.T.);
#26656=EDGE_CURVE('',#20469,#20463,#16390,.T.);
#26657=EDGE_CURVE('',#20406,#20399,#16391,.T.);
#26658=EDGE_CURVE('',#17536,#20385,#2150,.T.);
#26659=EDGE_CURVE('',#20388,#20376,#16392,.T.);
#26660=EDGE_CURVE('',#20449,#20445,#16393,.T.);
#26661=EDGE_CURVE('',#20379,#20367,#16394,.T.);
#26662=EDGE_CURVE('',#20446,#20436,#16395,.T.);
#26663=EDGE_CURVE('',#20370,#20358,#16396,.T.);
#26664=EDGE_CURVE('',#20437,#20427,#16397,.T.);
#26665=EDGE_CURVE('',#20361,#20349,#16398,.T.);
#26666=EDGE_CURVE('',#20428,#20418,#56,.T.);
#26667=EDGE_CURVE('',#20352,#20340,#16399,.T.);
#26668=EDGE_CURVE('',#20419,#20409,#16400,.T.);
#26669=EDGE_CURVE('',#20343,#20336,#16401,.T.);
#26670=EDGE_CURVE('',#20410,#20404,#16402,.T.);
#26671=EDGE_CURVE('',#20405,#20400,#16403,.T.);
#26672=EDGE_CURVE('',#20338,#17246,#16404,.T.);
#26673=EDGE_CURVE('',#17530,#20326,#2151,.T.);
#26674=EDGE_CURVE('',#20329,#20317,#16405,.T.);
#26675=EDGE_CURVE('',#20390,#20386,#16406,.T.);
#26676=EDGE_CURVE('',#20320,#20308,#16407,.T.);
#26677=EDGE_CURVE('',#20387,#20377,#16408,.T.);
#26678=EDGE_CURVE('',#20311,#20299,#16409,.T.);
#26679=EDGE_CURVE('',#20378,#20368,#16410,.T.);
#26680=EDGE_CURVE('',#20302,#20290,#16411,.T.);
#26681=EDGE_CURVE('',#20369,#20359,#57,.T.);
#26682=EDGE_CURVE('',#20293,#20281,#16412,.T.);
#26683=EDGE_CURVE('',#20360,#20350,#16413,.T.);
#26684=EDGE_CURVE('',#20284,#20273,#16414,.T.);
#26685=EDGE_CURVE('',#20351,#20341,#16415,.T.);
#26686=EDGE_CURVE('',#20342,#20337,#16416,.T.);
#26687=EDGE_CURVE('',#20275,#17250,#16417,.T.);
#26688=EDGE_CURVE('',#17524,#20267,#2152,.T.);
#26689=EDGE_CURVE('',#20270,#20258,#16418,.T.);
#26690=EDGE_CURVE('',#20331,#20327,#16419,.T.);
#26691=EDGE_CURVE('',#20261,#20249,#16420,.T.);
#26692=EDGE_CURVE('',#20328,#20318,#16421,.T.);
#26693=EDGE_CURVE('',#20252,#20240,#16422,.T.);
#26694=EDGE_CURVE('',#20319,#20309,#16423,.T.);
#26695=EDGE_CURVE('',#20243,#20231,#16424,.T.);
#26696=EDGE_CURVE('',#20310,#20300,#58,.T.);
#26697=EDGE_CURVE('',#20234,#20222,#16425,.T.);
#26698=EDGE_CURVE('',#20301,#20291,#16426,.T.);
#26699=EDGE_CURVE('',#20225,#20214,#16427,.T.);
#26700=EDGE_CURVE('',#20292,#20282,#16428,.T.);
#26701=EDGE_CURVE('',#20283,#20274,#16429,.T.);
#26702=EDGE_CURVE('',#20216,#17254,#16430,.T.);
#26703=EDGE_CURVE('',#17518,#20208,#2153,.T.);
#26704=EDGE_CURVE('',#20211,#20199,#16431,.T.);
#26705=EDGE_CURVE('',#20272,#20268,#16432,.T.);
#26706=EDGE_CURVE('',#20202,#20190,#16433,.T.);
#26707=EDGE_CURVE('',#20269,#20259,#16434,.T.);
#26708=EDGE_CURVE('',#20193,#20181,#16435,.T.);
#26709=EDGE_CURVE('',#20260,#20250,#16436,.T.);
#26710=EDGE_CURVE('',#20184,#20172,#16437,.T.);
#26711=EDGE_CURVE('',#20251,#20241,#59,.T.);
#26712=EDGE_CURVE('',#20175,#20163,#16438,.T.);
#26713=EDGE_CURVE('',#20242,#20232,#16439,.T.);
#26714=EDGE_CURVE('',#20166,#20155,#16440,.T.);
#26715=EDGE_CURVE('',#20233,#20223,#16441,.T.);
#26716=EDGE_CURVE('',#20224,#20215,#16442,.T.);
#26717=EDGE_CURVE('',#20157,#17258,#16443,.T.);
#26718=EDGE_CURVE('',#17512,#20149,#2154,.T.);
#26719=EDGE_CURVE('',#20152,#20140,#16444,.T.);
#26720=EDGE_CURVE('',#20213,#20209,#16445,.T.);
#26721=EDGE_CURVE('',#20143,#20131,#16446,.T.);
#26722=EDGE_CURVE('',#20210,#20200,#16447,.T.);
#26723=EDGE_CURVE('',#20134,#20122,#16448,.T.);
#26724=EDGE_CURVE('',#20201,#20191,#16449,.T.);
#26725=EDGE_CURVE('',#20125,#20113,#16450,.T.);
#26726=EDGE_CURVE('',#20192,#20182,#60,.T.);
#26727=EDGE_CURVE('',#20116,#20104,#16451,.T.);
#26728=EDGE_CURVE('',#20183,#20173,#16452,.T.);
#26729=EDGE_CURVE('',#20107,#20096,#16453,.T.);
#26730=EDGE_CURVE('',#20174,#20164,#16454,.T.);
#26731=EDGE_CURVE('',#20165,#20156,#16455,.T.);
#26732=EDGE_CURVE('',#20098,#17262,#16456,.T.);
#26733=EDGE_CURVE('',#17506,#20090,#2155,.T.);
#26734=EDGE_CURVE('',#20093,#20081,#16457,.T.);
#26735=EDGE_CURVE('',#20154,#20150,#16458,.T.);
#26736=EDGE_CURVE('',#20084,#20072,#16459,.T.);
#26737=EDGE_CURVE('',#20151,#20141,#16460,.T.);
#26738=EDGE_CURVE('',#20075,#20063,#16461,.T.);
#26739=EDGE_CURVE('',#20142,#20132,#16462,.T.);
#26740=EDGE_CURVE('',#20066,#20054,#16463,.T.);
#26741=EDGE_CURVE('',#20133,#20123,#61,.T.);
#26742=EDGE_CURVE('',#20057,#20045,#16464,.T.);
#26743=EDGE_CURVE('',#20124,#20114,#16465,.T.);
#26744=EDGE_CURVE('',#20048,#20037,#16466,.T.);
#26745=EDGE_CURVE('',#20115,#20105,#16467,.T.);
#26746=EDGE_CURVE('',#20106,#20097,#16468,.T.);
#26747=EDGE_CURVE('',#20039,#17266,#16469,.T.);
#26748=EDGE_CURVE('',#17500,#20031,#2156,.T.);
#26749=EDGE_CURVE('',#20034,#20022,#16470,.T.);
#26750=EDGE_CURVE('',#20095,#20091,#16471,.T.);
#26751=EDGE_CURVE('',#20025,#20013,#16472,.T.);
#26752=EDGE_CURVE('',#20092,#20082,#16473,.T.);
#26753=EDGE_CURVE('',#20016,#20004,#16474,.T.);
#26754=EDGE_CURVE('',#20083,#20073,#16475,.T.);
#26755=EDGE_CURVE('',#20007,#19995,#16476,.T.);
#26756=EDGE_CURVE('',#20074,#20064,#62,.T.);
#26757=EDGE_CURVE('',#19998,#19986,#16477,.T.);
#26758=EDGE_CURVE('',#20065,#20055,#16478,.T.);
#26759=EDGE_CURVE('',#19989,#19978,#16479,.T.);
#26760=EDGE_CURVE('',#20056,#20046,#16480,.T.);
#26761=EDGE_CURVE('',#20047,#20038,#16481,.T.);
#26762=EDGE_CURVE('',#19980,#17270,#16482,.T.);
#26763=EDGE_CURVE('',#17494,#19972,#2157,.T.);
#26764=EDGE_CURVE('',#19975,#19963,#16483,.T.);
#26765=EDGE_CURVE('',#20036,#20032,#16484,.T.);
#26766=EDGE_CURVE('',#19966,#19954,#16485,.T.);
#26767=EDGE_CURVE('',#20033,#20023,#16486,.T.);
#26768=EDGE_CURVE('',#19957,#19945,#16487,.T.);
#26769=EDGE_CURVE('',#20024,#20014,#16488,.T.);
#26770=EDGE_CURVE('',#19948,#19936,#16489,.T.);
#26771=EDGE_CURVE('',#20015,#20005,#63,.T.);
#26772=EDGE_CURVE('',#19939,#19927,#16490,.T.);
#26773=EDGE_CURVE('',#20006,#19996,#16491,.T.);
#26774=EDGE_CURVE('',#19930,#19919,#16492,.T.);
#26775=EDGE_CURVE('',#19997,#19987,#16493,.T.);
#26776=EDGE_CURVE('',#19988,#19979,#16494,.T.);
#26777=EDGE_CURVE('',#19921,#17274,#16495,.T.);
#26778=EDGE_CURVE('',#17488,#19913,#2158,.T.);
#26779=EDGE_CURVE('',#19916,#19904,#16496,.T.);
#26780=EDGE_CURVE('',#19977,#19973,#16497,.T.);
#26781=EDGE_CURVE('',#19907,#19895,#16498,.T.);
#26782=EDGE_CURVE('',#19974,#19964,#16499,.T.);
#26783=EDGE_CURVE('',#19898,#19886,#16500,.T.);
#26784=EDGE_CURVE('',#19965,#19955,#16501,.T.);
#26785=EDGE_CURVE('',#19889,#19877,#16502,.T.);
#26786=EDGE_CURVE('',#19956,#19946,#64,.T.);
#26787=EDGE_CURVE('',#19880,#19868,#16503,.T.);
#26788=EDGE_CURVE('',#19947,#19937,#16504,.T.);
#26789=EDGE_CURVE('',#19871,#19860,#16505,.T.);
#26790=EDGE_CURVE('',#19938,#19928,#16506,.T.);
#26791=EDGE_CURVE('',#19929,#19920,#16507,.T.);
#26792=EDGE_CURVE('',#19862,#17278,#16508,.T.);
#26793=EDGE_CURVE('',#17482,#19854,#2159,.T.);
#26794=EDGE_CURVE('',#19857,#19845,#16509,.T.);
#26795=EDGE_CURVE('',#19918,#19914,#16510,.T.);
#26796=EDGE_CURVE('',#19848,#19836,#16511,.T.);
#26797=EDGE_CURVE('',#19915,#19905,#16512,.T.);
#26798=EDGE_CURVE('',#19839,#19827,#16513,.T.);
#26799=EDGE_CURVE('',#19906,#19896,#16514,.T.);
#26800=EDGE_CURVE('',#19830,#19818,#16515,.T.);
#26801=EDGE_CURVE('',#19897,#19887,#65,.T.);
#26802=EDGE_CURVE('',#19821,#19809,#16516,.T.);
#26803=EDGE_CURVE('',#19888,#19878,#16517,.T.);
#26804=EDGE_CURVE('',#19812,#19801,#16518,.T.);
#26805=EDGE_CURVE('',#19879,#19869,#16519,.T.);
#26806=EDGE_CURVE('',#19870,#19861,#16520,.T.);
#26807=EDGE_CURVE('',#19803,#17282,#16521,.T.);
#26808=EDGE_CURVE('',#17476,#19795,#2160,.T.);
#26809=EDGE_CURVE('',#19798,#19786,#16522,.T.);
#26810=EDGE_CURVE('',#19859,#19855,#16523,.T.);
#26811=EDGE_CURVE('',#19789,#19777,#16524,.T.);
#26812=EDGE_CURVE('',#19856,#19846,#16525,.T.);
#26813=EDGE_CURVE('',#19780,#19768,#16526,.T.);
#26814=EDGE_CURVE('',#19847,#19837,#16527,.T.);
#26815=EDGE_CURVE('',#19771,#19759,#16528,.T.);
#26816=EDGE_CURVE('',#19838,#19828,#66,.T.);
#26817=EDGE_CURVE('',#19762,#19750,#16529,.T.);
#26818=EDGE_CURVE('',#19829,#19819,#16530,.T.);
#26819=EDGE_CURVE('',#19753,#19742,#16531,.T.);
#26820=EDGE_CURVE('',#19820,#19810,#16532,.T.);
#26821=EDGE_CURVE('',#19811,#19802,#16533,.T.);
#26822=EDGE_CURVE('',#19744,#17286,#16534,.T.);
#26823=EDGE_CURVE('',#17470,#19736,#2161,.T.);
#26824=EDGE_CURVE('',#19739,#19727,#16535,.T.);
#26825=EDGE_CURVE('',#19800,#19796,#16536,.T.);
#26826=EDGE_CURVE('',#19730,#19718,#16537,.T.);
#26827=EDGE_CURVE('',#19797,#19787,#16538,.T.);
#26828=EDGE_CURVE('',#19721,#19709,#16539,.T.);
#26829=EDGE_CURVE('',#19788,#19778,#16540,.T.);
#26830=EDGE_CURVE('',#19712,#19700,#16541,.T.);
#26831=EDGE_CURVE('',#19779,#19769,#67,.T.);
#26832=EDGE_CURVE('',#19703,#19691,#16542,.T.);
#26833=EDGE_CURVE('',#19770,#19760,#16543,.T.);
#26834=EDGE_CURVE('',#19694,#19683,#16544,.T.);
#26835=EDGE_CURVE('',#19761,#19751,#16545,.T.);
#26836=EDGE_CURVE('',#19752,#19743,#16546,.T.);
#26837=EDGE_CURVE('',#19685,#17290,#16547,.T.);
#26838=EDGE_CURVE('',#17464,#19677,#2162,.T.);
#26839=EDGE_CURVE('',#19680,#19668,#16548,.T.);
#26840=EDGE_CURVE('',#19741,#19737,#16549,.T.);
#26841=EDGE_CURVE('',#19671,#19659,#16550,.T.);
#26842=EDGE_CURVE('',#19738,#19728,#16551,.T.);
#26843=EDGE_CURVE('',#19662,#19650,#16552,.T.);
#26844=EDGE_CURVE('',#19729,#19719,#16553,.T.);
#26845=EDGE_CURVE('',#19653,#19641,#16554,.T.);
#26846=EDGE_CURVE('',#19720,#19710,#68,.T.);
#26847=EDGE_CURVE('',#19644,#19632,#16555,.T.);
#26848=EDGE_CURVE('',#19711,#19701,#16556,.T.);
#26849=EDGE_CURVE('',#19635,#19624,#16557,.T.);
#26850=EDGE_CURVE('',#19702,#19692,#16558,.T.);
#26851=EDGE_CURVE('',#19693,#19684,#16559,.T.);
#26852=EDGE_CURVE('',#19626,#17294,#16560,.T.);
#26853=EDGE_CURVE('',#17458,#19618,#2163,.T.);
#26854=EDGE_CURVE('',#19621,#19609,#16561,.T.);
#26855=EDGE_CURVE('',#19682,#19678,#16562,.T.);
#26856=EDGE_CURVE('',#19612,#19600,#16563,.T.);
#26857=EDGE_CURVE('',#19679,#19669,#16564,.T.);
#26858=EDGE_CURVE('',#19603,#19591,#16565,.T.);
#26859=EDGE_CURVE('',#19670,#19660,#16566,.T.);
#26860=EDGE_CURVE('',#19594,#19582,#16567,.T.);
#26861=EDGE_CURVE('',#19661,#19651,#69,.T.);
#26862=EDGE_CURVE('',#19585,#19573,#16568,.T.);
#26863=EDGE_CURVE('',#19652,#19642,#16569,.T.);
#26864=EDGE_CURVE('',#19576,#19565,#16570,.T.);
#26865=EDGE_CURVE('',#19643,#19633,#16571,.T.);
#26866=EDGE_CURVE('',#19634,#19625,#16572,.T.);
#26867=EDGE_CURVE('',#19567,#17298,#16573,.T.);
#26868=EDGE_CURVE('',#17452,#19559,#2164,.T.);
#26869=EDGE_CURVE('',#19562,#19550,#16574,.T.);
#26870=EDGE_CURVE('',#19623,#19619,#16575,.T.);
#26871=EDGE_CURVE('',#19553,#19541,#16576,.T.);
#26872=EDGE_CURVE('',#19620,#19610,#16577,.T.);
#26873=EDGE_CURVE('',#19544,#19532,#16578,.T.);
#26874=EDGE_CURVE('',#19611,#19601,#16579,.T.);
#26875=EDGE_CURVE('',#19535,#19523,#16580,.T.);
#26876=EDGE_CURVE('',#19602,#19592,#70,.T.);
#26877=EDGE_CURVE('',#19526,#19514,#16581,.T.);
#26878=EDGE_CURVE('',#19593,#19583,#16582,.T.);
#26879=EDGE_CURVE('',#19517,#19506,#16583,.T.);
#26880=EDGE_CURVE('',#19584,#19574,#16584,.T.);
#26881=EDGE_CURVE('',#19575,#19566,#16585,.T.);
#26882=EDGE_CURVE('',#19508,#17302,#16586,.T.);
#26883=EDGE_CURVE('',#17446,#19500,#2165,.T.);
#26884=EDGE_CURVE('',#19503,#19491,#16587,.T.);
#26885=EDGE_CURVE('',#19564,#19560,#16588,.T.);
#26886=EDGE_CURVE('',#19494,#19482,#16589,.T.);
#26887=EDGE_CURVE('',#19561,#19551,#16590,.T.);
#26888=EDGE_CURVE('',#19485,#19473,#16591,.T.);
#26889=EDGE_CURVE('',#19552,#19542,#16592,.T.);
#26890=EDGE_CURVE('',#19476,#19464,#16593,.T.);
#26891=EDGE_CURVE('',#19543,#19533,#71,.T.);
#26892=EDGE_CURVE('',#19467,#19455,#16594,.T.);
#26893=EDGE_CURVE('',#19534,#19524,#16595,.T.);
#26894=EDGE_CURVE('',#19458,#19447,#16596,.T.);
#26895=EDGE_CURVE('',#19525,#19515,#16597,.T.);
#26896=EDGE_CURVE('',#19516,#19507,#16598,.T.);
#26897=EDGE_CURVE('',#19449,#17306,#16599,.T.);
#26898=EDGE_CURVE('',#17440,#19441,#2166,.T.);
#26899=EDGE_CURVE('',#19444,#19432,#16600,.T.);
#26900=EDGE_CURVE('',#19505,#19501,#16601,.T.);
#26901=EDGE_CURVE('',#19435,#19423,#16602,.T.);
#26902=EDGE_CURVE('',#19502,#19492,#16603,.T.);
#26903=EDGE_CURVE('',#19426,#19414,#16604,.T.);
#26904=EDGE_CURVE('',#19493,#19483,#16605,.T.);
#26905=EDGE_CURVE('',#19417,#19405,#16606,.T.);
#26906=EDGE_CURVE('',#19484,#19474,#72,.T.);
#26907=EDGE_CURVE('',#19408,#19396,#16607,.T.);
#26908=EDGE_CURVE('',#19475,#19465,#16608,.T.);
#26909=EDGE_CURVE('',#19399,#19388,#16609,.T.);
#26910=EDGE_CURVE('',#19466,#19456,#16610,.T.);
#26911=EDGE_CURVE('',#19457,#19448,#16611,.T.);
#26912=EDGE_CURVE('',#19390,#17310,#16612,.T.);
#26913=EDGE_CURVE('',#17434,#19382,#2167,.T.);
#26914=EDGE_CURVE('',#19385,#19373,#16613,.T.);
#26915=EDGE_CURVE('',#19446,#19442,#16614,.T.);
#26916=EDGE_CURVE('',#19376,#19364,#16615,.T.);
#26917=EDGE_CURVE('',#19443,#19433,#16616,.T.);
#26918=EDGE_CURVE('',#19367,#19355,#16617,.T.);
#26919=EDGE_CURVE('',#19434,#19424,#16618,.T.);
#26920=EDGE_CURVE('',#19358,#19346,#16619,.T.);
#26921=EDGE_CURVE('',#19425,#19415,#73,.T.);
#26922=EDGE_CURVE('',#19349,#19337,#16620,.T.);
#26923=EDGE_CURVE('',#19416,#19406,#16621,.T.);
#26924=EDGE_CURVE('',#19340,#19329,#16622,.T.);
#26925=EDGE_CURVE('',#19407,#19397,#16623,.T.);
#26926=EDGE_CURVE('',#19398,#19389,#16624,.T.);
#26927=EDGE_CURVE('',#19331,#17314,#16625,.T.);
#26928=EDGE_CURVE('',#17728,#19323,#2168,.T.);
#26929=EDGE_CURVE('',#19326,#19314,#16626,.T.);
#26930=EDGE_CURVE('',#19387,#19383,#16627,.T.);
#26931=EDGE_CURVE('',#19317,#19305,#16628,.T.);
#26932=EDGE_CURVE('',#19384,#19374,#16629,.T.);
#26933=EDGE_CURVE('',#19308,#19296,#16630,.T.);
#26934=EDGE_CURVE('',#19375,#19365,#16631,.T.);
#26935=EDGE_CURVE('',#19299,#19287,#16632,.T.);
#26936=EDGE_CURVE('',#19366,#19356,#74,.T.);
#26937=EDGE_CURVE('',#19290,#19278,#16633,.T.);
#26938=EDGE_CURVE('',#19357,#19347,#16634,.T.);
#26939=EDGE_CURVE('',#19281,#19270,#16635,.T.);
#26940=EDGE_CURVE('',#19348,#19338,#16636,.T.);
#26941=EDGE_CURVE('',#19339,#19330,#16637,.T.);
#26942=EDGE_CURVE('',#19272,#17318,#16638,.T.);
#26943=EDGE_CURVE('',#17722,#19264,#2169,.T.);
#26944=EDGE_CURVE('',#19267,#19255,#16639,.T.);
#26945=EDGE_CURVE('',#19328,#19324,#16640,.T.);
#26946=EDGE_CURVE('',#19258,#19246,#16641,.T.);
#26947=EDGE_CURVE('',#19325,#19315,#16642,.T.);
#26948=EDGE_CURVE('',#19249,#19237,#16643,.T.);
#26949=EDGE_CURVE('',#19316,#19306,#16644,.T.);
#26950=EDGE_CURVE('',#19240,#19228,#16645,.T.);
#26951=EDGE_CURVE('',#19307,#19297,#75,.T.);
#26952=EDGE_CURVE('',#19231,#19219,#16646,.T.);
#26953=EDGE_CURVE('',#19298,#19288,#16647,.T.);
#26954=EDGE_CURVE('',#19222,#19211,#16648,.T.);
#26955=EDGE_CURVE('',#19289,#19279,#16649,.T.);
#26956=EDGE_CURVE('',#19280,#19271,#16650,.T.);
#26957=EDGE_CURVE('',#19213,#17322,#16651,.T.);
#26958=EDGE_CURVE('',#17716,#19205,#2170,.T.);
#26959=EDGE_CURVE('',#19208,#19196,#16652,.T.);
#26960=EDGE_CURVE('',#19269,#19265,#16653,.T.);
#26961=EDGE_CURVE('',#19199,#19187,#16654,.T.);
#26962=EDGE_CURVE('',#19266,#19256,#16655,.T.);
#26963=EDGE_CURVE('',#19190,#19178,#16656,.T.);
#26964=EDGE_CURVE('',#19257,#19247,#16657,.T.);
#26965=EDGE_CURVE('',#19181,#19169,#16658,.T.);
#26966=EDGE_CURVE('',#19248,#19238,#76,.T.);
#26967=EDGE_CURVE('',#19172,#19160,#16659,.T.);
#26968=EDGE_CURVE('',#19239,#19229,#16660,.T.);
#26969=EDGE_CURVE('',#19163,#19152,#16661,.T.);
#26970=EDGE_CURVE('',#19230,#19220,#16662,.T.);
#26971=EDGE_CURVE('',#19221,#19212,#16663,.T.);
#26972=EDGE_CURVE('',#19154,#17326,#16664,.T.);
#26973=EDGE_CURVE('',#17710,#19146,#2171,.T.);
#26974=EDGE_CURVE('',#19149,#19137,#16665,.T.);
#26975=EDGE_CURVE('',#19210,#19206,#16666,.T.);
#26976=EDGE_CURVE('',#19140,#19128,#16667,.T.);
#26977=EDGE_CURVE('',#19207,#19197,#16668,.T.);
#26978=EDGE_CURVE('',#19131,#19119,#16669,.T.);
#26979=EDGE_CURVE('',#19198,#19188,#16670,.T.);
#26980=EDGE_CURVE('',#19122,#19110,#16671,.T.);
#26981=EDGE_CURVE('',#19189,#19179,#77,.T.);
#26982=EDGE_CURVE('',#19113,#19101,#16672,.T.);
#26983=EDGE_CURVE('',#19180,#19170,#16673,.T.);
#26984=EDGE_CURVE('',#19104,#19093,#16674,.T.);
#26985=EDGE_CURVE('',#19171,#19161,#16675,.T.);
#26986=EDGE_CURVE('',#19162,#19153,#16676,.T.);
#26987=EDGE_CURVE('',#19095,#17330,#16677,.T.);
#26988=EDGE_CURVE('',#17704,#19087,#2172,.T.);
#26989=EDGE_CURVE('',#19090,#19078,#16678,.T.);
#26990=EDGE_CURVE('',#19151,#19147,#16679,.T.);
#26991=EDGE_CURVE('',#19081,#19069,#16680,.T.);
#26992=EDGE_CURVE('',#19148,#19138,#16681,.T.);
#26993=EDGE_CURVE('',#19072,#19060,#16682,.T.);
#26994=EDGE_CURVE('',#19139,#19129,#16683,.T.);
#26995=EDGE_CURVE('',#19063,#19051,#16684,.T.);
#26996=EDGE_CURVE('',#19130,#19120,#78,.T.);
#26997=EDGE_CURVE('',#19054,#19042,#16685,.T.);
#26998=EDGE_CURVE('',#19121,#19111,#16686,.T.);
#26999=EDGE_CURVE('',#19045,#19034,#16687,.T.);
#27000=EDGE_CURVE('',#19112,#19102,#16688,.T.);
#27001=EDGE_CURVE('',#19103,#19094,#16689,.T.);
#27002=EDGE_CURVE('',#19036,#17334,#16690,.T.);
#27003=EDGE_CURVE('',#17698,#19028,#2173,.T.);
#27004=EDGE_CURVE('',#19031,#19019,#16691,.T.);
#27005=EDGE_CURVE('',#19092,#19088,#16692,.T.);
#27006=EDGE_CURVE('',#19022,#19010,#16693,.T.);
#27007=EDGE_CURVE('',#19089,#19079,#16694,.T.);
#27008=EDGE_CURVE('',#19013,#19001,#16695,.T.);
#27009=EDGE_CURVE('',#19080,#19070,#16696,.T.);
#27010=EDGE_CURVE('',#19004,#18992,#16697,.T.);
#27011=EDGE_CURVE('',#19071,#19061,#79,.T.);
#27012=EDGE_CURVE('',#18995,#18983,#16698,.T.);
#27013=EDGE_CURVE('',#19062,#19052,#16699,.T.);
#27014=EDGE_CURVE('',#18986,#18975,#16700,.T.);
#27015=EDGE_CURVE('',#19053,#19043,#16701,.T.);
#27016=EDGE_CURVE('',#19044,#19035,#16702,.T.);
#27017=EDGE_CURVE('',#18977,#17338,#16703,.T.);
#27018=EDGE_CURVE('',#17692,#18969,#2174,.T.);
#27019=EDGE_CURVE('',#18972,#18960,#16704,.T.);
#27020=EDGE_CURVE('',#19033,#19029,#16705,.T.);
#27021=EDGE_CURVE('',#18963,#18951,#16706,.T.);
#27022=EDGE_CURVE('',#19030,#19020,#16707,.T.);
#27023=EDGE_CURVE('',#18954,#18942,#16708,.T.);
#27024=EDGE_CURVE('',#19021,#19011,#16709,.T.);
#27025=EDGE_CURVE('',#18945,#18933,#16710,.T.);
#27026=EDGE_CURVE('',#19012,#19002,#80,.T.);
#27027=EDGE_CURVE('',#18936,#18924,#16711,.T.);
#27028=EDGE_CURVE('',#19003,#18993,#16712,.T.);
#27029=EDGE_CURVE('',#18927,#18916,#16713,.T.);
#27030=EDGE_CURVE('',#18994,#18984,#16714,.T.);
#27031=EDGE_CURVE('',#18985,#18976,#16715,.T.);
#27032=EDGE_CURVE('',#18918,#17342,#16716,.T.);
#27033=EDGE_CURVE('',#17686,#18910,#2175,.T.);
#27034=EDGE_CURVE('',#18913,#18901,#16717,.T.);
#27035=EDGE_CURVE('',#18974,#18970,#16718,.T.);
#27036=EDGE_CURVE('',#18904,#18892,#16719,.T.);
#27037=EDGE_CURVE('',#18971,#18961,#16720,.T.);
#27038=EDGE_CURVE('',#18895,#18883,#16721,.T.);
#27039=EDGE_CURVE('',#18962,#18952,#16722,.T.);
#27040=EDGE_CURVE('',#18886,#18874,#16723,.T.);
#27041=EDGE_CURVE('',#18953,#18943,#81,.T.);
#27042=EDGE_CURVE('',#18877,#18865,#16724,.T.);
#27043=EDGE_CURVE('',#18944,#18934,#16725,.T.);
#27044=EDGE_CURVE('',#18868,#18857,#16726,.T.);
#27045=EDGE_CURVE('',#18935,#18925,#16727,.T.);
#27046=EDGE_CURVE('',#18926,#18917,#16728,.T.);
#27047=EDGE_CURVE('',#18859,#17346,#16729,.T.);
#27048=EDGE_CURVE('',#17680,#18851,#2176,.T.);
#27049=EDGE_CURVE('',#18854,#18842,#16730,.T.);
#27050=EDGE_CURVE('',#18915,#18911,#16731,.T.);
#27051=EDGE_CURVE('',#18845,#18833,#16732,.T.);
#27052=EDGE_CURVE('',#18912,#18902,#16733,.T.);
#27053=EDGE_CURVE('',#18836,#18824,#16734,.T.);
#27054=EDGE_CURVE('',#18903,#18893,#16735,.T.);
#27055=EDGE_CURVE('',#18827,#18815,#16736,.T.);
#27056=EDGE_CURVE('',#18894,#18884,#82,.T.);
#27057=EDGE_CURVE('',#18818,#18806,#16737,.T.);
#27058=EDGE_CURVE('',#18885,#18875,#16738,.T.);
#27059=EDGE_CURVE('',#18809,#18798,#16739,.T.);
#27060=EDGE_CURVE('',#18876,#18866,#16740,.T.);
#27061=EDGE_CURVE('',#18867,#18858,#16741,.T.);
#27062=EDGE_CURVE('',#18800,#17350,#16742,.T.);
#27063=EDGE_CURVE('',#17674,#18792,#2177,.T.);
#27064=EDGE_CURVE('',#18795,#18783,#16743,.T.);
#27065=EDGE_CURVE('',#18856,#18852,#16744,.T.);
#27066=EDGE_CURVE('',#18786,#18774,#16745,.T.);
#27067=EDGE_CURVE('',#18853,#18843,#16746,.T.);
#27068=EDGE_CURVE('',#18777,#18765,#16747,.T.);
#27069=EDGE_CURVE('',#18844,#18834,#16748,.T.);
#27070=EDGE_CURVE('',#18768,#18756,#16749,.T.);
#27071=EDGE_CURVE('',#18835,#18825,#83,.T.);
#27072=EDGE_CURVE('',#18759,#18747,#16750,.T.);
#27073=EDGE_CURVE('',#18826,#18816,#16751,.T.);
#27074=EDGE_CURVE('',#18750,#18739,#16752,.T.);
#27075=EDGE_CURVE('',#18817,#18807,#16753,.T.);
#27076=EDGE_CURVE('',#18808,#18799,#16754,.T.);
#27077=EDGE_CURVE('',#18741,#17354,#16755,.T.);
#27078=EDGE_CURVE('',#17668,#18733,#2178,.T.);
#27079=EDGE_CURVE('',#18736,#18724,#16756,.T.);
#27080=EDGE_CURVE('',#18797,#18793,#16757,.T.);
#27081=EDGE_CURVE('',#18727,#18715,#16758,.T.);
#27082=EDGE_CURVE('',#18794,#18784,#16759,.T.);
#27083=EDGE_CURVE('',#18718,#18706,#16760,.T.);
#27084=EDGE_CURVE('',#18785,#18775,#16761,.T.);
#27085=EDGE_CURVE('',#18709,#18697,#16762,.T.);
#27086=EDGE_CURVE('',#18776,#18766,#84,.T.);
#27087=EDGE_CURVE('',#18700,#18688,#16763,.T.);
#27088=EDGE_CURVE('',#18767,#18757,#16764,.T.);
#27089=EDGE_CURVE('',#18691,#18680,#16765,.T.);
#27090=EDGE_CURVE('',#18758,#18748,#16766,.T.);
#27091=EDGE_CURVE('',#18749,#18740,#16767,.T.);
#27092=EDGE_CURVE('',#18682,#17358,#16768,.T.);
#27093=EDGE_CURVE('',#17662,#18674,#2179,.T.);
#27094=EDGE_CURVE('',#18677,#18665,#16769,.T.);
#27095=EDGE_CURVE('',#18738,#18734,#16770,.T.);
#27096=EDGE_CURVE('',#18668,#18656,#16771,.T.);
#27097=EDGE_CURVE('',#18735,#18725,#16772,.T.);
#27098=EDGE_CURVE('',#18659,#18647,#16773,.T.);
#27099=EDGE_CURVE('',#18726,#18716,#16774,.T.);
#27100=EDGE_CURVE('',#18650,#18638,#16775,.T.);
#27101=EDGE_CURVE('',#18717,#18707,#85,.T.);
#27102=EDGE_CURVE('',#18641,#18629,#16776,.T.);
#27103=EDGE_CURVE('',#18708,#18698,#16777,.T.);
#27104=EDGE_CURVE('',#18632,#18621,#16778,.T.);
#27105=EDGE_CURVE('',#18699,#18689,#16779,.T.);
#27106=EDGE_CURVE('',#18690,#18681,#16780,.T.);
#27107=EDGE_CURVE('',#18623,#17362,#16781,.T.);
#27108=EDGE_CURVE('',#17656,#18615,#2180,.T.);
#27109=EDGE_CURVE('',#18618,#18606,#16782,.T.);
#27110=EDGE_CURVE('',#18679,#18675,#16783,.T.);
#27111=EDGE_CURVE('',#18609,#18597,#16784,.T.);
#27112=EDGE_CURVE('',#18676,#18666,#16785,.T.);
#27113=EDGE_CURVE('',#18600,#18588,#16786,.T.);
#27114=EDGE_CURVE('',#18667,#18657,#16787,.T.);
#27115=EDGE_CURVE('',#18591,#18579,#16788,.T.);
#27116=EDGE_CURVE('',#18658,#18648,#86,.T.);
#27117=EDGE_CURVE('',#18582,#18570,#16789,.T.);
#27118=EDGE_CURVE('',#18649,#18639,#16790,.T.);
#27119=EDGE_CURVE('',#18573,#18562,#16791,.T.);
#27120=EDGE_CURVE('',#18640,#18630,#16792,.T.);
#27121=EDGE_CURVE('',#18631,#18622,#16793,.T.);
#27122=EDGE_CURVE('',#18564,#17366,#16794,.T.);
#27123=EDGE_CURVE('',#17650,#18556,#2181,.T.);
#27124=EDGE_CURVE('',#18559,#18547,#16795,.T.);
#27125=EDGE_CURVE('',#18620,#18616,#16796,.T.);
#27126=EDGE_CURVE('',#18550,#18538,#16797,.T.);
#27127=EDGE_CURVE('',#18617,#18607,#16798,.T.);
#27128=EDGE_CURVE('',#18541,#18529,#16799,.T.);
#27129=EDGE_CURVE('',#18608,#18598,#16800,.T.);
#27130=EDGE_CURVE('',#18532,#18520,#16801,.T.);
#27131=EDGE_CURVE('',#18599,#18589,#87,.T.);
#27132=EDGE_CURVE('',#18523,#18511,#16802,.T.);
#27133=EDGE_CURVE('',#18590,#18580,#16803,.T.);
#27134=EDGE_CURVE('',#18514,#18503,#16804,.T.);
#27135=EDGE_CURVE('',#18581,#18571,#16805,.T.);
#27136=EDGE_CURVE('',#18572,#18563,#16806,.T.);
#27137=EDGE_CURVE('',#18505,#17370,#16807,.T.);
#27138=EDGE_CURVE('',#17644,#18497,#2182,.T.);
#27139=EDGE_CURVE('',#18500,#18488,#16808,.T.);
#27140=EDGE_CURVE('',#18561,#18557,#16809,.T.);
#27141=EDGE_CURVE('',#18491,#18479,#16810,.T.);
#27142=EDGE_CURVE('',#18558,#18548,#16811,.T.);
#27143=EDGE_CURVE('',#18482,#18470,#16812,.T.);
#27144=EDGE_CURVE('',#18549,#18539,#16813,.T.);
#27145=EDGE_CURVE('',#18473,#18461,#16814,.T.);
#27146=EDGE_CURVE('',#18540,#18530,#88,.T.);
#27147=EDGE_CURVE('',#18464,#18452,#16815,.T.);
#27148=EDGE_CURVE('',#18531,#18521,#16816,.T.);
#27149=EDGE_CURVE('',#18455,#18444,#16817,.T.);
#27150=EDGE_CURVE('',#18522,#18512,#16818,.T.);
#27151=EDGE_CURVE('',#18513,#18504,#16819,.T.);
#27152=EDGE_CURVE('',#18446,#17374,#16820,.T.);
#27153=EDGE_CURVE('',#17638,#18438,#2183,.T.);
#27154=EDGE_CURVE('',#18441,#18429,#16821,.T.);
#27155=EDGE_CURVE('',#18502,#18498,#16822,.T.);
#27156=EDGE_CURVE('',#18432,#18420,#16823,.T.);
#27157=EDGE_CURVE('',#18499,#18489,#16824,.T.);
#27158=EDGE_CURVE('',#18423,#18411,#16825,.T.);
#27159=EDGE_CURVE('',#18490,#18480,#16826,.T.);
#27160=EDGE_CURVE('',#18414,#18402,#16827,.T.);
#27161=EDGE_CURVE('',#18481,#18471,#89,.T.);
#27162=EDGE_CURVE('',#18405,#18393,#16828,.T.);
#27163=EDGE_CURVE('',#18472,#18462,#16829,.T.);
#27164=EDGE_CURVE('',#18396,#18385,#16830,.T.);
#27165=EDGE_CURVE('',#18463,#18453,#16831,.T.);
#27166=EDGE_CURVE('',#18454,#18445,#16832,.T.);
#27167=EDGE_CURVE('',#18387,#17378,#16833,.T.);
#27168=EDGE_CURVE('',#17632,#18379,#2184,.T.);
#27169=EDGE_CURVE('',#18382,#18370,#16834,.T.);
#27170=EDGE_CURVE('',#18443,#18439,#16835,.T.);
#27171=EDGE_CURVE('',#18373,#18361,#16836,.T.);
#27172=EDGE_CURVE('',#18440,#18430,#16837,.T.);
#27173=EDGE_CURVE('',#18364,#18352,#16838,.T.);
#27174=EDGE_CURVE('',#18431,#18421,#16839,.T.);
#27175=EDGE_CURVE('',#18355,#18343,#16840,.T.);
#27176=EDGE_CURVE('',#18422,#18412,#90,.T.);
#27177=EDGE_CURVE('',#18346,#18334,#16841,.T.);
#27178=EDGE_CURVE('',#18413,#18403,#16842,.T.);
#27179=EDGE_CURVE('',#18337,#18326,#16843,.T.);
#27180=EDGE_CURVE('',#18404,#18394,#16844,.T.);
#27181=EDGE_CURVE('',#18395,#18386,#16845,.T.);
#27182=EDGE_CURVE('',#18328,#17382,#16846,.T.);
#27183=EDGE_CURVE('',#17626,#18320,#2185,.T.);
#27184=EDGE_CURVE('',#18323,#18311,#16847,.T.);
#27185=EDGE_CURVE('',#18384,#18380,#16848,.T.);
#27186=EDGE_CURVE('',#18314,#18302,#16849,.T.);
#27187=EDGE_CURVE('',#18381,#18371,#16850,.T.);
#27188=EDGE_CURVE('',#18305,#18293,#16851,.T.);
#27189=EDGE_CURVE('',#18372,#18362,#16852,.T.);
#27190=EDGE_CURVE('',#18296,#18284,#16853,.T.);
#27191=EDGE_CURVE('',#18363,#18353,#91,.T.);
#27192=EDGE_CURVE('',#18287,#18275,#16854,.T.);
#27193=EDGE_CURVE('',#18354,#18344,#16855,.T.);
#27194=EDGE_CURVE('',#18278,#18267,#16856,.T.);
#27195=EDGE_CURVE('',#18345,#18335,#16857,.T.);
#27196=EDGE_CURVE('',#18336,#18327,#16858,.T.);
#27197=EDGE_CURVE('',#18269,#17386,#16859,.T.);
#27198=EDGE_CURVE('',#17620,#18261,#2186,.T.);
#27199=EDGE_CURVE('',#18264,#18252,#16860,.T.);
#27200=EDGE_CURVE('',#18325,#18321,#16861,.T.);
#27201=EDGE_CURVE('',#18255,#18243,#16862,.T.);
#27202=EDGE_CURVE('',#18322,#18312,#16863,.T.);
#27203=EDGE_CURVE('',#18246,#18234,#16864,.T.);
#27204=EDGE_CURVE('',#18313,#18303,#16865,.T.);
#27205=EDGE_CURVE('',#18237,#18225,#16866,.T.);
#27206=EDGE_CURVE('',#18304,#18294,#92,.T.);
#27207=EDGE_CURVE('',#18228,#18216,#16867,.T.);
#27208=EDGE_CURVE('',#18295,#18285,#16868,.T.);
#27209=EDGE_CURVE('',#18219,#18208,#16869,.T.);
#27210=EDGE_CURVE('',#18286,#18276,#16870,.T.);
#27211=EDGE_CURVE('',#18277,#18268,#16871,.T.);
#27212=EDGE_CURVE('',#18210,#17390,#16872,.T.);
#27213=EDGE_CURVE('',#17614,#18202,#2187,.T.);
#27214=EDGE_CURVE('',#18205,#18193,#16873,.T.);
#27215=EDGE_CURVE('',#18266,#18262,#16874,.T.);
#27216=EDGE_CURVE('',#18196,#18184,#16875,.T.);
#27217=EDGE_CURVE('',#18263,#18253,#16876,.T.);
#27218=EDGE_CURVE('',#18187,#18175,#16877,.T.);
#27219=EDGE_CURVE('',#18254,#18244,#16878,.T.);
#27220=EDGE_CURVE('',#18178,#18166,#16879,.T.);
#27221=EDGE_CURVE('',#18245,#18235,#93,.T.);
#27222=EDGE_CURVE('',#18169,#18157,#16880,.T.);
#27223=EDGE_CURVE('',#18236,#18226,#16881,.T.);
#27224=EDGE_CURVE('',#18160,#18149,#16882,.T.);
#27225=EDGE_CURVE('',#18227,#18217,#16883,.T.);
#27226=EDGE_CURVE('',#18218,#18209,#16884,.T.);
#27227=EDGE_CURVE('',#18151,#17394,#16885,.T.);
#27228=EDGE_CURVE('',#18144,#18134,#16886,.T.);
#27229=EDGE_CURVE('',#18207,#18203,#16887,.T.);
#27230=EDGE_CURVE('',#17608,#18141,#2188,.T.);
#27231=EDGE_CURVE('',#18137,#18125,#16888,.T.);
#27232=EDGE_CURVE('',#18204,#18194,#16889,.T.);
#27233=EDGE_CURVE('',#18128,#18116,#16890,.T.);
#27234=EDGE_CURVE('',#18195,#18185,#16891,.T.);
#27235=EDGE_CURVE('',#18119,#18107,#16892,.T.);
#27236=EDGE_CURVE('',#18186,#18176,#94,.T.);
#27237=EDGE_CURVE('',#18110,#18098,#16893,.T.);
#27238=EDGE_CURVE('',#18177,#18167,#16894,.T.);
#27239=EDGE_CURVE('',#18101,#18090,#16895,.T.);
#27240=EDGE_CURVE('',#18168,#18158,#16896,.T.);
#27241=EDGE_CURVE('',#18159,#18150,#16897,.T.);
#27242=EDGE_CURVE('',#18092,#17398,#16898,.T.);
#27243=EDGE_CURVE('',#17602,#18084,#2189,.T.);
#27244=EDGE_CURVE('',#18087,#18073,#16899,.T.);
#27245=EDGE_CURVE('',#18148,#18142,#16900,.T.);
#27246=EDGE_CURVE('',#18076,#18066,#16901,.T.);
#27247=EDGE_CURVE('',#18143,#18135,#16902,.T.);
#27248=EDGE_CURVE('',#18069,#18057,#16903,.T.);
#27249=EDGE_CURVE('',#18136,#18126,#16904,.T.);
#27250=EDGE_CURVE('',#18060,#18048,#16905,.T.);
#27251=EDGE_CURVE('',#18127,#18117,#95,.T.);
#27252=EDGE_CURVE('',#18051,#18039,#16906,.T.);
#27253=EDGE_CURVE('',#18118,#18108,#16907,.T.);
#27254=EDGE_CURVE('',#18042,#18031,#16908,.T.);
#27255=EDGE_CURVE('',#18109,#18099,#16909,.T.);
#27256=EDGE_CURVE('',#18100,#18091,#16910,.T.);
#27257=EDGE_CURVE('',#18033,#17402,#16911,.T.);
#27258=EDGE_CURVE('',#17596,#18025,#2190,.T.);
#27259=EDGE_CURVE('',#18028,#18016,#16912,.T.);
#27260=EDGE_CURVE('',#18089,#18085,#16913,.T.);
#27261=EDGE_CURVE('',#18019,#18005,#16914,.T.);
#27262=EDGE_CURVE('',#18086,#18074,#16915,.T.);
#27263=EDGE_CURVE('',#18008,#17998,#16916,.T.);
#27264=EDGE_CURVE('',#18075,#18067,#16917,.T.);
#27265=EDGE_CURVE('',#18001,#17989,#16918,.T.);
#27266=EDGE_CURVE('',#18068,#18058,#96,.T.);
#27267=EDGE_CURVE('',#17992,#17980,#16919,.T.);
#27268=EDGE_CURVE('',#18059,#18049,#16920,.T.);
#27269=EDGE_CURVE('',#17983,#17972,#16921,.T.);
#27270=EDGE_CURVE('',#18050,#18040,#16922,.T.);
#27271=EDGE_CURVE('',#18041,#18032,#16923,.T.);
#27272=EDGE_CURVE('',#17974,#17406,#16924,.T.);
#27273=EDGE_CURVE('',#17590,#17966,#2191,.T.);
#27274=EDGE_CURVE('',#17969,#17957,#16925,.T.);
#27275=EDGE_CURVE('',#18030,#18026,#16926,.T.);
#27276=EDGE_CURVE('',#17960,#17948,#16927,.T.);
#27277=EDGE_CURVE('',#18027,#18017,#16928,.T.);
#27278=EDGE_CURVE('',#17951,#17937,#16929,.T.);
#27279=EDGE_CURVE('',#18018,#18006,#16930,.T.);
#27280=EDGE_CURVE('',#17940,#17930,#16931,.T.);
#27281=EDGE_CURVE('',#18007,#17999,#97,.T.);
#27282=EDGE_CURVE('',#17933,#17921,#16932,.T.);
#27283=EDGE_CURVE('',#18000,#17990,#16933,.T.);
#27284=EDGE_CURVE('',#17924,#17913,#16934,.T.);
#27285=EDGE_CURVE('',#17991,#17981,#16935,.T.);
#27286=EDGE_CURVE('',#17982,#17973,#16936,.T.);
#27287=EDGE_CURVE('',#17915,#17410,#16937,.T.);
#27288=EDGE_CURVE('',#17584,#17907,#2192,.T.);
#27289=EDGE_CURVE('',#17910,#17898,#16938,.T.);
#27290=EDGE_CURVE('',#17971,#17967,#16939,.T.);
#27291=EDGE_CURVE('',#17901,#17889,#16940,.T.);
#27292=EDGE_CURVE('',#17968,#17958,#16941,.T.);
#27293=EDGE_CURVE('',#17892,#17880,#16942,.T.);
#27294=EDGE_CURVE('',#17959,#17949,#16943,.T.);
#27295=EDGE_CURVE('',#17883,#17869,#16944,.T.);
#27296=EDGE_CURVE('',#17950,#17938,#98,.T.);
#27297=EDGE_CURVE('',#17872,#17862,#16945,.T.);
#27298=EDGE_CURVE('',#17939,#17931,#16946,.T.);
#27299=EDGE_CURVE('',#17865,#17854,#16947,.T.);
#27300=EDGE_CURVE('',#17932,#17922,#16948,.T.);
#27301=EDGE_CURVE('',#17923,#17914,#16949,.T.);
#27302=EDGE_CURVE('',#17856,#17414,#16950,.T.);
#27303=EDGE_CURVE('',#17578,#17832,#2193,.T.);
#27304=EDGE_CURVE('',#17836,#17813,#16951,.T.);
#27305=EDGE_CURVE('',#17912,#17908,#16952,.T.);
#27306=EDGE_CURVE('',#17817,#17794,#16953,.T.);
#27307=EDGE_CURVE('',#17909,#17899,#16954,.T.);
#27308=EDGE_CURVE('',#17798,#17775,#16955,.T.);
#27309=EDGE_CURVE('',#17900,#17890,#16956,.T.);
#27310=EDGE_CURVE('',#17779,#17756,#16957,.T.);
#27311=EDGE_CURVE('',#17891,#17881,#99,.T.);
#27312=EDGE_CURVE('',#17760,#17737,#16958,.T.);
#27313=EDGE_CURVE('',#17882,#17870,#16959,.T.);
#27314=EDGE_CURVE('',#17741,#17731,#16960,.T.);
#27315=EDGE_CURVE('',#17871,#17863,#16961,.T.);
#27316=EDGE_CURVE('',#17864,#17855,#16962,.T.);
#27317=EDGE_CURVE('',#17733,#17418,#16963,.T.);
#27318=EDGE_CURVE('',#17572,#17851,#2194,.T.);
#27319=EDGE_CURVE('',#17849,#17840,#16964,.T.);
#27320=EDGE_CURVE('',#17848,#17833,#16965,.T.);
#27321=EDGE_CURVE('',#17838,#17821,#16966,.T.);
#27322=EDGE_CURVE('',#17835,#17814,#16967,.T.);
#27323=EDGE_CURVE('',#17819,#17802,#16968,.T.);
#27324=EDGE_CURVE('',#17816,#17795,#16969,.T.);
#27325=EDGE_CURVE('',#17800,#17783,#16970,.T.);
#27326=EDGE_CURVE('',#17797,#17776,#100,.T.);
#27327=EDGE_CURVE('',#17781,#17764,#16971,.T.);
#27328=EDGE_CURVE('',#17778,#17757,#16972,.T.);
#27329=EDGE_CURVE('',#17762,#17744,#16973,.T.);
#27330=EDGE_CURVE('',#17759,#17738,#16974,.T.);
#27331=EDGE_CURVE('',#17740,#17732,#16975,.T.);
#27332=EDGE_CURVE('',#17743,#17422,#16976,.T.);
#27333=EDGE_CURVE('',#20681,#20681,#16977,.T.);
#27334=EDGE_CURVE('',#20681,#20682,#11039,.T.);
#27335=EDGE_CURVE('',#20682,#20682,#16978,.T.);
#27336=EDGE_CURVE('',#20683,#20683,#16979,.T.);
#27337=EDGE_CURVE('',#20683,#20684,#11040,.T.);
#27338=EDGE_CURVE('',#20684,#20684,#16980,.T.);
#27339=EDGE_CURVE('',#20685,#20685,#16981,.T.);
#27340=EDGE_CURVE('',#20685,#20686,#11041,.T.);
#27341=EDGE_CURVE('',#20686,#20686,#16982,.T.);
#27342=EDGE_CURVE('',#20687,#20687,#16983,.T.);
#27343=EDGE_CURVE('',#20687,#20688,#11042,.T.);
#27344=EDGE_CURVE('',#20688,#20688,#16984,.T.);
#27345=EDGE_CURVE('',#20689,#20689,#16985,.T.);
#27346=EDGE_CURVE('',#20689,#20690,#11043,.T.);
#27347=EDGE_CURVE('',#20690,#20690,#16986,.T.);
#27348=EDGE_CURVE('',#20691,#20691,#16987,.T.);
#27349=EDGE_CURVE('',#20691,#20692,#11044,.T.);
#27350=EDGE_CURVE('',#20692,#20692,#16988,.T.);
#27351=EDGE_CURVE('',#20693,#20693,#16989,.T.);
#27352=EDGE_CURVE('',#20693,#20694,#11045,.T.);
#27353=EDGE_CURVE('',#20694,#20694,#16990,.T.);
#27354=EDGE_CURVE('',#20695,#20695,#16991,.T.);
#27355=EDGE_CURVE('',#20695,#20696,#11046,.T.);
#27356=EDGE_CURVE('',#20696,#20696,#16992,.T.);
#27357=EDGE_CURVE('',#20697,#20697,#16993,.T.);
#27358=EDGE_CURVE('',#20697,#20698,#11047,.T.);
#27359=EDGE_CURVE('',#20698,#20698,#16994,.T.);
#27360=EDGE_CURVE('',#20699,#20700,#11048,.T.);
#27361=EDGE_CURVE('',#20701,#20700,#16995,.T.);
#27362=EDGE_CURVE('',#20702,#20701,#11049,.T.);
#27363=EDGE_CURVE('',#20702,#20699,#16996,.T.);
#27364=EDGE_CURVE('',#20703,#20704,#11050,.T.);
#27365=EDGE_CURVE('',#20703,#20705,#16997,.T.);
#27366=EDGE_CURVE('',#20705,#20706,#11051,.T.);
#27367=EDGE_CURVE('',#20704,#20706,#16998,.T.);
#27368=EDGE_CURVE('',#20707,#20708,#11052,.T.);
#27369=EDGE_CURVE('',#20707,#20709,#16999,.T.);
#27370=EDGE_CURVE('',#20709,#20710,#11053,.T.);
#27371=EDGE_CURVE('',#20708,#20710,#17000,.T.);
#27372=EDGE_CURVE('',#20711,#20712,#11054,.T.);
#27373=EDGE_CURVE('',#20711,#20713,#17001,.T.);
#27374=EDGE_CURVE('',#20713,#20714,#11055,.T.);
#27375=EDGE_CURVE('',#20712,#20714,#17002,.T.);
#27376=EDGE_CURVE('',#20715,#20716,#11056,.T.);
#27377=EDGE_CURVE('',#20715,#20717,#17003,.T.);
#27378=EDGE_CURVE('',#20717,#20718,#11057,.T.);
#27379=EDGE_CURVE('',#20716,#20718,#17004,.T.);
#27380=EDGE_CURVE('',#20719,#20720,#11058,.T.);
#27381=EDGE_CURVE('',#20719,#20721,#17005,.T.);
#27382=EDGE_CURVE('',#20721,#20722,#11059,.T.);
#27383=EDGE_CURVE('',#20720,#20722,#17006,.T.);
#27384=EDGE_CURVE('',#20723,#20724,#11060,.T.);
#27385=EDGE_CURVE('',#20723,#20725,#17007,.T.);
#27386=EDGE_CURVE('',#20725,#20726,#11061,.T.);
#27387=EDGE_CURVE('',#20724,#20726,#17008,.T.);
#27388=EDGE_CURVE('',#20727,#20728,#11062,.T.);
#27389=EDGE_CURVE('',#20727,#20729,#17009,.T.);
#27390=EDGE_CURVE('',#20729,#20730,#11063,.T.);
#27391=EDGE_CURVE('',#20728,#20730,#17010,.T.);
#27392=EDGE_CURVE('',#20731,#20732,#11064,.T.);
#27393=EDGE_CURVE('',#20731,#20733,#17011,.T.);
#27394=EDGE_CURVE('',#20733,#20734,#11065,.T.);
#27395=EDGE_CURVE('',#20732,#20734,#17012,.T.);
#27396=EDGE_CURVE('',#20735,#20736,#11066,.T.);
#27397=EDGE_CURVE('',#20735,#20737,#17013,.T.);
#27398=EDGE_CURVE('',#20737,#20738,#11067,.T.);
#27399=EDGE_CURVE('',#20736,#20738,#17014,.T.);
#27400=EDGE_CURVE('',#20739,#20740,#11068,.T.);
#27401=EDGE_CURVE('',#20739,#20741,#17015,.T.);
#27402=EDGE_CURVE('',#20741,#20742,#11069,.T.);
#27403=EDGE_CURVE('',#20740,#20742,#17016,.T.);
#27404=EDGE_CURVE('',#20743,#20744,#11070,.T.);
#27405=EDGE_CURVE('',#20743,#20745,#17017,.T.);
#27406=EDGE_CURVE('',#20745,#20746,#11071,.T.);
#27407=EDGE_CURVE('',#20744,#20746,#17018,.T.);
#27408=EDGE_CURVE('',#20747,#20748,#11072,.T.);
#27409=EDGE_CURVE('',#20747,#20749,#17019,.T.);
#27410=EDGE_CURVE('',#20749,#20750,#11073,.T.);
#27411=EDGE_CURVE('',#20748,#20750,#17020,.T.);
#27412=EDGE_CURVE('',#20751,#20752,#11074,.T.);
#27413=EDGE_CURVE('',#20751,#20753,#17021,.T.);
#27414=EDGE_CURVE('',#20753,#20754,#11075,.T.);
#27415=EDGE_CURVE('',#20752,#20754,#17022,.T.);
#27416=EDGE_CURVE('',#20755,#20756,#11076,.T.);
#27417=EDGE_CURVE('',#20755,#20757,#17023,.T.);
#27418=EDGE_CURVE('',#20757,#20758,#11077,.T.);
#27419=EDGE_CURVE('',#20756,#20758,#17024,.T.);
#27420=EDGE_CURVE('',#20759,#20760,#11078,.T.);
#27421=EDGE_CURVE('',#20759,#20761,#17025,.T.);
#27422=EDGE_CURVE('',#20761,#20762,#11079,.T.);
#27423=EDGE_CURVE('',#20760,#20762,#17026,.T.);
#27424=EDGE_CURVE('',#20763,#20764,#11080,.T.);
#27425=EDGE_CURVE('',#20765,#20764,#17027,.T.);
#27426=EDGE_CURVE('',#20766,#20765,#11081,.T.);
#27427=EDGE_CURVE('',#20766,#20763,#17028,.T.);
#27428=EDGE_CURVE('',#20767,#20768,#11082,.T.);
#27429=EDGE_CURVE('',#20769,#20768,#17029,.T.);
#27430=EDGE_CURVE('',#20770,#20769,#11083,.T.);
#27431=EDGE_CURVE('',#20770,#20767,#17030,.T.);
#27432=EDGE_CURVE('',#20771,#20772,#11084,.T.);
#27433=EDGE_CURVE('',#20773,#20772,#17031,.T.);
#27434=EDGE_CURVE('',#20774,#20773,#11085,.T.);
#27435=EDGE_CURVE('',#20774,#20771,#17032,.T.);
#27436=EDGE_CURVE('',#20775,#20776,#11086,.T.);
#27437=EDGE_CURVE('',#20775,#20777,#17033,.T.);
#27438=EDGE_CURVE('',#20777,#20778,#11087,.T.);
#27439=EDGE_CURVE('',#20776,#20778,#17034,.T.);
#27440=EDGE_CURVE('',#20779,#20780,#11088,.T.);
#27441=EDGE_CURVE('',#20779,#20781,#17035,.T.);
#27442=EDGE_CURVE('',#20781,#20782,#11089,.T.);
#27443=EDGE_CURVE('',#20780,#20782,#17036,.T.);
#27444=EDGE_CURVE('',#20783,#20784,#11090,.T.);
#27445=EDGE_CURVE('',#20783,#20785,#17037,.T.);
#27446=EDGE_CURVE('',#20785,#20786,#11091,.T.);
#27447=EDGE_CURVE('',#20784,#20786,#17038,.T.);
#27448=EDGE_CURVE('',#20787,#20788,#11092,.T.);
#27449=EDGE_CURVE('',#20787,#20789,#17039,.T.);
#27450=EDGE_CURVE('',#20789,#20790,#11093,.T.);
#27451=EDGE_CURVE('',#20788,#20790,#17040,.T.);
#27452=EDGE_CURVE('',#20791,#20792,#11094,.T.);
#27453=EDGE_CURVE('',#20791,#20793,#17041,.T.);
#27454=EDGE_CURVE('',#20793,#20794,#11095,.T.);
#27455=EDGE_CURVE('',#20792,#20794,#17042,.T.);
#27456=EDGE_CURVE('',#20795,#20796,#11096,.T.);
#27457=EDGE_CURVE('',#20795,#20797,#17043,.T.);
#27458=EDGE_CURVE('',#20797,#20798,#11097,.T.);
#27459=EDGE_CURVE('',#20796,#20798,#17044,.T.);
#27460=EDGE_CURVE('',#20799,#20800,#11098,.T.);
#27461=EDGE_CURVE('',#20799,#20801,#17045,.T.);
#27462=EDGE_CURVE('',#20801,#20802,#11099,.T.);
#27463=EDGE_CURVE('',#20800,#20802,#17046,.T.);
#27464=EDGE_CURVE('',#20803,#20804,#11100,.T.);
#27465=EDGE_CURVE('',#20803,#20805,#17047,.T.);
#27466=EDGE_CURVE('',#20805,#20806,#11101,.T.);
#27467=EDGE_CURVE('',#20804,#20806,#17048,.T.);
#27468=EDGE_CURVE('',#20807,#20808,#11102,.T.);
#27469=EDGE_CURVE('',#20807,#20809,#17049,.T.);
#27470=EDGE_CURVE('',#20809,#20810,#11103,.T.);
#27471=EDGE_CURVE('',#20808,#20810,#17050,.T.);
#27472=EDGE_CURVE('',#20811,#20812,#11104,.T.);
#27473=EDGE_CURVE('',#20811,#20813,#17051,.T.);
#27474=EDGE_CURVE('',#20813,#20814,#11105,.T.);
#27475=EDGE_CURVE('',#20812,#20814,#17052,.T.);
#27476=EDGE_CURVE('',#20815,#20816,#11106,.T.);
#27477=EDGE_CURVE('',#20815,#20817,#17053,.T.);
#27478=EDGE_CURVE('',#20817,#20818,#11107,.T.);
#27479=EDGE_CURVE('',#20816,#20818,#17054,.T.);
#27480=EDGE_CURVE('',#20819,#20820,#11108,.T.);
#27481=EDGE_CURVE('',#20821,#20820,#17055,.T.);
#27482=EDGE_CURVE('',#20822,#20821,#11109,.T.);
#27483=EDGE_CURVE('',#20822,#20819,#17056,.T.);
#27484=EDGE_CURVE('',#20823,#20824,#11110,.T.);
#27485=EDGE_CURVE('',#20823,#20825,#17057,.T.);
#27486=EDGE_CURVE('',#20825,#20826,#11111,.T.);
#27487=EDGE_CURVE('',#20824,#20826,#17058,.T.);
#27488=EDGE_CURVE('',#20827,#20828,#11112,.T.);
#27489=EDGE_CURVE('',#20827,#20829,#17059,.T.);
#27490=EDGE_CURVE('',#20829,#20830,#11113,.T.);
#27491=EDGE_CURVE('',#20828,#20830,#17060,.T.);
#27492=EDGE_CURVE('',#20831,#20832,#11114,.T.);
#27493=EDGE_CURVE('',#20831,#20833,#17061,.T.);
#27494=EDGE_CURVE('',#20833,#20834,#11115,.T.);
#27495=EDGE_CURVE('',#20832,#20834,#17062,.T.);
#27496=EDGE_CURVE('',#20835,#20836,#11116,.T.);
#27497=EDGE_CURVE('',#20835,#20837,#17063,.T.);
#27498=EDGE_CURVE('',#20837,#20838,#11117,.T.);
#27499=EDGE_CURVE('',#20836,#20838,#17064,.T.);
#27500=EDGE_CURVE('',#20839,#20840,#11118,.T.);
#27501=EDGE_CURVE('',#20839,#20841,#17065,.T.);
#27502=EDGE_CURVE('',#20841,#20842,#11119,.T.);
#27503=EDGE_CURVE('',#20840,#20842,#17066,.T.);
#27504=EDGE_CURVE('',#20843,#20844,#11120,.T.);
#27505=EDGE_CURVE('',#20843,#20845,#17067,.T.);
#27506=EDGE_CURVE('',#20845,#20846,#11121,.T.);
#27507=EDGE_CURVE('',#20844,#20846,#17068,.T.);
#27508=EDGE_CURVE('',#20847,#20848,#11122,.T.);
#27509=EDGE_CURVE('',#20847,#20849,#17069,.T.);
#27510=EDGE_CURVE('',#20849,#20850,#11123,.T.);
#27511=EDGE_CURVE('',#20848,#20850,#17070,.T.);
#27512=EDGE_CURVE('',#20851,#20852,#11124,.T.);
#27513=EDGE_CURVE('',#20851,#20853,#17071,.T.);
#27514=EDGE_CURVE('',#20853,#20854,#11125,.T.);
#27515=EDGE_CURVE('',#20852,#20854,#17072,.T.);
#27516=EDGE_CURVE('',#20855,#20856,#11126,.T.);
#27517=EDGE_CURVE('',#20855,#20857,#17073,.T.);
#27518=EDGE_CURVE('',#20857,#20858,#11127,.T.);
#27519=EDGE_CURVE('',#20856,#20858,#17074,.T.);
#27520=EDGE_CURVE('',#20859,#20860,#11128,.T.);
#27521=EDGE_CURVE('',#20861,#20860,#17075,.T.);
#27522=EDGE_CURVE('',#20862,#20861,#11129,.T.);
#27523=EDGE_CURVE('',#20862,#20859,#17076,.T.);
#27524=EDGE_CURVE('',#20863,#20864,#11130,.T.);
#27525=EDGE_CURVE('',#20865,#20864,#17077,.T.);
#27526=EDGE_CURVE('',#20866,#20865,#11131,.T.);
#27527=EDGE_CURVE('',#20866,#20863,#17078,.T.);
#27528=EDGE_CURVE('',#20867,#20868,#11132,.T.);
#27529=EDGE_CURVE('',#20869,#20868,#17079,.T.);
#27530=EDGE_CURVE('',#20870,#20869,#11133,.T.);
#27531=EDGE_CURVE('',#20870,#20867,#17080,.T.);
#27532=EDGE_CURVE('',#20871,#20872,#11134,.T.);
#27533=EDGE_CURVE('',#20873,#20872,#17081,.T.);
#27534=EDGE_CURVE('',#20874,#20873,#11135,.T.);
#27535=EDGE_CURVE('',#20874,#20871,#17082,.T.);
#27536=EDGE_CURVE('',#20875,#20876,#11136,.T.);
#27537=EDGE_CURVE('',#20877,#20876,#17083,.T.);
#27538=EDGE_CURVE('',#20878,#20877,#11137,.T.);
#27539=EDGE_CURVE('',#20878,#20875,#17084,.T.);
#27540=EDGE_CURVE('',#20879,#20880,#11138,.T.);
#27541=EDGE_CURVE('',#20881,#20880,#17085,.T.);
#27542=EDGE_CURVE('',#20882,#20881,#11139,.T.);
#27543=EDGE_CURVE('',#20882,#20879,#17086,.T.);
#27544=EDGE_CURVE('',#20883,#20884,#11140,.T.);
#27545=EDGE_CURVE('',#20885,#20884,#17087,.T.);
#27546=EDGE_CURVE('',#20886,#20885,#11141,.T.);
#27547=EDGE_CURVE('',#20886,#20883,#17088,.T.);
#27548=EDGE_CURVE('',#20887,#20888,#11142,.T.);
#27549=EDGE_CURVE('',#20887,#20889,#17089,.T.);
#27550=EDGE_CURVE('',#20889,#20890,#11143,.T.);
#27551=EDGE_CURVE('',#20888,#20890,#17090,.T.);
#27552=EDGE_CURVE('',#20891,#20892,#11144,.T.);
#27553=EDGE_CURVE('',#20891,#20893,#17091,.T.);
#27554=EDGE_CURVE('',#20893,#20894,#11145,.T.);
#27555=EDGE_CURVE('',#20892,#20894,#17092,.T.);
#27556=EDGE_CURVE('',#20895,#20896,#11146,.T.);
#27557=EDGE_CURVE('',#20897,#20896,#17093,.T.);
#27558=EDGE_CURVE('',#20898,#20897,#11147,.T.);
#27559=EDGE_CURVE('',#20898,#20895,#17094,.T.);
#27560=EDGE_CURVE('',#20899,#20900,#11148,.T.);
#27561=EDGE_CURVE('',#20899,#20901,#17095,.T.);
#27562=EDGE_CURVE('',#20901,#20902,#11149,.T.);
#27563=EDGE_CURVE('',#20900,#20902,#17096,.T.);
#27564=EDGE_CURVE('',#20903,#20703,#11150,.T.);
#27565=EDGE_CURVE('',#20699,#20903,#11151,.T.);
#27566=EDGE_CURVE('',#20904,#20702,#11152,.T.);
#27567=EDGE_CURVE('',#20895,#20904,#11153,.T.);
#27568=EDGE_CURVE('',#20905,#20898,#11154,.T.);
#27569=EDGE_CURVE('',#20901,#20905,#11155,.T.);
#27570=EDGE_CURVE('',#20906,#20899,#11156,.T.);
#27571=EDGE_CURVE('',#20893,#20906,#11157,.T.);
#27572=EDGE_CURVE('',#20907,#20891,#11158,.T.);
#27573=EDGE_CURVE('',#20859,#20907,#11159,.T.);
#27574=EDGE_CURVE('',#20908,#20862,#11160,.T.);
#27575=EDGE_CURVE('',#20863,#20908,#11161,.T.);
#27576=EDGE_CURVE('',#20909,#20866,#11162,.T.);
#27577=EDGE_CURVE('',#20867,#20909,#11163,.T.);
#27578=EDGE_CURVE('',#20910,#20870,#11164,.T.);
#27579=EDGE_CURVE('',#20871,#20910,#11165,.T.);
#27580=EDGE_CURVE('',#20911,#20874,#11166,.T.);
#27581=EDGE_CURVE('',#20875,#20911,#11167,.T.);
#27582=EDGE_CURVE('',#20912,#20878,#11168,.T.);
#27583=EDGE_CURVE('',#20879,#20912,#11169,.T.);
#27584=EDGE_CURVE('',#20913,#20882,#11170,.T.);
#27585=EDGE_CURVE('',#20883,#20913,#11171,.T.);
#27586=EDGE_CURVE('',#20914,#20886,#11172,.T.);
#27587=EDGE_CURVE('',#20889,#20914,#11173,.T.);
#27588=EDGE_CURVE('',#20915,#20887,#11174,.T.);
#27589=EDGE_CURVE('',#20857,#20915,#11175,.T.);
#27590=EDGE_CURVE('',#20916,#20855,#11176,.T.);
#27591=EDGE_CURVE('',#20853,#20916,#11177,.T.);
#27592=EDGE_CURVE('',#20917,#20851,#11178,.T.);
#27593=EDGE_CURVE('',#20849,#20917,#11179,.T.);
#27594=EDGE_CURVE('',#20918,#20847,#11180,.T.);
#27595=EDGE_CURVE('',#20845,#20918,#11181,.T.);
#27596=EDGE_CURVE('',#20919,#20843,#11182,.T.);
#27597=EDGE_CURVE('',#20841,#20919,#11183,.T.);
#27598=EDGE_CURVE('',#20920,#20839,#11184,.T.);
#27599=EDGE_CURVE('',#20837,#20920,#11185,.T.);
#27600=EDGE_CURVE('',#20921,#20835,#11186,.T.);
#27601=EDGE_CURVE('',#20833,#20921,#11187,.T.);
#27602=EDGE_CURVE('',#20922,#20831,#11188,.T.);
#27603=EDGE_CURVE('',#20829,#20922,#11189,.T.);
#27604=EDGE_CURVE('',#20923,#20827,#11190,.T.);
#27605=EDGE_CURVE('',#20819,#20923,#11191,.T.);
#27606=EDGE_CURVE('',#20924,#20822,#11192,.T.);
#27607=EDGE_CURVE('',#20825,#20924,#11193,.T.);
#27608=EDGE_CURVE('',#20925,#20823,#11194,.T.);
#27609=EDGE_CURVE('',#20817,#20925,#11195,.T.);
#27610=EDGE_CURVE('',#20926,#20815,#11196,.T.);
#27611=EDGE_CURVE('',#20813,#20926,#11197,.T.);
#27612=EDGE_CURVE('',#20927,#20811,#11198,.T.);
#27613=EDGE_CURVE('',#20809,#20927,#11199,.T.);
#27614=EDGE_CURVE('',#20928,#20807,#11200,.T.);
#27615=EDGE_CURVE('',#20805,#20928,#11201,.T.);
#27616=EDGE_CURVE('',#20929,#20803,#11202,.T.);
#27617=EDGE_CURVE('',#20801,#20929,#11203,.T.);
#27618=EDGE_CURVE('',#20930,#20799,#11204,.T.);
#27619=EDGE_CURVE('',#20797,#20930,#11205,.T.);
#27620=EDGE_CURVE('',#20931,#20795,#11206,.T.);
#27621=EDGE_CURVE('',#20793,#20931,#11207,.T.);
#27622=EDGE_CURVE('',#20932,#20791,#11208,.T.);
#27623=EDGE_CURVE('',#20789,#20932,#11209,.T.);
#27624=EDGE_CURVE('',#20933,#20787,#11210,.T.);
#27625=EDGE_CURVE('',#20785,#20933,#11211,.T.);
#27626=EDGE_CURVE('',#20934,#20783,#11212,.T.);
#27627=EDGE_CURVE('',#20781,#20934,#11213,.T.);
#27628=EDGE_CURVE('',#20935,#20779,#11214,.T.);
#27629=EDGE_CURVE('',#20763,#20935,#11215,.T.);
#27630=EDGE_CURVE('',#20936,#20766,#11216,.T.);
#27631=EDGE_CURVE('',#20767,#20936,#11217,.T.);
#27632=EDGE_CURVE('',#20937,#20770,#11218,.T.);
#27633=EDGE_CURVE('',#20771,#20937,#11219,.T.);
#27634=EDGE_CURVE('',#20938,#20774,#11220,.T.);
#27635=EDGE_CURVE('',#20777,#20938,#11221,.T.);
#27636=EDGE_CURVE('',#20939,#20775,#11222,.T.);
#27637=EDGE_CURVE('',#20761,#20939,#11223,.T.);
#27638=EDGE_CURVE('',#20940,#20759,#11224,.T.);
#27639=EDGE_CURVE('',#20757,#20940,#11225,.T.);
#27640=EDGE_CURVE('',#20941,#20755,#11226,.T.);
#27641=EDGE_CURVE('',#20753,#20941,#11227,.T.);
#27642=EDGE_CURVE('',#20942,#20751,#11228,.T.);
#27643=EDGE_CURVE('',#20749,#20942,#11229,.T.);
#27644=EDGE_CURVE('',#20943,#20747,#11230,.T.);
#27645=EDGE_CURVE('',#20745,#20943,#11231,.T.);
#27646=EDGE_CURVE('',#20944,#20743,#11232,.T.);
#27647=EDGE_CURVE('',#20741,#20944,#11233,.T.);
#27648=EDGE_CURVE('',#20945,#20739,#11234,.T.);
#27649=EDGE_CURVE('',#20737,#20945,#11235,.T.);
#27650=EDGE_CURVE('',#20946,#20735,#11236,.T.);
#27651=EDGE_CURVE('',#20733,#20946,#11237,.T.);
#27652=EDGE_CURVE('',#20947,#20731,#11238,.T.);
#27653=EDGE_CURVE('',#20729,#20947,#11239,.T.);
#27654=EDGE_CURVE('',#20948,#20727,#11240,.T.);
#27655=EDGE_CURVE('',#20725,#20948,#11241,.T.);
#27656=EDGE_CURVE('',#20949,#20723,#11242,.T.);
#27657=EDGE_CURVE('',#20721,#20949,#11243,.T.);
#27658=EDGE_CURVE('',#20950,#20719,#11244,.T.);
#27659=EDGE_CURVE('',#20717,#20950,#11245,.T.);
#27660=EDGE_CURVE('',#20951,#20715,#11246,.T.);
#27661=EDGE_CURVE('',#20713,#20951,#11247,.T.);
#27662=EDGE_CURVE('',#20952,#20711,#11248,.T.);
#27663=EDGE_CURVE('',#20709,#20952,#11249,.T.);
#27664=EDGE_CURVE('',#20953,#20707,#11250,.T.);
#27665=EDGE_CURVE('',#20705,#20953,#11251,.T.);
#27666=EDGE_CURVE('',#20954,#20700,#11252,.T.);
#27667=EDGE_CURVE('',#20704,#20954,#11253,.T.);
#27668=EDGE_CURVE('',#20955,#20706,#11254,.T.);
#27669=EDGE_CURVE('',#20708,#20955,#11255,.T.);
#27670=EDGE_CURVE('',#20956,#20710,#11256,.T.);
#27671=EDGE_CURVE('',#20712,#20956,#11257,.T.);
#27672=EDGE_CURVE('',#20957,#20714,#11258,.T.);
#27673=EDGE_CURVE('',#20716,#20957,#11259,.T.);
#27674=EDGE_CURVE('',#20958,#20718,#11260,.T.);
#27675=EDGE_CURVE('',#20720,#20958,#11261,.T.);
#27676=EDGE_CURVE('',#20959,#20722,#11262,.T.);
#27677=EDGE_CURVE('',#20724,#20959,#11263,.T.);
#27678=EDGE_CURVE('',#20960,#20726,#11264,.T.);
#27679=EDGE_CURVE('',#20728,#20960,#11265,.T.);
#27680=EDGE_CURVE('',#20961,#20730,#11266,.T.);
#27681=EDGE_CURVE('',#20732,#20961,#11267,.T.);
#27682=EDGE_CURVE('',#20962,#20734,#11268,.T.);
#27683=EDGE_CURVE('',#20736,#20962,#11269,.T.);
#27684=EDGE_CURVE('',#20963,#20738,#11270,.T.);
#27685=EDGE_CURVE('',#20740,#20963,#11271,.T.);
#27686=EDGE_CURVE('',#20964,#20742,#11272,.T.);
#27687=EDGE_CURVE('',#20744,#20964,#11273,.T.);
#27688=EDGE_CURVE('',#20965,#20746,#11274,.T.);
#27689=EDGE_CURVE('',#20748,#20965,#11275,.T.);
#27690=EDGE_CURVE('',#20966,#20750,#11276,.T.);
#27691=EDGE_CURVE('',#20752,#20966,#11277,.T.);
#27692=EDGE_CURVE('',#20967,#20754,#11278,.T.);
#27693=EDGE_CURVE('',#20756,#20967,#11279,.T.);
#27694=EDGE_CURVE('',#20968,#20758,#11280,.T.);
#27695=EDGE_CURVE('',#20760,#20968,#11281,.T.);
#27696=EDGE_CURVE('',#20969,#20762,#11282,.T.);
#27697=EDGE_CURVE('',#20776,#20969,#11283,.T.);
#27698=EDGE_CURVE('',#20970,#20778,#11284,.T.);
#27699=EDGE_CURVE('',#20773,#20970,#11285,.T.);
#27700=EDGE_CURVE('',#20971,#20772,#11286,.T.);
#27701=EDGE_CURVE('',#20769,#20971,#11287,.T.);
#27702=EDGE_CURVE('',#20972,#20768,#11288,.T.);
#27703=EDGE_CURVE('',#20765,#20972,#11289,.T.);
#27704=EDGE_CURVE('',#20973,#20764,#11290,.T.);
#27705=EDGE_CURVE('',#20780,#20973,#11291,.T.);
#27706=EDGE_CURVE('',#20974,#20782,#11292,.T.);
#27707=EDGE_CURVE('',#20784,#20974,#11293,.T.);
#27708=EDGE_CURVE('',#20975,#20786,#11294,.T.);
#27709=EDGE_CURVE('',#20788,#20975,#11295,.T.);
#27710=EDGE_CURVE('',#20976,#20790,#11296,.T.);
#27711=EDGE_CURVE('',#20792,#20976,#11297,.T.);
#27712=EDGE_CURVE('',#20977,#20794,#11298,.T.);
#27713=EDGE_CURVE('',#20796,#20977,#11299,.T.);
#27714=EDGE_CURVE('',#20978,#20798,#11300,.T.);
#27715=EDGE_CURVE('',#20800,#20978,#11301,.T.);
#27716=EDGE_CURVE('',#20979,#20802,#11302,.T.);
#27717=EDGE_CURVE('',#20804,#20979,#11303,.T.);
#27718=EDGE_CURVE('',#20980,#20806,#11304,.T.);
#27719=EDGE_CURVE('',#20808,#20980,#11305,.T.);
#27720=EDGE_CURVE('',#20981,#20810,#11306,.T.);
#27721=EDGE_CURVE('',#20812,#20981,#11307,.T.);
#27722=EDGE_CURVE('',#20982,#20814,#11308,.T.);
#27723=EDGE_CURVE('',#20816,#20982,#11309,.T.);
#27724=EDGE_CURVE('',#20983,#20818,#11310,.T.);
#27725=EDGE_CURVE('',#20824,#20983,#11311,.T.);
#27726=EDGE_CURVE('',#20984,#20826,#11312,.T.);
#27727=EDGE_CURVE('',#20821,#20984,#11313,.T.);
#27728=EDGE_CURVE('',#20985,#20820,#11314,.T.);
#27729=EDGE_CURVE('',#20828,#20985,#11315,.T.);
#27730=EDGE_CURVE('',#20986,#20830,#11316,.T.);
#27731=EDGE_CURVE('',#20832,#20986,#11317,.T.);
#27732=EDGE_CURVE('',#20987,#20834,#11318,.T.);
#27733=EDGE_CURVE('',#20836,#20987,#11319,.T.);
#27734=EDGE_CURVE('',#20988,#20838,#11320,.T.);
#27735=EDGE_CURVE('',#20840,#20988,#11321,.T.);
#27736=EDGE_CURVE('',#20989,#20842,#11322,.T.);
#27737=EDGE_CURVE('',#20844,#20989,#11323,.T.);
#27738=EDGE_CURVE('',#20990,#20846,#11324,.T.);
#27739=EDGE_CURVE('',#20848,#20990,#11325,.T.);
#27740=EDGE_CURVE('',#20991,#20850,#11326,.T.);
#27741=EDGE_CURVE('',#20852,#20991,#11327,.T.);
#27742=EDGE_CURVE('',#20992,#20854,#11328,.T.);
#27743=EDGE_CURVE('',#20856,#20992,#11329,.T.);
#27744=EDGE_CURVE('',#20993,#20858,#11330,.T.);
#27745=EDGE_CURVE('',#20888,#20993,#11331,.T.);
#27746=EDGE_CURVE('',#20994,#20890,#11332,.T.);
#27747=EDGE_CURVE('',#20885,#20994,#11333,.T.);
#27748=EDGE_CURVE('',#20995,#20884,#11334,.T.);
#27749=EDGE_CURVE('',#20881,#20995,#11335,.T.);
#27750=EDGE_CURVE('',#20996,#20880,#11336,.T.);
#27751=EDGE_CURVE('',#20877,#20996,#11337,.T.);
#27752=EDGE_CURVE('',#20997,#20876,#11338,.T.);
#27753=EDGE_CURVE('',#20873,#20997,#11339,.T.);
#27754=EDGE_CURVE('',#20998,#20872,#11340,.T.);
#27755=EDGE_CURVE('',#20869,#20998,#11341,.T.);
#27756=EDGE_CURVE('',#20999,#20868,#11342,.T.);
#27757=EDGE_CURVE('',#20865,#20999,#11343,.T.);
#27758=EDGE_CURVE('',#21000,#20864,#11344,.T.);
#27759=EDGE_CURVE('',#20861,#21000,#11345,.T.);
#27760=EDGE_CURVE('',#21001,#20860,#11346,.T.);
#27761=EDGE_CURVE('',#20892,#21001,#11347,.T.);
#27762=EDGE_CURVE('',#21002,#20894,#11348,.T.);
#27763=EDGE_CURVE('',#20900,#21002,#11349,.T.);
#27764=EDGE_CURVE('',#21003,#20902,#11350,.T.);
#27765=EDGE_CURVE('',#20897,#21003,#11351,.T.);
#27766=EDGE_CURVE('',#21004,#20896,#11352,.T.);
#27767=EDGE_CURVE('',#20701,#21004,#11353,.T.);
#27768=EDGE_CURVE('',#20905,#21003,#11354,.T.);
#27769=EDGE_CURVE('',#20904,#21004,#11355,.T.);
#27770=EDGE_CURVE('',#20906,#21002,#11356,.T.);
#27771=EDGE_CURVE('',#20914,#20994,#11357,.T.);
#27772=EDGE_CURVE('',#20913,#20995,#11358,.T.);
#27773=EDGE_CURVE('',#20912,#20996,#11359,.T.);
#27774=EDGE_CURVE('',#20911,#20997,#11360,.T.);
#27775=EDGE_CURVE('',#20910,#20998,#11361,.T.);
#27776=EDGE_CURVE('',#20909,#20999,#11362,.T.);
#27777=EDGE_CURVE('',#20908,#21000,#11363,.T.);
#27778=EDGE_CURVE('',#20907,#21001,#11364,.T.);
#27779=EDGE_CURVE('',#20915,#20993,#11365,.T.);
#27780=EDGE_CURVE('',#20916,#20992,#11366,.T.);
#27781=EDGE_CURVE('',#20917,#20991,#11367,.T.);
#27782=EDGE_CURVE('',#20918,#20990,#11368,.T.);
#27783=EDGE_CURVE('',#20919,#20989,#11369,.T.);
#27784=EDGE_CURVE('',#20920,#20988,#11370,.T.);
#27785=EDGE_CURVE('',#20921,#20987,#11371,.T.);
#27786=EDGE_CURVE('',#20922,#20986,#11372,.T.);
#27787=EDGE_CURVE('',#20924,#20984,#11373,.T.);
#27788=EDGE_CURVE('',#20923,#20985,#11374,.T.);
#27789=EDGE_CURVE('',#20925,#20983,#11375,.T.);
#27790=EDGE_CURVE('',#20926,#20982,#11376,.T.);
#27791=EDGE_CURVE('',#20927,#20981,#11377,.T.);
#27792=EDGE_CURVE('',#20928,#20980,#11378,.T.);
#27793=EDGE_CURVE('',#20929,#20979,#11379,.T.);
#27794=EDGE_CURVE('',#20930,#20978,#11380,.T.);
#27795=EDGE_CURVE('',#20931,#20977,#11381,.T.);
#27796=EDGE_CURVE('',#20932,#20976,#11382,.T.);
#27797=EDGE_CURVE('',#20933,#20975,#11383,.T.);
#27798=EDGE_CURVE('',#20934,#20974,#11384,.T.);
#27799=EDGE_CURVE('',#20938,#20970,#11385,.T.);
#27800=EDGE_CURVE('',#20937,#20971,#11386,.T.);
#27801=EDGE_CURVE('',#20936,#20972,#11387,.T.);
#27802=EDGE_CURVE('',#20935,#20973,#11388,.T.);
#27803=EDGE_CURVE('',#20939,#20969,#11389,.T.);
#27804=EDGE_CURVE('',#20940,#20968,#11390,.T.);
#27805=EDGE_CURVE('',#20941,#20967,#11391,.T.);
#27806=EDGE_CURVE('',#20942,#20966,#11392,.T.);
#27807=EDGE_CURVE('',#20943,#20965,#11393,.T.);
#27808=EDGE_CURVE('',#20944,#20964,#11394,.T.);
#27809=EDGE_CURVE('',#20945,#20963,#11395,.T.);
#27810=EDGE_CURVE('',#20946,#20962,#11396,.T.);
#27811=EDGE_CURVE('',#20947,#20961,#11397,.T.);
#27812=EDGE_CURVE('',#20948,#20960,#11398,.T.);
#27813=EDGE_CURVE('',#20949,#20959,#11399,.T.);
#27814=EDGE_CURVE('',#20950,#20958,#11400,.T.);
#27815=EDGE_CURVE('',#20951,#20957,#11401,.T.);
#27816=EDGE_CURVE('',#20952,#20956,#11402,.T.);
#27817=EDGE_CURVE('',#20953,#20955,#11403,.T.);
#27818=EDGE_CURVE('',#20903,#20954,#11404,.T.);
#27819=EDGE_CURVE('',#21005,#21005,#17097,.T.);
#27820=EDGE_CURVE('',#21005,#21006,#11405,.T.);
#27821=EDGE_CURVE('',#21006,#21007,#17098,.T.);
#27822=EDGE_CURVE('',#21007,#21008,#11406,.T.);
#27823=EDGE_CURVE('',#21009,#21008,#17099,.T.);
#27824=EDGE_CURVE('',#21009,#21010,#11407,.T.);
#27825=EDGE_CURVE('',#21010,#21010,#17100,.T.);
#27826=EDGE_CURVE('',#21011,#21009,#17101,.T.);
#27827=EDGE_CURVE('',#21012,#21011,#11408,.T.);
#27828=EDGE_CURVE('',#21012,#21006,#17102,.T.);
#27829=EDGE_CURVE('',#21013,#21013,#17103,.T.);
#27830=EDGE_CURVE('',#21013,#21014,#11409,.T.);
#27831=EDGE_CURVE('',#21014,#21014,#17104,.T.);
#27832=EDGE_CURVE('',#21015,#21015,#2195,.F.);
#27833=EDGE_CURVE('',#21016,#21016,#17105,.T.);
#27834=EDGE_CURVE('',#21016,#21017,#11410,.T.);
#27835=EDGE_CURVE('',#21017,#21017,#17106,.T.);
#27836=EDGE_CURVE('',#21018,#21019,#17107,.T.);
#27837=EDGE_CURVE('',#21020,#21018,#11411,.T.);
#27838=EDGE_CURVE('',#21020,#21021,#17108,.T.);
#27839=EDGE_CURVE('',#21019,#21021,#11412,.T.);
#27840=EDGE_CURVE('',#21022,#21022,#17109,.T.);
#27841=EDGE_CURVE('',#21022,#21023,#11413,.T.);
#27842=EDGE_CURVE('',#21023,#21023,#17110,.T.);
#27843=EDGE_CURVE('',#21024,#21025,#17111,.T.);
#27844=EDGE_CURVE('',#21025,#21026,#11414,.T.);
#27845=EDGE_CURVE('',#21026,#21026,#17112,.T.);
#27846=EDGE_CURVE('',#21025,#21027,#17113,.T.);
#27847=EDGE_CURVE('',#21027,#21028,#2196,.F.);
#27848=EDGE_CURVE('',#21029,#21028,#17114,.T.);
#27849=EDGE_CURVE('',#21030,#21029,#17115,.T.);
#27850=EDGE_CURVE('',#21030,#21024,#2197,.F.);
#27851=EDGE_CURVE('',#21026,#21031,#11415,.T.);
#27852=EDGE_CURVE('',#21031,#21031,#17116,.T.);
#27853=EDGE_CURVE('',#21032,#21032,#17117,.T.);
#27854=EDGE_CURVE('',#21032,#21033,#11416,.T.);
#27855=EDGE_CURVE('',#21033,#21033,#17118,.T.);
#27856=EDGE_CURVE('',#21034,#21035,#17119,.T.);
#27857=EDGE_CURVE('',#21036,#21034,#11417,.T.);
#27858=EDGE_CURVE('',#21037,#21036,#17120,.T.);
#27859=EDGE_CURVE('',#21037,#21035,#11418,.T.);
#27860=EDGE_CURVE('',#21038,#21039,#17121,.T.);
#27861=EDGE_CURVE('',#21038,#21040,#11419,.T.);
#27862=EDGE_CURVE('',#21040,#21041,#17122,.T.);
#27863=EDGE_CURVE('',#21042,#21041,#11420,.T.);
#27864=EDGE_CURVE('',#21043,#21042,#17123,.T.);
#27865=EDGE_CURVE('',#21039,#21043,#11421,.T.);
#27866=EDGE_CURVE('',#21044,#21044,#17124,.T.);
#27867=EDGE_CURVE('',#21044,#21045,#11422,.T.);
#27868=EDGE_CURVE('',#21045,#21045,#17125,.T.);
#27869=EDGE_CURVE('',#21046,#21046,#17126,.T.);
#27870=EDGE_CURVE('',#21046,#21047,#11423,.T.);
#27871=EDGE_CURVE('',#21047,#21047,#17127,.T.);
#27872=EDGE_CURVE('',#21048,#21048,#17128,.T.);
#27873=EDGE_CURVE('',#21048,#21049,#11424,.T.);
#27874=EDGE_CURVE('',#21049,#21049,#17129,.T.);
#27875=EDGE_CURVE('',#21050,#21050,#17130,.T.);
#27876=EDGE_CURVE('',#21050,#21051,#11425,.T.);
#27877=EDGE_CURVE('',#21051,#21051,#17131,.T.);
#27878=EDGE_CURVE('',#21052,#21052,#17132,.T.);
#27879=EDGE_CURVE('',#21052,#21053,#11426,.T.);
#27880=EDGE_CURVE('',#21053,#21054,#17133,.T.);
#27881=EDGE_CURVE('',#21055,#21054,#11427,.T.);
#27882=EDGE_CURVE('',#21056,#21055,#17134,.T.);
#27883=EDGE_CURVE('',#21056,#21057,#11428,.T.);
#27884=EDGE_CURVE('',#21057,#21057,#17135,.T.);
#27885=EDGE_CURVE('',#21056,#21053,#11429,.T.);
#27886=EDGE_CURVE('',#21058,#21058,#17136,.T.);
#27887=EDGE_CURVE('',#21058,#21059,#11430,.T.);
#27888=EDGE_CURVE('',#21059,#21059,#17137,.T.);
#27889=EDGE_CURVE('',#21029,#21060,#11431,.T.);
#27890=EDGE_CURVE('',#21060,#21060,#17138,.T.);
#27891=EDGE_CURVE('',#21028,#21061,#11432,.T.);
#27892=EDGE_CURVE('',#21061,#21062,#17139,.T.);
#27893=EDGE_CURVE('',#21062,#21030,#11433,.T.);
#27894=EDGE_CURVE('',#21063,#21064,#17140,.T.);
#27895=EDGE_CURVE('',#21063,#21065,#11434,.T.);
#27896=EDGE_CURVE('',#21065,#21020,#17141,.T.);
#27897=EDGE_CURVE('',#21066,#21018,#17142,.T.);
#27898=EDGE_CURVE('',#21066,#21067,#11435,.T.);
#27899=EDGE_CURVE('',#21068,#21067,#17143,.T.);
#27900=EDGE_CURVE('',#21064,#21068,#11436,.T.);
#27901=EDGE_CURVE('',#21069,#21070,#11437,.T.);
#27902=EDGE_CURVE('',#21069,#21071,#11438,.T.);
#27903=EDGE_CURVE('',#21071,#21072,#11439,.T.);
#27904=EDGE_CURVE('',#21072,#21070,#11440,.T.);
#27905=EDGE_CURVE('',#21073,#21074,#11441,.T.);
#27906=EDGE_CURVE('',#21073,#21075,#17144,.T.);
#27907=EDGE_CURVE('',#21076,#21075,#11442,.T.);
#27908=EDGE_CURVE('',#21076,#21077,#17145,.T.);
#27909=EDGE_CURVE('',#21078,#21077,#11443,.T.);
#27910=EDGE_CURVE('',#21024,#21078,#17146,.T.);
#27911=EDGE_CURVE('',#21062,#21074,#17147,.T.);
#27912=EDGE_CURVE('',#21074,#21079,#11444,.T.);
#27913=EDGE_CURVE('',#21080,#21061,#17148,.T.);
#27914=EDGE_CURVE('',#21054,#21080,#11445,.T.);
#27915=EDGE_CURVE('',#21081,#21053,#11446,.T.);
#27916=EDGE_CURVE('',#21082,#21081,#17149,.T.);
#27917=EDGE_CURVE('',#21082,#21083,#11447,.T.);
#27918=EDGE_CURVE('',#21083,#21084,#11448,.T.);
#27919=EDGE_CURVE('',#21084,#21085,#11449,.T.);
#27920=EDGE_CURVE('',#21085,#21086,#11450,.T.);
#27921=EDGE_CURVE('',#21086,#21077,#11451,.T.);
#27922=EDGE_CURVE('',#21079,#21076,#11452,.T.);
#27923=EDGE_CURVE('',#21087,#21088,#11453,.T.);
#27924=EDGE_CURVE('',#21088,#21089,#11454,.T.);
#27925=EDGE_CURVE('',#21069,#21089,#11455,.T.);
#27926=EDGE_CURVE('',#21075,#21069,#11456,.T.);
#27927=EDGE_CURVE('',#21087,#21073,#11457,.T.);
#27928=EDGE_CURVE('',#21090,#21091,#11458,.T.);
#27929=EDGE_CURVE('',#21090,#21092,#11459,.T.);
#27930=EDGE_CURVE('',#21092,#21070,#11460,.T.);
#27931=EDGE_CURVE('',#21070,#21093,#11461,.T.);
#27932=EDGE_CURVE('',#21093,#21091,#11462,.T.);
#27933=EDGE_CURVE('',#21094,#21095,#11463,.T.);
#27934=EDGE_CURVE('',#21095,#21096,#11464,.T.);
#27935=EDGE_CURVE('',#21097,#21096,#11465,.T.);
#27936=EDGE_CURVE('',#21097,#21094,#11466,.T.);
#27937=EDGE_CURVE('',#21043,#21065,#17150,.T.);
#27938=EDGE_CURVE('',#21042,#21098,#11467,.T.);
#27939=EDGE_CURVE('',#21098,#21099,#17151,.T.);
#27940=EDGE_CURVE('',#21099,#21100,#11468,.T.);
#27941=EDGE_CURVE('',#21100,#21101,#17152,.T.);
#27942=EDGE_CURVE('',#21101,#21102,#11469,.T.);
#27943=EDGE_CURVE('',#21102,#21103,#17153,.T.);
#27944=EDGE_CURVE('',#21103,#21104,#11470,.T.);
#27945=EDGE_CURVE('',#21105,#21104,#17154,.T.);
#27946=EDGE_CURVE('',#21021,#21105,#17155,.T.);
#27947=EDGE_CURVE('',#21106,#21105,#11471,.T.);
#27948=EDGE_CURVE('',#21036,#21106,#17156,.T.);
#27949=EDGE_CURVE('',#21019,#21034,#17157,.T.);
#27950=EDGE_CURVE('',#21107,#21027,#17158,.T.);
#27951=EDGE_CURVE('',#21107,#21080,#11472,.T.);
#27952=EDGE_CURVE('',#21108,#21037,#11473,.T.);
#27953=EDGE_CURVE('',#21108,#21109,#11474,.T.);
#27954=EDGE_CURVE('',#21109,#21035,#11475,.T.);
#27955=EDGE_CURVE('',#21110,#21111,#11476,.T.);
#27956=EDGE_CURVE('',#21112,#21111,#11477,.T.);
#27957=EDGE_CURVE('',#21113,#21112,#11478,.T.);
#27958=EDGE_CURVE('',#21113,#21114,#11479,.T.);
#27959=EDGE_CURVE('',#21115,#21114,#11480,.T.);
#27960=EDGE_CURVE('',#21110,#21115,#11481,.T.);
#27961=EDGE_CURVE('',#21116,#21117,#11482,.T.);
#27962=EDGE_CURVE('',#21117,#21118,#11483,.T.);
#27963=EDGE_CURVE('',#21118,#21119,#11484,.T.);
#27964=EDGE_CURVE('',#21119,#21120,#11485,.T.);
#27965=EDGE_CURVE('',#21120,#21121,#11486,.T.);
#27966=EDGE_CURVE('',#21121,#21122,#11487,.T.);
#27967=EDGE_CURVE('',#21122,#21123,#11488,.T.);
#27968=EDGE_CURVE('',#21123,#21116,#11489,.T.);
#27969=EDGE_CURVE('',#21124,#21125,#11490,.T.);
#27970=EDGE_CURVE('',#21126,#21124,#11491,.T.);
#27971=EDGE_CURVE('',#21127,#21126,#11492,.T.);
#27972=EDGE_CURVE('',#21128,#21127,#11493,.T.);
#27973=EDGE_CURVE('',#21129,#21128,#11494,.T.);
#27974=EDGE_CURVE('',#21130,#21129,#11495,.T.);
#27975=EDGE_CURVE('',#21131,#21130,#11496,.T.);
#27976=EDGE_CURVE('',#21125,#21131,#11497,.T.);
#27977=EDGE_CURVE('',#21132,#21109,#11498,.T.);
#27978=EDGE_CURVE('',#21132,#21133,#11499,.T.);
#27979=EDGE_CURVE('',#21134,#21133,#11500,.T.);
#27980=EDGE_CURVE('',#21135,#21134,#11501,.T.);
#27981=EDGE_CURVE('',#21136,#21135,#11502,.T.);
#27982=EDGE_CURVE('',#21137,#21136,#11503,.T.);
#27983=EDGE_CURVE('',#21138,#21137,#11504,.T.);
#27984=EDGE_CURVE('',#21139,#21138,#11505,.T.);
#27985=EDGE_CURVE('',#21140,#21139,#11506,.T.);
#27986=EDGE_CURVE('',#21141,#21140,#17159,.T.);
#27987=EDGE_CURVE('',#21142,#21141,#11507,.T.);
#27988=EDGE_CURVE('',#21143,#21142,#17160,.T.);
#27989=EDGE_CURVE('',#21144,#21143,#11508,.T.);
#27990=EDGE_CURVE('',#21145,#21144,#17161,.T.);
#27991=EDGE_CURVE('',#21146,#21145,#11509,.T.);
#27992=EDGE_CURVE('',#21146,#21147,#11510,.T.);
#27993=EDGE_CURVE('',#21148,#21147,#11511,.T.);
#27994=EDGE_CURVE('',#21149,#21148,#17162,.T.);
#27995=EDGE_CURVE('',#21150,#21149,#11512,.T.);
#27996=EDGE_CURVE('',#21151,#21150,#17163,.T.);
#27997=EDGE_CURVE('',#21152,#21151,#11513,.T.);
#27998=EDGE_CURVE('',#21153,#21152,#17164,.T.);
#27999=EDGE_CURVE('',#21041,#21153,#11514,.T.);
#28000=EDGE_CURVE('',#21154,#21040,#11515,.T.);
#28001=EDGE_CURVE('',#21155,#21154,#17165,.T.);
#28002=EDGE_CURVE('',#21156,#21155,#11516,.T.);
#28003=EDGE_CURVE('',#21111,#21156,#17166,.T.);
#28004=EDGE_CURVE('',#21110,#21066,#17167,.T.);
#28005=EDGE_CURVE('',#21157,#21134,#11517,.T.);
#28006=EDGE_CURVE('',#21157,#21158,#11518,.T.);
#28007=EDGE_CURVE('',#21158,#21135,#11519,.T.);
#28008=EDGE_CURVE('',#21095,#21093,#11520,.T.);
#28009=EDGE_CURVE('',#21094,#21157,#11521,.T.);
#28010=EDGE_CURVE('',#21159,#21133,#11522,.T.);
#28011=EDGE_CURVE('',#21089,#21159,#11523,.T.);
#28012=EDGE_CURVE('',#21091,#21088,#11524,.T.);
#28013=EDGE_CURVE('',#21160,#21161,#11525,.T.);
#28014=EDGE_CURVE('',#21160,#21159,#11526,.T.);
#28015=EDGE_CURVE('',#21133,#21161,#11527,.T.);
#28016=EDGE_CURVE('',#21072,#21096,#11528,.T.);
#28017=EDGE_CURVE('',#21071,#21160,#11529,.T.);
#28018=EDGE_CURVE('',#21162,#21161,#11530,.T.);
#28019=EDGE_CURVE('',#21086,#21162,#11531,.T.);
#28020=EDGE_CURVE('',#21163,#21085,#11532,.T.);
#28021=EDGE_CURVE('',#21163,#21097,#11533,.T.);
#28022=EDGE_CURVE('',#21164,#21084,#11534,.T.);
#28023=EDGE_CURVE('',#21164,#21165,#11535,.T.);
#28024=EDGE_CURVE('',#21165,#21163,#11536,.T.);
#28025=EDGE_CURVE('',#21083,#21139,#11537,.T.);
#28026=EDGE_CURVE('',#21166,#21138,#11538,.T.);
#28027=EDGE_CURVE('',#21166,#21164,#11539,.T.);
#28028=EDGE_CURVE('',#21167,#21137,#11540,.T.);
#28029=EDGE_CURVE('',#21167,#21166,#11541,.T.);
#28030=EDGE_CURVE('',#21168,#21136,#11542,.T.);
#28031=EDGE_CURVE('',#21168,#21167,#11543,.T.);
#28032=EDGE_CURVE('',#21158,#21168,#11544,.T.);
#28033=EDGE_CURVE('',#21158,#21121,#11545,.T.);
#28034=EDGE_CURVE('',#21122,#21157,#11546,.T.);
#28035=EDGE_CURVE('',#21123,#21094,#11547,.T.);
#28036=EDGE_CURVE('',#21168,#21120,#11548,.T.);
#28037=EDGE_CURVE('',#21116,#21097,#11549,.T.);
#28038=EDGE_CURVE('',#21167,#21119,#11550,.T.);
#28039=EDGE_CURVE('',#21117,#21165,#11551,.T.);
#28040=EDGE_CURVE('',#21166,#21118,#11552,.T.);
#28041=EDGE_CURVE('',#21162,#21146,#11553,.T.);
#28042=EDGE_CURVE('',#21169,#21145,#11554,.T.);
#28043=EDGE_CURVE('',#21169,#21078,#11555,.T.);
#28044=EDGE_CURVE('',#21170,#21144,#11556,.T.);
#28045=EDGE_CURVE('',#21170,#21169,#17168,.T.);
#28046=EDGE_CURVE('',#21171,#21143,#11557,.T.);
#28047=EDGE_CURVE('',#21171,#21170,#11558,.T.);
#28048=EDGE_CURVE('',#21172,#21142,#11559,.T.);
#28049=EDGE_CURVE('',#21172,#21171,#17169,.T.);
#28050=EDGE_CURVE('',#21173,#21141,#11560,.T.);
#28051=EDGE_CURVE('',#21173,#21172,#11561,.T.);
#28052=EDGE_CURVE('',#21174,#21140,#11562,.T.);
#28053=EDGE_CURVE('',#21174,#21173,#17170,.T.);
#28054=EDGE_CURVE('',#21082,#21175,#11563,.T.);
#28055=EDGE_CURVE('',#21175,#21174,#11564,.T.);
#28056=EDGE_CURVE('',#21176,#21081,#11565,.T.);
#28057=EDGE_CURVE('',#21175,#21176,#17171,.T.);
#28058=EDGE_CURVE('',#21176,#21056,#11566,.T.);
#28059=EDGE_CURVE('',#21055,#21107,#11567,.T.);
#28060=EDGE_CURVE('',#21177,#21038,#11568,.T.);
#28061=EDGE_CURVE('',#21177,#21154,#11569,.T.);
#28062=EDGE_CURVE('',#21178,#21177,#17172,.T.);
#28063=EDGE_CURVE('',#21178,#21155,#11570,.T.);
#28064=EDGE_CURVE('',#21179,#21178,#11571,.T.);
#28065=EDGE_CURVE('',#21179,#21156,#11572,.T.);
#28066=EDGE_CURVE('',#21112,#21179,#17173,.T.);
#28067=EDGE_CURVE('',#21180,#21181,#11573,.T.);
#28068=EDGE_CURVE('',#21181,#21132,#11574,.T.);
#28069=EDGE_CURVE('',#21180,#21108,#11575,.T.);
#28070=EDGE_CURVE('',#21182,#21183,#11576,.T.);
#28071=EDGE_CURVE('',#21183,#21181,#11577,.T.);
#28072=EDGE_CURVE('',#21182,#21180,#11578,.T.);
#28073=EDGE_CURVE('',#21147,#21183,#11579,.T.);
#28074=EDGE_CURVE('',#21184,#21182,#11580,.T.);
#28075=EDGE_CURVE('',#21184,#21104,#11581,.T.);
#28076=EDGE_CURVE('',#21103,#21148,#11582,.T.);
#28077=EDGE_CURVE('',#21102,#21149,#11583,.T.);
#28078=EDGE_CURVE('',#21101,#21150,#11584,.T.);
#28079=EDGE_CURVE('',#21100,#21151,#11585,.T.);
#28080=EDGE_CURVE('',#21099,#21152,#11586,.T.);
#28081=EDGE_CURVE('',#21098,#21153,#11587,.T.);
#28082=EDGE_CURVE('',#21067,#21115,#17174,.T.);
#28083=EDGE_CURVE('',#21114,#21068,#11588,.T.);
#28084=EDGE_CURVE('',#21185,#21124,#11589,.T.);
#28085=EDGE_CURVE('',#21186,#21185,#11590,.T.);
#28086=EDGE_CURVE('',#21186,#21126,#11591,.T.);
#28087=EDGE_CURVE('',#21187,#21186,#11592,.T.);
#28088=EDGE_CURVE('',#21187,#21127,#11593,.T.);
#28089=EDGE_CURVE('',#21188,#21187,#11594,.T.);
#28090=EDGE_CURVE('',#21188,#21128,#11595,.T.);
#28091=EDGE_CURVE('',#21189,#21188,#11596,.T.);
#28092=EDGE_CURVE('',#21189,#21129,#11597,.T.);
#28093=EDGE_CURVE('',#21190,#21189,#11598,.T.);
#28094=EDGE_CURVE('',#21190,#21130,#11599,.T.);
#28095=EDGE_CURVE('',#21191,#21190,#11600,.T.);
#28096=EDGE_CURVE('',#21191,#21131,#11601,.T.);
#28097=EDGE_CURVE('',#21192,#21191,#11602,.T.);
#28098=EDGE_CURVE('',#21192,#21125,#11603,.T.);
#28099=EDGE_CURVE('',#21185,#21192,#11604,.T.);
#28100=EDGE_CURVE('',#21106,#21184,#17175,.T.);
#28101=EDGE_CURVE('',#21193,#21113,#11605,.T.);
#28102=EDGE_CURVE('',#21193,#21194,#11606,.T.);
#28103=EDGE_CURVE('',#21194,#21195,#11607,.T.);
#28104=EDGE_CURVE('',#21195,#21196,#11608,.T.);
#28105=EDGE_CURVE('',#21064,#21196,#11609,.T.);
#28106=EDGE_CURVE('',#21039,#21063,#17176,.T.);
#28107=EDGE_CURVE('',#21193,#21197,#11610,.T.);
#28108=EDGE_CURVE('',#21197,#21196,#11611,.T.);
#28109=EDGE_CURVE('',#21087,#21090,#11612,.T.);
#28110=EDGE_CURVE('',#21194,#21198,#11613,.T.);
#28111=EDGE_CURVE('',#21198,#21195,#11614,.T.);
#28112=EDGE_CURVE('',#21198,#21197,#11615,.T.);
#28113=EDGE_CURVE('',#21079,#21092,#11616,.T.);
#28114=EDGE_CURVE('',#21199,#21200,#17177,.T.);
#28115=EDGE_CURVE('',#21011,#21199,#11617,.T.);
#28116=EDGE_CURVE('',#21200,#21008,#11618,.T.);
#28117=EDGE_CURVE('',#21201,#21202,#17178,.T.);
#28118=EDGE_CURVE('',#21199,#21201,#11619,.T.);
#28119=EDGE_CURVE('',#21202,#21200,#11620,.T.);
#28120=EDGE_CURVE('',#21201,#21012,#11621,.T.);
#28121=EDGE_CURVE('',#21007,#21202,#11622,.T.);
#28122=ORIENTED_EDGE('',*,*,#21203,.T.);
#28123=ORIENTED_EDGE('',*,*,#21204,.T.);
#28124=ORIENTED_EDGE('',*,*,#21205,.F.);
#28125=ORIENTED_EDGE('',*,*,#21204,.F.);
#28126=ORIENTED_EDGE('',*,*,#21206,.T.);
#28127=ORIENTED_EDGE('',*,*,#21207,.T.);
#28128=ORIENTED_EDGE('',*,*,#21208,.F.);
#28129=ORIENTED_EDGE('',*,*,#21207,.F.);
#28130=ORIENTED_EDGE('',*,*,#21208,.T.);
#28131=ORIENTED_EDGE('',*,*,#21203,.F.);
#28132=ORIENTED_EDGE('',*,*,#21206,.F.);
#28133=ORIENTED_EDGE('',*,*,#21205,.T.);
#28134=ORIENTED_EDGE('',*,*,#21209,.T.);
#28135=ORIENTED_EDGE('',*,*,#21210,.T.);
#28136=ORIENTED_EDGE('',*,*,#21211,.T.);
#28137=ORIENTED_EDGE('',*,*,#21212,.T.);
#28138=ORIENTED_EDGE('',*,*,#21210,.F.);
#28139=ORIENTED_EDGE('',*,*,#21211,.F.);
#28140=ORIENTED_EDGE('',*,*,#21212,.F.);
#28141=ORIENTED_EDGE('',*,*,#21209,.F.);
#28142=ORIENTED_EDGE('',*,*,#21213,.F.);
#28143=ORIENTED_EDGE('',*,*,#21214,.T.);
#28144=ORIENTED_EDGE('',*,*,#21215,.F.);
#28145=ORIENTED_EDGE('',*,*,#21214,.F.);
#28146=ORIENTED_EDGE('',*,*,#21215,.T.);
#28147=ORIENTED_EDGE('',*,*,#21216,.T.);
#28148=ORIENTED_EDGE('',*,*,#21217,.T.);
#28149=ORIENTED_EDGE('',*,*,#21216,.F.);
#28150=ORIENTED_EDGE('',*,*,#21217,.F.);
#28151=ORIENTED_EDGE('',*,*,#21213,.T.);
#28152=ORIENTED_EDGE('',*,*,#21218,.F.);
#28153=ORIENTED_EDGE('',*,*,#21219,.T.);
#28154=ORIENTED_EDGE('',*,*,#21220,.T.);
#28155=ORIENTED_EDGE('',*,*,#21221,.F.);
#28156=ORIENTED_EDGE('',*,*,#21222,.T.);
#28157=ORIENTED_EDGE('',*,*,#21219,.F.);
#28158=ORIENTED_EDGE('',*,*,#21222,.F.);
#28159=ORIENTED_EDGE('',*,*,#21223,.T.);
#28160=ORIENTED_EDGE('',*,*,#21220,.F.);
#28161=ORIENTED_EDGE('',*,*,#21218,.T.);
#28162=ORIENTED_EDGE('',*,*,#21221,.T.);
#28163=ORIENTED_EDGE('',*,*,#21223,.F.);
#28164=ORIENTED_EDGE('',*,*,#21224,.T.);
#28165=ORIENTED_EDGE('',*,*,#21225,.T.);
#28166=ORIENTED_EDGE('',*,*,#21226,.T.);
#28167=ORIENTED_EDGE('',*,*,#21227,.F.);
#28168=ORIENTED_EDGE('',*,*,#21228,.F.);
#28169=ORIENTED_EDGE('',*,*,#21229,.T.);
#28170=ORIENTED_EDGE('',*,*,#21230,.T.);
#28171=ORIENTED_EDGE('',*,*,#21231,.F.);
#28172=ORIENTED_EDGE('',*,*,#21232,.T.);
#28173=ORIENTED_EDGE('',*,*,#21233,.F.);
#28174=ORIENTED_EDGE('',*,*,#21234,.F.);
#28175=ORIENTED_EDGE('',*,*,#21235,.F.);
#28176=ORIENTED_EDGE('',*,*,#21236,.F.);
#28177=ORIENTED_EDGE('',*,*,#21231,.T.);
#28178=ORIENTED_EDGE('',*,*,#21237,.F.);
#28179=ORIENTED_EDGE('',*,*,#21238,.F.);
#28180=ORIENTED_EDGE('',*,*,#21239,.F.);
#28181=ORIENTED_EDGE('',*,*,#21224,.F.);
#28182=ORIENTED_EDGE('',*,*,#21234,.T.);
#28183=ORIENTED_EDGE('',*,*,#21240,.T.);
#28184=ORIENTED_EDGE('',*,*,#21241,.F.);
#28185=ORIENTED_EDGE('',*,*,#21242,.T.);
#28186=ORIENTED_EDGE('',*,*,#21241,.T.);
#28187=ORIENTED_EDGE('',*,*,#21243,.T.);
#28188=ORIENTED_EDGE('',*,*,#21244,.F.);
#28189=ORIENTED_EDGE('',*,*,#21245,.T.);
#28190=ORIENTED_EDGE('',*,*,#21246,.T.);
#28191=ORIENTED_EDGE('',*,*,#21247,.T.);
#28192=ORIENTED_EDGE('',*,*,#21248,.F.);
#28193=ORIENTED_EDGE('',*,*,#21244,.T.);
#28194=ORIENTED_EDGE('',*,*,#21249,.T.);
#28195=ORIENTED_EDGE('',*,*,#21250,.T.);
#28196=ORIENTED_EDGE('',*,*,#21251,.F.);
#28197=ORIENTED_EDGE('',*,*,#21252,.T.);
#28198=ORIENTED_EDGE('',*,*,#21253,.T.);
#28199=ORIENTED_EDGE('',*,*,#21254,.T.);
#28200=ORIENTED_EDGE('',*,*,#21255,.F.);
#28201=ORIENTED_EDGE('',*,*,#21256,.F.);
#28202=ORIENTED_EDGE('',*,*,#21257,.F.);
#28203=ORIENTED_EDGE('',*,*,#21226,.F.);
#28204=ORIENTED_EDGE('',*,*,#21251,.T.);
#28205=ORIENTED_EDGE('',*,*,#21258,.T.);
#28206=ORIENTED_EDGE('',*,*,#21259,.T.);
#28207=ORIENTED_EDGE('',*,*,#21229,.F.);
#28208=ORIENTED_EDGE('',*,*,#21260,.F.);
#28209=ORIENTED_EDGE('',*,*,#21261,.T.);
#28210=ORIENTED_EDGE('',*,*,#21262,.T.);
#28211=ORIENTED_EDGE('',*,*,#21263,.T.);
#28212=ORIENTED_EDGE('',*,*,#21260,.T.);
#28213=ORIENTED_EDGE('',*,*,#21228,.T.);
#28214=ORIENTED_EDGE('',*,*,#21236,.T.);
#28215=ORIENTED_EDGE('',*,*,#21259,.F.);
#28216=ORIENTED_EDGE('',*,*,#21264,.T.);
#28217=ORIENTED_EDGE('',*,*,#21265,.F.);
#28218=ORIENTED_EDGE('',*,*,#21232,.F.);
#28219=ORIENTED_EDGE('',*,*,#21230,.F.);
#28220=ORIENTED_EDGE('',*,*,#21265,.T.);
#28221=ORIENTED_EDGE('',*,*,#21266,.T.);
#28222=ORIENTED_EDGE('',*,*,#21246,.F.);
#28223=ORIENTED_EDGE('',*,*,#21243,.F.);
#28224=ORIENTED_EDGE('',*,*,#21240,.F.);
#28225=ORIENTED_EDGE('',*,*,#21233,.T.);
#28226=ORIENTED_EDGE('',*,*,#21248,.T.);
#28227=ORIENTED_EDGE('',*,*,#21267,.T.);
#28228=ORIENTED_EDGE('',*,*,#21262,.F.);
#28229=ORIENTED_EDGE('',*,*,#21235,.T.);
#28230=ORIENTED_EDGE('',*,*,#21242,.F.);
#28231=ORIENTED_EDGE('',*,*,#21245,.F.);
#28232=ORIENTED_EDGE('',*,*,#21238,.T.);
#28233=ORIENTED_EDGE('',*,*,#21268,.T.);
#28234=ORIENTED_EDGE('',*,*,#21256,.T.);
#28235=ORIENTED_EDGE('',*,*,#21269,.F.);
#28236=ORIENTED_EDGE('',*,*,#21237,.T.);
#28237=ORIENTED_EDGE('',*,*,#21227,.T.);
#28238=ORIENTED_EDGE('',*,*,#21257,.T.);
#28239=ORIENTED_EDGE('',*,*,#21268,.F.);
#28240=ORIENTED_EDGE('',*,*,#21239,.T.);
#28241=ORIENTED_EDGE('',*,*,#21269,.T.);
#28242=ORIENTED_EDGE('',*,*,#21255,.T.);
#28243=ORIENTED_EDGE('',*,*,#21225,.F.);
#28244=ORIENTED_EDGE('',*,*,#21261,.F.);
#28245=ORIENTED_EDGE('',*,*,#21263,.F.);
#28246=ORIENTED_EDGE('',*,*,#21270,.F.);
#28247=ORIENTED_EDGE('',*,*,#21252,.F.);
#28248=ORIENTED_EDGE('',*,*,#21270,.T.);
#28249=ORIENTED_EDGE('',*,*,#21267,.F.);
#28250=ORIENTED_EDGE('',*,*,#21271,.F.);
#28251=ORIENTED_EDGE('',*,*,#21253,.F.);
#28252=ORIENTED_EDGE('',*,*,#21271,.T.);
#28253=ORIENTED_EDGE('',*,*,#21247,.F.);
#28254=ORIENTED_EDGE('',*,*,#21272,.F.);
#28255=ORIENTED_EDGE('',*,*,#21254,.F.);
#28256=ORIENTED_EDGE('',*,*,#21272,.T.);
#28257=ORIENTED_EDGE('',*,*,#21266,.F.);
#28258=ORIENTED_EDGE('',*,*,#21273,.F.);
#28259=ORIENTED_EDGE('',*,*,#21249,.F.);
#28260=ORIENTED_EDGE('',*,*,#21273,.T.);
#28261=ORIENTED_EDGE('',*,*,#21264,.F.);
#28262=ORIENTED_EDGE('',*,*,#21258,.F.);
#28263=ORIENTED_EDGE('',*,*,#21250,.F.);
#28264=ORIENTED_EDGE('',*,*,#21274,.T.);
#28265=ORIENTED_EDGE('',*,*,#21275,.T.);
#28266=ORIENTED_EDGE('',*,*,#21276,.F.);
#28267=ORIENTED_EDGE('',*,*,#21275,.F.);
#28268=ORIENTED_EDGE('',*,*,#21277,.T.);
#28269=ORIENTED_EDGE('',*,*,#21278,.T.);
#28270=ORIENTED_EDGE('',*,*,#21279,.F.);
#28271=ORIENTED_EDGE('',*,*,#21278,.F.);
#28272=ORIENTED_EDGE('',*,*,#21280,.T.);
#28273=ORIENTED_EDGE('',*,*,#21281,.T.);
#28274=ORIENTED_EDGE('',*,*,#21282,.T.);
#28275=ORIENTED_EDGE('',*,*,#21283,.T.);
#28276=ORIENTED_EDGE('',*,*,#21284,.T.);
#28277=ORIENTED_EDGE('',*,*,#21285,.T.);
#28278=ORIENTED_EDGE('',*,*,#21286,.T.);
#28279=ORIENTED_EDGE('',*,*,#21287,.T.);
#28280=ORIENTED_EDGE('',*,*,#21288,.T.);
#28281=ORIENTED_EDGE('',*,*,#21289,.T.);
#28282=ORIENTED_EDGE('',*,*,#21290,.T.);
#28283=ORIENTED_EDGE('',*,*,#21291,.T.);
#28284=ORIENTED_EDGE('',*,*,#21292,.T.);
#28285=ORIENTED_EDGE('',*,*,#21293,.T.);
#28286=ORIENTED_EDGE('',*,*,#21294,.T.);
#28287=ORIENTED_EDGE('',*,*,#21295,.T.);
#28288=ORIENTED_EDGE('',*,*,#21296,.T.);
#28289=ORIENTED_EDGE('',*,*,#21297,.T.);
#28290=ORIENTED_EDGE('',*,*,#21298,.T.);
#28291=ORIENTED_EDGE('',*,*,#21299,.T.);
#28292=ORIENTED_EDGE('',*,*,#21300,.T.);
#28293=ORIENTED_EDGE('',*,*,#21301,.T.);
#28294=ORIENTED_EDGE('',*,*,#21302,.T.);
#28295=ORIENTED_EDGE('',*,*,#21303,.T.);
#28296=ORIENTED_EDGE('',*,*,#21304,.T.);
#28297=ORIENTED_EDGE('',*,*,#21305,.T.);
#28298=ORIENTED_EDGE('',*,*,#21306,.T.);
#28299=ORIENTED_EDGE('',*,*,#21307,.T.);
#28300=ORIENTED_EDGE('',*,*,#21308,.T.);
#28301=ORIENTED_EDGE('',*,*,#21309,.T.);
#28302=ORIENTED_EDGE('',*,*,#21310,.T.);
#28303=ORIENTED_EDGE('',*,*,#21311,.T.);
#28304=ORIENTED_EDGE('',*,*,#21312,.T.);
#28305=ORIENTED_EDGE('',*,*,#21313,.T.);
#28306=ORIENTED_EDGE('',*,*,#21314,.T.);
#28307=ORIENTED_EDGE('',*,*,#21315,.T.);
#28308=ORIENTED_EDGE('',*,*,#21316,.T.);
#28309=ORIENTED_EDGE('',*,*,#21317,.T.);
#28310=ORIENTED_EDGE('',*,*,#21318,.T.);
#28311=ORIENTED_EDGE('',*,*,#21319,.T.);
#28312=ORIENTED_EDGE('',*,*,#21320,.T.);
#28313=ORIENTED_EDGE('',*,*,#21321,.T.);
#28314=ORIENTED_EDGE('',*,*,#21322,.T.);
#28315=ORIENTED_EDGE('',*,*,#21323,.T.);
#28316=ORIENTED_EDGE('',*,*,#21324,.T.);
#28317=ORIENTED_EDGE('',*,*,#21325,.T.);
#28318=ORIENTED_EDGE('',*,*,#21326,.T.);
#28319=ORIENTED_EDGE('',*,*,#21327,.T.);
#28320=ORIENTED_EDGE('',*,*,#21328,.T.);
#28321=ORIENTED_EDGE('',*,*,#21329,.T.);
#28322=ORIENTED_EDGE('',*,*,#21330,.T.);
#28323=ORIENTED_EDGE('',*,*,#21331,.T.);
#28324=ORIENTED_EDGE('',*,*,#21332,.T.);
#28325=ORIENTED_EDGE('',*,*,#21333,.T.);
#28326=ORIENTED_EDGE('',*,*,#21334,.T.);
#28327=ORIENTED_EDGE('',*,*,#21335,.T.);
#28328=ORIENTED_EDGE('',*,*,#21336,.T.);
#28329=ORIENTED_EDGE('',*,*,#21337,.T.);
#28330=ORIENTED_EDGE('',*,*,#21338,.T.);
#28331=ORIENTED_EDGE('',*,*,#21339,.T.);
#28332=ORIENTED_EDGE('',*,*,#21340,.T.);
#28333=ORIENTED_EDGE('',*,*,#21341,.T.);
#28334=ORIENTED_EDGE('',*,*,#21342,.T.);
#28335=ORIENTED_EDGE('',*,*,#21343,.T.);
#28336=ORIENTED_EDGE('',*,*,#21344,.T.);
#28337=ORIENTED_EDGE('',*,*,#21345,.T.);
#28338=ORIENTED_EDGE('',*,*,#21346,.T.);
#28339=ORIENTED_EDGE('',*,*,#21347,.T.);
#28340=ORIENTED_EDGE('',*,*,#21348,.T.);
#28341=ORIENTED_EDGE('',*,*,#21349,.T.);
#28342=ORIENTED_EDGE('',*,*,#21350,.T.);
#28343=ORIENTED_EDGE('',*,*,#21351,.T.);
#28344=ORIENTED_EDGE('',*,*,#21352,.T.);
#28345=ORIENTED_EDGE('',*,*,#21353,.T.);
#28346=ORIENTED_EDGE('',*,*,#21354,.T.);
#28347=ORIENTED_EDGE('',*,*,#21355,.T.);
#28348=ORIENTED_EDGE('',*,*,#21356,.T.);
#28349=ORIENTED_EDGE('',*,*,#21357,.T.);
#28350=ORIENTED_EDGE('',*,*,#21358,.T.);
#28351=ORIENTED_EDGE('',*,*,#21359,.T.);
#28352=ORIENTED_EDGE('',*,*,#21360,.T.);
#28353=ORIENTED_EDGE('',*,*,#21361,.T.);
#28354=ORIENTED_EDGE('',*,*,#21362,.T.);
#28355=ORIENTED_EDGE('',*,*,#21363,.T.);
#28356=ORIENTED_EDGE('',*,*,#21364,.T.);
#28357=ORIENTED_EDGE('',*,*,#21365,.T.);
#28358=ORIENTED_EDGE('',*,*,#21366,.T.);
#28359=ORIENTED_EDGE('',*,*,#21367,.T.);
#28360=ORIENTED_EDGE('',*,*,#21368,.T.);
#28361=ORIENTED_EDGE('',*,*,#21369,.T.);
#28362=ORIENTED_EDGE('',*,*,#21370,.T.);
#28363=ORIENTED_EDGE('',*,*,#21371,.T.);
#28364=ORIENTED_EDGE('',*,*,#21372,.T.);
#28365=ORIENTED_EDGE('',*,*,#21373,.T.);
#28366=ORIENTED_EDGE('',*,*,#21374,.T.);
#28367=ORIENTED_EDGE('',*,*,#21375,.T.);
#28368=ORIENTED_EDGE('',*,*,#21376,.T.);
#28369=ORIENTED_EDGE('',*,*,#21377,.T.);
#28370=ORIENTED_EDGE('',*,*,#21378,.T.);
#28371=ORIENTED_EDGE('',*,*,#21379,.T.);
#28372=ORIENTED_EDGE('',*,*,#21380,.T.);
#28373=ORIENTED_EDGE('',*,*,#21381,.T.);
#28374=ORIENTED_EDGE('',*,*,#21382,.T.);
#28375=ORIENTED_EDGE('',*,*,#21383,.T.);
#28376=ORIENTED_EDGE('',*,*,#21384,.T.);
#28377=ORIENTED_EDGE('',*,*,#21385,.T.);
#28378=ORIENTED_EDGE('',*,*,#21386,.T.);
#28379=ORIENTED_EDGE('',*,*,#21387,.T.);
#28380=ORIENTED_EDGE('',*,*,#21388,.T.);
#28381=ORIENTED_EDGE('',*,*,#21389,.T.);
#28382=ORIENTED_EDGE('',*,*,#21390,.T.);
#28383=ORIENTED_EDGE('',*,*,#21391,.T.);
#28384=ORIENTED_EDGE('',*,*,#21392,.T.);
#28385=ORIENTED_EDGE('',*,*,#21393,.T.);
#28386=ORIENTED_EDGE('',*,*,#21394,.T.);
#28387=ORIENTED_EDGE('',*,*,#21395,.T.);
#28388=ORIENTED_EDGE('',*,*,#21396,.T.);
#28389=ORIENTED_EDGE('',*,*,#21397,.T.);
#28390=ORIENTED_EDGE('',*,*,#21398,.T.);
#28391=ORIENTED_EDGE('',*,*,#21399,.T.);
#28392=ORIENTED_EDGE('',*,*,#21400,.T.);
#28393=ORIENTED_EDGE('',*,*,#21401,.T.);
#28394=ORIENTED_EDGE('',*,*,#21402,.T.);
#28395=ORIENTED_EDGE('',*,*,#21403,.T.);
#28396=ORIENTED_EDGE('',*,*,#21404,.T.);
#28397=ORIENTED_EDGE('',*,*,#21405,.T.);
#28398=ORIENTED_EDGE('',*,*,#21406,.T.);
#28399=ORIENTED_EDGE('',*,*,#21407,.T.);
#28400=ORIENTED_EDGE('',*,*,#21408,.T.);
#28401=ORIENTED_EDGE('',*,*,#21409,.T.);
#28402=ORIENTED_EDGE('',*,*,#21410,.T.);
#28403=ORIENTED_EDGE('',*,*,#21411,.T.);
#28404=ORIENTED_EDGE('',*,*,#21412,.T.);
#28405=ORIENTED_EDGE('',*,*,#21413,.T.);
#28406=ORIENTED_EDGE('',*,*,#21414,.T.);
#28407=ORIENTED_EDGE('',*,*,#21415,.T.);
#28408=ORIENTED_EDGE('',*,*,#21416,.T.);
#28409=ORIENTED_EDGE('',*,*,#21417,.T.);
#28410=ORIENTED_EDGE('',*,*,#21418,.T.);
#28411=ORIENTED_EDGE('',*,*,#21419,.T.);
#28412=ORIENTED_EDGE('',*,*,#21420,.T.);
#28413=ORIENTED_EDGE('',*,*,#21421,.T.);
#28414=ORIENTED_EDGE('',*,*,#21422,.T.);
#28415=ORIENTED_EDGE('',*,*,#21423,.T.);
#28416=ORIENTED_EDGE('',*,*,#21424,.T.);
#28417=ORIENTED_EDGE('',*,*,#21425,.T.);
#28418=ORIENTED_EDGE('',*,*,#21426,.T.);
#28419=ORIENTED_EDGE('',*,*,#21427,.T.);
#28420=ORIENTED_EDGE('',*,*,#21428,.T.);
#28421=ORIENTED_EDGE('',*,*,#21429,.T.);
#28422=ORIENTED_EDGE('',*,*,#21430,.T.);
#28423=ORIENTED_EDGE('',*,*,#21431,.T.);
#28424=ORIENTED_EDGE('',*,*,#21432,.T.);
#28425=ORIENTED_EDGE('',*,*,#21433,.T.);
#28426=ORIENTED_EDGE('',*,*,#21434,.T.);
#28427=ORIENTED_EDGE('',*,*,#21435,.T.);
#28428=ORIENTED_EDGE('',*,*,#21436,.T.);
#28429=ORIENTED_EDGE('',*,*,#21437,.T.);
#28430=ORIENTED_EDGE('',*,*,#21438,.T.);
#28431=ORIENTED_EDGE('',*,*,#21439,.T.);
#28432=ORIENTED_EDGE('',*,*,#21440,.T.);
#28433=ORIENTED_EDGE('',*,*,#21441,.T.);
#28434=ORIENTED_EDGE('',*,*,#21442,.T.);
#28435=ORIENTED_EDGE('',*,*,#21443,.T.);
#28436=ORIENTED_EDGE('',*,*,#21444,.T.);
#28437=ORIENTED_EDGE('',*,*,#21445,.T.);
#28438=ORIENTED_EDGE('',*,*,#21446,.T.);
#28439=ORIENTED_EDGE('',*,*,#21447,.T.);
#28440=ORIENTED_EDGE('',*,*,#21448,.T.);
#28441=ORIENTED_EDGE('',*,*,#21449,.T.);
#28442=ORIENTED_EDGE('',*,*,#21450,.T.);
#28443=ORIENTED_EDGE('',*,*,#21451,.T.);
#28444=ORIENTED_EDGE('',*,*,#21452,.T.);
#28445=ORIENTED_EDGE('',*,*,#21453,.T.);
#28446=ORIENTED_EDGE('',*,*,#21454,.T.);
#28447=ORIENTED_EDGE('',*,*,#21455,.T.);
#28448=ORIENTED_EDGE('',*,*,#21456,.T.);
#28449=ORIENTED_EDGE('',*,*,#21457,.T.);
#28450=ORIENTED_EDGE('',*,*,#21458,.T.);
#28451=ORIENTED_EDGE('',*,*,#21459,.T.);
#28452=ORIENTED_EDGE('',*,*,#21460,.T.);
#28453=ORIENTED_EDGE('',*,*,#21461,.T.);
#28454=ORIENTED_EDGE('',*,*,#21462,.T.);
#28455=ORIENTED_EDGE('',*,*,#21463,.T.);
#28456=ORIENTED_EDGE('',*,*,#21464,.T.);
#28457=ORIENTED_EDGE('',*,*,#21465,.T.);
#28458=ORIENTED_EDGE('',*,*,#21466,.T.);
#28459=ORIENTED_EDGE('',*,*,#21467,.T.);
#28460=ORIENTED_EDGE('',*,*,#21468,.T.);
#28461=ORIENTED_EDGE('',*,*,#21469,.T.);
#28462=ORIENTED_EDGE('',*,*,#21470,.T.);
#28463=ORIENTED_EDGE('',*,*,#21471,.T.);
#28464=ORIENTED_EDGE('',*,*,#21472,.T.);
#28465=ORIENTED_EDGE('',*,*,#21473,.T.);
#28466=ORIENTED_EDGE('',*,*,#21474,.T.);
#28467=ORIENTED_EDGE('',*,*,#21475,.T.);
#28468=ORIENTED_EDGE('',*,*,#21476,.T.);
#28469=ORIENTED_EDGE('',*,*,#21477,.T.);
#28470=ORIENTED_EDGE('',*,*,#21478,.T.);
#28471=ORIENTED_EDGE('',*,*,#21479,.T.);
#28472=ORIENTED_EDGE('',*,*,#21480,.T.);
#28473=ORIENTED_EDGE('',*,*,#21481,.T.);
#28474=ORIENTED_EDGE('',*,*,#21482,.F.);
#28475=ORIENTED_EDGE('',*,*,#21481,.F.);
#28476=ORIENTED_EDGE('',*,*,#21483,.T.);
#28477=ORIENTED_EDGE('',*,*,#21484,.T.);
#28478=ORIENTED_EDGE('',*,*,#21485,.T.);
#28479=ORIENTED_EDGE('',*,*,#21486,.T.);
#28480=ORIENTED_EDGE('',*,*,#21487,.T.);
#28481=ORIENTED_EDGE('',*,*,#21488,.T.);
#28482=ORIENTED_EDGE('',*,*,#21489,.T.);
#28483=ORIENTED_EDGE('',*,*,#21490,.T.);
#28484=ORIENTED_EDGE('',*,*,#21491,.T.);
#28485=ORIENTED_EDGE('',*,*,#21492,.T.);
#28486=ORIENTED_EDGE('',*,*,#21493,.T.);
#28487=ORIENTED_EDGE('',*,*,#21494,.T.);
#28488=ORIENTED_EDGE('',*,*,#21495,.T.);
#28489=ORIENTED_EDGE('',*,*,#21496,.T.);
#28490=ORIENTED_EDGE('',*,*,#21497,.T.);
#28491=ORIENTED_EDGE('',*,*,#21498,.T.);
#28492=ORIENTED_EDGE('',*,*,#21499,.T.);
#28493=ORIENTED_EDGE('',*,*,#21500,.T.);
#28494=ORIENTED_EDGE('',*,*,#21501,.T.);
#28495=ORIENTED_EDGE('',*,*,#21502,.T.);
#28496=ORIENTED_EDGE('',*,*,#21503,.T.);
#28497=ORIENTED_EDGE('',*,*,#21504,.T.);
#28498=ORIENTED_EDGE('',*,*,#21505,.T.);
#28499=ORIENTED_EDGE('',*,*,#21506,.T.);
#28500=ORIENTED_EDGE('',*,*,#21507,.T.);
#28501=ORIENTED_EDGE('',*,*,#21508,.T.);
#28502=ORIENTED_EDGE('',*,*,#21509,.T.);
#28503=ORIENTED_EDGE('',*,*,#21510,.T.);
#28504=ORIENTED_EDGE('',*,*,#21511,.T.);
#28505=ORIENTED_EDGE('',*,*,#21512,.T.);
#28506=ORIENTED_EDGE('',*,*,#21513,.T.);
#28507=ORIENTED_EDGE('',*,*,#21514,.T.);
#28508=ORIENTED_EDGE('',*,*,#21515,.T.);
#28509=ORIENTED_EDGE('',*,*,#21516,.T.);
#28510=ORIENTED_EDGE('',*,*,#21517,.T.);
#28511=ORIENTED_EDGE('',*,*,#21518,.T.);
#28512=ORIENTED_EDGE('',*,*,#21519,.T.);
#28513=ORIENTED_EDGE('',*,*,#21520,.T.);
#28514=ORIENTED_EDGE('',*,*,#21521,.T.);
#28515=ORIENTED_EDGE('',*,*,#21522,.T.);
#28516=ORIENTED_EDGE('',*,*,#21523,.T.);
#28517=ORIENTED_EDGE('',*,*,#21524,.T.);
#28518=ORIENTED_EDGE('',*,*,#21525,.T.);
#28519=ORIENTED_EDGE('',*,*,#21526,.T.);
#28520=ORIENTED_EDGE('',*,*,#21527,.T.);
#28521=ORIENTED_EDGE('',*,*,#21528,.T.);
#28522=ORIENTED_EDGE('',*,*,#21529,.T.);
#28523=ORIENTED_EDGE('',*,*,#21530,.T.);
#28524=ORIENTED_EDGE('',*,*,#21531,.T.);
#28525=ORIENTED_EDGE('',*,*,#21532,.T.);
#28526=ORIENTED_EDGE('',*,*,#21533,.T.);
#28527=ORIENTED_EDGE('',*,*,#21534,.T.);
#28528=ORIENTED_EDGE('',*,*,#21535,.T.);
#28529=ORIENTED_EDGE('',*,*,#21536,.T.);
#28530=ORIENTED_EDGE('',*,*,#21537,.T.);
#28531=ORIENTED_EDGE('',*,*,#21538,.T.);
#28532=ORIENTED_EDGE('',*,*,#21539,.T.);
#28533=ORIENTED_EDGE('',*,*,#21540,.T.);
#28534=ORIENTED_EDGE('',*,*,#21541,.T.);
#28535=ORIENTED_EDGE('',*,*,#21542,.T.);
#28536=ORIENTED_EDGE('',*,*,#21543,.T.);
#28537=ORIENTED_EDGE('',*,*,#21544,.T.);
#28538=ORIENTED_EDGE('',*,*,#21545,.T.);
#28539=ORIENTED_EDGE('',*,*,#21546,.T.);
#28540=ORIENTED_EDGE('',*,*,#21547,.T.);
#28541=ORIENTED_EDGE('',*,*,#21548,.T.);
#28542=ORIENTED_EDGE('',*,*,#21549,.T.);
#28543=ORIENTED_EDGE('',*,*,#21550,.T.);
#28544=ORIENTED_EDGE('',*,*,#21551,.T.);
#28545=ORIENTED_EDGE('',*,*,#21552,.T.);
#28546=ORIENTED_EDGE('',*,*,#21553,.T.);
#28547=ORIENTED_EDGE('',*,*,#21554,.T.);
#28548=ORIENTED_EDGE('',*,*,#21555,.T.);
#28549=ORIENTED_EDGE('',*,*,#21556,.T.);
#28550=ORIENTED_EDGE('',*,*,#21557,.T.);
#28551=ORIENTED_EDGE('',*,*,#21558,.T.);
#28552=ORIENTED_EDGE('',*,*,#21559,.T.);
#28553=ORIENTED_EDGE('',*,*,#21560,.T.);
#28554=ORIENTED_EDGE('',*,*,#21561,.T.);
#28555=ORIENTED_EDGE('',*,*,#21562,.T.);
#28556=ORIENTED_EDGE('',*,*,#21563,.T.);
#28557=ORIENTED_EDGE('',*,*,#21564,.T.);
#28558=ORIENTED_EDGE('',*,*,#21565,.T.);
#28559=ORIENTED_EDGE('',*,*,#21566,.T.);
#28560=ORIENTED_EDGE('',*,*,#21567,.T.);
#28561=ORIENTED_EDGE('',*,*,#21568,.T.);
#28562=ORIENTED_EDGE('',*,*,#21569,.T.);
#28563=ORIENTED_EDGE('',*,*,#21570,.T.);
#28564=ORIENTED_EDGE('',*,*,#21571,.T.);
#28565=ORIENTED_EDGE('',*,*,#21572,.T.);
#28566=ORIENTED_EDGE('',*,*,#21573,.T.);
#28567=ORIENTED_EDGE('',*,*,#21574,.T.);
#28568=ORIENTED_EDGE('',*,*,#21575,.T.);
#28569=ORIENTED_EDGE('',*,*,#21576,.T.);
#28570=ORIENTED_EDGE('',*,*,#21577,.T.);
#28571=ORIENTED_EDGE('',*,*,#21578,.T.);
#28572=ORIENTED_EDGE('',*,*,#21579,.T.);
#28573=ORIENTED_EDGE('',*,*,#21580,.T.);
#28574=ORIENTED_EDGE('',*,*,#21581,.T.);
#28575=ORIENTED_EDGE('',*,*,#21582,.T.);
#28576=ORIENTED_EDGE('',*,*,#21583,.T.);
#28577=ORIENTED_EDGE('',*,*,#21584,.T.);
#28578=ORIENTED_EDGE('',*,*,#21585,.T.);
#28579=ORIENTED_EDGE('',*,*,#21586,.T.);
#28580=ORIENTED_EDGE('',*,*,#21587,.T.);
#28581=ORIENTED_EDGE('',*,*,#21588,.T.);
#28582=ORIENTED_EDGE('',*,*,#21589,.T.);
#28583=ORIENTED_EDGE('',*,*,#21590,.T.);
#28584=ORIENTED_EDGE('',*,*,#21591,.T.);
#28585=ORIENTED_EDGE('',*,*,#21592,.T.);
#28586=ORIENTED_EDGE('',*,*,#21593,.T.);
#28587=ORIENTED_EDGE('',*,*,#21594,.T.);
#28588=ORIENTED_EDGE('',*,*,#21595,.T.);
#28589=ORIENTED_EDGE('',*,*,#21596,.T.);
#28590=ORIENTED_EDGE('',*,*,#21597,.T.);
#28591=ORIENTED_EDGE('',*,*,#21598,.T.);
#28592=ORIENTED_EDGE('',*,*,#21599,.T.);
#28593=ORIENTED_EDGE('',*,*,#21600,.T.);
#28594=ORIENTED_EDGE('',*,*,#21601,.T.);
#28595=ORIENTED_EDGE('',*,*,#21602,.T.);
#28596=ORIENTED_EDGE('',*,*,#21603,.T.);
#28597=ORIENTED_EDGE('',*,*,#21604,.T.);
#28598=ORIENTED_EDGE('',*,*,#21605,.T.);
#28599=ORIENTED_EDGE('',*,*,#21606,.T.);
#28600=ORIENTED_EDGE('',*,*,#21607,.T.);
#28601=ORIENTED_EDGE('',*,*,#21608,.T.);
#28602=ORIENTED_EDGE('',*,*,#21609,.T.);
#28603=ORIENTED_EDGE('',*,*,#21610,.T.);
#28604=ORIENTED_EDGE('',*,*,#21611,.T.);
#28605=ORIENTED_EDGE('',*,*,#21612,.T.);
#28606=ORIENTED_EDGE('',*,*,#21613,.T.);
#28607=ORIENTED_EDGE('',*,*,#21614,.T.);
#28608=ORIENTED_EDGE('',*,*,#21615,.T.);
#28609=ORIENTED_EDGE('',*,*,#21616,.T.);
#28610=ORIENTED_EDGE('',*,*,#21617,.T.);
#28611=ORIENTED_EDGE('',*,*,#21618,.T.);
#28612=ORIENTED_EDGE('',*,*,#21619,.T.);
#28613=ORIENTED_EDGE('',*,*,#21620,.T.);
#28614=ORIENTED_EDGE('',*,*,#21621,.T.);
#28615=ORIENTED_EDGE('',*,*,#21622,.T.);
#28616=ORIENTED_EDGE('',*,*,#21623,.T.);
#28617=ORIENTED_EDGE('',*,*,#21624,.T.);
#28618=ORIENTED_EDGE('',*,*,#21625,.T.);
#28619=ORIENTED_EDGE('',*,*,#21626,.T.);
#28620=ORIENTED_EDGE('',*,*,#21627,.T.);
#28621=ORIENTED_EDGE('',*,*,#21628,.T.);
#28622=ORIENTED_EDGE('',*,*,#21629,.T.);
#28623=ORIENTED_EDGE('',*,*,#21630,.T.);
#28624=ORIENTED_EDGE('',*,*,#21631,.T.);
#28625=ORIENTED_EDGE('',*,*,#21632,.T.);
#28626=ORIENTED_EDGE('',*,*,#21633,.T.);
#28627=ORIENTED_EDGE('',*,*,#21634,.T.);
#28628=ORIENTED_EDGE('',*,*,#21635,.T.);
#28629=ORIENTED_EDGE('',*,*,#21636,.T.);
#28630=ORIENTED_EDGE('',*,*,#21637,.T.);
#28631=ORIENTED_EDGE('',*,*,#21638,.T.);
#28632=ORIENTED_EDGE('',*,*,#21639,.T.);
#28633=ORIENTED_EDGE('',*,*,#21640,.T.);
#28634=ORIENTED_EDGE('',*,*,#21641,.T.);
#28635=ORIENTED_EDGE('',*,*,#21642,.T.);
#28636=ORIENTED_EDGE('',*,*,#21643,.T.);
#28637=ORIENTED_EDGE('',*,*,#21644,.T.);
#28638=ORIENTED_EDGE('',*,*,#21645,.T.);
#28639=ORIENTED_EDGE('',*,*,#21646,.T.);
#28640=ORIENTED_EDGE('',*,*,#21647,.T.);
#28641=ORIENTED_EDGE('',*,*,#21648,.T.);
#28642=ORIENTED_EDGE('',*,*,#21649,.T.);
#28643=ORIENTED_EDGE('',*,*,#21650,.T.);
#28644=ORIENTED_EDGE('',*,*,#21651,.T.);
#28645=ORIENTED_EDGE('',*,*,#21652,.T.);
#28646=ORIENTED_EDGE('',*,*,#21653,.T.);
#28647=ORIENTED_EDGE('',*,*,#21654,.T.);
#28648=ORIENTED_EDGE('',*,*,#21655,.T.);
#28649=ORIENTED_EDGE('',*,*,#21656,.T.);
#28650=ORIENTED_EDGE('',*,*,#21657,.T.);
#28651=ORIENTED_EDGE('',*,*,#21658,.T.);
#28652=ORIENTED_EDGE('',*,*,#21659,.T.);
#28653=ORIENTED_EDGE('',*,*,#21660,.T.);
#28654=ORIENTED_EDGE('',*,*,#21661,.T.);
#28655=ORIENTED_EDGE('',*,*,#21662,.T.);
#28656=ORIENTED_EDGE('',*,*,#21663,.T.);
#28657=ORIENTED_EDGE('',*,*,#21664,.T.);
#28658=ORIENTED_EDGE('',*,*,#21665,.T.);
#28659=ORIENTED_EDGE('',*,*,#21666,.T.);
#28660=ORIENTED_EDGE('',*,*,#21667,.T.);
#28661=ORIENTED_EDGE('',*,*,#21668,.T.);
#28662=ORIENTED_EDGE('',*,*,#21669,.T.);
#28663=ORIENTED_EDGE('',*,*,#21670,.T.);
#28664=ORIENTED_EDGE('',*,*,#21671,.T.);
#28665=ORIENTED_EDGE('',*,*,#21672,.T.);
#28666=ORIENTED_EDGE('',*,*,#21673,.T.);
#28667=ORIENTED_EDGE('',*,*,#21674,.T.);
#28668=ORIENTED_EDGE('',*,*,#21675,.T.);
#28669=ORIENTED_EDGE('',*,*,#21676,.T.);
#28670=ORIENTED_EDGE('',*,*,#21677,.T.);
#28671=ORIENTED_EDGE('',*,*,#21678,.T.);
#28672=ORIENTED_EDGE('',*,*,#21679,.T.);
#28673=ORIENTED_EDGE('',*,*,#21680,.T.);
#28674=ORIENTED_EDGE('',*,*,#21681,.T.);
#28675=ORIENTED_EDGE('',*,*,#21682,.T.);
#28676=ORIENTED_EDGE('',*,*,#21683,.T.);
#28677=ORIENTED_EDGE('',*,*,#21684,.T.);
#28678=ORIENTED_EDGE('',*,*,#21685,.T.);
#28679=ORIENTED_EDGE('',*,*,#21686,.T.);
#28680=ORIENTED_EDGE('',*,*,#21687,.T.);
#28681=ORIENTED_EDGE('',*,*,#21688,.T.);
#28682=ORIENTED_EDGE('',*,*,#21689,.T.);
#28683=ORIENTED_EDGE('',*,*,#21690,.T.);
#28684=ORIENTED_EDGE('',*,*,#21691,.T.);
#28685=ORIENTED_EDGE('',*,*,#21692,.T.);
#28686=ORIENTED_EDGE('',*,*,#21693,.T.);
#28687=ORIENTED_EDGE('',*,*,#21694,.T.);
#28688=ORIENTED_EDGE('',*,*,#21695,.T.);
#28689=ORIENTED_EDGE('',*,*,#21696,.T.);
#28690=ORIENTED_EDGE('',*,*,#21697,.T.);
#28691=ORIENTED_EDGE('',*,*,#21698,.T.);
#28692=ORIENTED_EDGE('',*,*,#21699,.T.);
#28693=ORIENTED_EDGE('',*,*,#21700,.T.);
#28694=ORIENTED_EDGE('',*,*,#21701,.T.);
#28695=ORIENTED_EDGE('',*,*,#21702,.T.);
#28696=ORIENTED_EDGE('',*,*,#21703,.T.);
#28697=ORIENTED_EDGE('',*,*,#21704,.T.);
#28698=ORIENTED_EDGE('',*,*,#21705,.T.);
#28699=ORIENTED_EDGE('',*,*,#21706,.T.);
#28700=ORIENTED_EDGE('',*,*,#21707,.T.);
#28701=ORIENTED_EDGE('',*,*,#21708,.T.);
#28702=ORIENTED_EDGE('',*,*,#21709,.T.);
#28703=ORIENTED_EDGE('',*,*,#21710,.T.);
#28704=ORIENTED_EDGE('',*,*,#21711,.T.);
#28705=ORIENTED_EDGE('',*,*,#21712,.T.);
#28706=ORIENTED_EDGE('',*,*,#21713,.T.);
#28707=ORIENTED_EDGE('',*,*,#21714,.T.);
#28708=ORIENTED_EDGE('',*,*,#21715,.T.);
#28709=ORIENTED_EDGE('',*,*,#21716,.T.);
#28710=ORIENTED_EDGE('',*,*,#21717,.T.);
#28711=ORIENTED_EDGE('',*,*,#21718,.T.);
#28712=ORIENTED_EDGE('',*,*,#21719,.T.);
#28713=ORIENTED_EDGE('',*,*,#21720,.T.);
#28714=ORIENTED_EDGE('',*,*,#21721,.T.);
#28715=ORIENTED_EDGE('',*,*,#21722,.T.);
#28716=ORIENTED_EDGE('',*,*,#21723,.T.);
#28717=ORIENTED_EDGE('',*,*,#21724,.T.);
#28718=ORIENTED_EDGE('',*,*,#21725,.T.);
#28719=ORIENTED_EDGE('',*,*,#21726,.T.);
#28720=ORIENTED_EDGE('',*,*,#21727,.T.);
#28721=ORIENTED_EDGE('',*,*,#21728,.T.);
#28722=ORIENTED_EDGE('',*,*,#21729,.T.);
#28723=ORIENTED_EDGE('',*,*,#21730,.T.);
#28724=ORIENTED_EDGE('',*,*,#21731,.T.);
#28725=ORIENTED_EDGE('',*,*,#21732,.T.);
#28726=ORIENTED_EDGE('',*,*,#21733,.T.);
#28727=ORIENTED_EDGE('',*,*,#21734,.T.);
#28728=ORIENTED_EDGE('',*,*,#21735,.T.);
#28729=ORIENTED_EDGE('',*,*,#21736,.T.);
#28730=ORIENTED_EDGE('',*,*,#21737,.T.);
#28731=ORIENTED_EDGE('',*,*,#21738,.T.);
#28732=ORIENTED_EDGE('',*,*,#21739,.T.);
#28733=ORIENTED_EDGE('',*,*,#21740,.T.);
#28734=ORIENTED_EDGE('',*,*,#21741,.T.);
#28735=ORIENTED_EDGE('',*,*,#21742,.T.);
#28736=ORIENTED_EDGE('',*,*,#21743,.T.);
#28737=ORIENTED_EDGE('',*,*,#21744,.T.);
#28738=ORIENTED_EDGE('',*,*,#21745,.T.);
#28739=ORIENTED_EDGE('',*,*,#21746,.T.);
#28740=ORIENTED_EDGE('',*,*,#21747,.T.);
#28741=ORIENTED_EDGE('',*,*,#21748,.T.);
#28742=ORIENTED_EDGE('',*,*,#21749,.T.);
#28743=ORIENTED_EDGE('',*,*,#21750,.T.);
#28744=ORIENTED_EDGE('',*,*,#21751,.T.);
#28745=ORIENTED_EDGE('',*,*,#21752,.T.);
#28746=ORIENTED_EDGE('',*,*,#21753,.T.);
#28747=ORIENTED_EDGE('',*,*,#21754,.T.);
#28748=ORIENTED_EDGE('',*,*,#21755,.T.);
#28749=ORIENTED_EDGE('',*,*,#21756,.T.);
#28750=ORIENTED_EDGE('',*,*,#21757,.T.);
#28751=ORIENTED_EDGE('',*,*,#21758,.T.);
#28752=ORIENTED_EDGE('',*,*,#21759,.T.);
#28753=ORIENTED_EDGE('',*,*,#21760,.T.);
#28754=ORIENTED_EDGE('',*,*,#21761,.T.);
#28755=ORIENTED_EDGE('',*,*,#21762,.T.);
#28756=ORIENTED_EDGE('',*,*,#21763,.T.);
#28757=ORIENTED_EDGE('',*,*,#21764,.T.);
#28758=ORIENTED_EDGE('',*,*,#21765,.T.);
#28759=ORIENTED_EDGE('',*,*,#21766,.T.);
#28760=ORIENTED_EDGE('',*,*,#21767,.T.);
#28761=ORIENTED_EDGE('',*,*,#21768,.T.);
#28762=ORIENTED_EDGE('',*,*,#21769,.T.);
#28763=ORIENTED_EDGE('',*,*,#21770,.T.);
#28764=ORIENTED_EDGE('',*,*,#21771,.T.);
#28765=ORIENTED_EDGE('',*,*,#21772,.T.);
#28766=ORIENTED_EDGE('',*,*,#21773,.T.);
#28767=ORIENTED_EDGE('',*,*,#21774,.T.);
#28768=ORIENTED_EDGE('',*,*,#21775,.T.);
#28769=ORIENTED_EDGE('',*,*,#21776,.T.);
#28770=ORIENTED_EDGE('',*,*,#21777,.T.);
#28771=ORIENTED_EDGE('',*,*,#21778,.T.);
#28772=ORIENTED_EDGE('',*,*,#21779,.T.);
#28773=ORIENTED_EDGE('',*,*,#21780,.T.);
#28774=ORIENTED_EDGE('',*,*,#21781,.T.);
#28775=ORIENTED_EDGE('',*,*,#21782,.T.);
#28776=ORIENTED_EDGE('',*,*,#21783,.T.);
#28777=ORIENTED_EDGE('',*,*,#21784,.T.);
#28778=ORIENTED_EDGE('',*,*,#21471,.F.);
#28779=ORIENTED_EDGE('',*,*,#21785,.F.);
#28780=ORIENTED_EDGE('',*,*,#21786,.T.);
#28781=ORIENTED_EDGE('',*,*,#21787,.T.);
#28782=ORIENTED_EDGE('',*,*,#21788,.F.);
#28783=ORIENTED_EDGE('',*,*,#21789,.T.);
#28784=ORIENTED_EDGE('',*,*,#21783,.F.);
#28785=ORIENTED_EDGE('',*,*,#21790,.T.);
#28786=ORIENTED_EDGE('',*,*,#21791,.T.);
#28787=ORIENTED_EDGE('',*,*,#21792,.T.);
#28788=ORIENTED_EDGE('',*,*,#21793,.T.);
#28789=ORIENTED_EDGE('',*,*,#21794,.F.);
#28790=ORIENTED_EDGE('',*,*,#21795,.T.);
#28791=ORIENTED_EDGE('',*,*,#21796,.T.);
#28792=ORIENTED_EDGE('',*,*,#21797,.F.);
#28793=ORIENTED_EDGE('',*,*,#21798,.T.);
#28794=ORIENTED_EDGE('',*,*,#21799,.T.);
#28795=ORIENTED_EDGE('',*,*,#21800,.T.);
#28796=ORIENTED_EDGE('',*,*,#21801,.T.);
#28797=ORIENTED_EDGE('',*,*,#21475,.F.);
#28798=ORIENTED_EDGE('',*,*,#21802,.F.);
#28799=ORIENTED_EDGE('',*,*,#21803,.T.);
#28800=ORIENTED_EDGE('',*,*,#21791,.F.);
#28801=ORIENTED_EDGE('',*,*,#21804,.T.);
#28802=ORIENTED_EDGE('',*,*,#21800,.F.);
#28803=ORIENTED_EDGE('',*,*,#21805,.T.);
#28804=ORIENTED_EDGE('',*,*,#21806,.F.);
#28805=ORIENTED_EDGE('',*,*,#21807,.T.);
#28806=ORIENTED_EDGE('',*,*,#21808,.T.);
#28807=ORIENTED_EDGE('',*,*,#21809,.T.);
#28808=ORIENTED_EDGE('',*,*,#21788,.T.);
#28809=ORIENTED_EDGE('',*,*,#21810,.T.);
#28810=ORIENTED_EDGE('',*,*,#21794,.T.);
#28811=ORIENTED_EDGE('',*,*,#21811,.T.);
#28812=ORIENTED_EDGE('',*,*,#21808,.F.);
#28813=ORIENTED_EDGE('',*,*,#21812,.T.);
#28814=ORIENTED_EDGE('',*,*,#21474,.F.);
#28815=ORIENTED_EDGE('',*,*,#21813,.T.);
#28816=ORIENTED_EDGE('',*,*,#21797,.T.);
#28817=ORIENTED_EDGE('',*,*,#21814,.T.);
#28818=ORIENTED_EDGE('',*,*,#21815,.T.);
#28819=ORIENTED_EDGE('',*,*,#21802,.T.);
#28820=ORIENTED_EDGE('',*,*,#21816,.T.);
#28821=ORIENTED_EDGE('',*,*,#21806,.T.);
#28822=ORIENTED_EDGE('',*,*,#21817,.T.);
#28823=ORIENTED_EDGE('',*,*,#21818,.T.);
#28824=ORIENTED_EDGE('',*,*,#21819,.T.);
#28825=ORIENTED_EDGE('',*,*,#21820,.T.);
#28826=ORIENTED_EDGE('',*,*,#21821,.T.);
#28827=ORIENTED_EDGE('',*,*,#21822,.T.);
#28828=ORIENTED_EDGE('',*,*,#21823,.F.);
#28829=ORIENTED_EDGE('',*,*,#21824,.T.);
#28830=ORIENTED_EDGE('',*,*,#21825,.T.);
#28831=ORIENTED_EDGE('',*,*,#21826,.F.);
#28832=ORIENTED_EDGE('',*,*,#21827,.T.);
#28833=ORIENTED_EDGE('',*,*,#21828,.T.);
#28834=ORIENTED_EDGE('',*,*,#21829,.T.);
#28835=ORIENTED_EDGE('',*,*,#21830,.T.);
#28836=ORIENTED_EDGE('',*,*,#21831,.T.);
#28837=ORIENTED_EDGE('',*,*,#21823,.T.);
#28838=ORIENTED_EDGE('',*,*,#21832,.T.);
#28839=ORIENTED_EDGE('',*,*,#21814,.F.);
#28840=ORIENTED_EDGE('',*,*,#21833,.T.);
#28841=ORIENTED_EDGE('',*,*,#21818,.F.);
#28842=ORIENTED_EDGE('',*,*,#21834,.T.);
#28843=ORIENTED_EDGE('',*,*,#21826,.T.);
#28844=ORIENTED_EDGE('',*,*,#21835,.T.);
#28845=ORIENTED_EDGE('',*,*,#21836,.F.);
#28846=ORIENTED_EDGE('',*,*,#21837,.T.);
#28847=ORIENTED_EDGE('',*,*,#21820,.F.);
#28848=ORIENTED_EDGE('',*,*,#21838,.T.);
#28849=ORIENTED_EDGE('',*,*,#21829,.F.);
#28850=ORIENTED_EDGE('',*,*,#21839,.T.);
#28851=ORIENTED_EDGE('',*,*,#21840,.F.);
#28852=ORIENTED_EDGE('',*,*,#21841,.T.);
#28853=ORIENTED_EDGE('',*,*,#21842,.T.);
#28854=ORIENTED_EDGE('',*,*,#21843,.T.);
#28855=ORIENTED_EDGE('',*,*,#21836,.T.);
#28856=ORIENTED_EDGE('',*,*,#21844,.T.);
#28857=ORIENTED_EDGE('',*,*,#21840,.T.);
#28858=ORIENTED_EDGE('',*,*,#21845,.T.);
#28859=ORIENTED_EDGE('',*,*,#21846,.T.);
#28860=ORIENTED_EDGE('',*,*,#21847,.T.);
#28861=ORIENTED_EDGE('',*,*,#21848,.T.);
#28862=ORIENTED_EDGE('',*,*,#21849,.T.);
#28863=ORIENTED_EDGE('',*,*,#21850,.T.);
#28864=ORIENTED_EDGE('',*,*,#21851,.F.);
#28865=ORIENTED_EDGE('',*,*,#21852,.T.);
#28866=ORIENTED_EDGE('',*,*,#21853,.T.);
#28867=ORIENTED_EDGE('',*,*,#21854,.F.);
#28868=ORIENTED_EDGE('',*,*,#21855,.T.);
#28869=ORIENTED_EDGE('',*,*,#21856,.T.);
#28870=ORIENTED_EDGE('',*,*,#21857,.T.);
#28871=ORIENTED_EDGE('',*,*,#21858,.T.);
#28872=ORIENTED_EDGE('',*,*,#21859,.T.);
#28873=ORIENTED_EDGE('',*,*,#21851,.T.);
#28874=ORIENTED_EDGE('',*,*,#21860,.T.);
#28875=ORIENTED_EDGE('',*,*,#21842,.F.);
#28876=ORIENTED_EDGE('',*,*,#21861,.T.);
#28877=ORIENTED_EDGE('',*,*,#21846,.F.);
#28878=ORIENTED_EDGE('',*,*,#21862,.T.);
#28879=ORIENTED_EDGE('',*,*,#21854,.T.);
#28880=ORIENTED_EDGE('',*,*,#21863,.T.);
#28881=ORIENTED_EDGE('',*,*,#21864,.F.);
#28882=ORIENTED_EDGE('',*,*,#21865,.T.);
#28883=ORIENTED_EDGE('',*,*,#21848,.F.);
#28884=ORIENTED_EDGE('',*,*,#21866,.T.);
#28885=ORIENTED_EDGE('',*,*,#21857,.F.);
#28886=ORIENTED_EDGE('',*,*,#21867,.T.);
#28887=ORIENTED_EDGE('',*,*,#21868,.F.);
#28888=ORIENTED_EDGE('',*,*,#21869,.T.);
#28889=ORIENTED_EDGE('',*,*,#21870,.T.);
#28890=ORIENTED_EDGE('',*,*,#21871,.T.);
#28891=ORIENTED_EDGE('',*,*,#21864,.T.);
#28892=ORIENTED_EDGE('',*,*,#21872,.T.);
#28893=ORIENTED_EDGE('',*,*,#21868,.T.);
#28894=ORIENTED_EDGE('',*,*,#21873,.T.);
#28895=ORIENTED_EDGE('',*,*,#21874,.T.);
#28896=ORIENTED_EDGE('',*,*,#21875,.T.);
#28897=ORIENTED_EDGE('',*,*,#21876,.T.);
#28898=ORIENTED_EDGE('',*,*,#21877,.T.);
#28899=ORIENTED_EDGE('',*,*,#21878,.T.);
#28900=ORIENTED_EDGE('',*,*,#21879,.F.);
#28901=ORIENTED_EDGE('',*,*,#21880,.T.);
#28902=ORIENTED_EDGE('',*,*,#21881,.T.);
#28903=ORIENTED_EDGE('',*,*,#21882,.F.);
#28904=ORIENTED_EDGE('',*,*,#21883,.T.);
#28905=ORIENTED_EDGE('',*,*,#21884,.T.);
#28906=ORIENTED_EDGE('',*,*,#21885,.T.);
#28907=ORIENTED_EDGE('',*,*,#21886,.T.);
#28908=ORIENTED_EDGE('',*,*,#21887,.T.);
#28909=ORIENTED_EDGE('',*,*,#21879,.T.);
#28910=ORIENTED_EDGE('',*,*,#21888,.T.);
#28911=ORIENTED_EDGE('',*,*,#21870,.F.);
#28912=ORIENTED_EDGE('',*,*,#21889,.T.);
#28913=ORIENTED_EDGE('',*,*,#21874,.F.);
#28914=ORIENTED_EDGE('',*,*,#21890,.T.);
#28915=ORIENTED_EDGE('',*,*,#21882,.T.);
#28916=ORIENTED_EDGE('',*,*,#21891,.T.);
#28917=ORIENTED_EDGE('',*,*,#21892,.F.);
#28918=ORIENTED_EDGE('',*,*,#21893,.T.);
#28919=ORIENTED_EDGE('',*,*,#21876,.F.);
#28920=ORIENTED_EDGE('',*,*,#21894,.T.);
#28921=ORIENTED_EDGE('',*,*,#21885,.F.);
#28922=ORIENTED_EDGE('',*,*,#21895,.T.);
#28923=ORIENTED_EDGE('',*,*,#21896,.F.);
#28924=ORIENTED_EDGE('',*,*,#21897,.T.);
#28925=ORIENTED_EDGE('',*,*,#21898,.T.);
#28926=ORIENTED_EDGE('',*,*,#21899,.T.);
#28927=ORIENTED_EDGE('',*,*,#21892,.T.);
#28928=ORIENTED_EDGE('',*,*,#21900,.T.);
#28929=ORIENTED_EDGE('',*,*,#21896,.T.);
#28930=ORIENTED_EDGE('',*,*,#21901,.T.);
#28931=ORIENTED_EDGE('',*,*,#21902,.T.);
#28932=ORIENTED_EDGE('',*,*,#21903,.T.);
#28933=ORIENTED_EDGE('',*,*,#21904,.T.);
#28934=ORIENTED_EDGE('',*,*,#21905,.T.);
#28935=ORIENTED_EDGE('',*,*,#21906,.T.);
#28936=ORIENTED_EDGE('',*,*,#21907,.F.);
#28937=ORIENTED_EDGE('',*,*,#21908,.T.);
#28938=ORIENTED_EDGE('',*,*,#21909,.T.);
#28939=ORIENTED_EDGE('',*,*,#21910,.F.);
#28940=ORIENTED_EDGE('',*,*,#21911,.T.);
#28941=ORIENTED_EDGE('',*,*,#21912,.T.);
#28942=ORIENTED_EDGE('',*,*,#21913,.T.);
#28943=ORIENTED_EDGE('',*,*,#21914,.T.);
#28944=ORIENTED_EDGE('',*,*,#21915,.T.);
#28945=ORIENTED_EDGE('',*,*,#21907,.T.);
#28946=ORIENTED_EDGE('',*,*,#21916,.T.);
#28947=ORIENTED_EDGE('',*,*,#21898,.F.);
#28948=ORIENTED_EDGE('',*,*,#21917,.T.);
#28949=ORIENTED_EDGE('',*,*,#21902,.F.);
#28950=ORIENTED_EDGE('',*,*,#21918,.T.);
#28951=ORIENTED_EDGE('',*,*,#21910,.T.);
#28952=ORIENTED_EDGE('',*,*,#21919,.T.);
#28953=ORIENTED_EDGE('',*,*,#21920,.F.);
#28954=ORIENTED_EDGE('',*,*,#21921,.T.);
#28955=ORIENTED_EDGE('',*,*,#21904,.F.);
#28956=ORIENTED_EDGE('',*,*,#21922,.T.);
#28957=ORIENTED_EDGE('',*,*,#21913,.F.);
#28958=ORIENTED_EDGE('',*,*,#21923,.T.);
#28959=ORIENTED_EDGE('',*,*,#21924,.F.);
#28960=ORIENTED_EDGE('',*,*,#21925,.T.);
#28961=ORIENTED_EDGE('',*,*,#21926,.T.);
#28962=ORIENTED_EDGE('',*,*,#21927,.T.);
#28963=ORIENTED_EDGE('',*,*,#21920,.T.);
#28964=ORIENTED_EDGE('',*,*,#21928,.T.);
#28965=ORIENTED_EDGE('',*,*,#21924,.T.);
#28966=ORIENTED_EDGE('',*,*,#21929,.T.);
#28967=ORIENTED_EDGE('',*,*,#21930,.T.);
#28968=ORIENTED_EDGE('',*,*,#21931,.T.);
#28969=ORIENTED_EDGE('',*,*,#21932,.T.);
#28970=ORIENTED_EDGE('',*,*,#21933,.T.);
#28971=ORIENTED_EDGE('',*,*,#21934,.T.);
#28972=ORIENTED_EDGE('',*,*,#21935,.F.);
#28973=ORIENTED_EDGE('',*,*,#21936,.T.);
#28974=ORIENTED_EDGE('',*,*,#21937,.T.);
#28975=ORIENTED_EDGE('',*,*,#21938,.F.);
#28976=ORIENTED_EDGE('',*,*,#21939,.T.);
#28977=ORIENTED_EDGE('',*,*,#21940,.T.);
#28978=ORIENTED_EDGE('',*,*,#21941,.T.);
#28979=ORIENTED_EDGE('',*,*,#21942,.T.);
#28980=ORIENTED_EDGE('',*,*,#21943,.T.);
#28981=ORIENTED_EDGE('',*,*,#21935,.T.);
#28982=ORIENTED_EDGE('',*,*,#21944,.T.);
#28983=ORIENTED_EDGE('',*,*,#21926,.F.);
#28984=ORIENTED_EDGE('',*,*,#21945,.T.);
#28985=ORIENTED_EDGE('',*,*,#21930,.F.);
#28986=ORIENTED_EDGE('',*,*,#21946,.T.);
#28987=ORIENTED_EDGE('',*,*,#21938,.T.);
#28988=ORIENTED_EDGE('',*,*,#21947,.T.);
#28989=ORIENTED_EDGE('',*,*,#21628,.F.);
#28990=ORIENTED_EDGE('',*,*,#21948,.T.);
#28991=ORIENTED_EDGE('',*,*,#21932,.F.);
#28992=ORIENTED_EDGE('',*,*,#21949,.T.);
#28993=ORIENTED_EDGE('',*,*,#21941,.F.);
#28994=ORIENTED_EDGE('',*,*,#21950,.T.);
#28995=ORIENTED_EDGE('',*,*,#21951,.F.);
#28996=ORIENTED_EDGE('',*,*,#21952,.T.);
#28997=ORIENTED_EDGE('',*,*,#21951,.T.);
#28998=ORIENTED_EDGE('',*,*,#21953,.T.);
#28999=ORIENTED_EDGE('',*,*,#21954,.T.);
#29000=ORIENTED_EDGE('',*,*,#21955,.T.);
#29001=ORIENTED_EDGE('',*,*,#21625,.F.);
#29002=ORIENTED_EDGE('',*,*,#21956,.T.);
#29003=ORIENTED_EDGE('',*,*,#21957,.T.);
#29004=ORIENTED_EDGE('',*,*,#21958,.F.);
#29005=ORIENTED_EDGE('',*,*,#21959,.F.);
#29006=ORIENTED_EDGE('',*,*,#21960,.T.);
#29007=ORIENTED_EDGE('',*,*,#21961,.T.);
#29008=ORIENTED_EDGE('',*,*,#21962,.T.);
#29009=ORIENTED_EDGE('',*,*,#21963,.T.);
#29010=ORIENTED_EDGE('',*,*,#21964,.T.);
#29011=ORIENTED_EDGE('',*,*,#21958,.T.);
#29012=ORIENTED_EDGE('',*,*,#21965,.T.);
#29013=ORIENTED_EDGE('',*,*,#21626,.F.);
#29014=ORIENTED_EDGE('',*,*,#21954,.F.);
#29015=ORIENTED_EDGE('',*,*,#21966,.T.);
#29016=ORIENTED_EDGE('',*,*,#21959,.T.);
#29017=ORIENTED_EDGE('',*,*,#21967,.T.);
#29018=ORIENTED_EDGE('',*,*,#21962,.F.);
#29019=ORIENTED_EDGE('',*,*,#21968,.T.);
#29020=ORIENTED_EDGE('',*,*,#21622,.F.);
#29021=ORIENTED_EDGE('',*,*,#21969,.T.);
#29022=ORIENTED_EDGE('',*,*,#21970,.T.);
#29023=ORIENTED_EDGE('',*,*,#21971,.T.);
#29024=ORIENTED_EDGE('',*,*,#21467,.F.);
#29025=ORIENTED_EDGE('',*,*,#21972,.F.);
#29026=ORIENTED_EDGE('',*,*,#21973,.T.);
#29027=ORIENTED_EDGE('',*,*,#21974,.T.);
#29028=ORIENTED_EDGE('',*,*,#21975,.F.);
#29029=ORIENTED_EDGE('',*,*,#21976,.T.);
#29030=ORIENTED_EDGE('',*,*,#21970,.F.);
#29031=ORIENTED_EDGE('',*,*,#21977,.T.);
#29032=ORIENTED_EDGE('',*,*,#21978,.T.);
#29033=ORIENTED_EDGE('',*,*,#21979,.T.);
#29034=ORIENTED_EDGE('',*,*,#21975,.T.);
#29035=ORIENTED_EDGE('',*,*,#21980,.T.);
#29036=ORIENTED_EDGE('',*,*,#21981,.T.);
#29037=ORIENTED_EDGE('',*,*,#21982,.T.);
#29038=ORIENTED_EDGE('',*,*,#21983,.T.);
#29039=ORIENTED_EDGE('',*,*,#21984,.F.);
#29040=ORIENTED_EDGE('',*,*,#21985,.T.);
#29041=ORIENTED_EDGE('',*,*,#21986,.T.);
#29042=ORIENTED_EDGE('',*,*,#21984,.T.);
#29043=ORIENTED_EDGE('',*,*,#21987,.T.);
#29044=ORIENTED_EDGE('',*,*,#21978,.F.);
#29045=ORIENTED_EDGE('',*,*,#21988,.T.);
#29046=ORIENTED_EDGE('',*,*,#21470,.F.);
#29047=ORIENTED_EDGE('',*,*,#21989,.T.);
#29048=ORIENTED_EDGE('',*,*,#21785,.T.);
#29049=ORIENTED_EDGE('',*,*,#21990,.F.);
#29050=ORIENTED_EDGE('',*,*,#21991,.T.);
#29051=ORIENTED_EDGE('',*,*,#21981,.F.);
#29052=ORIENTED_EDGE('',*,*,#21992,.T.);
#29053=ORIENTED_EDGE('',*,*,#21993,.T.);
#29054=ORIENTED_EDGE('',*,*,#21994,.T.);
#29055=ORIENTED_EDGE('',*,*,#21995,.T.);
#29056=ORIENTED_EDGE('',*,*,#21996,.F.);
#29057=ORIENTED_EDGE('',*,*,#21997,.T.);
#29058=ORIENTED_EDGE('',*,*,#21998,.T.);
#29059=ORIENTED_EDGE('',*,*,#21999,.F.);
#29060=ORIENTED_EDGE('',*,*,#22000,.T.);
#29061=ORIENTED_EDGE('',*,*,#21993,.F.);
#29062=ORIENTED_EDGE('',*,*,#22001,.T.);
#29063=ORIENTED_EDGE('',*,*,#22002,.T.);
#29064=ORIENTED_EDGE('',*,*,#22003,.T.);
#29065=ORIENTED_EDGE('',*,*,#21990,.T.);
#29066=ORIENTED_EDGE('',*,*,#22004,.T.);
#29067=ORIENTED_EDGE('',*,*,#21996,.T.);
#29068=ORIENTED_EDGE('',*,*,#22005,.T.);
#29069=ORIENTED_EDGE('',*,*,#22002,.F.);
#29070=ORIENTED_EDGE('',*,*,#22006,.T.);
#29071=ORIENTED_EDGE('',*,*,#22007,.T.);
#29072=ORIENTED_EDGE('',*,*,#22008,.T.);
#29073=ORIENTED_EDGE('',*,*,#21999,.T.);
#29074=ORIENTED_EDGE('',*,*,#22009,.T.);
#29075=ORIENTED_EDGE('',*,*,#22010,.T.);
#29076=ORIENTED_EDGE('',*,*,#22011,.T.);
#29077=ORIENTED_EDGE('',*,*,#22012,.T.);
#29078=ORIENTED_EDGE('',*,*,#22013,.F.);
#29079=ORIENTED_EDGE('',*,*,#22014,.T.);
#29080=ORIENTED_EDGE('',*,*,#22015,.T.);
#29081=ORIENTED_EDGE('',*,*,#22013,.T.);
#29082=ORIENTED_EDGE('',*,*,#22016,.T.);
#29083=ORIENTED_EDGE('',*,*,#22007,.F.);
#29084=ORIENTED_EDGE('',*,*,#22017,.T.);
#29085=ORIENTED_EDGE('',*,*,#22018,.F.);
#29086=ORIENTED_EDGE('',*,*,#22019,.T.);
#29087=ORIENTED_EDGE('',*,*,#22010,.F.);
#29088=ORIENTED_EDGE('',*,*,#22020,.T.);
#29089=ORIENTED_EDGE('',*,*,#22021,.T.);
#29090=ORIENTED_EDGE('',*,*,#22022,.T.);
#29091=ORIENTED_EDGE('',*,*,#22018,.T.);
#29092=ORIENTED_EDGE('',*,*,#22023,.T.);
#29093=ORIENTED_EDGE('',*,*,#22024,.T.);
#29094=ORIENTED_EDGE('',*,*,#22025,.T.);
#29095=ORIENTED_EDGE('',*,*,#22026,.T.);
#29096=ORIENTED_EDGE('',*,*,#22027,.F.);
#29097=ORIENTED_EDGE('',*,*,#22028,.T.);
#29098=ORIENTED_EDGE('',*,*,#22029,.T.);
#29099=ORIENTED_EDGE('',*,*,#22027,.T.);
#29100=ORIENTED_EDGE('',*,*,#22030,.T.);
#29101=ORIENTED_EDGE('',*,*,#22021,.F.);
#29102=ORIENTED_EDGE('',*,*,#22031,.T.);
#29103=ORIENTED_EDGE('',*,*,#22032,.F.);
#29104=ORIENTED_EDGE('',*,*,#22033,.T.);
#29105=ORIENTED_EDGE('',*,*,#22024,.F.);
#29106=ORIENTED_EDGE('',*,*,#22034,.T.);
#29107=ORIENTED_EDGE('',*,*,#22035,.T.);
#29108=ORIENTED_EDGE('',*,*,#22036,.T.);
#29109=ORIENTED_EDGE('',*,*,#22032,.T.);
#29110=ORIENTED_EDGE('',*,*,#22037,.T.);
#29111=ORIENTED_EDGE('',*,*,#22038,.T.);
#29112=ORIENTED_EDGE('',*,*,#22039,.T.);
#29113=ORIENTED_EDGE('',*,*,#22040,.T.);
#29114=ORIENTED_EDGE('',*,*,#22041,.F.);
#29115=ORIENTED_EDGE('',*,*,#22042,.T.);
#29116=ORIENTED_EDGE('',*,*,#22043,.T.);
#29117=ORIENTED_EDGE('',*,*,#22041,.T.);
#29118=ORIENTED_EDGE('',*,*,#22044,.T.);
#29119=ORIENTED_EDGE('',*,*,#22035,.F.);
#29120=ORIENTED_EDGE('',*,*,#22045,.T.);
#29121=ORIENTED_EDGE('',*,*,#22046,.F.);
#29122=ORIENTED_EDGE('',*,*,#22047,.T.);
#29123=ORIENTED_EDGE('',*,*,#22038,.F.);
#29124=ORIENTED_EDGE('',*,*,#22048,.T.);
#29125=ORIENTED_EDGE('',*,*,#22049,.T.);
#29126=ORIENTED_EDGE('',*,*,#22050,.T.);
#29127=ORIENTED_EDGE('',*,*,#22046,.T.);
#29128=ORIENTED_EDGE('',*,*,#22051,.T.);
#29129=ORIENTED_EDGE('',*,*,#22052,.T.);
#29130=ORIENTED_EDGE('',*,*,#22053,.T.);
#29131=ORIENTED_EDGE('',*,*,#22054,.T.);
#29132=ORIENTED_EDGE('',*,*,#22055,.F.);
#29133=ORIENTED_EDGE('',*,*,#22056,.T.);
#29134=ORIENTED_EDGE('',*,*,#22057,.T.);
#29135=ORIENTED_EDGE('',*,*,#22055,.T.);
#29136=ORIENTED_EDGE('',*,*,#22058,.T.);
#29137=ORIENTED_EDGE('',*,*,#22049,.F.);
#29138=ORIENTED_EDGE('',*,*,#22059,.T.);
#29139=ORIENTED_EDGE('',*,*,#21634,.F.);
#29140=ORIENTED_EDGE('',*,*,#22060,.T.);
#29141=ORIENTED_EDGE('',*,*,#22052,.F.);
#29142=ORIENTED_EDGE('',*,*,#22061,.T.);
#29143=ORIENTED_EDGE('',*,*,#21631,.F.);
#29144=ORIENTED_EDGE('',*,*,#22062,.T.);
#29145=ORIENTED_EDGE('',*,*,#22063,.T.);
#29146=ORIENTED_EDGE('',*,*,#22064,.F.);
#29147=ORIENTED_EDGE('',*,*,#22064,.T.);
#29148=ORIENTED_EDGE('',*,*,#22065,.T.);
#29149=ORIENTED_EDGE('',*,*,#21632,.F.);
#29150=ORIENTED_EDGE('',*,*,#22066,.T.);
#29151=ORIENTED_EDGE('',*,*,#22067,.T.);
#29152=ORIENTED_EDGE('',*,*,#21463,.F.);
#29153=ORIENTED_EDGE('',*,*,#22068,.F.);
#29154=ORIENTED_EDGE('',*,*,#22069,.T.);
#29155=ORIENTED_EDGE('',*,*,#22070,.T.);
#29156=ORIENTED_EDGE('',*,*,#22071,.F.);
#29157=ORIENTED_EDGE('',*,*,#22072,.T.);
#29158=ORIENTED_EDGE('',*,*,#22066,.F.);
#29159=ORIENTED_EDGE('',*,*,#22073,.T.);
#29160=ORIENTED_EDGE('',*,*,#22074,.T.);
#29161=ORIENTED_EDGE('',*,*,#22075,.T.);
#29162=ORIENTED_EDGE('',*,*,#22071,.T.);
#29163=ORIENTED_EDGE('',*,*,#22076,.T.);
#29164=ORIENTED_EDGE('',*,*,#22077,.T.);
#29165=ORIENTED_EDGE('',*,*,#22078,.T.);
#29166=ORIENTED_EDGE('',*,*,#22079,.T.);
#29167=ORIENTED_EDGE('',*,*,#22080,.F.);
#29168=ORIENTED_EDGE('',*,*,#22081,.T.);
#29169=ORIENTED_EDGE('',*,*,#22082,.T.);
#29170=ORIENTED_EDGE('',*,*,#22080,.T.);
#29171=ORIENTED_EDGE('',*,*,#22083,.T.);
#29172=ORIENTED_EDGE('',*,*,#22074,.F.);
#29173=ORIENTED_EDGE('',*,*,#22084,.T.);
#29174=ORIENTED_EDGE('',*,*,#21466,.F.);
#29175=ORIENTED_EDGE('',*,*,#22085,.T.);
#29176=ORIENTED_EDGE('',*,*,#21972,.T.);
#29177=ORIENTED_EDGE('',*,*,#22086,.F.);
#29178=ORIENTED_EDGE('',*,*,#22087,.T.);
#29179=ORIENTED_EDGE('',*,*,#22077,.F.);
#29180=ORIENTED_EDGE('',*,*,#22088,.T.);
#29181=ORIENTED_EDGE('',*,*,#22089,.T.);
#29182=ORIENTED_EDGE('',*,*,#22090,.T.);
#29183=ORIENTED_EDGE('',*,*,#22086,.T.);
#29184=ORIENTED_EDGE('',*,*,#22091,.T.);
#29185=ORIENTED_EDGE('',*,*,#22092,.T.);
#29186=ORIENTED_EDGE('',*,*,#22093,.T.);
#29187=ORIENTED_EDGE('',*,*,#22094,.T.);
#29188=ORIENTED_EDGE('',*,*,#22095,.F.);
#29189=ORIENTED_EDGE('',*,*,#22096,.T.);
#29190=ORIENTED_EDGE('',*,*,#22097,.T.);
#29191=ORIENTED_EDGE('',*,*,#22095,.T.);
#29192=ORIENTED_EDGE('',*,*,#22098,.T.);
#29193=ORIENTED_EDGE('',*,*,#22089,.F.);
#29194=ORIENTED_EDGE('',*,*,#22099,.T.);
#29195=ORIENTED_EDGE('',*,*,#22100,.F.);
#29196=ORIENTED_EDGE('',*,*,#22101,.T.);
#29197=ORIENTED_EDGE('',*,*,#22092,.F.);
#29198=ORIENTED_EDGE('',*,*,#22102,.T.);
#29199=ORIENTED_EDGE('',*,*,#22103,.T.);
#29200=ORIENTED_EDGE('',*,*,#22104,.T.);
#29201=ORIENTED_EDGE('',*,*,#22105,.T.);
#29202=ORIENTED_EDGE('',*,*,#22106,.F.);
#29203=ORIENTED_EDGE('',*,*,#22107,.T.);
#29204=ORIENTED_EDGE('',*,*,#22108,.T.);
#29205=ORIENTED_EDGE('',*,*,#22109,.F.);
#29206=ORIENTED_EDGE('',*,*,#22110,.T.);
#29207=ORIENTED_EDGE('',*,*,#22103,.F.);
#29208=ORIENTED_EDGE('',*,*,#22111,.T.);
#29209=ORIENTED_EDGE('',*,*,#22112,.T.);
#29210=ORIENTED_EDGE('',*,*,#22113,.T.);
#29211=ORIENTED_EDGE('',*,*,#22100,.T.);
#29212=ORIENTED_EDGE('',*,*,#22114,.T.);
#29213=ORIENTED_EDGE('',*,*,#22106,.T.);
#29214=ORIENTED_EDGE('',*,*,#22115,.T.);
#29215=ORIENTED_EDGE('',*,*,#22112,.F.);
#29216=ORIENTED_EDGE('',*,*,#22116,.T.);
#29217=ORIENTED_EDGE('',*,*,#22117,.T.);
#29218=ORIENTED_EDGE('',*,*,#22118,.T.);
#29219=ORIENTED_EDGE('',*,*,#22109,.T.);
#29220=ORIENTED_EDGE('',*,*,#22119,.T.);
#29221=ORIENTED_EDGE('',*,*,#22120,.T.);
#29222=ORIENTED_EDGE('',*,*,#22121,.T.);
#29223=ORIENTED_EDGE('',*,*,#22122,.T.);
#29224=ORIENTED_EDGE('',*,*,#22123,.F.);
#29225=ORIENTED_EDGE('',*,*,#22124,.T.);
#29226=ORIENTED_EDGE('',*,*,#22125,.T.);
#29227=ORIENTED_EDGE('',*,*,#22123,.T.);
#29228=ORIENTED_EDGE('',*,*,#22126,.T.);
#29229=ORIENTED_EDGE('',*,*,#22117,.F.);
#29230=ORIENTED_EDGE('',*,*,#22127,.T.);
#29231=ORIENTED_EDGE('',*,*,#22128,.F.);
#29232=ORIENTED_EDGE('',*,*,#22129,.T.);
#29233=ORIENTED_EDGE('',*,*,#22120,.F.);
#29234=ORIENTED_EDGE('',*,*,#22130,.T.);
#29235=ORIENTED_EDGE('',*,*,#22131,.T.);
#29236=ORIENTED_EDGE('',*,*,#22132,.T.);
#29237=ORIENTED_EDGE('',*,*,#22128,.T.);
#29238=ORIENTED_EDGE('',*,*,#22133,.T.);
#29239=ORIENTED_EDGE('',*,*,#22134,.T.);
#29240=ORIENTED_EDGE('',*,*,#22135,.T.);
#29241=ORIENTED_EDGE('',*,*,#22136,.T.);
#29242=ORIENTED_EDGE('',*,*,#22137,.F.);
#29243=ORIENTED_EDGE('',*,*,#22138,.T.);
#29244=ORIENTED_EDGE('',*,*,#22139,.T.);
#29245=ORIENTED_EDGE('',*,*,#22137,.T.);
#29246=ORIENTED_EDGE('',*,*,#22140,.T.);
#29247=ORIENTED_EDGE('',*,*,#22131,.F.);
#29248=ORIENTED_EDGE('',*,*,#22141,.T.);
#29249=ORIENTED_EDGE('',*,*,#22142,.F.);
#29250=ORIENTED_EDGE('',*,*,#22143,.T.);
#29251=ORIENTED_EDGE('',*,*,#22134,.F.);
#29252=ORIENTED_EDGE('',*,*,#22144,.T.);
#29253=ORIENTED_EDGE('',*,*,#22145,.T.);
#29254=ORIENTED_EDGE('',*,*,#22146,.T.);
#29255=ORIENTED_EDGE('',*,*,#22142,.T.);
#29256=ORIENTED_EDGE('',*,*,#22147,.T.);
#29257=ORIENTED_EDGE('',*,*,#22148,.T.);
#29258=ORIENTED_EDGE('',*,*,#22149,.T.);
#29259=ORIENTED_EDGE('',*,*,#22150,.T.);
#29260=ORIENTED_EDGE('',*,*,#22151,.F.);
#29261=ORIENTED_EDGE('',*,*,#22152,.T.);
#29262=ORIENTED_EDGE('',*,*,#22153,.T.);
#29263=ORIENTED_EDGE('',*,*,#22151,.T.);
#29264=ORIENTED_EDGE('',*,*,#22154,.T.);
#29265=ORIENTED_EDGE('',*,*,#22145,.F.);
#29266=ORIENTED_EDGE('',*,*,#22155,.T.);
#29267=ORIENTED_EDGE('',*,*,#21640,.F.);
#29268=ORIENTED_EDGE('',*,*,#22156,.T.);
#29269=ORIENTED_EDGE('',*,*,#22148,.F.);
#29270=ORIENTED_EDGE('',*,*,#22157,.T.);
#29271=ORIENTED_EDGE('',*,*,#21637,.F.);
#29272=ORIENTED_EDGE('',*,*,#22158,.T.);
#29273=ORIENTED_EDGE('',*,*,#22159,.T.);
#29274=ORIENTED_EDGE('',*,*,#22160,.F.);
#29275=ORIENTED_EDGE('',*,*,#22160,.T.);
#29276=ORIENTED_EDGE('',*,*,#22161,.T.);
#29277=ORIENTED_EDGE('',*,*,#21638,.F.);
#29278=ORIENTED_EDGE('',*,*,#22162,.T.);
#29279=ORIENTED_EDGE('',*,*,#22163,.T.);
#29280=ORIENTED_EDGE('',*,*,#21459,.F.);
#29281=ORIENTED_EDGE('',*,*,#22164,.F.);
#29282=ORIENTED_EDGE('',*,*,#22165,.T.);
#29283=ORIENTED_EDGE('',*,*,#22166,.T.);
#29284=ORIENTED_EDGE('',*,*,#22167,.F.);
#29285=ORIENTED_EDGE('',*,*,#22168,.T.);
#29286=ORIENTED_EDGE('',*,*,#22162,.F.);
#29287=ORIENTED_EDGE('',*,*,#22169,.T.);
#29288=ORIENTED_EDGE('',*,*,#22170,.T.);
#29289=ORIENTED_EDGE('',*,*,#22171,.T.);
#29290=ORIENTED_EDGE('',*,*,#22167,.T.);
#29291=ORIENTED_EDGE('',*,*,#22172,.T.);
#29292=ORIENTED_EDGE('',*,*,#22173,.T.);
#29293=ORIENTED_EDGE('',*,*,#22174,.T.);
#29294=ORIENTED_EDGE('',*,*,#22175,.T.);
#29295=ORIENTED_EDGE('',*,*,#22176,.F.);
#29296=ORIENTED_EDGE('',*,*,#22177,.T.);
#29297=ORIENTED_EDGE('',*,*,#22178,.T.);
#29298=ORIENTED_EDGE('',*,*,#22176,.T.);
#29299=ORIENTED_EDGE('',*,*,#22179,.T.);
#29300=ORIENTED_EDGE('',*,*,#22170,.F.);
#29301=ORIENTED_EDGE('',*,*,#22180,.T.);
#29302=ORIENTED_EDGE('',*,*,#21462,.F.);
#29303=ORIENTED_EDGE('',*,*,#22181,.T.);
#29304=ORIENTED_EDGE('',*,*,#22068,.T.);
#29305=ORIENTED_EDGE('',*,*,#22182,.F.);
#29306=ORIENTED_EDGE('',*,*,#22183,.T.);
#29307=ORIENTED_EDGE('',*,*,#22173,.F.);
#29308=ORIENTED_EDGE('',*,*,#22184,.T.);
#29309=ORIENTED_EDGE('',*,*,#22185,.T.);
#29310=ORIENTED_EDGE('',*,*,#22186,.T.);
#29311=ORIENTED_EDGE('',*,*,#22182,.T.);
#29312=ORIENTED_EDGE('',*,*,#22187,.T.);
#29313=ORIENTED_EDGE('',*,*,#22188,.T.);
#29314=ORIENTED_EDGE('',*,*,#22189,.T.);
#29315=ORIENTED_EDGE('',*,*,#22190,.T.);
#29316=ORIENTED_EDGE('',*,*,#22191,.F.);
#29317=ORIENTED_EDGE('',*,*,#22192,.T.);
#29318=ORIENTED_EDGE('',*,*,#22193,.T.);
#29319=ORIENTED_EDGE('',*,*,#22191,.T.);
#29320=ORIENTED_EDGE('',*,*,#22194,.T.);
#29321=ORIENTED_EDGE('',*,*,#22185,.F.);
#29322=ORIENTED_EDGE('',*,*,#22195,.T.);
#29323=ORIENTED_EDGE('',*,*,#22196,.F.);
#29324=ORIENTED_EDGE('',*,*,#22197,.T.);
#29325=ORIENTED_EDGE('',*,*,#22188,.F.);
#29326=ORIENTED_EDGE('',*,*,#22198,.T.);
#29327=ORIENTED_EDGE('',*,*,#22199,.T.);
#29328=ORIENTED_EDGE('',*,*,#22200,.T.);
#29329=ORIENTED_EDGE('',*,*,#22196,.T.);
#29330=ORIENTED_EDGE('',*,*,#22201,.T.);
#29331=ORIENTED_EDGE('',*,*,#22202,.T.);
#29332=ORIENTED_EDGE('',*,*,#22203,.T.);
#29333=ORIENTED_EDGE('',*,*,#22204,.T.);
#29334=ORIENTED_EDGE('',*,*,#22205,.F.);
#29335=ORIENTED_EDGE('',*,*,#22206,.T.);
#29336=ORIENTED_EDGE('',*,*,#22207,.T.);
#29337=ORIENTED_EDGE('',*,*,#22205,.T.);
#29338=ORIENTED_EDGE('',*,*,#22208,.T.);
#29339=ORIENTED_EDGE('',*,*,#22199,.F.);
#29340=ORIENTED_EDGE('',*,*,#22209,.T.);
#29341=ORIENTED_EDGE('',*,*,#22210,.F.);
#29342=ORIENTED_EDGE('',*,*,#22211,.T.);
#29343=ORIENTED_EDGE('',*,*,#22202,.F.);
#29344=ORIENTED_EDGE('',*,*,#22212,.T.);
#29345=ORIENTED_EDGE('',*,*,#22213,.T.);
#29346=ORIENTED_EDGE('',*,*,#22214,.T.);
#29347=ORIENTED_EDGE('',*,*,#22215,.T.);
#29348=ORIENTED_EDGE('',*,*,#22216,.F.);
#29349=ORIENTED_EDGE('',*,*,#22217,.T.);
#29350=ORIENTED_EDGE('',*,*,#22218,.T.);
#29351=ORIENTED_EDGE('',*,*,#22219,.F.);
#29352=ORIENTED_EDGE('',*,*,#22220,.T.);
#29353=ORIENTED_EDGE('',*,*,#22213,.F.);
#29354=ORIENTED_EDGE('',*,*,#22221,.T.);
#29355=ORIENTED_EDGE('',*,*,#22222,.T.);
#29356=ORIENTED_EDGE('',*,*,#22223,.T.);
#29357=ORIENTED_EDGE('',*,*,#22210,.T.);
#29358=ORIENTED_EDGE('',*,*,#22224,.T.);
#29359=ORIENTED_EDGE('',*,*,#22216,.T.);
#29360=ORIENTED_EDGE('',*,*,#22225,.T.);
#29361=ORIENTED_EDGE('',*,*,#22222,.F.);
#29362=ORIENTED_EDGE('',*,*,#22226,.T.);
#29363=ORIENTED_EDGE('',*,*,#22227,.T.);
#29364=ORIENTED_EDGE('',*,*,#22228,.T.);
#29365=ORIENTED_EDGE('',*,*,#22219,.T.);
#29366=ORIENTED_EDGE('',*,*,#22229,.T.);
#29367=ORIENTED_EDGE('',*,*,#22230,.T.);
#29368=ORIENTED_EDGE('',*,*,#22231,.T.);
#29369=ORIENTED_EDGE('',*,*,#22232,.T.);
#29370=ORIENTED_EDGE('',*,*,#22233,.F.);
#29371=ORIENTED_EDGE('',*,*,#22234,.T.);
#29372=ORIENTED_EDGE('',*,*,#22235,.T.);
#29373=ORIENTED_EDGE('',*,*,#22233,.T.);
#29374=ORIENTED_EDGE('',*,*,#22236,.T.);
#29375=ORIENTED_EDGE('',*,*,#22227,.F.);
#29376=ORIENTED_EDGE('',*,*,#22237,.T.);
#29377=ORIENTED_EDGE('',*,*,#22238,.F.);
#29378=ORIENTED_EDGE('',*,*,#22239,.T.);
#29379=ORIENTED_EDGE('',*,*,#22230,.F.);
#29380=ORIENTED_EDGE('',*,*,#22240,.T.);
#29381=ORIENTED_EDGE('',*,*,#22241,.T.);
#29382=ORIENTED_EDGE('',*,*,#22242,.T.);
#29383=ORIENTED_EDGE('',*,*,#22238,.T.);
#29384=ORIENTED_EDGE('',*,*,#22243,.T.);
#29385=ORIENTED_EDGE('',*,*,#22244,.T.);
#29386=ORIENTED_EDGE('',*,*,#22245,.T.);
#29387=ORIENTED_EDGE('',*,*,#22246,.T.);
#29388=ORIENTED_EDGE('',*,*,#22247,.F.);
#29389=ORIENTED_EDGE('',*,*,#22248,.T.);
#29390=ORIENTED_EDGE('',*,*,#22249,.T.);
#29391=ORIENTED_EDGE('',*,*,#22247,.T.);
#29392=ORIENTED_EDGE('',*,*,#22250,.T.);
#29393=ORIENTED_EDGE('',*,*,#22241,.F.);
#29394=ORIENTED_EDGE('',*,*,#22251,.T.);
#29395=ORIENTED_EDGE('',*,*,#21646,.F.);
#29396=ORIENTED_EDGE('',*,*,#22252,.T.);
#29397=ORIENTED_EDGE('',*,*,#22244,.F.);
#29398=ORIENTED_EDGE('',*,*,#22253,.T.);
#29399=ORIENTED_EDGE('',*,*,#21643,.F.);
#29400=ORIENTED_EDGE('',*,*,#22254,.T.);
#29401=ORIENTED_EDGE('',*,*,#22255,.T.);
#29402=ORIENTED_EDGE('',*,*,#22256,.F.);
#29403=ORIENTED_EDGE('',*,*,#22256,.T.);
#29404=ORIENTED_EDGE('',*,*,#22257,.T.);
#29405=ORIENTED_EDGE('',*,*,#21644,.F.);
#29406=ORIENTED_EDGE('',*,*,#22258,.T.);
#29407=ORIENTED_EDGE('',*,*,#22259,.T.);
#29408=ORIENTED_EDGE('',*,*,#21455,.F.);
#29409=ORIENTED_EDGE('',*,*,#22260,.F.);
#29410=ORIENTED_EDGE('',*,*,#22261,.T.);
#29411=ORIENTED_EDGE('',*,*,#22262,.T.);
#29412=ORIENTED_EDGE('',*,*,#22263,.F.);
#29413=ORIENTED_EDGE('',*,*,#22264,.T.);
#29414=ORIENTED_EDGE('',*,*,#22258,.F.);
#29415=ORIENTED_EDGE('',*,*,#22265,.T.);
#29416=ORIENTED_EDGE('',*,*,#22266,.T.);
#29417=ORIENTED_EDGE('',*,*,#22267,.T.);
#29418=ORIENTED_EDGE('',*,*,#22263,.T.);
#29419=ORIENTED_EDGE('',*,*,#22268,.T.);
#29420=ORIENTED_EDGE('',*,*,#22269,.T.);
#29421=ORIENTED_EDGE('',*,*,#22270,.T.);
#29422=ORIENTED_EDGE('',*,*,#22271,.T.);
#29423=ORIENTED_EDGE('',*,*,#22272,.F.);
#29424=ORIENTED_EDGE('',*,*,#22273,.T.);
#29425=ORIENTED_EDGE('',*,*,#22274,.T.);
#29426=ORIENTED_EDGE('',*,*,#22272,.T.);
#29427=ORIENTED_EDGE('',*,*,#22275,.T.);
#29428=ORIENTED_EDGE('',*,*,#22266,.F.);
#29429=ORIENTED_EDGE('',*,*,#22276,.T.);
#29430=ORIENTED_EDGE('',*,*,#21458,.F.);
#29431=ORIENTED_EDGE('',*,*,#22277,.T.);
#29432=ORIENTED_EDGE('',*,*,#22164,.T.);
#29433=ORIENTED_EDGE('',*,*,#22278,.F.);
#29434=ORIENTED_EDGE('',*,*,#22279,.T.);
#29435=ORIENTED_EDGE('',*,*,#22269,.F.);
#29436=ORIENTED_EDGE('',*,*,#22280,.T.);
#29437=ORIENTED_EDGE('',*,*,#22281,.T.);
#29438=ORIENTED_EDGE('',*,*,#22282,.T.);
#29439=ORIENTED_EDGE('',*,*,#22278,.T.);
#29440=ORIENTED_EDGE('',*,*,#22283,.T.);
#29441=ORIENTED_EDGE('',*,*,#22284,.T.);
#29442=ORIENTED_EDGE('',*,*,#22285,.T.);
#29443=ORIENTED_EDGE('',*,*,#22286,.T.);
#29444=ORIENTED_EDGE('',*,*,#22287,.F.);
#29445=ORIENTED_EDGE('',*,*,#22288,.T.);
#29446=ORIENTED_EDGE('',*,*,#22289,.T.);
#29447=ORIENTED_EDGE('',*,*,#22287,.T.);
#29448=ORIENTED_EDGE('',*,*,#22290,.T.);
#29449=ORIENTED_EDGE('',*,*,#22281,.F.);
#29450=ORIENTED_EDGE('',*,*,#22291,.T.);
#29451=ORIENTED_EDGE('',*,*,#22292,.F.);
#29452=ORIENTED_EDGE('',*,*,#22293,.T.);
#29453=ORIENTED_EDGE('',*,*,#22284,.F.);
#29454=ORIENTED_EDGE('',*,*,#22294,.T.);
#29455=ORIENTED_EDGE('',*,*,#22295,.T.);
#29456=ORIENTED_EDGE('',*,*,#22296,.T.);
#29457=ORIENTED_EDGE('',*,*,#22292,.T.);
#29458=ORIENTED_EDGE('',*,*,#22297,.T.);
#29459=ORIENTED_EDGE('',*,*,#22298,.T.);
#29460=ORIENTED_EDGE('',*,*,#22299,.T.);
#29461=ORIENTED_EDGE('',*,*,#22300,.T.);
#29462=ORIENTED_EDGE('',*,*,#22301,.F.);
#29463=ORIENTED_EDGE('',*,*,#22302,.T.);
#29464=ORIENTED_EDGE('',*,*,#22303,.T.);
#29465=ORIENTED_EDGE('',*,*,#22301,.T.);
#29466=ORIENTED_EDGE('',*,*,#22304,.T.);
#29467=ORIENTED_EDGE('',*,*,#22295,.F.);
#29468=ORIENTED_EDGE('',*,*,#22305,.T.);
#29469=ORIENTED_EDGE('',*,*,#22306,.F.);
#29470=ORIENTED_EDGE('',*,*,#22307,.T.);
#29471=ORIENTED_EDGE('',*,*,#22298,.F.);
#29472=ORIENTED_EDGE('',*,*,#22308,.T.);
#29473=ORIENTED_EDGE('',*,*,#22309,.T.);
#29474=ORIENTED_EDGE('',*,*,#22310,.T.);
#29475=ORIENTED_EDGE('',*,*,#22306,.T.);
#29476=ORIENTED_EDGE('',*,*,#22311,.T.);
#29477=ORIENTED_EDGE('',*,*,#22312,.T.);
#29478=ORIENTED_EDGE('',*,*,#22313,.T.);
#29479=ORIENTED_EDGE('',*,*,#22314,.T.);
#29480=ORIENTED_EDGE('',*,*,#22315,.F.);
#29481=ORIENTED_EDGE('',*,*,#22316,.T.);
#29482=ORIENTED_EDGE('',*,*,#22317,.T.);
#29483=ORIENTED_EDGE('',*,*,#22315,.T.);
#29484=ORIENTED_EDGE('',*,*,#22318,.T.);
#29485=ORIENTED_EDGE('',*,*,#22309,.F.);
#29486=ORIENTED_EDGE('',*,*,#22319,.T.);
#29487=ORIENTED_EDGE('',*,*,#22320,.F.);
#29488=ORIENTED_EDGE('',*,*,#22321,.T.);
#29489=ORIENTED_EDGE('',*,*,#22312,.F.);
#29490=ORIENTED_EDGE('',*,*,#22322,.T.);
#29491=ORIENTED_EDGE('',*,*,#22323,.T.);
#29492=ORIENTED_EDGE('',*,*,#22324,.T.);
#29493=ORIENTED_EDGE('',*,*,#22325,.T.);
#29494=ORIENTED_EDGE('',*,*,#22326,.F.);
#29495=ORIENTED_EDGE('',*,*,#22327,.T.);
#29496=ORIENTED_EDGE('',*,*,#22328,.T.);
#29497=ORIENTED_EDGE('',*,*,#22329,.F.);
#29498=ORIENTED_EDGE('',*,*,#22330,.T.);
#29499=ORIENTED_EDGE('',*,*,#22323,.F.);
#29500=ORIENTED_EDGE('',*,*,#22331,.T.);
#29501=ORIENTED_EDGE('',*,*,#22332,.T.);
#29502=ORIENTED_EDGE('',*,*,#22333,.T.);
#29503=ORIENTED_EDGE('',*,*,#22320,.T.);
#29504=ORIENTED_EDGE('',*,*,#22334,.T.);
#29505=ORIENTED_EDGE('',*,*,#22326,.T.);
#29506=ORIENTED_EDGE('',*,*,#22335,.T.);
#29507=ORIENTED_EDGE('',*,*,#22332,.F.);
#29508=ORIENTED_EDGE('',*,*,#22336,.T.);
#29509=ORIENTED_EDGE('',*,*,#22337,.T.);
#29510=ORIENTED_EDGE('',*,*,#22338,.T.);
#29511=ORIENTED_EDGE('',*,*,#22329,.T.);
#29512=ORIENTED_EDGE('',*,*,#22339,.T.);
#29513=ORIENTED_EDGE('',*,*,#22340,.T.);
#29514=ORIENTED_EDGE('',*,*,#22341,.T.);
#29515=ORIENTED_EDGE('',*,*,#22342,.T.);
#29516=ORIENTED_EDGE('',*,*,#22343,.F.);
#29517=ORIENTED_EDGE('',*,*,#22344,.T.);
#29518=ORIENTED_EDGE('',*,*,#22345,.T.);
#29519=ORIENTED_EDGE('',*,*,#22343,.T.);
#29520=ORIENTED_EDGE('',*,*,#22346,.T.);
#29521=ORIENTED_EDGE('',*,*,#22337,.F.);
#29522=ORIENTED_EDGE('',*,*,#22347,.T.);
#29523=ORIENTED_EDGE('',*,*,#21652,.F.);
#29524=ORIENTED_EDGE('',*,*,#22348,.T.);
#29525=ORIENTED_EDGE('',*,*,#22340,.F.);
#29526=ORIENTED_EDGE('',*,*,#22349,.T.);
#29527=ORIENTED_EDGE('',*,*,#21649,.F.);
#29528=ORIENTED_EDGE('',*,*,#22350,.T.);
#29529=ORIENTED_EDGE('',*,*,#22351,.T.);
#29530=ORIENTED_EDGE('',*,*,#22352,.F.);
#29531=ORIENTED_EDGE('',*,*,#22352,.T.);
#29532=ORIENTED_EDGE('',*,*,#22353,.T.);
#29533=ORIENTED_EDGE('',*,*,#21650,.F.);
#29534=ORIENTED_EDGE('',*,*,#22354,.T.);
#29535=ORIENTED_EDGE('',*,*,#22355,.T.);
#29536=ORIENTED_EDGE('',*,*,#21451,.F.);
#29537=ORIENTED_EDGE('',*,*,#22356,.F.);
#29538=ORIENTED_EDGE('',*,*,#22357,.T.);
#29539=ORIENTED_EDGE('',*,*,#22358,.T.);
#29540=ORIENTED_EDGE('',*,*,#22359,.F.);
#29541=ORIENTED_EDGE('',*,*,#22360,.T.);
#29542=ORIENTED_EDGE('',*,*,#22354,.F.);
#29543=ORIENTED_EDGE('',*,*,#22361,.T.);
#29544=ORIENTED_EDGE('',*,*,#22362,.T.);
#29545=ORIENTED_EDGE('',*,*,#22363,.T.);
#29546=ORIENTED_EDGE('',*,*,#22359,.T.);
#29547=ORIENTED_EDGE('',*,*,#22364,.T.);
#29548=ORIENTED_EDGE('',*,*,#22365,.T.);
#29549=ORIENTED_EDGE('',*,*,#22366,.T.);
#29550=ORIENTED_EDGE('',*,*,#22367,.T.);
#29551=ORIENTED_EDGE('',*,*,#22368,.F.);
#29552=ORIENTED_EDGE('',*,*,#22369,.T.);
#29553=ORIENTED_EDGE('',*,*,#22370,.T.);
#29554=ORIENTED_EDGE('',*,*,#22368,.T.);
#29555=ORIENTED_EDGE('',*,*,#22371,.T.);
#29556=ORIENTED_EDGE('',*,*,#22362,.F.);
#29557=ORIENTED_EDGE('',*,*,#22372,.T.);
#29558=ORIENTED_EDGE('',*,*,#21454,.F.);
#29559=ORIENTED_EDGE('',*,*,#22373,.T.);
#29560=ORIENTED_EDGE('',*,*,#22260,.T.);
#29561=ORIENTED_EDGE('',*,*,#22374,.F.);
#29562=ORIENTED_EDGE('',*,*,#22375,.T.);
#29563=ORIENTED_EDGE('',*,*,#22365,.F.);
#29564=ORIENTED_EDGE('',*,*,#22376,.T.);
#29565=ORIENTED_EDGE('',*,*,#22377,.T.);
#29566=ORIENTED_EDGE('',*,*,#22378,.T.);
#29567=ORIENTED_EDGE('',*,*,#22374,.T.);
#29568=ORIENTED_EDGE('',*,*,#22379,.T.);
#29569=ORIENTED_EDGE('',*,*,#22380,.T.);
#29570=ORIENTED_EDGE('',*,*,#22381,.T.);
#29571=ORIENTED_EDGE('',*,*,#22382,.T.);
#29572=ORIENTED_EDGE('',*,*,#22383,.F.);
#29573=ORIENTED_EDGE('',*,*,#22384,.T.);
#29574=ORIENTED_EDGE('',*,*,#22385,.T.);
#29575=ORIENTED_EDGE('',*,*,#22383,.T.);
#29576=ORIENTED_EDGE('',*,*,#22386,.T.);
#29577=ORIENTED_EDGE('',*,*,#22377,.F.);
#29578=ORIENTED_EDGE('',*,*,#22387,.T.);
#29579=ORIENTED_EDGE('',*,*,#22388,.F.);
#29580=ORIENTED_EDGE('',*,*,#22389,.T.);
#29581=ORIENTED_EDGE('',*,*,#22380,.F.);
#29582=ORIENTED_EDGE('',*,*,#22390,.T.);
#29583=ORIENTED_EDGE('',*,*,#22391,.T.);
#29584=ORIENTED_EDGE('',*,*,#22392,.T.);
#29585=ORIENTED_EDGE('',*,*,#22388,.T.);
#29586=ORIENTED_EDGE('',*,*,#22393,.T.);
#29587=ORIENTED_EDGE('',*,*,#22394,.T.);
#29588=ORIENTED_EDGE('',*,*,#22395,.T.);
#29589=ORIENTED_EDGE('',*,*,#22396,.T.);
#29590=ORIENTED_EDGE('',*,*,#22397,.F.);
#29591=ORIENTED_EDGE('',*,*,#22398,.T.);
#29592=ORIENTED_EDGE('',*,*,#22399,.T.);
#29593=ORIENTED_EDGE('',*,*,#22397,.T.);
#29594=ORIENTED_EDGE('',*,*,#22400,.T.);
#29595=ORIENTED_EDGE('',*,*,#22391,.F.);
#29596=ORIENTED_EDGE('',*,*,#22401,.T.);
#29597=ORIENTED_EDGE('',*,*,#22402,.F.);
#29598=ORIENTED_EDGE('',*,*,#22403,.T.);
#29599=ORIENTED_EDGE('',*,*,#22394,.F.);
#29600=ORIENTED_EDGE('',*,*,#22404,.T.);
#29601=ORIENTED_EDGE('',*,*,#22405,.T.);
#29602=ORIENTED_EDGE('',*,*,#22406,.T.);
#29603=ORIENTED_EDGE('',*,*,#22402,.T.);
#29604=ORIENTED_EDGE('',*,*,#22407,.T.);
#29605=ORIENTED_EDGE('',*,*,#22408,.T.);
#29606=ORIENTED_EDGE('',*,*,#22409,.T.);
#29607=ORIENTED_EDGE('',*,*,#22410,.T.);
#29608=ORIENTED_EDGE('',*,*,#22411,.F.);
#29609=ORIENTED_EDGE('',*,*,#22412,.T.);
#29610=ORIENTED_EDGE('',*,*,#22413,.T.);
#29611=ORIENTED_EDGE('',*,*,#22411,.T.);
#29612=ORIENTED_EDGE('',*,*,#22414,.T.);
#29613=ORIENTED_EDGE('',*,*,#22405,.F.);
#29614=ORIENTED_EDGE('',*,*,#22415,.T.);
#29615=ORIENTED_EDGE('',*,*,#22416,.F.);
#29616=ORIENTED_EDGE('',*,*,#22417,.T.);
#29617=ORIENTED_EDGE('',*,*,#22408,.F.);
#29618=ORIENTED_EDGE('',*,*,#22418,.T.);
#29619=ORIENTED_EDGE('',*,*,#22419,.T.);
#29620=ORIENTED_EDGE('',*,*,#22420,.T.);
#29621=ORIENTED_EDGE('',*,*,#22416,.T.);
#29622=ORIENTED_EDGE('',*,*,#22421,.T.);
#29623=ORIENTED_EDGE('',*,*,#22422,.T.);
#29624=ORIENTED_EDGE('',*,*,#22423,.T.);
#29625=ORIENTED_EDGE('',*,*,#22424,.T.);
#29626=ORIENTED_EDGE('',*,*,#22425,.F.);
#29627=ORIENTED_EDGE('',*,*,#22426,.T.);
#29628=ORIENTED_EDGE('',*,*,#22427,.T.);
#29629=ORIENTED_EDGE('',*,*,#22425,.T.);
#29630=ORIENTED_EDGE('',*,*,#22428,.T.);
#29631=ORIENTED_EDGE('',*,*,#22419,.F.);
#29632=ORIENTED_EDGE('',*,*,#22429,.T.);
#29633=ORIENTED_EDGE('',*,*,#22430,.F.);
#29634=ORIENTED_EDGE('',*,*,#22431,.T.);
#29635=ORIENTED_EDGE('',*,*,#22422,.F.);
#29636=ORIENTED_EDGE('',*,*,#22432,.T.);
#29637=ORIENTED_EDGE('',*,*,#22433,.T.);
#29638=ORIENTED_EDGE('',*,*,#22434,.T.);
#29639=ORIENTED_EDGE('',*,*,#22435,.T.);
#29640=ORIENTED_EDGE('',*,*,#22436,.F.);
#29641=ORIENTED_EDGE('',*,*,#22437,.T.);
#29642=ORIENTED_EDGE('',*,*,#22438,.T.);
#29643=ORIENTED_EDGE('',*,*,#21658,.F.);
#29644=ORIENTED_EDGE('',*,*,#22439,.T.);
#29645=ORIENTED_EDGE('',*,*,#22433,.F.);
#29646=ORIENTED_EDGE('',*,*,#22440,.T.);
#29647=ORIENTED_EDGE('',*,*,#22441,.T.);
#29648=ORIENTED_EDGE('',*,*,#22442,.T.);
#29649=ORIENTED_EDGE('',*,*,#22430,.T.);
#29650=ORIENTED_EDGE('',*,*,#22443,.T.);
#29651=ORIENTED_EDGE('',*,*,#22436,.T.);
#29652=ORIENTED_EDGE('',*,*,#22444,.T.);
#29653=ORIENTED_EDGE('',*,*,#22441,.F.);
#29654=ORIENTED_EDGE('',*,*,#22445,.T.);
#29655=ORIENTED_EDGE('',*,*,#21655,.F.);
#29656=ORIENTED_EDGE('',*,*,#22446,.T.);
#29657=ORIENTED_EDGE('',*,*,#22447,.T.);
#29658=ORIENTED_EDGE('',*,*,#22448,.F.);
#29659=ORIENTED_EDGE('',*,*,#22448,.T.);
#29660=ORIENTED_EDGE('',*,*,#22449,.T.);
#29661=ORIENTED_EDGE('',*,*,#21656,.F.);
#29662=ORIENTED_EDGE('',*,*,#22450,.T.);
#29663=ORIENTED_EDGE('',*,*,#22451,.T.);
#29664=ORIENTED_EDGE('',*,*,#21447,.F.);
#29665=ORIENTED_EDGE('',*,*,#22452,.F.);
#29666=ORIENTED_EDGE('',*,*,#22453,.T.);
#29667=ORIENTED_EDGE('',*,*,#22454,.T.);
#29668=ORIENTED_EDGE('',*,*,#22455,.F.);
#29669=ORIENTED_EDGE('',*,*,#22456,.T.);
#29670=ORIENTED_EDGE('',*,*,#22450,.F.);
#29671=ORIENTED_EDGE('',*,*,#22457,.T.);
#29672=ORIENTED_EDGE('',*,*,#22458,.T.);
#29673=ORIENTED_EDGE('',*,*,#22459,.T.);
#29674=ORIENTED_EDGE('',*,*,#22455,.T.);
#29675=ORIENTED_EDGE('',*,*,#22460,.T.);
#29676=ORIENTED_EDGE('',*,*,#22461,.T.);
#29677=ORIENTED_EDGE('',*,*,#22462,.T.);
#29678=ORIENTED_EDGE('',*,*,#22463,.T.);
#29679=ORIENTED_EDGE('',*,*,#22464,.F.);
#29680=ORIENTED_EDGE('',*,*,#22465,.T.);
#29681=ORIENTED_EDGE('',*,*,#22466,.T.);
#29682=ORIENTED_EDGE('',*,*,#22464,.T.);
#29683=ORIENTED_EDGE('',*,*,#22467,.T.);
#29684=ORIENTED_EDGE('',*,*,#22458,.F.);
#29685=ORIENTED_EDGE('',*,*,#22468,.T.);
#29686=ORIENTED_EDGE('',*,*,#21450,.F.);
#29687=ORIENTED_EDGE('',*,*,#22469,.T.);
#29688=ORIENTED_EDGE('',*,*,#22356,.T.);
#29689=ORIENTED_EDGE('',*,*,#22470,.F.);
#29690=ORIENTED_EDGE('',*,*,#22471,.T.);
#29691=ORIENTED_EDGE('',*,*,#22461,.F.);
#29692=ORIENTED_EDGE('',*,*,#22472,.T.);
#29693=ORIENTED_EDGE('',*,*,#22473,.T.);
#29694=ORIENTED_EDGE('',*,*,#22474,.T.);
#29695=ORIENTED_EDGE('',*,*,#22470,.T.);
#29696=ORIENTED_EDGE('',*,*,#22475,.T.);
#29697=ORIENTED_EDGE('',*,*,#22476,.T.);
#29698=ORIENTED_EDGE('',*,*,#22477,.T.);
#29699=ORIENTED_EDGE('',*,*,#22478,.T.);
#29700=ORIENTED_EDGE('',*,*,#22479,.F.);
#29701=ORIENTED_EDGE('',*,*,#22480,.T.);
#29702=ORIENTED_EDGE('',*,*,#22481,.T.);
#29703=ORIENTED_EDGE('',*,*,#22479,.T.);
#29704=ORIENTED_EDGE('',*,*,#22482,.T.);
#29705=ORIENTED_EDGE('',*,*,#22473,.F.);
#29706=ORIENTED_EDGE('',*,*,#22483,.T.);
#29707=ORIENTED_EDGE('',*,*,#22484,.F.);
#29708=ORIENTED_EDGE('',*,*,#22485,.T.);
#29709=ORIENTED_EDGE('',*,*,#22476,.F.);
#29710=ORIENTED_EDGE('',*,*,#22486,.T.);
#29711=ORIENTED_EDGE('',*,*,#22487,.T.);
#29712=ORIENTED_EDGE('',*,*,#22488,.T.);
#29713=ORIENTED_EDGE('',*,*,#22484,.T.);
#29714=ORIENTED_EDGE('',*,*,#22489,.T.);
#29715=ORIENTED_EDGE('',*,*,#22490,.T.);
#29716=ORIENTED_EDGE('',*,*,#22491,.T.);
#29717=ORIENTED_EDGE('',*,*,#22492,.T.);
#29718=ORIENTED_EDGE('',*,*,#22493,.F.);
#29719=ORIENTED_EDGE('',*,*,#22494,.T.);
#29720=ORIENTED_EDGE('',*,*,#22495,.T.);
#29721=ORIENTED_EDGE('',*,*,#22493,.T.);
#29722=ORIENTED_EDGE('',*,*,#22496,.T.);
#29723=ORIENTED_EDGE('',*,*,#22487,.F.);
#29724=ORIENTED_EDGE('',*,*,#22497,.T.);
#29725=ORIENTED_EDGE('',*,*,#22498,.F.);
#29726=ORIENTED_EDGE('',*,*,#22499,.T.);
#29727=ORIENTED_EDGE('',*,*,#22490,.F.);
#29728=ORIENTED_EDGE('',*,*,#22500,.T.);
#29729=ORIENTED_EDGE('',*,*,#22501,.T.);
#29730=ORIENTED_EDGE('',*,*,#22502,.T.);
#29731=ORIENTED_EDGE('',*,*,#22498,.T.);
#29732=ORIENTED_EDGE('',*,*,#22503,.T.);
#29733=ORIENTED_EDGE('',*,*,#22504,.T.);
#29734=ORIENTED_EDGE('',*,*,#22505,.T.);
#29735=ORIENTED_EDGE('',*,*,#22506,.T.);
#29736=ORIENTED_EDGE('',*,*,#22507,.F.);
#29737=ORIENTED_EDGE('',*,*,#22508,.T.);
#29738=ORIENTED_EDGE('',*,*,#22509,.T.);
#29739=ORIENTED_EDGE('',*,*,#22507,.T.);
#29740=ORIENTED_EDGE('',*,*,#22510,.T.);
#29741=ORIENTED_EDGE('',*,*,#22501,.F.);
#29742=ORIENTED_EDGE('',*,*,#22511,.T.);
#29743=ORIENTED_EDGE('',*,*,#22512,.F.);
#29744=ORIENTED_EDGE('',*,*,#22513,.T.);
#29745=ORIENTED_EDGE('',*,*,#22504,.F.);
#29746=ORIENTED_EDGE('',*,*,#22514,.T.);
#29747=ORIENTED_EDGE('',*,*,#22515,.T.);
#29748=ORIENTED_EDGE('',*,*,#22516,.T.);
#29749=ORIENTED_EDGE('',*,*,#22512,.T.);
#29750=ORIENTED_EDGE('',*,*,#22517,.T.);
#29751=ORIENTED_EDGE('',*,*,#22518,.T.);
#29752=ORIENTED_EDGE('',*,*,#22519,.T.);
#29753=ORIENTED_EDGE('',*,*,#22520,.T.);
#29754=ORIENTED_EDGE('',*,*,#22521,.F.);
#29755=ORIENTED_EDGE('',*,*,#22522,.T.);
#29756=ORIENTED_EDGE('',*,*,#22523,.T.);
#29757=ORIENTED_EDGE('',*,*,#22521,.T.);
#29758=ORIENTED_EDGE('',*,*,#22524,.T.);
#29759=ORIENTED_EDGE('',*,*,#22515,.F.);
#29760=ORIENTED_EDGE('',*,*,#22525,.T.);
#29761=ORIENTED_EDGE('',*,*,#22526,.F.);
#29762=ORIENTED_EDGE('',*,*,#22527,.T.);
#29763=ORIENTED_EDGE('',*,*,#22518,.F.);
#29764=ORIENTED_EDGE('',*,*,#22528,.T.);
#29765=ORIENTED_EDGE('',*,*,#22529,.T.);
#29766=ORIENTED_EDGE('',*,*,#22530,.T.);
#29767=ORIENTED_EDGE('',*,*,#22526,.T.);
#29768=ORIENTED_EDGE('',*,*,#22531,.T.);
#29769=ORIENTED_EDGE('',*,*,#22532,.T.);
#29770=ORIENTED_EDGE('',*,*,#22533,.T.);
#29771=ORIENTED_EDGE('',*,*,#22534,.T.);
#29772=ORIENTED_EDGE('',*,*,#22535,.F.);
#29773=ORIENTED_EDGE('',*,*,#22536,.T.);
#29774=ORIENTED_EDGE('',*,*,#22537,.T.);
#29775=ORIENTED_EDGE('',*,*,#22535,.T.);
#29776=ORIENTED_EDGE('',*,*,#22538,.T.);
#29777=ORIENTED_EDGE('',*,*,#22529,.F.);
#29778=ORIENTED_EDGE('',*,*,#22539,.T.);
#29779=ORIENTED_EDGE('',*,*,#21664,.F.);
#29780=ORIENTED_EDGE('',*,*,#22540,.T.);
#29781=ORIENTED_EDGE('',*,*,#22532,.F.);
#29782=ORIENTED_EDGE('',*,*,#22541,.T.);
#29783=ORIENTED_EDGE('',*,*,#21661,.F.);
#29784=ORIENTED_EDGE('',*,*,#22542,.T.);
#29785=ORIENTED_EDGE('',*,*,#22543,.T.);
#29786=ORIENTED_EDGE('',*,*,#22544,.F.);
#29787=ORIENTED_EDGE('',*,*,#22544,.T.);
#29788=ORIENTED_EDGE('',*,*,#22545,.T.);
#29789=ORIENTED_EDGE('',*,*,#21662,.F.);
#29790=ORIENTED_EDGE('',*,*,#22546,.T.);
#29791=ORIENTED_EDGE('',*,*,#22547,.T.);
#29792=ORIENTED_EDGE('',*,*,#21443,.F.);
#29793=ORIENTED_EDGE('',*,*,#22548,.F.);
#29794=ORIENTED_EDGE('',*,*,#22549,.T.);
#29795=ORIENTED_EDGE('',*,*,#22550,.T.);
#29796=ORIENTED_EDGE('',*,*,#22551,.F.);
#29797=ORIENTED_EDGE('',*,*,#22552,.T.);
#29798=ORIENTED_EDGE('',*,*,#22546,.F.);
#29799=ORIENTED_EDGE('',*,*,#22553,.T.);
#29800=ORIENTED_EDGE('',*,*,#22554,.T.);
#29801=ORIENTED_EDGE('',*,*,#22555,.T.);
#29802=ORIENTED_EDGE('',*,*,#22551,.T.);
#29803=ORIENTED_EDGE('',*,*,#22556,.T.);
#29804=ORIENTED_EDGE('',*,*,#22557,.T.);
#29805=ORIENTED_EDGE('',*,*,#22558,.T.);
#29806=ORIENTED_EDGE('',*,*,#22559,.T.);
#29807=ORIENTED_EDGE('',*,*,#22560,.F.);
#29808=ORIENTED_EDGE('',*,*,#22561,.T.);
#29809=ORIENTED_EDGE('',*,*,#22562,.T.);
#29810=ORIENTED_EDGE('',*,*,#22560,.T.);
#29811=ORIENTED_EDGE('',*,*,#22563,.T.);
#29812=ORIENTED_EDGE('',*,*,#22554,.F.);
#29813=ORIENTED_EDGE('',*,*,#22564,.T.);
#29814=ORIENTED_EDGE('',*,*,#21446,.F.);
#29815=ORIENTED_EDGE('',*,*,#22565,.T.);
#29816=ORIENTED_EDGE('',*,*,#22452,.T.);
#29817=ORIENTED_EDGE('',*,*,#22566,.F.);
#29818=ORIENTED_EDGE('',*,*,#22567,.T.);
#29819=ORIENTED_EDGE('',*,*,#22557,.F.);
#29820=ORIENTED_EDGE('',*,*,#22568,.T.);
#29821=ORIENTED_EDGE('',*,*,#22569,.T.);
#29822=ORIENTED_EDGE('',*,*,#22570,.T.);
#29823=ORIENTED_EDGE('',*,*,#22566,.T.);
#29824=ORIENTED_EDGE('',*,*,#22571,.T.);
#29825=ORIENTED_EDGE('',*,*,#22572,.T.);
#29826=ORIENTED_EDGE('',*,*,#22573,.T.);
#29827=ORIENTED_EDGE('',*,*,#22574,.T.);
#29828=ORIENTED_EDGE('',*,*,#22575,.F.);
#29829=ORIENTED_EDGE('',*,*,#22576,.T.);
#29830=ORIENTED_EDGE('',*,*,#22577,.T.);
#29831=ORIENTED_EDGE('',*,*,#22575,.T.);
#29832=ORIENTED_EDGE('',*,*,#22578,.T.);
#29833=ORIENTED_EDGE('',*,*,#22569,.F.);
#29834=ORIENTED_EDGE('',*,*,#22579,.T.);
#29835=ORIENTED_EDGE('',*,*,#22580,.F.);
#29836=ORIENTED_EDGE('',*,*,#22581,.T.);
#29837=ORIENTED_EDGE('',*,*,#22572,.F.);
#29838=ORIENTED_EDGE('',*,*,#22582,.T.);
#29839=ORIENTED_EDGE('',*,*,#22583,.T.);
#29840=ORIENTED_EDGE('',*,*,#22584,.T.);
#29841=ORIENTED_EDGE('',*,*,#22580,.T.);
#29842=ORIENTED_EDGE('',*,*,#22585,.T.);
#29843=ORIENTED_EDGE('',*,*,#22586,.T.);
#29844=ORIENTED_EDGE('',*,*,#22587,.T.);
#29845=ORIENTED_EDGE('',*,*,#22588,.T.);
#29846=ORIENTED_EDGE('',*,*,#22589,.F.);
#29847=ORIENTED_EDGE('',*,*,#22590,.T.);
#29848=ORIENTED_EDGE('',*,*,#22591,.T.);
#29849=ORIENTED_EDGE('',*,*,#22589,.T.);
#29850=ORIENTED_EDGE('',*,*,#22592,.T.);
#29851=ORIENTED_EDGE('',*,*,#22583,.F.);
#29852=ORIENTED_EDGE('',*,*,#22593,.T.);
#29853=ORIENTED_EDGE('',*,*,#22594,.F.);
#29854=ORIENTED_EDGE('',*,*,#22595,.T.);
#29855=ORIENTED_EDGE('',*,*,#22586,.F.);
#29856=ORIENTED_EDGE('',*,*,#22596,.T.);
#29857=ORIENTED_EDGE('',*,*,#22597,.T.);
#29858=ORIENTED_EDGE('',*,*,#22598,.T.);
#29859=ORIENTED_EDGE('',*,*,#22594,.T.);
#29860=ORIENTED_EDGE('',*,*,#22599,.T.);
#29861=ORIENTED_EDGE('',*,*,#22600,.T.);
#29862=ORIENTED_EDGE('',*,*,#22601,.T.);
#29863=ORIENTED_EDGE('',*,*,#22602,.T.);
#29864=ORIENTED_EDGE('',*,*,#22603,.F.);
#29865=ORIENTED_EDGE('',*,*,#22604,.T.);
#29866=ORIENTED_EDGE('',*,*,#22605,.T.);
#29867=ORIENTED_EDGE('',*,*,#22603,.T.);
#29868=ORIENTED_EDGE('',*,*,#22606,.T.);
#29869=ORIENTED_EDGE('',*,*,#22597,.F.);
#29870=ORIENTED_EDGE('',*,*,#22607,.T.);
#29871=ORIENTED_EDGE('',*,*,#22608,.F.);
#29872=ORIENTED_EDGE('',*,*,#22609,.T.);
#29873=ORIENTED_EDGE('',*,*,#22600,.F.);
#29874=ORIENTED_EDGE('',*,*,#22610,.T.);
#29875=ORIENTED_EDGE('',*,*,#22611,.T.);
#29876=ORIENTED_EDGE('',*,*,#22612,.T.);
#29877=ORIENTED_EDGE('',*,*,#22608,.T.);
#29878=ORIENTED_EDGE('',*,*,#22613,.T.);
#29879=ORIENTED_EDGE('',*,*,#22614,.T.);
#29880=ORIENTED_EDGE('',*,*,#22615,.T.);
#29881=ORIENTED_EDGE('',*,*,#22616,.T.);
#29882=ORIENTED_EDGE('',*,*,#22617,.F.);
#29883=ORIENTED_EDGE('',*,*,#22618,.T.);
#29884=ORIENTED_EDGE('',*,*,#22619,.T.);
#29885=ORIENTED_EDGE('',*,*,#22617,.T.);
#29886=ORIENTED_EDGE('',*,*,#22620,.T.);
#29887=ORIENTED_EDGE('',*,*,#22611,.F.);
#29888=ORIENTED_EDGE('',*,*,#22621,.T.);
#29889=ORIENTED_EDGE('',*,*,#22622,.F.);
#29890=ORIENTED_EDGE('',*,*,#22623,.T.);
#29891=ORIENTED_EDGE('',*,*,#22614,.F.);
#29892=ORIENTED_EDGE('',*,*,#22624,.T.);
#29893=ORIENTED_EDGE('',*,*,#22625,.T.);
#29894=ORIENTED_EDGE('',*,*,#22626,.T.);
#29895=ORIENTED_EDGE('',*,*,#22622,.T.);
#29896=ORIENTED_EDGE('',*,*,#22627,.T.);
#29897=ORIENTED_EDGE('',*,*,#22628,.T.);
#29898=ORIENTED_EDGE('',*,*,#22629,.T.);
#29899=ORIENTED_EDGE('',*,*,#22630,.T.);
#29900=ORIENTED_EDGE('',*,*,#22631,.F.);
#29901=ORIENTED_EDGE('',*,*,#22632,.T.);
#29902=ORIENTED_EDGE('',*,*,#22633,.T.);
#29903=ORIENTED_EDGE('',*,*,#22631,.T.);
#29904=ORIENTED_EDGE('',*,*,#22634,.T.);
#29905=ORIENTED_EDGE('',*,*,#22625,.F.);
#29906=ORIENTED_EDGE('',*,*,#22635,.T.);
#29907=ORIENTED_EDGE('',*,*,#21670,.F.);
#29908=ORIENTED_EDGE('',*,*,#22636,.T.);
#29909=ORIENTED_EDGE('',*,*,#22628,.F.);
#29910=ORIENTED_EDGE('',*,*,#22637,.T.);
#29911=ORIENTED_EDGE('',*,*,#21667,.F.);
#29912=ORIENTED_EDGE('',*,*,#22638,.T.);
#29913=ORIENTED_EDGE('',*,*,#22639,.T.);
#29914=ORIENTED_EDGE('',*,*,#22640,.F.);
#29915=ORIENTED_EDGE('',*,*,#22640,.T.);
#29916=ORIENTED_EDGE('',*,*,#22641,.T.);
#29917=ORIENTED_EDGE('',*,*,#21668,.F.);
#29918=ORIENTED_EDGE('',*,*,#22642,.T.);
#29919=ORIENTED_EDGE('',*,*,#22643,.T.);
#29920=ORIENTED_EDGE('',*,*,#21439,.F.);
#29921=ORIENTED_EDGE('',*,*,#22644,.F.);
#29922=ORIENTED_EDGE('',*,*,#22645,.T.);
#29923=ORIENTED_EDGE('',*,*,#22646,.T.);
#29924=ORIENTED_EDGE('',*,*,#22647,.F.);
#29925=ORIENTED_EDGE('',*,*,#22648,.T.);
#29926=ORIENTED_EDGE('',*,*,#22642,.F.);
#29927=ORIENTED_EDGE('',*,*,#22649,.T.);
#29928=ORIENTED_EDGE('',*,*,#22650,.T.);
#29929=ORIENTED_EDGE('',*,*,#22651,.T.);
#29930=ORIENTED_EDGE('',*,*,#22647,.T.);
#29931=ORIENTED_EDGE('',*,*,#22652,.T.);
#29932=ORIENTED_EDGE('',*,*,#22653,.T.);
#29933=ORIENTED_EDGE('',*,*,#22654,.T.);
#29934=ORIENTED_EDGE('',*,*,#22655,.T.);
#29935=ORIENTED_EDGE('',*,*,#22656,.F.);
#29936=ORIENTED_EDGE('',*,*,#22657,.T.);
#29937=ORIENTED_EDGE('',*,*,#22658,.T.);
#29938=ORIENTED_EDGE('',*,*,#22656,.T.);
#29939=ORIENTED_EDGE('',*,*,#22659,.T.);
#29940=ORIENTED_EDGE('',*,*,#22650,.F.);
#29941=ORIENTED_EDGE('',*,*,#22660,.T.);
#29942=ORIENTED_EDGE('',*,*,#21442,.F.);
#29943=ORIENTED_EDGE('',*,*,#22661,.T.);
#29944=ORIENTED_EDGE('',*,*,#22548,.T.);
#29945=ORIENTED_EDGE('',*,*,#22662,.F.);
#29946=ORIENTED_EDGE('',*,*,#22663,.T.);
#29947=ORIENTED_EDGE('',*,*,#22653,.F.);
#29948=ORIENTED_EDGE('',*,*,#22664,.T.);
#29949=ORIENTED_EDGE('',*,*,#22665,.T.);
#29950=ORIENTED_EDGE('',*,*,#22666,.T.);
#29951=ORIENTED_EDGE('',*,*,#22662,.T.);
#29952=ORIENTED_EDGE('',*,*,#22667,.T.);
#29953=ORIENTED_EDGE('',*,*,#22668,.T.);
#29954=ORIENTED_EDGE('',*,*,#22669,.T.);
#29955=ORIENTED_EDGE('',*,*,#22670,.T.);
#29956=ORIENTED_EDGE('',*,*,#22671,.F.);
#29957=ORIENTED_EDGE('',*,*,#22672,.T.);
#29958=ORIENTED_EDGE('',*,*,#22673,.T.);
#29959=ORIENTED_EDGE('',*,*,#22671,.T.);
#29960=ORIENTED_EDGE('',*,*,#22674,.T.);
#29961=ORIENTED_EDGE('',*,*,#22665,.F.);
#29962=ORIENTED_EDGE('',*,*,#22675,.T.);
#29963=ORIENTED_EDGE('',*,*,#22676,.F.);
#29964=ORIENTED_EDGE('',*,*,#22677,.T.);
#29965=ORIENTED_EDGE('',*,*,#22668,.F.);
#29966=ORIENTED_EDGE('',*,*,#22678,.T.);
#29967=ORIENTED_EDGE('',*,*,#22679,.T.);
#29968=ORIENTED_EDGE('',*,*,#22680,.T.);
#29969=ORIENTED_EDGE('',*,*,#22676,.T.);
#29970=ORIENTED_EDGE('',*,*,#22681,.T.);
#29971=ORIENTED_EDGE('',*,*,#22682,.T.);
#29972=ORIENTED_EDGE('',*,*,#22683,.T.);
#29973=ORIENTED_EDGE('',*,*,#22684,.T.);
#29974=ORIENTED_EDGE('',*,*,#22685,.F.);
#29975=ORIENTED_EDGE('',*,*,#22686,.T.);
#29976=ORIENTED_EDGE('',*,*,#22687,.T.);
#29977=ORIENTED_EDGE('',*,*,#22685,.T.);
#29978=ORIENTED_EDGE('',*,*,#22688,.T.);
#29979=ORIENTED_EDGE('',*,*,#22679,.F.);
#29980=ORIENTED_EDGE('',*,*,#22689,.T.);
#29981=ORIENTED_EDGE('',*,*,#22690,.F.);
#29982=ORIENTED_EDGE('',*,*,#22691,.T.);
#29983=ORIENTED_EDGE('',*,*,#22682,.F.);
#29984=ORIENTED_EDGE('',*,*,#22692,.T.);
#29985=ORIENTED_EDGE('',*,*,#22693,.T.);
#29986=ORIENTED_EDGE('',*,*,#22694,.T.);
#29987=ORIENTED_EDGE('',*,*,#22690,.T.);
#29988=ORIENTED_EDGE('',*,*,#22695,.T.);
#29989=ORIENTED_EDGE('',*,*,#22696,.T.);
#29990=ORIENTED_EDGE('',*,*,#22697,.T.);
#29991=ORIENTED_EDGE('',*,*,#22698,.T.);
#29992=ORIENTED_EDGE('',*,*,#22699,.F.);
#29993=ORIENTED_EDGE('',*,*,#22700,.T.);
#29994=ORIENTED_EDGE('',*,*,#22701,.T.);
#29995=ORIENTED_EDGE('',*,*,#22699,.T.);
#29996=ORIENTED_EDGE('',*,*,#22702,.T.);
#29997=ORIENTED_EDGE('',*,*,#22693,.F.);
#29998=ORIENTED_EDGE('',*,*,#22703,.T.);
#29999=ORIENTED_EDGE('',*,*,#22704,.F.);
#30000=ORIENTED_EDGE('',*,*,#22705,.T.);
#30001=ORIENTED_EDGE('',*,*,#22696,.F.);
#30002=ORIENTED_EDGE('',*,*,#22706,.T.);
#30003=ORIENTED_EDGE('',*,*,#22707,.T.);
#30004=ORIENTED_EDGE('',*,*,#22708,.T.);
#30005=ORIENTED_EDGE('',*,*,#22704,.T.);
#30006=ORIENTED_EDGE('',*,*,#22709,.T.);
#30007=ORIENTED_EDGE('',*,*,#22710,.T.);
#30008=ORIENTED_EDGE('',*,*,#22711,.T.);
#30009=ORIENTED_EDGE('',*,*,#22712,.T.);
#30010=ORIENTED_EDGE('',*,*,#22713,.F.);
#30011=ORIENTED_EDGE('',*,*,#22714,.T.);
#30012=ORIENTED_EDGE('',*,*,#22715,.T.);
#30013=ORIENTED_EDGE('',*,*,#22713,.T.);
#30014=ORIENTED_EDGE('',*,*,#22716,.T.);
#30015=ORIENTED_EDGE('',*,*,#22707,.F.);
#30016=ORIENTED_EDGE('',*,*,#22717,.T.);
#30017=ORIENTED_EDGE('',*,*,#22718,.F.);
#30018=ORIENTED_EDGE('',*,*,#22719,.T.);
#30019=ORIENTED_EDGE('',*,*,#22710,.F.);
#30020=ORIENTED_EDGE('',*,*,#22720,.T.);
#30021=ORIENTED_EDGE('',*,*,#22721,.T.);
#30022=ORIENTED_EDGE('',*,*,#22722,.T.);
#30023=ORIENTED_EDGE('',*,*,#22718,.T.);
#30024=ORIENTED_EDGE('',*,*,#22723,.T.);
#30025=ORIENTED_EDGE('',*,*,#22724,.T.);
#30026=ORIENTED_EDGE('',*,*,#22725,.T.);
#30027=ORIENTED_EDGE('',*,*,#22726,.T.);
#30028=ORIENTED_EDGE('',*,*,#22727,.F.);
#30029=ORIENTED_EDGE('',*,*,#22728,.T.);
#30030=ORIENTED_EDGE('',*,*,#22729,.T.);
#30031=ORIENTED_EDGE('',*,*,#22727,.T.);
#30032=ORIENTED_EDGE('',*,*,#22730,.T.);
#30033=ORIENTED_EDGE('',*,*,#22721,.F.);
#30034=ORIENTED_EDGE('',*,*,#22731,.T.);
#30035=ORIENTED_EDGE('',*,*,#21676,.F.);
#30036=ORIENTED_EDGE('',*,*,#22732,.T.);
#30037=ORIENTED_EDGE('',*,*,#22724,.F.);
#30038=ORIENTED_EDGE('',*,*,#22733,.T.);
#30039=ORIENTED_EDGE('',*,*,#21673,.F.);
#30040=ORIENTED_EDGE('',*,*,#22734,.T.);
#30041=ORIENTED_EDGE('',*,*,#22735,.T.);
#30042=ORIENTED_EDGE('',*,*,#22736,.F.);
#30043=ORIENTED_EDGE('',*,*,#22736,.T.);
#30044=ORIENTED_EDGE('',*,*,#22737,.T.);
#30045=ORIENTED_EDGE('',*,*,#21674,.F.);
#30046=ORIENTED_EDGE('',*,*,#22738,.T.);
#30047=ORIENTED_EDGE('',*,*,#22739,.T.);
#30048=ORIENTED_EDGE('',*,*,#21435,.F.);
#30049=ORIENTED_EDGE('',*,*,#22740,.F.);
#30050=ORIENTED_EDGE('',*,*,#22741,.T.);
#30051=ORIENTED_EDGE('',*,*,#22742,.T.);
#30052=ORIENTED_EDGE('',*,*,#22743,.F.);
#30053=ORIENTED_EDGE('',*,*,#22744,.T.);
#30054=ORIENTED_EDGE('',*,*,#22738,.F.);
#30055=ORIENTED_EDGE('',*,*,#22745,.T.);
#30056=ORIENTED_EDGE('',*,*,#22746,.T.);
#30057=ORIENTED_EDGE('',*,*,#22747,.T.);
#30058=ORIENTED_EDGE('',*,*,#22743,.T.);
#30059=ORIENTED_EDGE('',*,*,#22748,.T.);
#30060=ORIENTED_EDGE('',*,*,#22749,.T.);
#30061=ORIENTED_EDGE('',*,*,#22750,.T.);
#30062=ORIENTED_EDGE('',*,*,#22751,.T.);
#30063=ORIENTED_EDGE('',*,*,#22752,.F.);
#30064=ORIENTED_EDGE('',*,*,#22753,.T.);
#30065=ORIENTED_EDGE('',*,*,#22754,.T.);
#30066=ORIENTED_EDGE('',*,*,#22752,.T.);
#30067=ORIENTED_EDGE('',*,*,#22755,.T.);
#30068=ORIENTED_EDGE('',*,*,#22746,.F.);
#30069=ORIENTED_EDGE('',*,*,#22756,.T.);
#30070=ORIENTED_EDGE('',*,*,#21438,.F.);
#30071=ORIENTED_EDGE('',*,*,#22757,.T.);
#30072=ORIENTED_EDGE('',*,*,#22644,.T.);
#30073=ORIENTED_EDGE('',*,*,#22758,.F.);
#30074=ORIENTED_EDGE('',*,*,#22759,.T.);
#30075=ORIENTED_EDGE('',*,*,#22749,.F.);
#30076=ORIENTED_EDGE('',*,*,#22760,.T.);
#30077=ORIENTED_EDGE('',*,*,#22761,.T.);
#30078=ORIENTED_EDGE('',*,*,#22762,.T.);
#30079=ORIENTED_EDGE('',*,*,#22758,.T.);
#30080=ORIENTED_EDGE('',*,*,#22763,.T.);
#30081=ORIENTED_EDGE('',*,*,#22764,.T.);
#30082=ORIENTED_EDGE('',*,*,#22765,.T.);
#30083=ORIENTED_EDGE('',*,*,#22766,.T.);
#30084=ORIENTED_EDGE('',*,*,#22767,.F.);
#30085=ORIENTED_EDGE('',*,*,#22768,.T.);
#30086=ORIENTED_EDGE('',*,*,#22769,.T.);
#30087=ORIENTED_EDGE('',*,*,#22767,.T.);
#30088=ORIENTED_EDGE('',*,*,#22770,.T.);
#30089=ORIENTED_EDGE('',*,*,#22761,.F.);
#30090=ORIENTED_EDGE('',*,*,#22771,.T.);
#30091=ORIENTED_EDGE('',*,*,#22772,.F.);
#30092=ORIENTED_EDGE('',*,*,#22773,.T.);
#30093=ORIENTED_EDGE('',*,*,#22764,.F.);
#30094=ORIENTED_EDGE('',*,*,#22774,.T.);
#30095=ORIENTED_EDGE('',*,*,#22775,.T.);
#30096=ORIENTED_EDGE('',*,*,#22776,.T.);
#30097=ORIENTED_EDGE('',*,*,#22772,.T.);
#30098=ORIENTED_EDGE('',*,*,#22777,.T.);
#30099=ORIENTED_EDGE('',*,*,#22778,.T.);
#30100=ORIENTED_EDGE('',*,*,#22779,.T.);
#30101=ORIENTED_EDGE('',*,*,#22780,.T.);
#30102=ORIENTED_EDGE('',*,*,#22781,.F.);
#30103=ORIENTED_EDGE('',*,*,#22782,.T.);
#30104=ORIENTED_EDGE('',*,*,#22783,.T.);
#30105=ORIENTED_EDGE('',*,*,#22781,.T.);
#30106=ORIENTED_EDGE('',*,*,#22784,.T.);
#30107=ORIENTED_EDGE('',*,*,#22775,.F.);
#30108=ORIENTED_EDGE('',*,*,#22785,.T.);
#30109=ORIENTED_EDGE('',*,*,#22786,.F.);
#30110=ORIENTED_EDGE('',*,*,#22787,.T.);
#30111=ORIENTED_EDGE('',*,*,#22778,.F.);
#30112=ORIENTED_EDGE('',*,*,#22788,.T.);
#30113=ORIENTED_EDGE('',*,*,#22789,.T.);
#30114=ORIENTED_EDGE('',*,*,#22790,.T.);
#30115=ORIENTED_EDGE('',*,*,#22786,.T.);
#30116=ORIENTED_EDGE('',*,*,#22791,.T.);
#30117=ORIENTED_EDGE('',*,*,#22792,.T.);
#30118=ORIENTED_EDGE('',*,*,#22793,.T.);
#30119=ORIENTED_EDGE('',*,*,#22794,.T.);
#30120=ORIENTED_EDGE('',*,*,#22795,.F.);
#30121=ORIENTED_EDGE('',*,*,#22796,.T.);
#30122=ORIENTED_EDGE('',*,*,#22797,.T.);
#30123=ORIENTED_EDGE('',*,*,#22795,.T.);
#30124=ORIENTED_EDGE('',*,*,#22798,.T.);
#30125=ORIENTED_EDGE('',*,*,#22789,.F.);
#30126=ORIENTED_EDGE('',*,*,#22799,.T.);
#30127=ORIENTED_EDGE('',*,*,#22800,.F.);
#30128=ORIENTED_EDGE('',*,*,#22801,.T.);
#30129=ORIENTED_EDGE('',*,*,#22792,.F.);
#30130=ORIENTED_EDGE('',*,*,#22802,.T.);
#30131=ORIENTED_EDGE('',*,*,#22803,.T.);
#30132=ORIENTED_EDGE('',*,*,#22804,.T.);
#30133=ORIENTED_EDGE('',*,*,#22800,.T.);
#30134=ORIENTED_EDGE('',*,*,#22805,.T.);
#30135=ORIENTED_EDGE('',*,*,#22806,.T.);
#30136=ORIENTED_EDGE('',*,*,#22807,.T.);
#30137=ORIENTED_EDGE('',*,*,#22808,.T.);
#30138=ORIENTED_EDGE('',*,*,#22809,.F.);
#30139=ORIENTED_EDGE('',*,*,#22810,.T.);
#30140=ORIENTED_EDGE('',*,*,#22811,.T.);
#30141=ORIENTED_EDGE('',*,*,#22809,.T.);
#30142=ORIENTED_EDGE('',*,*,#22812,.T.);
#30143=ORIENTED_EDGE('',*,*,#22803,.F.);
#30144=ORIENTED_EDGE('',*,*,#22813,.T.);
#30145=ORIENTED_EDGE('',*,*,#22814,.F.);
#30146=ORIENTED_EDGE('',*,*,#22815,.T.);
#30147=ORIENTED_EDGE('',*,*,#22806,.F.);
#30148=ORIENTED_EDGE('',*,*,#22816,.T.);
#30149=ORIENTED_EDGE('',*,*,#22817,.T.);
#30150=ORIENTED_EDGE('',*,*,#22818,.T.);
#30151=ORIENTED_EDGE('',*,*,#22814,.T.);
#30152=ORIENTED_EDGE('',*,*,#22819,.T.);
#30153=ORIENTED_EDGE('',*,*,#22820,.T.);
#30154=ORIENTED_EDGE('',*,*,#22821,.T.);
#30155=ORIENTED_EDGE('',*,*,#22822,.T.);
#30156=ORIENTED_EDGE('',*,*,#22823,.F.);
#30157=ORIENTED_EDGE('',*,*,#22824,.T.);
#30158=ORIENTED_EDGE('',*,*,#22825,.T.);
#30159=ORIENTED_EDGE('',*,*,#22823,.T.);
#30160=ORIENTED_EDGE('',*,*,#22826,.T.);
#30161=ORIENTED_EDGE('',*,*,#22817,.F.);
#30162=ORIENTED_EDGE('',*,*,#22827,.T.);
#30163=ORIENTED_EDGE('',*,*,#21682,.F.);
#30164=ORIENTED_EDGE('',*,*,#22828,.T.);
#30165=ORIENTED_EDGE('',*,*,#22820,.F.);
#30166=ORIENTED_EDGE('',*,*,#22829,.T.);
#30167=ORIENTED_EDGE('',*,*,#21679,.F.);
#30168=ORIENTED_EDGE('',*,*,#22830,.T.);
#30169=ORIENTED_EDGE('',*,*,#22831,.T.);
#30170=ORIENTED_EDGE('',*,*,#22832,.F.);
#30171=ORIENTED_EDGE('',*,*,#22832,.T.);
#30172=ORIENTED_EDGE('',*,*,#22833,.T.);
#30173=ORIENTED_EDGE('',*,*,#21680,.F.);
#30174=ORIENTED_EDGE('',*,*,#22834,.T.);
#30175=ORIENTED_EDGE('',*,*,#22835,.T.);
#30176=ORIENTED_EDGE('',*,*,#21431,.F.);
#30177=ORIENTED_EDGE('',*,*,#22836,.F.);
#30178=ORIENTED_EDGE('',*,*,#22837,.T.);
#30179=ORIENTED_EDGE('',*,*,#22838,.T.);
#30180=ORIENTED_EDGE('',*,*,#22839,.F.);
#30181=ORIENTED_EDGE('',*,*,#22840,.T.);
#30182=ORIENTED_EDGE('',*,*,#22834,.F.);
#30183=ORIENTED_EDGE('',*,*,#22841,.T.);
#30184=ORIENTED_EDGE('',*,*,#22842,.T.);
#30185=ORIENTED_EDGE('',*,*,#22843,.T.);
#30186=ORIENTED_EDGE('',*,*,#22839,.T.);
#30187=ORIENTED_EDGE('',*,*,#22844,.T.);
#30188=ORIENTED_EDGE('',*,*,#22845,.T.);
#30189=ORIENTED_EDGE('',*,*,#22846,.T.);
#30190=ORIENTED_EDGE('',*,*,#22847,.T.);
#30191=ORIENTED_EDGE('',*,*,#22848,.F.);
#30192=ORIENTED_EDGE('',*,*,#22849,.T.);
#30193=ORIENTED_EDGE('',*,*,#22850,.T.);
#30194=ORIENTED_EDGE('',*,*,#22848,.T.);
#30195=ORIENTED_EDGE('',*,*,#22851,.T.);
#30196=ORIENTED_EDGE('',*,*,#22842,.F.);
#30197=ORIENTED_EDGE('',*,*,#22852,.T.);
#30198=ORIENTED_EDGE('',*,*,#21434,.F.);
#30199=ORIENTED_EDGE('',*,*,#22853,.T.);
#30200=ORIENTED_EDGE('',*,*,#22740,.T.);
#30201=ORIENTED_EDGE('',*,*,#22854,.F.);
#30202=ORIENTED_EDGE('',*,*,#22855,.T.);
#30203=ORIENTED_EDGE('',*,*,#22845,.F.);
#30204=ORIENTED_EDGE('',*,*,#22856,.T.);
#30205=ORIENTED_EDGE('',*,*,#22857,.T.);
#30206=ORIENTED_EDGE('',*,*,#22858,.T.);
#30207=ORIENTED_EDGE('',*,*,#22854,.T.);
#30208=ORIENTED_EDGE('',*,*,#22859,.T.);
#30209=ORIENTED_EDGE('',*,*,#22860,.T.);
#30210=ORIENTED_EDGE('',*,*,#22861,.T.);
#30211=ORIENTED_EDGE('',*,*,#22862,.T.);
#30212=ORIENTED_EDGE('',*,*,#22863,.F.);
#30213=ORIENTED_EDGE('',*,*,#22864,.T.);
#30214=ORIENTED_EDGE('',*,*,#22865,.T.);
#30215=ORIENTED_EDGE('',*,*,#22863,.T.);
#30216=ORIENTED_EDGE('',*,*,#22866,.T.);
#30217=ORIENTED_EDGE('',*,*,#22857,.F.);
#30218=ORIENTED_EDGE('',*,*,#22867,.T.);
#30219=ORIENTED_EDGE('',*,*,#22868,.F.);
#30220=ORIENTED_EDGE('',*,*,#22869,.T.);
#30221=ORIENTED_EDGE('',*,*,#22860,.F.);
#30222=ORIENTED_EDGE('',*,*,#22870,.T.);
#30223=ORIENTED_EDGE('',*,*,#22871,.T.);
#30224=ORIENTED_EDGE('',*,*,#22872,.T.);
#30225=ORIENTED_EDGE('',*,*,#22868,.T.);
#30226=ORIENTED_EDGE('',*,*,#22873,.T.);
#30227=ORIENTED_EDGE('',*,*,#22874,.T.);
#30228=ORIENTED_EDGE('',*,*,#22875,.T.);
#30229=ORIENTED_EDGE('',*,*,#22876,.T.);
#30230=ORIENTED_EDGE('',*,*,#22877,.F.);
#30231=ORIENTED_EDGE('',*,*,#22878,.T.);
#30232=ORIENTED_EDGE('',*,*,#22879,.T.);
#30233=ORIENTED_EDGE('',*,*,#22877,.T.);
#30234=ORIENTED_EDGE('',*,*,#22880,.T.);
#30235=ORIENTED_EDGE('',*,*,#22871,.F.);
#30236=ORIENTED_EDGE('',*,*,#22881,.T.);
#30237=ORIENTED_EDGE('',*,*,#22882,.F.);
#30238=ORIENTED_EDGE('',*,*,#22883,.T.);
#30239=ORIENTED_EDGE('',*,*,#22874,.F.);
#30240=ORIENTED_EDGE('',*,*,#22884,.T.);
#30241=ORIENTED_EDGE('',*,*,#22885,.T.);
#30242=ORIENTED_EDGE('',*,*,#22886,.T.);
#30243=ORIENTED_EDGE('',*,*,#22882,.T.);
#30244=ORIENTED_EDGE('',*,*,#22887,.T.);
#30245=ORIENTED_EDGE('',*,*,#22888,.T.);
#30246=ORIENTED_EDGE('',*,*,#22889,.T.);
#30247=ORIENTED_EDGE('',*,*,#22890,.T.);
#30248=ORIENTED_EDGE('',*,*,#22891,.F.);
#30249=ORIENTED_EDGE('',*,*,#22892,.T.);
#30250=ORIENTED_EDGE('',*,*,#22893,.T.);
#30251=ORIENTED_EDGE('',*,*,#22891,.T.);
#30252=ORIENTED_EDGE('',*,*,#22894,.T.);
#30253=ORIENTED_EDGE('',*,*,#22885,.F.);
#30254=ORIENTED_EDGE('',*,*,#22895,.T.);
#30255=ORIENTED_EDGE('',*,*,#22896,.F.);
#30256=ORIENTED_EDGE('',*,*,#22897,.T.);
#30257=ORIENTED_EDGE('',*,*,#22888,.F.);
#30258=ORIENTED_EDGE('',*,*,#22898,.T.);
#30259=ORIENTED_EDGE('',*,*,#22899,.T.);
#30260=ORIENTED_EDGE('',*,*,#22900,.T.);
#30261=ORIENTED_EDGE('',*,*,#22896,.T.);
#30262=ORIENTED_EDGE('',*,*,#22901,.T.);
#30263=ORIENTED_EDGE('',*,*,#22902,.T.);
#30264=ORIENTED_EDGE('',*,*,#22903,.T.);
#30265=ORIENTED_EDGE('',*,*,#22904,.T.);
#30266=ORIENTED_EDGE('',*,*,#22905,.F.);
#30267=ORIENTED_EDGE('',*,*,#22906,.T.);
#30268=ORIENTED_EDGE('',*,*,#22907,.T.);
#30269=ORIENTED_EDGE('',*,*,#22905,.T.);
#30270=ORIENTED_EDGE('',*,*,#22908,.T.);
#30271=ORIENTED_EDGE('',*,*,#22899,.F.);
#30272=ORIENTED_EDGE('',*,*,#22909,.T.);
#30273=ORIENTED_EDGE('',*,*,#22910,.F.);
#30274=ORIENTED_EDGE('',*,*,#22911,.T.);
#30275=ORIENTED_EDGE('',*,*,#22902,.F.);
#30276=ORIENTED_EDGE('',*,*,#22912,.T.);
#30277=ORIENTED_EDGE('',*,*,#22913,.T.);
#30278=ORIENTED_EDGE('',*,*,#22914,.T.);
#30279=ORIENTED_EDGE('',*,*,#22910,.T.);
#30280=ORIENTED_EDGE('',*,*,#22915,.T.);
#30281=ORIENTED_EDGE('',*,*,#22916,.T.);
#30282=ORIENTED_EDGE('',*,*,#22917,.T.);
#30283=ORIENTED_EDGE('',*,*,#22918,.T.);
#30284=ORIENTED_EDGE('',*,*,#22919,.F.);
#30285=ORIENTED_EDGE('',*,*,#22920,.T.);
#30286=ORIENTED_EDGE('',*,*,#22921,.T.);
#30287=ORIENTED_EDGE('',*,*,#22919,.T.);
#30288=ORIENTED_EDGE('',*,*,#22922,.T.);
#30289=ORIENTED_EDGE('',*,*,#22913,.F.);
#30290=ORIENTED_EDGE('',*,*,#22923,.T.);
#30291=ORIENTED_EDGE('',*,*,#21688,.F.);
#30292=ORIENTED_EDGE('',*,*,#22924,.T.);
#30293=ORIENTED_EDGE('',*,*,#22916,.F.);
#30294=ORIENTED_EDGE('',*,*,#22925,.T.);
#30295=ORIENTED_EDGE('',*,*,#21685,.F.);
#30296=ORIENTED_EDGE('',*,*,#22926,.T.);
#30297=ORIENTED_EDGE('',*,*,#22927,.T.);
#30298=ORIENTED_EDGE('',*,*,#22928,.F.);
#30299=ORIENTED_EDGE('',*,*,#22928,.T.);
#30300=ORIENTED_EDGE('',*,*,#22929,.T.);
#30301=ORIENTED_EDGE('',*,*,#21686,.F.);
#30302=ORIENTED_EDGE('',*,*,#22930,.T.);
#30303=ORIENTED_EDGE('',*,*,#22931,.T.);
#30304=ORIENTED_EDGE('',*,*,#21427,.F.);
#30305=ORIENTED_EDGE('',*,*,#22932,.F.);
#30306=ORIENTED_EDGE('',*,*,#22933,.T.);
#30307=ORIENTED_EDGE('',*,*,#22934,.T.);
#30308=ORIENTED_EDGE('',*,*,#22935,.F.);
#30309=ORIENTED_EDGE('',*,*,#22936,.T.);
#30310=ORIENTED_EDGE('',*,*,#22930,.F.);
#30311=ORIENTED_EDGE('',*,*,#22937,.T.);
#30312=ORIENTED_EDGE('',*,*,#22938,.T.);
#30313=ORIENTED_EDGE('',*,*,#22939,.T.);
#30314=ORIENTED_EDGE('',*,*,#22935,.T.);
#30315=ORIENTED_EDGE('',*,*,#22940,.T.);
#30316=ORIENTED_EDGE('',*,*,#22941,.T.);
#30317=ORIENTED_EDGE('',*,*,#22942,.T.);
#30318=ORIENTED_EDGE('',*,*,#22943,.T.);
#30319=ORIENTED_EDGE('',*,*,#22944,.F.);
#30320=ORIENTED_EDGE('',*,*,#22945,.T.);
#30321=ORIENTED_EDGE('',*,*,#22946,.T.);
#30322=ORIENTED_EDGE('',*,*,#22944,.T.);
#30323=ORIENTED_EDGE('',*,*,#22947,.T.);
#30324=ORIENTED_EDGE('',*,*,#22938,.F.);
#30325=ORIENTED_EDGE('',*,*,#22948,.T.);
#30326=ORIENTED_EDGE('',*,*,#21430,.F.);
#30327=ORIENTED_EDGE('',*,*,#22949,.T.);
#30328=ORIENTED_EDGE('',*,*,#22836,.T.);
#30329=ORIENTED_EDGE('',*,*,#22950,.F.);
#30330=ORIENTED_EDGE('',*,*,#22951,.T.);
#30331=ORIENTED_EDGE('',*,*,#22941,.F.);
#30332=ORIENTED_EDGE('',*,*,#22952,.T.);
#30333=ORIENTED_EDGE('',*,*,#22953,.T.);
#30334=ORIENTED_EDGE('',*,*,#22954,.T.);
#30335=ORIENTED_EDGE('',*,*,#22950,.T.);
#30336=ORIENTED_EDGE('',*,*,#22955,.T.);
#30337=ORIENTED_EDGE('',*,*,#22956,.T.);
#30338=ORIENTED_EDGE('',*,*,#22957,.T.);
#30339=ORIENTED_EDGE('',*,*,#22958,.T.);
#30340=ORIENTED_EDGE('',*,*,#22959,.F.);
#30341=ORIENTED_EDGE('',*,*,#22960,.T.);
#30342=ORIENTED_EDGE('',*,*,#22961,.T.);
#30343=ORIENTED_EDGE('',*,*,#22959,.T.);
#30344=ORIENTED_EDGE('',*,*,#22962,.T.);
#30345=ORIENTED_EDGE('',*,*,#22953,.F.);
#30346=ORIENTED_EDGE('',*,*,#22963,.T.);
#30347=ORIENTED_EDGE('',*,*,#22964,.F.);
#30348=ORIENTED_EDGE('',*,*,#22965,.T.);
#30349=ORIENTED_EDGE('',*,*,#22956,.F.);
#30350=ORIENTED_EDGE('',*,*,#22966,.T.);
#30351=ORIENTED_EDGE('',*,*,#22967,.T.);
#30352=ORIENTED_EDGE('',*,*,#22968,.T.);
#30353=ORIENTED_EDGE('',*,*,#22964,.T.);
#30354=ORIENTED_EDGE('',*,*,#22969,.T.);
#30355=ORIENTED_EDGE('',*,*,#22970,.T.);
#30356=ORIENTED_EDGE('',*,*,#22971,.T.);
#30357=ORIENTED_EDGE('',*,*,#22972,.T.);
#30358=ORIENTED_EDGE('',*,*,#22973,.F.);
#30359=ORIENTED_EDGE('',*,*,#22974,.T.);
#30360=ORIENTED_EDGE('',*,*,#22975,.T.);
#30361=ORIENTED_EDGE('',*,*,#22973,.T.);
#30362=ORIENTED_EDGE('',*,*,#22976,.T.);
#30363=ORIENTED_EDGE('',*,*,#22967,.F.);
#30364=ORIENTED_EDGE('',*,*,#22977,.T.);
#30365=ORIENTED_EDGE('',*,*,#22978,.F.);
#30366=ORIENTED_EDGE('',*,*,#22979,.T.);
#30367=ORIENTED_EDGE('',*,*,#22970,.F.);
#30368=ORIENTED_EDGE('',*,*,#22980,.T.);
#30369=ORIENTED_EDGE('',*,*,#22981,.T.);
#30370=ORIENTED_EDGE('',*,*,#22982,.T.);
#30371=ORIENTED_EDGE('',*,*,#22978,.T.);
#30372=ORIENTED_EDGE('',*,*,#22983,.T.);
#30373=ORIENTED_EDGE('',*,*,#22984,.T.);
#30374=ORIENTED_EDGE('',*,*,#22985,.T.);
#30375=ORIENTED_EDGE('',*,*,#22986,.T.);
#30376=ORIENTED_EDGE('',*,*,#22987,.F.);
#30377=ORIENTED_EDGE('',*,*,#22988,.T.);
#30378=ORIENTED_EDGE('',*,*,#22989,.T.);
#30379=ORIENTED_EDGE('',*,*,#22987,.T.);
#30380=ORIENTED_EDGE('',*,*,#22990,.T.);
#30381=ORIENTED_EDGE('',*,*,#22981,.F.);
#30382=ORIENTED_EDGE('',*,*,#22991,.T.);
#30383=ORIENTED_EDGE('',*,*,#22992,.F.);
#30384=ORIENTED_EDGE('',*,*,#22993,.T.);
#30385=ORIENTED_EDGE('',*,*,#22984,.F.);
#30386=ORIENTED_EDGE('',*,*,#22994,.T.);
#30387=ORIENTED_EDGE('',*,*,#22995,.T.);
#30388=ORIENTED_EDGE('',*,*,#22996,.T.);
#30389=ORIENTED_EDGE('',*,*,#22992,.T.);
#30390=ORIENTED_EDGE('',*,*,#22997,.T.);
#30391=ORIENTED_EDGE('',*,*,#22998,.T.);
#30392=ORIENTED_EDGE('',*,*,#22999,.T.);
#30393=ORIENTED_EDGE('',*,*,#23000,.T.);
#30394=ORIENTED_EDGE('',*,*,#23001,.F.);
#30395=ORIENTED_EDGE('',*,*,#23002,.T.);
#30396=ORIENTED_EDGE('',*,*,#23003,.T.);
#30397=ORIENTED_EDGE('',*,*,#23001,.T.);
#30398=ORIENTED_EDGE('',*,*,#23004,.T.);
#30399=ORIENTED_EDGE('',*,*,#22995,.F.);
#30400=ORIENTED_EDGE('',*,*,#23005,.T.);
#30401=ORIENTED_EDGE('',*,*,#23006,.F.);
#30402=ORIENTED_EDGE('',*,*,#23007,.T.);
#30403=ORIENTED_EDGE('',*,*,#22998,.F.);
#30404=ORIENTED_EDGE('',*,*,#23008,.T.);
#30405=ORIENTED_EDGE('',*,*,#23009,.T.);
#30406=ORIENTED_EDGE('',*,*,#23010,.T.);
#30407=ORIENTED_EDGE('',*,*,#23006,.T.);
#30408=ORIENTED_EDGE('',*,*,#23011,.T.);
#30409=ORIENTED_EDGE('',*,*,#23012,.T.);
#30410=ORIENTED_EDGE('',*,*,#23013,.T.);
#30411=ORIENTED_EDGE('',*,*,#23014,.T.);
#30412=ORIENTED_EDGE('',*,*,#23015,.F.);
#30413=ORIENTED_EDGE('',*,*,#23016,.T.);
#30414=ORIENTED_EDGE('',*,*,#23017,.T.);
#30415=ORIENTED_EDGE('',*,*,#23015,.T.);
#30416=ORIENTED_EDGE('',*,*,#23018,.T.);
#30417=ORIENTED_EDGE('',*,*,#23009,.F.);
#30418=ORIENTED_EDGE('',*,*,#23019,.T.);
#30419=ORIENTED_EDGE('',*,*,#21694,.F.);
#30420=ORIENTED_EDGE('',*,*,#23020,.T.);
#30421=ORIENTED_EDGE('',*,*,#23012,.F.);
#30422=ORIENTED_EDGE('',*,*,#23021,.T.);
#30423=ORIENTED_EDGE('',*,*,#21691,.F.);
#30424=ORIENTED_EDGE('',*,*,#23022,.T.);
#30425=ORIENTED_EDGE('',*,*,#23023,.T.);
#30426=ORIENTED_EDGE('',*,*,#23024,.F.);
#30427=ORIENTED_EDGE('',*,*,#23024,.T.);
#30428=ORIENTED_EDGE('',*,*,#23025,.T.);
#30429=ORIENTED_EDGE('',*,*,#21692,.F.);
#30430=ORIENTED_EDGE('',*,*,#23026,.T.);
#30431=ORIENTED_EDGE('',*,*,#23027,.T.);
#30432=ORIENTED_EDGE('',*,*,#21423,.F.);
#30433=ORIENTED_EDGE('',*,*,#23028,.F.);
#30434=ORIENTED_EDGE('',*,*,#23029,.T.);
#30435=ORIENTED_EDGE('',*,*,#23030,.T.);
#30436=ORIENTED_EDGE('',*,*,#23031,.F.);
#30437=ORIENTED_EDGE('',*,*,#23032,.T.);
#30438=ORIENTED_EDGE('',*,*,#23026,.F.);
#30439=ORIENTED_EDGE('',*,*,#23033,.T.);
#30440=ORIENTED_EDGE('',*,*,#23034,.T.);
#30441=ORIENTED_EDGE('',*,*,#23035,.T.);
#30442=ORIENTED_EDGE('',*,*,#23031,.T.);
#30443=ORIENTED_EDGE('',*,*,#23036,.T.);
#30444=ORIENTED_EDGE('',*,*,#23037,.T.);
#30445=ORIENTED_EDGE('',*,*,#23038,.T.);
#30446=ORIENTED_EDGE('',*,*,#23039,.T.);
#30447=ORIENTED_EDGE('',*,*,#23040,.F.);
#30448=ORIENTED_EDGE('',*,*,#23041,.T.);
#30449=ORIENTED_EDGE('',*,*,#23042,.T.);
#30450=ORIENTED_EDGE('',*,*,#23040,.T.);
#30451=ORIENTED_EDGE('',*,*,#23043,.T.);
#30452=ORIENTED_EDGE('',*,*,#23034,.F.);
#30453=ORIENTED_EDGE('',*,*,#23044,.T.);
#30454=ORIENTED_EDGE('',*,*,#21426,.F.);
#30455=ORIENTED_EDGE('',*,*,#23045,.T.);
#30456=ORIENTED_EDGE('',*,*,#22932,.T.);
#30457=ORIENTED_EDGE('',*,*,#23046,.F.);
#30458=ORIENTED_EDGE('',*,*,#23047,.T.);
#30459=ORIENTED_EDGE('',*,*,#23037,.F.);
#30460=ORIENTED_EDGE('',*,*,#23048,.T.);
#30461=ORIENTED_EDGE('',*,*,#23049,.T.);
#30462=ORIENTED_EDGE('',*,*,#23050,.T.);
#30463=ORIENTED_EDGE('',*,*,#23046,.T.);
#30464=ORIENTED_EDGE('',*,*,#23051,.T.);
#30465=ORIENTED_EDGE('',*,*,#23052,.T.);
#30466=ORIENTED_EDGE('',*,*,#23053,.T.);
#30467=ORIENTED_EDGE('',*,*,#23054,.T.);
#30468=ORIENTED_EDGE('',*,*,#23055,.F.);
#30469=ORIENTED_EDGE('',*,*,#23056,.T.);
#30470=ORIENTED_EDGE('',*,*,#23057,.T.);
#30471=ORIENTED_EDGE('',*,*,#23055,.T.);
#30472=ORIENTED_EDGE('',*,*,#23058,.T.);
#30473=ORIENTED_EDGE('',*,*,#23049,.F.);
#30474=ORIENTED_EDGE('',*,*,#23059,.T.);
#30475=ORIENTED_EDGE('',*,*,#23060,.F.);
#30476=ORIENTED_EDGE('',*,*,#23061,.T.);
#30477=ORIENTED_EDGE('',*,*,#23052,.F.);
#30478=ORIENTED_EDGE('',*,*,#23062,.T.);
#30479=ORIENTED_EDGE('',*,*,#23063,.T.);
#30480=ORIENTED_EDGE('',*,*,#23064,.T.);
#30481=ORIENTED_EDGE('',*,*,#23060,.T.);
#30482=ORIENTED_EDGE('',*,*,#23065,.T.);
#30483=ORIENTED_EDGE('',*,*,#23066,.T.);
#30484=ORIENTED_EDGE('',*,*,#23067,.T.);
#30485=ORIENTED_EDGE('',*,*,#23068,.T.);
#30486=ORIENTED_EDGE('',*,*,#23069,.F.);
#30487=ORIENTED_EDGE('',*,*,#23070,.T.);
#30488=ORIENTED_EDGE('',*,*,#23071,.T.);
#30489=ORIENTED_EDGE('',*,*,#23069,.T.);
#30490=ORIENTED_EDGE('',*,*,#23072,.T.);
#30491=ORIENTED_EDGE('',*,*,#23063,.F.);
#30492=ORIENTED_EDGE('',*,*,#23073,.T.);
#30493=ORIENTED_EDGE('',*,*,#23074,.F.);
#30494=ORIENTED_EDGE('',*,*,#23075,.T.);
#30495=ORIENTED_EDGE('',*,*,#23066,.F.);
#30496=ORIENTED_EDGE('',*,*,#23076,.T.);
#30497=ORIENTED_EDGE('',*,*,#23077,.T.);
#30498=ORIENTED_EDGE('',*,*,#23078,.T.);
#30499=ORIENTED_EDGE('',*,*,#23074,.T.);
#30500=ORIENTED_EDGE('',*,*,#23079,.T.);
#30501=ORIENTED_EDGE('',*,*,#23080,.T.);
#30502=ORIENTED_EDGE('',*,*,#23081,.T.);
#30503=ORIENTED_EDGE('',*,*,#23082,.T.);
#30504=ORIENTED_EDGE('',*,*,#23083,.F.);
#30505=ORIENTED_EDGE('',*,*,#23084,.T.);
#30506=ORIENTED_EDGE('',*,*,#23085,.T.);
#30507=ORIENTED_EDGE('',*,*,#23083,.T.);
#30508=ORIENTED_EDGE('',*,*,#23086,.T.);
#30509=ORIENTED_EDGE('',*,*,#23077,.F.);
#30510=ORIENTED_EDGE('',*,*,#23087,.T.);
#30511=ORIENTED_EDGE('',*,*,#23088,.F.);
#30512=ORIENTED_EDGE('',*,*,#23089,.T.);
#30513=ORIENTED_EDGE('',*,*,#23080,.F.);
#30514=ORIENTED_EDGE('',*,*,#23090,.T.);
#30515=ORIENTED_EDGE('',*,*,#23091,.T.);
#30516=ORIENTED_EDGE('',*,*,#23092,.T.);
#30517=ORIENTED_EDGE('',*,*,#23088,.T.);
#30518=ORIENTED_EDGE('',*,*,#23093,.T.);
#30519=ORIENTED_EDGE('',*,*,#23094,.T.);
#30520=ORIENTED_EDGE('',*,*,#23095,.T.);
#30521=ORIENTED_EDGE('',*,*,#23096,.T.);
#30522=ORIENTED_EDGE('',*,*,#23097,.F.);
#30523=ORIENTED_EDGE('',*,*,#23098,.T.);
#30524=ORIENTED_EDGE('',*,*,#23099,.T.);
#30525=ORIENTED_EDGE('',*,*,#23097,.T.);
#30526=ORIENTED_EDGE('',*,*,#23100,.T.);
#30527=ORIENTED_EDGE('',*,*,#23091,.F.);
#30528=ORIENTED_EDGE('',*,*,#23101,.T.);
#30529=ORIENTED_EDGE('',*,*,#23102,.F.);
#30530=ORIENTED_EDGE('',*,*,#23103,.T.);
#30531=ORIENTED_EDGE('',*,*,#23094,.F.);
#30532=ORIENTED_EDGE('',*,*,#23104,.T.);
#30533=ORIENTED_EDGE('',*,*,#23105,.T.);
#30534=ORIENTED_EDGE('',*,*,#23106,.T.);
#30535=ORIENTED_EDGE('',*,*,#23102,.T.);
#30536=ORIENTED_EDGE('',*,*,#23107,.T.);
#30537=ORIENTED_EDGE('',*,*,#23108,.T.);
#30538=ORIENTED_EDGE('',*,*,#23109,.T.);
#30539=ORIENTED_EDGE('',*,*,#23110,.T.);
#30540=ORIENTED_EDGE('',*,*,#23111,.F.);
#30541=ORIENTED_EDGE('',*,*,#23112,.T.);
#30542=ORIENTED_EDGE('',*,*,#23113,.T.);
#30543=ORIENTED_EDGE('',*,*,#23111,.T.);
#30544=ORIENTED_EDGE('',*,*,#23114,.T.);
#30545=ORIENTED_EDGE('',*,*,#23105,.F.);
#30546=ORIENTED_EDGE('',*,*,#23115,.T.);
#30547=ORIENTED_EDGE('',*,*,#21700,.F.);
#30548=ORIENTED_EDGE('',*,*,#23116,.T.);
#30549=ORIENTED_EDGE('',*,*,#23108,.F.);
#30550=ORIENTED_EDGE('',*,*,#23117,.T.);
#30551=ORIENTED_EDGE('',*,*,#21697,.F.);
#30552=ORIENTED_EDGE('',*,*,#23118,.T.);
#30553=ORIENTED_EDGE('',*,*,#23119,.T.);
#30554=ORIENTED_EDGE('',*,*,#23120,.F.);
#30555=ORIENTED_EDGE('',*,*,#23120,.T.);
#30556=ORIENTED_EDGE('',*,*,#23121,.T.);
#30557=ORIENTED_EDGE('',*,*,#21698,.F.);
#30558=ORIENTED_EDGE('',*,*,#23122,.T.);
#30559=ORIENTED_EDGE('',*,*,#23123,.T.);
#30560=ORIENTED_EDGE('',*,*,#21419,.F.);
#30561=ORIENTED_EDGE('',*,*,#23124,.F.);
#30562=ORIENTED_EDGE('',*,*,#23125,.T.);
#30563=ORIENTED_EDGE('',*,*,#23126,.T.);
#30564=ORIENTED_EDGE('',*,*,#23127,.F.);
#30565=ORIENTED_EDGE('',*,*,#23128,.T.);
#30566=ORIENTED_EDGE('',*,*,#23122,.F.);
#30567=ORIENTED_EDGE('',*,*,#23129,.T.);
#30568=ORIENTED_EDGE('',*,*,#23130,.T.);
#30569=ORIENTED_EDGE('',*,*,#23131,.T.);
#30570=ORIENTED_EDGE('',*,*,#23127,.T.);
#30571=ORIENTED_EDGE('',*,*,#23132,.T.);
#30572=ORIENTED_EDGE('',*,*,#23133,.T.);
#30573=ORIENTED_EDGE('',*,*,#23134,.T.);
#30574=ORIENTED_EDGE('',*,*,#23135,.T.);
#30575=ORIENTED_EDGE('',*,*,#23136,.F.);
#30576=ORIENTED_EDGE('',*,*,#23137,.T.);
#30577=ORIENTED_EDGE('',*,*,#23138,.T.);
#30578=ORIENTED_EDGE('',*,*,#23136,.T.);
#30579=ORIENTED_EDGE('',*,*,#23139,.T.);
#30580=ORIENTED_EDGE('',*,*,#23130,.F.);
#30581=ORIENTED_EDGE('',*,*,#23140,.T.);
#30582=ORIENTED_EDGE('',*,*,#21422,.F.);
#30583=ORIENTED_EDGE('',*,*,#23141,.T.);
#30584=ORIENTED_EDGE('',*,*,#23028,.T.);
#30585=ORIENTED_EDGE('',*,*,#23142,.F.);
#30586=ORIENTED_EDGE('',*,*,#23143,.T.);
#30587=ORIENTED_EDGE('',*,*,#23133,.F.);
#30588=ORIENTED_EDGE('',*,*,#23144,.T.);
#30589=ORIENTED_EDGE('',*,*,#23145,.T.);
#30590=ORIENTED_EDGE('',*,*,#23146,.T.);
#30591=ORIENTED_EDGE('',*,*,#23142,.T.);
#30592=ORIENTED_EDGE('',*,*,#23147,.T.);
#30593=ORIENTED_EDGE('',*,*,#23148,.T.);
#30594=ORIENTED_EDGE('',*,*,#23149,.T.);
#30595=ORIENTED_EDGE('',*,*,#23150,.T.);
#30596=ORIENTED_EDGE('',*,*,#23151,.F.);
#30597=ORIENTED_EDGE('',*,*,#23152,.T.);
#30598=ORIENTED_EDGE('',*,*,#23153,.T.);
#30599=ORIENTED_EDGE('',*,*,#23151,.T.);
#30600=ORIENTED_EDGE('',*,*,#23154,.T.);
#30601=ORIENTED_EDGE('',*,*,#23145,.F.);
#30602=ORIENTED_EDGE('',*,*,#23155,.T.);
#30603=ORIENTED_EDGE('',*,*,#23156,.F.);
#30604=ORIENTED_EDGE('',*,*,#23157,.T.);
#30605=ORIENTED_EDGE('',*,*,#23148,.F.);
#30606=ORIENTED_EDGE('',*,*,#23158,.T.);
#30607=ORIENTED_EDGE('',*,*,#23159,.T.);
#30608=ORIENTED_EDGE('',*,*,#23160,.T.);
#30609=ORIENTED_EDGE('',*,*,#23156,.T.);
#30610=ORIENTED_EDGE('',*,*,#23161,.T.);
#30611=ORIENTED_EDGE('',*,*,#23162,.T.);
#30612=ORIENTED_EDGE('',*,*,#23163,.T.);
#30613=ORIENTED_EDGE('',*,*,#23164,.T.);
#30614=ORIENTED_EDGE('',*,*,#23165,.F.);
#30615=ORIENTED_EDGE('',*,*,#23166,.T.);
#30616=ORIENTED_EDGE('',*,*,#23167,.T.);
#30617=ORIENTED_EDGE('',*,*,#23165,.T.);
#30618=ORIENTED_EDGE('',*,*,#23168,.T.);
#30619=ORIENTED_EDGE('',*,*,#23159,.F.);
#30620=ORIENTED_EDGE('',*,*,#23169,.T.);
#30621=ORIENTED_EDGE('',*,*,#23170,.F.);
#30622=ORIENTED_EDGE('',*,*,#23171,.T.);
#30623=ORIENTED_EDGE('',*,*,#23162,.F.);
#30624=ORIENTED_EDGE('',*,*,#23172,.T.);
#30625=ORIENTED_EDGE('',*,*,#23173,.T.);
#30626=ORIENTED_EDGE('',*,*,#23174,.T.);
#30627=ORIENTED_EDGE('',*,*,#23170,.T.);
#30628=ORIENTED_EDGE('',*,*,#23175,.T.);
#30629=ORIENTED_EDGE('',*,*,#23176,.T.);
#30630=ORIENTED_EDGE('',*,*,#23177,.T.);
#30631=ORIENTED_EDGE('',*,*,#23178,.T.);
#30632=ORIENTED_EDGE('',*,*,#23179,.F.);
#30633=ORIENTED_EDGE('',*,*,#23180,.T.);
#30634=ORIENTED_EDGE('',*,*,#23181,.T.);
#30635=ORIENTED_EDGE('',*,*,#23179,.T.);
#30636=ORIENTED_EDGE('',*,*,#23182,.T.);
#30637=ORIENTED_EDGE('',*,*,#23173,.F.);
#30638=ORIENTED_EDGE('',*,*,#23183,.T.);
#30639=ORIENTED_EDGE('',*,*,#23184,.F.);
#30640=ORIENTED_EDGE('',*,*,#23185,.T.);
#30641=ORIENTED_EDGE('',*,*,#23176,.F.);
#30642=ORIENTED_EDGE('',*,*,#23186,.T.);
#30643=ORIENTED_EDGE('',*,*,#23187,.T.);
#30644=ORIENTED_EDGE('',*,*,#23188,.T.);
#30645=ORIENTED_EDGE('',*,*,#23184,.T.);
#30646=ORIENTED_EDGE('',*,*,#23189,.T.);
#30647=ORIENTED_EDGE('',*,*,#23190,.T.);
#30648=ORIENTED_EDGE('',*,*,#23191,.T.);
#30649=ORIENTED_EDGE('',*,*,#23192,.T.);
#30650=ORIENTED_EDGE('',*,*,#23193,.F.);
#30651=ORIENTED_EDGE('',*,*,#23194,.T.);
#30652=ORIENTED_EDGE('',*,*,#23195,.T.);
#30653=ORIENTED_EDGE('',*,*,#23193,.T.);
#30654=ORIENTED_EDGE('',*,*,#23196,.T.);
#30655=ORIENTED_EDGE('',*,*,#23187,.F.);
#30656=ORIENTED_EDGE('',*,*,#23197,.T.);
#30657=ORIENTED_EDGE('',*,*,#23198,.F.);
#30658=ORIENTED_EDGE('',*,*,#23199,.T.);
#30659=ORIENTED_EDGE('',*,*,#23190,.F.);
#30660=ORIENTED_EDGE('',*,*,#23200,.T.);
#30661=ORIENTED_EDGE('',*,*,#23201,.T.);
#30662=ORIENTED_EDGE('',*,*,#23202,.T.);
#30663=ORIENTED_EDGE('',*,*,#23198,.T.);
#30664=ORIENTED_EDGE('',*,*,#23203,.T.);
#30665=ORIENTED_EDGE('',*,*,#23204,.T.);
#30666=ORIENTED_EDGE('',*,*,#23205,.T.);
#30667=ORIENTED_EDGE('',*,*,#23206,.T.);
#30668=ORIENTED_EDGE('',*,*,#23207,.F.);
#30669=ORIENTED_EDGE('',*,*,#23208,.T.);
#30670=ORIENTED_EDGE('',*,*,#23209,.T.);
#30671=ORIENTED_EDGE('',*,*,#23207,.T.);
#30672=ORIENTED_EDGE('',*,*,#23210,.T.);
#30673=ORIENTED_EDGE('',*,*,#23201,.F.);
#30674=ORIENTED_EDGE('',*,*,#23211,.T.);
#30675=ORIENTED_EDGE('',*,*,#21706,.F.);
#30676=ORIENTED_EDGE('',*,*,#23212,.T.);
#30677=ORIENTED_EDGE('',*,*,#23204,.F.);
#30678=ORIENTED_EDGE('',*,*,#23213,.T.);
#30679=ORIENTED_EDGE('',*,*,#21703,.F.);
#30680=ORIENTED_EDGE('',*,*,#23214,.T.);
#30681=ORIENTED_EDGE('',*,*,#23215,.T.);
#30682=ORIENTED_EDGE('',*,*,#23216,.F.);
#30683=ORIENTED_EDGE('',*,*,#23216,.T.);
#30684=ORIENTED_EDGE('',*,*,#23217,.T.);
#30685=ORIENTED_EDGE('',*,*,#21704,.F.);
#30686=ORIENTED_EDGE('',*,*,#23218,.T.);
#30687=ORIENTED_EDGE('',*,*,#23219,.T.);
#30688=ORIENTED_EDGE('',*,*,#21415,.F.);
#30689=ORIENTED_EDGE('',*,*,#23220,.F.);
#30690=ORIENTED_EDGE('',*,*,#23221,.T.);
#30691=ORIENTED_EDGE('',*,*,#23222,.T.);
#30692=ORIENTED_EDGE('',*,*,#23223,.F.);
#30693=ORIENTED_EDGE('',*,*,#23224,.T.);
#30694=ORIENTED_EDGE('',*,*,#23218,.F.);
#30695=ORIENTED_EDGE('',*,*,#23225,.T.);
#30696=ORIENTED_EDGE('',*,*,#23226,.T.);
#30697=ORIENTED_EDGE('',*,*,#23227,.T.);
#30698=ORIENTED_EDGE('',*,*,#23223,.T.);
#30699=ORIENTED_EDGE('',*,*,#23228,.T.);
#30700=ORIENTED_EDGE('',*,*,#23229,.T.);
#30701=ORIENTED_EDGE('',*,*,#23230,.T.);
#30702=ORIENTED_EDGE('',*,*,#23231,.T.);
#30703=ORIENTED_EDGE('',*,*,#23232,.F.);
#30704=ORIENTED_EDGE('',*,*,#23233,.T.);
#30705=ORIENTED_EDGE('',*,*,#23234,.T.);
#30706=ORIENTED_EDGE('',*,*,#23232,.T.);
#30707=ORIENTED_EDGE('',*,*,#23235,.T.);
#30708=ORIENTED_EDGE('',*,*,#23226,.F.);
#30709=ORIENTED_EDGE('',*,*,#23236,.T.);
#30710=ORIENTED_EDGE('',*,*,#21418,.F.);
#30711=ORIENTED_EDGE('',*,*,#23237,.T.);
#30712=ORIENTED_EDGE('',*,*,#23124,.T.);
#30713=ORIENTED_EDGE('',*,*,#23238,.F.);
#30714=ORIENTED_EDGE('',*,*,#23239,.T.);
#30715=ORIENTED_EDGE('',*,*,#23229,.F.);
#30716=ORIENTED_EDGE('',*,*,#23240,.T.);
#30717=ORIENTED_EDGE('',*,*,#23241,.T.);
#30718=ORIENTED_EDGE('',*,*,#23242,.T.);
#30719=ORIENTED_EDGE('',*,*,#23238,.T.);
#30720=ORIENTED_EDGE('',*,*,#23243,.T.);
#30721=ORIENTED_EDGE('',*,*,#23244,.T.);
#30722=ORIENTED_EDGE('',*,*,#23245,.T.);
#30723=ORIENTED_EDGE('',*,*,#23246,.T.);
#30724=ORIENTED_EDGE('',*,*,#23247,.F.);
#30725=ORIENTED_EDGE('',*,*,#23248,.T.);
#30726=ORIENTED_EDGE('',*,*,#23249,.T.);
#30727=ORIENTED_EDGE('',*,*,#23247,.T.);
#30728=ORIENTED_EDGE('',*,*,#23250,.T.);
#30729=ORIENTED_EDGE('',*,*,#23241,.F.);
#30730=ORIENTED_EDGE('',*,*,#23251,.T.);
#30731=ORIENTED_EDGE('',*,*,#23252,.F.);
#30732=ORIENTED_EDGE('',*,*,#23253,.T.);
#30733=ORIENTED_EDGE('',*,*,#23244,.F.);
#30734=ORIENTED_EDGE('',*,*,#23254,.T.);
#30735=ORIENTED_EDGE('',*,*,#23255,.T.);
#30736=ORIENTED_EDGE('',*,*,#23256,.T.);
#30737=ORIENTED_EDGE('',*,*,#23252,.T.);
#30738=ORIENTED_EDGE('',*,*,#23257,.T.);
#30739=ORIENTED_EDGE('',*,*,#23258,.T.);
#30740=ORIENTED_EDGE('',*,*,#23259,.T.);
#30741=ORIENTED_EDGE('',*,*,#23260,.T.);
#30742=ORIENTED_EDGE('',*,*,#23261,.F.);
#30743=ORIENTED_EDGE('',*,*,#23262,.T.);
#30744=ORIENTED_EDGE('',*,*,#23263,.T.);
#30745=ORIENTED_EDGE('',*,*,#23261,.T.);
#30746=ORIENTED_EDGE('',*,*,#23264,.T.);
#30747=ORIENTED_EDGE('',*,*,#23255,.F.);
#30748=ORIENTED_EDGE('',*,*,#23265,.T.);
#30749=ORIENTED_EDGE('',*,*,#23266,.F.);
#30750=ORIENTED_EDGE('',*,*,#23267,.T.);
#30751=ORIENTED_EDGE('',*,*,#23258,.F.);
#30752=ORIENTED_EDGE('',*,*,#23268,.T.);
#30753=ORIENTED_EDGE('',*,*,#23269,.T.);
#30754=ORIENTED_EDGE('',*,*,#23270,.T.);
#30755=ORIENTED_EDGE('',*,*,#23266,.T.);
#30756=ORIENTED_EDGE('',*,*,#23271,.T.);
#30757=ORIENTED_EDGE('',*,*,#23272,.T.);
#30758=ORIENTED_EDGE('',*,*,#23273,.T.);
#30759=ORIENTED_EDGE('',*,*,#23274,.T.);
#30760=ORIENTED_EDGE('',*,*,#23275,.F.);
#30761=ORIENTED_EDGE('',*,*,#23276,.T.);
#30762=ORIENTED_EDGE('',*,*,#23277,.T.);
#30763=ORIENTED_EDGE('',*,*,#23275,.T.);
#30764=ORIENTED_EDGE('',*,*,#23278,.T.);
#30765=ORIENTED_EDGE('',*,*,#23269,.F.);
#30766=ORIENTED_EDGE('',*,*,#23279,.T.);
#30767=ORIENTED_EDGE('',*,*,#23280,.F.);
#30768=ORIENTED_EDGE('',*,*,#23281,.T.);
#30769=ORIENTED_EDGE('',*,*,#23272,.F.);
#30770=ORIENTED_EDGE('',*,*,#23282,.T.);
#30771=ORIENTED_EDGE('',*,*,#23283,.T.);
#30772=ORIENTED_EDGE('',*,*,#23284,.T.);
#30773=ORIENTED_EDGE('',*,*,#23280,.T.);
#30774=ORIENTED_EDGE('',*,*,#23285,.T.);
#30775=ORIENTED_EDGE('',*,*,#23286,.T.);
#30776=ORIENTED_EDGE('',*,*,#23287,.T.);
#30777=ORIENTED_EDGE('',*,*,#23288,.T.);
#30778=ORIENTED_EDGE('',*,*,#23289,.F.);
#30779=ORIENTED_EDGE('',*,*,#23290,.T.);
#30780=ORIENTED_EDGE('',*,*,#23291,.T.);
#30781=ORIENTED_EDGE('',*,*,#23289,.T.);
#30782=ORIENTED_EDGE('',*,*,#23292,.T.);
#30783=ORIENTED_EDGE('',*,*,#23283,.F.);
#30784=ORIENTED_EDGE('',*,*,#23293,.T.);
#30785=ORIENTED_EDGE('',*,*,#23294,.F.);
#30786=ORIENTED_EDGE('',*,*,#23295,.T.);
#30787=ORIENTED_EDGE('',*,*,#23286,.F.);
#30788=ORIENTED_EDGE('',*,*,#23296,.T.);
#30789=ORIENTED_EDGE('',*,*,#23297,.T.);
#30790=ORIENTED_EDGE('',*,*,#23298,.T.);
#30791=ORIENTED_EDGE('',*,*,#23294,.T.);
#30792=ORIENTED_EDGE('',*,*,#23299,.T.);
#30793=ORIENTED_EDGE('',*,*,#23300,.T.);
#30794=ORIENTED_EDGE('',*,*,#23301,.T.);
#30795=ORIENTED_EDGE('',*,*,#23302,.T.);
#30796=ORIENTED_EDGE('',*,*,#23303,.F.);
#30797=ORIENTED_EDGE('',*,*,#23304,.T.);
#30798=ORIENTED_EDGE('',*,*,#23305,.T.);
#30799=ORIENTED_EDGE('',*,*,#23303,.T.);
#30800=ORIENTED_EDGE('',*,*,#23306,.T.);
#30801=ORIENTED_EDGE('',*,*,#23297,.F.);
#30802=ORIENTED_EDGE('',*,*,#23307,.T.);
#30803=ORIENTED_EDGE('',*,*,#21712,.F.);
#30804=ORIENTED_EDGE('',*,*,#23308,.T.);
#30805=ORIENTED_EDGE('',*,*,#23300,.F.);
#30806=ORIENTED_EDGE('',*,*,#23309,.T.);
#30807=ORIENTED_EDGE('',*,*,#21709,.F.);
#30808=ORIENTED_EDGE('',*,*,#23310,.T.);
#30809=ORIENTED_EDGE('',*,*,#23311,.T.);
#30810=ORIENTED_EDGE('',*,*,#23312,.F.);
#30811=ORIENTED_EDGE('',*,*,#23312,.T.);
#30812=ORIENTED_EDGE('',*,*,#23313,.T.);
#30813=ORIENTED_EDGE('',*,*,#21710,.F.);
#30814=ORIENTED_EDGE('',*,*,#23314,.T.);
#30815=ORIENTED_EDGE('',*,*,#23315,.T.);
#30816=ORIENTED_EDGE('',*,*,#21411,.F.);
#30817=ORIENTED_EDGE('',*,*,#23316,.F.);
#30818=ORIENTED_EDGE('',*,*,#23317,.T.);
#30819=ORIENTED_EDGE('',*,*,#23318,.T.);
#30820=ORIENTED_EDGE('',*,*,#23319,.F.);
#30821=ORIENTED_EDGE('',*,*,#23320,.T.);
#30822=ORIENTED_EDGE('',*,*,#23314,.F.);
#30823=ORIENTED_EDGE('',*,*,#23321,.T.);
#30824=ORIENTED_EDGE('',*,*,#23322,.T.);
#30825=ORIENTED_EDGE('',*,*,#23323,.T.);
#30826=ORIENTED_EDGE('',*,*,#23319,.T.);
#30827=ORIENTED_EDGE('',*,*,#23324,.T.);
#30828=ORIENTED_EDGE('',*,*,#23325,.T.);
#30829=ORIENTED_EDGE('',*,*,#23326,.T.);
#30830=ORIENTED_EDGE('',*,*,#23327,.T.);
#30831=ORIENTED_EDGE('',*,*,#23328,.F.);
#30832=ORIENTED_EDGE('',*,*,#23329,.T.);
#30833=ORIENTED_EDGE('',*,*,#23330,.T.);
#30834=ORIENTED_EDGE('',*,*,#23328,.T.);
#30835=ORIENTED_EDGE('',*,*,#23331,.T.);
#30836=ORIENTED_EDGE('',*,*,#23322,.F.);
#30837=ORIENTED_EDGE('',*,*,#23332,.T.);
#30838=ORIENTED_EDGE('',*,*,#21414,.F.);
#30839=ORIENTED_EDGE('',*,*,#23333,.T.);
#30840=ORIENTED_EDGE('',*,*,#23220,.T.);
#30841=ORIENTED_EDGE('',*,*,#23334,.F.);
#30842=ORIENTED_EDGE('',*,*,#23335,.T.);
#30843=ORIENTED_EDGE('',*,*,#23325,.F.);
#30844=ORIENTED_EDGE('',*,*,#23336,.T.);
#30845=ORIENTED_EDGE('',*,*,#23337,.T.);
#30846=ORIENTED_EDGE('',*,*,#23338,.T.);
#30847=ORIENTED_EDGE('',*,*,#23334,.T.);
#30848=ORIENTED_EDGE('',*,*,#23339,.T.);
#30849=ORIENTED_EDGE('',*,*,#23340,.T.);
#30850=ORIENTED_EDGE('',*,*,#23341,.T.);
#30851=ORIENTED_EDGE('',*,*,#23342,.T.);
#30852=ORIENTED_EDGE('',*,*,#23343,.F.);
#30853=ORIENTED_EDGE('',*,*,#23344,.T.);
#30854=ORIENTED_EDGE('',*,*,#23345,.T.);
#30855=ORIENTED_EDGE('',*,*,#23343,.T.);
#30856=ORIENTED_EDGE('',*,*,#23346,.T.);
#30857=ORIENTED_EDGE('',*,*,#23337,.F.);
#30858=ORIENTED_EDGE('',*,*,#23347,.T.);
#30859=ORIENTED_EDGE('',*,*,#23348,.F.);
#30860=ORIENTED_EDGE('',*,*,#23349,.T.);
#30861=ORIENTED_EDGE('',*,*,#23340,.F.);
#30862=ORIENTED_EDGE('',*,*,#23350,.T.);
#30863=ORIENTED_EDGE('',*,*,#23351,.T.);
#30864=ORIENTED_EDGE('',*,*,#23352,.T.);
#30865=ORIENTED_EDGE('',*,*,#23348,.T.);
#30866=ORIENTED_EDGE('',*,*,#23353,.T.);
#30867=ORIENTED_EDGE('',*,*,#23354,.T.);
#30868=ORIENTED_EDGE('',*,*,#23355,.T.);
#30869=ORIENTED_EDGE('',*,*,#23356,.T.);
#30870=ORIENTED_EDGE('',*,*,#23357,.F.);
#30871=ORIENTED_EDGE('',*,*,#23358,.T.);
#30872=ORIENTED_EDGE('',*,*,#23359,.T.);
#30873=ORIENTED_EDGE('',*,*,#23357,.T.);
#30874=ORIENTED_EDGE('',*,*,#23360,.T.);
#30875=ORIENTED_EDGE('',*,*,#23351,.F.);
#30876=ORIENTED_EDGE('',*,*,#23361,.T.);
#30877=ORIENTED_EDGE('',*,*,#23362,.F.);
#30878=ORIENTED_EDGE('',*,*,#23363,.T.);
#30879=ORIENTED_EDGE('',*,*,#23354,.F.);
#30880=ORIENTED_EDGE('',*,*,#23364,.T.);
#30881=ORIENTED_EDGE('',*,*,#23365,.T.);
#30882=ORIENTED_EDGE('',*,*,#23366,.T.);
#30883=ORIENTED_EDGE('',*,*,#23362,.T.);
#30884=ORIENTED_EDGE('',*,*,#23367,.T.);
#30885=ORIENTED_EDGE('',*,*,#23368,.T.);
#30886=ORIENTED_EDGE('',*,*,#23369,.T.);
#30887=ORIENTED_EDGE('',*,*,#23370,.T.);
#30888=ORIENTED_EDGE('',*,*,#23371,.F.);
#30889=ORIENTED_EDGE('',*,*,#23372,.T.);
#30890=ORIENTED_EDGE('',*,*,#23373,.T.);
#30891=ORIENTED_EDGE('',*,*,#23371,.T.);
#30892=ORIENTED_EDGE('',*,*,#23374,.T.);
#30893=ORIENTED_EDGE('',*,*,#23365,.F.);
#30894=ORIENTED_EDGE('',*,*,#23375,.T.);
#30895=ORIENTED_EDGE('',*,*,#23376,.F.);
#30896=ORIENTED_EDGE('',*,*,#23377,.T.);
#30897=ORIENTED_EDGE('',*,*,#23368,.F.);
#30898=ORIENTED_EDGE('',*,*,#23378,.T.);
#30899=ORIENTED_EDGE('',*,*,#23379,.T.);
#30900=ORIENTED_EDGE('',*,*,#23380,.T.);
#30901=ORIENTED_EDGE('',*,*,#23376,.T.);
#30902=ORIENTED_EDGE('',*,*,#23381,.T.);
#30903=ORIENTED_EDGE('',*,*,#23382,.T.);
#30904=ORIENTED_EDGE('',*,*,#23383,.T.);
#30905=ORIENTED_EDGE('',*,*,#23384,.T.);
#30906=ORIENTED_EDGE('',*,*,#23385,.F.);
#30907=ORIENTED_EDGE('',*,*,#23386,.T.);
#30908=ORIENTED_EDGE('',*,*,#23387,.T.);
#30909=ORIENTED_EDGE('',*,*,#23385,.T.);
#30910=ORIENTED_EDGE('',*,*,#23388,.T.);
#30911=ORIENTED_EDGE('',*,*,#23379,.F.);
#30912=ORIENTED_EDGE('',*,*,#23389,.T.);
#30913=ORIENTED_EDGE('',*,*,#23390,.F.);
#30914=ORIENTED_EDGE('',*,*,#23391,.T.);
#30915=ORIENTED_EDGE('',*,*,#23382,.F.);
#30916=ORIENTED_EDGE('',*,*,#23392,.T.);
#30917=ORIENTED_EDGE('',*,*,#23393,.T.);
#30918=ORIENTED_EDGE('',*,*,#23394,.T.);
#30919=ORIENTED_EDGE('',*,*,#23390,.T.);
#30920=ORIENTED_EDGE('',*,*,#23395,.T.);
#30921=ORIENTED_EDGE('',*,*,#23396,.T.);
#30922=ORIENTED_EDGE('',*,*,#23397,.T.);
#30923=ORIENTED_EDGE('',*,*,#23398,.T.);
#30924=ORIENTED_EDGE('',*,*,#23399,.F.);
#30925=ORIENTED_EDGE('',*,*,#23400,.T.);
#30926=ORIENTED_EDGE('',*,*,#23401,.T.);
#30927=ORIENTED_EDGE('',*,*,#23399,.T.);
#30928=ORIENTED_EDGE('',*,*,#23402,.T.);
#30929=ORIENTED_EDGE('',*,*,#23393,.F.);
#30930=ORIENTED_EDGE('',*,*,#23403,.T.);
#30931=ORIENTED_EDGE('',*,*,#21718,.F.);
#30932=ORIENTED_EDGE('',*,*,#23404,.T.);
#30933=ORIENTED_EDGE('',*,*,#23396,.F.);
#30934=ORIENTED_EDGE('',*,*,#23405,.T.);
#30935=ORIENTED_EDGE('',*,*,#21715,.F.);
#30936=ORIENTED_EDGE('',*,*,#23406,.T.);
#30937=ORIENTED_EDGE('',*,*,#23407,.T.);
#30938=ORIENTED_EDGE('',*,*,#23408,.F.);
#30939=ORIENTED_EDGE('',*,*,#23408,.T.);
#30940=ORIENTED_EDGE('',*,*,#23409,.T.);
#30941=ORIENTED_EDGE('',*,*,#21716,.F.);
#30942=ORIENTED_EDGE('',*,*,#23410,.T.);
#30943=ORIENTED_EDGE('',*,*,#23411,.T.);
#30944=ORIENTED_EDGE('',*,*,#21407,.F.);
#30945=ORIENTED_EDGE('',*,*,#23412,.F.);
#30946=ORIENTED_EDGE('',*,*,#23413,.T.);
#30947=ORIENTED_EDGE('',*,*,#23414,.T.);
#30948=ORIENTED_EDGE('',*,*,#23415,.F.);
#30949=ORIENTED_EDGE('',*,*,#23416,.T.);
#30950=ORIENTED_EDGE('',*,*,#23410,.F.);
#30951=ORIENTED_EDGE('',*,*,#23417,.T.);
#30952=ORIENTED_EDGE('',*,*,#23418,.T.);
#30953=ORIENTED_EDGE('',*,*,#23419,.T.);
#30954=ORIENTED_EDGE('',*,*,#23415,.T.);
#30955=ORIENTED_EDGE('',*,*,#23420,.T.);
#30956=ORIENTED_EDGE('',*,*,#23421,.T.);
#30957=ORIENTED_EDGE('',*,*,#23422,.T.);
#30958=ORIENTED_EDGE('',*,*,#23423,.T.);
#30959=ORIENTED_EDGE('',*,*,#23424,.F.);
#30960=ORIENTED_EDGE('',*,*,#23425,.T.);
#30961=ORIENTED_EDGE('',*,*,#23426,.T.);
#30962=ORIENTED_EDGE('',*,*,#23424,.T.);
#30963=ORIENTED_EDGE('',*,*,#23427,.T.);
#30964=ORIENTED_EDGE('',*,*,#23418,.F.);
#30965=ORIENTED_EDGE('',*,*,#23428,.T.);
#30966=ORIENTED_EDGE('',*,*,#21410,.F.);
#30967=ORIENTED_EDGE('',*,*,#23429,.T.);
#30968=ORIENTED_EDGE('',*,*,#23316,.T.);
#30969=ORIENTED_EDGE('',*,*,#23430,.F.);
#30970=ORIENTED_EDGE('',*,*,#23431,.T.);
#30971=ORIENTED_EDGE('',*,*,#23421,.F.);
#30972=ORIENTED_EDGE('',*,*,#23432,.T.);
#30973=ORIENTED_EDGE('',*,*,#23433,.T.);
#30974=ORIENTED_EDGE('',*,*,#23434,.T.);
#30975=ORIENTED_EDGE('',*,*,#23430,.T.);
#30976=ORIENTED_EDGE('',*,*,#23435,.T.);
#30977=ORIENTED_EDGE('',*,*,#23436,.T.);
#30978=ORIENTED_EDGE('',*,*,#23437,.T.);
#30979=ORIENTED_EDGE('',*,*,#23438,.T.);
#30980=ORIENTED_EDGE('',*,*,#23439,.F.);
#30981=ORIENTED_EDGE('',*,*,#23440,.T.);
#30982=ORIENTED_EDGE('',*,*,#23441,.T.);
#30983=ORIENTED_EDGE('',*,*,#23439,.T.);
#30984=ORIENTED_EDGE('',*,*,#23442,.T.);
#30985=ORIENTED_EDGE('',*,*,#23433,.F.);
#30986=ORIENTED_EDGE('',*,*,#23443,.T.);
#30987=ORIENTED_EDGE('',*,*,#23444,.F.);
#30988=ORIENTED_EDGE('',*,*,#23445,.T.);
#30989=ORIENTED_EDGE('',*,*,#23436,.F.);
#30990=ORIENTED_EDGE('',*,*,#23446,.T.);
#30991=ORIENTED_EDGE('',*,*,#23447,.T.);
#30992=ORIENTED_EDGE('',*,*,#23448,.T.);
#30993=ORIENTED_EDGE('',*,*,#23444,.T.);
#30994=ORIENTED_EDGE('',*,*,#23449,.T.);
#30995=ORIENTED_EDGE('',*,*,#23450,.T.);
#30996=ORIENTED_EDGE('',*,*,#23451,.T.);
#30997=ORIENTED_EDGE('',*,*,#23452,.T.);
#30998=ORIENTED_EDGE('',*,*,#23453,.F.);
#30999=ORIENTED_EDGE('',*,*,#23454,.T.);
#31000=ORIENTED_EDGE('',*,*,#23455,.T.);
#31001=ORIENTED_EDGE('',*,*,#23453,.T.);
#31002=ORIENTED_EDGE('',*,*,#23456,.T.);
#31003=ORIENTED_EDGE('',*,*,#23447,.F.);
#31004=ORIENTED_EDGE('',*,*,#23457,.T.);
#31005=ORIENTED_EDGE('',*,*,#23458,.F.);
#31006=ORIENTED_EDGE('',*,*,#23459,.T.);
#31007=ORIENTED_EDGE('',*,*,#23450,.F.);
#31008=ORIENTED_EDGE('',*,*,#23460,.T.);
#31009=ORIENTED_EDGE('',*,*,#23461,.T.);
#31010=ORIENTED_EDGE('',*,*,#23462,.T.);
#31011=ORIENTED_EDGE('',*,*,#23458,.T.);
#31012=ORIENTED_EDGE('',*,*,#23463,.T.);
#31013=ORIENTED_EDGE('',*,*,#23464,.T.);
#31014=ORIENTED_EDGE('',*,*,#23465,.T.);
#31015=ORIENTED_EDGE('',*,*,#23466,.T.);
#31016=ORIENTED_EDGE('',*,*,#23467,.F.);
#31017=ORIENTED_EDGE('',*,*,#23468,.T.);
#31018=ORIENTED_EDGE('',*,*,#23469,.T.);
#31019=ORIENTED_EDGE('',*,*,#23467,.T.);
#31020=ORIENTED_EDGE('',*,*,#23470,.T.);
#31021=ORIENTED_EDGE('',*,*,#23461,.F.);
#31022=ORIENTED_EDGE('',*,*,#23471,.T.);
#31023=ORIENTED_EDGE('',*,*,#23472,.F.);
#31024=ORIENTED_EDGE('',*,*,#23473,.T.);
#31025=ORIENTED_EDGE('',*,*,#23464,.F.);
#31026=ORIENTED_EDGE('',*,*,#23474,.T.);
#31027=ORIENTED_EDGE('',*,*,#23475,.T.);
#31028=ORIENTED_EDGE('',*,*,#23476,.T.);
#31029=ORIENTED_EDGE('',*,*,#23472,.T.);
#31030=ORIENTED_EDGE('',*,*,#23477,.T.);
#31031=ORIENTED_EDGE('',*,*,#23478,.T.);
#31032=ORIENTED_EDGE('',*,*,#23479,.T.);
#31033=ORIENTED_EDGE('',*,*,#23480,.T.);
#31034=ORIENTED_EDGE('',*,*,#23481,.F.);
#31035=ORIENTED_EDGE('',*,*,#23482,.T.);
#31036=ORIENTED_EDGE('',*,*,#23483,.T.);
#31037=ORIENTED_EDGE('',*,*,#23481,.T.);
#31038=ORIENTED_EDGE('',*,*,#23484,.T.);
#31039=ORIENTED_EDGE('',*,*,#23475,.F.);
#31040=ORIENTED_EDGE('',*,*,#23485,.T.);
#31041=ORIENTED_EDGE('',*,*,#23486,.F.);
#31042=ORIENTED_EDGE('',*,*,#23487,.T.);
#31043=ORIENTED_EDGE('',*,*,#23478,.F.);
#31044=ORIENTED_EDGE('',*,*,#23488,.T.);
#31045=ORIENTED_EDGE('',*,*,#23489,.T.);
#31046=ORIENTED_EDGE('',*,*,#23490,.T.);
#31047=ORIENTED_EDGE('',*,*,#23486,.T.);
#31048=ORIENTED_EDGE('',*,*,#23491,.T.);
#31049=ORIENTED_EDGE('',*,*,#23492,.T.);
#31050=ORIENTED_EDGE('',*,*,#23493,.T.);
#31051=ORIENTED_EDGE('',*,*,#23494,.T.);
#31052=ORIENTED_EDGE('',*,*,#23495,.F.);
#31053=ORIENTED_EDGE('',*,*,#23496,.T.);
#31054=ORIENTED_EDGE('',*,*,#23497,.T.);
#31055=ORIENTED_EDGE('',*,*,#23495,.T.);
#31056=ORIENTED_EDGE('',*,*,#23498,.T.);
#31057=ORIENTED_EDGE('',*,*,#23489,.F.);
#31058=ORIENTED_EDGE('',*,*,#23499,.T.);
#31059=ORIENTED_EDGE('',*,*,#21724,.F.);
#31060=ORIENTED_EDGE('',*,*,#23500,.T.);
#31061=ORIENTED_EDGE('',*,*,#23492,.F.);
#31062=ORIENTED_EDGE('',*,*,#23501,.T.);
#31063=ORIENTED_EDGE('',*,*,#21721,.F.);
#31064=ORIENTED_EDGE('',*,*,#23502,.T.);
#31065=ORIENTED_EDGE('',*,*,#23503,.T.);
#31066=ORIENTED_EDGE('',*,*,#23504,.F.);
#31067=ORIENTED_EDGE('',*,*,#23504,.T.);
#31068=ORIENTED_EDGE('',*,*,#23505,.T.);
#31069=ORIENTED_EDGE('',*,*,#21722,.F.);
#31070=ORIENTED_EDGE('',*,*,#23506,.T.);
#31071=ORIENTED_EDGE('',*,*,#23507,.T.);
#31072=ORIENTED_EDGE('',*,*,#21403,.F.);
#31073=ORIENTED_EDGE('',*,*,#23508,.F.);
#31074=ORIENTED_EDGE('',*,*,#23509,.T.);
#31075=ORIENTED_EDGE('',*,*,#23510,.T.);
#31076=ORIENTED_EDGE('',*,*,#23511,.F.);
#31077=ORIENTED_EDGE('',*,*,#23512,.T.);
#31078=ORIENTED_EDGE('',*,*,#23506,.F.);
#31079=ORIENTED_EDGE('',*,*,#23513,.T.);
#31080=ORIENTED_EDGE('',*,*,#23514,.T.);
#31081=ORIENTED_EDGE('',*,*,#23515,.T.);
#31082=ORIENTED_EDGE('',*,*,#23511,.T.);
#31083=ORIENTED_EDGE('',*,*,#23516,.T.);
#31084=ORIENTED_EDGE('',*,*,#23517,.T.);
#31085=ORIENTED_EDGE('',*,*,#23518,.T.);
#31086=ORIENTED_EDGE('',*,*,#23519,.T.);
#31087=ORIENTED_EDGE('',*,*,#23520,.F.);
#31088=ORIENTED_EDGE('',*,*,#23521,.T.);
#31089=ORIENTED_EDGE('',*,*,#23522,.T.);
#31090=ORIENTED_EDGE('',*,*,#23520,.T.);
#31091=ORIENTED_EDGE('',*,*,#23523,.T.);
#31092=ORIENTED_EDGE('',*,*,#23514,.F.);
#31093=ORIENTED_EDGE('',*,*,#23524,.T.);
#31094=ORIENTED_EDGE('',*,*,#21406,.F.);
#31095=ORIENTED_EDGE('',*,*,#23525,.T.);
#31096=ORIENTED_EDGE('',*,*,#23412,.T.);
#31097=ORIENTED_EDGE('',*,*,#23526,.F.);
#31098=ORIENTED_EDGE('',*,*,#23527,.T.);
#31099=ORIENTED_EDGE('',*,*,#23517,.F.);
#31100=ORIENTED_EDGE('',*,*,#23528,.T.);
#31101=ORIENTED_EDGE('',*,*,#23529,.T.);
#31102=ORIENTED_EDGE('',*,*,#23530,.T.);
#31103=ORIENTED_EDGE('',*,*,#23526,.T.);
#31104=ORIENTED_EDGE('',*,*,#23531,.T.);
#31105=ORIENTED_EDGE('',*,*,#23532,.T.);
#31106=ORIENTED_EDGE('',*,*,#23533,.T.);
#31107=ORIENTED_EDGE('',*,*,#23534,.T.);
#31108=ORIENTED_EDGE('',*,*,#23535,.F.);
#31109=ORIENTED_EDGE('',*,*,#23536,.T.);
#31110=ORIENTED_EDGE('',*,*,#23537,.T.);
#31111=ORIENTED_EDGE('',*,*,#23535,.T.);
#31112=ORIENTED_EDGE('',*,*,#23538,.T.);
#31113=ORIENTED_EDGE('',*,*,#23529,.F.);
#31114=ORIENTED_EDGE('',*,*,#23539,.T.);
#31115=ORIENTED_EDGE('',*,*,#23540,.F.);
#31116=ORIENTED_EDGE('',*,*,#23541,.T.);
#31117=ORIENTED_EDGE('',*,*,#23532,.F.);
#31118=ORIENTED_EDGE('',*,*,#23542,.T.);
#31119=ORIENTED_EDGE('',*,*,#23543,.T.);
#31120=ORIENTED_EDGE('',*,*,#23544,.T.);
#31121=ORIENTED_EDGE('',*,*,#23540,.T.);
#31122=ORIENTED_EDGE('',*,*,#23545,.T.);
#31123=ORIENTED_EDGE('',*,*,#23546,.T.);
#31124=ORIENTED_EDGE('',*,*,#23547,.T.);
#31125=ORIENTED_EDGE('',*,*,#23548,.T.);
#31126=ORIENTED_EDGE('',*,*,#23549,.F.);
#31127=ORIENTED_EDGE('',*,*,#23550,.T.);
#31128=ORIENTED_EDGE('',*,*,#23551,.T.);
#31129=ORIENTED_EDGE('',*,*,#23549,.T.);
#31130=ORIENTED_EDGE('',*,*,#23552,.T.);
#31131=ORIENTED_EDGE('',*,*,#23543,.F.);
#31132=ORIENTED_EDGE('',*,*,#23553,.T.);
#31133=ORIENTED_EDGE('',*,*,#23554,.F.);
#31134=ORIENTED_EDGE('',*,*,#23555,.T.);
#31135=ORIENTED_EDGE('',*,*,#23546,.F.);
#31136=ORIENTED_EDGE('',*,*,#23556,.T.);
#31137=ORIENTED_EDGE('',*,*,#23557,.T.);
#31138=ORIENTED_EDGE('',*,*,#23558,.T.);
#31139=ORIENTED_EDGE('',*,*,#23554,.T.);
#31140=ORIENTED_EDGE('',*,*,#23559,.T.);
#31141=ORIENTED_EDGE('',*,*,#23560,.T.);
#31142=ORIENTED_EDGE('',*,*,#23561,.T.);
#31143=ORIENTED_EDGE('',*,*,#23562,.T.);
#31144=ORIENTED_EDGE('',*,*,#23563,.F.);
#31145=ORIENTED_EDGE('',*,*,#23564,.T.);
#31146=ORIENTED_EDGE('',*,*,#23565,.T.);
#31147=ORIENTED_EDGE('',*,*,#23563,.T.);
#31148=ORIENTED_EDGE('',*,*,#23566,.T.);
#31149=ORIENTED_EDGE('',*,*,#23557,.F.);
#31150=ORIENTED_EDGE('',*,*,#23567,.T.);
#31151=ORIENTED_EDGE('',*,*,#23568,.F.);
#31152=ORIENTED_EDGE('',*,*,#23569,.T.);
#31153=ORIENTED_EDGE('',*,*,#23560,.F.);
#31154=ORIENTED_EDGE('',*,*,#23570,.T.);
#31155=ORIENTED_EDGE('',*,*,#23571,.T.);
#31156=ORIENTED_EDGE('',*,*,#23572,.T.);
#31157=ORIENTED_EDGE('',*,*,#23568,.T.);
#31158=ORIENTED_EDGE('',*,*,#23573,.T.);
#31159=ORIENTED_EDGE('',*,*,#23574,.T.);
#31160=ORIENTED_EDGE('',*,*,#23575,.T.);
#31161=ORIENTED_EDGE('',*,*,#23576,.T.);
#31162=ORIENTED_EDGE('',*,*,#23577,.F.);
#31163=ORIENTED_EDGE('',*,*,#23578,.T.);
#31164=ORIENTED_EDGE('',*,*,#23579,.T.);
#31165=ORIENTED_EDGE('',*,*,#23577,.T.);
#31166=ORIENTED_EDGE('',*,*,#23580,.T.);
#31167=ORIENTED_EDGE('',*,*,#23571,.F.);
#31168=ORIENTED_EDGE('',*,*,#23581,.T.);
#31169=ORIENTED_EDGE('',*,*,#23582,.F.);
#31170=ORIENTED_EDGE('',*,*,#23583,.T.);
#31171=ORIENTED_EDGE('',*,*,#23574,.F.);
#31172=ORIENTED_EDGE('',*,*,#23584,.T.);
#31173=ORIENTED_EDGE('',*,*,#23585,.T.);
#31174=ORIENTED_EDGE('',*,*,#23586,.T.);
#31175=ORIENTED_EDGE('',*,*,#23582,.T.);
#31176=ORIENTED_EDGE('',*,*,#23587,.T.);
#31177=ORIENTED_EDGE('',*,*,#23588,.T.);
#31178=ORIENTED_EDGE('',*,*,#23589,.T.);
#31179=ORIENTED_EDGE('',*,*,#23590,.T.);
#31180=ORIENTED_EDGE('',*,*,#23591,.F.);
#31181=ORIENTED_EDGE('',*,*,#23592,.T.);
#31182=ORIENTED_EDGE('',*,*,#23593,.T.);
#31183=ORIENTED_EDGE('',*,*,#23591,.T.);
#31184=ORIENTED_EDGE('',*,*,#23594,.T.);
#31185=ORIENTED_EDGE('',*,*,#23585,.F.);
#31186=ORIENTED_EDGE('',*,*,#23595,.T.);
#31187=ORIENTED_EDGE('',*,*,#21730,.F.);
#31188=ORIENTED_EDGE('',*,*,#23596,.T.);
#31189=ORIENTED_EDGE('',*,*,#23588,.F.);
#31190=ORIENTED_EDGE('',*,*,#23597,.T.);
#31191=ORIENTED_EDGE('',*,*,#21727,.F.);
#31192=ORIENTED_EDGE('',*,*,#23598,.T.);
#31193=ORIENTED_EDGE('',*,*,#23599,.T.);
#31194=ORIENTED_EDGE('',*,*,#23600,.F.);
#31195=ORIENTED_EDGE('',*,*,#23600,.T.);
#31196=ORIENTED_EDGE('',*,*,#23601,.T.);
#31197=ORIENTED_EDGE('',*,*,#21728,.F.);
#31198=ORIENTED_EDGE('',*,*,#23602,.T.);
#31199=ORIENTED_EDGE('',*,*,#23603,.T.);
#31200=ORIENTED_EDGE('',*,*,#21399,.F.);
#31201=ORIENTED_EDGE('',*,*,#23604,.F.);
#31202=ORIENTED_EDGE('',*,*,#23605,.T.);
#31203=ORIENTED_EDGE('',*,*,#23606,.T.);
#31204=ORIENTED_EDGE('',*,*,#23607,.F.);
#31205=ORIENTED_EDGE('',*,*,#23608,.T.);
#31206=ORIENTED_EDGE('',*,*,#23602,.F.);
#31207=ORIENTED_EDGE('',*,*,#23609,.T.);
#31208=ORIENTED_EDGE('',*,*,#23610,.T.);
#31209=ORIENTED_EDGE('',*,*,#23611,.T.);
#31210=ORIENTED_EDGE('',*,*,#23607,.T.);
#31211=ORIENTED_EDGE('',*,*,#23612,.T.);
#31212=ORIENTED_EDGE('',*,*,#23613,.T.);
#31213=ORIENTED_EDGE('',*,*,#23614,.T.);
#31214=ORIENTED_EDGE('',*,*,#23615,.T.);
#31215=ORIENTED_EDGE('',*,*,#23616,.F.);
#31216=ORIENTED_EDGE('',*,*,#23617,.T.);
#31217=ORIENTED_EDGE('',*,*,#23618,.T.);
#31218=ORIENTED_EDGE('',*,*,#23616,.T.);
#31219=ORIENTED_EDGE('',*,*,#23619,.T.);
#31220=ORIENTED_EDGE('',*,*,#23610,.F.);
#31221=ORIENTED_EDGE('',*,*,#23620,.T.);
#31222=ORIENTED_EDGE('',*,*,#21402,.F.);
#31223=ORIENTED_EDGE('',*,*,#23621,.T.);
#31224=ORIENTED_EDGE('',*,*,#23508,.T.);
#31225=ORIENTED_EDGE('',*,*,#23622,.F.);
#31226=ORIENTED_EDGE('',*,*,#23623,.T.);
#31227=ORIENTED_EDGE('',*,*,#23613,.F.);
#31228=ORIENTED_EDGE('',*,*,#23624,.T.);
#31229=ORIENTED_EDGE('',*,*,#23625,.T.);
#31230=ORIENTED_EDGE('',*,*,#23626,.T.);
#31231=ORIENTED_EDGE('',*,*,#23622,.T.);
#31232=ORIENTED_EDGE('',*,*,#23627,.T.);
#31233=ORIENTED_EDGE('',*,*,#23628,.T.);
#31234=ORIENTED_EDGE('',*,*,#23629,.T.);
#31235=ORIENTED_EDGE('',*,*,#23630,.T.);
#31236=ORIENTED_EDGE('',*,*,#23631,.F.);
#31237=ORIENTED_EDGE('',*,*,#23632,.T.);
#31238=ORIENTED_EDGE('',*,*,#23633,.T.);
#31239=ORIENTED_EDGE('',*,*,#23631,.T.);
#31240=ORIENTED_EDGE('',*,*,#23634,.T.);
#31241=ORIENTED_EDGE('',*,*,#23625,.F.);
#31242=ORIENTED_EDGE('',*,*,#23635,.T.);
#31243=ORIENTED_EDGE('',*,*,#23636,.F.);
#31244=ORIENTED_EDGE('',*,*,#23637,.T.);
#31245=ORIENTED_EDGE('',*,*,#23628,.F.);
#31246=ORIENTED_EDGE('',*,*,#23638,.T.);
#31247=ORIENTED_EDGE('',*,*,#23639,.T.);
#31248=ORIENTED_EDGE('',*,*,#23640,.T.);
#31249=ORIENTED_EDGE('',*,*,#23636,.T.);
#31250=ORIENTED_EDGE('',*,*,#23641,.T.);
#31251=ORIENTED_EDGE('',*,*,#23642,.T.);
#31252=ORIENTED_EDGE('',*,*,#23643,.T.);
#31253=ORIENTED_EDGE('',*,*,#23644,.T.);
#31254=ORIENTED_EDGE('',*,*,#23645,.F.);
#31255=ORIENTED_EDGE('',*,*,#23646,.T.);
#31256=ORIENTED_EDGE('',*,*,#23647,.T.);
#31257=ORIENTED_EDGE('',*,*,#23645,.T.);
#31258=ORIENTED_EDGE('',*,*,#23648,.T.);
#31259=ORIENTED_EDGE('',*,*,#23639,.F.);
#31260=ORIENTED_EDGE('',*,*,#23649,.T.);
#31261=ORIENTED_EDGE('',*,*,#23650,.F.);
#31262=ORIENTED_EDGE('',*,*,#23651,.T.);
#31263=ORIENTED_EDGE('',*,*,#23642,.F.);
#31264=ORIENTED_EDGE('',*,*,#23652,.T.);
#31265=ORIENTED_EDGE('',*,*,#23653,.T.);
#31266=ORIENTED_EDGE('',*,*,#23654,.T.);
#31267=ORIENTED_EDGE('',*,*,#23650,.T.);
#31268=ORIENTED_EDGE('',*,*,#23655,.T.);
#31269=ORIENTED_EDGE('',*,*,#23656,.T.);
#31270=ORIENTED_EDGE('',*,*,#23657,.T.);
#31271=ORIENTED_EDGE('',*,*,#23658,.T.);
#31272=ORIENTED_EDGE('',*,*,#23659,.F.);
#31273=ORIENTED_EDGE('',*,*,#23660,.T.);
#31274=ORIENTED_EDGE('',*,*,#23661,.T.);
#31275=ORIENTED_EDGE('',*,*,#23659,.T.);
#31276=ORIENTED_EDGE('',*,*,#23662,.T.);
#31277=ORIENTED_EDGE('',*,*,#23653,.F.);
#31278=ORIENTED_EDGE('',*,*,#23663,.T.);
#31279=ORIENTED_EDGE('',*,*,#23664,.F.);
#31280=ORIENTED_EDGE('',*,*,#23665,.T.);
#31281=ORIENTED_EDGE('',*,*,#23656,.F.);
#31282=ORIENTED_EDGE('',*,*,#23666,.T.);
#31283=ORIENTED_EDGE('',*,*,#23667,.T.);
#31284=ORIENTED_EDGE('',*,*,#23668,.T.);
#31285=ORIENTED_EDGE('',*,*,#23664,.T.);
#31286=ORIENTED_EDGE('',*,*,#23669,.T.);
#31287=ORIENTED_EDGE('',*,*,#23670,.T.);
#31288=ORIENTED_EDGE('',*,*,#23671,.T.);
#31289=ORIENTED_EDGE('',*,*,#23672,.T.);
#31290=ORIENTED_EDGE('',*,*,#23673,.F.);
#31291=ORIENTED_EDGE('',*,*,#23674,.T.);
#31292=ORIENTED_EDGE('',*,*,#23675,.T.);
#31293=ORIENTED_EDGE('',*,*,#23673,.T.);
#31294=ORIENTED_EDGE('',*,*,#23676,.T.);
#31295=ORIENTED_EDGE('',*,*,#23667,.F.);
#31296=ORIENTED_EDGE('',*,*,#23677,.T.);
#31297=ORIENTED_EDGE('',*,*,#23678,.F.);
#31298=ORIENTED_EDGE('',*,*,#23679,.T.);
#31299=ORIENTED_EDGE('',*,*,#23670,.F.);
#31300=ORIENTED_EDGE('',*,*,#23680,.T.);
#31301=ORIENTED_EDGE('',*,*,#23681,.T.);
#31302=ORIENTED_EDGE('',*,*,#23682,.T.);
#31303=ORIENTED_EDGE('',*,*,#23678,.T.);
#31304=ORIENTED_EDGE('',*,*,#23683,.T.);
#31305=ORIENTED_EDGE('',*,*,#23684,.T.);
#31306=ORIENTED_EDGE('',*,*,#23685,.T.);
#31307=ORIENTED_EDGE('',*,*,#23686,.T.);
#31308=ORIENTED_EDGE('',*,*,#23687,.F.);
#31309=ORIENTED_EDGE('',*,*,#23688,.T.);
#31310=ORIENTED_EDGE('',*,*,#23689,.T.);
#31311=ORIENTED_EDGE('',*,*,#23687,.T.);
#31312=ORIENTED_EDGE('',*,*,#23690,.T.);
#31313=ORIENTED_EDGE('',*,*,#23681,.F.);
#31314=ORIENTED_EDGE('',*,*,#23691,.T.);
#31315=ORIENTED_EDGE('',*,*,#21736,.F.);
#31316=ORIENTED_EDGE('',*,*,#23692,.T.);
#31317=ORIENTED_EDGE('',*,*,#23684,.F.);
#31318=ORIENTED_EDGE('',*,*,#23693,.T.);
#31319=ORIENTED_EDGE('',*,*,#21733,.F.);
#31320=ORIENTED_EDGE('',*,*,#23694,.T.);
#31321=ORIENTED_EDGE('',*,*,#23695,.T.);
#31322=ORIENTED_EDGE('',*,*,#23696,.F.);
#31323=ORIENTED_EDGE('',*,*,#23696,.T.);
#31324=ORIENTED_EDGE('',*,*,#23697,.T.);
#31325=ORIENTED_EDGE('',*,*,#21734,.F.);
#31326=ORIENTED_EDGE('',*,*,#23698,.T.);
#31327=ORIENTED_EDGE('',*,*,#23699,.T.);
#31328=ORIENTED_EDGE('',*,*,#21395,.F.);
#31329=ORIENTED_EDGE('',*,*,#23700,.F.);
#31330=ORIENTED_EDGE('',*,*,#23701,.T.);
#31331=ORIENTED_EDGE('',*,*,#23702,.T.);
#31332=ORIENTED_EDGE('',*,*,#23703,.F.);
#31333=ORIENTED_EDGE('',*,*,#23704,.T.);
#31334=ORIENTED_EDGE('',*,*,#23698,.F.);
#31335=ORIENTED_EDGE('',*,*,#23705,.T.);
#31336=ORIENTED_EDGE('',*,*,#23706,.T.);
#31337=ORIENTED_EDGE('',*,*,#23707,.T.);
#31338=ORIENTED_EDGE('',*,*,#23703,.T.);
#31339=ORIENTED_EDGE('',*,*,#23708,.T.);
#31340=ORIENTED_EDGE('',*,*,#23709,.T.);
#31341=ORIENTED_EDGE('',*,*,#23710,.T.);
#31342=ORIENTED_EDGE('',*,*,#23711,.T.);
#31343=ORIENTED_EDGE('',*,*,#23712,.F.);
#31344=ORIENTED_EDGE('',*,*,#23713,.T.);
#31345=ORIENTED_EDGE('',*,*,#23714,.T.);
#31346=ORIENTED_EDGE('',*,*,#23712,.T.);
#31347=ORIENTED_EDGE('',*,*,#23715,.T.);
#31348=ORIENTED_EDGE('',*,*,#23706,.F.);
#31349=ORIENTED_EDGE('',*,*,#23716,.T.);
#31350=ORIENTED_EDGE('',*,*,#21398,.F.);
#31351=ORIENTED_EDGE('',*,*,#23717,.T.);
#31352=ORIENTED_EDGE('',*,*,#23604,.T.);
#31353=ORIENTED_EDGE('',*,*,#23718,.F.);
#31354=ORIENTED_EDGE('',*,*,#23719,.T.);
#31355=ORIENTED_EDGE('',*,*,#23709,.F.);
#31356=ORIENTED_EDGE('',*,*,#23720,.T.);
#31357=ORIENTED_EDGE('',*,*,#23721,.T.);
#31358=ORIENTED_EDGE('',*,*,#23722,.T.);
#31359=ORIENTED_EDGE('',*,*,#23718,.T.);
#31360=ORIENTED_EDGE('',*,*,#23723,.T.);
#31361=ORIENTED_EDGE('',*,*,#23724,.T.);
#31362=ORIENTED_EDGE('',*,*,#23725,.T.);
#31363=ORIENTED_EDGE('',*,*,#23726,.T.);
#31364=ORIENTED_EDGE('',*,*,#23727,.F.);
#31365=ORIENTED_EDGE('',*,*,#23728,.T.);
#31366=ORIENTED_EDGE('',*,*,#23729,.T.);
#31367=ORIENTED_EDGE('',*,*,#23727,.T.);
#31368=ORIENTED_EDGE('',*,*,#23730,.T.);
#31369=ORIENTED_EDGE('',*,*,#23721,.F.);
#31370=ORIENTED_EDGE('',*,*,#23731,.T.);
#31371=ORIENTED_EDGE('',*,*,#23732,.F.);
#31372=ORIENTED_EDGE('',*,*,#23733,.T.);
#31373=ORIENTED_EDGE('',*,*,#23724,.F.);
#31374=ORIENTED_EDGE('',*,*,#23734,.T.);
#31375=ORIENTED_EDGE('',*,*,#23735,.T.);
#31376=ORIENTED_EDGE('',*,*,#23736,.T.);
#31377=ORIENTED_EDGE('',*,*,#23732,.T.);
#31378=ORIENTED_EDGE('',*,*,#23737,.T.);
#31379=ORIENTED_EDGE('',*,*,#23738,.T.);
#31380=ORIENTED_EDGE('',*,*,#23739,.T.);
#31381=ORIENTED_EDGE('',*,*,#23740,.T.);
#31382=ORIENTED_EDGE('',*,*,#23741,.F.);
#31383=ORIENTED_EDGE('',*,*,#23742,.T.);
#31384=ORIENTED_EDGE('',*,*,#23743,.T.);
#31385=ORIENTED_EDGE('',*,*,#23741,.T.);
#31386=ORIENTED_EDGE('',*,*,#23744,.T.);
#31387=ORIENTED_EDGE('',*,*,#23735,.F.);
#31388=ORIENTED_EDGE('',*,*,#23745,.T.);
#31389=ORIENTED_EDGE('',*,*,#23746,.F.);
#31390=ORIENTED_EDGE('',*,*,#23747,.T.);
#31391=ORIENTED_EDGE('',*,*,#23738,.F.);
#31392=ORIENTED_EDGE('',*,*,#23748,.T.);
#31393=ORIENTED_EDGE('',*,*,#23749,.T.);
#31394=ORIENTED_EDGE('',*,*,#23750,.T.);
#31395=ORIENTED_EDGE('',*,*,#23746,.T.);
#31396=ORIENTED_EDGE('',*,*,#23751,.T.);
#31397=ORIENTED_EDGE('',*,*,#23752,.T.);
#31398=ORIENTED_EDGE('',*,*,#23753,.T.);
#31399=ORIENTED_EDGE('',*,*,#23754,.T.);
#31400=ORIENTED_EDGE('',*,*,#23755,.F.);
#31401=ORIENTED_EDGE('',*,*,#23756,.T.);
#31402=ORIENTED_EDGE('',*,*,#23757,.T.);
#31403=ORIENTED_EDGE('',*,*,#23755,.T.);
#31404=ORIENTED_EDGE('',*,*,#23758,.T.);
#31405=ORIENTED_EDGE('',*,*,#23749,.F.);
#31406=ORIENTED_EDGE('',*,*,#23759,.T.);
#31407=ORIENTED_EDGE('',*,*,#23760,.F.);
#31408=ORIENTED_EDGE('',*,*,#23761,.T.);
#31409=ORIENTED_EDGE('',*,*,#23752,.F.);
#31410=ORIENTED_EDGE('',*,*,#23762,.T.);
#31411=ORIENTED_EDGE('',*,*,#23763,.T.);
#31412=ORIENTED_EDGE('',*,*,#23764,.T.);
#31413=ORIENTED_EDGE('',*,*,#23760,.T.);
#31414=ORIENTED_EDGE('',*,*,#23765,.T.);
#31415=ORIENTED_EDGE('',*,*,#23766,.T.);
#31416=ORIENTED_EDGE('',*,*,#23767,.T.);
#31417=ORIENTED_EDGE('',*,*,#23768,.T.);
#31418=ORIENTED_EDGE('',*,*,#23769,.F.);
#31419=ORIENTED_EDGE('',*,*,#23770,.T.);
#31420=ORIENTED_EDGE('',*,*,#23771,.T.);
#31421=ORIENTED_EDGE('',*,*,#23769,.T.);
#31422=ORIENTED_EDGE('',*,*,#23772,.T.);
#31423=ORIENTED_EDGE('',*,*,#23763,.F.);
#31424=ORIENTED_EDGE('',*,*,#23773,.T.);
#31425=ORIENTED_EDGE('',*,*,#23774,.F.);
#31426=ORIENTED_EDGE('',*,*,#23775,.T.);
#31427=ORIENTED_EDGE('',*,*,#23766,.F.);
#31428=ORIENTED_EDGE('',*,*,#23776,.T.);
#31429=ORIENTED_EDGE('',*,*,#23777,.T.);
#31430=ORIENTED_EDGE('',*,*,#23778,.T.);
#31431=ORIENTED_EDGE('',*,*,#23774,.T.);
#31432=ORIENTED_EDGE('',*,*,#23779,.T.);
#31433=ORIENTED_EDGE('',*,*,#23780,.T.);
#31434=ORIENTED_EDGE('',*,*,#23781,.T.);
#31435=ORIENTED_EDGE('',*,*,#23782,.T.);
#31436=ORIENTED_EDGE('',*,*,#23783,.F.);
#31437=ORIENTED_EDGE('',*,*,#23784,.T.);
#31438=ORIENTED_EDGE('',*,*,#23785,.T.);
#31439=ORIENTED_EDGE('',*,*,#23783,.T.);
#31440=ORIENTED_EDGE('',*,*,#23786,.T.);
#31441=ORIENTED_EDGE('',*,*,#23777,.F.);
#31442=ORIENTED_EDGE('',*,*,#23787,.T.);
#31443=ORIENTED_EDGE('',*,*,#21742,.F.);
#31444=ORIENTED_EDGE('',*,*,#23788,.T.);
#31445=ORIENTED_EDGE('',*,*,#23780,.F.);
#31446=ORIENTED_EDGE('',*,*,#23789,.T.);
#31447=ORIENTED_EDGE('',*,*,#21739,.F.);
#31448=ORIENTED_EDGE('',*,*,#23790,.T.);
#31449=ORIENTED_EDGE('',*,*,#23791,.T.);
#31450=ORIENTED_EDGE('',*,*,#23792,.F.);
#31451=ORIENTED_EDGE('',*,*,#23792,.T.);
#31452=ORIENTED_EDGE('',*,*,#23793,.T.);
#31453=ORIENTED_EDGE('',*,*,#21740,.F.);
#31454=ORIENTED_EDGE('',*,*,#23794,.T.);
#31455=ORIENTED_EDGE('',*,*,#23795,.T.);
#31456=ORIENTED_EDGE('',*,*,#21391,.F.);
#31457=ORIENTED_EDGE('',*,*,#23796,.F.);
#31458=ORIENTED_EDGE('',*,*,#23797,.T.);
#31459=ORIENTED_EDGE('',*,*,#23798,.T.);
#31460=ORIENTED_EDGE('',*,*,#23799,.F.);
#31461=ORIENTED_EDGE('',*,*,#23800,.T.);
#31462=ORIENTED_EDGE('',*,*,#23794,.F.);
#31463=ORIENTED_EDGE('',*,*,#23801,.T.);
#31464=ORIENTED_EDGE('',*,*,#23802,.T.);
#31465=ORIENTED_EDGE('',*,*,#23803,.T.);
#31466=ORIENTED_EDGE('',*,*,#23799,.T.);
#31467=ORIENTED_EDGE('',*,*,#23804,.T.);
#31468=ORIENTED_EDGE('',*,*,#23805,.T.);
#31469=ORIENTED_EDGE('',*,*,#23806,.T.);
#31470=ORIENTED_EDGE('',*,*,#23807,.T.);
#31471=ORIENTED_EDGE('',*,*,#23808,.F.);
#31472=ORIENTED_EDGE('',*,*,#23809,.T.);
#31473=ORIENTED_EDGE('',*,*,#23810,.T.);
#31474=ORIENTED_EDGE('',*,*,#23808,.T.);
#31475=ORIENTED_EDGE('',*,*,#23811,.T.);
#31476=ORIENTED_EDGE('',*,*,#23802,.F.);
#31477=ORIENTED_EDGE('',*,*,#23812,.T.);
#31478=ORIENTED_EDGE('',*,*,#21394,.F.);
#31479=ORIENTED_EDGE('',*,*,#23813,.T.);
#31480=ORIENTED_EDGE('',*,*,#23700,.T.);
#31481=ORIENTED_EDGE('',*,*,#23814,.F.);
#31482=ORIENTED_EDGE('',*,*,#23815,.T.);
#31483=ORIENTED_EDGE('',*,*,#23805,.F.);
#31484=ORIENTED_EDGE('',*,*,#23816,.T.);
#31485=ORIENTED_EDGE('',*,*,#23817,.T.);
#31486=ORIENTED_EDGE('',*,*,#23818,.T.);
#31487=ORIENTED_EDGE('',*,*,#23814,.T.);
#31488=ORIENTED_EDGE('',*,*,#23819,.T.);
#31489=ORIENTED_EDGE('',*,*,#23820,.T.);
#31490=ORIENTED_EDGE('',*,*,#23821,.T.);
#31491=ORIENTED_EDGE('',*,*,#23822,.T.);
#31492=ORIENTED_EDGE('',*,*,#23823,.F.);
#31493=ORIENTED_EDGE('',*,*,#23824,.T.);
#31494=ORIENTED_EDGE('',*,*,#23825,.T.);
#31495=ORIENTED_EDGE('',*,*,#23823,.T.);
#31496=ORIENTED_EDGE('',*,*,#23826,.T.);
#31497=ORIENTED_EDGE('',*,*,#23817,.F.);
#31498=ORIENTED_EDGE('',*,*,#23827,.T.);
#31499=ORIENTED_EDGE('',*,*,#23828,.F.);
#31500=ORIENTED_EDGE('',*,*,#23829,.T.);
#31501=ORIENTED_EDGE('',*,*,#23820,.F.);
#31502=ORIENTED_EDGE('',*,*,#23830,.T.);
#31503=ORIENTED_EDGE('',*,*,#23831,.T.);
#31504=ORIENTED_EDGE('',*,*,#23832,.T.);
#31505=ORIENTED_EDGE('',*,*,#23828,.T.);
#31506=ORIENTED_EDGE('',*,*,#23833,.T.);
#31507=ORIENTED_EDGE('',*,*,#23834,.T.);
#31508=ORIENTED_EDGE('',*,*,#23835,.T.);
#31509=ORIENTED_EDGE('',*,*,#23836,.T.);
#31510=ORIENTED_EDGE('',*,*,#23837,.F.);
#31511=ORIENTED_EDGE('',*,*,#23838,.T.);
#31512=ORIENTED_EDGE('',*,*,#23839,.T.);
#31513=ORIENTED_EDGE('',*,*,#23837,.T.);
#31514=ORIENTED_EDGE('',*,*,#23840,.T.);
#31515=ORIENTED_EDGE('',*,*,#23831,.F.);
#31516=ORIENTED_EDGE('',*,*,#23841,.T.);
#31517=ORIENTED_EDGE('',*,*,#23842,.F.);
#31518=ORIENTED_EDGE('',*,*,#23843,.T.);
#31519=ORIENTED_EDGE('',*,*,#23834,.F.);
#31520=ORIENTED_EDGE('',*,*,#23844,.T.);
#31521=ORIENTED_EDGE('',*,*,#23845,.T.);
#31522=ORIENTED_EDGE('',*,*,#23846,.T.);
#31523=ORIENTED_EDGE('',*,*,#23842,.T.);
#31524=ORIENTED_EDGE('',*,*,#23847,.T.);
#31525=ORIENTED_EDGE('',*,*,#23848,.T.);
#31526=ORIENTED_EDGE('',*,*,#23849,.T.);
#31527=ORIENTED_EDGE('',*,*,#23850,.T.);
#31528=ORIENTED_EDGE('',*,*,#23851,.F.);
#31529=ORIENTED_EDGE('',*,*,#23852,.T.);
#31530=ORIENTED_EDGE('',*,*,#23853,.T.);
#31531=ORIENTED_EDGE('',*,*,#23851,.T.);
#31532=ORIENTED_EDGE('',*,*,#23854,.T.);
#31533=ORIENTED_EDGE('',*,*,#23845,.F.);
#31534=ORIENTED_EDGE('',*,*,#23855,.T.);
#31535=ORIENTED_EDGE('',*,*,#23856,.F.);
#31536=ORIENTED_EDGE('',*,*,#23857,.T.);
#31537=ORIENTED_EDGE('',*,*,#23848,.F.);
#31538=ORIENTED_EDGE('',*,*,#23858,.T.);
#31539=ORIENTED_EDGE('',*,*,#23859,.T.);
#31540=ORIENTED_EDGE('',*,*,#23860,.T.);
#31541=ORIENTED_EDGE('',*,*,#23856,.T.);
#31542=ORIENTED_EDGE('',*,*,#23861,.T.);
#31543=ORIENTED_EDGE('',*,*,#23862,.T.);
#31544=ORIENTED_EDGE('',*,*,#23863,.T.);
#31545=ORIENTED_EDGE('',*,*,#23864,.T.);
#31546=ORIENTED_EDGE('',*,*,#23865,.F.);
#31547=ORIENTED_EDGE('',*,*,#23866,.T.);
#31548=ORIENTED_EDGE('',*,*,#23867,.T.);
#31549=ORIENTED_EDGE('',*,*,#23865,.T.);
#31550=ORIENTED_EDGE('',*,*,#23868,.T.);
#31551=ORIENTED_EDGE('',*,*,#23859,.F.);
#31552=ORIENTED_EDGE('',*,*,#23869,.T.);
#31553=ORIENTED_EDGE('',*,*,#23870,.F.);
#31554=ORIENTED_EDGE('',*,*,#23871,.T.);
#31555=ORIENTED_EDGE('',*,*,#23862,.F.);
#31556=ORIENTED_EDGE('',*,*,#23872,.T.);
#31557=ORIENTED_EDGE('',*,*,#23873,.T.);
#31558=ORIENTED_EDGE('',*,*,#23874,.T.);
#31559=ORIENTED_EDGE('',*,*,#23870,.T.);
#31560=ORIENTED_EDGE('',*,*,#23875,.T.);
#31561=ORIENTED_EDGE('',*,*,#23876,.T.);
#31562=ORIENTED_EDGE('',*,*,#23877,.T.);
#31563=ORIENTED_EDGE('',*,*,#23878,.T.);
#31564=ORIENTED_EDGE('',*,*,#23879,.F.);
#31565=ORIENTED_EDGE('',*,*,#23880,.T.);
#31566=ORIENTED_EDGE('',*,*,#23881,.T.);
#31567=ORIENTED_EDGE('',*,*,#23879,.T.);
#31568=ORIENTED_EDGE('',*,*,#23882,.T.);
#31569=ORIENTED_EDGE('',*,*,#23873,.F.);
#31570=ORIENTED_EDGE('',*,*,#23883,.T.);
#31571=ORIENTED_EDGE('',*,*,#21748,.F.);
#31572=ORIENTED_EDGE('',*,*,#23884,.T.);
#31573=ORIENTED_EDGE('',*,*,#23876,.F.);
#31574=ORIENTED_EDGE('',*,*,#23885,.T.);
#31575=ORIENTED_EDGE('',*,*,#21745,.F.);
#31576=ORIENTED_EDGE('',*,*,#23886,.T.);
#31577=ORIENTED_EDGE('',*,*,#23887,.T.);
#31578=ORIENTED_EDGE('',*,*,#23888,.F.);
#31579=ORIENTED_EDGE('',*,*,#23888,.T.);
#31580=ORIENTED_EDGE('',*,*,#23889,.T.);
#31581=ORIENTED_EDGE('',*,*,#21746,.F.);
#31582=ORIENTED_EDGE('',*,*,#23890,.T.);
#31583=ORIENTED_EDGE('',*,*,#23891,.T.);
#31584=ORIENTED_EDGE('',*,*,#21387,.F.);
#31585=ORIENTED_EDGE('',*,*,#23892,.F.);
#31586=ORIENTED_EDGE('',*,*,#23893,.T.);
#31587=ORIENTED_EDGE('',*,*,#23894,.T.);
#31588=ORIENTED_EDGE('',*,*,#23895,.F.);
#31589=ORIENTED_EDGE('',*,*,#23896,.T.);
#31590=ORIENTED_EDGE('',*,*,#23890,.F.);
#31591=ORIENTED_EDGE('',*,*,#23897,.T.);
#31592=ORIENTED_EDGE('',*,*,#23898,.T.);
#31593=ORIENTED_EDGE('',*,*,#23899,.T.);
#31594=ORIENTED_EDGE('',*,*,#23895,.T.);
#31595=ORIENTED_EDGE('',*,*,#23900,.T.);
#31596=ORIENTED_EDGE('',*,*,#23901,.T.);
#31597=ORIENTED_EDGE('',*,*,#23902,.T.);
#31598=ORIENTED_EDGE('',*,*,#23903,.T.);
#31599=ORIENTED_EDGE('',*,*,#23904,.F.);
#31600=ORIENTED_EDGE('',*,*,#23905,.T.);
#31601=ORIENTED_EDGE('',*,*,#23906,.T.);
#31602=ORIENTED_EDGE('',*,*,#23904,.T.);
#31603=ORIENTED_EDGE('',*,*,#23907,.T.);
#31604=ORIENTED_EDGE('',*,*,#23898,.F.);
#31605=ORIENTED_EDGE('',*,*,#23908,.T.);
#31606=ORIENTED_EDGE('',*,*,#21390,.F.);
#31607=ORIENTED_EDGE('',*,*,#23909,.T.);
#31608=ORIENTED_EDGE('',*,*,#23796,.T.);
#31609=ORIENTED_EDGE('',*,*,#23910,.F.);
#31610=ORIENTED_EDGE('',*,*,#23911,.T.);
#31611=ORIENTED_EDGE('',*,*,#23901,.F.);
#31612=ORIENTED_EDGE('',*,*,#23912,.T.);
#31613=ORIENTED_EDGE('',*,*,#23913,.T.);
#31614=ORIENTED_EDGE('',*,*,#23914,.T.);
#31615=ORIENTED_EDGE('',*,*,#23910,.T.);
#31616=ORIENTED_EDGE('',*,*,#23915,.T.);
#31617=ORIENTED_EDGE('',*,*,#23916,.T.);
#31618=ORIENTED_EDGE('',*,*,#23917,.T.);
#31619=ORIENTED_EDGE('',*,*,#23918,.T.);
#31620=ORIENTED_EDGE('',*,*,#23919,.F.);
#31621=ORIENTED_EDGE('',*,*,#23920,.T.);
#31622=ORIENTED_EDGE('',*,*,#23921,.T.);
#31623=ORIENTED_EDGE('',*,*,#23919,.T.);
#31624=ORIENTED_EDGE('',*,*,#23922,.T.);
#31625=ORIENTED_EDGE('',*,*,#23913,.F.);
#31626=ORIENTED_EDGE('',*,*,#23923,.T.);
#31627=ORIENTED_EDGE('',*,*,#23924,.F.);
#31628=ORIENTED_EDGE('',*,*,#23925,.T.);
#31629=ORIENTED_EDGE('',*,*,#23916,.F.);
#31630=ORIENTED_EDGE('',*,*,#23926,.T.);
#31631=ORIENTED_EDGE('',*,*,#23927,.T.);
#31632=ORIENTED_EDGE('',*,*,#23928,.T.);
#31633=ORIENTED_EDGE('',*,*,#23924,.T.);
#31634=ORIENTED_EDGE('',*,*,#23929,.T.);
#31635=ORIENTED_EDGE('',*,*,#23930,.T.);
#31636=ORIENTED_EDGE('',*,*,#23931,.T.);
#31637=ORIENTED_EDGE('',*,*,#23932,.T.);
#31638=ORIENTED_EDGE('',*,*,#23933,.F.);
#31639=ORIENTED_EDGE('',*,*,#23934,.T.);
#31640=ORIENTED_EDGE('',*,*,#23935,.T.);
#31641=ORIENTED_EDGE('',*,*,#23933,.T.);
#31642=ORIENTED_EDGE('',*,*,#23936,.T.);
#31643=ORIENTED_EDGE('',*,*,#23927,.F.);
#31644=ORIENTED_EDGE('',*,*,#23937,.T.);
#31645=ORIENTED_EDGE('',*,*,#23938,.F.);
#31646=ORIENTED_EDGE('',*,*,#23939,.T.);
#31647=ORIENTED_EDGE('',*,*,#23930,.F.);
#31648=ORIENTED_EDGE('',*,*,#23940,.T.);
#31649=ORIENTED_EDGE('',*,*,#23941,.T.);
#31650=ORIENTED_EDGE('',*,*,#23942,.T.);
#31651=ORIENTED_EDGE('',*,*,#23938,.T.);
#31652=ORIENTED_EDGE('',*,*,#23943,.T.);
#31653=ORIENTED_EDGE('',*,*,#23944,.T.);
#31654=ORIENTED_EDGE('',*,*,#23945,.T.);
#31655=ORIENTED_EDGE('',*,*,#23946,.T.);
#31656=ORIENTED_EDGE('',*,*,#23947,.F.);
#31657=ORIENTED_EDGE('',*,*,#23948,.T.);
#31658=ORIENTED_EDGE('',*,*,#23949,.T.);
#31659=ORIENTED_EDGE('',*,*,#23947,.T.);
#31660=ORIENTED_EDGE('',*,*,#23950,.T.);
#31661=ORIENTED_EDGE('',*,*,#23941,.F.);
#31662=ORIENTED_EDGE('',*,*,#23951,.T.);
#31663=ORIENTED_EDGE('',*,*,#23952,.F.);
#31664=ORIENTED_EDGE('',*,*,#23953,.T.);
#31665=ORIENTED_EDGE('',*,*,#23944,.F.);
#31666=ORIENTED_EDGE('',*,*,#23954,.T.);
#31667=ORIENTED_EDGE('',*,*,#23955,.T.);
#31668=ORIENTED_EDGE('',*,*,#23956,.T.);
#31669=ORIENTED_EDGE('',*,*,#23952,.T.);
#31670=ORIENTED_EDGE('',*,*,#23957,.T.);
#31671=ORIENTED_EDGE('',*,*,#23958,.T.);
#31672=ORIENTED_EDGE('',*,*,#23959,.T.);
#31673=ORIENTED_EDGE('',*,*,#23960,.T.);
#31674=ORIENTED_EDGE('',*,*,#23961,.F.);
#31675=ORIENTED_EDGE('',*,*,#23962,.T.);
#31676=ORIENTED_EDGE('',*,*,#23963,.T.);
#31677=ORIENTED_EDGE('',*,*,#23961,.T.);
#31678=ORIENTED_EDGE('',*,*,#23964,.T.);
#31679=ORIENTED_EDGE('',*,*,#23955,.F.);
#31680=ORIENTED_EDGE('',*,*,#23965,.T.);
#31681=ORIENTED_EDGE('',*,*,#23966,.F.);
#31682=ORIENTED_EDGE('',*,*,#23967,.T.);
#31683=ORIENTED_EDGE('',*,*,#23958,.F.);
#31684=ORIENTED_EDGE('',*,*,#23968,.T.);
#31685=ORIENTED_EDGE('',*,*,#23969,.T.);
#31686=ORIENTED_EDGE('',*,*,#23970,.T.);
#31687=ORIENTED_EDGE('',*,*,#23966,.T.);
#31688=ORIENTED_EDGE('',*,*,#23971,.T.);
#31689=ORIENTED_EDGE('',*,*,#23972,.T.);
#31690=ORIENTED_EDGE('',*,*,#23973,.T.);
#31691=ORIENTED_EDGE('',*,*,#23974,.T.);
#31692=ORIENTED_EDGE('',*,*,#23975,.F.);
#31693=ORIENTED_EDGE('',*,*,#23976,.T.);
#31694=ORIENTED_EDGE('',*,*,#23977,.T.);
#31695=ORIENTED_EDGE('',*,*,#23975,.T.);
#31696=ORIENTED_EDGE('',*,*,#23978,.T.);
#31697=ORIENTED_EDGE('',*,*,#23969,.F.);
#31698=ORIENTED_EDGE('',*,*,#23979,.T.);
#31699=ORIENTED_EDGE('',*,*,#21754,.F.);
#31700=ORIENTED_EDGE('',*,*,#23980,.T.);
#31701=ORIENTED_EDGE('',*,*,#23972,.F.);
#31702=ORIENTED_EDGE('',*,*,#23981,.T.);
#31703=ORIENTED_EDGE('',*,*,#21751,.F.);
#31704=ORIENTED_EDGE('',*,*,#23982,.T.);
#31705=ORIENTED_EDGE('',*,*,#23983,.T.);
#31706=ORIENTED_EDGE('',*,*,#23984,.F.);
#31707=ORIENTED_EDGE('',*,*,#23984,.T.);
#31708=ORIENTED_EDGE('',*,*,#23985,.T.);
#31709=ORIENTED_EDGE('',*,*,#21752,.F.);
#31710=ORIENTED_EDGE('',*,*,#23986,.T.);
#31711=ORIENTED_EDGE('',*,*,#23987,.T.);
#31712=ORIENTED_EDGE('',*,*,#21383,.F.);
#31713=ORIENTED_EDGE('',*,*,#23988,.F.);
#31714=ORIENTED_EDGE('',*,*,#23989,.T.);
#31715=ORIENTED_EDGE('',*,*,#23990,.T.);
#31716=ORIENTED_EDGE('',*,*,#23991,.F.);
#31717=ORIENTED_EDGE('',*,*,#23992,.T.);
#31718=ORIENTED_EDGE('',*,*,#23986,.F.);
#31719=ORIENTED_EDGE('',*,*,#23993,.T.);
#31720=ORIENTED_EDGE('',*,*,#23994,.T.);
#31721=ORIENTED_EDGE('',*,*,#23995,.T.);
#31722=ORIENTED_EDGE('',*,*,#23991,.T.);
#31723=ORIENTED_EDGE('',*,*,#23996,.T.);
#31724=ORIENTED_EDGE('',*,*,#23997,.T.);
#31725=ORIENTED_EDGE('',*,*,#23998,.T.);
#31726=ORIENTED_EDGE('',*,*,#23999,.T.);
#31727=ORIENTED_EDGE('',*,*,#24000,.F.);
#31728=ORIENTED_EDGE('',*,*,#24001,.T.);
#31729=ORIENTED_EDGE('',*,*,#24002,.T.);
#31730=ORIENTED_EDGE('',*,*,#24000,.T.);
#31731=ORIENTED_EDGE('',*,*,#24003,.T.);
#31732=ORIENTED_EDGE('',*,*,#23994,.F.);
#31733=ORIENTED_EDGE('',*,*,#24004,.T.);
#31734=ORIENTED_EDGE('',*,*,#21386,.F.);
#31735=ORIENTED_EDGE('',*,*,#24005,.T.);
#31736=ORIENTED_EDGE('',*,*,#23892,.T.);
#31737=ORIENTED_EDGE('',*,*,#24006,.F.);
#31738=ORIENTED_EDGE('',*,*,#24007,.T.);
#31739=ORIENTED_EDGE('',*,*,#23997,.F.);
#31740=ORIENTED_EDGE('',*,*,#24008,.T.);
#31741=ORIENTED_EDGE('',*,*,#24009,.T.);
#31742=ORIENTED_EDGE('',*,*,#24010,.T.);
#31743=ORIENTED_EDGE('',*,*,#24006,.T.);
#31744=ORIENTED_EDGE('',*,*,#24011,.T.);
#31745=ORIENTED_EDGE('',*,*,#24012,.T.);
#31746=ORIENTED_EDGE('',*,*,#24013,.T.);
#31747=ORIENTED_EDGE('',*,*,#24014,.T.);
#31748=ORIENTED_EDGE('',*,*,#24015,.F.);
#31749=ORIENTED_EDGE('',*,*,#24016,.T.);
#31750=ORIENTED_EDGE('',*,*,#24017,.T.);
#31751=ORIENTED_EDGE('',*,*,#24015,.T.);
#31752=ORIENTED_EDGE('',*,*,#24018,.T.);
#31753=ORIENTED_EDGE('',*,*,#24009,.F.);
#31754=ORIENTED_EDGE('',*,*,#24019,.T.);
#31755=ORIENTED_EDGE('',*,*,#24020,.F.);
#31756=ORIENTED_EDGE('',*,*,#24021,.T.);
#31757=ORIENTED_EDGE('',*,*,#24012,.F.);
#31758=ORIENTED_EDGE('',*,*,#24022,.T.);
#31759=ORIENTED_EDGE('',*,*,#24023,.T.);
#31760=ORIENTED_EDGE('',*,*,#24024,.T.);
#31761=ORIENTED_EDGE('',*,*,#24020,.T.);
#31762=ORIENTED_EDGE('',*,*,#24025,.T.);
#31763=ORIENTED_EDGE('',*,*,#24026,.T.);
#31764=ORIENTED_EDGE('',*,*,#24027,.T.);
#31765=ORIENTED_EDGE('',*,*,#24028,.T.);
#31766=ORIENTED_EDGE('',*,*,#24029,.F.);
#31767=ORIENTED_EDGE('',*,*,#24030,.T.);
#31768=ORIENTED_EDGE('',*,*,#24031,.T.);
#31769=ORIENTED_EDGE('',*,*,#24029,.T.);
#31770=ORIENTED_EDGE('',*,*,#24032,.T.);
#31771=ORIENTED_EDGE('',*,*,#24023,.F.);
#31772=ORIENTED_EDGE('',*,*,#24033,.T.);
#31773=ORIENTED_EDGE('',*,*,#24034,.F.);
#31774=ORIENTED_EDGE('',*,*,#24035,.T.);
#31775=ORIENTED_EDGE('',*,*,#24026,.F.);
#31776=ORIENTED_EDGE('',*,*,#24036,.T.);
#31777=ORIENTED_EDGE('',*,*,#24037,.T.);
#31778=ORIENTED_EDGE('',*,*,#24038,.T.);
#31779=ORIENTED_EDGE('',*,*,#24034,.T.);
#31780=ORIENTED_EDGE('',*,*,#24039,.T.);
#31781=ORIENTED_EDGE('',*,*,#24040,.T.);
#31782=ORIENTED_EDGE('',*,*,#24041,.T.);
#31783=ORIENTED_EDGE('',*,*,#24042,.T.);
#31784=ORIENTED_EDGE('',*,*,#24043,.F.);
#31785=ORIENTED_EDGE('',*,*,#24044,.T.);
#31786=ORIENTED_EDGE('',*,*,#24045,.T.);
#31787=ORIENTED_EDGE('',*,*,#24043,.T.);
#31788=ORIENTED_EDGE('',*,*,#24046,.T.);
#31789=ORIENTED_EDGE('',*,*,#24037,.F.);
#31790=ORIENTED_EDGE('',*,*,#24047,.T.);
#31791=ORIENTED_EDGE('',*,*,#24048,.F.);
#31792=ORIENTED_EDGE('',*,*,#24049,.T.);
#31793=ORIENTED_EDGE('',*,*,#24040,.F.);
#31794=ORIENTED_EDGE('',*,*,#24050,.T.);
#31795=ORIENTED_EDGE('',*,*,#24051,.T.);
#31796=ORIENTED_EDGE('',*,*,#24052,.T.);
#31797=ORIENTED_EDGE('',*,*,#24048,.T.);
#31798=ORIENTED_EDGE('',*,*,#24053,.T.);
#31799=ORIENTED_EDGE('',*,*,#24054,.T.);
#31800=ORIENTED_EDGE('',*,*,#24055,.T.);
#31801=ORIENTED_EDGE('',*,*,#24056,.T.);
#31802=ORIENTED_EDGE('',*,*,#24057,.F.);
#31803=ORIENTED_EDGE('',*,*,#24058,.T.);
#31804=ORIENTED_EDGE('',*,*,#24059,.T.);
#31805=ORIENTED_EDGE('',*,*,#24057,.T.);
#31806=ORIENTED_EDGE('',*,*,#24060,.T.);
#31807=ORIENTED_EDGE('',*,*,#24051,.F.);
#31808=ORIENTED_EDGE('',*,*,#24061,.T.);
#31809=ORIENTED_EDGE('',*,*,#24062,.F.);
#31810=ORIENTED_EDGE('',*,*,#24063,.T.);
#31811=ORIENTED_EDGE('',*,*,#24054,.F.);
#31812=ORIENTED_EDGE('',*,*,#24064,.T.);
#31813=ORIENTED_EDGE('',*,*,#24065,.T.);
#31814=ORIENTED_EDGE('',*,*,#24066,.T.);
#31815=ORIENTED_EDGE('',*,*,#24062,.T.);
#31816=ORIENTED_EDGE('',*,*,#24067,.T.);
#31817=ORIENTED_EDGE('',*,*,#24068,.T.);
#31818=ORIENTED_EDGE('',*,*,#24069,.T.);
#31819=ORIENTED_EDGE('',*,*,#24070,.T.);
#31820=ORIENTED_EDGE('',*,*,#24071,.F.);
#31821=ORIENTED_EDGE('',*,*,#24072,.T.);
#31822=ORIENTED_EDGE('',*,*,#24073,.T.);
#31823=ORIENTED_EDGE('',*,*,#24071,.T.);
#31824=ORIENTED_EDGE('',*,*,#24074,.T.);
#31825=ORIENTED_EDGE('',*,*,#24065,.F.);
#31826=ORIENTED_EDGE('',*,*,#24075,.T.);
#31827=ORIENTED_EDGE('',*,*,#21760,.F.);
#31828=ORIENTED_EDGE('',*,*,#24076,.T.);
#31829=ORIENTED_EDGE('',*,*,#24068,.F.);
#31830=ORIENTED_EDGE('',*,*,#24077,.T.);
#31831=ORIENTED_EDGE('',*,*,#21757,.F.);
#31832=ORIENTED_EDGE('',*,*,#24078,.T.);
#31833=ORIENTED_EDGE('',*,*,#24079,.T.);
#31834=ORIENTED_EDGE('',*,*,#24080,.F.);
#31835=ORIENTED_EDGE('',*,*,#24080,.T.);
#31836=ORIENTED_EDGE('',*,*,#24081,.T.);
#31837=ORIENTED_EDGE('',*,*,#21758,.F.);
#31838=ORIENTED_EDGE('',*,*,#24082,.T.);
#31839=ORIENTED_EDGE('',*,*,#24083,.T.);
#31840=ORIENTED_EDGE('',*,*,#21379,.F.);
#31841=ORIENTED_EDGE('',*,*,#24084,.F.);
#31842=ORIENTED_EDGE('',*,*,#24085,.T.);
#31843=ORIENTED_EDGE('',*,*,#24086,.T.);
#31844=ORIENTED_EDGE('',*,*,#24087,.F.);
#31845=ORIENTED_EDGE('',*,*,#24088,.T.);
#31846=ORIENTED_EDGE('',*,*,#24082,.F.);
#31847=ORIENTED_EDGE('',*,*,#24089,.T.);
#31848=ORIENTED_EDGE('',*,*,#24090,.T.);
#31849=ORIENTED_EDGE('',*,*,#24091,.T.);
#31850=ORIENTED_EDGE('',*,*,#24087,.T.);
#31851=ORIENTED_EDGE('',*,*,#24092,.T.);
#31852=ORIENTED_EDGE('',*,*,#24093,.T.);
#31853=ORIENTED_EDGE('',*,*,#24094,.T.);
#31854=ORIENTED_EDGE('',*,*,#24095,.T.);
#31855=ORIENTED_EDGE('',*,*,#24096,.F.);
#31856=ORIENTED_EDGE('',*,*,#24097,.T.);
#31857=ORIENTED_EDGE('',*,*,#24098,.T.);
#31858=ORIENTED_EDGE('',*,*,#24096,.T.);
#31859=ORIENTED_EDGE('',*,*,#24099,.T.);
#31860=ORIENTED_EDGE('',*,*,#24090,.F.);
#31861=ORIENTED_EDGE('',*,*,#24100,.T.);
#31862=ORIENTED_EDGE('',*,*,#21382,.F.);
#31863=ORIENTED_EDGE('',*,*,#24101,.T.);
#31864=ORIENTED_EDGE('',*,*,#23988,.T.);
#31865=ORIENTED_EDGE('',*,*,#24102,.F.);
#31866=ORIENTED_EDGE('',*,*,#24103,.T.);
#31867=ORIENTED_EDGE('',*,*,#24093,.F.);
#31868=ORIENTED_EDGE('',*,*,#24104,.T.);
#31869=ORIENTED_EDGE('',*,*,#24105,.T.);
#31870=ORIENTED_EDGE('',*,*,#24106,.T.);
#31871=ORIENTED_EDGE('',*,*,#24102,.T.);
#31872=ORIENTED_EDGE('',*,*,#24107,.T.);
#31873=ORIENTED_EDGE('',*,*,#24108,.T.);
#31874=ORIENTED_EDGE('',*,*,#24109,.T.);
#31875=ORIENTED_EDGE('',*,*,#24110,.T.);
#31876=ORIENTED_EDGE('',*,*,#24111,.F.);
#31877=ORIENTED_EDGE('',*,*,#24112,.T.);
#31878=ORIENTED_EDGE('',*,*,#24113,.T.);
#31879=ORIENTED_EDGE('',*,*,#24111,.T.);
#31880=ORIENTED_EDGE('',*,*,#24114,.T.);
#31881=ORIENTED_EDGE('',*,*,#24105,.F.);
#31882=ORIENTED_EDGE('',*,*,#24115,.T.);
#31883=ORIENTED_EDGE('',*,*,#24116,.F.);
#31884=ORIENTED_EDGE('',*,*,#24117,.T.);
#31885=ORIENTED_EDGE('',*,*,#24108,.F.);
#31886=ORIENTED_EDGE('',*,*,#24118,.T.);
#31887=ORIENTED_EDGE('',*,*,#24119,.T.);
#31888=ORIENTED_EDGE('',*,*,#24120,.T.);
#31889=ORIENTED_EDGE('',*,*,#24116,.T.);
#31890=ORIENTED_EDGE('',*,*,#24121,.T.);
#31891=ORIENTED_EDGE('',*,*,#24122,.T.);
#31892=ORIENTED_EDGE('',*,*,#24123,.T.);
#31893=ORIENTED_EDGE('',*,*,#24124,.T.);
#31894=ORIENTED_EDGE('',*,*,#24125,.F.);
#31895=ORIENTED_EDGE('',*,*,#24126,.T.);
#31896=ORIENTED_EDGE('',*,*,#24127,.T.);
#31897=ORIENTED_EDGE('',*,*,#24125,.T.);
#31898=ORIENTED_EDGE('',*,*,#24128,.T.);
#31899=ORIENTED_EDGE('',*,*,#24119,.F.);
#31900=ORIENTED_EDGE('',*,*,#24129,.T.);
#31901=ORIENTED_EDGE('',*,*,#24130,.F.);
#31902=ORIENTED_EDGE('',*,*,#24131,.T.);
#31903=ORIENTED_EDGE('',*,*,#24122,.F.);
#31904=ORIENTED_EDGE('',*,*,#24132,.T.);
#31905=ORIENTED_EDGE('',*,*,#24133,.T.);
#31906=ORIENTED_EDGE('',*,*,#24134,.T.);
#31907=ORIENTED_EDGE('',*,*,#24130,.T.);
#31908=ORIENTED_EDGE('',*,*,#24135,.T.);
#31909=ORIENTED_EDGE('',*,*,#24136,.T.);
#31910=ORIENTED_EDGE('',*,*,#24137,.T.);
#31911=ORIENTED_EDGE('',*,*,#24138,.T.);
#31912=ORIENTED_EDGE('',*,*,#24139,.F.);
#31913=ORIENTED_EDGE('',*,*,#24140,.T.);
#31914=ORIENTED_EDGE('',*,*,#24141,.T.);
#31915=ORIENTED_EDGE('',*,*,#24139,.T.);
#31916=ORIENTED_EDGE('',*,*,#24142,.T.);
#31917=ORIENTED_EDGE('',*,*,#24133,.F.);
#31918=ORIENTED_EDGE('',*,*,#24143,.T.);
#31919=ORIENTED_EDGE('',*,*,#24144,.F.);
#31920=ORIENTED_EDGE('',*,*,#24145,.T.);
#31921=ORIENTED_EDGE('',*,*,#24136,.F.);
#31922=ORIENTED_EDGE('',*,*,#24146,.T.);
#31923=ORIENTED_EDGE('',*,*,#24147,.T.);
#31924=ORIENTED_EDGE('',*,*,#24148,.T.);
#31925=ORIENTED_EDGE('',*,*,#24144,.T.);
#31926=ORIENTED_EDGE('',*,*,#24149,.T.);
#31927=ORIENTED_EDGE('',*,*,#24150,.T.);
#31928=ORIENTED_EDGE('',*,*,#24151,.T.);
#31929=ORIENTED_EDGE('',*,*,#24152,.T.);
#31930=ORIENTED_EDGE('',*,*,#24153,.F.);
#31931=ORIENTED_EDGE('',*,*,#24154,.T.);
#31932=ORIENTED_EDGE('',*,*,#24155,.T.);
#31933=ORIENTED_EDGE('',*,*,#24153,.T.);
#31934=ORIENTED_EDGE('',*,*,#24156,.T.);
#31935=ORIENTED_EDGE('',*,*,#24147,.F.);
#31936=ORIENTED_EDGE('',*,*,#24157,.T.);
#31937=ORIENTED_EDGE('',*,*,#24158,.F.);
#31938=ORIENTED_EDGE('',*,*,#24159,.T.);
#31939=ORIENTED_EDGE('',*,*,#24150,.F.);
#31940=ORIENTED_EDGE('',*,*,#24160,.T.);
#31941=ORIENTED_EDGE('',*,*,#24161,.T.);
#31942=ORIENTED_EDGE('',*,*,#24162,.T.);
#31943=ORIENTED_EDGE('',*,*,#24158,.T.);
#31944=ORIENTED_EDGE('',*,*,#24163,.T.);
#31945=ORIENTED_EDGE('',*,*,#24164,.T.);
#31946=ORIENTED_EDGE('',*,*,#24165,.T.);
#31947=ORIENTED_EDGE('',*,*,#24166,.T.);
#31948=ORIENTED_EDGE('',*,*,#24167,.F.);
#31949=ORIENTED_EDGE('',*,*,#24168,.T.);
#31950=ORIENTED_EDGE('',*,*,#24169,.T.);
#31951=ORIENTED_EDGE('',*,*,#24167,.T.);
#31952=ORIENTED_EDGE('',*,*,#24170,.T.);
#31953=ORIENTED_EDGE('',*,*,#24161,.F.);
#31954=ORIENTED_EDGE('',*,*,#24171,.T.);
#31955=ORIENTED_EDGE('',*,*,#21766,.F.);
#31956=ORIENTED_EDGE('',*,*,#24172,.T.);
#31957=ORIENTED_EDGE('',*,*,#24164,.F.);
#31958=ORIENTED_EDGE('',*,*,#24173,.T.);
#31959=ORIENTED_EDGE('',*,*,#21763,.F.);
#31960=ORIENTED_EDGE('',*,*,#24174,.T.);
#31961=ORIENTED_EDGE('',*,*,#24175,.T.);
#31962=ORIENTED_EDGE('',*,*,#24176,.F.);
#31963=ORIENTED_EDGE('',*,*,#24176,.T.);
#31964=ORIENTED_EDGE('',*,*,#24177,.T.);
#31965=ORIENTED_EDGE('',*,*,#21764,.F.);
#31966=ORIENTED_EDGE('',*,*,#24178,.T.);
#31967=ORIENTED_EDGE('',*,*,#24179,.T.);
#31968=ORIENTED_EDGE('',*,*,#21375,.F.);
#31969=ORIENTED_EDGE('',*,*,#24180,.F.);
#31970=ORIENTED_EDGE('',*,*,#24181,.T.);
#31971=ORIENTED_EDGE('',*,*,#24182,.T.);
#31972=ORIENTED_EDGE('',*,*,#24183,.F.);
#31973=ORIENTED_EDGE('',*,*,#24184,.T.);
#31974=ORIENTED_EDGE('',*,*,#24178,.F.);
#31975=ORIENTED_EDGE('',*,*,#24185,.T.);
#31976=ORIENTED_EDGE('',*,*,#24186,.T.);
#31977=ORIENTED_EDGE('',*,*,#24187,.T.);
#31978=ORIENTED_EDGE('',*,*,#24183,.T.);
#31979=ORIENTED_EDGE('',*,*,#24188,.T.);
#31980=ORIENTED_EDGE('',*,*,#24189,.T.);
#31981=ORIENTED_EDGE('',*,*,#24190,.T.);
#31982=ORIENTED_EDGE('',*,*,#24191,.T.);
#31983=ORIENTED_EDGE('',*,*,#24192,.F.);
#31984=ORIENTED_EDGE('',*,*,#24193,.T.);
#31985=ORIENTED_EDGE('',*,*,#24194,.T.);
#31986=ORIENTED_EDGE('',*,*,#24192,.T.);
#31987=ORIENTED_EDGE('',*,*,#24195,.T.);
#31988=ORIENTED_EDGE('',*,*,#24186,.F.);
#31989=ORIENTED_EDGE('',*,*,#24196,.T.);
#31990=ORIENTED_EDGE('',*,*,#21378,.F.);
#31991=ORIENTED_EDGE('',*,*,#24197,.T.);
#31992=ORIENTED_EDGE('',*,*,#24084,.T.);
#31993=ORIENTED_EDGE('',*,*,#24198,.F.);
#31994=ORIENTED_EDGE('',*,*,#24199,.T.);
#31995=ORIENTED_EDGE('',*,*,#24189,.F.);
#31996=ORIENTED_EDGE('',*,*,#24200,.T.);
#31997=ORIENTED_EDGE('',*,*,#24201,.T.);
#31998=ORIENTED_EDGE('',*,*,#24202,.T.);
#31999=ORIENTED_EDGE('',*,*,#24198,.T.);
#32000=ORIENTED_EDGE('',*,*,#24203,.T.);
#32001=ORIENTED_EDGE('',*,*,#24204,.T.);
#32002=ORIENTED_EDGE('',*,*,#24205,.T.);
#32003=ORIENTED_EDGE('',*,*,#24206,.T.);
#32004=ORIENTED_EDGE('',*,*,#24207,.F.);
#32005=ORIENTED_EDGE('',*,*,#24208,.T.);
#32006=ORIENTED_EDGE('',*,*,#24209,.T.);
#32007=ORIENTED_EDGE('',*,*,#24207,.T.);
#32008=ORIENTED_EDGE('',*,*,#24210,.T.);
#32009=ORIENTED_EDGE('',*,*,#24201,.F.);
#32010=ORIENTED_EDGE('',*,*,#24211,.T.);
#32011=ORIENTED_EDGE('',*,*,#24212,.F.);
#32012=ORIENTED_EDGE('',*,*,#24213,.T.);
#32013=ORIENTED_EDGE('',*,*,#24204,.F.);
#32014=ORIENTED_EDGE('',*,*,#24214,.T.);
#32015=ORIENTED_EDGE('',*,*,#24215,.T.);
#32016=ORIENTED_EDGE('',*,*,#24216,.T.);
#32017=ORIENTED_EDGE('',*,*,#24212,.T.);
#32018=ORIENTED_EDGE('',*,*,#24217,.T.);
#32019=ORIENTED_EDGE('',*,*,#24218,.T.);
#32020=ORIENTED_EDGE('',*,*,#24219,.T.);
#32021=ORIENTED_EDGE('',*,*,#24220,.T.);
#32022=ORIENTED_EDGE('',*,*,#24221,.F.);
#32023=ORIENTED_EDGE('',*,*,#24222,.T.);
#32024=ORIENTED_EDGE('',*,*,#24223,.T.);
#32025=ORIENTED_EDGE('',*,*,#24221,.T.);
#32026=ORIENTED_EDGE('',*,*,#24224,.T.);
#32027=ORIENTED_EDGE('',*,*,#24215,.F.);
#32028=ORIENTED_EDGE('',*,*,#24225,.T.);
#32029=ORIENTED_EDGE('',*,*,#24226,.F.);
#32030=ORIENTED_EDGE('',*,*,#24227,.T.);
#32031=ORIENTED_EDGE('',*,*,#24218,.F.);
#32032=ORIENTED_EDGE('',*,*,#24228,.T.);
#32033=ORIENTED_EDGE('',*,*,#24229,.T.);
#32034=ORIENTED_EDGE('',*,*,#24230,.T.);
#32035=ORIENTED_EDGE('',*,*,#24226,.T.);
#32036=ORIENTED_EDGE('',*,*,#24231,.T.);
#32037=ORIENTED_EDGE('',*,*,#24232,.T.);
#32038=ORIENTED_EDGE('',*,*,#24233,.T.);
#32039=ORIENTED_EDGE('',*,*,#24234,.T.);
#32040=ORIENTED_EDGE('',*,*,#24235,.F.);
#32041=ORIENTED_EDGE('',*,*,#24236,.T.);
#32042=ORIENTED_EDGE('',*,*,#24237,.T.);
#32043=ORIENTED_EDGE('',*,*,#24235,.T.);
#32044=ORIENTED_EDGE('',*,*,#24238,.T.);
#32045=ORIENTED_EDGE('',*,*,#24229,.F.);
#32046=ORIENTED_EDGE('',*,*,#24239,.T.);
#32047=ORIENTED_EDGE('',*,*,#24240,.F.);
#32048=ORIENTED_EDGE('',*,*,#24241,.T.);
#32049=ORIENTED_EDGE('',*,*,#24232,.F.);
#32050=ORIENTED_EDGE('',*,*,#24242,.T.);
#32051=ORIENTED_EDGE('',*,*,#24243,.T.);
#32052=ORIENTED_EDGE('',*,*,#24244,.T.);
#32053=ORIENTED_EDGE('',*,*,#24240,.T.);
#32054=ORIENTED_EDGE('',*,*,#24245,.T.);
#32055=ORIENTED_EDGE('',*,*,#24246,.T.);
#32056=ORIENTED_EDGE('',*,*,#24247,.T.);
#32057=ORIENTED_EDGE('',*,*,#24248,.T.);
#32058=ORIENTED_EDGE('',*,*,#24249,.F.);
#32059=ORIENTED_EDGE('',*,*,#24250,.T.);
#32060=ORIENTED_EDGE('',*,*,#24251,.T.);
#32061=ORIENTED_EDGE('',*,*,#24249,.T.);
#32062=ORIENTED_EDGE('',*,*,#24252,.T.);
#32063=ORIENTED_EDGE('',*,*,#24243,.F.);
#32064=ORIENTED_EDGE('',*,*,#24253,.T.);
#32065=ORIENTED_EDGE('',*,*,#24254,.F.);
#32066=ORIENTED_EDGE('',*,*,#24255,.T.);
#32067=ORIENTED_EDGE('',*,*,#24246,.F.);
#32068=ORIENTED_EDGE('',*,*,#24256,.T.);
#32069=ORIENTED_EDGE('',*,*,#24257,.T.);
#32070=ORIENTED_EDGE('',*,*,#24258,.T.);
#32071=ORIENTED_EDGE('',*,*,#24254,.T.);
#32072=ORIENTED_EDGE('',*,*,#24259,.T.);
#32073=ORIENTED_EDGE('',*,*,#24260,.T.);
#32074=ORIENTED_EDGE('',*,*,#24261,.T.);
#32075=ORIENTED_EDGE('',*,*,#24262,.T.);
#32076=ORIENTED_EDGE('',*,*,#24263,.F.);
#32077=ORIENTED_EDGE('',*,*,#24264,.T.);
#32078=ORIENTED_EDGE('',*,*,#24265,.T.);
#32079=ORIENTED_EDGE('',*,*,#24263,.T.);
#32080=ORIENTED_EDGE('',*,*,#24266,.T.);
#32081=ORIENTED_EDGE('',*,*,#24257,.F.);
#32082=ORIENTED_EDGE('',*,*,#24267,.T.);
#32083=ORIENTED_EDGE('',*,*,#21772,.F.);
#32084=ORIENTED_EDGE('',*,*,#24268,.T.);
#32085=ORIENTED_EDGE('',*,*,#24260,.F.);
#32086=ORIENTED_EDGE('',*,*,#24269,.T.);
#32087=ORIENTED_EDGE('',*,*,#21769,.F.);
#32088=ORIENTED_EDGE('',*,*,#24270,.T.);
#32089=ORIENTED_EDGE('',*,*,#24271,.T.);
#32090=ORIENTED_EDGE('',*,*,#24272,.F.);
#32091=ORIENTED_EDGE('',*,*,#24272,.T.);
#32092=ORIENTED_EDGE('',*,*,#24273,.T.);
#32093=ORIENTED_EDGE('',*,*,#21770,.F.);
#32094=ORIENTED_EDGE('',*,*,#24274,.T.);
#32095=ORIENTED_EDGE('',*,*,#24275,.T.);
#32096=ORIENTED_EDGE('',*,*,#21371,.F.);
#32097=ORIENTED_EDGE('',*,*,#24276,.F.);
#32098=ORIENTED_EDGE('',*,*,#24277,.T.);
#32099=ORIENTED_EDGE('',*,*,#24278,.T.);
#32100=ORIENTED_EDGE('',*,*,#24279,.F.);
#32101=ORIENTED_EDGE('',*,*,#24280,.T.);
#32102=ORIENTED_EDGE('',*,*,#24274,.F.);
#32103=ORIENTED_EDGE('',*,*,#24281,.T.);
#32104=ORIENTED_EDGE('',*,*,#24282,.T.);
#32105=ORIENTED_EDGE('',*,*,#24283,.T.);
#32106=ORIENTED_EDGE('',*,*,#24279,.T.);
#32107=ORIENTED_EDGE('',*,*,#24284,.T.);
#32108=ORIENTED_EDGE('',*,*,#24285,.T.);
#32109=ORIENTED_EDGE('',*,*,#24286,.T.);
#32110=ORIENTED_EDGE('',*,*,#24287,.T.);
#32111=ORIENTED_EDGE('',*,*,#24288,.F.);
#32112=ORIENTED_EDGE('',*,*,#24289,.T.);
#32113=ORIENTED_EDGE('',*,*,#24290,.T.);
#32114=ORIENTED_EDGE('',*,*,#24288,.T.);
#32115=ORIENTED_EDGE('',*,*,#24291,.T.);
#32116=ORIENTED_EDGE('',*,*,#24282,.F.);
#32117=ORIENTED_EDGE('',*,*,#24292,.T.);
#32118=ORIENTED_EDGE('',*,*,#21374,.F.);
#32119=ORIENTED_EDGE('',*,*,#24293,.T.);
#32120=ORIENTED_EDGE('',*,*,#24180,.T.);
#32121=ORIENTED_EDGE('',*,*,#24294,.F.);
#32122=ORIENTED_EDGE('',*,*,#24295,.T.);
#32123=ORIENTED_EDGE('',*,*,#24285,.F.);
#32124=ORIENTED_EDGE('',*,*,#24296,.T.);
#32125=ORIENTED_EDGE('',*,*,#24297,.T.);
#32126=ORIENTED_EDGE('',*,*,#24298,.T.);
#32127=ORIENTED_EDGE('',*,*,#24294,.T.);
#32128=ORIENTED_EDGE('',*,*,#24299,.T.);
#32129=ORIENTED_EDGE('',*,*,#24300,.T.);
#32130=ORIENTED_EDGE('',*,*,#24301,.T.);
#32131=ORIENTED_EDGE('',*,*,#24302,.T.);
#32132=ORIENTED_EDGE('',*,*,#24303,.F.);
#32133=ORIENTED_EDGE('',*,*,#24304,.T.);
#32134=ORIENTED_EDGE('',*,*,#24305,.T.);
#32135=ORIENTED_EDGE('',*,*,#24303,.T.);
#32136=ORIENTED_EDGE('',*,*,#24306,.T.);
#32137=ORIENTED_EDGE('',*,*,#24297,.F.);
#32138=ORIENTED_EDGE('',*,*,#24307,.T.);
#32139=ORIENTED_EDGE('',*,*,#24308,.F.);
#32140=ORIENTED_EDGE('',*,*,#24309,.T.);
#32141=ORIENTED_EDGE('',*,*,#24300,.F.);
#32142=ORIENTED_EDGE('',*,*,#24310,.T.);
#32143=ORIENTED_EDGE('',*,*,#24311,.T.);
#32144=ORIENTED_EDGE('',*,*,#24312,.T.);
#32145=ORIENTED_EDGE('',*,*,#24308,.T.);
#32146=ORIENTED_EDGE('',*,*,#24313,.T.);
#32147=ORIENTED_EDGE('',*,*,#24314,.T.);
#32148=ORIENTED_EDGE('',*,*,#24315,.T.);
#32149=ORIENTED_EDGE('',*,*,#24316,.T.);
#32150=ORIENTED_EDGE('',*,*,#24317,.F.);
#32151=ORIENTED_EDGE('',*,*,#24318,.T.);
#32152=ORIENTED_EDGE('',*,*,#24319,.T.);
#32153=ORIENTED_EDGE('',*,*,#24317,.T.);
#32154=ORIENTED_EDGE('',*,*,#24320,.T.);
#32155=ORIENTED_EDGE('',*,*,#24311,.F.);
#32156=ORIENTED_EDGE('',*,*,#24321,.T.);
#32157=ORIENTED_EDGE('',*,*,#24322,.F.);
#32158=ORIENTED_EDGE('',*,*,#24323,.T.);
#32159=ORIENTED_EDGE('',*,*,#24314,.F.);
#32160=ORIENTED_EDGE('',*,*,#24324,.T.);
#32161=ORIENTED_EDGE('',*,*,#24325,.T.);
#32162=ORIENTED_EDGE('',*,*,#24326,.T.);
#32163=ORIENTED_EDGE('',*,*,#24322,.T.);
#32164=ORIENTED_EDGE('',*,*,#24327,.T.);
#32165=ORIENTED_EDGE('',*,*,#24328,.T.);
#32166=ORIENTED_EDGE('',*,*,#24329,.T.);
#32167=ORIENTED_EDGE('',*,*,#24330,.T.);
#32168=ORIENTED_EDGE('',*,*,#24331,.F.);
#32169=ORIENTED_EDGE('',*,*,#24332,.T.);
#32170=ORIENTED_EDGE('',*,*,#24333,.T.);
#32171=ORIENTED_EDGE('',*,*,#24331,.T.);
#32172=ORIENTED_EDGE('',*,*,#24334,.T.);
#32173=ORIENTED_EDGE('',*,*,#24325,.F.);
#32174=ORIENTED_EDGE('',*,*,#24335,.T.);
#32175=ORIENTED_EDGE('',*,*,#24336,.F.);
#32176=ORIENTED_EDGE('',*,*,#24337,.T.);
#32177=ORIENTED_EDGE('',*,*,#24328,.F.);
#32178=ORIENTED_EDGE('',*,*,#24338,.T.);
#32179=ORIENTED_EDGE('',*,*,#24339,.T.);
#32180=ORIENTED_EDGE('',*,*,#24340,.T.);
#32181=ORIENTED_EDGE('',*,*,#24336,.T.);
#32182=ORIENTED_EDGE('',*,*,#24341,.T.);
#32183=ORIENTED_EDGE('',*,*,#24342,.T.);
#32184=ORIENTED_EDGE('',*,*,#24343,.T.);
#32185=ORIENTED_EDGE('',*,*,#24344,.T.);
#32186=ORIENTED_EDGE('',*,*,#24345,.F.);
#32187=ORIENTED_EDGE('',*,*,#24346,.T.);
#32188=ORIENTED_EDGE('',*,*,#24347,.T.);
#32189=ORIENTED_EDGE('',*,*,#24345,.T.);
#32190=ORIENTED_EDGE('',*,*,#24348,.T.);
#32191=ORIENTED_EDGE('',*,*,#24339,.F.);
#32192=ORIENTED_EDGE('',*,*,#24349,.T.);
#32193=ORIENTED_EDGE('',*,*,#24350,.F.);
#32194=ORIENTED_EDGE('',*,*,#24351,.T.);
#32195=ORIENTED_EDGE('',*,*,#24342,.F.);
#32196=ORIENTED_EDGE('',*,*,#24352,.T.);
#32197=ORIENTED_EDGE('',*,*,#24353,.T.);
#32198=ORIENTED_EDGE('',*,*,#24354,.T.);
#32199=ORIENTED_EDGE('',*,*,#24350,.T.);
#32200=ORIENTED_EDGE('',*,*,#24355,.T.);
#32201=ORIENTED_EDGE('',*,*,#24356,.T.);
#32202=ORIENTED_EDGE('',*,*,#24357,.T.);
#32203=ORIENTED_EDGE('',*,*,#24358,.T.);
#32204=ORIENTED_EDGE('',*,*,#24359,.F.);
#32205=ORIENTED_EDGE('',*,*,#24360,.T.);
#32206=ORIENTED_EDGE('',*,*,#24361,.T.);
#32207=ORIENTED_EDGE('',*,*,#24359,.T.);
#32208=ORIENTED_EDGE('',*,*,#24362,.T.);
#32209=ORIENTED_EDGE('',*,*,#24353,.F.);
#32210=ORIENTED_EDGE('',*,*,#24363,.T.);
#32211=ORIENTED_EDGE('',*,*,#21778,.F.);
#32212=ORIENTED_EDGE('',*,*,#24364,.T.);
#32213=ORIENTED_EDGE('',*,*,#24356,.F.);
#32214=ORIENTED_EDGE('',*,*,#24365,.T.);
#32215=ORIENTED_EDGE('',*,*,#21775,.F.);
#32216=ORIENTED_EDGE('',*,*,#24366,.T.);
#32217=ORIENTED_EDGE('',*,*,#24367,.T.);
#32218=ORIENTED_EDGE('',*,*,#24368,.F.);
#32219=ORIENTED_EDGE('',*,*,#24368,.T.);
#32220=ORIENTED_EDGE('',*,*,#24369,.T.);
#32221=ORIENTED_EDGE('',*,*,#21776,.F.);
#32222=ORIENTED_EDGE('',*,*,#24370,.T.);
#32223=ORIENTED_EDGE('',*,*,#24371,.T.);
#32224=ORIENTED_EDGE('',*,*,#21367,.F.);
#32225=ORIENTED_EDGE('',*,*,#24372,.F.);
#32226=ORIENTED_EDGE('',*,*,#24373,.T.);
#32227=ORIENTED_EDGE('',*,*,#24374,.T.);
#32228=ORIENTED_EDGE('',*,*,#24375,.F.);
#32229=ORIENTED_EDGE('',*,*,#24376,.T.);
#32230=ORIENTED_EDGE('',*,*,#24370,.F.);
#32231=ORIENTED_EDGE('',*,*,#24377,.T.);
#32232=ORIENTED_EDGE('',*,*,#24378,.T.);
#32233=ORIENTED_EDGE('',*,*,#24379,.T.);
#32234=ORIENTED_EDGE('',*,*,#24375,.T.);
#32235=ORIENTED_EDGE('',*,*,#24380,.T.);
#32236=ORIENTED_EDGE('',*,*,#24381,.T.);
#32237=ORIENTED_EDGE('',*,*,#24382,.T.);
#32238=ORIENTED_EDGE('',*,*,#24383,.T.);
#32239=ORIENTED_EDGE('',*,*,#24384,.F.);
#32240=ORIENTED_EDGE('',*,*,#24385,.T.);
#32241=ORIENTED_EDGE('',*,*,#24386,.T.);
#32242=ORIENTED_EDGE('',*,*,#24384,.T.);
#32243=ORIENTED_EDGE('',*,*,#24387,.T.);
#32244=ORIENTED_EDGE('',*,*,#24378,.F.);
#32245=ORIENTED_EDGE('',*,*,#24388,.T.);
#32246=ORIENTED_EDGE('',*,*,#21370,.F.);
#32247=ORIENTED_EDGE('',*,*,#24389,.T.);
#32248=ORIENTED_EDGE('',*,*,#24276,.T.);
#32249=ORIENTED_EDGE('',*,*,#24390,.F.);
#32250=ORIENTED_EDGE('',*,*,#24391,.T.);
#32251=ORIENTED_EDGE('',*,*,#24381,.F.);
#32252=ORIENTED_EDGE('',*,*,#24392,.T.);
#32253=ORIENTED_EDGE('',*,*,#24393,.T.);
#32254=ORIENTED_EDGE('',*,*,#24394,.T.);
#32255=ORIENTED_EDGE('',*,*,#24390,.T.);
#32256=ORIENTED_EDGE('',*,*,#24395,.T.);
#32257=ORIENTED_EDGE('',*,*,#24396,.T.);
#32258=ORIENTED_EDGE('',*,*,#24397,.T.);
#32259=ORIENTED_EDGE('',*,*,#24398,.T.);
#32260=ORIENTED_EDGE('',*,*,#24399,.F.);
#32261=ORIENTED_EDGE('',*,*,#24400,.T.);
#32262=ORIENTED_EDGE('',*,*,#24401,.T.);
#32263=ORIENTED_EDGE('',*,*,#24399,.T.);
#32264=ORIENTED_EDGE('',*,*,#24402,.T.);
#32265=ORIENTED_EDGE('',*,*,#24393,.F.);
#32266=ORIENTED_EDGE('',*,*,#24403,.T.);
#32267=ORIENTED_EDGE('',*,*,#24404,.F.);
#32268=ORIENTED_EDGE('',*,*,#24405,.T.);
#32269=ORIENTED_EDGE('',*,*,#24396,.F.);
#32270=ORIENTED_EDGE('',*,*,#24406,.T.);
#32271=ORIENTED_EDGE('',*,*,#24407,.T.);
#32272=ORIENTED_EDGE('',*,*,#24408,.T.);
#32273=ORIENTED_EDGE('',*,*,#24404,.T.);
#32274=ORIENTED_EDGE('',*,*,#24409,.T.);
#32275=ORIENTED_EDGE('',*,*,#24410,.T.);
#32276=ORIENTED_EDGE('',*,*,#24411,.T.);
#32277=ORIENTED_EDGE('',*,*,#24412,.T.);
#32278=ORIENTED_EDGE('',*,*,#24413,.F.);
#32279=ORIENTED_EDGE('',*,*,#24414,.T.);
#32280=ORIENTED_EDGE('',*,*,#24415,.T.);
#32281=ORIENTED_EDGE('',*,*,#24413,.T.);
#32282=ORIENTED_EDGE('',*,*,#24416,.T.);
#32283=ORIENTED_EDGE('',*,*,#24407,.F.);
#32284=ORIENTED_EDGE('',*,*,#24417,.T.);
#32285=ORIENTED_EDGE('',*,*,#24418,.F.);
#32286=ORIENTED_EDGE('',*,*,#24419,.T.);
#32287=ORIENTED_EDGE('',*,*,#24410,.F.);
#32288=ORIENTED_EDGE('',*,*,#24420,.T.);
#32289=ORIENTED_EDGE('',*,*,#24421,.T.);
#32290=ORIENTED_EDGE('',*,*,#24422,.T.);
#32291=ORIENTED_EDGE('',*,*,#24418,.T.);
#32292=ORIENTED_EDGE('',*,*,#24423,.T.);
#32293=ORIENTED_EDGE('',*,*,#24424,.T.);
#32294=ORIENTED_EDGE('',*,*,#24425,.T.);
#32295=ORIENTED_EDGE('',*,*,#24426,.T.);
#32296=ORIENTED_EDGE('',*,*,#24427,.F.);
#32297=ORIENTED_EDGE('',*,*,#24428,.T.);
#32298=ORIENTED_EDGE('',*,*,#24429,.T.);
#32299=ORIENTED_EDGE('',*,*,#24427,.T.);
#32300=ORIENTED_EDGE('',*,*,#24430,.T.);
#32301=ORIENTED_EDGE('',*,*,#24421,.F.);
#32302=ORIENTED_EDGE('',*,*,#24431,.T.);
#32303=ORIENTED_EDGE('',*,*,#24432,.F.);
#32304=ORIENTED_EDGE('',*,*,#24433,.T.);
#32305=ORIENTED_EDGE('',*,*,#24424,.F.);
#32306=ORIENTED_EDGE('',*,*,#24434,.T.);
#32307=ORIENTED_EDGE('',*,*,#24435,.T.);
#32308=ORIENTED_EDGE('',*,*,#24436,.T.);
#32309=ORIENTED_EDGE('',*,*,#24432,.T.);
#32310=ORIENTED_EDGE('',*,*,#24437,.T.);
#32311=ORIENTED_EDGE('',*,*,#24438,.T.);
#32312=ORIENTED_EDGE('',*,*,#24439,.T.);
#32313=ORIENTED_EDGE('',*,*,#24440,.T.);
#32314=ORIENTED_EDGE('',*,*,#24441,.F.);
#32315=ORIENTED_EDGE('',*,*,#24442,.T.);
#32316=ORIENTED_EDGE('',*,*,#24443,.T.);
#32317=ORIENTED_EDGE('',*,*,#24441,.T.);
#32318=ORIENTED_EDGE('',*,*,#24444,.T.);
#32319=ORIENTED_EDGE('',*,*,#24435,.F.);
#32320=ORIENTED_EDGE('',*,*,#24445,.T.);
#32321=ORIENTED_EDGE('',*,*,#24446,.F.);
#32322=ORIENTED_EDGE('',*,*,#24447,.T.);
#32323=ORIENTED_EDGE('',*,*,#24438,.F.);
#32324=ORIENTED_EDGE('',*,*,#24448,.T.);
#32325=ORIENTED_EDGE('',*,*,#24449,.T.);
#32326=ORIENTED_EDGE('',*,*,#24450,.T.);
#32327=ORIENTED_EDGE('',*,*,#24446,.T.);
#32328=ORIENTED_EDGE('',*,*,#24451,.T.);
#32329=ORIENTED_EDGE('',*,*,#24452,.T.);
#32330=ORIENTED_EDGE('',*,*,#24453,.T.);
#32331=ORIENTED_EDGE('',*,*,#24454,.T.);
#32332=ORIENTED_EDGE('',*,*,#24455,.F.);
#32333=ORIENTED_EDGE('',*,*,#24456,.T.);
#32334=ORIENTED_EDGE('',*,*,#24457,.T.);
#32335=ORIENTED_EDGE('',*,*,#24455,.T.);
#32336=ORIENTED_EDGE('',*,*,#24458,.T.);
#32337=ORIENTED_EDGE('',*,*,#24449,.F.);
#32338=ORIENTED_EDGE('',*,*,#24459,.T.);
#32339=ORIENTED_EDGE('',*,*,#21484,.F.);
#32340=ORIENTED_EDGE('',*,*,#24460,.T.);
#32341=ORIENTED_EDGE('',*,*,#24452,.F.);
#32342=ORIENTED_EDGE('',*,*,#24461,.T.);
#32343=ORIENTED_EDGE('',*,*,#21781,.F.);
#32344=ORIENTED_EDGE('',*,*,#24462,.T.);
#32345=ORIENTED_EDGE('',*,*,#24463,.T.);
#32346=ORIENTED_EDGE('',*,*,#24464,.F.);
#32347=ORIENTED_EDGE('',*,*,#24464,.T.);
#32348=ORIENTED_EDGE('',*,*,#24465,.T.);
#32349=ORIENTED_EDGE('',*,*,#21782,.F.);
#32350=ORIENTED_EDGE('',*,*,#24466,.T.);
#32351=ORIENTED_EDGE('',*,*,#24467,.T.);
#32352=ORIENTED_EDGE('',*,*,#21363,.F.);
#32353=ORIENTED_EDGE('',*,*,#24468,.F.);
#32354=ORIENTED_EDGE('',*,*,#24469,.T.);
#32355=ORIENTED_EDGE('',*,*,#24470,.T.);
#32356=ORIENTED_EDGE('',*,*,#24471,.F.);
#32357=ORIENTED_EDGE('',*,*,#24472,.T.);
#32358=ORIENTED_EDGE('',*,*,#24466,.F.);
#32359=ORIENTED_EDGE('',*,*,#24473,.T.);
#32360=ORIENTED_EDGE('',*,*,#24474,.T.);
#32361=ORIENTED_EDGE('',*,*,#24475,.T.);
#32362=ORIENTED_EDGE('',*,*,#24471,.T.);
#32363=ORIENTED_EDGE('',*,*,#24476,.T.);
#32364=ORIENTED_EDGE('',*,*,#24477,.T.);
#32365=ORIENTED_EDGE('',*,*,#24478,.T.);
#32366=ORIENTED_EDGE('',*,*,#24479,.T.);
#32367=ORIENTED_EDGE('',*,*,#24480,.F.);
#32368=ORIENTED_EDGE('',*,*,#24481,.T.);
#32369=ORIENTED_EDGE('',*,*,#24482,.T.);
#32370=ORIENTED_EDGE('',*,*,#24480,.T.);
#32371=ORIENTED_EDGE('',*,*,#24483,.T.);
#32372=ORIENTED_EDGE('',*,*,#24474,.F.);
#32373=ORIENTED_EDGE('',*,*,#24484,.T.);
#32374=ORIENTED_EDGE('',*,*,#21366,.F.);
#32375=ORIENTED_EDGE('',*,*,#24485,.T.);
#32376=ORIENTED_EDGE('',*,*,#24372,.T.);
#32377=ORIENTED_EDGE('',*,*,#24486,.F.);
#32378=ORIENTED_EDGE('',*,*,#24487,.T.);
#32379=ORIENTED_EDGE('',*,*,#24477,.F.);
#32380=ORIENTED_EDGE('',*,*,#24488,.T.);
#32381=ORIENTED_EDGE('',*,*,#24489,.T.);
#32382=ORIENTED_EDGE('',*,*,#24490,.T.);
#32383=ORIENTED_EDGE('',*,*,#24486,.T.);
#32384=ORIENTED_EDGE('',*,*,#24491,.T.);
#32385=ORIENTED_EDGE('',*,*,#24492,.T.);
#32386=ORIENTED_EDGE('',*,*,#24493,.T.);
#32387=ORIENTED_EDGE('',*,*,#24494,.T.);
#32388=ORIENTED_EDGE('',*,*,#24495,.F.);
#32389=ORIENTED_EDGE('',*,*,#24496,.T.);
#32390=ORIENTED_EDGE('',*,*,#24497,.T.);
#32391=ORIENTED_EDGE('',*,*,#24495,.T.);
#32392=ORIENTED_EDGE('',*,*,#24498,.T.);
#32393=ORIENTED_EDGE('',*,*,#24489,.F.);
#32394=ORIENTED_EDGE('',*,*,#24499,.T.);
#32395=ORIENTED_EDGE('',*,*,#24500,.F.);
#32396=ORIENTED_EDGE('',*,*,#24501,.T.);
#32397=ORIENTED_EDGE('',*,*,#24492,.F.);
#32398=ORIENTED_EDGE('',*,*,#24502,.T.);
#32399=ORIENTED_EDGE('',*,*,#24503,.T.);
#32400=ORIENTED_EDGE('',*,*,#24504,.T.);
#32401=ORIENTED_EDGE('',*,*,#24500,.T.);
#32402=ORIENTED_EDGE('',*,*,#24505,.T.);
#32403=ORIENTED_EDGE('',*,*,#24506,.T.);
#32404=ORIENTED_EDGE('',*,*,#24507,.T.);
#32405=ORIENTED_EDGE('',*,*,#24508,.T.);
#32406=ORIENTED_EDGE('',*,*,#24509,.F.);
#32407=ORIENTED_EDGE('',*,*,#24510,.T.);
#32408=ORIENTED_EDGE('',*,*,#24511,.T.);
#32409=ORIENTED_EDGE('',*,*,#24509,.T.);
#32410=ORIENTED_EDGE('',*,*,#24512,.T.);
#32411=ORIENTED_EDGE('',*,*,#24503,.F.);
#32412=ORIENTED_EDGE('',*,*,#24513,.T.);
#32413=ORIENTED_EDGE('',*,*,#24514,.F.);
#32414=ORIENTED_EDGE('',*,*,#24515,.T.);
#32415=ORIENTED_EDGE('',*,*,#24506,.F.);
#32416=ORIENTED_EDGE('',*,*,#24516,.T.);
#32417=ORIENTED_EDGE('',*,*,#24517,.T.);
#32418=ORIENTED_EDGE('',*,*,#24518,.T.);
#32419=ORIENTED_EDGE('',*,*,#24514,.T.);
#32420=ORIENTED_EDGE('',*,*,#24519,.T.);
#32421=ORIENTED_EDGE('',*,*,#24520,.T.);
#32422=ORIENTED_EDGE('',*,*,#24521,.T.);
#32423=ORIENTED_EDGE('',*,*,#24522,.T.);
#32424=ORIENTED_EDGE('',*,*,#24523,.F.);
#32425=ORIENTED_EDGE('',*,*,#24524,.T.);
#32426=ORIENTED_EDGE('',*,*,#24525,.T.);
#32427=ORIENTED_EDGE('',*,*,#24523,.T.);
#32428=ORIENTED_EDGE('',*,*,#24526,.T.);
#32429=ORIENTED_EDGE('',*,*,#24517,.F.);
#32430=ORIENTED_EDGE('',*,*,#24527,.T.);
#32431=ORIENTED_EDGE('',*,*,#24528,.F.);
#32432=ORIENTED_EDGE('',*,*,#24529,.T.);
#32433=ORIENTED_EDGE('',*,*,#24520,.F.);
#32434=ORIENTED_EDGE('',*,*,#24530,.T.);
#32435=ORIENTED_EDGE('',*,*,#24531,.T.);
#32436=ORIENTED_EDGE('',*,*,#24532,.T.);
#32437=ORIENTED_EDGE('',*,*,#24528,.T.);
#32438=ORIENTED_EDGE('',*,*,#24533,.T.);
#32439=ORIENTED_EDGE('',*,*,#24534,.T.);
#32440=ORIENTED_EDGE('',*,*,#24535,.T.);
#32441=ORIENTED_EDGE('',*,*,#24536,.T.);
#32442=ORIENTED_EDGE('',*,*,#24537,.F.);
#32443=ORIENTED_EDGE('',*,*,#24538,.T.);
#32444=ORIENTED_EDGE('',*,*,#24539,.T.);
#32445=ORIENTED_EDGE('',*,*,#24537,.T.);
#32446=ORIENTED_EDGE('',*,*,#24540,.T.);
#32447=ORIENTED_EDGE('',*,*,#24531,.F.);
#32448=ORIENTED_EDGE('',*,*,#24541,.T.);
#32449=ORIENTED_EDGE('',*,*,#24542,.F.);
#32450=ORIENTED_EDGE('',*,*,#24543,.T.);
#32451=ORIENTED_EDGE('',*,*,#24534,.F.);
#32452=ORIENTED_EDGE('',*,*,#24544,.T.);
#32453=ORIENTED_EDGE('',*,*,#24545,.T.);
#32454=ORIENTED_EDGE('',*,*,#24546,.T.);
#32455=ORIENTED_EDGE('',*,*,#24542,.T.);
#32456=ORIENTED_EDGE('',*,*,#24547,.T.);
#32457=ORIENTED_EDGE('',*,*,#24548,.T.);
#32458=ORIENTED_EDGE('',*,*,#24549,.T.);
#32459=ORIENTED_EDGE('',*,*,#24550,.T.);
#32460=ORIENTED_EDGE('',*,*,#24551,.F.);
#32461=ORIENTED_EDGE('',*,*,#24552,.T.);
#32462=ORIENTED_EDGE('',*,*,#24553,.T.);
#32463=ORIENTED_EDGE('',*,*,#24551,.T.);
#32464=ORIENTED_EDGE('',*,*,#24554,.T.);
#32465=ORIENTED_EDGE('',*,*,#24545,.F.);
#32466=ORIENTED_EDGE('',*,*,#24555,.T.);
#32467=ORIENTED_EDGE('',*,*,#21490,.F.);
#32468=ORIENTED_EDGE('',*,*,#24556,.T.);
#32469=ORIENTED_EDGE('',*,*,#24548,.F.);
#32470=ORIENTED_EDGE('',*,*,#24557,.T.);
#32471=ORIENTED_EDGE('',*,*,#21487,.F.);
#32472=ORIENTED_EDGE('',*,*,#24558,.T.);
#32473=ORIENTED_EDGE('',*,*,#24559,.T.);
#32474=ORIENTED_EDGE('',*,*,#24560,.F.);
#32475=ORIENTED_EDGE('',*,*,#24560,.T.);
#32476=ORIENTED_EDGE('',*,*,#24561,.T.);
#32477=ORIENTED_EDGE('',*,*,#21488,.F.);
#32478=ORIENTED_EDGE('',*,*,#24562,.T.);
#32479=ORIENTED_EDGE('',*,*,#24563,.T.);
#32480=ORIENTED_EDGE('',*,*,#21359,.F.);
#32481=ORIENTED_EDGE('',*,*,#24564,.F.);
#32482=ORIENTED_EDGE('',*,*,#24565,.T.);
#32483=ORIENTED_EDGE('',*,*,#24566,.T.);
#32484=ORIENTED_EDGE('',*,*,#24567,.F.);
#32485=ORIENTED_EDGE('',*,*,#24568,.T.);
#32486=ORIENTED_EDGE('',*,*,#24562,.F.);
#32487=ORIENTED_EDGE('',*,*,#24569,.T.);
#32488=ORIENTED_EDGE('',*,*,#24570,.T.);
#32489=ORIENTED_EDGE('',*,*,#24571,.T.);
#32490=ORIENTED_EDGE('',*,*,#24567,.T.);
#32491=ORIENTED_EDGE('',*,*,#24572,.T.);
#32492=ORIENTED_EDGE('',*,*,#24573,.T.);
#32493=ORIENTED_EDGE('',*,*,#24574,.T.);
#32494=ORIENTED_EDGE('',*,*,#24575,.T.);
#32495=ORIENTED_EDGE('',*,*,#24576,.F.);
#32496=ORIENTED_EDGE('',*,*,#24577,.T.);
#32497=ORIENTED_EDGE('',*,*,#24578,.T.);
#32498=ORIENTED_EDGE('',*,*,#24576,.T.);
#32499=ORIENTED_EDGE('',*,*,#24579,.T.);
#32500=ORIENTED_EDGE('',*,*,#24570,.F.);
#32501=ORIENTED_EDGE('',*,*,#24580,.T.);
#32502=ORIENTED_EDGE('',*,*,#21362,.F.);
#32503=ORIENTED_EDGE('',*,*,#24581,.T.);
#32504=ORIENTED_EDGE('',*,*,#24468,.T.);
#32505=ORIENTED_EDGE('',*,*,#24582,.F.);
#32506=ORIENTED_EDGE('',*,*,#24583,.T.);
#32507=ORIENTED_EDGE('',*,*,#24573,.F.);
#32508=ORIENTED_EDGE('',*,*,#24584,.T.);
#32509=ORIENTED_EDGE('',*,*,#24585,.T.);
#32510=ORIENTED_EDGE('',*,*,#24586,.T.);
#32511=ORIENTED_EDGE('',*,*,#24582,.T.);
#32512=ORIENTED_EDGE('',*,*,#24587,.T.);
#32513=ORIENTED_EDGE('',*,*,#24588,.T.);
#32514=ORIENTED_EDGE('',*,*,#24589,.T.);
#32515=ORIENTED_EDGE('',*,*,#24590,.T.);
#32516=ORIENTED_EDGE('',*,*,#24591,.F.);
#32517=ORIENTED_EDGE('',*,*,#24592,.T.);
#32518=ORIENTED_EDGE('',*,*,#24593,.T.);
#32519=ORIENTED_EDGE('',*,*,#24591,.T.);
#32520=ORIENTED_EDGE('',*,*,#24594,.T.);
#32521=ORIENTED_EDGE('',*,*,#24585,.F.);
#32522=ORIENTED_EDGE('',*,*,#24595,.T.);
#32523=ORIENTED_EDGE('',*,*,#24596,.F.);
#32524=ORIENTED_EDGE('',*,*,#24597,.T.);
#32525=ORIENTED_EDGE('',*,*,#24588,.F.);
#32526=ORIENTED_EDGE('',*,*,#24598,.T.);
#32527=ORIENTED_EDGE('',*,*,#24599,.T.);
#32528=ORIENTED_EDGE('',*,*,#24600,.T.);
#32529=ORIENTED_EDGE('',*,*,#24596,.T.);
#32530=ORIENTED_EDGE('',*,*,#24601,.T.);
#32531=ORIENTED_EDGE('',*,*,#24602,.T.);
#32532=ORIENTED_EDGE('',*,*,#24603,.T.);
#32533=ORIENTED_EDGE('',*,*,#24604,.T.);
#32534=ORIENTED_EDGE('',*,*,#24605,.F.);
#32535=ORIENTED_EDGE('',*,*,#24606,.T.);
#32536=ORIENTED_EDGE('',*,*,#24607,.T.);
#32537=ORIENTED_EDGE('',*,*,#24605,.T.);
#32538=ORIENTED_EDGE('',*,*,#24608,.T.);
#32539=ORIENTED_EDGE('',*,*,#24599,.F.);
#32540=ORIENTED_EDGE('',*,*,#24609,.T.);
#32541=ORIENTED_EDGE('',*,*,#24610,.F.);
#32542=ORIENTED_EDGE('',*,*,#24611,.T.);
#32543=ORIENTED_EDGE('',*,*,#24602,.F.);
#32544=ORIENTED_EDGE('',*,*,#24612,.T.);
#32545=ORIENTED_EDGE('',*,*,#24613,.T.);
#32546=ORIENTED_EDGE('',*,*,#24614,.T.);
#32547=ORIENTED_EDGE('',*,*,#24610,.T.);
#32548=ORIENTED_EDGE('',*,*,#24615,.T.);
#32549=ORIENTED_EDGE('',*,*,#24616,.T.);
#32550=ORIENTED_EDGE('',*,*,#24617,.T.);
#32551=ORIENTED_EDGE('',*,*,#24618,.T.);
#32552=ORIENTED_EDGE('',*,*,#24619,.F.);
#32553=ORIENTED_EDGE('',*,*,#24620,.T.);
#32554=ORIENTED_EDGE('',*,*,#24621,.T.);
#32555=ORIENTED_EDGE('',*,*,#24619,.T.);
#32556=ORIENTED_EDGE('',*,*,#24622,.T.);
#32557=ORIENTED_EDGE('',*,*,#24613,.F.);
#32558=ORIENTED_EDGE('',*,*,#24623,.T.);
#32559=ORIENTED_EDGE('',*,*,#24624,.F.);
#32560=ORIENTED_EDGE('',*,*,#24625,.T.);
#32561=ORIENTED_EDGE('',*,*,#24616,.F.);
#32562=ORIENTED_EDGE('',*,*,#24626,.T.);
#32563=ORIENTED_EDGE('',*,*,#24627,.T.);
#32564=ORIENTED_EDGE('',*,*,#24628,.T.);
#32565=ORIENTED_EDGE('',*,*,#24624,.T.);
#32566=ORIENTED_EDGE('',*,*,#24629,.T.);
#32567=ORIENTED_EDGE('',*,*,#24630,.T.);
#32568=ORIENTED_EDGE('',*,*,#24631,.T.);
#32569=ORIENTED_EDGE('',*,*,#24632,.T.);
#32570=ORIENTED_EDGE('',*,*,#24633,.F.);
#32571=ORIENTED_EDGE('',*,*,#24634,.T.);
#32572=ORIENTED_EDGE('',*,*,#24635,.T.);
#32573=ORIENTED_EDGE('',*,*,#24633,.T.);
#32574=ORIENTED_EDGE('',*,*,#24636,.T.);
#32575=ORIENTED_EDGE('',*,*,#24627,.F.);
#32576=ORIENTED_EDGE('',*,*,#24637,.T.);
#32577=ORIENTED_EDGE('',*,*,#24638,.F.);
#32578=ORIENTED_EDGE('',*,*,#24639,.T.);
#32579=ORIENTED_EDGE('',*,*,#24630,.F.);
#32580=ORIENTED_EDGE('',*,*,#24640,.T.);
#32581=ORIENTED_EDGE('',*,*,#24641,.T.);
#32582=ORIENTED_EDGE('',*,*,#24642,.T.);
#32583=ORIENTED_EDGE('',*,*,#24638,.T.);
#32584=ORIENTED_EDGE('',*,*,#24643,.T.);
#32585=ORIENTED_EDGE('',*,*,#24644,.T.);
#32586=ORIENTED_EDGE('',*,*,#24645,.T.);
#32587=ORIENTED_EDGE('',*,*,#24646,.T.);
#32588=ORIENTED_EDGE('',*,*,#24647,.F.);
#32589=ORIENTED_EDGE('',*,*,#24648,.T.);
#32590=ORIENTED_EDGE('',*,*,#24649,.T.);
#32591=ORIENTED_EDGE('',*,*,#24647,.T.);
#32592=ORIENTED_EDGE('',*,*,#24650,.T.);
#32593=ORIENTED_EDGE('',*,*,#24641,.F.);
#32594=ORIENTED_EDGE('',*,*,#24651,.T.);
#32595=ORIENTED_EDGE('',*,*,#21496,.F.);
#32596=ORIENTED_EDGE('',*,*,#24652,.T.);
#32597=ORIENTED_EDGE('',*,*,#24644,.F.);
#32598=ORIENTED_EDGE('',*,*,#24653,.T.);
#32599=ORIENTED_EDGE('',*,*,#21493,.F.);
#32600=ORIENTED_EDGE('',*,*,#24654,.T.);
#32601=ORIENTED_EDGE('',*,*,#24655,.T.);
#32602=ORIENTED_EDGE('',*,*,#24656,.F.);
#32603=ORIENTED_EDGE('',*,*,#24656,.T.);
#32604=ORIENTED_EDGE('',*,*,#24657,.T.);
#32605=ORIENTED_EDGE('',*,*,#21494,.F.);
#32606=ORIENTED_EDGE('',*,*,#24658,.T.);
#32607=ORIENTED_EDGE('',*,*,#24659,.T.);
#32608=ORIENTED_EDGE('',*,*,#21355,.F.);
#32609=ORIENTED_EDGE('',*,*,#24660,.F.);
#32610=ORIENTED_EDGE('',*,*,#24661,.T.);
#32611=ORIENTED_EDGE('',*,*,#24662,.T.);
#32612=ORIENTED_EDGE('',*,*,#24663,.F.);
#32613=ORIENTED_EDGE('',*,*,#24664,.T.);
#32614=ORIENTED_EDGE('',*,*,#24658,.F.);
#32615=ORIENTED_EDGE('',*,*,#24665,.T.);
#32616=ORIENTED_EDGE('',*,*,#24666,.T.);
#32617=ORIENTED_EDGE('',*,*,#24667,.T.);
#32618=ORIENTED_EDGE('',*,*,#24663,.T.);
#32619=ORIENTED_EDGE('',*,*,#24668,.T.);
#32620=ORIENTED_EDGE('',*,*,#24669,.T.);
#32621=ORIENTED_EDGE('',*,*,#24670,.T.);
#32622=ORIENTED_EDGE('',*,*,#24671,.T.);
#32623=ORIENTED_EDGE('',*,*,#24672,.F.);
#32624=ORIENTED_EDGE('',*,*,#24673,.T.);
#32625=ORIENTED_EDGE('',*,*,#24674,.T.);
#32626=ORIENTED_EDGE('',*,*,#24672,.T.);
#32627=ORIENTED_EDGE('',*,*,#24675,.T.);
#32628=ORIENTED_EDGE('',*,*,#24666,.F.);
#32629=ORIENTED_EDGE('',*,*,#24676,.T.);
#32630=ORIENTED_EDGE('',*,*,#21358,.F.);
#32631=ORIENTED_EDGE('',*,*,#24677,.T.);
#32632=ORIENTED_EDGE('',*,*,#24564,.T.);
#32633=ORIENTED_EDGE('',*,*,#24678,.F.);
#32634=ORIENTED_EDGE('',*,*,#24679,.T.);
#32635=ORIENTED_EDGE('',*,*,#24669,.F.);
#32636=ORIENTED_EDGE('',*,*,#24680,.T.);
#32637=ORIENTED_EDGE('',*,*,#24681,.T.);
#32638=ORIENTED_EDGE('',*,*,#24682,.T.);
#32639=ORIENTED_EDGE('',*,*,#24678,.T.);
#32640=ORIENTED_EDGE('',*,*,#24683,.T.);
#32641=ORIENTED_EDGE('',*,*,#24684,.T.);
#32642=ORIENTED_EDGE('',*,*,#24685,.T.);
#32643=ORIENTED_EDGE('',*,*,#24686,.T.);
#32644=ORIENTED_EDGE('',*,*,#24687,.F.);
#32645=ORIENTED_EDGE('',*,*,#24688,.T.);
#32646=ORIENTED_EDGE('',*,*,#24689,.T.);
#32647=ORIENTED_EDGE('',*,*,#24687,.T.);
#32648=ORIENTED_EDGE('',*,*,#24690,.T.);
#32649=ORIENTED_EDGE('',*,*,#24681,.F.);
#32650=ORIENTED_EDGE('',*,*,#24691,.T.);
#32651=ORIENTED_EDGE('',*,*,#24692,.F.);
#32652=ORIENTED_EDGE('',*,*,#24693,.T.);
#32653=ORIENTED_EDGE('',*,*,#24684,.F.);
#32654=ORIENTED_EDGE('',*,*,#24694,.T.);
#32655=ORIENTED_EDGE('',*,*,#24695,.T.);
#32656=ORIENTED_EDGE('',*,*,#24696,.T.);
#32657=ORIENTED_EDGE('',*,*,#24692,.T.);
#32658=ORIENTED_EDGE('',*,*,#24697,.T.);
#32659=ORIENTED_EDGE('',*,*,#24698,.T.);
#32660=ORIENTED_EDGE('',*,*,#24699,.T.);
#32661=ORIENTED_EDGE('',*,*,#24700,.T.);
#32662=ORIENTED_EDGE('',*,*,#24701,.F.);
#32663=ORIENTED_EDGE('',*,*,#24702,.T.);
#32664=ORIENTED_EDGE('',*,*,#24703,.T.);
#32665=ORIENTED_EDGE('',*,*,#24701,.T.);
#32666=ORIENTED_EDGE('',*,*,#24704,.T.);
#32667=ORIENTED_EDGE('',*,*,#24695,.F.);
#32668=ORIENTED_EDGE('',*,*,#24705,.T.);
#32669=ORIENTED_EDGE('',*,*,#24706,.F.);
#32670=ORIENTED_EDGE('',*,*,#24707,.T.);
#32671=ORIENTED_EDGE('',*,*,#24698,.F.);
#32672=ORIENTED_EDGE('',*,*,#24708,.T.);
#32673=ORIENTED_EDGE('',*,*,#24709,.T.);
#32674=ORIENTED_EDGE('',*,*,#24710,.T.);
#32675=ORIENTED_EDGE('',*,*,#24706,.T.);
#32676=ORIENTED_EDGE('',*,*,#24711,.T.);
#32677=ORIENTED_EDGE('',*,*,#24712,.T.);
#32678=ORIENTED_EDGE('',*,*,#24713,.T.);
#32679=ORIENTED_EDGE('',*,*,#24714,.T.);
#32680=ORIENTED_EDGE('',*,*,#24715,.F.);
#32681=ORIENTED_EDGE('',*,*,#24716,.T.);
#32682=ORIENTED_EDGE('',*,*,#24717,.T.);
#32683=ORIENTED_EDGE('',*,*,#24715,.T.);
#32684=ORIENTED_EDGE('',*,*,#24718,.T.);
#32685=ORIENTED_EDGE('',*,*,#24709,.F.);
#32686=ORIENTED_EDGE('',*,*,#24719,.T.);
#32687=ORIENTED_EDGE('',*,*,#24720,.F.);
#32688=ORIENTED_EDGE('',*,*,#24721,.T.);
#32689=ORIENTED_EDGE('',*,*,#24712,.F.);
#32690=ORIENTED_EDGE('',*,*,#24722,.T.);
#32691=ORIENTED_EDGE('',*,*,#24723,.T.);
#32692=ORIENTED_EDGE('',*,*,#24724,.T.);
#32693=ORIENTED_EDGE('',*,*,#24720,.T.);
#32694=ORIENTED_EDGE('',*,*,#24725,.T.);
#32695=ORIENTED_EDGE('',*,*,#24726,.T.);
#32696=ORIENTED_EDGE('',*,*,#24727,.T.);
#32697=ORIENTED_EDGE('',*,*,#24728,.T.);
#32698=ORIENTED_EDGE('',*,*,#24729,.F.);
#32699=ORIENTED_EDGE('',*,*,#24730,.T.);
#32700=ORIENTED_EDGE('',*,*,#24731,.T.);
#32701=ORIENTED_EDGE('',*,*,#24729,.T.);
#32702=ORIENTED_EDGE('',*,*,#24732,.T.);
#32703=ORIENTED_EDGE('',*,*,#24723,.F.);
#32704=ORIENTED_EDGE('',*,*,#24733,.T.);
#32705=ORIENTED_EDGE('',*,*,#24734,.F.);
#32706=ORIENTED_EDGE('',*,*,#24735,.T.);
#32707=ORIENTED_EDGE('',*,*,#24726,.F.);
#32708=ORIENTED_EDGE('',*,*,#24736,.T.);
#32709=ORIENTED_EDGE('',*,*,#24737,.T.);
#32710=ORIENTED_EDGE('',*,*,#24738,.T.);
#32711=ORIENTED_EDGE('',*,*,#24734,.T.);
#32712=ORIENTED_EDGE('',*,*,#24739,.T.);
#32713=ORIENTED_EDGE('',*,*,#24740,.T.);
#32714=ORIENTED_EDGE('',*,*,#24741,.T.);
#32715=ORIENTED_EDGE('',*,*,#24742,.T.);
#32716=ORIENTED_EDGE('',*,*,#24743,.F.);
#32717=ORIENTED_EDGE('',*,*,#24744,.T.);
#32718=ORIENTED_EDGE('',*,*,#24745,.T.);
#32719=ORIENTED_EDGE('',*,*,#24743,.T.);
#32720=ORIENTED_EDGE('',*,*,#24746,.T.);
#32721=ORIENTED_EDGE('',*,*,#24737,.F.);
#32722=ORIENTED_EDGE('',*,*,#24747,.T.);
#32723=ORIENTED_EDGE('',*,*,#21502,.F.);
#32724=ORIENTED_EDGE('',*,*,#24748,.T.);
#32725=ORIENTED_EDGE('',*,*,#24740,.F.);
#32726=ORIENTED_EDGE('',*,*,#24749,.T.);
#32727=ORIENTED_EDGE('',*,*,#21499,.F.);
#32728=ORIENTED_EDGE('',*,*,#24750,.T.);
#32729=ORIENTED_EDGE('',*,*,#24751,.T.);
#32730=ORIENTED_EDGE('',*,*,#24752,.F.);
#32731=ORIENTED_EDGE('',*,*,#24752,.T.);
#32732=ORIENTED_EDGE('',*,*,#24753,.T.);
#32733=ORIENTED_EDGE('',*,*,#21500,.F.);
#32734=ORIENTED_EDGE('',*,*,#24754,.T.);
#32735=ORIENTED_EDGE('',*,*,#24755,.T.);
#32736=ORIENTED_EDGE('',*,*,#21351,.F.);
#32737=ORIENTED_EDGE('',*,*,#24756,.F.);
#32738=ORIENTED_EDGE('',*,*,#24757,.T.);
#32739=ORIENTED_EDGE('',*,*,#24758,.T.);
#32740=ORIENTED_EDGE('',*,*,#24759,.F.);
#32741=ORIENTED_EDGE('',*,*,#24760,.T.);
#32742=ORIENTED_EDGE('',*,*,#24754,.F.);
#32743=ORIENTED_EDGE('',*,*,#24761,.T.);
#32744=ORIENTED_EDGE('',*,*,#24762,.T.);
#32745=ORIENTED_EDGE('',*,*,#24763,.T.);
#32746=ORIENTED_EDGE('',*,*,#24759,.T.);
#32747=ORIENTED_EDGE('',*,*,#24764,.T.);
#32748=ORIENTED_EDGE('',*,*,#24765,.T.);
#32749=ORIENTED_EDGE('',*,*,#24766,.T.);
#32750=ORIENTED_EDGE('',*,*,#24767,.T.);
#32751=ORIENTED_EDGE('',*,*,#24768,.F.);
#32752=ORIENTED_EDGE('',*,*,#24769,.T.);
#32753=ORIENTED_EDGE('',*,*,#24770,.T.);
#32754=ORIENTED_EDGE('',*,*,#24768,.T.);
#32755=ORIENTED_EDGE('',*,*,#24771,.T.);
#32756=ORIENTED_EDGE('',*,*,#24762,.F.);
#32757=ORIENTED_EDGE('',*,*,#24772,.T.);
#32758=ORIENTED_EDGE('',*,*,#21354,.F.);
#32759=ORIENTED_EDGE('',*,*,#24773,.T.);
#32760=ORIENTED_EDGE('',*,*,#24660,.T.);
#32761=ORIENTED_EDGE('',*,*,#24774,.F.);
#32762=ORIENTED_EDGE('',*,*,#24775,.T.);
#32763=ORIENTED_EDGE('',*,*,#24765,.F.);
#32764=ORIENTED_EDGE('',*,*,#24776,.T.);
#32765=ORIENTED_EDGE('',*,*,#24777,.T.);
#32766=ORIENTED_EDGE('',*,*,#24778,.T.);
#32767=ORIENTED_EDGE('',*,*,#24774,.T.);
#32768=ORIENTED_EDGE('',*,*,#24779,.T.);
#32769=ORIENTED_EDGE('',*,*,#24780,.T.);
#32770=ORIENTED_EDGE('',*,*,#24781,.T.);
#32771=ORIENTED_EDGE('',*,*,#24782,.T.);
#32772=ORIENTED_EDGE('',*,*,#24783,.F.);
#32773=ORIENTED_EDGE('',*,*,#24784,.T.);
#32774=ORIENTED_EDGE('',*,*,#24785,.T.);
#32775=ORIENTED_EDGE('',*,*,#24783,.T.);
#32776=ORIENTED_EDGE('',*,*,#24786,.T.);
#32777=ORIENTED_EDGE('',*,*,#24777,.F.);
#32778=ORIENTED_EDGE('',*,*,#24787,.T.);
#32779=ORIENTED_EDGE('',*,*,#24788,.F.);
#32780=ORIENTED_EDGE('',*,*,#24789,.T.);
#32781=ORIENTED_EDGE('',*,*,#24780,.F.);
#32782=ORIENTED_EDGE('',*,*,#24790,.T.);
#32783=ORIENTED_EDGE('',*,*,#24791,.T.);
#32784=ORIENTED_EDGE('',*,*,#24792,.T.);
#32785=ORIENTED_EDGE('',*,*,#24788,.T.);
#32786=ORIENTED_EDGE('',*,*,#24793,.T.);
#32787=ORIENTED_EDGE('',*,*,#24794,.T.);
#32788=ORIENTED_EDGE('',*,*,#24795,.T.);
#32789=ORIENTED_EDGE('',*,*,#24796,.T.);
#32790=ORIENTED_EDGE('',*,*,#24797,.F.);
#32791=ORIENTED_EDGE('',*,*,#24798,.T.);
#32792=ORIENTED_EDGE('',*,*,#24799,.T.);
#32793=ORIENTED_EDGE('',*,*,#24797,.T.);
#32794=ORIENTED_EDGE('',*,*,#24800,.T.);
#32795=ORIENTED_EDGE('',*,*,#24791,.F.);
#32796=ORIENTED_EDGE('',*,*,#24801,.T.);
#32797=ORIENTED_EDGE('',*,*,#24802,.F.);
#32798=ORIENTED_EDGE('',*,*,#24803,.T.);
#32799=ORIENTED_EDGE('',*,*,#24794,.F.);
#32800=ORIENTED_EDGE('',*,*,#24804,.T.);
#32801=ORIENTED_EDGE('',*,*,#24805,.T.);
#32802=ORIENTED_EDGE('',*,*,#24806,.T.);
#32803=ORIENTED_EDGE('',*,*,#24802,.T.);
#32804=ORIENTED_EDGE('',*,*,#24807,.T.);
#32805=ORIENTED_EDGE('',*,*,#24808,.T.);
#32806=ORIENTED_EDGE('',*,*,#24809,.T.);
#32807=ORIENTED_EDGE('',*,*,#24810,.T.);
#32808=ORIENTED_EDGE('',*,*,#24811,.F.);
#32809=ORIENTED_EDGE('',*,*,#24812,.T.);
#32810=ORIENTED_EDGE('',*,*,#24813,.T.);
#32811=ORIENTED_EDGE('',*,*,#24811,.T.);
#32812=ORIENTED_EDGE('',*,*,#24814,.T.);
#32813=ORIENTED_EDGE('',*,*,#24805,.F.);
#32814=ORIENTED_EDGE('',*,*,#24815,.T.);
#32815=ORIENTED_EDGE('',*,*,#24816,.F.);
#32816=ORIENTED_EDGE('',*,*,#24817,.T.);
#32817=ORIENTED_EDGE('',*,*,#24808,.F.);
#32818=ORIENTED_EDGE('',*,*,#24818,.T.);
#32819=ORIENTED_EDGE('',*,*,#24819,.T.);
#32820=ORIENTED_EDGE('',*,*,#24820,.T.);
#32821=ORIENTED_EDGE('',*,*,#24816,.T.);
#32822=ORIENTED_EDGE('',*,*,#24821,.T.);
#32823=ORIENTED_EDGE('',*,*,#24822,.T.);
#32824=ORIENTED_EDGE('',*,*,#24823,.T.);
#32825=ORIENTED_EDGE('',*,*,#24824,.T.);
#32826=ORIENTED_EDGE('',*,*,#24825,.F.);
#32827=ORIENTED_EDGE('',*,*,#24826,.T.);
#32828=ORIENTED_EDGE('',*,*,#24827,.T.);
#32829=ORIENTED_EDGE('',*,*,#24825,.T.);
#32830=ORIENTED_EDGE('',*,*,#24828,.T.);
#32831=ORIENTED_EDGE('',*,*,#24819,.F.);
#32832=ORIENTED_EDGE('',*,*,#24829,.T.);
#32833=ORIENTED_EDGE('',*,*,#24830,.F.);
#32834=ORIENTED_EDGE('',*,*,#24831,.T.);
#32835=ORIENTED_EDGE('',*,*,#24822,.F.);
#32836=ORIENTED_EDGE('',*,*,#24832,.T.);
#32837=ORIENTED_EDGE('',*,*,#24833,.T.);
#32838=ORIENTED_EDGE('',*,*,#24834,.T.);
#32839=ORIENTED_EDGE('',*,*,#24830,.T.);
#32840=ORIENTED_EDGE('',*,*,#24835,.T.);
#32841=ORIENTED_EDGE('',*,*,#24836,.T.);
#32842=ORIENTED_EDGE('',*,*,#24837,.T.);
#32843=ORIENTED_EDGE('',*,*,#24838,.T.);
#32844=ORIENTED_EDGE('',*,*,#24839,.F.);
#32845=ORIENTED_EDGE('',*,*,#24840,.T.);
#32846=ORIENTED_EDGE('',*,*,#24841,.T.);
#32847=ORIENTED_EDGE('',*,*,#24839,.T.);
#32848=ORIENTED_EDGE('',*,*,#24842,.T.);
#32849=ORIENTED_EDGE('',*,*,#24833,.F.);
#32850=ORIENTED_EDGE('',*,*,#24843,.T.);
#32851=ORIENTED_EDGE('',*,*,#21508,.F.);
#32852=ORIENTED_EDGE('',*,*,#24844,.T.);
#32853=ORIENTED_EDGE('',*,*,#24836,.F.);
#32854=ORIENTED_EDGE('',*,*,#24845,.T.);
#32855=ORIENTED_EDGE('',*,*,#21505,.F.);
#32856=ORIENTED_EDGE('',*,*,#24846,.T.);
#32857=ORIENTED_EDGE('',*,*,#24847,.T.);
#32858=ORIENTED_EDGE('',*,*,#24848,.F.);
#32859=ORIENTED_EDGE('',*,*,#24848,.T.);
#32860=ORIENTED_EDGE('',*,*,#24849,.T.);
#32861=ORIENTED_EDGE('',*,*,#21506,.F.);
#32862=ORIENTED_EDGE('',*,*,#24850,.T.);
#32863=ORIENTED_EDGE('',*,*,#24851,.T.);
#32864=ORIENTED_EDGE('',*,*,#21347,.F.);
#32865=ORIENTED_EDGE('',*,*,#24852,.F.);
#32866=ORIENTED_EDGE('',*,*,#24853,.T.);
#32867=ORIENTED_EDGE('',*,*,#24854,.T.);
#32868=ORIENTED_EDGE('',*,*,#24855,.F.);
#32869=ORIENTED_EDGE('',*,*,#24856,.T.);
#32870=ORIENTED_EDGE('',*,*,#24850,.F.);
#32871=ORIENTED_EDGE('',*,*,#24857,.T.);
#32872=ORIENTED_EDGE('',*,*,#24858,.T.);
#32873=ORIENTED_EDGE('',*,*,#24859,.T.);
#32874=ORIENTED_EDGE('',*,*,#24855,.T.);
#32875=ORIENTED_EDGE('',*,*,#24860,.T.);
#32876=ORIENTED_EDGE('',*,*,#24861,.T.);
#32877=ORIENTED_EDGE('',*,*,#24862,.T.);
#32878=ORIENTED_EDGE('',*,*,#24863,.T.);
#32879=ORIENTED_EDGE('',*,*,#24864,.F.);
#32880=ORIENTED_EDGE('',*,*,#24865,.T.);
#32881=ORIENTED_EDGE('',*,*,#24866,.T.);
#32882=ORIENTED_EDGE('',*,*,#24864,.T.);
#32883=ORIENTED_EDGE('',*,*,#24867,.T.);
#32884=ORIENTED_EDGE('',*,*,#24858,.F.);
#32885=ORIENTED_EDGE('',*,*,#24868,.T.);
#32886=ORIENTED_EDGE('',*,*,#21350,.F.);
#32887=ORIENTED_EDGE('',*,*,#24869,.T.);
#32888=ORIENTED_EDGE('',*,*,#24756,.T.);
#32889=ORIENTED_EDGE('',*,*,#24870,.F.);
#32890=ORIENTED_EDGE('',*,*,#24871,.T.);
#32891=ORIENTED_EDGE('',*,*,#24861,.F.);
#32892=ORIENTED_EDGE('',*,*,#24872,.T.);
#32893=ORIENTED_EDGE('',*,*,#24873,.T.);
#32894=ORIENTED_EDGE('',*,*,#24874,.T.);
#32895=ORIENTED_EDGE('',*,*,#24870,.T.);
#32896=ORIENTED_EDGE('',*,*,#24875,.T.);
#32897=ORIENTED_EDGE('',*,*,#24876,.T.);
#32898=ORIENTED_EDGE('',*,*,#24877,.T.);
#32899=ORIENTED_EDGE('',*,*,#24878,.T.);
#32900=ORIENTED_EDGE('',*,*,#24879,.F.);
#32901=ORIENTED_EDGE('',*,*,#24880,.T.);
#32902=ORIENTED_EDGE('',*,*,#24881,.T.);
#32903=ORIENTED_EDGE('',*,*,#24879,.T.);
#32904=ORIENTED_EDGE('',*,*,#24882,.T.);
#32905=ORIENTED_EDGE('',*,*,#24873,.F.);
#32906=ORIENTED_EDGE('',*,*,#24883,.T.);
#32907=ORIENTED_EDGE('',*,*,#24884,.F.);
#32908=ORIENTED_EDGE('',*,*,#24885,.T.);
#32909=ORIENTED_EDGE('',*,*,#24876,.F.);
#32910=ORIENTED_EDGE('',*,*,#24886,.T.);
#32911=ORIENTED_EDGE('',*,*,#24887,.T.);
#32912=ORIENTED_EDGE('',*,*,#24888,.T.);
#32913=ORIENTED_EDGE('',*,*,#24884,.T.);
#32914=ORIENTED_EDGE('',*,*,#24889,.T.);
#32915=ORIENTED_EDGE('',*,*,#24890,.T.);
#32916=ORIENTED_EDGE('',*,*,#24891,.T.);
#32917=ORIENTED_EDGE('',*,*,#24892,.T.);
#32918=ORIENTED_EDGE('',*,*,#24893,.F.);
#32919=ORIENTED_EDGE('',*,*,#24894,.T.);
#32920=ORIENTED_EDGE('',*,*,#24895,.T.);
#32921=ORIENTED_EDGE('',*,*,#24893,.T.);
#32922=ORIENTED_EDGE('',*,*,#24896,.T.);
#32923=ORIENTED_EDGE('',*,*,#24887,.F.);
#32924=ORIENTED_EDGE('',*,*,#24897,.T.);
#32925=ORIENTED_EDGE('',*,*,#24898,.F.);
#32926=ORIENTED_EDGE('',*,*,#24899,.T.);
#32927=ORIENTED_EDGE('',*,*,#24890,.F.);
#32928=ORIENTED_EDGE('',*,*,#24900,.T.);
#32929=ORIENTED_EDGE('',*,*,#24901,.T.);
#32930=ORIENTED_EDGE('',*,*,#24902,.T.);
#32931=ORIENTED_EDGE('',*,*,#24898,.T.);
#32932=ORIENTED_EDGE('',*,*,#24903,.T.);
#32933=ORIENTED_EDGE('',*,*,#24904,.T.);
#32934=ORIENTED_EDGE('',*,*,#24905,.T.);
#32935=ORIENTED_EDGE('',*,*,#24906,.T.);
#32936=ORIENTED_EDGE('',*,*,#24907,.F.);
#32937=ORIENTED_EDGE('',*,*,#24908,.T.);
#32938=ORIENTED_EDGE('',*,*,#24909,.T.);
#32939=ORIENTED_EDGE('',*,*,#24907,.T.);
#32940=ORIENTED_EDGE('',*,*,#24910,.T.);
#32941=ORIENTED_EDGE('',*,*,#24901,.F.);
#32942=ORIENTED_EDGE('',*,*,#24911,.T.);
#32943=ORIENTED_EDGE('',*,*,#24912,.F.);
#32944=ORIENTED_EDGE('',*,*,#24913,.T.);
#32945=ORIENTED_EDGE('',*,*,#24904,.F.);
#32946=ORIENTED_EDGE('',*,*,#24914,.T.);
#32947=ORIENTED_EDGE('',*,*,#24915,.T.);
#32948=ORIENTED_EDGE('',*,*,#24916,.T.);
#32949=ORIENTED_EDGE('',*,*,#24912,.T.);
#32950=ORIENTED_EDGE('',*,*,#24917,.T.);
#32951=ORIENTED_EDGE('',*,*,#24918,.T.);
#32952=ORIENTED_EDGE('',*,*,#24919,.T.);
#32953=ORIENTED_EDGE('',*,*,#24920,.T.);
#32954=ORIENTED_EDGE('',*,*,#24921,.F.);
#32955=ORIENTED_EDGE('',*,*,#24922,.T.);
#32956=ORIENTED_EDGE('',*,*,#24923,.T.);
#32957=ORIENTED_EDGE('',*,*,#24921,.T.);
#32958=ORIENTED_EDGE('',*,*,#24924,.T.);
#32959=ORIENTED_EDGE('',*,*,#24915,.F.);
#32960=ORIENTED_EDGE('',*,*,#24925,.T.);
#32961=ORIENTED_EDGE('',*,*,#24926,.F.);
#32962=ORIENTED_EDGE('',*,*,#24927,.T.);
#32963=ORIENTED_EDGE('',*,*,#24918,.F.);
#32964=ORIENTED_EDGE('',*,*,#24928,.T.);
#32965=ORIENTED_EDGE('',*,*,#24929,.T.);
#32966=ORIENTED_EDGE('',*,*,#24930,.T.);
#32967=ORIENTED_EDGE('',*,*,#24926,.T.);
#32968=ORIENTED_EDGE('',*,*,#24931,.T.);
#32969=ORIENTED_EDGE('',*,*,#24932,.T.);
#32970=ORIENTED_EDGE('',*,*,#24933,.T.);
#32971=ORIENTED_EDGE('',*,*,#24934,.T.);
#32972=ORIENTED_EDGE('',*,*,#24935,.F.);
#32973=ORIENTED_EDGE('',*,*,#24936,.T.);
#32974=ORIENTED_EDGE('',*,*,#24937,.T.);
#32975=ORIENTED_EDGE('',*,*,#24935,.T.);
#32976=ORIENTED_EDGE('',*,*,#24938,.T.);
#32977=ORIENTED_EDGE('',*,*,#24929,.F.);
#32978=ORIENTED_EDGE('',*,*,#24939,.T.);
#32979=ORIENTED_EDGE('',*,*,#21514,.F.);
#32980=ORIENTED_EDGE('',*,*,#24940,.T.);
#32981=ORIENTED_EDGE('',*,*,#24932,.F.);
#32982=ORIENTED_EDGE('',*,*,#24941,.T.);
#32983=ORIENTED_EDGE('',*,*,#21511,.F.);
#32984=ORIENTED_EDGE('',*,*,#24942,.T.);
#32985=ORIENTED_EDGE('',*,*,#24943,.T.);
#32986=ORIENTED_EDGE('',*,*,#24944,.F.);
#32987=ORIENTED_EDGE('',*,*,#24944,.T.);
#32988=ORIENTED_EDGE('',*,*,#24945,.T.);
#32989=ORIENTED_EDGE('',*,*,#21512,.F.);
#32990=ORIENTED_EDGE('',*,*,#24946,.T.);
#32991=ORIENTED_EDGE('',*,*,#24947,.T.);
#32992=ORIENTED_EDGE('',*,*,#21343,.F.);
#32993=ORIENTED_EDGE('',*,*,#24948,.F.);
#32994=ORIENTED_EDGE('',*,*,#24949,.T.);
#32995=ORIENTED_EDGE('',*,*,#24950,.T.);
#32996=ORIENTED_EDGE('',*,*,#24951,.F.);
#32997=ORIENTED_EDGE('',*,*,#24952,.T.);
#32998=ORIENTED_EDGE('',*,*,#24946,.F.);
#32999=ORIENTED_EDGE('',*,*,#24953,.T.);
#33000=ORIENTED_EDGE('',*,*,#24954,.T.);
#33001=ORIENTED_EDGE('',*,*,#24955,.T.);
#33002=ORIENTED_EDGE('',*,*,#24951,.T.);
#33003=ORIENTED_EDGE('',*,*,#24956,.T.);
#33004=ORIENTED_EDGE('',*,*,#24957,.T.);
#33005=ORIENTED_EDGE('',*,*,#24958,.T.);
#33006=ORIENTED_EDGE('',*,*,#24959,.T.);
#33007=ORIENTED_EDGE('',*,*,#24960,.F.);
#33008=ORIENTED_EDGE('',*,*,#24961,.T.);
#33009=ORIENTED_EDGE('',*,*,#24962,.T.);
#33010=ORIENTED_EDGE('',*,*,#24960,.T.);
#33011=ORIENTED_EDGE('',*,*,#24963,.T.);
#33012=ORIENTED_EDGE('',*,*,#24954,.F.);
#33013=ORIENTED_EDGE('',*,*,#24964,.T.);
#33014=ORIENTED_EDGE('',*,*,#21346,.F.);
#33015=ORIENTED_EDGE('',*,*,#24965,.T.);
#33016=ORIENTED_EDGE('',*,*,#24852,.T.);
#33017=ORIENTED_EDGE('',*,*,#24966,.F.);
#33018=ORIENTED_EDGE('',*,*,#24967,.T.);
#33019=ORIENTED_EDGE('',*,*,#24957,.F.);
#33020=ORIENTED_EDGE('',*,*,#24968,.T.);
#33021=ORIENTED_EDGE('',*,*,#24969,.T.);
#33022=ORIENTED_EDGE('',*,*,#24970,.T.);
#33023=ORIENTED_EDGE('',*,*,#24966,.T.);
#33024=ORIENTED_EDGE('',*,*,#24971,.T.);
#33025=ORIENTED_EDGE('',*,*,#24972,.T.);
#33026=ORIENTED_EDGE('',*,*,#24973,.T.);
#33027=ORIENTED_EDGE('',*,*,#24974,.T.);
#33028=ORIENTED_EDGE('',*,*,#24975,.F.);
#33029=ORIENTED_EDGE('',*,*,#24976,.T.);
#33030=ORIENTED_EDGE('',*,*,#24977,.T.);
#33031=ORIENTED_EDGE('',*,*,#24975,.T.);
#33032=ORIENTED_EDGE('',*,*,#24978,.T.);
#33033=ORIENTED_EDGE('',*,*,#24969,.F.);
#33034=ORIENTED_EDGE('',*,*,#24979,.T.);
#33035=ORIENTED_EDGE('',*,*,#24980,.F.);
#33036=ORIENTED_EDGE('',*,*,#24981,.T.);
#33037=ORIENTED_EDGE('',*,*,#24972,.F.);
#33038=ORIENTED_EDGE('',*,*,#24982,.T.);
#33039=ORIENTED_EDGE('',*,*,#24983,.T.);
#33040=ORIENTED_EDGE('',*,*,#24984,.T.);
#33041=ORIENTED_EDGE('',*,*,#24980,.T.);
#33042=ORIENTED_EDGE('',*,*,#24985,.T.);
#33043=ORIENTED_EDGE('',*,*,#24986,.T.);
#33044=ORIENTED_EDGE('',*,*,#24987,.T.);
#33045=ORIENTED_EDGE('',*,*,#24988,.T.);
#33046=ORIENTED_EDGE('',*,*,#24989,.F.);
#33047=ORIENTED_EDGE('',*,*,#24990,.T.);
#33048=ORIENTED_EDGE('',*,*,#24991,.T.);
#33049=ORIENTED_EDGE('',*,*,#24989,.T.);
#33050=ORIENTED_EDGE('',*,*,#24992,.T.);
#33051=ORIENTED_EDGE('',*,*,#24983,.F.);
#33052=ORIENTED_EDGE('',*,*,#24993,.T.);
#33053=ORIENTED_EDGE('',*,*,#24994,.F.);
#33054=ORIENTED_EDGE('',*,*,#24995,.T.);
#33055=ORIENTED_EDGE('',*,*,#24986,.F.);
#33056=ORIENTED_EDGE('',*,*,#24996,.T.);
#33057=ORIENTED_EDGE('',*,*,#24997,.T.);
#33058=ORIENTED_EDGE('',*,*,#24998,.T.);
#33059=ORIENTED_EDGE('',*,*,#24994,.T.);
#33060=ORIENTED_EDGE('',*,*,#24999,.T.);
#33061=ORIENTED_EDGE('',*,*,#25000,.T.);
#33062=ORIENTED_EDGE('',*,*,#25001,.T.);
#33063=ORIENTED_EDGE('',*,*,#25002,.T.);
#33064=ORIENTED_EDGE('',*,*,#25003,.F.);
#33065=ORIENTED_EDGE('',*,*,#25004,.T.);
#33066=ORIENTED_EDGE('',*,*,#25005,.T.);
#33067=ORIENTED_EDGE('',*,*,#25003,.T.);
#33068=ORIENTED_EDGE('',*,*,#25006,.T.);
#33069=ORIENTED_EDGE('',*,*,#24997,.F.);
#33070=ORIENTED_EDGE('',*,*,#25007,.T.);
#33071=ORIENTED_EDGE('',*,*,#25008,.F.);
#33072=ORIENTED_EDGE('',*,*,#25009,.T.);
#33073=ORIENTED_EDGE('',*,*,#25000,.F.);
#33074=ORIENTED_EDGE('',*,*,#25010,.T.);
#33075=ORIENTED_EDGE('',*,*,#25011,.T.);
#33076=ORIENTED_EDGE('',*,*,#25012,.T.);
#33077=ORIENTED_EDGE('',*,*,#25008,.T.);
#33078=ORIENTED_EDGE('',*,*,#25013,.T.);
#33079=ORIENTED_EDGE('',*,*,#25014,.T.);
#33080=ORIENTED_EDGE('',*,*,#25015,.T.);
#33081=ORIENTED_EDGE('',*,*,#25016,.T.);
#33082=ORIENTED_EDGE('',*,*,#25017,.F.);
#33083=ORIENTED_EDGE('',*,*,#25018,.T.);
#33084=ORIENTED_EDGE('',*,*,#25019,.T.);
#33085=ORIENTED_EDGE('',*,*,#25017,.T.);
#33086=ORIENTED_EDGE('',*,*,#25020,.T.);
#33087=ORIENTED_EDGE('',*,*,#25011,.F.);
#33088=ORIENTED_EDGE('',*,*,#25021,.T.);
#33089=ORIENTED_EDGE('',*,*,#25022,.F.);
#33090=ORIENTED_EDGE('',*,*,#25023,.T.);
#33091=ORIENTED_EDGE('',*,*,#25014,.F.);
#33092=ORIENTED_EDGE('',*,*,#25024,.T.);
#33093=ORIENTED_EDGE('',*,*,#25025,.T.);
#33094=ORIENTED_EDGE('',*,*,#25026,.T.);
#33095=ORIENTED_EDGE('',*,*,#25022,.T.);
#33096=ORIENTED_EDGE('',*,*,#25027,.T.);
#33097=ORIENTED_EDGE('',*,*,#25028,.T.);
#33098=ORIENTED_EDGE('',*,*,#25029,.T.);
#33099=ORIENTED_EDGE('',*,*,#25030,.T.);
#33100=ORIENTED_EDGE('',*,*,#25031,.F.);
#33101=ORIENTED_EDGE('',*,*,#25032,.T.);
#33102=ORIENTED_EDGE('',*,*,#25033,.T.);
#33103=ORIENTED_EDGE('',*,*,#25031,.T.);
#33104=ORIENTED_EDGE('',*,*,#25034,.T.);
#33105=ORIENTED_EDGE('',*,*,#25025,.F.);
#33106=ORIENTED_EDGE('',*,*,#25035,.T.);
#33107=ORIENTED_EDGE('',*,*,#21520,.F.);
#33108=ORIENTED_EDGE('',*,*,#25036,.T.);
#33109=ORIENTED_EDGE('',*,*,#25028,.F.);
#33110=ORIENTED_EDGE('',*,*,#25037,.T.);
#33111=ORIENTED_EDGE('',*,*,#21517,.F.);
#33112=ORIENTED_EDGE('',*,*,#25038,.T.);
#33113=ORIENTED_EDGE('',*,*,#25039,.T.);
#33114=ORIENTED_EDGE('',*,*,#25040,.F.);
#33115=ORIENTED_EDGE('',*,*,#25040,.T.);
#33116=ORIENTED_EDGE('',*,*,#25041,.T.);
#33117=ORIENTED_EDGE('',*,*,#21518,.F.);
#33118=ORIENTED_EDGE('',*,*,#25042,.T.);
#33119=ORIENTED_EDGE('',*,*,#25043,.T.);
#33120=ORIENTED_EDGE('',*,*,#21339,.F.);
#33121=ORIENTED_EDGE('',*,*,#25044,.F.);
#33122=ORIENTED_EDGE('',*,*,#25045,.T.);
#33123=ORIENTED_EDGE('',*,*,#25046,.T.);
#33124=ORIENTED_EDGE('',*,*,#25047,.F.);
#33125=ORIENTED_EDGE('',*,*,#25048,.T.);
#33126=ORIENTED_EDGE('',*,*,#25042,.F.);
#33127=ORIENTED_EDGE('',*,*,#25049,.T.);
#33128=ORIENTED_EDGE('',*,*,#25050,.T.);
#33129=ORIENTED_EDGE('',*,*,#25051,.T.);
#33130=ORIENTED_EDGE('',*,*,#25047,.T.);
#33131=ORIENTED_EDGE('',*,*,#25052,.T.);
#33132=ORIENTED_EDGE('',*,*,#25053,.T.);
#33133=ORIENTED_EDGE('',*,*,#25054,.T.);
#33134=ORIENTED_EDGE('',*,*,#25055,.T.);
#33135=ORIENTED_EDGE('',*,*,#25056,.F.);
#33136=ORIENTED_EDGE('',*,*,#25057,.T.);
#33137=ORIENTED_EDGE('',*,*,#25058,.T.);
#33138=ORIENTED_EDGE('',*,*,#25056,.T.);
#33139=ORIENTED_EDGE('',*,*,#25059,.T.);
#33140=ORIENTED_EDGE('',*,*,#25050,.F.);
#33141=ORIENTED_EDGE('',*,*,#25060,.T.);
#33142=ORIENTED_EDGE('',*,*,#21342,.F.);
#33143=ORIENTED_EDGE('',*,*,#25061,.T.);
#33144=ORIENTED_EDGE('',*,*,#24948,.T.);
#33145=ORIENTED_EDGE('',*,*,#25062,.F.);
#33146=ORIENTED_EDGE('',*,*,#25063,.T.);
#33147=ORIENTED_EDGE('',*,*,#25053,.F.);
#33148=ORIENTED_EDGE('',*,*,#25064,.T.);
#33149=ORIENTED_EDGE('',*,*,#25065,.T.);
#33150=ORIENTED_EDGE('',*,*,#25066,.T.);
#33151=ORIENTED_EDGE('',*,*,#25062,.T.);
#33152=ORIENTED_EDGE('',*,*,#25067,.T.);
#33153=ORIENTED_EDGE('',*,*,#25068,.T.);
#33154=ORIENTED_EDGE('',*,*,#25069,.T.);
#33155=ORIENTED_EDGE('',*,*,#25070,.T.);
#33156=ORIENTED_EDGE('',*,*,#25071,.F.);
#33157=ORIENTED_EDGE('',*,*,#25072,.T.);
#33158=ORIENTED_EDGE('',*,*,#25073,.T.);
#33159=ORIENTED_EDGE('',*,*,#25071,.T.);
#33160=ORIENTED_EDGE('',*,*,#25074,.T.);
#33161=ORIENTED_EDGE('',*,*,#25065,.F.);
#33162=ORIENTED_EDGE('',*,*,#25075,.T.);
#33163=ORIENTED_EDGE('',*,*,#25076,.F.);
#33164=ORIENTED_EDGE('',*,*,#25077,.T.);
#33165=ORIENTED_EDGE('',*,*,#25068,.F.);
#33166=ORIENTED_EDGE('',*,*,#25078,.T.);
#33167=ORIENTED_EDGE('',*,*,#25079,.T.);
#33168=ORIENTED_EDGE('',*,*,#25080,.T.);
#33169=ORIENTED_EDGE('',*,*,#25076,.T.);
#33170=ORIENTED_EDGE('',*,*,#25081,.T.);
#33171=ORIENTED_EDGE('',*,*,#25082,.T.);
#33172=ORIENTED_EDGE('',*,*,#25083,.T.);
#33173=ORIENTED_EDGE('',*,*,#25084,.T.);
#33174=ORIENTED_EDGE('',*,*,#25085,.F.);
#33175=ORIENTED_EDGE('',*,*,#25086,.T.);
#33176=ORIENTED_EDGE('',*,*,#25087,.T.);
#33177=ORIENTED_EDGE('',*,*,#25085,.T.);
#33178=ORIENTED_EDGE('',*,*,#25088,.T.);
#33179=ORIENTED_EDGE('',*,*,#25079,.F.);
#33180=ORIENTED_EDGE('',*,*,#25089,.T.);
#33181=ORIENTED_EDGE('',*,*,#25090,.F.);
#33182=ORIENTED_EDGE('',*,*,#25091,.T.);
#33183=ORIENTED_EDGE('',*,*,#25082,.F.);
#33184=ORIENTED_EDGE('',*,*,#25092,.T.);
#33185=ORIENTED_EDGE('',*,*,#25093,.T.);
#33186=ORIENTED_EDGE('',*,*,#25094,.T.);
#33187=ORIENTED_EDGE('',*,*,#25090,.T.);
#33188=ORIENTED_EDGE('',*,*,#25095,.T.);
#33189=ORIENTED_EDGE('',*,*,#25096,.T.);
#33190=ORIENTED_EDGE('',*,*,#25097,.T.);
#33191=ORIENTED_EDGE('',*,*,#25098,.T.);
#33192=ORIENTED_EDGE('',*,*,#25099,.F.);
#33193=ORIENTED_EDGE('',*,*,#25100,.T.);
#33194=ORIENTED_EDGE('',*,*,#25101,.T.);
#33195=ORIENTED_EDGE('',*,*,#25099,.T.);
#33196=ORIENTED_EDGE('',*,*,#25102,.T.);
#33197=ORIENTED_EDGE('',*,*,#25093,.F.);
#33198=ORIENTED_EDGE('',*,*,#25103,.T.);
#33199=ORIENTED_EDGE('',*,*,#25104,.F.);
#33200=ORIENTED_EDGE('',*,*,#25105,.T.);
#33201=ORIENTED_EDGE('',*,*,#25096,.F.);
#33202=ORIENTED_EDGE('',*,*,#25106,.T.);
#33203=ORIENTED_EDGE('',*,*,#25107,.T.);
#33204=ORIENTED_EDGE('',*,*,#25108,.T.);
#33205=ORIENTED_EDGE('',*,*,#25104,.T.);
#33206=ORIENTED_EDGE('',*,*,#25109,.T.);
#33207=ORIENTED_EDGE('',*,*,#25110,.T.);
#33208=ORIENTED_EDGE('',*,*,#25111,.T.);
#33209=ORIENTED_EDGE('',*,*,#25112,.T.);
#33210=ORIENTED_EDGE('',*,*,#25113,.F.);
#33211=ORIENTED_EDGE('',*,*,#25114,.T.);
#33212=ORIENTED_EDGE('',*,*,#25115,.T.);
#33213=ORIENTED_EDGE('',*,*,#25113,.T.);
#33214=ORIENTED_EDGE('',*,*,#25116,.T.);
#33215=ORIENTED_EDGE('',*,*,#25107,.F.);
#33216=ORIENTED_EDGE('',*,*,#25117,.T.);
#33217=ORIENTED_EDGE('',*,*,#25118,.F.);
#33218=ORIENTED_EDGE('',*,*,#25119,.T.);
#33219=ORIENTED_EDGE('',*,*,#25110,.F.);
#33220=ORIENTED_EDGE('',*,*,#25120,.T.);
#33221=ORIENTED_EDGE('',*,*,#25121,.T.);
#33222=ORIENTED_EDGE('',*,*,#25122,.T.);
#33223=ORIENTED_EDGE('',*,*,#25118,.T.);
#33224=ORIENTED_EDGE('',*,*,#25123,.T.);
#33225=ORIENTED_EDGE('',*,*,#25124,.T.);
#33226=ORIENTED_EDGE('',*,*,#25125,.T.);
#33227=ORIENTED_EDGE('',*,*,#25126,.T.);
#33228=ORIENTED_EDGE('',*,*,#25127,.F.);
#33229=ORIENTED_EDGE('',*,*,#25128,.T.);
#33230=ORIENTED_EDGE('',*,*,#25129,.T.);
#33231=ORIENTED_EDGE('',*,*,#25127,.T.);
#33232=ORIENTED_EDGE('',*,*,#25130,.T.);
#33233=ORIENTED_EDGE('',*,*,#25121,.F.);
#33234=ORIENTED_EDGE('',*,*,#25131,.T.);
#33235=ORIENTED_EDGE('',*,*,#21526,.F.);
#33236=ORIENTED_EDGE('',*,*,#25132,.T.);
#33237=ORIENTED_EDGE('',*,*,#25124,.F.);
#33238=ORIENTED_EDGE('',*,*,#25133,.T.);
#33239=ORIENTED_EDGE('',*,*,#21523,.F.);
#33240=ORIENTED_EDGE('',*,*,#25134,.T.);
#33241=ORIENTED_EDGE('',*,*,#25135,.T.);
#33242=ORIENTED_EDGE('',*,*,#25136,.F.);
#33243=ORIENTED_EDGE('',*,*,#25136,.T.);
#33244=ORIENTED_EDGE('',*,*,#25137,.T.);
#33245=ORIENTED_EDGE('',*,*,#21524,.F.);
#33246=ORIENTED_EDGE('',*,*,#25138,.T.);
#33247=ORIENTED_EDGE('',*,*,#25139,.T.);
#33248=ORIENTED_EDGE('',*,*,#21335,.F.);
#33249=ORIENTED_EDGE('',*,*,#25140,.F.);
#33250=ORIENTED_EDGE('',*,*,#25141,.T.);
#33251=ORIENTED_EDGE('',*,*,#25142,.T.);
#33252=ORIENTED_EDGE('',*,*,#25143,.F.);
#33253=ORIENTED_EDGE('',*,*,#25144,.T.);
#33254=ORIENTED_EDGE('',*,*,#25138,.F.);
#33255=ORIENTED_EDGE('',*,*,#25145,.T.);
#33256=ORIENTED_EDGE('',*,*,#25146,.T.);
#33257=ORIENTED_EDGE('',*,*,#25147,.T.);
#33258=ORIENTED_EDGE('',*,*,#25143,.T.);
#33259=ORIENTED_EDGE('',*,*,#25148,.T.);
#33260=ORIENTED_EDGE('',*,*,#25149,.T.);
#33261=ORIENTED_EDGE('',*,*,#25150,.T.);
#33262=ORIENTED_EDGE('',*,*,#25151,.T.);
#33263=ORIENTED_EDGE('',*,*,#25152,.F.);
#33264=ORIENTED_EDGE('',*,*,#25153,.T.);
#33265=ORIENTED_EDGE('',*,*,#25154,.T.);
#33266=ORIENTED_EDGE('',*,*,#25152,.T.);
#33267=ORIENTED_EDGE('',*,*,#25155,.T.);
#33268=ORIENTED_EDGE('',*,*,#25146,.F.);
#33269=ORIENTED_EDGE('',*,*,#25156,.T.);
#33270=ORIENTED_EDGE('',*,*,#21338,.F.);
#33271=ORIENTED_EDGE('',*,*,#25157,.T.);
#33272=ORIENTED_EDGE('',*,*,#25044,.T.);
#33273=ORIENTED_EDGE('',*,*,#25158,.F.);
#33274=ORIENTED_EDGE('',*,*,#25159,.T.);
#33275=ORIENTED_EDGE('',*,*,#25149,.F.);
#33276=ORIENTED_EDGE('',*,*,#25160,.T.);
#33277=ORIENTED_EDGE('',*,*,#25161,.T.);
#33278=ORIENTED_EDGE('',*,*,#25162,.T.);
#33279=ORIENTED_EDGE('',*,*,#25158,.T.);
#33280=ORIENTED_EDGE('',*,*,#25163,.T.);
#33281=ORIENTED_EDGE('',*,*,#25164,.T.);
#33282=ORIENTED_EDGE('',*,*,#25165,.T.);
#33283=ORIENTED_EDGE('',*,*,#25166,.T.);
#33284=ORIENTED_EDGE('',*,*,#25167,.F.);
#33285=ORIENTED_EDGE('',*,*,#25168,.T.);
#33286=ORIENTED_EDGE('',*,*,#25169,.T.);
#33287=ORIENTED_EDGE('',*,*,#25167,.T.);
#33288=ORIENTED_EDGE('',*,*,#25170,.T.);
#33289=ORIENTED_EDGE('',*,*,#25161,.F.);
#33290=ORIENTED_EDGE('',*,*,#25171,.T.);
#33291=ORIENTED_EDGE('',*,*,#25172,.F.);
#33292=ORIENTED_EDGE('',*,*,#25173,.T.);
#33293=ORIENTED_EDGE('',*,*,#25164,.F.);
#33294=ORIENTED_EDGE('',*,*,#25174,.T.);
#33295=ORIENTED_EDGE('',*,*,#25175,.T.);
#33296=ORIENTED_EDGE('',*,*,#25176,.T.);
#33297=ORIENTED_EDGE('',*,*,#25172,.T.);
#33298=ORIENTED_EDGE('',*,*,#25177,.T.);
#33299=ORIENTED_EDGE('',*,*,#25178,.T.);
#33300=ORIENTED_EDGE('',*,*,#25179,.T.);
#33301=ORIENTED_EDGE('',*,*,#25180,.T.);
#33302=ORIENTED_EDGE('',*,*,#25181,.F.);
#33303=ORIENTED_EDGE('',*,*,#25182,.T.);
#33304=ORIENTED_EDGE('',*,*,#25183,.T.);
#33305=ORIENTED_EDGE('',*,*,#25181,.T.);
#33306=ORIENTED_EDGE('',*,*,#25184,.T.);
#33307=ORIENTED_EDGE('',*,*,#25175,.F.);
#33308=ORIENTED_EDGE('',*,*,#25185,.T.);
#33309=ORIENTED_EDGE('',*,*,#25186,.F.);
#33310=ORIENTED_EDGE('',*,*,#25187,.T.);
#33311=ORIENTED_EDGE('',*,*,#25178,.F.);
#33312=ORIENTED_EDGE('',*,*,#25188,.T.);
#33313=ORIENTED_EDGE('',*,*,#25189,.T.);
#33314=ORIENTED_EDGE('',*,*,#25190,.T.);
#33315=ORIENTED_EDGE('',*,*,#25186,.T.);
#33316=ORIENTED_EDGE('',*,*,#25191,.T.);
#33317=ORIENTED_EDGE('',*,*,#25192,.T.);
#33318=ORIENTED_EDGE('',*,*,#25193,.T.);
#33319=ORIENTED_EDGE('',*,*,#25194,.T.);
#33320=ORIENTED_EDGE('',*,*,#25195,.F.);
#33321=ORIENTED_EDGE('',*,*,#25196,.T.);
#33322=ORIENTED_EDGE('',*,*,#25197,.T.);
#33323=ORIENTED_EDGE('',*,*,#25195,.T.);
#33324=ORIENTED_EDGE('',*,*,#25198,.T.);
#33325=ORIENTED_EDGE('',*,*,#25189,.F.);
#33326=ORIENTED_EDGE('',*,*,#25199,.T.);
#33327=ORIENTED_EDGE('',*,*,#25200,.F.);
#33328=ORIENTED_EDGE('',*,*,#25201,.T.);
#33329=ORIENTED_EDGE('',*,*,#25192,.F.);
#33330=ORIENTED_EDGE('',*,*,#25202,.T.);
#33331=ORIENTED_EDGE('',*,*,#25203,.T.);
#33332=ORIENTED_EDGE('',*,*,#25204,.T.);
#33333=ORIENTED_EDGE('',*,*,#25200,.T.);
#33334=ORIENTED_EDGE('',*,*,#25205,.T.);
#33335=ORIENTED_EDGE('',*,*,#25206,.T.);
#33336=ORIENTED_EDGE('',*,*,#25207,.T.);
#33337=ORIENTED_EDGE('',*,*,#25208,.T.);
#33338=ORIENTED_EDGE('',*,*,#25209,.F.);
#33339=ORIENTED_EDGE('',*,*,#25210,.T.);
#33340=ORIENTED_EDGE('',*,*,#25211,.T.);
#33341=ORIENTED_EDGE('',*,*,#25209,.T.);
#33342=ORIENTED_EDGE('',*,*,#25212,.T.);
#33343=ORIENTED_EDGE('',*,*,#25203,.F.);
#33344=ORIENTED_EDGE('',*,*,#25213,.T.);
#33345=ORIENTED_EDGE('',*,*,#25214,.F.);
#33346=ORIENTED_EDGE('',*,*,#25215,.T.);
#33347=ORIENTED_EDGE('',*,*,#25206,.F.);
#33348=ORIENTED_EDGE('',*,*,#25216,.T.);
#33349=ORIENTED_EDGE('',*,*,#25217,.T.);
#33350=ORIENTED_EDGE('',*,*,#25218,.T.);
#33351=ORIENTED_EDGE('',*,*,#25214,.T.);
#33352=ORIENTED_EDGE('',*,*,#25219,.T.);
#33353=ORIENTED_EDGE('',*,*,#25220,.T.);
#33354=ORIENTED_EDGE('',*,*,#25221,.T.);
#33355=ORIENTED_EDGE('',*,*,#25222,.T.);
#33356=ORIENTED_EDGE('',*,*,#25223,.F.);
#33357=ORIENTED_EDGE('',*,*,#25224,.T.);
#33358=ORIENTED_EDGE('',*,*,#25225,.T.);
#33359=ORIENTED_EDGE('',*,*,#25223,.T.);
#33360=ORIENTED_EDGE('',*,*,#25226,.T.);
#33361=ORIENTED_EDGE('',*,*,#25217,.F.);
#33362=ORIENTED_EDGE('',*,*,#25227,.T.);
#33363=ORIENTED_EDGE('',*,*,#21532,.F.);
#33364=ORIENTED_EDGE('',*,*,#25228,.T.);
#33365=ORIENTED_EDGE('',*,*,#25220,.F.);
#33366=ORIENTED_EDGE('',*,*,#25229,.T.);
#33367=ORIENTED_EDGE('',*,*,#21529,.F.);
#33368=ORIENTED_EDGE('',*,*,#25230,.T.);
#33369=ORIENTED_EDGE('',*,*,#25231,.T.);
#33370=ORIENTED_EDGE('',*,*,#25232,.F.);
#33371=ORIENTED_EDGE('',*,*,#25232,.T.);
#33372=ORIENTED_EDGE('',*,*,#25233,.T.);
#33373=ORIENTED_EDGE('',*,*,#21530,.F.);
#33374=ORIENTED_EDGE('',*,*,#25234,.T.);
#33375=ORIENTED_EDGE('',*,*,#25235,.T.);
#33376=ORIENTED_EDGE('',*,*,#21331,.F.);
#33377=ORIENTED_EDGE('',*,*,#25236,.F.);
#33378=ORIENTED_EDGE('',*,*,#25237,.T.);
#33379=ORIENTED_EDGE('',*,*,#25238,.T.);
#33380=ORIENTED_EDGE('',*,*,#25239,.F.);
#33381=ORIENTED_EDGE('',*,*,#25240,.T.);
#33382=ORIENTED_EDGE('',*,*,#25234,.F.);
#33383=ORIENTED_EDGE('',*,*,#25241,.T.);
#33384=ORIENTED_EDGE('',*,*,#25242,.T.);
#33385=ORIENTED_EDGE('',*,*,#25243,.T.);
#33386=ORIENTED_EDGE('',*,*,#25239,.T.);
#33387=ORIENTED_EDGE('',*,*,#25244,.T.);
#33388=ORIENTED_EDGE('',*,*,#25245,.T.);
#33389=ORIENTED_EDGE('',*,*,#25246,.T.);
#33390=ORIENTED_EDGE('',*,*,#25247,.T.);
#33391=ORIENTED_EDGE('',*,*,#25248,.F.);
#33392=ORIENTED_EDGE('',*,*,#25249,.T.);
#33393=ORIENTED_EDGE('',*,*,#25250,.T.);
#33394=ORIENTED_EDGE('',*,*,#25248,.T.);
#33395=ORIENTED_EDGE('',*,*,#25251,.T.);
#33396=ORIENTED_EDGE('',*,*,#25242,.F.);
#33397=ORIENTED_EDGE('',*,*,#25252,.T.);
#33398=ORIENTED_EDGE('',*,*,#21334,.F.);
#33399=ORIENTED_EDGE('',*,*,#25253,.T.);
#33400=ORIENTED_EDGE('',*,*,#25140,.T.);
#33401=ORIENTED_EDGE('',*,*,#25254,.F.);
#33402=ORIENTED_EDGE('',*,*,#25255,.T.);
#33403=ORIENTED_EDGE('',*,*,#25245,.F.);
#33404=ORIENTED_EDGE('',*,*,#25256,.T.);
#33405=ORIENTED_EDGE('',*,*,#25257,.T.);
#33406=ORIENTED_EDGE('',*,*,#25258,.T.);
#33407=ORIENTED_EDGE('',*,*,#25254,.T.);
#33408=ORIENTED_EDGE('',*,*,#25259,.T.);
#33409=ORIENTED_EDGE('',*,*,#25260,.T.);
#33410=ORIENTED_EDGE('',*,*,#25261,.T.);
#33411=ORIENTED_EDGE('',*,*,#25262,.T.);
#33412=ORIENTED_EDGE('',*,*,#25263,.F.);
#33413=ORIENTED_EDGE('',*,*,#25264,.T.);
#33414=ORIENTED_EDGE('',*,*,#25265,.T.);
#33415=ORIENTED_EDGE('',*,*,#25263,.T.);
#33416=ORIENTED_EDGE('',*,*,#25266,.T.);
#33417=ORIENTED_EDGE('',*,*,#25257,.F.);
#33418=ORIENTED_EDGE('',*,*,#25267,.T.);
#33419=ORIENTED_EDGE('',*,*,#25268,.F.);
#33420=ORIENTED_EDGE('',*,*,#25269,.T.);
#33421=ORIENTED_EDGE('',*,*,#25260,.F.);
#33422=ORIENTED_EDGE('',*,*,#25270,.T.);
#33423=ORIENTED_EDGE('',*,*,#25271,.T.);
#33424=ORIENTED_EDGE('',*,*,#25272,.T.);
#33425=ORIENTED_EDGE('',*,*,#25268,.T.);
#33426=ORIENTED_EDGE('',*,*,#25273,.T.);
#33427=ORIENTED_EDGE('',*,*,#25274,.T.);
#33428=ORIENTED_EDGE('',*,*,#25275,.T.);
#33429=ORIENTED_EDGE('',*,*,#25276,.T.);
#33430=ORIENTED_EDGE('',*,*,#25277,.F.);
#33431=ORIENTED_EDGE('',*,*,#25278,.T.);
#33432=ORIENTED_EDGE('',*,*,#25279,.T.);
#33433=ORIENTED_EDGE('',*,*,#25277,.T.);
#33434=ORIENTED_EDGE('',*,*,#25280,.T.);
#33435=ORIENTED_EDGE('',*,*,#25271,.F.);
#33436=ORIENTED_EDGE('',*,*,#25281,.T.);
#33437=ORIENTED_EDGE('',*,*,#25282,.F.);
#33438=ORIENTED_EDGE('',*,*,#25283,.T.);
#33439=ORIENTED_EDGE('',*,*,#25274,.F.);
#33440=ORIENTED_EDGE('',*,*,#25284,.T.);
#33441=ORIENTED_EDGE('',*,*,#25285,.T.);
#33442=ORIENTED_EDGE('',*,*,#25286,.T.);
#33443=ORIENTED_EDGE('',*,*,#25282,.T.);
#33444=ORIENTED_EDGE('',*,*,#25287,.T.);
#33445=ORIENTED_EDGE('',*,*,#25288,.T.);
#33446=ORIENTED_EDGE('',*,*,#25289,.T.);
#33447=ORIENTED_EDGE('',*,*,#25290,.T.);
#33448=ORIENTED_EDGE('',*,*,#25291,.F.);
#33449=ORIENTED_EDGE('',*,*,#25292,.T.);
#33450=ORIENTED_EDGE('',*,*,#25293,.T.);
#33451=ORIENTED_EDGE('',*,*,#25291,.T.);
#33452=ORIENTED_EDGE('',*,*,#25294,.T.);
#33453=ORIENTED_EDGE('',*,*,#25285,.F.);
#33454=ORIENTED_EDGE('',*,*,#25295,.T.);
#33455=ORIENTED_EDGE('',*,*,#25296,.F.);
#33456=ORIENTED_EDGE('',*,*,#25297,.T.);
#33457=ORIENTED_EDGE('',*,*,#25288,.F.);
#33458=ORIENTED_EDGE('',*,*,#25298,.T.);
#33459=ORIENTED_EDGE('',*,*,#25299,.T.);
#33460=ORIENTED_EDGE('',*,*,#25300,.T.);
#33461=ORIENTED_EDGE('',*,*,#25296,.T.);
#33462=ORIENTED_EDGE('',*,*,#25301,.T.);
#33463=ORIENTED_EDGE('',*,*,#25302,.T.);
#33464=ORIENTED_EDGE('',*,*,#25303,.T.);
#33465=ORIENTED_EDGE('',*,*,#25304,.T.);
#33466=ORIENTED_EDGE('',*,*,#25305,.F.);
#33467=ORIENTED_EDGE('',*,*,#25306,.T.);
#33468=ORIENTED_EDGE('',*,*,#25307,.T.);
#33469=ORIENTED_EDGE('',*,*,#25305,.T.);
#33470=ORIENTED_EDGE('',*,*,#25308,.T.);
#33471=ORIENTED_EDGE('',*,*,#25299,.F.);
#33472=ORIENTED_EDGE('',*,*,#25309,.T.);
#33473=ORIENTED_EDGE('',*,*,#25310,.F.);
#33474=ORIENTED_EDGE('',*,*,#25311,.T.);
#33475=ORIENTED_EDGE('',*,*,#25302,.F.);
#33476=ORIENTED_EDGE('',*,*,#25312,.T.);
#33477=ORIENTED_EDGE('',*,*,#25313,.T.);
#33478=ORIENTED_EDGE('',*,*,#25314,.T.);
#33479=ORIENTED_EDGE('',*,*,#25310,.T.);
#33480=ORIENTED_EDGE('',*,*,#25315,.T.);
#33481=ORIENTED_EDGE('',*,*,#25316,.T.);
#33482=ORIENTED_EDGE('',*,*,#25317,.T.);
#33483=ORIENTED_EDGE('',*,*,#25318,.T.);
#33484=ORIENTED_EDGE('',*,*,#25319,.F.);
#33485=ORIENTED_EDGE('',*,*,#25320,.T.);
#33486=ORIENTED_EDGE('',*,*,#25321,.T.);
#33487=ORIENTED_EDGE('',*,*,#25319,.T.);
#33488=ORIENTED_EDGE('',*,*,#25322,.T.);
#33489=ORIENTED_EDGE('',*,*,#25313,.F.);
#33490=ORIENTED_EDGE('',*,*,#25323,.T.);
#33491=ORIENTED_EDGE('',*,*,#21538,.F.);
#33492=ORIENTED_EDGE('',*,*,#25324,.T.);
#33493=ORIENTED_EDGE('',*,*,#25316,.F.);
#33494=ORIENTED_EDGE('',*,*,#25325,.T.);
#33495=ORIENTED_EDGE('',*,*,#21535,.F.);
#33496=ORIENTED_EDGE('',*,*,#25326,.T.);
#33497=ORIENTED_EDGE('',*,*,#25327,.T.);
#33498=ORIENTED_EDGE('',*,*,#25328,.F.);
#33499=ORIENTED_EDGE('',*,*,#25328,.T.);
#33500=ORIENTED_EDGE('',*,*,#25329,.T.);
#33501=ORIENTED_EDGE('',*,*,#21536,.F.);
#33502=ORIENTED_EDGE('',*,*,#25330,.T.);
#33503=ORIENTED_EDGE('',*,*,#25331,.T.);
#33504=ORIENTED_EDGE('',*,*,#21327,.F.);
#33505=ORIENTED_EDGE('',*,*,#25332,.F.);
#33506=ORIENTED_EDGE('',*,*,#25333,.T.);
#33507=ORIENTED_EDGE('',*,*,#25334,.T.);
#33508=ORIENTED_EDGE('',*,*,#25335,.F.);
#33509=ORIENTED_EDGE('',*,*,#25336,.T.);
#33510=ORIENTED_EDGE('',*,*,#25330,.F.);
#33511=ORIENTED_EDGE('',*,*,#25337,.T.);
#33512=ORIENTED_EDGE('',*,*,#25338,.T.);
#33513=ORIENTED_EDGE('',*,*,#25339,.T.);
#33514=ORIENTED_EDGE('',*,*,#25335,.T.);
#33515=ORIENTED_EDGE('',*,*,#25340,.T.);
#33516=ORIENTED_EDGE('',*,*,#25341,.T.);
#33517=ORIENTED_EDGE('',*,*,#25342,.T.);
#33518=ORIENTED_EDGE('',*,*,#25343,.T.);
#33519=ORIENTED_EDGE('',*,*,#25344,.F.);
#33520=ORIENTED_EDGE('',*,*,#25345,.T.);
#33521=ORIENTED_EDGE('',*,*,#25346,.T.);
#33522=ORIENTED_EDGE('',*,*,#25344,.T.);
#33523=ORIENTED_EDGE('',*,*,#25347,.T.);
#33524=ORIENTED_EDGE('',*,*,#25338,.F.);
#33525=ORIENTED_EDGE('',*,*,#25348,.T.);
#33526=ORIENTED_EDGE('',*,*,#21330,.F.);
#33527=ORIENTED_EDGE('',*,*,#25349,.T.);
#33528=ORIENTED_EDGE('',*,*,#25236,.T.);
#33529=ORIENTED_EDGE('',*,*,#25350,.F.);
#33530=ORIENTED_EDGE('',*,*,#25351,.T.);
#33531=ORIENTED_EDGE('',*,*,#25341,.F.);
#33532=ORIENTED_EDGE('',*,*,#25352,.T.);
#33533=ORIENTED_EDGE('',*,*,#25353,.T.);
#33534=ORIENTED_EDGE('',*,*,#25354,.T.);
#33535=ORIENTED_EDGE('',*,*,#25350,.T.);
#33536=ORIENTED_EDGE('',*,*,#25355,.T.);
#33537=ORIENTED_EDGE('',*,*,#25356,.T.);
#33538=ORIENTED_EDGE('',*,*,#25357,.T.);
#33539=ORIENTED_EDGE('',*,*,#25358,.T.);
#33540=ORIENTED_EDGE('',*,*,#25359,.F.);
#33541=ORIENTED_EDGE('',*,*,#25360,.T.);
#33542=ORIENTED_EDGE('',*,*,#25361,.T.);
#33543=ORIENTED_EDGE('',*,*,#25359,.T.);
#33544=ORIENTED_EDGE('',*,*,#25362,.T.);
#33545=ORIENTED_EDGE('',*,*,#25353,.F.);
#33546=ORIENTED_EDGE('',*,*,#25363,.T.);
#33547=ORIENTED_EDGE('',*,*,#25364,.F.);
#33548=ORIENTED_EDGE('',*,*,#25365,.T.);
#33549=ORIENTED_EDGE('',*,*,#25356,.F.);
#33550=ORIENTED_EDGE('',*,*,#25366,.T.);
#33551=ORIENTED_EDGE('',*,*,#25367,.T.);
#33552=ORIENTED_EDGE('',*,*,#25368,.T.);
#33553=ORIENTED_EDGE('',*,*,#25364,.T.);
#33554=ORIENTED_EDGE('',*,*,#25369,.T.);
#33555=ORIENTED_EDGE('',*,*,#25370,.T.);
#33556=ORIENTED_EDGE('',*,*,#25371,.T.);
#33557=ORIENTED_EDGE('',*,*,#25372,.T.);
#33558=ORIENTED_EDGE('',*,*,#25373,.F.);
#33559=ORIENTED_EDGE('',*,*,#25374,.T.);
#33560=ORIENTED_EDGE('',*,*,#25375,.T.);
#33561=ORIENTED_EDGE('',*,*,#25373,.T.);
#33562=ORIENTED_EDGE('',*,*,#25376,.T.);
#33563=ORIENTED_EDGE('',*,*,#25367,.F.);
#33564=ORIENTED_EDGE('',*,*,#25377,.T.);
#33565=ORIENTED_EDGE('',*,*,#25378,.F.);
#33566=ORIENTED_EDGE('',*,*,#25379,.T.);
#33567=ORIENTED_EDGE('',*,*,#25370,.F.);
#33568=ORIENTED_EDGE('',*,*,#25380,.T.);
#33569=ORIENTED_EDGE('',*,*,#25381,.T.);
#33570=ORIENTED_EDGE('',*,*,#25382,.T.);
#33571=ORIENTED_EDGE('',*,*,#25378,.T.);
#33572=ORIENTED_EDGE('',*,*,#25383,.T.);
#33573=ORIENTED_EDGE('',*,*,#25384,.T.);
#33574=ORIENTED_EDGE('',*,*,#25385,.T.);
#33575=ORIENTED_EDGE('',*,*,#25386,.T.);
#33576=ORIENTED_EDGE('',*,*,#25387,.F.);
#33577=ORIENTED_EDGE('',*,*,#25388,.T.);
#33578=ORIENTED_EDGE('',*,*,#25389,.T.);
#33579=ORIENTED_EDGE('',*,*,#25387,.T.);
#33580=ORIENTED_EDGE('',*,*,#25390,.T.);
#33581=ORIENTED_EDGE('',*,*,#25381,.F.);
#33582=ORIENTED_EDGE('',*,*,#25391,.T.);
#33583=ORIENTED_EDGE('',*,*,#25392,.F.);
#33584=ORIENTED_EDGE('',*,*,#25393,.T.);
#33585=ORIENTED_EDGE('',*,*,#25384,.F.);
#33586=ORIENTED_EDGE('',*,*,#25394,.T.);
#33587=ORIENTED_EDGE('',*,*,#25395,.T.);
#33588=ORIENTED_EDGE('',*,*,#25396,.T.);
#33589=ORIENTED_EDGE('',*,*,#25392,.T.);
#33590=ORIENTED_EDGE('',*,*,#25397,.T.);
#33591=ORIENTED_EDGE('',*,*,#25398,.T.);
#33592=ORIENTED_EDGE('',*,*,#25399,.T.);
#33593=ORIENTED_EDGE('',*,*,#25400,.T.);
#33594=ORIENTED_EDGE('',*,*,#25401,.F.);
#33595=ORIENTED_EDGE('',*,*,#25402,.T.);
#33596=ORIENTED_EDGE('',*,*,#25403,.T.);
#33597=ORIENTED_EDGE('',*,*,#25401,.T.);
#33598=ORIENTED_EDGE('',*,*,#25404,.T.);
#33599=ORIENTED_EDGE('',*,*,#25395,.F.);
#33600=ORIENTED_EDGE('',*,*,#25405,.T.);
#33601=ORIENTED_EDGE('',*,*,#25406,.F.);
#33602=ORIENTED_EDGE('',*,*,#25407,.T.);
#33603=ORIENTED_EDGE('',*,*,#25398,.F.);
#33604=ORIENTED_EDGE('',*,*,#25408,.T.);
#33605=ORIENTED_EDGE('',*,*,#25409,.T.);
#33606=ORIENTED_EDGE('',*,*,#25410,.T.);
#33607=ORIENTED_EDGE('',*,*,#25406,.T.);
#33608=ORIENTED_EDGE('',*,*,#25411,.T.);
#33609=ORIENTED_EDGE('',*,*,#25412,.T.);
#33610=ORIENTED_EDGE('',*,*,#25413,.T.);
#33611=ORIENTED_EDGE('',*,*,#25414,.T.);
#33612=ORIENTED_EDGE('',*,*,#25415,.F.);
#33613=ORIENTED_EDGE('',*,*,#25416,.T.);
#33614=ORIENTED_EDGE('',*,*,#25417,.T.);
#33615=ORIENTED_EDGE('',*,*,#25415,.T.);
#33616=ORIENTED_EDGE('',*,*,#25418,.T.);
#33617=ORIENTED_EDGE('',*,*,#25409,.F.);
#33618=ORIENTED_EDGE('',*,*,#25419,.T.);
#33619=ORIENTED_EDGE('',*,*,#21544,.F.);
#33620=ORIENTED_EDGE('',*,*,#25420,.T.);
#33621=ORIENTED_EDGE('',*,*,#25412,.F.);
#33622=ORIENTED_EDGE('',*,*,#25421,.T.);
#33623=ORIENTED_EDGE('',*,*,#21541,.F.);
#33624=ORIENTED_EDGE('',*,*,#25422,.T.);
#33625=ORIENTED_EDGE('',*,*,#25423,.T.);
#33626=ORIENTED_EDGE('',*,*,#25424,.F.);
#33627=ORIENTED_EDGE('',*,*,#25424,.T.);
#33628=ORIENTED_EDGE('',*,*,#25425,.T.);
#33629=ORIENTED_EDGE('',*,*,#21542,.F.);
#33630=ORIENTED_EDGE('',*,*,#25426,.T.);
#33631=ORIENTED_EDGE('',*,*,#25427,.T.);
#33632=ORIENTED_EDGE('',*,*,#21323,.F.);
#33633=ORIENTED_EDGE('',*,*,#25428,.F.);
#33634=ORIENTED_EDGE('',*,*,#25429,.T.);
#33635=ORIENTED_EDGE('',*,*,#25430,.T.);
#33636=ORIENTED_EDGE('',*,*,#25431,.F.);
#33637=ORIENTED_EDGE('',*,*,#25432,.T.);
#33638=ORIENTED_EDGE('',*,*,#25426,.F.);
#33639=ORIENTED_EDGE('',*,*,#25433,.T.);
#33640=ORIENTED_EDGE('',*,*,#25434,.T.);
#33641=ORIENTED_EDGE('',*,*,#25435,.T.);
#33642=ORIENTED_EDGE('',*,*,#25431,.T.);
#33643=ORIENTED_EDGE('',*,*,#25436,.T.);
#33644=ORIENTED_EDGE('',*,*,#25437,.T.);
#33645=ORIENTED_EDGE('',*,*,#25438,.T.);
#33646=ORIENTED_EDGE('',*,*,#25439,.T.);
#33647=ORIENTED_EDGE('',*,*,#25440,.F.);
#33648=ORIENTED_EDGE('',*,*,#25441,.T.);
#33649=ORIENTED_EDGE('',*,*,#25442,.T.);
#33650=ORIENTED_EDGE('',*,*,#25440,.T.);
#33651=ORIENTED_EDGE('',*,*,#25443,.T.);
#33652=ORIENTED_EDGE('',*,*,#25434,.F.);
#33653=ORIENTED_EDGE('',*,*,#25444,.T.);
#33654=ORIENTED_EDGE('',*,*,#21326,.F.);
#33655=ORIENTED_EDGE('',*,*,#25445,.T.);
#33656=ORIENTED_EDGE('',*,*,#25332,.T.);
#33657=ORIENTED_EDGE('',*,*,#25446,.F.);
#33658=ORIENTED_EDGE('',*,*,#25447,.T.);
#33659=ORIENTED_EDGE('',*,*,#25437,.F.);
#33660=ORIENTED_EDGE('',*,*,#25448,.T.);
#33661=ORIENTED_EDGE('',*,*,#25449,.T.);
#33662=ORIENTED_EDGE('',*,*,#25450,.T.);
#33663=ORIENTED_EDGE('',*,*,#25446,.T.);
#33664=ORIENTED_EDGE('',*,*,#25451,.T.);
#33665=ORIENTED_EDGE('',*,*,#25452,.T.);
#33666=ORIENTED_EDGE('',*,*,#25453,.T.);
#33667=ORIENTED_EDGE('',*,*,#25454,.T.);
#33668=ORIENTED_EDGE('',*,*,#25455,.F.);
#33669=ORIENTED_EDGE('',*,*,#25456,.T.);
#33670=ORIENTED_EDGE('',*,*,#25457,.T.);
#33671=ORIENTED_EDGE('',*,*,#25455,.T.);
#33672=ORIENTED_EDGE('',*,*,#25458,.T.);
#33673=ORIENTED_EDGE('',*,*,#25449,.F.);
#33674=ORIENTED_EDGE('',*,*,#25459,.T.);
#33675=ORIENTED_EDGE('',*,*,#25460,.F.);
#33676=ORIENTED_EDGE('',*,*,#25461,.T.);
#33677=ORIENTED_EDGE('',*,*,#25452,.F.);
#33678=ORIENTED_EDGE('',*,*,#25462,.T.);
#33679=ORIENTED_EDGE('',*,*,#25463,.T.);
#33680=ORIENTED_EDGE('',*,*,#25464,.T.);
#33681=ORIENTED_EDGE('',*,*,#25460,.T.);
#33682=ORIENTED_EDGE('',*,*,#25465,.T.);
#33683=ORIENTED_EDGE('',*,*,#25466,.T.);
#33684=ORIENTED_EDGE('',*,*,#25467,.T.);
#33685=ORIENTED_EDGE('',*,*,#25468,.T.);
#33686=ORIENTED_EDGE('',*,*,#25469,.F.);
#33687=ORIENTED_EDGE('',*,*,#25470,.T.);
#33688=ORIENTED_EDGE('',*,*,#25471,.T.);
#33689=ORIENTED_EDGE('',*,*,#25469,.T.);
#33690=ORIENTED_EDGE('',*,*,#25472,.T.);
#33691=ORIENTED_EDGE('',*,*,#25463,.F.);
#33692=ORIENTED_EDGE('',*,*,#25473,.T.);
#33693=ORIENTED_EDGE('',*,*,#25474,.F.);
#33694=ORIENTED_EDGE('',*,*,#25475,.T.);
#33695=ORIENTED_EDGE('',*,*,#25466,.F.);
#33696=ORIENTED_EDGE('',*,*,#25476,.T.);
#33697=ORIENTED_EDGE('',*,*,#25477,.T.);
#33698=ORIENTED_EDGE('',*,*,#25478,.T.);
#33699=ORIENTED_EDGE('',*,*,#25474,.T.);
#33700=ORIENTED_EDGE('',*,*,#25479,.T.);
#33701=ORIENTED_EDGE('',*,*,#25480,.T.);
#33702=ORIENTED_EDGE('',*,*,#25481,.T.);
#33703=ORIENTED_EDGE('',*,*,#25482,.T.);
#33704=ORIENTED_EDGE('',*,*,#25483,.F.);
#33705=ORIENTED_EDGE('',*,*,#25484,.T.);
#33706=ORIENTED_EDGE('',*,*,#25485,.T.);
#33707=ORIENTED_EDGE('',*,*,#25483,.T.);
#33708=ORIENTED_EDGE('',*,*,#25486,.T.);
#33709=ORIENTED_EDGE('',*,*,#25477,.F.);
#33710=ORIENTED_EDGE('',*,*,#25487,.T.);
#33711=ORIENTED_EDGE('',*,*,#25488,.F.);
#33712=ORIENTED_EDGE('',*,*,#25489,.T.);
#33713=ORIENTED_EDGE('',*,*,#25480,.F.);
#33714=ORIENTED_EDGE('',*,*,#25490,.T.);
#33715=ORIENTED_EDGE('',*,*,#25491,.T.);
#33716=ORIENTED_EDGE('',*,*,#25492,.T.);
#33717=ORIENTED_EDGE('',*,*,#25488,.T.);
#33718=ORIENTED_EDGE('',*,*,#25493,.T.);
#33719=ORIENTED_EDGE('',*,*,#25494,.T.);
#33720=ORIENTED_EDGE('',*,*,#25495,.T.);
#33721=ORIENTED_EDGE('',*,*,#25496,.T.);
#33722=ORIENTED_EDGE('',*,*,#25497,.F.);
#33723=ORIENTED_EDGE('',*,*,#25498,.T.);
#33724=ORIENTED_EDGE('',*,*,#25499,.T.);
#33725=ORIENTED_EDGE('',*,*,#25497,.T.);
#33726=ORIENTED_EDGE('',*,*,#25500,.T.);
#33727=ORIENTED_EDGE('',*,*,#25491,.F.);
#33728=ORIENTED_EDGE('',*,*,#25501,.T.);
#33729=ORIENTED_EDGE('',*,*,#25502,.F.);
#33730=ORIENTED_EDGE('',*,*,#25503,.T.);
#33731=ORIENTED_EDGE('',*,*,#25494,.F.);
#33732=ORIENTED_EDGE('',*,*,#25504,.T.);
#33733=ORIENTED_EDGE('',*,*,#25505,.T.);
#33734=ORIENTED_EDGE('',*,*,#25506,.T.);
#33735=ORIENTED_EDGE('',*,*,#25502,.T.);
#33736=ORIENTED_EDGE('',*,*,#25507,.T.);
#33737=ORIENTED_EDGE('',*,*,#25508,.T.);
#33738=ORIENTED_EDGE('',*,*,#25509,.T.);
#33739=ORIENTED_EDGE('',*,*,#25510,.T.);
#33740=ORIENTED_EDGE('',*,*,#25511,.F.);
#33741=ORIENTED_EDGE('',*,*,#25512,.T.);
#33742=ORIENTED_EDGE('',*,*,#25513,.T.);
#33743=ORIENTED_EDGE('',*,*,#25511,.T.);
#33744=ORIENTED_EDGE('',*,*,#25514,.T.);
#33745=ORIENTED_EDGE('',*,*,#25505,.F.);
#33746=ORIENTED_EDGE('',*,*,#25515,.T.);
#33747=ORIENTED_EDGE('',*,*,#21550,.F.);
#33748=ORIENTED_EDGE('',*,*,#25516,.T.);
#33749=ORIENTED_EDGE('',*,*,#25508,.F.);
#33750=ORIENTED_EDGE('',*,*,#25517,.T.);
#33751=ORIENTED_EDGE('',*,*,#21547,.F.);
#33752=ORIENTED_EDGE('',*,*,#25518,.T.);
#33753=ORIENTED_EDGE('',*,*,#25519,.T.);
#33754=ORIENTED_EDGE('',*,*,#25520,.F.);
#33755=ORIENTED_EDGE('',*,*,#25520,.T.);
#33756=ORIENTED_EDGE('',*,*,#25521,.T.);
#33757=ORIENTED_EDGE('',*,*,#21548,.F.);
#33758=ORIENTED_EDGE('',*,*,#25522,.T.);
#33759=ORIENTED_EDGE('',*,*,#25523,.T.);
#33760=ORIENTED_EDGE('',*,*,#21319,.F.);
#33761=ORIENTED_EDGE('',*,*,#25524,.F.);
#33762=ORIENTED_EDGE('',*,*,#25525,.T.);
#33763=ORIENTED_EDGE('',*,*,#25526,.T.);
#33764=ORIENTED_EDGE('',*,*,#25527,.F.);
#33765=ORIENTED_EDGE('',*,*,#25528,.T.);
#33766=ORIENTED_EDGE('',*,*,#25522,.F.);
#33767=ORIENTED_EDGE('',*,*,#25529,.T.);
#33768=ORIENTED_EDGE('',*,*,#25530,.T.);
#33769=ORIENTED_EDGE('',*,*,#25531,.T.);
#33770=ORIENTED_EDGE('',*,*,#25527,.T.);
#33771=ORIENTED_EDGE('',*,*,#25532,.T.);
#33772=ORIENTED_EDGE('',*,*,#25533,.T.);
#33773=ORIENTED_EDGE('',*,*,#25534,.T.);
#33774=ORIENTED_EDGE('',*,*,#25535,.T.);
#33775=ORIENTED_EDGE('',*,*,#25536,.F.);
#33776=ORIENTED_EDGE('',*,*,#25537,.T.);
#33777=ORIENTED_EDGE('',*,*,#25538,.T.);
#33778=ORIENTED_EDGE('',*,*,#25536,.T.);
#33779=ORIENTED_EDGE('',*,*,#25539,.T.);
#33780=ORIENTED_EDGE('',*,*,#25530,.F.);
#33781=ORIENTED_EDGE('',*,*,#25540,.T.);
#33782=ORIENTED_EDGE('',*,*,#21322,.F.);
#33783=ORIENTED_EDGE('',*,*,#25541,.T.);
#33784=ORIENTED_EDGE('',*,*,#25428,.T.);
#33785=ORIENTED_EDGE('',*,*,#25542,.F.);
#33786=ORIENTED_EDGE('',*,*,#25543,.T.);
#33787=ORIENTED_EDGE('',*,*,#25533,.F.);
#33788=ORIENTED_EDGE('',*,*,#25544,.T.);
#33789=ORIENTED_EDGE('',*,*,#25545,.T.);
#33790=ORIENTED_EDGE('',*,*,#25546,.T.);
#33791=ORIENTED_EDGE('',*,*,#25542,.T.);
#33792=ORIENTED_EDGE('',*,*,#25547,.T.);
#33793=ORIENTED_EDGE('',*,*,#25548,.T.);
#33794=ORIENTED_EDGE('',*,*,#25549,.T.);
#33795=ORIENTED_EDGE('',*,*,#25550,.T.);
#33796=ORIENTED_EDGE('',*,*,#25551,.F.);
#33797=ORIENTED_EDGE('',*,*,#25552,.T.);
#33798=ORIENTED_EDGE('',*,*,#25553,.T.);
#33799=ORIENTED_EDGE('',*,*,#25551,.T.);
#33800=ORIENTED_EDGE('',*,*,#25554,.T.);
#33801=ORIENTED_EDGE('',*,*,#25545,.F.);
#33802=ORIENTED_EDGE('',*,*,#25555,.T.);
#33803=ORIENTED_EDGE('',*,*,#25556,.F.);
#33804=ORIENTED_EDGE('',*,*,#25557,.T.);
#33805=ORIENTED_EDGE('',*,*,#25548,.F.);
#33806=ORIENTED_EDGE('',*,*,#25558,.T.);
#33807=ORIENTED_EDGE('',*,*,#25559,.T.);
#33808=ORIENTED_EDGE('',*,*,#25560,.T.);
#33809=ORIENTED_EDGE('',*,*,#25556,.T.);
#33810=ORIENTED_EDGE('',*,*,#25561,.T.);
#33811=ORIENTED_EDGE('',*,*,#25562,.T.);
#33812=ORIENTED_EDGE('',*,*,#25563,.T.);
#33813=ORIENTED_EDGE('',*,*,#25564,.T.);
#33814=ORIENTED_EDGE('',*,*,#25565,.F.);
#33815=ORIENTED_EDGE('',*,*,#25566,.T.);
#33816=ORIENTED_EDGE('',*,*,#25567,.T.);
#33817=ORIENTED_EDGE('',*,*,#25565,.T.);
#33818=ORIENTED_EDGE('',*,*,#25568,.T.);
#33819=ORIENTED_EDGE('',*,*,#25559,.F.);
#33820=ORIENTED_EDGE('',*,*,#25569,.T.);
#33821=ORIENTED_EDGE('',*,*,#25570,.F.);
#33822=ORIENTED_EDGE('',*,*,#25571,.T.);
#33823=ORIENTED_EDGE('',*,*,#25562,.F.);
#33824=ORIENTED_EDGE('',*,*,#25572,.T.);
#33825=ORIENTED_EDGE('',*,*,#25573,.T.);
#33826=ORIENTED_EDGE('',*,*,#25574,.T.);
#33827=ORIENTED_EDGE('',*,*,#25570,.T.);
#33828=ORIENTED_EDGE('',*,*,#25575,.T.);
#33829=ORIENTED_EDGE('',*,*,#25576,.T.);
#33830=ORIENTED_EDGE('',*,*,#25577,.T.);
#33831=ORIENTED_EDGE('',*,*,#25578,.T.);
#33832=ORIENTED_EDGE('',*,*,#25579,.F.);
#33833=ORIENTED_EDGE('',*,*,#25580,.T.);
#33834=ORIENTED_EDGE('',*,*,#25581,.T.);
#33835=ORIENTED_EDGE('',*,*,#25579,.T.);
#33836=ORIENTED_EDGE('',*,*,#25582,.T.);
#33837=ORIENTED_EDGE('',*,*,#25573,.F.);
#33838=ORIENTED_EDGE('',*,*,#25583,.T.);
#33839=ORIENTED_EDGE('',*,*,#25584,.F.);
#33840=ORIENTED_EDGE('',*,*,#25585,.T.);
#33841=ORIENTED_EDGE('',*,*,#25576,.F.);
#33842=ORIENTED_EDGE('',*,*,#25586,.T.);
#33843=ORIENTED_EDGE('',*,*,#25587,.T.);
#33844=ORIENTED_EDGE('',*,*,#25588,.T.);
#33845=ORIENTED_EDGE('',*,*,#25584,.T.);
#33846=ORIENTED_EDGE('',*,*,#25589,.T.);
#33847=ORIENTED_EDGE('',*,*,#25590,.T.);
#33848=ORIENTED_EDGE('',*,*,#25591,.T.);
#33849=ORIENTED_EDGE('',*,*,#25592,.T.);
#33850=ORIENTED_EDGE('',*,*,#25593,.F.);
#33851=ORIENTED_EDGE('',*,*,#25594,.T.);
#33852=ORIENTED_EDGE('',*,*,#25595,.T.);
#33853=ORIENTED_EDGE('',*,*,#25593,.T.);
#33854=ORIENTED_EDGE('',*,*,#25596,.T.);
#33855=ORIENTED_EDGE('',*,*,#25587,.F.);
#33856=ORIENTED_EDGE('',*,*,#25597,.T.);
#33857=ORIENTED_EDGE('',*,*,#25598,.F.);
#33858=ORIENTED_EDGE('',*,*,#25599,.T.);
#33859=ORIENTED_EDGE('',*,*,#25590,.F.);
#33860=ORIENTED_EDGE('',*,*,#25600,.T.);
#33861=ORIENTED_EDGE('',*,*,#25601,.T.);
#33862=ORIENTED_EDGE('',*,*,#25602,.T.);
#33863=ORIENTED_EDGE('',*,*,#25598,.T.);
#33864=ORIENTED_EDGE('',*,*,#25603,.T.);
#33865=ORIENTED_EDGE('',*,*,#25604,.T.);
#33866=ORIENTED_EDGE('',*,*,#25605,.T.);
#33867=ORIENTED_EDGE('',*,*,#25606,.T.);
#33868=ORIENTED_EDGE('',*,*,#25607,.F.);
#33869=ORIENTED_EDGE('',*,*,#25608,.T.);
#33870=ORIENTED_EDGE('',*,*,#25609,.T.);
#33871=ORIENTED_EDGE('',*,*,#25607,.T.);
#33872=ORIENTED_EDGE('',*,*,#25610,.T.);
#33873=ORIENTED_EDGE('',*,*,#25601,.F.);
#33874=ORIENTED_EDGE('',*,*,#25611,.T.);
#33875=ORIENTED_EDGE('',*,*,#21556,.F.);
#33876=ORIENTED_EDGE('',*,*,#25612,.T.);
#33877=ORIENTED_EDGE('',*,*,#25604,.F.);
#33878=ORIENTED_EDGE('',*,*,#25613,.T.);
#33879=ORIENTED_EDGE('',*,*,#21553,.F.);
#33880=ORIENTED_EDGE('',*,*,#25614,.T.);
#33881=ORIENTED_EDGE('',*,*,#25615,.T.);
#33882=ORIENTED_EDGE('',*,*,#25616,.F.);
#33883=ORIENTED_EDGE('',*,*,#25616,.T.);
#33884=ORIENTED_EDGE('',*,*,#25617,.T.);
#33885=ORIENTED_EDGE('',*,*,#21554,.F.);
#33886=ORIENTED_EDGE('',*,*,#25618,.T.);
#33887=ORIENTED_EDGE('',*,*,#25619,.T.);
#33888=ORIENTED_EDGE('',*,*,#21315,.F.);
#33889=ORIENTED_EDGE('',*,*,#25620,.F.);
#33890=ORIENTED_EDGE('',*,*,#25621,.T.);
#33891=ORIENTED_EDGE('',*,*,#25622,.T.);
#33892=ORIENTED_EDGE('',*,*,#25623,.F.);
#33893=ORIENTED_EDGE('',*,*,#25624,.T.);
#33894=ORIENTED_EDGE('',*,*,#25618,.F.);
#33895=ORIENTED_EDGE('',*,*,#25625,.T.);
#33896=ORIENTED_EDGE('',*,*,#25626,.T.);
#33897=ORIENTED_EDGE('',*,*,#25627,.T.);
#33898=ORIENTED_EDGE('',*,*,#25623,.T.);
#33899=ORIENTED_EDGE('',*,*,#25628,.T.);
#33900=ORIENTED_EDGE('',*,*,#25629,.T.);
#33901=ORIENTED_EDGE('',*,*,#25630,.T.);
#33902=ORIENTED_EDGE('',*,*,#25631,.T.);
#33903=ORIENTED_EDGE('',*,*,#25632,.F.);
#33904=ORIENTED_EDGE('',*,*,#25633,.T.);
#33905=ORIENTED_EDGE('',*,*,#25634,.T.);
#33906=ORIENTED_EDGE('',*,*,#25632,.T.);
#33907=ORIENTED_EDGE('',*,*,#25635,.T.);
#33908=ORIENTED_EDGE('',*,*,#25626,.F.);
#33909=ORIENTED_EDGE('',*,*,#25636,.T.);
#33910=ORIENTED_EDGE('',*,*,#21318,.F.);
#33911=ORIENTED_EDGE('',*,*,#25637,.T.);
#33912=ORIENTED_EDGE('',*,*,#25524,.T.);
#33913=ORIENTED_EDGE('',*,*,#25638,.F.);
#33914=ORIENTED_EDGE('',*,*,#25639,.T.);
#33915=ORIENTED_EDGE('',*,*,#25629,.F.);
#33916=ORIENTED_EDGE('',*,*,#25640,.T.);
#33917=ORIENTED_EDGE('',*,*,#25641,.T.);
#33918=ORIENTED_EDGE('',*,*,#25642,.T.);
#33919=ORIENTED_EDGE('',*,*,#25638,.T.);
#33920=ORIENTED_EDGE('',*,*,#25643,.T.);
#33921=ORIENTED_EDGE('',*,*,#25644,.T.);
#33922=ORIENTED_EDGE('',*,*,#25645,.T.);
#33923=ORIENTED_EDGE('',*,*,#25646,.T.);
#33924=ORIENTED_EDGE('',*,*,#25647,.F.);
#33925=ORIENTED_EDGE('',*,*,#25648,.T.);
#33926=ORIENTED_EDGE('',*,*,#25649,.T.);
#33927=ORIENTED_EDGE('',*,*,#25647,.T.);
#33928=ORIENTED_EDGE('',*,*,#25650,.T.);
#33929=ORIENTED_EDGE('',*,*,#25641,.F.);
#33930=ORIENTED_EDGE('',*,*,#25651,.T.);
#33931=ORIENTED_EDGE('',*,*,#25652,.F.);
#33932=ORIENTED_EDGE('',*,*,#25653,.T.);
#33933=ORIENTED_EDGE('',*,*,#25644,.F.);
#33934=ORIENTED_EDGE('',*,*,#25654,.T.);
#33935=ORIENTED_EDGE('',*,*,#25655,.T.);
#33936=ORIENTED_EDGE('',*,*,#25656,.T.);
#33937=ORIENTED_EDGE('',*,*,#25652,.T.);
#33938=ORIENTED_EDGE('',*,*,#25657,.T.);
#33939=ORIENTED_EDGE('',*,*,#25658,.T.);
#33940=ORIENTED_EDGE('',*,*,#25659,.T.);
#33941=ORIENTED_EDGE('',*,*,#25660,.T.);
#33942=ORIENTED_EDGE('',*,*,#25661,.F.);
#33943=ORIENTED_EDGE('',*,*,#25662,.T.);
#33944=ORIENTED_EDGE('',*,*,#25663,.T.);
#33945=ORIENTED_EDGE('',*,*,#25661,.T.);
#33946=ORIENTED_EDGE('',*,*,#25664,.T.);
#33947=ORIENTED_EDGE('',*,*,#25655,.F.);
#33948=ORIENTED_EDGE('',*,*,#25665,.T.);
#33949=ORIENTED_EDGE('',*,*,#25666,.F.);
#33950=ORIENTED_EDGE('',*,*,#25667,.T.);
#33951=ORIENTED_EDGE('',*,*,#25658,.F.);
#33952=ORIENTED_EDGE('',*,*,#25668,.T.);
#33953=ORIENTED_EDGE('',*,*,#25669,.T.);
#33954=ORIENTED_EDGE('',*,*,#25670,.T.);
#33955=ORIENTED_EDGE('',*,*,#25666,.T.);
#33956=ORIENTED_EDGE('',*,*,#25671,.T.);
#33957=ORIENTED_EDGE('',*,*,#25672,.T.);
#33958=ORIENTED_EDGE('',*,*,#25673,.T.);
#33959=ORIENTED_EDGE('',*,*,#25674,.T.);
#33960=ORIENTED_EDGE('',*,*,#25675,.F.);
#33961=ORIENTED_EDGE('',*,*,#25676,.T.);
#33962=ORIENTED_EDGE('',*,*,#25677,.T.);
#33963=ORIENTED_EDGE('',*,*,#25675,.T.);
#33964=ORIENTED_EDGE('',*,*,#25678,.T.);
#33965=ORIENTED_EDGE('',*,*,#25669,.F.);
#33966=ORIENTED_EDGE('',*,*,#25679,.T.);
#33967=ORIENTED_EDGE('',*,*,#25680,.F.);
#33968=ORIENTED_EDGE('',*,*,#25681,.T.);
#33969=ORIENTED_EDGE('',*,*,#25672,.F.);
#33970=ORIENTED_EDGE('',*,*,#25682,.T.);
#33971=ORIENTED_EDGE('',*,*,#25683,.T.);
#33972=ORIENTED_EDGE('',*,*,#25684,.T.);
#33973=ORIENTED_EDGE('',*,*,#25680,.T.);
#33974=ORIENTED_EDGE('',*,*,#25685,.T.);
#33975=ORIENTED_EDGE('',*,*,#25686,.T.);
#33976=ORIENTED_EDGE('',*,*,#25687,.T.);
#33977=ORIENTED_EDGE('',*,*,#25688,.T.);
#33978=ORIENTED_EDGE('',*,*,#25689,.F.);
#33979=ORIENTED_EDGE('',*,*,#25690,.T.);
#33980=ORIENTED_EDGE('',*,*,#25691,.T.);
#33981=ORIENTED_EDGE('',*,*,#25689,.T.);
#33982=ORIENTED_EDGE('',*,*,#25692,.T.);
#33983=ORIENTED_EDGE('',*,*,#25683,.F.);
#33984=ORIENTED_EDGE('',*,*,#25693,.T.);
#33985=ORIENTED_EDGE('',*,*,#25694,.F.);
#33986=ORIENTED_EDGE('',*,*,#25695,.T.);
#33987=ORIENTED_EDGE('',*,*,#25686,.F.);
#33988=ORIENTED_EDGE('',*,*,#25696,.T.);
#33989=ORIENTED_EDGE('',*,*,#25697,.T.);
#33990=ORIENTED_EDGE('',*,*,#25698,.T.);
#33991=ORIENTED_EDGE('',*,*,#25694,.T.);
#33992=ORIENTED_EDGE('',*,*,#25699,.T.);
#33993=ORIENTED_EDGE('',*,*,#25700,.T.);
#33994=ORIENTED_EDGE('',*,*,#25701,.T.);
#33995=ORIENTED_EDGE('',*,*,#25702,.T.);
#33996=ORIENTED_EDGE('',*,*,#25703,.F.);
#33997=ORIENTED_EDGE('',*,*,#25704,.T.);
#33998=ORIENTED_EDGE('',*,*,#25705,.T.);
#33999=ORIENTED_EDGE('',*,*,#25703,.T.);
#34000=ORIENTED_EDGE('',*,*,#25706,.T.);
#34001=ORIENTED_EDGE('',*,*,#25697,.F.);
#34002=ORIENTED_EDGE('',*,*,#25707,.T.);
#34003=ORIENTED_EDGE('',*,*,#21562,.F.);
#34004=ORIENTED_EDGE('',*,*,#25708,.T.);
#34005=ORIENTED_EDGE('',*,*,#25700,.F.);
#34006=ORIENTED_EDGE('',*,*,#25709,.T.);
#34007=ORIENTED_EDGE('',*,*,#21559,.F.);
#34008=ORIENTED_EDGE('',*,*,#25710,.T.);
#34009=ORIENTED_EDGE('',*,*,#25711,.T.);
#34010=ORIENTED_EDGE('',*,*,#25712,.F.);
#34011=ORIENTED_EDGE('',*,*,#25712,.T.);
#34012=ORIENTED_EDGE('',*,*,#25713,.T.);
#34013=ORIENTED_EDGE('',*,*,#21560,.F.);
#34014=ORIENTED_EDGE('',*,*,#25714,.T.);
#34015=ORIENTED_EDGE('',*,*,#25715,.T.);
#34016=ORIENTED_EDGE('',*,*,#21311,.F.);
#34017=ORIENTED_EDGE('',*,*,#25716,.F.);
#34018=ORIENTED_EDGE('',*,*,#25717,.T.);
#34019=ORIENTED_EDGE('',*,*,#25718,.T.);
#34020=ORIENTED_EDGE('',*,*,#25719,.F.);
#34021=ORIENTED_EDGE('',*,*,#25720,.T.);
#34022=ORIENTED_EDGE('',*,*,#25714,.F.);
#34023=ORIENTED_EDGE('',*,*,#25721,.T.);
#34024=ORIENTED_EDGE('',*,*,#25722,.T.);
#34025=ORIENTED_EDGE('',*,*,#25723,.T.);
#34026=ORIENTED_EDGE('',*,*,#25719,.T.);
#34027=ORIENTED_EDGE('',*,*,#25724,.T.);
#34028=ORIENTED_EDGE('',*,*,#25725,.T.);
#34029=ORIENTED_EDGE('',*,*,#25726,.T.);
#34030=ORIENTED_EDGE('',*,*,#25727,.T.);
#34031=ORIENTED_EDGE('',*,*,#25728,.F.);
#34032=ORIENTED_EDGE('',*,*,#25729,.T.);
#34033=ORIENTED_EDGE('',*,*,#25730,.T.);
#34034=ORIENTED_EDGE('',*,*,#25728,.T.);
#34035=ORIENTED_EDGE('',*,*,#25731,.T.);
#34036=ORIENTED_EDGE('',*,*,#25722,.F.);
#34037=ORIENTED_EDGE('',*,*,#25732,.T.);
#34038=ORIENTED_EDGE('',*,*,#21314,.F.);
#34039=ORIENTED_EDGE('',*,*,#25733,.T.);
#34040=ORIENTED_EDGE('',*,*,#25620,.T.);
#34041=ORIENTED_EDGE('',*,*,#25734,.F.);
#34042=ORIENTED_EDGE('',*,*,#25735,.T.);
#34043=ORIENTED_EDGE('',*,*,#25725,.F.);
#34044=ORIENTED_EDGE('',*,*,#25736,.T.);
#34045=ORIENTED_EDGE('',*,*,#25737,.T.);
#34046=ORIENTED_EDGE('',*,*,#25738,.T.);
#34047=ORIENTED_EDGE('',*,*,#25734,.T.);
#34048=ORIENTED_EDGE('',*,*,#25739,.T.);
#34049=ORIENTED_EDGE('',*,*,#25740,.T.);
#34050=ORIENTED_EDGE('',*,*,#25741,.T.);
#34051=ORIENTED_EDGE('',*,*,#25742,.T.);
#34052=ORIENTED_EDGE('',*,*,#25743,.F.);
#34053=ORIENTED_EDGE('',*,*,#25744,.T.);
#34054=ORIENTED_EDGE('',*,*,#25745,.T.);
#34055=ORIENTED_EDGE('',*,*,#25743,.T.);
#34056=ORIENTED_EDGE('',*,*,#25746,.T.);
#34057=ORIENTED_EDGE('',*,*,#25737,.F.);
#34058=ORIENTED_EDGE('',*,*,#25747,.T.);
#34059=ORIENTED_EDGE('',*,*,#25748,.F.);
#34060=ORIENTED_EDGE('',*,*,#25749,.T.);
#34061=ORIENTED_EDGE('',*,*,#25740,.F.);
#34062=ORIENTED_EDGE('',*,*,#25750,.T.);
#34063=ORIENTED_EDGE('',*,*,#25751,.T.);
#34064=ORIENTED_EDGE('',*,*,#25752,.T.);
#34065=ORIENTED_EDGE('',*,*,#25748,.T.);
#34066=ORIENTED_EDGE('',*,*,#25753,.T.);
#34067=ORIENTED_EDGE('',*,*,#25754,.T.);
#34068=ORIENTED_EDGE('',*,*,#25755,.T.);
#34069=ORIENTED_EDGE('',*,*,#25756,.T.);
#34070=ORIENTED_EDGE('',*,*,#25757,.F.);
#34071=ORIENTED_EDGE('',*,*,#25758,.T.);
#34072=ORIENTED_EDGE('',*,*,#25759,.T.);
#34073=ORIENTED_EDGE('',*,*,#25757,.T.);
#34074=ORIENTED_EDGE('',*,*,#25760,.T.);
#34075=ORIENTED_EDGE('',*,*,#25751,.F.);
#34076=ORIENTED_EDGE('',*,*,#25761,.T.);
#34077=ORIENTED_EDGE('',*,*,#25762,.F.);
#34078=ORIENTED_EDGE('',*,*,#25763,.T.);
#34079=ORIENTED_EDGE('',*,*,#25754,.F.);
#34080=ORIENTED_EDGE('',*,*,#25764,.T.);
#34081=ORIENTED_EDGE('',*,*,#25765,.T.);
#34082=ORIENTED_EDGE('',*,*,#25766,.T.);
#34083=ORIENTED_EDGE('',*,*,#25762,.T.);
#34084=ORIENTED_EDGE('',*,*,#25767,.T.);
#34085=ORIENTED_EDGE('',*,*,#25768,.T.);
#34086=ORIENTED_EDGE('',*,*,#25769,.T.);
#34087=ORIENTED_EDGE('',*,*,#25770,.T.);
#34088=ORIENTED_EDGE('',*,*,#25771,.F.);
#34089=ORIENTED_EDGE('',*,*,#25772,.T.);
#34090=ORIENTED_EDGE('',*,*,#25773,.T.);
#34091=ORIENTED_EDGE('',*,*,#25771,.T.);
#34092=ORIENTED_EDGE('',*,*,#25774,.T.);
#34093=ORIENTED_EDGE('',*,*,#25765,.F.);
#34094=ORIENTED_EDGE('',*,*,#25775,.T.);
#34095=ORIENTED_EDGE('',*,*,#25776,.F.);
#34096=ORIENTED_EDGE('',*,*,#25777,.T.);
#34097=ORIENTED_EDGE('',*,*,#25768,.F.);
#34098=ORIENTED_EDGE('',*,*,#25778,.T.);
#34099=ORIENTED_EDGE('',*,*,#25779,.T.);
#34100=ORIENTED_EDGE('',*,*,#25780,.T.);
#34101=ORIENTED_EDGE('',*,*,#25776,.T.);
#34102=ORIENTED_EDGE('',*,*,#25781,.T.);
#34103=ORIENTED_EDGE('',*,*,#25782,.T.);
#34104=ORIENTED_EDGE('',*,*,#25783,.T.);
#34105=ORIENTED_EDGE('',*,*,#25784,.T.);
#34106=ORIENTED_EDGE('',*,*,#25785,.F.);
#34107=ORIENTED_EDGE('',*,*,#25786,.T.);
#34108=ORIENTED_EDGE('',*,*,#25787,.T.);
#34109=ORIENTED_EDGE('',*,*,#25785,.T.);
#34110=ORIENTED_EDGE('',*,*,#25788,.T.);
#34111=ORIENTED_EDGE('',*,*,#25779,.F.);
#34112=ORIENTED_EDGE('',*,*,#25789,.T.);
#34113=ORIENTED_EDGE('',*,*,#25790,.F.);
#34114=ORIENTED_EDGE('',*,*,#25791,.T.);
#34115=ORIENTED_EDGE('',*,*,#25782,.F.);
#34116=ORIENTED_EDGE('',*,*,#25792,.T.);
#34117=ORIENTED_EDGE('',*,*,#25793,.T.);
#34118=ORIENTED_EDGE('',*,*,#25794,.T.);
#34119=ORIENTED_EDGE('',*,*,#25790,.T.);
#34120=ORIENTED_EDGE('',*,*,#25795,.T.);
#34121=ORIENTED_EDGE('',*,*,#25796,.T.);
#34122=ORIENTED_EDGE('',*,*,#25797,.T.);
#34123=ORIENTED_EDGE('',*,*,#25798,.T.);
#34124=ORIENTED_EDGE('',*,*,#25799,.F.);
#34125=ORIENTED_EDGE('',*,*,#25800,.T.);
#34126=ORIENTED_EDGE('',*,*,#25801,.T.);
#34127=ORIENTED_EDGE('',*,*,#25799,.T.);
#34128=ORIENTED_EDGE('',*,*,#25802,.T.);
#34129=ORIENTED_EDGE('',*,*,#25793,.F.);
#34130=ORIENTED_EDGE('',*,*,#25803,.T.);
#34131=ORIENTED_EDGE('',*,*,#21568,.F.);
#34132=ORIENTED_EDGE('',*,*,#25804,.T.);
#34133=ORIENTED_EDGE('',*,*,#25796,.F.);
#34134=ORIENTED_EDGE('',*,*,#25805,.T.);
#34135=ORIENTED_EDGE('',*,*,#21565,.F.);
#34136=ORIENTED_EDGE('',*,*,#25806,.T.);
#34137=ORIENTED_EDGE('',*,*,#25807,.T.);
#34138=ORIENTED_EDGE('',*,*,#25808,.F.);
#34139=ORIENTED_EDGE('',*,*,#25808,.T.);
#34140=ORIENTED_EDGE('',*,*,#25809,.T.);
#34141=ORIENTED_EDGE('',*,*,#21566,.F.);
#34142=ORIENTED_EDGE('',*,*,#25810,.T.);
#34143=ORIENTED_EDGE('',*,*,#25811,.T.);
#34144=ORIENTED_EDGE('',*,*,#21307,.F.);
#34145=ORIENTED_EDGE('',*,*,#25812,.F.);
#34146=ORIENTED_EDGE('',*,*,#25813,.T.);
#34147=ORIENTED_EDGE('',*,*,#25814,.T.);
#34148=ORIENTED_EDGE('',*,*,#25815,.F.);
#34149=ORIENTED_EDGE('',*,*,#25816,.T.);
#34150=ORIENTED_EDGE('',*,*,#25810,.F.);
#34151=ORIENTED_EDGE('',*,*,#25817,.T.);
#34152=ORIENTED_EDGE('',*,*,#25818,.T.);
#34153=ORIENTED_EDGE('',*,*,#25819,.T.);
#34154=ORIENTED_EDGE('',*,*,#25815,.T.);
#34155=ORIENTED_EDGE('',*,*,#25820,.T.);
#34156=ORIENTED_EDGE('',*,*,#25821,.T.);
#34157=ORIENTED_EDGE('',*,*,#25822,.T.);
#34158=ORIENTED_EDGE('',*,*,#25823,.T.);
#34159=ORIENTED_EDGE('',*,*,#25824,.F.);
#34160=ORIENTED_EDGE('',*,*,#25825,.T.);
#34161=ORIENTED_EDGE('',*,*,#25826,.T.);
#34162=ORIENTED_EDGE('',*,*,#25824,.T.);
#34163=ORIENTED_EDGE('',*,*,#25827,.T.);
#34164=ORIENTED_EDGE('',*,*,#25818,.F.);
#34165=ORIENTED_EDGE('',*,*,#25828,.T.);
#34166=ORIENTED_EDGE('',*,*,#21310,.F.);
#34167=ORIENTED_EDGE('',*,*,#25829,.T.);
#34168=ORIENTED_EDGE('',*,*,#25716,.T.);
#34169=ORIENTED_EDGE('',*,*,#25830,.F.);
#34170=ORIENTED_EDGE('',*,*,#25831,.T.);
#34171=ORIENTED_EDGE('',*,*,#25821,.F.);
#34172=ORIENTED_EDGE('',*,*,#25832,.T.);
#34173=ORIENTED_EDGE('',*,*,#25833,.T.);
#34174=ORIENTED_EDGE('',*,*,#25834,.T.);
#34175=ORIENTED_EDGE('',*,*,#25830,.T.);
#34176=ORIENTED_EDGE('',*,*,#25835,.T.);
#34177=ORIENTED_EDGE('',*,*,#25836,.T.);
#34178=ORIENTED_EDGE('',*,*,#25837,.T.);
#34179=ORIENTED_EDGE('',*,*,#25838,.T.);
#34180=ORIENTED_EDGE('',*,*,#25839,.F.);
#34181=ORIENTED_EDGE('',*,*,#25840,.T.);
#34182=ORIENTED_EDGE('',*,*,#25841,.T.);
#34183=ORIENTED_EDGE('',*,*,#25839,.T.);
#34184=ORIENTED_EDGE('',*,*,#25842,.T.);
#34185=ORIENTED_EDGE('',*,*,#25833,.F.);
#34186=ORIENTED_EDGE('',*,*,#25843,.T.);
#34187=ORIENTED_EDGE('',*,*,#25844,.F.);
#34188=ORIENTED_EDGE('',*,*,#25845,.T.);
#34189=ORIENTED_EDGE('',*,*,#25836,.F.);
#34190=ORIENTED_EDGE('',*,*,#25846,.T.);
#34191=ORIENTED_EDGE('',*,*,#25847,.T.);
#34192=ORIENTED_EDGE('',*,*,#25848,.T.);
#34193=ORIENTED_EDGE('',*,*,#25844,.T.);
#34194=ORIENTED_EDGE('',*,*,#25849,.T.);
#34195=ORIENTED_EDGE('',*,*,#25850,.T.);
#34196=ORIENTED_EDGE('',*,*,#25851,.T.);
#34197=ORIENTED_EDGE('',*,*,#25852,.T.);
#34198=ORIENTED_EDGE('',*,*,#25853,.F.);
#34199=ORIENTED_EDGE('',*,*,#25854,.T.);
#34200=ORIENTED_EDGE('',*,*,#25855,.T.);
#34201=ORIENTED_EDGE('',*,*,#25853,.T.);
#34202=ORIENTED_EDGE('',*,*,#25856,.T.);
#34203=ORIENTED_EDGE('',*,*,#25847,.F.);
#34204=ORIENTED_EDGE('',*,*,#25857,.T.);
#34205=ORIENTED_EDGE('',*,*,#25858,.F.);
#34206=ORIENTED_EDGE('',*,*,#25859,.T.);
#34207=ORIENTED_EDGE('',*,*,#25850,.F.);
#34208=ORIENTED_EDGE('',*,*,#25860,.T.);
#34209=ORIENTED_EDGE('',*,*,#25861,.T.);
#34210=ORIENTED_EDGE('',*,*,#25862,.T.);
#34211=ORIENTED_EDGE('',*,*,#25858,.T.);
#34212=ORIENTED_EDGE('',*,*,#25863,.T.);
#34213=ORIENTED_EDGE('',*,*,#25864,.T.);
#34214=ORIENTED_EDGE('',*,*,#25865,.T.);
#34215=ORIENTED_EDGE('',*,*,#25866,.T.);
#34216=ORIENTED_EDGE('',*,*,#25867,.F.);
#34217=ORIENTED_EDGE('',*,*,#25868,.T.);
#34218=ORIENTED_EDGE('',*,*,#25869,.T.);
#34219=ORIENTED_EDGE('',*,*,#25867,.T.);
#34220=ORIENTED_EDGE('',*,*,#25870,.T.);
#34221=ORIENTED_EDGE('',*,*,#25861,.F.);
#34222=ORIENTED_EDGE('',*,*,#25871,.T.);
#34223=ORIENTED_EDGE('',*,*,#25872,.F.);
#34224=ORIENTED_EDGE('',*,*,#25873,.T.);
#34225=ORIENTED_EDGE('',*,*,#25864,.F.);
#34226=ORIENTED_EDGE('',*,*,#25874,.T.);
#34227=ORIENTED_EDGE('',*,*,#25875,.T.);
#34228=ORIENTED_EDGE('',*,*,#25876,.T.);
#34229=ORIENTED_EDGE('',*,*,#25872,.T.);
#34230=ORIENTED_EDGE('',*,*,#25877,.T.);
#34231=ORIENTED_EDGE('',*,*,#25878,.T.);
#34232=ORIENTED_EDGE('',*,*,#25879,.T.);
#34233=ORIENTED_EDGE('',*,*,#25880,.T.);
#34234=ORIENTED_EDGE('',*,*,#25881,.F.);
#34235=ORIENTED_EDGE('',*,*,#25882,.T.);
#34236=ORIENTED_EDGE('',*,*,#25883,.T.);
#34237=ORIENTED_EDGE('',*,*,#25881,.T.);
#34238=ORIENTED_EDGE('',*,*,#25884,.T.);
#34239=ORIENTED_EDGE('',*,*,#25875,.F.);
#34240=ORIENTED_EDGE('',*,*,#25885,.T.);
#34241=ORIENTED_EDGE('',*,*,#25886,.F.);
#34242=ORIENTED_EDGE('',*,*,#25887,.T.);
#34243=ORIENTED_EDGE('',*,*,#25878,.F.);
#34244=ORIENTED_EDGE('',*,*,#25888,.T.);
#34245=ORIENTED_EDGE('',*,*,#25889,.T.);
#34246=ORIENTED_EDGE('',*,*,#25890,.T.);
#34247=ORIENTED_EDGE('',*,*,#25886,.T.);
#34248=ORIENTED_EDGE('',*,*,#25891,.T.);
#34249=ORIENTED_EDGE('',*,*,#25892,.T.);
#34250=ORIENTED_EDGE('',*,*,#25893,.T.);
#34251=ORIENTED_EDGE('',*,*,#25894,.T.);
#34252=ORIENTED_EDGE('',*,*,#25895,.F.);
#34253=ORIENTED_EDGE('',*,*,#25896,.T.);
#34254=ORIENTED_EDGE('',*,*,#25897,.T.);
#34255=ORIENTED_EDGE('',*,*,#25895,.T.);
#34256=ORIENTED_EDGE('',*,*,#25898,.T.);
#34257=ORIENTED_EDGE('',*,*,#25889,.F.);
#34258=ORIENTED_EDGE('',*,*,#25899,.T.);
#34259=ORIENTED_EDGE('',*,*,#21574,.F.);
#34260=ORIENTED_EDGE('',*,*,#25900,.T.);
#34261=ORIENTED_EDGE('',*,*,#25892,.F.);
#34262=ORIENTED_EDGE('',*,*,#25901,.T.);
#34263=ORIENTED_EDGE('',*,*,#21571,.F.);
#34264=ORIENTED_EDGE('',*,*,#25902,.T.);
#34265=ORIENTED_EDGE('',*,*,#25903,.T.);
#34266=ORIENTED_EDGE('',*,*,#25904,.F.);
#34267=ORIENTED_EDGE('',*,*,#25904,.T.);
#34268=ORIENTED_EDGE('',*,*,#25905,.T.);
#34269=ORIENTED_EDGE('',*,*,#21572,.F.);
#34270=ORIENTED_EDGE('',*,*,#25906,.T.);
#34271=ORIENTED_EDGE('',*,*,#25907,.T.);
#34272=ORIENTED_EDGE('',*,*,#21303,.F.);
#34273=ORIENTED_EDGE('',*,*,#25908,.F.);
#34274=ORIENTED_EDGE('',*,*,#25909,.T.);
#34275=ORIENTED_EDGE('',*,*,#25910,.T.);
#34276=ORIENTED_EDGE('',*,*,#25911,.F.);
#34277=ORIENTED_EDGE('',*,*,#25912,.T.);
#34278=ORIENTED_EDGE('',*,*,#25906,.F.);
#34279=ORIENTED_EDGE('',*,*,#25913,.T.);
#34280=ORIENTED_EDGE('',*,*,#25914,.T.);
#34281=ORIENTED_EDGE('',*,*,#25915,.T.);
#34282=ORIENTED_EDGE('',*,*,#25911,.T.);
#34283=ORIENTED_EDGE('',*,*,#25916,.T.);
#34284=ORIENTED_EDGE('',*,*,#25917,.T.);
#34285=ORIENTED_EDGE('',*,*,#25918,.T.);
#34286=ORIENTED_EDGE('',*,*,#25919,.T.);
#34287=ORIENTED_EDGE('',*,*,#25920,.F.);
#34288=ORIENTED_EDGE('',*,*,#25921,.T.);
#34289=ORIENTED_EDGE('',*,*,#25922,.T.);
#34290=ORIENTED_EDGE('',*,*,#25920,.T.);
#34291=ORIENTED_EDGE('',*,*,#25923,.T.);
#34292=ORIENTED_EDGE('',*,*,#25914,.F.);
#34293=ORIENTED_EDGE('',*,*,#25924,.T.);
#34294=ORIENTED_EDGE('',*,*,#21306,.F.);
#34295=ORIENTED_EDGE('',*,*,#25925,.T.);
#34296=ORIENTED_EDGE('',*,*,#25812,.T.);
#34297=ORIENTED_EDGE('',*,*,#25926,.F.);
#34298=ORIENTED_EDGE('',*,*,#25927,.T.);
#34299=ORIENTED_EDGE('',*,*,#25917,.F.);
#34300=ORIENTED_EDGE('',*,*,#25928,.T.);
#34301=ORIENTED_EDGE('',*,*,#25929,.T.);
#34302=ORIENTED_EDGE('',*,*,#25930,.T.);
#34303=ORIENTED_EDGE('',*,*,#25926,.T.);
#34304=ORIENTED_EDGE('',*,*,#25931,.T.);
#34305=ORIENTED_EDGE('',*,*,#25932,.T.);
#34306=ORIENTED_EDGE('',*,*,#25933,.T.);
#34307=ORIENTED_EDGE('',*,*,#25934,.T.);
#34308=ORIENTED_EDGE('',*,*,#25935,.F.);
#34309=ORIENTED_EDGE('',*,*,#25936,.T.);
#34310=ORIENTED_EDGE('',*,*,#25937,.T.);
#34311=ORIENTED_EDGE('',*,*,#25935,.T.);
#34312=ORIENTED_EDGE('',*,*,#25938,.T.);
#34313=ORIENTED_EDGE('',*,*,#25929,.F.);
#34314=ORIENTED_EDGE('',*,*,#25939,.T.);
#34315=ORIENTED_EDGE('',*,*,#25940,.F.);
#34316=ORIENTED_EDGE('',*,*,#25941,.T.);
#34317=ORIENTED_EDGE('',*,*,#25932,.F.);
#34318=ORIENTED_EDGE('',*,*,#25942,.T.);
#34319=ORIENTED_EDGE('',*,*,#25943,.T.);
#34320=ORIENTED_EDGE('',*,*,#25944,.T.);
#34321=ORIENTED_EDGE('',*,*,#25940,.T.);
#34322=ORIENTED_EDGE('',*,*,#25945,.T.);
#34323=ORIENTED_EDGE('',*,*,#25946,.T.);
#34324=ORIENTED_EDGE('',*,*,#25947,.T.);
#34325=ORIENTED_EDGE('',*,*,#25948,.T.);
#34326=ORIENTED_EDGE('',*,*,#25949,.F.);
#34327=ORIENTED_EDGE('',*,*,#25950,.T.);
#34328=ORIENTED_EDGE('',*,*,#25951,.T.);
#34329=ORIENTED_EDGE('',*,*,#25949,.T.);
#34330=ORIENTED_EDGE('',*,*,#25952,.T.);
#34331=ORIENTED_EDGE('',*,*,#25943,.F.);
#34332=ORIENTED_EDGE('',*,*,#25953,.T.);
#34333=ORIENTED_EDGE('',*,*,#25954,.F.);
#34334=ORIENTED_EDGE('',*,*,#25955,.T.);
#34335=ORIENTED_EDGE('',*,*,#25946,.F.);
#34336=ORIENTED_EDGE('',*,*,#25956,.T.);
#34337=ORIENTED_EDGE('',*,*,#25957,.T.);
#34338=ORIENTED_EDGE('',*,*,#25958,.T.);
#34339=ORIENTED_EDGE('',*,*,#25954,.T.);
#34340=ORIENTED_EDGE('',*,*,#25959,.T.);
#34341=ORIENTED_EDGE('',*,*,#25960,.T.);
#34342=ORIENTED_EDGE('',*,*,#25961,.T.);
#34343=ORIENTED_EDGE('',*,*,#25962,.T.);
#34344=ORIENTED_EDGE('',*,*,#25963,.F.);
#34345=ORIENTED_EDGE('',*,*,#25964,.T.);
#34346=ORIENTED_EDGE('',*,*,#25965,.T.);
#34347=ORIENTED_EDGE('',*,*,#25963,.T.);
#34348=ORIENTED_EDGE('',*,*,#25966,.T.);
#34349=ORIENTED_EDGE('',*,*,#25957,.F.);
#34350=ORIENTED_EDGE('',*,*,#25967,.T.);
#34351=ORIENTED_EDGE('',*,*,#25968,.F.);
#34352=ORIENTED_EDGE('',*,*,#25969,.T.);
#34353=ORIENTED_EDGE('',*,*,#25960,.F.);
#34354=ORIENTED_EDGE('',*,*,#25970,.T.);
#34355=ORIENTED_EDGE('',*,*,#25971,.T.);
#34356=ORIENTED_EDGE('',*,*,#25972,.T.);
#34357=ORIENTED_EDGE('',*,*,#25968,.T.);
#34358=ORIENTED_EDGE('',*,*,#25973,.T.);
#34359=ORIENTED_EDGE('',*,*,#25974,.T.);
#34360=ORIENTED_EDGE('',*,*,#25975,.T.);
#34361=ORIENTED_EDGE('',*,*,#25976,.T.);
#34362=ORIENTED_EDGE('',*,*,#25977,.F.);
#34363=ORIENTED_EDGE('',*,*,#25978,.T.);
#34364=ORIENTED_EDGE('',*,*,#25979,.T.);
#34365=ORIENTED_EDGE('',*,*,#25977,.T.);
#34366=ORIENTED_EDGE('',*,*,#25980,.T.);
#34367=ORIENTED_EDGE('',*,*,#25971,.F.);
#34368=ORIENTED_EDGE('',*,*,#25981,.T.);
#34369=ORIENTED_EDGE('',*,*,#25982,.F.);
#34370=ORIENTED_EDGE('',*,*,#25983,.T.);
#34371=ORIENTED_EDGE('',*,*,#25974,.F.);
#34372=ORIENTED_EDGE('',*,*,#25984,.T.);
#34373=ORIENTED_EDGE('',*,*,#25985,.T.);
#34374=ORIENTED_EDGE('',*,*,#25986,.T.);
#34375=ORIENTED_EDGE('',*,*,#25982,.T.);
#34376=ORIENTED_EDGE('',*,*,#25987,.T.);
#34377=ORIENTED_EDGE('',*,*,#25988,.T.);
#34378=ORIENTED_EDGE('',*,*,#25989,.T.);
#34379=ORIENTED_EDGE('',*,*,#25990,.T.);
#34380=ORIENTED_EDGE('',*,*,#25991,.F.);
#34381=ORIENTED_EDGE('',*,*,#25992,.T.);
#34382=ORIENTED_EDGE('',*,*,#25993,.T.);
#34383=ORIENTED_EDGE('',*,*,#25991,.T.);
#34384=ORIENTED_EDGE('',*,*,#25994,.T.);
#34385=ORIENTED_EDGE('',*,*,#25985,.F.);
#34386=ORIENTED_EDGE('',*,*,#25995,.T.);
#34387=ORIENTED_EDGE('',*,*,#21580,.F.);
#34388=ORIENTED_EDGE('',*,*,#25996,.T.);
#34389=ORIENTED_EDGE('',*,*,#25988,.F.);
#34390=ORIENTED_EDGE('',*,*,#25997,.T.);
#34391=ORIENTED_EDGE('',*,*,#21577,.F.);
#34392=ORIENTED_EDGE('',*,*,#25998,.T.);
#34393=ORIENTED_EDGE('',*,*,#25999,.T.);
#34394=ORIENTED_EDGE('',*,*,#26000,.F.);
#34395=ORIENTED_EDGE('',*,*,#26000,.T.);
#34396=ORIENTED_EDGE('',*,*,#26001,.T.);
#34397=ORIENTED_EDGE('',*,*,#21578,.F.);
#34398=ORIENTED_EDGE('',*,*,#26002,.T.);
#34399=ORIENTED_EDGE('',*,*,#26003,.T.);
#34400=ORIENTED_EDGE('',*,*,#26004,.T.);
#34401=ORIENTED_EDGE('',*,*,#26005,.T.);
#34402=ORIENTED_EDGE('',*,*,#26006,.T.);
#34403=ORIENTED_EDGE('',*,*,#26007,.T.);
#34404=ORIENTED_EDGE('',*,*,#21299,.F.);
#34405=ORIENTED_EDGE('',*,*,#26008,.F.);
#34406=ORIENTED_EDGE('',*,*,#26009,.T.);
#34407=ORIENTED_EDGE('',*,*,#26010,.T.);
#34408=ORIENTED_EDGE('',*,*,#26004,.F.);
#34409=ORIENTED_EDGE('',*,*,#26011,.T.);
#34410=ORIENTED_EDGE('',*,*,#26006,.F.);
#34411=ORIENTED_EDGE('',*,*,#26012,.T.);
#34412=ORIENTED_EDGE('',*,*,#26013,.T.);
#34413=ORIENTED_EDGE('',*,*,#26014,.T.);
#34414=ORIENTED_EDGE('',*,*,#26015,.T.);
#34415=ORIENTED_EDGE('',*,*,#26016,.F.);
#34416=ORIENTED_EDGE('',*,*,#26017,.T.);
#34417=ORIENTED_EDGE('',*,*,#26018,.T.);
#34418=ORIENTED_EDGE('',*,*,#26016,.T.);
#34419=ORIENTED_EDGE('',*,*,#26019,.T.);
#34420=ORIENTED_EDGE('',*,*,#26002,.F.);
#34421=ORIENTED_EDGE('',*,*,#26020,.T.);
#34422=ORIENTED_EDGE('',*,*,#21302,.F.);
#34423=ORIENTED_EDGE('',*,*,#26021,.T.);
#34424=ORIENTED_EDGE('',*,*,#25908,.T.);
#34425=ORIENTED_EDGE('',*,*,#26022,.F.);
#34426=ORIENTED_EDGE('',*,*,#26023,.T.);
#34427=ORIENTED_EDGE('',*,*,#26013,.F.);
#34428=ORIENTED_EDGE('',*,*,#26024,.T.);
#34429=ORIENTED_EDGE('',*,*,#26025,.T.);
#34430=ORIENTED_EDGE('',*,*,#26026,.T.);
#34431=ORIENTED_EDGE('',*,*,#26022,.T.);
#34432=ORIENTED_EDGE('',*,*,#26027,.T.);
#34433=ORIENTED_EDGE('',*,*,#26028,.T.);
#34434=ORIENTED_EDGE('',*,*,#26029,.T.);
#34435=ORIENTED_EDGE('',*,*,#26030,.T.);
#34436=ORIENTED_EDGE('',*,*,#26031,.F.);
#34437=ORIENTED_EDGE('',*,*,#26032,.T.);
#34438=ORIENTED_EDGE('',*,*,#26033,.T.);
#34439=ORIENTED_EDGE('',*,*,#26031,.T.);
#34440=ORIENTED_EDGE('',*,*,#26034,.T.);
#34441=ORIENTED_EDGE('',*,*,#26025,.F.);
#34442=ORIENTED_EDGE('',*,*,#26035,.T.);
#34443=ORIENTED_EDGE('',*,*,#26036,.F.);
#34444=ORIENTED_EDGE('',*,*,#26037,.T.);
#34445=ORIENTED_EDGE('',*,*,#26028,.F.);
#34446=ORIENTED_EDGE('',*,*,#26038,.T.);
#34447=ORIENTED_EDGE('',*,*,#26039,.T.);
#34448=ORIENTED_EDGE('',*,*,#26040,.T.);
#34449=ORIENTED_EDGE('',*,*,#26036,.T.);
#34450=ORIENTED_EDGE('',*,*,#26041,.T.);
#34451=ORIENTED_EDGE('',*,*,#26042,.T.);
#34452=ORIENTED_EDGE('',*,*,#26043,.T.);
#34453=ORIENTED_EDGE('',*,*,#26044,.T.);
#34454=ORIENTED_EDGE('',*,*,#26045,.F.);
#34455=ORIENTED_EDGE('',*,*,#26046,.T.);
#34456=ORIENTED_EDGE('',*,*,#26047,.T.);
#34457=ORIENTED_EDGE('',*,*,#26045,.T.);
#34458=ORIENTED_EDGE('',*,*,#26048,.T.);
#34459=ORIENTED_EDGE('',*,*,#26039,.F.);
#34460=ORIENTED_EDGE('',*,*,#26049,.T.);
#34461=ORIENTED_EDGE('',*,*,#26050,.F.);
#34462=ORIENTED_EDGE('',*,*,#26051,.T.);
#34463=ORIENTED_EDGE('',*,*,#26042,.F.);
#34464=ORIENTED_EDGE('',*,*,#26052,.T.);
#34465=ORIENTED_EDGE('',*,*,#26053,.T.);
#34466=ORIENTED_EDGE('',*,*,#26054,.T.);
#34467=ORIENTED_EDGE('',*,*,#26050,.T.);
#34468=ORIENTED_EDGE('',*,*,#26055,.T.);
#34469=ORIENTED_EDGE('',*,*,#26056,.T.);
#34470=ORIENTED_EDGE('',*,*,#26057,.T.);
#34471=ORIENTED_EDGE('',*,*,#26058,.T.);
#34472=ORIENTED_EDGE('',*,*,#26059,.F.);
#34473=ORIENTED_EDGE('',*,*,#26060,.T.);
#34474=ORIENTED_EDGE('',*,*,#26061,.T.);
#34475=ORIENTED_EDGE('',*,*,#26059,.T.);
#34476=ORIENTED_EDGE('',*,*,#26062,.T.);
#34477=ORIENTED_EDGE('',*,*,#26053,.F.);
#34478=ORIENTED_EDGE('',*,*,#26063,.T.);
#34479=ORIENTED_EDGE('',*,*,#26064,.F.);
#34480=ORIENTED_EDGE('',*,*,#26065,.T.);
#34481=ORIENTED_EDGE('',*,*,#26056,.F.);
#34482=ORIENTED_EDGE('',*,*,#26066,.T.);
#34483=ORIENTED_EDGE('',*,*,#26067,.T.);
#34484=ORIENTED_EDGE('',*,*,#26068,.T.);
#34485=ORIENTED_EDGE('',*,*,#26064,.T.);
#34486=ORIENTED_EDGE('',*,*,#26069,.T.);
#34487=ORIENTED_EDGE('',*,*,#26070,.T.);
#34488=ORIENTED_EDGE('',*,*,#26071,.T.);
#34489=ORIENTED_EDGE('',*,*,#26072,.T.);
#34490=ORIENTED_EDGE('',*,*,#26073,.F.);
#34491=ORIENTED_EDGE('',*,*,#26074,.T.);
#34492=ORIENTED_EDGE('',*,*,#26075,.T.);
#34493=ORIENTED_EDGE('',*,*,#26073,.T.);
#34494=ORIENTED_EDGE('',*,*,#26076,.T.);
#34495=ORIENTED_EDGE('',*,*,#26067,.F.);
#34496=ORIENTED_EDGE('',*,*,#26077,.T.);
#34497=ORIENTED_EDGE('',*,*,#26078,.F.);
#34498=ORIENTED_EDGE('',*,*,#26079,.T.);
#34499=ORIENTED_EDGE('',*,*,#26070,.F.);
#34500=ORIENTED_EDGE('',*,*,#26080,.T.);
#34501=ORIENTED_EDGE('',*,*,#26081,.T.);
#34502=ORIENTED_EDGE('',*,*,#26082,.T.);
#34503=ORIENTED_EDGE('',*,*,#26078,.T.);
#34504=ORIENTED_EDGE('',*,*,#26083,.T.);
#34505=ORIENTED_EDGE('',*,*,#26084,.T.);
#34506=ORIENTED_EDGE('',*,*,#26085,.T.);
#34507=ORIENTED_EDGE('',*,*,#26086,.T.);
#34508=ORIENTED_EDGE('',*,*,#26087,.F.);
#34509=ORIENTED_EDGE('',*,*,#26088,.T.);
#34510=ORIENTED_EDGE('',*,*,#26089,.T.);
#34511=ORIENTED_EDGE('',*,*,#26087,.T.);
#34512=ORIENTED_EDGE('',*,*,#26090,.T.);
#34513=ORIENTED_EDGE('',*,*,#26081,.F.);
#34514=ORIENTED_EDGE('',*,*,#26091,.T.);
#34515=ORIENTED_EDGE('',*,*,#21586,.F.);
#34516=ORIENTED_EDGE('',*,*,#26092,.T.);
#34517=ORIENTED_EDGE('',*,*,#26084,.F.);
#34518=ORIENTED_EDGE('',*,*,#26093,.T.);
#34519=ORIENTED_EDGE('',*,*,#21583,.F.);
#34520=ORIENTED_EDGE('',*,*,#26094,.T.);
#34521=ORIENTED_EDGE('',*,*,#26095,.T.);
#34522=ORIENTED_EDGE('',*,*,#26096,.F.);
#34523=ORIENTED_EDGE('',*,*,#26096,.T.);
#34524=ORIENTED_EDGE('',*,*,#26097,.T.);
#34525=ORIENTED_EDGE('',*,*,#21584,.F.);
#34526=ORIENTED_EDGE('',*,*,#26098,.T.);
#34527=ORIENTED_EDGE('',*,*,#26099,.T.);
#34528=ORIENTED_EDGE('',*,*,#26100,.T.);
#34529=ORIENTED_EDGE('',*,*,#26101,.T.);
#34530=ORIENTED_EDGE('',*,*,#26102,.T.);
#34531=ORIENTED_EDGE('',*,*,#26103,.T.);
#34532=ORIENTED_EDGE('',*,*,#26104,.T.);
#34533=ORIENTED_EDGE('',*,*,#26105,.T.);
#34534=ORIENTED_EDGE('',*,*,#26106,.T.);
#34535=ORIENTED_EDGE('',*,*,#26107,.T.);
#34536=ORIENTED_EDGE('',*,*,#21295,.F.);
#34537=ORIENTED_EDGE('',*,*,#26108,.F.);
#34538=ORIENTED_EDGE('',*,*,#26109,.T.);
#34539=ORIENTED_EDGE('',*,*,#26110,.T.);
#34540=ORIENTED_EDGE('',*,*,#26104,.F.);
#34541=ORIENTED_EDGE('',*,*,#26111,.T.);
#34542=ORIENTED_EDGE('',*,*,#26106,.F.);
#34543=ORIENTED_EDGE('',*,*,#26112,.T.);
#34544=ORIENTED_EDGE('',*,*,#26113,.T.);
#34545=ORIENTED_EDGE('',*,*,#26114,.T.);
#34546=ORIENTED_EDGE('',*,*,#26115,.T.);
#34547=ORIENTED_EDGE('',*,*,#26116,.F.);
#34548=ORIENTED_EDGE('',*,*,#26117,.T.);
#34549=ORIENTED_EDGE('',*,*,#26118,.T.);
#34550=ORIENTED_EDGE('',*,*,#26116,.T.);
#34551=ORIENTED_EDGE('',*,*,#26119,.T.);
#34552=ORIENTED_EDGE('',*,*,#26102,.F.);
#34553=ORIENTED_EDGE('',*,*,#26120,.T.);
#34554=ORIENTED_EDGE('',*,*,#21298,.F.);
#34555=ORIENTED_EDGE('',*,*,#26121,.T.);
#34556=ORIENTED_EDGE('',*,*,#26008,.T.);
#34557=ORIENTED_EDGE('',*,*,#26100,.F.);
#34558=ORIENTED_EDGE('',*,*,#26122,.T.);
#34559=ORIENTED_EDGE('',*,*,#26113,.F.);
#34560=ORIENTED_EDGE('',*,*,#26123,.T.);
#34561=ORIENTED_EDGE('',*,*,#26124,.T.);
#34562=ORIENTED_EDGE('',*,*,#26125,.T.);
#34563=ORIENTED_EDGE('',*,*,#26126,.T.);
#34564=ORIENTED_EDGE('',*,*,#26127,.F.);
#34565=ORIENTED_EDGE('',*,*,#26128,.T.);
#34566=ORIENTED_EDGE('',*,*,#26129,.T.);
#34567=ORIENTED_EDGE('',*,*,#26127,.T.);
#34568=ORIENTED_EDGE('',*,*,#26130,.T.);
#34569=ORIENTED_EDGE('',*,*,#26098,.F.);
#34570=ORIENTED_EDGE('',*,*,#26131,.T.);
#34571=ORIENTED_EDGE('',*,*,#26132,.F.);
#34572=ORIENTED_EDGE('',*,*,#26133,.T.);
#34573=ORIENTED_EDGE('',*,*,#26124,.F.);
#34574=ORIENTED_EDGE('',*,*,#26134,.T.);
#34575=ORIENTED_EDGE('',*,*,#26135,.T.);
#34576=ORIENTED_EDGE('',*,*,#26136,.T.);
#34577=ORIENTED_EDGE('',*,*,#26132,.T.);
#34578=ORIENTED_EDGE('',*,*,#26137,.T.);
#34579=ORIENTED_EDGE('',*,*,#26138,.T.);
#34580=ORIENTED_EDGE('',*,*,#26139,.T.);
#34581=ORIENTED_EDGE('',*,*,#26140,.T.);
#34582=ORIENTED_EDGE('',*,*,#26141,.F.);
#34583=ORIENTED_EDGE('',*,*,#26142,.T.);
#34584=ORIENTED_EDGE('',*,*,#26143,.T.);
#34585=ORIENTED_EDGE('',*,*,#26141,.T.);
#34586=ORIENTED_EDGE('',*,*,#26144,.T.);
#34587=ORIENTED_EDGE('',*,*,#26135,.F.);
#34588=ORIENTED_EDGE('',*,*,#26145,.T.);
#34589=ORIENTED_EDGE('',*,*,#26146,.F.);
#34590=ORIENTED_EDGE('',*,*,#26147,.T.);
#34591=ORIENTED_EDGE('',*,*,#26138,.F.);
#34592=ORIENTED_EDGE('',*,*,#26148,.T.);
#34593=ORIENTED_EDGE('',*,*,#26149,.T.);
#34594=ORIENTED_EDGE('',*,*,#26150,.T.);
#34595=ORIENTED_EDGE('',*,*,#26146,.T.);
#34596=ORIENTED_EDGE('',*,*,#26151,.T.);
#34597=ORIENTED_EDGE('',*,*,#26152,.T.);
#34598=ORIENTED_EDGE('',*,*,#26153,.T.);
#34599=ORIENTED_EDGE('',*,*,#26154,.T.);
#34600=ORIENTED_EDGE('',*,*,#26155,.F.);
#34601=ORIENTED_EDGE('',*,*,#26156,.T.);
#34602=ORIENTED_EDGE('',*,*,#26157,.T.);
#34603=ORIENTED_EDGE('',*,*,#26155,.T.);
#34604=ORIENTED_EDGE('',*,*,#26158,.T.);
#34605=ORIENTED_EDGE('',*,*,#26149,.F.);
#34606=ORIENTED_EDGE('',*,*,#26159,.T.);
#34607=ORIENTED_EDGE('',*,*,#26160,.F.);
#34608=ORIENTED_EDGE('',*,*,#26161,.T.);
#34609=ORIENTED_EDGE('',*,*,#26152,.F.);
#34610=ORIENTED_EDGE('',*,*,#26162,.T.);
#34611=ORIENTED_EDGE('',*,*,#26163,.T.);
#34612=ORIENTED_EDGE('',*,*,#26164,.T.);
#34613=ORIENTED_EDGE('',*,*,#26160,.T.);
#34614=ORIENTED_EDGE('',*,*,#26165,.T.);
#34615=ORIENTED_EDGE('',*,*,#26166,.T.);
#34616=ORIENTED_EDGE('',*,*,#26167,.T.);
#34617=ORIENTED_EDGE('',*,*,#26168,.T.);
#34618=ORIENTED_EDGE('',*,*,#26169,.F.);
#34619=ORIENTED_EDGE('',*,*,#26170,.T.);
#34620=ORIENTED_EDGE('',*,*,#26171,.T.);
#34621=ORIENTED_EDGE('',*,*,#26169,.T.);
#34622=ORIENTED_EDGE('',*,*,#26172,.T.);
#34623=ORIENTED_EDGE('',*,*,#26163,.F.);
#34624=ORIENTED_EDGE('',*,*,#26173,.T.);
#34625=ORIENTED_EDGE('',*,*,#26174,.F.);
#34626=ORIENTED_EDGE('',*,*,#26175,.T.);
#34627=ORIENTED_EDGE('',*,*,#26166,.F.);
#34628=ORIENTED_EDGE('',*,*,#26176,.T.);
#34629=ORIENTED_EDGE('',*,*,#26177,.T.);
#34630=ORIENTED_EDGE('',*,*,#26178,.T.);
#34631=ORIENTED_EDGE('',*,*,#26174,.T.);
#34632=ORIENTED_EDGE('',*,*,#26179,.T.);
#34633=ORIENTED_EDGE('',*,*,#26180,.T.);
#34634=ORIENTED_EDGE('',*,*,#26181,.T.);
#34635=ORIENTED_EDGE('',*,*,#26182,.T.);
#34636=ORIENTED_EDGE('',*,*,#26183,.F.);
#34637=ORIENTED_EDGE('',*,*,#26184,.T.);
#34638=ORIENTED_EDGE('',*,*,#26185,.T.);
#34639=ORIENTED_EDGE('',*,*,#26183,.T.);
#34640=ORIENTED_EDGE('',*,*,#26186,.T.);
#34641=ORIENTED_EDGE('',*,*,#26177,.F.);
#34642=ORIENTED_EDGE('',*,*,#26187,.T.);
#34643=ORIENTED_EDGE('',*,*,#21592,.F.);
#34644=ORIENTED_EDGE('',*,*,#26188,.T.);
#34645=ORIENTED_EDGE('',*,*,#26180,.F.);
#34646=ORIENTED_EDGE('',*,*,#26189,.T.);
#34647=ORIENTED_EDGE('',*,*,#21589,.F.);
#34648=ORIENTED_EDGE('',*,*,#26190,.T.);
#34649=ORIENTED_EDGE('',*,*,#26191,.T.);
#34650=ORIENTED_EDGE('',*,*,#26192,.F.);
#34651=ORIENTED_EDGE('',*,*,#26192,.T.);
#34652=ORIENTED_EDGE('',*,*,#26193,.T.);
#34653=ORIENTED_EDGE('',*,*,#21590,.F.);
#34654=ORIENTED_EDGE('',*,*,#26194,.T.);
#34655=ORIENTED_EDGE('',*,*,#26195,.T.);
#34656=ORIENTED_EDGE('',*,*,#26196,.T.);
#34657=ORIENTED_EDGE('',*,*,#26197,.T.);
#34658=ORIENTED_EDGE('',*,*,#26198,.T.);
#34659=ORIENTED_EDGE('',*,*,#26199,.T.);
#34660=ORIENTED_EDGE('',*,*,#26200,.T.);
#34661=ORIENTED_EDGE('',*,*,#26201,.T.);
#34662=ORIENTED_EDGE('',*,*,#26202,.T.);
#34663=ORIENTED_EDGE('',*,*,#26203,.T.);
#34664=ORIENTED_EDGE('',*,*,#26204,.T.);
#34665=ORIENTED_EDGE('',*,*,#26205,.T.);
#34666=ORIENTED_EDGE('',*,*,#26206,.T.);
#34667=ORIENTED_EDGE('',*,*,#26207,.T.);
#34668=ORIENTED_EDGE('',*,*,#26208,.T.);
#34669=ORIENTED_EDGE('',*,*,#26209,.F.);
#34670=ORIENTED_EDGE('',*,*,#26210,.T.);
#34671=ORIENTED_EDGE('',*,*,#26211,.T.);
#34672=ORIENTED_EDGE('',*,*,#26209,.T.);
#34673=ORIENTED_EDGE('',*,*,#26212,.T.);
#34674=ORIENTED_EDGE('',*,*,#26194,.F.);
#34675=ORIENTED_EDGE('',*,*,#26213,.T.);
#34676=ORIENTED_EDGE('',*,*,#21294,.F.);
#34677=ORIENTED_EDGE('',*,*,#26214,.T.);
#34678=ORIENTED_EDGE('',*,*,#26108,.T.);
#34679=ORIENTED_EDGE('',*,*,#26204,.F.);
#34680=ORIENTED_EDGE('',*,*,#26215,.T.);
#34681=ORIENTED_EDGE('',*,*,#26206,.F.);
#34682=ORIENTED_EDGE('',*,*,#26216,.T.);
#34683=ORIENTED_EDGE('',*,*,#26217,.T.);
#34684=ORIENTED_EDGE('',*,*,#26218,.T.);
#34685=ORIENTED_EDGE('',*,*,#26219,.T.);
#34686=ORIENTED_EDGE('',*,*,#26220,.F.);
#34687=ORIENTED_EDGE('',*,*,#26221,.T.);
#34688=ORIENTED_EDGE('',*,*,#26222,.T.);
#34689=ORIENTED_EDGE('',*,*,#26220,.T.);
#34690=ORIENTED_EDGE('',*,*,#26223,.T.);
#34691=ORIENTED_EDGE('',*,*,#26202,.F.);
#34692=ORIENTED_EDGE('',*,*,#26224,.T.);
#34693=ORIENTED_EDGE('',*,*,#26200,.F.);
#34694=ORIENTED_EDGE('',*,*,#26225,.T.);
#34695=ORIENTED_EDGE('',*,*,#26217,.F.);
#34696=ORIENTED_EDGE('',*,*,#26226,.T.);
#34697=ORIENTED_EDGE('',*,*,#26227,.T.);
#34698=ORIENTED_EDGE('',*,*,#26228,.T.);
#34699=ORIENTED_EDGE('',*,*,#26229,.T.);
#34700=ORIENTED_EDGE('',*,*,#26230,.F.);
#34701=ORIENTED_EDGE('',*,*,#26231,.T.);
#34702=ORIENTED_EDGE('',*,*,#26232,.T.);
#34703=ORIENTED_EDGE('',*,*,#26230,.T.);
#34704=ORIENTED_EDGE('',*,*,#26233,.T.);
#34705=ORIENTED_EDGE('',*,*,#26198,.F.);
#34706=ORIENTED_EDGE('',*,*,#26234,.T.);
#34707=ORIENTED_EDGE('',*,*,#26235,.F.);
#34708=ORIENTED_EDGE('',*,*,#26236,.T.);
#34709=ORIENTED_EDGE('',*,*,#26227,.F.);
#34710=ORIENTED_EDGE('',*,*,#26237,.T.);
#34711=ORIENTED_EDGE('',*,*,#26238,.T.);
#34712=ORIENTED_EDGE('',*,*,#26239,.T.);
#34713=ORIENTED_EDGE('',*,*,#21291,.F.);
#34714=ORIENTED_EDGE('',*,*,#26240,.F.);
#34715=ORIENTED_EDGE('',*,*,#26241,.T.);
#34716=ORIENTED_EDGE('',*,*,#26242,.T.);
#34717=ORIENTED_EDGE('',*,*,#26196,.F.);
#34718=ORIENTED_EDGE('',*,*,#26243,.T.);
#34719=ORIENTED_EDGE('',*,*,#26238,.F.);
#34720=ORIENTED_EDGE('',*,*,#26244,.T.);
#34721=ORIENTED_EDGE('',*,*,#26245,.T.);
#34722=ORIENTED_EDGE('',*,*,#26246,.T.);
#34723=ORIENTED_EDGE('',*,*,#26235,.T.);
#34724=ORIENTED_EDGE('',*,*,#26247,.T.);
#34725=ORIENTED_EDGE('',*,*,#26248,.T.);
#34726=ORIENTED_EDGE('',*,*,#26249,.T.);
#34727=ORIENTED_EDGE('',*,*,#26250,.T.);
#34728=ORIENTED_EDGE('',*,*,#26251,.F.);
#34729=ORIENTED_EDGE('',*,*,#26252,.T.);
#34730=ORIENTED_EDGE('',*,*,#26253,.T.);
#34731=ORIENTED_EDGE('',*,*,#26251,.T.);
#34732=ORIENTED_EDGE('',*,*,#26254,.T.);
#34733=ORIENTED_EDGE('',*,*,#26245,.F.);
#34734=ORIENTED_EDGE('',*,*,#26255,.T.);
#34735=ORIENTED_EDGE('',*,*,#26256,.F.);
#34736=ORIENTED_EDGE('',*,*,#26257,.T.);
#34737=ORIENTED_EDGE('',*,*,#26248,.F.);
#34738=ORIENTED_EDGE('',*,*,#26258,.T.);
#34739=ORIENTED_EDGE('',*,*,#26259,.T.);
#34740=ORIENTED_EDGE('',*,*,#26260,.T.);
#34741=ORIENTED_EDGE('',*,*,#26256,.T.);
#34742=ORIENTED_EDGE('',*,*,#26261,.T.);
#34743=ORIENTED_EDGE('',*,*,#26262,.T.);
#34744=ORIENTED_EDGE('',*,*,#26263,.T.);
#34745=ORIENTED_EDGE('',*,*,#26264,.T.);
#34746=ORIENTED_EDGE('',*,*,#26265,.F.);
#34747=ORIENTED_EDGE('',*,*,#26266,.T.);
#34748=ORIENTED_EDGE('',*,*,#26267,.T.);
#34749=ORIENTED_EDGE('',*,*,#26265,.T.);
#34750=ORIENTED_EDGE('',*,*,#26268,.T.);
#34751=ORIENTED_EDGE('',*,*,#26259,.F.);
#34752=ORIENTED_EDGE('',*,*,#26269,.T.);
#34753=ORIENTED_EDGE('',*,*,#26270,.F.);
#34754=ORIENTED_EDGE('',*,*,#26271,.T.);
#34755=ORIENTED_EDGE('',*,*,#26262,.F.);
#34756=ORIENTED_EDGE('',*,*,#26272,.T.);
#34757=ORIENTED_EDGE('',*,*,#26273,.T.);
#34758=ORIENTED_EDGE('',*,*,#26274,.T.);
#34759=ORIENTED_EDGE('',*,*,#26270,.T.);
#34760=ORIENTED_EDGE('',*,*,#26275,.T.);
#34761=ORIENTED_EDGE('',*,*,#26276,.T.);
#34762=ORIENTED_EDGE('',*,*,#26277,.T.);
#34763=ORIENTED_EDGE('',*,*,#26278,.T.);
#34764=ORIENTED_EDGE('',*,*,#26279,.F.);
#34765=ORIENTED_EDGE('',*,*,#26280,.T.);
#34766=ORIENTED_EDGE('',*,*,#26281,.T.);
#34767=ORIENTED_EDGE('',*,*,#26279,.T.);
#34768=ORIENTED_EDGE('',*,*,#26282,.T.);
#34769=ORIENTED_EDGE('',*,*,#26273,.F.);
#34770=ORIENTED_EDGE('',*,*,#26283,.T.);
#34771=ORIENTED_EDGE('',*,*,#21598,.F.);
#34772=ORIENTED_EDGE('',*,*,#26284,.T.);
#34773=ORIENTED_EDGE('',*,*,#26276,.F.);
#34774=ORIENTED_EDGE('',*,*,#26285,.T.);
#34775=ORIENTED_EDGE('',*,*,#21595,.F.);
#34776=ORIENTED_EDGE('',*,*,#26286,.T.);
#34777=ORIENTED_EDGE('',*,*,#26287,.T.);
#34778=ORIENTED_EDGE('',*,*,#26288,.F.);
#34779=ORIENTED_EDGE('',*,*,#26288,.T.);
#34780=ORIENTED_EDGE('',*,*,#26289,.T.);
#34781=ORIENTED_EDGE('',*,*,#21596,.F.);
#34782=ORIENTED_EDGE('',*,*,#26290,.T.);
#34783=ORIENTED_EDGE('',*,*,#26291,.T.);
#34784=ORIENTED_EDGE('',*,*,#26292,.T.);
#34785=ORIENTED_EDGE('',*,*,#26293,.T.);
#34786=ORIENTED_EDGE('',*,*,#26294,.T.);
#34787=ORIENTED_EDGE('',*,*,#26295,.T.);
#34788=ORIENTED_EDGE('',*,*,#26296,.T.);
#34789=ORIENTED_EDGE('',*,*,#26297,.T.);
#34790=ORIENTED_EDGE('',*,*,#26298,.T.);
#34791=ORIENTED_EDGE('',*,*,#26299,.T.);
#34792=ORIENTED_EDGE('',*,*,#26300,.T.);
#34793=ORIENTED_EDGE('',*,*,#26301,.T.);
#34794=ORIENTED_EDGE('',*,*,#26302,.T.);
#34795=ORIENTED_EDGE('',*,*,#26303,.T.);
#34796=ORIENTED_EDGE('',*,*,#26304,.T.);
#34797=ORIENTED_EDGE('',*,*,#26305,.T.);
#34798=ORIENTED_EDGE('',*,*,#26306,.T.);
#34799=ORIENTED_EDGE('',*,*,#26307,.T.);
#34800=ORIENTED_EDGE('',*,*,#26308,.T.);
#34801=ORIENTED_EDGE('',*,*,#26309,.F.);
#34802=ORIENTED_EDGE('',*,*,#26310,.T.);
#34803=ORIENTED_EDGE('',*,*,#26311,.T.);
#34804=ORIENTED_EDGE('',*,*,#26309,.T.);
#34805=ORIENTED_EDGE('',*,*,#26312,.T.);
#34806=ORIENTED_EDGE('',*,*,#26294,.F.);
#34807=ORIENTED_EDGE('',*,*,#26313,.T.);
#34808=ORIENTED_EDGE('',*,*,#26304,.F.);
#34809=ORIENTED_EDGE('',*,*,#26314,.T.);
#34810=ORIENTED_EDGE('',*,*,#26306,.F.);
#34811=ORIENTED_EDGE('',*,*,#26315,.T.);
#34812=ORIENTED_EDGE('',*,*,#26316,.T.);
#34813=ORIENTED_EDGE('',*,*,#26317,.T.);
#34814=ORIENTED_EDGE('',*,*,#26318,.T.);
#34815=ORIENTED_EDGE('',*,*,#26319,.F.);
#34816=ORIENTED_EDGE('',*,*,#26320,.T.);
#34817=ORIENTED_EDGE('',*,*,#26321,.T.);
#34818=ORIENTED_EDGE('',*,*,#26319,.T.);
#34819=ORIENTED_EDGE('',*,*,#26322,.T.);
#34820=ORIENTED_EDGE('',*,*,#26302,.F.);
#34821=ORIENTED_EDGE('',*,*,#26323,.T.);
#34822=ORIENTED_EDGE('',*,*,#26300,.F.);
#34823=ORIENTED_EDGE('',*,*,#26324,.T.);
#34824=ORIENTED_EDGE('',*,*,#26316,.F.);
#34825=ORIENTED_EDGE('',*,*,#26325,.T.);
#34826=ORIENTED_EDGE('',*,*,#26326,.T.);
#34827=ORIENTED_EDGE('',*,*,#26327,.T.);
#34828=ORIENTED_EDGE('',*,*,#26328,.T.);
#34829=ORIENTED_EDGE('',*,*,#26329,.F.);
#34830=ORIENTED_EDGE('',*,*,#26330,.T.);
#34831=ORIENTED_EDGE('',*,*,#26331,.T.);
#34832=ORIENTED_EDGE('',*,*,#26329,.T.);
#34833=ORIENTED_EDGE('',*,*,#26332,.T.);
#34834=ORIENTED_EDGE('',*,*,#26298,.F.);
#34835=ORIENTED_EDGE('',*,*,#26333,.T.);
#34836=ORIENTED_EDGE('',*,*,#26334,.F.);
#34837=ORIENTED_EDGE('',*,*,#26335,.T.);
#34838=ORIENTED_EDGE('',*,*,#26326,.F.);
#34839=ORIENTED_EDGE('',*,*,#26336,.T.);
#34840=ORIENTED_EDGE('',*,*,#26337,.T.);
#34841=ORIENTED_EDGE('',*,*,#26338,.T.);
#34842=ORIENTED_EDGE('',*,*,#21287,.F.);
#34843=ORIENTED_EDGE('',*,*,#26339,.F.);
#34844=ORIENTED_EDGE('',*,*,#26340,.T.);
#34845=ORIENTED_EDGE('',*,*,#26341,.T.);
#34846=ORIENTED_EDGE('',*,*,#26292,.F.);
#34847=ORIENTED_EDGE('',*,*,#26342,.T.);
#34848=ORIENTED_EDGE('',*,*,#26337,.F.);
#34849=ORIENTED_EDGE('',*,*,#26343,.T.);
#34850=ORIENTED_EDGE('',*,*,#26344,.T.);
#34851=ORIENTED_EDGE('',*,*,#26345,.T.);
#34852=ORIENTED_EDGE('',*,*,#26346,.T.);
#34853=ORIENTED_EDGE('',*,*,#26347,.F.);
#34854=ORIENTED_EDGE('',*,*,#26348,.T.);
#34855=ORIENTED_EDGE('',*,*,#26349,.T.);
#34856=ORIENTED_EDGE('',*,*,#26347,.T.);
#34857=ORIENTED_EDGE('',*,*,#26350,.T.);
#34858=ORIENTED_EDGE('',*,*,#26290,.F.);
#34859=ORIENTED_EDGE('',*,*,#26351,.T.);
#34860=ORIENTED_EDGE('',*,*,#21290,.F.);
#34861=ORIENTED_EDGE('',*,*,#26352,.T.);
#34862=ORIENTED_EDGE('',*,*,#26240,.T.);
#34863=ORIENTED_EDGE('',*,*,#26296,.F.);
#34864=ORIENTED_EDGE('',*,*,#26353,.T.);
#34865=ORIENTED_EDGE('',*,*,#26344,.F.);
#34866=ORIENTED_EDGE('',*,*,#26354,.T.);
#34867=ORIENTED_EDGE('',*,*,#26355,.T.);
#34868=ORIENTED_EDGE('',*,*,#26356,.T.);
#34869=ORIENTED_EDGE('',*,*,#26334,.T.);
#34870=ORIENTED_EDGE('',*,*,#26357,.T.);
#34871=ORIENTED_EDGE('',*,*,#26358,.T.);
#34872=ORIENTED_EDGE('',*,*,#26359,.T.);
#34873=ORIENTED_EDGE('',*,*,#26360,.T.);
#34874=ORIENTED_EDGE('',*,*,#26361,.F.);
#34875=ORIENTED_EDGE('',*,*,#26362,.T.);
#34876=ORIENTED_EDGE('',*,*,#26363,.T.);
#34877=ORIENTED_EDGE('',*,*,#26361,.T.);
#34878=ORIENTED_EDGE('',*,*,#26364,.T.);
#34879=ORIENTED_EDGE('',*,*,#26355,.F.);
#34880=ORIENTED_EDGE('',*,*,#26365,.T.);
#34881=ORIENTED_EDGE('',*,*,#26366,.F.);
#34882=ORIENTED_EDGE('',*,*,#26367,.T.);
#34883=ORIENTED_EDGE('',*,*,#26358,.F.);
#34884=ORIENTED_EDGE('',*,*,#26368,.T.);
#34885=ORIENTED_EDGE('',*,*,#26369,.T.);
#34886=ORIENTED_EDGE('',*,*,#26370,.T.);
#34887=ORIENTED_EDGE('',*,*,#26366,.T.);
#34888=ORIENTED_EDGE('',*,*,#26371,.T.);
#34889=ORIENTED_EDGE('',*,*,#26372,.T.);
#34890=ORIENTED_EDGE('',*,*,#26373,.T.);
#34891=ORIENTED_EDGE('',*,*,#26374,.T.);
#34892=ORIENTED_EDGE('',*,*,#26375,.F.);
#34893=ORIENTED_EDGE('',*,*,#26376,.T.);
#34894=ORIENTED_EDGE('',*,*,#26377,.T.);
#34895=ORIENTED_EDGE('',*,*,#26375,.T.);
#34896=ORIENTED_EDGE('',*,*,#26378,.T.);
#34897=ORIENTED_EDGE('',*,*,#26369,.F.);
#34898=ORIENTED_EDGE('',*,*,#26379,.T.);
#34899=ORIENTED_EDGE('',*,*,#21604,.F.);
#34900=ORIENTED_EDGE('',*,*,#26380,.T.);
#34901=ORIENTED_EDGE('',*,*,#26372,.F.);
#34902=ORIENTED_EDGE('',*,*,#26381,.T.);
#34903=ORIENTED_EDGE('',*,*,#21601,.F.);
#34904=ORIENTED_EDGE('',*,*,#26382,.T.);
#34905=ORIENTED_EDGE('',*,*,#26383,.T.);
#34906=ORIENTED_EDGE('',*,*,#26384,.F.);
#34907=ORIENTED_EDGE('',*,*,#26384,.T.);
#34908=ORIENTED_EDGE('',*,*,#26385,.T.);
#34909=ORIENTED_EDGE('',*,*,#21602,.F.);
#34910=ORIENTED_EDGE('',*,*,#26386,.T.);
#34911=ORIENTED_EDGE('',*,*,#26387,.T.);
#34912=ORIENTED_EDGE('',*,*,#26388,.T.);
#34913=ORIENTED_EDGE('',*,*,#26389,.T.);
#34914=ORIENTED_EDGE('',*,*,#26390,.T.);
#34915=ORIENTED_EDGE('',*,*,#26391,.T.);
#34916=ORIENTED_EDGE('',*,*,#26392,.T.);
#34917=ORIENTED_EDGE('',*,*,#26393,.T.);
#34918=ORIENTED_EDGE('',*,*,#26394,.T.);
#34919=ORIENTED_EDGE('',*,*,#26395,.T.);
#34920=ORIENTED_EDGE('',*,*,#26396,.T.);
#34921=ORIENTED_EDGE('',*,*,#26397,.T.);
#34922=ORIENTED_EDGE('',*,*,#26398,.T.);
#34923=ORIENTED_EDGE('',*,*,#26399,.T.);
#34924=ORIENTED_EDGE('',*,*,#26400,.T.);
#34925=ORIENTED_EDGE('',*,*,#26401,.T.);
#34926=ORIENTED_EDGE('',*,*,#26402,.T.);
#34927=ORIENTED_EDGE('',*,*,#26403,.T.);
#34928=ORIENTED_EDGE('',*,*,#26404,.T.);
#34929=ORIENTED_EDGE('',*,*,#26405,.T.);
#34930=ORIENTED_EDGE('',*,*,#26406,.T.);
#34931=ORIENTED_EDGE('',*,*,#26407,.T.);
#34932=ORIENTED_EDGE('',*,*,#26408,.T.);
#34933=ORIENTED_EDGE('',*,*,#26409,.F.);
#34934=ORIENTED_EDGE('',*,*,#26410,.T.);
#34935=ORIENTED_EDGE('',*,*,#26411,.T.);
#34936=ORIENTED_EDGE('',*,*,#26409,.T.);
#34937=ORIENTED_EDGE('',*,*,#26412,.T.);
#34938=ORIENTED_EDGE('',*,*,#26390,.F.);
#34939=ORIENTED_EDGE('',*,*,#26413,.T.);
#34940=ORIENTED_EDGE('',*,*,#26404,.F.);
#34941=ORIENTED_EDGE('',*,*,#26414,.T.);
#34942=ORIENTED_EDGE('',*,*,#26406,.F.);
#34943=ORIENTED_EDGE('',*,*,#26415,.T.);
#34944=ORIENTED_EDGE('',*,*,#26416,.T.);
#34945=ORIENTED_EDGE('',*,*,#26417,.T.);
#34946=ORIENTED_EDGE('',*,*,#26418,.T.);
#34947=ORIENTED_EDGE('',*,*,#26419,.F.);
#34948=ORIENTED_EDGE('',*,*,#26420,.T.);
#34949=ORIENTED_EDGE('',*,*,#26421,.T.);
#34950=ORIENTED_EDGE('',*,*,#26419,.T.);
#34951=ORIENTED_EDGE('',*,*,#26422,.T.);
#34952=ORIENTED_EDGE('',*,*,#26402,.F.);
#34953=ORIENTED_EDGE('',*,*,#26423,.T.);
#34954=ORIENTED_EDGE('',*,*,#26400,.F.);
#34955=ORIENTED_EDGE('',*,*,#26424,.T.);
#34956=ORIENTED_EDGE('',*,*,#26416,.F.);
#34957=ORIENTED_EDGE('',*,*,#26425,.T.);
#34958=ORIENTED_EDGE('',*,*,#26426,.T.);
#34959=ORIENTED_EDGE('',*,*,#26427,.T.);
#34960=ORIENTED_EDGE('',*,*,#26428,.T.);
#34961=ORIENTED_EDGE('',*,*,#26429,.F.);
#34962=ORIENTED_EDGE('',*,*,#26430,.T.);
#34963=ORIENTED_EDGE('',*,*,#26431,.T.);
#34964=ORIENTED_EDGE('',*,*,#26429,.T.);
#34965=ORIENTED_EDGE('',*,*,#26432,.T.);
#34966=ORIENTED_EDGE('',*,*,#26398,.F.);
#34967=ORIENTED_EDGE('',*,*,#26433,.T.);
#34968=ORIENTED_EDGE('',*,*,#26434,.F.);
#34969=ORIENTED_EDGE('',*,*,#26435,.T.);
#34970=ORIENTED_EDGE('',*,*,#26426,.F.);
#34971=ORIENTED_EDGE('',*,*,#26436,.T.);
#34972=ORIENTED_EDGE('',*,*,#26437,.T.);
#34973=ORIENTED_EDGE('',*,*,#26438,.T.);
#34974=ORIENTED_EDGE('',*,*,#21283,.F.);
#34975=ORIENTED_EDGE('',*,*,#26439,.F.);
#34976=ORIENTED_EDGE('',*,*,#26440,.T.);
#34977=ORIENTED_EDGE('',*,*,#26441,.T.);
#34978=ORIENTED_EDGE('',*,*,#26396,.F.);
#34979=ORIENTED_EDGE('',*,*,#26442,.T.);
#34980=ORIENTED_EDGE('',*,*,#26437,.F.);
#34981=ORIENTED_EDGE('',*,*,#26443,.T.);
#34982=ORIENTED_EDGE('',*,*,#26444,.T.);
#34983=ORIENTED_EDGE('',*,*,#26445,.T.);
#34984=ORIENTED_EDGE('',*,*,#26446,.T.);
#34985=ORIENTED_EDGE('',*,*,#26447,.F.);
#34986=ORIENTED_EDGE('',*,*,#26448,.T.);
#34987=ORIENTED_EDGE('',*,*,#26449,.T.);
#34988=ORIENTED_EDGE('',*,*,#26447,.T.);
#34989=ORIENTED_EDGE('',*,*,#26450,.T.);
#34990=ORIENTED_EDGE('',*,*,#26394,.F.);
#34991=ORIENTED_EDGE('',*,*,#26451,.T.);
#34992=ORIENTED_EDGE('',*,*,#21286,.F.);
#34993=ORIENTED_EDGE('',*,*,#26452,.T.);
#34994=ORIENTED_EDGE('',*,*,#26339,.T.);
#34995=ORIENTED_EDGE('',*,*,#26388,.F.);
#34996=ORIENTED_EDGE('',*,*,#26453,.T.);
#34997=ORIENTED_EDGE('',*,*,#26444,.F.);
#34998=ORIENTED_EDGE('',*,*,#26454,.T.);
#34999=ORIENTED_EDGE('',*,*,#26455,.T.);
#35000=ORIENTED_EDGE('',*,*,#26456,.T.);
#35001=ORIENTED_EDGE('',*,*,#26457,.T.);
#35002=ORIENTED_EDGE('',*,*,#26458,.F.);
#35003=ORIENTED_EDGE('',*,*,#26459,.T.);
#35004=ORIENTED_EDGE('',*,*,#26460,.T.);
#35005=ORIENTED_EDGE('',*,*,#26458,.T.);
#35006=ORIENTED_EDGE('',*,*,#26461,.T.);
#35007=ORIENTED_EDGE('',*,*,#26386,.F.);
#35008=ORIENTED_EDGE('',*,*,#26462,.T.);
#35009=ORIENTED_EDGE('',*,*,#26392,.F.);
#35010=ORIENTED_EDGE('',*,*,#26463,.T.);
#35011=ORIENTED_EDGE('',*,*,#26455,.F.);
#35012=ORIENTED_EDGE('',*,*,#26464,.T.);
#35013=ORIENTED_EDGE('',*,*,#26465,.T.);
#35014=ORIENTED_EDGE('',*,*,#26466,.T.);
#35015=ORIENTED_EDGE('',*,*,#26434,.T.);
#35016=ORIENTED_EDGE('',*,*,#26467,.T.);
#35017=ORIENTED_EDGE('',*,*,#26468,.T.);
#35018=ORIENTED_EDGE('',*,*,#26469,.T.);
#35019=ORIENTED_EDGE('',*,*,#26470,.T.);
#35020=ORIENTED_EDGE('',*,*,#26471,.F.);
#35021=ORIENTED_EDGE('',*,*,#26472,.T.);
#35022=ORIENTED_EDGE('',*,*,#26473,.T.);
#35023=ORIENTED_EDGE('',*,*,#26471,.T.);
#35024=ORIENTED_EDGE('',*,*,#26474,.T.);
#35025=ORIENTED_EDGE('',*,*,#26465,.F.);
#35026=ORIENTED_EDGE('',*,*,#26475,.T.);
#35027=ORIENTED_EDGE('',*,*,#21610,.F.);
#35028=ORIENTED_EDGE('',*,*,#26476,.T.);
#35029=ORIENTED_EDGE('',*,*,#26468,.F.);
#35030=ORIENTED_EDGE('',*,*,#26477,.T.);
#35031=ORIENTED_EDGE('',*,*,#21607,.F.);
#35032=ORIENTED_EDGE('',*,*,#26478,.T.);
#35033=ORIENTED_EDGE('',*,*,#26479,.T.);
#35034=ORIENTED_EDGE('',*,*,#26480,.F.);
#35035=ORIENTED_EDGE('',*,*,#26480,.T.);
#35036=ORIENTED_EDGE('',*,*,#26481,.T.);
#35037=ORIENTED_EDGE('',*,*,#21608,.F.);
#35038=ORIENTED_EDGE('',*,*,#26482,.T.);
#35039=ORIENTED_EDGE('',*,*,#26483,.T.);
#35040=ORIENTED_EDGE('',*,*,#26484,.T.);
#35041=ORIENTED_EDGE('',*,*,#26485,.T.);
#35042=ORIENTED_EDGE('',*,*,#26486,.T.);
#35043=ORIENTED_EDGE('',*,*,#26487,.T.);
#35044=ORIENTED_EDGE('',*,*,#26488,.T.);
#35045=ORIENTED_EDGE('',*,*,#26489,.T.);
#35046=ORIENTED_EDGE('',*,*,#26490,.T.);
#35047=ORIENTED_EDGE('',*,*,#26491,.T.);
#35048=ORIENTED_EDGE('',*,*,#26492,.T.);
#35049=ORIENTED_EDGE('',*,*,#26493,.T.);
#35050=ORIENTED_EDGE('',*,*,#26494,.T.);
#35051=ORIENTED_EDGE('',*,*,#26495,.T.);
#35052=ORIENTED_EDGE('',*,*,#26496,.T.);
#35053=ORIENTED_EDGE('',*,*,#26497,.T.);
#35054=ORIENTED_EDGE('',*,*,#26498,.T.);
#35055=ORIENTED_EDGE('',*,*,#26499,.T.);
#35056=ORIENTED_EDGE('',*,*,#26500,.T.);
#35057=ORIENTED_EDGE('',*,*,#26501,.T.);
#35058=ORIENTED_EDGE('',*,*,#26502,.T.);
#35059=ORIENTED_EDGE('',*,*,#26503,.T.);
#35060=ORIENTED_EDGE('',*,*,#26504,.T.);
#35061=ORIENTED_EDGE('',*,*,#26505,.T.);
#35062=ORIENTED_EDGE('',*,*,#26506,.T.);
#35063=ORIENTED_EDGE('',*,*,#26507,.T.);
#35064=ORIENTED_EDGE('',*,*,#26508,.T.);
#35065=ORIENTED_EDGE('',*,*,#26509,.F.);
#35066=ORIENTED_EDGE('',*,*,#26510,.T.);
#35067=ORIENTED_EDGE('',*,*,#26511,.T.);
#35068=ORIENTED_EDGE('',*,*,#26509,.T.);
#35069=ORIENTED_EDGE('',*,*,#26512,.T.);
#35070=ORIENTED_EDGE('',*,*,#26486,.F.);
#35071=ORIENTED_EDGE('',*,*,#26513,.T.);
#35072=ORIENTED_EDGE('',*,*,#26504,.F.);
#35073=ORIENTED_EDGE('',*,*,#26514,.T.);
#35074=ORIENTED_EDGE('',*,*,#26506,.F.);
#35075=ORIENTED_EDGE('',*,*,#26515,.T.);
#35076=ORIENTED_EDGE('',*,*,#26516,.T.);
#35077=ORIENTED_EDGE('',*,*,#26517,.T.);
#35078=ORIENTED_EDGE('',*,*,#26518,.T.);
#35079=ORIENTED_EDGE('',*,*,#26519,.F.);
#35080=ORIENTED_EDGE('',*,*,#26520,.T.);
#35081=ORIENTED_EDGE('',*,*,#26521,.T.);
#35082=ORIENTED_EDGE('',*,*,#26519,.T.);
#35083=ORIENTED_EDGE('',*,*,#26522,.T.);
#35084=ORIENTED_EDGE('',*,*,#26502,.F.);
#35085=ORIENTED_EDGE('',*,*,#26523,.T.);
#35086=ORIENTED_EDGE('',*,*,#26500,.F.);
#35087=ORIENTED_EDGE('',*,*,#26524,.T.);
#35088=ORIENTED_EDGE('',*,*,#26516,.F.);
#35089=ORIENTED_EDGE('',*,*,#26525,.T.);
#35090=ORIENTED_EDGE('',*,*,#26526,.T.);
#35091=ORIENTED_EDGE('',*,*,#26527,.T.);
#35092=ORIENTED_EDGE('',*,*,#26528,.T.);
#35093=ORIENTED_EDGE('',*,*,#26529,.F.);
#35094=ORIENTED_EDGE('',*,*,#26530,.T.);
#35095=ORIENTED_EDGE('',*,*,#26531,.T.);
#35096=ORIENTED_EDGE('',*,*,#26529,.T.);
#35097=ORIENTED_EDGE('',*,*,#26532,.T.);
#35098=ORIENTED_EDGE('',*,*,#26498,.F.);
#35099=ORIENTED_EDGE('',*,*,#26533,.T.);
#35100=ORIENTED_EDGE('',*,*,#21616,.F.);
#35101=ORIENTED_EDGE('',*,*,#26534,.T.);
#35102=ORIENTED_EDGE('',*,*,#26526,.F.);
#35103=ORIENTED_EDGE('',*,*,#26535,.T.);
#35104=ORIENTED_EDGE('',*,*,#26536,.T.);
#35105=ORIENTED_EDGE('',*,*,#26537,.T.);
#35106=ORIENTED_EDGE('',*,*,#21479,.F.);
#35107=ORIENTED_EDGE('',*,*,#26538,.F.);
#35108=ORIENTED_EDGE('',*,*,#26539,.T.);
#35109=ORIENTED_EDGE('',*,*,#26540,.T.);
#35110=ORIENTED_EDGE('',*,*,#26496,.F.);
#35111=ORIENTED_EDGE('',*,*,#26541,.T.);
#35112=ORIENTED_EDGE('',*,*,#26536,.F.);
#35113=ORIENTED_EDGE('',*,*,#26542,.T.);
#35114=ORIENTED_EDGE('',*,*,#26543,.T.);
#35115=ORIENTED_EDGE('',*,*,#26544,.T.);
#35116=ORIENTED_EDGE('',*,*,#26545,.T.);
#35117=ORIENTED_EDGE('',*,*,#26546,.F.);
#35118=ORIENTED_EDGE('',*,*,#26547,.T.);
#35119=ORIENTED_EDGE('',*,*,#26548,.T.);
#35120=ORIENTED_EDGE('',*,*,#26546,.T.);
#35121=ORIENTED_EDGE('',*,*,#26549,.T.);
#35122=ORIENTED_EDGE('',*,*,#26494,.F.);
#35123=ORIENTED_EDGE('',*,*,#26550,.T.);
#35124=ORIENTED_EDGE('',*,*,#21282,.F.);
#35125=ORIENTED_EDGE('',*,*,#26551,.T.);
#35126=ORIENTED_EDGE('',*,*,#26439,.T.);
#35127=ORIENTED_EDGE('',*,*,#26492,.F.);
#35128=ORIENTED_EDGE('',*,*,#26552,.T.);
#35129=ORIENTED_EDGE('',*,*,#26543,.F.);
#35130=ORIENTED_EDGE('',*,*,#26553,.T.);
#35131=ORIENTED_EDGE('',*,*,#26554,.T.);
#35132=ORIENTED_EDGE('',*,*,#26555,.T.);
#35133=ORIENTED_EDGE('',*,*,#26556,.T.);
#35134=ORIENTED_EDGE('',*,*,#26557,.F.);
#35135=ORIENTED_EDGE('',*,*,#26558,.T.);
#35136=ORIENTED_EDGE('',*,*,#26559,.T.);
#35137=ORIENTED_EDGE('',*,*,#26557,.T.);
#35138=ORIENTED_EDGE('',*,*,#26560,.T.);
#35139=ORIENTED_EDGE('',*,*,#26490,.F.);
#35140=ORIENTED_EDGE('',*,*,#26561,.T.);
#35141=ORIENTED_EDGE('',*,*,#26484,.F.);
#35142=ORIENTED_EDGE('',*,*,#26562,.T.);
#35143=ORIENTED_EDGE('',*,*,#26554,.F.);
#35144=ORIENTED_EDGE('',*,*,#26563,.T.);
#35145=ORIENTED_EDGE('',*,*,#26564,.T.);
#35146=ORIENTED_EDGE('',*,*,#26565,.T.);
#35147=ORIENTED_EDGE('',*,*,#26566,.T.);
#35148=ORIENTED_EDGE('',*,*,#26567,.F.);
#35149=ORIENTED_EDGE('',*,*,#26568,.T.);
#35150=ORIENTED_EDGE('',*,*,#26569,.T.);
#35151=ORIENTED_EDGE('',*,*,#26567,.T.);
#35152=ORIENTED_EDGE('',*,*,#26570,.T.);
#35153=ORIENTED_EDGE('',*,*,#26482,.F.);
#35154=ORIENTED_EDGE('',*,*,#26571,.T.);
#35155=ORIENTED_EDGE('',*,*,#26488,.F.);
#35156=ORIENTED_EDGE('',*,*,#26572,.T.);
#35157=ORIENTED_EDGE('',*,*,#26564,.F.);
#35158=ORIENTED_EDGE('',*,*,#26573,.T.);
#35159=ORIENTED_EDGE('',*,*,#21613,.F.);
#35160=ORIENTED_EDGE('',*,*,#26574,.T.);
#35161=ORIENTED_EDGE('',*,*,#26575,.T.);
#35162=ORIENTED_EDGE('',*,*,#26576,.F.);
#35163=ORIENTED_EDGE('',*,*,#26576,.T.);
#35164=ORIENTED_EDGE('',*,*,#26577,.T.);
#35165=ORIENTED_EDGE('',*,*,#21614,.F.);
#35166=ORIENTED_EDGE('',*,*,#21619,.F.);
#35167=ORIENTED_EDGE('',*,*,#26578,.T.);
#35168=ORIENTED_EDGE('',*,*,#26579,.T.);
#35169=ORIENTED_EDGE('',*,*,#26580,.F.);
#35170=ORIENTED_EDGE('',*,*,#26580,.T.);
#35171=ORIENTED_EDGE('',*,*,#26581,.T.);
#35172=ORIENTED_EDGE('',*,*,#21620,.F.);
#35173=ORIENTED_EDGE('',*,*,#21478,.F.);
#35174=ORIENTED_EDGE('',*,*,#26582,.T.);
#35175=ORIENTED_EDGE('',*,*,#26538,.T.);
#35176=ORIENTED_EDGE('',*,*,#21274,.F.);
#35177=ORIENTED_EDGE('',*,*,#21279,.T.);
#35178=ORIENTED_EDGE('',*,*,#21276,.T.);
#35179=ORIENTED_EDGE('',*,*,#21482,.T.);
#35180=ORIENTED_EDGE('',*,*,#26583,.T.);
#35181=ORIENTED_EDGE('',*,*,#21925,.F.);
#35182=ORIENTED_EDGE('',*,*,#21931,.F.);
#35183=ORIENTED_EDGE('',*,*,#21947,.F.);
#35184=ORIENTED_EDGE('',*,*,#26489,.F.);
#35185=ORIENTED_EDGE('',*,*,#26573,.F.);
#35186=ORIENTED_EDGE('',*,*,#26584,.F.);
#35187=ORIENTED_EDGE('',*,*,#26513,.F.);
#35188=ORIENTED_EDGE('',*,*,#26584,.T.);
#35189=ORIENTED_EDGE('',*,*,#26569,.F.);
#35190=ORIENTED_EDGE('',*,*,#21914,.F.);
#35191=ORIENTED_EDGE('',*,*,#26583,.F.);
#35192=ORIENTED_EDGE('',*,*,#21943,.F.);
#35193=ORIENTED_EDGE('',*,*,#26510,.F.);
#35194=ORIENTED_EDGE('',*,*,#26585,.F.);
#35195=ORIENTED_EDGE('',*,*,#26571,.F.);
#35196=ORIENTED_EDGE('',*,*,#26485,.F.);
#35197=ORIENTED_EDGE('',*,*,#26563,.F.);
#35198=ORIENTED_EDGE('',*,*,#21903,.F.);
#35199=ORIENTED_EDGE('',*,*,#21919,.F.);
#35200=ORIENTED_EDGE('',*,*,#26586,.T.);
#35201=ORIENTED_EDGE('',*,*,#21897,.F.);
#35202=ORIENTED_EDGE('',*,*,#26586,.F.);
#35203=ORIENTED_EDGE('',*,*,#21915,.F.);
#35204=ORIENTED_EDGE('',*,*,#26568,.F.);
#35205=ORIENTED_EDGE('',*,*,#26585,.T.);
#35206=ORIENTED_EDGE('',*,*,#26559,.F.);
#35207=ORIENTED_EDGE('',*,*,#21886,.F.);
#35208=ORIENTED_EDGE('',*,*,#26587,.F.);
#35209=ORIENTED_EDGE('',*,*,#26561,.F.);
#35210=ORIENTED_EDGE('',*,*,#26493,.F.);
#35211=ORIENTED_EDGE('',*,*,#26553,.F.);
#35212=ORIENTED_EDGE('',*,*,#21875,.F.);
#35213=ORIENTED_EDGE('',*,*,#21891,.F.);
#35214=ORIENTED_EDGE('',*,*,#26588,.T.);
#35215=ORIENTED_EDGE('',*,*,#21869,.F.);
#35216=ORIENTED_EDGE('',*,*,#26588,.F.);
#35217=ORIENTED_EDGE('',*,*,#21887,.F.);
#35218=ORIENTED_EDGE('',*,*,#26558,.F.);
#35219=ORIENTED_EDGE('',*,*,#26587,.T.);
#35220=ORIENTED_EDGE('',*,*,#26548,.F.);
#35221=ORIENTED_EDGE('',*,*,#21858,.F.);
#35222=ORIENTED_EDGE('',*,*,#26589,.F.);
#35223=ORIENTED_EDGE('',*,*,#26550,.F.);
#35224=ORIENTED_EDGE('',*,*,#26497,.F.);
#35225=ORIENTED_EDGE('',*,*,#26542,.F.);
#35226=ORIENTED_EDGE('',*,*,#21847,.F.);
#35227=ORIENTED_EDGE('',*,*,#21863,.F.);
#35228=ORIENTED_EDGE('',*,*,#26590,.T.);
#35229=ORIENTED_EDGE('',*,*,#21841,.F.);
#35230=ORIENTED_EDGE('',*,*,#26590,.F.);
#35231=ORIENTED_EDGE('',*,*,#21859,.F.);
#35232=ORIENTED_EDGE('',*,*,#26547,.F.);
#35233=ORIENTED_EDGE('',*,*,#26589,.T.);
#35234=ORIENTED_EDGE('',*,*,#26540,.F.);
#35235=ORIENTED_EDGE('',*,*,#21830,.F.);
#35236=ORIENTED_EDGE('',*,*,#21819,.F.);
#35237=ORIENTED_EDGE('',*,*,#21835,.F.);
#35238=ORIENTED_EDGE('',*,*,#26591,.T.);
#35239=ORIENTED_EDGE('',*,*,#21807,.F.);
#35240=ORIENTED_EDGE('',*,*,#26592,.F.);
#35241=ORIENTED_EDGE('',*,*,#26582,.F.);
#35242=ORIENTED_EDGE('',*,*,#21477,.F.);
#35243=ORIENTED_EDGE('',*,*,#21801,.F.);
#35244=ORIENTED_EDGE('',*,*,#26591,.F.);
#35245=ORIENTED_EDGE('',*,*,#21831,.F.);
#35246=ORIENTED_EDGE('',*,*,#26539,.F.);
#35247=ORIENTED_EDGE('',*,*,#26592,.T.);
#35248=ORIENTED_EDGE('',*,*,#21476,.F.);
#35249=ORIENTED_EDGE('',*,*,#26535,.F.);
#35250=ORIENTED_EDGE('',*,*,#26593,.F.);
#35251=ORIENTED_EDGE('',*,*,#21617,.F.);
#35252=ORIENTED_EDGE('',*,*,#26593,.T.);
#35253=ORIENTED_EDGE('',*,*,#26531,.F.);
#35254=ORIENTED_EDGE('',*,*,#26578,.F.);
#35255=ORIENTED_EDGE('',*,*,#21618,.F.);
#35256=ORIENTED_EDGE('',*,*,#26594,.F.);
#35257=ORIENTED_EDGE('',*,*,#26533,.F.);
#35258=ORIENTED_EDGE('',*,*,#26501,.F.);
#35259=ORIENTED_EDGE('',*,*,#26525,.F.);
#35260=ORIENTED_EDGE('',*,*,#21621,.F.);
#35261=ORIENTED_EDGE('',*,*,#26581,.F.);
#35262=ORIENTED_EDGE('',*,*,#26595,.T.);
#35263=ORIENTED_EDGE('',*,*,#21969,.F.);
#35264=ORIENTED_EDGE('',*,*,#26595,.F.);
#35265=ORIENTED_EDGE('',*,*,#26579,.F.);
#35266=ORIENTED_EDGE('',*,*,#26530,.F.);
#35267=ORIENTED_EDGE('',*,*,#26594,.T.);
#35268=ORIENTED_EDGE('',*,*,#26521,.F.);
#35269=ORIENTED_EDGE('',*,*,#21963,.F.);
#35270=ORIENTED_EDGE('',*,*,#26596,.F.);
#35271=ORIENTED_EDGE('',*,*,#21964,.F.);
#35272=ORIENTED_EDGE('',*,*,#26520,.F.);
#35273=ORIENTED_EDGE('',*,*,#26597,.T.);
#35274=ORIENTED_EDGE('',*,*,#26511,.F.);
#35275=ORIENTED_EDGE('',*,*,#21942,.F.);
#35276=ORIENTED_EDGE('',*,*,#21955,.F.);
#35277=ORIENTED_EDGE('',*,*,#21967,.F.);
#35278=ORIENTED_EDGE('',*,*,#26596,.T.);
#35279=ORIENTED_EDGE('',*,*,#21952,.F.);
#35280=ORIENTED_EDGE('',*,*,#26597,.F.);
#35281=ORIENTED_EDGE('',*,*,#26523,.F.);
#35282=ORIENTED_EDGE('',*,*,#26505,.F.);
#35283=ORIENTED_EDGE('',*,*,#26515,.F.);
#35284=ORIENTED_EDGE('',*,*,#26477,.F.);
#35285=ORIENTED_EDGE('',*,*,#26598,.F.);
#35286=ORIENTED_EDGE('',*,*,#21611,.F.);
#35287=ORIENTED_EDGE('',*,*,#26598,.T.);
#35288=ORIENTED_EDGE('',*,*,#26473,.F.);
#35289=ORIENTED_EDGE('',*,*,#26574,.F.);
#35290=ORIENTED_EDGE('',*,*,#21612,.F.);
#35291=ORIENTED_EDGE('',*,*,#26599,.F.);
#35292=ORIENTED_EDGE('',*,*,#26475,.F.);
#35293=ORIENTED_EDGE('',*,*,#26467,.F.);
#35294=ORIENTED_EDGE('',*,*,#26436,.F.);
#35295=ORIENTED_EDGE('',*,*,#21615,.F.);
#35296=ORIENTED_EDGE('',*,*,#26577,.F.);
#35297=ORIENTED_EDGE('',*,*,#26600,.T.);
#35298=ORIENTED_EDGE('',*,*,#26534,.F.);
#35299=ORIENTED_EDGE('',*,*,#26600,.F.);
#35300=ORIENTED_EDGE('',*,*,#26575,.F.);
#35301=ORIENTED_EDGE('',*,*,#26472,.F.);
#35302=ORIENTED_EDGE('',*,*,#26599,.T.);
#35303=ORIENTED_EDGE('',*,*,#26431,.F.);
#35304=ORIENTED_EDGE('',*,*,#26527,.F.);
#35305=ORIENTED_EDGE('',*,*,#26601,.T.);
#35306=ORIENTED_EDGE('',*,*,#26572,.F.);
#35307=ORIENTED_EDGE('',*,*,#26487,.F.);
#35308=ORIENTED_EDGE('',*,*,#26512,.F.);
#35309=ORIENTED_EDGE('',*,*,#26393,.F.);
#35310=ORIENTED_EDGE('',*,*,#26464,.F.);
#35311=ORIENTED_EDGE('',*,*,#26602,.F.);
#35312=ORIENTED_EDGE('',*,*,#26413,.F.);
#35313=ORIENTED_EDGE('',*,*,#26602,.T.);
#35314=ORIENTED_EDGE('',*,*,#26460,.F.);
#35315=ORIENTED_EDGE('',*,*,#26565,.F.);
#35316=ORIENTED_EDGE('',*,*,#26601,.F.);
#35317=ORIENTED_EDGE('',*,*,#26508,.F.);
#35318=ORIENTED_EDGE('',*,*,#26410,.F.);
#35319=ORIENTED_EDGE('',*,*,#26603,.F.);
#35320=ORIENTED_EDGE('',*,*,#26462,.F.);
#35321=ORIENTED_EDGE('',*,*,#26389,.F.);
#35322=ORIENTED_EDGE('',*,*,#26454,.F.);
#35323=ORIENTED_EDGE('',*,*,#26483,.F.);
#35324=ORIENTED_EDGE('',*,*,#26570,.F.);
#35325=ORIENTED_EDGE('',*,*,#26604,.T.);
#35326=ORIENTED_EDGE('',*,*,#26562,.F.);
#35327=ORIENTED_EDGE('',*,*,#26604,.F.);
#35328=ORIENTED_EDGE('',*,*,#26566,.F.);
#35329=ORIENTED_EDGE('',*,*,#26459,.F.);
#35330=ORIENTED_EDGE('',*,*,#26603,.T.);
#35331=ORIENTED_EDGE('',*,*,#26449,.F.);
#35332=ORIENTED_EDGE('',*,*,#26555,.F.);
#35333=ORIENTED_EDGE('',*,*,#26605,.F.);
#35334=ORIENTED_EDGE('',*,*,#26451,.F.);
#35335=ORIENTED_EDGE('',*,*,#26397,.F.);
#35336=ORIENTED_EDGE('',*,*,#26443,.F.);
#35337=ORIENTED_EDGE('',*,*,#26491,.F.);
#35338=ORIENTED_EDGE('',*,*,#26560,.F.);
#35339=ORIENTED_EDGE('',*,*,#26606,.T.);
#35340=ORIENTED_EDGE('',*,*,#26552,.F.);
#35341=ORIENTED_EDGE('',*,*,#26606,.F.);
#35342=ORIENTED_EDGE('',*,*,#26556,.F.);
#35343=ORIENTED_EDGE('',*,*,#26448,.F.);
#35344=ORIENTED_EDGE('',*,*,#26605,.T.);
#35345=ORIENTED_EDGE('',*,*,#26441,.F.);
#35346=ORIENTED_EDGE('',*,*,#26544,.F.);
#35347=ORIENTED_EDGE('',*,*,#26495,.F.);
#35348=ORIENTED_EDGE('',*,*,#26549,.F.);
#35349=ORIENTED_EDGE('',*,*,#26607,.T.);
#35350=ORIENTED_EDGE('',*,*,#26541,.F.);
#35351=ORIENTED_EDGE('',*,*,#26608,.F.);
#35352=ORIENTED_EDGE('',*,*,#26551,.F.);
#35353=ORIENTED_EDGE('',*,*,#21281,.F.);
#35354=ORIENTED_EDGE('',*,*,#26537,.F.);
#35355=ORIENTED_EDGE('',*,*,#26607,.F.);
#35356=ORIENTED_EDGE('',*,*,#26545,.F.);
#35357=ORIENTED_EDGE('',*,*,#26440,.F.);
#35358=ORIENTED_EDGE('',*,*,#26608,.T.);
#35359=ORIENTED_EDGE('',*,*,#21280,.F.);
#35360=ORIENTED_EDGE('',*,*,#21277,.F.);
#35361=ORIENTED_EDGE('',*,*,#26609,.F.);
#35362=ORIENTED_EDGE('',*,*,#26433,.F.);
#35363=ORIENTED_EDGE('',*,*,#26401,.F.);
#35364=ORIENTED_EDGE('',*,*,#26425,.F.);
#35365=ORIENTED_EDGE('',*,*,#26499,.F.);
#35366=ORIENTED_EDGE('',*,*,#26532,.F.);
#35367=ORIENTED_EDGE('',*,*,#26610,.T.);
#35368=ORIENTED_EDGE('',*,*,#26524,.F.);
#35369=ORIENTED_EDGE('',*,*,#26610,.F.);
#35370=ORIENTED_EDGE('',*,*,#26528,.F.);
#35371=ORIENTED_EDGE('',*,*,#26430,.F.);
#35372=ORIENTED_EDGE('',*,*,#26609,.T.);
#35373=ORIENTED_EDGE('',*,*,#26421,.F.);
#35374=ORIENTED_EDGE('',*,*,#26517,.F.);
#35375=ORIENTED_EDGE('',*,*,#26611,.F.);
#35376=ORIENTED_EDGE('',*,*,#26518,.F.);
#35377=ORIENTED_EDGE('',*,*,#26420,.F.);
#35378=ORIENTED_EDGE('',*,*,#26612,.T.);
#35379=ORIENTED_EDGE('',*,*,#26411,.F.);
#35380=ORIENTED_EDGE('',*,*,#26507,.F.);
#35381=ORIENTED_EDGE('',*,*,#26503,.F.);
#35382=ORIENTED_EDGE('',*,*,#26522,.F.);
#35383=ORIENTED_EDGE('',*,*,#26611,.T.);
#35384=ORIENTED_EDGE('',*,*,#26514,.F.);
#35385=ORIENTED_EDGE('',*,*,#26612,.F.);
#35386=ORIENTED_EDGE('',*,*,#26423,.F.);
#35387=ORIENTED_EDGE('',*,*,#26405,.F.);
#35388=ORIENTED_EDGE('',*,*,#26415,.F.);
#35389=ORIENTED_EDGE('',*,*,#26381,.F.);
#35390=ORIENTED_EDGE('',*,*,#26613,.F.);
#35391=ORIENTED_EDGE('',*,*,#21605,.F.);
#35392=ORIENTED_EDGE('',*,*,#26613,.T.);
#35393=ORIENTED_EDGE('',*,*,#26377,.F.);
#35394=ORIENTED_EDGE('',*,*,#26478,.F.);
#35395=ORIENTED_EDGE('',*,*,#21606,.F.);
#35396=ORIENTED_EDGE('',*,*,#26614,.F.);
#35397=ORIENTED_EDGE('',*,*,#26379,.F.);
#35398=ORIENTED_EDGE('',*,*,#26371,.F.);
#35399=ORIENTED_EDGE('',*,*,#26368,.F.);
#35400=ORIENTED_EDGE('',*,*,#21609,.F.);
#35401=ORIENTED_EDGE('',*,*,#26481,.F.);
#35402=ORIENTED_EDGE('',*,*,#26615,.T.);
#35403=ORIENTED_EDGE('',*,*,#26476,.F.);
#35404=ORIENTED_EDGE('',*,*,#26615,.F.);
#35405=ORIENTED_EDGE('',*,*,#26479,.F.);
#35406=ORIENTED_EDGE('',*,*,#26376,.F.);
#35407=ORIENTED_EDGE('',*,*,#26614,.T.);
#35408=ORIENTED_EDGE('',*,*,#26363,.F.);
#35409=ORIENTED_EDGE('',*,*,#26469,.F.);
#35410=ORIENTED_EDGE('',*,*,#26616,.F.);
#35411=ORIENTED_EDGE('',*,*,#26365,.F.);
#35412=ORIENTED_EDGE('',*,*,#26357,.F.);
#35413=ORIENTED_EDGE('',*,*,#26336,.F.);
#35414=ORIENTED_EDGE('',*,*,#26466,.F.);
#35415=ORIENTED_EDGE('',*,*,#26474,.F.);
#35416=ORIENTED_EDGE('',*,*,#26617,.T.);
#35417=ORIENTED_EDGE('',*,*,#26435,.F.);
#35418=ORIENTED_EDGE('',*,*,#26617,.F.);
#35419=ORIENTED_EDGE('',*,*,#26470,.F.);
#35420=ORIENTED_EDGE('',*,*,#26362,.F.);
#35421=ORIENTED_EDGE('',*,*,#26616,.T.);
#35422=ORIENTED_EDGE('',*,*,#26331,.F.);
#35423=ORIENTED_EDGE('',*,*,#26427,.F.);
#35424=ORIENTED_EDGE('',*,*,#26618,.T.);
#35425=ORIENTED_EDGE('',*,*,#26463,.F.);
#35426=ORIENTED_EDGE('',*,*,#26391,.F.);
#35427=ORIENTED_EDGE('',*,*,#26412,.F.);
#35428=ORIENTED_EDGE('',*,*,#26297,.F.);
#35429=ORIENTED_EDGE('',*,*,#26354,.F.);
#35430=ORIENTED_EDGE('',*,*,#26619,.F.);
#35431=ORIENTED_EDGE('',*,*,#26313,.F.);
#35432=ORIENTED_EDGE('',*,*,#26619,.T.);
#35433=ORIENTED_EDGE('',*,*,#26349,.F.);
#35434=ORIENTED_EDGE('',*,*,#26456,.F.);
#35435=ORIENTED_EDGE('',*,*,#26618,.F.);
#35436=ORIENTED_EDGE('',*,*,#26408,.F.);
#35437=ORIENTED_EDGE('',*,*,#26310,.F.);
#35438=ORIENTED_EDGE('',*,*,#26620,.F.);
#35439=ORIENTED_EDGE('',*,*,#26351,.F.);
#35440=ORIENTED_EDGE('',*,*,#26293,.F.);
#35441=ORIENTED_EDGE('',*,*,#26343,.F.);
#35442=ORIENTED_EDGE('',*,*,#26387,.F.);
#35443=ORIENTED_EDGE('',*,*,#26461,.F.);
#35444=ORIENTED_EDGE('',*,*,#26621,.T.);
#35445=ORIENTED_EDGE('',*,*,#26453,.F.);
#35446=ORIENTED_EDGE('',*,*,#26621,.F.);
#35447=ORIENTED_EDGE('',*,*,#26457,.F.);
#35448=ORIENTED_EDGE('',*,*,#26348,.F.);
#35449=ORIENTED_EDGE('',*,*,#26620,.T.);
#35450=ORIENTED_EDGE('',*,*,#26341,.F.);
#35451=ORIENTED_EDGE('',*,*,#26445,.F.);
#35452=ORIENTED_EDGE('',*,*,#26395,.F.);
#35453=ORIENTED_EDGE('',*,*,#26450,.F.);
#35454=ORIENTED_EDGE('',*,*,#26622,.T.);
#35455=ORIENTED_EDGE('',*,*,#26442,.F.);
#35456=ORIENTED_EDGE('',*,*,#26623,.F.);
#35457=ORIENTED_EDGE('',*,*,#26452,.F.);
#35458=ORIENTED_EDGE('',*,*,#21285,.F.);
#35459=ORIENTED_EDGE('',*,*,#26438,.F.);
#35460=ORIENTED_EDGE('',*,*,#26622,.F.);
#35461=ORIENTED_EDGE('',*,*,#26446,.F.);
#35462=ORIENTED_EDGE('',*,*,#26340,.F.);
#35463=ORIENTED_EDGE('',*,*,#26623,.T.);
#35464=ORIENTED_EDGE('',*,*,#21284,.F.);
#35465=ORIENTED_EDGE('',*,*,#26624,.F.);
#35466=ORIENTED_EDGE('',*,*,#26333,.F.);
#35467=ORIENTED_EDGE('',*,*,#26301,.F.);
#35468=ORIENTED_EDGE('',*,*,#26325,.F.);
#35469=ORIENTED_EDGE('',*,*,#26399,.F.);
#35470=ORIENTED_EDGE('',*,*,#26432,.F.);
#35471=ORIENTED_EDGE('',*,*,#26625,.T.);
#35472=ORIENTED_EDGE('',*,*,#26424,.F.);
#35473=ORIENTED_EDGE('',*,*,#26625,.F.);
#35474=ORIENTED_EDGE('',*,*,#26428,.F.);
#35475=ORIENTED_EDGE('',*,*,#26330,.F.);
#35476=ORIENTED_EDGE('',*,*,#26624,.T.);
#35477=ORIENTED_EDGE('',*,*,#26321,.F.);
#35478=ORIENTED_EDGE('',*,*,#26417,.F.);
#35479=ORIENTED_EDGE('',*,*,#26626,.F.);
#35480=ORIENTED_EDGE('',*,*,#26418,.F.);
#35481=ORIENTED_EDGE('',*,*,#26320,.F.);
#35482=ORIENTED_EDGE('',*,*,#26627,.T.);
#35483=ORIENTED_EDGE('',*,*,#26311,.F.);
#35484=ORIENTED_EDGE('',*,*,#26407,.F.);
#35485=ORIENTED_EDGE('',*,*,#26403,.F.);
#35486=ORIENTED_EDGE('',*,*,#26422,.F.);
#35487=ORIENTED_EDGE('',*,*,#26626,.T.);
#35488=ORIENTED_EDGE('',*,*,#26414,.F.);
#35489=ORIENTED_EDGE('',*,*,#26627,.F.);
#35490=ORIENTED_EDGE('',*,*,#26323,.F.);
#35491=ORIENTED_EDGE('',*,*,#26305,.F.);
#35492=ORIENTED_EDGE('',*,*,#26315,.F.);
#35493=ORIENTED_EDGE('',*,*,#26285,.F.);
#35494=ORIENTED_EDGE('',*,*,#26628,.F.);
#35495=ORIENTED_EDGE('',*,*,#21599,.F.);
#35496=ORIENTED_EDGE('',*,*,#26628,.T.);
#35497=ORIENTED_EDGE('',*,*,#26281,.F.);
#35498=ORIENTED_EDGE('',*,*,#26382,.F.);
#35499=ORIENTED_EDGE('',*,*,#21600,.F.);
#35500=ORIENTED_EDGE('',*,*,#26629,.F.);
#35501=ORIENTED_EDGE('',*,*,#26283,.F.);
#35502=ORIENTED_EDGE('',*,*,#26275,.F.);
#35503=ORIENTED_EDGE('',*,*,#26272,.F.);
#35504=ORIENTED_EDGE('',*,*,#21603,.F.);
#35505=ORIENTED_EDGE('',*,*,#26385,.F.);
#35506=ORIENTED_EDGE('',*,*,#26630,.T.);
#35507=ORIENTED_EDGE('',*,*,#26380,.F.);
#35508=ORIENTED_EDGE('',*,*,#26630,.F.);
#35509=ORIENTED_EDGE('',*,*,#26383,.F.);
#35510=ORIENTED_EDGE('',*,*,#26280,.F.);
#35511=ORIENTED_EDGE('',*,*,#26629,.T.);
#35512=ORIENTED_EDGE('',*,*,#26267,.F.);
#35513=ORIENTED_EDGE('',*,*,#26373,.F.);
#35514=ORIENTED_EDGE('',*,*,#26631,.F.);
#35515=ORIENTED_EDGE('',*,*,#26269,.F.);
#35516=ORIENTED_EDGE('',*,*,#26261,.F.);
#35517=ORIENTED_EDGE('',*,*,#26258,.F.);
#35518=ORIENTED_EDGE('',*,*,#26370,.F.);
#35519=ORIENTED_EDGE('',*,*,#26378,.F.);
#35520=ORIENTED_EDGE('',*,*,#26632,.T.);
#35521=ORIENTED_EDGE('',*,*,#26367,.F.);
#35522=ORIENTED_EDGE('',*,*,#26632,.F.);
#35523=ORIENTED_EDGE('',*,*,#26374,.F.);
#35524=ORIENTED_EDGE('',*,*,#26266,.F.);
#35525=ORIENTED_EDGE('',*,*,#26631,.T.);
#35526=ORIENTED_EDGE('',*,*,#26253,.F.);
#35527=ORIENTED_EDGE('',*,*,#26359,.F.);
#35528=ORIENTED_EDGE('',*,*,#26633,.F.);
#35529=ORIENTED_EDGE('',*,*,#26255,.F.);
#35530=ORIENTED_EDGE('',*,*,#26247,.F.);
#35531=ORIENTED_EDGE('',*,*,#26237,.F.);
#35532=ORIENTED_EDGE('',*,*,#26356,.F.);
#35533=ORIENTED_EDGE('',*,*,#26364,.F.);
#35534=ORIENTED_EDGE('',*,*,#26634,.T.);
#35535=ORIENTED_EDGE('',*,*,#26335,.F.);
#35536=ORIENTED_EDGE('',*,*,#26634,.F.);
#35537=ORIENTED_EDGE('',*,*,#26360,.F.);
#35538=ORIENTED_EDGE('',*,*,#26252,.F.);
#35539=ORIENTED_EDGE('',*,*,#26633,.T.);
#35540=ORIENTED_EDGE('',*,*,#26232,.F.);
#35541=ORIENTED_EDGE('',*,*,#26327,.F.);
#35542=ORIENTED_EDGE('',*,*,#26635,.T.);
#35543=ORIENTED_EDGE('',*,*,#26353,.F.);
#35544=ORIENTED_EDGE('',*,*,#26295,.F.);
#35545=ORIENTED_EDGE('',*,*,#26312,.F.);
#35546=ORIENTED_EDGE('',*,*,#26197,.F.);
#35547=ORIENTED_EDGE('',*,*,#26244,.F.);
#35548=ORIENTED_EDGE('',*,*,#26636,.F.);
#35549=ORIENTED_EDGE('',*,*,#26213,.F.);
#35550=ORIENTED_EDGE('',*,*,#26636,.T.);
#35551=ORIENTED_EDGE('',*,*,#26242,.F.);
#35552=ORIENTED_EDGE('',*,*,#26345,.F.);
#35553=ORIENTED_EDGE('',*,*,#26635,.F.);
#35554=ORIENTED_EDGE('',*,*,#26308,.F.);
#35555=ORIENTED_EDGE('',*,*,#26210,.F.);
#35556=ORIENTED_EDGE('',*,*,#26291,.F.);
#35557=ORIENTED_EDGE('',*,*,#26350,.F.);
#35558=ORIENTED_EDGE('',*,*,#26637,.T.);
#35559=ORIENTED_EDGE('',*,*,#26342,.F.);
#35560=ORIENTED_EDGE('',*,*,#26638,.F.);
#35561=ORIENTED_EDGE('',*,*,#26352,.F.);
#35562=ORIENTED_EDGE('',*,*,#21289,.F.);
#35563=ORIENTED_EDGE('',*,*,#26338,.F.);
#35564=ORIENTED_EDGE('',*,*,#26637,.F.);
#35565=ORIENTED_EDGE('',*,*,#26346,.F.);
#35566=ORIENTED_EDGE('',*,*,#26241,.F.);
#35567=ORIENTED_EDGE('',*,*,#26638,.T.);
#35568=ORIENTED_EDGE('',*,*,#21288,.F.);
#35569=ORIENTED_EDGE('',*,*,#26639,.F.);
#35570=ORIENTED_EDGE('',*,*,#26234,.F.);
#35571=ORIENTED_EDGE('',*,*,#26201,.F.);
#35572=ORIENTED_EDGE('',*,*,#26226,.F.);
#35573=ORIENTED_EDGE('',*,*,#26299,.F.);
#35574=ORIENTED_EDGE('',*,*,#26332,.F.);
#35575=ORIENTED_EDGE('',*,*,#26640,.T.);
#35576=ORIENTED_EDGE('',*,*,#26324,.F.);
#35577=ORIENTED_EDGE('',*,*,#26640,.F.);
#35578=ORIENTED_EDGE('',*,*,#26328,.F.);
#35579=ORIENTED_EDGE('',*,*,#26231,.F.);
#35580=ORIENTED_EDGE('',*,*,#26639,.T.);
#35581=ORIENTED_EDGE('',*,*,#26222,.F.);
#35582=ORIENTED_EDGE('',*,*,#26317,.F.);
#35583=ORIENTED_EDGE('',*,*,#26641,.F.);
#35584=ORIENTED_EDGE('',*,*,#26318,.F.);
#35585=ORIENTED_EDGE('',*,*,#26221,.F.);
#35586=ORIENTED_EDGE('',*,*,#26642,.T.);
#35587=ORIENTED_EDGE('',*,*,#26211,.F.);
#35588=ORIENTED_EDGE('',*,*,#26307,.F.);
#35589=ORIENTED_EDGE('',*,*,#26303,.F.);
#35590=ORIENTED_EDGE('',*,*,#26322,.F.);
#35591=ORIENTED_EDGE('',*,*,#26641,.T.);
#35592=ORIENTED_EDGE('',*,*,#26314,.F.);
#35593=ORIENTED_EDGE('',*,*,#26642,.F.);
#35594=ORIENTED_EDGE('',*,*,#26224,.F.);
#35595=ORIENTED_EDGE('',*,*,#26205,.F.);
#35596=ORIENTED_EDGE('',*,*,#26216,.F.);
#35597=ORIENTED_EDGE('',*,*,#26189,.F.);
#35598=ORIENTED_EDGE('',*,*,#26643,.F.);
#35599=ORIENTED_EDGE('',*,*,#21593,.F.);
#35600=ORIENTED_EDGE('',*,*,#26643,.T.);
#35601=ORIENTED_EDGE('',*,*,#26185,.F.);
#35602=ORIENTED_EDGE('',*,*,#26286,.F.);
#35603=ORIENTED_EDGE('',*,*,#21594,.F.);
#35604=ORIENTED_EDGE('',*,*,#26644,.F.);
#35605=ORIENTED_EDGE('',*,*,#26187,.F.);
#35606=ORIENTED_EDGE('',*,*,#26179,.F.);
#35607=ORIENTED_EDGE('',*,*,#26176,.F.);
#35608=ORIENTED_EDGE('',*,*,#21597,.F.);
#35609=ORIENTED_EDGE('',*,*,#26289,.F.);
#35610=ORIENTED_EDGE('',*,*,#26645,.T.);
#35611=ORIENTED_EDGE('',*,*,#26284,.F.);
#35612=ORIENTED_EDGE('',*,*,#26645,.F.);
#35613=ORIENTED_EDGE('',*,*,#26287,.F.);
#35614=ORIENTED_EDGE('',*,*,#26184,.F.);
#35615=ORIENTED_EDGE('',*,*,#26644,.T.);
#35616=ORIENTED_EDGE('',*,*,#26171,.F.);
#35617=ORIENTED_EDGE('',*,*,#26277,.F.);
#35618=ORIENTED_EDGE('',*,*,#26646,.F.);
#35619=ORIENTED_EDGE('',*,*,#26173,.F.);
#35620=ORIENTED_EDGE('',*,*,#26165,.F.);
#35621=ORIENTED_EDGE('',*,*,#26162,.F.);
#35622=ORIENTED_EDGE('',*,*,#26274,.F.);
#35623=ORIENTED_EDGE('',*,*,#26282,.F.);
#35624=ORIENTED_EDGE('',*,*,#26647,.T.);
#35625=ORIENTED_EDGE('',*,*,#26271,.F.);
#35626=ORIENTED_EDGE('',*,*,#26647,.F.);
#35627=ORIENTED_EDGE('',*,*,#26278,.F.);
#35628=ORIENTED_EDGE('',*,*,#26170,.F.);
#35629=ORIENTED_EDGE('',*,*,#26646,.T.);
#35630=ORIENTED_EDGE('',*,*,#26157,.F.);
#35631=ORIENTED_EDGE('',*,*,#26263,.F.);
#35632=ORIENTED_EDGE('',*,*,#26648,.F.);
#35633=ORIENTED_EDGE('',*,*,#26159,.F.);
#35634=ORIENTED_EDGE('',*,*,#26151,.F.);
#35635=ORIENTED_EDGE('',*,*,#26148,.F.);
#35636=ORIENTED_EDGE('',*,*,#26260,.F.);
#35637=ORIENTED_EDGE('',*,*,#26268,.F.);
#35638=ORIENTED_EDGE('',*,*,#26649,.T.);
#35639=ORIENTED_EDGE('',*,*,#26257,.F.);
#35640=ORIENTED_EDGE('',*,*,#26649,.F.);
#35641=ORIENTED_EDGE('',*,*,#26264,.F.);
#35642=ORIENTED_EDGE('',*,*,#26156,.F.);
#35643=ORIENTED_EDGE('',*,*,#26648,.T.);
#35644=ORIENTED_EDGE('',*,*,#26143,.F.);
#35645=ORIENTED_EDGE('',*,*,#26249,.F.);
#35646=ORIENTED_EDGE('',*,*,#26650,.F.);
#35647=ORIENTED_EDGE('',*,*,#26145,.F.);
#35648=ORIENTED_EDGE('',*,*,#26137,.F.);
#35649=ORIENTED_EDGE('',*,*,#26134,.F.);
#35650=ORIENTED_EDGE('',*,*,#26246,.F.);
#35651=ORIENTED_EDGE('',*,*,#26254,.F.);
#35652=ORIENTED_EDGE('',*,*,#26651,.T.);
#35653=ORIENTED_EDGE('',*,*,#26236,.F.);
#35654=ORIENTED_EDGE('',*,*,#26651,.F.);
#35655=ORIENTED_EDGE('',*,*,#26250,.F.);
#35656=ORIENTED_EDGE('',*,*,#26142,.F.);
#35657=ORIENTED_EDGE('',*,*,#26650,.T.);
#35658=ORIENTED_EDGE('',*,*,#26129,.F.);
#35659=ORIENTED_EDGE('',*,*,#26228,.F.);
#35660=ORIENTED_EDGE('',*,*,#26652,.T.);
#35661=ORIENTED_EDGE('',*,*,#26243,.F.);
#35662=ORIENTED_EDGE('',*,*,#26195,.F.);
#35663=ORIENTED_EDGE('',*,*,#26212,.F.);
#35664=ORIENTED_EDGE('',*,*,#26653,.T.);
#35665=ORIENTED_EDGE('',*,*,#21292,.F.);
#35666=ORIENTED_EDGE('',*,*,#26239,.F.);
#35667=ORIENTED_EDGE('',*,*,#26652,.F.);
#35668=ORIENTED_EDGE('',*,*,#26208,.F.);
#35669=ORIENTED_EDGE('',*,*,#26109,.F.);
#35670=ORIENTED_EDGE('',*,*,#26653,.F.);
#35671=ORIENTED_EDGE('',*,*,#26214,.F.);
#35672=ORIENTED_EDGE('',*,*,#21293,.F.);
#35673=ORIENTED_EDGE('',*,*,#26654,.F.);
#35674=ORIENTED_EDGE('',*,*,#26131,.F.);
#35675=ORIENTED_EDGE('',*,*,#26101,.F.);
#35676=ORIENTED_EDGE('',*,*,#26123,.F.);
#35677=ORIENTED_EDGE('',*,*,#26199,.F.);
#35678=ORIENTED_EDGE('',*,*,#26233,.F.);
#35679=ORIENTED_EDGE('',*,*,#26655,.T.);
#35680=ORIENTED_EDGE('',*,*,#26225,.F.);
#35681=ORIENTED_EDGE('',*,*,#26655,.F.);
#35682=ORIENTED_EDGE('',*,*,#26229,.F.);
#35683=ORIENTED_EDGE('',*,*,#26128,.F.);
#35684=ORIENTED_EDGE('',*,*,#26654,.T.);
#35685=ORIENTED_EDGE('',*,*,#26118,.F.);
#35686=ORIENTED_EDGE('',*,*,#26218,.F.);
#35687=ORIENTED_EDGE('',*,*,#26656,.F.);
#35688=ORIENTED_EDGE('',*,*,#26219,.F.);
#35689=ORIENTED_EDGE('',*,*,#26117,.F.);
#35690=ORIENTED_EDGE('',*,*,#26657,.T.);
#35691=ORIENTED_EDGE('',*,*,#26110,.F.);
#35692=ORIENTED_EDGE('',*,*,#26207,.F.);
#35693=ORIENTED_EDGE('',*,*,#26203,.F.);
#35694=ORIENTED_EDGE('',*,*,#26223,.F.);
#35695=ORIENTED_EDGE('',*,*,#26656,.T.);
#35696=ORIENTED_EDGE('',*,*,#26215,.F.);
#35697=ORIENTED_EDGE('',*,*,#26657,.F.);
#35698=ORIENTED_EDGE('',*,*,#26120,.F.);
#35699=ORIENTED_EDGE('',*,*,#26105,.F.);
#35700=ORIENTED_EDGE('',*,*,#26112,.F.);
#35701=ORIENTED_EDGE('',*,*,#26093,.F.);
#35702=ORIENTED_EDGE('',*,*,#26658,.F.);
#35703=ORIENTED_EDGE('',*,*,#21587,.F.);
#35704=ORIENTED_EDGE('',*,*,#26658,.T.);
#35705=ORIENTED_EDGE('',*,*,#26089,.F.);
#35706=ORIENTED_EDGE('',*,*,#26190,.F.);
#35707=ORIENTED_EDGE('',*,*,#21588,.F.);
#35708=ORIENTED_EDGE('',*,*,#26659,.F.);
#35709=ORIENTED_EDGE('',*,*,#26091,.F.);
#35710=ORIENTED_EDGE('',*,*,#26083,.F.);
#35711=ORIENTED_EDGE('',*,*,#26080,.F.);
#35712=ORIENTED_EDGE('',*,*,#21591,.F.);
#35713=ORIENTED_EDGE('',*,*,#26193,.F.);
#35714=ORIENTED_EDGE('',*,*,#26660,.T.);
#35715=ORIENTED_EDGE('',*,*,#26188,.F.);
#35716=ORIENTED_EDGE('',*,*,#26660,.F.);
#35717=ORIENTED_EDGE('',*,*,#26191,.F.);
#35718=ORIENTED_EDGE('',*,*,#26088,.F.);
#35719=ORIENTED_EDGE('',*,*,#26659,.T.);
#35720=ORIENTED_EDGE('',*,*,#26075,.F.);
#35721=ORIENTED_EDGE('',*,*,#26181,.F.);
#35722=ORIENTED_EDGE('',*,*,#26661,.F.);
#35723=ORIENTED_EDGE('',*,*,#26077,.F.);
#35724=ORIENTED_EDGE('',*,*,#26069,.F.);
#35725=ORIENTED_EDGE('',*,*,#26066,.F.);
#35726=ORIENTED_EDGE('',*,*,#26178,.F.);
#35727=ORIENTED_EDGE('',*,*,#26186,.F.);
#35728=ORIENTED_EDGE('',*,*,#26662,.T.);
#35729=ORIENTED_EDGE('',*,*,#26175,.F.);
#35730=ORIENTED_EDGE('',*,*,#26662,.F.);
#35731=ORIENTED_EDGE('',*,*,#26182,.F.);
#35732=ORIENTED_EDGE('',*,*,#26074,.F.);
#35733=ORIENTED_EDGE('',*,*,#26661,.T.);
#35734=ORIENTED_EDGE('',*,*,#26061,.F.);
#35735=ORIENTED_EDGE('',*,*,#26167,.F.);
#35736=ORIENTED_EDGE('',*,*,#26663,.F.);
#35737=ORIENTED_EDGE('',*,*,#26063,.F.);
#35738=ORIENTED_EDGE('',*,*,#26055,.F.);
#35739=ORIENTED_EDGE('',*,*,#26052,.F.);
#35740=ORIENTED_EDGE('',*,*,#26164,.F.);
#35741=ORIENTED_EDGE('',*,*,#26172,.F.);
#35742=ORIENTED_EDGE('',*,*,#26664,.T.);
#35743=ORIENTED_EDGE('',*,*,#26161,.F.);
#35744=ORIENTED_EDGE('',*,*,#26664,.F.);
#35745=ORIENTED_EDGE('',*,*,#26168,.F.);
#35746=ORIENTED_EDGE('',*,*,#26060,.F.);
#35747=ORIENTED_EDGE('',*,*,#26663,.T.);
#35748=ORIENTED_EDGE('',*,*,#26047,.F.);
#35749=ORIENTED_EDGE('',*,*,#26153,.F.);
#35750=ORIENTED_EDGE('',*,*,#26665,.F.);
#35751=ORIENTED_EDGE('',*,*,#26049,.F.);
#35752=ORIENTED_EDGE('',*,*,#26041,.F.);
#35753=ORIENTED_EDGE('',*,*,#26038,.F.);
#35754=ORIENTED_EDGE('',*,*,#26150,.F.);
#35755=ORIENTED_EDGE('',*,*,#26158,.F.);
#35756=ORIENTED_EDGE('',*,*,#26666,.T.);
#35757=ORIENTED_EDGE('',*,*,#26147,.F.);
#35758=ORIENTED_EDGE('',*,*,#26666,.F.);
#35759=ORIENTED_EDGE('',*,*,#26154,.F.);
#35760=ORIENTED_EDGE('',*,*,#26046,.F.);
#35761=ORIENTED_EDGE('',*,*,#26665,.T.);
#35762=ORIENTED_EDGE('',*,*,#26033,.F.);
#35763=ORIENTED_EDGE('',*,*,#26139,.F.);
#35764=ORIENTED_EDGE('',*,*,#26667,.F.);
#35765=ORIENTED_EDGE('',*,*,#26035,.F.);
#35766=ORIENTED_EDGE('',*,*,#26027,.F.);
#35767=ORIENTED_EDGE('',*,*,#26024,.F.);
#35768=ORIENTED_EDGE('',*,*,#26136,.F.);
#35769=ORIENTED_EDGE('',*,*,#26144,.F.);
#35770=ORIENTED_EDGE('',*,*,#26668,.T.);
#35771=ORIENTED_EDGE('',*,*,#26133,.F.);
#35772=ORIENTED_EDGE('',*,*,#26668,.F.);
#35773=ORIENTED_EDGE('',*,*,#26140,.F.);
#35774=ORIENTED_EDGE('',*,*,#26032,.F.);
#35775=ORIENTED_EDGE('',*,*,#26667,.T.);
#35776=ORIENTED_EDGE('',*,*,#26018,.F.);
#35777=ORIENTED_EDGE('',*,*,#26125,.F.);
#35778=ORIENTED_EDGE('',*,*,#26669,.F.);
#35779=ORIENTED_EDGE('',*,*,#26020,.F.);
#35780=ORIENTED_EDGE('',*,*,#26005,.F.);
#35781=ORIENTED_EDGE('',*,*,#26012,.F.);
#35782=ORIENTED_EDGE('',*,*,#26099,.F.);
#35783=ORIENTED_EDGE('',*,*,#26130,.F.);
#35784=ORIENTED_EDGE('',*,*,#26670,.T.);
#35785=ORIENTED_EDGE('',*,*,#26122,.F.);
#35786=ORIENTED_EDGE('',*,*,#26670,.F.);
#35787=ORIENTED_EDGE('',*,*,#26126,.F.);
#35788=ORIENTED_EDGE('',*,*,#26017,.F.);
#35789=ORIENTED_EDGE('',*,*,#26669,.T.);
#35790=ORIENTED_EDGE('',*,*,#26010,.F.);
#35791=ORIENTED_EDGE('',*,*,#26114,.F.);
#35792=ORIENTED_EDGE('',*,*,#26107,.F.);
#35793=ORIENTED_EDGE('',*,*,#26671,.F.);
#35794=ORIENTED_EDGE('',*,*,#26115,.F.);
#35795=ORIENTED_EDGE('',*,*,#26009,.F.);
#35796=ORIENTED_EDGE('',*,*,#26672,.T.);
#35797=ORIENTED_EDGE('',*,*,#21296,.F.);
#35798=ORIENTED_EDGE('',*,*,#26103,.F.);
#35799=ORIENTED_EDGE('',*,*,#26119,.F.);
#35800=ORIENTED_EDGE('',*,*,#26671,.T.);
#35801=ORIENTED_EDGE('',*,*,#26111,.F.);
#35802=ORIENTED_EDGE('',*,*,#26672,.F.);
#35803=ORIENTED_EDGE('',*,*,#26121,.F.);
#35804=ORIENTED_EDGE('',*,*,#21297,.F.);
#35805=ORIENTED_EDGE('',*,*,#25997,.F.);
#35806=ORIENTED_EDGE('',*,*,#26673,.F.);
#35807=ORIENTED_EDGE('',*,*,#21581,.F.);
#35808=ORIENTED_EDGE('',*,*,#26673,.T.);
#35809=ORIENTED_EDGE('',*,*,#25993,.F.);
#35810=ORIENTED_EDGE('',*,*,#26094,.F.);
#35811=ORIENTED_EDGE('',*,*,#21582,.F.);
#35812=ORIENTED_EDGE('',*,*,#26674,.F.);
#35813=ORIENTED_EDGE('',*,*,#25995,.F.);
#35814=ORIENTED_EDGE('',*,*,#25987,.F.);
#35815=ORIENTED_EDGE('',*,*,#25984,.F.);
#35816=ORIENTED_EDGE('',*,*,#21585,.F.);
#35817=ORIENTED_EDGE('',*,*,#26097,.F.);
#35818=ORIENTED_EDGE('',*,*,#26675,.T.);
#35819=ORIENTED_EDGE('',*,*,#26092,.F.);
#35820=ORIENTED_EDGE('',*,*,#26675,.F.);
#35821=ORIENTED_EDGE('',*,*,#26095,.F.);
#35822=ORIENTED_EDGE('',*,*,#25992,.F.);
#35823=ORIENTED_EDGE('',*,*,#26674,.T.);
#35824=ORIENTED_EDGE('',*,*,#25979,.F.);
#35825=ORIENTED_EDGE('',*,*,#26085,.F.);
#35826=ORIENTED_EDGE('',*,*,#26676,.F.);
#35827=ORIENTED_EDGE('',*,*,#25981,.F.);
#35828=ORIENTED_EDGE('',*,*,#25973,.F.);
#35829=ORIENTED_EDGE('',*,*,#25970,.F.);
#35830=ORIENTED_EDGE('',*,*,#26082,.F.);
#35831=ORIENTED_EDGE('',*,*,#26090,.F.);
#35832=ORIENTED_EDGE('',*,*,#26677,.T.);
#35833=ORIENTED_EDGE('',*,*,#26079,.F.);
#35834=ORIENTED_EDGE('',*,*,#26677,.F.);
#35835=ORIENTED_EDGE('',*,*,#26086,.F.);
#35836=ORIENTED_EDGE('',*,*,#25978,.F.);
#35837=ORIENTED_EDGE('',*,*,#26676,.T.);
#35838=ORIENTED_EDGE('',*,*,#25965,.F.);
#35839=ORIENTED_EDGE('',*,*,#26071,.F.);
#35840=ORIENTED_EDGE('',*,*,#26678,.F.);
#35841=ORIENTED_EDGE('',*,*,#25967,.F.);
#35842=ORIENTED_EDGE('',*,*,#25959,.F.);
#35843=ORIENTED_EDGE('',*,*,#25956,.F.);
#35844=ORIENTED_EDGE('',*,*,#26068,.F.);
#35845=ORIENTED_EDGE('',*,*,#26076,.F.);
#35846=ORIENTED_EDGE('',*,*,#26679,.T.);
#35847=ORIENTED_EDGE('',*,*,#26065,.F.);
#35848=ORIENTED_EDGE('',*,*,#26679,.F.);
#35849=ORIENTED_EDGE('',*,*,#26072,.F.);
#35850=ORIENTED_EDGE('',*,*,#25964,.F.);
#35851=ORIENTED_EDGE('',*,*,#26678,.T.);
#35852=ORIENTED_EDGE('',*,*,#25951,.F.);
#35853=ORIENTED_EDGE('',*,*,#26057,.F.);
#35854=ORIENTED_EDGE('',*,*,#26680,.F.);
#35855=ORIENTED_EDGE('',*,*,#25953,.F.);
#35856=ORIENTED_EDGE('',*,*,#25945,.F.);
#35857=ORIENTED_EDGE('',*,*,#25942,.F.);
#35858=ORIENTED_EDGE('',*,*,#26054,.F.);
#35859=ORIENTED_EDGE('',*,*,#26062,.F.);
#35860=ORIENTED_EDGE('',*,*,#26681,.T.);
#35861=ORIENTED_EDGE('',*,*,#26051,.F.);
#35862=ORIENTED_EDGE('',*,*,#26681,.F.);
#35863=ORIENTED_EDGE('',*,*,#26058,.F.);
#35864=ORIENTED_EDGE('',*,*,#25950,.F.);
#35865=ORIENTED_EDGE('',*,*,#26680,.T.);
#35866=ORIENTED_EDGE('',*,*,#25937,.F.);
#35867=ORIENTED_EDGE('',*,*,#26043,.F.);
#35868=ORIENTED_EDGE('',*,*,#26682,.F.);
#35869=ORIENTED_EDGE('',*,*,#25939,.F.);
#35870=ORIENTED_EDGE('',*,*,#25931,.F.);
#35871=ORIENTED_EDGE('',*,*,#25928,.F.);
#35872=ORIENTED_EDGE('',*,*,#26040,.F.);
#35873=ORIENTED_EDGE('',*,*,#26048,.F.);
#35874=ORIENTED_EDGE('',*,*,#26683,.T.);
#35875=ORIENTED_EDGE('',*,*,#26037,.F.);
#35876=ORIENTED_EDGE('',*,*,#26683,.F.);
#35877=ORIENTED_EDGE('',*,*,#26044,.F.);
#35878=ORIENTED_EDGE('',*,*,#25936,.F.);
#35879=ORIENTED_EDGE('',*,*,#26682,.T.);
#35880=ORIENTED_EDGE('',*,*,#25922,.F.);
#35881=ORIENTED_EDGE('',*,*,#26029,.F.);
#35882=ORIENTED_EDGE('',*,*,#26684,.F.);
#35883=ORIENTED_EDGE('',*,*,#25924,.F.);
#35884=ORIENTED_EDGE('',*,*,#25916,.F.);
#35885=ORIENTED_EDGE('',*,*,#25913,.F.);
#35886=ORIENTED_EDGE('',*,*,#26026,.F.);
#35887=ORIENTED_EDGE('',*,*,#26034,.F.);
#35888=ORIENTED_EDGE('',*,*,#26685,.T.);
#35889=ORIENTED_EDGE('',*,*,#26023,.F.);
#35890=ORIENTED_EDGE('',*,*,#26685,.F.);
#35891=ORIENTED_EDGE('',*,*,#26030,.F.);
#35892=ORIENTED_EDGE('',*,*,#25921,.F.);
#35893=ORIENTED_EDGE('',*,*,#26684,.T.);
#35894=ORIENTED_EDGE('',*,*,#25910,.F.);
#35895=ORIENTED_EDGE('',*,*,#26014,.F.);
#35896=ORIENTED_EDGE('',*,*,#26007,.F.);
#35897=ORIENTED_EDGE('',*,*,#26686,.F.);
#35898=ORIENTED_EDGE('',*,*,#26015,.F.);
#35899=ORIENTED_EDGE('',*,*,#25909,.F.);
#35900=ORIENTED_EDGE('',*,*,#26687,.T.);
#35901=ORIENTED_EDGE('',*,*,#21300,.F.);
#35902=ORIENTED_EDGE('',*,*,#26003,.F.);
#35903=ORIENTED_EDGE('',*,*,#26019,.F.);
#35904=ORIENTED_EDGE('',*,*,#26686,.T.);
#35905=ORIENTED_EDGE('',*,*,#26011,.F.);
#35906=ORIENTED_EDGE('',*,*,#26687,.F.);
#35907=ORIENTED_EDGE('',*,*,#26021,.F.);
#35908=ORIENTED_EDGE('',*,*,#21301,.F.);
#35909=ORIENTED_EDGE('',*,*,#25901,.F.);
#35910=ORIENTED_EDGE('',*,*,#26688,.F.);
#35911=ORIENTED_EDGE('',*,*,#21575,.F.);
#35912=ORIENTED_EDGE('',*,*,#26688,.T.);
#35913=ORIENTED_EDGE('',*,*,#25897,.F.);
#35914=ORIENTED_EDGE('',*,*,#25998,.F.);
#35915=ORIENTED_EDGE('',*,*,#21576,.F.);
#35916=ORIENTED_EDGE('',*,*,#26689,.F.);
#35917=ORIENTED_EDGE('',*,*,#25899,.F.);
#35918=ORIENTED_EDGE('',*,*,#25891,.F.);
#35919=ORIENTED_EDGE('',*,*,#25888,.F.);
#35920=ORIENTED_EDGE('',*,*,#21579,.F.);
#35921=ORIENTED_EDGE('',*,*,#26001,.F.);
#35922=ORIENTED_EDGE('',*,*,#26690,.T.);
#35923=ORIENTED_EDGE('',*,*,#25996,.F.);
#35924=ORIENTED_EDGE('',*,*,#26690,.F.);
#35925=ORIENTED_EDGE('',*,*,#25999,.F.);
#35926=ORIENTED_EDGE('',*,*,#25896,.F.);
#35927=ORIENTED_EDGE('',*,*,#26689,.T.);
#35928=ORIENTED_EDGE('',*,*,#25883,.F.);
#35929=ORIENTED_EDGE('',*,*,#25989,.F.);
#35930=ORIENTED_EDGE('',*,*,#26691,.F.);
#35931=ORIENTED_EDGE('',*,*,#25885,.F.);
#35932=ORIENTED_EDGE('',*,*,#25877,.F.);
#35933=ORIENTED_EDGE('',*,*,#25874,.F.);
#35934=ORIENTED_EDGE('',*,*,#25986,.F.);
#35935=ORIENTED_EDGE('',*,*,#25994,.F.);
#35936=ORIENTED_EDGE('',*,*,#26692,.T.);
#35937=ORIENTED_EDGE('',*,*,#25983,.F.);
#35938=ORIENTED_EDGE('',*,*,#26692,.F.);
#35939=ORIENTED_EDGE('',*,*,#25990,.F.);
#35940=ORIENTED_EDGE('',*,*,#25882,.F.);
#35941=ORIENTED_EDGE('',*,*,#26691,.T.);
#35942=ORIENTED_EDGE('',*,*,#25869,.F.);
#35943=ORIENTED_EDGE('',*,*,#25975,.F.);
#35944=ORIENTED_EDGE('',*,*,#26693,.F.);
#35945=ORIENTED_EDGE('',*,*,#25871,.F.);
#35946=ORIENTED_EDGE('',*,*,#25863,.F.);
#35947=ORIENTED_EDGE('',*,*,#25860,.F.);
#35948=ORIENTED_EDGE('',*,*,#25972,.F.);
#35949=ORIENTED_EDGE('',*,*,#25980,.F.);
#35950=ORIENTED_EDGE('',*,*,#26694,.T.);
#35951=ORIENTED_EDGE('',*,*,#25969,.F.);
#35952=ORIENTED_EDGE('',*,*,#26694,.F.);
#35953=ORIENTED_EDGE('',*,*,#25976,.F.);
#35954=ORIENTED_EDGE('',*,*,#25868,.F.);
#35955=ORIENTED_EDGE('',*,*,#26693,.T.);
#35956=ORIENTED_EDGE('',*,*,#25855,.F.);
#35957=ORIENTED_EDGE('',*,*,#25961,.F.);
#35958=ORIENTED_EDGE('',*,*,#26695,.F.);
#35959=ORIENTED_EDGE('',*,*,#25857,.F.);
#35960=ORIENTED_EDGE('',*,*,#25849,.F.);
#35961=ORIENTED_EDGE('',*,*,#25846,.F.);
#35962=ORIENTED_EDGE('',*,*,#25958,.F.);
#35963=ORIENTED_EDGE('',*,*,#25966,.F.);
#35964=ORIENTED_EDGE('',*,*,#26696,.T.);
#35965=ORIENTED_EDGE('',*,*,#25955,.F.);
#35966=ORIENTED_EDGE('',*,*,#26696,.F.);
#35967=ORIENTED_EDGE('',*,*,#25962,.F.);
#35968=ORIENTED_EDGE('',*,*,#25854,.F.);
#35969=ORIENTED_EDGE('',*,*,#26695,.T.);
#35970=ORIENTED_EDGE('',*,*,#25841,.F.);
#35971=ORIENTED_EDGE('',*,*,#25947,.F.);
#35972=ORIENTED_EDGE('',*,*,#26697,.F.);
#35973=ORIENTED_EDGE('',*,*,#25843,.F.);
#35974=ORIENTED_EDGE('',*,*,#25835,.F.);
#35975=ORIENTED_EDGE('',*,*,#25832,.F.);
#35976=ORIENTED_EDGE('',*,*,#25944,.F.);
#35977=ORIENTED_EDGE('',*,*,#25952,.F.);
#35978=ORIENTED_EDGE('',*,*,#26698,.T.);
#35979=ORIENTED_EDGE('',*,*,#25941,.F.);
#35980=ORIENTED_EDGE('',*,*,#26698,.F.);
#35981=ORIENTED_EDGE('',*,*,#25948,.F.);
#35982=ORIENTED_EDGE('',*,*,#25840,.F.);
#35983=ORIENTED_EDGE('',*,*,#26697,.T.);
#35984=ORIENTED_EDGE('',*,*,#25826,.F.);
#35985=ORIENTED_EDGE('',*,*,#25933,.F.);
#35986=ORIENTED_EDGE('',*,*,#26699,.F.);
#35987=ORIENTED_EDGE('',*,*,#25828,.F.);
#35988=ORIENTED_EDGE('',*,*,#25820,.F.);
#35989=ORIENTED_EDGE('',*,*,#25817,.F.);
#35990=ORIENTED_EDGE('',*,*,#25930,.F.);
#35991=ORIENTED_EDGE('',*,*,#25938,.F.);
#35992=ORIENTED_EDGE('',*,*,#26700,.T.);
#35993=ORIENTED_EDGE('',*,*,#25927,.F.);
#35994=ORIENTED_EDGE('',*,*,#26700,.F.);
#35995=ORIENTED_EDGE('',*,*,#25934,.F.);
#35996=ORIENTED_EDGE('',*,*,#25825,.F.);
#35997=ORIENTED_EDGE('',*,*,#26699,.T.);
#35998=ORIENTED_EDGE('',*,*,#25814,.F.);
#35999=ORIENTED_EDGE('',*,*,#25918,.F.);
#36000=ORIENTED_EDGE('',*,*,#25907,.F.);
#36001=ORIENTED_EDGE('',*,*,#26701,.F.);
#36002=ORIENTED_EDGE('',*,*,#25919,.F.);
#36003=ORIENTED_EDGE('',*,*,#25813,.F.);
#36004=ORIENTED_EDGE('',*,*,#26702,.T.);
#36005=ORIENTED_EDGE('',*,*,#21304,.F.);
#36006=ORIENTED_EDGE('',*,*,#25915,.F.);
#36007=ORIENTED_EDGE('',*,*,#25923,.F.);
#36008=ORIENTED_EDGE('',*,*,#26701,.T.);
#36009=ORIENTED_EDGE('',*,*,#25912,.F.);
#36010=ORIENTED_EDGE('',*,*,#26702,.F.);
#36011=ORIENTED_EDGE('',*,*,#25925,.F.);
#36012=ORIENTED_EDGE('',*,*,#21305,.F.);
#36013=ORIENTED_EDGE('',*,*,#25805,.F.);
#36014=ORIENTED_EDGE('',*,*,#26703,.F.);
#36015=ORIENTED_EDGE('',*,*,#21569,.F.);
#36016=ORIENTED_EDGE('',*,*,#26703,.T.);
#36017=ORIENTED_EDGE('',*,*,#25801,.F.);
#36018=ORIENTED_EDGE('',*,*,#25902,.F.);
#36019=ORIENTED_EDGE('',*,*,#21570,.F.);
#36020=ORIENTED_EDGE('',*,*,#26704,.F.);
#36021=ORIENTED_EDGE('',*,*,#25803,.F.);
#36022=ORIENTED_EDGE('',*,*,#25795,.F.);
#36023=ORIENTED_EDGE('',*,*,#25792,.F.);
#36024=ORIENTED_EDGE('',*,*,#21573,.F.);
#36025=ORIENTED_EDGE('',*,*,#25905,.F.);
#36026=ORIENTED_EDGE('',*,*,#26705,.T.);
#36027=ORIENTED_EDGE('',*,*,#25900,.F.);
#36028=ORIENTED_EDGE('',*,*,#26705,.F.);
#36029=ORIENTED_EDGE('',*,*,#25903,.F.);
#36030=ORIENTED_EDGE('',*,*,#25800,.F.);
#36031=ORIENTED_EDGE('',*,*,#26704,.T.);
#36032=ORIENTED_EDGE('',*,*,#25787,.F.);
#36033=ORIENTED_EDGE('',*,*,#25893,.F.);
#36034=ORIENTED_EDGE('',*,*,#26706,.F.);
#36035=ORIENTED_EDGE('',*,*,#25789,.F.);
#36036=ORIENTED_EDGE('',*,*,#25781,.F.);
#36037=ORIENTED_EDGE('',*,*,#25778,.F.);
#36038=ORIENTED_EDGE('',*,*,#25890,.F.);
#36039=ORIENTED_EDGE('',*,*,#25898,.F.);
#36040=ORIENTED_EDGE('',*,*,#26707,.T.);
#36041=ORIENTED_EDGE('',*,*,#25887,.F.);
#36042=ORIENTED_EDGE('',*,*,#26707,.F.);
#36043=ORIENTED_EDGE('',*,*,#25894,.F.);
#36044=ORIENTED_EDGE('',*,*,#25786,.F.);
#36045=ORIENTED_EDGE('',*,*,#26706,.T.);
#36046=ORIENTED_EDGE('',*,*,#25773,.F.);
#36047=ORIENTED_EDGE('',*,*,#25879,.F.);
#36048=ORIENTED_EDGE('',*,*,#26708,.F.);
#36049=ORIENTED_EDGE('',*,*,#25775,.F.);
#36050=ORIENTED_EDGE('',*,*,#25767,.F.);
#36051=ORIENTED_EDGE('',*,*,#25764,.F.);
#36052=ORIENTED_EDGE('',*,*,#25876,.F.);
#36053=ORIENTED_EDGE('',*,*,#25884,.F.);
#36054=ORIENTED_EDGE('',*,*,#26709,.T.);
#36055=ORIENTED_EDGE('',*,*,#25873,.F.);
#36056=ORIENTED_EDGE('',*,*,#26709,.F.);
#36057=ORIENTED_EDGE('',*,*,#25880,.F.);
#36058=ORIENTED_EDGE('',*,*,#25772,.F.);
#36059=ORIENTED_EDGE('',*,*,#26708,.T.);
#36060=ORIENTED_EDGE('',*,*,#25759,.F.);
#36061=ORIENTED_EDGE('',*,*,#25865,.F.);
#36062=ORIENTED_EDGE('',*,*,#26710,.F.);
#36063=ORIENTED_EDGE('',*,*,#25761,.F.);
#36064=ORIENTED_EDGE('',*,*,#25753,.F.);
#36065=ORIENTED_EDGE('',*,*,#25750,.F.);
#36066=ORIENTED_EDGE('',*,*,#25862,.F.);
#36067=ORIENTED_EDGE('',*,*,#25870,.F.);
#36068=ORIENTED_EDGE('',*,*,#26711,.T.);
#36069=ORIENTED_EDGE('',*,*,#25859,.F.);
#36070=ORIENTED_EDGE('',*,*,#26711,.F.);
#36071=ORIENTED_EDGE('',*,*,#25866,.F.);
#36072=ORIENTED_EDGE('',*,*,#25758,.F.);
#36073=ORIENTED_EDGE('',*,*,#26710,.T.);
#36074=ORIENTED_EDGE('',*,*,#25745,.F.);
#36075=ORIENTED_EDGE('',*,*,#25851,.F.);
#36076=ORIENTED_EDGE('',*,*,#26712,.F.);
#36077=ORIENTED_EDGE('',*,*,#25747,.F.);
#36078=ORIENTED_EDGE('',*,*,#25739,.F.);
#36079=ORIENTED_EDGE('',*,*,#25736,.F.);
#36080=ORIENTED_EDGE('',*,*,#25848,.F.);
#36081=ORIENTED_EDGE('',*,*,#25856,.F.);
#36082=ORIENTED_EDGE('',*,*,#26713,.T.);
#36083=ORIENTED_EDGE('',*,*,#25845,.F.);
#36084=ORIENTED_EDGE('',*,*,#26713,.F.);
#36085=ORIENTED_EDGE('',*,*,#25852,.F.);
#36086=ORIENTED_EDGE('',*,*,#25744,.F.);
#36087=ORIENTED_EDGE('',*,*,#26712,.T.);
#36088=ORIENTED_EDGE('',*,*,#25730,.F.);
#36089=ORIENTED_EDGE('',*,*,#25837,.F.);
#36090=ORIENTED_EDGE('',*,*,#26714,.F.);
#36091=ORIENTED_EDGE('',*,*,#25732,.F.);
#36092=ORIENTED_EDGE('',*,*,#25724,.F.);
#36093=ORIENTED_EDGE('',*,*,#25721,.F.);
#36094=ORIENTED_EDGE('',*,*,#25834,.F.);
#36095=ORIENTED_EDGE('',*,*,#25842,.F.);
#36096=ORIENTED_EDGE('',*,*,#26715,.T.);
#36097=ORIENTED_EDGE('',*,*,#25831,.F.);
#36098=ORIENTED_EDGE('',*,*,#26715,.F.);
#36099=ORIENTED_EDGE('',*,*,#25838,.F.);
#36100=ORIENTED_EDGE('',*,*,#25729,.F.);
#36101=ORIENTED_EDGE('',*,*,#26714,.T.);
#36102=ORIENTED_EDGE('',*,*,#25718,.F.);
#36103=ORIENTED_EDGE('',*,*,#25822,.F.);
#36104=ORIENTED_EDGE('',*,*,#25811,.F.);
#36105=ORIENTED_EDGE('',*,*,#26716,.F.);
#36106=ORIENTED_EDGE('',*,*,#25823,.F.);
#36107=ORIENTED_EDGE('',*,*,#25717,.F.);
#36108=ORIENTED_EDGE('',*,*,#26717,.T.);
#36109=ORIENTED_EDGE('',*,*,#21308,.F.);
#36110=ORIENTED_EDGE('',*,*,#25819,.F.);
#36111=ORIENTED_EDGE('',*,*,#25827,.F.);
#36112=ORIENTED_EDGE('',*,*,#26716,.T.);
#36113=ORIENTED_EDGE('',*,*,#25816,.F.);
#36114=ORIENTED_EDGE('',*,*,#26717,.F.);
#36115=ORIENTED_EDGE('',*,*,#25829,.F.);
#36116=ORIENTED_EDGE('',*,*,#21309,.F.);
#36117=ORIENTED_EDGE('',*,*,#25709,.F.);
#36118=ORIENTED_EDGE('',*,*,#26718,.F.);
#36119=ORIENTED_EDGE('',*,*,#21563,.F.);
#36120=ORIENTED_EDGE('',*,*,#26718,.T.);
#36121=ORIENTED_EDGE('',*,*,#25705,.F.);
#36122=ORIENTED_EDGE('',*,*,#25806,.F.);
#36123=ORIENTED_EDGE('',*,*,#21564,.F.);
#36124=ORIENTED_EDGE('',*,*,#26719,.F.);
#36125=ORIENTED_EDGE('',*,*,#25707,.F.);
#36126=ORIENTED_EDGE('',*,*,#25699,.F.);
#36127=ORIENTED_EDGE('',*,*,#25696,.F.);
#36128=ORIENTED_EDGE('',*,*,#21567,.F.);
#36129=ORIENTED_EDGE('',*,*,#25809,.F.);
#36130=ORIENTED_EDGE('',*,*,#26720,.T.);
#36131=ORIENTED_EDGE('',*,*,#25804,.F.);
#36132=ORIENTED_EDGE('',*,*,#26720,.F.);
#36133=ORIENTED_EDGE('',*,*,#25807,.F.);
#36134=ORIENTED_EDGE('',*,*,#25704,.F.);
#36135=ORIENTED_EDGE('',*,*,#26719,.T.);
#36136=ORIENTED_EDGE('',*,*,#25691,.F.);
#36137=ORIENTED_EDGE('',*,*,#25797,.F.);
#36138=ORIENTED_EDGE('',*,*,#26721,.F.);
#36139=ORIENTED_EDGE('',*,*,#25693,.F.);
#36140=ORIENTED_EDGE('',*,*,#25685,.F.);
#36141=ORIENTED_EDGE('',*,*,#25682,.F.);
#36142=ORIENTED_EDGE('',*,*,#25794,.F.);
#36143=ORIENTED_EDGE('',*,*,#25802,.F.);
#36144=ORIENTED_EDGE('',*,*,#26722,.T.);
#36145=ORIENTED_EDGE('',*,*,#25791,.F.);
#36146=ORIENTED_EDGE('',*,*,#26722,.F.);
#36147=ORIENTED_EDGE('',*,*,#25798,.F.);
#36148=ORIENTED_EDGE('',*,*,#25690,.F.);
#36149=ORIENTED_EDGE('',*,*,#26721,.T.);
#36150=ORIENTED_EDGE('',*,*,#25677,.F.);
#36151=ORIENTED_EDGE('',*,*,#25783,.F.);
#36152=ORIENTED_EDGE('',*,*,#26723,.F.);
#36153=ORIENTED_EDGE('',*,*,#25679,.F.);
#36154=ORIENTED_EDGE('',*,*,#25671,.F.);
#36155=ORIENTED_EDGE('',*,*,#25668,.F.);
#36156=ORIENTED_EDGE('',*,*,#25780,.F.);
#36157=ORIENTED_EDGE('',*,*,#25788,.F.);
#36158=ORIENTED_EDGE('',*,*,#26724,.T.);
#36159=ORIENTED_EDGE('',*,*,#25777,.F.);
#36160=ORIENTED_EDGE('',*,*,#26724,.F.);
#36161=ORIENTED_EDGE('',*,*,#25784,.F.);
#36162=ORIENTED_EDGE('',*,*,#25676,.F.);
#36163=ORIENTED_EDGE('',*,*,#26723,.T.);
#36164=ORIENTED_EDGE('',*,*,#25663,.F.);
#36165=ORIENTED_EDGE('',*,*,#25769,.F.);
#36166=ORIENTED_EDGE('',*,*,#26725,.F.);
#36167=ORIENTED_EDGE('',*,*,#25665,.F.);
#36168=ORIENTED_EDGE('',*,*,#25657,.F.);
#36169=ORIENTED_EDGE('',*,*,#25654,.F.);
#36170=ORIENTED_EDGE('',*,*,#25766,.F.);
#36171=ORIENTED_EDGE('',*,*,#25774,.F.);
#36172=ORIENTED_EDGE('',*,*,#26726,.T.);
#36173=ORIENTED_EDGE('',*,*,#25763,.F.);
#36174=ORIENTED_EDGE('',*,*,#26726,.F.);
#36175=ORIENTED_EDGE('',*,*,#25770,.F.);
#36176=ORIENTED_EDGE('',*,*,#25662,.F.);
#36177=ORIENTED_EDGE('',*,*,#26725,.T.);
#36178=ORIENTED_EDGE('',*,*,#25649,.F.);
#36179=ORIENTED_EDGE('',*,*,#25755,.F.);
#36180=ORIENTED_EDGE('',*,*,#26727,.F.);
#36181=ORIENTED_EDGE('',*,*,#25651,.F.);
#36182=ORIENTED_EDGE('',*,*,#25643,.F.);
#36183=ORIENTED_EDGE('',*,*,#25640,.F.);
#36184=ORIENTED_EDGE('',*,*,#25752,.F.);
#36185=ORIENTED_EDGE('',*,*,#25760,.F.);
#36186=ORIENTED_EDGE('',*,*,#26728,.T.);
#36187=ORIENTED_EDGE('',*,*,#25749,.F.);
#36188=ORIENTED_EDGE('',*,*,#26728,.F.);
#36189=ORIENTED_EDGE('',*,*,#25756,.F.);
#36190=ORIENTED_EDGE('',*,*,#25648,.F.);
#36191=ORIENTED_EDGE('',*,*,#26727,.T.);
#36192=ORIENTED_EDGE('',*,*,#25634,.F.);
#36193=ORIENTED_EDGE('',*,*,#25741,.F.);
#36194=ORIENTED_EDGE('',*,*,#26729,.F.);
#36195=ORIENTED_EDGE('',*,*,#25636,.F.);
#36196=ORIENTED_EDGE('',*,*,#25628,.F.);
#36197=ORIENTED_EDGE('',*,*,#25625,.F.);
#36198=ORIENTED_EDGE('',*,*,#25738,.F.);
#36199=ORIENTED_EDGE('',*,*,#25746,.F.);
#36200=ORIENTED_EDGE('',*,*,#26730,.T.);
#36201=ORIENTED_EDGE('',*,*,#25735,.F.);
#36202=ORIENTED_EDGE('',*,*,#26730,.F.);
#36203=ORIENTED_EDGE('',*,*,#25742,.F.);
#36204=ORIENTED_EDGE('',*,*,#25633,.F.);
#36205=ORIENTED_EDGE('',*,*,#26729,.T.);
#36206=ORIENTED_EDGE('',*,*,#25622,.F.);
#36207=ORIENTED_EDGE('',*,*,#25726,.F.);
#36208=ORIENTED_EDGE('',*,*,#25715,.F.);
#36209=ORIENTED_EDGE('',*,*,#26731,.F.);
#36210=ORIENTED_EDGE('',*,*,#25727,.F.);
#36211=ORIENTED_EDGE('',*,*,#25621,.F.);
#36212=ORIENTED_EDGE('',*,*,#26732,.T.);
#36213=ORIENTED_EDGE('',*,*,#21312,.F.);
#36214=ORIENTED_EDGE('',*,*,#25723,.F.);
#36215=ORIENTED_EDGE('',*,*,#25731,.F.);
#36216=ORIENTED_EDGE('',*,*,#26731,.T.);
#36217=ORIENTED_EDGE('',*,*,#25720,.F.);
#36218=ORIENTED_EDGE('',*,*,#26732,.F.);
#36219=ORIENTED_EDGE('',*,*,#25733,.F.);
#36220=ORIENTED_EDGE('',*,*,#21313,.F.);
#36221=ORIENTED_EDGE('',*,*,#25613,.F.);
#36222=ORIENTED_EDGE('',*,*,#26733,.F.);
#36223=ORIENTED_EDGE('',*,*,#21557,.F.);
#36224=ORIENTED_EDGE('',*,*,#26733,.T.);
#36225=ORIENTED_EDGE('',*,*,#25609,.F.);
#36226=ORIENTED_EDGE('',*,*,#25710,.F.);
#36227=ORIENTED_EDGE('',*,*,#21558,.F.);
#36228=ORIENTED_EDGE('',*,*,#26734,.F.);
#36229=ORIENTED_EDGE('',*,*,#25611,.F.);
#36230=ORIENTED_EDGE('',*,*,#25603,.F.);
#36231=ORIENTED_EDGE('',*,*,#25600,.F.);
#36232=ORIENTED_EDGE('',*,*,#21561,.F.);
#36233=ORIENTED_EDGE('',*,*,#25713,.F.);
#36234=ORIENTED_EDGE('',*,*,#26735,.T.);
#36235=ORIENTED_EDGE('',*,*,#25708,.F.);
#36236=ORIENTED_EDGE('',*,*,#26735,.F.);
#36237=ORIENTED_EDGE('',*,*,#25711,.F.);
#36238=ORIENTED_EDGE('',*,*,#25608,.F.);
#36239=ORIENTED_EDGE('',*,*,#26734,.T.);
#36240=ORIENTED_EDGE('',*,*,#25595,.F.);
#36241=ORIENTED_EDGE('',*,*,#25701,.F.);
#36242=ORIENTED_EDGE('',*,*,#26736,.F.);
#36243=ORIENTED_EDGE('',*,*,#25597,.F.);
#36244=ORIENTED_EDGE('',*,*,#25589,.F.);
#36245=ORIENTED_EDGE('',*,*,#25586,.F.);
#36246=ORIENTED_EDGE('',*,*,#25698,.F.);
#36247=ORIENTED_EDGE('',*,*,#25706,.F.);
#36248=ORIENTED_EDGE('',*,*,#26737,.T.);
#36249=ORIENTED_EDGE('',*,*,#25695,.F.);
#36250=ORIENTED_EDGE('',*,*,#26737,.F.);
#36251=ORIENTED_EDGE('',*,*,#25702,.F.);
#36252=ORIENTED_EDGE('',*,*,#25594,.F.);
#36253=ORIENTED_EDGE('',*,*,#26736,.T.);
#36254=ORIENTED_EDGE('',*,*,#25581,.F.);
#36255=ORIENTED_EDGE('',*,*,#25687,.F.);
#36256=ORIENTED_EDGE('',*,*,#26738,.F.);
#36257=ORIENTED_EDGE('',*,*,#25583,.F.);
#36258=ORIENTED_EDGE('',*,*,#25575,.F.);
#36259=ORIENTED_EDGE('',*,*,#25572,.F.);
#36260=ORIENTED_EDGE('',*,*,#25684,.F.);
#36261=ORIENTED_EDGE('',*,*,#25692,.F.);
#36262=ORIENTED_EDGE('',*,*,#26739,.T.);
#36263=ORIENTED_EDGE('',*,*,#25681,.F.);
#36264=ORIENTED_EDGE('',*,*,#26739,.F.);
#36265=ORIENTED_EDGE('',*,*,#25688,.F.);
#36266=ORIENTED_EDGE('',*,*,#25580,.F.);
#36267=ORIENTED_EDGE('',*,*,#26738,.T.);
#36268=ORIENTED_EDGE('',*,*,#25567,.F.);
#36269=ORIENTED_EDGE('',*,*,#25673,.F.);
#36270=ORIENTED_EDGE('',*,*,#26740,.F.);
#36271=ORIENTED_EDGE('',*,*,#25569,.F.);
#36272=ORIENTED_EDGE('',*,*,#25561,.F.);
#36273=ORIENTED_EDGE('',*,*,#25558,.F.);
#36274=ORIENTED_EDGE('',*,*,#25670,.F.);
#36275=ORIENTED_EDGE('',*,*,#25678,.F.);
#36276=ORIENTED_EDGE('',*,*,#26741,.T.);
#36277=ORIENTED_EDGE('',*,*,#25667,.F.);
#36278=ORIENTED_EDGE('',*,*,#26741,.F.);
#36279=ORIENTED_EDGE('',*,*,#25674,.F.);
#36280=ORIENTED_EDGE('',*,*,#25566,.F.);
#36281=ORIENTED_EDGE('',*,*,#26740,.T.);
#36282=ORIENTED_EDGE('',*,*,#25553,.F.);
#36283=ORIENTED_EDGE('',*,*,#25659,.F.);
#36284=ORIENTED_EDGE('',*,*,#26742,.F.);
#36285=ORIENTED_EDGE('',*,*,#25555,.F.);
#36286=ORIENTED_EDGE('',*,*,#25547,.F.);
#36287=ORIENTED_EDGE('',*,*,#25544,.F.);
#36288=ORIENTED_EDGE('',*,*,#25656,.F.);
#36289=ORIENTED_EDGE('',*,*,#25664,.F.);
#36290=ORIENTED_EDGE('',*,*,#26743,.T.);
#36291=ORIENTED_EDGE('',*,*,#25653,.F.);
#36292=ORIENTED_EDGE('',*,*,#26743,.F.);
#36293=ORIENTED_EDGE('',*,*,#25660,.F.);
#36294=ORIENTED_EDGE('',*,*,#25552,.F.);
#36295=ORIENTED_EDGE('',*,*,#26742,.T.);
#36296=ORIENTED_EDGE('',*,*,#25538,.F.);
#36297=ORIENTED_EDGE('',*,*,#25645,.F.);
#36298=ORIENTED_EDGE('',*,*,#26744,.F.);
#36299=ORIENTED_EDGE('',*,*,#25540,.F.);
#36300=ORIENTED_EDGE('',*,*,#25532,.F.);
#36301=ORIENTED_EDGE('',*,*,#25529,.F.);
#36302=ORIENTED_EDGE('',*,*,#25642,.F.);
#36303=ORIENTED_EDGE('',*,*,#25650,.F.);
#36304=ORIENTED_EDGE('',*,*,#26745,.T.);
#36305=ORIENTED_EDGE('',*,*,#25639,.F.);
#36306=ORIENTED_EDGE('',*,*,#26745,.F.);
#36307=ORIENTED_EDGE('',*,*,#25646,.F.);
#36308=ORIENTED_EDGE('',*,*,#25537,.F.);
#36309=ORIENTED_EDGE('',*,*,#26744,.T.);
#36310=ORIENTED_EDGE('',*,*,#25526,.F.);
#36311=ORIENTED_EDGE('',*,*,#25630,.F.);
#36312=ORIENTED_EDGE('',*,*,#25619,.F.);
#36313=ORIENTED_EDGE('',*,*,#26746,.F.);
#36314=ORIENTED_EDGE('',*,*,#25631,.F.);
#36315=ORIENTED_EDGE('',*,*,#25525,.F.);
#36316=ORIENTED_EDGE('',*,*,#26747,.T.);
#36317=ORIENTED_EDGE('',*,*,#21316,.F.);
#36318=ORIENTED_EDGE('',*,*,#25627,.F.);
#36319=ORIENTED_EDGE('',*,*,#25635,.F.);
#36320=ORIENTED_EDGE('',*,*,#26746,.T.);
#36321=ORIENTED_EDGE('',*,*,#25624,.F.);
#36322=ORIENTED_EDGE('',*,*,#26747,.F.);
#36323=ORIENTED_EDGE('',*,*,#25637,.F.);
#36324=ORIENTED_EDGE('',*,*,#21317,.F.);
#36325=ORIENTED_EDGE('',*,*,#25517,.F.);
#36326=ORIENTED_EDGE('',*,*,#26748,.F.);
#36327=ORIENTED_EDGE('',*,*,#21551,.F.);
#36328=ORIENTED_EDGE('',*,*,#26748,.T.);
#36329=ORIENTED_EDGE('',*,*,#25513,.F.);
#36330=ORIENTED_EDGE('',*,*,#25614,.F.);
#36331=ORIENTED_EDGE('',*,*,#21552,.F.);
#36332=ORIENTED_EDGE('',*,*,#26749,.F.);
#36333=ORIENTED_EDGE('',*,*,#25515,.F.);
#36334=ORIENTED_EDGE('',*,*,#25507,.F.);
#36335=ORIENTED_EDGE('',*,*,#25504,.F.);
#36336=ORIENTED_EDGE('',*,*,#21555,.F.);
#36337=ORIENTED_EDGE('',*,*,#25617,.F.);
#36338=ORIENTED_EDGE('',*,*,#26750,.T.);
#36339=ORIENTED_EDGE('',*,*,#25612,.F.);
#36340=ORIENTED_EDGE('',*,*,#26750,.F.);
#36341=ORIENTED_EDGE('',*,*,#25615,.F.);
#36342=ORIENTED_EDGE('',*,*,#25512,.F.);
#36343=ORIENTED_EDGE('',*,*,#26749,.T.);
#36344=ORIENTED_EDGE('',*,*,#25499,.F.);
#36345=ORIENTED_EDGE('',*,*,#25605,.F.);
#36346=ORIENTED_EDGE('',*,*,#26751,.F.);
#36347=ORIENTED_EDGE('',*,*,#25501,.F.);
#36348=ORIENTED_EDGE('',*,*,#25493,.F.);
#36349=ORIENTED_EDGE('',*,*,#25490,.F.);
#36350=ORIENTED_EDGE('',*,*,#25602,.F.);
#36351=ORIENTED_EDGE('',*,*,#25610,.F.);
#36352=ORIENTED_EDGE('',*,*,#26752,.T.);
#36353=ORIENTED_EDGE('',*,*,#25599,.F.);
#36354=ORIENTED_EDGE('',*,*,#26752,.F.);
#36355=ORIENTED_EDGE('',*,*,#25606,.F.);
#36356=ORIENTED_EDGE('',*,*,#25498,.F.);
#36357=ORIENTED_EDGE('',*,*,#26751,.T.);
#36358=ORIENTED_EDGE('',*,*,#25485,.F.);
#36359=ORIENTED_EDGE('',*,*,#25591,.F.);
#36360=ORIENTED_EDGE('',*,*,#26753,.F.);
#36361=ORIENTED_EDGE('',*,*,#25487,.F.);
#36362=ORIENTED_EDGE('',*,*,#25479,.F.);
#36363=ORIENTED_EDGE('',*,*,#25476,.F.);
#36364=ORIENTED_EDGE('',*,*,#25588,.F.);
#36365=ORIENTED_EDGE('',*,*,#25596,.F.);
#36366=ORIENTED_EDGE('',*,*,#26754,.T.);
#36367=ORIENTED_EDGE('',*,*,#25585,.F.);
#36368=ORIENTED_EDGE('',*,*,#26754,.F.);
#36369=ORIENTED_EDGE('',*,*,#25592,.F.);
#36370=ORIENTED_EDGE('',*,*,#25484,.F.);
#36371=ORIENTED_EDGE('',*,*,#26753,.T.);
#36372=ORIENTED_EDGE('',*,*,#25471,.F.);
#36373=ORIENTED_EDGE('',*,*,#25577,.F.);
#36374=ORIENTED_EDGE('',*,*,#26755,.F.);
#36375=ORIENTED_EDGE('',*,*,#25473,.F.);
#36376=ORIENTED_EDGE('',*,*,#25465,.F.);
#36377=ORIENTED_EDGE('',*,*,#25462,.F.);
#36378=ORIENTED_EDGE('',*,*,#25574,.F.);
#36379=ORIENTED_EDGE('',*,*,#25582,.F.);
#36380=ORIENTED_EDGE('',*,*,#26756,.T.);
#36381=ORIENTED_EDGE('',*,*,#25571,.F.);
#36382=ORIENTED_EDGE('',*,*,#26756,.F.);
#36383=ORIENTED_EDGE('',*,*,#25578,.F.);
#36384=ORIENTED_EDGE('',*,*,#25470,.F.);
#36385=ORIENTED_EDGE('',*,*,#26755,.T.);
#36386=ORIENTED_EDGE('',*,*,#25457,.F.);
#36387=ORIENTED_EDGE('',*,*,#25563,.F.);
#36388=ORIENTED_EDGE('',*,*,#26757,.F.);
#36389=ORIENTED_EDGE('',*,*,#25459,.F.);
#36390=ORIENTED_EDGE('',*,*,#25451,.F.);
#36391=ORIENTED_EDGE('',*,*,#25448,.F.);
#36392=ORIENTED_EDGE('',*,*,#25560,.F.);
#36393=ORIENTED_EDGE('',*,*,#25568,.F.);
#36394=ORIENTED_EDGE('',*,*,#26758,.T.);
#36395=ORIENTED_EDGE('',*,*,#25557,.F.);
#36396=ORIENTED_EDGE('',*,*,#26758,.F.);
#36397=ORIENTED_EDGE('',*,*,#25564,.F.);
#36398=ORIENTED_EDGE('',*,*,#25456,.F.);
#36399=ORIENTED_EDGE('',*,*,#26757,.T.);
#36400=ORIENTED_EDGE('',*,*,#25442,.F.);
#36401=ORIENTED_EDGE('',*,*,#25549,.F.);
#36402=ORIENTED_EDGE('',*,*,#26759,.F.);
#36403=ORIENTED_EDGE('',*,*,#25444,.F.);
#36404=ORIENTED_EDGE('',*,*,#25436,.F.);
#36405=ORIENTED_EDGE('',*,*,#25433,.F.);
#36406=ORIENTED_EDGE('',*,*,#25546,.F.);
#36407=ORIENTED_EDGE('',*,*,#25554,.F.);
#36408=ORIENTED_EDGE('',*,*,#26760,.T.);
#36409=ORIENTED_EDGE('',*,*,#25543,.F.);
#36410=ORIENTED_EDGE('',*,*,#26760,.F.);
#36411=ORIENTED_EDGE('',*,*,#25550,.F.);
#36412=ORIENTED_EDGE('',*,*,#25441,.F.);
#36413=ORIENTED_EDGE('',*,*,#26759,.T.);
#36414=ORIENTED_EDGE('',*,*,#25430,.F.);
#36415=ORIENTED_EDGE('',*,*,#25534,.F.);
#36416=ORIENTED_EDGE('',*,*,#25523,.F.);
#36417=ORIENTED_EDGE('',*,*,#26761,.F.);
#36418=ORIENTED_EDGE('',*,*,#25535,.F.);
#36419=ORIENTED_EDGE('',*,*,#25429,.F.);
#36420=ORIENTED_EDGE('',*,*,#26762,.T.);
#36421=ORIENTED_EDGE('',*,*,#21320,.F.);
#36422=ORIENTED_EDGE('',*,*,#25531,.F.);
#36423=ORIENTED_EDGE('',*,*,#25539,.F.);
#36424=ORIENTED_EDGE('',*,*,#26761,.T.);
#36425=ORIENTED_EDGE('',*,*,#25528,.F.);
#36426=ORIENTED_EDGE('',*,*,#26762,.F.);
#36427=ORIENTED_EDGE('',*,*,#25541,.F.);
#36428=ORIENTED_EDGE('',*,*,#21321,.F.);
#36429=ORIENTED_EDGE('',*,*,#25421,.F.);
#36430=ORIENTED_EDGE('',*,*,#26763,.F.);
#36431=ORIENTED_EDGE('',*,*,#21545,.F.);
#36432=ORIENTED_EDGE('',*,*,#26763,.T.);
#36433=ORIENTED_EDGE('',*,*,#25417,.F.);
#36434=ORIENTED_EDGE('',*,*,#25518,.F.);
#36435=ORIENTED_EDGE('',*,*,#21546,.F.);
#36436=ORIENTED_EDGE('',*,*,#26764,.F.);
#36437=ORIENTED_EDGE('',*,*,#25419,.F.);
#36438=ORIENTED_EDGE('',*,*,#25411,.F.);
#36439=ORIENTED_EDGE('',*,*,#25408,.F.);
#36440=ORIENTED_EDGE('',*,*,#21549,.F.);
#36441=ORIENTED_EDGE('',*,*,#25521,.F.);
#36442=ORIENTED_EDGE('',*,*,#26765,.T.);
#36443=ORIENTED_EDGE('',*,*,#25516,.F.);
#36444=ORIENTED_EDGE('',*,*,#26765,.F.);
#36445=ORIENTED_EDGE('',*,*,#25519,.F.);
#36446=ORIENTED_EDGE('',*,*,#25416,.F.);
#36447=ORIENTED_EDGE('',*,*,#26764,.T.);
#36448=ORIENTED_EDGE('',*,*,#25403,.F.);
#36449=ORIENTED_EDGE('',*,*,#25509,.F.);
#36450=ORIENTED_EDGE('',*,*,#26766,.F.);
#36451=ORIENTED_EDGE('',*,*,#25405,.F.);
#36452=ORIENTED_EDGE('',*,*,#25397,.F.);
#36453=ORIENTED_EDGE('',*,*,#25394,.F.);
#36454=ORIENTED_EDGE('',*,*,#25506,.F.);
#36455=ORIENTED_EDGE('',*,*,#25514,.F.);
#36456=ORIENTED_EDGE('',*,*,#26767,.T.);
#36457=ORIENTED_EDGE('',*,*,#25503,.F.);
#36458=ORIENTED_EDGE('',*,*,#26767,.F.);
#36459=ORIENTED_EDGE('',*,*,#25510,.F.);
#36460=ORIENTED_EDGE('',*,*,#25402,.F.);
#36461=ORIENTED_EDGE('',*,*,#26766,.T.);
#36462=ORIENTED_EDGE('',*,*,#25389,.F.);
#36463=ORIENTED_EDGE('',*,*,#25495,.F.);
#36464=ORIENTED_EDGE('',*,*,#26768,.F.);
#36465=ORIENTED_EDGE('',*,*,#25391,.F.);
#36466=ORIENTED_EDGE('',*,*,#25383,.F.);
#36467=ORIENTED_EDGE('',*,*,#25380,.F.);
#36468=ORIENTED_EDGE('',*,*,#25492,.F.);
#36469=ORIENTED_EDGE('',*,*,#25500,.F.);
#36470=ORIENTED_EDGE('',*,*,#26769,.T.);
#36471=ORIENTED_EDGE('',*,*,#25489,.F.);
#36472=ORIENTED_EDGE('',*,*,#26769,.F.);
#36473=ORIENTED_EDGE('',*,*,#25496,.F.);
#36474=ORIENTED_EDGE('',*,*,#25388,.F.);
#36475=ORIENTED_EDGE('',*,*,#26768,.T.);
#36476=ORIENTED_EDGE('',*,*,#25375,.F.);
#36477=ORIENTED_EDGE('',*,*,#25481,.F.);
#36478=ORIENTED_EDGE('',*,*,#26770,.F.);
#36479=ORIENTED_EDGE('',*,*,#25377,.F.);
#36480=ORIENTED_EDGE('',*,*,#25369,.F.);
#36481=ORIENTED_EDGE('',*,*,#25366,.F.);
#36482=ORIENTED_EDGE('',*,*,#25478,.F.);
#36483=ORIENTED_EDGE('',*,*,#25486,.F.);
#36484=ORIENTED_EDGE('',*,*,#26771,.T.);
#36485=ORIENTED_EDGE('',*,*,#25475,.F.);
#36486=ORIENTED_EDGE('',*,*,#26771,.F.);
#36487=ORIENTED_EDGE('',*,*,#25482,.F.);
#36488=ORIENTED_EDGE('',*,*,#25374,.F.);
#36489=ORIENTED_EDGE('',*,*,#26770,.T.);
#36490=ORIENTED_EDGE('',*,*,#25361,.F.);
#36491=ORIENTED_EDGE('',*,*,#25467,.F.);
#36492=ORIENTED_EDGE('',*,*,#26772,.F.);
#36493=ORIENTED_EDGE('',*,*,#25363,.F.);
#36494=ORIENTED_EDGE('',*,*,#25355,.F.);
#36495=ORIENTED_EDGE('',*,*,#25352,.F.);
#36496=ORIENTED_EDGE('',*,*,#25464,.F.);
#36497=ORIENTED_EDGE('',*,*,#25472,.F.);
#36498=ORIENTED_EDGE('',*,*,#26773,.T.);
#36499=ORIENTED_EDGE('',*,*,#25461,.F.);
#36500=ORIENTED_EDGE('',*,*,#26773,.F.);
#36501=ORIENTED_EDGE('',*,*,#25468,.F.);
#36502=ORIENTED_EDGE('',*,*,#25360,.F.);
#36503=ORIENTED_EDGE('',*,*,#26772,.T.);
#36504=ORIENTED_EDGE('',*,*,#25346,.F.);
#36505=ORIENTED_EDGE('',*,*,#25453,.F.);
#36506=ORIENTED_EDGE('',*,*,#26774,.F.);
#36507=ORIENTED_EDGE('',*,*,#25348,.F.);
#36508=ORIENTED_EDGE('',*,*,#25340,.F.);
#36509=ORIENTED_EDGE('',*,*,#25337,.F.);
#36510=ORIENTED_EDGE('',*,*,#25450,.F.);
#36511=ORIENTED_EDGE('',*,*,#25458,.F.);
#36512=ORIENTED_EDGE('',*,*,#26775,.T.);
#36513=ORIENTED_EDGE('',*,*,#25447,.F.);
#36514=ORIENTED_EDGE('',*,*,#26775,.F.);
#36515=ORIENTED_EDGE('',*,*,#25454,.F.);
#36516=ORIENTED_EDGE('',*,*,#25345,.F.);
#36517=ORIENTED_EDGE('',*,*,#26774,.T.);
#36518=ORIENTED_EDGE('',*,*,#25334,.F.);
#36519=ORIENTED_EDGE('',*,*,#25438,.F.);
#36520=ORIENTED_EDGE('',*,*,#25427,.F.);
#36521=ORIENTED_EDGE('',*,*,#26776,.F.);
#36522=ORIENTED_EDGE('',*,*,#25439,.F.);
#36523=ORIENTED_EDGE('',*,*,#25333,.F.);
#36524=ORIENTED_EDGE('',*,*,#26777,.T.);
#36525=ORIENTED_EDGE('',*,*,#21324,.F.);
#36526=ORIENTED_EDGE('',*,*,#25435,.F.);
#36527=ORIENTED_EDGE('',*,*,#25443,.F.);
#36528=ORIENTED_EDGE('',*,*,#26776,.T.);
#36529=ORIENTED_EDGE('',*,*,#25432,.F.);
#36530=ORIENTED_EDGE('',*,*,#26777,.F.);
#36531=ORIENTED_EDGE('',*,*,#25445,.F.);
#36532=ORIENTED_EDGE('',*,*,#21325,.F.);
#36533=ORIENTED_EDGE('',*,*,#25325,.F.);
#36534=ORIENTED_EDGE('',*,*,#26778,.F.);
#36535=ORIENTED_EDGE('',*,*,#21539,.F.);
#36536=ORIENTED_EDGE('',*,*,#26778,.T.);
#36537=ORIENTED_EDGE('',*,*,#25321,.F.);
#36538=ORIENTED_EDGE('',*,*,#25422,.F.);
#36539=ORIENTED_EDGE('',*,*,#21540,.F.);
#36540=ORIENTED_EDGE('',*,*,#26779,.F.);
#36541=ORIENTED_EDGE('',*,*,#25323,.F.);
#36542=ORIENTED_EDGE('',*,*,#25315,.F.);
#36543=ORIENTED_EDGE('',*,*,#25312,.F.);
#36544=ORIENTED_EDGE('',*,*,#21543,.F.);
#36545=ORIENTED_EDGE('',*,*,#25425,.F.);
#36546=ORIENTED_EDGE('',*,*,#26780,.T.);
#36547=ORIENTED_EDGE('',*,*,#25420,.F.);
#36548=ORIENTED_EDGE('',*,*,#26780,.F.);
#36549=ORIENTED_EDGE('',*,*,#25423,.F.);
#36550=ORIENTED_EDGE('',*,*,#25320,.F.);
#36551=ORIENTED_EDGE('',*,*,#26779,.T.);
#36552=ORIENTED_EDGE('',*,*,#25307,.F.);
#36553=ORIENTED_EDGE('',*,*,#25413,.F.);
#36554=ORIENTED_EDGE('',*,*,#26781,.F.);
#36555=ORIENTED_EDGE('',*,*,#25309,.F.);
#36556=ORIENTED_EDGE('',*,*,#25301,.F.);
#36557=ORIENTED_EDGE('',*,*,#25298,.F.);
#36558=ORIENTED_EDGE('',*,*,#25410,.F.);
#36559=ORIENTED_EDGE('',*,*,#25418,.F.);
#36560=ORIENTED_EDGE('',*,*,#26782,.T.);
#36561=ORIENTED_EDGE('',*,*,#25407,.F.);
#36562=ORIENTED_EDGE('',*,*,#26782,.F.);
#36563=ORIENTED_EDGE('',*,*,#25414,.F.);
#36564=ORIENTED_EDGE('',*,*,#25306,.F.);
#36565=ORIENTED_EDGE('',*,*,#26781,.T.);
#36566=ORIENTED_EDGE('',*,*,#25293,.F.);
#36567=ORIENTED_EDGE('',*,*,#25399,.F.);
#36568=ORIENTED_EDGE('',*,*,#26783,.F.);
#36569=ORIENTED_EDGE('',*,*,#25295,.F.);
#36570=ORIENTED_EDGE('',*,*,#25287,.F.);
#36571=ORIENTED_EDGE('',*,*,#25284,.F.);
#36572=ORIENTED_EDGE('',*,*,#25396,.F.);
#36573=ORIENTED_EDGE('',*,*,#25404,.F.);
#36574=ORIENTED_EDGE('',*,*,#26784,.T.);
#36575=ORIENTED_EDGE('',*,*,#25393,.F.);
#36576=ORIENTED_EDGE('',*,*,#26784,.F.);
#36577=ORIENTED_EDGE('',*,*,#25400,.F.);
#36578=ORIENTED_EDGE('',*,*,#25292,.F.);
#36579=ORIENTED_EDGE('',*,*,#26783,.T.);
#36580=ORIENTED_EDGE('',*,*,#25279,.F.);
#36581=ORIENTED_EDGE('',*,*,#25385,.F.);
#36582=ORIENTED_EDGE('',*,*,#26785,.F.);
#36583=ORIENTED_EDGE('',*,*,#25281,.F.);
#36584=ORIENTED_EDGE('',*,*,#25273,.F.);
#36585=ORIENTED_EDGE('',*,*,#25270,.F.);
#36586=ORIENTED_EDGE('',*,*,#25382,.F.);
#36587=ORIENTED_EDGE('',*,*,#25390,.F.);
#36588=ORIENTED_EDGE('',*,*,#26786,.T.);
#36589=ORIENTED_EDGE('',*,*,#25379,.F.);
#36590=ORIENTED_EDGE('',*,*,#26786,.F.);
#36591=ORIENTED_EDGE('',*,*,#25386,.F.);
#36592=ORIENTED_EDGE('',*,*,#25278,.F.);
#36593=ORIENTED_EDGE('',*,*,#26785,.T.);
#36594=ORIENTED_EDGE('',*,*,#25265,.F.);
#36595=ORIENTED_EDGE('',*,*,#25371,.F.);
#36596=ORIENTED_EDGE('',*,*,#26787,.F.);
#36597=ORIENTED_EDGE('',*,*,#25267,.F.);
#36598=ORIENTED_EDGE('',*,*,#25259,.F.);
#36599=ORIENTED_EDGE('',*,*,#25256,.F.);
#36600=ORIENTED_EDGE('',*,*,#25368,.F.);
#36601=ORIENTED_EDGE('',*,*,#25376,.F.);
#36602=ORIENTED_EDGE('',*,*,#26788,.T.);
#36603=ORIENTED_EDGE('',*,*,#25365,.F.);
#36604=ORIENTED_EDGE('',*,*,#26788,.F.);
#36605=ORIENTED_EDGE('',*,*,#25372,.F.);
#36606=ORIENTED_EDGE('',*,*,#25264,.F.);
#36607=ORIENTED_EDGE('',*,*,#26787,.T.);
#36608=ORIENTED_EDGE('',*,*,#25250,.F.);
#36609=ORIENTED_EDGE('',*,*,#25357,.F.);
#36610=ORIENTED_EDGE('',*,*,#26789,.F.);
#36611=ORIENTED_EDGE('',*,*,#25252,.F.);
#36612=ORIENTED_EDGE('',*,*,#25244,.F.);
#36613=ORIENTED_EDGE('',*,*,#25241,.F.);
#36614=ORIENTED_EDGE('',*,*,#25354,.F.);
#36615=ORIENTED_EDGE('',*,*,#25362,.F.);
#36616=ORIENTED_EDGE('',*,*,#26790,.T.);
#36617=ORIENTED_EDGE('',*,*,#25351,.F.);
#36618=ORIENTED_EDGE('',*,*,#26790,.F.);
#36619=ORIENTED_EDGE('',*,*,#25358,.F.);
#36620=ORIENTED_EDGE('',*,*,#25249,.F.);
#36621=ORIENTED_EDGE('',*,*,#26789,.T.);
#36622=ORIENTED_EDGE('',*,*,#25238,.F.);
#36623=ORIENTED_EDGE('',*,*,#25342,.F.);
#36624=ORIENTED_EDGE('',*,*,#25331,.F.);
#36625=ORIENTED_EDGE('',*,*,#26791,.F.);
#36626=ORIENTED_EDGE('',*,*,#25343,.F.);
#36627=ORIENTED_EDGE('',*,*,#25237,.F.);
#36628=ORIENTED_EDGE('',*,*,#26792,.T.);
#36629=ORIENTED_EDGE('',*,*,#21328,.F.);
#36630=ORIENTED_EDGE('',*,*,#25339,.F.);
#36631=ORIENTED_EDGE('',*,*,#25347,.F.);
#36632=ORIENTED_EDGE('',*,*,#26791,.T.);
#36633=ORIENTED_EDGE('',*,*,#25336,.F.);
#36634=ORIENTED_EDGE('',*,*,#26792,.F.);
#36635=ORIENTED_EDGE('',*,*,#25349,.F.);
#36636=ORIENTED_EDGE('',*,*,#21329,.F.);
#36637=ORIENTED_EDGE('',*,*,#25229,.F.);
#36638=ORIENTED_EDGE('',*,*,#26793,.F.);
#36639=ORIENTED_EDGE('',*,*,#21533,.F.);
#36640=ORIENTED_EDGE('',*,*,#26793,.T.);
#36641=ORIENTED_EDGE('',*,*,#25225,.F.);
#36642=ORIENTED_EDGE('',*,*,#25326,.F.);
#36643=ORIENTED_EDGE('',*,*,#21534,.F.);
#36644=ORIENTED_EDGE('',*,*,#26794,.F.);
#36645=ORIENTED_EDGE('',*,*,#25227,.F.);
#36646=ORIENTED_EDGE('',*,*,#25219,.F.);
#36647=ORIENTED_EDGE('',*,*,#25216,.F.);
#36648=ORIENTED_EDGE('',*,*,#21537,.F.);
#36649=ORIENTED_EDGE('',*,*,#25329,.F.);
#36650=ORIENTED_EDGE('',*,*,#26795,.T.);
#36651=ORIENTED_EDGE('',*,*,#25324,.F.);
#36652=ORIENTED_EDGE('',*,*,#26795,.F.);
#36653=ORIENTED_EDGE('',*,*,#25327,.F.);
#36654=ORIENTED_EDGE('',*,*,#25224,.F.);
#36655=ORIENTED_EDGE('',*,*,#26794,.T.);
#36656=ORIENTED_EDGE('',*,*,#25211,.F.);
#36657=ORIENTED_EDGE('',*,*,#25317,.F.);
#36658=ORIENTED_EDGE('',*,*,#26796,.F.);
#36659=ORIENTED_EDGE('',*,*,#25213,.F.);
#36660=ORIENTED_EDGE('',*,*,#25205,.F.);
#36661=ORIENTED_EDGE('',*,*,#25202,.F.);
#36662=ORIENTED_EDGE('',*,*,#25314,.F.);
#36663=ORIENTED_EDGE('',*,*,#25322,.F.);
#36664=ORIENTED_EDGE('',*,*,#26797,.T.);
#36665=ORIENTED_EDGE('',*,*,#25311,.F.);
#36666=ORIENTED_EDGE('',*,*,#26797,.F.);
#36667=ORIENTED_EDGE('',*,*,#25318,.F.);
#36668=ORIENTED_EDGE('',*,*,#25210,.F.);
#36669=ORIENTED_EDGE('',*,*,#26796,.T.);
#36670=ORIENTED_EDGE('',*,*,#25197,.F.);
#36671=ORIENTED_EDGE('',*,*,#25303,.F.);
#36672=ORIENTED_EDGE('',*,*,#26798,.F.);
#36673=ORIENTED_EDGE('',*,*,#25199,.F.);
#36674=ORIENTED_EDGE('',*,*,#25191,.F.);
#36675=ORIENTED_EDGE('',*,*,#25188,.F.);
#36676=ORIENTED_EDGE('',*,*,#25300,.F.);
#36677=ORIENTED_EDGE('',*,*,#25308,.F.);
#36678=ORIENTED_EDGE('',*,*,#26799,.T.);
#36679=ORIENTED_EDGE('',*,*,#25297,.F.);
#36680=ORIENTED_EDGE('',*,*,#26799,.F.);
#36681=ORIENTED_EDGE('',*,*,#25304,.F.);
#36682=ORIENTED_EDGE('',*,*,#25196,.F.);
#36683=ORIENTED_EDGE('',*,*,#26798,.T.);
#36684=ORIENTED_EDGE('',*,*,#25183,.F.);
#36685=ORIENTED_EDGE('',*,*,#25289,.F.);
#36686=ORIENTED_EDGE('',*,*,#26800,.F.);
#36687=ORIENTED_EDGE('',*,*,#25185,.F.);
#36688=ORIENTED_EDGE('',*,*,#25177,.F.);
#36689=ORIENTED_EDGE('',*,*,#25174,.F.);
#36690=ORIENTED_EDGE('',*,*,#25286,.F.);
#36691=ORIENTED_EDGE('',*,*,#25294,.F.);
#36692=ORIENTED_EDGE('',*,*,#26801,.T.);
#36693=ORIENTED_EDGE('',*,*,#25283,.F.);
#36694=ORIENTED_EDGE('',*,*,#26801,.F.);
#36695=ORIENTED_EDGE('',*,*,#25290,.F.);
#36696=ORIENTED_EDGE('',*,*,#25182,.F.);
#36697=ORIENTED_EDGE('',*,*,#26800,.T.);
#36698=ORIENTED_EDGE('',*,*,#25169,.F.);
#36699=ORIENTED_EDGE('',*,*,#25275,.F.);
#36700=ORIENTED_EDGE('',*,*,#26802,.F.);
#36701=ORIENTED_EDGE('',*,*,#25171,.F.);
#36702=ORIENTED_EDGE('',*,*,#25163,.F.);
#36703=ORIENTED_EDGE('',*,*,#25160,.F.);
#36704=ORIENTED_EDGE('',*,*,#25272,.F.);
#36705=ORIENTED_EDGE('',*,*,#25280,.F.);
#36706=ORIENTED_EDGE('',*,*,#26803,.T.);
#36707=ORIENTED_EDGE('',*,*,#25269,.F.);
#36708=ORIENTED_EDGE('',*,*,#26803,.F.);
#36709=ORIENTED_EDGE('',*,*,#25276,.F.);
#36710=ORIENTED_EDGE('',*,*,#25168,.F.);
#36711=ORIENTED_EDGE('',*,*,#26802,.T.);
#36712=ORIENTED_EDGE('',*,*,#25154,.F.);
#36713=ORIENTED_EDGE('',*,*,#25261,.F.);
#36714=ORIENTED_EDGE('',*,*,#26804,.F.);
#36715=ORIENTED_EDGE('',*,*,#25156,.F.);
#36716=ORIENTED_EDGE('',*,*,#25148,.F.);
#36717=ORIENTED_EDGE('',*,*,#25145,.F.);
#36718=ORIENTED_EDGE('',*,*,#25258,.F.);
#36719=ORIENTED_EDGE('',*,*,#25266,.F.);
#36720=ORIENTED_EDGE('',*,*,#26805,.T.);
#36721=ORIENTED_EDGE('',*,*,#25255,.F.);
#36722=ORIENTED_EDGE('',*,*,#26805,.F.);
#36723=ORIENTED_EDGE('',*,*,#25262,.F.);
#36724=ORIENTED_EDGE('',*,*,#25153,.F.);
#36725=ORIENTED_EDGE('',*,*,#26804,.T.);
#36726=ORIENTED_EDGE('',*,*,#25142,.F.);
#36727=ORIENTED_EDGE('',*,*,#25246,.F.);
#36728=ORIENTED_EDGE('',*,*,#25235,.F.);
#36729=ORIENTED_EDGE('',*,*,#26806,.F.);
#36730=ORIENTED_EDGE('',*,*,#25247,.F.);
#36731=ORIENTED_EDGE('',*,*,#25141,.F.);
#36732=ORIENTED_EDGE('',*,*,#26807,.T.);
#36733=ORIENTED_EDGE('',*,*,#21332,.F.);
#36734=ORIENTED_EDGE('',*,*,#25243,.F.);
#36735=ORIENTED_EDGE('',*,*,#25251,.F.);
#36736=ORIENTED_EDGE('',*,*,#26806,.T.);
#36737=ORIENTED_EDGE('',*,*,#25240,.F.);
#36738=ORIENTED_EDGE('',*,*,#26807,.F.);
#36739=ORIENTED_EDGE('',*,*,#25253,.F.);
#36740=ORIENTED_EDGE('',*,*,#21333,.F.);
#36741=ORIENTED_EDGE('',*,*,#25133,.F.);
#36742=ORIENTED_EDGE('',*,*,#26808,.F.);
#36743=ORIENTED_EDGE('',*,*,#21527,.F.);
#36744=ORIENTED_EDGE('',*,*,#26808,.T.);
#36745=ORIENTED_EDGE('',*,*,#25129,.F.);
#36746=ORIENTED_EDGE('',*,*,#25230,.F.);
#36747=ORIENTED_EDGE('',*,*,#21528,.F.);
#36748=ORIENTED_EDGE('',*,*,#26809,.F.);
#36749=ORIENTED_EDGE('',*,*,#25131,.F.);
#36750=ORIENTED_EDGE('',*,*,#25123,.F.);
#36751=ORIENTED_EDGE('',*,*,#25120,.F.);
#36752=ORIENTED_EDGE('',*,*,#21531,.F.);
#36753=ORIENTED_EDGE('',*,*,#25233,.F.);
#36754=ORIENTED_EDGE('',*,*,#26810,.T.);
#36755=ORIENTED_EDGE('',*,*,#25228,.F.);
#36756=ORIENTED_EDGE('',*,*,#26810,.F.);
#36757=ORIENTED_EDGE('',*,*,#25231,.F.);
#36758=ORIENTED_EDGE('',*,*,#25128,.F.);
#36759=ORIENTED_EDGE('',*,*,#26809,.T.);
#36760=ORIENTED_EDGE('',*,*,#25115,.F.);
#36761=ORIENTED_EDGE('',*,*,#25221,.F.);
#36762=ORIENTED_EDGE('',*,*,#26811,.F.);
#36763=ORIENTED_EDGE('',*,*,#25117,.F.);
#36764=ORIENTED_EDGE('',*,*,#25109,.F.);
#36765=ORIENTED_EDGE('',*,*,#25106,.F.);
#36766=ORIENTED_EDGE('',*,*,#25218,.F.);
#36767=ORIENTED_EDGE('',*,*,#25226,.F.);
#36768=ORIENTED_EDGE('',*,*,#26812,.T.);
#36769=ORIENTED_EDGE('',*,*,#25215,.F.);
#36770=ORIENTED_EDGE('',*,*,#26812,.F.);
#36771=ORIENTED_EDGE('',*,*,#25222,.F.);
#36772=ORIENTED_EDGE('',*,*,#25114,.F.);
#36773=ORIENTED_EDGE('',*,*,#26811,.T.);
#36774=ORIENTED_EDGE('',*,*,#25101,.F.);
#36775=ORIENTED_EDGE('',*,*,#25207,.F.);
#36776=ORIENTED_EDGE('',*,*,#26813,.F.);
#36777=ORIENTED_EDGE('',*,*,#25103,.F.);
#36778=ORIENTED_EDGE('',*,*,#25095,.F.);
#36779=ORIENTED_EDGE('',*,*,#25092,.F.);
#36780=ORIENTED_EDGE('',*,*,#25204,.F.);
#36781=ORIENTED_EDGE('',*,*,#25212,.F.);
#36782=ORIENTED_EDGE('',*,*,#26814,.T.);
#36783=ORIENTED_EDGE('',*,*,#25201,.F.);
#36784=ORIENTED_EDGE('',*,*,#26814,.F.);
#36785=ORIENTED_EDGE('',*,*,#25208,.F.);
#36786=ORIENTED_EDGE('',*,*,#25100,.F.);
#36787=ORIENTED_EDGE('',*,*,#26813,.T.);
#36788=ORIENTED_EDGE('',*,*,#25087,.F.);
#36789=ORIENTED_EDGE('',*,*,#25193,.F.);
#36790=ORIENTED_EDGE('',*,*,#26815,.F.);
#36791=ORIENTED_EDGE('',*,*,#25089,.F.);
#36792=ORIENTED_EDGE('',*,*,#25081,.F.);
#36793=ORIENTED_EDGE('',*,*,#25078,.F.);
#36794=ORIENTED_EDGE('',*,*,#25190,.F.);
#36795=ORIENTED_EDGE('',*,*,#25198,.F.);
#36796=ORIENTED_EDGE('',*,*,#26816,.T.);
#36797=ORIENTED_EDGE('',*,*,#25187,.F.);
#36798=ORIENTED_EDGE('',*,*,#26816,.F.);
#36799=ORIENTED_EDGE('',*,*,#25194,.F.);
#36800=ORIENTED_EDGE('',*,*,#25086,.F.);
#36801=ORIENTED_EDGE('',*,*,#26815,.T.);
#36802=ORIENTED_EDGE('',*,*,#25073,.F.);
#36803=ORIENTED_EDGE('',*,*,#25179,.F.);
#36804=ORIENTED_EDGE('',*,*,#26817,.F.);
#36805=ORIENTED_EDGE('',*,*,#25075,.F.);
#36806=ORIENTED_EDGE('',*,*,#25067,.F.);
#36807=ORIENTED_EDGE('',*,*,#25064,.F.);
#36808=ORIENTED_EDGE('',*,*,#25176,.F.);
#36809=ORIENTED_EDGE('',*,*,#25184,.F.);
#36810=ORIENTED_EDGE('',*,*,#26818,.T.);
#36811=ORIENTED_EDGE('',*,*,#25173,.F.);
#36812=ORIENTED_EDGE('',*,*,#26818,.F.);
#36813=ORIENTED_EDGE('',*,*,#25180,.F.);
#36814=ORIENTED_EDGE('',*,*,#25072,.F.);
#36815=ORIENTED_EDGE('',*,*,#26817,.T.);
#36816=ORIENTED_EDGE('',*,*,#25058,.F.);
#36817=ORIENTED_EDGE('',*,*,#25165,.F.);
#36818=ORIENTED_EDGE('',*,*,#26819,.F.);
#36819=ORIENTED_EDGE('',*,*,#25060,.F.);
#36820=ORIENTED_EDGE('',*,*,#25052,.F.);
#36821=ORIENTED_EDGE('',*,*,#25049,.F.);
#36822=ORIENTED_EDGE('',*,*,#25162,.F.);
#36823=ORIENTED_EDGE('',*,*,#25170,.F.);
#36824=ORIENTED_EDGE('',*,*,#26820,.T.);
#36825=ORIENTED_EDGE('',*,*,#25159,.F.);
#36826=ORIENTED_EDGE('',*,*,#26820,.F.);
#36827=ORIENTED_EDGE('',*,*,#25166,.F.);
#36828=ORIENTED_EDGE('',*,*,#25057,.F.);
#36829=ORIENTED_EDGE('',*,*,#26819,.T.);
#36830=ORIENTED_EDGE('',*,*,#25046,.F.);
#36831=ORIENTED_EDGE('',*,*,#25150,.F.);
#36832=ORIENTED_EDGE('',*,*,#25139,.F.);
#36833=ORIENTED_EDGE('',*,*,#26821,.F.);
#36834=ORIENTED_EDGE('',*,*,#25151,.F.);
#36835=ORIENTED_EDGE('',*,*,#25045,.F.);
#36836=ORIENTED_EDGE('',*,*,#26822,.T.);
#36837=ORIENTED_EDGE('',*,*,#21336,.F.);
#36838=ORIENTED_EDGE('',*,*,#25147,.F.);
#36839=ORIENTED_EDGE('',*,*,#25155,.F.);
#36840=ORIENTED_EDGE('',*,*,#26821,.T.);
#36841=ORIENTED_EDGE('',*,*,#25144,.F.);
#36842=ORIENTED_EDGE('',*,*,#26822,.F.);
#36843=ORIENTED_EDGE('',*,*,#25157,.F.);
#36844=ORIENTED_EDGE('',*,*,#21337,.F.);
#36845=ORIENTED_EDGE('',*,*,#25037,.F.);
#36846=ORIENTED_EDGE('',*,*,#26823,.F.);
#36847=ORIENTED_EDGE('',*,*,#21521,.F.);
#36848=ORIENTED_EDGE('',*,*,#26823,.T.);
#36849=ORIENTED_EDGE('',*,*,#25033,.F.);
#36850=ORIENTED_EDGE('',*,*,#25134,.F.);
#36851=ORIENTED_EDGE('',*,*,#21522,.F.);
#36852=ORIENTED_EDGE('',*,*,#26824,.F.);
#36853=ORIENTED_EDGE('',*,*,#25035,.F.);
#36854=ORIENTED_EDGE('',*,*,#25027,.F.);
#36855=ORIENTED_EDGE('',*,*,#25024,.F.);
#36856=ORIENTED_EDGE('',*,*,#21525,.F.);
#36857=ORIENTED_EDGE('',*,*,#25137,.F.);
#36858=ORIENTED_EDGE('',*,*,#26825,.T.);
#36859=ORIENTED_EDGE('',*,*,#25132,.F.);
#36860=ORIENTED_EDGE('',*,*,#26825,.F.);
#36861=ORIENTED_EDGE('',*,*,#25135,.F.);
#36862=ORIENTED_EDGE('',*,*,#25032,.F.);
#36863=ORIENTED_EDGE('',*,*,#26824,.T.);
#36864=ORIENTED_EDGE('',*,*,#25019,.F.);
#36865=ORIENTED_EDGE('',*,*,#25125,.F.);
#36866=ORIENTED_EDGE('',*,*,#26826,.F.);
#36867=ORIENTED_EDGE('',*,*,#25021,.F.);
#36868=ORIENTED_EDGE('',*,*,#25013,.F.);
#36869=ORIENTED_EDGE('',*,*,#25010,.F.);
#36870=ORIENTED_EDGE('',*,*,#25122,.F.);
#36871=ORIENTED_EDGE('',*,*,#25130,.F.);
#36872=ORIENTED_EDGE('',*,*,#26827,.T.);
#36873=ORIENTED_EDGE('',*,*,#25119,.F.);
#36874=ORIENTED_EDGE('',*,*,#26827,.F.);
#36875=ORIENTED_EDGE('',*,*,#25126,.F.);
#36876=ORIENTED_EDGE('',*,*,#25018,.F.);
#36877=ORIENTED_EDGE('',*,*,#26826,.T.);
#36878=ORIENTED_EDGE('',*,*,#25005,.F.);
#36879=ORIENTED_EDGE('',*,*,#25111,.F.);
#36880=ORIENTED_EDGE('',*,*,#26828,.F.);
#36881=ORIENTED_EDGE('',*,*,#25007,.F.);
#36882=ORIENTED_EDGE('',*,*,#24999,.F.);
#36883=ORIENTED_EDGE('',*,*,#24996,.F.);
#36884=ORIENTED_EDGE('',*,*,#25108,.F.);
#36885=ORIENTED_EDGE('',*,*,#25116,.F.);
#36886=ORIENTED_EDGE('',*,*,#26829,.T.);
#36887=ORIENTED_EDGE('',*,*,#25105,.F.);
#36888=ORIENTED_EDGE('',*,*,#26829,.F.);
#36889=ORIENTED_EDGE('',*,*,#25112,.F.);
#36890=ORIENTED_EDGE('',*,*,#25004,.F.);
#36891=ORIENTED_EDGE('',*,*,#26828,.T.);
#36892=ORIENTED_EDGE('',*,*,#24991,.F.);
#36893=ORIENTED_EDGE('',*,*,#25097,.F.);
#36894=ORIENTED_EDGE('',*,*,#26830,.F.);
#36895=ORIENTED_EDGE('',*,*,#24993,.F.);
#36896=ORIENTED_EDGE('',*,*,#24985,.F.);
#36897=ORIENTED_EDGE('',*,*,#24982,.F.);
#36898=ORIENTED_EDGE('',*,*,#25094,.F.);
#36899=ORIENTED_EDGE('',*,*,#25102,.F.);
#36900=ORIENTED_EDGE('',*,*,#26831,.T.);
#36901=ORIENTED_EDGE('',*,*,#25091,.F.);
#36902=ORIENTED_EDGE('',*,*,#26831,.F.);
#36903=ORIENTED_EDGE('',*,*,#25098,.F.);
#36904=ORIENTED_EDGE('',*,*,#24990,.F.);
#36905=ORIENTED_EDGE('',*,*,#26830,.T.);
#36906=ORIENTED_EDGE('',*,*,#24977,.F.);
#36907=ORIENTED_EDGE('',*,*,#25083,.F.);
#36908=ORIENTED_EDGE('',*,*,#26832,.F.);
#36909=ORIENTED_EDGE('',*,*,#24979,.F.);
#36910=ORIENTED_EDGE('',*,*,#24971,.F.);
#36911=ORIENTED_EDGE('',*,*,#24968,.F.);
#36912=ORIENTED_EDGE('',*,*,#25080,.F.);
#36913=ORIENTED_EDGE('',*,*,#25088,.F.);
#36914=ORIENTED_EDGE('',*,*,#26833,.T.);
#36915=ORIENTED_EDGE('',*,*,#25077,.F.);
#36916=ORIENTED_EDGE('',*,*,#26833,.F.);
#36917=ORIENTED_EDGE('',*,*,#25084,.F.);
#36918=ORIENTED_EDGE('',*,*,#24976,.F.);
#36919=ORIENTED_EDGE('',*,*,#26832,.T.);
#36920=ORIENTED_EDGE('',*,*,#24962,.F.);
#36921=ORIENTED_EDGE('',*,*,#25069,.F.);
#36922=ORIENTED_EDGE('',*,*,#26834,.F.);
#36923=ORIENTED_EDGE('',*,*,#24964,.F.);
#36924=ORIENTED_EDGE('',*,*,#24956,.F.);
#36925=ORIENTED_EDGE('',*,*,#24953,.F.);
#36926=ORIENTED_EDGE('',*,*,#25066,.F.);
#36927=ORIENTED_EDGE('',*,*,#25074,.F.);
#36928=ORIENTED_EDGE('',*,*,#26835,.T.);
#36929=ORIENTED_EDGE('',*,*,#25063,.F.);
#36930=ORIENTED_EDGE('',*,*,#26835,.F.);
#36931=ORIENTED_EDGE('',*,*,#25070,.F.);
#36932=ORIENTED_EDGE('',*,*,#24961,.F.);
#36933=ORIENTED_EDGE('',*,*,#26834,.T.);
#36934=ORIENTED_EDGE('',*,*,#24950,.F.);
#36935=ORIENTED_EDGE('',*,*,#25054,.F.);
#36936=ORIENTED_EDGE('',*,*,#25043,.F.);
#36937=ORIENTED_EDGE('',*,*,#26836,.F.);
#36938=ORIENTED_EDGE('',*,*,#25055,.F.);
#36939=ORIENTED_EDGE('',*,*,#24949,.F.);
#36940=ORIENTED_EDGE('',*,*,#26837,.T.);
#36941=ORIENTED_EDGE('',*,*,#21340,.F.);
#36942=ORIENTED_EDGE('',*,*,#25051,.F.);
#36943=ORIENTED_EDGE('',*,*,#25059,.F.);
#36944=ORIENTED_EDGE('',*,*,#26836,.T.);
#36945=ORIENTED_EDGE('',*,*,#25048,.F.);
#36946=ORIENTED_EDGE('',*,*,#26837,.F.);
#36947=ORIENTED_EDGE('',*,*,#25061,.F.);
#36948=ORIENTED_EDGE('',*,*,#21341,.F.);
#36949=ORIENTED_EDGE('',*,*,#24941,.F.);
#36950=ORIENTED_EDGE('',*,*,#26838,.F.);
#36951=ORIENTED_EDGE('',*,*,#21515,.F.);
#36952=ORIENTED_EDGE('',*,*,#26838,.T.);
#36953=ORIENTED_EDGE('',*,*,#24937,.F.);
#36954=ORIENTED_EDGE('',*,*,#25038,.F.);
#36955=ORIENTED_EDGE('',*,*,#21516,.F.);
#36956=ORIENTED_EDGE('',*,*,#26839,.F.);
#36957=ORIENTED_EDGE('',*,*,#24939,.F.);
#36958=ORIENTED_EDGE('',*,*,#24931,.F.);
#36959=ORIENTED_EDGE('',*,*,#24928,.F.);
#36960=ORIENTED_EDGE('',*,*,#21519,.F.);
#36961=ORIENTED_EDGE('',*,*,#25041,.F.);
#36962=ORIENTED_EDGE('',*,*,#26840,.T.);
#36963=ORIENTED_EDGE('',*,*,#25036,.F.);
#36964=ORIENTED_EDGE('',*,*,#26840,.F.);
#36965=ORIENTED_EDGE('',*,*,#25039,.F.);
#36966=ORIENTED_EDGE('',*,*,#24936,.F.);
#36967=ORIENTED_EDGE('',*,*,#26839,.T.);
#36968=ORIENTED_EDGE('',*,*,#24923,.F.);
#36969=ORIENTED_EDGE('',*,*,#25029,.F.);
#36970=ORIENTED_EDGE('',*,*,#26841,.F.);
#36971=ORIENTED_EDGE('',*,*,#24925,.F.);
#36972=ORIENTED_EDGE('',*,*,#24917,.F.);
#36973=ORIENTED_EDGE('',*,*,#24914,.F.);
#36974=ORIENTED_EDGE('',*,*,#25026,.F.);
#36975=ORIENTED_EDGE('',*,*,#25034,.F.);
#36976=ORIENTED_EDGE('',*,*,#26842,.T.);
#36977=ORIENTED_EDGE('',*,*,#25023,.F.);
#36978=ORIENTED_EDGE('',*,*,#26842,.F.);
#36979=ORIENTED_EDGE('',*,*,#25030,.F.);
#36980=ORIENTED_EDGE('',*,*,#24922,.F.);
#36981=ORIENTED_EDGE('',*,*,#26841,.T.);
#36982=ORIENTED_EDGE('',*,*,#24909,.F.);
#36983=ORIENTED_EDGE('',*,*,#25015,.F.);
#36984=ORIENTED_EDGE('',*,*,#26843,.F.);
#36985=ORIENTED_EDGE('',*,*,#24911,.F.);
#36986=ORIENTED_EDGE('',*,*,#24903,.F.);
#36987=ORIENTED_EDGE('',*,*,#24900,.F.);
#36988=ORIENTED_EDGE('',*,*,#25012,.F.);
#36989=ORIENTED_EDGE('',*,*,#25020,.F.);
#36990=ORIENTED_EDGE('',*,*,#26844,.T.);
#36991=ORIENTED_EDGE('',*,*,#25009,.F.);
#36992=ORIENTED_EDGE('',*,*,#26844,.F.);
#36993=ORIENTED_EDGE('',*,*,#25016,.F.);
#36994=ORIENTED_EDGE('',*,*,#24908,.F.);
#36995=ORIENTED_EDGE('',*,*,#26843,.T.);
#36996=ORIENTED_EDGE('',*,*,#24895,.F.);
#36997=ORIENTED_EDGE('',*,*,#25001,.F.);
#36998=ORIENTED_EDGE('',*,*,#26845,.F.);
#36999=ORIENTED_EDGE('',*,*,#24897,.F.);
#37000=ORIENTED_EDGE('',*,*,#24889,.F.);
#37001=ORIENTED_EDGE('',*,*,#24886,.F.);
#37002=ORIENTED_EDGE('',*,*,#24998,.F.);
#37003=ORIENTED_EDGE('',*,*,#25006,.F.);
#37004=ORIENTED_EDGE('',*,*,#26846,.T.);
#37005=ORIENTED_EDGE('',*,*,#24995,.F.);
#37006=ORIENTED_EDGE('',*,*,#26846,.F.);
#37007=ORIENTED_EDGE('',*,*,#25002,.F.);
#37008=ORIENTED_EDGE('',*,*,#24894,.F.);
#37009=ORIENTED_EDGE('',*,*,#26845,.T.);
#37010=ORIENTED_EDGE('',*,*,#24881,.F.);
#37011=ORIENTED_EDGE('',*,*,#24987,.F.);
#37012=ORIENTED_EDGE('',*,*,#26847,.F.);
#37013=ORIENTED_EDGE('',*,*,#24883,.F.);
#37014=ORIENTED_EDGE('',*,*,#24875,.F.);
#37015=ORIENTED_EDGE('',*,*,#24872,.F.);
#37016=ORIENTED_EDGE('',*,*,#24984,.F.);
#37017=ORIENTED_EDGE('',*,*,#24992,.F.);
#37018=ORIENTED_EDGE('',*,*,#26848,.T.);
#37019=ORIENTED_EDGE('',*,*,#24981,.F.);
#37020=ORIENTED_EDGE('',*,*,#26848,.F.);
#37021=ORIENTED_EDGE('',*,*,#24988,.F.);
#37022=ORIENTED_EDGE('',*,*,#24880,.F.);
#37023=ORIENTED_EDGE('',*,*,#26847,.T.);
#37024=ORIENTED_EDGE('',*,*,#24866,.F.);
#37025=ORIENTED_EDGE('',*,*,#24973,.F.);
#37026=ORIENTED_EDGE('',*,*,#26849,.F.);
#37027=ORIENTED_EDGE('',*,*,#24868,.F.);
#37028=ORIENTED_EDGE('',*,*,#24860,.F.);
#37029=ORIENTED_EDGE('',*,*,#24857,.F.);
#37030=ORIENTED_EDGE('',*,*,#24970,.F.);
#37031=ORIENTED_EDGE('',*,*,#24978,.F.);
#37032=ORIENTED_EDGE('',*,*,#26850,.T.);
#37033=ORIENTED_EDGE('',*,*,#24967,.F.);
#37034=ORIENTED_EDGE('',*,*,#26850,.F.);
#37035=ORIENTED_EDGE('',*,*,#24974,.F.);
#37036=ORIENTED_EDGE('',*,*,#24865,.F.);
#37037=ORIENTED_EDGE('',*,*,#26849,.T.);
#37038=ORIENTED_EDGE('',*,*,#24854,.F.);
#37039=ORIENTED_EDGE('',*,*,#24958,.F.);
#37040=ORIENTED_EDGE('',*,*,#24947,.F.);
#37041=ORIENTED_EDGE('',*,*,#26851,.F.);
#37042=ORIENTED_EDGE('',*,*,#24959,.F.);
#37043=ORIENTED_EDGE('',*,*,#24853,.F.);
#37044=ORIENTED_EDGE('',*,*,#26852,.T.);
#37045=ORIENTED_EDGE('',*,*,#21344,.F.);
#37046=ORIENTED_EDGE('',*,*,#24955,.F.);
#37047=ORIENTED_EDGE('',*,*,#24963,.F.);
#37048=ORIENTED_EDGE('',*,*,#26851,.T.);
#37049=ORIENTED_EDGE('',*,*,#24952,.F.);
#37050=ORIENTED_EDGE('',*,*,#26852,.F.);
#37051=ORIENTED_EDGE('',*,*,#24965,.F.);
#37052=ORIENTED_EDGE('',*,*,#21345,.F.);
#37053=ORIENTED_EDGE('',*,*,#24845,.F.);
#37054=ORIENTED_EDGE('',*,*,#26853,.F.);
#37055=ORIENTED_EDGE('',*,*,#21509,.F.);
#37056=ORIENTED_EDGE('',*,*,#26853,.T.);
#37057=ORIENTED_EDGE('',*,*,#24841,.F.);
#37058=ORIENTED_EDGE('',*,*,#24942,.F.);
#37059=ORIENTED_EDGE('',*,*,#21510,.F.);
#37060=ORIENTED_EDGE('',*,*,#26854,.F.);
#37061=ORIENTED_EDGE('',*,*,#24843,.F.);
#37062=ORIENTED_EDGE('',*,*,#24835,.F.);
#37063=ORIENTED_EDGE('',*,*,#24832,.F.);
#37064=ORIENTED_EDGE('',*,*,#21513,.F.);
#37065=ORIENTED_EDGE('',*,*,#24945,.F.);
#37066=ORIENTED_EDGE('',*,*,#26855,.T.);
#37067=ORIENTED_EDGE('',*,*,#24940,.F.);
#37068=ORIENTED_EDGE('',*,*,#26855,.F.);
#37069=ORIENTED_EDGE('',*,*,#24943,.F.);
#37070=ORIENTED_EDGE('',*,*,#24840,.F.);
#37071=ORIENTED_EDGE('',*,*,#26854,.T.);
#37072=ORIENTED_EDGE('',*,*,#24827,.F.);
#37073=ORIENTED_EDGE('',*,*,#24933,.F.);
#37074=ORIENTED_EDGE('',*,*,#26856,.F.);
#37075=ORIENTED_EDGE('',*,*,#24829,.F.);
#37076=ORIENTED_EDGE('',*,*,#24821,.F.);
#37077=ORIENTED_EDGE('',*,*,#24818,.F.);
#37078=ORIENTED_EDGE('',*,*,#24930,.F.);
#37079=ORIENTED_EDGE('',*,*,#24938,.F.);
#37080=ORIENTED_EDGE('',*,*,#26857,.T.);
#37081=ORIENTED_EDGE('',*,*,#24927,.F.);
#37082=ORIENTED_EDGE('',*,*,#26857,.F.);
#37083=ORIENTED_EDGE('',*,*,#24934,.F.);
#37084=ORIENTED_EDGE('',*,*,#24826,.F.);
#37085=ORIENTED_EDGE('',*,*,#26856,.T.);
#37086=ORIENTED_EDGE('',*,*,#24813,.F.);
#37087=ORIENTED_EDGE('',*,*,#24919,.F.);
#37088=ORIENTED_EDGE('',*,*,#26858,.F.);
#37089=ORIENTED_EDGE('',*,*,#24815,.F.);
#37090=ORIENTED_EDGE('',*,*,#24807,.F.);
#37091=ORIENTED_EDGE('',*,*,#24804,.F.);
#37092=ORIENTED_EDGE('',*,*,#24916,.F.);
#37093=ORIENTED_EDGE('',*,*,#24924,.F.);
#37094=ORIENTED_EDGE('',*,*,#26859,.T.);
#37095=ORIENTED_EDGE('',*,*,#24913,.F.);
#37096=ORIENTED_EDGE('',*,*,#26859,.F.);
#37097=ORIENTED_EDGE('',*,*,#24920,.F.);
#37098=ORIENTED_EDGE('',*,*,#24812,.F.);
#37099=ORIENTED_EDGE('',*,*,#26858,.T.);
#37100=ORIENTED_EDGE('',*,*,#24799,.F.);
#37101=ORIENTED_EDGE('',*,*,#24905,.F.);
#37102=ORIENTED_EDGE('',*,*,#26860,.F.);
#37103=ORIENTED_EDGE('',*,*,#24801,.F.);
#37104=ORIENTED_EDGE('',*,*,#24793,.F.);
#37105=ORIENTED_EDGE('',*,*,#24790,.F.);
#37106=ORIENTED_EDGE('',*,*,#24902,.F.);
#37107=ORIENTED_EDGE('',*,*,#24910,.F.);
#37108=ORIENTED_EDGE('',*,*,#26861,.T.);
#37109=ORIENTED_EDGE('',*,*,#24899,.F.);
#37110=ORIENTED_EDGE('',*,*,#26861,.F.);
#37111=ORIENTED_EDGE('',*,*,#24906,.F.);
#37112=ORIENTED_EDGE('',*,*,#24798,.F.);
#37113=ORIENTED_EDGE('',*,*,#26860,.T.);
#37114=ORIENTED_EDGE('',*,*,#24785,.F.);
#37115=ORIENTED_EDGE('',*,*,#24891,.F.);
#37116=ORIENTED_EDGE('',*,*,#26862,.F.);
#37117=ORIENTED_EDGE('',*,*,#24787,.F.);
#37118=ORIENTED_EDGE('',*,*,#24779,.F.);
#37119=ORIENTED_EDGE('',*,*,#24776,.F.);
#37120=ORIENTED_EDGE('',*,*,#24888,.F.);
#37121=ORIENTED_EDGE('',*,*,#24896,.F.);
#37122=ORIENTED_EDGE('',*,*,#26863,.T.);
#37123=ORIENTED_EDGE('',*,*,#24885,.F.);
#37124=ORIENTED_EDGE('',*,*,#26863,.F.);
#37125=ORIENTED_EDGE('',*,*,#24892,.F.);
#37126=ORIENTED_EDGE('',*,*,#24784,.F.);
#37127=ORIENTED_EDGE('',*,*,#26862,.T.);
#37128=ORIENTED_EDGE('',*,*,#24770,.F.);
#37129=ORIENTED_EDGE('',*,*,#24877,.F.);
#37130=ORIENTED_EDGE('',*,*,#26864,.F.);
#37131=ORIENTED_EDGE('',*,*,#24772,.F.);
#37132=ORIENTED_EDGE('',*,*,#24764,.F.);
#37133=ORIENTED_EDGE('',*,*,#24761,.F.);
#37134=ORIENTED_EDGE('',*,*,#24874,.F.);
#37135=ORIENTED_EDGE('',*,*,#24882,.F.);
#37136=ORIENTED_EDGE('',*,*,#26865,.T.);
#37137=ORIENTED_EDGE('',*,*,#24871,.F.);
#37138=ORIENTED_EDGE('',*,*,#26865,.F.);
#37139=ORIENTED_EDGE('',*,*,#24878,.F.);
#37140=ORIENTED_EDGE('',*,*,#24769,.F.);
#37141=ORIENTED_EDGE('',*,*,#26864,.T.);
#37142=ORIENTED_EDGE('',*,*,#24758,.F.);
#37143=ORIENTED_EDGE('',*,*,#24862,.F.);
#37144=ORIENTED_EDGE('',*,*,#24851,.F.);
#37145=ORIENTED_EDGE('',*,*,#26866,.F.);
#37146=ORIENTED_EDGE('',*,*,#24863,.F.);
#37147=ORIENTED_EDGE('',*,*,#24757,.F.);
#37148=ORIENTED_EDGE('',*,*,#26867,.T.);
#37149=ORIENTED_EDGE('',*,*,#21348,.F.);
#37150=ORIENTED_EDGE('',*,*,#24859,.F.);
#37151=ORIENTED_EDGE('',*,*,#24867,.F.);
#37152=ORIENTED_EDGE('',*,*,#26866,.T.);
#37153=ORIENTED_EDGE('',*,*,#24856,.F.);
#37154=ORIENTED_EDGE('',*,*,#26867,.F.);
#37155=ORIENTED_EDGE('',*,*,#24869,.F.);
#37156=ORIENTED_EDGE('',*,*,#21349,.F.);
#37157=ORIENTED_EDGE('',*,*,#24749,.F.);
#37158=ORIENTED_EDGE('',*,*,#26868,.F.);
#37159=ORIENTED_EDGE('',*,*,#21503,.F.);
#37160=ORIENTED_EDGE('',*,*,#26868,.T.);
#37161=ORIENTED_EDGE('',*,*,#24745,.F.);
#37162=ORIENTED_EDGE('',*,*,#24846,.F.);
#37163=ORIENTED_EDGE('',*,*,#21504,.F.);
#37164=ORIENTED_EDGE('',*,*,#26869,.F.);
#37165=ORIENTED_EDGE('',*,*,#24747,.F.);
#37166=ORIENTED_EDGE('',*,*,#24739,.F.);
#37167=ORIENTED_EDGE('',*,*,#24736,.F.);
#37168=ORIENTED_EDGE('',*,*,#21507,.F.);
#37169=ORIENTED_EDGE('',*,*,#24849,.F.);
#37170=ORIENTED_EDGE('',*,*,#26870,.T.);
#37171=ORIENTED_EDGE('',*,*,#24844,.F.);
#37172=ORIENTED_EDGE('',*,*,#26870,.F.);
#37173=ORIENTED_EDGE('',*,*,#24847,.F.);
#37174=ORIENTED_EDGE('',*,*,#24744,.F.);
#37175=ORIENTED_EDGE('',*,*,#26869,.T.);
#37176=ORIENTED_EDGE('',*,*,#24731,.F.);
#37177=ORIENTED_EDGE('',*,*,#24837,.F.);
#37178=ORIENTED_EDGE('',*,*,#26871,.F.);
#37179=ORIENTED_EDGE('',*,*,#24733,.F.);
#37180=ORIENTED_EDGE('',*,*,#24725,.F.);
#37181=ORIENTED_EDGE('',*,*,#24722,.F.);
#37182=ORIENTED_EDGE('',*,*,#24834,.F.);
#37183=ORIENTED_EDGE('',*,*,#24842,.F.);
#37184=ORIENTED_EDGE('',*,*,#26872,.T.);
#37185=ORIENTED_EDGE('',*,*,#24831,.F.);
#37186=ORIENTED_EDGE('',*,*,#26872,.F.);
#37187=ORIENTED_EDGE('',*,*,#24838,.F.);
#37188=ORIENTED_EDGE('',*,*,#24730,.F.);
#37189=ORIENTED_EDGE('',*,*,#26871,.T.);
#37190=ORIENTED_EDGE('',*,*,#24717,.F.);
#37191=ORIENTED_EDGE('',*,*,#24823,.F.);
#37192=ORIENTED_EDGE('',*,*,#26873,.F.);
#37193=ORIENTED_EDGE('',*,*,#24719,.F.);
#37194=ORIENTED_EDGE('',*,*,#24711,.F.);
#37195=ORIENTED_EDGE('',*,*,#24708,.F.);
#37196=ORIENTED_EDGE('',*,*,#24820,.F.);
#37197=ORIENTED_EDGE('',*,*,#24828,.F.);
#37198=ORIENTED_EDGE('',*,*,#26874,.T.);
#37199=ORIENTED_EDGE('',*,*,#24817,.F.);
#37200=ORIENTED_EDGE('',*,*,#26874,.F.);
#37201=ORIENTED_EDGE('',*,*,#24824,.F.);
#37202=ORIENTED_EDGE('',*,*,#24716,.F.);
#37203=ORIENTED_EDGE('',*,*,#26873,.T.);
#37204=ORIENTED_EDGE('',*,*,#24703,.F.);
#37205=ORIENTED_EDGE('',*,*,#24809,.F.);
#37206=ORIENTED_EDGE('',*,*,#26875,.F.);
#37207=ORIENTED_EDGE('',*,*,#24705,.F.);
#37208=ORIENTED_EDGE('',*,*,#24697,.F.);
#37209=ORIENTED_EDGE('',*,*,#24694,.F.);
#37210=ORIENTED_EDGE('',*,*,#24806,.F.);
#37211=ORIENTED_EDGE('',*,*,#24814,.F.);
#37212=ORIENTED_EDGE('',*,*,#26876,.T.);
#37213=ORIENTED_EDGE('',*,*,#24803,.F.);
#37214=ORIENTED_EDGE('',*,*,#26876,.F.);
#37215=ORIENTED_EDGE('',*,*,#24810,.F.);
#37216=ORIENTED_EDGE('',*,*,#24702,.F.);
#37217=ORIENTED_EDGE('',*,*,#26875,.T.);
#37218=ORIENTED_EDGE('',*,*,#24689,.F.);
#37219=ORIENTED_EDGE('',*,*,#24795,.F.);
#37220=ORIENTED_EDGE('',*,*,#26877,.F.);
#37221=ORIENTED_EDGE('',*,*,#24691,.F.);
#37222=ORIENTED_EDGE('',*,*,#24683,.F.);
#37223=ORIENTED_EDGE('',*,*,#24680,.F.);
#37224=ORIENTED_EDGE('',*,*,#24792,.F.);
#37225=ORIENTED_EDGE('',*,*,#24800,.F.);
#37226=ORIENTED_EDGE('',*,*,#26878,.T.);
#37227=ORIENTED_EDGE('',*,*,#24789,.F.);
#37228=ORIENTED_EDGE('',*,*,#26878,.F.);
#37229=ORIENTED_EDGE('',*,*,#24796,.F.);
#37230=ORIENTED_EDGE('',*,*,#24688,.F.);
#37231=ORIENTED_EDGE('',*,*,#26877,.T.);
#37232=ORIENTED_EDGE('',*,*,#24674,.F.);
#37233=ORIENTED_EDGE('',*,*,#24781,.F.);
#37234=ORIENTED_EDGE('',*,*,#26879,.F.);
#37235=ORIENTED_EDGE('',*,*,#24676,.F.);
#37236=ORIENTED_EDGE('',*,*,#24668,.F.);
#37237=ORIENTED_EDGE('',*,*,#24665,.F.);
#37238=ORIENTED_EDGE('',*,*,#24778,.F.);
#37239=ORIENTED_EDGE('',*,*,#24786,.F.);
#37240=ORIENTED_EDGE('',*,*,#26880,.T.);
#37241=ORIENTED_EDGE('',*,*,#24775,.F.);
#37242=ORIENTED_EDGE('',*,*,#26880,.F.);
#37243=ORIENTED_EDGE('',*,*,#24782,.F.);
#37244=ORIENTED_EDGE('',*,*,#24673,.F.);
#37245=ORIENTED_EDGE('',*,*,#26879,.T.);
#37246=ORIENTED_EDGE('',*,*,#24662,.F.);
#37247=ORIENTED_EDGE('',*,*,#24766,.F.);
#37248=ORIENTED_EDGE('',*,*,#24755,.F.);
#37249=ORIENTED_EDGE('',*,*,#26881,.F.);
#37250=ORIENTED_EDGE('',*,*,#24767,.F.);
#37251=ORIENTED_EDGE('',*,*,#24661,.F.);
#37252=ORIENTED_EDGE('',*,*,#26882,.T.);
#37253=ORIENTED_EDGE('',*,*,#21352,.F.);
#37254=ORIENTED_EDGE('',*,*,#24763,.F.);
#37255=ORIENTED_EDGE('',*,*,#24771,.F.);
#37256=ORIENTED_EDGE('',*,*,#26881,.T.);
#37257=ORIENTED_EDGE('',*,*,#24760,.F.);
#37258=ORIENTED_EDGE('',*,*,#26882,.F.);
#37259=ORIENTED_EDGE('',*,*,#24773,.F.);
#37260=ORIENTED_EDGE('',*,*,#21353,.F.);
#37261=ORIENTED_EDGE('',*,*,#24653,.F.);
#37262=ORIENTED_EDGE('',*,*,#26883,.F.);
#37263=ORIENTED_EDGE('',*,*,#21497,.F.);
#37264=ORIENTED_EDGE('',*,*,#26883,.T.);
#37265=ORIENTED_EDGE('',*,*,#24649,.F.);
#37266=ORIENTED_EDGE('',*,*,#24750,.F.);
#37267=ORIENTED_EDGE('',*,*,#21498,.F.);
#37268=ORIENTED_EDGE('',*,*,#26884,.F.);
#37269=ORIENTED_EDGE('',*,*,#24651,.F.);
#37270=ORIENTED_EDGE('',*,*,#24643,.F.);
#37271=ORIENTED_EDGE('',*,*,#24640,.F.);
#37272=ORIENTED_EDGE('',*,*,#21501,.F.);
#37273=ORIENTED_EDGE('',*,*,#24753,.F.);
#37274=ORIENTED_EDGE('',*,*,#26885,.T.);
#37275=ORIENTED_EDGE('',*,*,#24748,.F.);
#37276=ORIENTED_EDGE('',*,*,#26885,.F.);
#37277=ORIENTED_EDGE('',*,*,#24751,.F.);
#37278=ORIENTED_EDGE('',*,*,#24648,.F.);
#37279=ORIENTED_EDGE('',*,*,#26884,.T.);
#37280=ORIENTED_EDGE('',*,*,#24635,.F.);
#37281=ORIENTED_EDGE('',*,*,#24741,.F.);
#37282=ORIENTED_EDGE('',*,*,#26886,.F.);
#37283=ORIENTED_EDGE('',*,*,#24637,.F.);
#37284=ORIENTED_EDGE('',*,*,#24629,.F.);
#37285=ORIENTED_EDGE('',*,*,#24626,.F.);
#37286=ORIENTED_EDGE('',*,*,#24738,.F.);
#37287=ORIENTED_EDGE('',*,*,#24746,.F.);
#37288=ORIENTED_EDGE('',*,*,#26887,.T.);
#37289=ORIENTED_EDGE('',*,*,#24735,.F.);
#37290=ORIENTED_EDGE('',*,*,#26887,.F.);
#37291=ORIENTED_EDGE('',*,*,#24742,.F.);
#37292=ORIENTED_EDGE('',*,*,#24634,.F.);
#37293=ORIENTED_EDGE('',*,*,#26886,.T.);
#37294=ORIENTED_EDGE('',*,*,#24621,.F.);
#37295=ORIENTED_EDGE('',*,*,#24727,.F.);
#37296=ORIENTED_EDGE('',*,*,#26888,.F.);
#37297=ORIENTED_EDGE('',*,*,#24623,.F.);
#37298=ORIENTED_EDGE('',*,*,#24615,.F.);
#37299=ORIENTED_EDGE('',*,*,#24612,.F.);
#37300=ORIENTED_EDGE('',*,*,#24724,.F.);
#37301=ORIENTED_EDGE('',*,*,#24732,.F.);
#37302=ORIENTED_EDGE('',*,*,#26889,.T.);
#37303=ORIENTED_EDGE('',*,*,#24721,.F.);
#37304=ORIENTED_EDGE('',*,*,#26889,.F.);
#37305=ORIENTED_EDGE('',*,*,#24728,.F.);
#37306=ORIENTED_EDGE('',*,*,#24620,.F.);
#37307=ORIENTED_EDGE('',*,*,#26888,.T.);
#37308=ORIENTED_EDGE('',*,*,#24607,.F.);
#37309=ORIENTED_EDGE('',*,*,#24713,.F.);
#37310=ORIENTED_EDGE('',*,*,#26890,.F.);
#37311=ORIENTED_EDGE('',*,*,#24609,.F.);
#37312=ORIENTED_EDGE('',*,*,#24601,.F.);
#37313=ORIENTED_EDGE('',*,*,#24598,.F.);
#37314=ORIENTED_EDGE('',*,*,#24710,.F.);
#37315=ORIENTED_EDGE('',*,*,#24718,.F.);
#37316=ORIENTED_EDGE('',*,*,#26891,.T.);
#37317=ORIENTED_EDGE('',*,*,#24707,.F.);
#37318=ORIENTED_EDGE('',*,*,#26891,.F.);
#37319=ORIENTED_EDGE('',*,*,#24714,.F.);
#37320=ORIENTED_EDGE('',*,*,#24606,.F.);
#37321=ORIENTED_EDGE('',*,*,#26890,.T.);
#37322=ORIENTED_EDGE('',*,*,#24593,.F.);
#37323=ORIENTED_EDGE('',*,*,#24699,.F.);
#37324=ORIENTED_EDGE('',*,*,#26892,.F.);
#37325=ORIENTED_EDGE('',*,*,#24595,.F.);
#37326=ORIENTED_EDGE('',*,*,#24587,.F.);
#37327=ORIENTED_EDGE('',*,*,#24584,.F.);
#37328=ORIENTED_EDGE('',*,*,#24696,.F.);
#37329=ORIENTED_EDGE('',*,*,#24704,.F.);
#37330=ORIENTED_EDGE('',*,*,#26893,.T.);
#37331=ORIENTED_EDGE('',*,*,#24693,.F.);
#37332=ORIENTED_EDGE('',*,*,#26893,.F.);
#37333=ORIENTED_EDGE('',*,*,#24700,.F.);
#37334=ORIENTED_EDGE('',*,*,#24592,.F.);
#37335=ORIENTED_EDGE('',*,*,#26892,.T.);
#37336=ORIENTED_EDGE('',*,*,#24578,.F.);
#37337=ORIENTED_EDGE('',*,*,#24685,.F.);
#37338=ORIENTED_EDGE('',*,*,#26894,.F.);
#37339=ORIENTED_EDGE('',*,*,#24580,.F.);
#37340=ORIENTED_EDGE('',*,*,#24572,.F.);
#37341=ORIENTED_EDGE('',*,*,#24569,.F.);
#37342=ORIENTED_EDGE('',*,*,#24682,.F.);
#37343=ORIENTED_EDGE('',*,*,#24690,.F.);
#37344=ORIENTED_EDGE('',*,*,#26895,.T.);
#37345=ORIENTED_EDGE('',*,*,#24679,.F.);
#37346=ORIENTED_EDGE('',*,*,#26895,.F.);
#37347=ORIENTED_EDGE('',*,*,#24686,.F.);
#37348=ORIENTED_EDGE('',*,*,#24577,.F.);
#37349=ORIENTED_EDGE('',*,*,#26894,.T.);
#37350=ORIENTED_EDGE('',*,*,#24566,.F.);
#37351=ORIENTED_EDGE('',*,*,#24670,.F.);
#37352=ORIENTED_EDGE('',*,*,#24659,.F.);
#37353=ORIENTED_EDGE('',*,*,#26896,.F.);
#37354=ORIENTED_EDGE('',*,*,#24671,.F.);
#37355=ORIENTED_EDGE('',*,*,#24565,.F.);
#37356=ORIENTED_EDGE('',*,*,#26897,.T.);
#37357=ORIENTED_EDGE('',*,*,#21356,.F.);
#37358=ORIENTED_EDGE('',*,*,#24667,.F.);
#37359=ORIENTED_EDGE('',*,*,#24675,.F.);
#37360=ORIENTED_EDGE('',*,*,#26896,.T.);
#37361=ORIENTED_EDGE('',*,*,#24664,.F.);
#37362=ORIENTED_EDGE('',*,*,#26897,.F.);
#37363=ORIENTED_EDGE('',*,*,#24677,.F.);
#37364=ORIENTED_EDGE('',*,*,#21357,.F.);
#37365=ORIENTED_EDGE('',*,*,#24557,.F.);
#37366=ORIENTED_EDGE('',*,*,#26898,.F.);
#37367=ORIENTED_EDGE('',*,*,#21491,.F.);
#37368=ORIENTED_EDGE('',*,*,#26898,.T.);
#37369=ORIENTED_EDGE('',*,*,#24553,.F.);
#37370=ORIENTED_EDGE('',*,*,#24654,.F.);
#37371=ORIENTED_EDGE('',*,*,#21492,.F.);
#37372=ORIENTED_EDGE('',*,*,#26899,.F.);
#37373=ORIENTED_EDGE('',*,*,#24555,.F.);
#37374=ORIENTED_EDGE('',*,*,#24547,.F.);
#37375=ORIENTED_EDGE('',*,*,#24544,.F.);
#37376=ORIENTED_EDGE('',*,*,#21495,.F.);
#37377=ORIENTED_EDGE('',*,*,#24657,.F.);
#37378=ORIENTED_EDGE('',*,*,#26900,.T.);
#37379=ORIENTED_EDGE('',*,*,#24652,.F.);
#37380=ORIENTED_EDGE('',*,*,#26900,.F.);
#37381=ORIENTED_EDGE('',*,*,#24655,.F.);
#37382=ORIENTED_EDGE('',*,*,#24552,.F.);
#37383=ORIENTED_EDGE('',*,*,#26899,.T.);
#37384=ORIENTED_EDGE('',*,*,#24539,.F.);
#37385=ORIENTED_EDGE('',*,*,#24645,.F.);
#37386=ORIENTED_EDGE('',*,*,#26901,.F.);
#37387=ORIENTED_EDGE('',*,*,#24541,.F.);
#37388=ORIENTED_EDGE('',*,*,#24533,.F.);
#37389=ORIENTED_EDGE('',*,*,#24530,.F.);
#37390=ORIENTED_EDGE('',*,*,#24642,.F.);
#37391=ORIENTED_EDGE('',*,*,#24650,.F.);
#37392=ORIENTED_EDGE('',*,*,#26902,.T.);
#37393=ORIENTED_EDGE('',*,*,#24639,.F.);
#37394=ORIENTED_EDGE('',*,*,#26902,.F.);
#37395=ORIENTED_EDGE('',*,*,#24646,.F.);
#37396=ORIENTED_EDGE('',*,*,#24538,.F.);
#37397=ORIENTED_EDGE('',*,*,#26901,.T.);
#37398=ORIENTED_EDGE('',*,*,#24525,.F.);
#37399=ORIENTED_EDGE('',*,*,#24631,.F.);
#37400=ORIENTED_EDGE('',*,*,#26903,.F.);
#37401=ORIENTED_EDGE('',*,*,#24527,.F.);
#37402=ORIENTED_EDGE('',*,*,#24519,.F.);
#37403=ORIENTED_EDGE('',*,*,#24516,.F.);
#37404=ORIENTED_EDGE('',*,*,#24628,.F.);
#37405=ORIENTED_EDGE('',*,*,#24636,.F.);
#37406=ORIENTED_EDGE('',*,*,#26904,.T.);
#37407=ORIENTED_EDGE('',*,*,#24625,.F.);
#37408=ORIENTED_EDGE('',*,*,#26904,.F.);
#37409=ORIENTED_EDGE('',*,*,#24632,.F.);
#37410=ORIENTED_EDGE('',*,*,#24524,.F.);
#37411=ORIENTED_EDGE('',*,*,#26903,.T.);
#37412=ORIENTED_EDGE('',*,*,#24511,.F.);
#37413=ORIENTED_EDGE('',*,*,#24617,.F.);
#37414=ORIENTED_EDGE('',*,*,#26905,.F.);
#37415=ORIENTED_EDGE('',*,*,#24513,.F.);
#37416=ORIENTED_EDGE('',*,*,#24505,.F.);
#37417=ORIENTED_EDGE('',*,*,#24502,.F.);
#37418=ORIENTED_EDGE('',*,*,#24614,.F.);
#37419=ORIENTED_EDGE('',*,*,#24622,.F.);
#37420=ORIENTED_EDGE('',*,*,#26906,.T.);
#37421=ORIENTED_EDGE('',*,*,#24611,.F.);
#37422=ORIENTED_EDGE('',*,*,#26906,.F.);
#37423=ORIENTED_EDGE('',*,*,#24618,.F.);
#37424=ORIENTED_EDGE('',*,*,#24510,.F.);
#37425=ORIENTED_EDGE('',*,*,#26905,.T.);
#37426=ORIENTED_EDGE('',*,*,#24497,.F.);
#37427=ORIENTED_EDGE('',*,*,#24603,.F.);
#37428=ORIENTED_EDGE('',*,*,#26907,.F.);
#37429=ORIENTED_EDGE('',*,*,#24499,.F.);
#37430=ORIENTED_EDGE('',*,*,#24491,.F.);
#37431=ORIENTED_EDGE('',*,*,#24488,.F.);
#37432=ORIENTED_EDGE('',*,*,#24600,.F.);
#37433=ORIENTED_EDGE('',*,*,#24608,.F.);
#37434=ORIENTED_EDGE('',*,*,#26908,.T.);
#37435=ORIENTED_EDGE('',*,*,#24597,.F.);
#37436=ORIENTED_EDGE('',*,*,#26908,.F.);
#37437=ORIENTED_EDGE('',*,*,#24604,.F.);
#37438=ORIENTED_EDGE('',*,*,#24496,.F.);
#37439=ORIENTED_EDGE('',*,*,#26907,.T.);
#37440=ORIENTED_EDGE('',*,*,#24482,.F.);
#37441=ORIENTED_EDGE('',*,*,#24589,.F.);
#37442=ORIENTED_EDGE('',*,*,#26909,.F.);
#37443=ORIENTED_EDGE('',*,*,#24484,.F.);
#37444=ORIENTED_EDGE('',*,*,#24476,.F.);
#37445=ORIENTED_EDGE('',*,*,#24473,.F.);
#37446=ORIENTED_EDGE('',*,*,#24586,.F.);
#37447=ORIENTED_EDGE('',*,*,#24594,.F.);
#37448=ORIENTED_EDGE('',*,*,#26910,.T.);
#37449=ORIENTED_EDGE('',*,*,#24583,.F.);
#37450=ORIENTED_EDGE('',*,*,#26910,.F.);
#37451=ORIENTED_EDGE('',*,*,#24590,.F.);
#37452=ORIENTED_EDGE('',*,*,#24481,.F.);
#37453=ORIENTED_EDGE('',*,*,#26909,.T.);
#37454=ORIENTED_EDGE('',*,*,#24470,.F.);
#37455=ORIENTED_EDGE('',*,*,#24574,.F.);
#37456=ORIENTED_EDGE('',*,*,#24563,.F.);
#37457=ORIENTED_EDGE('',*,*,#26911,.F.);
#37458=ORIENTED_EDGE('',*,*,#24575,.F.);
#37459=ORIENTED_EDGE('',*,*,#24469,.F.);
#37460=ORIENTED_EDGE('',*,*,#26912,.T.);
#37461=ORIENTED_EDGE('',*,*,#21360,.F.);
#37462=ORIENTED_EDGE('',*,*,#24571,.F.);
#37463=ORIENTED_EDGE('',*,*,#24579,.F.);
#37464=ORIENTED_EDGE('',*,*,#26911,.T.);
#37465=ORIENTED_EDGE('',*,*,#24568,.F.);
#37466=ORIENTED_EDGE('',*,*,#26912,.F.);
#37467=ORIENTED_EDGE('',*,*,#24581,.F.);
#37468=ORIENTED_EDGE('',*,*,#21361,.F.);
#37469=ORIENTED_EDGE('',*,*,#24461,.F.);
#37470=ORIENTED_EDGE('',*,*,#26913,.F.);
#37471=ORIENTED_EDGE('',*,*,#21485,.F.);
#37472=ORIENTED_EDGE('',*,*,#26913,.T.);
#37473=ORIENTED_EDGE('',*,*,#24457,.F.);
#37474=ORIENTED_EDGE('',*,*,#24558,.F.);
#37475=ORIENTED_EDGE('',*,*,#21486,.F.);
#37476=ORIENTED_EDGE('',*,*,#26914,.F.);
#37477=ORIENTED_EDGE('',*,*,#24459,.F.);
#37478=ORIENTED_EDGE('',*,*,#24451,.F.);
#37479=ORIENTED_EDGE('',*,*,#24448,.F.);
#37480=ORIENTED_EDGE('',*,*,#21489,.F.);
#37481=ORIENTED_EDGE('',*,*,#24561,.F.);
#37482=ORIENTED_EDGE('',*,*,#26915,.T.);
#37483=ORIENTED_EDGE('',*,*,#24556,.F.);
#37484=ORIENTED_EDGE('',*,*,#26915,.F.);
#37485=ORIENTED_EDGE('',*,*,#24559,.F.);
#37486=ORIENTED_EDGE('',*,*,#24456,.F.);
#37487=ORIENTED_EDGE('',*,*,#26914,.T.);
#37488=ORIENTED_EDGE('',*,*,#24443,.F.);
#37489=ORIENTED_EDGE('',*,*,#24549,.F.);
#37490=ORIENTED_EDGE('',*,*,#26916,.F.);
#37491=ORIENTED_EDGE('',*,*,#24445,.F.);
#37492=ORIENTED_EDGE('',*,*,#24437,.F.);
#37493=ORIENTED_EDGE('',*,*,#24434,.F.);
#37494=ORIENTED_EDGE('',*,*,#24546,.F.);
#37495=ORIENTED_EDGE('',*,*,#24554,.F.);
#37496=ORIENTED_EDGE('',*,*,#26917,.T.);
#37497=ORIENTED_EDGE('',*,*,#24543,.F.);
#37498=ORIENTED_EDGE('',*,*,#26917,.F.);
#37499=ORIENTED_EDGE('',*,*,#24550,.F.);
#37500=ORIENTED_EDGE('',*,*,#24442,.F.);
#37501=ORIENTED_EDGE('',*,*,#26916,.T.);
#37502=ORIENTED_EDGE('',*,*,#24429,.F.);
#37503=ORIENTED_EDGE('',*,*,#24535,.F.);
#37504=ORIENTED_EDGE('',*,*,#26918,.F.);
#37505=ORIENTED_EDGE('',*,*,#24431,.F.);
#37506=ORIENTED_EDGE('',*,*,#24423,.F.);
#37507=ORIENTED_EDGE('',*,*,#24420,.F.);
#37508=ORIENTED_EDGE('',*,*,#24532,.F.);
#37509=ORIENTED_EDGE('',*,*,#24540,.F.);
#37510=ORIENTED_EDGE('',*,*,#26919,.T.);
#37511=ORIENTED_EDGE('',*,*,#24529,.F.);
#37512=ORIENTED_EDGE('',*,*,#26919,.F.);
#37513=ORIENTED_EDGE('',*,*,#24536,.F.);
#37514=ORIENTED_EDGE('',*,*,#24428,.F.);
#37515=ORIENTED_EDGE('',*,*,#26918,.T.);
#37516=ORIENTED_EDGE('',*,*,#24415,.F.);
#37517=ORIENTED_EDGE('',*,*,#24521,.F.);
#37518=ORIENTED_EDGE('',*,*,#26920,.F.);
#37519=ORIENTED_EDGE('',*,*,#24417,.F.);
#37520=ORIENTED_EDGE('',*,*,#24409,.F.);
#37521=ORIENTED_EDGE('',*,*,#24406,.F.);
#37522=ORIENTED_EDGE('',*,*,#24518,.F.);
#37523=ORIENTED_EDGE('',*,*,#24526,.F.);
#37524=ORIENTED_EDGE('',*,*,#26921,.T.);
#37525=ORIENTED_EDGE('',*,*,#24515,.F.);
#37526=ORIENTED_EDGE('',*,*,#26921,.F.);
#37527=ORIENTED_EDGE('',*,*,#24522,.F.);
#37528=ORIENTED_EDGE('',*,*,#24414,.F.);
#37529=ORIENTED_EDGE('',*,*,#26920,.T.);
#37530=ORIENTED_EDGE('',*,*,#24401,.F.);
#37531=ORIENTED_EDGE('',*,*,#24507,.F.);
#37532=ORIENTED_EDGE('',*,*,#26922,.F.);
#37533=ORIENTED_EDGE('',*,*,#24403,.F.);
#37534=ORIENTED_EDGE('',*,*,#24395,.F.);
#37535=ORIENTED_EDGE('',*,*,#24392,.F.);
#37536=ORIENTED_EDGE('',*,*,#24504,.F.);
#37537=ORIENTED_EDGE('',*,*,#24512,.F.);
#37538=ORIENTED_EDGE('',*,*,#26923,.T.);
#37539=ORIENTED_EDGE('',*,*,#24501,.F.);
#37540=ORIENTED_EDGE('',*,*,#26923,.F.);
#37541=ORIENTED_EDGE('',*,*,#24508,.F.);
#37542=ORIENTED_EDGE('',*,*,#24400,.F.);
#37543=ORIENTED_EDGE('',*,*,#26922,.T.);
#37544=ORIENTED_EDGE('',*,*,#24386,.F.);
#37545=ORIENTED_EDGE('',*,*,#24493,.F.);
#37546=ORIENTED_EDGE('',*,*,#26924,.F.);
#37547=ORIENTED_EDGE('',*,*,#24388,.F.);
#37548=ORIENTED_EDGE('',*,*,#24380,.F.);
#37549=ORIENTED_EDGE('',*,*,#24377,.F.);
#37550=ORIENTED_EDGE('',*,*,#24490,.F.);
#37551=ORIENTED_EDGE('',*,*,#24498,.F.);
#37552=ORIENTED_EDGE('',*,*,#26925,.T.);
#37553=ORIENTED_EDGE('',*,*,#24487,.F.);
#37554=ORIENTED_EDGE('',*,*,#26925,.F.);
#37555=ORIENTED_EDGE('',*,*,#24494,.F.);
#37556=ORIENTED_EDGE('',*,*,#24385,.F.);
#37557=ORIENTED_EDGE('',*,*,#26924,.T.);
#37558=ORIENTED_EDGE('',*,*,#24374,.F.);
#37559=ORIENTED_EDGE('',*,*,#24478,.F.);
#37560=ORIENTED_EDGE('',*,*,#24467,.F.);
#37561=ORIENTED_EDGE('',*,*,#26926,.F.);
#37562=ORIENTED_EDGE('',*,*,#24479,.F.);
#37563=ORIENTED_EDGE('',*,*,#24373,.F.);
#37564=ORIENTED_EDGE('',*,*,#26927,.T.);
#37565=ORIENTED_EDGE('',*,*,#21364,.F.);
#37566=ORIENTED_EDGE('',*,*,#24475,.F.);
#37567=ORIENTED_EDGE('',*,*,#24483,.F.);
#37568=ORIENTED_EDGE('',*,*,#26926,.T.);
#37569=ORIENTED_EDGE('',*,*,#24472,.F.);
#37570=ORIENTED_EDGE('',*,*,#26927,.F.);
#37571=ORIENTED_EDGE('',*,*,#24485,.F.);
#37572=ORIENTED_EDGE('',*,*,#21365,.F.);
#37573=ORIENTED_EDGE('',*,*,#24365,.F.);
#37574=ORIENTED_EDGE('',*,*,#26928,.F.);
#37575=ORIENTED_EDGE('',*,*,#21779,.F.);
#37576=ORIENTED_EDGE('',*,*,#26928,.T.);
#37577=ORIENTED_EDGE('',*,*,#24361,.F.);
#37578=ORIENTED_EDGE('',*,*,#24462,.F.);
#37579=ORIENTED_EDGE('',*,*,#21780,.F.);
#37580=ORIENTED_EDGE('',*,*,#26929,.F.);
#37581=ORIENTED_EDGE('',*,*,#24363,.F.);
#37582=ORIENTED_EDGE('',*,*,#24355,.F.);
#37583=ORIENTED_EDGE('',*,*,#24352,.F.);
#37584=ORIENTED_EDGE('',*,*,#21480,.F.);
#37585=ORIENTED_EDGE('',*,*,#24465,.F.);
#37586=ORIENTED_EDGE('',*,*,#26930,.T.);
#37587=ORIENTED_EDGE('',*,*,#24460,.F.);
#37588=ORIENTED_EDGE('',*,*,#21483,.F.);
#37589=ORIENTED_EDGE('',*,*,#26930,.F.);
#37590=ORIENTED_EDGE('',*,*,#24463,.F.);
#37591=ORIENTED_EDGE('',*,*,#24360,.F.);
#37592=ORIENTED_EDGE('',*,*,#26929,.T.);
#37593=ORIENTED_EDGE('',*,*,#24347,.F.);
#37594=ORIENTED_EDGE('',*,*,#24453,.F.);
#37595=ORIENTED_EDGE('',*,*,#26931,.F.);
#37596=ORIENTED_EDGE('',*,*,#24349,.F.);
#37597=ORIENTED_EDGE('',*,*,#24341,.F.);
#37598=ORIENTED_EDGE('',*,*,#24338,.F.);
#37599=ORIENTED_EDGE('',*,*,#24450,.F.);
#37600=ORIENTED_EDGE('',*,*,#24458,.F.);
#37601=ORIENTED_EDGE('',*,*,#26932,.T.);
#37602=ORIENTED_EDGE('',*,*,#24447,.F.);
#37603=ORIENTED_EDGE('',*,*,#26932,.F.);
#37604=ORIENTED_EDGE('',*,*,#24454,.F.);
#37605=ORIENTED_EDGE('',*,*,#24346,.F.);
#37606=ORIENTED_EDGE('',*,*,#26931,.T.);
#37607=ORIENTED_EDGE('',*,*,#24333,.F.);
#37608=ORIENTED_EDGE('',*,*,#24439,.F.);
#37609=ORIENTED_EDGE('',*,*,#26933,.F.);
#37610=ORIENTED_EDGE('',*,*,#24335,.F.);
#37611=ORIENTED_EDGE('',*,*,#24327,.F.);
#37612=ORIENTED_EDGE('',*,*,#24324,.F.);
#37613=ORIENTED_EDGE('',*,*,#24436,.F.);
#37614=ORIENTED_EDGE('',*,*,#24444,.F.);
#37615=ORIENTED_EDGE('',*,*,#26934,.T.);
#37616=ORIENTED_EDGE('',*,*,#24433,.F.);
#37617=ORIENTED_EDGE('',*,*,#26934,.F.);
#37618=ORIENTED_EDGE('',*,*,#24440,.F.);
#37619=ORIENTED_EDGE('',*,*,#24332,.F.);
#37620=ORIENTED_EDGE('',*,*,#26933,.T.);
#37621=ORIENTED_EDGE('',*,*,#24319,.F.);
#37622=ORIENTED_EDGE('',*,*,#24425,.F.);
#37623=ORIENTED_EDGE('',*,*,#26935,.F.);
#37624=ORIENTED_EDGE('',*,*,#24321,.F.);
#37625=ORIENTED_EDGE('',*,*,#24313,.F.);
#37626=ORIENTED_EDGE('',*,*,#24310,.F.);
#37627=ORIENTED_EDGE('',*,*,#24422,.F.);
#37628=ORIENTED_EDGE('',*,*,#24430,.F.);
#37629=ORIENTED_EDGE('',*,*,#26936,.T.);
#37630=ORIENTED_EDGE('',*,*,#24419,.F.);
#37631=ORIENTED_EDGE('',*,*,#26936,.F.);
#37632=ORIENTED_EDGE('',*,*,#24426,.F.);
#37633=ORIENTED_EDGE('',*,*,#24318,.F.);
#37634=ORIENTED_EDGE('',*,*,#26935,.T.);
#37635=ORIENTED_EDGE('',*,*,#24305,.F.);
#37636=ORIENTED_EDGE('',*,*,#24411,.F.);
#37637=ORIENTED_EDGE('',*,*,#26937,.F.);
#37638=ORIENTED_EDGE('',*,*,#24307,.F.);
#37639=ORIENTED_EDGE('',*,*,#24299,.F.);
#37640=ORIENTED_EDGE('',*,*,#24296,.F.);
#37641=ORIENTED_EDGE('',*,*,#24408,.F.);
#37642=ORIENTED_EDGE('',*,*,#24416,.F.);
#37643=ORIENTED_EDGE('',*,*,#26938,.T.);
#37644=ORIENTED_EDGE('',*,*,#24405,.F.);
#37645=ORIENTED_EDGE('',*,*,#26938,.F.);
#37646=ORIENTED_EDGE('',*,*,#24412,.F.);
#37647=ORIENTED_EDGE('',*,*,#24304,.F.);
#37648=ORIENTED_EDGE('',*,*,#26937,.T.);
#37649=ORIENTED_EDGE('',*,*,#24290,.F.);
#37650=ORIENTED_EDGE('',*,*,#24397,.F.);
#37651=ORIENTED_EDGE('',*,*,#26939,.F.);
#37652=ORIENTED_EDGE('',*,*,#24292,.F.);
#37653=ORIENTED_EDGE('',*,*,#24284,.F.);
#37654=ORIENTED_EDGE('',*,*,#24281,.F.);
#37655=ORIENTED_EDGE('',*,*,#24394,.F.);
#37656=ORIENTED_EDGE('',*,*,#24402,.F.);
#37657=ORIENTED_EDGE('',*,*,#26940,.T.);
#37658=ORIENTED_EDGE('',*,*,#24391,.F.);
#37659=ORIENTED_EDGE('',*,*,#26940,.F.);
#37660=ORIENTED_EDGE('',*,*,#24398,.F.);
#37661=ORIENTED_EDGE('',*,*,#24289,.F.);
#37662=ORIENTED_EDGE('',*,*,#26939,.T.);
#37663=ORIENTED_EDGE('',*,*,#24278,.F.);
#37664=ORIENTED_EDGE('',*,*,#24382,.F.);
#37665=ORIENTED_EDGE('',*,*,#24371,.F.);
#37666=ORIENTED_EDGE('',*,*,#26941,.F.);
#37667=ORIENTED_EDGE('',*,*,#24383,.F.);
#37668=ORIENTED_EDGE('',*,*,#24277,.F.);
#37669=ORIENTED_EDGE('',*,*,#26942,.T.);
#37670=ORIENTED_EDGE('',*,*,#21368,.F.);
#37671=ORIENTED_EDGE('',*,*,#24379,.F.);
#37672=ORIENTED_EDGE('',*,*,#24387,.F.);
#37673=ORIENTED_EDGE('',*,*,#26941,.T.);
#37674=ORIENTED_EDGE('',*,*,#24376,.F.);
#37675=ORIENTED_EDGE('',*,*,#26942,.F.);
#37676=ORIENTED_EDGE('',*,*,#24389,.F.);
#37677=ORIENTED_EDGE('',*,*,#21369,.F.);
#37678=ORIENTED_EDGE('',*,*,#24269,.F.);
#37679=ORIENTED_EDGE('',*,*,#26943,.F.);
#37680=ORIENTED_EDGE('',*,*,#21773,.F.);
#37681=ORIENTED_EDGE('',*,*,#26943,.T.);
#37682=ORIENTED_EDGE('',*,*,#24265,.F.);
#37683=ORIENTED_EDGE('',*,*,#24366,.F.);
#37684=ORIENTED_EDGE('',*,*,#21774,.F.);
#37685=ORIENTED_EDGE('',*,*,#26944,.F.);
#37686=ORIENTED_EDGE('',*,*,#24267,.F.);
#37687=ORIENTED_EDGE('',*,*,#24259,.F.);
#37688=ORIENTED_EDGE('',*,*,#24256,.F.);
#37689=ORIENTED_EDGE('',*,*,#21777,.F.);
#37690=ORIENTED_EDGE('',*,*,#24369,.F.);
#37691=ORIENTED_EDGE('',*,*,#26945,.T.);
#37692=ORIENTED_EDGE('',*,*,#24364,.F.);
#37693=ORIENTED_EDGE('',*,*,#26945,.F.);
#37694=ORIENTED_EDGE('',*,*,#24367,.F.);
#37695=ORIENTED_EDGE('',*,*,#24264,.F.);
#37696=ORIENTED_EDGE('',*,*,#26944,.T.);
#37697=ORIENTED_EDGE('',*,*,#24251,.F.);
#37698=ORIENTED_EDGE('',*,*,#24357,.F.);
#37699=ORIENTED_EDGE('',*,*,#26946,.F.);
#37700=ORIENTED_EDGE('',*,*,#24253,.F.);
#37701=ORIENTED_EDGE('',*,*,#24245,.F.);
#37702=ORIENTED_EDGE('',*,*,#24242,.F.);
#37703=ORIENTED_EDGE('',*,*,#24354,.F.);
#37704=ORIENTED_EDGE('',*,*,#24362,.F.);
#37705=ORIENTED_EDGE('',*,*,#26947,.T.);
#37706=ORIENTED_EDGE('',*,*,#24351,.F.);
#37707=ORIENTED_EDGE('',*,*,#26947,.F.);
#37708=ORIENTED_EDGE('',*,*,#24358,.F.);
#37709=ORIENTED_EDGE('',*,*,#24250,.F.);
#37710=ORIENTED_EDGE('',*,*,#26946,.T.);
#37711=ORIENTED_EDGE('',*,*,#24237,.F.);
#37712=ORIENTED_EDGE('',*,*,#24343,.F.);
#37713=ORIENTED_EDGE('',*,*,#26948,.F.);
#37714=ORIENTED_EDGE('',*,*,#24239,.F.);
#37715=ORIENTED_EDGE('',*,*,#24231,.F.);
#37716=ORIENTED_EDGE('',*,*,#24228,.F.);
#37717=ORIENTED_EDGE('',*,*,#24340,.F.);
#37718=ORIENTED_EDGE('',*,*,#24348,.F.);
#37719=ORIENTED_EDGE('',*,*,#26949,.T.);
#37720=ORIENTED_EDGE('',*,*,#24337,.F.);
#37721=ORIENTED_EDGE('',*,*,#26949,.F.);
#37722=ORIENTED_EDGE('',*,*,#24344,.F.);
#37723=ORIENTED_EDGE('',*,*,#24236,.F.);
#37724=ORIENTED_EDGE('',*,*,#26948,.T.);
#37725=ORIENTED_EDGE('',*,*,#24223,.F.);
#37726=ORIENTED_EDGE('',*,*,#24329,.F.);
#37727=ORIENTED_EDGE('',*,*,#26950,.F.);
#37728=ORIENTED_EDGE('',*,*,#24225,.F.);
#37729=ORIENTED_EDGE('',*,*,#24217,.F.);
#37730=ORIENTED_EDGE('',*,*,#24214,.F.);
#37731=ORIENTED_EDGE('',*,*,#24326,.F.);
#37732=ORIENTED_EDGE('',*,*,#24334,.F.);
#37733=ORIENTED_EDGE('',*,*,#26951,.T.);
#37734=ORIENTED_EDGE('',*,*,#24323,.F.);
#37735=ORIENTED_EDGE('',*,*,#26951,.F.);
#37736=ORIENTED_EDGE('',*,*,#24330,.F.);
#37737=ORIENTED_EDGE('',*,*,#24222,.F.);
#37738=ORIENTED_EDGE('',*,*,#26950,.T.);
#37739=ORIENTED_EDGE('',*,*,#24209,.F.);
#37740=ORIENTED_EDGE('',*,*,#24315,.F.);
#37741=ORIENTED_EDGE('',*,*,#26952,.F.);
#37742=ORIENTED_EDGE('',*,*,#24211,.F.);
#37743=ORIENTED_EDGE('',*,*,#24203,.F.);
#37744=ORIENTED_EDGE('',*,*,#24200,.F.);
#37745=ORIENTED_EDGE('',*,*,#24312,.F.);
#37746=ORIENTED_EDGE('',*,*,#24320,.F.);
#37747=ORIENTED_EDGE('',*,*,#26953,.T.);
#37748=ORIENTED_EDGE('',*,*,#24309,.F.);
#37749=ORIENTED_EDGE('',*,*,#26953,.F.);
#37750=ORIENTED_EDGE('',*,*,#24316,.F.);
#37751=ORIENTED_EDGE('',*,*,#24208,.F.);
#37752=ORIENTED_EDGE('',*,*,#26952,.T.);
#37753=ORIENTED_EDGE('',*,*,#24194,.F.);
#37754=ORIENTED_EDGE('',*,*,#24301,.F.);
#37755=ORIENTED_EDGE('',*,*,#26954,.F.);
#37756=ORIENTED_EDGE('',*,*,#24196,.F.);
#37757=ORIENTED_EDGE('',*,*,#24188,.F.);
#37758=ORIENTED_EDGE('',*,*,#24185,.F.);
#37759=ORIENTED_EDGE('',*,*,#24298,.F.);
#37760=ORIENTED_EDGE('',*,*,#24306,.F.);
#37761=ORIENTED_EDGE('',*,*,#26955,.T.);
#37762=ORIENTED_EDGE('',*,*,#24295,.F.);
#37763=ORIENTED_EDGE('',*,*,#26955,.F.);
#37764=ORIENTED_EDGE('',*,*,#24302,.F.);
#37765=ORIENTED_EDGE('',*,*,#24193,.F.);
#37766=ORIENTED_EDGE('',*,*,#26954,.T.);
#37767=ORIENTED_EDGE('',*,*,#24182,.F.);
#37768=ORIENTED_EDGE('',*,*,#24286,.F.);
#37769=ORIENTED_EDGE('',*,*,#24275,.F.);
#37770=ORIENTED_EDGE('',*,*,#26956,.F.);
#37771=ORIENTED_EDGE('',*,*,#24287,.F.);
#37772=ORIENTED_EDGE('',*,*,#24181,.F.);
#37773=ORIENTED_EDGE('',*,*,#26957,.T.);
#37774=ORIENTED_EDGE('',*,*,#21372,.F.);
#37775=ORIENTED_EDGE('',*,*,#24283,.F.);
#37776=ORIENTED_EDGE('',*,*,#24291,.F.);
#37777=ORIENTED_EDGE('',*,*,#26956,.T.);
#37778=ORIENTED_EDGE('',*,*,#24280,.F.);
#37779=ORIENTED_EDGE('',*,*,#26957,.F.);
#37780=ORIENTED_EDGE('',*,*,#24293,.F.);
#37781=ORIENTED_EDGE('',*,*,#21373,.F.);
#37782=ORIENTED_EDGE('',*,*,#24173,.F.);
#37783=ORIENTED_EDGE('',*,*,#26958,.F.);
#37784=ORIENTED_EDGE('',*,*,#21767,.F.);
#37785=ORIENTED_EDGE('',*,*,#26958,.T.);
#37786=ORIENTED_EDGE('',*,*,#24169,.F.);
#37787=ORIENTED_EDGE('',*,*,#24270,.F.);
#37788=ORIENTED_EDGE('',*,*,#21768,.F.);
#37789=ORIENTED_EDGE('',*,*,#26959,.F.);
#37790=ORIENTED_EDGE('',*,*,#24171,.F.);
#37791=ORIENTED_EDGE('',*,*,#24163,.F.);
#37792=ORIENTED_EDGE('',*,*,#24160,.F.);
#37793=ORIENTED_EDGE('',*,*,#21771,.F.);
#37794=ORIENTED_EDGE('',*,*,#24273,.F.);
#37795=ORIENTED_EDGE('',*,*,#26960,.T.);
#37796=ORIENTED_EDGE('',*,*,#24268,.F.);
#37797=ORIENTED_EDGE('',*,*,#26960,.F.);
#37798=ORIENTED_EDGE('',*,*,#24271,.F.);
#37799=ORIENTED_EDGE('',*,*,#24168,.F.);
#37800=ORIENTED_EDGE('',*,*,#26959,.T.);
#37801=ORIENTED_EDGE('',*,*,#24155,.F.);
#37802=ORIENTED_EDGE('',*,*,#24261,.F.);
#37803=ORIENTED_EDGE('',*,*,#26961,.F.);
#37804=ORIENTED_EDGE('',*,*,#24157,.F.);
#37805=ORIENTED_EDGE('',*,*,#24149,.F.);
#37806=ORIENTED_EDGE('',*,*,#24146,.F.);
#37807=ORIENTED_EDGE('',*,*,#24258,.F.);
#37808=ORIENTED_EDGE('',*,*,#24266,.F.);
#37809=ORIENTED_EDGE('',*,*,#26962,.T.);
#37810=ORIENTED_EDGE('',*,*,#24255,.F.);
#37811=ORIENTED_EDGE('',*,*,#26962,.F.);
#37812=ORIENTED_EDGE('',*,*,#24262,.F.);
#37813=ORIENTED_EDGE('',*,*,#24154,.F.);
#37814=ORIENTED_EDGE('',*,*,#26961,.T.);
#37815=ORIENTED_EDGE('',*,*,#24141,.F.);
#37816=ORIENTED_EDGE('',*,*,#24247,.F.);
#37817=ORIENTED_EDGE('',*,*,#26963,.F.);
#37818=ORIENTED_EDGE('',*,*,#24143,.F.);
#37819=ORIENTED_EDGE('',*,*,#24135,.F.);
#37820=ORIENTED_EDGE('',*,*,#24132,.F.);
#37821=ORIENTED_EDGE('',*,*,#24244,.F.);
#37822=ORIENTED_EDGE('',*,*,#24252,.F.);
#37823=ORIENTED_EDGE('',*,*,#26964,.T.);
#37824=ORIENTED_EDGE('',*,*,#24241,.F.);
#37825=ORIENTED_EDGE('',*,*,#26964,.F.);
#37826=ORIENTED_EDGE('',*,*,#24248,.F.);
#37827=ORIENTED_EDGE('',*,*,#24140,.F.);
#37828=ORIENTED_EDGE('',*,*,#26963,.T.);
#37829=ORIENTED_EDGE('',*,*,#24127,.F.);
#37830=ORIENTED_EDGE('',*,*,#24233,.F.);
#37831=ORIENTED_EDGE('',*,*,#26965,.F.);
#37832=ORIENTED_EDGE('',*,*,#24129,.F.);
#37833=ORIENTED_EDGE('',*,*,#24121,.F.);
#37834=ORIENTED_EDGE('',*,*,#24118,.F.);
#37835=ORIENTED_EDGE('',*,*,#24230,.F.);
#37836=ORIENTED_EDGE('',*,*,#24238,.F.);
#37837=ORIENTED_EDGE('',*,*,#26966,.T.);
#37838=ORIENTED_EDGE('',*,*,#24227,.F.);
#37839=ORIENTED_EDGE('',*,*,#26966,.F.);
#37840=ORIENTED_EDGE('',*,*,#24234,.F.);
#37841=ORIENTED_EDGE('',*,*,#24126,.F.);
#37842=ORIENTED_EDGE('',*,*,#26965,.T.);
#37843=ORIENTED_EDGE('',*,*,#24113,.F.);
#37844=ORIENTED_EDGE('',*,*,#24219,.F.);
#37845=ORIENTED_EDGE('',*,*,#26967,.F.);
#37846=ORIENTED_EDGE('',*,*,#24115,.F.);
#37847=ORIENTED_EDGE('',*,*,#24107,.F.);
#37848=ORIENTED_EDGE('',*,*,#24104,.F.);
#37849=ORIENTED_EDGE('',*,*,#24216,.F.);
#37850=ORIENTED_EDGE('',*,*,#24224,.F.);
#37851=ORIENTED_EDGE('',*,*,#26968,.T.);
#37852=ORIENTED_EDGE('',*,*,#24213,.F.);
#37853=ORIENTED_EDGE('',*,*,#26968,.F.);
#37854=ORIENTED_EDGE('',*,*,#24220,.F.);
#37855=ORIENTED_EDGE('',*,*,#24112,.F.);
#37856=ORIENTED_EDGE('',*,*,#26967,.T.);
#37857=ORIENTED_EDGE('',*,*,#24098,.F.);
#37858=ORIENTED_EDGE('',*,*,#24205,.F.);
#37859=ORIENTED_EDGE('',*,*,#26969,.F.);
#37860=ORIENTED_EDGE('',*,*,#24100,.F.);
#37861=ORIENTED_EDGE('',*,*,#24092,.F.);
#37862=ORIENTED_EDGE('',*,*,#24089,.F.);
#37863=ORIENTED_EDGE('',*,*,#24202,.F.);
#37864=ORIENTED_EDGE('',*,*,#24210,.F.);
#37865=ORIENTED_EDGE('',*,*,#26970,.T.);
#37866=ORIENTED_EDGE('',*,*,#24199,.F.);
#37867=ORIENTED_EDGE('',*,*,#26970,.F.);
#37868=ORIENTED_EDGE('',*,*,#24206,.F.);
#37869=ORIENTED_EDGE('',*,*,#24097,.F.);
#37870=ORIENTED_EDGE('',*,*,#26969,.T.);
#37871=ORIENTED_EDGE('',*,*,#24086,.F.);
#37872=ORIENTED_EDGE('',*,*,#24190,.F.);
#37873=ORIENTED_EDGE('',*,*,#24179,.F.);
#37874=ORIENTED_EDGE('',*,*,#26971,.F.);
#37875=ORIENTED_EDGE('',*,*,#24191,.F.);
#37876=ORIENTED_EDGE('',*,*,#24085,.F.);
#37877=ORIENTED_EDGE('',*,*,#26972,.T.);
#37878=ORIENTED_EDGE('',*,*,#21376,.F.);
#37879=ORIENTED_EDGE('',*,*,#24187,.F.);
#37880=ORIENTED_EDGE('',*,*,#24195,.F.);
#37881=ORIENTED_EDGE('',*,*,#26971,.T.);
#37882=ORIENTED_EDGE('',*,*,#24184,.F.);
#37883=ORIENTED_EDGE('',*,*,#26972,.F.);
#37884=ORIENTED_EDGE('',*,*,#24197,.F.);
#37885=ORIENTED_EDGE('',*,*,#21377,.F.);
#37886=ORIENTED_EDGE('',*,*,#24077,.F.);
#37887=ORIENTED_EDGE('',*,*,#26973,.F.);
#37888=ORIENTED_EDGE('',*,*,#21761,.F.);
#37889=ORIENTED_EDGE('',*,*,#26973,.T.);
#37890=ORIENTED_EDGE('',*,*,#24073,.F.);
#37891=ORIENTED_EDGE('',*,*,#24174,.F.);
#37892=ORIENTED_EDGE('',*,*,#21762,.F.);
#37893=ORIENTED_EDGE('',*,*,#26974,.F.);
#37894=ORIENTED_EDGE('',*,*,#24075,.F.);
#37895=ORIENTED_EDGE('',*,*,#24067,.F.);
#37896=ORIENTED_EDGE('',*,*,#24064,.F.);
#37897=ORIENTED_EDGE('',*,*,#21765,.F.);
#37898=ORIENTED_EDGE('',*,*,#24177,.F.);
#37899=ORIENTED_EDGE('',*,*,#26975,.T.);
#37900=ORIENTED_EDGE('',*,*,#24172,.F.);
#37901=ORIENTED_EDGE('',*,*,#26975,.F.);
#37902=ORIENTED_EDGE('',*,*,#24175,.F.);
#37903=ORIENTED_EDGE('',*,*,#24072,.F.);
#37904=ORIENTED_EDGE('',*,*,#26974,.T.);
#37905=ORIENTED_EDGE('',*,*,#24059,.F.);
#37906=ORIENTED_EDGE('',*,*,#24165,.F.);
#37907=ORIENTED_EDGE('',*,*,#26976,.F.);
#37908=ORIENTED_EDGE('',*,*,#24061,.F.);
#37909=ORIENTED_EDGE('',*,*,#24053,.F.);
#37910=ORIENTED_EDGE('',*,*,#24050,.F.);
#37911=ORIENTED_EDGE('',*,*,#24162,.F.);
#37912=ORIENTED_EDGE('',*,*,#24170,.F.);
#37913=ORIENTED_EDGE('',*,*,#26977,.T.);
#37914=ORIENTED_EDGE('',*,*,#24159,.F.);
#37915=ORIENTED_EDGE('',*,*,#26977,.F.);
#37916=ORIENTED_EDGE('',*,*,#24166,.F.);
#37917=ORIENTED_EDGE('',*,*,#24058,.F.);
#37918=ORIENTED_EDGE('',*,*,#26976,.T.);
#37919=ORIENTED_EDGE('',*,*,#24045,.F.);
#37920=ORIENTED_EDGE('',*,*,#24151,.F.);
#37921=ORIENTED_EDGE('',*,*,#26978,.F.);
#37922=ORIENTED_EDGE('',*,*,#24047,.F.);
#37923=ORIENTED_EDGE('',*,*,#24039,.F.);
#37924=ORIENTED_EDGE('',*,*,#24036,.F.);
#37925=ORIENTED_EDGE('',*,*,#24148,.F.);
#37926=ORIENTED_EDGE('',*,*,#24156,.F.);
#37927=ORIENTED_EDGE('',*,*,#26979,.T.);
#37928=ORIENTED_EDGE('',*,*,#24145,.F.);
#37929=ORIENTED_EDGE('',*,*,#26979,.F.);
#37930=ORIENTED_EDGE('',*,*,#24152,.F.);
#37931=ORIENTED_EDGE('',*,*,#24044,.F.);
#37932=ORIENTED_EDGE('',*,*,#26978,.T.);
#37933=ORIENTED_EDGE('',*,*,#24031,.F.);
#37934=ORIENTED_EDGE('',*,*,#24137,.F.);
#37935=ORIENTED_EDGE('',*,*,#26980,.F.);
#37936=ORIENTED_EDGE('',*,*,#24033,.F.);
#37937=ORIENTED_EDGE('',*,*,#24025,.F.);
#37938=ORIENTED_EDGE('',*,*,#24022,.F.);
#37939=ORIENTED_EDGE('',*,*,#24134,.F.);
#37940=ORIENTED_EDGE('',*,*,#24142,.F.);
#37941=ORIENTED_EDGE('',*,*,#26981,.T.);
#37942=ORIENTED_EDGE('',*,*,#24131,.F.);
#37943=ORIENTED_EDGE('',*,*,#26981,.F.);
#37944=ORIENTED_EDGE('',*,*,#24138,.F.);
#37945=ORIENTED_EDGE('',*,*,#24030,.F.);
#37946=ORIENTED_EDGE('',*,*,#26980,.T.);
#37947=ORIENTED_EDGE('',*,*,#24017,.F.);
#37948=ORIENTED_EDGE('',*,*,#24123,.F.);
#37949=ORIENTED_EDGE('',*,*,#26982,.F.);
#37950=ORIENTED_EDGE('',*,*,#24019,.F.);
#37951=ORIENTED_EDGE('',*,*,#24011,.F.);
#37952=ORIENTED_EDGE('',*,*,#24008,.F.);
#37953=ORIENTED_EDGE('',*,*,#24120,.F.);
#37954=ORIENTED_EDGE('',*,*,#24128,.F.);
#37955=ORIENTED_EDGE('',*,*,#26983,.T.);
#37956=ORIENTED_EDGE('',*,*,#24117,.F.);
#37957=ORIENTED_EDGE('',*,*,#26983,.F.);
#37958=ORIENTED_EDGE('',*,*,#24124,.F.);
#37959=ORIENTED_EDGE('',*,*,#24016,.F.);
#37960=ORIENTED_EDGE('',*,*,#26982,.T.);
#37961=ORIENTED_EDGE('',*,*,#24002,.F.);
#37962=ORIENTED_EDGE('',*,*,#24109,.F.);
#37963=ORIENTED_EDGE('',*,*,#26984,.F.);
#37964=ORIENTED_EDGE('',*,*,#24004,.F.);
#37965=ORIENTED_EDGE('',*,*,#23996,.F.);
#37966=ORIENTED_EDGE('',*,*,#23993,.F.);
#37967=ORIENTED_EDGE('',*,*,#24106,.F.);
#37968=ORIENTED_EDGE('',*,*,#24114,.F.);
#37969=ORIENTED_EDGE('',*,*,#26985,.T.);
#37970=ORIENTED_EDGE('',*,*,#24103,.F.);
#37971=ORIENTED_EDGE('',*,*,#26985,.F.);
#37972=ORIENTED_EDGE('',*,*,#24110,.F.);
#37973=ORIENTED_EDGE('',*,*,#24001,.F.);
#37974=ORIENTED_EDGE('',*,*,#26984,.T.);
#37975=ORIENTED_EDGE('',*,*,#23990,.F.);
#37976=ORIENTED_EDGE('',*,*,#24094,.F.);
#37977=ORIENTED_EDGE('',*,*,#24083,.F.);
#37978=ORIENTED_EDGE('',*,*,#26986,.F.);
#37979=ORIENTED_EDGE('',*,*,#24095,.F.);
#37980=ORIENTED_EDGE('',*,*,#23989,.F.);
#37981=ORIENTED_EDGE('',*,*,#26987,.T.);
#37982=ORIENTED_EDGE('',*,*,#21380,.F.);
#37983=ORIENTED_EDGE('',*,*,#24091,.F.);
#37984=ORIENTED_EDGE('',*,*,#24099,.F.);
#37985=ORIENTED_EDGE('',*,*,#26986,.T.);
#37986=ORIENTED_EDGE('',*,*,#24088,.F.);
#37987=ORIENTED_EDGE('',*,*,#26987,.F.);
#37988=ORIENTED_EDGE('',*,*,#24101,.F.);
#37989=ORIENTED_EDGE('',*,*,#21381,.F.);
#37990=ORIENTED_EDGE('',*,*,#23981,.F.);
#37991=ORIENTED_EDGE('',*,*,#26988,.F.);
#37992=ORIENTED_EDGE('',*,*,#21755,.F.);
#37993=ORIENTED_EDGE('',*,*,#26988,.T.);
#37994=ORIENTED_EDGE('',*,*,#23977,.F.);
#37995=ORIENTED_EDGE('',*,*,#24078,.F.);
#37996=ORIENTED_EDGE('',*,*,#21756,.F.);
#37997=ORIENTED_EDGE('',*,*,#26989,.F.);
#37998=ORIENTED_EDGE('',*,*,#23979,.F.);
#37999=ORIENTED_EDGE('',*,*,#23971,.F.);
#38000=ORIENTED_EDGE('',*,*,#23968,.F.);
#38001=ORIENTED_EDGE('',*,*,#21759,.F.);
#38002=ORIENTED_EDGE('',*,*,#24081,.F.);
#38003=ORIENTED_EDGE('',*,*,#26990,.T.);
#38004=ORIENTED_EDGE('',*,*,#24076,.F.);
#38005=ORIENTED_EDGE('',*,*,#26990,.F.);
#38006=ORIENTED_EDGE('',*,*,#24079,.F.);
#38007=ORIENTED_EDGE('',*,*,#23976,.F.);
#38008=ORIENTED_EDGE('',*,*,#26989,.T.);
#38009=ORIENTED_EDGE('',*,*,#23963,.F.);
#38010=ORIENTED_EDGE('',*,*,#24069,.F.);
#38011=ORIENTED_EDGE('',*,*,#26991,.F.);
#38012=ORIENTED_EDGE('',*,*,#23965,.F.);
#38013=ORIENTED_EDGE('',*,*,#23957,.F.);
#38014=ORIENTED_EDGE('',*,*,#23954,.F.);
#38015=ORIENTED_EDGE('',*,*,#24066,.F.);
#38016=ORIENTED_EDGE('',*,*,#24074,.F.);
#38017=ORIENTED_EDGE('',*,*,#26992,.T.);
#38018=ORIENTED_EDGE('',*,*,#24063,.F.);
#38019=ORIENTED_EDGE('',*,*,#26992,.F.);
#38020=ORIENTED_EDGE('',*,*,#24070,.F.);
#38021=ORIENTED_EDGE('',*,*,#23962,.F.);
#38022=ORIENTED_EDGE('',*,*,#26991,.T.);
#38023=ORIENTED_EDGE('',*,*,#23949,.F.);
#38024=ORIENTED_EDGE('',*,*,#24055,.F.);
#38025=ORIENTED_EDGE('',*,*,#26993,.F.);
#38026=ORIENTED_EDGE('',*,*,#23951,.F.);
#38027=ORIENTED_EDGE('',*,*,#23943,.F.);
#38028=ORIENTED_EDGE('',*,*,#23940,.F.);
#38029=ORIENTED_EDGE('',*,*,#24052,.F.);
#38030=ORIENTED_EDGE('',*,*,#24060,.F.);
#38031=ORIENTED_EDGE('',*,*,#26994,.T.);
#38032=ORIENTED_EDGE('',*,*,#24049,.F.);
#38033=ORIENTED_EDGE('',*,*,#26994,.F.);
#38034=ORIENTED_EDGE('',*,*,#24056,.F.);
#38035=ORIENTED_EDGE('',*,*,#23948,.F.);
#38036=ORIENTED_EDGE('',*,*,#26993,.T.);
#38037=ORIENTED_EDGE('',*,*,#23935,.F.);
#38038=ORIENTED_EDGE('',*,*,#24041,.F.);
#38039=ORIENTED_EDGE('',*,*,#26995,.F.);
#38040=ORIENTED_EDGE('',*,*,#23937,.F.);
#38041=ORIENTED_EDGE('',*,*,#23929,.F.);
#38042=ORIENTED_EDGE('',*,*,#23926,.F.);
#38043=ORIENTED_EDGE('',*,*,#24038,.F.);
#38044=ORIENTED_EDGE('',*,*,#24046,.F.);
#38045=ORIENTED_EDGE('',*,*,#26996,.T.);
#38046=ORIENTED_EDGE('',*,*,#24035,.F.);
#38047=ORIENTED_EDGE('',*,*,#26996,.F.);
#38048=ORIENTED_EDGE('',*,*,#24042,.F.);
#38049=ORIENTED_EDGE('',*,*,#23934,.F.);
#38050=ORIENTED_EDGE('',*,*,#26995,.T.);
#38051=ORIENTED_EDGE('',*,*,#23921,.F.);
#38052=ORIENTED_EDGE('',*,*,#24027,.F.);
#38053=ORIENTED_EDGE('',*,*,#26997,.F.);
#38054=ORIENTED_EDGE('',*,*,#23923,.F.);
#38055=ORIENTED_EDGE('',*,*,#23915,.F.);
#38056=ORIENTED_EDGE('',*,*,#23912,.F.);
#38057=ORIENTED_EDGE('',*,*,#24024,.F.);
#38058=ORIENTED_EDGE('',*,*,#24032,.F.);
#38059=ORIENTED_EDGE('',*,*,#26998,.T.);
#38060=ORIENTED_EDGE('',*,*,#24021,.F.);
#38061=ORIENTED_EDGE('',*,*,#26998,.F.);
#38062=ORIENTED_EDGE('',*,*,#24028,.F.);
#38063=ORIENTED_EDGE('',*,*,#23920,.F.);
#38064=ORIENTED_EDGE('',*,*,#26997,.T.);
#38065=ORIENTED_EDGE('',*,*,#23906,.F.);
#38066=ORIENTED_EDGE('',*,*,#24013,.F.);
#38067=ORIENTED_EDGE('',*,*,#26999,.F.);
#38068=ORIENTED_EDGE('',*,*,#23908,.F.);
#38069=ORIENTED_EDGE('',*,*,#23900,.F.);
#38070=ORIENTED_EDGE('',*,*,#23897,.F.);
#38071=ORIENTED_EDGE('',*,*,#24010,.F.);
#38072=ORIENTED_EDGE('',*,*,#24018,.F.);
#38073=ORIENTED_EDGE('',*,*,#27000,.T.);
#38074=ORIENTED_EDGE('',*,*,#24007,.F.);
#38075=ORIENTED_EDGE('',*,*,#27000,.F.);
#38076=ORIENTED_EDGE('',*,*,#24014,.F.);
#38077=ORIENTED_EDGE('',*,*,#23905,.F.);
#38078=ORIENTED_EDGE('',*,*,#26999,.T.);
#38079=ORIENTED_EDGE('',*,*,#23894,.F.);
#38080=ORIENTED_EDGE('',*,*,#23998,.F.);
#38081=ORIENTED_EDGE('',*,*,#23987,.F.);
#38082=ORIENTED_EDGE('',*,*,#27001,.F.);
#38083=ORIENTED_EDGE('',*,*,#23999,.F.);
#38084=ORIENTED_EDGE('',*,*,#23893,.F.);
#38085=ORIENTED_EDGE('',*,*,#27002,.T.);
#38086=ORIENTED_EDGE('',*,*,#21384,.F.);
#38087=ORIENTED_EDGE('',*,*,#23995,.F.);
#38088=ORIENTED_EDGE('',*,*,#24003,.F.);
#38089=ORIENTED_EDGE('',*,*,#27001,.T.);
#38090=ORIENTED_EDGE('',*,*,#23992,.F.);
#38091=ORIENTED_EDGE('',*,*,#27002,.F.);
#38092=ORIENTED_EDGE('',*,*,#24005,.F.);
#38093=ORIENTED_EDGE('',*,*,#21385,.F.);
#38094=ORIENTED_EDGE('',*,*,#23885,.F.);
#38095=ORIENTED_EDGE('',*,*,#27003,.F.);
#38096=ORIENTED_EDGE('',*,*,#21749,.F.);
#38097=ORIENTED_EDGE('',*,*,#27003,.T.);
#38098=ORIENTED_EDGE('',*,*,#23881,.F.);
#38099=ORIENTED_EDGE('',*,*,#23982,.F.);
#38100=ORIENTED_EDGE('',*,*,#21750,.F.);
#38101=ORIENTED_EDGE('',*,*,#27004,.F.);
#38102=ORIENTED_EDGE('',*,*,#23883,.F.);
#38103=ORIENTED_EDGE('',*,*,#23875,.F.);
#38104=ORIENTED_EDGE('',*,*,#23872,.F.);
#38105=ORIENTED_EDGE('',*,*,#21753,.F.);
#38106=ORIENTED_EDGE('',*,*,#23985,.F.);
#38107=ORIENTED_EDGE('',*,*,#27005,.T.);
#38108=ORIENTED_EDGE('',*,*,#23980,.F.);
#38109=ORIENTED_EDGE('',*,*,#27005,.F.);
#38110=ORIENTED_EDGE('',*,*,#23983,.F.);
#38111=ORIENTED_EDGE('',*,*,#23880,.F.);
#38112=ORIENTED_EDGE('',*,*,#27004,.T.);
#38113=ORIENTED_EDGE('',*,*,#23867,.F.);
#38114=ORIENTED_EDGE('',*,*,#23973,.F.);
#38115=ORIENTED_EDGE('',*,*,#27006,.F.);
#38116=ORIENTED_EDGE('',*,*,#23869,.F.);
#38117=ORIENTED_EDGE('',*,*,#23861,.F.);
#38118=ORIENTED_EDGE('',*,*,#23858,.F.);
#38119=ORIENTED_EDGE('',*,*,#23970,.F.);
#38120=ORIENTED_EDGE('',*,*,#23978,.F.);
#38121=ORIENTED_EDGE('',*,*,#27007,.T.);
#38122=ORIENTED_EDGE('',*,*,#23967,.F.);
#38123=ORIENTED_EDGE('',*,*,#27007,.F.);
#38124=ORIENTED_EDGE('',*,*,#23974,.F.);
#38125=ORIENTED_EDGE('',*,*,#23866,.F.);
#38126=ORIENTED_EDGE('',*,*,#27006,.T.);
#38127=ORIENTED_EDGE('',*,*,#23853,.F.);
#38128=ORIENTED_EDGE('',*,*,#23959,.F.);
#38129=ORIENTED_EDGE('',*,*,#27008,.F.);
#38130=ORIENTED_EDGE('',*,*,#23855,.F.);
#38131=ORIENTED_EDGE('',*,*,#23847,.F.);
#38132=ORIENTED_EDGE('',*,*,#23844,.F.);
#38133=ORIENTED_EDGE('',*,*,#23956,.F.);
#38134=ORIENTED_EDGE('',*,*,#23964,.F.);
#38135=ORIENTED_EDGE('',*,*,#27009,.T.);
#38136=ORIENTED_EDGE('',*,*,#23953,.F.);
#38137=ORIENTED_EDGE('',*,*,#27009,.F.);
#38138=ORIENTED_EDGE('',*,*,#23960,.F.);
#38139=ORIENTED_EDGE('',*,*,#23852,.F.);
#38140=ORIENTED_EDGE('',*,*,#27008,.T.);
#38141=ORIENTED_EDGE('',*,*,#23839,.F.);
#38142=ORIENTED_EDGE('',*,*,#23945,.F.);
#38143=ORIENTED_EDGE('',*,*,#27010,.F.);
#38144=ORIENTED_EDGE('',*,*,#23841,.F.);
#38145=ORIENTED_EDGE('',*,*,#23833,.F.);
#38146=ORIENTED_EDGE('',*,*,#23830,.F.);
#38147=ORIENTED_EDGE('',*,*,#23942,.F.);
#38148=ORIENTED_EDGE('',*,*,#23950,.F.);
#38149=ORIENTED_EDGE('',*,*,#27011,.T.);
#38150=ORIENTED_EDGE('',*,*,#23939,.F.);
#38151=ORIENTED_EDGE('',*,*,#27011,.F.);
#38152=ORIENTED_EDGE('',*,*,#23946,.F.);
#38153=ORIENTED_EDGE('',*,*,#23838,.F.);
#38154=ORIENTED_EDGE('',*,*,#27010,.T.);
#38155=ORIENTED_EDGE('',*,*,#23825,.F.);
#38156=ORIENTED_EDGE('',*,*,#23931,.F.);
#38157=ORIENTED_EDGE('',*,*,#27012,.F.);
#38158=ORIENTED_EDGE('',*,*,#23827,.F.);
#38159=ORIENTED_EDGE('',*,*,#23819,.F.);
#38160=ORIENTED_EDGE('',*,*,#23816,.F.);
#38161=ORIENTED_EDGE('',*,*,#23928,.F.);
#38162=ORIENTED_EDGE('',*,*,#23936,.F.);
#38163=ORIENTED_EDGE('',*,*,#27013,.T.);
#38164=ORIENTED_EDGE('',*,*,#23925,.F.);
#38165=ORIENTED_EDGE('',*,*,#27013,.F.);
#38166=ORIENTED_EDGE('',*,*,#23932,.F.);
#38167=ORIENTED_EDGE('',*,*,#23824,.F.);
#38168=ORIENTED_EDGE('',*,*,#27012,.T.);
#38169=ORIENTED_EDGE('',*,*,#23810,.F.);
#38170=ORIENTED_EDGE('',*,*,#23917,.F.);
#38171=ORIENTED_EDGE('',*,*,#27014,.F.);
#38172=ORIENTED_EDGE('',*,*,#23812,.F.);
#38173=ORIENTED_EDGE('',*,*,#23804,.F.);
#38174=ORIENTED_EDGE('',*,*,#23801,.F.);
#38175=ORIENTED_EDGE('',*,*,#23914,.F.);
#38176=ORIENTED_EDGE('',*,*,#23922,.F.);
#38177=ORIENTED_EDGE('',*,*,#27015,.T.);
#38178=ORIENTED_EDGE('',*,*,#23911,.F.);
#38179=ORIENTED_EDGE('',*,*,#27015,.F.);
#38180=ORIENTED_EDGE('',*,*,#23918,.F.);
#38181=ORIENTED_EDGE('',*,*,#23809,.F.);
#38182=ORIENTED_EDGE('',*,*,#27014,.T.);
#38183=ORIENTED_EDGE('',*,*,#23798,.F.);
#38184=ORIENTED_EDGE('',*,*,#23902,.F.);
#38185=ORIENTED_EDGE('',*,*,#23891,.F.);
#38186=ORIENTED_EDGE('',*,*,#27016,.F.);
#38187=ORIENTED_EDGE('',*,*,#23903,.F.);
#38188=ORIENTED_EDGE('',*,*,#23797,.F.);
#38189=ORIENTED_EDGE('',*,*,#27017,.T.);
#38190=ORIENTED_EDGE('',*,*,#21388,.F.);
#38191=ORIENTED_EDGE('',*,*,#23899,.F.);
#38192=ORIENTED_EDGE('',*,*,#23907,.F.);
#38193=ORIENTED_EDGE('',*,*,#27016,.T.);
#38194=ORIENTED_EDGE('',*,*,#23896,.F.);
#38195=ORIENTED_EDGE('',*,*,#27017,.F.);
#38196=ORIENTED_EDGE('',*,*,#23909,.F.);
#38197=ORIENTED_EDGE('',*,*,#21389,.F.);
#38198=ORIENTED_EDGE('',*,*,#23789,.F.);
#38199=ORIENTED_EDGE('',*,*,#27018,.F.);
#38200=ORIENTED_EDGE('',*,*,#21743,.F.);
#38201=ORIENTED_EDGE('',*,*,#27018,.T.);
#38202=ORIENTED_EDGE('',*,*,#23785,.F.);
#38203=ORIENTED_EDGE('',*,*,#23886,.F.);
#38204=ORIENTED_EDGE('',*,*,#21744,.F.);
#38205=ORIENTED_EDGE('',*,*,#27019,.F.);
#38206=ORIENTED_EDGE('',*,*,#23787,.F.);
#38207=ORIENTED_EDGE('',*,*,#23779,.F.);
#38208=ORIENTED_EDGE('',*,*,#23776,.F.);
#38209=ORIENTED_EDGE('',*,*,#21747,.F.);
#38210=ORIENTED_EDGE('',*,*,#23889,.F.);
#38211=ORIENTED_EDGE('',*,*,#27020,.T.);
#38212=ORIENTED_EDGE('',*,*,#23884,.F.);
#38213=ORIENTED_EDGE('',*,*,#27020,.F.);
#38214=ORIENTED_EDGE('',*,*,#23887,.F.);
#38215=ORIENTED_EDGE('',*,*,#23784,.F.);
#38216=ORIENTED_EDGE('',*,*,#27019,.T.);
#38217=ORIENTED_EDGE('',*,*,#23771,.F.);
#38218=ORIENTED_EDGE('',*,*,#23877,.F.);
#38219=ORIENTED_EDGE('',*,*,#27021,.F.);
#38220=ORIENTED_EDGE('',*,*,#23773,.F.);
#38221=ORIENTED_EDGE('',*,*,#23765,.F.);
#38222=ORIENTED_EDGE('',*,*,#23762,.F.);
#38223=ORIENTED_EDGE('',*,*,#23874,.F.);
#38224=ORIENTED_EDGE('',*,*,#23882,.F.);
#38225=ORIENTED_EDGE('',*,*,#27022,.T.);
#38226=ORIENTED_EDGE('',*,*,#23871,.F.);
#38227=ORIENTED_EDGE('',*,*,#27022,.F.);
#38228=ORIENTED_EDGE('',*,*,#23878,.F.);
#38229=ORIENTED_EDGE('',*,*,#23770,.F.);
#38230=ORIENTED_EDGE('',*,*,#27021,.T.);
#38231=ORIENTED_EDGE('',*,*,#23757,.F.);
#38232=ORIENTED_EDGE('',*,*,#23863,.F.);
#38233=ORIENTED_EDGE('',*,*,#27023,.F.);
#38234=ORIENTED_EDGE('',*,*,#23759,.F.);
#38235=ORIENTED_EDGE('',*,*,#23751,.F.);
#38236=ORIENTED_EDGE('',*,*,#23748,.F.);
#38237=ORIENTED_EDGE('',*,*,#23860,.F.);
#38238=ORIENTED_EDGE('',*,*,#23868,.F.);
#38239=ORIENTED_EDGE('',*,*,#27024,.T.);
#38240=ORIENTED_EDGE('',*,*,#23857,.F.);
#38241=ORIENTED_EDGE('',*,*,#27024,.F.);
#38242=ORIENTED_EDGE('',*,*,#23864,.F.);
#38243=ORIENTED_EDGE('',*,*,#23756,.F.);
#38244=ORIENTED_EDGE('',*,*,#27023,.T.);
#38245=ORIENTED_EDGE('',*,*,#23743,.F.);
#38246=ORIENTED_EDGE('',*,*,#23849,.F.);
#38247=ORIENTED_EDGE('',*,*,#27025,.F.);
#38248=ORIENTED_EDGE('',*,*,#23745,.F.);
#38249=ORIENTED_EDGE('',*,*,#23737,.F.);
#38250=ORIENTED_EDGE('',*,*,#23734,.F.);
#38251=ORIENTED_EDGE('',*,*,#23846,.F.);
#38252=ORIENTED_EDGE('',*,*,#23854,.F.);
#38253=ORIENTED_EDGE('',*,*,#27026,.T.);
#38254=ORIENTED_EDGE('',*,*,#23843,.F.);
#38255=ORIENTED_EDGE('',*,*,#27026,.F.);
#38256=ORIENTED_EDGE('',*,*,#23850,.F.);
#38257=ORIENTED_EDGE('',*,*,#23742,.F.);
#38258=ORIENTED_EDGE('',*,*,#27025,.T.);
#38259=ORIENTED_EDGE('',*,*,#23729,.F.);
#38260=ORIENTED_EDGE('',*,*,#23835,.F.);
#38261=ORIENTED_EDGE('',*,*,#27027,.F.);
#38262=ORIENTED_EDGE('',*,*,#23731,.F.);
#38263=ORIENTED_EDGE('',*,*,#23723,.F.);
#38264=ORIENTED_EDGE('',*,*,#23720,.F.);
#38265=ORIENTED_EDGE('',*,*,#23832,.F.);
#38266=ORIENTED_EDGE('',*,*,#23840,.F.);
#38267=ORIENTED_EDGE('',*,*,#27028,.T.);
#38268=ORIENTED_EDGE('',*,*,#23829,.F.);
#38269=ORIENTED_EDGE('',*,*,#27028,.F.);
#38270=ORIENTED_EDGE('',*,*,#23836,.F.);
#38271=ORIENTED_EDGE('',*,*,#23728,.F.);
#38272=ORIENTED_EDGE('',*,*,#27027,.T.);
#38273=ORIENTED_EDGE('',*,*,#23714,.F.);
#38274=ORIENTED_EDGE('',*,*,#23821,.F.);
#38275=ORIENTED_EDGE('',*,*,#27029,.F.);
#38276=ORIENTED_EDGE('',*,*,#23716,.F.);
#38277=ORIENTED_EDGE('',*,*,#23708,.F.);
#38278=ORIENTED_EDGE('',*,*,#23705,.F.);
#38279=ORIENTED_EDGE('',*,*,#23818,.F.);
#38280=ORIENTED_EDGE('',*,*,#23826,.F.);
#38281=ORIENTED_EDGE('',*,*,#27030,.T.);
#38282=ORIENTED_EDGE('',*,*,#23815,.F.);
#38283=ORIENTED_EDGE('',*,*,#27030,.F.);
#38284=ORIENTED_EDGE('',*,*,#23822,.F.);
#38285=ORIENTED_EDGE('',*,*,#23713,.F.);
#38286=ORIENTED_EDGE('',*,*,#27029,.T.);
#38287=ORIENTED_EDGE('',*,*,#23702,.F.);
#38288=ORIENTED_EDGE('',*,*,#23806,.F.);
#38289=ORIENTED_EDGE('',*,*,#23795,.F.);
#38290=ORIENTED_EDGE('',*,*,#27031,.F.);
#38291=ORIENTED_EDGE('',*,*,#23807,.F.);
#38292=ORIENTED_EDGE('',*,*,#23701,.F.);
#38293=ORIENTED_EDGE('',*,*,#27032,.T.);
#38294=ORIENTED_EDGE('',*,*,#21392,.F.);
#38295=ORIENTED_EDGE('',*,*,#23803,.F.);
#38296=ORIENTED_EDGE('',*,*,#23811,.F.);
#38297=ORIENTED_EDGE('',*,*,#27031,.T.);
#38298=ORIENTED_EDGE('',*,*,#23800,.F.);
#38299=ORIENTED_EDGE('',*,*,#27032,.F.);
#38300=ORIENTED_EDGE('',*,*,#23813,.F.);
#38301=ORIENTED_EDGE('',*,*,#21393,.F.);
#38302=ORIENTED_EDGE('',*,*,#23693,.F.);
#38303=ORIENTED_EDGE('',*,*,#27033,.F.);
#38304=ORIENTED_EDGE('',*,*,#21737,.F.);
#38305=ORIENTED_EDGE('',*,*,#27033,.T.);
#38306=ORIENTED_EDGE('',*,*,#23689,.F.);
#38307=ORIENTED_EDGE('',*,*,#23790,.F.);
#38308=ORIENTED_EDGE('',*,*,#21738,.F.);
#38309=ORIENTED_EDGE('',*,*,#27034,.F.);
#38310=ORIENTED_EDGE('',*,*,#23691,.F.);
#38311=ORIENTED_EDGE('',*,*,#23683,.F.);
#38312=ORIENTED_EDGE('',*,*,#23680,.F.);
#38313=ORIENTED_EDGE('',*,*,#21741,.F.);
#38314=ORIENTED_EDGE('',*,*,#23793,.F.);
#38315=ORIENTED_EDGE('',*,*,#27035,.T.);
#38316=ORIENTED_EDGE('',*,*,#23788,.F.);
#38317=ORIENTED_EDGE('',*,*,#27035,.F.);
#38318=ORIENTED_EDGE('',*,*,#23791,.F.);
#38319=ORIENTED_EDGE('',*,*,#23688,.F.);
#38320=ORIENTED_EDGE('',*,*,#27034,.T.);
#38321=ORIENTED_EDGE('',*,*,#23675,.F.);
#38322=ORIENTED_EDGE('',*,*,#23781,.F.);
#38323=ORIENTED_EDGE('',*,*,#27036,.F.);
#38324=ORIENTED_EDGE('',*,*,#23677,.F.);
#38325=ORIENTED_EDGE('',*,*,#23669,.F.);
#38326=ORIENTED_EDGE('',*,*,#23666,.F.);
#38327=ORIENTED_EDGE('',*,*,#23778,.F.);
#38328=ORIENTED_EDGE('',*,*,#23786,.F.);
#38329=ORIENTED_EDGE('',*,*,#27037,.T.);
#38330=ORIENTED_EDGE('',*,*,#23775,.F.);
#38331=ORIENTED_EDGE('',*,*,#27037,.F.);
#38332=ORIENTED_EDGE('',*,*,#23782,.F.);
#38333=ORIENTED_EDGE('',*,*,#23674,.F.);
#38334=ORIENTED_EDGE('',*,*,#27036,.T.);
#38335=ORIENTED_EDGE('',*,*,#23661,.F.);
#38336=ORIENTED_EDGE('',*,*,#23767,.F.);
#38337=ORIENTED_EDGE('',*,*,#27038,.F.);
#38338=ORIENTED_EDGE('',*,*,#23663,.F.);
#38339=ORIENTED_EDGE('',*,*,#23655,.F.);
#38340=ORIENTED_EDGE('',*,*,#23652,.F.);
#38341=ORIENTED_EDGE('',*,*,#23764,.F.);
#38342=ORIENTED_EDGE('',*,*,#23772,.F.);
#38343=ORIENTED_EDGE('',*,*,#27039,.T.);
#38344=ORIENTED_EDGE('',*,*,#23761,.F.);
#38345=ORIENTED_EDGE('',*,*,#27039,.F.);
#38346=ORIENTED_EDGE('',*,*,#23768,.F.);
#38347=ORIENTED_EDGE('',*,*,#23660,.F.);
#38348=ORIENTED_EDGE('',*,*,#27038,.T.);
#38349=ORIENTED_EDGE('',*,*,#23647,.F.);
#38350=ORIENTED_EDGE('',*,*,#23753,.F.);
#38351=ORIENTED_EDGE('',*,*,#27040,.F.);
#38352=ORIENTED_EDGE('',*,*,#23649,.F.);
#38353=ORIENTED_EDGE('',*,*,#23641,.F.);
#38354=ORIENTED_EDGE('',*,*,#23638,.F.);
#38355=ORIENTED_EDGE('',*,*,#23750,.F.);
#38356=ORIENTED_EDGE('',*,*,#23758,.F.);
#38357=ORIENTED_EDGE('',*,*,#27041,.T.);
#38358=ORIENTED_EDGE('',*,*,#23747,.F.);
#38359=ORIENTED_EDGE('',*,*,#27041,.F.);
#38360=ORIENTED_EDGE('',*,*,#23754,.F.);
#38361=ORIENTED_EDGE('',*,*,#23646,.F.);
#38362=ORIENTED_EDGE('',*,*,#27040,.T.);
#38363=ORIENTED_EDGE('',*,*,#23633,.F.);
#38364=ORIENTED_EDGE('',*,*,#23739,.F.);
#38365=ORIENTED_EDGE('',*,*,#27042,.F.);
#38366=ORIENTED_EDGE('',*,*,#23635,.F.);
#38367=ORIENTED_EDGE('',*,*,#23627,.F.);
#38368=ORIENTED_EDGE('',*,*,#23624,.F.);
#38369=ORIENTED_EDGE('',*,*,#23736,.F.);
#38370=ORIENTED_EDGE('',*,*,#23744,.F.);
#38371=ORIENTED_EDGE('',*,*,#27043,.T.);
#38372=ORIENTED_EDGE('',*,*,#23733,.F.);
#38373=ORIENTED_EDGE('',*,*,#27043,.F.);
#38374=ORIENTED_EDGE('',*,*,#23740,.F.);
#38375=ORIENTED_EDGE('',*,*,#23632,.F.);
#38376=ORIENTED_EDGE('',*,*,#27042,.T.);
#38377=ORIENTED_EDGE('',*,*,#23618,.F.);
#38378=ORIENTED_EDGE('',*,*,#23725,.F.);
#38379=ORIENTED_EDGE('',*,*,#27044,.F.);
#38380=ORIENTED_EDGE('',*,*,#23620,.F.);
#38381=ORIENTED_EDGE('',*,*,#23612,.F.);
#38382=ORIENTED_EDGE('',*,*,#23609,.F.);
#38383=ORIENTED_EDGE('',*,*,#23722,.F.);
#38384=ORIENTED_EDGE('',*,*,#23730,.F.);
#38385=ORIENTED_EDGE('',*,*,#27045,.T.);
#38386=ORIENTED_EDGE('',*,*,#23719,.F.);
#38387=ORIENTED_EDGE('',*,*,#27045,.F.);
#38388=ORIENTED_EDGE('',*,*,#23726,.F.);
#38389=ORIENTED_EDGE('',*,*,#23617,.F.);
#38390=ORIENTED_EDGE('',*,*,#27044,.T.);
#38391=ORIENTED_EDGE('',*,*,#23606,.F.);
#38392=ORIENTED_EDGE('',*,*,#23710,.F.);
#38393=ORIENTED_EDGE('',*,*,#23699,.F.);
#38394=ORIENTED_EDGE('',*,*,#27046,.F.);
#38395=ORIENTED_EDGE('',*,*,#23711,.F.);
#38396=ORIENTED_EDGE('',*,*,#23605,.F.);
#38397=ORIENTED_EDGE('',*,*,#27047,.T.);
#38398=ORIENTED_EDGE('',*,*,#21396,.F.);
#38399=ORIENTED_EDGE('',*,*,#23707,.F.);
#38400=ORIENTED_EDGE('',*,*,#23715,.F.);
#38401=ORIENTED_EDGE('',*,*,#27046,.T.);
#38402=ORIENTED_EDGE('',*,*,#23704,.F.);
#38403=ORIENTED_EDGE('',*,*,#27047,.F.);
#38404=ORIENTED_EDGE('',*,*,#23717,.F.);
#38405=ORIENTED_EDGE('',*,*,#21397,.F.);
#38406=ORIENTED_EDGE('',*,*,#23597,.F.);
#38407=ORIENTED_EDGE('',*,*,#27048,.F.);
#38408=ORIENTED_EDGE('',*,*,#21731,.F.);
#38409=ORIENTED_EDGE('',*,*,#27048,.T.);
#38410=ORIENTED_EDGE('',*,*,#23593,.F.);
#38411=ORIENTED_EDGE('',*,*,#23694,.F.);
#38412=ORIENTED_EDGE('',*,*,#21732,.F.);
#38413=ORIENTED_EDGE('',*,*,#27049,.F.);
#38414=ORIENTED_EDGE('',*,*,#23595,.F.);
#38415=ORIENTED_EDGE('',*,*,#23587,.F.);
#38416=ORIENTED_EDGE('',*,*,#23584,.F.);
#38417=ORIENTED_EDGE('',*,*,#21735,.F.);
#38418=ORIENTED_EDGE('',*,*,#23697,.F.);
#38419=ORIENTED_EDGE('',*,*,#27050,.T.);
#38420=ORIENTED_EDGE('',*,*,#23692,.F.);
#38421=ORIENTED_EDGE('',*,*,#27050,.F.);
#38422=ORIENTED_EDGE('',*,*,#23695,.F.);
#38423=ORIENTED_EDGE('',*,*,#23592,.F.);
#38424=ORIENTED_EDGE('',*,*,#27049,.T.);
#38425=ORIENTED_EDGE('',*,*,#23579,.F.);
#38426=ORIENTED_EDGE('',*,*,#23685,.F.);
#38427=ORIENTED_EDGE('',*,*,#27051,.F.);
#38428=ORIENTED_EDGE('',*,*,#23581,.F.);
#38429=ORIENTED_EDGE('',*,*,#23573,.F.);
#38430=ORIENTED_EDGE('',*,*,#23570,.F.);
#38431=ORIENTED_EDGE('',*,*,#23682,.F.);
#38432=ORIENTED_EDGE('',*,*,#23690,.F.);
#38433=ORIENTED_EDGE('',*,*,#27052,.T.);
#38434=ORIENTED_EDGE('',*,*,#23679,.F.);
#38435=ORIENTED_EDGE('',*,*,#27052,.F.);
#38436=ORIENTED_EDGE('',*,*,#23686,.F.);
#38437=ORIENTED_EDGE('',*,*,#23578,.F.);
#38438=ORIENTED_EDGE('',*,*,#27051,.T.);
#38439=ORIENTED_EDGE('',*,*,#23565,.F.);
#38440=ORIENTED_EDGE('',*,*,#23671,.F.);
#38441=ORIENTED_EDGE('',*,*,#27053,.F.);
#38442=ORIENTED_EDGE('',*,*,#23567,.F.);
#38443=ORIENTED_EDGE('',*,*,#23559,.F.);
#38444=ORIENTED_EDGE('',*,*,#23556,.F.);
#38445=ORIENTED_EDGE('',*,*,#23668,.F.);
#38446=ORIENTED_EDGE('',*,*,#23676,.F.);
#38447=ORIENTED_EDGE('',*,*,#27054,.T.);
#38448=ORIENTED_EDGE('',*,*,#23665,.F.);
#38449=ORIENTED_EDGE('',*,*,#27054,.F.);
#38450=ORIENTED_EDGE('',*,*,#23672,.F.);
#38451=ORIENTED_EDGE('',*,*,#23564,.F.);
#38452=ORIENTED_EDGE('',*,*,#27053,.T.);
#38453=ORIENTED_EDGE('',*,*,#23551,.F.);
#38454=ORIENTED_EDGE('',*,*,#23657,.F.);
#38455=ORIENTED_EDGE('',*,*,#27055,.F.);
#38456=ORIENTED_EDGE('',*,*,#23553,.F.);
#38457=ORIENTED_EDGE('',*,*,#23545,.F.);
#38458=ORIENTED_EDGE('',*,*,#23542,.F.);
#38459=ORIENTED_EDGE('',*,*,#23654,.F.);
#38460=ORIENTED_EDGE('',*,*,#23662,.F.);
#38461=ORIENTED_EDGE('',*,*,#27056,.T.);
#38462=ORIENTED_EDGE('',*,*,#23651,.F.);
#38463=ORIENTED_EDGE('',*,*,#27056,.F.);
#38464=ORIENTED_EDGE('',*,*,#23658,.F.);
#38465=ORIENTED_EDGE('',*,*,#23550,.F.);
#38466=ORIENTED_EDGE('',*,*,#27055,.T.);
#38467=ORIENTED_EDGE('',*,*,#23537,.F.);
#38468=ORIENTED_EDGE('',*,*,#23643,.F.);
#38469=ORIENTED_EDGE('',*,*,#27057,.F.);
#38470=ORIENTED_EDGE('',*,*,#23539,.F.);
#38471=ORIENTED_EDGE('',*,*,#23531,.F.);
#38472=ORIENTED_EDGE('',*,*,#23528,.F.);
#38473=ORIENTED_EDGE('',*,*,#23640,.F.);
#38474=ORIENTED_EDGE('',*,*,#23648,.F.);
#38475=ORIENTED_EDGE('',*,*,#27058,.T.);
#38476=ORIENTED_EDGE('',*,*,#23637,.F.);
#38477=ORIENTED_EDGE('',*,*,#27058,.F.);
#38478=ORIENTED_EDGE('',*,*,#23644,.F.);
#38479=ORIENTED_EDGE('',*,*,#23536,.F.);
#38480=ORIENTED_EDGE('',*,*,#27057,.T.);
#38481=ORIENTED_EDGE('',*,*,#23522,.F.);
#38482=ORIENTED_EDGE('',*,*,#23629,.F.);
#38483=ORIENTED_EDGE('',*,*,#27059,.F.);
#38484=ORIENTED_EDGE('',*,*,#23524,.F.);
#38485=ORIENTED_EDGE('',*,*,#23516,.F.);
#38486=ORIENTED_EDGE('',*,*,#23513,.F.);
#38487=ORIENTED_EDGE('',*,*,#23626,.F.);
#38488=ORIENTED_EDGE('',*,*,#23634,.F.);
#38489=ORIENTED_EDGE('',*,*,#27060,.T.);
#38490=ORIENTED_EDGE('',*,*,#23623,.F.);
#38491=ORIENTED_EDGE('',*,*,#27060,.F.);
#38492=ORIENTED_EDGE('',*,*,#23630,.F.);
#38493=ORIENTED_EDGE('',*,*,#23521,.F.);
#38494=ORIENTED_EDGE('',*,*,#27059,.T.);
#38495=ORIENTED_EDGE('',*,*,#23510,.F.);
#38496=ORIENTED_EDGE('',*,*,#23614,.F.);
#38497=ORIENTED_EDGE('',*,*,#23603,.F.);
#38498=ORIENTED_EDGE('',*,*,#27061,.F.);
#38499=ORIENTED_EDGE('',*,*,#23615,.F.);
#38500=ORIENTED_EDGE('',*,*,#23509,.F.);
#38501=ORIENTED_EDGE('',*,*,#27062,.T.);
#38502=ORIENTED_EDGE('',*,*,#21400,.F.);
#38503=ORIENTED_EDGE('',*,*,#23611,.F.);
#38504=ORIENTED_EDGE('',*,*,#23619,.F.);
#38505=ORIENTED_EDGE('',*,*,#27061,.T.);
#38506=ORIENTED_EDGE('',*,*,#23608,.F.);
#38507=ORIENTED_EDGE('',*,*,#27062,.F.);
#38508=ORIENTED_EDGE('',*,*,#23621,.F.);
#38509=ORIENTED_EDGE('',*,*,#21401,.F.);
#38510=ORIENTED_EDGE('',*,*,#23501,.F.);
#38511=ORIENTED_EDGE('',*,*,#27063,.F.);
#38512=ORIENTED_EDGE('',*,*,#21725,.F.);
#38513=ORIENTED_EDGE('',*,*,#27063,.T.);
#38514=ORIENTED_EDGE('',*,*,#23497,.F.);
#38515=ORIENTED_EDGE('',*,*,#23598,.F.);
#38516=ORIENTED_EDGE('',*,*,#21726,.F.);
#38517=ORIENTED_EDGE('',*,*,#27064,.F.);
#38518=ORIENTED_EDGE('',*,*,#23499,.F.);
#38519=ORIENTED_EDGE('',*,*,#23491,.F.);
#38520=ORIENTED_EDGE('',*,*,#23488,.F.);
#38521=ORIENTED_EDGE('',*,*,#21729,.F.);
#38522=ORIENTED_EDGE('',*,*,#23601,.F.);
#38523=ORIENTED_EDGE('',*,*,#27065,.T.);
#38524=ORIENTED_EDGE('',*,*,#23596,.F.);
#38525=ORIENTED_EDGE('',*,*,#27065,.F.);
#38526=ORIENTED_EDGE('',*,*,#23599,.F.);
#38527=ORIENTED_EDGE('',*,*,#23496,.F.);
#38528=ORIENTED_EDGE('',*,*,#27064,.T.);
#38529=ORIENTED_EDGE('',*,*,#23483,.F.);
#38530=ORIENTED_EDGE('',*,*,#23589,.F.);
#38531=ORIENTED_EDGE('',*,*,#27066,.F.);
#38532=ORIENTED_EDGE('',*,*,#23485,.F.);
#38533=ORIENTED_EDGE('',*,*,#23477,.F.);
#38534=ORIENTED_EDGE('',*,*,#23474,.F.);
#38535=ORIENTED_EDGE('',*,*,#23586,.F.);
#38536=ORIENTED_EDGE('',*,*,#23594,.F.);
#38537=ORIENTED_EDGE('',*,*,#27067,.T.);
#38538=ORIENTED_EDGE('',*,*,#23583,.F.);
#38539=ORIENTED_EDGE('',*,*,#27067,.F.);
#38540=ORIENTED_EDGE('',*,*,#23590,.F.);
#38541=ORIENTED_EDGE('',*,*,#23482,.F.);
#38542=ORIENTED_EDGE('',*,*,#27066,.T.);
#38543=ORIENTED_EDGE('',*,*,#23469,.F.);
#38544=ORIENTED_EDGE('',*,*,#23575,.F.);
#38545=ORIENTED_EDGE('',*,*,#27068,.F.);
#38546=ORIENTED_EDGE('',*,*,#23471,.F.);
#38547=ORIENTED_EDGE('',*,*,#23463,.F.);
#38548=ORIENTED_EDGE('',*,*,#23460,.F.);
#38549=ORIENTED_EDGE('',*,*,#23572,.F.);
#38550=ORIENTED_EDGE('',*,*,#23580,.F.);
#38551=ORIENTED_EDGE('',*,*,#27069,.T.);
#38552=ORIENTED_EDGE('',*,*,#23569,.F.);
#38553=ORIENTED_EDGE('',*,*,#27069,.F.);
#38554=ORIENTED_EDGE('',*,*,#23576,.F.);
#38555=ORIENTED_EDGE('',*,*,#23468,.F.);
#38556=ORIENTED_EDGE('',*,*,#27068,.T.);
#38557=ORIENTED_EDGE('',*,*,#23455,.F.);
#38558=ORIENTED_EDGE('',*,*,#23561,.F.);
#38559=ORIENTED_EDGE('',*,*,#27070,.F.);
#38560=ORIENTED_EDGE('',*,*,#23457,.F.);
#38561=ORIENTED_EDGE('',*,*,#23449,.F.);
#38562=ORIENTED_EDGE('',*,*,#23446,.F.);
#38563=ORIENTED_EDGE('',*,*,#23558,.F.);
#38564=ORIENTED_EDGE('',*,*,#23566,.F.);
#38565=ORIENTED_EDGE('',*,*,#27071,.T.);
#38566=ORIENTED_EDGE('',*,*,#23555,.F.);
#38567=ORIENTED_EDGE('',*,*,#27071,.F.);
#38568=ORIENTED_EDGE('',*,*,#23562,.F.);
#38569=ORIENTED_EDGE('',*,*,#23454,.F.);
#38570=ORIENTED_EDGE('',*,*,#27070,.T.);
#38571=ORIENTED_EDGE('',*,*,#23441,.F.);
#38572=ORIENTED_EDGE('',*,*,#23547,.F.);
#38573=ORIENTED_EDGE('',*,*,#27072,.F.);
#38574=ORIENTED_EDGE('',*,*,#23443,.F.);
#38575=ORIENTED_EDGE('',*,*,#23435,.F.);
#38576=ORIENTED_EDGE('',*,*,#23432,.F.);
#38577=ORIENTED_EDGE('',*,*,#23544,.F.);
#38578=ORIENTED_EDGE('',*,*,#23552,.F.);
#38579=ORIENTED_EDGE('',*,*,#27073,.T.);
#38580=ORIENTED_EDGE('',*,*,#23541,.F.);
#38581=ORIENTED_EDGE('',*,*,#27073,.F.);
#38582=ORIENTED_EDGE('',*,*,#23548,.F.);
#38583=ORIENTED_EDGE('',*,*,#23440,.F.);
#38584=ORIENTED_EDGE('',*,*,#27072,.T.);
#38585=ORIENTED_EDGE('',*,*,#23426,.F.);
#38586=ORIENTED_EDGE('',*,*,#23533,.F.);
#38587=ORIENTED_EDGE('',*,*,#27074,.F.);
#38588=ORIENTED_EDGE('',*,*,#23428,.F.);
#38589=ORIENTED_EDGE('',*,*,#23420,.F.);
#38590=ORIENTED_EDGE('',*,*,#23417,.F.);
#38591=ORIENTED_EDGE('',*,*,#23530,.F.);
#38592=ORIENTED_EDGE('',*,*,#23538,.F.);
#38593=ORIENTED_EDGE('',*,*,#27075,.T.);
#38594=ORIENTED_EDGE('',*,*,#23527,.F.);
#38595=ORIENTED_EDGE('',*,*,#27075,.F.);
#38596=ORIENTED_EDGE('',*,*,#23534,.F.);
#38597=ORIENTED_EDGE('',*,*,#23425,.F.);
#38598=ORIENTED_EDGE('',*,*,#27074,.T.);
#38599=ORIENTED_EDGE('',*,*,#23414,.F.);
#38600=ORIENTED_EDGE('',*,*,#23518,.F.);
#38601=ORIENTED_EDGE('',*,*,#23507,.F.);
#38602=ORIENTED_EDGE('',*,*,#27076,.F.);
#38603=ORIENTED_EDGE('',*,*,#23519,.F.);
#38604=ORIENTED_EDGE('',*,*,#23413,.F.);
#38605=ORIENTED_EDGE('',*,*,#27077,.T.);
#38606=ORIENTED_EDGE('',*,*,#21404,.F.);
#38607=ORIENTED_EDGE('',*,*,#23515,.F.);
#38608=ORIENTED_EDGE('',*,*,#23523,.F.);
#38609=ORIENTED_EDGE('',*,*,#27076,.T.);
#38610=ORIENTED_EDGE('',*,*,#23512,.F.);
#38611=ORIENTED_EDGE('',*,*,#27077,.F.);
#38612=ORIENTED_EDGE('',*,*,#23525,.F.);
#38613=ORIENTED_EDGE('',*,*,#21405,.F.);
#38614=ORIENTED_EDGE('',*,*,#23405,.F.);
#38615=ORIENTED_EDGE('',*,*,#27078,.F.);
#38616=ORIENTED_EDGE('',*,*,#21719,.F.);
#38617=ORIENTED_EDGE('',*,*,#27078,.T.);
#38618=ORIENTED_EDGE('',*,*,#23401,.F.);
#38619=ORIENTED_EDGE('',*,*,#23502,.F.);
#38620=ORIENTED_EDGE('',*,*,#21720,.F.);
#38621=ORIENTED_EDGE('',*,*,#27079,.F.);
#38622=ORIENTED_EDGE('',*,*,#23403,.F.);
#38623=ORIENTED_EDGE('',*,*,#23395,.F.);
#38624=ORIENTED_EDGE('',*,*,#23392,.F.);
#38625=ORIENTED_EDGE('',*,*,#21723,.F.);
#38626=ORIENTED_EDGE('',*,*,#23505,.F.);
#38627=ORIENTED_EDGE('',*,*,#27080,.T.);
#38628=ORIENTED_EDGE('',*,*,#23500,.F.);
#38629=ORIENTED_EDGE('',*,*,#27080,.F.);
#38630=ORIENTED_EDGE('',*,*,#23503,.F.);
#38631=ORIENTED_EDGE('',*,*,#23400,.F.);
#38632=ORIENTED_EDGE('',*,*,#27079,.T.);
#38633=ORIENTED_EDGE('',*,*,#23387,.F.);
#38634=ORIENTED_EDGE('',*,*,#23493,.F.);
#38635=ORIENTED_EDGE('',*,*,#27081,.F.);
#38636=ORIENTED_EDGE('',*,*,#23389,.F.);
#38637=ORIENTED_EDGE('',*,*,#23381,.F.);
#38638=ORIENTED_EDGE('',*,*,#23378,.F.);
#38639=ORIENTED_EDGE('',*,*,#23490,.F.);
#38640=ORIENTED_EDGE('',*,*,#23498,.F.);
#38641=ORIENTED_EDGE('',*,*,#27082,.T.);
#38642=ORIENTED_EDGE('',*,*,#23487,.F.);
#38643=ORIENTED_EDGE('',*,*,#27082,.F.);
#38644=ORIENTED_EDGE('',*,*,#23494,.F.);
#38645=ORIENTED_EDGE('',*,*,#23386,.F.);
#38646=ORIENTED_EDGE('',*,*,#27081,.T.);
#38647=ORIENTED_EDGE('',*,*,#23373,.F.);
#38648=ORIENTED_EDGE('',*,*,#23479,.F.);
#38649=ORIENTED_EDGE('',*,*,#27083,.F.);
#38650=ORIENTED_EDGE('',*,*,#23375,.F.);
#38651=ORIENTED_EDGE('',*,*,#23367,.F.);
#38652=ORIENTED_EDGE('',*,*,#23364,.F.);
#38653=ORIENTED_EDGE('',*,*,#23476,.F.);
#38654=ORIENTED_EDGE('',*,*,#23484,.F.);
#38655=ORIENTED_EDGE('',*,*,#27084,.T.);
#38656=ORIENTED_EDGE('',*,*,#23473,.F.);
#38657=ORIENTED_EDGE('',*,*,#27084,.F.);
#38658=ORIENTED_EDGE('',*,*,#23480,.F.);
#38659=ORIENTED_EDGE('',*,*,#23372,.F.);
#38660=ORIENTED_EDGE('',*,*,#27083,.T.);
#38661=ORIENTED_EDGE('',*,*,#23359,.F.);
#38662=ORIENTED_EDGE('',*,*,#23465,.F.);
#38663=ORIENTED_EDGE('',*,*,#27085,.F.);
#38664=ORIENTED_EDGE('',*,*,#23361,.F.);
#38665=ORIENTED_EDGE('',*,*,#23353,.F.);
#38666=ORIENTED_EDGE('',*,*,#23350,.F.);
#38667=ORIENTED_EDGE('',*,*,#23462,.F.);
#38668=ORIENTED_EDGE('',*,*,#23470,.F.);
#38669=ORIENTED_EDGE('',*,*,#27086,.T.);
#38670=ORIENTED_EDGE('',*,*,#23459,.F.);
#38671=ORIENTED_EDGE('',*,*,#27086,.F.);
#38672=ORIENTED_EDGE('',*,*,#23466,.F.);
#38673=ORIENTED_EDGE('',*,*,#23358,.F.);
#38674=ORIENTED_EDGE('',*,*,#27085,.T.);
#38675=ORIENTED_EDGE('',*,*,#23345,.F.);
#38676=ORIENTED_EDGE('',*,*,#23451,.F.);
#38677=ORIENTED_EDGE('',*,*,#27087,.F.);
#38678=ORIENTED_EDGE('',*,*,#23347,.F.);
#38679=ORIENTED_EDGE('',*,*,#23339,.F.);
#38680=ORIENTED_EDGE('',*,*,#23336,.F.);
#38681=ORIENTED_EDGE('',*,*,#23448,.F.);
#38682=ORIENTED_EDGE('',*,*,#23456,.F.);
#38683=ORIENTED_EDGE('',*,*,#27088,.T.);
#38684=ORIENTED_EDGE('',*,*,#23445,.F.);
#38685=ORIENTED_EDGE('',*,*,#27088,.F.);
#38686=ORIENTED_EDGE('',*,*,#23452,.F.);
#38687=ORIENTED_EDGE('',*,*,#23344,.F.);
#38688=ORIENTED_EDGE('',*,*,#27087,.T.);
#38689=ORIENTED_EDGE('',*,*,#23330,.F.);
#38690=ORIENTED_EDGE('',*,*,#23437,.F.);
#38691=ORIENTED_EDGE('',*,*,#27089,.F.);
#38692=ORIENTED_EDGE('',*,*,#23332,.F.);
#38693=ORIENTED_EDGE('',*,*,#23324,.F.);
#38694=ORIENTED_EDGE('',*,*,#23321,.F.);
#38695=ORIENTED_EDGE('',*,*,#23434,.F.);
#38696=ORIENTED_EDGE('',*,*,#23442,.F.);
#38697=ORIENTED_EDGE('',*,*,#27090,.T.);
#38698=ORIENTED_EDGE('',*,*,#23431,.F.);
#38699=ORIENTED_EDGE('',*,*,#27090,.F.);
#38700=ORIENTED_EDGE('',*,*,#23438,.F.);
#38701=ORIENTED_EDGE('',*,*,#23329,.F.);
#38702=ORIENTED_EDGE('',*,*,#27089,.T.);
#38703=ORIENTED_EDGE('',*,*,#23318,.F.);
#38704=ORIENTED_EDGE('',*,*,#23422,.F.);
#38705=ORIENTED_EDGE('',*,*,#23411,.F.);
#38706=ORIENTED_EDGE('',*,*,#27091,.F.);
#38707=ORIENTED_EDGE('',*,*,#23423,.F.);
#38708=ORIENTED_EDGE('',*,*,#23317,.F.);
#38709=ORIENTED_EDGE('',*,*,#27092,.T.);
#38710=ORIENTED_EDGE('',*,*,#21408,.F.);
#38711=ORIENTED_EDGE('',*,*,#23419,.F.);
#38712=ORIENTED_EDGE('',*,*,#23427,.F.);
#38713=ORIENTED_EDGE('',*,*,#27091,.T.);
#38714=ORIENTED_EDGE('',*,*,#23416,.F.);
#38715=ORIENTED_EDGE('',*,*,#27092,.F.);
#38716=ORIENTED_EDGE('',*,*,#23429,.F.);
#38717=ORIENTED_EDGE('',*,*,#21409,.F.);
#38718=ORIENTED_EDGE('',*,*,#23309,.F.);
#38719=ORIENTED_EDGE('',*,*,#27093,.F.);
#38720=ORIENTED_EDGE('',*,*,#21713,.F.);
#38721=ORIENTED_EDGE('',*,*,#27093,.T.);
#38722=ORIENTED_EDGE('',*,*,#23305,.F.);
#38723=ORIENTED_EDGE('',*,*,#23406,.F.);
#38724=ORIENTED_EDGE('',*,*,#21714,.F.);
#38725=ORIENTED_EDGE('',*,*,#27094,.F.);
#38726=ORIENTED_EDGE('',*,*,#23307,.F.);
#38727=ORIENTED_EDGE('',*,*,#23299,.F.);
#38728=ORIENTED_EDGE('',*,*,#23296,.F.);
#38729=ORIENTED_EDGE('',*,*,#21717,.F.);
#38730=ORIENTED_EDGE('',*,*,#23409,.F.);
#38731=ORIENTED_EDGE('',*,*,#27095,.T.);
#38732=ORIENTED_EDGE('',*,*,#23404,.F.);
#38733=ORIENTED_EDGE('',*,*,#27095,.F.);
#38734=ORIENTED_EDGE('',*,*,#23407,.F.);
#38735=ORIENTED_EDGE('',*,*,#23304,.F.);
#38736=ORIENTED_EDGE('',*,*,#27094,.T.);
#38737=ORIENTED_EDGE('',*,*,#23291,.F.);
#38738=ORIENTED_EDGE('',*,*,#23397,.F.);
#38739=ORIENTED_EDGE('',*,*,#27096,.F.);
#38740=ORIENTED_EDGE('',*,*,#23293,.F.);
#38741=ORIENTED_EDGE('',*,*,#23285,.F.);
#38742=ORIENTED_EDGE('',*,*,#23282,.F.);
#38743=ORIENTED_EDGE('',*,*,#23394,.F.);
#38744=ORIENTED_EDGE('',*,*,#23402,.F.);
#38745=ORIENTED_EDGE('',*,*,#27097,.T.);
#38746=ORIENTED_EDGE('',*,*,#23391,.F.);
#38747=ORIENTED_EDGE('',*,*,#27097,.F.);
#38748=ORIENTED_EDGE('',*,*,#23398,.F.);
#38749=ORIENTED_EDGE('',*,*,#23290,.F.);
#38750=ORIENTED_EDGE('',*,*,#27096,.T.);
#38751=ORIENTED_EDGE('',*,*,#23277,.F.);
#38752=ORIENTED_EDGE('',*,*,#23383,.F.);
#38753=ORIENTED_EDGE('',*,*,#27098,.F.);
#38754=ORIENTED_EDGE('',*,*,#23279,.F.);
#38755=ORIENTED_EDGE('',*,*,#23271,.F.);
#38756=ORIENTED_EDGE('',*,*,#23268,.F.);
#38757=ORIENTED_EDGE('',*,*,#23380,.F.);
#38758=ORIENTED_EDGE('',*,*,#23388,.F.);
#38759=ORIENTED_EDGE('',*,*,#27099,.T.);
#38760=ORIENTED_EDGE('',*,*,#23377,.F.);
#38761=ORIENTED_EDGE('',*,*,#27099,.F.);
#38762=ORIENTED_EDGE('',*,*,#23384,.F.);
#38763=ORIENTED_EDGE('',*,*,#23276,.F.);
#38764=ORIENTED_EDGE('',*,*,#27098,.T.);
#38765=ORIENTED_EDGE('',*,*,#23263,.F.);
#38766=ORIENTED_EDGE('',*,*,#23369,.F.);
#38767=ORIENTED_EDGE('',*,*,#27100,.F.);
#38768=ORIENTED_EDGE('',*,*,#23265,.F.);
#38769=ORIENTED_EDGE('',*,*,#23257,.F.);
#38770=ORIENTED_EDGE('',*,*,#23254,.F.);
#38771=ORIENTED_EDGE('',*,*,#23366,.F.);
#38772=ORIENTED_EDGE('',*,*,#23374,.F.);
#38773=ORIENTED_EDGE('',*,*,#27101,.T.);
#38774=ORIENTED_EDGE('',*,*,#23363,.F.);
#38775=ORIENTED_EDGE('',*,*,#27101,.F.);
#38776=ORIENTED_EDGE('',*,*,#23370,.F.);
#38777=ORIENTED_EDGE('',*,*,#23262,.F.);
#38778=ORIENTED_EDGE('',*,*,#27100,.T.);
#38779=ORIENTED_EDGE('',*,*,#23249,.F.);
#38780=ORIENTED_EDGE('',*,*,#23355,.F.);
#38781=ORIENTED_EDGE('',*,*,#27102,.F.);
#38782=ORIENTED_EDGE('',*,*,#23251,.F.);
#38783=ORIENTED_EDGE('',*,*,#23243,.F.);
#38784=ORIENTED_EDGE('',*,*,#23240,.F.);
#38785=ORIENTED_EDGE('',*,*,#23352,.F.);
#38786=ORIENTED_EDGE('',*,*,#23360,.F.);
#38787=ORIENTED_EDGE('',*,*,#27103,.T.);
#38788=ORIENTED_EDGE('',*,*,#23349,.F.);
#38789=ORIENTED_EDGE('',*,*,#27103,.F.);
#38790=ORIENTED_EDGE('',*,*,#23356,.F.);
#38791=ORIENTED_EDGE('',*,*,#23248,.F.);
#38792=ORIENTED_EDGE('',*,*,#27102,.T.);
#38793=ORIENTED_EDGE('',*,*,#23234,.F.);
#38794=ORIENTED_EDGE('',*,*,#23341,.F.);
#38795=ORIENTED_EDGE('',*,*,#27104,.F.);
#38796=ORIENTED_EDGE('',*,*,#23236,.F.);
#38797=ORIENTED_EDGE('',*,*,#23228,.F.);
#38798=ORIENTED_EDGE('',*,*,#23225,.F.);
#38799=ORIENTED_EDGE('',*,*,#23338,.F.);
#38800=ORIENTED_EDGE('',*,*,#23346,.F.);
#38801=ORIENTED_EDGE('',*,*,#27105,.T.);
#38802=ORIENTED_EDGE('',*,*,#23335,.F.);
#38803=ORIENTED_EDGE('',*,*,#27105,.F.);
#38804=ORIENTED_EDGE('',*,*,#23342,.F.);
#38805=ORIENTED_EDGE('',*,*,#23233,.F.);
#38806=ORIENTED_EDGE('',*,*,#27104,.T.);
#38807=ORIENTED_EDGE('',*,*,#23222,.F.);
#38808=ORIENTED_EDGE('',*,*,#23326,.F.);
#38809=ORIENTED_EDGE('',*,*,#23315,.F.);
#38810=ORIENTED_EDGE('',*,*,#27106,.F.);
#38811=ORIENTED_EDGE('',*,*,#23327,.F.);
#38812=ORIENTED_EDGE('',*,*,#23221,.F.);
#38813=ORIENTED_EDGE('',*,*,#27107,.T.);
#38814=ORIENTED_EDGE('',*,*,#21412,.F.);
#38815=ORIENTED_EDGE('',*,*,#23323,.F.);
#38816=ORIENTED_EDGE('',*,*,#23331,.F.);
#38817=ORIENTED_EDGE('',*,*,#27106,.T.);
#38818=ORIENTED_EDGE('',*,*,#23320,.F.);
#38819=ORIENTED_EDGE('',*,*,#27107,.F.);
#38820=ORIENTED_EDGE('',*,*,#23333,.F.);
#38821=ORIENTED_EDGE('',*,*,#21413,.F.);
#38822=ORIENTED_EDGE('',*,*,#23213,.F.);
#38823=ORIENTED_EDGE('',*,*,#27108,.F.);
#38824=ORIENTED_EDGE('',*,*,#21707,.F.);
#38825=ORIENTED_EDGE('',*,*,#27108,.T.);
#38826=ORIENTED_EDGE('',*,*,#23209,.F.);
#38827=ORIENTED_EDGE('',*,*,#23310,.F.);
#38828=ORIENTED_EDGE('',*,*,#21708,.F.);
#38829=ORIENTED_EDGE('',*,*,#27109,.F.);
#38830=ORIENTED_EDGE('',*,*,#23211,.F.);
#38831=ORIENTED_EDGE('',*,*,#23203,.F.);
#38832=ORIENTED_EDGE('',*,*,#23200,.F.);
#38833=ORIENTED_EDGE('',*,*,#21711,.F.);
#38834=ORIENTED_EDGE('',*,*,#23313,.F.);
#38835=ORIENTED_EDGE('',*,*,#27110,.T.);
#38836=ORIENTED_EDGE('',*,*,#23308,.F.);
#38837=ORIENTED_EDGE('',*,*,#27110,.F.);
#38838=ORIENTED_EDGE('',*,*,#23311,.F.);
#38839=ORIENTED_EDGE('',*,*,#23208,.F.);
#38840=ORIENTED_EDGE('',*,*,#27109,.T.);
#38841=ORIENTED_EDGE('',*,*,#23195,.F.);
#38842=ORIENTED_EDGE('',*,*,#23301,.F.);
#38843=ORIENTED_EDGE('',*,*,#27111,.F.);
#38844=ORIENTED_EDGE('',*,*,#23197,.F.);
#38845=ORIENTED_EDGE('',*,*,#23189,.F.);
#38846=ORIENTED_EDGE('',*,*,#23186,.F.);
#38847=ORIENTED_EDGE('',*,*,#23298,.F.);
#38848=ORIENTED_EDGE('',*,*,#23306,.F.);
#38849=ORIENTED_EDGE('',*,*,#27112,.T.);
#38850=ORIENTED_EDGE('',*,*,#23295,.F.);
#38851=ORIENTED_EDGE('',*,*,#27112,.F.);
#38852=ORIENTED_EDGE('',*,*,#23302,.F.);
#38853=ORIENTED_EDGE('',*,*,#23194,.F.);
#38854=ORIENTED_EDGE('',*,*,#27111,.T.);
#38855=ORIENTED_EDGE('',*,*,#23181,.F.);
#38856=ORIENTED_EDGE('',*,*,#23287,.F.);
#38857=ORIENTED_EDGE('',*,*,#27113,.F.);
#38858=ORIENTED_EDGE('',*,*,#23183,.F.);
#38859=ORIENTED_EDGE('',*,*,#23175,.F.);
#38860=ORIENTED_EDGE('',*,*,#23172,.F.);
#38861=ORIENTED_EDGE('',*,*,#23284,.F.);
#38862=ORIENTED_EDGE('',*,*,#23292,.F.);
#38863=ORIENTED_EDGE('',*,*,#27114,.T.);
#38864=ORIENTED_EDGE('',*,*,#23281,.F.);
#38865=ORIENTED_EDGE('',*,*,#27114,.F.);
#38866=ORIENTED_EDGE('',*,*,#23288,.F.);
#38867=ORIENTED_EDGE('',*,*,#23180,.F.);
#38868=ORIENTED_EDGE('',*,*,#27113,.T.);
#38869=ORIENTED_EDGE('',*,*,#23167,.F.);
#38870=ORIENTED_EDGE('',*,*,#23273,.F.);
#38871=ORIENTED_EDGE('',*,*,#27115,.F.);
#38872=ORIENTED_EDGE('',*,*,#23169,.F.);
#38873=ORIENTED_EDGE('',*,*,#23161,.F.);
#38874=ORIENTED_EDGE('',*,*,#23158,.F.);
#38875=ORIENTED_EDGE('',*,*,#23270,.F.);
#38876=ORIENTED_EDGE('',*,*,#23278,.F.);
#38877=ORIENTED_EDGE('',*,*,#27116,.T.);
#38878=ORIENTED_EDGE('',*,*,#23267,.F.);
#38879=ORIENTED_EDGE('',*,*,#27116,.F.);
#38880=ORIENTED_EDGE('',*,*,#23274,.F.);
#38881=ORIENTED_EDGE('',*,*,#23166,.F.);
#38882=ORIENTED_EDGE('',*,*,#27115,.T.);
#38883=ORIENTED_EDGE('',*,*,#23153,.F.);
#38884=ORIENTED_EDGE('',*,*,#23259,.F.);
#38885=ORIENTED_EDGE('',*,*,#27117,.F.);
#38886=ORIENTED_EDGE('',*,*,#23155,.F.);
#38887=ORIENTED_EDGE('',*,*,#23147,.F.);
#38888=ORIENTED_EDGE('',*,*,#23144,.F.);
#38889=ORIENTED_EDGE('',*,*,#23256,.F.);
#38890=ORIENTED_EDGE('',*,*,#23264,.F.);
#38891=ORIENTED_EDGE('',*,*,#27118,.T.);
#38892=ORIENTED_EDGE('',*,*,#23253,.F.);
#38893=ORIENTED_EDGE('',*,*,#27118,.F.);
#38894=ORIENTED_EDGE('',*,*,#23260,.F.);
#38895=ORIENTED_EDGE('',*,*,#23152,.F.);
#38896=ORIENTED_EDGE('',*,*,#27117,.T.);
#38897=ORIENTED_EDGE('',*,*,#23138,.F.);
#38898=ORIENTED_EDGE('',*,*,#23245,.F.);
#38899=ORIENTED_EDGE('',*,*,#27119,.F.);
#38900=ORIENTED_EDGE('',*,*,#23140,.F.);
#38901=ORIENTED_EDGE('',*,*,#23132,.F.);
#38902=ORIENTED_EDGE('',*,*,#23129,.F.);
#38903=ORIENTED_EDGE('',*,*,#23242,.F.);
#38904=ORIENTED_EDGE('',*,*,#23250,.F.);
#38905=ORIENTED_EDGE('',*,*,#27120,.T.);
#38906=ORIENTED_EDGE('',*,*,#23239,.F.);
#38907=ORIENTED_EDGE('',*,*,#27120,.F.);
#38908=ORIENTED_EDGE('',*,*,#23246,.F.);
#38909=ORIENTED_EDGE('',*,*,#23137,.F.);
#38910=ORIENTED_EDGE('',*,*,#27119,.T.);
#38911=ORIENTED_EDGE('',*,*,#23126,.F.);
#38912=ORIENTED_EDGE('',*,*,#23230,.F.);
#38913=ORIENTED_EDGE('',*,*,#23219,.F.);
#38914=ORIENTED_EDGE('',*,*,#27121,.F.);
#38915=ORIENTED_EDGE('',*,*,#23231,.F.);
#38916=ORIENTED_EDGE('',*,*,#23125,.F.);
#38917=ORIENTED_EDGE('',*,*,#27122,.T.);
#38918=ORIENTED_EDGE('',*,*,#21416,.F.);
#38919=ORIENTED_EDGE('',*,*,#23227,.F.);
#38920=ORIENTED_EDGE('',*,*,#23235,.F.);
#38921=ORIENTED_EDGE('',*,*,#27121,.T.);
#38922=ORIENTED_EDGE('',*,*,#23224,.F.);
#38923=ORIENTED_EDGE('',*,*,#27122,.F.);
#38924=ORIENTED_EDGE('',*,*,#23237,.F.);
#38925=ORIENTED_EDGE('',*,*,#21417,.F.);
#38926=ORIENTED_EDGE('',*,*,#23117,.F.);
#38927=ORIENTED_EDGE('',*,*,#27123,.F.);
#38928=ORIENTED_EDGE('',*,*,#21701,.F.);
#38929=ORIENTED_EDGE('',*,*,#27123,.T.);
#38930=ORIENTED_EDGE('',*,*,#23113,.F.);
#38931=ORIENTED_EDGE('',*,*,#23214,.F.);
#38932=ORIENTED_EDGE('',*,*,#21702,.F.);
#38933=ORIENTED_EDGE('',*,*,#27124,.F.);
#38934=ORIENTED_EDGE('',*,*,#23115,.F.);
#38935=ORIENTED_EDGE('',*,*,#23107,.F.);
#38936=ORIENTED_EDGE('',*,*,#23104,.F.);
#38937=ORIENTED_EDGE('',*,*,#21705,.F.);
#38938=ORIENTED_EDGE('',*,*,#23217,.F.);
#38939=ORIENTED_EDGE('',*,*,#27125,.T.);
#38940=ORIENTED_EDGE('',*,*,#23212,.F.);
#38941=ORIENTED_EDGE('',*,*,#27125,.F.);
#38942=ORIENTED_EDGE('',*,*,#23215,.F.);
#38943=ORIENTED_EDGE('',*,*,#23112,.F.);
#38944=ORIENTED_EDGE('',*,*,#27124,.T.);
#38945=ORIENTED_EDGE('',*,*,#23099,.F.);
#38946=ORIENTED_EDGE('',*,*,#23205,.F.);
#38947=ORIENTED_EDGE('',*,*,#27126,.F.);
#38948=ORIENTED_EDGE('',*,*,#23101,.F.);
#38949=ORIENTED_EDGE('',*,*,#23093,.F.);
#38950=ORIENTED_EDGE('',*,*,#23090,.F.);
#38951=ORIENTED_EDGE('',*,*,#23202,.F.);
#38952=ORIENTED_EDGE('',*,*,#23210,.F.);
#38953=ORIENTED_EDGE('',*,*,#27127,.T.);
#38954=ORIENTED_EDGE('',*,*,#23199,.F.);
#38955=ORIENTED_EDGE('',*,*,#27127,.F.);
#38956=ORIENTED_EDGE('',*,*,#23206,.F.);
#38957=ORIENTED_EDGE('',*,*,#23098,.F.);
#38958=ORIENTED_EDGE('',*,*,#27126,.T.);
#38959=ORIENTED_EDGE('',*,*,#23085,.F.);
#38960=ORIENTED_EDGE('',*,*,#23191,.F.);
#38961=ORIENTED_EDGE('',*,*,#27128,.F.);
#38962=ORIENTED_EDGE('',*,*,#23087,.F.);
#38963=ORIENTED_EDGE('',*,*,#23079,.F.);
#38964=ORIENTED_EDGE('',*,*,#23076,.F.);
#38965=ORIENTED_EDGE('',*,*,#23188,.F.);
#38966=ORIENTED_EDGE('',*,*,#23196,.F.);
#38967=ORIENTED_EDGE('',*,*,#27129,.T.);
#38968=ORIENTED_EDGE('',*,*,#23185,.F.);
#38969=ORIENTED_EDGE('',*,*,#27129,.F.);
#38970=ORIENTED_EDGE('',*,*,#23192,.F.);
#38971=ORIENTED_EDGE('',*,*,#23084,.F.);
#38972=ORIENTED_EDGE('',*,*,#27128,.T.);
#38973=ORIENTED_EDGE('',*,*,#23071,.F.);
#38974=ORIENTED_EDGE('',*,*,#23177,.F.);
#38975=ORIENTED_EDGE('',*,*,#27130,.F.);
#38976=ORIENTED_EDGE('',*,*,#23073,.F.);
#38977=ORIENTED_EDGE('',*,*,#23065,.F.);
#38978=ORIENTED_EDGE('',*,*,#23062,.F.);
#38979=ORIENTED_EDGE('',*,*,#23174,.F.);
#38980=ORIENTED_EDGE('',*,*,#23182,.F.);
#38981=ORIENTED_EDGE('',*,*,#27131,.T.);
#38982=ORIENTED_EDGE('',*,*,#23171,.F.);
#38983=ORIENTED_EDGE('',*,*,#27131,.F.);
#38984=ORIENTED_EDGE('',*,*,#23178,.F.);
#38985=ORIENTED_EDGE('',*,*,#23070,.F.);
#38986=ORIENTED_EDGE('',*,*,#27130,.T.);
#38987=ORIENTED_EDGE('',*,*,#23057,.F.);
#38988=ORIENTED_EDGE('',*,*,#23163,.F.);
#38989=ORIENTED_EDGE('',*,*,#27132,.F.);
#38990=ORIENTED_EDGE('',*,*,#23059,.F.);
#38991=ORIENTED_EDGE('',*,*,#23051,.F.);
#38992=ORIENTED_EDGE('',*,*,#23048,.F.);
#38993=ORIENTED_EDGE('',*,*,#23160,.F.);
#38994=ORIENTED_EDGE('',*,*,#23168,.F.);
#38995=ORIENTED_EDGE('',*,*,#27133,.T.);
#38996=ORIENTED_EDGE('',*,*,#23157,.F.);
#38997=ORIENTED_EDGE('',*,*,#27133,.F.);
#38998=ORIENTED_EDGE('',*,*,#23164,.F.);
#38999=ORIENTED_EDGE('',*,*,#23056,.F.);
#39000=ORIENTED_EDGE('',*,*,#27132,.T.);
#39001=ORIENTED_EDGE('',*,*,#23042,.F.);
#39002=ORIENTED_EDGE('',*,*,#23149,.F.);
#39003=ORIENTED_EDGE('',*,*,#27134,.F.);
#39004=ORIENTED_EDGE('',*,*,#23044,.F.);
#39005=ORIENTED_EDGE('',*,*,#23036,.F.);
#39006=ORIENTED_EDGE('',*,*,#23033,.F.);
#39007=ORIENTED_EDGE('',*,*,#23146,.F.);
#39008=ORIENTED_EDGE('',*,*,#23154,.F.);
#39009=ORIENTED_EDGE('',*,*,#27135,.T.);
#39010=ORIENTED_EDGE('',*,*,#23143,.F.);
#39011=ORIENTED_EDGE('',*,*,#27135,.F.);
#39012=ORIENTED_EDGE('',*,*,#23150,.F.);
#39013=ORIENTED_EDGE('',*,*,#23041,.F.);
#39014=ORIENTED_EDGE('',*,*,#27134,.T.);
#39015=ORIENTED_EDGE('',*,*,#23030,.F.);
#39016=ORIENTED_EDGE('',*,*,#23134,.F.);
#39017=ORIENTED_EDGE('',*,*,#23123,.F.);
#39018=ORIENTED_EDGE('',*,*,#27136,.F.);
#39019=ORIENTED_EDGE('',*,*,#23135,.F.);
#39020=ORIENTED_EDGE('',*,*,#23029,.F.);
#39021=ORIENTED_EDGE('',*,*,#27137,.T.);
#39022=ORIENTED_EDGE('',*,*,#21420,.F.);
#39023=ORIENTED_EDGE('',*,*,#23131,.F.);
#39024=ORIENTED_EDGE('',*,*,#23139,.F.);
#39025=ORIENTED_EDGE('',*,*,#27136,.T.);
#39026=ORIENTED_EDGE('',*,*,#23128,.F.);
#39027=ORIENTED_EDGE('',*,*,#27137,.F.);
#39028=ORIENTED_EDGE('',*,*,#23141,.F.);
#39029=ORIENTED_EDGE('',*,*,#21421,.F.);
#39030=ORIENTED_EDGE('',*,*,#23021,.F.);
#39031=ORIENTED_EDGE('',*,*,#27138,.F.);
#39032=ORIENTED_EDGE('',*,*,#21695,.F.);
#39033=ORIENTED_EDGE('',*,*,#27138,.T.);
#39034=ORIENTED_EDGE('',*,*,#23017,.F.);
#39035=ORIENTED_EDGE('',*,*,#23118,.F.);
#39036=ORIENTED_EDGE('',*,*,#21696,.F.);
#39037=ORIENTED_EDGE('',*,*,#27139,.F.);
#39038=ORIENTED_EDGE('',*,*,#23019,.F.);
#39039=ORIENTED_EDGE('',*,*,#23011,.F.);
#39040=ORIENTED_EDGE('',*,*,#23008,.F.);
#39041=ORIENTED_EDGE('',*,*,#21699,.F.);
#39042=ORIENTED_EDGE('',*,*,#23121,.F.);
#39043=ORIENTED_EDGE('',*,*,#27140,.T.);
#39044=ORIENTED_EDGE('',*,*,#23116,.F.);
#39045=ORIENTED_EDGE('',*,*,#27140,.F.);
#39046=ORIENTED_EDGE('',*,*,#23119,.F.);
#39047=ORIENTED_EDGE('',*,*,#23016,.F.);
#39048=ORIENTED_EDGE('',*,*,#27139,.T.);
#39049=ORIENTED_EDGE('',*,*,#23003,.F.);
#39050=ORIENTED_EDGE('',*,*,#23109,.F.);
#39051=ORIENTED_EDGE('',*,*,#27141,.F.);
#39052=ORIENTED_EDGE('',*,*,#23005,.F.);
#39053=ORIENTED_EDGE('',*,*,#22997,.F.);
#39054=ORIENTED_EDGE('',*,*,#22994,.F.);
#39055=ORIENTED_EDGE('',*,*,#23106,.F.);
#39056=ORIENTED_EDGE('',*,*,#23114,.F.);
#39057=ORIENTED_EDGE('',*,*,#27142,.T.);
#39058=ORIENTED_EDGE('',*,*,#23103,.F.);
#39059=ORIENTED_EDGE('',*,*,#27142,.F.);
#39060=ORIENTED_EDGE('',*,*,#23110,.F.);
#39061=ORIENTED_EDGE('',*,*,#23002,.F.);
#39062=ORIENTED_EDGE('',*,*,#27141,.T.);
#39063=ORIENTED_EDGE('',*,*,#22989,.F.);
#39064=ORIENTED_EDGE('',*,*,#23095,.F.);
#39065=ORIENTED_EDGE('',*,*,#27143,.F.);
#39066=ORIENTED_EDGE('',*,*,#22991,.F.);
#39067=ORIENTED_EDGE('',*,*,#22983,.F.);
#39068=ORIENTED_EDGE('',*,*,#22980,.F.);
#39069=ORIENTED_EDGE('',*,*,#23092,.F.);
#39070=ORIENTED_EDGE('',*,*,#23100,.F.);
#39071=ORIENTED_EDGE('',*,*,#27144,.T.);
#39072=ORIENTED_EDGE('',*,*,#23089,.F.);
#39073=ORIENTED_EDGE('',*,*,#27144,.F.);
#39074=ORIENTED_EDGE('',*,*,#23096,.F.);
#39075=ORIENTED_EDGE('',*,*,#22988,.F.);
#39076=ORIENTED_EDGE('',*,*,#27143,.T.);
#39077=ORIENTED_EDGE('',*,*,#22975,.F.);
#39078=ORIENTED_EDGE('',*,*,#23081,.F.);
#39079=ORIENTED_EDGE('',*,*,#27145,.F.);
#39080=ORIENTED_EDGE('',*,*,#22977,.F.);
#39081=ORIENTED_EDGE('',*,*,#22969,.F.);
#39082=ORIENTED_EDGE('',*,*,#22966,.F.);
#39083=ORIENTED_EDGE('',*,*,#23078,.F.);
#39084=ORIENTED_EDGE('',*,*,#23086,.F.);
#39085=ORIENTED_EDGE('',*,*,#27146,.T.);
#39086=ORIENTED_EDGE('',*,*,#23075,.F.);
#39087=ORIENTED_EDGE('',*,*,#27146,.F.);
#39088=ORIENTED_EDGE('',*,*,#23082,.F.);
#39089=ORIENTED_EDGE('',*,*,#22974,.F.);
#39090=ORIENTED_EDGE('',*,*,#27145,.T.);
#39091=ORIENTED_EDGE('',*,*,#22961,.F.);
#39092=ORIENTED_EDGE('',*,*,#23067,.F.);
#39093=ORIENTED_EDGE('',*,*,#27147,.F.);
#39094=ORIENTED_EDGE('',*,*,#22963,.F.);
#39095=ORIENTED_EDGE('',*,*,#22955,.F.);
#39096=ORIENTED_EDGE('',*,*,#22952,.F.);
#39097=ORIENTED_EDGE('',*,*,#23064,.F.);
#39098=ORIENTED_EDGE('',*,*,#23072,.F.);
#39099=ORIENTED_EDGE('',*,*,#27148,.T.);
#39100=ORIENTED_EDGE('',*,*,#23061,.F.);
#39101=ORIENTED_EDGE('',*,*,#27148,.F.);
#39102=ORIENTED_EDGE('',*,*,#23068,.F.);
#39103=ORIENTED_EDGE('',*,*,#22960,.F.);
#39104=ORIENTED_EDGE('',*,*,#27147,.T.);
#39105=ORIENTED_EDGE('',*,*,#22946,.F.);
#39106=ORIENTED_EDGE('',*,*,#23053,.F.);
#39107=ORIENTED_EDGE('',*,*,#27149,.F.);
#39108=ORIENTED_EDGE('',*,*,#22948,.F.);
#39109=ORIENTED_EDGE('',*,*,#22940,.F.);
#39110=ORIENTED_EDGE('',*,*,#22937,.F.);
#39111=ORIENTED_EDGE('',*,*,#23050,.F.);
#39112=ORIENTED_EDGE('',*,*,#23058,.F.);
#39113=ORIENTED_EDGE('',*,*,#27150,.T.);
#39114=ORIENTED_EDGE('',*,*,#23047,.F.);
#39115=ORIENTED_EDGE('',*,*,#27150,.F.);
#39116=ORIENTED_EDGE('',*,*,#23054,.F.);
#39117=ORIENTED_EDGE('',*,*,#22945,.F.);
#39118=ORIENTED_EDGE('',*,*,#27149,.T.);
#39119=ORIENTED_EDGE('',*,*,#22934,.F.);
#39120=ORIENTED_EDGE('',*,*,#23038,.F.);
#39121=ORIENTED_EDGE('',*,*,#23027,.F.);
#39122=ORIENTED_EDGE('',*,*,#27151,.F.);
#39123=ORIENTED_EDGE('',*,*,#23039,.F.);
#39124=ORIENTED_EDGE('',*,*,#22933,.F.);
#39125=ORIENTED_EDGE('',*,*,#27152,.T.);
#39126=ORIENTED_EDGE('',*,*,#21424,.F.);
#39127=ORIENTED_EDGE('',*,*,#23035,.F.);
#39128=ORIENTED_EDGE('',*,*,#23043,.F.);
#39129=ORIENTED_EDGE('',*,*,#27151,.T.);
#39130=ORIENTED_EDGE('',*,*,#23032,.F.);
#39131=ORIENTED_EDGE('',*,*,#27152,.F.);
#39132=ORIENTED_EDGE('',*,*,#23045,.F.);
#39133=ORIENTED_EDGE('',*,*,#21425,.F.);
#39134=ORIENTED_EDGE('',*,*,#22925,.F.);
#39135=ORIENTED_EDGE('',*,*,#27153,.F.);
#39136=ORIENTED_EDGE('',*,*,#21689,.F.);
#39137=ORIENTED_EDGE('',*,*,#27153,.T.);
#39138=ORIENTED_EDGE('',*,*,#22921,.F.);
#39139=ORIENTED_EDGE('',*,*,#23022,.F.);
#39140=ORIENTED_EDGE('',*,*,#21690,.F.);
#39141=ORIENTED_EDGE('',*,*,#27154,.F.);
#39142=ORIENTED_EDGE('',*,*,#22923,.F.);
#39143=ORIENTED_EDGE('',*,*,#22915,.F.);
#39144=ORIENTED_EDGE('',*,*,#22912,.F.);
#39145=ORIENTED_EDGE('',*,*,#21693,.F.);
#39146=ORIENTED_EDGE('',*,*,#23025,.F.);
#39147=ORIENTED_EDGE('',*,*,#27155,.T.);
#39148=ORIENTED_EDGE('',*,*,#23020,.F.);
#39149=ORIENTED_EDGE('',*,*,#27155,.F.);
#39150=ORIENTED_EDGE('',*,*,#23023,.F.);
#39151=ORIENTED_EDGE('',*,*,#22920,.F.);
#39152=ORIENTED_EDGE('',*,*,#27154,.T.);
#39153=ORIENTED_EDGE('',*,*,#22907,.F.);
#39154=ORIENTED_EDGE('',*,*,#23013,.F.);
#39155=ORIENTED_EDGE('',*,*,#27156,.F.);
#39156=ORIENTED_EDGE('',*,*,#22909,.F.);
#39157=ORIENTED_EDGE('',*,*,#22901,.F.);
#39158=ORIENTED_EDGE('',*,*,#22898,.F.);
#39159=ORIENTED_EDGE('',*,*,#23010,.F.);
#39160=ORIENTED_EDGE('',*,*,#23018,.F.);
#39161=ORIENTED_EDGE('',*,*,#27157,.T.);
#39162=ORIENTED_EDGE('',*,*,#23007,.F.);
#39163=ORIENTED_EDGE('',*,*,#27157,.F.);
#39164=ORIENTED_EDGE('',*,*,#23014,.F.);
#39165=ORIENTED_EDGE('',*,*,#22906,.F.);
#39166=ORIENTED_EDGE('',*,*,#27156,.T.);
#39167=ORIENTED_EDGE('',*,*,#22893,.F.);
#39168=ORIENTED_EDGE('',*,*,#22999,.F.);
#39169=ORIENTED_EDGE('',*,*,#27158,.F.);
#39170=ORIENTED_EDGE('',*,*,#22895,.F.);
#39171=ORIENTED_EDGE('',*,*,#22887,.F.);
#39172=ORIENTED_EDGE('',*,*,#22884,.F.);
#39173=ORIENTED_EDGE('',*,*,#22996,.F.);
#39174=ORIENTED_EDGE('',*,*,#23004,.F.);
#39175=ORIENTED_EDGE('',*,*,#27159,.T.);
#39176=ORIENTED_EDGE('',*,*,#22993,.F.);
#39177=ORIENTED_EDGE('',*,*,#27159,.F.);
#39178=ORIENTED_EDGE('',*,*,#23000,.F.);
#39179=ORIENTED_EDGE('',*,*,#22892,.F.);
#39180=ORIENTED_EDGE('',*,*,#27158,.T.);
#39181=ORIENTED_EDGE('',*,*,#22879,.F.);
#39182=ORIENTED_EDGE('',*,*,#22985,.F.);
#39183=ORIENTED_EDGE('',*,*,#27160,.F.);
#39184=ORIENTED_EDGE('',*,*,#22881,.F.);
#39185=ORIENTED_EDGE('',*,*,#22873,.F.);
#39186=ORIENTED_EDGE('',*,*,#22870,.F.);
#39187=ORIENTED_EDGE('',*,*,#22982,.F.);
#39188=ORIENTED_EDGE('',*,*,#22990,.F.);
#39189=ORIENTED_EDGE('',*,*,#27161,.T.);
#39190=ORIENTED_EDGE('',*,*,#22979,.F.);
#39191=ORIENTED_EDGE('',*,*,#27161,.F.);
#39192=ORIENTED_EDGE('',*,*,#22986,.F.);
#39193=ORIENTED_EDGE('',*,*,#22878,.F.);
#39194=ORIENTED_EDGE('',*,*,#27160,.T.);
#39195=ORIENTED_EDGE('',*,*,#22865,.F.);
#39196=ORIENTED_EDGE('',*,*,#22971,.F.);
#39197=ORIENTED_EDGE('',*,*,#27162,.F.);
#39198=ORIENTED_EDGE('',*,*,#22867,.F.);
#39199=ORIENTED_EDGE('',*,*,#22859,.F.);
#39200=ORIENTED_EDGE('',*,*,#22856,.F.);
#39201=ORIENTED_EDGE('',*,*,#22968,.F.);
#39202=ORIENTED_EDGE('',*,*,#22976,.F.);
#39203=ORIENTED_EDGE('',*,*,#27163,.T.);
#39204=ORIENTED_EDGE('',*,*,#22965,.F.);
#39205=ORIENTED_EDGE('',*,*,#27163,.F.);
#39206=ORIENTED_EDGE('',*,*,#22972,.F.);
#39207=ORIENTED_EDGE('',*,*,#22864,.F.);
#39208=ORIENTED_EDGE('',*,*,#27162,.T.);
#39209=ORIENTED_EDGE('',*,*,#22850,.F.);
#39210=ORIENTED_EDGE('',*,*,#22957,.F.);
#39211=ORIENTED_EDGE('',*,*,#27164,.F.);
#39212=ORIENTED_EDGE('',*,*,#22852,.F.);
#39213=ORIENTED_EDGE('',*,*,#22844,.F.);
#39214=ORIENTED_EDGE('',*,*,#22841,.F.);
#39215=ORIENTED_EDGE('',*,*,#22954,.F.);
#39216=ORIENTED_EDGE('',*,*,#22962,.F.);
#39217=ORIENTED_EDGE('',*,*,#27165,.T.);
#39218=ORIENTED_EDGE('',*,*,#22951,.F.);
#39219=ORIENTED_EDGE('',*,*,#27165,.F.);
#39220=ORIENTED_EDGE('',*,*,#22958,.F.);
#39221=ORIENTED_EDGE('',*,*,#22849,.F.);
#39222=ORIENTED_EDGE('',*,*,#27164,.T.);
#39223=ORIENTED_EDGE('',*,*,#22838,.F.);
#39224=ORIENTED_EDGE('',*,*,#22942,.F.);
#39225=ORIENTED_EDGE('',*,*,#22931,.F.);
#39226=ORIENTED_EDGE('',*,*,#27166,.F.);
#39227=ORIENTED_EDGE('',*,*,#22943,.F.);
#39228=ORIENTED_EDGE('',*,*,#22837,.F.);
#39229=ORIENTED_EDGE('',*,*,#27167,.T.);
#39230=ORIENTED_EDGE('',*,*,#21428,.F.);
#39231=ORIENTED_EDGE('',*,*,#22939,.F.);
#39232=ORIENTED_EDGE('',*,*,#22947,.F.);
#39233=ORIENTED_EDGE('',*,*,#27166,.T.);
#39234=ORIENTED_EDGE('',*,*,#22936,.F.);
#39235=ORIENTED_EDGE('',*,*,#27167,.F.);
#39236=ORIENTED_EDGE('',*,*,#22949,.F.);
#39237=ORIENTED_EDGE('',*,*,#21429,.F.);
#39238=ORIENTED_EDGE('',*,*,#22829,.F.);
#39239=ORIENTED_EDGE('',*,*,#27168,.F.);
#39240=ORIENTED_EDGE('',*,*,#21683,.F.);
#39241=ORIENTED_EDGE('',*,*,#27168,.T.);
#39242=ORIENTED_EDGE('',*,*,#22825,.F.);
#39243=ORIENTED_EDGE('',*,*,#22926,.F.);
#39244=ORIENTED_EDGE('',*,*,#21684,.F.);
#39245=ORIENTED_EDGE('',*,*,#27169,.F.);
#39246=ORIENTED_EDGE('',*,*,#22827,.F.);
#39247=ORIENTED_EDGE('',*,*,#22819,.F.);
#39248=ORIENTED_EDGE('',*,*,#22816,.F.);
#39249=ORIENTED_EDGE('',*,*,#21687,.F.);
#39250=ORIENTED_EDGE('',*,*,#22929,.F.);
#39251=ORIENTED_EDGE('',*,*,#27170,.T.);
#39252=ORIENTED_EDGE('',*,*,#22924,.F.);
#39253=ORIENTED_EDGE('',*,*,#27170,.F.);
#39254=ORIENTED_EDGE('',*,*,#22927,.F.);
#39255=ORIENTED_EDGE('',*,*,#22824,.F.);
#39256=ORIENTED_EDGE('',*,*,#27169,.T.);
#39257=ORIENTED_EDGE('',*,*,#22811,.F.);
#39258=ORIENTED_EDGE('',*,*,#22917,.F.);
#39259=ORIENTED_EDGE('',*,*,#27171,.F.);
#39260=ORIENTED_EDGE('',*,*,#22813,.F.);
#39261=ORIENTED_EDGE('',*,*,#22805,.F.);
#39262=ORIENTED_EDGE('',*,*,#22802,.F.);
#39263=ORIENTED_EDGE('',*,*,#22914,.F.);
#39264=ORIENTED_EDGE('',*,*,#22922,.F.);
#39265=ORIENTED_EDGE('',*,*,#27172,.T.);
#39266=ORIENTED_EDGE('',*,*,#22911,.F.);
#39267=ORIENTED_EDGE('',*,*,#27172,.F.);
#39268=ORIENTED_EDGE('',*,*,#22918,.F.);
#39269=ORIENTED_EDGE('',*,*,#22810,.F.);
#39270=ORIENTED_EDGE('',*,*,#27171,.T.);
#39271=ORIENTED_EDGE('',*,*,#22797,.F.);
#39272=ORIENTED_EDGE('',*,*,#22903,.F.);
#39273=ORIENTED_EDGE('',*,*,#27173,.F.);
#39274=ORIENTED_EDGE('',*,*,#22799,.F.);
#39275=ORIENTED_EDGE('',*,*,#22791,.F.);
#39276=ORIENTED_EDGE('',*,*,#22788,.F.);
#39277=ORIENTED_EDGE('',*,*,#22900,.F.);
#39278=ORIENTED_EDGE('',*,*,#22908,.F.);
#39279=ORIENTED_EDGE('',*,*,#27174,.T.);
#39280=ORIENTED_EDGE('',*,*,#22897,.F.);
#39281=ORIENTED_EDGE('',*,*,#27174,.F.);
#39282=ORIENTED_EDGE('',*,*,#22904,.F.);
#39283=ORIENTED_EDGE('',*,*,#22796,.F.);
#39284=ORIENTED_EDGE('',*,*,#27173,.T.);
#39285=ORIENTED_EDGE('',*,*,#22783,.F.);
#39286=ORIENTED_EDGE('',*,*,#22889,.F.);
#39287=ORIENTED_EDGE('',*,*,#27175,.F.);
#39288=ORIENTED_EDGE('',*,*,#22785,.F.);
#39289=ORIENTED_EDGE('',*,*,#22777,.F.);
#39290=ORIENTED_EDGE('',*,*,#22774,.F.);
#39291=ORIENTED_EDGE('',*,*,#22886,.F.);
#39292=ORIENTED_EDGE('',*,*,#22894,.F.);
#39293=ORIENTED_EDGE('',*,*,#27176,.T.);
#39294=ORIENTED_EDGE('',*,*,#22883,.F.);
#39295=ORIENTED_EDGE('',*,*,#27176,.F.);
#39296=ORIENTED_EDGE('',*,*,#22890,.F.);
#39297=ORIENTED_EDGE('',*,*,#22782,.F.);
#39298=ORIENTED_EDGE('',*,*,#27175,.T.);
#39299=ORIENTED_EDGE('',*,*,#22769,.F.);
#39300=ORIENTED_EDGE('',*,*,#22875,.F.);
#39301=ORIENTED_EDGE('',*,*,#27177,.F.);
#39302=ORIENTED_EDGE('',*,*,#22771,.F.);
#39303=ORIENTED_EDGE('',*,*,#22763,.F.);
#39304=ORIENTED_EDGE('',*,*,#22760,.F.);
#39305=ORIENTED_EDGE('',*,*,#22872,.F.);
#39306=ORIENTED_EDGE('',*,*,#22880,.F.);
#39307=ORIENTED_EDGE('',*,*,#27178,.T.);
#39308=ORIENTED_EDGE('',*,*,#22869,.F.);
#39309=ORIENTED_EDGE('',*,*,#27178,.F.);
#39310=ORIENTED_EDGE('',*,*,#22876,.F.);
#39311=ORIENTED_EDGE('',*,*,#22768,.F.);
#39312=ORIENTED_EDGE('',*,*,#27177,.T.);
#39313=ORIENTED_EDGE('',*,*,#22754,.F.);
#39314=ORIENTED_EDGE('',*,*,#22861,.F.);
#39315=ORIENTED_EDGE('',*,*,#27179,.F.);
#39316=ORIENTED_EDGE('',*,*,#22756,.F.);
#39317=ORIENTED_EDGE('',*,*,#22748,.F.);
#39318=ORIENTED_EDGE('',*,*,#22745,.F.);
#39319=ORIENTED_EDGE('',*,*,#22858,.F.);
#39320=ORIENTED_EDGE('',*,*,#22866,.F.);
#39321=ORIENTED_EDGE('',*,*,#27180,.T.);
#39322=ORIENTED_EDGE('',*,*,#22855,.F.);
#39323=ORIENTED_EDGE('',*,*,#27180,.F.);
#39324=ORIENTED_EDGE('',*,*,#22862,.F.);
#39325=ORIENTED_EDGE('',*,*,#22753,.F.);
#39326=ORIENTED_EDGE('',*,*,#27179,.T.);
#39327=ORIENTED_EDGE('',*,*,#22742,.F.);
#39328=ORIENTED_EDGE('',*,*,#22846,.F.);
#39329=ORIENTED_EDGE('',*,*,#22835,.F.);
#39330=ORIENTED_EDGE('',*,*,#27181,.F.);
#39331=ORIENTED_EDGE('',*,*,#22847,.F.);
#39332=ORIENTED_EDGE('',*,*,#22741,.F.);
#39333=ORIENTED_EDGE('',*,*,#27182,.T.);
#39334=ORIENTED_EDGE('',*,*,#21432,.F.);
#39335=ORIENTED_EDGE('',*,*,#22843,.F.);
#39336=ORIENTED_EDGE('',*,*,#22851,.F.);
#39337=ORIENTED_EDGE('',*,*,#27181,.T.);
#39338=ORIENTED_EDGE('',*,*,#22840,.F.);
#39339=ORIENTED_EDGE('',*,*,#27182,.F.);
#39340=ORIENTED_EDGE('',*,*,#22853,.F.);
#39341=ORIENTED_EDGE('',*,*,#21433,.F.);
#39342=ORIENTED_EDGE('',*,*,#22733,.F.);
#39343=ORIENTED_EDGE('',*,*,#27183,.F.);
#39344=ORIENTED_EDGE('',*,*,#21677,.F.);
#39345=ORIENTED_EDGE('',*,*,#27183,.T.);
#39346=ORIENTED_EDGE('',*,*,#22729,.F.);
#39347=ORIENTED_EDGE('',*,*,#22830,.F.);
#39348=ORIENTED_EDGE('',*,*,#21678,.F.);
#39349=ORIENTED_EDGE('',*,*,#27184,.F.);
#39350=ORIENTED_EDGE('',*,*,#22731,.F.);
#39351=ORIENTED_EDGE('',*,*,#22723,.F.);
#39352=ORIENTED_EDGE('',*,*,#22720,.F.);
#39353=ORIENTED_EDGE('',*,*,#21681,.F.);
#39354=ORIENTED_EDGE('',*,*,#22833,.F.);
#39355=ORIENTED_EDGE('',*,*,#27185,.T.);
#39356=ORIENTED_EDGE('',*,*,#22828,.F.);
#39357=ORIENTED_EDGE('',*,*,#27185,.F.);
#39358=ORIENTED_EDGE('',*,*,#22831,.F.);
#39359=ORIENTED_EDGE('',*,*,#22728,.F.);
#39360=ORIENTED_EDGE('',*,*,#27184,.T.);
#39361=ORIENTED_EDGE('',*,*,#22715,.F.);
#39362=ORIENTED_EDGE('',*,*,#22821,.F.);
#39363=ORIENTED_EDGE('',*,*,#27186,.F.);
#39364=ORIENTED_EDGE('',*,*,#22717,.F.);
#39365=ORIENTED_EDGE('',*,*,#22709,.F.);
#39366=ORIENTED_EDGE('',*,*,#22706,.F.);
#39367=ORIENTED_EDGE('',*,*,#22818,.F.);
#39368=ORIENTED_EDGE('',*,*,#22826,.F.);
#39369=ORIENTED_EDGE('',*,*,#27187,.T.);
#39370=ORIENTED_EDGE('',*,*,#22815,.F.);
#39371=ORIENTED_EDGE('',*,*,#27187,.F.);
#39372=ORIENTED_EDGE('',*,*,#22822,.F.);
#39373=ORIENTED_EDGE('',*,*,#22714,.F.);
#39374=ORIENTED_EDGE('',*,*,#27186,.T.);
#39375=ORIENTED_EDGE('',*,*,#22701,.F.);
#39376=ORIENTED_EDGE('',*,*,#22807,.F.);
#39377=ORIENTED_EDGE('',*,*,#27188,.F.);
#39378=ORIENTED_EDGE('',*,*,#22703,.F.);
#39379=ORIENTED_EDGE('',*,*,#22695,.F.);
#39380=ORIENTED_EDGE('',*,*,#22692,.F.);
#39381=ORIENTED_EDGE('',*,*,#22804,.F.);
#39382=ORIENTED_EDGE('',*,*,#22812,.F.);
#39383=ORIENTED_EDGE('',*,*,#27189,.T.);
#39384=ORIENTED_EDGE('',*,*,#22801,.F.);
#39385=ORIENTED_EDGE('',*,*,#27189,.F.);
#39386=ORIENTED_EDGE('',*,*,#22808,.F.);
#39387=ORIENTED_EDGE('',*,*,#22700,.F.);
#39388=ORIENTED_EDGE('',*,*,#27188,.T.);
#39389=ORIENTED_EDGE('',*,*,#22687,.F.);
#39390=ORIENTED_EDGE('',*,*,#22793,.F.);
#39391=ORIENTED_EDGE('',*,*,#27190,.F.);
#39392=ORIENTED_EDGE('',*,*,#22689,.F.);
#39393=ORIENTED_EDGE('',*,*,#22681,.F.);
#39394=ORIENTED_EDGE('',*,*,#22678,.F.);
#39395=ORIENTED_EDGE('',*,*,#22790,.F.);
#39396=ORIENTED_EDGE('',*,*,#22798,.F.);
#39397=ORIENTED_EDGE('',*,*,#27191,.T.);
#39398=ORIENTED_EDGE('',*,*,#22787,.F.);
#39399=ORIENTED_EDGE('',*,*,#27191,.F.);
#39400=ORIENTED_EDGE('',*,*,#22794,.F.);
#39401=ORIENTED_EDGE('',*,*,#22686,.F.);
#39402=ORIENTED_EDGE('',*,*,#27190,.T.);
#39403=ORIENTED_EDGE('',*,*,#22673,.F.);
#39404=ORIENTED_EDGE('',*,*,#22779,.F.);
#39405=ORIENTED_EDGE('',*,*,#27192,.F.);
#39406=ORIENTED_EDGE('',*,*,#22675,.F.);
#39407=ORIENTED_EDGE('',*,*,#22667,.F.);
#39408=ORIENTED_EDGE('',*,*,#22664,.F.);
#39409=ORIENTED_EDGE('',*,*,#22776,.F.);
#39410=ORIENTED_EDGE('',*,*,#22784,.F.);
#39411=ORIENTED_EDGE('',*,*,#27193,.T.);
#39412=ORIENTED_EDGE('',*,*,#22773,.F.);
#39413=ORIENTED_EDGE('',*,*,#27193,.F.);
#39414=ORIENTED_EDGE('',*,*,#22780,.F.);
#39415=ORIENTED_EDGE('',*,*,#22672,.F.);
#39416=ORIENTED_EDGE('',*,*,#27192,.T.);
#39417=ORIENTED_EDGE('',*,*,#22658,.F.);
#39418=ORIENTED_EDGE('',*,*,#22765,.F.);
#39419=ORIENTED_EDGE('',*,*,#27194,.F.);
#39420=ORIENTED_EDGE('',*,*,#22660,.F.);
#39421=ORIENTED_EDGE('',*,*,#22652,.F.);
#39422=ORIENTED_EDGE('',*,*,#22649,.F.);
#39423=ORIENTED_EDGE('',*,*,#22762,.F.);
#39424=ORIENTED_EDGE('',*,*,#22770,.F.);
#39425=ORIENTED_EDGE('',*,*,#27195,.T.);
#39426=ORIENTED_EDGE('',*,*,#22759,.F.);
#39427=ORIENTED_EDGE('',*,*,#27195,.F.);
#39428=ORIENTED_EDGE('',*,*,#22766,.F.);
#39429=ORIENTED_EDGE('',*,*,#22657,.F.);
#39430=ORIENTED_EDGE('',*,*,#27194,.T.);
#39431=ORIENTED_EDGE('',*,*,#22646,.F.);
#39432=ORIENTED_EDGE('',*,*,#22750,.F.);
#39433=ORIENTED_EDGE('',*,*,#22739,.F.);
#39434=ORIENTED_EDGE('',*,*,#27196,.F.);
#39435=ORIENTED_EDGE('',*,*,#22751,.F.);
#39436=ORIENTED_EDGE('',*,*,#22645,.F.);
#39437=ORIENTED_EDGE('',*,*,#27197,.T.);
#39438=ORIENTED_EDGE('',*,*,#21436,.F.);
#39439=ORIENTED_EDGE('',*,*,#22747,.F.);
#39440=ORIENTED_EDGE('',*,*,#22755,.F.);
#39441=ORIENTED_EDGE('',*,*,#27196,.T.);
#39442=ORIENTED_EDGE('',*,*,#22744,.F.);
#39443=ORIENTED_EDGE('',*,*,#27197,.F.);
#39444=ORIENTED_EDGE('',*,*,#22757,.F.);
#39445=ORIENTED_EDGE('',*,*,#21437,.F.);
#39446=ORIENTED_EDGE('',*,*,#22637,.F.);
#39447=ORIENTED_EDGE('',*,*,#27198,.F.);
#39448=ORIENTED_EDGE('',*,*,#21671,.F.);
#39449=ORIENTED_EDGE('',*,*,#27198,.T.);
#39450=ORIENTED_EDGE('',*,*,#22633,.F.);
#39451=ORIENTED_EDGE('',*,*,#22734,.F.);
#39452=ORIENTED_EDGE('',*,*,#21672,.F.);
#39453=ORIENTED_EDGE('',*,*,#27199,.F.);
#39454=ORIENTED_EDGE('',*,*,#22635,.F.);
#39455=ORIENTED_EDGE('',*,*,#22627,.F.);
#39456=ORIENTED_EDGE('',*,*,#22624,.F.);
#39457=ORIENTED_EDGE('',*,*,#21675,.F.);
#39458=ORIENTED_EDGE('',*,*,#22737,.F.);
#39459=ORIENTED_EDGE('',*,*,#27200,.T.);
#39460=ORIENTED_EDGE('',*,*,#22732,.F.);
#39461=ORIENTED_EDGE('',*,*,#27200,.F.);
#39462=ORIENTED_EDGE('',*,*,#22735,.F.);
#39463=ORIENTED_EDGE('',*,*,#22632,.F.);
#39464=ORIENTED_EDGE('',*,*,#27199,.T.);
#39465=ORIENTED_EDGE('',*,*,#22619,.F.);
#39466=ORIENTED_EDGE('',*,*,#22725,.F.);
#39467=ORIENTED_EDGE('',*,*,#27201,.F.);
#39468=ORIENTED_EDGE('',*,*,#22621,.F.);
#39469=ORIENTED_EDGE('',*,*,#22613,.F.);
#39470=ORIENTED_EDGE('',*,*,#22610,.F.);
#39471=ORIENTED_EDGE('',*,*,#22722,.F.);
#39472=ORIENTED_EDGE('',*,*,#22730,.F.);
#39473=ORIENTED_EDGE('',*,*,#27202,.T.);
#39474=ORIENTED_EDGE('',*,*,#22719,.F.);
#39475=ORIENTED_EDGE('',*,*,#27202,.F.);
#39476=ORIENTED_EDGE('',*,*,#22726,.F.);
#39477=ORIENTED_EDGE('',*,*,#22618,.F.);
#39478=ORIENTED_EDGE('',*,*,#27201,.T.);
#39479=ORIENTED_EDGE('',*,*,#22605,.F.);
#39480=ORIENTED_EDGE('',*,*,#22711,.F.);
#39481=ORIENTED_EDGE('',*,*,#27203,.F.);
#39482=ORIENTED_EDGE('',*,*,#22607,.F.);
#39483=ORIENTED_EDGE('',*,*,#22599,.F.);
#39484=ORIENTED_EDGE('',*,*,#22596,.F.);
#39485=ORIENTED_EDGE('',*,*,#22708,.F.);
#39486=ORIENTED_EDGE('',*,*,#22716,.F.);
#39487=ORIENTED_EDGE('',*,*,#27204,.T.);
#39488=ORIENTED_EDGE('',*,*,#22705,.F.);
#39489=ORIENTED_EDGE('',*,*,#27204,.F.);
#39490=ORIENTED_EDGE('',*,*,#22712,.F.);
#39491=ORIENTED_EDGE('',*,*,#22604,.F.);
#39492=ORIENTED_EDGE('',*,*,#27203,.T.);
#39493=ORIENTED_EDGE('',*,*,#22591,.F.);
#39494=ORIENTED_EDGE('',*,*,#22697,.F.);
#39495=ORIENTED_EDGE('',*,*,#27205,.F.);
#39496=ORIENTED_EDGE('',*,*,#22593,.F.);
#39497=ORIENTED_EDGE('',*,*,#22585,.F.);
#39498=ORIENTED_EDGE('',*,*,#22582,.F.);
#39499=ORIENTED_EDGE('',*,*,#22694,.F.);
#39500=ORIENTED_EDGE('',*,*,#22702,.F.);
#39501=ORIENTED_EDGE('',*,*,#27206,.T.);
#39502=ORIENTED_EDGE('',*,*,#22691,.F.);
#39503=ORIENTED_EDGE('',*,*,#27206,.F.);
#39504=ORIENTED_EDGE('',*,*,#22698,.F.);
#39505=ORIENTED_EDGE('',*,*,#22590,.F.);
#39506=ORIENTED_EDGE('',*,*,#27205,.T.);
#39507=ORIENTED_EDGE('',*,*,#22577,.F.);
#39508=ORIENTED_EDGE('',*,*,#22683,.F.);
#39509=ORIENTED_EDGE('',*,*,#27207,.F.);
#39510=ORIENTED_EDGE('',*,*,#22579,.F.);
#39511=ORIENTED_EDGE('',*,*,#22571,.F.);
#39512=ORIENTED_EDGE('',*,*,#22568,.F.);
#39513=ORIENTED_EDGE('',*,*,#22680,.F.);
#39514=ORIENTED_EDGE('',*,*,#22688,.F.);
#39515=ORIENTED_EDGE('',*,*,#27208,.T.);
#39516=ORIENTED_EDGE('',*,*,#22677,.F.);
#39517=ORIENTED_EDGE('',*,*,#27208,.F.);
#39518=ORIENTED_EDGE('',*,*,#22684,.F.);
#39519=ORIENTED_EDGE('',*,*,#22576,.F.);
#39520=ORIENTED_EDGE('',*,*,#27207,.T.);
#39521=ORIENTED_EDGE('',*,*,#22562,.F.);
#39522=ORIENTED_EDGE('',*,*,#22669,.F.);
#39523=ORIENTED_EDGE('',*,*,#27209,.F.);
#39524=ORIENTED_EDGE('',*,*,#22564,.F.);
#39525=ORIENTED_EDGE('',*,*,#22556,.F.);
#39526=ORIENTED_EDGE('',*,*,#22553,.F.);
#39527=ORIENTED_EDGE('',*,*,#22666,.F.);
#39528=ORIENTED_EDGE('',*,*,#22674,.F.);
#39529=ORIENTED_EDGE('',*,*,#27210,.T.);
#39530=ORIENTED_EDGE('',*,*,#22663,.F.);
#39531=ORIENTED_EDGE('',*,*,#27210,.F.);
#39532=ORIENTED_EDGE('',*,*,#22670,.F.);
#39533=ORIENTED_EDGE('',*,*,#22561,.F.);
#39534=ORIENTED_EDGE('',*,*,#27209,.T.);
#39535=ORIENTED_EDGE('',*,*,#22550,.F.);
#39536=ORIENTED_EDGE('',*,*,#22654,.F.);
#39537=ORIENTED_EDGE('',*,*,#22643,.F.);
#39538=ORIENTED_EDGE('',*,*,#27211,.F.);
#39539=ORIENTED_EDGE('',*,*,#22655,.F.);
#39540=ORIENTED_EDGE('',*,*,#22549,.F.);
#39541=ORIENTED_EDGE('',*,*,#27212,.T.);
#39542=ORIENTED_EDGE('',*,*,#21440,.F.);
#39543=ORIENTED_EDGE('',*,*,#22651,.F.);
#39544=ORIENTED_EDGE('',*,*,#22659,.F.);
#39545=ORIENTED_EDGE('',*,*,#27211,.T.);
#39546=ORIENTED_EDGE('',*,*,#22648,.F.);
#39547=ORIENTED_EDGE('',*,*,#27212,.F.);
#39548=ORIENTED_EDGE('',*,*,#22661,.F.);
#39549=ORIENTED_EDGE('',*,*,#21441,.F.);
#39550=ORIENTED_EDGE('',*,*,#22541,.F.);
#39551=ORIENTED_EDGE('',*,*,#27213,.F.);
#39552=ORIENTED_EDGE('',*,*,#21665,.F.);
#39553=ORIENTED_EDGE('',*,*,#27213,.T.);
#39554=ORIENTED_EDGE('',*,*,#22537,.F.);
#39555=ORIENTED_EDGE('',*,*,#22638,.F.);
#39556=ORIENTED_EDGE('',*,*,#21666,.F.);
#39557=ORIENTED_EDGE('',*,*,#27214,.F.);
#39558=ORIENTED_EDGE('',*,*,#22539,.F.);
#39559=ORIENTED_EDGE('',*,*,#22531,.F.);
#39560=ORIENTED_EDGE('',*,*,#22528,.F.);
#39561=ORIENTED_EDGE('',*,*,#21669,.F.);
#39562=ORIENTED_EDGE('',*,*,#22641,.F.);
#39563=ORIENTED_EDGE('',*,*,#27215,.T.);
#39564=ORIENTED_EDGE('',*,*,#22636,.F.);
#39565=ORIENTED_EDGE('',*,*,#27215,.F.);
#39566=ORIENTED_EDGE('',*,*,#22639,.F.);
#39567=ORIENTED_EDGE('',*,*,#22536,.F.);
#39568=ORIENTED_EDGE('',*,*,#27214,.T.);
#39569=ORIENTED_EDGE('',*,*,#22523,.F.);
#39570=ORIENTED_EDGE('',*,*,#22629,.F.);
#39571=ORIENTED_EDGE('',*,*,#27216,.F.);
#39572=ORIENTED_EDGE('',*,*,#22525,.F.);
#39573=ORIENTED_EDGE('',*,*,#22517,.F.);
#39574=ORIENTED_EDGE('',*,*,#22514,.F.);
#39575=ORIENTED_EDGE('',*,*,#22626,.F.);
#39576=ORIENTED_EDGE('',*,*,#22634,.F.);
#39577=ORIENTED_EDGE('',*,*,#27217,.T.);
#39578=ORIENTED_EDGE('',*,*,#22623,.F.);
#39579=ORIENTED_EDGE('',*,*,#27217,.F.);
#39580=ORIENTED_EDGE('',*,*,#22630,.F.);
#39581=ORIENTED_EDGE('',*,*,#22522,.F.);
#39582=ORIENTED_EDGE('',*,*,#27216,.T.);
#39583=ORIENTED_EDGE('',*,*,#22509,.F.);
#39584=ORIENTED_EDGE('',*,*,#22615,.F.);
#39585=ORIENTED_EDGE('',*,*,#27218,.F.);
#39586=ORIENTED_EDGE('',*,*,#22511,.F.);
#39587=ORIENTED_EDGE('',*,*,#22503,.F.);
#39588=ORIENTED_EDGE('',*,*,#22500,.F.);
#39589=ORIENTED_EDGE('',*,*,#22612,.F.);
#39590=ORIENTED_EDGE('',*,*,#22620,.F.);
#39591=ORIENTED_EDGE('',*,*,#27219,.T.);
#39592=ORIENTED_EDGE('',*,*,#22609,.F.);
#39593=ORIENTED_EDGE('',*,*,#27219,.F.);
#39594=ORIENTED_EDGE('',*,*,#22616,.F.);
#39595=ORIENTED_EDGE('',*,*,#22508,.F.);
#39596=ORIENTED_EDGE('',*,*,#27218,.T.);
#39597=ORIENTED_EDGE('',*,*,#22495,.F.);
#39598=ORIENTED_EDGE('',*,*,#22601,.F.);
#39599=ORIENTED_EDGE('',*,*,#27220,.F.);
#39600=ORIENTED_EDGE('',*,*,#22497,.F.);
#39601=ORIENTED_EDGE('',*,*,#22489,.F.);
#39602=ORIENTED_EDGE('',*,*,#22486,.F.);
#39603=ORIENTED_EDGE('',*,*,#22598,.F.);
#39604=ORIENTED_EDGE('',*,*,#22606,.F.);
#39605=ORIENTED_EDGE('',*,*,#27221,.T.);
#39606=ORIENTED_EDGE('',*,*,#22595,.F.);
#39607=ORIENTED_EDGE('',*,*,#27221,.F.);
#39608=ORIENTED_EDGE('',*,*,#22602,.F.);
#39609=ORIENTED_EDGE('',*,*,#22494,.F.);
#39610=ORIENTED_EDGE('',*,*,#27220,.T.);
#39611=ORIENTED_EDGE('',*,*,#22481,.F.);
#39612=ORIENTED_EDGE('',*,*,#22587,.F.);
#39613=ORIENTED_EDGE('',*,*,#27222,.F.);
#39614=ORIENTED_EDGE('',*,*,#22483,.F.);
#39615=ORIENTED_EDGE('',*,*,#22475,.F.);
#39616=ORIENTED_EDGE('',*,*,#22472,.F.);
#39617=ORIENTED_EDGE('',*,*,#22584,.F.);
#39618=ORIENTED_EDGE('',*,*,#22592,.F.);
#39619=ORIENTED_EDGE('',*,*,#27223,.T.);
#39620=ORIENTED_EDGE('',*,*,#22581,.F.);
#39621=ORIENTED_EDGE('',*,*,#27223,.F.);
#39622=ORIENTED_EDGE('',*,*,#22588,.F.);
#39623=ORIENTED_EDGE('',*,*,#22480,.F.);
#39624=ORIENTED_EDGE('',*,*,#27222,.T.);
#39625=ORIENTED_EDGE('',*,*,#22466,.F.);
#39626=ORIENTED_EDGE('',*,*,#22573,.F.);
#39627=ORIENTED_EDGE('',*,*,#27224,.F.);
#39628=ORIENTED_EDGE('',*,*,#22468,.F.);
#39629=ORIENTED_EDGE('',*,*,#22460,.F.);
#39630=ORIENTED_EDGE('',*,*,#22457,.F.);
#39631=ORIENTED_EDGE('',*,*,#22570,.F.);
#39632=ORIENTED_EDGE('',*,*,#22578,.F.);
#39633=ORIENTED_EDGE('',*,*,#27225,.T.);
#39634=ORIENTED_EDGE('',*,*,#22567,.F.);
#39635=ORIENTED_EDGE('',*,*,#27225,.F.);
#39636=ORIENTED_EDGE('',*,*,#22574,.F.);
#39637=ORIENTED_EDGE('',*,*,#22465,.F.);
#39638=ORIENTED_EDGE('',*,*,#27224,.T.);
#39639=ORIENTED_EDGE('',*,*,#22454,.F.);
#39640=ORIENTED_EDGE('',*,*,#22558,.F.);
#39641=ORIENTED_EDGE('',*,*,#22547,.F.);
#39642=ORIENTED_EDGE('',*,*,#27226,.F.);
#39643=ORIENTED_EDGE('',*,*,#22559,.F.);
#39644=ORIENTED_EDGE('',*,*,#22453,.F.);
#39645=ORIENTED_EDGE('',*,*,#27227,.T.);
#39646=ORIENTED_EDGE('',*,*,#21444,.F.);
#39647=ORIENTED_EDGE('',*,*,#22555,.F.);
#39648=ORIENTED_EDGE('',*,*,#22563,.F.);
#39649=ORIENTED_EDGE('',*,*,#27226,.T.);
#39650=ORIENTED_EDGE('',*,*,#22552,.F.);
#39651=ORIENTED_EDGE('',*,*,#27227,.F.);
#39652=ORIENTED_EDGE('',*,*,#22565,.F.);
#39653=ORIENTED_EDGE('',*,*,#21445,.F.);
#39654=ORIENTED_EDGE('',*,*,#27228,.F.);
#39655=ORIENTED_EDGE('',*,*,#22445,.F.);
#39656=ORIENTED_EDGE('',*,*,#22443,.F.);
#39657=ORIENTED_EDGE('',*,*,#22432,.F.);
#39658=ORIENTED_EDGE('',*,*,#21663,.F.);
#39659=ORIENTED_EDGE('',*,*,#22545,.F.);
#39660=ORIENTED_EDGE('',*,*,#27229,.T.);
#39661=ORIENTED_EDGE('',*,*,#22540,.F.);
#39662=ORIENTED_EDGE('',*,*,#27229,.F.);
#39663=ORIENTED_EDGE('',*,*,#22543,.F.);
#39664=ORIENTED_EDGE('',*,*,#22437,.F.);
#39665=ORIENTED_EDGE('',*,*,#27228,.T.);
#39666=ORIENTED_EDGE('',*,*,#22427,.F.);
#39667=ORIENTED_EDGE('',*,*,#22533,.F.);
#39668=ORIENTED_EDGE('',*,*,#22440,.F.);
#39669=ORIENTED_EDGE('',*,*,#27230,.F.);
#39670=ORIENTED_EDGE('',*,*,#21659,.F.);
#39671=ORIENTED_EDGE('',*,*,#27230,.T.);
#39672=ORIENTED_EDGE('',*,*,#22438,.F.);
#39673=ORIENTED_EDGE('',*,*,#22542,.F.);
#39674=ORIENTED_EDGE('',*,*,#21660,.F.);
#39675=ORIENTED_EDGE('',*,*,#27231,.F.);
#39676=ORIENTED_EDGE('',*,*,#22429,.F.);
#39677=ORIENTED_EDGE('',*,*,#22421,.F.);
#39678=ORIENTED_EDGE('',*,*,#22418,.F.);
#39679=ORIENTED_EDGE('',*,*,#22530,.F.);
#39680=ORIENTED_EDGE('',*,*,#22538,.F.);
#39681=ORIENTED_EDGE('',*,*,#27232,.T.);
#39682=ORIENTED_EDGE('',*,*,#22527,.F.);
#39683=ORIENTED_EDGE('',*,*,#27232,.F.);
#39684=ORIENTED_EDGE('',*,*,#22534,.F.);
#39685=ORIENTED_EDGE('',*,*,#22426,.F.);
#39686=ORIENTED_EDGE('',*,*,#27231,.T.);
#39687=ORIENTED_EDGE('',*,*,#22413,.F.);
#39688=ORIENTED_EDGE('',*,*,#22519,.F.);
#39689=ORIENTED_EDGE('',*,*,#27233,.F.);
#39690=ORIENTED_EDGE('',*,*,#22415,.F.);
#39691=ORIENTED_EDGE('',*,*,#22407,.F.);
#39692=ORIENTED_EDGE('',*,*,#22404,.F.);
#39693=ORIENTED_EDGE('',*,*,#22516,.F.);
#39694=ORIENTED_EDGE('',*,*,#22524,.F.);
#39695=ORIENTED_EDGE('',*,*,#27234,.T.);
#39696=ORIENTED_EDGE('',*,*,#22513,.F.);
#39697=ORIENTED_EDGE('',*,*,#27234,.F.);
#39698=ORIENTED_EDGE('',*,*,#22520,.F.);
#39699=ORIENTED_EDGE('',*,*,#22412,.F.);
#39700=ORIENTED_EDGE('',*,*,#27233,.T.);
#39701=ORIENTED_EDGE('',*,*,#22399,.F.);
#39702=ORIENTED_EDGE('',*,*,#22505,.F.);
#39703=ORIENTED_EDGE('',*,*,#27235,.F.);
#39704=ORIENTED_EDGE('',*,*,#22401,.F.);
#39705=ORIENTED_EDGE('',*,*,#22393,.F.);
#39706=ORIENTED_EDGE('',*,*,#22390,.F.);
#39707=ORIENTED_EDGE('',*,*,#22502,.F.);
#39708=ORIENTED_EDGE('',*,*,#22510,.F.);
#39709=ORIENTED_EDGE('',*,*,#27236,.T.);
#39710=ORIENTED_EDGE('',*,*,#22499,.F.);
#39711=ORIENTED_EDGE('',*,*,#27236,.F.);
#39712=ORIENTED_EDGE('',*,*,#22506,.F.);
#39713=ORIENTED_EDGE('',*,*,#22398,.F.);
#39714=ORIENTED_EDGE('',*,*,#27235,.T.);
#39715=ORIENTED_EDGE('',*,*,#22385,.F.);
#39716=ORIENTED_EDGE('',*,*,#22491,.F.);
#39717=ORIENTED_EDGE('',*,*,#27237,.F.);
#39718=ORIENTED_EDGE('',*,*,#22387,.F.);
#39719=ORIENTED_EDGE('',*,*,#22379,.F.);
#39720=ORIENTED_EDGE('',*,*,#22376,.F.);
#39721=ORIENTED_EDGE('',*,*,#22488,.F.);
#39722=ORIENTED_EDGE('',*,*,#22496,.F.);
#39723=ORIENTED_EDGE('',*,*,#27238,.T.);
#39724=ORIENTED_EDGE('',*,*,#22485,.F.);
#39725=ORIENTED_EDGE('',*,*,#27238,.F.);
#39726=ORIENTED_EDGE('',*,*,#22492,.F.);
#39727=ORIENTED_EDGE('',*,*,#22384,.F.);
#39728=ORIENTED_EDGE('',*,*,#27237,.T.);
#39729=ORIENTED_EDGE('',*,*,#22370,.F.);
#39730=ORIENTED_EDGE('',*,*,#22477,.F.);
#39731=ORIENTED_EDGE('',*,*,#27239,.F.);
#39732=ORIENTED_EDGE('',*,*,#22372,.F.);
#39733=ORIENTED_EDGE('',*,*,#22364,.F.);
#39734=ORIENTED_EDGE('',*,*,#22361,.F.);
#39735=ORIENTED_EDGE('',*,*,#22474,.F.);
#39736=ORIENTED_EDGE('',*,*,#22482,.F.);
#39737=ORIENTED_EDGE('',*,*,#27240,.T.);
#39738=ORIENTED_EDGE('',*,*,#22471,.F.);
#39739=ORIENTED_EDGE('',*,*,#27240,.F.);
#39740=ORIENTED_EDGE('',*,*,#22478,.F.);
#39741=ORIENTED_EDGE('',*,*,#22369,.F.);
#39742=ORIENTED_EDGE('',*,*,#27239,.T.);
#39743=ORIENTED_EDGE('',*,*,#22358,.F.);
#39744=ORIENTED_EDGE('',*,*,#22462,.F.);
#39745=ORIENTED_EDGE('',*,*,#22451,.F.);
#39746=ORIENTED_EDGE('',*,*,#27241,.F.);
#39747=ORIENTED_EDGE('',*,*,#22463,.F.);
#39748=ORIENTED_EDGE('',*,*,#22357,.F.);
#39749=ORIENTED_EDGE('',*,*,#27242,.T.);
#39750=ORIENTED_EDGE('',*,*,#21448,.F.);
#39751=ORIENTED_EDGE('',*,*,#22459,.F.);
#39752=ORIENTED_EDGE('',*,*,#22467,.F.);
#39753=ORIENTED_EDGE('',*,*,#27241,.T.);
#39754=ORIENTED_EDGE('',*,*,#22456,.F.);
#39755=ORIENTED_EDGE('',*,*,#27242,.F.);
#39756=ORIENTED_EDGE('',*,*,#22469,.F.);
#39757=ORIENTED_EDGE('',*,*,#21449,.F.);
#39758=ORIENTED_EDGE('',*,*,#22349,.F.);
#39759=ORIENTED_EDGE('',*,*,#27243,.F.);
#39760=ORIENTED_EDGE('',*,*,#21653,.F.);
#39761=ORIENTED_EDGE('',*,*,#27243,.T.);
#39762=ORIENTED_EDGE('',*,*,#22345,.F.);
#39763=ORIENTED_EDGE('',*,*,#22446,.F.);
#39764=ORIENTED_EDGE('',*,*,#21654,.F.);
#39765=ORIENTED_EDGE('',*,*,#27244,.F.);
#39766=ORIENTED_EDGE('',*,*,#22347,.F.);
#39767=ORIENTED_EDGE('',*,*,#22339,.F.);
#39768=ORIENTED_EDGE('',*,*,#22331,.F.);
#39769=ORIENTED_EDGE('',*,*,#21657,.F.);
#39770=ORIENTED_EDGE('',*,*,#22449,.F.);
#39771=ORIENTED_EDGE('',*,*,#27245,.T.);
#39772=ORIENTED_EDGE('',*,*,#22439,.F.);
#39773=ORIENTED_EDGE('',*,*,#27245,.F.);
#39774=ORIENTED_EDGE('',*,*,#22447,.F.);
#39775=ORIENTED_EDGE('',*,*,#22344,.F.);
#39776=ORIENTED_EDGE('',*,*,#27244,.T.);
#39777=ORIENTED_EDGE('',*,*,#22328,.F.);
#39778=ORIENTED_EDGE('',*,*,#22434,.F.);
#39779=ORIENTED_EDGE('',*,*,#27246,.F.);
#39780=ORIENTED_EDGE('',*,*,#22336,.F.);
#39781=ORIENTED_EDGE('',*,*,#22334,.F.);
#39782=ORIENTED_EDGE('',*,*,#22322,.F.);
#39783=ORIENTED_EDGE('',*,*,#22442,.F.);
#39784=ORIENTED_EDGE('',*,*,#22444,.F.);
#39785=ORIENTED_EDGE('',*,*,#27247,.T.);
#39786=ORIENTED_EDGE('',*,*,#22431,.F.);
#39787=ORIENTED_EDGE('',*,*,#27247,.F.);
#39788=ORIENTED_EDGE('',*,*,#22435,.F.);
#39789=ORIENTED_EDGE('',*,*,#22327,.F.);
#39790=ORIENTED_EDGE('',*,*,#27246,.T.);
#39791=ORIENTED_EDGE('',*,*,#22317,.F.);
#39792=ORIENTED_EDGE('',*,*,#22423,.F.);
#39793=ORIENTED_EDGE('',*,*,#27248,.F.);
#39794=ORIENTED_EDGE('',*,*,#22319,.F.);
#39795=ORIENTED_EDGE('',*,*,#22311,.F.);
#39796=ORIENTED_EDGE('',*,*,#22308,.F.);
#39797=ORIENTED_EDGE('',*,*,#22420,.F.);
#39798=ORIENTED_EDGE('',*,*,#22428,.F.);
#39799=ORIENTED_EDGE('',*,*,#27249,.T.);
#39800=ORIENTED_EDGE('',*,*,#22417,.F.);
#39801=ORIENTED_EDGE('',*,*,#27249,.F.);
#39802=ORIENTED_EDGE('',*,*,#22424,.F.);
#39803=ORIENTED_EDGE('',*,*,#22316,.F.);
#39804=ORIENTED_EDGE('',*,*,#27248,.T.);
#39805=ORIENTED_EDGE('',*,*,#22303,.F.);
#39806=ORIENTED_EDGE('',*,*,#22409,.F.);
#39807=ORIENTED_EDGE('',*,*,#27250,.F.);
#39808=ORIENTED_EDGE('',*,*,#22305,.F.);
#39809=ORIENTED_EDGE('',*,*,#22297,.F.);
#39810=ORIENTED_EDGE('',*,*,#22294,.F.);
#39811=ORIENTED_EDGE('',*,*,#22406,.F.);
#39812=ORIENTED_EDGE('',*,*,#22414,.F.);
#39813=ORIENTED_EDGE('',*,*,#27251,.T.);
#39814=ORIENTED_EDGE('',*,*,#22403,.F.);
#39815=ORIENTED_EDGE('',*,*,#27251,.F.);
#39816=ORIENTED_EDGE('',*,*,#22410,.F.);
#39817=ORIENTED_EDGE('',*,*,#22302,.F.);
#39818=ORIENTED_EDGE('',*,*,#27250,.T.);
#39819=ORIENTED_EDGE('',*,*,#22289,.F.);
#39820=ORIENTED_EDGE('',*,*,#22395,.F.);
#39821=ORIENTED_EDGE('',*,*,#27252,.F.);
#39822=ORIENTED_EDGE('',*,*,#22291,.F.);
#39823=ORIENTED_EDGE('',*,*,#22283,.F.);
#39824=ORIENTED_EDGE('',*,*,#22280,.F.);
#39825=ORIENTED_EDGE('',*,*,#22392,.F.);
#39826=ORIENTED_EDGE('',*,*,#22400,.F.);
#39827=ORIENTED_EDGE('',*,*,#27253,.T.);
#39828=ORIENTED_EDGE('',*,*,#22389,.F.);
#39829=ORIENTED_EDGE('',*,*,#27253,.F.);
#39830=ORIENTED_EDGE('',*,*,#22396,.F.);
#39831=ORIENTED_EDGE('',*,*,#22288,.F.);
#39832=ORIENTED_EDGE('',*,*,#27252,.T.);
#39833=ORIENTED_EDGE('',*,*,#22274,.F.);
#39834=ORIENTED_EDGE('',*,*,#22381,.F.);
#39835=ORIENTED_EDGE('',*,*,#27254,.F.);
#39836=ORIENTED_EDGE('',*,*,#22276,.F.);
#39837=ORIENTED_EDGE('',*,*,#22268,.F.);
#39838=ORIENTED_EDGE('',*,*,#22265,.F.);
#39839=ORIENTED_EDGE('',*,*,#22378,.F.);
#39840=ORIENTED_EDGE('',*,*,#22386,.F.);
#39841=ORIENTED_EDGE('',*,*,#27255,.T.);
#39842=ORIENTED_EDGE('',*,*,#22375,.F.);
#39843=ORIENTED_EDGE('',*,*,#27255,.F.);
#39844=ORIENTED_EDGE('',*,*,#22382,.F.);
#39845=ORIENTED_EDGE('',*,*,#22273,.F.);
#39846=ORIENTED_EDGE('',*,*,#27254,.T.);
#39847=ORIENTED_EDGE('',*,*,#22262,.F.);
#39848=ORIENTED_EDGE('',*,*,#22366,.F.);
#39849=ORIENTED_EDGE('',*,*,#22355,.F.);
#39850=ORIENTED_EDGE('',*,*,#27256,.F.);
#39851=ORIENTED_EDGE('',*,*,#22367,.F.);
#39852=ORIENTED_EDGE('',*,*,#22261,.F.);
#39853=ORIENTED_EDGE('',*,*,#27257,.T.);
#39854=ORIENTED_EDGE('',*,*,#21452,.F.);
#39855=ORIENTED_EDGE('',*,*,#22363,.F.);
#39856=ORIENTED_EDGE('',*,*,#22371,.F.);
#39857=ORIENTED_EDGE('',*,*,#27256,.T.);
#39858=ORIENTED_EDGE('',*,*,#22360,.F.);
#39859=ORIENTED_EDGE('',*,*,#27257,.F.);
#39860=ORIENTED_EDGE('',*,*,#22373,.F.);
#39861=ORIENTED_EDGE('',*,*,#21453,.F.);
#39862=ORIENTED_EDGE('',*,*,#22253,.F.);
#39863=ORIENTED_EDGE('',*,*,#27258,.F.);
#39864=ORIENTED_EDGE('',*,*,#21647,.F.);
#39865=ORIENTED_EDGE('',*,*,#27258,.T.);
#39866=ORIENTED_EDGE('',*,*,#22249,.F.);
#39867=ORIENTED_EDGE('',*,*,#22350,.F.);
#39868=ORIENTED_EDGE('',*,*,#21648,.F.);
#39869=ORIENTED_EDGE('',*,*,#27259,.F.);
#39870=ORIENTED_EDGE('',*,*,#22251,.F.);
#39871=ORIENTED_EDGE('',*,*,#22243,.F.);
#39872=ORIENTED_EDGE('',*,*,#22240,.F.);
#39873=ORIENTED_EDGE('',*,*,#21651,.F.);
#39874=ORIENTED_EDGE('',*,*,#22353,.F.);
#39875=ORIENTED_EDGE('',*,*,#27260,.T.);
#39876=ORIENTED_EDGE('',*,*,#22348,.F.);
#39877=ORIENTED_EDGE('',*,*,#27260,.F.);
#39878=ORIENTED_EDGE('',*,*,#22351,.F.);
#39879=ORIENTED_EDGE('',*,*,#22248,.F.);
#39880=ORIENTED_EDGE('',*,*,#27259,.T.);
#39881=ORIENTED_EDGE('',*,*,#22235,.F.);
#39882=ORIENTED_EDGE('',*,*,#22341,.F.);
#39883=ORIENTED_EDGE('',*,*,#27261,.F.);
#39884=ORIENTED_EDGE('',*,*,#22237,.F.);
#39885=ORIENTED_EDGE('',*,*,#22229,.F.);
#39886=ORIENTED_EDGE('',*,*,#22221,.F.);
#39887=ORIENTED_EDGE('',*,*,#22338,.F.);
#39888=ORIENTED_EDGE('',*,*,#22346,.F.);
#39889=ORIENTED_EDGE('',*,*,#27262,.T.);
#39890=ORIENTED_EDGE('',*,*,#22330,.F.);
#39891=ORIENTED_EDGE('',*,*,#27262,.F.);
#39892=ORIENTED_EDGE('',*,*,#22342,.F.);
#39893=ORIENTED_EDGE('',*,*,#22234,.F.);
#39894=ORIENTED_EDGE('',*,*,#27261,.T.);
#39895=ORIENTED_EDGE('',*,*,#22218,.F.);
#39896=ORIENTED_EDGE('',*,*,#22324,.F.);
#39897=ORIENTED_EDGE('',*,*,#27263,.F.);
#39898=ORIENTED_EDGE('',*,*,#22226,.F.);
#39899=ORIENTED_EDGE('',*,*,#22224,.F.);
#39900=ORIENTED_EDGE('',*,*,#22212,.F.);
#39901=ORIENTED_EDGE('',*,*,#22333,.F.);
#39902=ORIENTED_EDGE('',*,*,#22335,.F.);
#39903=ORIENTED_EDGE('',*,*,#27264,.T.);
#39904=ORIENTED_EDGE('',*,*,#22321,.F.);
#39905=ORIENTED_EDGE('',*,*,#27264,.F.);
#39906=ORIENTED_EDGE('',*,*,#22325,.F.);
#39907=ORIENTED_EDGE('',*,*,#22217,.F.);
#39908=ORIENTED_EDGE('',*,*,#27263,.T.);
#39909=ORIENTED_EDGE('',*,*,#22207,.F.);
#39910=ORIENTED_EDGE('',*,*,#22313,.F.);
#39911=ORIENTED_EDGE('',*,*,#27265,.F.);
#39912=ORIENTED_EDGE('',*,*,#22209,.F.);
#39913=ORIENTED_EDGE('',*,*,#22201,.F.);
#39914=ORIENTED_EDGE('',*,*,#22198,.F.);
#39915=ORIENTED_EDGE('',*,*,#22310,.F.);
#39916=ORIENTED_EDGE('',*,*,#22318,.F.);
#39917=ORIENTED_EDGE('',*,*,#27266,.T.);
#39918=ORIENTED_EDGE('',*,*,#22307,.F.);
#39919=ORIENTED_EDGE('',*,*,#27266,.F.);
#39920=ORIENTED_EDGE('',*,*,#22314,.F.);
#39921=ORIENTED_EDGE('',*,*,#22206,.F.);
#39922=ORIENTED_EDGE('',*,*,#27265,.T.);
#39923=ORIENTED_EDGE('',*,*,#22193,.F.);
#39924=ORIENTED_EDGE('',*,*,#22299,.F.);
#39925=ORIENTED_EDGE('',*,*,#27267,.F.);
#39926=ORIENTED_EDGE('',*,*,#22195,.F.);
#39927=ORIENTED_EDGE('',*,*,#22187,.F.);
#39928=ORIENTED_EDGE('',*,*,#22184,.F.);
#39929=ORIENTED_EDGE('',*,*,#22296,.F.);
#39930=ORIENTED_EDGE('',*,*,#22304,.F.);
#39931=ORIENTED_EDGE('',*,*,#27268,.T.);
#39932=ORIENTED_EDGE('',*,*,#22293,.F.);
#39933=ORIENTED_EDGE('',*,*,#27268,.F.);
#39934=ORIENTED_EDGE('',*,*,#22300,.F.);
#39935=ORIENTED_EDGE('',*,*,#22192,.F.);
#39936=ORIENTED_EDGE('',*,*,#27267,.T.);
#39937=ORIENTED_EDGE('',*,*,#22178,.F.);
#39938=ORIENTED_EDGE('',*,*,#22285,.F.);
#39939=ORIENTED_EDGE('',*,*,#27269,.F.);
#39940=ORIENTED_EDGE('',*,*,#22180,.F.);
#39941=ORIENTED_EDGE('',*,*,#22172,.F.);
#39942=ORIENTED_EDGE('',*,*,#22169,.F.);
#39943=ORIENTED_EDGE('',*,*,#22282,.F.);
#39944=ORIENTED_EDGE('',*,*,#22290,.F.);
#39945=ORIENTED_EDGE('',*,*,#27270,.T.);
#39946=ORIENTED_EDGE('',*,*,#22279,.F.);
#39947=ORIENTED_EDGE('',*,*,#27270,.F.);
#39948=ORIENTED_EDGE('',*,*,#22286,.F.);
#39949=ORIENTED_EDGE('',*,*,#22177,.F.);
#39950=ORIENTED_EDGE('',*,*,#27269,.T.);
#39951=ORIENTED_EDGE('',*,*,#22166,.F.);
#39952=ORIENTED_EDGE('',*,*,#22270,.F.);
#39953=ORIENTED_EDGE('',*,*,#22259,.F.);
#39954=ORIENTED_EDGE('',*,*,#27271,.F.);
#39955=ORIENTED_EDGE('',*,*,#22271,.F.);
#39956=ORIENTED_EDGE('',*,*,#22165,.F.);
#39957=ORIENTED_EDGE('',*,*,#27272,.T.);
#39958=ORIENTED_EDGE('',*,*,#21456,.F.);
#39959=ORIENTED_EDGE('',*,*,#22267,.F.);
#39960=ORIENTED_EDGE('',*,*,#22275,.F.);
#39961=ORIENTED_EDGE('',*,*,#27271,.T.);
#39962=ORIENTED_EDGE('',*,*,#22264,.F.);
#39963=ORIENTED_EDGE('',*,*,#27272,.F.);
#39964=ORIENTED_EDGE('',*,*,#22277,.F.);
#39965=ORIENTED_EDGE('',*,*,#21457,.F.);
#39966=ORIENTED_EDGE('',*,*,#22157,.F.);
#39967=ORIENTED_EDGE('',*,*,#27273,.F.);
#39968=ORIENTED_EDGE('',*,*,#21641,.F.);
#39969=ORIENTED_EDGE('',*,*,#27273,.T.);
#39970=ORIENTED_EDGE('',*,*,#22153,.F.);
#39971=ORIENTED_EDGE('',*,*,#22254,.F.);
#39972=ORIENTED_EDGE('',*,*,#21642,.F.);
#39973=ORIENTED_EDGE('',*,*,#27274,.F.);
#39974=ORIENTED_EDGE('',*,*,#22155,.F.);
#39975=ORIENTED_EDGE('',*,*,#22147,.F.);
#39976=ORIENTED_EDGE('',*,*,#22144,.F.);
#39977=ORIENTED_EDGE('',*,*,#21645,.F.);
#39978=ORIENTED_EDGE('',*,*,#22257,.F.);
#39979=ORIENTED_EDGE('',*,*,#27275,.T.);
#39980=ORIENTED_EDGE('',*,*,#22252,.F.);
#39981=ORIENTED_EDGE('',*,*,#27275,.F.);
#39982=ORIENTED_EDGE('',*,*,#22255,.F.);
#39983=ORIENTED_EDGE('',*,*,#22152,.F.);
#39984=ORIENTED_EDGE('',*,*,#27274,.T.);
#39985=ORIENTED_EDGE('',*,*,#22139,.F.);
#39986=ORIENTED_EDGE('',*,*,#22245,.F.);
#39987=ORIENTED_EDGE('',*,*,#27276,.F.);
#39988=ORIENTED_EDGE('',*,*,#22141,.F.);
#39989=ORIENTED_EDGE('',*,*,#22133,.F.);
#39990=ORIENTED_EDGE('',*,*,#22130,.F.);
#39991=ORIENTED_EDGE('',*,*,#22242,.F.);
#39992=ORIENTED_EDGE('',*,*,#22250,.F.);
#39993=ORIENTED_EDGE('',*,*,#27277,.T.);
#39994=ORIENTED_EDGE('',*,*,#22239,.F.);
#39995=ORIENTED_EDGE('',*,*,#27277,.F.);
#39996=ORIENTED_EDGE('',*,*,#22246,.F.);
#39997=ORIENTED_EDGE('',*,*,#22138,.F.);
#39998=ORIENTED_EDGE('',*,*,#27276,.T.);
#39999=ORIENTED_EDGE('',*,*,#22125,.F.);
#40000=ORIENTED_EDGE('',*,*,#22231,.F.);
#40001=ORIENTED_EDGE('',*,*,#27278,.F.);
#40002=ORIENTED_EDGE('',*,*,#22127,.F.);
#40003=ORIENTED_EDGE('',*,*,#22119,.F.);
#40004=ORIENTED_EDGE('',*,*,#22111,.F.);
#40005=ORIENTED_EDGE('',*,*,#22228,.F.);
#40006=ORIENTED_EDGE('',*,*,#22236,.F.);
#40007=ORIENTED_EDGE('',*,*,#27279,.T.);
#40008=ORIENTED_EDGE('',*,*,#22220,.F.);
#40009=ORIENTED_EDGE('',*,*,#27279,.F.);
#40010=ORIENTED_EDGE('',*,*,#22232,.F.);
#40011=ORIENTED_EDGE('',*,*,#22124,.F.);
#40012=ORIENTED_EDGE('',*,*,#27278,.T.);
#40013=ORIENTED_EDGE('',*,*,#22108,.F.);
#40014=ORIENTED_EDGE('',*,*,#22214,.F.);
#40015=ORIENTED_EDGE('',*,*,#27280,.F.);
#40016=ORIENTED_EDGE('',*,*,#22116,.F.);
#40017=ORIENTED_EDGE('',*,*,#22114,.F.);
#40018=ORIENTED_EDGE('',*,*,#22102,.F.);
#40019=ORIENTED_EDGE('',*,*,#22223,.F.);
#40020=ORIENTED_EDGE('',*,*,#22225,.F.);
#40021=ORIENTED_EDGE('',*,*,#27281,.T.);
#40022=ORIENTED_EDGE('',*,*,#22211,.F.);
#40023=ORIENTED_EDGE('',*,*,#27281,.F.);
#40024=ORIENTED_EDGE('',*,*,#22215,.F.);
#40025=ORIENTED_EDGE('',*,*,#22107,.F.);
#40026=ORIENTED_EDGE('',*,*,#27280,.T.);
#40027=ORIENTED_EDGE('',*,*,#22097,.F.);
#40028=ORIENTED_EDGE('',*,*,#22203,.F.);
#40029=ORIENTED_EDGE('',*,*,#27282,.F.);
#40030=ORIENTED_EDGE('',*,*,#22099,.F.);
#40031=ORIENTED_EDGE('',*,*,#22091,.F.);
#40032=ORIENTED_EDGE('',*,*,#22088,.F.);
#40033=ORIENTED_EDGE('',*,*,#22200,.F.);
#40034=ORIENTED_EDGE('',*,*,#22208,.F.);
#40035=ORIENTED_EDGE('',*,*,#27283,.T.);
#40036=ORIENTED_EDGE('',*,*,#22197,.F.);
#40037=ORIENTED_EDGE('',*,*,#27283,.F.);
#40038=ORIENTED_EDGE('',*,*,#22204,.F.);
#40039=ORIENTED_EDGE('',*,*,#22096,.F.);
#40040=ORIENTED_EDGE('',*,*,#27282,.T.);
#40041=ORIENTED_EDGE('',*,*,#22082,.F.);
#40042=ORIENTED_EDGE('',*,*,#22189,.F.);
#40043=ORIENTED_EDGE('',*,*,#27284,.F.);
#40044=ORIENTED_EDGE('',*,*,#22084,.F.);
#40045=ORIENTED_EDGE('',*,*,#22076,.F.);
#40046=ORIENTED_EDGE('',*,*,#22073,.F.);
#40047=ORIENTED_EDGE('',*,*,#22186,.F.);
#40048=ORIENTED_EDGE('',*,*,#22194,.F.);
#40049=ORIENTED_EDGE('',*,*,#27285,.T.);
#40050=ORIENTED_EDGE('',*,*,#22183,.F.);
#40051=ORIENTED_EDGE('',*,*,#27285,.F.);
#40052=ORIENTED_EDGE('',*,*,#22190,.F.);
#40053=ORIENTED_EDGE('',*,*,#22081,.F.);
#40054=ORIENTED_EDGE('',*,*,#27284,.T.);
#40055=ORIENTED_EDGE('',*,*,#22070,.F.);
#40056=ORIENTED_EDGE('',*,*,#22174,.F.);
#40057=ORIENTED_EDGE('',*,*,#22163,.F.);
#40058=ORIENTED_EDGE('',*,*,#27286,.F.);
#40059=ORIENTED_EDGE('',*,*,#22175,.F.);
#40060=ORIENTED_EDGE('',*,*,#22069,.F.);
#40061=ORIENTED_EDGE('',*,*,#27287,.T.);
#40062=ORIENTED_EDGE('',*,*,#21460,.F.);
#40063=ORIENTED_EDGE('',*,*,#22171,.F.);
#40064=ORIENTED_EDGE('',*,*,#22179,.F.);
#40065=ORIENTED_EDGE('',*,*,#27286,.T.);
#40066=ORIENTED_EDGE('',*,*,#22168,.F.);
#40067=ORIENTED_EDGE('',*,*,#27287,.F.);
#40068=ORIENTED_EDGE('',*,*,#22181,.F.);
#40069=ORIENTED_EDGE('',*,*,#21461,.F.);
#40070=ORIENTED_EDGE('',*,*,#22061,.F.);
#40071=ORIENTED_EDGE('',*,*,#27288,.F.);
#40072=ORIENTED_EDGE('',*,*,#21635,.F.);
#40073=ORIENTED_EDGE('',*,*,#27288,.T.);
#40074=ORIENTED_EDGE('',*,*,#22057,.F.);
#40075=ORIENTED_EDGE('',*,*,#22158,.F.);
#40076=ORIENTED_EDGE('',*,*,#21636,.F.);
#40077=ORIENTED_EDGE('',*,*,#27289,.F.);
#40078=ORIENTED_EDGE('',*,*,#22059,.F.);
#40079=ORIENTED_EDGE('',*,*,#22051,.F.);
#40080=ORIENTED_EDGE('',*,*,#22048,.F.);
#40081=ORIENTED_EDGE('',*,*,#21639,.F.);
#40082=ORIENTED_EDGE('',*,*,#22161,.F.);
#40083=ORIENTED_EDGE('',*,*,#27290,.T.);
#40084=ORIENTED_EDGE('',*,*,#22156,.F.);
#40085=ORIENTED_EDGE('',*,*,#27290,.F.);
#40086=ORIENTED_EDGE('',*,*,#22159,.F.);
#40087=ORIENTED_EDGE('',*,*,#22056,.F.);
#40088=ORIENTED_EDGE('',*,*,#27289,.T.);
#40089=ORIENTED_EDGE('',*,*,#22043,.F.);
#40090=ORIENTED_EDGE('',*,*,#22149,.F.);
#40091=ORIENTED_EDGE('',*,*,#27291,.F.);
#40092=ORIENTED_EDGE('',*,*,#22045,.F.);
#40093=ORIENTED_EDGE('',*,*,#22037,.F.);
#40094=ORIENTED_EDGE('',*,*,#22034,.F.);
#40095=ORIENTED_EDGE('',*,*,#22146,.F.);
#40096=ORIENTED_EDGE('',*,*,#22154,.F.);
#40097=ORIENTED_EDGE('',*,*,#27292,.T.);
#40098=ORIENTED_EDGE('',*,*,#22143,.F.);
#40099=ORIENTED_EDGE('',*,*,#27292,.F.);
#40100=ORIENTED_EDGE('',*,*,#22150,.F.);
#40101=ORIENTED_EDGE('',*,*,#22042,.F.);
#40102=ORIENTED_EDGE('',*,*,#27291,.T.);
#40103=ORIENTED_EDGE('',*,*,#22029,.F.);
#40104=ORIENTED_EDGE('',*,*,#22135,.F.);
#40105=ORIENTED_EDGE('',*,*,#27293,.F.);
#40106=ORIENTED_EDGE('',*,*,#22031,.F.);
#40107=ORIENTED_EDGE('',*,*,#22023,.F.);
#40108=ORIENTED_EDGE('',*,*,#22020,.F.);
#40109=ORIENTED_EDGE('',*,*,#22132,.F.);
#40110=ORIENTED_EDGE('',*,*,#22140,.F.);
#40111=ORIENTED_EDGE('',*,*,#27294,.T.);
#40112=ORIENTED_EDGE('',*,*,#22129,.F.);
#40113=ORIENTED_EDGE('',*,*,#27294,.F.);
#40114=ORIENTED_EDGE('',*,*,#22136,.F.);
#40115=ORIENTED_EDGE('',*,*,#22028,.F.);
#40116=ORIENTED_EDGE('',*,*,#27293,.T.);
#40117=ORIENTED_EDGE('',*,*,#22015,.F.);
#40118=ORIENTED_EDGE('',*,*,#22121,.F.);
#40119=ORIENTED_EDGE('',*,*,#27295,.F.);
#40120=ORIENTED_EDGE('',*,*,#22017,.F.);
#40121=ORIENTED_EDGE('',*,*,#22009,.F.);
#40122=ORIENTED_EDGE('',*,*,#22001,.F.);
#40123=ORIENTED_EDGE('',*,*,#22118,.F.);
#40124=ORIENTED_EDGE('',*,*,#22126,.F.);
#40125=ORIENTED_EDGE('',*,*,#27296,.T.);
#40126=ORIENTED_EDGE('',*,*,#22110,.F.);
#40127=ORIENTED_EDGE('',*,*,#27296,.F.);
#40128=ORIENTED_EDGE('',*,*,#22122,.F.);
#40129=ORIENTED_EDGE('',*,*,#22014,.F.);
#40130=ORIENTED_EDGE('',*,*,#27295,.T.);
#40131=ORIENTED_EDGE('',*,*,#21998,.F.);
#40132=ORIENTED_EDGE('',*,*,#22104,.F.);
#40133=ORIENTED_EDGE('',*,*,#27297,.F.);
#40134=ORIENTED_EDGE('',*,*,#22006,.F.);
#40135=ORIENTED_EDGE('',*,*,#22004,.F.);
#40136=ORIENTED_EDGE('',*,*,#21992,.F.);
#40137=ORIENTED_EDGE('',*,*,#22113,.F.);
#40138=ORIENTED_EDGE('',*,*,#22115,.F.);
#40139=ORIENTED_EDGE('',*,*,#27298,.T.);
#40140=ORIENTED_EDGE('',*,*,#22101,.F.);
#40141=ORIENTED_EDGE('',*,*,#27298,.F.);
#40142=ORIENTED_EDGE('',*,*,#22105,.F.);
#40143=ORIENTED_EDGE('',*,*,#21997,.F.);
#40144=ORIENTED_EDGE('',*,*,#27297,.T.);
#40145=ORIENTED_EDGE('',*,*,#21986,.F.);
#40146=ORIENTED_EDGE('',*,*,#22093,.F.);
#40147=ORIENTED_EDGE('',*,*,#27299,.F.);
#40148=ORIENTED_EDGE('',*,*,#21988,.F.);
#40149=ORIENTED_EDGE('',*,*,#21980,.F.);
#40150=ORIENTED_EDGE('',*,*,#21977,.F.);
#40151=ORIENTED_EDGE('',*,*,#22090,.F.);
#40152=ORIENTED_EDGE('',*,*,#22098,.F.);
#40153=ORIENTED_EDGE('',*,*,#27300,.T.);
#40154=ORIENTED_EDGE('',*,*,#22087,.F.);
#40155=ORIENTED_EDGE('',*,*,#27300,.F.);
#40156=ORIENTED_EDGE('',*,*,#22094,.F.);
#40157=ORIENTED_EDGE('',*,*,#21985,.F.);
#40158=ORIENTED_EDGE('',*,*,#27299,.T.);
#40159=ORIENTED_EDGE('',*,*,#21974,.F.);
#40160=ORIENTED_EDGE('',*,*,#22078,.F.);
#40161=ORIENTED_EDGE('',*,*,#22067,.F.);
#40162=ORIENTED_EDGE('',*,*,#27301,.F.);
#40163=ORIENTED_EDGE('',*,*,#22079,.F.);
#40164=ORIENTED_EDGE('',*,*,#21973,.F.);
#40165=ORIENTED_EDGE('',*,*,#27302,.T.);
#40166=ORIENTED_EDGE('',*,*,#21464,.F.);
#40167=ORIENTED_EDGE('',*,*,#22075,.F.);
#40168=ORIENTED_EDGE('',*,*,#22083,.F.);
#40169=ORIENTED_EDGE('',*,*,#27301,.T.);
#40170=ORIENTED_EDGE('',*,*,#22072,.F.);
#40171=ORIENTED_EDGE('',*,*,#27302,.F.);
#40172=ORIENTED_EDGE('',*,*,#22085,.F.);
#40173=ORIENTED_EDGE('',*,*,#21465,.F.);
#40174=ORIENTED_EDGE('',*,*,#21949,.F.);
#40175=ORIENTED_EDGE('',*,*,#27303,.F.);
#40176=ORIENTED_EDGE('',*,*,#21629,.F.);
#40177=ORIENTED_EDGE('',*,*,#27303,.T.);
#40178=ORIENTED_EDGE('',*,*,#21937,.F.);
#40179=ORIENTED_EDGE('',*,*,#22062,.F.);
#40180=ORIENTED_EDGE('',*,*,#21630,.F.);
#40181=ORIENTED_EDGE('',*,*,#27304,.F.);
#40182=ORIENTED_EDGE('',*,*,#21945,.F.);
#40183=ORIENTED_EDGE('',*,*,#21928,.F.);
#40184=ORIENTED_EDGE('',*,*,#21922,.F.);
#40185=ORIENTED_EDGE('',*,*,#21633,.F.);
#40186=ORIENTED_EDGE('',*,*,#22065,.F.);
#40187=ORIENTED_EDGE('',*,*,#27305,.T.);
#40188=ORIENTED_EDGE('',*,*,#22060,.F.);
#40189=ORIENTED_EDGE('',*,*,#27305,.F.);
#40190=ORIENTED_EDGE('',*,*,#22063,.F.);
#40191=ORIENTED_EDGE('',*,*,#21936,.F.);
#40192=ORIENTED_EDGE('',*,*,#27304,.T.);
#40193=ORIENTED_EDGE('',*,*,#21909,.F.);
#40194=ORIENTED_EDGE('',*,*,#22053,.F.);
#40195=ORIENTED_EDGE('',*,*,#27306,.F.);
#40196=ORIENTED_EDGE('',*,*,#21917,.F.);
#40197=ORIENTED_EDGE('',*,*,#21900,.F.);
#40198=ORIENTED_EDGE('',*,*,#21894,.F.);
#40199=ORIENTED_EDGE('',*,*,#22050,.F.);
#40200=ORIENTED_EDGE('',*,*,#22058,.F.);
#40201=ORIENTED_EDGE('',*,*,#27307,.T.);
#40202=ORIENTED_EDGE('',*,*,#22047,.F.);
#40203=ORIENTED_EDGE('',*,*,#27307,.F.);
#40204=ORIENTED_EDGE('',*,*,#22054,.F.);
#40205=ORIENTED_EDGE('',*,*,#21908,.F.);
#40206=ORIENTED_EDGE('',*,*,#27306,.T.);
#40207=ORIENTED_EDGE('',*,*,#21881,.F.);
#40208=ORIENTED_EDGE('',*,*,#22039,.F.);
#40209=ORIENTED_EDGE('',*,*,#27308,.F.);
#40210=ORIENTED_EDGE('',*,*,#21889,.F.);
#40211=ORIENTED_EDGE('',*,*,#21872,.F.);
#40212=ORIENTED_EDGE('',*,*,#21866,.F.);
#40213=ORIENTED_EDGE('',*,*,#22036,.F.);
#40214=ORIENTED_EDGE('',*,*,#22044,.F.);
#40215=ORIENTED_EDGE('',*,*,#27309,.T.);
#40216=ORIENTED_EDGE('',*,*,#22033,.F.);
#40217=ORIENTED_EDGE('',*,*,#27309,.F.);
#40218=ORIENTED_EDGE('',*,*,#22040,.F.);
#40219=ORIENTED_EDGE('',*,*,#21880,.F.);
#40220=ORIENTED_EDGE('',*,*,#27308,.T.);
#40221=ORIENTED_EDGE('',*,*,#21853,.F.);
#40222=ORIENTED_EDGE('',*,*,#22025,.F.);
#40223=ORIENTED_EDGE('',*,*,#27310,.F.);
#40224=ORIENTED_EDGE('',*,*,#21861,.F.);
#40225=ORIENTED_EDGE('',*,*,#21844,.F.);
#40226=ORIENTED_EDGE('',*,*,#21838,.F.);
#40227=ORIENTED_EDGE('',*,*,#22022,.F.);
#40228=ORIENTED_EDGE('',*,*,#22030,.F.);
#40229=ORIENTED_EDGE('',*,*,#27311,.T.);
#40230=ORIENTED_EDGE('',*,*,#22019,.F.);
#40231=ORIENTED_EDGE('',*,*,#27311,.F.);
#40232=ORIENTED_EDGE('',*,*,#22026,.F.);
#40233=ORIENTED_EDGE('',*,*,#21852,.F.);
#40234=ORIENTED_EDGE('',*,*,#27310,.T.);
#40235=ORIENTED_EDGE('',*,*,#21825,.F.);
#40236=ORIENTED_EDGE('',*,*,#22011,.F.);
#40237=ORIENTED_EDGE('',*,*,#27312,.F.);
#40238=ORIENTED_EDGE('',*,*,#21833,.F.);
#40239=ORIENTED_EDGE('',*,*,#21816,.F.);
#40240=ORIENTED_EDGE('',*,*,#21804,.F.);
#40241=ORIENTED_EDGE('',*,*,#22008,.F.);
#40242=ORIENTED_EDGE('',*,*,#22016,.F.);
#40243=ORIENTED_EDGE('',*,*,#27313,.T.);
#40244=ORIENTED_EDGE('',*,*,#22000,.F.);
#40245=ORIENTED_EDGE('',*,*,#27313,.F.);
#40246=ORIENTED_EDGE('',*,*,#22012,.F.);
#40247=ORIENTED_EDGE('',*,*,#21824,.F.);
#40248=ORIENTED_EDGE('',*,*,#27312,.T.);
#40249=ORIENTED_EDGE('',*,*,#21796,.F.);
#40250=ORIENTED_EDGE('',*,*,#21994,.F.);
#40251=ORIENTED_EDGE('',*,*,#27314,.F.);
#40252=ORIENTED_EDGE('',*,*,#21812,.F.);
#40253=ORIENTED_EDGE('',*,*,#21810,.F.);
#40254=ORIENTED_EDGE('',*,*,#21790,.F.);
#40255=ORIENTED_EDGE('',*,*,#22003,.F.);
#40256=ORIENTED_EDGE('',*,*,#22005,.F.);
#40257=ORIENTED_EDGE('',*,*,#27315,.T.);
#40258=ORIENTED_EDGE('',*,*,#21991,.F.);
#40259=ORIENTED_EDGE('',*,*,#27315,.F.);
#40260=ORIENTED_EDGE('',*,*,#21995,.F.);
#40261=ORIENTED_EDGE('',*,*,#21795,.F.);
#40262=ORIENTED_EDGE('',*,*,#27314,.T.);
#40263=ORIENTED_EDGE('',*,*,#21787,.F.);
#40264=ORIENTED_EDGE('',*,*,#21982,.F.);
#40265=ORIENTED_EDGE('',*,*,#21971,.F.);
#40266=ORIENTED_EDGE('',*,*,#27316,.F.);
#40267=ORIENTED_EDGE('',*,*,#21983,.F.);
#40268=ORIENTED_EDGE('',*,*,#21786,.F.);
#40269=ORIENTED_EDGE('',*,*,#27317,.T.);
#40270=ORIENTED_EDGE('',*,*,#21468,.F.);
#40271=ORIENTED_EDGE('',*,*,#21979,.F.);
#40272=ORIENTED_EDGE('',*,*,#21987,.F.);
#40273=ORIENTED_EDGE('',*,*,#27316,.T.);
#40274=ORIENTED_EDGE('',*,*,#21976,.F.);
#40275=ORIENTED_EDGE('',*,*,#27317,.F.);
#40276=ORIENTED_EDGE('',*,*,#21989,.F.);
#40277=ORIENTED_EDGE('',*,*,#21469,.F.);
#40278=ORIENTED_EDGE('',*,*,#21968,.F.);
#40279=ORIENTED_EDGE('',*,*,#27318,.F.);
#40280=ORIENTED_EDGE('',*,*,#21623,.F.);
#40281=ORIENTED_EDGE('',*,*,#27318,.T.);
#40282=ORIENTED_EDGE('',*,*,#21961,.F.);
#40283=ORIENTED_EDGE('',*,*,#21956,.F.);
#40284=ORIENTED_EDGE('',*,*,#21624,.F.);
#40285=ORIENTED_EDGE('',*,*,#27319,.F.);
#40286=ORIENTED_EDGE('',*,*,#21966,.F.);
#40287=ORIENTED_EDGE('',*,*,#21953,.F.);
#40288=ORIENTED_EDGE('',*,*,#21950,.F.);
#40289=ORIENTED_EDGE('',*,*,#21627,.F.);
#40290=ORIENTED_EDGE('',*,*,#21965,.F.);
#40291=ORIENTED_EDGE('',*,*,#27320,.T.);
#40292=ORIENTED_EDGE('',*,*,#21948,.F.);
#40293=ORIENTED_EDGE('',*,*,#27320,.F.);
#40294=ORIENTED_EDGE('',*,*,#21957,.F.);
#40295=ORIENTED_EDGE('',*,*,#21960,.F.);
#40296=ORIENTED_EDGE('',*,*,#27319,.T.);
#40297=ORIENTED_EDGE('',*,*,#21940,.F.);
#40298=ORIENTED_EDGE('',*,*,#21933,.F.);
#40299=ORIENTED_EDGE('',*,*,#27321,.F.);
#40300=ORIENTED_EDGE('',*,*,#21946,.F.);
#40301=ORIENTED_EDGE('',*,*,#21929,.F.);
#40302=ORIENTED_EDGE('',*,*,#21923,.F.);
#40303=ORIENTED_EDGE('',*,*,#21927,.F.);
#40304=ORIENTED_EDGE('',*,*,#21944,.F.);
#40305=ORIENTED_EDGE('',*,*,#27322,.T.);
#40306=ORIENTED_EDGE('',*,*,#21921,.F.);
#40307=ORIENTED_EDGE('',*,*,#27322,.F.);
#40308=ORIENTED_EDGE('',*,*,#21934,.F.);
#40309=ORIENTED_EDGE('',*,*,#21939,.F.);
#40310=ORIENTED_EDGE('',*,*,#27321,.T.);
#40311=ORIENTED_EDGE('',*,*,#21912,.F.);
#40312=ORIENTED_EDGE('',*,*,#21905,.F.);
#40313=ORIENTED_EDGE('',*,*,#27323,.F.);
#40314=ORIENTED_EDGE('',*,*,#21918,.F.);
#40315=ORIENTED_EDGE('',*,*,#21901,.F.);
#40316=ORIENTED_EDGE('',*,*,#21895,.F.);
#40317=ORIENTED_EDGE('',*,*,#21899,.F.);
#40318=ORIENTED_EDGE('',*,*,#21916,.F.);
#40319=ORIENTED_EDGE('',*,*,#27324,.T.);
#40320=ORIENTED_EDGE('',*,*,#21893,.F.);
#40321=ORIENTED_EDGE('',*,*,#27324,.F.);
#40322=ORIENTED_EDGE('',*,*,#21906,.F.);
#40323=ORIENTED_EDGE('',*,*,#21911,.F.);
#40324=ORIENTED_EDGE('',*,*,#27323,.T.);
#40325=ORIENTED_EDGE('',*,*,#21884,.F.);
#40326=ORIENTED_EDGE('',*,*,#21877,.F.);
#40327=ORIENTED_EDGE('',*,*,#27325,.F.);
#40328=ORIENTED_EDGE('',*,*,#21890,.F.);
#40329=ORIENTED_EDGE('',*,*,#21873,.F.);
#40330=ORIENTED_EDGE('',*,*,#21867,.F.);
#40331=ORIENTED_EDGE('',*,*,#21871,.F.);
#40332=ORIENTED_EDGE('',*,*,#21888,.F.);
#40333=ORIENTED_EDGE('',*,*,#27326,.T.);
#40334=ORIENTED_EDGE('',*,*,#21865,.F.);
#40335=ORIENTED_EDGE('',*,*,#27326,.F.);
#40336=ORIENTED_EDGE('',*,*,#21878,.F.);
#40337=ORIENTED_EDGE('',*,*,#21883,.F.);
#40338=ORIENTED_EDGE('',*,*,#27325,.T.);
#40339=ORIENTED_EDGE('',*,*,#21856,.F.);
#40340=ORIENTED_EDGE('',*,*,#21849,.F.);
#40341=ORIENTED_EDGE('',*,*,#27327,.F.);
#40342=ORIENTED_EDGE('',*,*,#21862,.F.);
#40343=ORIENTED_EDGE('',*,*,#21845,.F.);
#40344=ORIENTED_EDGE('',*,*,#21839,.F.);
#40345=ORIENTED_EDGE('',*,*,#21843,.F.);
#40346=ORIENTED_EDGE('',*,*,#21860,.F.);
#40347=ORIENTED_EDGE('',*,*,#27328,.T.);
#40348=ORIENTED_EDGE('',*,*,#21837,.F.);
#40349=ORIENTED_EDGE('',*,*,#27328,.F.);
#40350=ORIENTED_EDGE('',*,*,#21850,.F.);
#40351=ORIENTED_EDGE('',*,*,#21855,.F.);
#40352=ORIENTED_EDGE('',*,*,#27327,.T.);
#40353=ORIENTED_EDGE('',*,*,#21828,.F.);
#40354=ORIENTED_EDGE('',*,*,#21821,.F.);
#40355=ORIENTED_EDGE('',*,*,#27329,.F.);
#40356=ORIENTED_EDGE('',*,*,#21834,.F.);
#40357=ORIENTED_EDGE('',*,*,#21817,.F.);
#40358=ORIENTED_EDGE('',*,*,#21805,.F.);
#40359=ORIENTED_EDGE('',*,*,#21815,.F.);
#40360=ORIENTED_EDGE('',*,*,#21832,.F.);
#40361=ORIENTED_EDGE('',*,*,#27330,.T.);
#40362=ORIENTED_EDGE('',*,*,#21803,.F.);
#40363=ORIENTED_EDGE('',*,*,#27330,.F.);
#40364=ORIENTED_EDGE('',*,*,#21822,.F.);
#40365=ORIENTED_EDGE('',*,*,#21827,.F.);
#40366=ORIENTED_EDGE('',*,*,#27329,.T.);
#40367=ORIENTED_EDGE('',*,*,#21799,.F.);
#40368=ORIENTED_EDGE('',*,*,#21792,.F.);
#40369=ORIENTED_EDGE('',*,*,#21784,.F.);
#40370=ORIENTED_EDGE('',*,*,#27331,.F.);
#40371=ORIENTED_EDGE('',*,*,#21793,.F.);
#40372=ORIENTED_EDGE('',*,*,#21798,.F.);
#40373=ORIENTED_EDGE('',*,*,#27332,.T.);
#40374=ORIENTED_EDGE('',*,*,#21472,.F.);
#40375=ORIENTED_EDGE('',*,*,#21809,.F.);
#40376=ORIENTED_EDGE('',*,*,#21811,.F.);
#40377=ORIENTED_EDGE('',*,*,#27331,.T.);
#40378=ORIENTED_EDGE('',*,*,#21789,.F.);
#40379=ORIENTED_EDGE('',*,*,#27332,.F.);
#40380=ORIENTED_EDGE('',*,*,#21813,.F.);
#40381=ORIENTED_EDGE('',*,*,#21473,.F.);
#40382=ORIENTED_EDGE('',*,*,#27333,.F.);
#40383=ORIENTED_EDGE('',*,*,#27334,.T.);
#40384=ORIENTED_EDGE('',*,*,#27335,.T.);
#40385=ORIENTED_EDGE('',*,*,#27334,.F.);
#40386=ORIENTED_EDGE('',*,*,#27336,.T.);
#40387=ORIENTED_EDGE('',*,*,#27337,.T.);
#40388=ORIENTED_EDGE('',*,*,#27338,.F.);
#40389=ORIENTED_EDGE('',*,*,#27337,.F.);
#40390=ORIENTED_EDGE('',*,*,#27339,.T.);
#40391=ORIENTED_EDGE('',*,*,#27340,.T.);
#40392=ORIENTED_EDGE('',*,*,#27341,.F.);
#40393=ORIENTED_EDGE('',*,*,#27340,.F.);
#40394=ORIENTED_EDGE('',*,*,#27339,.F.);
#40395=ORIENTED_EDGE('',*,*,#27333,.T.);
#40396=ORIENTED_EDGE('',*,*,#27338,.T.);
#40397=ORIENTED_EDGE('',*,*,#27335,.F.);
#40398=ORIENTED_EDGE('',*,*,#27336,.F.);
#40399=ORIENTED_EDGE('',*,*,#27341,.T.);
#40400=ORIENTED_EDGE('',*,*,#27342,.F.);
#40401=ORIENTED_EDGE('',*,*,#27343,.T.);
#40402=ORIENTED_EDGE('',*,*,#27344,.T.);
#40403=ORIENTED_EDGE('',*,*,#27343,.F.);
#40404=ORIENTED_EDGE('',*,*,#27345,.T.);
#40405=ORIENTED_EDGE('',*,*,#27346,.T.);
#40406=ORIENTED_EDGE('',*,*,#27347,.F.);
#40407=ORIENTED_EDGE('',*,*,#27346,.F.);
#40408=ORIENTED_EDGE('',*,*,#27347,.T.);
#40409=ORIENTED_EDGE('',*,*,#27344,.F.);
#40410=ORIENTED_EDGE('',*,*,#27345,.F.);
#40411=ORIENTED_EDGE('',*,*,#27342,.T.);
#40412=ORIENTED_EDGE('',*,*,#27348,.T.);
#40413=ORIENTED_EDGE('',*,*,#27349,.T.);
#40414=ORIENTED_EDGE('',*,*,#27350,.F.);
#40415=ORIENTED_EDGE('',*,*,#27349,.F.);
#40416=ORIENTED_EDGE('',*,*,#27351,.T.);
#40417=ORIENTED_EDGE('',*,*,#27352,.T.);
#40418=ORIENTED_EDGE('',*,*,#27353,.F.);
#40419=ORIENTED_EDGE('',*,*,#27352,.F.);
#40420=ORIENTED_EDGE('',*,*,#27354,.F.);
#40421=ORIENTED_EDGE('',*,*,#27355,.T.);
#40422=ORIENTED_EDGE('',*,*,#27356,.T.);
#40423=ORIENTED_EDGE('',*,*,#27355,.F.);
#40424=ORIENTED_EDGE('',*,*,#27357,.F.);
#40425=ORIENTED_EDGE('',*,*,#27358,.T.);
#40426=ORIENTED_EDGE('',*,*,#27359,.T.);
#40427=ORIENTED_EDGE('',*,*,#27358,.F.);
#40428=ORIENTED_EDGE('',*,*,#27360,.T.);
#40429=ORIENTED_EDGE('',*,*,#27361,.F.);
#40430=ORIENTED_EDGE('',*,*,#27362,.F.);
#40431=ORIENTED_EDGE('',*,*,#27363,.T.);
#40432=ORIENTED_EDGE('',*,*,#27364,.F.);
#40433=ORIENTED_EDGE('',*,*,#27365,.T.);
#40434=ORIENTED_EDGE('',*,*,#27366,.T.);
#40435=ORIENTED_EDGE('',*,*,#27367,.F.);
#40436=ORIENTED_EDGE('',*,*,#27368,.F.);
#40437=ORIENTED_EDGE('',*,*,#27369,.T.);
#40438=ORIENTED_EDGE('',*,*,#27370,.T.);
#40439=ORIENTED_EDGE('',*,*,#27371,.F.);
#40440=ORIENTED_EDGE('',*,*,#27372,.F.);
#40441=ORIENTED_EDGE('',*,*,#27373,.T.);
#40442=ORIENTED_EDGE('',*,*,#27374,.T.);
#40443=ORIENTED_EDGE('',*,*,#27375,.F.);
#40444=ORIENTED_EDGE('',*,*,#27376,.F.);
#40445=ORIENTED_EDGE('',*,*,#27377,.T.);
#40446=ORIENTED_EDGE('',*,*,#27378,.T.);
#40447=ORIENTED_EDGE('',*,*,#27379,.F.);
#40448=ORIENTED_EDGE('',*,*,#27380,.F.);
#40449=ORIENTED_EDGE('',*,*,#27381,.T.);
#40450=ORIENTED_EDGE('',*,*,#27382,.T.);
#40451=ORIENTED_EDGE('',*,*,#27383,.F.);
#40452=ORIENTED_EDGE('',*,*,#27384,.F.);
#40453=ORIENTED_EDGE('',*,*,#27385,.T.);
#40454=ORIENTED_EDGE('',*,*,#27386,.T.);
#40455=ORIENTED_EDGE('',*,*,#27387,.F.);
#40456=ORIENTED_EDGE('',*,*,#27388,.F.);
#40457=ORIENTED_EDGE('',*,*,#27389,.T.);
#40458=ORIENTED_EDGE('',*,*,#27390,.T.);
#40459=ORIENTED_EDGE('',*,*,#27391,.F.);
#40460=ORIENTED_EDGE('',*,*,#27392,.F.);
#40461=ORIENTED_EDGE('',*,*,#27393,.T.);
#40462=ORIENTED_EDGE('',*,*,#27394,.T.);
#40463=ORIENTED_EDGE('',*,*,#27395,.F.);
#40464=ORIENTED_EDGE('',*,*,#27396,.F.);
#40465=ORIENTED_EDGE('',*,*,#27397,.T.);
#40466=ORIENTED_EDGE('',*,*,#27398,.T.);
#40467=ORIENTED_EDGE('',*,*,#27399,.F.);
#40468=ORIENTED_EDGE('',*,*,#27400,.F.);
#40469=ORIENTED_EDGE('',*,*,#27401,.T.);
#40470=ORIENTED_EDGE('',*,*,#27402,.T.);
#40471=ORIENTED_EDGE('',*,*,#27403,.F.);
#40472=ORIENTED_EDGE('',*,*,#27404,.F.);
#40473=ORIENTED_EDGE('',*,*,#27405,.T.);
#40474=ORIENTED_EDGE('',*,*,#27406,.T.);
#40475=ORIENTED_EDGE('',*,*,#27407,.F.);
#40476=ORIENTED_EDGE('',*,*,#27408,.F.);
#40477=ORIENTED_EDGE('',*,*,#27409,.T.);
#40478=ORIENTED_EDGE('',*,*,#27410,.T.);
#40479=ORIENTED_EDGE('',*,*,#27411,.F.);
#40480=ORIENTED_EDGE('',*,*,#27412,.F.);
#40481=ORIENTED_EDGE('',*,*,#27413,.T.);
#40482=ORIENTED_EDGE('',*,*,#27414,.T.);
#40483=ORIENTED_EDGE('',*,*,#27415,.F.);
#40484=ORIENTED_EDGE('',*,*,#27416,.F.);
#40485=ORIENTED_EDGE('',*,*,#27417,.T.);
#40486=ORIENTED_EDGE('',*,*,#27418,.T.);
#40487=ORIENTED_EDGE('',*,*,#27419,.F.);
#40488=ORIENTED_EDGE('',*,*,#27420,.F.);
#40489=ORIENTED_EDGE('',*,*,#27421,.T.);
#40490=ORIENTED_EDGE('',*,*,#27422,.T.);
#40491=ORIENTED_EDGE('',*,*,#27423,.F.);
#40492=ORIENTED_EDGE('',*,*,#27424,.T.);
#40493=ORIENTED_EDGE('',*,*,#27425,.F.);
#40494=ORIENTED_EDGE('',*,*,#27426,.F.);
#40495=ORIENTED_EDGE('',*,*,#27427,.T.);
#40496=ORIENTED_EDGE('',*,*,#27428,.T.);
#40497=ORIENTED_EDGE('',*,*,#27429,.F.);
#40498=ORIENTED_EDGE('',*,*,#27430,.F.);
#40499=ORIENTED_EDGE('',*,*,#27431,.T.);
#40500=ORIENTED_EDGE('',*,*,#27432,.T.);
#40501=ORIENTED_EDGE('',*,*,#27433,.F.);
#40502=ORIENTED_EDGE('',*,*,#27434,.F.);
#40503=ORIENTED_EDGE('',*,*,#27435,.T.);
#40504=ORIENTED_EDGE('',*,*,#27436,.F.);
#40505=ORIENTED_EDGE('',*,*,#27437,.T.);
#40506=ORIENTED_EDGE('',*,*,#27438,.T.);
#40507=ORIENTED_EDGE('',*,*,#27439,.F.);
#40508=ORIENTED_EDGE('',*,*,#27440,.F.);
#40509=ORIENTED_EDGE('',*,*,#27441,.T.);
#40510=ORIENTED_EDGE('',*,*,#27442,.T.);
#40511=ORIENTED_EDGE('',*,*,#27443,.F.);
#40512=ORIENTED_EDGE('',*,*,#27444,.F.);
#40513=ORIENTED_EDGE('',*,*,#27445,.T.);
#40514=ORIENTED_EDGE('',*,*,#27446,.T.);
#40515=ORIENTED_EDGE('',*,*,#27447,.F.);
#40516=ORIENTED_EDGE('',*,*,#27448,.F.);
#40517=ORIENTED_EDGE('',*,*,#27449,.T.);
#40518=ORIENTED_EDGE('',*,*,#27450,.T.);
#40519=ORIENTED_EDGE('',*,*,#27451,.F.);
#40520=ORIENTED_EDGE('',*,*,#27452,.F.);
#40521=ORIENTED_EDGE('',*,*,#27453,.T.);
#40522=ORIENTED_EDGE('',*,*,#27454,.T.);
#40523=ORIENTED_EDGE('',*,*,#27455,.F.);
#40524=ORIENTED_EDGE('',*,*,#27456,.F.);
#40525=ORIENTED_EDGE('',*,*,#27457,.T.);
#40526=ORIENTED_EDGE('',*,*,#27458,.T.);
#40527=ORIENTED_EDGE('',*,*,#27459,.F.);
#40528=ORIENTED_EDGE('',*,*,#27460,.F.);
#40529=ORIENTED_EDGE('',*,*,#27461,.T.);
#40530=ORIENTED_EDGE('',*,*,#27462,.T.);
#40531=ORIENTED_EDGE('',*,*,#27463,.F.);
#40532=ORIENTED_EDGE('',*,*,#27464,.F.);
#40533=ORIENTED_EDGE('',*,*,#27465,.T.);
#40534=ORIENTED_EDGE('',*,*,#27466,.T.);
#40535=ORIENTED_EDGE('',*,*,#27467,.F.);
#40536=ORIENTED_EDGE('',*,*,#27468,.F.);
#40537=ORIENTED_EDGE('',*,*,#27469,.T.);
#40538=ORIENTED_EDGE('',*,*,#27470,.T.);
#40539=ORIENTED_EDGE('',*,*,#27471,.F.);
#40540=ORIENTED_EDGE('',*,*,#27472,.F.);
#40541=ORIENTED_EDGE('',*,*,#27473,.T.);
#40542=ORIENTED_EDGE('',*,*,#27474,.T.);
#40543=ORIENTED_EDGE('',*,*,#27475,.F.);
#40544=ORIENTED_EDGE('',*,*,#27476,.F.);
#40545=ORIENTED_EDGE('',*,*,#27477,.T.);
#40546=ORIENTED_EDGE('',*,*,#27478,.T.);
#40547=ORIENTED_EDGE('',*,*,#27479,.F.);
#40548=ORIENTED_EDGE('',*,*,#27480,.T.);
#40549=ORIENTED_EDGE('',*,*,#27481,.F.);
#40550=ORIENTED_EDGE('',*,*,#27482,.F.);
#40551=ORIENTED_EDGE('',*,*,#27483,.T.);
#40552=ORIENTED_EDGE('',*,*,#27484,.F.);
#40553=ORIENTED_EDGE('',*,*,#27485,.T.);
#40554=ORIENTED_EDGE('',*,*,#27486,.T.);
#40555=ORIENTED_EDGE('',*,*,#27487,.F.);
#40556=ORIENTED_EDGE('',*,*,#27488,.F.);
#40557=ORIENTED_EDGE('',*,*,#27489,.T.);
#40558=ORIENTED_EDGE('',*,*,#27490,.T.);
#40559=ORIENTED_EDGE('',*,*,#27491,.F.);
#40560=ORIENTED_EDGE('',*,*,#27492,.F.);
#40561=ORIENTED_EDGE('',*,*,#27493,.T.);
#40562=ORIENTED_EDGE('',*,*,#27494,.T.);
#40563=ORIENTED_EDGE('',*,*,#27495,.F.);
#40564=ORIENTED_EDGE('',*,*,#27496,.F.);
#40565=ORIENTED_EDGE('',*,*,#27497,.T.);
#40566=ORIENTED_EDGE('',*,*,#27498,.T.);
#40567=ORIENTED_EDGE('',*,*,#27499,.F.);
#40568=ORIENTED_EDGE('',*,*,#27500,.F.);
#40569=ORIENTED_EDGE('',*,*,#27501,.T.);
#40570=ORIENTED_EDGE('',*,*,#27502,.T.);
#40571=ORIENTED_EDGE('',*,*,#27503,.F.);
#40572=ORIENTED_EDGE('',*,*,#27504,.F.);
#40573=ORIENTED_EDGE('',*,*,#27505,.T.);
#40574=ORIENTED_EDGE('',*,*,#27506,.T.);
#40575=ORIENTED_EDGE('',*,*,#27507,.F.);
#40576=ORIENTED_EDGE('',*,*,#27508,.F.);
#40577=ORIENTED_EDGE('',*,*,#27509,.T.);
#40578=ORIENTED_EDGE('',*,*,#27510,.T.);
#40579=ORIENTED_EDGE('',*,*,#27511,.F.);
#40580=ORIENTED_EDGE('',*,*,#27512,.F.);
#40581=ORIENTED_EDGE('',*,*,#27513,.T.);
#40582=ORIENTED_EDGE('',*,*,#27514,.T.);
#40583=ORIENTED_EDGE('',*,*,#27515,.F.);
#40584=ORIENTED_EDGE('',*,*,#27516,.F.);
#40585=ORIENTED_EDGE('',*,*,#27517,.T.);
#40586=ORIENTED_EDGE('',*,*,#27518,.T.);
#40587=ORIENTED_EDGE('',*,*,#27519,.F.);
#40588=ORIENTED_EDGE('',*,*,#27520,.T.);
#40589=ORIENTED_EDGE('',*,*,#27521,.F.);
#40590=ORIENTED_EDGE('',*,*,#27522,.F.);
#40591=ORIENTED_EDGE('',*,*,#27523,.T.);
#40592=ORIENTED_EDGE('',*,*,#27524,.T.);
#40593=ORIENTED_EDGE('',*,*,#27525,.F.);
#40594=ORIENTED_EDGE('',*,*,#27526,.F.);
#40595=ORIENTED_EDGE('',*,*,#27527,.T.);
#40596=ORIENTED_EDGE('',*,*,#27528,.T.);
#40597=ORIENTED_EDGE('',*,*,#27529,.F.);
#40598=ORIENTED_EDGE('',*,*,#27530,.F.);
#40599=ORIENTED_EDGE('',*,*,#27531,.T.);
#40600=ORIENTED_EDGE('',*,*,#27532,.T.);
#40601=ORIENTED_EDGE('',*,*,#27533,.F.);
#40602=ORIENTED_EDGE('',*,*,#27534,.F.);
#40603=ORIENTED_EDGE('',*,*,#27535,.T.);
#40604=ORIENTED_EDGE('',*,*,#27536,.T.);
#40605=ORIENTED_EDGE('',*,*,#27537,.F.);
#40606=ORIENTED_EDGE('',*,*,#27538,.F.);
#40607=ORIENTED_EDGE('',*,*,#27539,.T.);
#40608=ORIENTED_EDGE('',*,*,#27540,.T.);
#40609=ORIENTED_EDGE('',*,*,#27541,.F.);
#40610=ORIENTED_EDGE('',*,*,#27542,.F.);
#40611=ORIENTED_EDGE('',*,*,#27543,.T.);
#40612=ORIENTED_EDGE('',*,*,#27544,.T.);
#40613=ORIENTED_EDGE('',*,*,#27545,.F.);
#40614=ORIENTED_EDGE('',*,*,#27546,.F.);
#40615=ORIENTED_EDGE('',*,*,#27547,.T.);
#40616=ORIENTED_EDGE('',*,*,#27548,.F.);
#40617=ORIENTED_EDGE('',*,*,#27549,.T.);
#40618=ORIENTED_EDGE('',*,*,#27550,.T.);
#40619=ORIENTED_EDGE('',*,*,#27551,.F.);
#40620=ORIENTED_EDGE('',*,*,#27552,.F.);
#40621=ORIENTED_EDGE('',*,*,#27553,.T.);
#40622=ORIENTED_EDGE('',*,*,#27554,.T.);
#40623=ORIENTED_EDGE('',*,*,#27555,.F.);
#40624=ORIENTED_EDGE('',*,*,#27556,.T.);
#40625=ORIENTED_EDGE('',*,*,#27557,.F.);
#40626=ORIENTED_EDGE('',*,*,#27558,.F.);
#40627=ORIENTED_EDGE('',*,*,#27559,.T.);
#40628=ORIENTED_EDGE('',*,*,#27560,.F.);
#40629=ORIENTED_EDGE('',*,*,#27561,.T.);
#40630=ORIENTED_EDGE('',*,*,#27562,.T.);
#40631=ORIENTED_EDGE('',*,*,#27563,.F.);
#40632=ORIENTED_EDGE('',*,*,#27564,.F.);
#40633=ORIENTED_EDGE('',*,*,#27565,.F.);
#40634=ORIENTED_EDGE('',*,*,#27363,.F.);
#40635=ORIENTED_EDGE('',*,*,#27566,.F.);
#40636=ORIENTED_EDGE('',*,*,#27567,.F.);
#40637=ORIENTED_EDGE('',*,*,#27559,.F.);
#40638=ORIENTED_EDGE('',*,*,#27568,.F.);
#40639=ORIENTED_EDGE('',*,*,#27569,.F.);
#40640=ORIENTED_EDGE('',*,*,#27561,.F.);
#40641=ORIENTED_EDGE('',*,*,#27570,.F.);
#40642=ORIENTED_EDGE('',*,*,#27571,.F.);
#40643=ORIENTED_EDGE('',*,*,#27553,.F.);
#40644=ORIENTED_EDGE('',*,*,#27572,.F.);
#40645=ORIENTED_EDGE('',*,*,#27573,.F.);
#40646=ORIENTED_EDGE('',*,*,#27523,.F.);
#40647=ORIENTED_EDGE('',*,*,#27574,.F.);
#40648=ORIENTED_EDGE('',*,*,#27575,.F.);
#40649=ORIENTED_EDGE('',*,*,#27527,.F.);
#40650=ORIENTED_EDGE('',*,*,#27576,.F.);
#40651=ORIENTED_EDGE('',*,*,#27577,.F.);
#40652=ORIENTED_EDGE('',*,*,#27531,.F.);
#40653=ORIENTED_EDGE('',*,*,#27578,.F.);
#40654=ORIENTED_EDGE('',*,*,#27579,.F.);
#40655=ORIENTED_EDGE('',*,*,#27535,.F.);
#40656=ORIENTED_EDGE('',*,*,#27580,.F.);
#40657=ORIENTED_EDGE('',*,*,#27581,.F.);
#40658=ORIENTED_EDGE('',*,*,#27539,.F.);
#40659=ORIENTED_EDGE('',*,*,#27582,.F.);
#40660=ORIENTED_EDGE('',*,*,#27583,.F.);
#40661=ORIENTED_EDGE('',*,*,#27543,.F.);
#40662=ORIENTED_EDGE('',*,*,#27584,.F.);
#40663=ORIENTED_EDGE('',*,*,#27585,.F.);
#40664=ORIENTED_EDGE('',*,*,#27547,.F.);
#40665=ORIENTED_EDGE('',*,*,#27586,.F.);
#40666=ORIENTED_EDGE('',*,*,#27587,.F.);
#40667=ORIENTED_EDGE('',*,*,#27549,.F.);
#40668=ORIENTED_EDGE('',*,*,#27588,.F.);
#40669=ORIENTED_EDGE('',*,*,#27589,.F.);
#40670=ORIENTED_EDGE('',*,*,#27517,.F.);
#40671=ORIENTED_EDGE('',*,*,#27590,.F.);
#40672=ORIENTED_EDGE('',*,*,#27591,.F.);
#40673=ORIENTED_EDGE('',*,*,#27513,.F.);
#40674=ORIENTED_EDGE('',*,*,#27592,.F.);
#40675=ORIENTED_EDGE('',*,*,#27593,.F.);
#40676=ORIENTED_EDGE('',*,*,#27509,.F.);
#40677=ORIENTED_EDGE('',*,*,#27594,.F.);
#40678=ORIENTED_EDGE('',*,*,#27595,.F.);
#40679=ORIENTED_EDGE('',*,*,#27505,.F.);
#40680=ORIENTED_EDGE('',*,*,#27596,.F.);
#40681=ORIENTED_EDGE('',*,*,#27597,.F.);
#40682=ORIENTED_EDGE('',*,*,#27501,.F.);
#40683=ORIENTED_EDGE('',*,*,#27598,.F.);
#40684=ORIENTED_EDGE('',*,*,#27599,.F.);
#40685=ORIENTED_EDGE('',*,*,#27497,.F.);
#40686=ORIENTED_EDGE('',*,*,#27600,.F.);
#40687=ORIENTED_EDGE('',*,*,#27601,.F.);
#40688=ORIENTED_EDGE('',*,*,#27493,.F.);
#40689=ORIENTED_EDGE('',*,*,#27602,.F.);
#40690=ORIENTED_EDGE('',*,*,#27603,.F.);
#40691=ORIENTED_EDGE('',*,*,#27489,.F.);
#40692=ORIENTED_EDGE('',*,*,#27604,.F.);
#40693=ORIENTED_EDGE('',*,*,#27605,.F.);
#40694=ORIENTED_EDGE('',*,*,#27483,.F.);
#40695=ORIENTED_EDGE('',*,*,#27606,.F.);
#40696=ORIENTED_EDGE('',*,*,#27607,.F.);
#40697=ORIENTED_EDGE('',*,*,#27485,.F.);
#40698=ORIENTED_EDGE('',*,*,#27608,.F.);
#40699=ORIENTED_EDGE('',*,*,#27609,.F.);
#40700=ORIENTED_EDGE('',*,*,#27477,.F.);
#40701=ORIENTED_EDGE('',*,*,#27610,.F.);
#40702=ORIENTED_EDGE('',*,*,#27611,.F.);
#40703=ORIENTED_EDGE('',*,*,#27473,.F.);
#40704=ORIENTED_EDGE('',*,*,#27612,.F.);
#40705=ORIENTED_EDGE('',*,*,#27613,.F.);
#40706=ORIENTED_EDGE('',*,*,#27469,.F.);
#40707=ORIENTED_EDGE('',*,*,#27614,.F.);
#40708=ORIENTED_EDGE('',*,*,#27615,.F.);
#40709=ORIENTED_EDGE('',*,*,#27465,.F.);
#40710=ORIENTED_EDGE('',*,*,#27616,.F.);
#40711=ORIENTED_EDGE('',*,*,#27617,.F.);
#40712=ORIENTED_EDGE('',*,*,#27461,.F.);
#40713=ORIENTED_EDGE('',*,*,#27618,.F.);
#40714=ORIENTED_EDGE('',*,*,#27619,.F.);
#40715=ORIENTED_EDGE('',*,*,#27457,.F.);
#40716=ORIENTED_EDGE('',*,*,#27620,.F.);
#40717=ORIENTED_EDGE('',*,*,#27621,.F.);
#40718=ORIENTED_EDGE('',*,*,#27453,.F.);
#40719=ORIENTED_EDGE('',*,*,#27622,.F.);
#40720=ORIENTED_EDGE('',*,*,#27623,.F.);
#40721=ORIENTED_EDGE('',*,*,#27449,.F.);
#40722=ORIENTED_EDGE('',*,*,#27624,.F.);
#40723=ORIENTED_EDGE('',*,*,#27625,.F.);
#40724=ORIENTED_EDGE('',*,*,#27445,.F.);
#40725=ORIENTED_EDGE('',*,*,#27626,.F.);
#40726=ORIENTED_EDGE('',*,*,#27627,.F.);
#40727=ORIENTED_EDGE('',*,*,#27441,.F.);
#40728=ORIENTED_EDGE('',*,*,#27628,.F.);
#40729=ORIENTED_EDGE('',*,*,#27629,.F.);
#40730=ORIENTED_EDGE('',*,*,#27427,.F.);
#40731=ORIENTED_EDGE('',*,*,#27630,.F.);
#40732=ORIENTED_EDGE('',*,*,#27631,.F.);
#40733=ORIENTED_EDGE('',*,*,#27431,.F.);
#40734=ORIENTED_EDGE('',*,*,#27632,.F.);
#40735=ORIENTED_EDGE('',*,*,#27633,.F.);
#40736=ORIENTED_EDGE('',*,*,#27435,.F.);
#40737=ORIENTED_EDGE('',*,*,#27634,.F.);
#40738=ORIENTED_EDGE('',*,*,#27635,.F.);
#40739=ORIENTED_EDGE('',*,*,#27437,.F.);
#40740=ORIENTED_EDGE('',*,*,#27636,.F.);
#40741=ORIENTED_EDGE('',*,*,#27637,.F.);
#40742=ORIENTED_EDGE('',*,*,#27421,.F.);
#40743=ORIENTED_EDGE('',*,*,#27638,.F.);
#40744=ORIENTED_EDGE('',*,*,#27639,.F.);
#40745=ORIENTED_EDGE('',*,*,#27417,.F.);
#40746=ORIENTED_EDGE('',*,*,#27640,.F.);
#40747=ORIENTED_EDGE('',*,*,#27641,.F.);
#40748=ORIENTED_EDGE('',*,*,#27413,.F.);
#40749=ORIENTED_EDGE('',*,*,#27642,.F.);
#40750=ORIENTED_EDGE('',*,*,#27643,.F.);
#40751=ORIENTED_EDGE('',*,*,#27409,.F.);
#40752=ORIENTED_EDGE('',*,*,#27644,.F.);
#40753=ORIENTED_EDGE('',*,*,#27645,.F.);
#40754=ORIENTED_EDGE('',*,*,#27405,.F.);
#40755=ORIENTED_EDGE('',*,*,#27646,.F.);
#40756=ORIENTED_EDGE('',*,*,#27647,.F.);
#40757=ORIENTED_EDGE('',*,*,#27401,.F.);
#40758=ORIENTED_EDGE('',*,*,#27648,.F.);
#40759=ORIENTED_EDGE('',*,*,#27649,.F.);
#40760=ORIENTED_EDGE('',*,*,#27397,.F.);
#40761=ORIENTED_EDGE('',*,*,#27650,.F.);
#40762=ORIENTED_EDGE('',*,*,#27651,.F.);
#40763=ORIENTED_EDGE('',*,*,#27393,.F.);
#40764=ORIENTED_EDGE('',*,*,#27652,.F.);
#40765=ORIENTED_EDGE('',*,*,#27653,.F.);
#40766=ORIENTED_EDGE('',*,*,#27389,.F.);
#40767=ORIENTED_EDGE('',*,*,#27654,.F.);
#40768=ORIENTED_EDGE('',*,*,#27655,.F.);
#40769=ORIENTED_EDGE('',*,*,#27385,.F.);
#40770=ORIENTED_EDGE('',*,*,#27656,.F.);
#40771=ORIENTED_EDGE('',*,*,#27657,.F.);
#40772=ORIENTED_EDGE('',*,*,#27381,.F.);
#40773=ORIENTED_EDGE('',*,*,#27658,.F.);
#40774=ORIENTED_EDGE('',*,*,#27659,.F.);
#40775=ORIENTED_EDGE('',*,*,#27377,.F.);
#40776=ORIENTED_EDGE('',*,*,#27660,.F.);
#40777=ORIENTED_EDGE('',*,*,#27661,.F.);
#40778=ORIENTED_EDGE('',*,*,#27373,.F.);
#40779=ORIENTED_EDGE('',*,*,#27662,.F.);
#40780=ORIENTED_EDGE('',*,*,#27663,.F.);
#40781=ORIENTED_EDGE('',*,*,#27369,.F.);
#40782=ORIENTED_EDGE('',*,*,#27664,.F.);
#40783=ORIENTED_EDGE('',*,*,#27665,.F.);
#40784=ORIENTED_EDGE('',*,*,#27365,.F.);
#40785=ORIENTED_EDGE('',*,*,#27356,.F.);
#40786=ORIENTED_EDGE('',*,*,#27666,.F.);
#40787=ORIENTED_EDGE('',*,*,#27667,.F.);
#40788=ORIENTED_EDGE('',*,*,#27367,.T.);
#40789=ORIENTED_EDGE('',*,*,#27668,.F.);
#40790=ORIENTED_EDGE('',*,*,#27669,.F.);
#40791=ORIENTED_EDGE('',*,*,#27371,.T.);
#40792=ORIENTED_EDGE('',*,*,#27670,.F.);
#40793=ORIENTED_EDGE('',*,*,#27671,.F.);
#40794=ORIENTED_EDGE('',*,*,#27375,.T.);
#40795=ORIENTED_EDGE('',*,*,#27672,.F.);
#40796=ORIENTED_EDGE('',*,*,#27673,.F.);
#40797=ORIENTED_EDGE('',*,*,#27379,.T.);
#40798=ORIENTED_EDGE('',*,*,#27674,.F.);
#40799=ORIENTED_EDGE('',*,*,#27675,.F.);
#40800=ORIENTED_EDGE('',*,*,#27383,.T.);
#40801=ORIENTED_EDGE('',*,*,#27676,.F.);
#40802=ORIENTED_EDGE('',*,*,#27677,.F.);
#40803=ORIENTED_EDGE('',*,*,#27387,.T.);
#40804=ORIENTED_EDGE('',*,*,#27678,.F.);
#40805=ORIENTED_EDGE('',*,*,#27679,.F.);
#40806=ORIENTED_EDGE('',*,*,#27391,.T.);
#40807=ORIENTED_EDGE('',*,*,#27680,.F.);
#40808=ORIENTED_EDGE('',*,*,#27681,.F.);
#40809=ORIENTED_EDGE('',*,*,#27395,.T.);
#40810=ORIENTED_EDGE('',*,*,#27682,.F.);
#40811=ORIENTED_EDGE('',*,*,#27683,.F.);
#40812=ORIENTED_EDGE('',*,*,#27399,.T.);
#40813=ORIENTED_EDGE('',*,*,#27684,.F.);
#40814=ORIENTED_EDGE('',*,*,#27685,.F.);
#40815=ORIENTED_EDGE('',*,*,#27403,.T.);
#40816=ORIENTED_EDGE('',*,*,#27686,.F.);
#40817=ORIENTED_EDGE('',*,*,#27687,.F.);
#40818=ORIENTED_EDGE('',*,*,#27407,.T.);
#40819=ORIENTED_EDGE('',*,*,#27688,.F.);
#40820=ORIENTED_EDGE('',*,*,#27689,.F.);
#40821=ORIENTED_EDGE('',*,*,#27411,.T.);
#40822=ORIENTED_EDGE('',*,*,#27690,.F.);
#40823=ORIENTED_EDGE('',*,*,#27691,.F.);
#40824=ORIENTED_EDGE('',*,*,#27415,.T.);
#40825=ORIENTED_EDGE('',*,*,#27692,.F.);
#40826=ORIENTED_EDGE('',*,*,#27693,.F.);
#40827=ORIENTED_EDGE('',*,*,#27419,.T.);
#40828=ORIENTED_EDGE('',*,*,#27694,.F.);
#40829=ORIENTED_EDGE('',*,*,#27695,.F.);
#40830=ORIENTED_EDGE('',*,*,#27423,.T.);
#40831=ORIENTED_EDGE('',*,*,#27696,.F.);
#40832=ORIENTED_EDGE('',*,*,#27697,.F.);
#40833=ORIENTED_EDGE('',*,*,#27439,.T.);
#40834=ORIENTED_EDGE('',*,*,#27698,.F.);
#40835=ORIENTED_EDGE('',*,*,#27699,.F.);
#40836=ORIENTED_EDGE('',*,*,#27433,.T.);
#40837=ORIENTED_EDGE('',*,*,#27700,.F.);
#40838=ORIENTED_EDGE('',*,*,#27701,.F.);
#40839=ORIENTED_EDGE('',*,*,#27429,.T.);
#40840=ORIENTED_EDGE('',*,*,#27702,.F.);
#40841=ORIENTED_EDGE('',*,*,#27703,.F.);
#40842=ORIENTED_EDGE('',*,*,#27425,.T.);
#40843=ORIENTED_EDGE('',*,*,#27704,.F.);
#40844=ORIENTED_EDGE('',*,*,#27705,.F.);
#40845=ORIENTED_EDGE('',*,*,#27443,.T.);
#40846=ORIENTED_EDGE('',*,*,#27706,.F.);
#40847=ORIENTED_EDGE('',*,*,#27707,.F.);
#40848=ORIENTED_EDGE('',*,*,#27447,.T.);
#40849=ORIENTED_EDGE('',*,*,#27708,.F.);
#40850=ORIENTED_EDGE('',*,*,#27709,.F.);
#40851=ORIENTED_EDGE('',*,*,#27451,.T.);
#40852=ORIENTED_EDGE('',*,*,#27710,.F.);
#40853=ORIENTED_EDGE('',*,*,#27711,.F.);
#40854=ORIENTED_EDGE('',*,*,#27455,.T.);
#40855=ORIENTED_EDGE('',*,*,#27712,.F.);
#40856=ORIENTED_EDGE('',*,*,#27713,.F.);
#40857=ORIENTED_EDGE('',*,*,#27459,.T.);
#40858=ORIENTED_EDGE('',*,*,#27714,.F.);
#40859=ORIENTED_EDGE('',*,*,#27715,.F.);
#40860=ORIENTED_EDGE('',*,*,#27463,.T.);
#40861=ORIENTED_EDGE('',*,*,#27716,.F.);
#40862=ORIENTED_EDGE('',*,*,#27717,.F.);
#40863=ORIENTED_EDGE('',*,*,#27467,.T.);
#40864=ORIENTED_EDGE('',*,*,#27718,.F.);
#40865=ORIENTED_EDGE('',*,*,#27719,.F.);
#40866=ORIENTED_EDGE('',*,*,#27471,.T.);
#40867=ORIENTED_EDGE('',*,*,#27720,.F.);
#40868=ORIENTED_EDGE('',*,*,#27721,.F.);
#40869=ORIENTED_EDGE('',*,*,#27475,.T.);
#40870=ORIENTED_EDGE('',*,*,#27722,.F.);
#40871=ORIENTED_EDGE('',*,*,#27723,.F.);
#40872=ORIENTED_EDGE('',*,*,#27479,.T.);
#40873=ORIENTED_EDGE('',*,*,#27724,.F.);
#40874=ORIENTED_EDGE('',*,*,#27725,.F.);
#40875=ORIENTED_EDGE('',*,*,#27487,.T.);
#40876=ORIENTED_EDGE('',*,*,#27726,.F.);
#40877=ORIENTED_EDGE('',*,*,#27727,.F.);
#40878=ORIENTED_EDGE('',*,*,#27481,.T.);
#40879=ORIENTED_EDGE('',*,*,#27728,.F.);
#40880=ORIENTED_EDGE('',*,*,#27729,.F.);
#40881=ORIENTED_EDGE('',*,*,#27491,.T.);
#40882=ORIENTED_EDGE('',*,*,#27730,.F.);
#40883=ORIENTED_EDGE('',*,*,#27731,.F.);
#40884=ORIENTED_EDGE('',*,*,#27495,.T.);
#40885=ORIENTED_EDGE('',*,*,#27732,.F.);
#40886=ORIENTED_EDGE('',*,*,#27733,.F.);
#40887=ORIENTED_EDGE('',*,*,#27499,.T.);
#40888=ORIENTED_EDGE('',*,*,#27734,.F.);
#40889=ORIENTED_EDGE('',*,*,#27735,.F.);
#40890=ORIENTED_EDGE('',*,*,#27503,.T.);
#40891=ORIENTED_EDGE('',*,*,#27736,.F.);
#40892=ORIENTED_EDGE('',*,*,#27737,.F.);
#40893=ORIENTED_EDGE('',*,*,#27507,.T.);
#40894=ORIENTED_EDGE('',*,*,#27738,.F.);
#40895=ORIENTED_EDGE('',*,*,#27739,.F.);
#40896=ORIENTED_EDGE('',*,*,#27511,.T.);
#40897=ORIENTED_EDGE('',*,*,#27740,.F.);
#40898=ORIENTED_EDGE('',*,*,#27741,.F.);
#40899=ORIENTED_EDGE('',*,*,#27515,.T.);
#40900=ORIENTED_EDGE('',*,*,#27742,.F.);
#40901=ORIENTED_EDGE('',*,*,#27743,.F.);
#40902=ORIENTED_EDGE('',*,*,#27519,.T.);
#40903=ORIENTED_EDGE('',*,*,#27744,.F.);
#40904=ORIENTED_EDGE('',*,*,#27745,.F.);
#40905=ORIENTED_EDGE('',*,*,#27551,.T.);
#40906=ORIENTED_EDGE('',*,*,#27746,.F.);
#40907=ORIENTED_EDGE('',*,*,#27747,.F.);
#40908=ORIENTED_EDGE('',*,*,#27545,.T.);
#40909=ORIENTED_EDGE('',*,*,#27748,.F.);
#40910=ORIENTED_EDGE('',*,*,#27749,.F.);
#40911=ORIENTED_EDGE('',*,*,#27541,.T.);
#40912=ORIENTED_EDGE('',*,*,#27750,.F.);
#40913=ORIENTED_EDGE('',*,*,#27751,.F.);
#40914=ORIENTED_EDGE('',*,*,#27537,.T.);
#40915=ORIENTED_EDGE('',*,*,#27752,.F.);
#40916=ORIENTED_EDGE('',*,*,#27753,.F.);
#40917=ORIENTED_EDGE('',*,*,#27533,.T.);
#40918=ORIENTED_EDGE('',*,*,#27754,.F.);
#40919=ORIENTED_EDGE('',*,*,#27755,.F.);
#40920=ORIENTED_EDGE('',*,*,#27529,.T.);
#40921=ORIENTED_EDGE('',*,*,#27756,.F.);
#40922=ORIENTED_EDGE('',*,*,#27757,.F.);
#40923=ORIENTED_EDGE('',*,*,#27525,.T.);
#40924=ORIENTED_EDGE('',*,*,#27758,.F.);
#40925=ORIENTED_EDGE('',*,*,#27759,.F.);
#40926=ORIENTED_EDGE('',*,*,#27521,.T.);
#40927=ORIENTED_EDGE('',*,*,#27760,.F.);
#40928=ORIENTED_EDGE('',*,*,#27761,.F.);
#40929=ORIENTED_EDGE('',*,*,#27555,.T.);
#40930=ORIENTED_EDGE('',*,*,#27762,.F.);
#40931=ORIENTED_EDGE('',*,*,#27763,.F.);
#40932=ORIENTED_EDGE('',*,*,#27563,.T.);
#40933=ORIENTED_EDGE('',*,*,#27764,.F.);
#40934=ORIENTED_EDGE('',*,*,#27765,.F.);
#40935=ORIENTED_EDGE('',*,*,#27557,.T.);
#40936=ORIENTED_EDGE('',*,*,#27766,.F.);
#40937=ORIENTED_EDGE('',*,*,#27767,.F.);
#40938=ORIENTED_EDGE('',*,*,#27361,.T.);
#40939=ORIENTED_EDGE('',*,*,#27359,.F.);
#40940=ORIENTED_EDGE('',*,*,#27357,.T.);
#40941=ORIENTED_EDGE('',*,*,#27348,.F.);
#40942=ORIENTED_EDGE('',*,*,#27354,.T.);
#40943=ORIENTED_EDGE('',*,*,#27351,.F.);
#40944=ORIENTED_EDGE('',*,*,#27353,.T.);
#40945=ORIENTED_EDGE('',*,*,#27350,.T.);
#40946=ORIENTED_EDGE('',*,*,#27569,.T.);
#40947=ORIENTED_EDGE('',*,*,#27768,.T.);
#40948=ORIENTED_EDGE('',*,*,#27764,.T.);
#40949=ORIENTED_EDGE('',*,*,#27562,.F.);
#40950=ORIENTED_EDGE('',*,*,#27568,.T.);
#40951=ORIENTED_EDGE('',*,*,#27558,.T.);
#40952=ORIENTED_EDGE('',*,*,#27765,.T.);
#40953=ORIENTED_EDGE('',*,*,#27768,.F.);
#40954=ORIENTED_EDGE('',*,*,#27567,.T.);
#40955=ORIENTED_EDGE('',*,*,#27769,.T.);
#40956=ORIENTED_EDGE('',*,*,#27766,.T.);
#40957=ORIENTED_EDGE('',*,*,#27556,.F.);
#40958=ORIENTED_EDGE('',*,*,#27566,.T.);
#40959=ORIENTED_EDGE('',*,*,#27362,.T.);
#40960=ORIENTED_EDGE('',*,*,#27767,.T.);
#40961=ORIENTED_EDGE('',*,*,#27769,.F.);
#40962=ORIENTED_EDGE('',*,*,#27571,.T.);
#40963=ORIENTED_EDGE('',*,*,#27770,.T.);
#40964=ORIENTED_EDGE('',*,*,#27762,.T.);
#40965=ORIENTED_EDGE('',*,*,#27554,.F.);
#40966=ORIENTED_EDGE('',*,*,#27570,.T.);
#40967=ORIENTED_EDGE('',*,*,#27560,.T.);
#40968=ORIENTED_EDGE('',*,*,#27763,.T.);
#40969=ORIENTED_EDGE('',*,*,#27770,.F.);
#40970=ORIENTED_EDGE('',*,*,#27587,.T.);
#40971=ORIENTED_EDGE('',*,*,#27771,.T.);
#40972=ORIENTED_EDGE('',*,*,#27746,.T.);
#40973=ORIENTED_EDGE('',*,*,#27550,.F.);
#40974=ORIENTED_EDGE('',*,*,#27586,.T.);
#40975=ORIENTED_EDGE('',*,*,#27546,.T.);
#40976=ORIENTED_EDGE('',*,*,#27747,.T.);
#40977=ORIENTED_EDGE('',*,*,#27771,.F.);
#40978=ORIENTED_EDGE('',*,*,#27585,.T.);
#40979=ORIENTED_EDGE('',*,*,#27772,.T.);
#40980=ORIENTED_EDGE('',*,*,#27748,.T.);
#40981=ORIENTED_EDGE('',*,*,#27544,.F.);
#40982=ORIENTED_EDGE('',*,*,#27584,.T.);
#40983=ORIENTED_EDGE('',*,*,#27542,.T.);
#40984=ORIENTED_EDGE('',*,*,#27749,.T.);
#40985=ORIENTED_EDGE('',*,*,#27772,.F.);
#40986=ORIENTED_EDGE('',*,*,#27583,.T.);
#40987=ORIENTED_EDGE('',*,*,#27773,.T.);
#40988=ORIENTED_EDGE('',*,*,#27750,.T.);
#40989=ORIENTED_EDGE('',*,*,#27540,.F.);
#40990=ORIENTED_EDGE('',*,*,#27582,.T.);
#40991=ORIENTED_EDGE('',*,*,#27538,.T.);
#40992=ORIENTED_EDGE('',*,*,#27751,.T.);
#40993=ORIENTED_EDGE('',*,*,#27773,.F.);
#40994=ORIENTED_EDGE('',*,*,#27581,.T.);
#40995=ORIENTED_EDGE('',*,*,#27774,.T.);
#40996=ORIENTED_EDGE('',*,*,#27752,.T.);
#40997=ORIENTED_EDGE('',*,*,#27536,.F.);
#40998=ORIENTED_EDGE('',*,*,#27580,.T.);
#40999=ORIENTED_EDGE('',*,*,#27534,.T.);
#41000=ORIENTED_EDGE('',*,*,#27753,.T.);
#41001=ORIENTED_EDGE('',*,*,#27774,.F.);
#41002=ORIENTED_EDGE('',*,*,#27579,.T.);
#41003=ORIENTED_EDGE('',*,*,#27775,.T.);
#41004=ORIENTED_EDGE('',*,*,#27754,.T.);
#41005=ORIENTED_EDGE('',*,*,#27532,.F.);
#41006=ORIENTED_EDGE('',*,*,#27578,.T.);
#41007=ORIENTED_EDGE('',*,*,#27530,.T.);
#41008=ORIENTED_EDGE('',*,*,#27755,.T.);
#41009=ORIENTED_EDGE('',*,*,#27775,.F.);
#41010=ORIENTED_EDGE('',*,*,#27577,.T.);
#41011=ORIENTED_EDGE('',*,*,#27776,.T.);
#41012=ORIENTED_EDGE('',*,*,#27756,.T.);
#41013=ORIENTED_EDGE('',*,*,#27528,.F.);
#41014=ORIENTED_EDGE('',*,*,#27576,.T.);
#41015=ORIENTED_EDGE('',*,*,#27526,.T.);
#41016=ORIENTED_EDGE('',*,*,#27757,.T.);
#41017=ORIENTED_EDGE('',*,*,#27776,.F.);
#41018=ORIENTED_EDGE('',*,*,#27575,.T.);
#41019=ORIENTED_EDGE('',*,*,#27777,.T.);
#41020=ORIENTED_EDGE('',*,*,#27758,.T.);
#41021=ORIENTED_EDGE('',*,*,#27524,.F.);
#41022=ORIENTED_EDGE('',*,*,#27574,.T.);
#41023=ORIENTED_EDGE('',*,*,#27522,.T.);
#41024=ORIENTED_EDGE('',*,*,#27759,.T.);
#41025=ORIENTED_EDGE('',*,*,#27777,.F.);
#41026=ORIENTED_EDGE('',*,*,#27573,.T.);
#41027=ORIENTED_EDGE('',*,*,#27778,.T.);
#41028=ORIENTED_EDGE('',*,*,#27760,.T.);
#41029=ORIENTED_EDGE('',*,*,#27520,.F.);
#41030=ORIENTED_EDGE('',*,*,#27572,.T.);
#41031=ORIENTED_EDGE('',*,*,#27552,.T.);
#41032=ORIENTED_EDGE('',*,*,#27761,.T.);
#41033=ORIENTED_EDGE('',*,*,#27778,.F.);
#41034=ORIENTED_EDGE('',*,*,#27589,.T.);
#41035=ORIENTED_EDGE('',*,*,#27779,.T.);
#41036=ORIENTED_EDGE('',*,*,#27744,.T.);
#41037=ORIENTED_EDGE('',*,*,#27518,.F.);
#41038=ORIENTED_EDGE('',*,*,#27588,.T.);
#41039=ORIENTED_EDGE('',*,*,#27548,.T.);
#41040=ORIENTED_EDGE('',*,*,#27745,.T.);
#41041=ORIENTED_EDGE('',*,*,#27779,.F.);
#41042=ORIENTED_EDGE('',*,*,#27591,.T.);
#41043=ORIENTED_EDGE('',*,*,#27780,.T.);
#41044=ORIENTED_EDGE('',*,*,#27742,.T.);
#41045=ORIENTED_EDGE('',*,*,#27514,.F.);
#41046=ORIENTED_EDGE('',*,*,#27590,.T.);
#41047=ORIENTED_EDGE('',*,*,#27516,.T.);
#41048=ORIENTED_EDGE('',*,*,#27743,.T.);
#41049=ORIENTED_EDGE('',*,*,#27780,.F.);
#41050=ORIENTED_EDGE('',*,*,#27593,.T.);
#41051=ORIENTED_EDGE('',*,*,#27781,.T.);
#41052=ORIENTED_EDGE('',*,*,#27740,.T.);
#41053=ORIENTED_EDGE('',*,*,#27510,.F.);
#41054=ORIENTED_EDGE('',*,*,#27592,.T.);
#41055=ORIENTED_EDGE('',*,*,#27512,.T.);
#41056=ORIENTED_EDGE('',*,*,#27741,.T.);
#41057=ORIENTED_EDGE('',*,*,#27781,.F.);
#41058=ORIENTED_EDGE('',*,*,#27595,.T.);
#41059=ORIENTED_EDGE('',*,*,#27782,.T.);
#41060=ORIENTED_EDGE('',*,*,#27738,.T.);
#41061=ORIENTED_EDGE('',*,*,#27506,.F.);
#41062=ORIENTED_EDGE('',*,*,#27594,.T.);
#41063=ORIENTED_EDGE('',*,*,#27508,.T.);
#41064=ORIENTED_EDGE('',*,*,#27739,.T.);
#41065=ORIENTED_EDGE('',*,*,#27782,.F.);
#41066=ORIENTED_EDGE('',*,*,#27597,.T.);
#41067=ORIENTED_EDGE('',*,*,#27783,.T.);
#41068=ORIENTED_EDGE('',*,*,#27736,.T.);
#41069=ORIENTED_EDGE('',*,*,#27502,.F.);
#41070=ORIENTED_EDGE('',*,*,#27596,.T.);
#41071=ORIENTED_EDGE('',*,*,#27504,.T.);
#41072=ORIENTED_EDGE('',*,*,#27737,.T.);
#41073=ORIENTED_EDGE('',*,*,#27783,.F.);
#41074=ORIENTED_EDGE('',*,*,#27599,.T.);
#41075=ORIENTED_EDGE('',*,*,#27784,.T.);
#41076=ORIENTED_EDGE('',*,*,#27734,.T.);
#41077=ORIENTED_EDGE('',*,*,#27498,.F.);
#41078=ORIENTED_EDGE('',*,*,#27598,.T.);
#41079=ORIENTED_EDGE('',*,*,#27500,.T.);
#41080=ORIENTED_EDGE('',*,*,#27735,.T.);
#41081=ORIENTED_EDGE('',*,*,#27784,.F.);
#41082=ORIENTED_EDGE('',*,*,#27601,.T.);
#41083=ORIENTED_EDGE('',*,*,#27785,.T.);
#41084=ORIENTED_EDGE('',*,*,#27732,.T.);
#41085=ORIENTED_EDGE('',*,*,#27494,.F.);
#41086=ORIENTED_EDGE('',*,*,#27600,.T.);
#41087=ORIENTED_EDGE('',*,*,#27496,.T.);
#41088=ORIENTED_EDGE('',*,*,#27733,.T.);
#41089=ORIENTED_EDGE('',*,*,#27785,.F.);
#41090=ORIENTED_EDGE('',*,*,#27603,.T.);
#41091=ORIENTED_EDGE('',*,*,#27786,.T.);
#41092=ORIENTED_EDGE('',*,*,#27730,.T.);
#41093=ORIENTED_EDGE('',*,*,#27490,.F.);
#41094=ORIENTED_EDGE('',*,*,#27602,.T.);
#41095=ORIENTED_EDGE('',*,*,#27492,.T.);
#41096=ORIENTED_EDGE('',*,*,#27731,.T.);
#41097=ORIENTED_EDGE('',*,*,#27786,.F.);
#41098=ORIENTED_EDGE('',*,*,#27607,.T.);
#41099=ORIENTED_EDGE('',*,*,#27787,.T.);
#41100=ORIENTED_EDGE('',*,*,#27726,.T.);
#41101=ORIENTED_EDGE('',*,*,#27486,.F.);
#41102=ORIENTED_EDGE('',*,*,#27606,.T.);
#41103=ORIENTED_EDGE('',*,*,#27482,.T.);
#41104=ORIENTED_EDGE('',*,*,#27727,.T.);
#41105=ORIENTED_EDGE('',*,*,#27787,.F.);
#41106=ORIENTED_EDGE('',*,*,#27605,.T.);
#41107=ORIENTED_EDGE('',*,*,#27788,.T.);
#41108=ORIENTED_EDGE('',*,*,#27728,.T.);
#41109=ORIENTED_EDGE('',*,*,#27480,.F.);
#41110=ORIENTED_EDGE('',*,*,#27604,.T.);
#41111=ORIENTED_EDGE('',*,*,#27488,.T.);
#41112=ORIENTED_EDGE('',*,*,#27729,.T.);
#41113=ORIENTED_EDGE('',*,*,#27788,.F.);
#41114=ORIENTED_EDGE('',*,*,#27609,.T.);
#41115=ORIENTED_EDGE('',*,*,#27789,.T.);
#41116=ORIENTED_EDGE('',*,*,#27724,.T.);
#41117=ORIENTED_EDGE('',*,*,#27478,.F.);
#41118=ORIENTED_EDGE('',*,*,#27608,.T.);
#41119=ORIENTED_EDGE('',*,*,#27484,.T.);
#41120=ORIENTED_EDGE('',*,*,#27725,.T.);
#41121=ORIENTED_EDGE('',*,*,#27789,.F.);
#41122=ORIENTED_EDGE('',*,*,#27611,.T.);
#41123=ORIENTED_EDGE('',*,*,#27790,.T.);
#41124=ORIENTED_EDGE('',*,*,#27722,.T.);
#41125=ORIENTED_EDGE('',*,*,#27474,.F.);
#41126=ORIENTED_EDGE('',*,*,#27610,.T.);
#41127=ORIENTED_EDGE('',*,*,#27476,.T.);
#41128=ORIENTED_EDGE('',*,*,#27723,.T.);
#41129=ORIENTED_EDGE('',*,*,#27790,.F.);
#41130=ORIENTED_EDGE('',*,*,#27613,.T.);
#41131=ORIENTED_EDGE('',*,*,#27791,.T.);
#41132=ORIENTED_EDGE('',*,*,#27720,.T.);
#41133=ORIENTED_EDGE('',*,*,#27470,.F.);
#41134=ORIENTED_EDGE('',*,*,#27612,.T.);
#41135=ORIENTED_EDGE('',*,*,#27472,.T.);
#41136=ORIENTED_EDGE('',*,*,#27721,.T.);
#41137=ORIENTED_EDGE('',*,*,#27791,.F.);
#41138=ORIENTED_EDGE('',*,*,#27615,.T.);
#41139=ORIENTED_EDGE('',*,*,#27792,.T.);
#41140=ORIENTED_EDGE('',*,*,#27718,.T.);
#41141=ORIENTED_EDGE('',*,*,#27466,.F.);
#41142=ORIENTED_EDGE('',*,*,#27614,.T.);
#41143=ORIENTED_EDGE('',*,*,#27468,.T.);
#41144=ORIENTED_EDGE('',*,*,#27719,.T.);
#41145=ORIENTED_EDGE('',*,*,#27792,.F.);
#41146=ORIENTED_EDGE('',*,*,#27617,.T.);
#41147=ORIENTED_EDGE('',*,*,#27793,.T.);
#41148=ORIENTED_EDGE('',*,*,#27716,.T.);
#41149=ORIENTED_EDGE('',*,*,#27462,.F.);
#41150=ORIENTED_EDGE('',*,*,#27616,.T.);
#41151=ORIENTED_EDGE('',*,*,#27464,.T.);
#41152=ORIENTED_EDGE('',*,*,#27717,.T.);
#41153=ORIENTED_EDGE('',*,*,#27793,.F.);
#41154=ORIENTED_EDGE('',*,*,#27619,.T.);
#41155=ORIENTED_EDGE('',*,*,#27794,.T.);
#41156=ORIENTED_EDGE('',*,*,#27714,.T.);
#41157=ORIENTED_EDGE('',*,*,#27458,.F.);
#41158=ORIENTED_EDGE('',*,*,#27618,.T.);
#41159=ORIENTED_EDGE('',*,*,#27460,.T.);
#41160=ORIENTED_EDGE('',*,*,#27715,.T.);
#41161=ORIENTED_EDGE('',*,*,#27794,.F.);
#41162=ORIENTED_EDGE('',*,*,#27621,.T.);
#41163=ORIENTED_EDGE('',*,*,#27795,.T.);
#41164=ORIENTED_EDGE('',*,*,#27712,.T.);
#41165=ORIENTED_EDGE('',*,*,#27454,.F.);
#41166=ORIENTED_EDGE('',*,*,#27620,.T.);
#41167=ORIENTED_EDGE('',*,*,#27456,.T.);
#41168=ORIENTED_EDGE('',*,*,#27713,.T.);
#41169=ORIENTED_EDGE('',*,*,#27795,.F.);
#41170=ORIENTED_EDGE('',*,*,#27623,.T.);
#41171=ORIENTED_EDGE('',*,*,#27796,.T.);
#41172=ORIENTED_EDGE('',*,*,#27710,.T.);
#41173=ORIENTED_EDGE('',*,*,#27450,.F.);
#41174=ORIENTED_EDGE('',*,*,#27622,.T.);
#41175=ORIENTED_EDGE('',*,*,#27452,.T.);
#41176=ORIENTED_EDGE('',*,*,#27711,.T.);
#41177=ORIENTED_EDGE('',*,*,#27796,.F.);
#41178=ORIENTED_EDGE('',*,*,#27625,.T.);
#41179=ORIENTED_EDGE('',*,*,#27797,.T.);
#41180=ORIENTED_EDGE('',*,*,#27708,.T.);
#41181=ORIENTED_EDGE('',*,*,#27446,.F.);
#41182=ORIENTED_EDGE('',*,*,#27624,.T.);
#41183=ORIENTED_EDGE('',*,*,#27448,.T.);
#41184=ORIENTED_EDGE('',*,*,#27709,.T.);
#41185=ORIENTED_EDGE('',*,*,#27797,.F.);
#41186=ORIENTED_EDGE('',*,*,#27627,.T.);
#41187=ORIENTED_EDGE('',*,*,#27798,.T.);
#41188=ORIENTED_EDGE('',*,*,#27706,.T.);
#41189=ORIENTED_EDGE('',*,*,#27442,.F.);
#41190=ORIENTED_EDGE('',*,*,#27626,.T.);
#41191=ORIENTED_EDGE('',*,*,#27444,.T.);
#41192=ORIENTED_EDGE('',*,*,#27707,.T.);
#41193=ORIENTED_EDGE('',*,*,#27798,.F.);
#41194=ORIENTED_EDGE('',*,*,#27635,.T.);
#41195=ORIENTED_EDGE('',*,*,#27799,.T.);
#41196=ORIENTED_EDGE('',*,*,#27698,.T.);
#41197=ORIENTED_EDGE('',*,*,#27438,.F.);
#41198=ORIENTED_EDGE('',*,*,#27634,.T.);
#41199=ORIENTED_EDGE('',*,*,#27434,.T.);
#41200=ORIENTED_EDGE('',*,*,#27699,.T.);
#41201=ORIENTED_EDGE('',*,*,#27799,.F.);
#41202=ORIENTED_EDGE('',*,*,#27633,.T.);
#41203=ORIENTED_EDGE('',*,*,#27800,.T.);
#41204=ORIENTED_EDGE('',*,*,#27700,.T.);
#41205=ORIENTED_EDGE('',*,*,#27432,.F.);
#41206=ORIENTED_EDGE('',*,*,#27632,.T.);
#41207=ORIENTED_EDGE('',*,*,#27430,.T.);
#41208=ORIENTED_EDGE('',*,*,#27701,.T.);
#41209=ORIENTED_EDGE('',*,*,#27800,.F.);
#41210=ORIENTED_EDGE('',*,*,#27631,.T.);
#41211=ORIENTED_EDGE('',*,*,#27801,.T.);
#41212=ORIENTED_EDGE('',*,*,#27702,.T.);
#41213=ORIENTED_EDGE('',*,*,#27428,.F.);
#41214=ORIENTED_EDGE('',*,*,#27630,.T.);
#41215=ORIENTED_EDGE('',*,*,#27426,.T.);
#41216=ORIENTED_EDGE('',*,*,#27703,.T.);
#41217=ORIENTED_EDGE('',*,*,#27801,.F.);
#41218=ORIENTED_EDGE('',*,*,#27629,.T.);
#41219=ORIENTED_EDGE('',*,*,#27802,.T.);
#41220=ORIENTED_EDGE('',*,*,#27704,.T.);
#41221=ORIENTED_EDGE('',*,*,#27424,.F.);
#41222=ORIENTED_EDGE('',*,*,#27628,.T.);
#41223=ORIENTED_EDGE('',*,*,#27440,.T.);
#41224=ORIENTED_EDGE('',*,*,#27705,.T.);
#41225=ORIENTED_EDGE('',*,*,#27802,.F.);
#41226=ORIENTED_EDGE('',*,*,#27637,.T.);
#41227=ORIENTED_EDGE('',*,*,#27803,.T.);
#41228=ORIENTED_EDGE('',*,*,#27696,.T.);
#41229=ORIENTED_EDGE('',*,*,#27422,.F.);
#41230=ORIENTED_EDGE('',*,*,#27636,.T.);
#41231=ORIENTED_EDGE('',*,*,#27436,.T.);
#41232=ORIENTED_EDGE('',*,*,#27697,.T.);
#41233=ORIENTED_EDGE('',*,*,#27803,.F.);
#41234=ORIENTED_EDGE('',*,*,#27639,.T.);
#41235=ORIENTED_EDGE('',*,*,#27804,.T.);
#41236=ORIENTED_EDGE('',*,*,#27694,.T.);
#41237=ORIENTED_EDGE('',*,*,#27418,.F.);
#41238=ORIENTED_EDGE('',*,*,#27638,.T.);
#41239=ORIENTED_EDGE('',*,*,#27420,.T.);
#41240=ORIENTED_EDGE('',*,*,#27695,.T.);
#41241=ORIENTED_EDGE('',*,*,#27804,.F.);
#41242=ORIENTED_EDGE('',*,*,#27641,.T.);
#41243=ORIENTED_EDGE('',*,*,#27805,.T.);
#41244=ORIENTED_EDGE('',*,*,#27692,.T.);
#41245=ORIENTED_EDGE('',*,*,#27414,.F.);
#41246=ORIENTED_EDGE('',*,*,#27640,.T.);
#41247=ORIENTED_EDGE('',*,*,#27416,.T.);
#41248=ORIENTED_EDGE('',*,*,#27693,.T.);
#41249=ORIENTED_EDGE('',*,*,#27805,.F.);
#41250=ORIENTED_EDGE('',*,*,#27643,.T.);
#41251=ORIENTED_EDGE('',*,*,#27806,.T.);
#41252=ORIENTED_EDGE('',*,*,#27690,.T.);
#41253=ORIENTED_EDGE('',*,*,#27410,.F.);
#41254=ORIENTED_EDGE('',*,*,#27642,.T.);
#41255=ORIENTED_EDGE('',*,*,#27412,.T.);
#41256=ORIENTED_EDGE('',*,*,#27691,.T.);
#41257=ORIENTED_EDGE('',*,*,#27806,.F.);
#41258=ORIENTED_EDGE('',*,*,#27645,.T.);
#41259=ORIENTED_EDGE('',*,*,#27807,.T.);
#41260=ORIENTED_EDGE('',*,*,#27688,.T.);
#41261=ORIENTED_EDGE('',*,*,#27406,.F.);
#41262=ORIENTED_EDGE('',*,*,#27644,.T.);
#41263=ORIENTED_EDGE('',*,*,#27408,.T.);
#41264=ORIENTED_EDGE('',*,*,#27689,.T.);
#41265=ORIENTED_EDGE('',*,*,#27807,.F.);
#41266=ORIENTED_EDGE('',*,*,#27647,.T.);
#41267=ORIENTED_EDGE('',*,*,#27808,.T.);
#41268=ORIENTED_EDGE('',*,*,#27686,.T.);
#41269=ORIENTED_EDGE('',*,*,#27402,.F.);
#41270=ORIENTED_EDGE('',*,*,#27646,.T.);
#41271=ORIENTED_EDGE('',*,*,#27404,.T.);
#41272=ORIENTED_EDGE('',*,*,#27687,.T.);
#41273=ORIENTED_EDGE('',*,*,#27808,.F.);
#41274=ORIENTED_EDGE('',*,*,#27649,.T.);
#41275=ORIENTED_EDGE('',*,*,#27809,.T.);
#41276=ORIENTED_EDGE('',*,*,#27684,.T.);
#41277=ORIENTED_EDGE('',*,*,#27398,.F.);
#41278=ORIENTED_EDGE('',*,*,#27648,.T.);
#41279=ORIENTED_EDGE('',*,*,#27400,.T.);
#41280=ORIENTED_EDGE('',*,*,#27685,.T.);
#41281=ORIENTED_EDGE('',*,*,#27809,.F.);
#41282=ORIENTED_EDGE('',*,*,#27651,.T.);
#41283=ORIENTED_EDGE('',*,*,#27810,.T.);
#41284=ORIENTED_EDGE('',*,*,#27682,.T.);
#41285=ORIENTED_EDGE('',*,*,#27394,.F.);
#41286=ORIENTED_EDGE('',*,*,#27650,.T.);
#41287=ORIENTED_EDGE('',*,*,#27396,.T.);
#41288=ORIENTED_EDGE('',*,*,#27683,.T.);
#41289=ORIENTED_EDGE('',*,*,#27810,.F.);
#41290=ORIENTED_EDGE('',*,*,#27653,.T.);
#41291=ORIENTED_EDGE('',*,*,#27811,.T.);
#41292=ORIENTED_EDGE('',*,*,#27680,.T.);
#41293=ORIENTED_EDGE('',*,*,#27390,.F.);
#41294=ORIENTED_EDGE('',*,*,#27652,.T.);
#41295=ORIENTED_EDGE('',*,*,#27392,.T.);
#41296=ORIENTED_EDGE('',*,*,#27681,.T.);
#41297=ORIENTED_EDGE('',*,*,#27811,.F.);
#41298=ORIENTED_EDGE('',*,*,#27655,.T.);
#41299=ORIENTED_EDGE('',*,*,#27812,.T.);
#41300=ORIENTED_EDGE('',*,*,#27678,.T.);
#41301=ORIENTED_EDGE('',*,*,#27386,.F.);
#41302=ORIENTED_EDGE('',*,*,#27654,.T.);
#41303=ORIENTED_EDGE('',*,*,#27388,.T.);
#41304=ORIENTED_EDGE('',*,*,#27679,.T.);
#41305=ORIENTED_EDGE('',*,*,#27812,.F.);
#41306=ORIENTED_EDGE('',*,*,#27657,.T.);
#41307=ORIENTED_EDGE('',*,*,#27813,.T.);
#41308=ORIENTED_EDGE('',*,*,#27676,.T.);
#41309=ORIENTED_EDGE('',*,*,#27382,.F.);
#41310=ORIENTED_EDGE('',*,*,#27656,.T.);
#41311=ORIENTED_EDGE('',*,*,#27384,.T.);
#41312=ORIENTED_EDGE('',*,*,#27677,.T.);
#41313=ORIENTED_EDGE('',*,*,#27813,.F.);
#41314=ORIENTED_EDGE('',*,*,#27659,.T.);
#41315=ORIENTED_EDGE('',*,*,#27814,.T.);
#41316=ORIENTED_EDGE('',*,*,#27674,.T.);
#41317=ORIENTED_EDGE('',*,*,#27378,.F.);
#41318=ORIENTED_EDGE('',*,*,#27658,.T.);
#41319=ORIENTED_EDGE('',*,*,#27380,.T.);
#41320=ORIENTED_EDGE('',*,*,#27675,.T.);
#41321=ORIENTED_EDGE('',*,*,#27814,.F.);
#41322=ORIENTED_EDGE('',*,*,#27661,.T.);
#41323=ORIENTED_EDGE('',*,*,#27815,.T.);
#41324=ORIENTED_EDGE('',*,*,#27672,.T.);
#41325=ORIENTED_EDGE('',*,*,#27374,.F.);
#41326=ORIENTED_EDGE('',*,*,#27660,.T.);
#41327=ORIENTED_EDGE('',*,*,#27376,.T.);
#41328=ORIENTED_EDGE('',*,*,#27673,.T.);
#41329=ORIENTED_EDGE('',*,*,#27815,.F.);
#41330=ORIENTED_EDGE('',*,*,#27663,.T.);
#41331=ORIENTED_EDGE('',*,*,#27816,.T.);
#41332=ORIENTED_EDGE('',*,*,#27670,.T.);
#41333=ORIENTED_EDGE('',*,*,#27370,.F.);
#41334=ORIENTED_EDGE('',*,*,#27662,.T.);
#41335=ORIENTED_EDGE('',*,*,#27372,.T.);
#41336=ORIENTED_EDGE('',*,*,#27671,.T.);
#41337=ORIENTED_EDGE('',*,*,#27816,.F.);
#41338=ORIENTED_EDGE('',*,*,#27665,.T.);
#41339=ORIENTED_EDGE('',*,*,#27817,.T.);
#41340=ORIENTED_EDGE('',*,*,#27668,.T.);
#41341=ORIENTED_EDGE('',*,*,#27366,.F.);
#41342=ORIENTED_EDGE('',*,*,#27664,.T.);
#41343=ORIENTED_EDGE('',*,*,#27368,.T.);
#41344=ORIENTED_EDGE('',*,*,#27669,.T.);
#41345=ORIENTED_EDGE('',*,*,#27817,.F.);
#41346=ORIENTED_EDGE('',*,*,#27565,.T.);
#41347=ORIENTED_EDGE('',*,*,#27818,.T.);
#41348=ORIENTED_EDGE('',*,*,#27666,.T.);
#41349=ORIENTED_EDGE('',*,*,#27360,.F.);
#41350=ORIENTED_EDGE('',*,*,#27564,.T.);
#41351=ORIENTED_EDGE('',*,*,#27364,.T.);
#41352=ORIENTED_EDGE('',*,*,#27667,.T.);
#41353=ORIENTED_EDGE('',*,*,#27818,.F.);
#41354=ORIENTED_EDGE('',*,*,#27819,.F.);
#41355=ORIENTED_EDGE('',*,*,#27820,.T.);
#41356=ORIENTED_EDGE('',*,*,#27821,.T.);
#41357=ORIENTED_EDGE('',*,*,#27822,.T.);
#41358=ORIENTED_EDGE('',*,*,#27823,.F.);
#41359=ORIENTED_EDGE('',*,*,#27824,.T.);
#41360=ORIENTED_EDGE('',*,*,#27825,.T.);
#41361=ORIENTED_EDGE('',*,*,#27824,.F.);
#41362=ORIENTED_EDGE('',*,*,#27826,.F.);
#41363=ORIENTED_EDGE('',*,*,#27827,.F.);
#41364=ORIENTED_EDGE('',*,*,#27828,.T.);
#41365=ORIENTED_EDGE('',*,*,#27820,.F.);
#41366=ORIENTED_EDGE('',*,*,#27829,.T.);
#41367=ORIENTED_EDGE('',*,*,#27830,.T.);
#41368=ORIENTED_EDGE('',*,*,#27831,.F.);
#41369=ORIENTED_EDGE('',*,*,#27830,.F.);
#41370=ORIENTED_EDGE('',*,*,#27832,.F.);
#41371=ORIENTED_EDGE('',*,*,#27833,.T.);
#41372=ORIENTED_EDGE('',*,*,#27834,.T.);
#41373=ORIENTED_EDGE('',*,*,#27835,.T.);
#41374=ORIENTED_EDGE('',*,*,#27834,.F.);
#41375=ORIENTED_EDGE('',*,*,#27836,.F.);
#41376=ORIENTED_EDGE('',*,*,#27837,.F.);
#41377=ORIENTED_EDGE('',*,*,#27838,.T.);
#41378=ORIENTED_EDGE('',*,*,#27839,.F.);
#41379=ORIENTED_EDGE('',*,*,#27840,.F.);
#41380=ORIENTED_EDGE('',*,*,#27841,.T.);
#41381=ORIENTED_EDGE('',*,*,#27842,.T.);
#41382=ORIENTED_EDGE('',*,*,#27841,.F.);
#41383=ORIENTED_EDGE('',*,*,#27832,.T.);
#41384=ORIENTED_EDGE('',*,*,#27843,.T.);
#41385=ORIENTED_EDGE('',*,*,#27844,.T.);
#41386=ORIENTED_EDGE('',*,*,#27845,.T.);
#41387=ORIENTED_EDGE('',*,*,#27844,.F.);
#41388=ORIENTED_EDGE('',*,*,#27846,.T.);
#41389=ORIENTED_EDGE('',*,*,#27847,.T.);
#41390=ORIENTED_EDGE('',*,*,#27848,.F.);
#41391=ORIENTED_EDGE('',*,*,#27849,.F.);
#41392=ORIENTED_EDGE('',*,*,#27850,.T.);
#41393=ORIENTED_EDGE('',*,*,#27845,.F.);
#41394=ORIENTED_EDGE('',*,*,#27851,.T.);
#41395=ORIENTED_EDGE('',*,*,#27852,.T.);
#41396=ORIENTED_EDGE('',*,*,#27851,.F.);
#41397=ORIENTED_EDGE('',*,*,#27853,.T.);
#41398=ORIENTED_EDGE('',*,*,#27854,.T.);
#41399=ORIENTED_EDGE('',*,*,#27855,.T.);
#41400=ORIENTED_EDGE('',*,*,#27854,.F.);
#41401=ORIENTED_EDGE('',*,*,#27856,.F.);
#41402=ORIENTED_EDGE('',*,*,#27857,.F.);
#41403=ORIENTED_EDGE('',*,*,#27858,.F.);
#41404=ORIENTED_EDGE('',*,*,#27859,.T.);
#41405=ORIENTED_EDGE('',*,*,#27860,.F.);
#41406=ORIENTED_EDGE('',*,*,#27861,.T.);
#41407=ORIENTED_EDGE('',*,*,#27862,.T.);
#41408=ORIENTED_EDGE('',*,*,#27863,.F.);
#41409=ORIENTED_EDGE('',*,*,#27864,.F.);
#41410=ORIENTED_EDGE('',*,*,#27865,.F.);
#41411=ORIENTED_EDGE('',*,*,#27866,.F.);
#41412=ORIENTED_EDGE('',*,*,#27867,.T.);
#41413=ORIENTED_EDGE('',*,*,#27868,.T.);
#41414=ORIENTED_EDGE('',*,*,#27867,.F.);
#41415=ORIENTED_EDGE('',*,*,#27869,.F.);
#41416=ORIENTED_EDGE('',*,*,#27870,.T.);
#41417=ORIENTED_EDGE('',*,*,#27871,.T.);
#41418=ORIENTED_EDGE('',*,*,#27870,.F.);
#41419=ORIENTED_EDGE('',*,*,#27872,.F.);
#41420=ORIENTED_EDGE('',*,*,#27873,.T.);
#41421=ORIENTED_EDGE('',*,*,#27874,.T.);
#41422=ORIENTED_EDGE('',*,*,#27873,.F.);
#41423=ORIENTED_EDGE('',*,*,#27875,.T.);
#41424=ORIENTED_EDGE('',*,*,#27876,.T.);
#41425=ORIENTED_EDGE('',*,*,#27877,.F.);
#41426=ORIENTED_EDGE('',*,*,#27876,.F.);
#41427=ORIENTED_EDGE('',*,*,#27878,.T.);
#41428=ORIENTED_EDGE('',*,*,#27879,.T.);
#41429=ORIENTED_EDGE('',*,*,#27880,.T.);
#41430=ORIENTED_EDGE('',*,*,#27881,.F.);
#41431=ORIENTED_EDGE('',*,*,#27882,.F.);
#41432=ORIENTED_EDGE('',*,*,#27883,.T.);
#41433=ORIENTED_EDGE('',*,*,#27884,.F.);
#41434=ORIENTED_EDGE('',*,*,#27883,.F.);
#41435=ORIENTED_EDGE('',*,*,#27885,.T.);
#41436=ORIENTED_EDGE('',*,*,#27879,.F.);
#41437=ORIENTED_EDGE('',*,*,#27886,.T.);
#41438=ORIENTED_EDGE('',*,*,#27887,.T.);
#41439=ORIENTED_EDGE('',*,*,#27888,.F.);
#41440=ORIENTED_EDGE('',*,*,#27887,.F.);
#41441=ORIENTED_EDGE('',*,*,#27849,.T.);
#41442=ORIENTED_EDGE('',*,*,#27889,.T.);
#41443=ORIENTED_EDGE('',*,*,#27890,.F.);
#41444=ORIENTED_EDGE('',*,*,#27889,.F.);
#41445=ORIENTED_EDGE('',*,*,#27848,.T.);
#41446=ORIENTED_EDGE('',*,*,#27891,.T.);
#41447=ORIENTED_EDGE('',*,*,#27892,.T.);
#41448=ORIENTED_EDGE('',*,*,#27893,.T.);
#41449=ORIENTED_EDGE('',*,*,#27894,.F.);
#41450=ORIENTED_EDGE('',*,*,#27895,.T.);
#41451=ORIENTED_EDGE('',*,*,#27896,.T.);
#41452=ORIENTED_EDGE('',*,*,#27837,.T.);
#41453=ORIENTED_EDGE('',*,*,#27897,.F.);
#41454=ORIENTED_EDGE('',*,*,#27898,.T.);
#41455=ORIENTED_EDGE('',*,*,#27899,.F.);
#41456=ORIENTED_EDGE('',*,*,#27900,.F.);
#41457=ORIENTED_EDGE('',*,*,#27901,.F.);
#41458=ORIENTED_EDGE('',*,*,#27902,.T.);
#41459=ORIENTED_EDGE('',*,*,#27903,.T.);
#41460=ORIENTED_EDGE('',*,*,#27904,.T.);
#41461=ORIENTED_EDGE('',*,*,#27905,.F.);
#41462=ORIENTED_EDGE('',*,*,#27906,.T.);
#41463=ORIENTED_EDGE('',*,*,#27907,.F.);
#41464=ORIENTED_EDGE('',*,*,#27908,.T.);
#41465=ORIENTED_EDGE('',*,*,#27909,.F.);
#41466=ORIENTED_EDGE('',*,*,#27910,.F.);
#41467=ORIENTED_EDGE('',*,*,#27850,.F.);
#41468=ORIENTED_EDGE('',*,*,#27893,.F.);
#41469=ORIENTED_EDGE('',*,*,#27911,.T.);
#41470=ORIENTED_EDGE('',*,*,#27912,.F.);
#41471=ORIENTED_EDGE('',*,*,#27911,.F.);
#41472=ORIENTED_EDGE('',*,*,#27892,.F.);
#41473=ORIENTED_EDGE('',*,*,#27913,.F.);
#41474=ORIENTED_EDGE('',*,*,#27914,.F.);
#41475=ORIENTED_EDGE('',*,*,#27880,.F.);
#41476=ORIENTED_EDGE('',*,*,#27915,.F.);
#41477=ORIENTED_EDGE('',*,*,#27916,.F.);
#41478=ORIENTED_EDGE('',*,*,#27917,.T.);
#41479=ORIENTED_EDGE('',*,*,#27918,.T.);
#41480=ORIENTED_EDGE('',*,*,#27919,.T.);
#41481=ORIENTED_EDGE('',*,*,#27920,.T.);
#41482=ORIENTED_EDGE('',*,*,#27921,.T.);
#41483=ORIENTED_EDGE('',*,*,#27908,.F.);
#41484=ORIENTED_EDGE('',*,*,#27922,.F.);
#41485=ORIENTED_EDGE('',*,*,#27923,.T.);
#41486=ORIENTED_EDGE('',*,*,#27924,.T.);
#41487=ORIENTED_EDGE('',*,*,#27925,.F.);
#41488=ORIENTED_EDGE('',*,*,#27926,.F.);
#41489=ORIENTED_EDGE('',*,*,#27906,.F.);
#41490=ORIENTED_EDGE('',*,*,#27927,.F.);
#41491=ORIENTED_EDGE('',*,*,#27928,.F.);
#41492=ORIENTED_EDGE('',*,*,#27929,.T.);
#41493=ORIENTED_EDGE('',*,*,#27930,.T.);
#41494=ORIENTED_EDGE('',*,*,#27931,.T.);
#41495=ORIENTED_EDGE('',*,*,#27932,.T.);
#41496=ORIENTED_EDGE('',*,*,#27933,.T.);
#41497=ORIENTED_EDGE('',*,*,#27934,.T.);
#41498=ORIENTED_EDGE('',*,*,#27935,.F.);
#41499=ORIENTED_EDGE('',*,*,#27936,.T.);
#41500=ORIENTED_EDGE('',*,*,#27937,.F.);
#41501=ORIENTED_EDGE('',*,*,#27864,.T.);
#41502=ORIENTED_EDGE('',*,*,#27938,.T.);
#41503=ORIENTED_EDGE('',*,*,#27939,.T.);
#41504=ORIENTED_EDGE('',*,*,#27940,.T.);
#41505=ORIENTED_EDGE('',*,*,#27941,.T.);
#41506=ORIENTED_EDGE('',*,*,#27942,.T.);
#41507=ORIENTED_EDGE('',*,*,#27943,.T.);
#41508=ORIENTED_EDGE('',*,*,#27944,.T.);
#41509=ORIENTED_EDGE('',*,*,#27945,.F.);
#41510=ORIENTED_EDGE('',*,*,#27946,.F.);
#41511=ORIENTED_EDGE('',*,*,#27838,.F.);
#41512=ORIENTED_EDGE('',*,*,#27896,.F.);
#41513=ORIENTED_EDGE('',*,*,#27946,.T.);
#41514=ORIENTED_EDGE('',*,*,#27947,.F.);
#41515=ORIENTED_EDGE('',*,*,#27948,.F.);
#41516=ORIENTED_EDGE('',*,*,#27857,.T.);
#41517=ORIENTED_EDGE('',*,*,#27949,.F.);
#41518=ORIENTED_EDGE('',*,*,#27839,.T.);
#41519=ORIENTED_EDGE('',*,*,#27847,.F.);
#41520=ORIENTED_EDGE('',*,*,#27950,.F.);
#41521=ORIENTED_EDGE('',*,*,#27951,.T.);
#41522=ORIENTED_EDGE('',*,*,#27913,.T.);
#41523=ORIENTED_EDGE('',*,*,#27891,.F.);
#41524=ORIENTED_EDGE('',*,*,#27859,.F.);
#41525=ORIENTED_EDGE('',*,*,#27952,.F.);
#41526=ORIENTED_EDGE('',*,*,#27953,.T.);
#41527=ORIENTED_EDGE('',*,*,#27954,.T.);
#41528=ORIENTED_EDGE('',*,*,#27955,.T.);
#41529=ORIENTED_EDGE('',*,*,#27956,.F.);
#41530=ORIENTED_EDGE('',*,*,#27957,.F.);
#41531=ORIENTED_EDGE('',*,*,#27958,.T.);
#41532=ORIENTED_EDGE('',*,*,#27959,.F.);
#41533=ORIENTED_EDGE('',*,*,#27960,.F.);
#41534=ORIENTED_EDGE('',*,*,#27961,.T.);
#41535=ORIENTED_EDGE('',*,*,#27962,.T.);
#41536=ORIENTED_EDGE('',*,*,#27963,.T.);
#41537=ORIENTED_EDGE('',*,*,#27964,.T.);
#41538=ORIENTED_EDGE('',*,*,#27965,.T.);
#41539=ORIENTED_EDGE('',*,*,#27966,.T.);
#41540=ORIENTED_EDGE('',*,*,#27967,.T.);
#41541=ORIENTED_EDGE('',*,*,#27968,.T.);
#41542=ORIENTED_EDGE('',*,*,#27969,.F.);
#41543=ORIENTED_EDGE('',*,*,#27970,.F.);
#41544=ORIENTED_EDGE('',*,*,#27971,.F.);
#41545=ORIENTED_EDGE('',*,*,#27972,.F.);
#41546=ORIENTED_EDGE('',*,*,#27973,.F.);
#41547=ORIENTED_EDGE('',*,*,#27974,.F.);
#41548=ORIENTED_EDGE('',*,*,#27975,.F.);
#41549=ORIENTED_EDGE('',*,*,#27976,.F.);
#41550=ORIENTED_EDGE('',*,*,#27874,.F.);
#41551=ORIENTED_EDGE('',*,*,#27871,.F.);
#41552=ORIENTED_EDGE('',*,*,#27868,.F.);
#41553=ORIENTED_EDGE('',*,*,#27897,.T.);
#41554=ORIENTED_EDGE('',*,*,#27836,.T.);
#41555=ORIENTED_EDGE('',*,*,#27949,.T.);
#41556=ORIENTED_EDGE('',*,*,#27856,.T.);
#41557=ORIENTED_EDGE('',*,*,#27954,.F.);
#41558=ORIENTED_EDGE('',*,*,#27977,.F.);
#41559=ORIENTED_EDGE('',*,*,#27978,.T.);
#41560=ORIENTED_EDGE('',*,*,#27979,.F.);
#41561=ORIENTED_EDGE('',*,*,#27980,.F.);
#41562=ORIENTED_EDGE('',*,*,#27981,.F.);
#41563=ORIENTED_EDGE('',*,*,#27982,.F.);
#41564=ORIENTED_EDGE('',*,*,#27983,.F.);
#41565=ORIENTED_EDGE('',*,*,#27984,.F.);
#41566=ORIENTED_EDGE('',*,*,#27985,.F.);
#41567=ORIENTED_EDGE('',*,*,#27986,.F.);
#41568=ORIENTED_EDGE('',*,*,#27987,.F.);
#41569=ORIENTED_EDGE('',*,*,#27988,.F.);
#41570=ORIENTED_EDGE('',*,*,#27989,.F.);
#41571=ORIENTED_EDGE('',*,*,#27990,.F.);
#41572=ORIENTED_EDGE('',*,*,#27991,.F.);
#41573=ORIENTED_EDGE('',*,*,#27992,.T.);
#41574=ORIENTED_EDGE('',*,*,#27993,.F.);
#41575=ORIENTED_EDGE('',*,*,#27994,.F.);
#41576=ORIENTED_EDGE('',*,*,#27995,.F.);
#41577=ORIENTED_EDGE('',*,*,#27996,.F.);
#41578=ORIENTED_EDGE('',*,*,#27997,.F.);
#41579=ORIENTED_EDGE('',*,*,#27998,.F.);
#41580=ORIENTED_EDGE('',*,*,#27999,.F.);
#41581=ORIENTED_EDGE('',*,*,#27862,.F.);
#41582=ORIENTED_EDGE('',*,*,#28000,.F.);
#41583=ORIENTED_EDGE('',*,*,#28001,.F.);
#41584=ORIENTED_EDGE('',*,*,#28002,.F.);
#41585=ORIENTED_EDGE('',*,*,#28003,.F.);
#41586=ORIENTED_EDGE('',*,*,#27955,.F.);
#41587=ORIENTED_EDGE('',*,*,#28004,.T.);
#41588=ORIENTED_EDGE('',*,*,#27852,.F.);
#41589=ORIENTED_EDGE('',*,*,#27884,.T.);
#41590=ORIENTED_EDGE('',*,*,#27888,.T.);
#41591=ORIENTED_EDGE('',*,*,#27877,.T.);
#41592=ORIENTED_EDGE('',*,*,#27853,.F.);
#41593=ORIENTED_EDGE('',*,*,#27833,.F.);
#41594=ORIENTED_EDGE('',*,*,#28005,.F.);
#41595=ORIENTED_EDGE('',*,*,#28006,.T.);
#41596=ORIENTED_EDGE('',*,*,#28007,.T.);
#41597=ORIENTED_EDGE('',*,*,#27980,.T.);
#41598=ORIENTED_EDGE('',*,*,#27932,.F.);
#41599=ORIENTED_EDGE('',*,*,#28008,.F.);
#41600=ORIENTED_EDGE('',*,*,#27933,.F.);
#41601=ORIENTED_EDGE('',*,*,#28009,.T.);
#41602=ORIENTED_EDGE('',*,*,#28005,.T.);
#41603=ORIENTED_EDGE('',*,*,#27979,.T.);
#41604=ORIENTED_EDGE('',*,*,#28010,.F.);
#41605=ORIENTED_EDGE('',*,*,#28011,.F.);
#41606=ORIENTED_EDGE('',*,*,#27924,.F.);
#41607=ORIENTED_EDGE('',*,*,#28012,.F.);
#41608=ORIENTED_EDGE('',*,*,#28013,.F.);
#41609=ORIENTED_EDGE('',*,*,#28014,.T.);
#41610=ORIENTED_EDGE('',*,*,#28010,.T.);
#41611=ORIENTED_EDGE('',*,*,#28015,.T.);
#41612=ORIENTED_EDGE('',*,*,#27935,.T.);
#41613=ORIENTED_EDGE('',*,*,#28016,.F.);
#41614=ORIENTED_EDGE('',*,*,#27903,.F.);
#41615=ORIENTED_EDGE('',*,*,#28017,.T.);
#41616=ORIENTED_EDGE('',*,*,#28013,.T.);
#41617=ORIENTED_EDGE('',*,*,#28018,.F.);
#41618=ORIENTED_EDGE('',*,*,#28019,.F.);
#41619=ORIENTED_EDGE('',*,*,#27920,.F.);
#41620=ORIENTED_EDGE('',*,*,#28020,.F.);
#41621=ORIENTED_EDGE('',*,*,#28021,.T.);
#41622=ORIENTED_EDGE('',*,*,#27831,.T.);
#41623=ORIENTED_EDGE('',*,*,#28020,.T.);
#41624=ORIENTED_EDGE('',*,*,#27919,.F.);
#41625=ORIENTED_EDGE('',*,*,#28022,.F.);
#41626=ORIENTED_EDGE('',*,*,#28023,.T.);
#41627=ORIENTED_EDGE('',*,*,#28024,.T.);
#41628=ORIENTED_EDGE('',*,*,#28022,.T.);
#41629=ORIENTED_EDGE('',*,*,#27918,.F.);
#41630=ORIENTED_EDGE('',*,*,#28025,.T.);
#41631=ORIENTED_EDGE('',*,*,#27984,.T.);
#41632=ORIENTED_EDGE('',*,*,#28026,.F.);
#41633=ORIENTED_EDGE('',*,*,#28027,.T.);
#41634=ORIENTED_EDGE('',*,*,#28028,.F.);
#41635=ORIENTED_EDGE('',*,*,#28029,.T.);
#41636=ORIENTED_EDGE('',*,*,#28026,.T.);
#41637=ORIENTED_EDGE('',*,*,#27983,.T.);
#41638=ORIENTED_EDGE('',*,*,#28030,.F.);
#41639=ORIENTED_EDGE('',*,*,#28031,.T.);
#41640=ORIENTED_EDGE('',*,*,#28028,.T.);
#41641=ORIENTED_EDGE('',*,*,#27982,.T.);
#41642=ORIENTED_EDGE('',*,*,#28007,.F.);
#41643=ORIENTED_EDGE('',*,*,#28032,.T.);
#41644=ORIENTED_EDGE('',*,*,#28030,.T.);
#41645=ORIENTED_EDGE('',*,*,#27981,.T.);
#41646=ORIENTED_EDGE('',*,*,#27825,.F.);
#41647=ORIENTED_EDGE('',*,*,#28033,.F.);
#41648=ORIENTED_EDGE('',*,*,#28006,.F.);
#41649=ORIENTED_EDGE('',*,*,#28034,.F.);
#41650=ORIENTED_EDGE('',*,*,#27966,.F.);
#41651=ORIENTED_EDGE('',*,*,#28034,.T.);
#41652=ORIENTED_EDGE('',*,*,#28009,.F.);
#41653=ORIENTED_EDGE('',*,*,#28035,.F.);
#41654=ORIENTED_EDGE('',*,*,#27967,.F.);
#41655=ORIENTED_EDGE('',*,*,#28033,.T.);
#41656=ORIENTED_EDGE('',*,*,#27965,.F.);
#41657=ORIENTED_EDGE('',*,*,#28036,.F.);
#41658=ORIENTED_EDGE('',*,*,#28032,.F.);
#41659=ORIENTED_EDGE('',*,*,#28035,.T.);
#41660=ORIENTED_EDGE('',*,*,#27936,.F.);
#41661=ORIENTED_EDGE('',*,*,#28037,.F.);
#41662=ORIENTED_EDGE('',*,*,#27968,.F.);
#41663=ORIENTED_EDGE('',*,*,#28036,.T.);
#41664=ORIENTED_EDGE('',*,*,#27964,.F.);
#41665=ORIENTED_EDGE('',*,*,#28038,.F.);
#41666=ORIENTED_EDGE('',*,*,#28031,.F.);
#41667=ORIENTED_EDGE('',*,*,#28021,.F.);
#41668=ORIENTED_EDGE('',*,*,#28024,.F.);
#41669=ORIENTED_EDGE('',*,*,#28039,.F.);
#41670=ORIENTED_EDGE('',*,*,#27961,.F.);
#41671=ORIENTED_EDGE('',*,*,#28037,.T.);
#41672=ORIENTED_EDGE('',*,*,#28038,.T.);
#41673=ORIENTED_EDGE('',*,*,#27963,.F.);
#41674=ORIENTED_EDGE('',*,*,#28040,.F.);
#41675=ORIENTED_EDGE('',*,*,#28029,.F.);
#41676=ORIENTED_EDGE('',*,*,#28023,.F.);
#41677=ORIENTED_EDGE('',*,*,#28027,.F.);
#41678=ORIENTED_EDGE('',*,*,#28040,.T.);
#41679=ORIENTED_EDGE('',*,*,#27962,.F.);
#41680=ORIENTED_EDGE('',*,*,#28039,.T.);
#41681=ORIENTED_EDGE('',*,*,#27872,.T.);
#41682=ORIENTED_EDGE('',*,*,#27875,.F.);
#41683=ORIENTED_EDGE('',*,*,#27869,.T.);
#41684=ORIENTED_EDGE('',*,*,#27878,.F.);
#41685=ORIENTED_EDGE('',*,*,#27866,.T.);
#41686=ORIENTED_EDGE('',*,*,#27886,.F.);
#41687=ORIENTED_EDGE('',*,*,#28019,.T.);
#41688=ORIENTED_EDGE('',*,*,#28041,.T.);
#41689=ORIENTED_EDGE('',*,*,#27991,.T.);
#41690=ORIENTED_EDGE('',*,*,#28042,.F.);
#41691=ORIENTED_EDGE('',*,*,#28043,.T.);
#41692=ORIENTED_EDGE('',*,*,#27909,.T.);
#41693=ORIENTED_EDGE('',*,*,#27921,.F.);
#41694=ORIENTED_EDGE('',*,*,#28044,.F.);
#41695=ORIENTED_EDGE('',*,*,#28045,.T.);
#41696=ORIENTED_EDGE('',*,*,#28042,.T.);
#41697=ORIENTED_EDGE('',*,*,#27990,.T.);
#41698=ORIENTED_EDGE('',*,*,#28046,.F.);
#41699=ORIENTED_EDGE('',*,*,#28047,.T.);
#41700=ORIENTED_EDGE('',*,*,#28044,.T.);
#41701=ORIENTED_EDGE('',*,*,#27989,.T.);
#41702=ORIENTED_EDGE('',*,*,#28048,.F.);
#41703=ORIENTED_EDGE('',*,*,#28049,.T.);
#41704=ORIENTED_EDGE('',*,*,#28046,.T.);
#41705=ORIENTED_EDGE('',*,*,#27988,.T.);
#41706=ORIENTED_EDGE('',*,*,#28050,.F.);
#41707=ORIENTED_EDGE('',*,*,#28051,.T.);
#41708=ORIENTED_EDGE('',*,*,#28048,.T.);
#41709=ORIENTED_EDGE('',*,*,#27987,.T.);
#41710=ORIENTED_EDGE('',*,*,#28052,.F.);
#41711=ORIENTED_EDGE('',*,*,#28053,.T.);
#41712=ORIENTED_EDGE('',*,*,#28050,.T.);
#41713=ORIENTED_EDGE('',*,*,#27986,.T.);
#41714=ORIENTED_EDGE('',*,*,#27917,.F.);
#41715=ORIENTED_EDGE('',*,*,#28054,.T.);
#41716=ORIENTED_EDGE('',*,*,#28055,.T.);
#41717=ORIENTED_EDGE('',*,*,#28052,.T.);
#41718=ORIENTED_EDGE('',*,*,#27985,.T.);
#41719=ORIENTED_EDGE('',*,*,#28025,.F.);
#41720=ORIENTED_EDGE('',*,*,#27916,.T.);
#41721=ORIENTED_EDGE('',*,*,#28056,.F.);
#41722=ORIENTED_EDGE('',*,*,#28057,.F.);
#41723=ORIENTED_EDGE('',*,*,#28054,.F.);
#41724=ORIENTED_EDGE('',*,*,#27843,.F.);
#41725=ORIENTED_EDGE('',*,*,#27910,.T.);
#41726=ORIENTED_EDGE('',*,*,#28043,.F.);
#41727=ORIENTED_EDGE('',*,*,#28045,.F.);
#41728=ORIENTED_EDGE('',*,*,#28047,.F.);
#41729=ORIENTED_EDGE('',*,*,#28049,.F.);
#41730=ORIENTED_EDGE('',*,*,#28051,.F.);
#41731=ORIENTED_EDGE('',*,*,#28053,.F.);
#41732=ORIENTED_EDGE('',*,*,#28055,.F.);
#41733=ORIENTED_EDGE('',*,*,#28057,.T.);
#41734=ORIENTED_EDGE('',*,*,#28058,.T.);
#41735=ORIENTED_EDGE('',*,*,#27882,.T.);
#41736=ORIENTED_EDGE('',*,*,#28059,.T.);
#41737=ORIENTED_EDGE('',*,*,#27950,.T.);
#41738=ORIENTED_EDGE('',*,*,#27846,.F.);
#41739=ORIENTED_EDGE('',*,*,#27915,.T.);
#41740=ORIENTED_EDGE('',*,*,#27885,.F.);
#41741=ORIENTED_EDGE('',*,*,#28058,.F.);
#41742=ORIENTED_EDGE('',*,*,#28056,.T.);
#41743=ORIENTED_EDGE('',*,*,#27914,.T.);
#41744=ORIENTED_EDGE('',*,*,#27951,.F.);
#41745=ORIENTED_EDGE('',*,*,#28059,.F.);
#41746=ORIENTED_EDGE('',*,*,#27881,.T.);
#41747=ORIENTED_EDGE('',*,*,#28000,.T.);
#41748=ORIENTED_EDGE('',*,*,#27861,.F.);
#41749=ORIENTED_EDGE('',*,*,#28060,.F.);
#41750=ORIENTED_EDGE('',*,*,#28061,.T.);
#41751=ORIENTED_EDGE('',*,*,#28001,.T.);
#41752=ORIENTED_EDGE('',*,*,#28061,.F.);
#41753=ORIENTED_EDGE('',*,*,#28062,.F.);
#41754=ORIENTED_EDGE('',*,*,#28063,.T.);
#41755=ORIENTED_EDGE('',*,*,#28002,.T.);
#41756=ORIENTED_EDGE('',*,*,#28063,.F.);
#41757=ORIENTED_EDGE('',*,*,#28064,.F.);
#41758=ORIENTED_EDGE('',*,*,#28065,.T.);
#41759=ORIENTED_EDGE('',*,*,#28003,.T.);
#41760=ORIENTED_EDGE('',*,*,#28065,.F.);
#41761=ORIENTED_EDGE('',*,*,#28066,.F.);
#41762=ORIENTED_EDGE('',*,*,#27956,.T.);
#41763=ORIENTED_EDGE('',*,*,#28067,.T.);
#41764=ORIENTED_EDGE('',*,*,#28068,.T.);
#41765=ORIENTED_EDGE('',*,*,#27977,.T.);
#41766=ORIENTED_EDGE('',*,*,#27953,.F.);
#41767=ORIENTED_EDGE('',*,*,#28069,.F.);
#41768=ORIENTED_EDGE('',*,*,#28070,.T.);
#41769=ORIENTED_EDGE('',*,*,#28071,.T.);
#41770=ORIENTED_EDGE('',*,*,#28067,.F.);
#41771=ORIENTED_EDGE('',*,*,#28072,.F.);
#41772=ORIENTED_EDGE('',*,*,#27993,.T.);
#41773=ORIENTED_EDGE('',*,*,#28073,.T.);
#41774=ORIENTED_EDGE('',*,*,#28070,.F.);
#41775=ORIENTED_EDGE('',*,*,#28074,.F.);
#41776=ORIENTED_EDGE('',*,*,#28075,.T.);
#41777=ORIENTED_EDGE('',*,*,#27944,.F.);
#41778=ORIENTED_EDGE('',*,*,#28076,.T.);
#41779=ORIENTED_EDGE('',*,*,#27994,.T.);
#41780=ORIENTED_EDGE('',*,*,#28076,.F.);
#41781=ORIENTED_EDGE('',*,*,#27943,.F.);
#41782=ORIENTED_EDGE('',*,*,#28077,.T.);
#41783=ORIENTED_EDGE('',*,*,#27995,.T.);
#41784=ORIENTED_EDGE('',*,*,#28077,.F.);
#41785=ORIENTED_EDGE('',*,*,#27942,.F.);
#41786=ORIENTED_EDGE('',*,*,#28078,.T.);
#41787=ORIENTED_EDGE('',*,*,#27996,.T.);
#41788=ORIENTED_EDGE('',*,*,#28078,.F.);
#41789=ORIENTED_EDGE('',*,*,#27941,.F.);
#41790=ORIENTED_EDGE('',*,*,#28079,.T.);
#41791=ORIENTED_EDGE('',*,*,#27997,.T.);
#41792=ORIENTED_EDGE('',*,*,#28079,.F.);
#41793=ORIENTED_EDGE('',*,*,#27940,.F.);
#41794=ORIENTED_EDGE('',*,*,#28080,.T.);
#41795=ORIENTED_EDGE('',*,*,#27998,.T.);
#41796=ORIENTED_EDGE('',*,*,#28080,.F.);
#41797=ORIENTED_EDGE('',*,*,#27939,.F.);
#41798=ORIENTED_EDGE('',*,*,#28081,.T.);
#41799=ORIENTED_EDGE('',*,*,#27999,.T.);
#41800=ORIENTED_EDGE('',*,*,#28081,.F.);
#41801=ORIENTED_EDGE('',*,*,#27938,.F.);
#41802=ORIENTED_EDGE('',*,*,#27863,.T.);
#41803=ORIENTED_EDGE('',*,*,#27978,.F.);
#41804=ORIENTED_EDGE('',*,*,#28068,.F.);
#41805=ORIENTED_EDGE('',*,*,#28071,.F.);
#41806=ORIENTED_EDGE('',*,*,#28073,.F.);
#41807=ORIENTED_EDGE('',*,*,#27992,.F.);
#41808=ORIENTED_EDGE('',*,*,#28041,.F.);
#41809=ORIENTED_EDGE('',*,*,#28018,.T.);
#41810=ORIENTED_EDGE('',*,*,#28015,.F.);
#41811=ORIENTED_EDGE('',*,*,#28004,.F.);
#41812=ORIENTED_EDGE('',*,*,#27960,.T.);
#41813=ORIENTED_EDGE('',*,*,#28082,.F.);
#41814=ORIENTED_EDGE('',*,*,#27898,.F.);
#41815=ORIENTED_EDGE('',*,*,#27855,.F.);
#41816=ORIENTED_EDGE('',*,*,#27899,.T.);
#41817=ORIENTED_EDGE('',*,*,#28082,.T.);
#41818=ORIENTED_EDGE('',*,*,#27959,.T.);
#41819=ORIENTED_EDGE('',*,*,#28083,.T.);
#41820=ORIENTED_EDGE('',*,*,#27890,.T.);
#41821=ORIENTED_EDGE('',*,*,#27842,.F.);
#41822=ORIENTED_EDGE('',*,*,#27840,.T.);
#41823=ORIENTED_EDGE('',*,*,#27835,.F.);
#41824=ORIENTED_EDGE('',*,*,#27970,.T.);
#41825=ORIENTED_EDGE('',*,*,#28084,.F.);
#41826=ORIENTED_EDGE('',*,*,#28085,.F.);
#41827=ORIENTED_EDGE('',*,*,#28086,.T.);
#41828=ORIENTED_EDGE('',*,*,#27971,.T.);
#41829=ORIENTED_EDGE('',*,*,#28086,.F.);
#41830=ORIENTED_EDGE('',*,*,#28087,.F.);
#41831=ORIENTED_EDGE('',*,*,#28088,.T.);
#41832=ORIENTED_EDGE('',*,*,#27972,.T.);
#41833=ORIENTED_EDGE('',*,*,#28088,.F.);
#41834=ORIENTED_EDGE('',*,*,#28089,.F.);
#41835=ORIENTED_EDGE('',*,*,#28090,.T.);
#41836=ORIENTED_EDGE('',*,*,#27973,.T.);
#41837=ORIENTED_EDGE('',*,*,#28090,.F.);
#41838=ORIENTED_EDGE('',*,*,#28091,.F.);
#41839=ORIENTED_EDGE('',*,*,#28092,.T.);
#41840=ORIENTED_EDGE('',*,*,#27974,.T.);
#41841=ORIENTED_EDGE('',*,*,#28092,.F.);
#41842=ORIENTED_EDGE('',*,*,#28093,.F.);
#41843=ORIENTED_EDGE('',*,*,#28094,.T.);
#41844=ORIENTED_EDGE('',*,*,#27975,.T.);
#41845=ORIENTED_EDGE('',*,*,#28094,.F.);
#41846=ORIENTED_EDGE('',*,*,#28095,.F.);
#41847=ORIENTED_EDGE('',*,*,#28096,.T.);
#41848=ORIENTED_EDGE('',*,*,#27976,.T.);
#41849=ORIENTED_EDGE('',*,*,#28096,.F.);
#41850=ORIENTED_EDGE('',*,*,#28097,.F.);
#41851=ORIENTED_EDGE('',*,*,#28098,.T.);
#41852=ORIENTED_EDGE('',*,*,#27969,.T.);
#41853=ORIENTED_EDGE('',*,*,#28098,.F.);
#41854=ORIENTED_EDGE('',*,*,#28099,.F.);
#41855=ORIENTED_EDGE('',*,*,#28084,.T.);
#41856=ORIENTED_EDGE('',*,*,#28085,.T.);
#41857=ORIENTED_EDGE('',*,*,#28099,.T.);
#41858=ORIENTED_EDGE('',*,*,#28097,.T.);
#41859=ORIENTED_EDGE('',*,*,#28095,.T.);
#41860=ORIENTED_EDGE('',*,*,#28093,.T.);
#41861=ORIENTED_EDGE('',*,*,#28091,.T.);
#41862=ORIENTED_EDGE('',*,*,#28089,.T.);
#41863=ORIENTED_EDGE('',*,*,#28087,.T.);
#41864=ORIENTED_EDGE('',*,*,#27945,.T.);
#41865=ORIENTED_EDGE('',*,*,#28075,.F.);
#41866=ORIENTED_EDGE('',*,*,#28100,.F.);
#41867=ORIENTED_EDGE('',*,*,#27947,.T.);
#41868=ORIENTED_EDGE('',*,*,#28100,.T.);
#41869=ORIENTED_EDGE('',*,*,#28074,.T.);
#41870=ORIENTED_EDGE('',*,*,#28072,.T.);
#41871=ORIENTED_EDGE('',*,*,#28069,.T.);
#41872=ORIENTED_EDGE('',*,*,#27952,.T.);
#41873=ORIENTED_EDGE('',*,*,#27858,.T.);
#41874=ORIENTED_EDGE('',*,*,#27948,.T.);
#41875=ORIENTED_EDGE('',*,*,#28101,.F.);
#41876=ORIENTED_EDGE('',*,*,#28102,.T.);
#41877=ORIENTED_EDGE('',*,*,#28103,.T.);
#41878=ORIENTED_EDGE('',*,*,#28104,.T.);
#41879=ORIENTED_EDGE('',*,*,#28105,.F.);
#41880=ORIENTED_EDGE('',*,*,#27900,.T.);
#41881=ORIENTED_EDGE('',*,*,#28083,.F.);
#41882=ORIENTED_EDGE('',*,*,#27958,.F.);
#41883=ORIENTED_EDGE('',*,*,#27937,.T.);
#41884=ORIENTED_EDGE('',*,*,#27895,.F.);
#41885=ORIENTED_EDGE('',*,*,#28106,.F.);
#41886=ORIENTED_EDGE('',*,*,#27865,.T.);
#41887=ORIENTED_EDGE('',*,*,#28107,.F.);
#41888=ORIENTED_EDGE('',*,*,#28101,.T.);
#41889=ORIENTED_EDGE('',*,*,#27957,.T.);
#41890=ORIENTED_EDGE('',*,*,#28066,.T.);
#41891=ORIENTED_EDGE('',*,*,#28064,.T.);
#41892=ORIENTED_EDGE('',*,*,#28062,.T.);
#41893=ORIENTED_EDGE('',*,*,#28060,.T.);
#41894=ORIENTED_EDGE('',*,*,#27860,.T.);
#41895=ORIENTED_EDGE('',*,*,#28106,.T.);
#41896=ORIENTED_EDGE('',*,*,#27894,.T.);
#41897=ORIENTED_EDGE('',*,*,#28105,.T.);
#41898=ORIENTED_EDGE('',*,*,#28108,.F.);
#41899=ORIENTED_EDGE('',*,*,#28008,.T.);
#41900=ORIENTED_EDGE('',*,*,#27931,.F.);
#41901=ORIENTED_EDGE('',*,*,#27904,.F.);
#41902=ORIENTED_EDGE('',*,*,#28016,.T.);
#41903=ORIENTED_EDGE('',*,*,#27934,.F.);
#41904=ORIENTED_EDGE('',*,*,#28017,.F.);
#41905=ORIENTED_EDGE('',*,*,#27902,.F.);
#41906=ORIENTED_EDGE('',*,*,#27925,.T.);
#41907=ORIENTED_EDGE('',*,*,#28011,.T.);
#41908=ORIENTED_EDGE('',*,*,#28014,.F.);
#41909=ORIENTED_EDGE('',*,*,#27923,.F.);
#41910=ORIENTED_EDGE('',*,*,#28109,.T.);
#41911=ORIENTED_EDGE('',*,*,#27928,.T.);
#41912=ORIENTED_EDGE('',*,*,#28012,.T.);
#41913=ORIENTED_EDGE('',*,*,#28103,.F.);
#41914=ORIENTED_EDGE('',*,*,#28110,.T.);
#41915=ORIENTED_EDGE('',*,*,#28111,.T.);
#41916=ORIENTED_EDGE('',*,*,#28110,.F.);
#41917=ORIENTED_EDGE('',*,*,#28102,.F.);
#41918=ORIENTED_EDGE('',*,*,#28107,.T.);
#41919=ORIENTED_EDGE('',*,*,#28112,.F.);
#41920=ORIENTED_EDGE('',*,*,#28108,.T.);
#41921=ORIENTED_EDGE('',*,*,#28104,.F.);
#41922=ORIENTED_EDGE('',*,*,#28111,.F.);
#41923=ORIENTED_EDGE('',*,*,#28112,.T.);
#41924=ORIENTED_EDGE('',*,*,#27905,.T.);
#41925=ORIENTED_EDGE('',*,*,#27912,.T.);
#41926=ORIENTED_EDGE('',*,*,#28113,.T.);
#41927=ORIENTED_EDGE('',*,*,#27929,.F.);
#41928=ORIENTED_EDGE('',*,*,#28109,.F.);
#41929=ORIENTED_EDGE('',*,*,#27927,.T.);
#41930=ORIENTED_EDGE('',*,*,#27907,.T.);
#41931=ORIENTED_EDGE('',*,*,#27926,.T.);
#41932=ORIENTED_EDGE('',*,*,#27901,.T.);
#41933=ORIENTED_EDGE('',*,*,#27930,.F.);
#41934=ORIENTED_EDGE('',*,*,#28113,.F.);
#41935=ORIENTED_EDGE('',*,*,#27922,.T.);
#41936=ORIENTED_EDGE('',*,*,#27819,.T.);
#41937=ORIENTED_EDGE('',*,*,#27829,.F.);
#41938=ORIENTED_EDGE('',*,*,#28114,.F.);
#41939=ORIENTED_EDGE('',*,*,#28115,.F.);
#41940=ORIENTED_EDGE('',*,*,#27826,.T.);
#41941=ORIENTED_EDGE('',*,*,#27823,.T.);
#41942=ORIENTED_EDGE('',*,*,#28116,.F.);
#41943=ORIENTED_EDGE('',*,*,#28117,.F.);
#41944=ORIENTED_EDGE('',*,*,#28118,.F.);
#41945=ORIENTED_EDGE('',*,*,#28114,.T.);
#41946=ORIENTED_EDGE('',*,*,#28119,.F.);
#41947=ORIENTED_EDGE('',*,*,#27828,.F.);
#41948=ORIENTED_EDGE('',*,*,#28120,.F.);
#41949=ORIENTED_EDGE('',*,*,#28117,.T.);
#41950=ORIENTED_EDGE('',*,*,#28121,.F.);
#41951=ORIENTED_EDGE('',*,*,#27821,.F.);
#41952=ORIENTED_EDGE('',*,*,#28118,.T.);
#41953=ORIENTED_EDGE('',*,*,#28120,.T.);
#41954=ORIENTED_EDGE('',*,*,#27827,.T.);
#41955=ORIENTED_EDGE('',*,*,#28115,.T.);
#41956=ORIENTED_EDGE('',*,*,#28119,.T.);
#41957=ORIENTED_EDGE('',*,*,#28116,.T.);
#41958=ORIENTED_EDGE('',*,*,#27822,.F.);
#41959=ORIENTED_EDGE('',*,*,#28121,.T.);
#41960=CYLINDRICAL_SURFACE('',#45660,0.0015);
#41961=CYLINDRICAL_SURFACE('',#45663,0.004);
#41962=CYLINDRICAL_SURFACE('',#45676,0.0015);
#41963=CYLINDRICAL_SURFACE('',#45681,0.0025);
#41964=CYLINDRICAL_SURFACE('',#45687,0.002);
#41965=CYLINDRICAL_SURFACE('',#45689,0.00175);
#41966=CYLINDRICAL_SURFACE('',#45692,0.0045);
#41967=CYLINDRICAL_SURFACE('',#45697,0.00788400944250797);
#41968=CYLINDRICAL_SURFACE('',#45709,0.00175);
#41969=CYLINDRICAL_SURFACE('',#45718,0.0015);
#41970=CYLINDRICAL_SURFACE('',#46087,0.006);
#41971=CYLINDRICAL_SURFACE('',#46091,0.01201615316635);
#41972=CYLINDRICAL_SURFACE('',#46093,0.006);
#41973=CYLINDRICAL_SURFACE('',#46097,0.006);
#41974=CYLINDRICAL_SURFACE('',#46111,0.006);
#41975=CYLINDRICAL_SURFACE('',#46115,0.006);
#41976=CYLINDRICAL_SURFACE('',#46126,0.006);
#41977=CYLINDRICAL_SURFACE('',#46129,0.006);
#41978=CYLINDRICAL_SURFACE('',#46140,0.006);
#41979=CYLINDRICAL_SURFACE('',#46144,0.006);
#41980=CYLINDRICAL_SURFACE('',#46157,0.006);
#41981=CYLINDRICAL_SURFACE('',#46161,0.006);
#41982=CYLINDRICAL_SURFACE('',#46175,0.006);
#41983=CYLINDRICAL_SURFACE('',#46179,0.00672352098562279);
#41984=CYLINDRICAL_SURFACE('',#46186,0.0115242502778466);
#41985=CYLINDRICAL_SURFACE('',#46193,0.006);
#41986=CYLINDRICAL_SURFACE('',#46201,0.0120161531663839);
#41987=CYLINDRICAL_SURFACE('',#46209,0.006);
#41988=CYLINDRICAL_SURFACE('',#46213,0.006);
#41989=CYLINDRICAL_SURFACE('',#46219,0.006);
#41990=CYLINDRICAL_SURFACE('',#46227,0.006);
#41991=CYLINDRICAL_SURFACE('',#46236,0.006);
#41992=CYLINDRICAL_SURFACE('',#46245,0.0067235209855194);
#41993=CYLINDRICAL_SURFACE('',#46248,0.0115242502778774);
#41994=CYLINDRICAL_SURFACE('',#46254,0.006);
#41995=CYLINDRICAL_SURFACE('',#46262,0.0120161531664264);
#41996=CYLINDRICAL_SURFACE('',#46265,0.006);
#41997=CYLINDRICAL_SURFACE('',#46276,0.006);
#41998=CYLINDRICAL_SURFACE('',#46280,0.006);
#41999=CYLINDRICAL_SURFACE('',#46288,0.006);
#42000=CYLINDRICAL_SURFACE('',#46297,0.006);
#42001=CYLINDRICAL_SURFACE('',#46306,0.00672352092876986);
#42002=CYLINDRICAL_SURFACE('',#46309,0.011524250277822);
#42003=CYLINDRICAL_SURFACE('',#46315,0.006);
#42004=CYLINDRICAL_SURFACE('',#46323,0.012016153166251);
#42005=CYLINDRICAL_SURFACE('',#46326,0.006);
#42006=CYLINDRICAL_SURFACE('',#46335,0.006);
#42007=CYLINDRICAL_SURFACE('',#46346,0.006);
#42008=CYLINDRICAL_SURFACE('',#46349,0.006);
#42009=CYLINDRICAL_SURFACE('',#46358,0.006);
#42010=CYLINDRICAL_SURFACE('',#46367,0.00672352092876213);
#42011=CYLINDRICAL_SURFACE('',#46370,0.0115242502778217);
#42012=CYLINDRICAL_SURFACE('',#46376,0.006);
#42013=CYLINDRICAL_SURFACE('',#46384,0.0120161531662437);
#42014=CYLINDRICAL_SURFACE('',#46387,0.006);
#42015=CYLINDRICAL_SURFACE('',#46396,0.006);
#42016=CYLINDRICAL_SURFACE('',#46402,0.006);
#42017=CYLINDRICAL_SURFACE('',#46415,0.006);
#42018=CYLINDRICAL_SURFACE('',#46419,0.006);
#42019=CYLINDRICAL_SURFACE('',#46428,0.00672352092874661);
#42020=CYLINDRICAL_SURFACE('',#46431,0.0115242502777059);
#42021=CYLINDRICAL_SURFACE('',#46437,0.006);
#42022=CYLINDRICAL_SURFACE('',#46445,0.012016153166215);
#42023=CYLINDRICAL_SURFACE('',#46448,0.006);
#42024=CYLINDRICAL_SURFACE('',#46457,0.006);
#42025=CYLINDRICAL_SURFACE('',#46463,0.006);
#42026=CYLINDRICAL_SURFACE('',#46471,0.006);
#42027=CYLINDRICAL_SURFACE('',#46485,0.006);
#42028=CYLINDRICAL_SURFACE('',#46489,0.00672352098540828);
#42029=CYLINDRICAL_SURFACE('',#46492,0.011524250277971);
#42030=CYLINDRICAL_SURFACE('',#46498,0.006);
#42031=CYLINDRICAL_SURFACE('',#46506,0.0120161531662294);
#42032=CYLINDRICAL_SURFACE('',#46509,0.006);
#42033=CYLINDRICAL_SURFACE('',#46518,0.006);
#42034=CYLINDRICAL_SURFACE('',#46524,0.006);
#42035=CYLINDRICAL_SURFACE('',#46532,0.006);
#42036=CYLINDRICAL_SURFACE('',#46541,0.006);
#42037=CYLINDRICAL_SURFACE('',#46550,0.00672352092867469);
#42038=CYLINDRICAL_SURFACE('',#46553,0.0115242502779462);
#42039=CYLINDRICAL_SURFACE('',#46559,0.006);
#42040=CYLINDRICAL_SURFACE('',#46567,0.0120161531662171);
#42041=CYLINDRICAL_SURFACE('',#46570,0.006);
#42042=CYLINDRICAL_SURFACE('',#46579,0.006);
#42043=CYLINDRICAL_SURFACE('',#46585,0.006);
#42044=CYLINDRICAL_SURFACE('',#46593,0.006);
#42045=CYLINDRICAL_SURFACE('',#46602,0.006);
#42046=CYLINDRICAL_SURFACE('',#46611,0.00672352092871933);
#42047=CYLINDRICAL_SURFACE('',#46614,0.011524250277966);
#42048=CYLINDRICAL_SURFACE('',#46620,0.006);
#42049=CYLINDRICAL_SURFACE('',#46628,0.0120161531661977);
#42050=CYLINDRICAL_SURFACE('',#46631,0.006);
#42051=CYLINDRICAL_SURFACE('',#46640,0.006);
#42052=CYLINDRICAL_SURFACE('',#46646,0.006);
#42053=CYLINDRICAL_SURFACE('',#46654,0.006);
#42054=CYLINDRICAL_SURFACE('',#46663,0.006);
#42055=CYLINDRICAL_SURFACE('',#46672,0.0067235209286786);
#42056=CYLINDRICAL_SURFACE('',#46675,0.0115242502779575);
#42057=CYLINDRICAL_SURFACE('',#46681,0.006);
#42058=CYLINDRICAL_SURFACE('',#46689,0.0120161531661926);
#42059=CYLINDRICAL_SURFACE('',#46692,0.006);
#42060=CYLINDRICAL_SURFACE('',#46701,0.006);
#42061=CYLINDRICAL_SURFACE('',#46707,0.006);
#42062=CYLINDRICAL_SURFACE('',#46715,0.006);
#42063=CYLINDRICAL_SURFACE('',#46724,0.006);
#42064=CYLINDRICAL_SURFACE('',#46733,0.00672352092870445);
#42065=CYLINDRICAL_SURFACE('',#46736,0.0115242502780043);
#42066=CYLINDRICAL_SURFACE('',#46742,0.006);
#42067=CYLINDRICAL_SURFACE('',#46750,0.0120161531661802);
#42068=CYLINDRICAL_SURFACE('',#46753,0.006);
#42069=CYLINDRICAL_SURFACE('',#46762,0.006);
#42070=CYLINDRICAL_SURFACE('',#46768,0.006);
#42071=CYLINDRICAL_SURFACE('',#46776,0.006);
#42072=CYLINDRICAL_SURFACE('',#46785,0.006);
#42073=CYLINDRICAL_SURFACE('',#46794,0.00672352092873228);
#42074=CYLINDRICAL_SURFACE('',#46797,0.011524250277956);
#42075=CYLINDRICAL_SURFACE('',#46803,0.006);
#42076=CYLINDRICAL_SURFACE('',#46811,0.0120161531661636);
#42077=CYLINDRICAL_SURFACE('',#46814,0.006);
#42078=CYLINDRICAL_SURFACE('',#46823,0.006);
#42079=CYLINDRICAL_SURFACE('',#46829,0.006);
#42080=CYLINDRICAL_SURFACE('',#46837,0.006);
#42081=CYLINDRICAL_SURFACE('',#46846,0.006);
#42082=CYLINDRICAL_SURFACE('',#46855,0.00672352092873291);
#42083=CYLINDRICAL_SURFACE('',#46858,0.0115242502780166);
#42084=CYLINDRICAL_SURFACE('',#46864,0.006);
#42085=CYLINDRICAL_SURFACE('',#46872,0.0120161531661576);
#42086=CYLINDRICAL_SURFACE('',#46875,0.006);
#42087=CYLINDRICAL_SURFACE('',#46884,0.006);
#42088=CYLINDRICAL_SURFACE('',#46890,0.006);
#42089=CYLINDRICAL_SURFACE('',#46898,0.006);
#42090=CYLINDRICAL_SURFACE('',#46907,0.006);
#42091=CYLINDRICAL_SURFACE('',#46916,0.0067235209287966);
#42092=CYLINDRICAL_SURFACE('',#46919,0.0115242502780193);
#42093=CYLINDRICAL_SURFACE('',#46925,0.006);
#42094=CYLINDRICAL_SURFACE('',#46933,0.0120161531661516);
#42095=CYLINDRICAL_SURFACE('',#46936,0.006);
#42096=CYLINDRICAL_SURFACE('',#46945,0.006);
#42097=CYLINDRICAL_SURFACE('',#46951,0.006);
#42098=CYLINDRICAL_SURFACE('',#46959,0.006);
#42099=CYLINDRICAL_SURFACE('',#46968,0.006);
#42100=CYLINDRICAL_SURFACE('',#46977,0.00672352092871571);
#42101=CYLINDRICAL_SURFACE('',#46980,0.0115242502780358);
#42102=CYLINDRICAL_SURFACE('',#46986,0.006);
#42103=CYLINDRICAL_SURFACE('',#46994,0.0120161531661375);
#42104=CYLINDRICAL_SURFACE('',#46997,0.006);
#42105=CYLINDRICAL_SURFACE('',#47006,0.006);
#42106=CYLINDRICAL_SURFACE('',#47012,0.006);
#42107=CYLINDRICAL_SURFACE('',#47020,0.006);
#42108=CYLINDRICAL_SURFACE('',#47029,0.006);
#42109=CYLINDRICAL_SURFACE('',#47038,0.00672352092882081);
#42110=CYLINDRICAL_SURFACE('',#47041,0.0115242502780597);
#42111=CYLINDRICAL_SURFACE('',#47047,0.006);
#42112=CYLINDRICAL_SURFACE('',#47055,0.0120161531661259);
#42113=CYLINDRICAL_SURFACE('',#47058,0.006);
#42114=CYLINDRICAL_SURFACE('',#47067,0.006);
#42115=CYLINDRICAL_SURFACE('',#47073,0.006);
#42116=CYLINDRICAL_SURFACE('',#47081,0.006);
#42117=CYLINDRICAL_SURFACE('',#47090,0.006);
#42118=CYLINDRICAL_SURFACE('',#47099,0.00672352092887584);
#42119=CYLINDRICAL_SURFACE('',#47102,0.0115242502780683);
#42120=CYLINDRICAL_SURFACE('',#47108,0.006);
#42121=CYLINDRICAL_SURFACE('',#47116,0.0120161531661189);
#42122=CYLINDRICAL_SURFACE('',#47119,0.006);
#42123=CYLINDRICAL_SURFACE('',#47128,0.006);
#42124=CYLINDRICAL_SURFACE('',#47134,0.006);
#42125=CYLINDRICAL_SURFACE('',#47142,0.006);
#42126=CYLINDRICAL_SURFACE('',#47151,0.006);
#42127=CYLINDRICAL_SURFACE('',#47160,0.00672352092894656);
#42128=CYLINDRICAL_SURFACE('',#47163,0.0115242502780745);
#42129=CYLINDRICAL_SURFACE('',#47169,0.006);
#42130=CYLINDRICAL_SURFACE('',#47177,0.0120161531661058);
#42131=CYLINDRICAL_SURFACE('',#47180,0.006);
#42132=CYLINDRICAL_SURFACE('',#47189,0.006);
#42133=CYLINDRICAL_SURFACE('',#47195,0.006);
#42134=CYLINDRICAL_SURFACE('',#47203,0.006);
#42135=CYLINDRICAL_SURFACE('',#47212,0.006);
#42136=CYLINDRICAL_SURFACE('',#47221,0.0067235209289897);
#42137=CYLINDRICAL_SURFACE('',#47224,0.0115242502781104);
#42138=CYLINDRICAL_SURFACE('',#47230,0.006);
#42139=CYLINDRICAL_SURFACE('',#47238,0.0120161531661046);
#42140=CYLINDRICAL_SURFACE('',#47241,0.006);
#42141=CYLINDRICAL_SURFACE('',#47250,0.006);
#42142=CYLINDRICAL_SURFACE('',#47256,0.006);
#42143=CYLINDRICAL_SURFACE('',#47264,0.006);
#42144=CYLINDRICAL_SURFACE('',#47273,0.006);
#42145=CYLINDRICAL_SURFACE('',#47282,0.00672352092902962);
#42146=CYLINDRICAL_SURFACE('',#47285,0.0115242502780876);
#42147=CYLINDRICAL_SURFACE('',#47291,0.006);
#42148=CYLINDRICAL_SURFACE('',#47299,0.0120161531660918);
#42149=CYLINDRICAL_SURFACE('',#47302,0.006);
#42150=CYLINDRICAL_SURFACE('',#47311,0.006);
#42151=CYLINDRICAL_SURFACE('',#47317,0.006);
#42152=CYLINDRICAL_SURFACE('',#47325,0.006);
#42153=CYLINDRICAL_SURFACE('',#47334,0.006);
#42154=CYLINDRICAL_SURFACE('',#47343,0.00672352092909496);
#42155=CYLINDRICAL_SURFACE('',#47346,0.0115242502781071);
#42156=CYLINDRICAL_SURFACE('',#47352,0.006);
#42157=CYLINDRICAL_SURFACE('',#47360,0.0120161531660884);
#42158=CYLINDRICAL_SURFACE('',#47363,0.006);
#42159=CYLINDRICAL_SURFACE('',#47372,0.006);
#42160=CYLINDRICAL_SURFACE('',#47378,0.006);
#42161=CYLINDRICAL_SURFACE('',#47386,0.006);
#42162=CYLINDRICAL_SURFACE('',#47395,0.006);
#42163=CYLINDRICAL_SURFACE('',#47404,0.00672352092911924);
#42164=CYLINDRICAL_SURFACE('',#47407,0.0115242502781167);
#42165=CYLINDRICAL_SURFACE('',#47413,0.006);
#42166=CYLINDRICAL_SURFACE('',#47421,0.0120161531660803);
#42167=CYLINDRICAL_SURFACE('',#47424,0.006);
#42168=CYLINDRICAL_SURFACE('',#47433,0.006);
#42169=CYLINDRICAL_SURFACE('',#47439,0.006);
#42170=CYLINDRICAL_SURFACE('',#47447,0.006);
#42171=CYLINDRICAL_SURFACE('',#47456,0.006);
#42172=CYLINDRICAL_SURFACE('',#47465,0.00672352092921552);
#42173=CYLINDRICAL_SURFACE('',#47468,0.0115242502781272);
#42174=CYLINDRICAL_SURFACE('',#47474,0.006);
#42175=CYLINDRICAL_SURFACE('',#47482,0.0120161531660835);
#42176=CYLINDRICAL_SURFACE('',#47485,0.006);
#42177=CYLINDRICAL_SURFACE('',#47494,0.006);
#42178=CYLINDRICAL_SURFACE('',#47500,0.006);
#42179=CYLINDRICAL_SURFACE('',#47508,0.006);
#42180=CYLINDRICAL_SURFACE('',#47517,0.006);
#42181=CYLINDRICAL_SURFACE('',#47526,0.00672352092925948);
#42182=CYLINDRICAL_SURFACE('',#47529,0.0115242502781359);
#42183=CYLINDRICAL_SURFACE('',#47535,0.006);
#42184=CYLINDRICAL_SURFACE('',#47543,0.0120161531660829);
#42185=CYLINDRICAL_SURFACE('',#47546,0.006);
#42186=CYLINDRICAL_SURFACE('',#47555,0.006);
#42187=CYLINDRICAL_SURFACE('',#47561,0.006);
#42188=CYLINDRICAL_SURFACE('',#47569,0.006);
#42189=CYLINDRICAL_SURFACE('',#47578,0.006);
#42190=CYLINDRICAL_SURFACE('',#47587,0.00672352092931105);
#42191=CYLINDRICAL_SURFACE('',#47590,0.0115242502781424);
#42192=CYLINDRICAL_SURFACE('',#47596,0.006);
#42193=CYLINDRICAL_SURFACE('',#47604,0.0120161531662401);
#42194=CYLINDRICAL_SURFACE('',#47607,0.006);
#42195=CYLINDRICAL_SURFACE('',#47616,0.006);
#42196=CYLINDRICAL_SURFACE('',#47622,0.006);
#42197=CYLINDRICAL_SURFACE('',#47630,0.006);
#42198=CYLINDRICAL_SURFACE('',#47639,0.006);
#42199=CYLINDRICAL_SURFACE('',#47648,0.00672352092933407);
#42200=CYLINDRICAL_SURFACE('',#47651,0.0115242502781404);
#42201=CYLINDRICAL_SURFACE('',#47657,0.006);
#42202=CYLINDRICAL_SURFACE('',#47665,0.0120161531662008);
#42203=CYLINDRICAL_SURFACE('',#47668,0.006);
#42204=CYLINDRICAL_SURFACE('',#47677,0.006);
#42205=CYLINDRICAL_SURFACE('',#47683,0.006);
#42206=CYLINDRICAL_SURFACE('',#47691,0.006);
#42207=CYLINDRICAL_SURFACE('',#47700,0.006);
#42208=CYLINDRICAL_SURFACE('',#47709,0.00672352092934602);
#42209=CYLINDRICAL_SURFACE('',#47712,0.0115242502781491);
#42210=CYLINDRICAL_SURFACE('',#47718,0.006);
#42211=CYLINDRICAL_SURFACE('',#47726,0.0120161531661581);
#42212=CYLINDRICAL_SURFACE('',#47729,0.006);
#42213=CYLINDRICAL_SURFACE('',#47738,0.006);
#42214=CYLINDRICAL_SURFACE('',#47744,0.006);
#42215=CYLINDRICAL_SURFACE('',#47752,0.006);
#42216=CYLINDRICAL_SURFACE('',#47761,0.006);
#42217=CYLINDRICAL_SURFACE('',#47770,0.00672352092933986);
#42218=CYLINDRICAL_SURFACE('',#47773,0.0115242502781903);
#42219=CYLINDRICAL_SURFACE('',#47779,0.006);
#42220=CYLINDRICAL_SURFACE('',#47787,0.0120161531661162);
#42221=CYLINDRICAL_SURFACE('',#47790,0.006);
#42222=CYLINDRICAL_SURFACE('',#47799,0.006);
#42223=CYLINDRICAL_SURFACE('',#47805,0.006);
#42224=CYLINDRICAL_SURFACE('',#47813,0.006);
#42225=CYLINDRICAL_SURFACE('',#47822,0.006);
#42226=CYLINDRICAL_SURFACE('',#47831,0.00672352092930669);
#42227=CYLINDRICAL_SURFACE('',#47834,0.0115242502778983);
#42228=CYLINDRICAL_SURFACE('',#47840,0.006);
#42229=CYLINDRICAL_SURFACE('',#47848,0.0120161531661211);
#42230=CYLINDRICAL_SURFACE('',#47851,0.006);
#42231=CYLINDRICAL_SURFACE('',#47860,0.006);
#42232=CYLINDRICAL_SURFACE('',#47866,0.006);
#42233=CYLINDRICAL_SURFACE('',#47874,0.006);
#42234=CYLINDRICAL_SURFACE('',#47883,0.006);
#42235=CYLINDRICAL_SURFACE('',#47892,0.00672352092933276);
#42236=CYLINDRICAL_SURFACE('',#47895,0.0115242502779026);
#42237=CYLINDRICAL_SURFACE('',#47901,0.006);
#42238=CYLINDRICAL_SURFACE('',#47909,0.0120161531661695);
#42239=CYLINDRICAL_SURFACE('',#47912,0.006);
#42240=CYLINDRICAL_SURFACE('',#47921,0.006);
#42241=CYLINDRICAL_SURFACE('',#47927,0.006);
#42242=CYLINDRICAL_SURFACE('',#47935,0.006);
#42243=CYLINDRICAL_SURFACE('',#47944,0.006);
#42244=CYLINDRICAL_SURFACE('',#47953,0.00672352092937054);
#42245=CYLINDRICAL_SURFACE('',#47956,0.0115242502779253);
#42246=CYLINDRICAL_SURFACE('',#47962,0.006);
#42247=CYLINDRICAL_SURFACE('',#47970,0.0120161531662158);
#42248=CYLINDRICAL_SURFACE('',#47973,0.006);
#42249=CYLINDRICAL_SURFACE('',#47982,0.006);
#42250=CYLINDRICAL_SURFACE('',#47988,0.006);
#42251=CYLINDRICAL_SURFACE('',#47996,0.006);
#42252=CYLINDRICAL_SURFACE('',#48005,0.006);
#42253=CYLINDRICAL_SURFACE('',#48014,0.00672352092931684);
#42254=CYLINDRICAL_SURFACE('',#48017,0.0115242502779055);
#42255=CYLINDRICAL_SURFACE('',#48023,0.006);
#42256=CYLINDRICAL_SURFACE('',#48031,0.0120161531662664);
#42257=CYLINDRICAL_SURFACE('',#48034,0.006);
#42258=CYLINDRICAL_SURFACE('',#48043,0.006);
#42259=CYLINDRICAL_SURFACE('',#48049,0.006);
#42260=CYLINDRICAL_SURFACE('',#48057,0.006);
#42261=CYLINDRICAL_SURFACE('',#48066,0.006);
#42262=CYLINDRICAL_SURFACE('',#48075,0.00672352092935101);
#42263=CYLINDRICAL_SURFACE('',#48078,0.0115242502778479);
#42264=CYLINDRICAL_SURFACE('',#48084,0.006);
#42265=CYLINDRICAL_SURFACE('',#48092,0.0120161531662955);
#42266=CYLINDRICAL_SURFACE('',#48095,0.006);
#42267=CYLINDRICAL_SURFACE('',#48104,0.006);
#42268=CYLINDRICAL_SURFACE('',#48110,0.006);
#42269=CYLINDRICAL_SURFACE('',#48118,0.006);
#42270=CYLINDRICAL_SURFACE('',#48127,0.006);
#42271=CYLINDRICAL_SURFACE('',#48136,0.0067235209293286);
#42272=CYLINDRICAL_SURFACE('',#48139,0.0115242502777874);
#42273=CYLINDRICAL_SURFACE('',#48145,0.006);
#42274=CYLINDRICAL_SURFACE('',#48153,0.0120161531663449);
#42275=CYLINDRICAL_SURFACE('',#48156,0.006);
#42276=CYLINDRICAL_SURFACE('',#48165,0.006);
#42277=CYLINDRICAL_SURFACE('',#48171,0.006);
#42278=CYLINDRICAL_SURFACE('',#48179,0.006);
#42279=CYLINDRICAL_SURFACE('',#48188,0.006);
#42280=CYLINDRICAL_SURFACE('',#48197,0.00672352092931084);
#42281=CYLINDRICAL_SURFACE('',#48200,0.0115242502777255);
#42282=CYLINDRICAL_SURFACE('',#48206,0.006);
#42283=CYLINDRICAL_SURFACE('',#48214,0.0120161531663728);
#42284=CYLINDRICAL_SURFACE('',#48217,0.006);
#42285=CYLINDRICAL_SURFACE('',#48226,0.006);
#42286=CYLINDRICAL_SURFACE('',#48232,0.006);
#42287=CYLINDRICAL_SURFACE('',#48240,0.006);
#42288=CYLINDRICAL_SURFACE('',#48249,0.006);
#42289=CYLINDRICAL_SURFACE('',#48258,0.00672352092931385);
#42290=CYLINDRICAL_SURFACE('',#48261,0.0115242502777398);
#42291=CYLINDRICAL_SURFACE('',#48267,0.006);
#42292=CYLINDRICAL_SURFACE('',#48275,0.0120161531664183);
#42293=CYLINDRICAL_SURFACE('',#48278,0.006);
#42294=CYLINDRICAL_SURFACE('',#48287,0.006);
#42295=CYLINDRICAL_SURFACE('',#48293,0.006);
#42296=CYLINDRICAL_SURFACE('',#48301,0.006);
#42297=CYLINDRICAL_SURFACE('',#48310,0.006);
#42298=CYLINDRICAL_SURFACE('',#48319,0.00672352092933332);
#42299=CYLINDRICAL_SURFACE('',#48322,0.0115242502778913);
#42300=CYLINDRICAL_SURFACE('',#48328,0.006);
#42301=CYLINDRICAL_SURFACE('',#48336,0.0120161531664379);
#42302=CYLINDRICAL_SURFACE('',#48339,0.006);
#42303=CYLINDRICAL_SURFACE('',#48348,0.006);
#42304=CYLINDRICAL_SURFACE('',#48354,0.006);
#42305=CYLINDRICAL_SURFACE('',#48362,0.006);
#42306=CYLINDRICAL_SURFACE('',#48371,0.006);
#42307=CYLINDRICAL_SURFACE('',#48380,0.00672352092934512);
#42308=CYLINDRICAL_SURFACE('',#48383,0.0115242502779201);
#42309=CYLINDRICAL_SURFACE('',#48389,0.006);
#42310=CYLINDRICAL_SURFACE('',#48397,0.0120161531664445);
#42311=CYLINDRICAL_SURFACE('',#48400,0.006);
#42312=CYLINDRICAL_SURFACE('',#48409,0.006);
#42313=CYLINDRICAL_SURFACE('',#48415,0.006);
#42314=CYLINDRICAL_SURFACE('',#48423,0.006);
#42315=CYLINDRICAL_SURFACE('',#48432,0.006);
#42316=CYLINDRICAL_SURFACE('',#48441,0.00672352092933164);
#42317=CYLINDRICAL_SURFACE('',#48444,0.0115242502779111);
#42318=CYLINDRICAL_SURFACE('',#48450,0.006);
#42319=CYLINDRICAL_SURFACE('',#48458,0.0120161531664562);
#42320=CYLINDRICAL_SURFACE('',#48461,0.006);
#42321=CYLINDRICAL_SURFACE('',#48470,0.006);
#42322=CYLINDRICAL_SURFACE('',#48476,0.006);
#42323=CYLINDRICAL_SURFACE('',#48484,0.006);
#42324=CYLINDRICAL_SURFACE('',#48493,0.006);
#42325=CYLINDRICAL_SURFACE('',#48502,0.00672352092931991);
#42326=CYLINDRICAL_SURFACE('',#48505,0.0115242502778819);
#42327=CYLINDRICAL_SURFACE('',#48511,0.006);
#42328=CYLINDRICAL_SURFACE('',#48519,0.0120161531664664);
#42329=CYLINDRICAL_SURFACE('',#48522,0.006);
#42330=CYLINDRICAL_SURFACE('',#48531,0.006);
#42331=CYLINDRICAL_SURFACE('',#48537,0.006);
#42332=CYLINDRICAL_SURFACE('',#48545,0.006);
#42333=CYLINDRICAL_SURFACE('',#48554,0.006);
#42334=CYLINDRICAL_SURFACE('',#48563,0.00672352092931163);
#42335=CYLINDRICAL_SURFACE('',#48566,0.0115242502779297);
#42336=CYLINDRICAL_SURFACE('',#48572,0.006);
#42337=CYLINDRICAL_SURFACE('',#48580,0.0120161531664594);
#42338=CYLINDRICAL_SURFACE('',#48583,0.006);
#42339=CYLINDRICAL_SURFACE('',#48592,0.006);
#42340=CYLINDRICAL_SURFACE('',#48598,0.006);
#42341=CYLINDRICAL_SURFACE('',#48606,0.006);
#42342=CYLINDRICAL_SURFACE('',#48615,0.006);
#42343=CYLINDRICAL_SURFACE('',#48624,0.00672352092935956);
#42344=CYLINDRICAL_SURFACE('',#48627,0.0115242502779183);
#42345=CYLINDRICAL_SURFACE('',#48633,0.006);
#42346=CYLINDRICAL_SURFACE('',#48641,0.0120161531664567);
#42347=CYLINDRICAL_SURFACE('',#48644,0.006);
#42348=CYLINDRICAL_SURFACE('',#48653,0.006);
#42349=CYLINDRICAL_SURFACE('',#48659,0.006);
#42350=CYLINDRICAL_SURFACE('',#48667,0.006);
#42351=CYLINDRICAL_SURFACE('',#48676,0.006);
#42352=CYLINDRICAL_SURFACE('',#48685,0.0067235209293039);
#42353=CYLINDRICAL_SURFACE('',#48688,0.0115242502778913);
#42354=CYLINDRICAL_SURFACE('',#48694,0.006);
#42355=CYLINDRICAL_SURFACE('',#48702,0.0120161531664457);
#42356=CYLINDRICAL_SURFACE('',#48705,0.006);
#42357=CYLINDRICAL_SURFACE('',#48714,0.006);
#42358=CYLINDRICAL_SURFACE('',#48720,0.006);
#42359=CYLINDRICAL_SURFACE('',#48728,0.006);
#42360=CYLINDRICAL_SURFACE('',#48737,0.006);
#42361=CYLINDRICAL_SURFACE('',#48746,0.00672352092926038);
#42362=CYLINDRICAL_SURFACE('',#48749,0.0115242502779262);
#42363=CYLINDRICAL_SURFACE('',#48751,0.006);
#42364=CYLINDRICAL_SURFACE('',#48763,0.0120161531664297);
#42365=CYLINDRICAL_SURFACE('',#48766,0.006);
#42366=CYLINDRICAL_SURFACE('',#48775,0.006);
#42367=CYLINDRICAL_SURFACE('',#48781,0.006);
#42368=CYLINDRICAL_SURFACE('',#48789,0.006);
#42369=CYLINDRICAL_SURFACE('',#48798,0.006);
#42370=CYLINDRICAL_SURFACE('',#48807,0.00672352092922533);
#42371=CYLINDRICAL_SURFACE('',#48810,0.0115242502779126);
#42372=CYLINDRICAL_SURFACE('',#48812,0.006);
#42373=CYLINDRICAL_SURFACE('',#48817,0.006);
#42374=CYLINDRICAL_SURFACE('',#48829,0.0120161531664118);
#42375=CYLINDRICAL_SURFACE('',#48836,0.006);
#42376=CYLINDRICAL_SURFACE('',#48842,0.006);
#42377=CYLINDRICAL_SURFACE('',#48850,0.006);
#42378=CYLINDRICAL_SURFACE('',#48859,0.006);
#42379=CYLINDRICAL_SURFACE('',#48868,0.00672352092915246);
#42380=CYLINDRICAL_SURFACE('',#48871,0.0115242502779174);
#42381=CYLINDRICAL_SURFACE('',#48873,0.006);
#42382=CYLINDRICAL_SURFACE('',#48878,0.006);
#42383=CYLINDRICAL_SURFACE('',#48883,0.006);
#42384=CYLINDRICAL_SURFACE('',#48892,0.0120161531663761);
#42385=CYLINDRICAL_SURFACE('',#48903,0.006);
#42386=CYLINDRICAL_SURFACE('',#48911,0.006);
#42387=CYLINDRICAL_SURFACE('',#48920,0.006);
#42388=CYLINDRICAL_SURFACE('',#48929,0.0067235209291287);
#42389=CYLINDRICAL_SURFACE('',#48932,0.0115242502779053);
#42390=CYLINDRICAL_SURFACE('',#48934,0.006);
#42391=CYLINDRICAL_SURFACE('',#48939,0.006);
#42392=CYLINDRICAL_SURFACE('',#48944,0.006);
#42393=CYLINDRICAL_SURFACE('',#48947,0.006);
#42394=CYLINDRICAL_SURFACE('',#48970,0.0120161531663417);
#42395=CYLINDRICAL_SURFACE('',#48972,0.006);
#42396=CYLINDRICAL_SURFACE('',#48981,0.006);
#42397=CYLINDRICAL_SURFACE('',#48990,0.00672352092909558);
#42398=CYLINDRICAL_SURFACE('',#48993,0.0115242502776438);
#42399=CYLINDRICAL_SURFACE('',#48995,0.006);
#42400=CYLINDRICAL_SURFACE('',#49000,0.006);
#42401=CYLINDRICAL_SURFACE('',#49005,0.006);
#42402=CYLINDRICAL_SURFACE('',#49010,0.006);
#42403=CYLINDRICAL_SURFACE('',#49015,0.006);
#42404=CYLINDRICAL_SURFACE('',#49036,0.0120161531663077);
#42405=CYLINDRICAL_SURFACE('',#49042,0.006);
#42406=CYLINDRICAL_SURFACE('',#49051,0.00672352092901901);
#42407=CYLINDRICAL_SURFACE('',#49054,0.011524250277674);
#42408=CYLINDRICAL_SURFACE('',#49056,0.006);
#42409=CYLINDRICAL_SURFACE('',#49061,0.006);
#42410=CYLINDRICAL_SURFACE('',#49064,0.006);
#42411=CYLINDRICAL_SURFACE('',#49069,0.006);
#42412=CYLINDRICAL_SURFACE('',#49074,0.006);
#42413=CYLINDRICAL_SURFACE('',#49079,0.006);
#42414=CYLINDRICAL_SURFACE('',#49104,0.012016153166264);
#42415=CYLINDRICAL_SURFACE('',#49112,0.00672352092891286);
#42416=CYLINDRICAL_SURFACE('',#49115,0.0115242502777387);
#42417=CYLINDRICAL_SURFACE('',#49117,0.00672352092892855);
#42418=CYLINDRICAL_SURFACE('',#49120,0.011524250277794);
#42419=CYLINDRICAL_SURFACE('',#49122,0.0120161531662885);
#42420=CYLINDRICAL_SURFACE('',#49136,0.00830951479144525);
#42421=CYLINDRICAL_SURFACE('',#49137,0.00489777760244533);
#42422=CYLINDRICAL_SURFACE('',#49142,0.00830951479147278);
#42423=CYLINDRICAL_SURFACE('',#49143,0.0048977776024695);
#42424=CYLINDRICAL_SURFACE('',#49157,0.00830951479145815);
#42425=CYLINDRICAL_SURFACE('',#49158,0.00489777760247165);
#42426=CYLINDRICAL_SURFACE('',#49172,0.00830951479142899);
#42427=CYLINDRICAL_SURFACE('',#49173,0.00489777760244579);
#42428=CYLINDRICAL_SURFACE('',#49187,0.00830951479141785);
#42429=CYLINDRICAL_SURFACE('',#49188,0.00489777760247916);
#42430=CYLINDRICAL_SURFACE('',#49202,0.00830951479144501);
#42431=CYLINDRICAL_SURFACE('',#49203,0.00489777760244294);
#42432=CYLINDRICAL_SURFACE('',#49217,0.00830951479145066);
#42433=CYLINDRICAL_SURFACE('',#49218,0.00489777760242687);
#42434=CYLINDRICAL_SURFACE('',#49232,0.00830951479140252);
#42435=CYLINDRICAL_SURFACE('',#49233,0.00489777760240844);
#42436=CYLINDRICAL_SURFACE('',#49247,0.00830951479142787);
#42437=CYLINDRICAL_SURFACE('',#49248,0.00489777760239372);
#42438=CYLINDRICAL_SURFACE('',#49262,0.00830951479138556);
#42439=CYLINDRICAL_SURFACE('',#49263,0.00489777760235847);
#42440=CYLINDRICAL_SURFACE('',#49277,0.00830951479141585);
#42441=CYLINDRICAL_SURFACE('',#49278,0.00489777760236036);
#42442=CYLINDRICAL_SURFACE('',#49292,0.00830951479142129);
#42443=CYLINDRICAL_SURFACE('',#49293,0.00489777760234243);
#42444=CYLINDRICAL_SURFACE('',#49307,0.00830951479143295);
#42445=CYLINDRICAL_SURFACE('',#49308,0.00489777760232894);
#42446=CYLINDRICAL_SURFACE('',#49322,0.00830951479143844);
#42447=CYLINDRICAL_SURFACE('',#49323,0.00489777760230745);
#42448=CYLINDRICAL_SURFACE('',#49337,0.00830951479141942);
#42449=CYLINDRICAL_SURFACE('',#49338,0.00489777760230435);
#42450=CYLINDRICAL_SURFACE('',#49352,0.0083095147914072);
#42451=CYLINDRICAL_SURFACE('',#49353,0.00489777760230926);
#42452=CYLINDRICAL_SURFACE('',#49367,0.00830951479140723);
#42453=CYLINDRICAL_SURFACE('',#49368,0.00489777760229998);
#42454=CYLINDRICAL_SURFACE('',#49382,0.00830951479140655);
#42455=CYLINDRICAL_SURFACE('',#49383,0.00489777760231482);
#42456=CYLINDRICAL_SURFACE('',#49397,0.00830951479140061);
#42457=CYLINDRICAL_SURFACE('',#49398,0.00489777760230995);
#42458=CYLINDRICAL_SURFACE('',#49412,0.00830951479141865);
#42459=CYLINDRICAL_SURFACE('',#49413,0.00489777760231243);
#42460=CYLINDRICAL_SURFACE('',#49427,0.00830951479139597);
#42461=CYLINDRICAL_SURFACE('',#49428,0.00489777760228124);
#42462=CYLINDRICAL_SURFACE('',#49442,0.00830951479139311);
#42463=CYLINDRICAL_SURFACE('',#49443,0.0048977776023241);
#42464=CYLINDRICAL_SURFACE('',#49457,0.00830951479138788);
#42465=CYLINDRICAL_SURFACE('',#49458,0.00489777760231598);
#42466=CYLINDRICAL_SURFACE('',#49472,0.00830951479139345);
#42467=CYLINDRICAL_SURFACE('',#49473,0.00489777760238264);
#42468=CYLINDRICAL_SURFACE('',#49487,0.00830951479136789);
#42469=CYLINDRICAL_SURFACE('',#49488,0.00489777760236428);
#42470=CYLINDRICAL_SURFACE('',#49502,0.00830951479137509);
#42471=CYLINDRICAL_SURFACE('',#49503,0.00489777760239822);
#42472=CYLINDRICAL_SURFACE('',#49517,0.00830951479138404);
#42473=CYLINDRICAL_SURFACE('',#49518,0.004897777602424);
#42474=CYLINDRICAL_SURFACE('',#49532,0.00830951479139002);
#42475=CYLINDRICAL_SURFACE('',#49533,0.00489777760244448);
#42476=CYLINDRICAL_SURFACE('',#49547,0.0083095147913546);
#42477=CYLINDRICAL_SURFACE('',#49548,0.00489777760246637);
#42478=CYLINDRICAL_SURFACE('',#49562,0.00830951479138939);
#42479=CYLINDRICAL_SURFACE('',#49563,0.00489777760247895);
#42480=CYLINDRICAL_SURFACE('',#49577,0.00830951479137315);
#42481=CYLINDRICAL_SURFACE('',#49578,0.00489777760247943);
#42482=CYLINDRICAL_SURFACE('',#49592,0.00830951479133772);
#42483=CYLINDRICAL_SURFACE('',#49593,0.00489777760248803);
#42484=CYLINDRICAL_SURFACE('',#49607,0.00830951479137358);
#42485=CYLINDRICAL_SURFACE('',#49608,0.00489777760245939);
#42486=CYLINDRICAL_SURFACE('',#49622,0.00830951479136423);
#42487=CYLINDRICAL_SURFACE('',#49623,0.00489777760247564);
#42488=CYLINDRICAL_SURFACE('',#49637,0.00830951479136581);
#42489=CYLINDRICAL_SURFACE('',#49638,0.00489777760248512);
#42490=CYLINDRICAL_SURFACE('',#49652,0.00830951479137988);
#42491=CYLINDRICAL_SURFACE('',#49653,0.00489777760253342);
#42492=CYLINDRICAL_SURFACE('',#49667,0.00830951479136722);
#42493=CYLINDRICAL_SURFACE('',#49668,0.00489777760257392);
#42494=CYLINDRICAL_SURFACE('',#49682,0.00830951479136156);
#42495=CYLINDRICAL_SURFACE('',#49683,0.00489777760253943);
#42496=CYLINDRICAL_SURFACE('',#49697,0.00830951479135765);
#42497=CYLINDRICAL_SURFACE('',#49698,0.00489777760256031);
#42498=CYLINDRICAL_SURFACE('',#49712,0.00830951479137079);
#42499=CYLINDRICAL_SURFACE('',#49713,0.0048977776025707);
#42500=CYLINDRICAL_SURFACE('',#49727,0.00830951479137468);
#42501=CYLINDRICAL_SURFACE('',#49728,0.00489777760256102);
#42502=CYLINDRICAL_SURFACE('',#49742,0.00830951479138694);
#42503=CYLINDRICAL_SURFACE('',#49743,0.00489777760258809);
#42504=CYLINDRICAL_SURFACE('',#49757,0.00830951479138659);
#42505=CYLINDRICAL_SURFACE('',#49758,0.00489777760258593);
#42506=CYLINDRICAL_SURFACE('',#49774,0.00830951479140578);
#42507=CYLINDRICAL_SURFACE('',#49775,0.00489777760257164);
#42508=CYLINDRICAL_SURFACE('',#49787,0.00830951479141365);
#42509=CYLINDRICAL_SURFACE('',#49788,0.00489777760255856);
#42510=CYLINDRICAL_SURFACE('',#49802,0.0083095147914008);
#42511=CYLINDRICAL_SURFACE('',#49803,0.00489777760254268);
#42512=CYLINDRICAL_SURFACE('',#49817,0.0083095147914313);
#42513=CYLINDRICAL_SURFACE('',#49818,0.00489777760254623);
#42514=CYLINDRICAL_SURFACE('',#49832,0.00830951479143087);
#42515=CYLINDRICAL_SURFACE('',#49833,0.00489777760250727);
#42516=CYLINDRICAL_SURFACE('',#49847,0.00830951479143416);
#42517=CYLINDRICAL_SURFACE('',#49848,0.00489777760251401);
#42518=CYLINDRICAL_SURFACE('',#49862,0.0083095147914544);
#42519=CYLINDRICAL_SURFACE('',#49863,0.00489777760247736);
#42520=CYLINDRICAL_SURFACE('',#49878,0.002);
#42521=CYLINDRICAL_SURFACE('',#49881,0.00525);
#42522=CYLINDRICAL_SURFACE('',#49884,0.0043952301441823);
#42523=CYLINDRICAL_SURFACE('',#49891,0.002);
#42524=CYLINDRICAL_SURFACE('',#49894,0.00525);
#42525=CYLINDRICAL_SURFACE('',#49900,0.004);
#42526=CYLINDRICAL_SURFACE('',#49903,0.005825);
#42527=CYLINDRICAL_SURFACE('',#49906,0.010875);
#42528=CYLINDRICAL_SURFACE('',#49909,0.010875);
#42529=CYLINDRICAL_SURFACE('',#49912,0.0135);
#42530=CYLINDRICAL_SURFACE('',#49915,0.0135);
#42531=CYLINDRICAL_SURFACE('',#49918,0.0135);
#42532=CYLINDRICAL_SURFACE('',#49921,0.0135);
#42533=CYLINDRICAL_SURFACE('',#49924,0.0135);
#42534=CYLINDRICAL_SURFACE('',#49927,0.0135);
#42535=CYLINDRICAL_SURFACE('',#49930,0.0135);
#42536=CYLINDRICAL_SURFACE('',#49933,0.0135);
#42537=CYLINDRICAL_SURFACE('',#49936,0.0135);
#42538=CYLINDRICAL_SURFACE('',#49939,0.0135);
#42539=CYLINDRICAL_SURFACE('',#49942,0.0135);
#42540=CYLINDRICAL_SURFACE('',#49945,0.0135);
#42541=CYLINDRICAL_SURFACE('',#49948,0.0135);
#42542=CYLINDRICAL_SURFACE('',#49951,0.0135);
#42543=CYLINDRICAL_SURFACE('',#49954,0.0135);
#42544=CYLINDRICAL_SURFACE('',#49957,0.0135);
#42545=CYLINDRICAL_SURFACE('',#49960,0.0135);
#42546=CYLINDRICAL_SURFACE('',#49963,0.0135);
#42547=CYLINDRICAL_SURFACE('',#49966,0.0135);
#42548=CYLINDRICAL_SURFACE('',#49969,0.0135);
#42549=CYLINDRICAL_SURFACE('',#49972,0.0135);
#42550=CYLINDRICAL_SURFACE('',#49975,0.0135);
#42551=CYLINDRICAL_SURFACE('',#49978,0.0135);
#42552=CYLINDRICAL_SURFACE('',#49981,0.0135);
#42553=CYLINDRICAL_SURFACE('',#49984,0.0135);
#42554=CYLINDRICAL_SURFACE('',#49987,0.0135);
#42555=CYLINDRICAL_SURFACE('',#49990,0.0135);
#42556=CYLINDRICAL_SURFACE('',#49993,0.0135);
#42557=CYLINDRICAL_SURFACE('',#49996,0.0135);
#42558=CYLINDRICAL_SURFACE('',#49999,0.0135);
#42559=CYLINDRICAL_SURFACE('',#50002,0.0135);
#42560=CYLINDRICAL_SURFACE('',#50005,0.0135);
#42561=CYLINDRICAL_SURFACE('',#50008,0.0135);
#42562=CYLINDRICAL_SURFACE('',#50011,0.0135);
#42563=CYLINDRICAL_SURFACE('',#50014,0.0135);
#42564=CYLINDRICAL_SURFACE('',#50017,0.0135);
#42565=CYLINDRICAL_SURFACE('',#50020,0.0135);
#42566=CYLINDRICAL_SURFACE('',#50023,0.0135);
#42567=CYLINDRICAL_SURFACE('',#50026,0.0135);
#42568=CYLINDRICAL_SURFACE('',#50029,0.0135);
#42569=CYLINDRICAL_SURFACE('',#50032,0.0135);
#42570=CYLINDRICAL_SURFACE('',#50035,0.0135);
#42571=CYLINDRICAL_SURFACE('',#50038,0.0135);
#42572=CYLINDRICAL_SURFACE('',#50041,0.0135);
#42573=CYLINDRICAL_SURFACE('',#50044,0.0135);
#42574=CYLINDRICAL_SURFACE('',#50047,0.0135);
#42575=CYLINDRICAL_SURFACE('',#50050,0.0135);
#42576=CYLINDRICAL_SURFACE('',#50053,0.0135);
#42577=CYLINDRICAL_SURFACE('',#50056,0.0135);
#42578=CYLINDRICAL_SURFACE('',#50059,0.0135);
#42579=CYLINDRICAL_SURFACE('',#50062,0.0135);
#42580=CYLINDRICAL_SURFACE('',#50174,0.008);
#42581=CYLINDRICAL_SURFACE('',#50181,0.002125);
#42582=CYLINDRICAL_SURFACE('',#50184,0.003);
#42583=CYLINDRICAL_SURFACE('',#50187,0.005);
#42584=CYLINDRICAL_SURFACE('',#50190,0.0025);
#42585=CYLINDRICAL_SURFACE('',#50199,0.01125);
#42586=CYLINDRICAL_SURFACE('',#50201,0.0015);
#42587=CYLINDRICAL_SURFACE('',#50204,0.0036);
#42588=CYLINDRICAL_SURFACE('',#50207,0.0037);
#42589=CYLINDRICAL_SURFACE('',#50211,0.002825);
#42590=CYLINDRICAL_SURFACE('',#50214,0.002825);
#42591=CYLINDRICAL_SURFACE('',#50217,0.002825);
#42592=CYLINDRICAL_SURFACE('',#50220,0.0016);
#42593=CYLINDRICAL_SURFACE('',#50223,0.0016);
#42594=CYLINDRICAL_SURFACE('',#50228,0.0016);
#42595=CYLINDRICAL_SURFACE('',#50231,0.0059);
#42596=CYLINDRICAL_SURFACE('',#50234,0.0135);
#42597=CYLINDRICAL_SURFACE('',#50240,0.014);
#42598=CYLINDRICAL_SURFACE('',#50258,0.0135);
#42599=CYLINDRICAL_SURFACE('',#50261,0.014);
#42600=CYLINDRICAL_SURFACE('',#50297,0.003);
#42601=CYLINDRICAL_SURFACE('',#50300,0.00725);
#42602=CYLINDRICAL_SURFACE('',#50303,0.004);
#42603=CYLINDRICAL_SURFACE('',#50306,0.014);
#42604=CYLINDRICAL_SURFACE('',#50312,0.0037);
#42605=CYLINDRICAL_SURFACE('',#50315,0.0037);
#42606=CYLINDRICAL_SURFACE('',#50320,0.005);
#42607=CYLINDRICAL_SURFACE('',#50322,0.00525);
#42608=CYLINDRICAL_SURFACE('',#50324,0.00650498845854181);
#42609=CYLINDRICAL_SURFACE('',#50327,0.0036);
#42610=CYLINDRICAL_SURFACE('',#50343,0.01565);
#42611=CYLINDRICAL_SURFACE('',#50347,0.01565);
#42612=CYLINDRICAL_SURFACE('',#50361,0.006);
#42613=ADVANCED_FACE('',(#3758),#41960,.F.);
#42614=ADVANCED_FACE('',(#3759),#41961,.T.);
#42615=ADVANCED_FACE('',(#3760,#3509),#3542,.T.);
#42616=ADVANCED_FACE('',(#3761,#3510),#3543,.F.);
#42617=ADVANCED_FACE('',(#3762),#2198,.T.);
#42618=ADVANCED_FACE('',(#3763),#3544,.T.);
#42619=ADVANCED_FACE('',(#3764),#3545,.T.);
#42620=ADVANCED_FACE('',(#3765),#1136,.T.);
#42621=ADVANCED_FACE('',(#3766),#41962,.T.);
#42622=ADVANCED_FACE('',(#3767),#3546,.F.);
#42623=ADVANCED_FACE('',(#3768),#3547,.T.);
#42624=ADVANCED_FACE('',(#3769),#41963,.T.);
#42625=ADVANCED_FACE('',(#3770),#3548,.F.);
#42626=ADVANCED_FACE('',(#3771),#3549,.T.);
#42627=ADVANCED_FACE('',(#3772),#41964,.F.);
#42628=ADVANCED_FACE('',(#3773),#41965,.F.);
#42629=ADVANCED_FACE('',(#3774),#41966,.T.);
#42630=ADVANCED_FACE('',(#3775,#3511),#3550,.F.);
#42631=ADVANCED_FACE('',(#3776),#41967,.F.);
#42632=ADVANCED_FACE('',(#3777),#3551,.F.);
#42633=ADVANCED_FACE('',(#3778),#3552,.F.);
#42634=ADVANCED_FACE('',(#3779,#3512),#3553,.F.);
#42635=ADVANCED_FACE('',(#3780),#3554,.F.);
#42636=ADVANCED_FACE('',(#3781),#3555,.T.);
#42637=ADVANCED_FACE('',(#3782),#3556,.T.);
#42638=ADVANCED_FACE('',(#3783),#3557,.F.);
#42639=ADVANCED_FACE('',(#3784),#3558,.F.);
#42640=ADVANCED_FACE('',(#3785),#41968,.F.);
#42641=ADVANCED_FACE('',(#3786),#3559,.F.);
#42642=ADVANCED_FACE('',(#3787),#3560,.F.);
#42643=ADVANCED_FACE('',(#3788),#3561,.T.);
#42644=ADVANCED_FACE('',(#3789),#3562,.F.);
#42645=ADVANCED_FACE('',(#3790),#3563,.F.);
#42646=ADVANCED_FACE('',(#3791),#3564,.F.);
#42647=ADVANCED_FACE('',(#3792),#3565,.T.);
#42648=ADVANCED_FACE('',(#3793),#41969,.T.);
#42649=ADVANCED_FACE('',(#3794),#881,.T.);
#42650=ADVANCED_FACE('',(#3795),#882,.T.);
#42651=ADVANCED_FACE('',(#3796),#2199,.T.);
#42652=ADVANCED_FACE('',(#3797),#2200,.T.);
#42653=ADVANCED_FACE('',(#3798),#101,.T.);
#42654=ADVANCED_FACE('',(#3799),#102,.T.);
#42655=ADVANCED_FACE('',(#3800),#2201,.T.);
#42656=ADVANCED_FACE('',(#3801),#2202,.T.);
#42657=ADVANCED_FACE('',(#3802),#41970,.T.);
#42658=ADVANCED_FACE('',(#3803),#2203,.T.);
#42659=ADVANCED_FACE('',(#3804),#41971,.T.);
#42660=ADVANCED_FACE('',(#3805),#41972,.T.);
#42661=ADVANCED_FACE('',(#3806),#41973,.T.);
#42662=ADVANCED_FACE('',(#3807),#103,.T.);
#42663=ADVANCED_FACE('',(#3808),#104,.T.);
#42664=ADVANCED_FACE('',(#3809),#2204,.T.);
#42665=ADVANCED_FACE('',(#3810),#2205,.T.);
#42666=ADVANCED_FACE('',(#3811),#105,.T.);
#42667=ADVANCED_FACE('',(#3812),#106,.T.);
#42668=ADVANCED_FACE('',(#3813),#41974,.T.);
#42669=ADVANCED_FACE('',(#3814),#41975,.T.);
#42670=ADVANCED_FACE('',(#3815),#107,.T.);
#42671=ADVANCED_FACE('',(#3816),#108,.T.);
#42672=ADVANCED_FACE('',(#3817),#2206,.T.);
#42673=ADVANCED_FACE('',(#3818),#2207,.T.);
#42674=ADVANCED_FACE('',(#3819),#109,.T.);
#42675=ADVANCED_FACE('',(#3820),#110,.T.);
#42676=ADVANCED_FACE('',(#3821),#41976,.T.);
#42677=ADVANCED_FACE('',(#3822),#41977,.T.);
#42678=ADVANCED_FACE('',(#3823),#111,.T.);
#42679=ADVANCED_FACE('',(#3824),#112,.T.);
#42680=ADVANCED_FACE('',(#3825),#2208,.T.);
#42681=ADVANCED_FACE('',(#3826),#2209,.T.);
#42682=ADVANCED_FACE('',(#3827),#2210,.T.);
#42683=ADVANCED_FACE('',(#3828),#113,.T.);
#42684=ADVANCED_FACE('',(#3829),#41978,.T.);
#42685=ADVANCED_FACE('',(#3830),#41979,.T.);
#42686=ADVANCED_FACE('',(#3831),#2211,.T.);
#42687=ADVANCED_FACE('',(#3832),#114,.T.);
#42688=ADVANCED_FACE('',(#3833),#2212,.T.);
#42689=ADVANCED_FACE('',(#3834),#2213,.T.);
#42690=ADVANCED_FACE('',(#3835),#2214,.T.);
#42691=ADVANCED_FACE('',(#3836),#2215,.T.);
#42692=ADVANCED_FACE('',(#3837),#41980,.T.);
#42693=ADVANCED_FACE('',(#3838),#41981,.T.);
#42694=ADVANCED_FACE('',(#3839),#115,.T.);
#42695=ADVANCED_FACE('',(#3840),#2216,.T.);
#42696=ADVANCED_FACE('',(#3841),#2217,.T.);
#42697=ADVANCED_FACE('',(#3842),#2218,.T.);
#42698=ADVANCED_FACE('',(#3843),#2219,.T.);
#42699=ADVANCED_FACE('',(#3844),#2220,.T.);
#42700=ADVANCED_FACE('',(#3845),#41982,.T.);
#42701=ADVANCED_FACE('',(#3846),#41983,.T.);
#42702=ADVANCED_FACE('',(#3847),#116,.T.);
#42703=ADVANCED_FACE('',(#3848),#41984,.T.);
#42704=ADVANCED_FACE('',(#3849),#2221,.T.);
#42705=ADVANCED_FACE('',(#3850),#2222,.T.);
#42706=ADVANCED_FACE('',(#3851),#2223,.T.);
#42707=ADVANCED_FACE('',(#3852),#2224,.T.);
#42708=ADVANCED_FACE('',(#3853),#41985,.T.);
#42709=ADVANCED_FACE('',(#3854),#117,.T.);
#42710=ADVANCED_FACE('',(#3855),#2225,.T.);
#42711=ADVANCED_FACE('',(#3856),#41986,.T.);
#42712=ADVANCED_FACE('',(#3857),#2226,.T.);
#42713=ADVANCED_FACE('',(#3858),#118,.T.);
#42714=ADVANCED_FACE('',(#3859),#119,.T.);
#42715=ADVANCED_FACE('',(#3860),#41987,.T.);
#42716=ADVANCED_FACE('',(#3861),#2227,.T.);
#42717=ADVANCED_FACE('',(#3862),#41988,.T.);
#42718=ADVANCED_FACE('',(#3863),#120,.T.);
#42719=ADVANCED_FACE('',(#3864),#2228,.T.);
#42720=ADVANCED_FACE('',(#3865),#121,.T.);
#42721=ADVANCED_FACE('',(#3866),#41989,.T.);
#42722=ADVANCED_FACE('',(#3867),#122,.T.);
#42723=ADVANCED_FACE('',(#3868),#2229,.T.);
#42724=ADVANCED_FACE('',(#3869),#123,.T.);
#42725=ADVANCED_FACE('',(#3870),#41990,.T.);
#42726=ADVANCED_FACE('',(#3871),#2230,.T.);
#42727=ADVANCED_FACE('',(#3872),#2231,.T.);
#42728=ADVANCED_FACE('',(#3873),#2232,.T.);
#42729=ADVANCED_FACE('',(#3874),#41991,.T.);
#42730=ADVANCED_FACE('',(#3875),#124,.T.);
#42731=ADVANCED_FACE('',(#3876),#2233,.T.);
#42732=ADVANCED_FACE('',(#3877),#2234,.T.);
#42733=ADVANCED_FACE('',(#3878),#41992,.T.);
#42734=ADVANCED_FACE('',(#3879),#41993,.T.);
#42735=ADVANCED_FACE('',(#3880),#2235,.T.);
#42736=ADVANCED_FACE('',(#3881),#2236,.T.);
#42737=ADVANCED_FACE('',(#3882),#41994,.T.);
#42738=ADVANCED_FACE('',(#3883),#125,.T.);
#42739=ADVANCED_FACE('',(#3884),#2237,.T.);
#42740=ADVANCED_FACE('',(#3885),#41995,.T.);
#42741=ADVANCED_FACE('',(#3886),#2238,.T.);
#42742=ADVANCED_FACE('',(#3887),#41996,.T.);
#42743=ADVANCED_FACE('',(#3888),#126,.T.);
#42744=ADVANCED_FACE('',(#3889),#2239,.T.);
#42745=ADVANCED_FACE('',(#3890),#127,.T.);
#42746=ADVANCED_FACE('',(#3891),#128,.T.);
#42747=ADVANCED_FACE('',(#3892),#129,.T.);
#42748=ADVANCED_FACE('',(#3893),#41997,.T.);
#42749=ADVANCED_FACE('',(#3894),#2240,.T.);
#42750=ADVANCED_FACE('',(#3895),#41998,.T.);
#42751=ADVANCED_FACE('',(#3896),#130,.T.);
#42752=ADVANCED_FACE('',(#3897),#2241,.T.);
#42753=ADVANCED_FACE('',(#3898),#131,.T.);
#42754=ADVANCED_FACE('',(#3899),#41999,.T.);
#42755=ADVANCED_FACE('',(#3900),#2242,.T.);
#42756=ADVANCED_FACE('',(#3901),#2243,.T.);
#42757=ADVANCED_FACE('',(#3902),#132,.T.);
#42758=ADVANCED_FACE('',(#3903),#42000,.T.);
#42759=ADVANCED_FACE('',(#3904),#133,.T.);
#42760=ADVANCED_FACE('',(#3905),#2244,.T.);
#42761=ADVANCED_FACE('',(#3906),#2245,.T.);
#42762=ADVANCED_FACE('',(#3907),#42001,.T.);
#42763=ADVANCED_FACE('',(#3908),#42002,.T.);
#42764=ADVANCED_FACE('',(#3909),#2246,.T.);
#42765=ADVANCED_FACE('',(#3910),#2247,.T.);
#42766=ADVANCED_FACE('',(#3911),#42003,.T.);
#42767=ADVANCED_FACE('',(#3912),#134,.T.);
#42768=ADVANCED_FACE('',(#3913),#2248,.T.);
#42769=ADVANCED_FACE('',(#3914),#42004,.T.);
#42770=ADVANCED_FACE('',(#3915),#2249,.T.);
#42771=ADVANCED_FACE('',(#3916),#42005,.T.);
#42772=ADVANCED_FACE('',(#3917),#135,.T.);
#42773=ADVANCED_FACE('',(#3918),#2250,.T.);
#42774=ADVANCED_FACE('',(#3919),#136,.T.);
#42775=ADVANCED_FACE('',(#3920),#42006,.T.);
#42776=ADVANCED_FACE('',(#3921),#137,.T.);
#42777=ADVANCED_FACE('',(#3922),#2251,.T.);
#42778=ADVANCED_FACE('',(#3923),#138,.T.);
#42779=ADVANCED_FACE('',(#3924),#139,.T.);
#42780=ADVANCED_FACE('',(#3925),#140,.T.);
#42781=ADVANCED_FACE('',(#3926),#42007,.T.);
#42782=ADVANCED_FACE('',(#3927),#2252,.T.);
#42783=ADVANCED_FACE('',(#3928),#42008,.T.);
#42784=ADVANCED_FACE('',(#3929),#2253,.T.);
#42785=ADVANCED_FACE('',(#3930),#2254,.T.);
#42786=ADVANCED_FACE('',(#3931),#141,.T.);
#42787=ADVANCED_FACE('',(#3932),#42009,.T.);
#42788=ADVANCED_FACE('',(#3933),#142,.T.);
#42789=ADVANCED_FACE('',(#3934),#2255,.T.);
#42790=ADVANCED_FACE('',(#3935),#143,.T.);
#42791=ADVANCED_FACE('',(#3936),#42010,.T.);
#42792=ADVANCED_FACE('',(#3937),#42011,.T.);
#42793=ADVANCED_FACE('',(#3938),#2256,.T.);
#42794=ADVANCED_FACE('',(#3939),#2257,.T.);
#42795=ADVANCED_FACE('',(#3940),#42012,.T.);
#42796=ADVANCED_FACE('',(#3941),#144,.T.);
#42797=ADVANCED_FACE('',(#3942),#2258,.T.);
#42798=ADVANCED_FACE('',(#3943),#42013,.T.);
#42799=ADVANCED_FACE('',(#3944),#2259,.T.);
#42800=ADVANCED_FACE('',(#3945),#42014,.T.);
#42801=ADVANCED_FACE('',(#3946),#145,.T.);
#42802=ADVANCED_FACE('',(#3947),#2260,.T.);
#42803=ADVANCED_FACE('',(#3948),#146,.T.);
#42804=ADVANCED_FACE('',(#3949),#42015,.T.);
#42805=ADVANCED_FACE('',(#3950),#147,.T.);
#42806=ADVANCED_FACE('',(#3951),#2261,.T.);
#42807=ADVANCED_FACE('',(#3952),#148,.T.);
#42808=ADVANCED_FACE('',(#3953),#42016,.T.);
#42809=ADVANCED_FACE('',(#3954),#149,.T.);
#42810=ADVANCED_FACE('',(#3955),#2262,.T.);
#42811=ADVANCED_FACE('',(#3956),#150,.T.);
#42812=ADVANCED_FACE('',(#3957),#2263,.T.);
#42813=ADVANCED_FACE('',(#3958),#151,.T.);
#42814=ADVANCED_FACE('',(#3959),#42017,.T.);
#42815=ADVANCED_FACE('',(#3960),#2264,.T.);
#42816=ADVANCED_FACE('',(#3961),#42018,.T.);
#42817=ADVANCED_FACE('',(#3962),#152,.T.);
#42818=ADVANCED_FACE('',(#3963),#2265,.T.);
#42819=ADVANCED_FACE('',(#3964),#153,.T.);
#42820=ADVANCED_FACE('',(#3965),#42019,.T.);
#42821=ADVANCED_FACE('',(#3966),#42020,.T.);
#42822=ADVANCED_FACE('',(#3967),#2266,.T.);
#42823=ADVANCED_FACE('',(#3968),#2267,.T.);
#42824=ADVANCED_FACE('',(#3969),#42021,.T.);
#42825=ADVANCED_FACE('',(#3970),#154,.T.);
#42826=ADVANCED_FACE('',(#3971),#2268,.T.);
#42827=ADVANCED_FACE('',(#3972),#42022,.T.);
#42828=ADVANCED_FACE('',(#3973),#2269,.T.);
#42829=ADVANCED_FACE('',(#3974),#42023,.T.);
#42830=ADVANCED_FACE('',(#3975),#155,.T.);
#42831=ADVANCED_FACE('',(#3976),#2270,.T.);
#42832=ADVANCED_FACE('',(#3977),#156,.T.);
#42833=ADVANCED_FACE('',(#3978),#42024,.T.);
#42834=ADVANCED_FACE('',(#3979),#157,.T.);
#42835=ADVANCED_FACE('',(#3980),#2271,.T.);
#42836=ADVANCED_FACE('',(#3981),#158,.T.);
#42837=ADVANCED_FACE('',(#3982),#42025,.T.);
#42838=ADVANCED_FACE('',(#3983),#159,.T.);
#42839=ADVANCED_FACE('',(#3984),#2272,.T.);
#42840=ADVANCED_FACE('',(#3985),#160,.T.);
#42841=ADVANCED_FACE('',(#3986),#42026,.T.);
#42842=ADVANCED_FACE('',(#3987),#2273,.T.);
#42843=ADVANCED_FACE('',(#3988),#2274,.T.);
#42844=ADVANCED_FACE('',(#3989),#161,.T.);
#42845=ADVANCED_FACE('',(#3990),#162,.T.);
#42846=ADVANCED_FACE('',(#3991),#163,.T.);
#42847=ADVANCED_FACE('',(#3992),#42027,.T.);
#42848=ADVANCED_FACE('',(#3993),#2275,.T.);
#42849=ADVANCED_FACE('',(#3994),#42028,.T.);
#42850=ADVANCED_FACE('',(#3995),#42029,.T.);
#42851=ADVANCED_FACE('',(#3996),#2276,.T.);
#42852=ADVANCED_FACE('',(#3997),#2277,.T.);
#42853=ADVANCED_FACE('',(#3998),#42030,.T.);
#42854=ADVANCED_FACE('',(#3999),#164,.T.);
#42855=ADVANCED_FACE('',(#4000),#2278,.T.);
#42856=ADVANCED_FACE('',(#4001),#42031,.T.);
#42857=ADVANCED_FACE('',(#4002),#2279,.T.);
#42858=ADVANCED_FACE('',(#4003),#42032,.T.);
#42859=ADVANCED_FACE('',(#4004),#165,.T.);
#42860=ADVANCED_FACE('',(#4005),#2280,.T.);
#42861=ADVANCED_FACE('',(#4006),#166,.T.);
#42862=ADVANCED_FACE('',(#4007),#42033,.T.);
#42863=ADVANCED_FACE('',(#4008),#167,.T.);
#42864=ADVANCED_FACE('',(#4009),#2281,.T.);
#42865=ADVANCED_FACE('',(#4010),#168,.T.);
#42866=ADVANCED_FACE('',(#4011),#42034,.T.);
#42867=ADVANCED_FACE('',(#4012),#169,.T.);
#42868=ADVANCED_FACE('',(#4013),#2282,.T.);
#42869=ADVANCED_FACE('',(#4014),#170,.T.);
#42870=ADVANCED_FACE('',(#4015),#42035,.T.);
#42871=ADVANCED_FACE('',(#4016),#2283,.T.);
#42872=ADVANCED_FACE('',(#4017),#2284,.T.);
#42873=ADVANCED_FACE('',(#4018),#171,.T.);
#42874=ADVANCED_FACE('',(#4019),#42036,.T.);
#42875=ADVANCED_FACE('',(#4020),#172,.T.);
#42876=ADVANCED_FACE('',(#4021),#2285,.T.);
#42877=ADVANCED_FACE('',(#4022),#173,.T.);
#42878=ADVANCED_FACE('',(#4023),#42037,.T.);
#42879=ADVANCED_FACE('',(#4024),#42038,.T.);
#42880=ADVANCED_FACE('',(#4025),#2286,.T.);
#42881=ADVANCED_FACE('',(#4026),#2287,.T.);
#42882=ADVANCED_FACE('',(#4027),#42039,.T.);
#42883=ADVANCED_FACE('',(#4028),#174,.T.);
#42884=ADVANCED_FACE('',(#4029),#2288,.T.);
#42885=ADVANCED_FACE('',(#4030),#42040,.T.);
#42886=ADVANCED_FACE('',(#4031),#2289,.T.);
#42887=ADVANCED_FACE('',(#4032),#42041,.T.);
#42888=ADVANCED_FACE('',(#4033),#175,.T.);
#42889=ADVANCED_FACE('',(#4034),#2290,.T.);
#42890=ADVANCED_FACE('',(#4035),#176,.T.);
#42891=ADVANCED_FACE('',(#4036),#42042,.T.);
#42892=ADVANCED_FACE('',(#4037),#177,.T.);
#42893=ADVANCED_FACE('',(#4038),#2291,.T.);
#42894=ADVANCED_FACE('',(#4039),#178,.T.);
#42895=ADVANCED_FACE('',(#4040),#42043,.T.);
#42896=ADVANCED_FACE('',(#4041),#179,.T.);
#42897=ADVANCED_FACE('',(#4042),#2292,.T.);
#42898=ADVANCED_FACE('',(#4043),#180,.T.);
#42899=ADVANCED_FACE('',(#4044),#42044,.T.);
#42900=ADVANCED_FACE('',(#4045),#2293,.T.);
#42901=ADVANCED_FACE('',(#4046),#2294,.T.);
#42902=ADVANCED_FACE('',(#4047),#181,.T.);
#42903=ADVANCED_FACE('',(#4048),#42045,.T.);
#42904=ADVANCED_FACE('',(#4049),#182,.T.);
#42905=ADVANCED_FACE('',(#4050),#2295,.T.);
#42906=ADVANCED_FACE('',(#4051),#183,.T.);
#42907=ADVANCED_FACE('',(#4052),#42046,.T.);
#42908=ADVANCED_FACE('',(#4053),#42047,.T.);
#42909=ADVANCED_FACE('',(#4054),#2296,.T.);
#42910=ADVANCED_FACE('',(#4055),#2297,.T.);
#42911=ADVANCED_FACE('',(#4056),#42048,.T.);
#42912=ADVANCED_FACE('',(#4057),#184,.T.);
#42913=ADVANCED_FACE('',(#4058),#2298,.T.);
#42914=ADVANCED_FACE('',(#4059),#42049,.T.);
#42915=ADVANCED_FACE('',(#4060),#2299,.T.);
#42916=ADVANCED_FACE('',(#4061),#42050,.T.);
#42917=ADVANCED_FACE('',(#4062),#185,.T.);
#42918=ADVANCED_FACE('',(#4063),#2300,.T.);
#42919=ADVANCED_FACE('',(#4064),#186,.T.);
#42920=ADVANCED_FACE('',(#4065),#42051,.T.);
#42921=ADVANCED_FACE('',(#4066),#187,.T.);
#42922=ADVANCED_FACE('',(#4067),#2301,.T.);
#42923=ADVANCED_FACE('',(#4068),#188,.T.);
#42924=ADVANCED_FACE('',(#4069),#42052,.T.);
#42925=ADVANCED_FACE('',(#4070),#189,.T.);
#42926=ADVANCED_FACE('',(#4071),#2302,.T.);
#42927=ADVANCED_FACE('',(#4072),#190,.T.);
#42928=ADVANCED_FACE('',(#4073),#42053,.T.);
#42929=ADVANCED_FACE('',(#4074),#2303,.T.);
#42930=ADVANCED_FACE('',(#4075),#2304,.T.);
#42931=ADVANCED_FACE('',(#4076),#191,.T.);
#42932=ADVANCED_FACE('',(#4077),#42054,.T.);
#42933=ADVANCED_FACE('',(#4078),#192,.T.);
#42934=ADVANCED_FACE('',(#4079),#2305,.T.);
#42935=ADVANCED_FACE('',(#4080),#193,.T.);
#42936=ADVANCED_FACE('',(#4081),#42055,.T.);
#42937=ADVANCED_FACE('',(#4082),#42056,.T.);
#42938=ADVANCED_FACE('',(#4083),#2306,.T.);
#42939=ADVANCED_FACE('',(#4084),#2307,.T.);
#42940=ADVANCED_FACE('',(#4085),#42057,.T.);
#42941=ADVANCED_FACE('',(#4086),#194,.T.);
#42942=ADVANCED_FACE('',(#4087),#2308,.T.);
#42943=ADVANCED_FACE('',(#4088),#42058,.T.);
#42944=ADVANCED_FACE('',(#4089),#2309,.T.);
#42945=ADVANCED_FACE('',(#4090),#42059,.T.);
#42946=ADVANCED_FACE('',(#4091),#195,.T.);
#42947=ADVANCED_FACE('',(#4092),#2310,.T.);
#42948=ADVANCED_FACE('',(#4093),#196,.T.);
#42949=ADVANCED_FACE('',(#4094),#42060,.T.);
#42950=ADVANCED_FACE('',(#4095),#197,.T.);
#42951=ADVANCED_FACE('',(#4096),#2311,.T.);
#42952=ADVANCED_FACE('',(#4097),#198,.T.);
#42953=ADVANCED_FACE('',(#4098),#42061,.T.);
#42954=ADVANCED_FACE('',(#4099),#199,.T.);
#42955=ADVANCED_FACE('',(#4100),#2312,.T.);
#42956=ADVANCED_FACE('',(#4101),#200,.T.);
#42957=ADVANCED_FACE('',(#4102),#42062,.T.);
#42958=ADVANCED_FACE('',(#4103),#2313,.T.);
#42959=ADVANCED_FACE('',(#4104),#2314,.T.);
#42960=ADVANCED_FACE('',(#4105),#201,.T.);
#42961=ADVANCED_FACE('',(#4106),#42063,.T.);
#42962=ADVANCED_FACE('',(#4107),#202,.T.);
#42963=ADVANCED_FACE('',(#4108),#2315,.T.);
#42964=ADVANCED_FACE('',(#4109),#203,.T.);
#42965=ADVANCED_FACE('',(#4110),#42064,.T.);
#42966=ADVANCED_FACE('',(#4111),#42065,.T.);
#42967=ADVANCED_FACE('',(#4112),#2316,.T.);
#42968=ADVANCED_FACE('',(#4113),#2317,.T.);
#42969=ADVANCED_FACE('',(#4114),#42066,.T.);
#42970=ADVANCED_FACE('',(#4115),#204,.T.);
#42971=ADVANCED_FACE('',(#4116),#2318,.T.);
#42972=ADVANCED_FACE('',(#4117),#42067,.T.);
#42973=ADVANCED_FACE('',(#4118),#2319,.T.);
#42974=ADVANCED_FACE('',(#4119),#42068,.T.);
#42975=ADVANCED_FACE('',(#4120),#205,.T.);
#42976=ADVANCED_FACE('',(#4121),#2320,.T.);
#42977=ADVANCED_FACE('',(#4122),#206,.T.);
#42978=ADVANCED_FACE('',(#4123),#42069,.T.);
#42979=ADVANCED_FACE('',(#4124),#207,.T.);
#42980=ADVANCED_FACE('',(#4125),#2321,.T.);
#42981=ADVANCED_FACE('',(#4126),#208,.T.);
#42982=ADVANCED_FACE('',(#4127),#42070,.T.);
#42983=ADVANCED_FACE('',(#4128),#209,.T.);
#42984=ADVANCED_FACE('',(#4129),#2322,.T.);
#42985=ADVANCED_FACE('',(#4130),#210,.T.);
#42986=ADVANCED_FACE('',(#4131),#42071,.T.);
#42987=ADVANCED_FACE('',(#4132),#2323,.T.);
#42988=ADVANCED_FACE('',(#4133),#2324,.T.);
#42989=ADVANCED_FACE('',(#4134),#211,.T.);
#42990=ADVANCED_FACE('',(#4135),#42072,.T.);
#42991=ADVANCED_FACE('',(#4136),#212,.T.);
#42992=ADVANCED_FACE('',(#4137),#2325,.T.);
#42993=ADVANCED_FACE('',(#4138),#213,.T.);
#42994=ADVANCED_FACE('',(#4139),#42073,.T.);
#42995=ADVANCED_FACE('',(#4140),#42074,.T.);
#42996=ADVANCED_FACE('',(#4141),#2326,.T.);
#42997=ADVANCED_FACE('',(#4142),#2327,.T.);
#42998=ADVANCED_FACE('',(#4143),#42075,.T.);
#42999=ADVANCED_FACE('',(#4144),#214,.T.);
#43000=ADVANCED_FACE('',(#4145),#2328,.T.);
#43001=ADVANCED_FACE('',(#4146),#42076,.T.);
#43002=ADVANCED_FACE('',(#4147),#2329,.T.);
#43003=ADVANCED_FACE('',(#4148),#42077,.T.);
#43004=ADVANCED_FACE('',(#4149),#215,.T.);
#43005=ADVANCED_FACE('',(#4150),#2330,.T.);
#43006=ADVANCED_FACE('',(#4151),#216,.T.);
#43007=ADVANCED_FACE('',(#4152),#42078,.T.);
#43008=ADVANCED_FACE('',(#4153),#217,.T.);
#43009=ADVANCED_FACE('',(#4154),#2331,.T.);
#43010=ADVANCED_FACE('',(#4155),#218,.T.);
#43011=ADVANCED_FACE('',(#4156),#42079,.T.);
#43012=ADVANCED_FACE('',(#4157),#219,.T.);
#43013=ADVANCED_FACE('',(#4158),#2332,.T.);
#43014=ADVANCED_FACE('',(#4159),#220,.T.);
#43015=ADVANCED_FACE('',(#4160),#42080,.T.);
#43016=ADVANCED_FACE('',(#4161),#2333,.T.);
#43017=ADVANCED_FACE('',(#4162),#2334,.T.);
#43018=ADVANCED_FACE('',(#4163),#221,.T.);
#43019=ADVANCED_FACE('',(#4164),#42081,.T.);
#43020=ADVANCED_FACE('',(#4165),#222,.T.);
#43021=ADVANCED_FACE('',(#4166),#2335,.T.);
#43022=ADVANCED_FACE('',(#4167),#223,.T.);
#43023=ADVANCED_FACE('',(#4168),#42082,.T.);
#43024=ADVANCED_FACE('',(#4169),#42083,.T.);
#43025=ADVANCED_FACE('',(#4170),#2336,.T.);
#43026=ADVANCED_FACE('',(#4171),#2337,.T.);
#43027=ADVANCED_FACE('',(#4172),#42084,.T.);
#43028=ADVANCED_FACE('',(#4173),#224,.T.);
#43029=ADVANCED_FACE('',(#4174),#2338,.T.);
#43030=ADVANCED_FACE('',(#4175),#42085,.T.);
#43031=ADVANCED_FACE('',(#4176),#2339,.T.);
#43032=ADVANCED_FACE('',(#4177),#42086,.T.);
#43033=ADVANCED_FACE('',(#4178),#225,.T.);
#43034=ADVANCED_FACE('',(#4179),#2340,.T.);
#43035=ADVANCED_FACE('',(#4180),#226,.T.);
#43036=ADVANCED_FACE('',(#4181),#42087,.T.);
#43037=ADVANCED_FACE('',(#4182),#227,.T.);
#43038=ADVANCED_FACE('',(#4183),#2341,.T.);
#43039=ADVANCED_FACE('',(#4184),#228,.T.);
#43040=ADVANCED_FACE('',(#4185),#42088,.T.);
#43041=ADVANCED_FACE('',(#4186),#229,.T.);
#43042=ADVANCED_FACE('',(#4187),#2342,.T.);
#43043=ADVANCED_FACE('',(#4188),#230,.T.);
#43044=ADVANCED_FACE('',(#4189),#42089,.T.);
#43045=ADVANCED_FACE('',(#4190),#2343,.T.);
#43046=ADVANCED_FACE('',(#4191),#2344,.T.);
#43047=ADVANCED_FACE('',(#4192),#231,.T.);
#43048=ADVANCED_FACE('',(#4193),#42090,.T.);
#43049=ADVANCED_FACE('',(#4194),#232,.T.);
#43050=ADVANCED_FACE('',(#4195),#2345,.T.);
#43051=ADVANCED_FACE('',(#4196),#233,.T.);
#43052=ADVANCED_FACE('',(#4197),#42091,.T.);
#43053=ADVANCED_FACE('',(#4198),#42092,.T.);
#43054=ADVANCED_FACE('',(#4199),#2346,.T.);
#43055=ADVANCED_FACE('',(#4200),#2347,.T.);
#43056=ADVANCED_FACE('',(#4201),#42093,.T.);
#43057=ADVANCED_FACE('',(#4202),#234,.T.);
#43058=ADVANCED_FACE('',(#4203),#2348,.T.);
#43059=ADVANCED_FACE('',(#4204),#42094,.T.);
#43060=ADVANCED_FACE('',(#4205),#2349,.T.);
#43061=ADVANCED_FACE('',(#4206),#42095,.T.);
#43062=ADVANCED_FACE('',(#4207),#235,.T.);
#43063=ADVANCED_FACE('',(#4208),#2350,.T.);
#43064=ADVANCED_FACE('',(#4209),#236,.T.);
#43065=ADVANCED_FACE('',(#4210),#42096,.T.);
#43066=ADVANCED_FACE('',(#4211),#237,.T.);
#43067=ADVANCED_FACE('',(#4212),#2351,.T.);
#43068=ADVANCED_FACE('',(#4213),#238,.T.);
#43069=ADVANCED_FACE('',(#4214),#42097,.T.);
#43070=ADVANCED_FACE('',(#4215),#239,.T.);
#43071=ADVANCED_FACE('',(#4216),#2352,.T.);
#43072=ADVANCED_FACE('',(#4217),#240,.T.);
#43073=ADVANCED_FACE('',(#4218),#42098,.T.);
#43074=ADVANCED_FACE('',(#4219),#2353,.T.);
#43075=ADVANCED_FACE('',(#4220),#2354,.T.);
#43076=ADVANCED_FACE('',(#4221),#241,.T.);
#43077=ADVANCED_FACE('',(#4222),#42099,.T.);
#43078=ADVANCED_FACE('',(#4223),#242,.T.);
#43079=ADVANCED_FACE('',(#4224),#2355,.T.);
#43080=ADVANCED_FACE('',(#4225),#243,.T.);
#43081=ADVANCED_FACE('',(#4226),#42100,.T.);
#43082=ADVANCED_FACE('',(#4227),#42101,.T.);
#43083=ADVANCED_FACE('',(#4228),#2356,.T.);
#43084=ADVANCED_FACE('',(#4229),#2357,.T.);
#43085=ADVANCED_FACE('',(#4230),#42102,.T.);
#43086=ADVANCED_FACE('',(#4231),#244,.T.);
#43087=ADVANCED_FACE('',(#4232),#2358,.T.);
#43088=ADVANCED_FACE('',(#4233),#42103,.T.);
#43089=ADVANCED_FACE('',(#4234),#2359,.T.);
#43090=ADVANCED_FACE('',(#4235),#42104,.T.);
#43091=ADVANCED_FACE('',(#4236),#245,.T.);
#43092=ADVANCED_FACE('',(#4237),#2360,.T.);
#43093=ADVANCED_FACE('',(#4238),#2361,.T.);
#43094=ADVANCED_FACE('',(#4239),#42105,.T.);
#43095=ADVANCED_FACE('',(#4240),#246,.T.);
#43096=ADVANCED_FACE('',(#4241),#2362,.T.);
#43097=ADVANCED_FACE('',(#4242),#247,.T.);
#43098=ADVANCED_FACE('',(#4243),#42106,.T.);
#43099=ADVANCED_FACE('',(#4244),#248,.T.);
#43100=ADVANCED_FACE('',(#4245),#2363,.T.);
#43101=ADVANCED_FACE('',(#4246),#249,.T.);
#43102=ADVANCED_FACE('',(#4247),#42107,.T.);
#43103=ADVANCED_FACE('',(#4248),#2364,.T.);
#43104=ADVANCED_FACE('',(#4249),#2365,.T.);
#43105=ADVANCED_FACE('',(#4250),#250,.T.);
#43106=ADVANCED_FACE('',(#4251),#42108,.T.);
#43107=ADVANCED_FACE('',(#4252),#251,.T.);
#43108=ADVANCED_FACE('',(#4253),#2366,.T.);
#43109=ADVANCED_FACE('',(#4254),#252,.T.);
#43110=ADVANCED_FACE('',(#4255),#42109,.T.);
#43111=ADVANCED_FACE('',(#4256),#42110,.T.);
#43112=ADVANCED_FACE('',(#4257),#2367,.T.);
#43113=ADVANCED_FACE('',(#4258),#2368,.T.);
#43114=ADVANCED_FACE('',(#4259),#42111,.T.);
#43115=ADVANCED_FACE('',(#4260),#253,.T.);
#43116=ADVANCED_FACE('',(#4261),#2369,.T.);
#43117=ADVANCED_FACE('',(#4262),#42112,.T.);
#43118=ADVANCED_FACE('',(#4263),#2370,.T.);
#43119=ADVANCED_FACE('',(#4264),#42113,.T.);
#43120=ADVANCED_FACE('',(#4265),#254,.T.);
#43121=ADVANCED_FACE('',(#4266),#2371,.T.);
#43122=ADVANCED_FACE('',(#4267),#255,.T.);
#43123=ADVANCED_FACE('',(#4268),#42114,.T.);
#43124=ADVANCED_FACE('',(#4269),#256,.T.);
#43125=ADVANCED_FACE('',(#4270),#2372,.T.);
#43126=ADVANCED_FACE('',(#4271),#257,.T.);
#43127=ADVANCED_FACE('',(#4272),#42115,.T.);
#43128=ADVANCED_FACE('',(#4273),#258,.T.);
#43129=ADVANCED_FACE('',(#4274),#2373,.T.);
#43130=ADVANCED_FACE('',(#4275),#259,.T.);
#43131=ADVANCED_FACE('',(#4276),#42116,.T.);
#43132=ADVANCED_FACE('',(#4277),#2374,.T.);
#43133=ADVANCED_FACE('',(#4278),#2375,.T.);
#43134=ADVANCED_FACE('',(#4279),#260,.T.);
#43135=ADVANCED_FACE('',(#4280),#42117,.T.);
#43136=ADVANCED_FACE('',(#4281),#261,.T.);
#43137=ADVANCED_FACE('',(#4282),#2376,.T.);
#43138=ADVANCED_FACE('',(#4283),#262,.T.);
#43139=ADVANCED_FACE('',(#4284),#42118,.T.);
#43140=ADVANCED_FACE('',(#4285),#42119,.T.);
#43141=ADVANCED_FACE('',(#4286),#2377,.T.);
#43142=ADVANCED_FACE('',(#4287),#2378,.T.);
#43143=ADVANCED_FACE('',(#4288),#42120,.T.);
#43144=ADVANCED_FACE('',(#4289),#263,.T.);
#43145=ADVANCED_FACE('',(#4290),#2379,.T.);
#43146=ADVANCED_FACE('',(#4291),#42121,.T.);
#43147=ADVANCED_FACE('',(#4292),#2380,.T.);
#43148=ADVANCED_FACE('',(#4293),#42122,.T.);
#43149=ADVANCED_FACE('',(#4294),#264,.T.);
#43150=ADVANCED_FACE('',(#4295),#2381,.T.);
#43151=ADVANCED_FACE('',(#4296),#265,.T.);
#43152=ADVANCED_FACE('',(#4297),#42123,.T.);
#43153=ADVANCED_FACE('',(#4298),#266,.T.);
#43154=ADVANCED_FACE('',(#4299),#2382,.T.);
#43155=ADVANCED_FACE('',(#4300),#267,.T.);
#43156=ADVANCED_FACE('',(#4301),#42124,.T.);
#43157=ADVANCED_FACE('',(#4302),#268,.T.);
#43158=ADVANCED_FACE('',(#4303),#2383,.T.);
#43159=ADVANCED_FACE('',(#4304),#269,.T.);
#43160=ADVANCED_FACE('',(#4305),#42125,.T.);
#43161=ADVANCED_FACE('',(#4306),#2384,.T.);
#43162=ADVANCED_FACE('',(#4307),#2385,.T.);
#43163=ADVANCED_FACE('',(#4308),#270,.T.);
#43164=ADVANCED_FACE('',(#4309),#42126,.T.);
#43165=ADVANCED_FACE('',(#4310),#271,.T.);
#43166=ADVANCED_FACE('',(#4311),#2386,.T.);
#43167=ADVANCED_FACE('',(#4312),#272,.T.);
#43168=ADVANCED_FACE('',(#4313),#42127,.T.);
#43169=ADVANCED_FACE('',(#4314),#42128,.T.);
#43170=ADVANCED_FACE('',(#4315),#2387,.T.);
#43171=ADVANCED_FACE('',(#4316),#2388,.T.);
#43172=ADVANCED_FACE('',(#4317),#42129,.T.);
#43173=ADVANCED_FACE('',(#4318),#273,.T.);
#43174=ADVANCED_FACE('',(#4319),#2389,.T.);
#43175=ADVANCED_FACE('',(#4320),#42130,.T.);
#43176=ADVANCED_FACE('',(#4321),#2390,.T.);
#43177=ADVANCED_FACE('',(#4322),#42131,.T.);
#43178=ADVANCED_FACE('',(#4323),#274,.T.);
#43179=ADVANCED_FACE('',(#4324),#2391,.T.);
#43180=ADVANCED_FACE('',(#4325),#275,.T.);
#43181=ADVANCED_FACE('',(#4326),#42132,.T.);
#43182=ADVANCED_FACE('',(#4327),#276,.T.);
#43183=ADVANCED_FACE('',(#4328),#2392,.T.);
#43184=ADVANCED_FACE('',(#4329),#277,.T.);
#43185=ADVANCED_FACE('',(#4330),#42133,.T.);
#43186=ADVANCED_FACE('',(#4331),#278,.T.);
#43187=ADVANCED_FACE('',(#4332),#2393,.T.);
#43188=ADVANCED_FACE('',(#4333),#279,.T.);
#43189=ADVANCED_FACE('',(#4334),#42134,.T.);
#43190=ADVANCED_FACE('',(#4335),#2394,.T.);
#43191=ADVANCED_FACE('',(#4336),#2395,.T.);
#43192=ADVANCED_FACE('',(#4337),#280,.T.);
#43193=ADVANCED_FACE('',(#4338),#42135,.T.);
#43194=ADVANCED_FACE('',(#4339),#281,.T.);
#43195=ADVANCED_FACE('',(#4340),#2396,.T.);
#43196=ADVANCED_FACE('',(#4341),#282,.T.);
#43197=ADVANCED_FACE('',(#4342),#42136,.T.);
#43198=ADVANCED_FACE('',(#4343),#42137,.T.);
#43199=ADVANCED_FACE('',(#4344),#2397,.T.);
#43200=ADVANCED_FACE('',(#4345),#2398,.T.);
#43201=ADVANCED_FACE('',(#4346),#42138,.T.);
#43202=ADVANCED_FACE('',(#4347),#283,.T.);
#43203=ADVANCED_FACE('',(#4348),#2399,.T.);
#43204=ADVANCED_FACE('',(#4349),#42139,.T.);
#43205=ADVANCED_FACE('',(#4350),#2400,.T.);
#43206=ADVANCED_FACE('',(#4351),#42140,.T.);
#43207=ADVANCED_FACE('',(#4352),#284,.T.);
#43208=ADVANCED_FACE('',(#4353),#2401,.T.);
#43209=ADVANCED_FACE('',(#4354),#285,.T.);
#43210=ADVANCED_FACE('',(#4355),#42141,.T.);
#43211=ADVANCED_FACE('',(#4356),#286,.T.);
#43212=ADVANCED_FACE('',(#4357),#2402,.T.);
#43213=ADVANCED_FACE('',(#4358),#287,.T.);
#43214=ADVANCED_FACE('',(#4359),#42142,.T.);
#43215=ADVANCED_FACE('',(#4360),#288,.T.);
#43216=ADVANCED_FACE('',(#4361),#2403,.T.);
#43217=ADVANCED_FACE('',(#4362),#289,.T.);
#43218=ADVANCED_FACE('',(#4363),#42143,.T.);
#43219=ADVANCED_FACE('',(#4364),#2404,.T.);
#43220=ADVANCED_FACE('',(#4365),#2405,.T.);
#43221=ADVANCED_FACE('',(#4366),#290,.T.);
#43222=ADVANCED_FACE('',(#4367),#42144,.T.);
#43223=ADVANCED_FACE('',(#4368),#291,.T.);
#43224=ADVANCED_FACE('',(#4369),#2406,.T.);
#43225=ADVANCED_FACE('',(#4370),#292,.T.);
#43226=ADVANCED_FACE('',(#4371),#42145,.T.);
#43227=ADVANCED_FACE('',(#4372),#42146,.T.);
#43228=ADVANCED_FACE('',(#4373),#2407,.T.);
#43229=ADVANCED_FACE('',(#4374),#2408,.T.);
#43230=ADVANCED_FACE('',(#4375),#42147,.T.);
#43231=ADVANCED_FACE('',(#4376),#293,.T.);
#43232=ADVANCED_FACE('',(#4377),#2409,.T.);
#43233=ADVANCED_FACE('',(#4378),#42148,.T.);
#43234=ADVANCED_FACE('',(#4379),#2410,.T.);
#43235=ADVANCED_FACE('',(#4380),#42149,.T.);
#43236=ADVANCED_FACE('',(#4381),#294,.T.);
#43237=ADVANCED_FACE('',(#4382),#2411,.T.);
#43238=ADVANCED_FACE('',(#4383),#2412,.T.);
#43239=ADVANCED_FACE('',(#4384),#42150,.T.);
#43240=ADVANCED_FACE('',(#4385),#295,.T.);
#43241=ADVANCED_FACE('',(#4386),#2413,.T.);
#43242=ADVANCED_FACE('',(#4387),#296,.T.);
#43243=ADVANCED_FACE('',(#4388),#42151,.T.);
#43244=ADVANCED_FACE('',(#4389),#297,.T.);
#43245=ADVANCED_FACE('',(#4390),#2414,.T.);
#43246=ADVANCED_FACE('',(#4391),#298,.T.);
#43247=ADVANCED_FACE('',(#4392),#42152,.T.);
#43248=ADVANCED_FACE('',(#4393),#2415,.T.);
#43249=ADVANCED_FACE('',(#4394),#2416,.T.);
#43250=ADVANCED_FACE('',(#4395),#299,.T.);
#43251=ADVANCED_FACE('',(#4396),#42153,.T.);
#43252=ADVANCED_FACE('',(#4397),#300,.T.);
#43253=ADVANCED_FACE('',(#4398),#2417,.T.);
#43254=ADVANCED_FACE('',(#4399),#301,.T.);
#43255=ADVANCED_FACE('',(#4400),#42154,.T.);
#43256=ADVANCED_FACE('',(#4401),#42155,.T.);
#43257=ADVANCED_FACE('',(#4402),#2418,.T.);
#43258=ADVANCED_FACE('',(#4403),#2419,.T.);
#43259=ADVANCED_FACE('',(#4404),#42156,.T.);
#43260=ADVANCED_FACE('',(#4405),#302,.T.);
#43261=ADVANCED_FACE('',(#4406),#2420,.T.);
#43262=ADVANCED_FACE('',(#4407),#42157,.T.);
#43263=ADVANCED_FACE('',(#4408),#2421,.T.);
#43264=ADVANCED_FACE('',(#4409),#42158,.T.);
#43265=ADVANCED_FACE('',(#4410),#303,.T.);
#43266=ADVANCED_FACE('',(#4411),#2422,.T.);
#43267=ADVANCED_FACE('',(#4412),#304,.T.);
#43268=ADVANCED_FACE('',(#4413),#42159,.T.);
#43269=ADVANCED_FACE('',(#4414),#2423,.T.);
#43270=ADVANCED_FACE('',(#4415),#2424,.T.);
#43271=ADVANCED_FACE('',(#4416),#305,.T.);
#43272=ADVANCED_FACE('',(#4417),#42160,.T.);
#43273=ADVANCED_FACE('',(#4418),#306,.T.);
#43274=ADVANCED_FACE('',(#4419),#2425,.T.);
#43275=ADVANCED_FACE('',(#4420),#307,.T.);
#43276=ADVANCED_FACE('',(#4421),#42161,.T.);
#43277=ADVANCED_FACE('',(#4422),#2426,.T.);
#43278=ADVANCED_FACE('',(#4423),#2427,.T.);
#43279=ADVANCED_FACE('',(#4424),#308,.T.);
#43280=ADVANCED_FACE('',(#4425),#42162,.T.);
#43281=ADVANCED_FACE('',(#4426),#309,.T.);
#43282=ADVANCED_FACE('',(#4427),#2428,.T.);
#43283=ADVANCED_FACE('',(#4428),#310,.T.);
#43284=ADVANCED_FACE('',(#4429),#42163,.T.);
#43285=ADVANCED_FACE('',(#4430),#42164,.T.);
#43286=ADVANCED_FACE('',(#4431),#2429,.T.);
#43287=ADVANCED_FACE('',(#4432),#2430,.T.);
#43288=ADVANCED_FACE('',(#4433),#42165,.T.);
#43289=ADVANCED_FACE('',(#4434),#311,.T.);
#43290=ADVANCED_FACE('',(#4435),#2431,.T.);
#43291=ADVANCED_FACE('',(#4436),#42166,.T.);
#43292=ADVANCED_FACE('',(#4437),#2432,.T.);
#43293=ADVANCED_FACE('',(#4438),#42167,.T.);
#43294=ADVANCED_FACE('',(#4439),#312,.T.);
#43295=ADVANCED_FACE('',(#4440),#2433,.T.);
#43296=ADVANCED_FACE('',(#4441),#2434,.T.);
#43297=ADVANCED_FACE('',(#4442),#42168,.T.);
#43298=ADVANCED_FACE('',(#4443),#313,.T.);
#43299=ADVANCED_FACE('',(#4444),#2435,.T.);
#43300=ADVANCED_FACE('',(#4445),#314,.T.);
#43301=ADVANCED_FACE('',(#4446),#42169,.T.);
#43302=ADVANCED_FACE('',(#4447),#315,.T.);
#43303=ADVANCED_FACE('',(#4448),#2436,.T.);
#43304=ADVANCED_FACE('',(#4449),#2437,.T.);
#43305=ADVANCED_FACE('',(#4450),#42170,.T.);
#43306=ADVANCED_FACE('',(#4451),#2438,.T.);
#43307=ADVANCED_FACE('',(#4452),#2439,.T.);
#43308=ADVANCED_FACE('',(#4453),#316,.T.);
#43309=ADVANCED_FACE('',(#4454),#42171,.T.);
#43310=ADVANCED_FACE('',(#4455),#317,.T.);
#43311=ADVANCED_FACE('',(#4456),#2440,.T.);
#43312=ADVANCED_FACE('',(#4457),#318,.T.);
#43313=ADVANCED_FACE('',(#4458),#42172,.T.);
#43314=ADVANCED_FACE('',(#4459),#42173,.T.);
#43315=ADVANCED_FACE('',(#4460),#2441,.T.);
#43316=ADVANCED_FACE('',(#4461),#2442,.T.);
#43317=ADVANCED_FACE('',(#4462),#42174,.T.);
#43318=ADVANCED_FACE('',(#4463),#319,.T.);
#43319=ADVANCED_FACE('',(#4464),#2443,.T.);
#43320=ADVANCED_FACE('',(#4465),#42175,.T.);
#43321=ADVANCED_FACE('',(#4466),#2444,.T.);
#43322=ADVANCED_FACE('',(#4467),#42176,.T.);
#43323=ADVANCED_FACE('',(#4468),#320,.T.);
#43324=ADVANCED_FACE('',(#4469),#2445,.T.);
#43325=ADVANCED_FACE('',(#4470),#321,.T.);
#43326=ADVANCED_FACE('',(#4471),#42177,.T.);
#43327=ADVANCED_FACE('',(#4472),#322,.T.);
#43328=ADVANCED_FACE('',(#4473),#2446,.T.);
#43329=ADVANCED_FACE('',(#4474),#323,.T.);
#43330=ADVANCED_FACE('',(#4475),#42178,.T.);
#43331=ADVANCED_FACE('',(#4476),#324,.T.);
#43332=ADVANCED_FACE('',(#4477),#2447,.T.);
#43333=ADVANCED_FACE('',(#4478),#325,.T.);
#43334=ADVANCED_FACE('',(#4479),#42179,.T.);
#43335=ADVANCED_FACE('',(#4480),#2448,.T.);
#43336=ADVANCED_FACE('',(#4481),#2449,.T.);
#43337=ADVANCED_FACE('',(#4482),#2450,.T.);
#43338=ADVANCED_FACE('',(#4483),#42180,.T.);
#43339=ADVANCED_FACE('',(#4484),#326,.T.);
#43340=ADVANCED_FACE('',(#4485),#2451,.T.);
#43341=ADVANCED_FACE('',(#4486),#327,.T.);
#43342=ADVANCED_FACE('',(#4487),#42181,.T.);
#43343=ADVANCED_FACE('',(#4488),#42182,.T.);
#43344=ADVANCED_FACE('',(#4489),#2452,.T.);
#43345=ADVANCED_FACE('',(#4490),#2453,.T.);
#43346=ADVANCED_FACE('',(#4491),#42183,.T.);
#43347=ADVANCED_FACE('',(#4492),#328,.T.);
#43348=ADVANCED_FACE('',(#4493),#2454,.T.);
#43349=ADVANCED_FACE('',(#4494),#42184,.T.);
#43350=ADVANCED_FACE('',(#4495),#2455,.T.);
#43351=ADVANCED_FACE('',(#4496),#42185,.T.);
#43352=ADVANCED_FACE('',(#4497),#329,.T.);
#43353=ADVANCED_FACE('',(#4498),#2456,.T.);
#43354=ADVANCED_FACE('',(#4499),#330,.T.);
#43355=ADVANCED_FACE('',(#4500),#42186,.T.);
#43356=ADVANCED_FACE('',(#4501),#331,.T.);
#43357=ADVANCED_FACE('',(#4502),#2457,.T.);
#43358=ADVANCED_FACE('',(#4503),#332,.T.);
#43359=ADVANCED_FACE('',(#4504),#42187,.T.);
#43360=ADVANCED_FACE('',(#4505),#333,.T.);
#43361=ADVANCED_FACE('',(#4506),#2458,.T.);
#43362=ADVANCED_FACE('',(#4507),#334,.T.);
#43363=ADVANCED_FACE('',(#4508),#42188,.T.);
#43364=ADVANCED_FACE('',(#4509),#2459,.T.);
#43365=ADVANCED_FACE('',(#4510),#2460,.T.);
#43366=ADVANCED_FACE('',(#4511),#335,.T.);
#43367=ADVANCED_FACE('',(#4512),#42189,.T.);
#43368=ADVANCED_FACE('',(#4513),#336,.T.);
#43369=ADVANCED_FACE('',(#4514),#2461,.T.);
#43370=ADVANCED_FACE('',(#4515),#2462,.T.);
#43371=ADVANCED_FACE('',(#4516),#42190,.T.);
#43372=ADVANCED_FACE('',(#4517),#42191,.T.);
#43373=ADVANCED_FACE('',(#4518),#2463,.T.);
#43374=ADVANCED_FACE('',(#4519),#2464,.T.);
#43375=ADVANCED_FACE('',(#4520),#42192,.T.);
#43376=ADVANCED_FACE('',(#4521),#337,.T.);
#43377=ADVANCED_FACE('',(#4522),#2465,.T.);
#43378=ADVANCED_FACE('',(#4523),#42193,.T.);
#43379=ADVANCED_FACE('',(#4524),#2466,.T.);
#43380=ADVANCED_FACE('',(#4525),#42194,.T.);
#43381=ADVANCED_FACE('',(#4526),#338,.T.);
#43382=ADVANCED_FACE('',(#4527),#2467,.T.);
#43383=ADVANCED_FACE('',(#4528),#339,.T.);
#43384=ADVANCED_FACE('',(#4529),#42195,.T.);
#43385=ADVANCED_FACE('',(#4530),#340,.T.);
#43386=ADVANCED_FACE('',(#4531),#2468,.T.);
#43387=ADVANCED_FACE('',(#4532),#341,.T.);
#43388=ADVANCED_FACE('',(#4533),#42196,.T.);
#43389=ADVANCED_FACE('',(#4534),#342,.T.);
#43390=ADVANCED_FACE('',(#4535),#2469,.T.);
#43391=ADVANCED_FACE('',(#4536),#343,.T.);
#43392=ADVANCED_FACE('',(#4537),#42197,.T.);
#43393=ADVANCED_FACE('',(#4538),#2470,.T.);
#43394=ADVANCED_FACE('',(#4539),#2471,.T.);
#43395=ADVANCED_FACE('',(#4540),#344,.T.);
#43396=ADVANCED_FACE('',(#4541),#42198,.T.);
#43397=ADVANCED_FACE('',(#4542),#345,.T.);
#43398=ADVANCED_FACE('',(#4543),#2472,.T.);
#43399=ADVANCED_FACE('',(#4544),#346,.T.);
#43400=ADVANCED_FACE('',(#4545),#42199,.T.);
#43401=ADVANCED_FACE('',(#4546),#42200,.T.);
#43402=ADVANCED_FACE('',(#4547),#2473,.T.);
#43403=ADVANCED_FACE('',(#4548),#2474,.T.);
#43404=ADVANCED_FACE('',(#4549),#42201,.T.);
#43405=ADVANCED_FACE('',(#4550),#347,.T.);
#43406=ADVANCED_FACE('',(#4551),#2475,.T.);
#43407=ADVANCED_FACE('',(#4552),#42202,.T.);
#43408=ADVANCED_FACE('',(#4553),#2476,.T.);
#43409=ADVANCED_FACE('',(#4554),#42203,.T.);
#43410=ADVANCED_FACE('',(#4555),#348,.T.);
#43411=ADVANCED_FACE('',(#4556),#2477,.T.);
#43412=ADVANCED_FACE('',(#4557),#349,.T.);
#43413=ADVANCED_FACE('',(#4558),#42204,.T.);
#43414=ADVANCED_FACE('',(#4559),#350,.T.);
#43415=ADVANCED_FACE('',(#4560),#2478,.T.);
#43416=ADVANCED_FACE('',(#4561),#351,.T.);
#43417=ADVANCED_FACE('',(#4562),#42205,.T.);
#43418=ADVANCED_FACE('',(#4563),#352,.T.);
#43419=ADVANCED_FACE('',(#4564),#2479,.T.);
#43420=ADVANCED_FACE('',(#4565),#353,.T.);
#43421=ADVANCED_FACE('',(#4566),#42206,.T.);
#43422=ADVANCED_FACE('',(#4567),#2480,.T.);
#43423=ADVANCED_FACE('',(#4568),#2481,.T.);
#43424=ADVANCED_FACE('',(#4569),#354,.T.);
#43425=ADVANCED_FACE('',(#4570),#42207,.T.);
#43426=ADVANCED_FACE('',(#4571),#355,.T.);
#43427=ADVANCED_FACE('',(#4572),#2482,.T.);
#43428=ADVANCED_FACE('',(#4573),#356,.T.);
#43429=ADVANCED_FACE('',(#4574),#42208,.T.);
#43430=ADVANCED_FACE('',(#4575),#42209,.T.);
#43431=ADVANCED_FACE('',(#4576),#2483,.T.);
#43432=ADVANCED_FACE('',(#4577),#2484,.T.);
#43433=ADVANCED_FACE('',(#4578),#42210,.T.);
#43434=ADVANCED_FACE('',(#4579),#357,.T.);
#43435=ADVANCED_FACE('',(#4580),#2485,.T.);
#43436=ADVANCED_FACE('',(#4581),#42211,.T.);
#43437=ADVANCED_FACE('',(#4582),#2486,.T.);
#43438=ADVANCED_FACE('',(#4583),#42212,.T.);
#43439=ADVANCED_FACE('',(#4584),#358,.T.);
#43440=ADVANCED_FACE('',(#4585),#2487,.T.);
#43441=ADVANCED_FACE('',(#4586),#359,.T.);
#43442=ADVANCED_FACE('',(#4587),#42213,.T.);
#43443=ADVANCED_FACE('',(#4588),#360,.T.);
#43444=ADVANCED_FACE('',(#4589),#2488,.T.);
#43445=ADVANCED_FACE('',(#4590),#361,.T.);
#43446=ADVANCED_FACE('',(#4591),#42214,.T.);
#43447=ADVANCED_FACE('',(#4592),#362,.T.);
#43448=ADVANCED_FACE('',(#4593),#2489,.T.);
#43449=ADVANCED_FACE('',(#4594),#363,.T.);
#43450=ADVANCED_FACE('',(#4595),#42215,.T.);
#43451=ADVANCED_FACE('',(#4596),#2490,.T.);
#43452=ADVANCED_FACE('',(#4597),#2491,.T.);
#43453=ADVANCED_FACE('',(#4598),#364,.T.);
#43454=ADVANCED_FACE('',(#4599),#42216,.T.);
#43455=ADVANCED_FACE('',(#4600),#365,.T.);
#43456=ADVANCED_FACE('',(#4601),#2492,.T.);
#43457=ADVANCED_FACE('',(#4602),#366,.T.);
#43458=ADVANCED_FACE('',(#4603),#42217,.T.);
#43459=ADVANCED_FACE('',(#4604),#42218,.T.);
#43460=ADVANCED_FACE('',(#4605),#2493,.T.);
#43461=ADVANCED_FACE('',(#4606),#2494,.T.);
#43462=ADVANCED_FACE('',(#4607),#42219,.T.);
#43463=ADVANCED_FACE('',(#4608),#367,.T.);
#43464=ADVANCED_FACE('',(#4609),#2495,.T.);
#43465=ADVANCED_FACE('',(#4610),#42220,.T.);
#43466=ADVANCED_FACE('',(#4611),#2496,.T.);
#43467=ADVANCED_FACE('',(#4612),#42221,.T.);
#43468=ADVANCED_FACE('',(#4613),#368,.T.);
#43469=ADVANCED_FACE('',(#4614),#2497,.T.);
#43470=ADVANCED_FACE('',(#4615),#369,.T.);
#43471=ADVANCED_FACE('',(#4616),#42222,.T.);
#43472=ADVANCED_FACE('',(#4617),#370,.T.);
#43473=ADVANCED_FACE('',(#4618),#2498,.T.);
#43474=ADVANCED_FACE('',(#4619),#371,.T.);
#43475=ADVANCED_FACE('',(#4620),#42223,.T.);
#43476=ADVANCED_FACE('',(#4621),#372,.T.);
#43477=ADVANCED_FACE('',(#4622),#2499,.T.);
#43478=ADVANCED_FACE('',(#4623),#373,.T.);
#43479=ADVANCED_FACE('',(#4624),#42224,.T.);
#43480=ADVANCED_FACE('',(#4625),#2500,.T.);
#43481=ADVANCED_FACE('',(#4626),#2501,.T.);
#43482=ADVANCED_FACE('',(#4627),#374,.T.);
#43483=ADVANCED_FACE('',(#4628),#42225,.T.);
#43484=ADVANCED_FACE('',(#4629),#375,.T.);
#43485=ADVANCED_FACE('',(#4630),#2502,.T.);
#43486=ADVANCED_FACE('',(#4631),#376,.T.);
#43487=ADVANCED_FACE('',(#4632),#42226,.T.);
#43488=ADVANCED_FACE('',(#4633),#42227,.T.);
#43489=ADVANCED_FACE('',(#4634),#2503,.T.);
#43490=ADVANCED_FACE('',(#4635),#2504,.T.);
#43491=ADVANCED_FACE('',(#4636),#42228,.T.);
#43492=ADVANCED_FACE('',(#4637),#377,.T.);
#43493=ADVANCED_FACE('',(#4638),#2505,.T.);
#43494=ADVANCED_FACE('',(#4639),#42229,.T.);
#43495=ADVANCED_FACE('',(#4640),#2506,.T.);
#43496=ADVANCED_FACE('',(#4641),#42230,.T.);
#43497=ADVANCED_FACE('',(#4642),#378,.T.);
#43498=ADVANCED_FACE('',(#4643),#2507,.T.);
#43499=ADVANCED_FACE('',(#4644),#379,.T.);
#43500=ADVANCED_FACE('',(#4645),#42231,.T.);
#43501=ADVANCED_FACE('',(#4646),#380,.T.);
#43502=ADVANCED_FACE('',(#4647),#2508,.T.);
#43503=ADVANCED_FACE('',(#4648),#381,.T.);
#43504=ADVANCED_FACE('',(#4649),#42232,.T.);
#43505=ADVANCED_FACE('',(#4650),#382,.T.);
#43506=ADVANCED_FACE('',(#4651),#2509,.T.);
#43507=ADVANCED_FACE('',(#4652),#383,.T.);
#43508=ADVANCED_FACE('',(#4653),#42233,.T.);
#43509=ADVANCED_FACE('',(#4654),#2510,.T.);
#43510=ADVANCED_FACE('',(#4655),#2511,.T.);
#43511=ADVANCED_FACE('',(#4656),#384,.T.);
#43512=ADVANCED_FACE('',(#4657),#42234,.T.);
#43513=ADVANCED_FACE('',(#4658),#385,.T.);
#43514=ADVANCED_FACE('',(#4659),#2512,.T.);
#43515=ADVANCED_FACE('',(#4660),#386,.T.);
#43516=ADVANCED_FACE('',(#4661),#42235,.T.);
#43517=ADVANCED_FACE('',(#4662),#42236,.T.);
#43518=ADVANCED_FACE('',(#4663),#2513,.T.);
#43519=ADVANCED_FACE('',(#4664),#2514,.T.);
#43520=ADVANCED_FACE('',(#4665),#42237,.T.);
#43521=ADVANCED_FACE('',(#4666),#387,.T.);
#43522=ADVANCED_FACE('',(#4667),#2515,.T.);
#43523=ADVANCED_FACE('',(#4668),#42238,.T.);
#43524=ADVANCED_FACE('',(#4669),#2516,.T.);
#43525=ADVANCED_FACE('',(#4670),#42239,.T.);
#43526=ADVANCED_FACE('',(#4671),#388,.T.);
#43527=ADVANCED_FACE('',(#4672),#2517,.T.);
#43528=ADVANCED_FACE('',(#4673),#389,.T.);
#43529=ADVANCED_FACE('',(#4674),#42240,.T.);
#43530=ADVANCED_FACE('',(#4675),#390,.T.);
#43531=ADVANCED_FACE('',(#4676),#2518,.T.);
#43532=ADVANCED_FACE('',(#4677),#391,.T.);
#43533=ADVANCED_FACE('',(#4678),#42241,.T.);
#43534=ADVANCED_FACE('',(#4679),#392,.T.);
#43535=ADVANCED_FACE('',(#4680),#2519,.T.);
#43536=ADVANCED_FACE('',(#4681),#393,.T.);
#43537=ADVANCED_FACE('',(#4682),#42242,.T.);
#43538=ADVANCED_FACE('',(#4683),#2520,.T.);
#43539=ADVANCED_FACE('',(#4684),#2521,.T.);
#43540=ADVANCED_FACE('',(#4685),#394,.T.);
#43541=ADVANCED_FACE('',(#4686),#42243,.T.);
#43542=ADVANCED_FACE('',(#4687),#395,.T.);
#43543=ADVANCED_FACE('',(#4688),#2522,.T.);
#43544=ADVANCED_FACE('',(#4689),#396,.T.);
#43545=ADVANCED_FACE('',(#4690),#42244,.T.);
#43546=ADVANCED_FACE('',(#4691),#42245,.T.);
#43547=ADVANCED_FACE('',(#4692),#2523,.T.);
#43548=ADVANCED_FACE('',(#4693),#2524,.T.);
#43549=ADVANCED_FACE('',(#4694),#42246,.T.);
#43550=ADVANCED_FACE('',(#4695),#397,.T.);
#43551=ADVANCED_FACE('',(#4696),#2525,.T.);
#43552=ADVANCED_FACE('',(#4697),#42247,.T.);
#43553=ADVANCED_FACE('',(#4698),#2526,.T.);
#43554=ADVANCED_FACE('',(#4699),#42248,.T.);
#43555=ADVANCED_FACE('',(#4700),#398,.T.);
#43556=ADVANCED_FACE('',(#4701),#2527,.T.);
#43557=ADVANCED_FACE('',(#4702),#2528,.T.);
#43558=ADVANCED_FACE('',(#4703),#42249,.T.);
#43559=ADVANCED_FACE('',(#4704),#399,.T.);
#43560=ADVANCED_FACE('',(#4705),#2529,.T.);
#43561=ADVANCED_FACE('',(#4706),#400,.T.);
#43562=ADVANCED_FACE('',(#4707),#42250,.T.);
#43563=ADVANCED_FACE('',(#4708),#401,.T.);
#43564=ADVANCED_FACE('',(#4709),#2530,.T.);
#43565=ADVANCED_FACE('',(#4710),#402,.T.);
#43566=ADVANCED_FACE('',(#4711),#42251,.T.);
#43567=ADVANCED_FACE('',(#4712),#2531,.T.);
#43568=ADVANCED_FACE('',(#4713),#2532,.T.);
#43569=ADVANCED_FACE('',(#4714),#403,.T.);
#43570=ADVANCED_FACE('',(#4715),#42252,.T.);
#43571=ADVANCED_FACE('',(#4716),#404,.T.);
#43572=ADVANCED_FACE('',(#4717),#2533,.T.);
#43573=ADVANCED_FACE('',(#4718),#405,.T.);
#43574=ADVANCED_FACE('',(#4719),#42253,.T.);
#43575=ADVANCED_FACE('',(#4720),#42254,.T.);
#43576=ADVANCED_FACE('',(#4721),#2534,.T.);
#43577=ADVANCED_FACE('',(#4722),#2535,.T.);
#43578=ADVANCED_FACE('',(#4723),#42255,.T.);
#43579=ADVANCED_FACE('',(#4724),#406,.T.);
#43580=ADVANCED_FACE('',(#4725),#2536,.T.);
#43581=ADVANCED_FACE('',(#4726),#42256,.T.);
#43582=ADVANCED_FACE('',(#4727),#2537,.T.);
#43583=ADVANCED_FACE('',(#4728),#42257,.T.);
#43584=ADVANCED_FACE('',(#4729),#407,.T.);
#43585=ADVANCED_FACE('',(#4730),#2538,.T.);
#43586=ADVANCED_FACE('',(#4731),#408,.T.);
#43587=ADVANCED_FACE('',(#4732),#42258,.T.);
#43588=ADVANCED_FACE('',(#4733),#2539,.T.);
#43589=ADVANCED_FACE('',(#4734),#2540,.T.);
#43590=ADVANCED_FACE('',(#4735),#409,.T.);
#43591=ADVANCED_FACE('',(#4736),#42259,.T.);
#43592=ADVANCED_FACE('',(#4737),#410,.T.);
#43593=ADVANCED_FACE('',(#4738),#2541,.T.);
#43594=ADVANCED_FACE('',(#4739),#411,.T.);
#43595=ADVANCED_FACE('',(#4740),#42260,.T.);
#43596=ADVANCED_FACE('',(#4741),#2542,.T.);
#43597=ADVANCED_FACE('',(#4742),#2543,.T.);
#43598=ADVANCED_FACE('',(#4743),#412,.T.);
#43599=ADVANCED_FACE('',(#4744),#42261,.T.);
#43600=ADVANCED_FACE('',(#4745),#413,.T.);
#43601=ADVANCED_FACE('',(#4746),#2544,.T.);
#43602=ADVANCED_FACE('',(#4747),#414,.T.);
#43603=ADVANCED_FACE('',(#4748),#42262,.T.);
#43604=ADVANCED_FACE('',(#4749),#42263,.T.);
#43605=ADVANCED_FACE('',(#4750),#2545,.T.);
#43606=ADVANCED_FACE('',(#4751),#2546,.T.);
#43607=ADVANCED_FACE('',(#4752),#42264,.T.);
#43608=ADVANCED_FACE('',(#4753),#415,.T.);
#43609=ADVANCED_FACE('',(#4754),#2547,.T.);
#43610=ADVANCED_FACE('',(#4755),#42265,.T.);
#43611=ADVANCED_FACE('',(#4756),#2548,.T.);
#43612=ADVANCED_FACE('',(#4757),#42266,.T.);
#43613=ADVANCED_FACE('',(#4758),#416,.T.);
#43614=ADVANCED_FACE('',(#4759),#2549,.T.);
#43615=ADVANCED_FACE('',(#4760),#417,.T.);
#43616=ADVANCED_FACE('',(#4761),#42267,.T.);
#43617=ADVANCED_FACE('',(#4762),#418,.T.);
#43618=ADVANCED_FACE('',(#4763),#2550,.T.);
#43619=ADVANCED_FACE('',(#4764),#419,.T.);
#43620=ADVANCED_FACE('',(#4765),#42268,.T.);
#43621=ADVANCED_FACE('',(#4766),#420,.T.);
#43622=ADVANCED_FACE('',(#4767),#2551,.T.);
#43623=ADVANCED_FACE('',(#4768),#2552,.T.);
#43624=ADVANCED_FACE('',(#4769),#42269,.T.);
#43625=ADVANCED_FACE('',(#4770),#2553,.T.);
#43626=ADVANCED_FACE('',(#4771),#2554,.T.);
#43627=ADVANCED_FACE('',(#4772),#421,.T.);
#43628=ADVANCED_FACE('',(#4773),#42270,.T.);
#43629=ADVANCED_FACE('',(#4774),#422,.T.);
#43630=ADVANCED_FACE('',(#4775),#2555,.T.);
#43631=ADVANCED_FACE('',(#4776),#423,.T.);
#43632=ADVANCED_FACE('',(#4777),#42271,.T.);
#43633=ADVANCED_FACE('',(#4778),#42272,.T.);
#43634=ADVANCED_FACE('',(#4779),#2556,.T.);
#43635=ADVANCED_FACE('',(#4780),#2557,.T.);
#43636=ADVANCED_FACE('',(#4781),#42273,.T.);
#43637=ADVANCED_FACE('',(#4782),#424,.T.);
#43638=ADVANCED_FACE('',(#4783),#2558,.T.);
#43639=ADVANCED_FACE('',(#4784),#42274,.T.);
#43640=ADVANCED_FACE('',(#4785),#2559,.T.);
#43641=ADVANCED_FACE('',(#4786),#42275,.T.);
#43642=ADVANCED_FACE('',(#4787),#425,.T.);
#43643=ADVANCED_FACE('',(#4788),#2560,.T.);
#43644=ADVANCED_FACE('',(#4789),#426,.T.);
#43645=ADVANCED_FACE('',(#4790),#42276,.T.);
#43646=ADVANCED_FACE('',(#4791),#427,.T.);
#43647=ADVANCED_FACE('',(#4792),#2561,.T.);
#43648=ADVANCED_FACE('',(#4793),#428,.T.);
#43649=ADVANCED_FACE('',(#4794),#42277,.T.);
#43650=ADVANCED_FACE('',(#4795),#429,.T.);
#43651=ADVANCED_FACE('',(#4796),#2562,.T.);
#43652=ADVANCED_FACE('',(#4797),#430,.T.);
#43653=ADVANCED_FACE('',(#4798),#42278,.T.);
#43654=ADVANCED_FACE('',(#4799),#2563,.T.);
#43655=ADVANCED_FACE('',(#4800),#2564,.T.);
#43656=ADVANCED_FACE('',(#4801),#2565,.T.);
#43657=ADVANCED_FACE('',(#4802),#42279,.T.);
#43658=ADVANCED_FACE('',(#4803),#431,.T.);
#43659=ADVANCED_FACE('',(#4804),#2566,.T.);
#43660=ADVANCED_FACE('',(#4805),#432,.T.);
#43661=ADVANCED_FACE('',(#4806),#42280,.T.);
#43662=ADVANCED_FACE('',(#4807),#42281,.T.);
#43663=ADVANCED_FACE('',(#4808),#2567,.T.);
#43664=ADVANCED_FACE('',(#4809),#2568,.T.);
#43665=ADVANCED_FACE('',(#4810),#42282,.T.);
#43666=ADVANCED_FACE('',(#4811),#433,.T.);
#43667=ADVANCED_FACE('',(#4812),#2569,.T.);
#43668=ADVANCED_FACE('',(#4813),#42283,.T.);
#43669=ADVANCED_FACE('',(#4814),#2570,.T.);
#43670=ADVANCED_FACE('',(#4815),#42284,.T.);
#43671=ADVANCED_FACE('',(#4816),#434,.T.);
#43672=ADVANCED_FACE('',(#4817),#2571,.T.);
#43673=ADVANCED_FACE('',(#4818),#435,.T.);
#43674=ADVANCED_FACE('',(#4819),#42285,.T.);
#43675=ADVANCED_FACE('',(#4820),#436,.T.);
#43676=ADVANCED_FACE('',(#4821),#2572,.T.);
#43677=ADVANCED_FACE('',(#4822),#437,.T.);
#43678=ADVANCED_FACE('',(#4823),#42286,.T.);
#43679=ADVANCED_FACE('',(#4824),#438,.T.);
#43680=ADVANCED_FACE('',(#4825),#2573,.T.);
#43681=ADVANCED_FACE('',(#4826),#439,.T.);
#43682=ADVANCED_FACE('',(#4827),#42287,.T.);
#43683=ADVANCED_FACE('',(#4828),#2574,.T.);
#43684=ADVANCED_FACE('',(#4829),#2575,.T.);
#43685=ADVANCED_FACE('',(#4830),#440,.T.);
#43686=ADVANCED_FACE('',(#4831),#42288,.T.);
#43687=ADVANCED_FACE('',(#4832),#441,.T.);
#43688=ADVANCED_FACE('',(#4833),#2576,.T.);
#43689=ADVANCED_FACE('',(#4834),#2577,.T.);
#43690=ADVANCED_FACE('',(#4835),#42289,.T.);
#43691=ADVANCED_FACE('',(#4836),#42290,.T.);
#43692=ADVANCED_FACE('',(#4837),#2578,.T.);
#43693=ADVANCED_FACE('',(#4838),#2579,.T.);
#43694=ADVANCED_FACE('',(#4839),#42291,.T.);
#43695=ADVANCED_FACE('',(#4840),#442,.T.);
#43696=ADVANCED_FACE('',(#4841),#2580,.T.);
#43697=ADVANCED_FACE('',(#4842),#42292,.T.);
#43698=ADVANCED_FACE('',(#4843),#2581,.T.);
#43699=ADVANCED_FACE('',(#4844),#42293,.T.);
#43700=ADVANCED_FACE('',(#4845),#443,.T.);
#43701=ADVANCED_FACE('',(#4846),#2582,.T.);
#43702=ADVANCED_FACE('',(#4847),#444,.T.);
#43703=ADVANCED_FACE('',(#4848),#42294,.T.);
#43704=ADVANCED_FACE('',(#4849),#445,.T.);
#43705=ADVANCED_FACE('',(#4850),#2583,.T.);
#43706=ADVANCED_FACE('',(#4851),#446,.T.);
#43707=ADVANCED_FACE('',(#4852),#42295,.T.);
#43708=ADVANCED_FACE('',(#4853),#447,.T.);
#43709=ADVANCED_FACE('',(#4854),#2584,.T.);
#43710=ADVANCED_FACE('',(#4855),#448,.T.);
#43711=ADVANCED_FACE('',(#4856),#42296,.T.);
#43712=ADVANCED_FACE('',(#4857),#2585,.T.);
#43713=ADVANCED_FACE('',(#4858),#2586,.T.);
#43714=ADVANCED_FACE('',(#4859),#449,.T.);
#43715=ADVANCED_FACE('',(#4860),#42297,.T.);
#43716=ADVANCED_FACE('',(#4861),#450,.T.);
#43717=ADVANCED_FACE('',(#4862),#2587,.T.);
#43718=ADVANCED_FACE('',(#4863),#451,.T.);
#43719=ADVANCED_FACE('',(#4864),#42298,.T.);
#43720=ADVANCED_FACE('',(#4865),#42299,.T.);
#43721=ADVANCED_FACE('',(#4866),#2588,.T.);
#43722=ADVANCED_FACE('',(#4867),#2589,.T.);
#43723=ADVANCED_FACE('',(#4868),#42300,.T.);
#43724=ADVANCED_FACE('',(#4869),#452,.T.);
#43725=ADVANCED_FACE('',(#4870),#2590,.T.);
#43726=ADVANCED_FACE('',(#4871),#42301,.T.);
#43727=ADVANCED_FACE('',(#4872),#2591,.T.);
#43728=ADVANCED_FACE('',(#4873),#42302,.T.);
#43729=ADVANCED_FACE('',(#4874),#453,.T.);
#43730=ADVANCED_FACE('',(#4875),#2592,.T.);
#43731=ADVANCED_FACE('',(#4876),#454,.T.);
#43732=ADVANCED_FACE('',(#4877),#42303,.T.);
#43733=ADVANCED_FACE('',(#4878),#455,.T.);
#43734=ADVANCED_FACE('',(#4879),#2593,.T.);
#43735=ADVANCED_FACE('',(#4880),#456,.T.);
#43736=ADVANCED_FACE('',(#4881),#42304,.T.);
#43737=ADVANCED_FACE('',(#4882),#457,.T.);
#43738=ADVANCED_FACE('',(#4883),#2594,.T.);
#43739=ADVANCED_FACE('',(#4884),#458,.T.);
#43740=ADVANCED_FACE('',(#4885),#42305,.T.);
#43741=ADVANCED_FACE('',(#4886),#2595,.T.);
#43742=ADVANCED_FACE('',(#4887),#2596,.T.);
#43743=ADVANCED_FACE('',(#4888),#459,.T.);
#43744=ADVANCED_FACE('',(#4889),#42306,.T.);
#43745=ADVANCED_FACE('',(#4890),#460,.T.);
#43746=ADVANCED_FACE('',(#4891),#2597,.T.);
#43747=ADVANCED_FACE('',(#4892),#461,.T.);
#43748=ADVANCED_FACE('',(#4893),#42307,.T.);
#43749=ADVANCED_FACE('',(#4894),#42308,.T.);
#43750=ADVANCED_FACE('',(#4895),#2598,.T.);
#43751=ADVANCED_FACE('',(#4896),#2599,.T.);
#43752=ADVANCED_FACE('',(#4897),#42309,.T.);
#43753=ADVANCED_FACE('',(#4898),#462,.T.);
#43754=ADVANCED_FACE('',(#4899),#2600,.T.);
#43755=ADVANCED_FACE('',(#4900),#42310,.T.);
#43756=ADVANCED_FACE('',(#4901),#2601,.T.);
#43757=ADVANCED_FACE('',(#4902),#42311,.T.);
#43758=ADVANCED_FACE('',(#4903),#463,.T.);
#43759=ADVANCED_FACE('',(#4904),#2602,.T.);
#43760=ADVANCED_FACE('',(#4905),#464,.T.);
#43761=ADVANCED_FACE('',(#4906),#42312,.T.);
#43762=ADVANCED_FACE('',(#4907),#465,.T.);
#43763=ADVANCED_FACE('',(#4908),#2603,.T.);
#43764=ADVANCED_FACE('',(#4909),#466,.T.);
#43765=ADVANCED_FACE('',(#4910),#42313,.T.);
#43766=ADVANCED_FACE('',(#4911),#467,.T.);
#43767=ADVANCED_FACE('',(#4912),#2604,.T.);
#43768=ADVANCED_FACE('',(#4913),#468,.T.);
#43769=ADVANCED_FACE('',(#4914),#42314,.T.);
#43770=ADVANCED_FACE('',(#4915),#2605,.T.);
#43771=ADVANCED_FACE('',(#4916),#2606,.T.);
#43772=ADVANCED_FACE('',(#4917),#469,.T.);
#43773=ADVANCED_FACE('',(#4918),#42315,.T.);
#43774=ADVANCED_FACE('',(#4919),#470,.T.);
#43775=ADVANCED_FACE('',(#4920),#2607,.T.);
#43776=ADVANCED_FACE('',(#4921),#471,.T.);
#43777=ADVANCED_FACE('',(#4922),#42316,.T.);
#43778=ADVANCED_FACE('',(#4923),#42317,.T.);
#43779=ADVANCED_FACE('',(#4924),#2608,.T.);
#43780=ADVANCED_FACE('',(#4925),#2609,.T.);
#43781=ADVANCED_FACE('',(#4926),#42318,.T.);
#43782=ADVANCED_FACE('',(#4927),#472,.T.);
#43783=ADVANCED_FACE('',(#4928),#2610,.T.);
#43784=ADVANCED_FACE('',(#4929),#42319,.T.);
#43785=ADVANCED_FACE('',(#4930),#2611,.T.);
#43786=ADVANCED_FACE('',(#4931),#42320,.T.);
#43787=ADVANCED_FACE('',(#4932),#473,.T.);
#43788=ADVANCED_FACE('',(#4933),#2612,.T.);
#43789=ADVANCED_FACE('',(#4934),#474,.T.);
#43790=ADVANCED_FACE('',(#4935),#42321,.T.);
#43791=ADVANCED_FACE('',(#4936),#475,.T.);
#43792=ADVANCED_FACE('',(#4937),#2613,.T.);
#43793=ADVANCED_FACE('',(#4938),#476,.T.);
#43794=ADVANCED_FACE('',(#4939),#42322,.T.);
#43795=ADVANCED_FACE('',(#4940),#477,.T.);
#43796=ADVANCED_FACE('',(#4941),#2614,.T.);
#43797=ADVANCED_FACE('',(#4942),#478,.T.);
#43798=ADVANCED_FACE('',(#4943),#42323,.T.);
#43799=ADVANCED_FACE('',(#4944),#2615,.T.);
#43800=ADVANCED_FACE('',(#4945),#2616,.T.);
#43801=ADVANCED_FACE('',(#4946),#479,.T.);
#43802=ADVANCED_FACE('',(#4947),#42324,.T.);
#43803=ADVANCED_FACE('',(#4948),#480,.T.);
#43804=ADVANCED_FACE('',(#4949),#2617,.T.);
#43805=ADVANCED_FACE('',(#4950),#481,.T.);
#43806=ADVANCED_FACE('',(#4951),#42325,.T.);
#43807=ADVANCED_FACE('',(#4952),#42326,.T.);
#43808=ADVANCED_FACE('',(#4953),#2618,.T.);
#43809=ADVANCED_FACE('',(#4954),#2619,.T.);
#43810=ADVANCED_FACE('',(#4955),#42327,.T.);
#43811=ADVANCED_FACE('',(#4956),#482,.T.);
#43812=ADVANCED_FACE('',(#4957),#2620,.T.);
#43813=ADVANCED_FACE('',(#4958),#42328,.T.);
#43814=ADVANCED_FACE('',(#4959),#2621,.T.);
#43815=ADVANCED_FACE('',(#4960),#42329,.T.);
#43816=ADVANCED_FACE('',(#4961),#483,.T.);
#43817=ADVANCED_FACE('',(#4962),#2622,.T.);
#43818=ADVANCED_FACE('',(#4963),#484,.T.);
#43819=ADVANCED_FACE('',(#4964),#42330,.T.);
#43820=ADVANCED_FACE('',(#4965),#485,.T.);
#43821=ADVANCED_FACE('',(#4966),#2623,.T.);
#43822=ADVANCED_FACE('',(#4967),#486,.T.);
#43823=ADVANCED_FACE('',(#4968),#42331,.T.);
#43824=ADVANCED_FACE('',(#4969),#487,.T.);
#43825=ADVANCED_FACE('',(#4970),#2624,.T.);
#43826=ADVANCED_FACE('',(#4971),#488,.T.);
#43827=ADVANCED_FACE('',(#4972),#42332,.T.);
#43828=ADVANCED_FACE('',(#4973),#2625,.T.);
#43829=ADVANCED_FACE('',(#4974),#2626,.T.);
#43830=ADVANCED_FACE('',(#4975),#489,.T.);
#43831=ADVANCED_FACE('',(#4976),#42333,.T.);
#43832=ADVANCED_FACE('',(#4977),#490,.T.);
#43833=ADVANCED_FACE('',(#4978),#2627,.T.);
#43834=ADVANCED_FACE('',(#4979),#491,.T.);
#43835=ADVANCED_FACE('',(#4980),#42334,.T.);
#43836=ADVANCED_FACE('',(#4981),#42335,.T.);
#43837=ADVANCED_FACE('',(#4982),#2628,.T.);
#43838=ADVANCED_FACE('',(#4983),#2629,.T.);
#43839=ADVANCED_FACE('',(#4984),#42336,.T.);
#43840=ADVANCED_FACE('',(#4985),#492,.T.);
#43841=ADVANCED_FACE('',(#4986),#2630,.T.);
#43842=ADVANCED_FACE('',(#4987),#42337,.T.);
#43843=ADVANCED_FACE('',(#4988),#2631,.T.);
#43844=ADVANCED_FACE('',(#4989),#42338,.T.);
#43845=ADVANCED_FACE('',(#4990),#493,.T.);
#43846=ADVANCED_FACE('',(#4991),#2632,.T.);
#43847=ADVANCED_FACE('',(#4992),#494,.T.);
#43848=ADVANCED_FACE('',(#4993),#42339,.T.);
#43849=ADVANCED_FACE('',(#4994),#495,.T.);
#43850=ADVANCED_FACE('',(#4995),#2633,.T.);
#43851=ADVANCED_FACE('',(#4996),#496,.T.);
#43852=ADVANCED_FACE('',(#4997),#42340,.T.);
#43853=ADVANCED_FACE('',(#4998),#497,.T.);
#43854=ADVANCED_FACE('',(#4999),#2634,.T.);
#43855=ADVANCED_FACE('',(#5000),#498,.T.);
#43856=ADVANCED_FACE('',(#5001),#42341,.T.);
#43857=ADVANCED_FACE('',(#5002),#2635,.T.);
#43858=ADVANCED_FACE('',(#5003),#2636,.T.);
#43859=ADVANCED_FACE('',(#5004),#499,.T.);
#43860=ADVANCED_FACE('',(#5005),#42342,.T.);
#43861=ADVANCED_FACE('',(#5006),#500,.T.);
#43862=ADVANCED_FACE('',(#5007),#2637,.T.);
#43863=ADVANCED_FACE('',(#5008),#501,.T.);
#43864=ADVANCED_FACE('',(#5009),#42343,.T.);
#43865=ADVANCED_FACE('',(#5010),#42344,.T.);
#43866=ADVANCED_FACE('',(#5011),#2638,.T.);
#43867=ADVANCED_FACE('',(#5012),#2639,.T.);
#43868=ADVANCED_FACE('',(#5013),#42345,.T.);
#43869=ADVANCED_FACE('',(#5014),#502,.T.);
#43870=ADVANCED_FACE('',(#5015),#2640,.T.);
#43871=ADVANCED_FACE('',(#5016),#42346,.T.);
#43872=ADVANCED_FACE('',(#5017),#2641,.T.);
#43873=ADVANCED_FACE('',(#5018),#42347,.T.);
#43874=ADVANCED_FACE('',(#5019),#503,.T.);
#43875=ADVANCED_FACE('',(#5020),#2642,.T.);
#43876=ADVANCED_FACE('',(#5021),#504,.T.);
#43877=ADVANCED_FACE('',(#5022),#42348,.T.);
#43878=ADVANCED_FACE('',(#5023),#505,.T.);
#43879=ADVANCED_FACE('',(#5024),#2643,.T.);
#43880=ADVANCED_FACE('',(#5025),#506,.T.);
#43881=ADVANCED_FACE('',(#5026),#42349,.T.);
#43882=ADVANCED_FACE('',(#5027),#507,.T.);
#43883=ADVANCED_FACE('',(#5028),#2644,.T.);
#43884=ADVANCED_FACE('',(#5029),#508,.T.);
#43885=ADVANCED_FACE('',(#5030),#42350,.T.);
#43886=ADVANCED_FACE('',(#5031),#2645,.T.);
#43887=ADVANCED_FACE('',(#5032),#2646,.T.);
#43888=ADVANCED_FACE('',(#5033),#509,.T.);
#43889=ADVANCED_FACE('',(#5034),#42351,.T.);
#43890=ADVANCED_FACE('',(#5035),#510,.T.);
#43891=ADVANCED_FACE('',(#5036),#2647,.T.);
#43892=ADVANCED_FACE('',(#5037),#511,.T.);
#43893=ADVANCED_FACE('',(#5038),#42352,.T.);
#43894=ADVANCED_FACE('',(#5039),#42353,.T.);
#43895=ADVANCED_FACE('',(#5040),#2648,.T.);
#43896=ADVANCED_FACE('',(#5041),#2649,.T.);
#43897=ADVANCED_FACE('',(#5042),#42354,.T.);
#43898=ADVANCED_FACE('',(#5043),#512,.T.);
#43899=ADVANCED_FACE('',(#5044),#2650,.T.);
#43900=ADVANCED_FACE('',(#5045),#42355,.T.);
#43901=ADVANCED_FACE('',(#5046),#2651,.T.);
#43902=ADVANCED_FACE('',(#5047),#42356,.T.);
#43903=ADVANCED_FACE('',(#5048),#513,.T.);
#43904=ADVANCED_FACE('',(#5049),#2652,.T.);
#43905=ADVANCED_FACE('',(#5050),#514,.T.);
#43906=ADVANCED_FACE('',(#5051),#42357,.T.);
#43907=ADVANCED_FACE('',(#5052),#515,.T.);
#43908=ADVANCED_FACE('',(#5053),#2653,.T.);
#43909=ADVANCED_FACE('',(#5054),#516,.T.);
#43910=ADVANCED_FACE('',(#5055),#42358,.T.);
#43911=ADVANCED_FACE('',(#5056),#517,.T.);
#43912=ADVANCED_FACE('',(#5057),#2654,.T.);
#43913=ADVANCED_FACE('',(#5058),#518,.T.);
#43914=ADVANCED_FACE('',(#5059),#42359,.T.);
#43915=ADVANCED_FACE('',(#5060),#2655,.T.);
#43916=ADVANCED_FACE('',(#5061),#2656,.T.);
#43917=ADVANCED_FACE('',(#5062),#519,.T.);
#43918=ADVANCED_FACE('',(#5063),#42360,.T.);
#43919=ADVANCED_FACE('',(#5064),#520,.T.);
#43920=ADVANCED_FACE('',(#5065),#2657,.T.);
#43921=ADVANCED_FACE('',(#5066),#521,.T.);
#43922=ADVANCED_FACE('',(#5067),#42361,.T.);
#43923=ADVANCED_FACE('',(#5068),#42362,.T.);
#43924=ADVANCED_FACE('',(#5069),#42363,.T.);
#43925=ADVANCED_FACE('',(#5070),#2658,.T.);
#43926=ADVANCED_FACE('',(#5071),#2659,.T.);
#43927=ADVANCED_FACE('',(#5072),#522,.T.);
#43928=ADVANCED_FACE('',(#5073),#2660,.T.);
#43929=ADVANCED_FACE('',(#5074),#42364,.T.);
#43930=ADVANCED_FACE('',(#5075),#2661,.T.);
#43931=ADVANCED_FACE('',(#5076),#42365,.T.);
#43932=ADVANCED_FACE('',(#5077),#523,.T.);
#43933=ADVANCED_FACE('',(#5078),#2662,.T.);
#43934=ADVANCED_FACE('',(#5079),#524,.T.);
#43935=ADVANCED_FACE('',(#5080),#42366,.T.);
#43936=ADVANCED_FACE('',(#5081),#525,.T.);
#43937=ADVANCED_FACE('',(#5082),#2663,.T.);
#43938=ADVANCED_FACE('',(#5083),#526,.T.);
#43939=ADVANCED_FACE('',(#5084),#42367,.T.);
#43940=ADVANCED_FACE('',(#5085),#527,.T.);
#43941=ADVANCED_FACE('',(#5086),#2664,.T.);
#43942=ADVANCED_FACE('',(#5087),#528,.T.);
#43943=ADVANCED_FACE('',(#5088),#42368,.T.);
#43944=ADVANCED_FACE('',(#5089),#2665,.T.);
#43945=ADVANCED_FACE('',(#5090),#2666,.T.);
#43946=ADVANCED_FACE('',(#5091),#529,.T.);
#43947=ADVANCED_FACE('',(#5092),#42369,.T.);
#43948=ADVANCED_FACE('',(#5093),#530,.T.);
#43949=ADVANCED_FACE('',(#5094),#2667,.T.);
#43950=ADVANCED_FACE('',(#5095),#531,.T.);
#43951=ADVANCED_FACE('',(#5096),#42370,.T.);
#43952=ADVANCED_FACE('',(#5097),#42371,.T.);
#43953=ADVANCED_FACE('',(#5098),#42372,.T.);
#43954=ADVANCED_FACE('',(#5099),#42373,.T.);
#43955=ADVANCED_FACE('',(#5100),#2668,.T.);
#43956=ADVANCED_FACE('',(#5101),#2669,.T.);
#43957=ADVANCED_FACE('',(#5102),#532,.T.);
#43958=ADVANCED_FACE('',(#5103),#2670,.T.);
#43959=ADVANCED_FACE('',(#5104),#42374,.T.);
#43960=ADVANCED_FACE('',(#5105),#2671,.T.);
#43961=ADVANCED_FACE('',(#5106),#533,.T.);
#43962=ADVANCED_FACE('',(#5107),#2672,.T.);
#43963=ADVANCED_FACE('',(#5108),#2673,.T.);
#43964=ADVANCED_FACE('',(#5109),#42375,.T.);
#43965=ADVANCED_FACE('',(#5110),#534,.T.);
#43966=ADVANCED_FACE('',(#5111),#2674,.T.);
#43967=ADVANCED_FACE('',(#5112),#535,.T.);
#43968=ADVANCED_FACE('',(#5113),#42376,.T.);
#43969=ADVANCED_FACE('',(#5114),#536,.T.);
#43970=ADVANCED_FACE('',(#5115),#2675,.T.);
#43971=ADVANCED_FACE('',(#5116),#537,.T.);
#43972=ADVANCED_FACE('',(#5117),#42377,.T.);
#43973=ADVANCED_FACE('',(#5118),#2676,.T.);
#43974=ADVANCED_FACE('',(#5119),#2677,.T.);
#43975=ADVANCED_FACE('',(#5120),#538,.T.);
#43976=ADVANCED_FACE('',(#5121),#42378,.T.);
#43977=ADVANCED_FACE('',(#5122),#539,.T.);
#43978=ADVANCED_FACE('',(#5123),#2678,.T.);
#43979=ADVANCED_FACE('',(#5124),#540,.T.);
#43980=ADVANCED_FACE('',(#5125),#42379,.T.);
#43981=ADVANCED_FACE('',(#5126),#42380,.T.);
#43982=ADVANCED_FACE('',(#5127),#42381,.T.);
#43983=ADVANCED_FACE('',(#5128),#42382,.T.);
#43984=ADVANCED_FACE('',(#5129),#42383,.T.);
#43985=ADVANCED_FACE('',(#5130),#541,.T.);
#43986=ADVANCED_FACE('',(#5131),#2679,.T.);
#43987=ADVANCED_FACE('',(#5132),#42384,.T.);
#43988=ADVANCED_FACE('',(#5133),#2680,.T.);
#43989=ADVANCED_FACE('',(#5134),#542,.T.);
#43990=ADVANCED_FACE('',(#5135),#2681,.T.);
#43991=ADVANCED_FACE('',(#5136),#543,.T.);
#43992=ADVANCED_FACE('',(#5137),#2682,.T.);
#43993=ADVANCED_FACE('',(#5138),#2683,.T.);
#43994=ADVANCED_FACE('',(#5139),#544,.T.);
#43995=ADVANCED_FACE('',(#5140),#545,.T.);
#43996=ADVANCED_FACE('',(#5141),#2684,.T.);
#43997=ADVANCED_FACE('',(#5142),#42385,.T.);
#43998=ADVANCED_FACE('',(#5143),#546,.T.);
#43999=ADVANCED_FACE('',(#5144),#2685,.T.);
#44000=ADVANCED_FACE('',(#5145),#547,.T.);
#44001=ADVANCED_FACE('',(#5146),#42386,.T.);
#44002=ADVANCED_FACE('',(#5147),#2686,.T.);
#44003=ADVANCED_FACE('',(#5148),#2687,.T.);
#44004=ADVANCED_FACE('',(#5149),#548,.T.);
#44005=ADVANCED_FACE('',(#5150),#42387,.T.);
#44006=ADVANCED_FACE('',(#5151),#549,.T.);
#44007=ADVANCED_FACE('',(#5152),#2688,.T.);
#44008=ADVANCED_FACE('',(#5153),#550,.T.);
#44009=ADVANCED_FACE('',(#5154),#42388,.T.);
#44010=ADVANCED_FACE('',(#5155),#42389,.T.);
#44011=ADVANCED_FACE('',(#5156),#42390,.T.);
#44012=ADVANCED_FACE('',(#5157),#42391,.T.);
#44013=ADVANCED_FACE('',(#5158),#42392,.T.);
#44014=ADVANCED_FACE('',(#5159),#42393,.T.);
#44015=ADVANCED_FACE('',(#5160),#551,.T.);
#44016=ADVANCED_FACE('',(#5161),#2689,.T.);
#44017=ADVANCED_FACE('',(#5162),#2690,.T.);
#44018=ADVANCED_FACE('',(#5163),#552,.T.);
#44019=ADVANCED_FACE('',(#5164),#2691,.T.);
#44020=ADVANCED_FACE('',(#5165),#553,.T.);
#44021=ADVANCED_FACE('',(#5166),#554,.T.);
#44022=ADVANCED_FACE('',(#5167),#2692,.T.);
#44023=ADVANCED_FACE('',(#5168),#2693,.T.);
#44024=ADVANCED_FACE('',(#5169),#555,.T.);
#44025=ADVANCED_FACE('',(#5170),#2694,.T.);
#44026=ADVANCED_FACE('',(#5171),#556,.T.);
#44027=ADVANCED_FACE('',(#5172),#2695,.T.);
#44028=ADVANCED_FACE('',(#5173),#42394,.T.);
#44029=ADVANCED_FACE('',(#5174),#2696,.T.);
#44030=ADVANCED_FACE('',(#5175),#42395,.T.);
#44031=ADVANCED_FACE('',(#5176),#2697,.T.);
#44032=ADVANCED_FACE('',(#5177),#2698,.T.);
#44033=ADVANCED_FACE('',(#5178),#557,.T.);
#44034=ADVANCED_FACE('',(#5179),#42396,.T.);
#44035=ADVANCED_FACE('',(#5180),#558,.T.);
#44036=ADVANCED_FACE('',(#5181),#2699,.T.);
#44037=ADVANCED_FACE('',(#5182),#559,.T.);
#44038=ADVANCED_FACE('',(#5183),#42397,.T.);
#44039=ADVANCED_FACE('',(#5184),#42398,.T.);
#44040=ADVANCED_FACE('',(#5185),#42399,.T.);
#44041=ADVANCED_FACE('',(#5186),#42400,.T.);
#44042=ADVANCED_FACE('',(#5187),#42401,.T.);
#44043=ADVANCED_FACE('',(#5188),#42402,.T.);
#44044=ADVANCED_FACE('',(#5189),#42403,.T.);
#44045=ADVANCED_FACE('',(#5190),#2700,.T.);
#44046=ADVANCED_FACE('',(#5191),#2701,.T.);
#44047=ADVANCED_FACE('',(#5192),#560,.T.);
#44048=ADVANCED_FACE('',(#5193),#561,.T.);
#44049=ADVANCED_FACE('',(#5194),#2702,.T.);
#44050=ADVANCED_FACE('',(#5195),#562,.T.);
#44051=ADVANCED_FACE('',(#5196),#2703,.T.);
#44052=ADVANCED_FACE('',(#5197),#2704,.T.);
#44053=ADVANCED_FACE('',(#5198),#2705,.T.);
#44054=ADVANCED_FACE('',(#5199),#2706,.T.);
#44055=ADVANCED_FACE('',(#5200),#563,.T.);
#44056=ADVANCED_FACE('',(#5201),#564,.T.);
#44057=ADVANCED_FACE('',(#5202),#2707,.T.);
#44058=ADVANCED_FACE('',(#5203),#42404,.T.);
#44059=ADVANCED_FACE('',(#5204),#2708,.T.);
#44060=ADVANCED_FACE('',(#5205),#565,.T.);
#44061=ADVANCED_FACE('',(#5206),#2709,.T.);
#44062=ADVANCED_FACE('',(#5207),#566,.T.);
#44063=ADVANCED_FACE('',(#5208),#42405,.T.);
#44064=ADVANCED_FACE('',(#5209),#567,.T.);
#44065=ADVANCED_FACE('',(#5210),#2710,.T.);
#44066=ADVANCED_FACE('',(#5211),#568,.T.);
#44067=ADVANCED_FACE('',(#5212),#42406,.T.);
#44068=ADVANCED_FACE('',(#5213),#42407,.T.);
#44069=ADVANCED_FACE('',(#5214),#42408,.T.);
#44070=ADVANCED_FACE('',(#5215),#42409,.T.);
#44071=ADVANCED_FACE('',(#5216),#42410,.T.);
#44072=ADVANCED_FACE('',(#5217),#42411,.T.);
#44073=ADVANCED_FACE('',(#5218),#42412,.T.);
#44074=ADVANCED_FACE('',(#5219),#42413,.T.);
#44075=ADVANCED_FACE('',(#5220),#569,.T.);
#44076=ADVANCED_FACE('',(#5221),#2711,.T.);
#44077=ADVANCED_FACE('',(#5222),#2712,.T.);
#44078=ADVANCED_FACE('',(#5223),#570,.T.);
#44079=ADVANCED_FACE('',(#5224),#2713,.T.);
#44080=ADVANCED_FACE('',(#5225),#571,.T.);
#44081=ADVANCED_FACE('',(#5226),#572,.T.);
#44082=ADVANCED_FACE('',(#5227),#2714,.T.);
#44083=ADVANCED_FACE('',(#5228),#2715,.T.);
#44084=ADVANCED_FACE('',(#5229),#573,.T.);
#44085=ADVANCED_FACE('',(#5230),#574,.T.);
#44086=ADVANCED_FACE('',(#5231),#575,.T.);
#44087=ADVANCED_FACE('',(#5232),#2716,.T.);
#44088=ADVANCED_FACE('',(#5233),#42414,.T.);
#44089=ADVANCED_FACE('',(#5234),#576,.T.);
#44090=ADVANCED_FACE('',(#5235),#577,.T.);
#44091=ADVANCED_FACE('',(#5236),#2717,.T.);
#44092=ADVANCED_FACE('',(#5237),#578,.T.);
#44093=ADVANCED_FACE('',(#5238),#579,.T.);
#44094=ADVANCED_FACE('',(#5239),#2718,.T.);
#44095=ADVANCED_FACE('',(#5240),#580,.T.);
#44096=ADVANCED_FACE('',(#5241),#42415,.T.);
#44097=ADVANCED_FACE('',(#5242),#42416,.T.);
#44098=ADVANCED_FACE('',(#5243),#42417,.T.);
#44099=ADVANCED_FACE('',(#5244),#42418,.T.);
#44100=ADVANCED_FACE('',(#5245),#42419,.T.);
#44101=ADVANCED_FACE('',(#5246),#3566,.F.);
#44102=ADVANCED_FACE('',(#5247,#3513),#3567,.F.);
#44103=ADVANCED_FACE('',(#5248),#3568,.T.);
#44104=ADVANCED_FACE('',(#5249),#2719,.T.);
#44105=ADVANCED_FACE('',(#5250),#2720,.T.);
#44106=ADVANCED_FACE('',(#5251),#581,.T.);
#44107=ADVANCED_FACE('',(#5252),#2721,.T.);
#44108=ADVANCED_FACE('',(#5253),#582,.T.);
#44109=ADVANCED_FACE('',(#5254),#2722,.T.);
#44110=ADVANCED_FACE('',(#5255),#2723,.T.);
#44111=ADVANCED_FACE('',(#5256),#2724,.T.);
#44112=ADVANCED_FACE('',(#5257),#583,.T.);
#44113=ADVANCED_FACE('',(#5258),#2725,.T.);
#44114=ADVANCED_FACE('',(#5259),#2726,.T.);
#44115=ADVANCED_FACE('',(#5260),#584,.T.);
#44116=ADVANCED_FACE('',(#5261),#2727,.T.);
#44117=ADVANCED_FACE('',(#5262),#2728,.T.);
#44118=ADVANCED_FACE('',(#5263),#585,.T.);
#44119=ADVANCED_FACE('',(#5264),#42420,.F.);
#44120=ADVANCED_FACE('',(#5265),#42421,.F.);
#44121=ADVANCED_FACE('',(#5266),#2729,.T.);
#44122=ADVANCED_FACE('',(#5267),#2730,.T.);
#44123=ADVANCED_FACE('',(#5268),#586,.T.);
#44124=ADVANCED_FACE('',(#5269),#2731,.T.);
#44125=ADVANCED_FACE('',(#5270),#2732,.T.);
#44126=ADVANCED_FACE('',(#5271),#2733,.T.);
#44127=ADVANCED_FACE('',(#5272),#42422,.F.);
#44128=ADVANCED_FACE('',(#5273),#42423,.F.);
#44129=ADVANCED_FACE('',(#5274),#2734,.T.);
#44130=ADVANCED_FACE('',(#5275),#2735,.T.);
#44131=ADVANCED_FACE('',(#5276),#587,.T.);
#44132=ADVANCED_FACE('',(#5277),#588,.T.);
#44133=ADVANCED_FACE('',(#5278),#2736,.T.);
#44134=ADVANCED_FACE('',(#5279),#2737,.T.);
#44135=ADVANCED_FACE('',(#5280),#2738,.T.);
#44136=ADVANCED_FACE('',(#5281),#2739,.T.);
#44137=ADVANCED_FACE('',(#5282),#589,.T.);
#44138=ADVANCED_FACE('',(#5283),#2740,.T.);
#44139=ADVANCED_FACE('',(#5284),#2741,.T.);
#44140=ADVANCED_FACE('',(#5285),#590,.T.);
#44141=ADVANCED_FACE('',(#5286),#2742,.T.);
#44142=ADVANCED_FACE('',(#5287),#2743,.T.);
#44143=ADVANCED_FACE('',(#5288),#591,.T.);
#44144=ADVANCED_FACE('',(#5289),#2744,.T.);
#44145=ADVANCED_FACE('',(#5290),#2745,.T.);
#44146=ADVANCED_FACE('',(#5291),#2746,.T.);
#44147=ADVANCED_FACE('',(#5292),#592,.T.);
#44148=ADVANCED_FACE('',(#5293),#2747,.T.);
#44149=ADVANCED_FACE('',(#5294),#2748,.T.);
#44150=ADVANCED_FACE('',(#5295),#42424,.F.);
#44151=ADVANCED_FACE('',(#5296),#42425,.F.);
#44152=ADVANCED_FACE('',(#5297),#2749,.T.);
#44153=ADVANCED_FACE('',(#5298),#2750,.T.);
#44154=ADVANCED_FACE('',(#5299),#593,.T.);
#44155=ADVANCED_FACE('',(#5300),#2751,.T.);
#44156=ADVANCED_FACE('',(#5301),#2752,.T.);
#44157=ADVANCED_FACE('',(#5302),#2753,.T.);
#44158=ADVANCED_FACE('',(#5303),#2754,.T.);
#44159=ADVANCED_FACE('',(#5304),#2755,.T.);
#44160=ADVANCED_FACE('',(#5305),#594,.T.);
#44161=ADVANCED_FACE('',(#5306),#2756,.T.);
#44162=ADVANCED_FACE('',(#5307),#2757,.T.);
#44163=ADVANCED_FACE('',(#5308),#595,.T.);
#44164=ADVANCED_FACE('',(#5309),#2758,.T.);
#44165=ADVANCED_FACE('',(#5310),#2759,.T.);
#44166=ADVANCED_FACE('',(#5311),#596,.T.);
#44167=ADVANCED_FACE('',(#5312),#2760,.T.);
#44168=ADVANCED_FACE('',(#5313),#2761,.T.);
#44169=ADVANCED_FACE('',(#5314),#597,.T.);
#44170=ADVANCED_FACE('',(#5315),#2762,.T.);
#44171=ADVANCED_FACE('',(#5316),#598,.T.);
#44172=ADVANCED_FACE('',(#5317),#2763,.T.);
#44173=ADVANCED_FACE('',(#5318),#42426,.F.);
#44174=ADVANCED_FACE('',(#5319),#42427,.F.);
#44175=ADVANCED_FACE('',(#5320),#2764,.T.);
#44176=ADVANCED_FACE('',(#5321),#2765,.T.);
#44177=ADVANCED_FACE('',(#5322),#599,.T.);
#44178=ADVANCED_FACE('',(#5323),#2766,.T.);
#44179=ADVANCED_FACE('',(#5324),#2767,.T.);
#44180=ADVANCED_FACE('',(#5325),#2768,.T.);
#44181=ADVANCED_FACE('',(#5326),#2769,.T.);
#44182=ADVANCED_FACE('',(#5327),#2770,.T.);
#44183=ADVANCED_FACE('',(#5328),#600,.T.);
#44184=ADVANCED_FACE('',(#5329),#2771,.T.);
#44185=ADVANCED_FACE('',(#5330),#2772,.T.);
#44186=ADVANCED_FACE('',(#5331),#601,.T.);
#44187=ADVANCED_FACE('',(#5332),#2773,.T.);
#44188=ADVANCED_FACE('',(#5333),#2774,.T.);
#44189=ADVANCED_FACE('',(#5334),#602,.T.);
#44190=ADVANCED_FACE('',(#5335),#2775,.T.);
#44191=ADVANCED_FACE('',(#5336),#603,.T.);
#44192=ADVANCED_FACE('',(#5337),#2776,.T.);
#44193=ADVANCED_FACE('',(#5338),#604,.T.);
#44194=ADVANCED_FACE('',(#5339),#2777,.T.);
#44195=ADVANCED_FACE('',(#5340),#2778,.T.);
#44196=ADVANCED_FACE('',(#5341),#42428,.F.);
#44197=ADVANCED_FACE('',(#5342),#42429,.F.);
#44198=ADVANCED_FACE('',(#5343),#2779,.T.);
#44199=ADVANCED_FACE('',(#5344),#2780,.T.);
#44200=ADVANCED_FACE('',(#5345),#605,.T.);
#44201=ADVANCED_FACE('',(#5346),#2781,.T.);
#44202=ADVANCED_FACE('',(#5347),#2782,.T.);
#44203=ADVANCED_FACE('',(#5348),#2783,.T.);
#44204=ADVANCED_FACE('',(#5349),#2784,.T.);
#44205=ADVANCED_FACE('',(#5350),#2785,.T.);
#44206=ADVANCED_FACE('',(#5351),#606,.T.);
#44207=ADVANCED_FACE('',(#5352),#2786,.T.);
#44208=ADVANCED_FACE('',(#5353),#607,.T.);
#44209=ADVANCED_FACE('',(#5354),#2787,.T.);
#44210=ADVANCED_FACE('',(#5355),#2788,.T.);
#44211=ADVANCED_FACE('',(#5356),#608,.T.);
#44212=ADVANCED_FACE('',(#5357),#2789,.T.);
#44213=ADVANCED_FACE('',(#5358),#2790,.T.);
#44214=ADVANCED_FACE('',(#5359),#2791,.T.);
#44215=ADVANCED_FACE('',(#5360),#609,.T.);
#44216=ADVANCED_FACE('',(#5361),#610,.T.);
#44217=ADVANCED_FACE('',(#5362),#2792,.T.);
#44218=ADVANCED_FACE('',(#5363),#2793,.T.);
#44219=ADVANCED_FACE('',(#5364),#42430,.F.);
#44220=ADVANCED_FACE('',(#5365),#42431,.F.);
#44221=ADVANCED_FACE('',(#5366),#2794,.T.);
#44222=ADVANCED_FACE('',(#5367),#2795,.T.);
#44223=ADVANCED_FACE('',(#5368),#611,.T.);
#44224=ADVANCED_FACE('',(#5369),#2796,.T.);
#44225=ADVANCED_FACE('',(#5370),#2797,.T.);
#44226=ADVANCED_FACE('',(#5371),#2798,.T.);
#44227=ADVANCED_FACE('',(#5372),#2799,.T.);
#44228=ADVANCED_FACE('',(#5373),#2800,.T.);
#44229=ADVANCED_FACE('',(#5374),#612,.T.);
#44230=ADVANCED_FACE('',(#5375),#2801,.T.);
#44231=ADVANCED_FACE('',(#5376),#613,.T.);
#44232=ADVANCED_FACE('',(#5377),#2802,.T.);
#44233=ADVANCED_FACE('',(#5378),#2803,.T.);
#44234=ADVANCED_FACE('',(#5379),#2804,.T.);
#44235=ADVANCED_FACE('',(#5380),#614,.T.);
#44236=ADVANCED_FACE('',(#5381),#2805,.T.);
#44237=ADVANCED_FACE('',(#5382),#2806,.T.);
#44238=ADVANCED_FACE('',(#5383),#615,.T.);
#44239=ADVANCED_FACE('',(#5384),#616,.T.);
#44240=ADVANCED_FACE('',(#5385),#2807,.T.);
#44241=ADVANCED_FACE('',(#5386),#2808,.T.);
#44242=ADVANCED_FACE('',(#5387),#42432,.F.);
#44243=ADVANCED_FACE('',(#5388),#42433,.F.);
#44244=ADVANCED_FACE('',(#5389),#2809,.T.);
#44245=ADVANCED_FACE('',(#5390),#2810,.T.);
#44246=ADVANCED_FACE('',(#5391),#617,.T.);
#44247=ADVANCED_FACE('',(#5392),#2811,.T.);
#44248=ADVANCED_FACE('',(#5393),#2812,.T.);
#44249=ADVANCED_FACE('',(#5394),#2813,.T.);
#44250=ADVANCED_FACE('',(#5395),#2814,.T.);
#44251=ADVANCED_FACE('',(#5396),#2815,.T.);
#44252=ADVANCED_FACE('',(#5397),#618,.T.);
#44253=ADVANCED_FACE('',(#5398),#2816,.T.);
#44254=ADVANCED_FACE('',(#5399),#619,.T.);
#44255=ADVANCED_FACE('',(#5400),#2817,.T.);
#44256=ADVANCED_FACE('',(#5401),#2818,.T.);
#44257=ADVANCED_FACE('',(#5402),#2819,.T.);
#44258=ADVANCED_FACE('',(#5403),#620,.T.);
#44259=ADVANCED_FACE('',(#5404),#2820,.T.);
#44260=ADVANCED_FACE('',(#5405),#2821,.T.);
#44261=ADVANCED_FACE('',(#5406),#621,.T.);
#44262=ADVANCED_FACE('',(#5407),#622,.T.);
#44263=ADVANCED_FACE('',(#5408),#2822,.T.);
#44264=ADVANCED_FACE('',(#5409),#2823,.T.);
#44265=ADVANCED_FACE('',(#5410),#42434,.F.);
#44266=ADVANCED_FACE('',(#5411),#42435,.F.);
#44267=ADVANCED_FACE('',(#5412),#2824,.T.);
#44268=ADVANCED_FACE('',(#5413),#2825,.T.);
#44269=ADVANCED_FACE('',(#5414),#623,.T.);
#44270=ADVANCED_FACE('',(#5415),#2826,.T.);
#44271=ADVANCED_FACE('',(#5416),#2827,.T.);
#44272=ADVANCED_FACE('',(#5417),#2828,.T.);
#44273=ADVANCED_FACE('',(#5418),#2829,.T.);
#44274=ADVANCED_FACE('',(#5419),#2830,.T.);
#44275=ADVANCED_FACE('',(#5420),#624,.T.);
#44276=ADVANCED_FACE('',(#5421),#2831,.T.);
#44277=ADVANCED_FACE('',(#5422),#625,.T.);
#44278=ADVANCED_FACE('',(#5423),#2832,.T.);
#44279=ADVANCED_FACE('',(#5424),#2833,.T.);
#44280=ADVANCED_FACE('',(#5425),#2834,.T.);
#44281=ADVANCED_FACE('',(#5426),#626,.T.);
#44282=ADVANCED_FACE('',(#5427),#2835,.T.);
#44283=ADVANCED_FACE('',(#5428),#2836,.T.);
#44284=ADVANCED_FACE('',(#5429),#627,.T.);
#44285=ADVANCED_FACE('',(#5430),#628,.T.);
#44286=ADVANCED_FACE('',(#5431),#2837,.T.);
#44287=ADVANCED_FACE('',(#5432),#2838,.T.);
#44288=ADVANCED_FACE('',(#5433),#42436,.F.);
#44289=ADVANCED_FACE('',(#5434),#42437,.F.);
#44290=ADVANCED_FACE('',(#5435),#2839,.T.);
#44291=ADVANCED_FACE('',(#5436),#2840,.T.);
#44292=ADVANCED_FACE('',(#5437),#629,.T.);
#44293=ADVANCED_FACE('',(#5438),#2841,.T.);
#44294=ADVANCED_FACE('',(#5439),#2842,.T.);
#44295=ADVANCED_FACE('',(#5440),#2843,.T.);
#44296=ADVANCED_FACE('',(#5441),#2844,.T.);
#44297=ADVANCED_FACE('',(#5442),#2845,.T.);
#44298=ADVANCED_FACE('',(#5443),#630,.T.);
#44299=ADVANCED_FACE('',(#5444),#2846,.T.);
#44300=ADVANCED_FACE('',(#5445),#631,.T.);
#44301=ADVANCED_FACE('',(#5446),#2847,.T.);
#44302=ADVANCED_FACE('',(#5447),#2848,.T.);
#44303=ADVANCED_FACE('',(#5448),#2849,.T.);
#44304=ADVANCED_FACE('',(#5449),#632,.T.);
#44305=ADVANCED_FACE('',(#5450),#2850,.T.);
#44306=ADVANCED_FACE('',(#5451),#2851,.T.);
#44307=ADVANCED_FACE('',(#5452),#633,.T.);
#44308=ADVANCED_FACE('',(#5453),#634,.T.);
#44309=ADVANCED_FACE('',(#5454),#2852,.T.);
#44310=ADVANCED_FACE('',(#5455),#2853,.T.);
#44311=ADVANCED_FACE('',(#5456),#42438,.F.);
#44312=ADVANCED_FACE('',(#5457),#42439,.F.);
#44313=ADVANCED_FACE('',(#5458),#2854,.T.);
#44314=ADVANCED_FACE('',(#5459),#2855,.T.);
#44315=ADVANCED_FACE('',(#5460),#635,.T.);
#44316=ADVANCED_FACE('',(#5461),#2856,.T.);
#44317=ADVANCED_FACE('',(#5462),#2857,.T.);
#44318=ADVANCED_FACE('',(#5463),#2858,.T.);
#44319=ADVANCED_FACE('',(#5464),#2859,.T.);
#44320=ADVANCED_FACE('',(#5465),#2860,.T.);
#44321=ADVANCED_FACE('',(#5466),#636,.T.);
#44322=ADVANCED_FACE('',(#5467),#2861,.T.);
#44323=ADVANCED_FACE('',(#5468),#637,.T.);
#44324=ADVANCED_FACE('',(#5469),#2862,.T.);
#44325=ADVANCED_FACE('',(#5470),#2863,.T.);
#44326=ADVANCED_FACE('',(#5471),#2864,.T.);
#44327=ADVANCED_FACE('',(#5472),#638,.T.);
#44328=ADVANCED_FACE('',(#5473),#2865,.T.);
#44329=ADVANCED_FACE('',(#5474),#2866,.T.);
#44330=ADVANCED_FACE('',(#5475),#639,.T.);
#44331=ADVANCED_FACE('',(#5476),#640,.T.);
#44332=ADVANCED_FACE('',(#5477),#2867,.T.);
#44333=ADVANCED_FACE('',(#5478),#2868,.T.);
#44334=ADVANCED_FACE('',(#5479),#42440,.F.);
#44335=ADVANCED_FACE('',(#5480),#42441,.F.);
#44336=ADVANCED_FACE('',(#5481),#2869,.T.);
#44337=ADVANCED_FACE('',(#5482),#2870,.T.);
#44338=ADVANCED_FACE('',(#5483),#641,.T.);
#44339=ADVANCED_FACE('',(#5484),#2871,.T.);
#44340=ADVANCED_FACE('',(#5485),#2872,.T.);
#44341=ADVANCED_FACE('',(#5486),#2873,.T.);
#44342=ADVANCED_FACE('',(#5487),#2874,.T.);
#44343=ADVANCED_FACE('',(#5488),#2875,.T.);
#44344=ADVANCED_FACE('',(#5489),#642,.T.);
#44345=ADVANCED_FACE('',(#5490),#2876,.T.);
#44346=ADVANCED_FACE('',(#5491),#643,.T.);
#44347=ADVANCED_FACE('',(#5492),#2877,.T.);
#44348=ADVANCED_FACE('',(#5493),#2878,.T.);
#44349=ADVANCED_FACE('',(#5494),#2879,.T.);
#44350=ADVANCED_FACE('',(#5495),#644,.T.);
#44351=ADVANCED_FACE('',(#5496),#2880,.T.);
#44352=ADVANCED_FACE('',(#5497),#2881,.T.);
#44353=ADVANCED_FACE('',(#5498),#645,.T.);
#44354=ADVANCED_FACE('',(#5499),#646,.T.);
#44355=ADVANCED_FACE('',(#5500),#2882,.T.);
#44356=ADVANCED_FACE('',(#5501),#2883,.T.);
#44357=ADVANCED_FACE('',(#5502),#42442,.F.);
#44358=ADVANCED_FACE('',(#5503),#42443,.F.);
#44359=ADVANCED_FACE('',(#5504),#2884,.T.);
#44360=ADVANCED_FACE('',(#5505),#2885,.T.);
#44361=ADVANCED_FACE('',(#5506),#647,.T.);
#44362=ADVANCED_FACE('',(#5507),#2886,.T.);
#44363=ADVANCED_FACE('',(#5508),#2887,.T.);
#44364=ADVANCED_FACE('',(#5509),#2888,.T.);
#44365=ADVANCED_FACE('',(#5510),#2889,.T.);
#44366=ADVANCED_FACE('',(#5511),#2890,.T.);
#44367=ADVANCED_FACE('',(#5512),#648,.T.);
#44368=ADVANCED_FACE('',(#5513),#2891,.T.);
#44369=ADVANCED_FACE('',(#5514),#649,.T.);
#44370=ADVANCED_FACE('',(#5515),#2892,.T.);
#44371=ADVANCED_FACE('',(#5516),#2893,.T.);
#44372=ADVANCED_FACE('',(#5517),#2894,.T.);
#44373=ADVANCED_FACE('',(#5518),#650,.T.);
#44374=ADVANCED_FACE('',(#5519),#2895,.T.);
#44375=ADVANCED_FACE('',(#5520),#2896,.T.);
#44376=ADVANCED_FACE('',(#5521),#651,.T.);
#44377=ADVANCED_FACE('',(#5522),#652,.T.);
#44378=ADVANCED_FACE('',(#5523),#2897,.T.);
#44379=ADVANCED_FACE('',(#5524),#2898,.T.);
#44380=ADVANCED_FACE('',(#5525),#42444,.F.);
#44381=ADVANCED_FACE('',(#5526),#42445,.F.);
#44382=ADVANCED_FACE('',(#5527),#2899,.T.);
#44383=ADVANCED_FACE('',(#5528),#2900,.T.);
#44384=ADVANCED_FACE('',(#5529),#653,.T.);
#44385=ADVANCED_FACE('',(#5530),#2901,.T.);
#44386=ADVANCED_FACE('',(#5531),#2902,.T.);
#44387=ADVANCED_FACE('',(#5532),#2903,.T.);
#44388=ADVANCED_FACE('',(#5533),#2904,.T.);
#44389=ADVANCED_FACE('',(#5534),#2905,.T.);
#44390=ADVANCED_FACE('',(#5535),#654,.T.);
#44391=ADVANCED_FACE('',(#5536),#2906,.T.);
#44392=ADVANCED_FACE('',(#5537),#655,.T.);
#44393=ADVANCED_FACE('',(#5538),#2907,.T.);
#44394=ADVANCED_FACE('',(#5539),#2908,.T.);
#44395=ADVANCED_FACE('',(#5540),#2909,.T.);
#44396=ADVANCED_FACE('',(#5541),#656,.T.);
#44397=ADVANCED_FACE('',(#5542),#2910,.T.);
#44398=ADVANCED_FACE('',(#5543),#2911,.T.);
#44399=ADVANCED_FACE('',(#5544),#657,.T.);
#44400=ADVANCED_FACE('',(#5545),#658,.T.);
#44401=ADVANCED_FACE('',(#5546),#2912,.T.);
#44402=ADVANCED_FACE('',(#5547),#2913,.T.);
#44403=ADVANCED_FACE('',(#5548),#42446,.F.);
#44404=ADVANCED_FACE('',(#5549),#42447,.F.);
#44405=ADVANCED_FACE('',(#5550),#2914,.T.);
#44406=ADVANCED_FACE('',(#5551),#2915,.T.);
#44407=ADVANCED_FACE('',(#5552),#659,.T.);
#44408=ADVANCED_FACE('',(#5553),#2916,.T.);
#44409=ADVANCED_FACE('',(#5554),#2917,.T.);
#44410=ADVANCED_FACE('',(#5555),#2918,.T.);
#44411=ADVANCED_FACE('',(#5556),#2919,.T.);
#44412=ADVANCED_FACE('',(#5557),#2920,.T.);
#44413=ADVANCED_FACE('',(#5558),#660,.T.);
#44414=ADVANCED_FACE('',(#5559),#2921,.T.);
#44415=ADVANCED_FACE('',(#5560),#661,.T.);
#44416=ADVANCED_FACE('',(#5561),#2922,.T.);
#44417=ADVANCED_FACE('',(#5562),#2923,.T.);
#44418=ADVANCED_FACE('',(#5563),#2924,.T.);
#44419=ADVANCED_FACE('',(#5564),#662,.T.);
#44420=ADVANCED_FACE('',(#5565),#2925,.T.);
#44421=ADVANCED_FACE('',(#5566),#2926,.T.);
#44422=ADVANCED_FACE('',(#5567),#663,.T.);
#44423=ADVANCED_FACE('',(#5568),#664,.T.);
#44424=ADVANCED_FACE('',(#5569),#2927,.T.);
#44425=ADVANCED_FACE('',(#5570),#2928,.T.);
#44426=ADVANCED_FACE('',(#5571),#42448,.F.);
#44427=ADVANCED_FACE('',(#5572),#42449,.F.);
#44428=ADVANCED_FACE('',(#5573),#2929,.T.);
#44429=ADVANCED_FACE('',(#5574),#2930,.T.);
#44430=ADVANCED_FACE('',(#5575),#665,.T.);
#44431=ADVANCED_FACE('',(#5576),#2931,.T.);
#44432=ADVANCED_FACE('',(#5577),#2932,.T.);
#44433=ADVANCED_FACE('',(#5578),#2933,.T.);
#44434=ADVANCED_FACE('',(#5579),#2934,.T.);
#44435=ADVANCED_FACE('',(#5580),#2935,.T.);
#44436=ADVANCED_FACE('',(#5581),#666,.T.);
#44437=ADVANCED_FACE('',(#5582),#2936,.T.);
#44438=ADVANCED_FACE('',(#5583),#667,.T.);
#44439=ADVANCED_FACE('',(#5584),#2937,.T.);
#44440=ADVANCED_FACE('',(#5585),#2938,.T.);
#44441=ADVANCED_FACE('',(#5586),#2939,.T.);
#44442=ADVANCED_FACE('',(#5587),#668,.T.);
#44443=ADVANCED_FACE('',(#5588),#2940,.T.);
#44444=ADVANCED_FACE('',(#5589),#2941,.T.);
#44445=ADVANCED_FACE('',(#5590),#669,.T.);
#44446=ADVANCED_FACE('',(#5591),#670,.T.);
#44447=ADVANCED_FACE('',(#5592),#2942,.T.);
#44448=ADVANCED_FACE('',(#5593),#2943,.T.);
#44449=ADVANCED_FACE('',(#5594),#42450,.F.);
#44450=ADVANCED_FACE('',(#5595),#42451,.F.);
#44451=ADVANCED_FACE('',(#5596),#2944,.T.);
#44452=ADVANCED_FACE('',(#5597),#2945,.T.);
#44453=ADVANCED_FACE('',(#5598),#671,.T.);
#44454=ADVANCED_FACE('',(#5599),#2946,.T.);
#44455=ADVANCED_FACE('',(#5600),#2947,.T.);
#44456=ADVANCED_FACE('',(#5601),#2948,.T.);
#44457=ADVANCED_FACE('',(#5602),#2949,.T.);
#44458=ADVANCED_FACE('',(#5603),#2950,.T.);
#44459=ADVANCED_FACE('',(#5604),#672,.T.);
#44460=ADVANCED_FACE('',(#5605),#2951,.T.);
#44461=ADVANCED_FACE('',(#5606),#673,.T.);
#44462=ADVANCED_FACE('',(#5607),#2952,.T.);
#44463=ADVANCED_FACE('',(#5608),#2953,.T.);
#44464=ADVANCED_FACE('',(#5609),#2954,.T.);
#44465=ADVANCED_FACE('',(#5610),#674,.T.);
#44466=ADVANCED_FACE('',(#5611),#2955,.T.);
#44467=ADVANCED_FACE('',(#5612),#2956,.T.);
#44468=ADVANCED_FACE('',(#5613),#675,.T.);
#44469=ADVANCED_FACE('',(#5614),#676,.T.);
#44470=ADVANCED_FACE('',(#5615),#2957,.T.);
#44471=ADVANCED_FACE('',(#5616),#2958,.T.);
#44472=ADVANCED_FACE('',(#5617),#42452,.F.);
#44473=ADVANCED_FACE('',(#5618),#42453,.F.);
#44474=ADVANCED_FACE('',(#5619),#2959,.T.);
#44475=ADVANCED_FACE('',(#5620),#2960,.T.);
#44476=ADVANCED_FACE('',(#5621),#677,.T.);
#44477=ADVANCED_FACE('',(#5622),#2961,.T.);
#44478=ADVANCED_FACE('',(#5623),#2962,.T.);
#44479=ADVANCED_FACE('',(#5624),#2963,.T.);
#44480=ADVANCED_FACE('',(#5625),#2964,.T.);
#44481=ADVANCED_FACE('',(#5626),#2965,.T.);
#44482=ADVANCED_FACE('',(#5627),#678,.T.);
#44483=ADVANCED_FACE('',(#5628),#2966,.T.);
#44484=ADVANCED_FACE('',(#5629),#679,.T.);
#44485=ADVANCED_FACE('',(#5630),#2967,.T.);
#44486=ADVANCED_FACE('',(#5631),#2968,.T.);
#44487=ADVANCED_FACE('',(#5632),#2969,.T.);
#44488=ADVANCED_FACE('',(#5633),#680,.T.);
#44489=ADVANCED_FACE('',(#5634),#2970,.T.);
#44490=ADVANCED_FACE('',(#5635),#2971,.T.);
#44491=ADVANCED_FACE('',(#5636),#681,.T.);
#44492=ADVANCED_FACE('',(#5637),#682,.T.);
#44493=ADVANCED_FACE('',(#5638),#2972,.T.);
#44494=ADVANCED_FACE('',(#5639),#2973,.T.);
#44495=ADVANCED_FACE('',(#5640),#42454,.F.);
#44496=ADVANCED_FACE('',(#5641),#42455,.F.);
#44497=ADVANCED_FACE('',(#5642),#2974,.T.);
#44498=ADVANCED_FACE('',(#5643),#2975,.T.);
#44499=ADVANCED_FACE('',(#5644),#683,.T.);
#44500=ADVANCED_FACE('',(#5645),#2976,.T.);
#44501=ADVANCED_FACE('',(#5646),#2977,.T.);
#44502=ADVANCED_FACE('',(#5647),#2978,.T.);
#44503=ADVANCED_FACE('',(#5648),#2979,.T.);
#44504=ADVANCED_FACE('',(#5649),#2980,.T.);
#44505=ADVANCED_FACE('',(#5650),#684,.T.);
#44506=ADVANCED_FACE('',(#5651),#2981,.T.);
#44507=ADVANCED_FACE('',(#5652),#685,.T.);
#44508=ADVANCED_FACE('',(#5653),#2982,.T.);
#44509=ADVANCED_FACE('',(#5654),#2983,.T.);
#44510=ADVANCED_FACE('',(#5655),#2984,.T.);
#44511=ADVANCED_FACE('',(#5656),#686,.T.);
#44512=ADVANCED_FACE('',(#5657),#2985,.T.);
#44513=ADVANCED_FACE('',(#5658),#2986,.T.);
#44514=ADVANCED_FACE('',(#5659),#687,.T.);
#44515=ADVANCED_FACE('',(#5660),#688,.T.);
#44516=ADVANCED_FACE('',(#5661),#2987,.T.);
#44517=ADVANCED_FACE('',(#5662),#2988,.T.);
#44518=ADVANCED_FACE('',(#5663),#42456,.F.);
#44519=ADVANCED_FACE('',(#5664),#42457,.F.);
#44520=ADVANCED_FACE('',(#5665),#2989,.T.);
#44521=ADVANCED_FACE('',(#5666),#2990,.T.);
#44522=ADVANCED_FACE('',(#5667),#689,.T.);
#44523=ADVANCED_FACE('',(#5668),#2991,.T.);
#44524=ADVANCED_FACE('',(#5669),#2992,.T.);
#44525=ADVANCED_FACE('',(#5670),#2993,.T.);
#44526=ADVANCED_FACE('',(#5671),#2994,.T.);
#44527=ADVANCED_FACE('',(#5672),#2995,.T.);
#44528=ADVANCED_FACE('',(#5673),#690,.T.);
#44529=ADVANCED_FACE('',(#5674),#2996,.T.);
#44530=ADVANCED_FACE('',(#5675),#691,.T.);
#44531=ADVANCED_FACE('',(#5676),#2997,.T.);
#44532=ADVANCED_FACE('',(#5677),#2998,.T.);
#44533=ADVANCED_FACE('',(#5678),#2999,.T.);
#44534=ADVANCED_FACE('',(#5679),#692,.T.);
#44535=ADVANCED_FACE('',(#5680),#3000,.T.);
#44536=ADVANCED_FACE('',(#5681),#3001,.T.);
#44537=ADVANCED_FACE('',(#5682),#693,.T.);
#44538=ADVANCED_FACE('',(#5683),#694,.T.);
#44539=ADVANCED_FACE('',(#5684),#3002,.T.);
#44540=ADVANCED_FACE('',(#5685),#3003,.T.);
#44541=ADVANCED_FACE('',(#5686),#42458,.F.);
#44542=ADVANCED_FACE('',(#5687),#42459,.F.);
#44543=ADVANCED_FACE('',(#5688),#3004,.T.);
#44544=ADVANCED_FACE('',(#5689),#3005,.T.);
#44545=ADVANCED_FACE('',(#5690),#695,.T.);
#44546=ADVANCED_FACE('',(#5691),#3006,.T.);
#44547=ADVANCED_FACE('',(#5692),#3007,.T.);
#44548=ADVANCED_FACE('',(#5693),#3008,.T.);
#44549=ADVANCED_FACE('',(#5694),#3009,.T.);
#44550=ADVANCED_FACE('',(#5695),#3010,.T.);
#44551=ADVANCED_FACE('',(#5696),#696,.T.);
#44552=ADVANCED_FACE('',(#5697),#3011,.T.);
#44553=ADVANCED_FACE('',(#5698),#697,.T.);
#44554=ADVANCED_FACE('',(#5699),#3012,.T.);
#44555=ADVANCED_FACE('',(#5700),#3013,.T.);
#44556=ADVANCED_FACE('',(#5701),#3014,.T.);
#44557=ADVANCED_FACE('',(#5702),#698,.T.);
#44558=ADVANCED_FACE('',(#5703),#3015,.T.);
#44559=ADVANCED_FACE('',(#5704),#3016,.T.);
#44560=ADVANCED_FACE('',(#5705),#699,.T.);
#44561=ADVANCED_FACE('',(#5706),#700,.T.);
#44562=ADVANCED_FACE('',(#5707),#3017,.T.);
#44563=ADVANCED_FACE('',(#5708),#3018,.T.);
#44564=ADVANCED_FACE('',(#5709),#42460,.F.);
#44565=ADVANCED_FACE('',(#5710),#42461,.F.);
#44566=ADVANCED_FACE('',(#5711),#3019,.T.);
#44567=ADVANCED_FACE('',(#5712),#3020,.T.);
#44568=ADVANCED_FACE('',(#5713),#701,.T.);
#44569=ADVANCED_FACE('',(#5714),#3021,.T.);
#44570=ADVANCED_FACE('',(#5715),#3022,.T.);
#44571=ADVANCED_FACE('',(#5716),#3023,.T.);
#44572=ADVANCED_FACE('',(#5717),#3024,.T.);
#44573=ADVANCED_FACE('',(#5718),#3025,.T.);
#44574=ADVANCED_FACE('',(#5719),#702,.T.);
#44575=ADVANCED_FACE('',(#5720),#3026,.T.);
#44576=ADVANCED_FACE('',(#5721),#703,.T.);
#44577=ADVANCED_FACE('',(#5722),#3027,.T.);
#44578=ADVANCED_FACE('',(#5723),#3028,.T.);
#44579=ADVANCED_FACE('',(#5724),#3029,.T.);
#44580=ADVANCED_FACE('',(#5725),#704,.T.);
#44581=ADVANCED_FACE('',(#5726),#3030,.T.);
#44582=ADVANCED_FACE('',(#5727),#3031,.T.);
#44583=ADVANCED_FACE('',(#5728),#705,.T.);
#44584=ADVANCED_FACE('',(#5729),#706,.T.);
#44585=ADVANCED_FACE('',(#5730),#3032,.T.);
#44586=ADVANCED_FACE('',(#5731),#3033,.T.);
#44587=ADVANCED_FACE('',(#5732),#42462,.F.);
#44588=ADVANCED_FACE('',(#5733),#42463,.F.);
#44589=ADVANCED_FACE('',(#5734),#3034,.T.);
#44590=ADVANCED_FACE('',(#5735),#3035,.T.);
#44591=ADVANCED_FACE('',(#5736),#707,.T.);
#44592=ADVANCED_FACE('',(#5737),#3036,.T.);
#44593=ADVANCED_FACE('',(#5738),#3037,.T.);
#44594=ADVANCED_FACE('',(#5739),#3038,.T.);
#44595=ADVANCED_FACE('',(#5740),#3039,.T.);
#44596=ADVANCED_FACE('',(#5741),#3040,.T.);
#44597=ADVANCED_FACE('',(#5742),#708,.T.);
#44598=ADVANCED_FACE('',(#5743),#3041,.T.);
#44599=ADVANCED_FACE('',(#5744),#709,.T.);
#44600=ADVANCED_FACE('',(#5745),#3042,.T.);
#44601=ADVANCED_FACE('',(#5746),#3043,.T.);
#44602=ADVANCED_FACE('',(#5747),#3044,.T.);
#44603=ADVANCED_FACE('',(#5748),#710,.T.);
#44604=ADVANCED_FACE('',(#5749),#3045,.T.);
#44605=ADVANCED_FACE('',(#5750),#3046,.T.);
#44606=ADVANCED_FACE('',(#5751),#711,.T.);
#44607=ADVANCED_FACE('',(#5752),#712,.T.);
#44608=ADVANCED_FACE('',(#5753),#3047,.T.);
#44609=ADVANCED_FACE('',(#5754),#3048,.T.);
#44610=ADVANCED_FACE('',(#5755),#42464,.F.);
#44611=ADVANCED_FACE('',(#5756),#42465,.F.);
#44612=ADVANCED_FACE('',(#5757),#3049,.T.);
#44613=ADVANCED_FACE('',(#5758),#3050,.T.);
#44614=ADVANCED_FACE('',(#5759),#713,.T.);
#44615=ADVANCED_FACE('',(#5760),#3051,.T.);
#44616=ADVANCED_FACE('',(#5761),#3052,.T.);
#44617=ADVANCED_FACE('',(#5762),#3053,.T.);
#44618=ADVANCED_FACE('',(#5763),#3054,.T.);
#44619=ADVANCED_FACE('',(#5764),#3055,.T.);
#44620=ADVANCED_FACE('',(#5765),#714,.T.);
#44621=ADVANCED_FACE('',(#5766),#3056,.T.);
#44622=ADVANCED_FACE('',(#5767),#715,.T.);
#44623=ADVANCED_FACE('',(#5768),#3057,.T.);
#44624=ADVANCED_FACE('',(#5769),#3058,.T.);
#44625=ADVANCED_FACE('',(#5770),#3059,.T.);
#44626=ADVANCED_FACE('',(#5771),#716,.T.);
#44627=ADVANCED_FACE('',(#5772),#3060,.T.);
#44628=ADVANCED_FACE('',(#5773),#3061,.T.);
#44629=ADVANCED_FACE('',(#5774),#717,.T.);
#44630=ADVANCED_FACE('',(#5775),#718,.T.);
#44631=ADVANCED_FACE('',(#5776),#3062,.T.);
#44632=ADVANCED_FACE('',(#5777),#3063,.T.);
#44633=ADVANCED_FACE('',(#5778),#42466,.F.);
#44634=ADVANCED_FACE('',(#5779),#42467,.F.);
#44635=ADVANCED_FACE('',(#5780),#3064,.T.);
#44636=ADVANCED_FACE('',(#5781),#3065,.T.);
#44637=ADVANCED_FACE('',(#5782),#719,.T.);
#44638=ADVANCED_FACE('',(#5783),#3066,.T.);
#44639=ADVANCED_FACE('',(#5784),#3067,.T.);
#44640=ADVANCED_FACE('',(#5785),#3068,.T.);
#44641=ADVANCED_FACE('',(#5786),#3069,.T.);
#44642=ADVANCED_FACE('',(#5787),#3070,.T.);
#44643=ADVANCED_FACE('',(#5788),#720,.T.);
#44644=ADVANCED_FACE('',(#5789),#3071,.T.);
#44645=ADVANCED_FACE('',(#5790),#721,.T.);
#44646=ADVANCED_FACE('',(#5791),#3072,.T.);
#44647=ADVANCED_FACE('',(#5792),#3073,.T.);
#44648=ADVANCED_FACE('',(#5793),#3074,.T.);
#44649=ADVANCED_FACE('',(#5794),#722,.T.);
#44650=ADVANCED_FACE('',(#5795),#3075,.T.);
#44651=ADVANCED_FACE('',(#5796),#3076,.T.);
#44652=ADVANCED_FACE('',(#5797),#723,.T.);
#44653=ADVANCED_FACE('',(#5798),#724,.T.);
#44654=ADVANCED_FACE('',(#5799),#3077,.T.);
#44655=ADVANCED_FACE('',(#5800),#3078,.T.);
#44656=ADVANCED_FACE('',(#5801),#42468,.F.);
#44657=ADVANCED_FACE('',(#5802),#42469,.F.);
#44658=ADVANCED_FACE('',(#5803),#3079,.T.);
#44659=ADVANCED_FACE('',(#5804),#3080,.T.);
#44660=ADVANCED_FACE('',(#5805),#725,.T.);
#44661=ADVANCED_FACE('',(#5806),#3081,.T.);
#44662=ADVANCED_FACE('',(#5807),#3082,.T.);
#44663=ADVANCED_FACE('',(#5808),#3083,.T.);
#44664=ADVANCED_FACE('',(#5809),#3084,.T.);
#44665=ADVANCED_FACE('',(#5810),#3085,.T.);
#44666=ADVANCED_FACE('',(#5811),#726,.T.);
#44667=ADVANCED_FACE('',(#5812),#3086,.T.);
#44668=ADVANCED_FACE('',(#5813),#727,.T.);
#44669=ADVANCED_FACE('',(#5814),#3087,.T.);
#44670=ADVANCED_FACE('',(#5815),#3088,.T.);
#44671=ADVANCED_FACE('',(#5816),#3089,.T.);
#44672=ADVANCED_FACE('',(#5817),#728,.T.);
#44673=ADVANCED_FACE('',(#5818),#3090,.T.);
#44674=ADVANCED_FACE('',(#5819),#3091,.T.);
#44675=ADVANCED_FACE('',(#5820),#729,.T.);
#44676=ADVANCED_FACE('',(#5821),#730,.T.);
#44677=ADVANCED_FACE('',(#5822),#3092,.T.);
#44678=ADVANCED_FACE('',(#5823),#3093,.T.);
#44679=ADVANCED_FACE('',(#5824),#42470,.F.);
#44680=ADVANCED_FACE('',(#5825),#42471,.F.);
#44681=ADVANCED_FACE('',(#5826),#3094,.T.);
#44682=ADVANCED_FACE('',(#5827),#3095,.T.);
#44683=ADVANCED_FACE('',(#5828),#731,.T.);
#44684=ADVANCED_FACE('',(#5829),#3096,.T.);
#44685=ADVANCED_FACE('',(#5830),#3097,.T.);
#44686=ADVANCED_FACE('',(#5831),#3098,.T.);
#44687=ADVANCED_FACE('',(#5832),#3099,.T.);
#44688=ADVANCED_FACE('',(#5833),#3100,.T.);
#44689=ADVANCED_FACE('',(#5834),#732,.T.);
#44690=ADVANCED_FACE('',(#5835),#3101,.T.);
#44691=ADVANCED_FACE('',(#5836),#733,.T.);
#44692=ADVANCED_FACE('',(#5837),#3102,.T.);
#44693=ADVANCED_FACE('',(#5838),#3103,.T.);
#44694=ADVANCED_FACE('',(#5839),#3104,.T.);
#44695=ADVANCED_FACE('',(#5840),#734,.T.);
#44696=ADVANCED_FACE('',(#5841),#3105,.T.);
#44697=ADVANCED_FACE('',(#5842),#3106,.T.);
#44698=ADVANCED_FACE('',(#5843),#735,.T.);
#44699=ADVANCED_FACE('',(#5844),#736,.T.);
#44700=ADVANCED_FACE('',(#5845),#3107,.T.);
#44701=ADVANCED_FACE('',(#5846),#3108,.T.);
#44702=ADVANCED_FACE('',(#5847),#42472,.F.);
#44703=ADVANCED_FACE('',(#5848),#42473,.F.);
#44704=ADVANCED_FACE('',(#5849),#3109,.T.);
#44705=ADVANCED_FACE('',(#5850),#3110,.T.);
#44706=ADVANCED_FACE('',(#5851),#737,.T.);
#44707=ADVANCED_FACE('',(#5852),#3111,.T.);
#44708=ADVANCED_FACE('',(#5853),#3112,.T.);
#44709=ADVANCED_FACE('',(#5854),#3113,.T.);
#44710=ADVANCED_FACE('',(#5855),#3114,.T.);
#44711=ADVANCED_FACE('',(#5856),#3115,.T.);
#44712=ADVANCED_FACE('',(#5857),#738,.T.);
#44713=ADVANCED_FACE('',(#5858),#3116,.T.);
#44714=ADVANCED_FACE('',(#5859),#739,.T.);
#44715=ADVANCED_FACE('',(#5860),#3117,.T.);
#44716=ADVANCED_FACE('',(#5861),#3118,.T.);
#44717=ADVANCED_FACE('',(#5862),#3119,.T.);
#44718=ADVANCED_FACE('',(#5863),#740,.T.);
#44719=ADVANCED_FACE('',(#5864),#3120,.T.);
#44720=ADVANCED_FACE('',(#5865),#3121,.T.);
#44721=ADVANCED_FACE('',(#5866),#741,.T.);
#44722=ADVANCED_FACE('',(#5867),#742,.T.);
#44723=ADVANCED_FACE('',(#5868),#3122,.T.);
#44724=ADVANCED_FACE('',(#5869),#3123,.T.);
#44725=ADVANCED_FACE('',(#5870),#42474,.F.);
#44726=ADVANCED_FACE('',(#5871),#42475,.F.);
#44727=ADVANCED_FACE('',(#5872),#3124,.T.);
#44728=ADVANCED_FACE('',(#5873),#3125,.T.);
#44729=ADVANCED_FACE('',(#5874),#743,.T.);
#44730=ADVANCED_FACE('',(#5875),#3126,.T.);
#44731=ADVANCED_FACE('',(#5876),#3127,.T.);
#44732=ADVANCED_FACE('',(#5877),#3128,.T.);
#44733=ADVANCED_FACE('',(#5878),#3129,.T.);
#44734=ADVANCED_FACE('',(#5879),#3130,.T.);
#44735=ADVANCED_FACE('',(#5880),#744,.T.);
#44736=ADVANCED_FACE('',(#5881),#3131,.T.);
#44737=ADVANCED_FACE('',(#5882),#745,.T.);
#44738=ADVANCED_FACE('',(#5883),#3132,.T.);
#44739=ADVANCED_FACE('',(#5884),#3133,.T.);
#44740=ADVANCED_FACE('',(#5885),#3134,.T.);
#44741=ADVANCED_FACE('',(#5886),#746,.T.);
#44742=ADVANCED_FACE('',(#5887),#3135,.T.);
#44743=ADVANCED_FACE('',(#5888),#3136,.T.);
#44744=ADVANCED_FACE('',(#5889),#747,.T.);
#44745=ADVANCED_FACE('',(#5890),#748,.T.);
#44746=ADVANCED_FACE('',(#5891),#3137,.T.);
#44747=ADVANCED_FACE('',(#5892),#3138,.T.);
#44748=ADVANCED_FACE('',(#5893),#42476,.F.);
#44749=ADVANCED_FACE('',(#5894),#42477,.F.);
#44750=ADVANCED_FACE('',(#5895),#3139,.T.);
#44751=ADVANCED_FACE('',(#5896),#3140,.T.);
#44752=ADVANCED_FACE('',(#5897),#749,.T.);
#44753=ADVANCED_FACE('',(#5898),#3141,.T.);
#44754=ADVANCED_FACE('',(#5899),#3142,.T.);
#44755=ADVANCED_FACE('',(#5900),#3143,.T.);
#44756=ADVANCED_FACE('',(#5901),#3144,.T.);
#44757=ADVANCED_FACE('',(#5902),#3145,.T.);
#44758=ADVANCED_FACE('',(#5903),#750,.T.);
#44759=ADVANCED_FACE('',(#5904),#3146,.T.);
#44760=ADVANCED_FACE('',(#5905),#751,.T.);
#44761=ADVANCED_FACE('',(#5906),#3147,.T.);
#44762=ADVANCED_FACE('',(#5907),#3148,.T.);
#44763=ADVANCED_FACE('',(#5908),#3149,.T.);
#44764=ADVANCED_FACE('',(#5909),#752,.T.);
#44765=ADVANCED_FACE('',(#5910),#3150,.T.);
#44766=ADVANCED_FACE('',(#5911),#3151,.T.);
#44767=ADVANCED_FACE('',(#5912),#753,.T.);
#44768=ADVANCED_FACE('',(#5913),#754,.T.);
#44769=ADVANCED_FACE('',(#5914),#3152,.T.);
#44770=ADVANCED_FACE('',(#5915),#3153,.T.);
#44771=ADVANCED_FACE('',(#5916),#42478,.F.);
#44772=ADVANCED_FACE('',(#5917),#42479,.F.);
#44773=ADVANCED_FACE('',(#5918),#3154,.T.);
#44774=ADVANCED_FACE('',(#5919),#3155,.T.);
#44775=ADVANCED_FACE('',(#5920),#755,.T.);
#44776=ADVANCED_FACE('',(#5921),#3156,.T.);
#44777=ADVANCED_FACE('',(#5922),#3157,.T.);
#44778=ADVANCED_FACE('',(#5923),#3158,.T.);
#44779=ADVANCED_FACE('',(#5924),#3159,.T.);
#44780=ADVANCED_FACE('',(#5925),#3160,.T.);
#44781=ADVANCED_FACE('',(#5926),#756,.T.);
#44782=ADVANCED_FACE('',(#5927),#3161,.T.);
#44783=ADVANCED_FACE('',(#5928),#757,.T.);
#44784=ADVANCED_FACE('',(#5929),#3162,.T.);
#44785=ADVANCED_FACE('',(#5930),#3163,.T.);
#44786=ADVANCED_FACE('',(#5931),#3164,.T.);
#44787=ADVANCED_FACE('',(#5932),#758,.T.);
#44788=ADVANCED_FACE('',(#5933),#3165,.T.);
#44789=ADVANCED_FACE('',(#5934),#3166,.T.);
#44790=ADVANCED_FACE('',(#5935),#759,.T.);
#44791=ADVANCED_FACE('',(#5936),#760,.T.);
#44792=ADVANCED_FACE('',(#5937),#3167,.T.);
#44793=ADVANCED_FACE('',(#5938),#3168,.T.);
#44794=ADVANCED_FACE('',(#5939),#42480,.F.);
#44795=ADVANCED_FACE('',(#5940),#42481,.F.);
#44796=ADVANCED_FACE('',(#5941),#3169,.T.);
#44797=ADVANCED_FACE('',(#5942),#3170,.T.);
#44798=ADVANCED_FACE('',(#5943),#761,.T.);
#44799=ADVANCED_FACE('',(#5944),#3171,.T.);
#44800=ADVANCED_FACE('',(#5945),#3172,.T.);
#44801=ADVANCED_FACE('',(#5946),#3173,.T.);
#44802=ADVANCED_FACE('',(#5947),#3174,.T.);
#44803=ADVANCED_FACE('',(#5948),#3175,.T.);
#44804=ADVANCED_FACE('',(#5949),#762,.T.);
#44805=ADVANCED_FACE('',(#5950),#3176,.T.);
#44806=ADVANCED_FACE('',(#5951),#763,.T.);
#44807=ADVANCED_FACE('',(#5952),#3177,.T.);
#44808=ADVANCED_FACE('',(#5953),#3178,.T.);
#44809=ADVANCED_FACE('',(#5954),#3179,.T.);
#44810=ADVANCED_FACE('',(#5955),#764,.T.);
#44811=ADVANCED_FACE('',(#5956),#3180,.T.);
#44812=ADVANCED_FACE('',(#5957),#3181,.T.);
#44813=ADVANCED_FACE('',(#5958),#765,.T.);
#44814=ADVANCED_FACE('',(#5959),#766,.T.);
#44815=ADVANCED_FACE('',(#5960),#3182,.T.);
#44816=ADVANCED_FACE('',(#5961),#3183,.T.);
#44817=ADVANCED_FACE('',(#5962),#42482,.F.);
#44818=ADVANCED_FACE('',(#5963),#42483,.F.);
#44819=ADVANCED_FACE('',(#5964),#3184,.T.);
#44820=ADVANCED_FACE('',(#5965),#3185,.T.);
#44821=ADVANCED_FACE('',(#5966),#767,.T.);
#44822=ADVANCED_FACE('',(#5967),#3186,.T.);
#44823=ADVANCED_FACE('',(#5968),#3187,.T.);
#44824=ADVANCED_FACE('',(#5969),#3188,.T.);
#44825=ADVANCED_FACE('',(#5970),#3189,.T.);
#44826=ADVANCED_FACE('',(#5971),#3190,.T.);
#44827=ADVANCED_FACE('',(#5972),#768,.T.);
#44828=ADVANCED_FACE('',(#5973),#3191,.T.);
#44829=ADVANCED_FACE('',(#5974),#769,.T.);
#44830=ADVANCED_FACE('',(#5975),#3192,.T.);
#44831=ADVANCED_FACE('',(#5976),#3193,.T.);
#44832=ADVANCED_FACE('',(#5977),#3194,.T.);
#44833=ADVANCED_FACE('',(#5978),#770,.T.);
#44834=ADVANCED_FACE('',(#5979),#3195,.T.);
#44835=ADVANCED_FACE('',(#5980),#3196,.T.);
#44836=ADVANCED_FACE('',(#5981),#771,.T.);
#44837=ADVANCED_FACE('',(#5982),#772,.T.);
#44838=ADVANCED_FACE('',(#5983),#3197,.T.);
#44839=ADVANCED_FACE('',(#5984),#3198,.T.);
#44840=ADVANCED_FACE('',(#5985),#42484,.F.);
#44841=ADVANCED_FACE('',(#5986),#42485,.F.);
#44842=ADVANCED_FACE('',(#5987),#3199,.T.);
#44843=ADVANCED_FACE('',(#5988),#3200,.T.);
#44844=ADVANCED_FACE('',(#5989),#773,.T.);
#44845=ADVANCED_FACE('',(#5990),#3201,.T.);
#44846=ADVANCED_FACE('',(#5991),#3202,.T.);
#44847=ADVANCED_FACE('',(#5992),#3203,.T.);
#44848=ADVANCED_FACE('',(#5993),#3204,.T.);
#44849=ADVANCED_FACE('',(#5994),#3205,.T.);
#44850=ADVANCED_FACE('',(#5995),#774,.T.);
#44851=ADVANCED_FACE('',(#5996),#3206,.T.);
#44852=ADVANCED_FACE('',(#5997),#775,.T.);
#44853=ADVANCED_FACE('',(#5998),#3207,.T.);
#44854=ADVANCED_FACE('',(#5999),#3208,.T.);
#44855=ADVANCED_FACE('',(#6000),#3209,.T.);
#44856=ADVANCED_FACE('',(#6001),#776,.T.);
#44857=ADVANCED_FACE('',(#6002),#3210,.T.);
#44858=ADVANCED_FACE('',(#6003),#3211,.T.);
#44859=ADVANCED_FACE('',(#6004),#777,.T.);
#44860=ADVANCED_FACE('',(#6005),#778,.T.);
#44861=ADVANCED_FACE('',(#6006),#3212,.T.);
#44862=ADVANCED_FACE('',(#6007),#3213,.T.);
#44863=ADVANCED_FACE('',(#6008),#42486,.F.);
#44864=ADVANCED_FACE('',(#6009),#42487,.F.);
#44865=ADVANCED_FACE('',(#6010),#3214,.T.);
#44866=ADVANCED_FACE('',(#6011),#3215,.T.);
#44867=ADVANCED_FACE('',(#6012),#779,.T.);
#44868=ADVANCED_FACE('',(#6013),#3216,.T.);
#44869=ADVANCED_FACE('',(#6014),#3217,.T.);
#44870=ADVANCED_FACE('',(#6015),#3218,.T.);
#44871=ADVANCED_FACE('',(#6016),#3219,.T.);
#44872=ADVANCED_FACE('',(#6017),#3220,.T.);
#44873=ADVANCED_FACE('',(#6018),#780,.T.);
#44874=ADVANCED_FACE('',(#6019),#3221,.T.);
#44875=ADVANCED_FACE('',(#6020),#781,.T.);
#44876=ADVANCED_FACE('',(#6021),#3222,.T.);
#44877=ADVANCED_FACE('',(#6022),#3223,.T.);
#44878=ADVANCED_FACE('',(#6023),#3224,.T.);
#44879=ADVANCED_FACE('',(#6024),#782,.T.);
#44880=ADVANCED_FACE('',(#6025),#3225,.T.);
#44881=ADVANCED_FACE('',(#6026),#3226,.T.);
#44882=ADVANCED_FACE('',(#6027),#783,.T.);
#44883=ADVANCED_FACE('',(#6028),#784,.T.);
#44884=ADVANCED_FACE('',(#6029),#3227,.T.);
#44885=ADVANCED_FACE('',(#6030),#3228,.T.);
#44886=ADVANCED_FACE('',(#6031),#42488,.F.);
#44887=ADVANCED_FACE('',(#6032),#42489,.F.);
#44888=ADVANCED_FACE('',(#6033),#3229,.T.);
#44889=ADVANCED_FACE('',(#6034),#3230,.T.);
#44890=ADVANCED_FACE('',(#6035),#785,.T.);
#44891=ADVANCED_FACE('',(#6036),#3231,.T.);
#44892=ADVANCED_FACE('',(#6037),#3232,.T.);
#44893=ADVANCED_FACE('',(#6038),#3233,.T.);
#44894=ADVANCED_FACE('',(#6039),#3234,.T.);
#44895=ADVANCED_FACE('',(#6040),#3235,.T.);
#44896=ADVANCED_FACE('',(#6041),#786,.T.);
#44897=ADVANCED_FACE('',(#6042),#3236,.T.);
#44898=ADVANCED_FACE('',(#6043),#787,.T.);
#44899=ADVANCED_FACE('',(#6044),#3237,.T.);
#44900=ADVANCED_FACE('',(#6045),#3238,.T.);
#44901=ADVANCED_FACE('',(#6046),#3239,.T.);
#44902=ADVANCED_FACE('',(#6047),#788,.T.);
#44903=ADVANCED_FACE('',(#6048),#3240,.T.);
#44904=ADVANCED_FACE('',(#6049),#3241,.T.);
#44905=ADVANCED_FACE('',(#6050),#789,.T.);
#44906=ADVANCED_FACE('',(#6051),#790,.T.);
#44907=ADVANCED_FACE('',(#6052),#3242,.T.);
#44908=ADVANCED_FACE('',(#6053),#3243,.T.);
#44909=ADVANCED_FACE('',(#6054),#42490,.F.);
#44910=ADVANCED_FACE('',(#6055),#42491,.F.);
#44911=ADVANCED_FACE('',(#6056),#3244,.T.);
#44912=ADVANCED_FACE('',(#6057),#3245,.T.);
#44913=ADVANCED_FACE('',(#6058),#791,.T.);
#44914=ADVANCED_FACE('',(#6059),#3246,.T.);
#44915=ADVANCED_FACE('',(#6060),#3247,.T.);
#44916=ADVANCED_FACE('',(#6061),#3248,.T.);
#44917=ADVANCED_FACE('',(#6062),#3249,.T.);
#44918=ADVANCED_FACE('',(#6063),#3250,.T.);
#44919=ADVANCED_FACE('',(#6064),#792,.T.);
#44920=ADVANCED_FACE('',(#6065),#3251,.T.);
#44921=ADVANCED_FACE('',(#6066),#793,.T.);
#44922=ADVANCED_FACE('',(#6067),#3252,.T.);
#44923=ADVANCED_FACE('',(#6068),#3253,.T.);
#44924=ADVANCED_FACE('',(#6069),#3254,.T.);
#44925=ADVANCED_FACE('',(#6070),#794,.T.);
#44926=ADVANCED_FACE('',(#6071),#3255,.T.);
#44927=ADVANCED_FACE('',(#6072),#3256,.T.);
#44928=ADVANCED_FACE('',(#6073),#795,.T.);
#44929=ADVANCED_FACE('',(#6074),#796,.T.);
#44930=ADVANCED_FACE('',(#6075),#3257,.T.);
#44931=ADVANCED_FACE('',(#6076),#3258,.T.);
#44932=ADVANCED_FACE('',(#6077),#42492,.F.);
#44933=ADVANCED_FACE('',(#6078),#42493,.F.);
#44934=ADVANCED_FACE('',(#6079),#3259,.T.);
#44935=ADVANCED_FACE('',(#6080),#3260,.T.);
#44936=ADVANCED_FACE('',(#6081),#797,.T.);
#44937=ADVANCED_FACE('',(#6082),#3261,.T.);
#44938=ADVANCED_FACE('',(#6083),#3262,.T.);
#44939=ADVANCED_FACE('',(#6084),#3263,.T.);
#44940=ADVANCED_FACE('',(#6085),#3264,.T.);
#44941=ADVANCED_FACE('',(#6086),#3265,.T.);
#44942=ADVANCED_FACE('',(#6087),#798,.T.);
#44943=ADVANCED_FACE('',(#6088),#3266,.T.);
#44944=ADVANCED_FACE('',(#6089),#799,.T.);
#44945=ADVANCED_FACE('',(#6090),#3267,.T.);
#44946=ADVANCED_FACE('',(#6091),#3268,.T.);
#44947=ADVANCED_FACE('',(#6092),#3269,.T.);
#44948=ADVANCED_FACE('',(#6093),#800,.T.);
#44949=ADVANCED_FACE('',(#6094),#3270,.T.);
#44950=ADVANCED_FACE('',(#6095),#3271,.T.);
#44951=ADVANCED_FACE('',(#6096),#801,.T.);
#44952=ADVANCED_FACE('',(#6097),#802,.T.);
#44953=ADVANCED_FACE('',(#6098),#3272,.T.);
#44954=ADVANCED_FACE('',(#6099),#3273,.T.);
#44955=ADVANCED_FACE('',(#6100),#42494,.F.);
#44956=ADVANCED_FACE('',(#6101),#42495,.F.);
#44957=ADVANCED_FACE('',(#6102),#3274,.T.);
#44958=ADVANCED_FACE('',(#6103),#3275,.T.);
#44959=ADVANCED_FACE('',(#6104),#803,.T.);
#44960=ADVANCED_FACE('',(#6105),#3276,.T.);
#44961=ADVANCED_FACE('',(#6106),#3277,.T.);
#44962=ADVANCED_FACE('',(#6107),#3278,.T.);
#44963=ADVANCED_FACE('',(#6108),#3279,.T.);
#44964=ADVANCED_FACE('',(#6109),#3280,.T.);
#44965=ADVANCED_FACE('',(#6110),#804,.T.);
#44966=ADVANCED_FACE('',(#6111),#3281,.T.);
#44967=ADVANCED_FACE('',(#6112),#805,.T.);
#44968=ADVANCED_FACE('',(#6113),#3282,.T.);
#44969=ADVANCED_FACE('',(#6114),#3283,.T.);
#44970=ADVANCED_FACE('',(#6115),#3284,.T.);
#44971=ADVANCED_FACE('',(#6116),#806,.T.);
#44972=ADVANCED_FACE('',(#6117),#3285,.T.);
#44973=ADVANCED_FACE('',(#6118),#3286,.T.);
#44974=ADVANCED_FACE('',(#6119),#807,.T.);
#44975=ADVANCED_FACE('',(#6120),#808,.T.);
#44976=ADVANCED_FACE('',(#6121),#3287,.T.);
#44977=ADVANCED_FACE('',(#6122),#3288,.T.);
#44978=ADVANCED_FACE('',(#6123),#42496,.F.);
#44979=ADVANCED_FACE('',(#6124),#42497,.F.);
#44980=ADVANCED_FACE('',(#6125),#3289,.T.);
#44981=ADVANCED_FACE('',(#6126),#3290,.T.);
#44982=ADVANCED_FACE('',(#6127),#809,.T.);
#44983=ADVANCED_FACE('',(#6128),#3291,.T.);
#44984=ADVANCED_FACE('',(#6129),#3292,.T.);
#44985=ADVANCED_FACE('',(#6130),#3293,.T.);
#44986=ADVANCED_FACE('',(#6131),#3294,.T.);
#44987=ADVANCED_FACE('',(#6132),#3295,.T.);
#44988=ADVANCED_FACE('',(#6133),#810,.T.);
#44989=ADVANCED_FACE('',(#6134),#3296,.T.);
#44990=ADVANCED_FACE('',(#6135),#811,.T.);
#44991=ADVANCED_FACE('',(#6136),#3297,.T.);
#44992=ADVANCED_FACE('',(#6137),#3298,.T.);
#44993=ADVANCED_FACE('',(#6138),#3299,.T.);
#44994=ADVANCED_FACE('',(#6139),#812,.T.);
#44995=ADVANCED_FACE('',(#6140),#3300,.T.);
#44996=ADVANCED_FACE('',(#6141),#3301,.T.);
#44997=ADVANCED_FACE('',(#6142),#813,.T.);
#44998=ADVANCED_FACE('',(#6143),#814,.T.);
#44999=ADVANCED_FACE('',(#6144),#3302,.T.);
#45000=ADVANCED_FACE('',(#6145),#3303,.T.);
#45001=ADVANCED_FACE('',(#6146),#42498,.F.);
#45002=ADVANCED_FACE('',(#6147),#42499,.F.);
#45003=ADVANCED_FACE('',(#6148),#3304,.T.);
#45004=ADVANCED_FACE('',(#6149),#3305,.T.);
#45005=ADVANCED_FACE('',(#6150),#815,.T.);
#45006=ADVANCED_FACE('',(#6151),#3306,.T.);
#45007=ADVANCED_FACE('',(#6152),#3307,.T.);
#45008=ADVANCED_FACE('',(#6153),#3308,.T.);
#45009=ADVANCED_FACE('',(#6154),#3309,.T.);
#45010=ADVANCED_FACE('',(#6155),#3310,.T.);
#45011=ADVANCED_FACE('',(#6156),#816,.T.);
#45012=ADVANCED_FACE('',(#6157),#3311,.T.);
#45013=ADVANCED_FACE('',(#6158),#817,.T.);
#45014=ADVANCED_FACE('',(#6159),#3312,.T.);
#45015=ADVANCED_FACE('',(#6160),#3313,.T.);
#45016=ADVANCED_FACE('',(#6161),#3314,.T.);
#45017=ADVANCED_FACE('',(#6162),#818,.T.);
#45018=ADVANCED_FACE('',(#6163),#3315,.T.);
#45019=ADVANCED_FACE('',(#6164),#3316,.T.);
#45020=ADVANCED_FACE('',(#6165),#819,.T.);
#45021=ADVANCED_FACE('',(#6166),#820,.T.);
#45022=ADVANCED_FACE('',(#6167),#3317,.T.);
#45023=ADVANCED_FACE('',(#6168),#3318,.T.);
#45024=ADVANCED_FACE('',(#6169),#42500,.F.);
#45025=ADVANCED_FACE('',(#6170),#42501,.F.);
#45026=ADVANCED_FACE('',(#6171),#3319,.T.);
#45027=ADVANCED_FACE('',(#6172),#3320,.T.);
#45028=ADVANCED_FACE('',(#6173),#821,.T.);
#45029=ADVANCED_FACE('',(#6174),#3321,.T.);
#45030=ADVANCED_FACE('',(#6175),#3322,.T.);
#45031=ADVANCED_FACE('',(#6176),#3323,.T.);
#45032=ADVANCED_FACE('',(#6177),#3324,.T.);
#45033=ADVANCED_FACE('',(#6178),#3325,.T.);
#45034=ADVANCED_FACE('',(#6179),#822,.T.);
#45035=ADVANCED_FACE('',(#6180),#3326,.T.);
#45036=ADVANCED_FACE('',(#6181),#823,.T.);
#45037=ADVANCED_FACE('',(#6182),#3327,.T.);
#45038=ADVANCED_FACE('',(#6183),#3328,.T.);
#45039=ADVANCED_FACE('',(#6184),#3329,.T.);
#45040=ADVANCED_FACE('',(#6185),#824,.T.);
#45041=ADVANCED_FACE('',(#6186),#3330,.T.);
#45042=ADVANCED_FACE('',(#6187),#3331,.T.);
#45043=ADVANCED_FACE('',(#6188),#825,.T.);
#45044=ADVANCED_FACE('',(#6189),#826,.T.);
#45045=ADVANCED_FACE('',(#6190),#3332,.T.);
#45046=ADVANCED_FACE('',(#6191),#3333,.T.);
#45047=ADVANCED_FACE('',(#6192),#42502,.F.);
#45048=ADVANCED_FACE('',(#6193),#42503,.F.);
#45049=ADVANCED_FACE('',(#6194),#3334,.T.);
#45050=ADVANCED_FACE('',(#6195),#3335,.T.);
#45051=ADVANCED_FACE('',(#6196),#827,.T.);
#45052=ADVANCED_FACE('',(#6197),#3336,.T.);
#45053=ADVANCED_FACE('',(#6198),#3337,.T.);
#45054=ADVANCED_FACE('',(#6199),#3338,.T.);
#45055=ADVANCED_FACE('',(#6200),#3339,.T.);
#45056=ADVANCED_FACE('',(#6201),#3340,.T.);
#45057=ADVANCED_FACE('',(#6202),#828,.T.);
#45058=ADVANCED_FACE('',(#6203),#3341,.T.);
#45059=ADVANCED_FACE('',(#6204),#829,.T.);
#45060=ADVANCED_FACE('',(#6205),#3342,.T.);
#45061=ADVANCED_FACE('',(#6206),#3343,.T.);
#45062=ADVANCED_FACE('',(#6207),#3344,.T.);
#45063=ADVANCED_FACE('',(#6208),#830,.T.);
#45064=ADVANCED_FACE('',(#6209),#3345,.T.);
#45065=ADVANCED_FACE('',(#6210),#3346,.T.);
#45066=ADVANCED_FACE('',(#6211),#831,.T.);
#45067=ADVANCED_FACE('',(#6212),#832,.T.);
#45068=ADVANCED_FACE('',(#6213),#3347,.T.);
#45069=ADVANCED_FACE('',(#6214),#3348,.T.);
#45070=ADVANCED_FACE('',(#6215),#42504,.F.);
#45071=ADVANCED_FACE('',(#6216),#42505,.F.);
#45072=ADVANCED_FACE('',(#6217),#3349,.T.);
#45073=ADVANCED_FACE('',(#6218),#3350,.T.);
#45074=ADVANCED_FACE('',(#6219),#833,.T.);
#45075=ADVANCED_FACE('',(#6220),#3351,.T.);
#45076=ADVANCED_FACE('',(#6221),#3352,.T.);
#45077=ADVANCED_FACE('',(#6222),#3353,.T.);
#45078=ADVANCED_FACE('',(#6223),#3354,.T.);
#45079=ADVANCED_FACE('',(#6224),#3355,.T.);
#45080=ADVANCED_FACE('',(#6225),#834,.T.);
#45081=ADVANCED_FACE('',(#6226),#3356,.T.);
#45082=ADVANCED_FACE('',(#6227),#835,.T.);
#45083=ADVANCED_FACE('',(#6228),#3357,.T.);
#45084=ADVANCED_FACE('',(#6229),#3358,.T.);
#45085=ADVANCED_FACE('',(#6230),#3359,.T.);
#45086=ADVANCED_FACE('',(#6231),#836,.T.);
#45087=ADVANCED_FACE('',(#6232),#3360,.T.);
#45088=ADVANCED_FACE('',(#6233),#3361,.T.);
#45089=ADVANCED_FACE('',(#6234),#837,.T.);
#45090=ADVANCED_FACE('',(#6235),#838,.T.);
#45091=ADVANCED_FACE('',(#6236),#3362,.T.);
#45092=ADVANCED_FACE('',(#6237),#3363,.T.);
#45093=ADVANCED_FACE('',(#6238),#3364,.T.);
#45094=ADVANCED_FACE('',(#6239),#3365,.T.);
#45095=ADVANCED_FACE('',(#6240),#839,.T.);
#45096=ADVANCED_FACE('',(#6241),#42506,.F.);
#45097=ADVANCED_FACE('',(#6242),#42507,.F.);
#45098=ADVANCED_FACE('',(#6243),#3366,.T.);
#45099=ADVANCED_FACE('',(#6244),#3367,.T.);
#45100=ADVANCED_FACE('',(#6245),#3368,.T.);
#45101=ADVANCED_FACE('',(#6246),#3369,.T.);
#45102=ADVANCED_FACE('',(#6247),#3370,.T.);
#45103=ADVANCED_FACE('',(#6248),#840,.T.);
#45104=ADVANCED_FACE('',(#6249),#3371,.T.);
#45105=ADVANCED_FACE('',(#6250),#841,.T.);
#45106=ADVANCED_FACE('',(#6251),#3372,.T.);
#45107=ADVANCED_FACE('',(#6252),#3373,.T.);
#45108=ADVANCED_FACE('',(#6253),#3374,.T.);
#45109=ADVANCED_FACE('',(#6254),#842,.T.);
#45110=ADVANCED_FACE('',(#6255),#3375,.T.);
#45111=ADVANCED_FACE('',(#6256),#3376,.T.);
#45112=ADVANCED_FACE('',(#6257),#843,.T.);
#45113=ADVANCED_FACE('',(#6258),#844,.T.);
#45114=ADVANCED_FACE('',(#6259),#3377,.T.);
#45115=ADVANCED_FACE('',(#6260),#3378,.T.);
#45116=ADVANCED_FACE('',(#6261),#42508,.F.);
#45117=ADVANCED_FACE('',(#6262),#42509,.F.);
#45118=ADVANCED_FACE('',(#6263),#3379,.T.);
#45119=ADVANCED_FACE('',(#6264),#3380,.T.);
#45120=ADVANCED_FACE('',(#6265),#845,.T.);
#45121=ADVANCED_FACE('',(#6266),#3381,.T.);
#45122=ADVANCED_FACE('',(#6267),#3382,.T.);
#45123=ADVANCED_FACE('',(#6268),#3383,.T.);
#45124=ADVANCED_FACE('',(#6269),#3384,.T.);
#45125=ADVANCED_FACE('',(#6270),#3385,.T.);
#45126=ADVANCED_FACE('',(#6271),#846,.T.);
#45127=ADVANCED_FACE('',(#6272),#3386,.T.);
#45128=ADVANCED_FACE('',(#6273),#847,.T.);
#45129=ADVANCED_FACE('',(#6274),#3387,.T.);
#45130=ADVANCED_FACE('',(#6275),#3388,.T.);
#45131=ADVANCED_FACE('',(#6276),#3389,.T.);
#45132=ADVANCED_FACE('',(#6277),#848,.T.);
#45133=ADVANCED_FACE('',(#6278),#3390,.T.);
#45134=ADVANCED_FACE('',(#6279),#3391,.T.);
#45135=ADVANCED_FACE('',(#6280),#849,.T.);
#45136=ADVANCED_FACE('',(#6281),#850,.T.);
#45137=ADVANCED_FACE('',(#6282),#3392,.T.);
#45138=ADVANCED_FACE('',(#6283),#3393,.T.);
#45139=ADVANCED_FACE('',(#6284),#42510,.F.);
#45140=ADVANCED_FACE('',(#6285),#42511,.F.);
#45141=ADVANCED_FACE('',(#6286),#3394,.T.);
#45142=ADVANCED_FACE('',(#6287),#3395,.T.);
#45143=ADVANCED_FACE('',(#6288),#851,.T.);
#45144=ADVANCED_FACE('',(#6289),#3396,.T.);
#45145=ADVANCED_FACE('',(#6290),#3397,.T.);
#45146=ADVANCED_FACE('',(#6291),#3398,.T.);
#45147=ADVANCED_FACE('',(#6292),#3399,.T.);
#45148=ADVANCED_FACE('',(#6293),#3400,.T.);
#45149=ADVANCED_FACE('',(#6294),#852,.T.);
#45150=ADVANCED_FACE('',(#6295),#3401,.T.);
#45151=ADVANCED_FACE('',(#6296),#853,.T.);
#45152=ADVANCED_FACE('',(#6297),#3402,.T.);
#45153=ADVANCED_FACE('',(#6298),#3403,.T.);
#45154=ADVANCED_FACE('',(#6299),#3404,.T.);
#45155=ADVANCED_FACE('',(#6300),#854,.T.);
#45156=ADVANCED_FACE('',(#6301),#3405,.T.);
#45157=ADVANCED_FACE('',(#6302),#3406,.T.);
#45158=ADVANCED_FACE('',(#6303),#855,.T.);
#45159=ADVANCED_FACE('',(#6304),#856,.T.);
#45160=ADVANCED_FACE('',(#6305),#3407,.T.);
#45161=ADVANCED_FACE('',(#6306),#3408,.T.);
#45162=ADVANCED_FACE('',(#6307),#42512,.F.);
#45163=ADVANCED_FACE('',(#6308),#42513,.F.);
#45164=ADVANCED_FACE('',(#6309),#3409,.T.);
#45165=ADVANCED_FACE('',(#6310),#3410,.T.);
#45166=ADVANCED_FACE('',(#6311),#857,.T.);
#45167=ADVANCED_FACE('',(#6312),#3411,.T.);
#45168=ADVANCED_FACE('',(#6313),#3412,.T.);
#45169=ADVANCED_FACE('',(#6314),#3413,.T.);
#45170=ADVANCED_FACE('',(#6315),#3414,.T.);
#45171=ADVANCED_FACE('',(#6316),#3415,.T.);
#45172=ADVANCED_FACE('',(#6317),#858,.T.);
#45173=ADVANCED_FACE('',(#6318),#3416,.T.);
#45174=ADVANCED_FACE('',(#6319),#859,.T.);
#45175=ADVANCED_FACE('',(#6320),#3417,.T.);
#45176=ADVANCED_FACE('',(#6321),#3418,.T.);
#45177=ADVANCED_FACE('',(#6322),#3419,.T.);
#45178=ADVANCED_FACE('',(#6323),#860,.T.);
#45179=ADVANCED_FACE('',(#6324),#3420,.T.);
#45180=ADVANCED_FACE('',(#6325),#3421,.T.);
#45181=ADVANCED_FACE('',(#6326),#861,.T.);
#45182=ADVANCED_FACE('',(#6327),#862,.T.);
#45183=ADVANCED_FACE('',(#6328),#3422,.T.);
#45184=ADVANCED_FACE('',(#6329),#3423,.T.);
#45185=ADVANCED_FACE('',(#6330),#42514,.F.);
#45186=ADVANCED_FACE('',(#6331),#42515,.F.);
#45187=ADVANCED_FACE('',(#6332),#3424,.T.);
#45188=ADVANCED_FACE('',(#6333),#3425,.T.);
#45189=ADVANCED_FACE('',(#6334),#863,.T.);
#45190=ADVANCED_FACE('',(#6335),#3426,.T.);
#45191=ADVANCED_FACE('',(#6336),#3427,.T.);
#45192=ADVANCED_FACE('',(#6337),#3428,.T.);
#45193=ADVANCED_FACE('',(#6338),#3429,.T.);
#45194=ADVANCED_FACE('',(#6339),#3430,.T.);
#45195=ADVANCED_FACE('',(#6340),#864,.T.);
#45196=ADVANCED_FACE('',(#6341),#3431,.T.);
#45197=ADVANCED_FACE('',(#6342),#865,.T.);
#45198=ADVANCED_FACE('',(#6343),#3432,.T.);
#45199=ADVANCED_FACE('',(#6344),#3433,.T.);
#45200=ADVANCED_FACE('',(#6345),#3434,.T.);
#45201=ADVANCED_FACE('',(#6346),#866,.T.);
#45202=ADVANCED_FACE('',(#6347),#3435,.T.);
#45203=ADVANCED_FACE('',(#6348),#3436,.T.);
#45204=ADVANCED_FACE('',(#6349),#867,.T.);
#45205=ADVANCED_FACE('',(#6350),#868,.T.);
#45206=ADVANCED_FACE('',(#6351),#3437,.T.);
#45207=ADVANCED_FACE('',(#6352),#3438,.T.);
#45208=ADVANCED_FACE('',(#6353),#42516,.F.);
#45209=ADVANCED_FACE('',(#6354),#42517,.F.);
#45210=ADVANCED_FACE('',(#6355),#3439,.T.);
#45211=ADVANCED_FACE('',(#6356),#3440,.T.);
#45212=ADVANCED_FACE('',(#6357),#869,.T.);
#45213=ADVANCED_FACE('',(#6358),#3441,.T.);
#45214=ADVANCED_FACE('',(#6359),#3442,.T.);
#45215=ADVANCED_FACE('',(#6360),#3443,.T.);
#45216=ADVANCED_FACE('',(#6361),#3444,.T.);
#45217=ADVANCED_FACE('',(#6362),#3445,.T.);
#45218=ADVANCED_FACE('',(#6363),#870,.T.);
#45219=ADVANCED_FACE('',(#6364),#3446,.T.);
#45220=ADVANCED_FACE('',(#6365),#871,.T.);
#45221=ADVANCED_FACE('',(#6366),#3447,.T.);
#45222=ADVANCED_FACE('',(#6367),#3448,.T.);
#45223=ADVANCED_FACE('',(#6368),#3449,.T.);
#45224=ADVANCED_FACE('',(#6369),#872,.T.);
#45225=ADVANCED_FACE('',(#6370),#3450,.T.);
#45226=ADVANCED_FACE('',(#6371),#3451,.T.);
#45227=ADVANCED_FACE('',(#6372),#873,.T.);
#45228=ADVANCED_FACE('',(#6373),#874,.T.);
#45229=ADVANCED_FACE('',(#6374),#3452,.T.);
#45230=ADVANCED_FACE('',(#6375),#3453,.T.);
#45231=ADVANCED_FACE('',(#6376),#42518,.F.);
#45232=ADVANCED_FACE('',(#6377),#42519,.F.);
#45233=ADVANCED_FACE('',(#6378),#3454,.T.);
#45234=ADVANCED_FACE('',(#6379),#3455,.T.);
#45235=ADVANCED_FACE('',(#6380),#875,.T.);
#45236=ADVANCED_FACE('',(#6381),#3456,.T.);
#45237=ADVANCED_FACE('',(#6382),#3457,.T.);
#45238=ADVANCED_FACE('',(#6383),#3458,.T.);
#45239=ADVANCED_FACE('',(#6384),#3459,.T.);
#45240=ADVANCED_FACE('',(#6385),#3460,.T.);
#45241=ADVANCED_FACE('',(#6386),#876,.T.);
#45242=ADVANCED_FACE('',(#6387),#3461,.T.);
#45243=ADVANCED_FACE('',(#6388),#877,.T.);
#45244=ADVANCED_FACE('',(#6389),#3462,.T.);
#45245=ADVANCED_FACE('',(#6390),#3463,.T.);
#45246=ADVANCED_FACE('',(#6391),#3464,.T.);
#45247=ADVANCED_FACE('',(#6392),#878,.T.);
#45248=ADVANCED_FACE('',(#6393),#3465,.T.);
#45249=ADVANCED_FACE('',(#6394),#3466,.T.);
#45250=ADVANCED_FACE('',(#6395),#879,.T.);
#45251=ADVANCED_FACE('',(#6396),#880,.T.);
#45252=ADVANCED_FACE('',(#6397),#3467,.T.);
#45253=ADVANCED_FACE('',(#6398),#3468,.T.);
#45254=ADVANCED_FACE('',(#6399),#42520,.F.);
#45255=ADVANCED_FACE('',(#6400),#42521,.T.);
#45256=ADVANCED_FACE('',(#6401),#42522,.T.);
#45257=ADVANCED_FACE('',(#6402,#3514),#3569,.F.);
#45258=ADVANCED_FACE('',(#6403,#3515),#3570,.T.);
#45259=ADVANCED_FACE('',(#6404,#3516),#3571,.F.);
#45260=ADVANCED_FACE('',(#6405),#42523,.F.);
#45261=ADVANCED_FACE('',(#6406),#42524,.T.);
#45262=ADVANCED_FACE('',(#6407,#3517),#3572,.T.);
#45263=ADVANCED_FACE('',(#6408,#3518),#3573,.F.);
#45264=ADVANCED_FACE('',(#6409),#42525,.T.);
#45265=ADVANCED_FACE('',(#6410),#42526,.T.);
#45266=ADVANCED_FACE('',(#6411),#42527,.F.);
#45267=ADVANCED_FACE('',(#6412),#42528,.F.);
#45268=ADVANCED_FACE('',(#6413),#42529,.T.);
#45269=ADVANCED_FACE('',(#6414),#42530,.T.);
#45270=ADVANCED_FACE('',(#6415),#42531,.T.);
#45271=ADVANCED_FACE('',(#6416),#42532,.T.);
#45272=ADVANCED_FACE('',(#6417),#42533,.T.);
#45273=ADVANCED_FACE('',(#6418),#42534,.T.);
#45274=ADVANCED_FACE('',(#6419),#42535,.T.);
#45275=ADVANCED_FACE('',(#6420),#42536,.T.);
#45276=ADVANCED_FACE('',(#6421),#42537,.T.);
#45277=ADVANCED_FACE('',(#6422),#42538,.T.);
#45278=ADVANCED_FACE('',(#6423),#42539,.T.);
#45279=ADVANCED_FACE('',(#6424),#42540,.T.);
#45280=ADVANCED_FACE('',(#6425),#42541,.T.);
#45281=ADVANCED_FACE('',(#6426),#42542,.T.);
#45282=ADVANCED_FACE('',(#6427),#42543,.T.);
#45283=ADVANCED_FACE('',(#6428),#42544,.T.);
#45284=ADVANCED_FACE('',(#6429),#42545,.T.);
#45285=ADVANCED_FACE('',(#6430),#42546,.T.);
#45286=ADVANCED_FACE('',(#6431),#42547,.T.);
#45287=ADVANCED_FACE('',(#6432),#42548,.T.);
#45288=ADVANCED_FACE('',(#6433),#42549,.T.);
#45289=ADVANCED_FACE('',(#6434),#42550,.T.);
#45290=ADVANCED_FACE('',(#6435),#42551,.T.);
#45291=ADVANCED_FACE('',(#6436),#42552,.T.);
#45292=ADVANCED_FACE('',(#6437),#42553,.T.);
#45293=ADVANCED_FACE('',(#6438),#42554,.T.);
#45294=ADVANCED_FACE('',(#6439),#42555,.T.);
#45295=ADVANCED_FACE('',(#6440),#42556,.T.);
#45296=ADVANCED_FACE('',(#6441),#42557,.T.);
#45297=ADVANCED_FACE('',(#6442),#42558,.T.);
#45298=ADVANCED_FACE('',(#6443),#42559,.T.);
#45299=ADVANCED_FACE('',(#6444),#42560,.T.);
#45300=ADVANCED_FACE('',(#6445),#42561,.T.);
#45301=ADVANCED_FACE('',(#6446),#42562,.T.);
#45302=ADVANCED_FACE('',(#6447),#42563,.T.);
#45303=ADVANCED_FACE('',(#6448),#42564,.T.);
#45304=ADVANCED_FACE('',(#6449),#42565,.T.);
#45305=ADVANCED_FACE('',(#6450),#42566,.T.);
#45306=ADVANCED_FACE('',(#6451),#42567,.T.);
#45307=ADVANCED_FACE('',(#6452),#42568,.T.);
#45308=ADVANCED_FACE('',(#6453),#42569,.T.);
#45309=ADVANCED_FACE('',(#6454),#42570,.T.);
#45310=ADVANCED_FACE('',(#6455),#42571,.T.);
#45311=ADVANCED_FACE('',(#6456),#42572,.T.);
#45312=ADVANCED_FACE('',(#6457),#42573,.T.);
#45313=ADVANCED_FACE('',(#6458),#42574,.T.);
#45314=ADVANCED_FACE('',(#6459),#42575,.T.);
#45315=ADVANCED_FACE('',(#6460),#42576,.T.);
#45316=ADVANCED_FACE('',(#6461),#42577,.T.);
#45317=ADVANCED_FACE('',(#6462),#42578,.T.);
#45318=ADVANCED_FACE('',(#6463),#42579,.T.);
#45319=ADVANCED_FACE('',(#6464,#3519),#3574,.F.);
#45320=ADVANCED_FACE('',(#6465,#3520),#3575,.T.);
#45321=ADVANCED_FACE('',(#6466,#3521),#3576,.T.);
#45322=ADVANCED_FACE('',(#6467,#3522),#3577,.T.);
#45323=ADVANCED_FACE('',(#6468),#3578,.T.);
#45324=ADVANCED_FACE('',(#6469),#3579,.T.);
#45325=ADVANCED_FACE('',(#6470),#3580,.F.);
#45326=ADVANCED_FACE('',(#6471),#3581,.F.);
#45327=ADVANCED_FACE('',(#6472),#3582,.F.);
#45328=ADVANCED_FACE('',(#6473),#3583,.F.);
#45329=ADVANCED_FACE('',(#6474),#3584,.F.);
#45330=ADVANCED_FACE('',(#6475),#3585,.F.);
#45331=ADVANCED_FACE('',(#6476),#3586,.F.);
#45332=ADVANCED_FACE('',(#6477),#3587,.F.);
#45333=ADVANCED_FACE('',(#6478),#3588,.F.);
#45334=ADVANCED_FACE('',(#6479),#3589,.F.);
#45335=ADVANCED_FACE('',(#6480),#3590,.F.);
#45336=ADVANCED_FACE('',(#6481),#3591,.F.);
#45337=ADVANCED_FACE('',(#6482),#3592,.F.);
#45338=ADVANCED_FACE('',(#6483),#3593,.F.);
#45339=ADVANCED_FACE('',(#6484),#3594,.F.);
#45340=ADVANCED_FACE('',(#6485),#3595,.F.);
#45341=ADVANCED_FACE('',(#6486),#3596,.F.);
#45342=ADVANCED_FACE('',(#6487),#3597,.F.);
#45343=ADVANCED_FACE('',(#6488),#3598,.F.);
#45344=ADVANCED_FACE('',(#6489),#3599,.F.);
#45345=ADVANCED_FACE('',(#6490),#3600,.F.);
#45346=ADVANCED_FACE('',(#6491),#3601,.F.);
#45347=ADVANCED_FACE('',(#6492),#3602,.F.);
#45348=ADVANCED_FACE('',(#6493),#3603,.F.);
#45349=ADVANCED_FACE('',(#6494),#3604,.F.);
#45350=ADVANCED_FACE('',(#6495),#3605,.F.);
#45351=ADVANCED_FACE('',(#6496),#3606,.F.);
#45352=ADVANCED_FACE('',(#6497),#3607,.F.);
#45353=ADVANCED_FACE('',(#6498),#3608,.F.);
#45354=ADVANCED_FACE('',(#6499),#3609,.F.);
#45355=ADVANCED_FACE('',(#6500),#3610,.F.);
#45356=ADVANCED_FACE('',(#6501),#3611,.F.);
#45357=ADVANCED_FACE('',(#6502),#3612,.F.);
#45358=ADVANCED_FACE('',(#6503),#3613,.F.);
#45359=ADVANCED_FACE('',(#6504),#3614,.F.);
#45360=ADVANCED_FACE('',(#6505),#3615,.F.);
#45361=ADVANCED_FACE('',(#6506),#3616,.F.);
#45362=ADVANCED_FACE('',(#6507),#3617,.F.);
#45363=ADVANCED_FACE('',(#6508),#3618,.F.);
#45364=ADVANCED_FACE('',(#6509),#3619,.F.);
#45365=ADVANCED_FACE('',(#6510),#3620,.F.);
#45366=ADVANCED_FACE('',(#6511),#3621,.F.);
#45367=ADVANCED_FACE('',(#6512),#3622,.F.);
#45368=ADVANCED_FACE('',(#6513),#3623,.F.);
#45369=ADVANCED_FACE('',(#6514),#3624,.F.);
#45370=ADVANCED_FACE('',(#6515),#3625,.F.);
#45371=ADVANCED_FACE('',(#6516),#3626,.F.);
#45372=ADVANCED_FACE('',(#6517),#3627,.F.);
#45373=ADVANCED_FACE('',(#6518),#3628,.F.);
#45374=ADVANCED_FACE('',(#6519),#3629,.F.);
#45375=ADVANCED_FACE('',(#6520),#3630,.F.);
#45376=ADVANCED_FACE('',(#6521),#3631,.F.);
#45377=ADVANCED_FACE('',(#6522),#3632,.F.);
#45378=ADVANCED_FACE('',(#6523),#3633,.F.);
#45379=ADVANCED_FACE('',(#6524),#3634,.F.);
#45380=ADVANCED_FACE('',(#6525),#3635,.F.);
#45381=ADVANCED_FACE('',(#6526),#3636,.F.);
#45382=ADVANCED_FACE('',(#6527),#3637,.F.);
#45383=ADVANCED_FACE('',(#6528),#3638,.F.);
#45384=ADVANCED_FACE('',(#6529),#3639,.F.);
#45385=ADVANCED_FACE('',(#6530),#3640,.F.);
#45386=ADVANCED_FACE('',(#6531),#3641,.F.);
#45387=ADVANCED_FACE('',(#6532),#3642,.F.);
#45388=ADVANCED_FACE('',(#6533),#3643,.F.);
#45389=ADVANCED_FACE('',(#6534),#3644,.F.);
#45390=ADVANCED_FACE('',(#6535),#3645,.F.);
#45391=ADVANCED_FACE('',(#6536),#3646,.F.);
#45392=ADVANCED_FACE('',(#6537),#3647,.F.);
#45393=ADVANCED_FACE('',(#6538),#3648,.F.);
#45394=ADVANCED_FACE('',(#6539),#3649,.F.);
#45395=ADVANCED_FACE('',(#6540),#3650,.F.);
#45396=ADVANCED_FACE('',(#6541),#3651,.F.);
#45397=ADVANCED_FACE('',(#6542),#3652,.F.);
#45398=ADVANCED_FACE('',(#6543),#3653,.F.);
#45399=ADVANCED_FACE('',(#6544),#3654,.F.);
#45400=ADVANCED_FACE('',(#6545),#3655,.F.);
#45401=ADVANCED_FACE('',(#6546),#3656,.F.);
#45402=ADVANCED_FACE('',(#6547),#3657,.F.);
#45403=ADVANCED_FACE('',(#6548),#3658,.F.);
#45404=ADVANCED_FACE('',(#6549),#3659,.F.);
#45405=ADVANCED_FACE('',(#6550),#3660,.F.);
#45406=ADVANCED_FACE('',(#6551),#3661,.F.);
#45407=ADVANCED_FACE('',(#6552),#3662,.F.);
#45408=ADVANCED_FACE('',(#6553),#3663,.F.);
#45409=ADVANCED_FACE('',(#6554),#3664,.F.);
#45410=ADVANCED_FACE('',(#6555),#3665,.F.);
#45411=ADVANCED_FACE('',(#6556),#3666,.F.);
#45412=ADVANCED_FACE('',(#6557),#3667,.F.);
#45413=ADVANCED_FACE('',(#6558),#3668,.F.);
#45414=ADVANCED_FACE('',(#6559),#3669,.F.);
#45415=ADVANCED_FACE('',(#6560),#3670,.F.);
#45416=ADVANCED_FACE('',(#6561),#3671,.F.);
#45417=ADVANCED_FACE('',(#6562),#3672,.F.);
#45418=ADVANCED_FACE('',(#6563),#3673,.F.);
#45419=ADVANCED_FACE('',(#6564),#3674,.F.);
#45420=ADVANCED_FACE('',(#6565),#3675,.F.);
#45421=ADVANCED_FACE('',(#6566),#3676,.F.);
#45422=ADVANCED_FACE('',(#6567),#3677,.F.);
#45423=ADVANCED_FACE('',(#6568),#3678,.F.);
#45424=ADVANCED_FACE('',(#6569),#3679,.F.);
#45425=ADVANCED_FACE('',(#6570),#3680,.F.);
#45426=ADVANCED_FACE('',(#6571),#3681,.F.);
#45427=ADVANCED_FACE('',(#6572),#42580,.F.);
#45428=ADVANCED_FACE('',(#6573,#3523),#42581,.F.);
#45429=ADVANCED_FACE('',(#6574),#42582,.F.);
#45430=ADVANCED_FACE('',(#6575),#42583,.T.);
#45431=ADVANCED_FACE('',(#6576,#3524),#42584,.F.);
#45432=ADVANCED_FACE('',(#6577),#883,.F.);
#45433=ADVANCED_FACE('',(#6578),#42585,.F.);
#45434=ADVANCED_FACE('',(#6579),#42586,.F.);
#45435=ADVANCED_FACE('',(#6580),#42587,.T.);
#45436=ADVANCED_FACE('',(#6581),#42588,.T.);
#45437=ADVANCED_FACE('',(#6582),#42589,.F.);
#45438=ADVANCED_FACE('',(#6583),#42590,.F.);
#45439=ADVANCED_FACE('',(#6584),#42591,.F.);
#45440=ADVANCED_FACE('',(#6585),#42592,.F.);
#45441=ADVANCED_FACE('',(#6586),#42593,.F.);
#45442=ADVANCED_FACE('',(#6587),#42594,.F.);
#45443=ADVANCED_FACE('',(#6588),#42595,.F.);
#45444=ADVANCED_FACE('',(#6589),#42596,.T.);
#45445=ADVANCED_FACE('',(#6590),#3682,.F.);
#45446=ADVANCED_FACE('',(#6591),#42597,.F.);
#45447=ADVANCED_FACE('',(#6592),#3683,.F.);
#45448=ADVANCED_FACE('',(#6593),#3684,.F.);
#45449=ADVANCED_FACE('',(#6594),#3685,.F.);
#45450=ADVANCED_FACE('',(#6595),#3686,.F.);
#45451=ADVANCED_FACE('',(#6596),#3687,.T.);
#45452=ADVANCED_FACE('',(#6597),#42598,.T.);
#45453=ADVANCED_FACE('',(#6598),#42599,.F.);
#45454=ADVANCED_FACE('',(#6599),#3688,.F.);
#45455=ADVANCED_FACE('',(#6600),#3689,.F.);
#45456=ADVANCED_FACE('',(#6601,#3525,#3526,#3527,#3528),#3690,.F.);
#45457=ADVANCED_FACE('',(#6602,#3529,#3530,#3531,#3532,#3533,#3534),#3691,
 .T.);
#45458=ADVANCED_FACE('',(#6603),#3692,.F.);
#45459=ADVANCED_FACE('',(#6604),#3693,.F.);
#45460=ADVANCED_FACE('',(#6605),#3694,.F.);
#45461=ADVANCED_FACE('',(#6606,#3535),#3695,.F.);
#45462=ADVANCED_FACE('',(#6607),#3696,.F.);
#45463=ADVANCED_FACE('',(#6608),#3697,.F.);
#45464=ADVANCED_FACE('',(#6609),#3698,.F.);
#45465=ADVANCED_FACE('',(#6610),#3699,.F.);
#45466=ADVANCED_FACE('',(#6611,#3536),#3700,.F.);
#45467=ADVANCED_FACE('',(#6612),#3701,.F.);
#45468=ADVANCED_FACE('',(#6613),#3702,.F.);
#45469=ADVANCED_FACE('',(#6614),#3703,.F.);
#45470=ADVANCED_FACE('',(#6615),#3704,.F.);
#45471=ADVANCED_FACE('',(#6616),#3705,.F.);
#45472=ADVANCED_FACE('',(#6617),#3706,.F.);
#45473=ADVANCED_FACE('',(#6618),#3707,.F.);
#45474=ADVANCED_FACE('',(#6619),#3708,.F.);
#45475=ADVANCED_FACE('',(#6620,#3537),#3709,.T.);
#45476=ADVANCED_FACE('',(#6621,#3538),#3710,.T.);
#45477=ADVANCED_FACE('',(#6622,#3539),#3711,.T.);
#45478=ADVANCED_FACE('',(#6623),#3712,.F.);
#45479=ADVANCED_FACE('',(#6624),#42600,.F.);
#45480=ADVANCED_FACE('',(#6625),#3713,.F.);
#45481=ADVANCED_FACE('',(#6626),#42601,.T.);
#45482=ADVANCED_FACE('',(#6627),#3714,.F.);
#45483=ADVANCED_FACE('',(#6628),#42602,.F.);
#45484=ADVANCED_FACE('',(#6629),#3715,.F.);
#45485=ADVANCED_FACE('',(#6630),#42603,.F.);
#45486=ADVANCED_FACE('',(#6631),#3716,.F.);
#45487=ADVANCED_FACE('',(#6632),#3717,.F.);
#45488=ADVANCED_FACE('',(#6633),#3718,.F.);
#45489=ADVANCED_FACE('',(#6634),#3719,.F.);
#45490=ADVANCED_FACE('',(#6635),#42604,.T.);
#45491=ADVANCED_FACE('',(#6636),#3720,.F.);
#45492=ADVANCED_FACE('',(#6637),#42605,.T.);
#45493=ADVANCED_FACE('',(#6638),#3721,.F.);
#45494=ADVANCED_FACE('',(#6639),#3722,.F.);
#45495=ADVANCED_FACE('',(#6640),#3723,.F.);
#45496=ADVANCED_FACE('',(#6641),#42606,.T.);
#45497=ADVANCED_FACE('',(#6642),#3724,.F.);
#45498=ADVANCED_FACE('',(#6643),#42607,.F.);
#45499=ADVANCED_FACE('',(#6644),#3725,.F.);
#45500=ADVANCED_FACE('',(#6645),#42608,.T.);
#45501=ADVANCED_FACE('',(#6646),#3726,.F.);
#45502=ADVANCED_FACE('',(#6647),#3727,.F.);
#45503=ADVANCED_FACE('',(#6648),#42609,.T.);
#45504=ADVANCED_FACE('',(#6649),#3728,.T.);
#45505=ADVANCED_FACE('',(#6650),#3729,.F.);
#45506=ADVANCED_FACE('',(#6651,#3540),#3730,.T.);
#45507=ADVANCED_FACE('',(#6652),#3731,.T.);
#45508=ADVANCED_FACE('',(#6653),#3732,.T.);
#45509=ADVANCED_FACE('',(#6654),#3733,.F.);
#45510=ADVANCED_FACE('',(#6655),#3734,.F.);
#45511=ADVANCED_FACE('',(#6656),#3735,.F.);
#45512=ADVANCED_FACE('',(#6657),#3736,.F.);
#45513=ADVANCED_FACE('',(#6658),#3737,.F.);
#45514=ADVANCED_FACE('',(#6659),#3738,.F.);
#45515=ADVANCED_FACE('',(#6660),#3739,.F.);
#45516=ADVANCED_FACE('',(#6661),#3740,.F.);
#45517=ADVANCED_FACE('',(#6662),#3741,.F.);
#45518=ADVANCED_FACE('',(#6663),#42610,.T.);
#45519=ADVANCED_FACE('',(#6664),#3742,.T.);
#45520=ADVANCED_FACE('',(#6665),#3743,.F.);
#45521=ADVANCED_FACE('',(#6666),#42611,.T.);
#45522=ADVANCED_FACE('',(#6667),#3744,.T.);
#45523=ADVANCED_FACE('',(#6668),#3745,.F.);
#45524=ADVANCED_FACE('',(#6669),#3746,.F.);
#45525=ADVANCED_FACE('',(#6670),#3747,.F.);
#45526=ADVANCED_FACE('',(#6671),#3748,.T.);
#45527=ADVANCED_FACE('',(#6672),#3749,.F.);
#45528=ADVANCED_FACE('',(#6673),#3750,.F.);
#45529=ADVANCED_FACE('',(#6674),#3751,.T.);
#45530=ADVANCED_FACE('',(#6675),#3752,.T.);
#45531=ADVANCED_FACE('',(#6676,#3541),#3753,.F.);
#45532=ADVANCED_FACE('',(#6677),#3754,.F.);
#45533=ADVANCED_FACE('',(#6678),#42612,.F.);
#45534=ADVANCED_FACE('',(#6679),#3755,.F.);
#45535=ADVANCED_FACE('',(#6680),#3756,.F.);
#45536=ADVANCED_FACE('',(#6681),#3757,.F.);
#45537=CLOSED_SHELL('',(#42613,#42614,#42615,#42616));
#45538=CLOSED_SHELL('',(#42617,#42618,#42619));
#45539=CLOSED_SHELL('',(#42620,#42621,#42622,#42623));
#45540=CLOSED_SHELL('',(#42624,#42625,#42626,#42627));
#45541=CLOSED_SHELL('',(#42628,#42629,#42630,#42631,#42632,#42633,#42634,
#42635,#42636,#42637,#42638,#42639,#42640,#42641,#42642,#42643,#42644,#42645,
#42646,#42647));
#45542=CLOSED_SHELL('',(#42648,#42649,#42650,#42651,#42652,#42653,#42654,
#42655,#42656,#42657,#42658,#42659,#42660,#42661,#42662,#42663,#42664,#42665,
#42666,#42667,#42668,#42669,#42670,#42671,#42672,#42673,#42674,#42675,#42676,
#42677,#42678,#42679,#42680,#42681,#42682,#42683,#42684,#42685,#42686,#42687,
#42688,#42689,#42690,#42691,#42692,#42693,#42694,#42695,#42696,#42697,#42698,
#42699,#42700,#42701,#42702,#42703,#42704,#42705,#42706,#42707,#42708,#42709,
#42710,#42711,#42712,#42713,#42714,#42715,#42716,#42717,#42718,#42719,#42720,
#42721,#42722,#42723,#42724,#42725,#42726,#42727,#42728,#42729,#42730,#42731,
#42732,#42733,#42734,#42735,#42736,#42737,#42738,#42739,#42740,#42741,#42742,
#42743,#42744,#42745,#42746,#42747,#42748,#42749,#42750,#42751,#42752,#42753,
#42754,#42755,#42756,#42757,#42758,#42759,#42760,#42761,#42762,#42763,#42764,
#42765,#42766,#42767,#42768,#42769,#42770,#42771,#42772,#42773,#42774,#42775,
#42776,#42777,#42778,#42779,#42780,#42781,#42782,#42783,#42784,#42785,#42786,
#42787,#42788,#42789,#42790,#42791,#42792,#42793,#42794,#42795,#42796,#42797,
#42798,#42799,#42800,#42801,#42802,#42803,#42804,#42805,#42806,#42807,#42808,
#42809,#42810,#42811,#42812,#42813,#42814,#42815,#42816,#42817,#42818,#42819,
#42820,#42821,#42822,#42823,#42824,#42825,#42826,#42827,#42828,#42829,#42830,
#42831,#42832,#42833,#42834,#42835,#42836,#42837,#42838,#42839,#42840,#42841,
#42842,#42843,#42844,#42845,#42846,#42847,#42848,#42849,#42850,#42851,#42852,
#42853,#42854,#42855,#42856,#42857,#42858,#42859,#42860,#42861,#42862,#42863,
#42864,#42865,#42866,#42867,#42868,#42869,#42870,#42871,#42872,#42873,#42874,
#42875,#42876,#42877,#42878,#42879,#42880,#42881,#42882,#42883,#42884,#42885,
#42886,#42887,#42888,#42889,#42890,#42891,#42892,#42893,#42894,#42895,#42896,
#42897,#42898,#42899,#42900,#42901,#42902,#42903,#42904,#42905,#42906,#42907,
#42908,#42909,#42910,#42911,#42912,#42913,#42914,#42915,#42916,#42917,#42918,
#42919,#42920,#42921,#42922,#42923,#42924,#42925,#42926,#42927,#42928,#42929,
#42930,#42931,#42932,#42933,#42934,#42935,#42936,#42937,#42938,#42939,#42940,
#42941,#42942,#42943,#42944,#42945,#42946,#42947,#42948,#42949,#42950,#42951,
#42952,#42953,#42954,#42955,#42956,#42957,#42958,#42959,#42960,#42961,#42962,
#42963,#42964,#42965,#42966,#42967,#42968,#42969,#42970,#42971,#42972,#42973,
#42974,#42975,#42976,#42977,#42978,#42979,#42980,#42981,#42982,#42983,#42984,
#42985,#42986,#42987,#42988,#42989,#42990,#42991,#42992,#42993,#42994,#42995,
#42996,#42997,#42998,#42999,#43000,#43001,#43002,#43003,#43004,#43005,#43006,
#43007,#43008,#43009,#43010,#43011,#43012,#43013,#43014,#43015,#43016,#43017,
#43018,#43019,#43020,#43021,#43022,#43023,#43024,#43025,#43026,#43027,#43028,
#43029,#43030,#43031,#43032,#43033,#43034,#43035,#43036,#43037,#43038,#43039,
#43040,#43041,#43042,#43043,#43044,#43045,#43046,#43047,#43048,#43049,#43050,
#43051,#43052,#43053,#43054,#43055,#43056,#43057,#43058,#43059,#43060,#43061,
#43062,#43063,#43064,#43065,#43066,#43067,#43068,#43069,#43070,#43071,#43072,
#43073,#43074,#43075,#43076,#43077,#43078,#43079,#43080,#43081,#43082,#43083,
#43084,#43085,#43086,#43087,#43088,#43089,#43090,#43091,#43092,#43093,#43094,
#43095,#43096,#43097,#43098,#43099,#43100,#43101,#43102,#43103,#43104,#43105,
#43106,#43107,#43108,#43109,#43110,#43111,#43112,#43113,#43114,#43115,#43116,
#43117,#43118,#43119,#43120,#43121,#43122,#43123,#43124,#43125,#43126,#43127,
#43128,#43129,#43130,#43131,#43132,#43133,#43134,#43135,#43136,#43137,#43138,
#43139,#43140,#43141,#43142,#43143,#43144,#43145,#43146,#43147,#43148,#43149,
#43150,#43151,#43152,#43153,#43154,#43155,#43156,#43157,#43158,#43159,#43160,
#43161,#43162,#43163,#43164,#43165,#43166,#43167,#43168,#43169,#43170,#43171,
#43172,#43173,#43174,#43175,#43176,#43177,#43178,#43179,#43180,#43181,#43182,
#43183,#43184,#43185,#43186,#43187,#43188,#43189,#43190,#43191,#43192,#43193,
#43194,#43195,#43196,#43197,#43198,#43199,#43200,#43201,#43202,#43203,#43204,
#43205,#43206,#43207,#43208,#43209,#43210,#43211,#43212,#43213,#43214,#43215,
#43216,#43217,#43218,#43219,#43220,#43221,#43222,#43223,#43224,#43225,#43226,
#43227,#43228,#43229,#43230,#43231,#43232,#43233,#43234,#43235,#43236,#43237,
#43238,#43239,#43240,#43241,#43242,#43243,#43244,#43245,#43246,#43247,#43248,
#43249,#43250,#43251,#43252,#43253,#43254,#43255,#43256,#43257,#43258,#43259,
#43260,#43261,#43262,#43263,#43264,#43265,#43266,#43267,#43268,#43269,#43270,
#43271,#43272,#43273,#43274,#43275,#43276,#43277,#43278,#43279,#43280,#43281,
#43282,#43283,#43284,#43285,#43286,#43287,#43288,#43289,#43290,#43291,#43292,
#43293,#43294,#43295,#43296,#43297,#43298,#43299,#43300,#43301,#43302,#43303,
#43304,#43305,#43306,#43307,#43308,#43309,#43310,#43311,#43312,#43313,#43314,
#43315,#43316,#43317,#43318,#43319,#43320,#43321,#43322,#43323,#43324,#43325,
#43326,#43327,#43328,#43329,#43330,#43331,#43332,#43333,#43334,#43335,#43336,
#43337,#43338,#43339,#43340,#43341,#43342,#43343,#43344,#43345,#43346,#43347,
#43348,#43349,#43350,#43351,#43352,#43353,#43354,#43355,#43356,#43357,#43358,
#43359,#43360,#43361,#43362,#43363,#43364,#43365,#43366,#43367,#43368,#43369,
#43370,#43371,#43372,#43373,#43374,#43375,#43376,#43377,#43378,#43379,#43380,
#43381,#43382,#43383,#43384,#43385,#43386,#43387,#43388,#43389,#43390,#43391,
#43392,#43393,#43394,#43395,#43396,#43397,#43398,#43399,#43400,#43401,#43402,
#43403,#43404,#43405,#43406,#43407,#43408,#43409,#43410,#43411,#43412,#43413,
#43414,#43415,#43416,#43417,#43418,#43419,#43420,#43421,#43422,#43423,#43424,
#43425,#43426,#43427,#43428,#43429,#43430,#43431,#43432,#43433,#43434,#43435,
#43436,#43437,#43438,#43439,#43440,#43441,#43442,#43443,#43444,#43445,#43446,
#43447,#43448,#43449,#43450,#43451,#43452,#43453,#43454,#43455,#43456,#43457,
#43458,#43459,#43460,#43461,#43462,#43463,#43464,#43465,#43466,#43467,#43468,
#43469,#43470,#43471,#43472,#43473,#43474,#43475,#43476,#43477,#43478,#43479,
#43480,#43481,#43482,#43483,#43484,#43485,#43486,#43487,#43488,#43489,#43490,
#43491,#43492,#43493,#43494,#43495,#43496,#43497,#43498,#43499,#43500,#43501,
#43502,#43503,#43504,#43505,#43506,#43507,#43508,#43509,#43510,#43511,#43512,
#43513,#43514,#43515,#43516,#43517,#43518,#43519,#43520,#43521,#43522,#43523,
#43524,#43525,#43526,#43527,#43528,#43529,#43530,#43531,#43532,#43533,#43534,
#43535,#43536,#43537,#43538,#43539,#43540,#43541,#43542,#43543,#43544,#43545,
#43546,#43547,#43548,#43549,#43550,#43551,#43552,#43553,#43554,#43555,#43556,
#43557,#43558,#43559,#43560,#43561,#43562,#43563,#43564,#43565,#43566,#43567,
#43568,#43569,#43570,#43571,#43572,#43573,#43574,#43575,#43576,#43577,#43578,
#43579,#43580,#43581,#43582,#43583,#43584,#43585,#43586,#43587,#43588,#43589,
#43590,#43591,#43592,#43593,#43594,#43595,#43596,#43597,#43598,#43599,#43600,
#43601,#43602,#43603,#43604,#43605,#43606,#43607,#43608,#43609,#43610,#43611,
#43612,#43613,#43614,#43615,#43616,#43617,#43618,#43619,#43620,#43621,#43622,
#43623,#43624,#43625,#43626,#43627,#43628,#43629,#43630,#43631,#43632,#43633,
#43634,#43635,#43636,#43637,#43638,#43639,#43640,#43641,#43642,#43643,#43644,
#43645,#43646,#43647,#43648,#43649,#43650,#43651,#43652,#43653,#43654,#43655,
#43656,#43657,#43658,#43659,#43660,#43661,#43662,#43663,#43664,#43665,#43666,
#43667,#43668,#43669,#43670,#43671,#43672,#43673,#43674,#43675,#43676,#43677,
#43678,#43679,#43680,#43681,#43682,#43683,#43684,#43685,#43686,#43687,#43688,
#43689,#43690,#43691,#43692,#43693,#43694,#43695,#43696,#43697,#43698,#43699,
#43700,#43701,#43702,#43703,#43704,#43705,#43706,#43707,#43708,#43709,#43710,
#43711,#43712,#43713,#43714,#43715,#43716,#43717,#43718,#43719,#43720,#43721,
#43722,#43723,#43724,#43725,#43726,#43727,#43728,#43729,#43730,#43731,#43732,
#43733,#43734,#43735,#43736,#43737,#43738,#43739,#43740,#43741,#43742,#43743,
#43744,#43745,#43746,#43747,#43748,#43749,#43750,#43751,#43752,#43753,#43754,
#43755,#43756,#43757,#43758,#43759,#43760,#43761,#43762,#43763,#43764,#43765,
#43766,#43767,#43768,#43769,#43770,#43771,#43772,#43773,#43774,#43775,#43776,
#43777,#43778,#43779,#43780,#43781,#43782,#43783,#43784,#43785,#43786,#43787,
#43788,#43789,#43790,#43791,#43792,#43793,#43794,#43795,#43796,#43797,#43798,
#43799,#43800,#43801,#43802,#43803,#43804,#43805,#43806,#43807,#43808,#43809,
#43810,#43811,#43812,#43813,#43814,#43815,#43816,#43817,#43818,#43819,#43820,
#43821,#43822,#43823,#43824,#43825,#43826,#43827,#43828,#43829,#43830,#43831,
#43832,#43833,#43834,#43835,#43836,#43837,#43838,#43839,#43840,#43841,#43842,
#43843,#43844,#43845,#43846,#43847,#43848,#43849,#43850,#43851,#43852,#43853,
#43854,#43855,#43856,#43857,#43858,#43859,#43860,#43861,#43862,#43863,#43864,
#43865,#43866,#43867,#43868,#43869,#43870,#43871,#43872,#43873,#43874,#43875,
#43876,#43877,#43878,#43879,#43880,#43881,#43882,#43883,#43884,#43885,#43886,
#43887,#43888,#43889,#43890,#43891,#43892,#43893,#43894,#43895,#43896,#43897,
#43898,#43899,#43900,#43901,#43902,#43903,#43904,#43905,#43906,#43907,#43908,
#43909,#43910,#43911,#43912,#43913,#43914,#43915,#43916,#43917,#43918,#43919,
#43920,#43921,#43922,#43923,#43924,#43925,#43926,#43927,#43928,#43929,#43930,
#43931,#43932,#43933,#43934,#43935,#43936,#43937,#43938,#43939,#43940,#43941,
#43942,#43943,#43944,#43945,#43946,#43947,#43948,#43949,#43950,#43951,#43952,
#43953,#43954,#43955,#43956,#43957,#43958,#43959,#43960,#43961,#43962,#43963,
#43964,#43965,#43966,#43967,#43968,#43969,#43970,#43971,#43972,#43973,#43974,
#43975,#43976,#43977,#43978,#43979,#43980,#43981,#43982,#43983,#43984,#43985,
#43986,#43987,#43988,#43989,#43990,#43991,#43992,#43993,#43994,#43995,#43996,
#43997,#43998,#43999,#44000,#44001,#44002,#44003,#44004,#44005,#44006,#44007,
#44008,#44009,#44010,#44011,#44012,#44013,#44014,#44015,#44016,#44017,#44018,
#44019,#44020,#44021,#44022,#44023,#44024,#44025,#44026,#44027,#44028,#44029,
#44030,#44031,#44032,#44033,#44034,#44035,#44036,#44037,#44038,#44039,#44040,
#44041,#44042,#44043,#44044,#44045,#44046,#44047,#44048,#44049,#44050,#44051,
#44052,#44053,#44054,#44055,#44056,#44057,#44058,#44059,#44060,#44061,#44062,
#44063,#44064,#44065,#44066,#44067,#44068,#44069,#44070,#44071,#44072,#44073,
#44074,#44075,#44076,#44077,#44078,#44079,#44080,#44081,#44082,#44083,#44084,
#44085,#44086,#44087,#44088,#44089,#44090,#44091,#44092,#44093,#44094,#44095,
#44096,#44097,#44098,#44099,#44100,#44101,#44102,#44103,#44104,#44105,#44106,
#44107,#44108,#44109,#44110,#44111,#44112,#44113,#44114,#44115,#44116,#44117,
#44118,#44119,#44120,#44121,#44122,#44123,#44124,#44125,#44126,#44127,#44128,
#44129,#44130,#44131,#44132,#44133,#44134,#44135,#44136,#44137,#44138,#44139,
#44140,#44141,#44142,#44143,#44144,#44145,#44146,#44147,#44148,#44149,#44150,
#44151,#44152,#44153,#44154,#44155,#44156,#44157,#44158,#44159,#44160,#44161,
#44162,#44163,#44164,#44165,#44166,#44167,#44168,#44169,#44170,#44171,#44172,
#44173,#44174,#44175,#44176,#44177,#44178,#44179,#44180,#44181,#44182,#44183,
#44184,#44185,#44186,#44187,#44188,#44189,#44190,#44191,#44192,#44193,#44194,
#44195,#44196,#44197,#44198,#44199,#44200,#44201,#44202,#44203,#44204,#44205,
#44206,#44207,#44208,#44209,#44210,#44211,#44212,#44213,#44214,#44215,#44216,
#44217,#44218,#44219,#44220,#44221,#44222,#44223,#44224,#44225,#44226,#44227,
#44228,#44229,#44230,#44231,#44232,#44233,#44234,#44235,#44236,#44237,#44238,
#44239,#44240,#44241,#44242,#44243,#44244,#44245,#44246,#44247,#44248,#44249,
#44250,#44251,#44252,#44253,#44254,#44255,#44256,#44257,#44258,#44259,#44260,
#44261,#44262,#44263,#44264,#44265,#44266,#44267,#44268,#44269,#44270,#44271,
#44272,#44273,#44274,#44275,#44276,#44277,#44278,#44279,#44280,#44281,#44282,
#44283,#44284,#44285,#44286,#44287,#44288,#44289,#44290,#44291,#44292,#44293,
#44294,#44295,#44296,#44297,#44298,#44299,#44300,#44301,#44302,#44303,#44304,
#44305,#44306,#44307,#44308,#44309,#44310,#44311,#44312,#44313,#44314,#44315,
#44316,#44317,#44318,#44319,#44320,#44321,#44322,#44323,#44324,#44325,#44326,
#44327,#44328,#44329,#44330,#44331,#44332,#44333,#44334,#44335,#44336,#44337,
#44338,#44339,#44340,#44341,#44342,#44343,#44344,#44345,#44346,#44347,#44348,
#44349,#44350,#44351,#44352,#44353,#44354,#44355,#44356,#44357,#44358,#44359,
#44360,#44361,#44362,#44363,#44364,#44365,#44366,#44367,#44368,#44369,#44370,
#44371,#44372,#44373,#44374,#44375,#44376,#44377,#44378,#44379,#44380,#44381,
#44382,#44383,#44384,#44385,#44386,#44387,#44388,#44389,#44390,#44391,#44392,
#44393,#44394,#44395,#44396,#44397,#44398,#44399,#44400,#44401,#44402,#44403,
#44404,#44405,#44406,#44407,#44408,#44409,#44410,#44411,#44412,#44413,#44414,
#44415,#44416,#44417,#44418,#44419,#44420,#44421,#44422,#44423,#44424,#44425,
#44426,#44427,#44428,#44429,#44430,#44431,#44432,#44433,#44434,#44435,#44436,
#44437,#44438,#44439,#44440,#44441,#44442,#44443,#44444,#44445,#44446,#44447,
#44448,#44449,#44450,#44451,#44452,#44453,#44454,#44455,#44456,#44457,#44458,
#44459,#44460,#44461,#44462,#44463,#44464,#44465,#44466,#44467,#44468,#44469,
#44470,#44471,#44472,#44473,#44474,#44475,#44476,#44477,#44478,#44479,#44480,
#44481,#44482,#44483,#44484,#44485,#44486,#44487,#44488,#44489,#44490,#44491,
#44492,#44493,#44494,#44495,#44496,#44497,#44498,#44499,#44500,#44501,#44502,
#44503,#44504,#44505,#44506,#44507,#44508,#44509,#44510,#44511,#44512,#44513,
#44514,#44515,#44516,#44517,#44518,#44519,#44520,#44521,#44522,#44523,#44524,
#44525,#44526,#44527,#44528,#44529,#44530,#44531,#44532,#44533,#44534,#44535,
#44536,#44537,#44538,#44539,#44540,#44541,#44542,#44543,#44544,#44545,#44546,
#44547,#44548,#44549,#44550,#44551,#44552,#44553,#44554,#44555,#44556,#44557,
#44558,#44559,#44560,#44561,#44562,#44563,#44564,#44565,#44566,#44567,#44568,
#44569,#44570,#44571,#44572,#44573,#44574,#44575,#44576,#44577,#44578,#44579,
#44580,#44581,#44582,#44583,#44584,#44585,#44586,#44587,#44588,#44589,#44590,
#44591,#44592,#44593,#44594,#44595,#44596,#44597,#44598,#44599,#44600,#44601,
#44602,#44603,#44604,#44605,#44606,#44607,#44608,#44609,#44610,#44611,#44612,
#44613,#44614,#44615,#44616,#44617,#44618,#44619,#44620,#44621,#44622,#44623,
#44624,#44625,#44626,#44627,#44628,#44629,#44630,#44631,#44632,#44633,#44634,
#44635,#44636,#44637,#44638,#44639,#44640,#44641,#44642,#44643,#44644,#44645,
#44646,#44647,#44648,#44649,#44650,#44651,#44652,#44653,#44654,#44655,#44656,
#44657,#44658,#44659,#44660,#44661,#44662,#44663,#44664,#44665,#44666,#44667,
#44668,#44669,#44670,#44671,#44672,#44673,#44674,#44675,#44676,#44677,#44678,
#44679,#44680,#44681,#44682,#44683,#44684,#44685,#44686,#44687,#44688,#44689,
#44690,#44691,#44692,#44693,#44694,#44695,#44696,#44697,#44698,#44699,#44700,
#44701,#44702,#44703,#44704,#44705,#44706,#44707,#44708,#44709,#44710,#44711,
#44712,#44713,#44714,#44715,#44716,#44717,#44718,#44719,#44720,#44721,#44722,
#44723,#44724,#44725,#44726,#44727,#44728,#44729,#44730,#44731,#44732,#44733,
#44734,#44735,#44736,#44737,#44738,#44739,#44740,#44741,#44742,#44743,#44744,
#44745,#44746,#44747,#44748,#44749,#44750,#44751,#44752,#44753,#44754,#44755,
#44756,#44757,#44758,#44759,#44760,#44761,#44762,#44763,#44764,#44765,#44766,
#44767,#44768,#44769,#44770,#44771,#44772,#44773,#44774,#44775,#44776,#44777,
#44778,#44779,#44780,#44781,#44782,#44783,#44784,#44785,#44786,#44787,#44788,
#44789,#44790,#44791,#44792,#44793,#44794,#44795,#44796,#44797,#44798,#44799,
#44800,#44801,#44802,#44803,#44804,#44805,#44806,#44807,#44808,#44809,#44810,
#44811,#44812,#44813,#44814,#44815,#44816,#44817,#44818,#44819,#44820,#44821,
#44822,#44823,#44824,#44825,#44826,#44827,#44828,#44829,#44830,#44831,#44832,
#44833,#44834,#44835,#44836,#44837,#44838,#44839,#44840,#44841,#44842,#44843,
#44844,#44845,#44846,#44847,#44848,#44849,#44850,#44851,#44852,#44853,#44854,
#44855,#44856,#44857,#44858,#44859,#44860,#44861,#44862,#44863,#44864,#44865,
#44866,#44867,#44868,#44869,#44870,#44871,#44872,#44873,#44874,#44875,#44876,
#44877,#44878,#44879,#44880,#44881,#44882,#44883,#44884,#44885,#44886,#44887,
#44888,#44889,#44890,#44891,#44892,#44893,#44894,#44895,#44896,#44897,#44898,
#44899,#44900,#44901,#44902,#44903,#44904,#44905,#44906,#44907,#44908,#44909,
#44910,#44911,#44912,#44913,#44914,#44915,#44916,#44917,#44918,#44919,#44920,
#44921,#44922,#44923,#44924,#44925,#44926,#44927,#44928,#44929,#44930,#44931,
#44932,#44933,#44934,#44935,#44936,#44937,#44938,#44939,#44940,#44941,#44942,
#44943,#44944,#44945,#44946,#44947,#44948,#44949,#44950,#44951,#44952,#44953,
#44954,#44955,#44956,#44957,#44958,#44959,#44960,#44961,#44962,#44963,#44964,
#44965,#44966,#44967,#44968,#44969,#44970,#44971,#44972,#44973,#44974,#44975,
#44976,#44977,#44978,#44979,#44980,#44981,#44982,#44983,#44984,#44985,#44986,
#44987,#44988,#44989,#44990,#44991,#44992,#44993,#44994,#44995,#44996,#44997,
#44998,#44999,#45000,#45001,#45002,#45003,#45004,#45005,#45006,#45007,#45008,
#45009,#45010,#45011,#45012,#45013,#45014,#45015,#45016,#45017,#45018,#45019,
#45020,#45021,#45022,#45023,#45024,#45025,#45026,#45027,#45028,#45029,#45030,
#45031,#45032,#45033,#45034,#45035,#45036,#45037,#45038,#45039,#45040,#45041,
#45042,#45043,#45044,#45045,#45046,#45047,#45048,#45049,#45050,#45051,#45052,
#45053,#45054,#45055,#45056,#45057,#45058,#45059,#45060,#45061,#45062,#45063,
#45064,#45065,#45066,#45067,#45068,#45069,#45070,#45071,#45072,#45073,#45074,
#45075,#45076,#45077,#45078,#45079,#45080,#45081,#45082,#45083,#45084,#45085,
#45086,#45087,#45088,#45089,#45090,#45091,#45092,#45093,#45094,#45095,#45096,
#45097,#45098,#45099,#45100,#45101,#45102,#45103,#45104,#45105,#45106,#45107,
#45108,#45109,#45110,#45111,#45112,#45113,#45114,#45115,#45116,#45117,#45118,
#45119,#45120,#45121,#45122,#45123,#45124,#45125,#45126,#45127,#45128,#45129,
#45130,#45131,#45132,#45133,#45134,#45135,#45136,#45137,#45138,#45139,#45140,
#45141,#45142,#45143,#45144,#45145,#45146,#45147,#45148,#45149,#45150,#45151,
#45152,#45153,#45154,#45155,#45156,#45157,#45158,#45159,#45160,#45161,#45162,
#45163,#45164,#45165,#45166,#45167,#45168,#45169,#45170,#45171,#45172,#45173,
#45174,#45175,#45176,#45177,#45178,#45179,#45180,#45181,#45182,#45183,#45184,
#45185,#45186,#45187,#45188,#45189,#45190,#45191,#45192,#45193,#45194,#45195,
#45196,#45197,#45198,#45199,#45200,#45201,#45202,#45203,#45204,#45205,#45206,
#45207,#45208,#45209,#45210,#45211,#45212,#45213,#45214,#45215,#45216,#45217,
#45218,#45219,#45220,#45221,#45222,#45223,#45224,#45225,#45226,#45227,#45228,
#45229,#45230,#45231,#45232,#45233,#45234,#45235,#45236,#45237,#45238,#45239,
#45240,#45241,#45242,#45243,#45244,#45245,#45246,#45247,#45248,#45249,#45250,
#45251,#45252,#45253));
#45543=CLOSED_SHELL('',(#45254,#45255,#45256,#45257,#45258,#45259));
#45544=CLOSED_SHELL('',(#45260,#45261,#45262,#45263));
#45545=CLOSED_SHELL('',(#45264,#45265,#45266,#45267,#45268,#45269,#45270,
#45271,#45272,#45273,#45274,#45275,#45276,#45277,#45278,#45279,#45280,#45281,
#45282,#45283,#45284,#45285,#45286,#45287,#45288,#45289,#45290,#45291,#45292,
#45293,#45294,#45295,#45296,#45297,#45298,#45299,#45300,#45301,#45302,#45303,
#45304,#45305,#45306,#45307,#45308,#45309,#45310,#45311,#45312,#45313,#45314,
#45315,#45316,#45317,#45318,#45319,#45320,#45321,#45322,#45323,#45324,#45325,
#45326,#45327,#45328,#45329,#45330,#45331,#45332,#45333,#45334,#45335,#45336,
#45337,#45338,#45339,#45340,#45341,#45342,#45343,#45344,#45345,#45346,#45347,
#45348,#45349,#45350,#45351,#45352,#45353,#45354,#45355,#45356,#45357,#45358,
#45359,#45360,#45361,#45362,#45363,#45364,#45365,#45366,#45367,#45368,#45369,
#45370,#45371,#45372,#45373,#45374,#45375,#45376,#45377,#45378,#45379,#45380,
#45381,#45382,#45383,#45384,#45385,#45386,#45387,#45388,#45389,#45390,#45391,
#45392,#45393,#45394,#45395,#45396,#45397,#45398,#45399,#45400,#45401,#45402,
#45403,#45404,#45405,#45406,#45407,#45408,#45409,#45410,#45411,#45412,#45413,
#45414,#45415,#45416,#45417,#45418,#45419,#45420,#45421,#45422,#45423,#45424,
#45425,#45426));
#45546=CLOSED_SHELL('',(#45427,#45428,#45429,#45430,#45431,#45432,#45433,
#45434,#45435,#45436,#45437,#45438,#45439,#45440,#45441,#45442,#45443,#45444,
#45445,#45446,#45447,#45448,#45449,#45450,#45451,#45452,#45453,#45454,#45455,
#45456,#45457,#45458,#45459,#45460,#45461,#45462,#45463,#45464,#45465,#45466,
#45467,#45468,#45469,#45470,#45471,#45472,#45473,#45474,#45475,#45476,#45477,
#45478,#45479,#45480,#45481,#45482,#45483,#45484,#45485,#45486,#45487,#45488,
#45489,#45490,#45491,#45492,#45493,#45494,#45495,#45496,#45497,#45498,#45499,
#45500,#45501,#45502,#45503,#45504,#45505,#45506,#45507,#45508,#45509,#45510,
#45511,#45512,#45513,#45514,#45515,#45516,#45517,#45518,#45519,#45520,#45521,
#45522,#45523,#45524,#45525,#45526,#45527,#45528,#45529,#45530,#45531,#45532,
#45533,#45534,#45535,#45536));
#45547=DERIVED_UNIT_ELEMENT(#45567,1.);
#45548=DERIVED_UNIT_ELEMENT(#107911,-3.);
#45549=DERIVED_UNIT_ELEMENT(#45567,1.);
#45550=DERIVED_UNIT_ELEMENT(#107911,-3.);
#45551=DERIVED_UNIT_ELEMENT(#45567,1.);
#45552=DERIVED_UNIT_ELEMENT(#107911,-3.);
#45553=DERIVED_UNIT_ELEMENT(#45567,1.);
#45554=DERIVED_UNIT_ELEMENT(#107911,-3.);
#45555=DERIVED_UNIT_ELEMENT(#45567,1.);
#45556=DERIVED_UNIT_ELEMENT(#107911,-3.);
#45557=DERIVED_UNIT_ELEMENT(#45567,1.);
#45558=DERIVED_UNIT_ELEMENT(#107911,-3.);
#45559=DERIVED_UNIT_ELEMENT(#45567,1.);
#45560=DERIVED_UNIT_ELEMENT(#107911,-3.);
#45561=DERIVED_UNIT_ELEMENT(#45567,1.);
#45562=DERIVED_UNIT_ELEMENT(#107911,-3.);
#45563=DERIVED_UNIT_ELEMENT(#45567,1.);
#45564=DERIVED_UNIT_ELEMENT(#107911,-3.);
#45565=DERIVED_UNIT_ELEMENT(#45567,1.);
#45566=DERIVED_UNIT_ELEMENT(#107911,-3.);
#45567=(
MASS_UNIT()
NAMED_UNIT(*)
SI_UNIT(.KILO.,.GRAM.)
);
#45568=DERIVED_UNIT((#45547,#45548));
#45569=DERIVED_UNIT((#45549,#45550));
#45570=DERIVED_UNIT((#45551,#45552));
#45571=DERIVED_UNIT((#45553,#45554));
#45572=DERIVED_UNIT((#45555,#45556));
#45573=DERIVED_UNIT((#45557,#45558));
#45574=DERIVED_UNIT((#45559,#45560));
#45575=DERIVED_UNIT((#45561,#45562));
#45576=DERIVED_UNIT((#45563,#45564));
#45577=DERIVED_UNIT((#45565,#45566));
#45578=MEASURE_REPRESENTATION_ITEM('density measure',
POSITIVE_RATIO_MEASURE(7850.),#45568);
#45579=MEASURE_REPRESENTATION_ITEM('density measure',
POSITIVE_RATIO_MEASURE(7850.),#45569);
#45580=MEASURE_REPRESENTATION_ITEM('density measure',
POSITIVE_RATIO_MEASURE(7850.),#45570);
#45581=MEASURE_REPRESENTATION_ITEM('density measure',
POSITIVE_RATIO_MEASURE(7850.),#45571);
#45582=MEASURE_REPRESENTATION_ITEM('density measure',
POSITIVE_RATIO_MEASURE(7850.),#45572);
#45583=MEASURE_REPRESENTATION_ITEM('density measure',
POSITIVE_RATIO_MEASURE(7850.),#45573);
#45584=MEASURE_REPRESENTATION_ITEM('density measure',
POSITIVE_RATIO_MEASURE(7850.),#45574);
#45585=MEASURE_REPRESENTATION_ITEM('density measure',
POSITIVE_RATIO_MEASURE(7850.),#45575);
#45586=MEASURE_REPRESENTATION_ITEM('density measure',
POSITIVE_RATIO_MEASURE(7850.),#45576);
#45587=MEASURE_REPRESENTATION_ITEM('density measure',
POSITIVE_RATIO_MEASURE(7850.),#45577);
#45588=PROPERTY_DEFINITION_REPRESENTATION(#45638,#45608);
#45589=PROPERTY_DEFINITION_REPRESENTATION(#45639,#45609);
#45590=PROPERTY_DEFINITION_REPRESENTATION(#45640,#45610);
#45591=PROPERTY_DEFINITION_REPRESENTATION(#45641,#45611);
#45592=PROPERTY_DEFINITION_REPRESENTATION(#45642,#45612);
#45593=PROPERTY_DEFINITION_REPRESENTATION(#45643,#45613);
#45594=PROPERTY_DEFINITION_REPRESENTATION(#45644,#45614);
#45595=PROPERTY_DEFINITION_REPRESENTATION(#45645,#45615);
#45596=PROPERTY_DEFINITION_REPRESENTATION(#45646,#45616);
#45597=PROPERTY_DEFINITION_REPRESENTATION(#45647,#45617);
#45598=PROPERTY_DEFINITION_REPRESENTATION(#45648,#45618);
#45599=PROPERTY_DEFINITION_REPRESENTATION(#45649,#45619);
#45600=PROPERTY_DEFINITION_REPRESENTATION(#45650,#45620);
#45601=PROPERTY_DEFINITION_REPRESENTATION(#45651,#45621);
#45602=PROPERTY_DEFINITION_REPRESENTATION(#45652,#45622);
#45603=PROPERTY_DEFINITION_REPRESENTATION(#45653,#45623);
#45604=PROPERTY_DEFINITION_REPRESENTATION(#45654,#45624);
#45605=PROPERTY_DEFINITION_REPRESENTATION(#45655,#45625);
#45606=PROPERTY_DEFINITION_REPRESENTATION(#45656,#45626);
#45607=PROPERTY_DEFINITION_REPRESENTATION(#45657,#45627);
#45608=REPRESENTATION('material name',(#45628),#107900);
#45609=REPRESENTATION('density',(#45578),#107900);
#45610=REPRESENTATION('material name',(#45629),#107901);
#45611=REPRESENTATION('density',(#45579),#107901);
#45612=REPRESENTATION('material name',(#45630),#107902);
#45613=REPRESENTATION('density',(#45580),#107902);
#45614=REPRESENTATION('material name',(#45631),#107903);
#45615=REPRESENTATION('density',(#45581),#107903);
#45616=REPRESENTATION('material name',(#45632),#107904);
#45617=REPRESENTATION('density',(#45582),#107904);
#45618=REPRESENTATION('material name',(#45633),#107905);
#45619=REPRESENTATION('density',(#45583),#107905);
#45620=REPRESENTATION('material name',(#45634),#107906);
#45621=REPRESENTATION('density',(#45584),#107906);
#45622=REPRESENTATION('material name',(#45635),#107907);
#45623=REPRESENTATION('density',(#45585),#107907);
#45624=REPRESENTATION('material name',(#45636),#107908);
#45625=REPRESENTATION('density',(#45586),#107908);
#45626=REPRESENTATION('material name',(#45637),#107909);
#45627=REPRESENTATION('density',(#45587),#107909);
#45628=DESCRIPTIVE_REPRESENTATION_ITEM('Steel','Steel');
#45629=DESCRIPTIVE_REPRESENTATION_ITEM('Steel','Steel');
#45630=DESCRIPTIVE_REPRESENTATION_ITEM('Steel','Steel');
#45631=DESCRIPTIVE_REPRESENTATION_ITEM('Steel','Steel');
#45632=DESCRIPTIVE_REPRESENTATION_ITEM('Steel','Steel');
#45633=DESCRIPTIVE_REPRESENTATION_ITEM('Steel','Steel');
#45634=DESCRIPTIVE_REPRESENTATION_ITEM('Steel','Steel');
#45635=DESCRIPTIVE_REPRESENTATION_ITEM('Steel','Steel');
#45636=DESCRIPTIVE_REPRESENTATION_ITEM('Steel','Steel');
#45637=DESCRIPTIVE_REPRESENTATION_ITEM('Steel','Steel');
#45638=PROPERTY_DEFINITION('material property','material name',#107959);
#45639=PROPERTY_DEFINITION('material property','density of part',#107959);
#45640=PROPERTY_DEFINITION('material property','material name',#107960);
#45641=PROPERTY_DEFINITION('material property','density of part',#107960);
#45642=PROPERTY_DEFINITION('material property','material name',#107961);
#45643=PROPERTY_DEFINITION('material property','density of part',#107961);
#45644=PROPERTY_DEFINITION('material property','material name',#107962);
#45645=PROPERTY_DEFINITION('material property','density of part',#107962);
#45646=PROPERTY_DEFINITION('material property','material name',#107963);
#45647=PROPERTY_DEFINITION('material property','density of part',#107963);
#45648=PROPERTY_DEFINITION('material property','material name',#107964);
#45649=PROPERTY_DEFINITION('material property','density of part',#107964);
#45650=PROPERTY_DEFINITION('material property','material name',#107965);
#45651=PROPERTY_DEFINITION('material property','density of part',#107965);
#45652=PROPERTY_DEFINITION('material property','material name',#107966);
#45653=PROPERTY_DEFINITION('material property','density of part',#107966);
#45654=PROPERTY_DEFINITION('material property','material name',#107967);
#45655=PROPERTY_DEFINITION('material property','density of part',#107967);
#45656=PROPERTY_DEFINITION('material property','material name',#107968);
#45657=PROPERTY_DEFINITION('material property','density of part',#107968);
#45658=AXIS2_PLACEMENT_3D('',#61796,#50376,#50377);
#45659=AXIS2_PLACEMENT_3D('',#61797,#50378,#50379);
#45660=AXIS2_PLACEMENT_3D('',#61798,#50380,#50381);
#45661=AXIS2_PLACEMENT_3D('',#61800,#50382,#50383);
#45662=AXIS2_PLACEMENT_3D('',#61803,#50385,#50386);
#45663=AXIS2_PLACEMENT_3D('',#61804,#50387,#50388);
#45664=AXIS2_PLACEMENT_3D('',#61806,#50389,#50390);
#45665=AXIS2_PLACEMENT_3D('',#61809,#50392,#50393);
#45666=AXIS2_PLACEMENT_3D('',#61810,#50394,#50395);
#45667=AXIS2_PLACEMENT_3D('',#61811,#50396,#50397);
#45668=AXIS2_PLACEMENT_3D('',#61812,#50398,#50399);
#45669=AXIS2_PLACEMENT_3D('',#63363,#50400,#50401);
#45670=AXIS2_PLACEMENT_3D('',#63364,#50402,#50403);
#45671=AXIS2_PLACEMENT_3D('',#63365,#50404,#50405);
#45672=AXIS2_PLACEMENT_3D('',#63366,#50406,#50407);
#45673=AXIS2_PLACEMENT_3D('',#63368,#50408,#50409);
#45674=AXIS2_PLACEMENT_3D('',#63370,#50410,#50411);
#45675=AXIS2_PLACEMENT_3D('',#63371,#50412,#50413);
#45676=AXIS2_PLACEMENT_3D('',#63372,#50414,#50415);
#45677=AXIS2_PLACEMENT_3D('',#63375,#50417,#50418);
#45678=AXIS2_PLACEMENT_3D('',#63376,#50419,#50420);
#45679=AXIS2_PLACEMENT_3D('',#63377,#50421,#50422);
#45680=AXIS2_PLACEMENT_3D('',#63378,#50423,#50424);
#45681=AXIS2_PLACEMENT_3D('',#63379,#50425,#50426);
#45682=AXIS2_PLACEMENT_3D('',#63381,#50427,#50428);
#45683=AXIS2_PLACEMENT_3D('',#63385,#50430,#50431);
#45684=AXIS2_PLACEMENT_3D('',#63414,#50432,#50433);
#45685=AXIS2_PLACEMENT_3D('',#63415,#50434,#50435);
#45686=AXIS2_PLACEMENT_3D('',#63417,#50437,#50438);
#45687=AXIS2_PLACEMENT_3D('',#63418,#50439,#50440);
#45688=AXIS2_PLACEMENT_3D('',#63419,#50441,#50442);
#45689=AXIS2_PLACEMENT_3D('',#63420,#50443,#50444);
#45690=AXIS2_PLACEMENT_3D('',#63423,#50445,#50446);
#45691=AXIS2_PLACEMENT_3D('',#63427,#50448,#50449);
#45692=AXIS2_PLACEMENT_3D('',#63429,#50451,#50452);
#45693=AXIS2_PLACEMENT_3D('',#63432,#50453,#50454);
#45694=AXIS2_PLACEMENT_3D('',#63436,#50456,#50457);
#45695=AXIS2_PLACEMENT_3D('',#63438,#50459,#50460);
#45696=AXIS2_PLACEMENT_3D('',#63451,#50467,#50468);
#45697=AXIS2_PLACEMENT_3D('',#63453,#50470,#50471);
#45698=AXIS2_PLACEMENT_3D('',#63455,#50472,#50473);
#45699=AXIS2_PLACEMENT_3D('',#63458,#50475,#50476);
#45700=AXIS2_PLACEMENT_3D('',#63459,#50477,#50478);
#45701=AXIS2_PLACEMENT_3D('',#63465,#50482,#50483);
#45702=AXIS2_PLACEMENT_3D('',#63471,#50487,#50488);
#45703=AXIS2_PLACEMENT_3D('',#63487,#50496,#50497);
#45704=AXIS2_PLACEMENT_3D('',#63489,#50499,#50500);
#45705=AXIS2_PLACEMENT_3D('',#63496,#50505,#50506);
#45706=AXIS2_PLACEMENT_3D('',#63500,#50509,#50510);
#45707=AXIS2_PLACEMENT_3D('',#63504,#50513,#50514);
#45708=AXIS2_PLACEMENT_3D('',#63506,#50516,#50517);
#45709=AXIS2_PLACEMENT_3D('',#63508,#50519,#50520);
#45710=AXIS2_PLACEMENT_3D('',#63511,#50523,#50524);
#45711=AXIS2_PLACEMENT_3D('',#63512,#50525,#50526);
#45712=AXIS2_PLACEMENT_3D('',#63513,#50527,#50528);
#45713=AXIS2_PLACEMENT_3D('',#63515,#50530,#50531);
#45714=AXIS2_PLACEMENT_3D('',#63517,#50533,#50534);
#45715=AXIS2_PLACEMENT_3D('',#63519,#50536,#50537);
#45716=AXIS2_PLACEMENT_3D('',#63521,#50539,#50540);
#45717=AXIS2_PLACEMENT_3D('',#63522,#50541,#50542);
#45718=AXIS2_PLACEMENT_3D('',#63523,#50543,#50544);
#45719=AXIS2_PLACEMENT_3D('',#63525,#50545,#50546);
#45720=AXIS2_PLACEMENT_3D('',#63528,#50548,#50549);
#45721=AXIS2_PLACEMENT_3D('',#63529,#50550,#50551);
#45722=AXIS2_PLACEMENT_3D('',#63540,#50553,#50554);
#45723=AXIS2_PLACEMENT_3D('',#63547,#50555,#50556);
#45724=AXIS2_PLACEMENT_3D('',#63549,#50557,#50558);
#45725=AXIS2_PLACEMENT_3D('',#63565,#50559,#50560);
#45726=AXIS2_PLACEMENT_3D('',#63567,#50561,#50562);
#45727=AXIS2_PLACEMENT_3D('',#63583,#50563,#50564);
#45728=AXIS2_PLACEMENT_3D('',#63585,#50565,#50566);
#45729=AXIS2_PLACEMENT_3D('',#63601,#50567,#50568);
#45730=AXIS2_PLACEMENT_3D('',#63603,#50569,#50570);
#45731=AXIS2_PLACEMENT_3D('',#63619,#50571,#50572);
#45732=AXIS2_PLACEMENT_3D('',#63621,#50573,#50574);
#45733=AXIS2_PLACEMENT_3D('',#63637,#50575,#50576);
#45734=AXIS2_PLACEMENT_3D('',#63639,#50577,#50578);
#45735=AXIS2_PLACEMENT_3D('',#63655,#50579,#50580);
#45736=AXIS2_PLACEMENT_3D('',#63657,#50581,#50582);
#45737=AXIS2_PLACEMENT_3D('',#63673,#50583,#50584);
#45738=AXIS2_PLACEMENT_3D('',#63675,#50585,#50586);
#45739=AXIS2_PLACEMENT_3D('',#63691,#50587,#50588);
#45740=AXIS2_PLACEMENT_3D('',#63693,#50589,#50590);
#45741=AXIS2_PLACEMENT_3D('',#63709,#50591,#50592);
#45742=AXIS2_PLACEMENT_3D('',#63711,#50593,#50594);
#45743=AXIS2_PLACEMENT_3D('',#63727,#50595,#50596);
#45744=AXIS2_PLACEMENT_3D('',#63729,#50597,#50598);
#45745=AXIS2_PLACEMENT_3D('',#63745,#50599,#50600);
#45746=AXIS2_PLACEMENT_3D('',#63747,#50601,#50602);
#45747=AXIS2_PLACEMENT_3D('',#63763,#50603,#50604);
#45748=AXIS2_PLACEMENT_3D('',#63765,#50605,#50606);
#45749=AXIS2_PLACEMENT_3D('',#63781,#50607,#50608);
#45750=AXIS2_PLACEMENT_3D('',#63783,#50609,#50610);
#45751=AXIS2_PLACEMENT_3D('',#63799,#50611,#50612);
#45752=AXIS2_PLACEMENT_3D('',#63801,#50613,#50614);
#45753=AXIS2_PLACEMENT_3D('',#63817,#50615,#50616);
#45754=AXIS2_PLACEMENT_3D('',#63819,#50617,#50618);
#45755=AXIS2_PLACEMENT_3D('',#63835,#50619,#50620);
#45756=AXIS2_PLACEMENT_3D('',#63837,#50621,#50622);
#45757=AXIS2_PLACEMENT_3D('',#63853,#50623,#50624);
#45758=AXIS2_PLACEMENT_3D('',#63855,#50625,#50626);
#45759=AXIS2_PLACEMENT_3D('',#63871,#50627,#50628);
#45760=AXIS2_PLACEMENT_3D('',#63873,#50629,#50630);
#45761=AXIS2_PLACEMENT_3D('',#63889,#50631,#50632);
#45762=AXIS2_PLACEMENT_3D('',#63891,#50633,#50634);
#45763=AXIS2_PLACEMENT_3D('',#63907,#50635,#50636);
#45764=AXIS2_PLACEMENT_3D('',#63909,#50637,#50638);
#45765=AXIS2_PLACEMENT_3D('',#63925,#50639,#50640);
#45766=AXIS2_PLACEMENT_3D('',#63927,#50641,#50642);
#45767=AXIS2_PLACEMENT_3D('',#63943,#50643,#50644);
#45768=AXIS2_PLACEMENT_3D('',#63945,#50645,#50646);
#45769=AXIS2_PLACEMENT_3D('',#63961,#50647,#50648);
#45770=AXIS2_PLACEMENT_3D('',#63963,#50649,#50650);
#45771=AXIS2_PLACEMENT_3D('',#63979,#50651,#50652);
#45772=AXIS2_PLACEMENT_3D('',#63981,#50653,#50654);
#45773=AXIS2_PLACEMENT_3D('',#63997,#50655,#50656);
#45774=AXIS2_PLACEMENT_3D('',#63999,#50657,#50658);
#45775=AXIS2_PLACEMENT_3D('',#64015,#50659,#50660);
#45776=AXIS2_PLACEMENT_3D('',#64017,#50661,#50662);
#45777=AXIS2_PLACEMENT_3D('',#64033,#50663,#50664);
#45778=AXIS2_PLACEMENT_3D('',#64035,#50665,#50666);
#45779=AXIS2_PLACEMENT_3D('',#64051,#50667,#50668);
#45780=AXIS2_PLACEMENT_3D('',#64053,#50669,#50670);
#45781=AXIS2_PLACEMENT_3D('',#64069,#50671,#50672);
#45782=AXIS2_PLACEMENT_3D('',#64071,#50673,#50674);
#45783=AXIS2_PLACEMENT_3D('',#64087,#50675,#50676);
#45784=AXIS2_PLACEMENT_3D('',#64089,#50677,#50678);
#45785=AXIS2_PLACEMENT_3D('',#64105,#50679,#50680);
#45786=AXIS2_PLACEMENT_3D('',#64107,#50681,#50682);
#45787=AXIS2_PLACEMENT_3D('',#64123,#50683,#50684);
#45788=AXIS2_PLACEMENT_3D('',#64125,#50685,#50686);
#45789=AXIS2_PLACEMENT_3D('',#64141,#50687,#50688);
#45790=AXIS2_PLACEMENT_3D('',#64143,#50689,#50690);
#45791=AXIS2_PLACEMENT_3D('',#64159,#50691,#50692);
#45792=AXIS2_PLACEMENT_3D('',#64161,#50693,#50694);
#45793=AXIS2_PLACEMENT_3D('',#64177,#50695,#50696);
#45794=AXIS2_PLACEMENT_3D('',#64179,#50697,#50698);
#45795=AXIS2_PLACEMENT_3D('',#64195,#50699,#50700);
#45796=AXIS2_PLACEMENT_3D('',#64197,#50701,#50702);
#45797=AXIS2_PLACEMENT_3D('',#64213,#50703,#50704);
#45798=AXIS2_PLACEMENT_3D('',#64215,#50705,#50706);
#45799=AXIS2_PLACEMENT_3D('',#64231,#50707,#50708);
#45800=AXIS2_PLACEMENT_3D('',#64233,#50709,#50710);
#45801=AXIS2_PLACEMENT_3D('',#64249,#50711,#50712);
#45802=AXIS2_PLACEMENT_3D('',#64251,#50713,#50714);
#45803=AXIS2_PLACEMENT_3D('',#64267,#50715,#50716);
#45804=AXIS2_PLACEMENT_3D('',#64269,#50717,#50718);
#45805=AXIS2_PLACEMENT_3D('',#64285,#50719,#50720);
#45806=AXIS2_PLACEMENT_3D('',#64287,#50721,#50722);
#45807=AXIS2_PLACEMENT_3D('',#64303,#50723,#50724);
#45808=AXIS2_PLACEMENT_3D('',#64305,#50725,#50726);
#45809=AXIS2_PLACEMENT_3D('',#64321,#50727,#50728);
#45810=AXIS2_PLACEMENT_3D('',#64323,#50729,#50730);
#45811=AXIS2_PLACEMENT_3D('',#64339,#50731,#50732);
#45812=AXIS2_PLACEMENT_3D('',#64341,#50733,#50734);
#45813=AXIS2_PLACEMENT_3D('',#64357,#50735,#50736);
#45814=AXIS2_PLACEMENT_3D('',#64359,#50737,#50738);
#45815=AXIS2_PLACEMENT_3D('',#64375,#50739,#50740);
#45816=AXIS2_PLACEMENT_3D('',#64377,#50741,#50742);
#45817=AXIS2_PLACEMENT_3D('',#64393,#50743,#50744);
#45818=AXIS2_PLACEMENT_3D('',#64395,#50745,#50746);
#45819=AXIS2_PLACEMENT_3D('',#64411,#50747,#50748);
#45820=AXIS2_PLACEMENT_3D('',#64413,#50749,#50750);
#45821=AXIS2_PLACEMENT_3D('',#64429,#50751,#50752);
#45822=AXIS2_PLACEMENT_3D('',#64431,#50753,#50754);
#45823=AXIS2_PLACEMENT_3D('',#64438,#50755,#50756);
#45824=AXIS2_PLACEMENT_3D('',#64447,#50758,#50759);
#45825=AXIS2_PLACEMENT_3D('',#64456,#50760,#50761);
#45826=AXIS2_PLACEMENT_3D('',#64458,#50762,#50763);
#45827=AXIS2_PLACEMENT_3D('',#64460,#50764,#50765);
#45828=AXIS2_PLACEMENT_3D('',#64462,#50766,#50767);
#45829=AXIS2_PLACEMENT_3D('',#64469,#50768,#50769);
#45830=AXIS2_PLACEMENT_3D('',#64471,#50770,#50771);
#45831=AXIS2_PLACEMENT_3D('',#64473,#50772,#50773);
#45832=AXIS2_PLACEMENT_3D('',#64475,#50774,#50775);
#45833=AXIS2_PLACEMENT_3D('',#64477,#50776,#50777);
#45834=AXIS2_PLACEMENT_3D('',#64484,#50778,#50779);
#45835=AXIS2_PLACEMENT_3D('',#64486,#50780,#50781);
#45836=AXIS2_PLACEMENT_3D('',#64488,#50782,#50783);
#45837=AXIS2_PLACEMENT_3D('',#64490,#50784,#50785);
#45838=AXIS2_PLACEMENT_3D('',#64492,#50786,#50787);
#45839=AXIS2_PLACEMENT_3D('',#64499,#50788,#50789);
#45840=AXIS2_PLACEMENT_3D('',#64501,#50790,#50791);
#45841=AXIS2_PLACEMENT_3D('',#64503,#50792,#50793);
#45842=AXIS2_PLACEMENT_3D('',#64505,#50794,#50795);
#45843=AXIS2_PLACEMENT_3D('',#64507,#50796,#50797);
#45844=AXIS2_PLACEMENT_3D('',#64514,#50798,#50799);
#45845=AXIS2_PLACEMENT_3D('',#64516,#50800,#50801);
#45846=AXIS2_PLACEMENT_3D('',#64518,#50802,#50803);
#45847=AXIS2_PLACEMENT_3D('',#64520,#50804,#50805);
#45848=AXIS2_PLACEMENT_3D('',#64522,#50806,#50807);
#45849=AXIS2_PLACEMENT_3D('',#64529,#50808,#50809);
#45850=AXIS2_PLACEMENT_3D('',#64531,#50810,#50811);
#45851=AXIS2_PLACEMENT_3D('',#64533,#50812,#50813);
#45852=AXIS2_PLACEMENT_3D('',#64535,#50814,#50815);
#45853=AXIS2_PLACEMENT_3D('',#64537,#50816,#50817);
#45854=AXIS2_PLACEMENT_3D('',#64544,#50818,#50819);
#45855=AXIS2_PLACEMENT_3D('',#64546,#50820,#50821);
#45856=AXIS2_PLACEMENT_3D('',#64548,#50822,#50823);
#45857=AXIS2_PLACEMENT_3D('',#64550,#50824,#50825);
#45858=AXIS2_PLACEMENT_3D('',#64552,#50826,#50827);
#45859=AXIS2_PLACEMENT_3D('',#64559,#50828,#50829);
#45860=AXIS2_PLACEMENT_3D('',#64561,#50830,#50831);
#45861=AXIS2_PLACEMENT_3D('',#64563,#50832,#50833);
#45862=AXIS2_PLACEMENT_3D('',#64565,#50834,#50835);
#45863=AXIS2_PLACEMENT_3D('',#64567,#50836,#50837);
#45864=AXIS2_PLACEMENT_3D('',#64574,#50838,#50839);
#45865=AXIS2_PLACEMENT_3D('',#64576,#50840,#50841);
#45866=AXIS2_PLACEMENT_3D('',#64578,#50842,#50843);
#45867=AXIS2_PLACEMENT_3D('',#64580,#50844,#50845);
#45868=AXIS2_PLACEMENT_3D('',#64582,#50846,#50847);
#45869=AXIS2_PLACEMENT_3D('',#64589,#50848,#50849);
#45870=AXIS2_PLACEMENT_3D('',#64591,#50850,#50851);
#45871=AXIS2_PLACEMENT_3D('',#64593,#50852,#50853);
#45872=AXIS2_PLACEMENT_3D('',#64595,#50854,#50855);
#45873=AXIS2_PLACEMENT_3D('',#64597,#50856,#50857);
#45874=AXIS2_PLACEMENT_3D('',#64604,#50858,#50859);
#45875=AXIS2_PLACEMENT_3D('',#64606,#50860,#50861);
#45876=AXIS2_PLACEMENT_3D('',#64608,#50862,#50863);
#45877=AXIS2_PLACEMENT_3D('',#64610,#50864,#50865);
#45878=AXIS2_PLACEMENT_3D('',#64612,#50866,#50867);
#45879=AXIS2_PLACEMENT_3D('',#64619,#50868,#50869);
#45880=AXIS2_PLACEMENT_3D('',#64621,#50870,#50871);
#45881=AXIS2_PLACEMENT_3D('',#64623,#50872,#50873);
#45882=AXIS2_PLACEMENT_3D('',#64625,#50874,#50875);
#45883=AXIS2_PLACEMENT_3D('',#64627,#50876,#50877);
#45884=AXIS2_PLACEMENT_3D('',#64634,#50878,#50879);
#45885=AXIS2_PLACEMENT_3D('',#64636,#50880,#50881);
#45886=AXIS2_PLACEMENT_3D('',#64638,#50882,#50883);
#45887=AXIS2_PLACEMENT_3D('',#64640,#50884,#50885);
#45888=AXIS2_PLACEMENT_3D('',#64642,#50886,#50887);
#45889=AXIS2_PLACEMENT_3D('',#64649,#50888,#50889);
#45890=AXIS2_PLACEMENT_3D('',#64651,#50890,#50891);
#45891=AXIS2_PLACEMENT_3D('',#64653,#50892,#50893);
#45892=AXIS2_PLACEMENT_3D('',#64655,#50894,#50895);
#45893=AXIS2_PLACEMENT_3D('',#64657,#50896,#50897);
#45894=AXIS2_PLACEMENT_3D('',#64664,#50898,#50899);
#45895=AXIS2_PLACEMENT_3D('',#64666,#50900,#50901);
#45896=AXIS2_PLACEMENT_3D('',#64668,#50902,#50903);
#45897=AXIS2_PLACEMENT_3D('',#64670,#50904,#50905);
#45898=AXIS2_PLACEMENT_3D('',#64672,#50906,#50907);
#45899=AXIS2_PLACEMENT_3D('',#64679,#50908,#50909);
#45900=AXIS2_PLACEMENT_3D('',#64681,#50910,#50911);
#45901=AXIS2_PLACEMENT_3D('',#64683,#50912,#50913);
#45902=AXIS2_PLACEMENT_3D('',#64685,#50914,#50915);
#45903=AXIS2_PLACEMENT_3D('',#64687,#50916,#50917);
#45904=AXIS2_PLACEMENT_3D('',#64694,#50918,#50919);
#45905=AXIS2_PLACEMENT_3D('',#64696,#50920,#50921);
#45906=AXIS2_PLACEMENT_3D('',#64698,#50922,#50923);
#45907=AXIS2_PLACEMENT_3D('',#64700,#50924,#50925);
#45908=AXIS2_PLACEMENT_3D('',#64702,#50926,#50927);
#45909=AXIS2_PLACEMENT_3D('',#64709,#50928,#50929);
#45910=AXIS2_PLACEMENT_3D('',#64711,#50930,#50931);
#45911=AXIS2_PLACEMENT_3D('',#64713,#50932,#50933);
#45912=AXIS2_PLACEMENT_3D('',#64715,#50934,#50935);
#45913=AXIS2_PLACEMENT_3D('',#64717,#50936,#50937);
#45914=AXIS2_PLACEMENT_3D('',#64724,#50938,#50939);
#45915=AXIS2_PLACEMENT_3D('',#64726,#50940,#50941);
#45916=AXIS2_PLACEMENT_3D('',#64728,#50942,#50943);
#45917=AXIS2_PLACEMENT_3D('',#64730,#50944,#50945);
#45918=AXIS2_PLACEMENT_3D('',#64732,#50946,#50947);
#45919=AXIS2_PLACEMENT_3D('',#64739,#50948,#50949);
#45920=AXIS2_PLACEMENT_3D('',#64741,#50950,#50951);
#45921=AXIS2_PLACEMENT_3D('',#64743,#50952,#50953);
#45922=AXIS2_PLACEMENT_3D('',#64745,#50954,#50955);
#45923=AXIS2_PLACEMENT_3D('',#64747,#50956,#50957);
#45924=AXIS2_PLACEMENT_3D('',#64754,#50958,#50959);
#45925=AXIS2_PLACEMENT_3D('',#64756,#50960,#50961);
#45926=AXIS2_PLACEMENT_3D('',#64758,#50962,#50963);
#45927=AXIS2_PLACEMENT_3D('',#64760,#50964,#50965);
#45928=AXIS2_PLACEMENT_3D('',#64762,#50966,#50967);
#45929=AXIS2_PLACEMENT_3D('',#64769,#50968,#50969);
#45930=AXIS2_PLACEMENT_3D('',#64771,#50970,#50971);
#45931=AXIS2_PLACEMENT_3D('',#64773,#50972,#50973);
#45932=AXIS2_PLACEMENT_3D('',#64775,#50974,#50975);
#45933=AXIS2_PLACEMENT_3D('',#64777,#50976,#50977);
#45934=AXIS2_PLACEMENT_3D('',#64784,#50978,#50979);
#45935=AXIS2_PLACEMENT_3D('',#64786,#50980,#50981);
#45936=AXIS2_PLACEMENT_3D('',#64788,#50982,#50983);
#45937=AXIS2_PLACEMENT_3D('',#64790,#50984,#50985);
#45938=AXIS2_PLACEMENT_3D('',#64792,#50986,#50987);
#45939=AXIS2_PLACEMENT_3D('',#64799,#50988,#50989);
#45940=AXIS2_PLACEMENT_3D('',#64801,#50990,#50991);
#45941=AXIS2_PLACEMENT_3D('',#64803,#50992,#50993);
#45942=AXIS2_PLACEMENT_3D('',#64805,#50994,#50995);
#45943=AXIS2_PLACEMENT_3D('',#64807,#50996,#50997);
#45944=AXIS2_PLACEMENT_3D('',#64814,#50998,#50999);
#45945=AXIS2_PLACEMENT_3D('',#64816,#51000,#51001);
#45946=AXIS2_PLACEMENT_3D('',#64818,#51002,#51003);
#45947=AXIS2_PLACEMENT_3D('',#64820,#51004,#51005);
#45948=AXIS2_PLACEMENT_3D('',#64822,#51006,#51007);
#45949=AXIS2_PLACEMENT_3D('',#64829,#51008,#51009);
#45950=AXIS2_PLACEMENT_3D('',#64831,#51010,#51011);
#45951=AXIS2_PLACEMENT_3D('',#64833,#51012,#51013);
#45952=AXIS2_PLACEMENT_3D('',#64835,#51014,#51015);
#45953=AXIS2_PLACEMENT_3D('',#64837,#51016,#51017);
#45954=AXIS2_PLACEMENT_3D('',#64844,#51018,#51019);
#45955=AXIS2_PLACEMENT_3D('',#64846,#51020,#51021);
#45956=AXIS2_PLACEMENT_3D('',#64848,#51022,#51023);
#45957=AXIS2_PLACEMENT_3D('',#64850,#51024,#51025);
#45958=AXIS2_PLACEMENT_3D('',#64852,#51026,#51027);
#45959=AXIS2_PLACEMENT_3D('',#64859,#51028,#51029);
#45960=AXIS2_PLACEMENT_3D('',#64861,#51030,#51031);
#45961=AXIS2_PLACEMENT_3D('',#64863,#51032,#51033);
#45962=AXIS2_PLACEMENT_3D('',#64865,#51034,#51035);
#45963=AXIS2_PLACEMENT_3D('',#64867,#51036,#51037);
#45964=AXIS2_PLACEMENT_3D('',#64874,#51038,#51039);
#45965=AXIS2_PLACEMENT_3D('',#64876,#51040,#51041);
#45966=AXIS2_PLACEMENT_3D('',#64878,#51042,#51043);
#45967=AXIS2_PLACEMENT_3D('',#64880,#51044,#51045);
#45968=AXIS2_PLACEMENT_3D('',#64882,#51046,#51047);
#45969=AXIS2_PLACEMENT_3D('',#64889,#51048,#51049);
#45970=AXIS2_PLACEMENT_3D('',#64891,#51050,#51051);
#45971=AXIS2_PLACEMENT_3D('',#64893,#51052,#51053);
#45972=AXIS2_PLACEMENT_3D('',#64895,#51054,#51055);
#45973=AXIS2_PLACEMENT_3D('',#64897,#51056,#51057);
#45974=AXIS2_PLACEMENT_3D('',#64904,#51058,#51059);
#45975=AXIS2_PLACEMENT_3D('',#64906,#51060,#51061);
#45976=AXIS2_PLACEMENT_3D('',#64908,#51062,#51063);
#45977=AXIS2_PLACEMENT_3D('',#64910,#51064,#51065);
#45978=AXIS2_PLACEMENT_3D('',#64912,#51066,#51067);
#45979=AXIS2_PLACEMENT_3D('',#64919,#51068,#51069);
#45980=AXIS2_PLACEMENT_3D('',#64921,#51070,#51071);
#45981=AXIS2_PLACEMENT_3D('',#64923,#51072,#51073);
#45982=AXIS2_PLACEMENT_3D('',#64925,#51074,#51075);
#45983=AXIS2_PLACEMENT_3D('',#64927,#51076,#51077);
#45984=AXIS2_PLACEMENT_3D('',#64934,#51078,#51079);
#45985=AXIS2_PLACEMENT_3D('',#64936,#51080,#51081);
#45986=AXIS2_PLACEMENT_3D('',#64938,#51082,#51083);
#45987=AXIS2_PLACEMENT_3D('',#64940,#51084,#51085);
#45988=AXIS2_PLACEMENT_3D('',#64942,#51086,#51087);
#45989=AXIS2_PLACEMENT_3D('',#64949,#51088,#51089);
#45990=AXIS2_PLACEMENT_3D('',#64951,#51090,#51091);
#45991=AXIS2_PLACEMENT_3D('',#64953,#51092,#51093);
#45992=AXIS2_PLACEMENT_3D('',#64955,#51094,#51095);
#45993=AXIS2_PLACEMENT_3D('',#64957,#51096,#51097);
#45994=AXIS2_PLACEMENT_3D('',#64964,#51098,#51099);
#45995=AXIS2_PLACEMENT_3D('',#64966,#51100,#51101);
#45996=AXIS2_PLACEMENT_3D('',#64968,#51102,#51103);
#45997=AXIS2_PLACEMENT_3D('',#64970,#51104,#51105);
#45998=AXIS2_PLACEMENT_3D('',#64972,#51106,#51107);
#45999=AXIS2_PLACEMENT_3D('',#64979,#51108,#51109);
#46000=AXIS2_PLACEMENT_3D('',#64981,#51110,#51111);
#46001=AXIS2_PLACEMENT_3D('',#64983,#51112,#51113);
#46002=AXIS2_PLACEMENT_3D('',#64985,#51114,#51115);
#46003=AXIS2_PLACEMENT_3D('',#64987,#51116,#51117);
#46004=AXIS2_PLACEMENT_3D('',#64994,#51118,#51119);
#46005=AXIS2_PLACEMENT_3D('',#64996,#51120,#51121);
#46006=AXIS2_PLACEMENT_3D('',#64998,#51122,#51123);
#46007=AXIS2_PLACEMENT_3D('',#65000,#51124,#51125);
#46008=AXIS2_PLACEMENT_3D('',#65002,#51126,#51127);
#46009=AXIS2_PLACEMENT_3D('',#65009,#51128,#51129);
#46010=AXIS2_PLACEMENT_3D('',#65011,#51130,#51131);
#46011=AXIS2_PLACEMENT_3D('',#65013,#51132,#51133);
#46012=AXIS2_PLACEMENT_3D('',#65015,#51134,#51135);
#46013=AXIS2_PLACEMENT_3D('',#65017,#51136,#51137);
#46014=AXIS2_PLACEMENT_3D('',#65024,#51138,#51139);
#46015=AXIS2_PLACEMENT_3D('',#65026,#51140,#51141);
#46016=AXIS2_PLACEMENT_3D('',#65028,#51142,#51143);
#46017=AXIS2_PLACEMENT_3D('',#65030,#51144,#51145);
#46018=AXIS2_PLACEMENT_3D('',#65032,#51146,#51147);
#46019=AXIS2_PLACEMENT_3D('',#65039,#51148,#51149);
#46020=AXIS2_PLACEMENT_3D('',#65041,#51150,#51151);
#46021=AXIS2_PLACEMENT_3D('',#65043,#51152,#51153);
#46022=AXIS2_PLACEMENT_3D('',#65045,#51154,#51155);
#46023=AXIS2_PLACEMENT_3D('',#65047,#51156,#51157);
#46024=AXIS2_PLACEMENT_3D('',#65054,#51158,#51159);
#46025=AXIS2_PLACEMENT_3D('',#65056,#51160,#51161);
#46026=AXIS2_PLACEMENT_3D('',#65058,#51162,#51163);
#46027=AXIS2_PLACEMENT_3D('',#65060,#51164,#51165);
#46028=AXIS2_PLACEMENT_3D('',#65062,#51166,#51167);
#46029=AXIS2_PLACEMENT_3D('',#65069,#51168,#51169);
#46030=AXIS2_PLACEMENT_3D('',#65071,#51170,#51171);
#46031=AXIS2_PLACEMENT_3D('',#65073,#51172,#51173);
#46032=AXIS2_PLACEMENT_3D('',#65075,#51174,#51175);
#46033=AXIS2_PLACEMENT_3D('',#65077,#51176,#51177);
#46034=AXIS2_PLACEMENT_3D('',#65084,#51178,#51179);
#46035=AXIS2_PLACEMENT_3D('',#65086,#51180,#51181);
#46036=AXIS2_PLACEMENT_3D('',#65088,#51182,#51183);
#46037=AXIS2_PLACEMENT_3D('',#65090,#51184,#51185);
#46038=AXIS2_PLACEMENT_3D('',#65092,#51186,#51187);
#46039=AXIS2_PLACEMENT_3D('',#65099,#51188,#51189);
#46040=AXIS2_PLACEMENT_3D('',#65101,#51190,#51191);
#46041=AXIS2_PLACEMENT_3D('',#65103,#51192,#51193);
#46042=AXIS2_PLACEMENT_3D('',#65105,#51194,#51195);
#46043=AXIS2_PLACEMENT_3D('',#65107,#51196,#51197);
#46044=AXIS2_PLACEMENT_3D('',#65114,#51198,#51199);
#46045=AXIS2_PLACEMENT_3D('',#65116,#51200,#51201);
#46046=AXIS2_PLACEMENT_3D('',#65118,#51202,#51203);
#46047=AXIS2_PLACEMENT_3D('',#65120,#51204,#51205);
#46048=AXIS2_PLACEMENT_3D('',#65122,#51206,#51207);
#46049=AXIS2_PLACEMENT_3D('',#65129,#51208,#51209);
#46050=AXIS2_PLACEMENT_3D('',#65131,#51210,#51211);
#46051=AXIS2_PLACEMENT_3D('',#65133,#51212,#51213);
#46052=AXIS2_PLACEMENT_3D('',#65135,#51214,#51215);
#46053=AXIS2_PLACEMENT_3D('',#65137,#51216,#51217);
#46054=AXIS2_PLACEMENT_3D('',#65144,#51218,#51219);
#46055=AXIS2_PLACEMENT_3D('',#65146,#51220,#51221);
#46056=AXIS2_PLACEMENT_3D('',#65148,#51222,#51223);
#46057=AXIS2_PLACEMENT_3D('',#65150,#51224,#51225);
#46058=AXIS2_PLACEMENT_3D('',#65152,#51226,#51227);
#46059=AXIS2_PLACEMENT_3D('',#65159,#51228,#51229);
#46060=AXIS2_PLACEMENT_3D('',#65161,#51230,#51231);
#46061=AXIS2_PLACEMENT_3D('',#65163,#51232,#51233);
#46062=AXIS2_PLACEMENT_3D('',#65165,#51234,#51235);
#46063=AXIS2_PLACEMENT_3D('',#65167,#51236,#51237);
#46064=AXIS2_PLACEMENT_3D('',#65174,#51238,#51239);
#46065=AXIS2_PLACEMENT_3D('',#65176,#51240,#51241);
#46066=AXIS2_PLACEMENT_3D('',#65178,#51242,#51243);
#46067=AXIS2_PLACEMENT_3D('',#65180,#51244,#51245);
#46068=AXIS2_PLACEMENT_3D('',#65182,#51246,#51247);
#46069=AXIS2_PLACEMENT_3D('',#65189,#51248,#51249);
#46070=AXIS2_PLACEMENT_3D('',#65191,#51250,#51251);
#46071=AXIS2_PLACEMENT_3D('',#65193,#51252,#51253);
#46072=AXIS2_PLACEMENT_3D('',#65195,#51254,#51255);
#46073=AXIS2_PLACEMENT_3D('',#65197,#51256,#51257);
#46074=AXIS2_PLACEMENT_3D('',#65220,#51258,#51259);
#46075=AXIS2_PLACEMENT_3D('',#65221,#51260,#51261);
#46076=AXIS2_PLACEMENT_3D('',#65231,#51262,#51263);
#46077=AXIS2_PLACEMENT_3D('',#65251,#51265,#51266);
#46078=AXIS2_PLACEMENT_3D('',#65267,#51268,#51269);
#46079=AXIS2_PLACEMENT_3D('',#65269,#51270,#51271);
#46080=AXIS2_PLACEMENT_3D('',#65273,#51273,#51274);
#46081=AXIS2_PLACEMENT_3D('',#65275,#51275,#51276);
#46082=AXIS2_PLACEMENT_3D('',#65294,#51278,#51279);
#46083=AXIS2_PLACEMENT_3D('',#65298,#51281,#51282);
#46084=AXIS2_PLACEMENT_3D('',#65299,#51283,#51284);
#46085=AXIS2_PLACEMENT_3D('',#65318,#51285,#51286);
#46086=AXIS2_PLACEMENT_3D('',#65345,#51289,#51290);
#46087=AXIS2_PLACEMENT_3D('',#65352,#51291,#51292);
#46088=AXIS2_PLACEMENT_3D('',#65355,#51293,#51294);
#46089=AXIS2_PLACEMENT_3D('',#65356,#51295,#51296);
#46090=AXIS2_PLACEMENT_3D('',#65357,#51297,#51298);
#46091=AXIS2_PLACEMENT_3D('',#65381,#51300,#51301);
#46092=AXIS2_PLACEMENT_3D('',#65382,#51302,#51303);
#46093=AXIS2_PLACEMENT_3D('',#65383,#51304,#51305);
#46094=AXIS2_PLACEMENT_3D('',#65386,#51306,#51307);
#46095=AXIS2_PLACEMENT_3D('',#65387,#51308,#51309);
#46096=AXIS2_PLACEMENT_3D('',#65388,#51310,#51311);
#46097=AXIS2_PLACEMENT_3D('',#65389,#51312,#51313);
#46098=AXIS2_PLACEMENT_3D('',#65391,#51314,#51315);
#46099=AXIS2_PLACEMENT_3D('',#65393,#51316,#51317);
#46100=AXIS2_PLACEMENT_3D('',#65394,#51318,#51319);
#46101=AXIS2_PLACEMENT_3D('',#65406,#51320,#51321);
#46102=AXIS2_PLACEMENT_3D('',#65408,#51322,#51323);
#46103=AXIS2_PLACEMENT_3D('',#65412,#51325,#51326);
#46104=AXIS2_PLACEMENT_3D('',#65414,#51327,#51328);
#46105=AXIS2_PLACEMENT_3D('',#65427,#51330,#51331);
#46106=AXIS2_PLACEMENT_3D('',#65428,#51332,#51333);
#46107=AXIS2_PLACEMENT_3D('',#65432,#51335,#51336);
#46108=AXIS2_PLACEMENT_3D('',#65434,#51337,#51338);
#46109=AXIS2_PLACEMENT_3D('',#65493,#51342,#51343);
#46110=AXIS2_PLACEMENT_3D('',#65513,#51346,#51347);
#46111=AXIS2_PLACEMENT_3D('',#65520,#51348,#51349);
#46112=AXIS2_PLACEMENT_3D('',#65523,#51350,#51351);
#46113=AXIS2_PLACEMENT_3D('',#65524,#51352,#51353);
#46114=AXIS2_PLACEMENT_3D('',#65525,#51354,#51355);
#46115=AXIS2_PLACEMENT_3D('',#65526,#51356,#51357);
#46116=AXIS2_PLACEMENT_3D('',#65528,#51358,#51359);
#46117=AXIS2_PLACEMENT_3D('',#65530,#51360,#51361);
#46118=AXIS2_PLACEMENT_3D('',#65531,#51362,#51363);
#46119=AXIS2_PLACEMENT_3D('',#65568,#51365,#51366);
#46120=AXIS2_PLACEMENT_3D('',#65570,#51367,#51368);
#46121=AXIS2_PLACEMENT_3D('',#65580,#51370,#51371);
#46122=AXIS2_PLACEMENT_3D('',#65581,#51372,#51373);
#46123=AXIS2_PLACEMENT_3D('',#65585,#51375,#51376);
#46124=AXIS2_PLACEMENT_3D('',#65587,#51377,#51378);
#46125=AXIS2_PLACEMENT_3D('',#65677,#51384,#51385);
#46126=AXIS2_PLACEMENT_3D('',#65684,#51386,#51387);
#46127=AXIS2_PLACEMENT_3D('',#65687,#51388,#51389);
#46128=AXIS2_PLACEMENT_3D('',#65694,#51390,#51391);
#46129=AXIS2_PLACEMENT_3D('',#65695,#51392,#51393);
#46130=AXIS2_PLACEMENT_3D('',#65697,#51394,#51395);
#46131=AXIS2_PLACEMENT_3D('',#65699,#51396,#51397);
#46132=AXIS2_PLACEMENT_3D('',#65700,#51398,#51399);
#46133=AXIS2_PLACEMENT_3D('',#65709,#51400,#51401);
#46134=AXIS2_PLACEMENT_3D('',#65711,#51402,#51403);
#46135=AXIS2_PLACEMENT_3D('',#65715,#51405,#51406);
#46136=AXIS2_PLACEMENT_3D('',#65717,#51407,#51408);
#46137=AXIS2_PLACEMENT_3D('',#65736,#51410,#51411);
#46138=AXIS2_PLACEMENT_3D('',#65737,#51412,#51413);
#46139=AXIS2_PLACEMENT_3D('',#65822,#51418,#51419);
#46140=AXIS2_PLACEMENT_3D('',#65855,#51422,#51423);
#46141=AXIS2_PLACEMENT_3D('',#65858,#51424,#51425);
#46142=AXIS2_PLACEMENT_3D('',#65859,#51426,#51427);
#46143=AXIS2_PLACEMENT_3D('',#65860,#51428,#51429);
#46144=AXIS2_PLACEMENT_3D('',#65861,#51430,#51431);
#46145=AXIS2_PLACEMENT_3D('',#65863,#51432,#51433);
#46146=AXIS2_PLACEMENT_3D('',#65865,#51434,#51435);
#46147=AXIS2_PLACEMENT_3D('',#65890,#51436,#51437);
#46148=AXIS2_PLACEMENT_3D('',#65892,#51438,#51439);
#46149=AXIS2_PLACEMENT_3D('',#65896,#51441,#51442);
#46150=AXIS2_PLACEMENT_3D('',#65898,#51443,#51444);
#46151=AXIS2_PLACEMENT_3D('',#65911,#51446,#51447);
#46152=AXIS2_PLACEMENT_3D('',#65912,#51448,#51449);
#46153=AXIS2_PLACEMENT_3D('',#65916,#51451,#51452);
#46154=AXIS2_PLACEMENT_3D('',#65918,#51453,#51454);
#46155=AXIS2_PLACEMENT_3D('',#65984,#51458,#51459);
#46156=AXIS2_PLACEMENT_3D('',#66011,#51462,#51463);
#46157=AXIS2_PLACEMENT_3D('',#66018,#51464,#51465);
#46158=AXIS2_PLACEMENT_3D('',#66021,#51466,#51467);
#46159=AXIS2_PLACEMENT_3D('',#66022,#51468,#51469);
#46160=AXIS2_PLACEMENT_3D('',#66023,#51470,#51471);
#46161=AXIS2_PLACEMENT_3D('',#66024,#51472,#51473);
#46162=AXIS2_PLACEMENT_3D('',#66026,#51474,#51475);
#46163=AXIS2_PLACEMENT_3D('',#66028,#51476,#51477);
#46164=AXIS2_PLACEMENT_3D('',#66029,#51478,#51479);
#46165=AXIS2_PLACEMENT_3D('',#66041,#51480,#51481);
#46166=AXIS2_PLACEMENT_3D('',#66043,#51482,#51483);
#46167=AXIS2_PLACEMENT_3D('',#66047,#51485,#51486);
#46168=AXIS2_PLACEMENT_3D('',#66049,#51487,#51488);
#46169=AXIS2_PLACEMENT_3D('',#66069,#51490,#51491);
#46170=AXIS2_PLACEMENT_3D('',#66070,#51492,#51493);
#46171=AXIS2_PLACEMENT_3D('',#66074,#51495,#51496);
#46172=AXIS2_PLACEMENT_3D('',#66076,#51497,#51498);
#46173=AXIS2_PLACEMENT_3D('',#66140,#51502,#51503);
#46174=AXIS2_PLACEMENT_3D('',#66161,#51506,#51507);
#46175=AXIS2_PLACEMENT_3D('',#66168,#51508,#51509);
#46176=AXIS2_PLACEMENT_3D('',#66170,#51510,#51511);
#46177=AXIS2_PLACEMENT_3D('',#66172,#51512,#51513);
#46178=AXIS2_PLACEMENT_3D('',#66173,#51514,#51515);
#46179=AXIS2_PLACEMENT_3D('',#66174,#51516,#51517);
#46180=AXIS2_PLACEMENT_3D('',#66176,#51518,#51519);
#46181=AXIS2_PLACEMENT_3D('',#66179,#51521,#51522);
#46182=AXIS2_PLACEMENT_3D('',#66191,#51523,#51524);
#46183=AXIS2_PLACEMENT_3D('',#66192,#51525,#51526);
#46184=AXIS2_PLACEMENT_3D('',#66196,#51528,#51529);
#46185=AXIS2_PLACEMENT_3D('',#66198,#51530,#51531);
#46186=AXIS2_PLACEMENT_3D('',#66200,#51533,#51534);
#46187=AXIS2_PLACEMENT_3D('',#66201,#51535,#51536);
#46188=AXIS2_PLACEMENT_3D('',#66242,#51539,#51540);
#46189=AXIS2_PLACEMENT_3D('',#66261,#51541,#51542);
#46190=AXIS2_PLACEMENT_3D('',#66262,#51543,#51544);
#46191=AXIS2_PLACEMENT_3D('',#66272,#51545,#51546);
#46192=AXIS2_PLACEMENT_3D('',#66292,#51548,#51549);
#46193=AXIS2_PLACEMENT_3D('',#66300,#51551,#51552);
#46194=AXIS2_PLACEMENT_3D('',#66303,#51553,#51554);
#46195=AXIS2_PLACEMENT_3D('',#66304,#51555,#51556);
#46196=AXIS2_PLACEMENT_3D('',#66305,#51557,#51558);
#46197=AXIS2_PLACEMENT_3D('',#66314,#51559,#51560);
#46198=AXIS2_PLACEMENT_3D('',#66315,#51561,#51562);
#46199=AXIS2_PLACEMENT_3D('',#66319,#51564,#51565);
#46200=AXIS2_PLACEMENT_3D('',#66321,#51566,#51567);
#46201=AXIS2_PLACEMENT_3D('',#66346,#51570,#51571);
#46202=AXIS2_PLACEMENT_3D('',#66347,#51572,#51573);
#46203=AXIS2_PLACEMENT_3D('',#66366,#51574,#51575);
#46204=AXIS2_PLACEMENT_3D('',#66385,#51577,#51578);
#46205=AXIS2_PLACEMENT_3D('',#66386,#51579,#51580);
#46206=AXIS2_PLACEMENT_3D('',#66390,#51582,#51583);
#46207=AXIS2_PLACEMENT_3D('',#66392,#51584,#51585);
#46208=AXIS2_PLACEMENT_3D('',#66405,#51587,#51588);
#46209=AXIS2_PLACEMENT_3D('',#66413,#51590,#51591);
#46210=AXIS2_PLACEMENT_3D('',#66416,#51592,#51593);
#46211=AXIS2_PLACEMENT_3D('',#66417,#51594,#51595);
#46212=AXIS2_PLACEMENT_3D('',#66418,#51596,#51597);
#46213=AXIS2_PLACEMENT_3D('',#66442,#51599,#51600);
#46214=AXIS2_PLACEMENT_3D('',#66445,#51601,#51602);
#46215=AXIS2_PLACEMENT_3D('',#66446,#51603,#51604);
#46216=AXIS2_PLACEMENT_3D('',#66447,#51605,#51606);
#46217=AXIS2_PLACEMENT_3D('',#66483,#51608,#51609);
#46218=AXIS2_PLACEMENT_3D('',#66485,#51610,#51611);
#46219=AXIS2_PLACEMENT_3D('',#66540,#51615,#51616);
#46220=AXIS2_PLACEMENT_3D('',#66543,#51617,#51618);
#46221=AXIS2_PLACEMENT_3D('',#66550,#51619,#51620);
#46222=AXIS2_PLACEMENT_3D('',#66559,#51621,#51622);
#46223=AXIS2_PLACEMENT_3D('',#66560,#51623,#51624);
#46224=AXIS2_PLACEMENT_3D('',#66564,#51626,#51627);
#46225=AXIS2_PLACEMENT_3D('',#66566,#51628,#51629);
#46226=AXIS2_PLACEMENT_3D('',#66602,#51632,#51633);
#46227=AXIS2_PLACEMENT_3D('',#66610,#51635,#51636);
#46228=AXIS2_PLACEMENT_3D('',#66613,#51637,#51638);
#46229=AXIS2_PLACEMENT_3D('',#66614,#51639,#51640);
#46230=AXIS2_PLACEMENT_3D('',#66615,#51641,#51642);
#46231=AXIS2_PLACEMENT_3D('',#66634,#51643,#51644);
#46232=AXIS2_PLACEMENT_3D('',#66635,#51645,#51646);
#46233=AXIS2_PLACEMENT_3D('',#66639,#51648,#51649);
#46234=AXIS2_PLACEMENT_3D('',#66641,#51650,#51651);
#46235=AXIS2_PLACEMENT_3D('',#66684,#51654,#51655);
#46236=AXIS2_PLACEMENT_3D('',#66692,#51657,#51658);
#46237=AXIS2_PLACEMENT_3D('',#66695,#51659,#51660);
#46238=AXIS2_PLACEMENT_3D('',#66696,#51661,#51662);
#46239=AXIS2_PLACEMENT_3D('',#66697,#51663,#51664);
#46240=AXIS2_PLACEMENT_3D('',#66712,#51665,#51666);
#46241=AXIS2_PLACEMENT_3D('',#66713,#51667,#51668);
#46242=AXIS2_PLACEMENT_3D('',#66717,#51670,#51671);
#46243=AXIS2_PLACEMENT_3D('',#66719,#51672,#51673);
#46244=AXIS2_PLACEMENT_3D('',#66760,#51676,#51677);
#46245=AXIS2_PLACEMENT_3D('',#66762,#51679,#51680);
#46246=AXIS2_PLACEMENT_3D('',#66763,#51681,#51682);
#46247=AXIS2_PLACEMENT_3D('',#66766,#51684,#51685);
#46248=AXIS2_PLACEMENT_3D('',#66767,#51686,#51687);
#46249=AXIS2_PLACEMENT_3D('',#66768,#51688,#51689);
#46250=AXIS2_PLACEMENT_3D('',#66787,#51690,#51691);
#46251=AXIS2_PLACEMENT_3D('',#66788,#51692,#51693);
#46252=AXIS2_PLACEMENT_3D('',#66798,#51694,#51695);
#46253=AXIS2_PLACEMENT_3D('',#66818,#51697,#51698);
#46254=AXIS2_PLACEMENT_3D('',#66826,#51700,#51701);
#46255=AXIS2_PLACEMENT_3D('',#66829,#51702,#51703);
#46256=AXIS2_PLACEMENT_3D('',#66830,#51704,#51705);
#46257=AXIS2_PLACEMENT_3D('',#66831,#51706,#51707);
#46258=AXIS2_PLACEMENT_3D('',#66840,#51708,#51709);
#46259=AXIS2_PLACEMENT_3D('',#66841,#51710,#51711);
#46260=AXIS2_PLACEMENT_3D('',#66845,#51713,#51714);
#46261=AXIS2_PLACEMENT_3D('',#66847,#51715,#51716);
#46262=AXIS2_PLACEMENT_3D('',#66872,#51719,#51720);
#46263=AXIS2_PLACEMENT_3D('',#66873,#51721,#51722);
#46264=AXIS2_PLACEMENT_3D('',#66892,#51723,#51724);
#46265=AXIS2_PLACEMENT_3D('',#66900,#51726,#51727);
#46266=AXIS2_PLACEMENT_3D('',#66903,#51728,#51729);
#46267=AXIS2_PLACEMENT_3D('',#66904,#51730,#51731);
#46268=AXIS2_PLACEMENT_3D('',#66905,#51732,#51733);
#46269=AXIS2_PLACEMENT_3D('',#66917,#51734,#51735);
#46270=AXIS2_PLACEMENT_3D('',#66918,#51736,#51737);
#46271=AXIS2_PLACEMENT_3D('',#66922,#51739,#51740);
#46272=AXIS2_PLACEMENT_3D('',#66924,#51741,#51742);
#46273=AXIS2_PLACEMENT_3D('',#66960,#51745,#51746);
#46274=AXIS2_PLACEMENT_3D('',#67003,#51749,#51750);
#46275=AXIS2_PLACEMENT_3D('',#67005,#51751,#51752);
#46276=AXIS2_PLACEMENT_3D('',#67037,#51755,#51756);
#46277=AXIS2_PLACEMENT_3D('',#67040,#51757,#51758);
#46278=AXIS2_PLACEMENT_3D('',#67041,#51759,#51760);
#46279=AXIS2_PLACEMENT_3D('',#67042,#51761,#51762);
#46280=AXIS2_PLACEMENT_3D('',#67066,#51764,#51765);
#46281=AXIS2_PLACEMENT_3D('',#67069,#51766,#51767);
#46282=AXIS2_PLACEMENT_3D('',#67076,#51768,#51769);
#46283=AXIS2_PLACEMENT_3D('',#67088,#51770,#51771);
#46284=AXIS2_PLACEMENT_3D('',#67089,#51772,#51773);
#46285=AXIS2_PLACEMENT_3D('',#67093,#51775,#51776);
#46286=AXIS2_PLACEMENT_3D('',#67095,#51777,#51778);
#46287=AXIS2_PLACEMENT_3D('',#67131,#51781,#51782);
#46288=AXIS2_PLACEMENT_3D('',#67139,#51784,#51785);
#46289=AXIS2_PLACEMENT_3D('',#67142,#51786,#51787);
#46290=AXIS2_PLACEMENT_3D('',#67143,#51788,#51789);
#46291=AXIS2_PLACEMENT_3D('',#67144,#51790,#51791);
#46292=AXIS2_PLACEMENT_3D('',#67163,#51792,#51793);
#46293=AXIS2_PLACEMENT_3D('',#67164,#51794,#51795);
#46294=AXIS2_PLACEMENT_3D('',#67168,#51797,#51798);
#46295=AXIS2_PLACEMENT_3D('',#67170,#51799,#51800);
#46296=AXIS2_PLACEMENT_3D('',#67206,#51803,#51804);
#46297=AXIS2_PLACEMENT_3D('',#67214,#51806,#51807);
#46298=AXIS2_PLACEMENT_3D('',#67217,#51808,#51809);
#46299=AXIS2_PLACEMENT_3D('',#67218,#51810,#51811);
#46300=AXIS2_PLACEMENT_3D('',#67219,#51812,#51813);
#46301=AXIS2_PLACEMENT_3D('',#67234,#51814,#51815);
#46302=AXIS2_PLACEMENT_3D('',#67235,#51816,#51817);
#46303=AXIS2_PLACEMENT_3D('',#67239,#51819,#51820);
#46304=AXIS2_PLACEMENT_3D('',#67241,#51821,#51822);
#46305=AXIS2_PLACEMENT_3D('',#67282,#51825,#51826);
#46306=AXIS2_PLACEMENT_3D('',#67284,#51828,#51829);
#46307=AXIS2_PLACEMENT_3D('',#67285,#51830,#51831);
#46308=AXIS2_PLACEMENT_3D('',#67288,#51833,#51834);
#46309=AXIS2_PLACEMENT_3D('',#67289,#51835,#51836);
#46310=AXIS2_PLACEMENT_3D('',#67290,#51837,#51838);
#46311=AXIS2_PLACEMENT_3D('',#67309,#51839,#51840);
#46312=AXIS2_PLACEMENT_3D('',#67310,#51841,#51842);
#46313=AXIS2_PLACEMENT_3D('',#67320,#51843,#51844);
#46314=AXIS2_PLACEMENT_3D('',#67340,#51846,#51847);
#46315=AXIS2_PLACEMENT_3D('',#67348,#51849,#51850);
#46316=AXIS2_PLACEMENT_3D('',#67351,#51851,#51852);
#46317=AXIS2_PLACEMENT_3D('',#67352,#51853,#51854);
#46318=AXIS2_PLACEMENT_3D('',#67353,#51855,#51856);
#46319=AXIS2_PLACEMENT_3D('',#67362,#51857,#51858);
#46320=AXIS2_PLACEMENT_3D('',#67363,#51859,#51860);
#46321=AXIS2_PLACEMENT_3D('',#67367,#51862,#51863);
#46322=AXIS2_PLACEMENT_3D('',#67369,#51864,#51865);
#46323=AXIS2_PLACEMENT_3D('',#67394,#51868,#51869);
#46324=AXIS2_PLACEMENT_3D('',#67395,#51870,#51871);
#46325=AXIS2_PLACEMENT_3D('',#67414,#51872,#51873);
#46326=AXIS2_PLACEMENT_3D('',#67422,#51875,#51876);
#46327=AXIS2_PLACEMENT_3D('',#67425,#51877,#51878);
#46328=AXIS2_PLACEMENT_3D('',#67426,#51879,#51880);
#46329=AXIS2_PLACEMENT_3D('',#67427,#51881,#51882);
#46330=AXIS2_PLACEMENT_3D('',#67439,#51883,#51884);
#46331=AXIS2_PLACEMENT_3D('',#67440,#51885,#51886);
#46332=AXIS2_PLACEMENT_3D('',#67444,#51888,#51889);
#46333=AXIS2_PLACEMENT_3D('',#67446,#51890,#51891);
#46334=AXIS2_PLACEMENT_3D('',#67482,#51894,#51895);
#46335=AXIS2_PLACEMENT_3D('',#67490,#51897,#51898);
#46336=AXIS2_PLACEMENT_3D('',#67493,#51899,#51900);
#46337=AXIS2_PLACEMENT_3D('',#67494,#51901,#51902);
#46338=AXIS2_PLACEMENT_3D('',#67495,#51903,#51904);
#46339=AXIS2_PLACEMENT_3D('',#67531,#51906,#51907);
#46340=AXIS2_PLACEMENT_3D('',#67533,#51908,#51909);
#46341=AXIS2_PLACEMENT_3D('',#67599,#51913,#51914);
#46342=AXIS2_PLACEMENT_3D('',#67600,#51915,#51916);
#46343=AXIS2_PLACEMENT_3D('',#67604,#51918,#51919);
#46344=AXIS2_PLACEMENT_3D('',#67606,#51920,#51921);
#46345=AXIS2_PLACEMENT_3D('',#67619,#51923,#51924);
#46346=AXIS2_PLACEMENT_3D('',#67627,#51926,#51927);
#46347=AXIS2_PLACEMENT_3D('',#67630,#51928,#51929);
#46348=AXIS2_PLACEMENT_3D('',#67637,#51930,#51931);
#46349=AXIS2_PLACEMENT_3D('',#67661,#51933,#51934);
#46350=AXIS2_PLACEMENT_3D('',#67664,#51935,#51936);
#46351=AXIS2_PLACEMENT_3D('',#67665,#51937,#51938);
#46352=AXIS2_PLACEMENT_3D('',#67666,#51939,#51940);
#46353=AXIS2_PLACEMENT_3D('',#67685,#51941,#51942);
#46354=AXIS2_PLACEMENT_3D('',#67686,#51943,#51944);
#46355=AXIS2_PLACEMENT_3D('',#67690,#51946,#51947);
#46356=AXIS2_PLACEMENT_3D('',#67692,#51948,#51949);
#46357=AXIS2_PLACEMENT_3D('',#67728,#51952,#51953);
#46358=AXIS2_PLACEMENT_3D('',#67736,#51955,#51956);
#46359=AXIS2_PLACEMENT_3D('',#67739,#51957,#51958);
#46360=AXIS2_PLACEMENT_3D('',#67740,#51959,#51960);
#46361=AXIS2_PLACEMENT_3D('',#67741,#51961,#51962);
#46362=AXIS2_PLACEMENT_3D('',#67753,#51963,#51964);
#46363=AXIS2_PLACEMENT_3D('',#67754,#51965,#51966);
#46364=AXIS2_PLACEMENT_3D('',#67758,#51968,#51969);
#46365=AXIS2_PLACEMENT_3D('',#67760,#51970,#51971);
#46366=AXIS2_PLACEMENT_3D('',#67794,#51974,#51975);
#46367=AXIS2_PLACEMENT_3D('',#67796,#51977,#51978);
#46368=AXIS2_PLACEMENT_3D('',#67797,#51979,#51980);
#46369=AXIS2_PLACEMENT_3D('',#67800,#51982,#51983);
#46370=AXIS2_PLACEMENT_3D('',#67801,#51984,#51985);
#46371=AXIS2_PLACEMENT_3D('',#67802,#51986,#51987);
#46372=AXIS2_PLACEMENT_3D('',#67821,#51988,#51989);
#46373=AXIS2_PLACEMENT_3D('',#67822,#51990,#51991);
#46374=AXIS2_PLACEMENT_3D('',#67832,#51992,#51993);
#46375=AXIS2_PLACEMENT_3D('',#67852,#51995,#51996);
#46376=AXIS2_PLACEMENT_3D('',#67860,#51998,#51999);
#46377=AXIS2_PLACEMENT_3D('',#67863,#52000,#52001);
#46378=AXIS2_PLACEMENT_3D('',#67864,#52002,#52003);
#46379=AXIS2_PLACEMENT_3D('',#67865,#52004,#52005);
#46380=AXIS2_PLACEMENT_3D('',#67874,#52006,#52007);
#46381=AXIS2_PLACEMENT_3D('',#67875,#52008,#52009);
#46382=AXIS2_PLACEMENT_3D('',#67879,#52011,#52012);
#46383=AXIS2_PLACEMENT_3D('',#67881,#52013,#52014);
#46384=AXIS2_PLACEMENT_3D('',#67906,#52017,#52018);
#46385=AXIS2_PLACEMENT_3D('',#67907,#52019,#52020);
#46386=AXIS2_PLACEMENT_3D('',#67926,#52021,#52022);
#46387=AXIS2_PLACEMENT_3D('',#67934,#52024,#52025);
#46388=AXIS2_PLACEMENT_3D('',#67937,#52026,#52027);
#46389=AXIS2_PLACEMENT_3D('',#67938,#52028,#52029);
#46390=AXIS2_PLACEMENT_3D('',#67939,#52030,#52031);
#46391=AXIS2_PLACEMENT_3D('',#67951,#52032,#52033);
#46392=AXIS2_PLACEMENT_3D('',#67952,#52034,#52035);
#46393=AXIS2_PLACEMENT_3D('',#67956,#52037,#52038);
#46394=AXIS2_PLACEMENT_3D('',#67958,#52039,#52040);
#46395=AXIS2_PLACEMENT_3D('',#67994,#52043,#52044);
#46396=AXIS2_PLACEMENT_3D('',#68002,#52046,#52047);
#46397=AXIS2_PLACEMENT_3D('',#68005,#52048,#52049);
#46398=AXIS2_PLACEMENT_3D('',#68006,#52050,#52051);
#46399=AXIS2_PLACEMENT_3D('',#68007,#52052,#52053);
#46400=AXIS2_PLACEMENT_3D('',#68043,#52055,#52056);
#46401=AXIS2_PLACEMENT_3D('',#68045,#52057,#52058);
#46402=AXIS2_PLACEMENT_3D('',#68100,#52062,#52063);
#46403=AXIS2_PLACEMENT_3D('',#68103,#52064,#52065);
#46404=AXIS2_PLACEMENT_3D('',#68110,#52066,#52067);
#46405=AXIS2_PLACEMENT_3D('',#68122,#52068,#52069);
#46406=AXIS2_PLACEMENT_3D('',#68123,#52070,#52071);
#46407=AXIS2_PLACEMENT_3D('',#68127,#52073,#52074);
#46408=AXIS2_PLACEMENT_3D('',#68129,#52075,#52076);
#46409=AXIS2_PLACEMENT_3D('',#68165,#52079,#52080);
#46410=AXIS2_PLACEMENT_3D('',#68191,#52082,#52083);
#46411=AXIS2_PLACEMENT_3D('',#68192,#52084,#52085);
#46412=AXIS2_PLACEMENT_3D('',#68196,#52087,#52088);
#46413=AXIS2_PLACEMENT_3D('',#68198,#52089,#52090);
#46414=AXIS2_PLACEMENT_3D('',#68211,#52092,#52093);
#46415=AXIS2_PLACEMENT_3D('',#68219,#52095,#52096);
#46416=AXIS2_PLACEMENT_3D('',#68222,#52097,#52098);
#46417=AXIS2_PLACEMENT_3D('',#68223,#52099,#52100);
#46418=AXIS2_PLACEMENT_3D('',#68224,#52101,#52102);
#46419=AXIS2_PLACEMENT_3D('',#68248,#52104,#52105);
#46420=AXIS2_PLACEMENT_3D('',#68251,#52106,#52107);
#46421=AXIS2_PLACEMENT_3D('',#68252,#52108,#52109);
#46422=AXIS2_PLACEMENT_3D('',#68253,#52110,#52111);
#46423=AXIS2_PLACEMENT_3D('',#68265,#52112,#52113);
#46424=AXIS2_PLACEMENT_3D('',#68266,#52114,#52115);
#46425=AXIS2_PLACEMENT_3D('',#68270,#52117,#52118);
#46426=AXIS2_PLACEMENT_3D('',#68272,#52119,#52120);
#46427=AXIS2_PLACEMENT_3D('',#68306,#52123,#52124);
#46428=AXIS2_PLACEMENT_3D('',#68308,#52126,#52127);
#46429=AXIS2_PLACEMENT_3D('',#68309,#52128,#52129);
#46430=AXIS2_PLACEMENT_3D('',#68312,#52131,#52132);
#46431=AXIS2_PLACEMENT_3D('',#68313,#52133,#52134);
#46432=AXIS2_PLACEMENT_3D('',#68314,#52135,#52136);
#46433=AXIS2_PLACEMENT_3D('',#68333,#52137,#52138);
#46434=AXIS2_PLACEMENT_3D('',#68334,#52139,#52140);
#46435=AXIS2_PLACEMENT_3D('',#68344,#52141,#52142);
#46436=AXIS2_PLACEMENT_3D('',#68364,#52144,#52145);
#46437=AXIS2_PLACEMENT_3D('',#68372,#52147,#52148);
#46438=AXIS2_PLACEMENT_3D('',#68375,#52149,#52150);
#46439=AXIS2_PLACEMENT_3D('',#68376,#52151,#52152);
#46440=AXIS2_PLACEMENT_3D('',#68377,#52153,#52154);
#46441=AXIS2_PLACEMENT_3D('',#68386,#52155,#52156);
#46442=AXIS2_PLACEMENT_3D('',#68387,#52157,#52158);
#46443=AXIS2_PLACEMENT_3D('',#68391,#52160,#52161);
#46444=AXIS2_PLACEMENT_3D('',#68393,#52162,#52163);
#46445=AXIS2_PLACEMENT_3D('',#68418,#52166,#52167);
#46446=AXIS2_PLACEMENT_3D('',#68419,#52168,#52169);
#46447=AXIS2_PLACEMENT_3D('',#68438,#52170,#52171);
#46448=AXIS2_PLACEMENT_3D('',#68446,#52173,#52174);
#46449=AXIS2_PLACEMENT_3D('',#68449,#52175,#52176);
#46450=AXIS2_PLACEMENT_3D('',#68450,#52177,#52178);
#46451=AXIS2_PLACEMENT_3D('',#68451,#52179,#52180);
#46452=AXIS2_PLACEMENT_3D('',#68463,#52181,#52182);
#46453=AXIS2_PLACEMENT_3D('',#68464,#52183,#52184);
#46454=AXIS2_PLACEMENT_3D('',#68468,#52186,#52187);
#46455=AXIS2_PLACEMENT_3D('',#68470,#52188,#52189);
#46456=AXIS2_PLACEMENT_3D('',#68506,#52192,#52193);
#46457=AXIS2_PLACEMENT_3D('',#68514,#52195,#52196);
#46458=AXIS2_PLACEMENT_3D('',#68517,#52197,#52198);
#46459=AXIS2_PLACEMENT_3D('',#68518,#52199,#52200);
#46460=AXIS2_PLACEMENT_3D('',#68519,#52201,#52202);
#46461=AXIS2_PLACEMENT_3D('',#68555,#52204,#52205);
#46462=AXIS2_PLACEMENT_3D('',#68557,#52206,#52207);
#46463=AXIS2_PLACEMENT_3D('',#68612,#52211,#52212);
#46464=AXIS2_PLACEMENT_3D('',#68615,#52213,#52214);
#46465=AXIS2_PLACEMENT_3D('',#68622,#52215,#52216);
#46466=AXIS2_PLACEMENT_3D('',#68634,#52217,#52218);
#46467=AXIS2_PLACEMENT_3D('',#68635,#52219,#52220);
#46468=AXIS2_PLACEMENT_3D('',#68639,#52222,#52223);
#46469=AXIS2_PLACEMENT_3D('',#68641,#52224,#52225);
#46470=AXIS2_PLACEMENT_3D('',#68677,#52228,#52229);
#46471=AXIS2_PLACEMENT_3D('',#68685,#52231,#52232);
#46472=AXIS2_PLACEMENT_3D('',#68688,#52233,#52234);
#46473=AXIS2_PLACEMENT_3D('',#68689,#52235,#52236);
#46474=AXIS2_PLACEMENT_3D('',#68690,#52237,#52238);
#46475=AXIS2_PLACEMENT_3D('',#68709,#52239,#52240);
#46476=AXIS2_PLACEMENT_3D('',#68710,#52241,#52242);
#46477=AXIS2_PLACEMENT_3D('',#68714,#52244,#52245);
#46478=AXIS2_PLACEMENT_3D('',#68716,#52246,#52247);
#46479=AXIS2_PLACEMENT_3D('',#68752,#52250,#52251);
#46480=AXIS2_PLACEMENT_3D('',#68774,#52253,#52254);
#46481=AXIS2_PLACEMENT_3D('',#68775,#52255,#52256);
#46482=AXIS2_PLACEMENT_3D('',#68779,#52258,#52259);
#46483=AXIS2_PLACEMENT_3D('',#68781,#52260,#52261);
#46484=AXIS2_PLACEMENT_3D('',#68792,#52263,#52264);
#46485=AXIS2_PLACEMENT_3D('',#68794,#52266,#52267);
#46486=AXIS2_PLACEMENT_3D('',#68797,#52268,#52269);
#46487=AXIS2_PLACEMENT_3D('',#68798,#52270,#52271);
#46488=AXIS2_PLACEMENT_3D('',#68799,#52272,#52273);
#46489=AXIS2_PLACEMENT_3D('',#68823,#52275,#52276);
#46490=AXIS2_PLACEMENT_3D('',#68824,#52277,#52278);
#46491=AXIS2_PLACEMENT_3D('',#68827,#52280,#52281);
#46492=AXIS2_PLACEMENT_3D('',#68828,#52282,#52283);
#46493=AXIS2_PLACEMENT_3D('',#68829,#52284,#52285);
#46494=AXIS2_PLACEMENT_3D('',#68848,#52286,#52287);
#46495=AXIS2_PLACEMENT_3D('',#68849,#52288,#52289);
#46496=AXIS2_PLACEMENT_3D('',#68859,#52290,#52291);
#46497=AXIS2_PLACEMENT_3D('',#68879,#52293,#52294);
#46498=AXIS2_PLACEMENT_3D('',#68887,#52296,#52297);
#46499=AXIS2_PLACEMENT_3D('',#68890,#52298,#52299);
#46500=AXIS2_PLACEMENT_3D('',#68891,#52300,#52301);
#46501=AXIS2_PLACEMENT_3D('',#68892,#52302,#52303);
#46502=AXIS2_PLACEMENT_3D('',#68901,#52304,#52305);
#46503=AXIS2_PLACEMENT_3D('',#68902,#52306,#52307);
#46504=AXIS2_PLACEMENT_3D('',#68906,#52309,#52310);
#46505=AXIS2_PLACEMENT_3D('',#68908,#52311,#52312);
#46506=AXIS2_PLACEMENT_3D('',#68933,#52315,#52316);
#46507=AXIS2_PLACEMENT_3D('',#68934,#52317,#52318);
#46508=AXIS2_PLACEMENT_3D('',#68953,#52319,#52320);
#46509=AXIS2_PLACEMENT_3D('',#68961,#52322,#52323);
#46510=AXIS2_PLACEMENT_3D('',#68964,#52324,#52325);
#46511=AXIS2_PLACEMENT_3D('',#68965,#52326,#52327);
#46512=AXIS2_PLACEMENT_3D('',#68966,#52328,#52329);
#46513=AXIS2_PLACEMENT_3D('',#68978,#52330,#52331);
#46514=AXIS2_PLACEMENT_3D('',#68979,#52332,#52333);
#46515=AXIS2_PLACEMENT_3D('',#68983,#52335,#52336);
#46516=AXIS2_PLACEMENT_3D('',#68985,#52337,#52338);
#46517=AXIS2_PLACEMENT_3D('',#69021,#52341,#52342);
#46518=AXIS2_PLACEMENT_3D('',#69029,#52344,#52345);
#46519=AXIS2_PLACEMENT_3D('',#69032,#52346,#52347);
#46520=AXIS2_PLACEMENT_3D('',#69033,#52348,#52349);
#46521=AXIS2_PLACEMENT_3D('',#69034,#52350,#52351);
#46522=AXIS2_PLACEMENT_3D('',#69070,#52353,#52354);
#46523=AXIS2_PLACEMENT_3D('',#69072,#52355,#52356);
#46524=AXIS2_PLACEMENT_3D('',#69127,#52360,#52361);
#46525=AXIS2_PLACEMENT_3D('',#69130,#52362,#52363);
#46526=AXIS2_PLACEMENT_3D('',#69137,#52364,#52365);
#46527=AXIS2_PLACEMENT_3D('',#69149,#52366,#52367);
#46528=AXIS2_PLACEMENT_3D('',#69150,#52368,#52369);
#46529=AXIS2_PLACEMENT_3D('',#69154,#52371,#52372);
#46530=AXIS2_PLACEMENT_3D('',#69156,#52373,#52374);
#46531=AXIS2_PLACEMENT_3D('',#69192,#52377,#52378);
#46532=AXIS2_PLACEMENT_3D('',#69200,#52380,#52381);
#46533=AXIS2_PLACEMENT_3D('',#69203,#52382,#52383);
#46534=AXIS2_PLACEMENT_3D('',#69204,#52384,#52385);
#46535=AXIS2_PLACEMENT_3D('',#69205,#52386,#52387);
#46536=AXIS2_PLACEMENT_3D('',#69224,#52388,#52389);
#46537=AXIS2_PLACEMENT_3D('',#69225,#52390,#52391);
#46538=AXIS2_PLACEMENT_3D('',#69229,#52393,#52394);
#46539=AXIS2_PLACEMENT_3D('',#69231,#52395,#52396);
#46540=AXIS2_PLACEMENT_3D('',#69267,#52399,#52400);
#46541=AXIS2_PLACEMENT_3D('',#69275,#52402,#52403);
#46542=AXIS2_PLACEMENT_3D('',#69278,#52404,#52405);
#46543=AXIS2_PLACEMENT_3D('',#69279,#52406,#52407);
#46544=AXIS2_PLACEMENT_3D('',#69280,#52408,#52409);
#46545=AXIS2_PLACEMENT_3D('',#69295,#52410,#52411);
#46546=AXIS2_PLACEMENT_3D('',#69296,#52412,#52413);
#46547=AXIS2_PLACEMENT_3D('',#69300,#52415,#52416);
#46548=AXIS2_PLACEMENT_3D('',#69302,#52417,#52418);
#46549=AXIS2_PLACEMENT_3D('',#69336,#52421,#52422);
#46550=AXIS2_PLACEMENT_3D('',#69338,#52424,#52425);
#46551=AXIS2_PLACEMENT_3D('',#69339,#52426,#52427);
#46552=AXIS2_PLACEMENT_3D('',#69342,#52429,#52430);
#46553=AXIS2_PLACEMENT_3D('',#69343,#52431,#52432);
#46554=AXIS2_PLACEMENT_3D('',#69344,#52433,#52434);
#46555=AXIS2_PLACEMENT_3D('',#69363,#52435,#52436);
#46556=AXIS2_PLACEMENT_3D('',#69364,#52437,#52438);
#46557=AXIS2_PLACEMENT_3D('',#69374,#52439,#52440);
#46558=AXIS2_PLACEMENT_3D('',#69394,#52442,#52443);
#46559=AXIS2_PLACEMENT_3D('',#69402,#52445,#52446);
#46560=AXIS2_PLACEMENT_3D('',#69405,#52447,#52448);
#46561=AXIS2_PLACEMENT_3D('',#69406,#52449,#52450);
#46562=AXIS2_PLACEMENT_3D('',#69407,#52451,#52452);
#46563=AXIS2_PLACEMENT_3D('',#69416,#52453,#52454);
#46564=AXIS2_PLACEMENT_3D('',#69417,#52455,#52456);
#46565=AXIS2_PLACEMENT_3D('',#69421,#52458,#52459);
#46566=AXIS2_PLACEMENT_3D('',#69423,#52460,#52461);
#46567=AXIS2_PLACEMENT_3D('',#69448,#52464,#52465);
#46568=AXIS2_PLACEMENT_3D('',#69449,#52466,#52467);
#46569=AXIS2_PLACEMENT_3D('',#69468,#52468,#52469);
#46570=AXIS2_PLACEMENT_3D('',#69476,#52471,#52472);
#46571=AXIS2_PLACEMENT_3D('',#69479,#52473,#52474);
#46572=AXIS2_PLACEMENT_3D('',#69480,#52475,#52476);
#46573=AXIS2_PLACEMENT_3D('',#69481,#52477,#52478);
#46574=AXIS2_PLACEMENT_3D('',#69493,#52479,#52480);
#46575=AXIS2_PLACEMENT_3D('',#69494,#52481,#52482);
#46576=AXIS2_PLACEMENT_3D('',#69498,#52484,#52485);
#46577=AXIS2_PLACEMENT_3D('',#69500,#52486,#52487);
#46578=AXIS2_PLACEMENT_3D('',#69536,#52490,#52491);
#46579=AXIS2_PLACEMENT_3D('',#69544,#52493,#52494);
#46580=AXIS2_PLACEMENT_3D('',#69547,#52495,#52496);
#46581=AXIS2_PLACEMENT_3D('',#69548,#52497,#52498);
#46582=AXIS2_PLACEMENT_3D('',#69549,#52499,#52500);
#46583=AXIS2_PLACEMENT_3D('',#69585,#52502,#52503);
#46584=AXIS2_PLACEMENT_3D('',#69587,#52504,#52505);
#46585=AXIS2_PLACEMENT_3D('',#69642,#52509,#52510);
#46586=AXIS2_PLACEMENT_3D('',#69645,#52511,#52512);
#46587=AXIS2_PLACEMENT_3D('',#69652,#52513,#52514);
#46588=AXIS2_PLACEMENT_3D('',#69664,#52515,#52516);
#46589=AXIS2_PLACEMENT_3D('',#69665,#52517,#52518);
#46590=AXIS2_PLACEMENT_3D('',#69669,#52520,#52521);
#46591=AXIS2_PLACEMENT_3D('',#69671,#52522,#52523);
#46592=AXIS2_PLACEMENT_3D('',#69707,#52526,#52527);
#46593=AXIS2_PLACEMENT_3D('',#69715,#52529,#52530);
#46594=AXIS2_PLACEMENT_3D('',#69718,#52531,#52532);
#46595=AXIS2_PLACEMENT_3D('',#69719,#52533,#52534);
#46596=AXIS2_PLACEMENT_3D('',#69720,#52535,#52536);
#46597=AXIS2_PLACEMENT_3D('',#69739,#52537,#52538);
#46598=AXIS2_PLACEMENT_3D('',#69740,#52539,#52540);
#46599=AXIS2_PLACEMENT_3D('',#69744,#52542,#52543);
#46600=AXIS2_PLACEMENT_3D('',#69746,#52544,#52545);
#46601=AXIS2_PLACEMENT_3D('',#69782,#52548,#52549);
#46602=AXIS2_PLACEMENT_3D('',#69790,#52551,#52552);
#46603=AXIS2_PLACEMENT_3D('',#69793,#52553,#52554);
#46604=AXIS2_PLACEMENT_3D('',#69794,#52555,#52556);
#46605=AXIS2_PLACEMENT_3D('',#69795,#52557,#52558);
#46606=AXIS2_PLACEMENT_3D('',#69810,#52559,#52560);
#46607=AXIS2_PLACEMENT_3D('',#69811,#52561,#52562);
#46608=AXIS2_PLACEMENT_3D('',#69815,#52564,#52565);
#46609=AXIS2_PLACEMENT_3D('',#69817,#52566,#52567);
#46610=AXIS2_PLACEMENT_3D('',#69851,#52570,#52571);
#46611=AXIS2_PLACEMENT_3D('',#69853,#52573,#52574);
#46612=AXIS2_PLACEMENT_3D('',#69854,#52575,#52576);
#46613=AXIS2_PLACEMENT_3D('',#69857,#52578,#52579);
#46614=AXIS2_PLACEMENT_3D('',#69858,#52580,#52581);
#46615=AXIS2_PLACEMENT_3D('',#69859,#52582,#52583);
#46616=AXIS2_PLACEMENT_3D('',#69878,#52584,#52585);
#46617=AXIS2_PLACEMENT_3D('',#69879,#52586,#52587);
#46618=AXIS2_PLACEMENT_3D('',#69889,#52588,#52589);
#46619=AXIS2_PLACEMENT_3D('',#69909,#52591,#52592);
#46620=AXIS2_PLACEMENT_3D('',#69917,#52594,#52595);
#46621=AXIS2_PLACEMENT_3D('',#69920,#52596,#52597);
#46622=AXIS2_PLACEMENT_3D('',#69921,#52598,#52599);
#46623=AXIS2_PLACEMENT_3D('',#69922,#52600,#52601);
#46624=AXIS2_PLACEMENT_3D('',#69931,#52602,#52603);
#46625=AXIS2_PLACEMENT_3D('',#69932,#52604,#52605);
#46626=AXIS2_PLACEMENT_3D('',#69936,#52607,#52608);
#46627=AXIS2_PLACEMENT_3D('',#69938,#52609,#52610);
#46628=AXIS2_PLACEMENT_3D('',#69963,#52613,#52614);
#46629=AXIS2_PLACEMENT_3D('',#69964,#52615,#52616);
#46630=AXIS2_PLACEMENT_3D('',#69983,#52617,#52618);
#46631=AXIS2_PLACEMENT_3D('',#69991,#52620,#52621);
#46632=AXIS2_PLACEMENT_3D('',#69994,#52622,#52623);
#46633=AXIS2_PLACEMENT_3D('',#69995,#52624,#52625);
#46634=AXIS2_PLACEMENT_3D('',#69996,#52626,#52627);
#46635=AXIS2_PLACEMENT_3D('',#70008,#52628,#52629);
#46636=AXIS2_PLACEMENT_3D('',#70009,#52630,#52631);
#46637=AXIS2_PLACEMENT_3D('',#70013,#52633,#52634);
#46638=AXIS2_PLACEMENT_3D('',#70015,#52635,#52636);
#46639=AXIS2_PLACEMENT_3D('',#70051,#52639,#52640);
#46640=AXIS2_PLACEMENT_3D('',#70059,#52642,#52643);
#46641=AXIS2_PLACEMENT_3D('',#70062,#52644,#52645);
#46642=AXIS2_PLACEMENT_3D('',#70063,#52646,#52647);
#46643=AXIS2_PLACEMENT_3D('',#70064,#52648,#52649);
#46644=AXIS2_PLACEMENT_3D('',#70100,#52651,#52652);
#46645=AXIS2_PLACEMENT_3D('',#70102,#52653,#52654);
#46646=AXIS2_PLACEMENT_3D('',#70157,#52658,#52659);
#46647=AXIS2_PLACEMENT_3D('',#70160,#52660,#52661);
#46648=AXIS2_PLACEMENT_3D('',#70167,#52662,#52663);
#46649=AXIS2_PLACEMENT_3D('',#70179,#52664,#52665);
#46650=AXIS2_PLACEMENT_3D('',#70180,#52666,#52667);
#46651=AXIS2_PLACEMENT_3D('',#70184,#52669,#52670);
#46652=AXIS2_PLACEMENT_3D('',#70186,#52671,#52672);
#46653=AXIS2_PLACEMENT_3D('',#70222,#52675,#52676);
#46654=AXIS2_PLACEMENT_3D('',#70230,#52678,#52679);
#46655=AXIS2_PLACEMENT_3D('',#70233,#52680,#52681);
#46656=AXIS2_PLACEMENT_3D('',#70234,#52682,#52683);
#46657=AXIS2_PLACEMENT_3D('',#70235,#52684,#52685);
#46658=AXIS2_PLACEMENT_3D('',#70254,#52686,#52687);
#46659=AXIS2_PLACEMENT_3D('',#70255,#52688,#52689);
#46660=AXIS2_PLACEMENT_3D('',#70259,#52691,#52692);
#46661=AXIS2_PLACEMENT_3D('',#70261,#52693,#52694);
#46662=AXIS2_PLACEMENT_3D('',#70297,#52697,#52698);
#46663=AXIS2_PLACEMENT_3D('',#70305,#52700,#52701);
#46664=AXIS2_PLACEMENT_3D('',#70308,#52702,#52703);
#46665=AXIS2_PLACEMENT_3D('',#70309,#52704,#52705);
#46666=AXIS2_PLACEMENT_3D('',#70310,#52706,#52707);
#46667=AXIS2_PLACEMENT_3D('',#70325,#52708,#52709);
#46668=AXIS2_PLACEMENT_3D('',#70326,#52710,#52711);
#46669=AXIS2_PLACEMENT_3D('',#70330,#52713,#52714);
#46670=AXIS2_PLACEMENT_3D('',#70332,#52715,#52716);
#46671=AXIS2_PLACEMENT_3D('',#70366,#52719,#52720);
#46672=AXIS2_PLACEMENT_3D('',#70368,#52722,#52723);
#46673=AXIS2_PLACEMENT_3D('',#70369,#52724,#52725);
#46674=AXIS2_PLACEMENT_3D('',#70372,#52727,#52728);
#46675=AXIS2_PLACEMENT_3D('',#70373,#52729,#52730);
#46676=AXIS2_PLACEMENT_3D('',#70374,#52731,#52732);
#46677=AXIS2_PLACEMENT_3D('',#70393,#52733,#52734);
#46678=AXIS2_PLACEMENT_3D('',#70394,#52735,#52736);
#46679=AXIS2_PLACEMENT_3D('',#70404,#52737,#52738);
#46680=AXIS2_PLACEMENT_3D('',#70424,#52740,#52741);
#46681=AXIS2_PLACEMENT_3D('',#70432,#52743,#52744);
#46682=AXIS2_PLACEMENT_3D('',#70435,#52745,#52746);
#46683=AXIS2_PLACEMENT_3D('',#70436,#52747,#52748);
#46684=AXIS2_PLACEMENT_3D('',#70437,#52749,#52750);
#46685=AXIS2_PLACEMENT_3D('',#70446,#52751,#52752);
#46686=AXIS2_PLACEMENT_3D('',#70447,#52753,#52754);
#46687=AXIS2_PLACEMENT_3D('',#70451,#52756,#52757);
#46688=AXIS2_PLACEMENT_3D('',#70453,#52758,#52759);
#46689=AXIS2_PLACEMENT_3D('',#70478,#52762,#52763);
#46690=AXIS2_PLACEMENT_3D('',#70479,#52764,#52765);
#46691=AXIS2_PLACEMENT_3D('',#70498,#52766,#52767);
#46692=AXIS2_PLACEMENT_3D('',#70506,#52769,#52770);
#46693=AXIS2_PLACEMENT_3D('',#70509,#52771,#52772);
#46694=AXIS2_PLACEMENT_3D('',#70510,#52773,#52774);
#46695=AXIS2_PLACEMENT_3D('',#70511,#52775,#52776);
#46696=AXIS2_PLACEMENT_3D('',#70523,#52777,#52778);
#46697=AXIS2_PLACEMENT_3D('',#70524,#52779,#52780);
#46698=AXIS2_PLACEMENT_3D('',#70528,#52782,#52783);
#46699=AXIS2_PLACEMENT_3D('',#70530,#52784,#52785);
#46700=AXIS2_PLACEMENT_3D('',#70566,#52788,#52789);
#46701=AXIS2_PLACEMENT_3D('',#70574,#52791,#52792);
#46702=AXIS2_PLACEMENT_3D('',#70577,#52793,#52794);
#46703=AXIS2_PLACEMENT_3D('',#70578,#52795,#52796);
#46704=AXIS2_PLACEMENT_3D('',#70579,#52797,#52798);
#46705=AXIS2_PLACEMENT_3D('',#70615,#52800,#52801);
#46706=AXIS2_PLACEMENT_3D('',#70617,#52802,#52803);
#46707=AXIS2_PLACEMENT_3D('',#70672,#52807,#52808);
#46708=AXIS2_PLACEMENT_3D('',#70675,#52809,#52810);
#46709=AXIS2_PLACEMENT_3D('',#70682,#52811,#52812);
#46710=AXIS2_PLACEMENT_3D('',#70694,#52813,#52814);
#46711=AXIS2_PLACEMENT_3D('',#70695,#52815,#52816);
#46712=AXIS2_PLACEMENT_3D('',#70699,#52818,#52819);
#46713=AXIS2_PLACEMENT_3D('',#70701,#52820,#52821);
#46714=AXIS2_PLACEMENT_3D('',#70737,#52824,#52825);
#46715=AXIS2_PLACEMENT_3D('',#70745,#52827,#52828);
#46716=AXIS2_PLACEMENT_3D('',#70748,#52829,#52830);
#46717=AXIS2_PLACEMENT_3D('',#70749,#52831,#52832);
#46718=AXIS2_PLACEMENT_3D('',#70750,#52833,#52834);
#46719=AXIS2_PLACEMENT_3D('',#70769,#52835,#52836);
#46720=AXIS2_PLACEMENT_3D('',#70770,#52837,#52838);
#46721=AXIS2_PLACEMENT_3D('',#70774,#52840,#52841);
#46722=AXIS2_PLACEMENT_3D('',#70776,#52842,#52843);
#46723=AXIS2_PLACEMENT_3D('',#70812,#52846,#52847);
#46724=AXIS2_PLACEMENT_3D('',#70820,#52849,#52850);
#46725=AXIS2_PLACEMENT_3D('',#70823,#52851,#52852);
#46726=AXIS2_PLACEMENT_3D('',#70824,#52853,#52854);
#46727=AXIS2_PLACEMENT_3D('',#70825,#52855,#52856);
#46728=AXIS2_PLACEMENT_3D('',#70840,#52857,#52858);
#46729=AXIS2_PLACEMENT_3D('',#70841,#52859,#52860);
#46730=AXIS2_PLACEMENT_3D('',#70845,#52862,#52863);
#46731=AXIS2_PLACEMENT_3D('',#70847,#52864,#52865);
#46732=AXIS2_PLACEMENT_3D('',#70881,#52868,#52869);
#46733=AXIS2_PLACEMENT_3D('',#70883,#52871,#52872);
#46734=AXIS2_PLACEMENT_3D('',#70884,#52873,#52874);
#46735=AXIS2_PLACEMENT_3D('',#70887,#52876,#52877);
#46736=AXIS2_PLACEMENT_3D('',#70888,#52878,#52879);
#46737=AXIS2_PLACEMENT_3D('',#70889,#52880,#52881);
#46738=AXIS2_PLACEMENT_3D('',#70908,#52882,#52883);
#46739=AXIS2_PLACEMENT_3D('',#70909,#52884,#52885);
#46740=AXIS2_PLACEMENT_3D('',#70919,#52886,#52887);
#46741=AXIS2_PLACEMENT_3D('',#70939,#52889,#52890);
#46742=AXIS2_PLACEMENT_3D('',#70947,#52892,#52893);
#46743=AXIS2_PLACEMENT_3D('',#70950,#52894,#52895);
#46744=AXIS2_PLACEMENT_3D('',#70951,#52896,#52897);
#46745=AXIS2_PLACEMENT_3D('',#70952,#52898,#52899);
#46746=AXIS2_PLACEMENT_3D('',#70961,#52900,#52901);
#46747=AXIS2_PLACEMENT_3D('',#70962,#52902,#52903);
#46748=AXIS2_PLACEMENT_3D('',#70966,#52905,#52906);
#46749=AXIS2_PLACEMENT_3D('',#70968,#52907,#52908);
#46750=AXIS2_PLACEMENT_3D('',#70993,#52911,#52912);
#46751=AXIS2_PLACEMENT_3D('',#70994,#52913,#52914);
#46752=AXIS2_PLACEMENT_3D('',#71013,#52915,#52916);
#46753=AXIS2_PLACEMENT_3D('',#71021,#52918,#52919);
#46754=AXIS2_PLACEMENT_3D('',#71024,#52920,#52921);
#46755=AXIS2_PLACEMENT_3D('',#71025,#52922,#52923);
#46756=AXIS2_PLACEMENT_3D('',#71026,#52924,#52925);
#46757=AXIS2_PLACEMENT_3D('',#71038,#52926,#52927);
#46758=AXIS2_PLACEMENT_3D('',#71039,#52928,#52929);
#46759=AXIS2_PLACEMENT_3D('',#71043,#52931,#52932);
#46760=AXIS2_PLACEMENT_3D('',#71045,#52933,#52934);
#46761=AXIS2_PLACEMENT_3D('',#71081,#52937,#52938);
#46762=AXIS2_PLACEMENT_3D('',#71089,#52940,#52941);
#46763=AXIS2_PLACEMENT_3D('',#71092,#52942,#52943);
#46764=AXIS2_PLACEMENT_3D('',#71093,#52944,#52945);
#46765=AXIS2_PLACEMENT_3D('',#71094,#52946,#52947);
#46766=AXIS2_PLACEMENT_3D('',#71130,#52949,#52950);
#46767=AXIS2_PLACEMENT_3D('',#71132,#52951,#52952);
#46768=AXIS2_PLACEMENT_3D('',#71187,#52956,#52957);
#46769=AXIS2_PLACEMENT_3D('',#71190,#52958,#52959);
#46770=AXIS2_PLACEMENT_3D('',#71197,#52960,#52961);
#46771=AXIS2_PLACEMENT_3D('',#71209,#52962,#52963);
#46772=AXIS2_PLACEMENT_3D('',#71210,#52964,#52965);
#46773=AXIS2_PLACEMENT_3D('',#71214,#52967,#52968);
#46774=AXIS2_PLACEMENT_3D('',#71216,#52969,#52970);
#46775=AXIS2_PLACEMENT_3D('',#71252,#52973,#52974);
#46776=AXIS2_PLACEMENT_3D('',#71260,#52976,#52977);
#46777=AXIS2_PLACEMENT_3D('',#71263,#52978,#52979);
#46778=AXIS2_PLACEMENT_3D('',#71264,#52980,#52981);
#46779=AXIS2_PLACEMENT_3D('',#71265,#52982,#52983);
#46780=AXIS2_PLACEMENT_3D('',#71284,#52984,#52985);
#46781=AXIS2_PLACEMENT_3D('',#71285,#52986,#52987);
#46782=AXIS2_PLACEMENT_3D('',#71289,#52989,#52990);
#46783=AXIS2_PLACEMENT_3D('',#71291,#52991,#52992);
#46784=AXIS2_PLACEMENT_3D('',#71327,#52995,#52996);
#46785=AXIS2_PLACEMENT_3D('',#71335,#52998,#52999);
#46786=AXIS2_PLACEMENT_3D('',#71338,#53000,#53001);
#46787=AXIS2_PLACEMENT_3D('',#71339,#53002,#53003);
#46788=AXIS2_PLACEMENT_3D('',#71340,#53004,#53005);
#46789=AXIS2_PLACEMENT_3D('',#71355,#53006,#53007);
#46790=AXIS2_PLACEMENT_3D('',#71356,#53008,#53009);
#46791=AXIS2_PLACEMENT_3D('',#71360,#53011,#53012);
#46792=AXIS2_PLACEMENT_3D('',#71362,#53013,#53014);
#46793=AXIS2_PLACEMENT_3D('',#71396,#53017,#53018);
#46794=AXIS2_PLACEMENT_3D('',#71398,#53020,#53021);
#46795=AXIS2_PLACEMENT_3D('',#71399,#53022,#53023);
#46796=AXIS2_PLACEMENT_3D('',#71402,#53025,#53026);
#46797=AXIS2_PLACEMENT_3D('',#71403,#53027,#53028);
#46798=AXIS2_PLACEMENT_3D('',#71404,#53029,#53030);
#46799=AXIS2_PLACEMENT_3D('',#71423,#53031,#53032);
#46800=AXIS2_PLACEMENT_3D('',#71424,#53033,#53034);
#46801=AXIS2_PLACEMENT_3D('',#71434,#53035,#53036);
#46802=AXIS2_PLACEMENT_3D('',#71454,#53038,#53039);
#46803=AXIS2_PLACEMENT_3D('',#71462,#53041,#53042);
#46804=AXIS2_PLACEMENT_3D('',#71465,#53043,#53044);
#46805=AXIS2_PLACEMENT_3D('',#71466,#53045,#53046);
#46806=AXIS2_PLACEMENT_3D('',#71467,#53047,#53048);
#46807=AXIS2_PLACEMENT_3D('',#71476,#53049,#53050);
#46808=AXIS2_PLACEMENT_3D('',#71477,#53051,#53052);
#46809=AXIS2_PLACEMENT_3D('',#71481,#53054,#53055);
#46810=AXIS2_PLACEMENT_3D('',#71483,#53056,#53057);
#46811=AXIS2_PLACEMENT_3D('',#71508,#53060,#53061);
#46812=AXIS2_PLACEMENT_3D('',#71509,#53062,#53063);
#46813=AXIS2_PLACEMENT_3D('',#71528,#53064,#53065);
#46814=AXIS2_PLACEMENT_3D('',#71536,#53067,#53068);
#46815=AXIS2_PLACEMENT_3D('',#71539,#53069,#53070);
#46816=AXIS2_PLACEMENT_3D('',#71540,#53071,#53072);
#46817=AXIS2_PLACEMENT_3D('',#71541,#53073,#53074);
#46818=AXIS2_PLACEMENT_3D('',#71553,#53075,#53076);
#46819=AXIS2_PLACEMENT_3D('',#71554,#53077,#53078);
#46820=AXIS2_PLACEMENT_3D('',#71558,#53080,#53081);
#46821=AXIS2_PLACEMENT_3D('',#71560,#53082,#53083);
#46822=AXIS2_PLACEMENT_3D('',#71596,#53086,#53087);
#46823=AXIS2_PLACEMENT_3D('',#71604,#53089,#53090);
#46824=AXIS2_PLACEMENT_3D('',#71607,#53091,#53092);
#46825=AXIS2_PLACEMENT_3D('',#71608,#53093,#53094);
#46826=AXIS2_PLACEMENT_3D('',#71609,#53095,#53096);
#46827=AXIS2_PLACEMENT_3D('',#71645,#53098,#53099);
#46828=AXIS2_PLACEMENT_3D('',#71647,#53100,#53101);
#46829=AXIS2_PLACEMENT_3D('',#71702,#53105,#53106);
#46830=AXIS2_PLACEMENT_3D('',#71705,#53107,#53108);
#46831=AXIS2_PLACEMENT_3D('',#71712,#53109,#53110);
#46832=AXIS2_PLACEMENT_3D('',#71724,#53111,#53112);
#46833=AXIS2_PLACEMENT_3D('',#71725,#53113,#53114);
#46834=AXIS2_PLACEMENT_3D('',#71729,#53116,#53117);
#46835=AXIS2_PLACEMENT_3D('',#71731,#53118,#53119);
#46836=AXIS2_PLACEMENT_3D('',#71767,#53122,#53123);
#46837=AXIS2_PLACEMENT_3D('',#71775,#53125,#53126);
#46838=AXIS2_PLACEMENT_3D('',#71778,#53127,#53128);
#46839=AXIS2_PLACEMENT_3D('',#71779,#53129,#53130);
#46840=AXIS2_PLACEMENT_3D('',#71780,#53131,#53132);
#46841=AXIS2_PLACEMENT_3D('',#71799,#53133,#53134);
#46842=AXIS2_PLACEMENT_3D('',#71800,#53135,#53136);
#46843=AXIS2_PLACEMENT_3D('',#71804,#53138,#53139);
#46844=AXIS2_PLACEMENT_3D('',#71806,#53140,#53141);
#46845=AXIS2_PLACEMENT_3D('',#71842,#53144,#53145);
#46846=AXIS2_PLACEMENT_3D('',#71850,#53147,#53148);
#46847=AXIS2_PLACEMENT_3D('',#71853,#53149,#53150);
#46848=AXIS2_PLACEMENT_3D('',#71854,#53151,#53152);
#46849=AXIS2_PLACEMENT_3D('',#71855,#53153,#53154);
#46850=AXIS2_PLACEMENT_3D('',#71870,#53155,#53156);
#46851=AXIS2_PLACEMENT_3D('',#71871,#53157,#53158);
#46852=AXIS2_PLACEMENT_3D('',#71875,#53160,#53161);
#46853=AXIS2_PLACEMENT_3D('',#71877,#53162,#53163);
#46854=AXIS2_PLACEMENT_3D('',#71911,#53166,#53167);
#46855=AXIS2_PLACEMENT_3D('',#71913,#53169,#53170);
#46856=AXIS2_PLACEMENT_3D('',#71914,#53171,#53172);
#46857=AXIS2_PLACEMENT_3D('',#71917,#53174,#53175);
#46858=AXIS2_PLACEMENT_3D('',#71918,#53176,#53177);
#46859=AXIS2_PLACEMENT_3D('',#71919,#53178,#53179);
#46860=AXIS2_PLACEMENT_3D('',#71938,#53180,#53181);
#46861=AXIS2_PLACEMENT_3D('',#71939,#53182,#53183);
#46862=AXIS2_PLACEMENT_3D('',#71949,#53184,#53185);
#46863=AXIS2_PLACEMENT_3D('',#71969,#53187,#53188);
#46864=AXIS2_PLACEMENT_3D('',#71977,#53190,#53191);
#46865=AXIS2_PLACEMENT_3D('',#71980,#53192,#53193);
#46866=AXIS2_PLACEMENT_3D('',#71981,#53194,#53195);
#46867=AXIS2_PLACEMENT_3D('',#71982,#53196,#53197);
#46868=AXIS2_PLACEMENT_3D('',#71991,#53198,#53199);
#46869=AXIS2_PLACEMENT_3D('',#71992,#53200,#53201);
#46870=AXIS2_PLACEMENT_3D('',#71996,#53203,#53204);
#46871=AXIS2_PLACEMENT_3D('',#71998,#53205,#53206);
#46872=AXIS2_PLACEMENT_3D('',#72023,#53209,#53210);
#46873=AXIS2_PLACEMENT_3D('',#72024,#53211,#53212);
#46874=AXIS2_PLACEMENT_3D('',#72043,#53213,#53214);
#46875=AXIS2_PLACEMENT_3D('',#72051,#53216,#53217);
#46876=AXIS2_PLACEMENT_3D('',#72054,#53218,#53219);
#46877=AXIS2_PLACEMENT_3D('',#72055,#53220,#53221);
#46878=AXIS2_PLACEMENT_3D('',#72056,#53222,#53223);
#46879=AXIS2_PLACEMENT_3D('',#72068,#53224,#53225);
#46880=AXIS2_PLACEMENT_3D('',#72069,#53226,#53227);
#46881=AXIS2_PLACEMENT_3D('',#72073,#53229,#53230);
#46882=AXIS2_PLACEMENT_3D('',#72075,#53231,#53232);
#46883=AXIS2_PLACEMENT_3D('',#72111,#53235,#53236);
#46884=AXIS2_PLACEMENT_3D('',#72119,#53238,#53239);
#46885=AXIS2_PLACEMENT_3D('',#72122,#53240,#53241);
#46886=AXIS2_PLACEMENT_3D('',#72123,#53242,#53243);
#46887=AXIS2_PLACEMENT_3D('',#72124,#53244,#53245);
#46888=AXIS2_PLACEMENT_3D('',#72160,#53247,#53248);
#46889=AXIS2_PLACEMENT_3D('',#72162,#53249,#53250);
#46890=AXIS2_PLACEMENT_3D('',#72217,#53254,#53255);
#46891=AXIS2_PLACEMENT_3D('',#72220,#53256,#53257);
#46892=AXIS2_PLACEMENT_3D('',#72227,#53258,#53259);
#46893=AXIS2_PLACEMENT_3D('',#72239,#53260,#53261);
#46894=AXIS2_PLACEMENT_3D('',#72240,#53262,#53263);
#46895=AXIS2_PLACEMENT_3D('',#72244,#53265,#53266);
#46896=AXIS2_PLACEMENT_3D('',#72246,#53267,#53268);
#46897=AXIS2_PLACEMENT_3D('',#72282,#53271,#53272);
#46898=AXIS2_PLACEMENT_3D('',#72290,#53274,#53275);
#46899=AXIS2_PLACEMENT_3D('',#72293,#53276,#53277);
#46900=AXIS2_PLACEMENT_3D('',#72294,#53278,#53279);
#46901=AXIS2_PLACEMENT_3D('',#72295,#53280,#53281);
#46902=AXIS2_PLACEMENT_3D('',#72314,#53282,#53283);
#46903=AXIS2_PLACEMENT_3D('',#72315,#53284,#53285);
#46904=AXIS2_PLACEMENT_3D('',#72319,#53287,#53288);
#46905=AXIS2_PLACEMENT_3D('',#72321,#53289,#53290);
#46906=AXIS2_PLACEMENT_3D('',#72357,#53293,#53294);
#46907=AXIS2_PLACEMENT_3D('',#72365,#53296,#53297);
#46908=AXIS2_PLACEMENT_3D('',#72368,#53298,#53299);
#46909=AXIS2_PLACEMENT_3D('',#72369,#53300,#53301);
#46910=AXIS2_PLACEMENT_3D('',#72370,#53302,#53303);
#46911=AXIS2_PLACEMENT_3D('',#72385,#53304,#53305);
#46912=AXIS2_PLACEMENT_3D('',#72386,#53306,#53307);
#46913=AXIS2_PLACEMENT_3D('',#72390,#53309,#53310);
#46914=AXIS2_PLACEMENT_3D('',#72392,#53311,#53312);
#46915=AXIS2_PLACEMENT_3D('',#72426,#53315,#53316);
#46916=AXIS2_PLACEMENT_3D('',#72428,#53318,#53319);
#46917=AXIS2_PLACEMENT_3D('',#72429,#53320,#53321);
#46918=AXIS2_PLACEMENT_3D('',#72432,#53323,#53324);
#46919=AXIS2_PLACEMENT_3D('',#72433,#53325,#53326);
#46920=AXIS2_PLACEMENT_3D('',#72434,#53327,#53328);
#46921=AXIS2_PLACEMENT_3D('',#72453,#53329,#53330);
#46922=AXIS2_PLACEMENT_3D('',#72454,#53331,#53332);
#46923=AXIS2_PLACEMENT_3D('',#72464,#53333,#53334);
#46924=AXIS2_PLACEMENT_3D('',#72484,#53336,#53337);
#46925=AXIS2_PLACEMENT_3D('',#72492,#53339,#53340);
#46926=AXIS2_PLACEMENT_3D('',#72495,#53341,#53342);
#46927=AXIS2_PLACEMENT_3D('',#72496,#53343,#53344);
#46928=AXIS2_PLACEMENT_3D('',#72497,#53345,#53346);
#46929=AXIS2_PLACEMENT_3D('',#72506,#53347,#53348);
#46930=AXIS2_PLACEMENT_3D('',#72507,#53349,#53350);
#46931=AXIS2_PLACEMENT_3D('',#72511,#53352,#53353);
#46932=AXIS2_PLACEMENT_3D('',#72513,#53354,#53355);
#46933=AXIS2_PLACEMENT_3D('',#72538,#53358,#53359);
#46934=AXIS2_PLACEMENT_3D('',#72539,#53360,#53361);
#46935=AXIS2_PLACEMENT_3D('',#72558,#53362,#53363);
#46936=AXIS2_PLACEMENT_3D('',#72566,#53365,#53366);
#46937=AXIS2_PLACEMENT_3D('',#72569,#53367,#53368);
#46938=AXIS2_PLACEMENT_3D('',#72570,#53369,#53370);
#46939=AXIS2_PLACEMENT_3D('',#72571,#53371,#53372);
#46940=AXIS2_PLACEMENT_3D('',#72583,#53373,#53374);
#46941=AXIS2_PLACEMENT_3D('',#72584,#53375,#53376);
#46942=AXIS2_PLACEMENT_3D('',#72588,#53378,#53379);
#46943=AXIS2_PLACEMENT_3D('',#72590,#53380,#53381);
#46944=AXIS2_PLACEMENT_3D('',#72626,#53384,#53385);
#46945=AXIS2_PLACEMENT_3D('',#72634,#53387,#53388);
#46946=AXIS2_PLACEMENT_3D('',#72637,#53389,#53390);
#46947=AXIS2_PLACEMENT_3D('',#72638,#53391,#53392);
#46948=AXIS2_PLACEMENT_3D('',#72639,#53393,#53394);
#46949=AXIS2_PLACEMENT_3D('',#72675,#53396,#53397);
#46950=AXIS2_PLACEMENT_3D('',#72677,#53398,#53399);
#46951=AXIS2_PLACEMENT_3D('',#72732,#53403,#53404);
#46952=AXIS2_PLACEMENT_3D('',#72735,#53405,#53406);
#46953=AXIS2_PLACEMENT_3D('',#72742,#53407,#53408);
#46954=AXIS2_PLACEMENT_3D('',#72754,#53409,#53410);
#46955=AXIS2_PLACEMENT_3D('',#72755,#53411,#53412);
#46956=AXIS2_PLACEMENT_3D('',#72759,#53414,#53415);
#46957=AXIS2_PLACEMENT_3D('',#72761,#53416,#53417);
#46958=AXIS2_PLACEMENT_3D('',#72797,#53420,#53421);
#46959=AXIS2_PLACEMENT_3D('',#72805,#53423,#53424);
#46960=AXIS2_PLACEMENT_3D('',#72808,#53425,#53426);
#46961=AXIS2_PLACEMENT_3D('',#72809,#53427,#53428);
#46962=AXIS2_PLACEMENT_3D('',#72810,#53429,#53430);
#46963=AXIS2_PLACEMENT_3D('',#72829,#53431,#53432);
#46964=AXIS2_PLACEMENT_3D('',#72830,#53433,#53434);
#46965=AXIS2_PLACEMENT_3D('',#72834,#53436,#53437);
#46966=AXIS2_PLACEMENT_3D('',#72836,#53438,#53439);
#46967=AXIS2_PLACEMENT_3D('',#72872,#53442,#53443);
#46968=AXIS2_PLACEMENT_3D('',#72880,#53445,#53446);
#46969=AXIS2_PLACEMENT_3D('',#72883,#53447,#53448);
#46970=AXIS2_PLACEMENT_3D('',#72884,#53449,#53450);
#46971=AXIS2_PLACEMENT_3D('',#72885,#53451,#53452);
#46972=AXIS2_PLACEMENT_3D('',#72900,#53453,#53454);
#46973=AXIS2_PLACEMENT_3D('',#72901,#53455,#53456);
#46974=AXIS2_PLACEMENT_3D('',#72905,#53458,#53459);
#46975=AXIS2_PLACEMENT_3D('',#72907,#53460,#53461);
#46976=AXIS2_PLACEMENT_3D('',#72941,#53464,#53465);
#46977=AXIS2_PLACEMENT_3D('',#72943,#53467,#53468);
#46978=AXIS2_PLACEMENT_3D('',#72944,#53469,#53470);
#46979=AXIS2_PLACEMENT_3D('',#72947,#53472,#53473);
#46980=AXIS2_PLACEMENT_3D('',#72948,#53474,#53475);
#46981=AXIS2_PLACEMENT_3D('',#72949,#53476,#53477);
#46982=AXIS2_PLACEMENT_3D('',#72968,#53478,#53479);
#46983=AXIS2_PLACEMENT_3D('',#72969,#53480,#53481);
#46984=AXIS2_PLACEMENT_3D('',#72979,#53482,#53483);
#46985=AXIS2_PLACEMENT_3D('',#72999,#53485,#53486);
#46986=AXIS2_PLACEMENT_3D('',#73007,#53488,#53489);
#46987=AXIS2_PLACEMENT_3D('',#73010,#53490,#53491);
#46988=AXIS2_PLACEMENT_3D('',#73011,#53492,#53493);
#46989=AXIS2_PLACEMENT_3D('',#73012,#53494,#53495);
#46990=AXIS2_PLACEMENT_3D('',#73021,#53496,#53497);
#46991=AXIS2_PLACEMENT_3D('',#73022,#53498,#53499);
#46992=AXIS2_PLACEMENT_3D('',#73026,#53501,#53502);
#46993=AXIS2_PLACEMENT_3D('',#73028,#53503,#53504);
#46994=AXIS2_PLACEMENT_3D('',#73053,#53507,#53508);
#46995=AXIS2_PLACEMENT_3D('',#73054,#53509,#53510);
#46996=AXIS2_PLACEMENT_3D('',#73073,#53511,#53512);
#46997=AXIS2_PLACEMENT_3D('',#73081,#53514,#53515);
#46998=AXIS2_PLACEMENT_3D('',#73084,#53516,#53517);
#46999=AXIS2_PLACEMENT_3D('',#73085,#53518,#53519);
#47000=AXIS2_PLACEMENT_3D('',#73086,#53520,#53521);
#47001=AXIS2_PLACEMENT_3D('',#73095,#53522,#53523);
#47002=AXIS2_PLACEMENT_3D('',#73096,#53524,#53525);
#47003=AXIS2_PLACEMENT_3D('',#73100,#53527,#53528);
#47004=AXIS2_PLACEMENT_3D('',#73102,#53529,#53530);
#47005=AXIS2_PLACEMENT_3D('',#73145,#53533,#53534);
#47006=AXIS2_PLACEMENT_3D('',#73153,#53536,#53537);
#47007=AXIS2_PLACEMENT_3D('',#73156,#53538,#53539);
#47008=AXIS2_PLACEMENT_3D('',#73157,#53540,#53541);
#47009=AXIS2_PLACEMENT_3D('',#73158,#53542,#53543);
#47010=AXIS2_PLACEMENT_3D('',#73194,#53545,#53546);
#47011=AXIS2_PLACEMENT_3D('',#73196,#53547,#53548);
#47012=AXIS2_PLACEMENT_3D('',#73251,#53552,#53553);
#47013=AXIS2_PLACEMENT_3D('',#73254,#53554,#53555);
#47014=AXIS2_PLACEMENT_3D('',#73261,#53556,#53557);
#47015=AXIS2_PLACEMENT_3D('',#73273,#53558,#53559);
#47016=AXIS2_PLACEMENT_3D('',#73274,#53560,#53561);
#47017=AXIS2_PLACEMENT_3D('',#73278,#53563,#53564);
#47018=AXIS2_PLACEMENT_3D('',#73280,#53565,#53566);
#47019=AXIS2_PLACEMENT_3D('',#73316,#53569,#53570);
#47020=AXIS2_PLACEMENT_3D('',#73324,#53572,#53573);
#47021=AXIS2_PLACEMENT_3D('',#73327,#53574,#53575);
#47022=AXIS2_PLACEMENT_3D('',#73328,#53576,#53577);
#47023=AXIS2_PLACEMENT_3D('',#73329,#53578,#53579);
#47024=AXIS2_PLACEMENT_3D('',#73348,#53580,#53581);
#47025=AXIS2_PLACEMENT_3D('',#73349,#53582,#53583);
#47026=AXIS2_PLACEMENT_3D('',#73353,#53585,#53586);
#47027=AXIS2_PLACEMENT_3D('',#73355,#53587,#53588);
#47028=AXIS2_PLACEMENT_3D('',#73391,#53591,#53592);
#47029=AXIS2_PLACEMENT_3D('',#73399,#53594,#53595);
#47030=AXIS2_PLACEMENT_3D('',#73402,#53596,#53597);
#47031=AXIS2_PLACEMENT_3D('',#73403,#53598,#53599);
#47032=AXIS2_PLACEMENT_3D('',#73404,#53600,#53601);
#47033=AXIS2_PLACEMENT_3D('',#73419,#53602,#53603);
#47034=AXIS2_PLACEMENT_3D('',#73420,#53604,#53605);
#47035=AXIS2_PLACEMENT_3D('',#73424,#53607,#53608);
#47036=AXIS2_PLACEMENT_3D('',#73426,#53609,#53610);
#47037=AXIS2_PLACEMENT_3D('',#73460,#53613,#53614);
#47038=AXIS2_PLACEMENT_3D('',#73462,#53616,#53617);
#47039=AXIS2_PLACEMENT_3D('',#73463,#53618,#53619);
#47040=AXIS2_PLACEMENT_3D('',#73466,#53621,#53622);
#47041=AXIS2_PLACEMENT_3D('',#73467,#53623,#53624);
#47042=AXIS2_PLACEMENT_3D('',#73468,#53625,#53626);
#47043=AXIS2_PLACEMENT_3D('',#73487,#53627,#53628);
#47044=AXIS2_PLACEMENT_3D('',#73488,#53629,#53630);
#47045=AXIS2_PLACEMENT_3D('',#73498,#53631,#53632);
#47046=AXIS2_PLACEMENT_3D('',#73518,#53634,#53635);
#47047=AXIS2_PLACEMENT_3D('',#73526,#53637,#53638);
#47048=AXIS2_PLACEMENT_3D('',#73529,#53639,#53640);
#47049=AXIS2_PLACEMENT_3D('',#73530,#53641,#53642);
#47050=AXIS2_PLACEMENT_3D('',#73531,#53643,#53644);
#47051=AXIS2_PLACEMENT_3D('',#73540,#53645,#53646);
#47052=AXIS2_PLACEMENT_3D('',#73541,#53647,#53648);
#47053=AXIS2_PLACEMENT_3D('',#73545,#53650,#53651);
#47054=AXIS2_PLACEMENT_3D('',#73547,#53652,#53653);
#47055=AXIS2_PLACEMENT_3D('',#73572,#53656,#53657);
#47056=AXIS2_PLACEMENT_3D('',#73573,#53658,#53659);
#47057=AXIS2_PLACEMENT_3D('',#73592,#53660,#53661);
#47058=AXIS2_PLACEMENT_3D('',#73600,#53663,#53664);
#47059=AXIS2_PLACEMENT_3D('',#73603,#53665,#53666);
#47060=AXIS2_PLACEMENT_3D('',#73604,#53667,#53668);
#47061=AXIS2_PLACEMENT_3D('',#73605,#53669,#53670);
#47062=AXIS2_PLACEMENT_3D('',#73617,#53671,#53672);
#47063=AXIS2_PLACEMENT_3D('',#73618,#53673,#53674);
#47064=AXIS2_PLACEMENT_3D('',#73622,#53676,#53677);
#47065=AXIS2_PLACEMENT_3D('',#73624,#53678,#53679);
#47066=AXIS2_PLACEMENT_3D('',#73660,#53682,#53683);
#47067=AXIS2_PLACEMENT_3D('',#73668,#53685,#53686);
#47068=AXIS2_PLACEMENT_3D('',#73671,#53687,#53688);
#47069=AXIS2_PLACEMENT_3D('',#73672,#53689,#53690);
#47070=AXIS2_PLACEMENT_3D('',#73673,#53691,#53692);
#47071=AXIS2_PLACEMENT_3D('',#73709,#53694,#53695);
#47072=AXIS2_PLACEMENT_3D('',#73711,#53696,#53697);
#47073=AXIS2_PLACEMENT_3D('',#73766,#53701,#53702);
#47074=AXIS2_PLACEMENT_3D('',#73769,#53703,#53704);
#47075=AXIS2_PLACEMENT_3D('',#73776,#53705,#53706);
#47076=AXIS2_PLACEMENT_3D('',#73788,#53707,#53708);
#47077=AXIS2_PLACEMENT_3D('',#73789,#53709,#53710);
#47078=AXIS2_PLACEMENT_3D('',#73793,#53712,#53713);
#47079=AXIS2_PLACEMENT_3D('',#73795,#53714,#53715);
#47080=AXIS2_PLACEMENT_3D('',#73831,#53718,#53719);
#47081=AXIS2_PLACEMENT_3D('',#73839,#53721,#53722);
#47082=AXIS2_PLACEMENT_3D('',#73842,#53723,#53724);
#47083=AXIS2_PLACEMENT_3D('',#73843,#53725,#53726);
#47084=AXIS2_PLACEMENT_3D('',#73844,#53727,#53728);
#47085=AXIS2_PLACEMENT_3D('',#73863,#53729,#53730);
#47086=AXIS2_PLACEMENT_3D('',#73864,#53731,#53732);
#47087=AXIS2_PLACEMENT_3D('',#73868,#53734,#53735);
#47088=AXIS2_PLACEMENT_3D('',#73870,#53736,#53737);
#47089=AXIS2_PLACEMENT_3D('',#73906,#53740,#53741);
#47090=AXIS2_PLACEMENT_3D('',#73914,#53743,#53744);
#47091=AXIS2_PLACEMENT_3D('',#73917,#53745,#53746);
#47092=AXIS2_PLACEMENT_3D('',#73918,#53747,#53748);
#47093=AXIS2_PLACEMENT_3D('',#73919,#53749,#53750);
#47094=AXIS2_PLACEMENT_3D('',#73934,#53751,#53752);
#47095=AXIS2_PLACEMENT_3D('',#73935,#53753,#53754);
#47096=AXIS2_PLACEMENT_3D('',#73939,#53756,#53757);
#47097=AXIS2_PLACEMENT_3D('',#73941,#53758,#53759);
#47098=AXIS2_PLACEMENT_3D('',#73975,#53762,#53763);
#47099=AXIS2_PLACEMENT_3D('',#73977,#53765,#53766);
#47100=AXIS2_PLACEMENT_3D('',#73978,#53767,#53768);
#47101=AXIS2_PLACEMENT_3D('',#73981,#53770,#53771);
#47102=AXIS2_PLACEMENT_3D('',#73982,#53772,#53773);
#47103=AXIS2_PLACEMENT_3D('',#73983,#53774,#53775);
#47104=AXIS2_PLACEMENT_3D('',#74002,#53776,#53777);
#47105=AXIS2_PLACEMENT_3D('',#74003,#53778,#53779);
#47106=AXIS2_PLACEMENT_3D('',#74013,#53780,#53781);
#47107=AXIS2_PLACEMENT_3D('',#74033,#53783,#53784);
#47108=AXIS2_PLACEMENT_3D('',#74041,#53786,#53787);
#47109=AXIS2_PLACEMENT_3D('',#74044,#53788,#53789);
#47110=AXIS2_PLACEMENT_3D('',#74045,#53790,#53791);
#47111=AXIS2_PLACEMENT_3D('',#74046,#53792,#53793);
#47112=AXIS2_PLACEMENT_3D('',#74055,#53794,#53795);
#47113=AXIS2_PLACEMENT_3D('',#74056,#53796,#53797);
#47114=AXIS2_PLACEMENT_3D('',#74060,#53799,#53800);
#47115=AXIS2_PLACEMENT_3D('',#74062,#53801,#53802);
#47116=AXIS2_PLACEMENT_3D('',#74087,#53805,#53806);
#47117=AXIS2_PLACEMENT_3D('',#74088,#53807,#53808);
#47118=AXIS2_PLACEMENT_3D('',#74107,#53809,#53810);
#47119=AXIS2_PLACEMENT_3D('',#74115,#53812,#53813);
#47120=AXIS2_PLACEMENT_3D('',#74118,#53814,#53815);
#47121=AXIS2_PLACEMENT_3D('',#74119,#53816,#53817);
#47122=AXIS2_PLACEMENT_3D('',#74120,#53818,#53819);
#47123=AXIS2_PLACEMENT_3D('',#74132,#53820,#53821);
#47124=AXIS2_PLACEMENT_3D('',#74133,#53822,#53823);
#47125=AXIS2_PLACEMENT_3D('',#74137,#53825,#53826);
#47126=AXIS2_PLACEMENT_3D('',#74139,#53827,#53828);
#47127=AXIS2_PLACEMENT_3D('',#74175,#53831,#53832);
#47128=AXIS2_PLACEMENT_3D('',#74183,#53834,#53835);
#47129=AXIS2_PLACEMENT_3D('',#74186,#53836,#53837);
#47130=AXIS2_PLACEMENT_3D('',#74187,#53838,#53839);
#47131=AXIS2_PLACEMENT_3D('',#74188,#53840,#53841);
#47132=AXIS2_PLACEMENT_3D('',#74224,#53843,#53844);
#47133=AXIS2_PLACEMENT_3D('',#74226,#53845,#53846);
#47134=AXIS2_PLACEMENT_3D('',#74281,#53850,#53851);
#47135=AXIS2_PLACEMENT_3D('',#74284,#53852,#53853);
#47136=AXIS2_PLACEMENT_3D('',#74291,#53854,#53855);
#47137=AXIS2_PLACEMENT_3D('',#74303,#53856,#53857);
#47138=AXIS2_PLACEMENT_3D('',#74304,#53858,#53859);
#47139=AXIS2_PLACEMENT_3D('',#74308,#53861,#53862);
#47140=AXIS2_PLACEMENT_3D('',#74310,#53863,#53864);
#47141=AXIS2_PLACEMENT_3D('',#74346,#53867,#53868);
#47142=AXIS2_PLACEMENT_3D('',#74354,#53870,#53871);
#47143=AXIS2_PLACEMENT_3D('',#74357,#53872,#53873);
#47144=AXIS2_PLACEMENT_3D('',#74358,#53874,#53875);
#47145=AXIS2_PLACEMENT_3D('',#74359,#53876,#53877);
#47146=AXIS2_PLACEMENT_3D('',#74378,#53878,#53879);
#47147=AXIS2_PLACEMENT_3D('',#74379,#53880,#53881);
#47148=AXIS2_PLACEMENT_3D('',#74383,#53883,#53884);
#47149=AXIS2_PLACEMENT_3D('',#74385,#53885,#53886);
#47150=AXIS2_PLACEMENT_3D('',#74421,#53889,#53890);
#47151=AXIS2_PLACEMENT_3D('',#74429,#53892,#53893);
#47152=AXIS2_PLACEMENT_3D('',#74432,#53894,#53895);
#47153=AXIS2_PLACEMENT_3D('',#74433,#53896,#53897);
#47154=AXIS2_PLACEMENT_3D('',#74434,#53898,#53899);
#47155=AXIS2_PLACEMENT_3D('',#74449,#53900,#53901);
#47156=AXIS2_PLACEMENT_3D('',#74450,#53902,#53903);
#47157=AXIS2_PLACEMENT_3D('',#74454,#53905,#53906);
#47158=AXIS2_PLACEMENT_3D('',#74456,#53907,#53908);
#47159=AXIS2_PLACEMENT_3D('',#74490,#53911,#53912);
#47160=AXIS2_PLACEMENT_3D('',#74492,#53914,#53915);
#47161=AXIS2_PLACEMENT_3D('',#74493,#53916,#53917);
#47162=AXIS2_PLACEMENT_3D('',#74496,#53919,#53920);
#47163=AXIS2_PLACEMENT_3D('',#74497,#53921,#53922);
#47164=AXIS2_PLACEMENT_3D('',#74498,#53923,#53924);
#47165=AXIS2_PLACEMENT_3D('',#74517,#53925,#53926);
#47166=AXIS2_PLACEMENT_3D('',#74518,#53927,#53928);
#47167=AXIS2_PLACEMENT_3D('',#74528,#53929,#53930);
#47168=AXIS2_PLACEMENT_3D('',#74548,#53932,#53933);
#47169=AXIS2_PLACEMENT_3D('',#74556,#53935,#53936);
#47170=AXIS2_PLACEMENT_3D('',#74559,#53937,#53938);
#47171=AXIS2_PLACEMENT_3D('',#74560,#53939,#53940);
#47172=AXIS2_PLACEMENT_3D('',#74561,#53941,#53942);
#47173=AXIS2_PLACEMENT_3D('',#74570,#53943,#53944);
#47174=AXIS2_PLACEMENT_3D('',#74571,#53945,#53946);
#47175=AXIS2_PLACEMENT_3D('',#74575,#53948,#53949);
#47176=AXIS2_PLACEMENT_3D('',#74577,#53950,#53951);
#47177=AXIS2_PLACEMENT_3D('',#74602,#53954,#53955);
#47178=AXIS2_PLACEMENT_3D('',#74603,#53956,#53957);
#47179=AXIS2_PLACEMENT_3D('',#74622,#53958,#53959);
#47180=AXIS2_PLACEMENT_3D('',#74630,#53961,#53962);
#47181=AXIS2_PLACEMENT_3D('',#74633,#53963,#53964);
#47182=AXIS2_PLACEMENT_3D('',#74634,#53965,#53966);
#47183=AXIS2_PLACEMENT_3D('',#74635,#53967,#53968);
#47184=AXIS2_PLACEMENT_3D('',#74647,#53969,#53970);
#47185=AXIS2_PLACEMENT_3D('',#74648,#53971,#53972);
#47186=AXIS2_PLACEMENT_3D('',#74652,#53974,#53975);
#47187=AXIS2_PLACEMENT_3D('',#74654,#53976,#53977);
#47188=AXIS2_PLACEMENT_3D('',#74690,#53980,#53981);
#47189=AXIS2_PLACEMENT_3D('',#74698,#53983,#53984);
#47190=AXIS2_PLACEMENT_3D('',#74701,#53985,#53986);
#47191=AXIS2_PLACEMENT_3D('',#74702,#53987,#53988);
#47192=AXIS2_PLACEMENT_3D('',#74703,#53989,#53990);
#47193=AXIS2_PLACEMENT_3D('',#74739,#53992,#53993);
#47194=AXIS2_PLACEMENT_3D('',#74741,#53994,#53995);
#47195=AXIS2_PLACEMENT_3D('',#74796,#53999,#54000);
#47196=AXIS2_PLACEMENT_3D('',#74799,#54001,#54002);
#47197=AXIS2_PLACEMENT_3D('',#74806,#54003,#54004);
#47198=AXIS2_PLACEMENT_3D('',#74818,#54005,#54006);
#47199=AXIS2_PLACEMENT_3D('',#74819,#54007,#54008);
#47200=AXIS2_PLACEMENT_3D('',#74823,#54010,#54011);
#47201=AXIS2_PLACEMENT_3D('',#74825,#54012,#54013);
#47202=AXIS2_PLACEMENT_3D('',#74861,#54016,#54017);
#47203=AXIS2_PLACEMENT_3D('',#74869,#54019,#54020);
#47204=AXIS2_PLACEMENT_3D('',#74872,#54021,#54022);
#47205=AXIS2_PLACEMENT_3D('',#74873,#54023,#54024);
#47206=AXIS2_PLACEMENT_3D('',#74874,#54025,#54026);
#47207=AXIS2_PLACEMENT_3D('',#74893,#54027,#54028);
#47208=AXIS2_PLACEMENT_3D('',#74894,#54029,#54030);
#47209=AXIS2_PLACEMENT_3D('',#74898,#54032,#54033);
#47210=AXIS2_PLACEMENT_3D('',#74900,#54034,#54035);
#47211=AXIS2_PLACEMENT_3D('',#74936,#54038,#54039);
#47212=AXIS2_PLACEMENT_3D('',#74944,#54041,#54042);
#47213=AXIS2_PLACEMENT_3D('',#74947,#54043,#54044);
#47214=AXIS2_PLACEMENT_3D('',#74948,#54045,#54046);
#47215=AXIS2_PLACEMENT_3D('',#74949,#54047,#54048);
#47216=AXIS2_PLACEMENT_3D('',#74964,#54049,#54050);
#47217=AXIS2_PLACEMENT_3D('',#74965,#54051,#54052);
#47218=AXIS2_PLACEMENT_3D('',#74969,#54054,#54055);
#47219=AXIS2_PLACEMENT_3D('',#74971,#54056,#54057);
#47220=AXIS2_PLACEMENT_3D('',#75005,#54060,#54061);
#47221=AXIS2_PLACEMENT_3D('',#75007,#54063,#54064);
#47222=AXIS2_PLACEMENT_3D('',#75008,#54065,#54066);
#47223=AXIS2_PLACEMENT_3D('',#75011,#54068,#54069);
#47224=AXIS2_PLACEMENT_3D('',#75012,#54070,#54071);
#47225=AXIS2_PLACEMENT_3D('',#75013,#54072,#54073);
#47226=AXIS2_PLACEMENT_3D('',#75032,#54074,#54075);
#47227=AXIS2_PLACEMENT_3D('',#75033,#54076,#54077);
#47228=AXIS2_PLACEMENT_3D('',#75043,#54078,#54079);
#47229=AXIS2_PLACEMENT_3D('',#75063,#54081,#54082);
#47230=AXIS2_PLACEMENT_3D('',#75071,#54084,#54085);
#47231=AXIS2_PLACEMENT_3D('',#75074,#54086,#54087);
#47232=AXIS2_PLACEMENT_3D('',#75075,#54088,#54089);
#47233=AXIS2_PLACEMENT_3D('',#75076,#54090,#54091);
#47234=AXIS2_PLACEMENT_3D('',#75085,#54092,#54093);
#47235=AXIS2_PLACEMENT_3D('',#75086,#54094,#54095);
#47236=AXIS2_PLACEMENT_3D('',#75090,#54097,#54098);
#47237=AXIS2_PLACEMENT_3D('',#75092,#54099,#54100);
#47238=AXIS2_PLACEMENT_3D('',#75117,#54103,#54104);
#47239=AXIS2_PLACEMENT_3D('',#75118,#54105,#54106);
#47240=AXIS2_PLACEMENT_3D('',#75137,#54107,#54108);
#47241=AXIS2_PLACEMENT_3D('',#75145,#54110,#54111);
#47242=AXIS2_PLACEMENT_3D('',#75148,#54112,#54113);
#47243=AXIS2_PLACEMENT_3D('',#75149,#54114,#54115);
#47244=AXIS2_PLACEMENT_3D('',#75150,#54116,#54117);
#47245=AXIS2_PLACEMENT_3D('',#75162,#54118,#54119);
#47246=AXIS2_PLACEMENT_3D('',#75163,#54120,#54121);
#47247=AXIS2_PLACEMENT_3D('',#75167,#54123,#54124);
#47248=AXIS2_PLACEMENT_3D('',#75169,#54125,#54126);
#47249=AXIS2_PLACEMENT_3D('',#75205,#54129,#54130);
#47250=AXIS2_PLACEMENT_3D('',#75213,#54132,#54133);
#47251=AXIS2_PLACEMENT_3D('',#75216,#54134,#54135);
#47252=AXIS2_PLACEMENT_3D('',#75217,#54136,#54137);
#47253=AXIS2_PLACEMENT_3D('',#75218,#54138,#54139);
#47254=AXIS2_PLACEMENT_3D('',#75254,#54141,#54142);
#47255=AXIS2_PLACEMENT_3D('',#75256,#54143,#54144);
#47256=AXIS2_PLACEMENT_3D('',#75311,#54148,#54149);
#47257=AXIS2_PLACEMENT_3D('',#75314,#54150,#54151);
#47258=AXIS2_PLACEMENT_3D('',#75321,#54152,#54153);
#47259=AXIS2_PLACEMENT_3D('',#75333,#54154,#54155);
#47260=AXIS2_PLACEMENT_3D('',#75334,#54156,#54157);
#47261=AXIS2_PLACEMENT_3D('',#75338,#54159,#54160);
#47262=AXIS2_PLACEMENT_3D('',#75340,#54161,#54162);
#47263=AXIS2_PLACEMENT_3D('',#75376,#54165,#54166);
#47264=AXIS2_PLACEMENT_3D('',#75384,#54168,#54169);
#47265=AXIS2_PLACEMENT_3D('',#75387,#54170,#54171);
#47266=AXIS2_PLACEMENT_3D('',#75388,#54172,#54173);
#47267=AXIS2_PLACEMENT_3D('',#75389,#54174,#54175);
#47268=AXIS2_PLACEMENT_3D('',#75408,#54176,#54177);
#47269=AXIS2_PLACEMENT_3D('',#75409,#54178,#54179);
#47270=AXIS2_PLACEMENT_3D('',#75413,#54181,#54182);
#47271=AXIS2_PLACEMENT_3D('',#75415,#54183,#54184);
#47272=AXIS2_PLACEMENT_3D('',#75451,#54187,#54188);
#47273=AXIS2_PLACEMENT_3D('',#75459,#54190,#54191);
#47274=AXIS2_PLACEMENT_3D('',#75462,#54192,#54193);
#47275=AXIS2_PLACEMENT_3D('',#75463,#54194,#54195);
#47276=AXIS2_PLACEMENT_3D('',#75464,#54196,#54197);
#47277=AXIS2_PLACEMENT_3D('',#75479,#54198,#54199);
#47278=AXIS2_PLACEMENT_3D('',#75480,#54200,#54201);
#47279=AXIS2_PLACEMENT_3D('',#75484,#54203,#54204);
#47280=AXIS2_PLACEMENT_3D('',#75486,#54205,#54206);
#47281=AXIS2_PLACEMENT_3D('',#75520,#54209,#54210);
#47282=AXIS2_PLACEMENT_3D('',#75522,#54212,#54213);
#47283=AXIS2_PLACEMENT_3D('',#75523,#54214,#54215);
#47284=AXIS2_PLACEMENT_3D('',#75526,#54217,#54218);
#47285=AXIS2_PLACEMENT_3D('',#75527,#54219,#54220);
#47286=AXIS2_PLACEMENT_3D('',#75528,#54221,#54222);
#47287=AXIS2_PLACEMENT_3D('',#75547,#54223,#54224);
#47288=AXIS2_PLACEMENT_3D('',#75548,#54225,#54226);
#47289=AXIS2_PLACEMENT_3D('',#75558,#54227,#54228);
#47290=AXIS2_PLACEMENT_3D('',#75578,#54230,#54231);
#47291=AXIS2_PLACEMENT_3D('',#75586,#54233,#54234);
#47292=AXIS2_PLACEMENT_3D('',#75589,#54235,#54236);
#47293=AXIS2_PLACEMENT_3D('',#75590,#54237,#54238);
#47294=AXIS2_PLACEMENT_3D('',#75591,#54239,#54240);
#47295=AXIS2_PLACEMENT_3D('',#75600,#54241,#54242);
#47296=AXIS2_PLACEMENT_3D('',#75601,#54243,#54244);
#47297=AXIS2_PLACEMENT_3D('',#75605,#54246,#54247);
#47298=AXIS2_PLACEMENT_3D('',#75607,#54248,#54249);
#47299=AXIS2_PLACEMENT_3D('',#75632,#54252,#54253);
#47300=AXIS2_PLACEMENT_3D('',#75633,#54254,#54255);
#47301=AXIS2_PLACEMENT_3D('',#75652,#54256,#54257);
#47302=AXIS2_PLACEMENT_3D('',#75660,#54259,#54260);
#47303=AXIS2_PLACEMENT_3D('',#75663,#54261,#54262);
#47304=AXIS2_PLACEMENT_3D('',#75664,#54263,#54264);
#47305=AXIS2_PLACEMENT_3D('',#75665,#54265,#54266);
#47306=AXIS2_PLACEMENT_3D('',#75674,#54267,#54268);
#47307=AXIS2_PLACEMENT_3D('',#75675,#54269,#54270);
#47308=AXIS2_PLACEMENT_3D('',#75679,#54272,#54273);
#47309=AXIS2_PLACEMENT_3D('',#75681,#54274,#54275);
#47310=AXIS2_PLACEMENT_3D('',#75724,#54278,#54279);
#47311=AXIS2_PLACEMENT_3D('',#75732,#54281,#54282);
#47312=AXIS2_PLACEMENT_3D('',#75735,#54283,#54284);
#47313=AXIS2_PLACEMENT_3D('',#75736,#54285,#54286);
#47314=AXIS2_PLACEMENT_3D('',#75737,#54287,#54288);
#47315=AXIS2_PLACEMENT_3D('',#75773,#54290,#54291);
#47316=AXIS2_PLACEMENT_3D('',#75775,#54292,#54293);
#47317=AXIS2_PLACEMENT_3D('',#75830,#54297,#54298);
#47318=AXIS2_PLACEMENT_3D('',#75833,#54299,#54300);
#47319=AXIS2_PLACEMENT_3D('',#75840,#54301,#54302);
#47320=AXIS2_PLACEMENT_3D('',#75852,#54303,#54304);
#47321=AXIS2_PLACEMENT_3D('',#75853,#54305,#54306);
#47322=AXIS2_PLACEMENT_3D('',#75857,#54308,#54309);
#47323=AXIS2_PLACEMENT_3D('',#75859,#54310,#54311);
#47324=AXIS2_PLACEMENT_3D('',#75895,#54314,#54315);
#47325=AXIS2_PLACEMENT_3D('',#75903,#54317,#54318);
#47326=AXIS2_PLACEMENT_3D('',#75906,#54319,#54320);
#47327=AXIS2_PLACEMENT_3D('',#75907,#54321,#54322);
#47328=AXIS2_PLACEMENT_3D('',#75908,#54323,#54324);
#47329=AXIS2_PLACEMENT_3D('',#75927,#54325,#54326);
#47330=AXIS2_PLACEMENT_3D('',#75928,#54327,#54328);
#47331=AXIS2_PLACEMENT_3D('',#75932,#54330,#54331);
#47332=AXIS2_PLACEMENT_3D('',#75934,#54332,#54333);
#47333=AXIS2_PLACEMENT_3D('',#75970,#54336,#54337);
#47334=AXIS2_PLACEMENT_3D('',#75978,#54339,#54340);
#47335=AXIS2_PLACEMENT_3D('',#75981,#54341,#54342);
#47336=AXIS2_PLACEMENT_3D('',#75982,#54343,#54344);
#47337=AXIS2_PLACEMENT_3D('',#75983,#54345,#54346);
#47338=AXIS2_PLACEMENT_3D('',#75998,#54347,#54348);
#47339=AXIS2_PLACEMENT_3D('',#75999,#54349,#54350);
#47340=AXIS2_PLACEMENT_3D('',#76003,#54352,#54353);
#47341=AXIS2_PLACEMENT_3D('',#76005,#54354,#54355);
#47342=AXIS2_PLACEMENT_3D('',#76039,#54358,#54359);
#47343=AXIS2_PLACEMENT_3D('',#76041,#54361,#54362);
#47344=AXIS2_PLACEMENT_3D('',#76042,#54363,#54364);
#47345=AXIS2_PLACEMENT_3D('',#76045,#54366,#54367);
#47346=AXIS2_PLACEMENT_3D('',#76046,#54368,#54369);
#47347=AXIS2_PLACEMENT_3D('',#76047,#54370,#54371);
#47348=AXIS2_PLACEMENT_3D('',#76066,#54372,#54373);
#47349=AXIS2_PLACEMENT_3D('',#76067,#54374,#54375);
#47350=AXIS2_PLACEMENT_3D('',#76077,#54376,#54377);
#47351=AXIS2_PLACEMENT_3D('',#76097,#54379,#54380);
#47352=AXIS2_PLACEMENT_3D('',#76105,#54382,#54383);
#47353=AXIS2_PLACEMENT_3D('',#76108,#54384,#54385);
#47354=AXIS2_PLACEMENT_3D('',#76109,#54386,#54387);
#47355=AXIS2_PLACEMENT_3D('',#76110,#54388,#54389);
#47356=AXIS2_PLACEMENT_3D('',#76119,#54390,#54391);
#47357=AXIS2_PLACEMENT_3D('',#76120,#54392,#54393);
#47358=AXIS2_PLACEMENT_3D('',#76124,#54395,#54396);
#47359=AXIS2_PLACEMENT_3D('',#76126,#54397,#54398);
#47360=AXIS2_PLACEMENT_3D('',#76151,#54401,#54402);
#47361=AXIS2_PLACEMENT_3D('',#76152,#54403,#54404);
#47362=AXIS2_PLACEMENT_3D('',#76171,#54405,#54406);
#47363=AXIS2_PLACEMENT_3D('',#76179,#54408,#54409);
#47364=AXIS2_PLACEMENT_3D('',#76182,#54410,#54411);
#47365=AXIS2_PLACEMENT_3D('',#76183,#54412,#54413);
#47366=AXIS2_PLACEMENT_3D('',#76184,#54414,#54415);
#47367=AXIS2_PLACEMENT_3D('',#76196,#54416,#54417);
#47368=AXIS2_PLACEMENT_3D('',#76197,#54418,#54419);
#47369=AXIS2_PLACEMENT_3D('',#76201,#54421,#54422);
#47370=AXIS2_PLACEMENT_3D('',#76203,#54423,#54424);
#47371=AXIS2_PLACEMENT_3D('',#76239,#54427,#54428);
#47372=AXIS2_PLACEMENT_3D('',#76247,#54430,#54431);
#47373=AXIS2_PLACEMENT_3D('',#76250,#54432,#54433);
#47374=AXIS2_PLACEMENT_3D('',#76251,#54434,#54435);
#47375=AXIS2_PLACEMENT_3D('',#76252,#54436,#54437);
#47376=AXIS2_PLACEMENT_3D('',#76287,#54439,#54440);
#47377=AXIS2_PLACEMENT_3D('',#76289,#54441,#54442);
#47378=AXIS2_PLACEMENT_3D('',#76339,#54446,#54447);
#47379=AXIS2_PLACEMENT_3D('',#76342,#54448,#54449);
#47380=AXIS2_PLACEMENT_3D('',#76349,#54450,#54451);
#47381=AXIS2_PLACEMENT_3D('',#76361,#54452,#54453);
#47382=AXIS2_PLACEMENT_3D('',#76362,#54454,#54455);
#47383=AXIS2_PLACEMENT_3D('',#76366,#54457,#54458);
#47384=AXIS2_PLACEMENT_3D('',#76368,#54459,#54460);
#47385=AXIS2_PLACEMENT_3D('',#76404,#54463,#54464);
#47386=AXIS2_PLACEMENT_3D('',#76412,#54466,#54467);
#47387=AXIS2_PLACEMENT_3D('',#76415,#54468,#54469);
#47388=AXIS2_PLACEMENT_3D('',#76416,#54470,#54471);
#47389=AXIS2_PLACEMENT_3D('',#76417,#54472,#54473);
#47390=AXIS2_PLACEMENT_3D('',#76436,#54474,#54475);
#47391=AXIS2_PLACEMENT_3D('',#76437,#54476,#54477);
#47392=AXIS2_PLACEMENT_3D('',#76441,#54479,#54480);
#47393=AXIS2_PLACEMENT_3D('',#76443,#54481,#54482);
#47394=AXIS2_PLACEMENT_3D('',#76479,#54485,#54486);
#47395=AXIS2_PLACEMENT_3D('',#76487,#54488,#54489);
#47396=AXIS2_PLACEMENT_3D('',#76490,#54490,#54491);
#47397=AXIS2_PLACEMENT_3D('',#76491,#54492,#54493);
#47398=AXIS2_PLACEMENT_3D('',#76492,#54494,#54495);
#47399=AXIS2_PLACEMENT_3D('',#76507,#54496,#54497);
#47400=AXIS2_PLACEMENT_3D('',#76508,#54498,#54499);
#47401=AXIS2_PLACEMENT_3D('',#76512,#54501,#54502);
#47402=AXIS2_PLACEMENT_3D('',#76514,#54503,#54504);
#47403=AXIS2_PLACEMENT_3D('',#76548,#54507,#54508);
#47404=AXIS2_PLACEMENT_3D('',#76550,#54510,#54511);
#47405=AXIS2_PLACEMENT_3D('',#76551,#54512,#54513);
#47406=AXIS2_PLACEMENT_3D('',#76554,#54515,#54516);
#47407=AXIS2_PLACEMENT_3D('',#76555,#54517,#54518);
#47408=AXIS2_PLACEMENT_3D('',#76556,#54519,#54520);
#47409=AXIS2_PLACEMENT_3D('',#76575,#54521,#54522);
#47410=AXIS2_PLACEMENT_3D('',#76576,#54523,#54524);
#47411=AXIS2_PLACEMENT_3D('',#76586,#54525,#54526);
#47412=AXIS2_PLACEMENT_3D('',#76606,#54528,#54529);
#47413=AXIS2_PLACEMENT_3D('',#76614,#54531,#54532);
#47414=AXIS2_PLACEMENT_3D('',#76617,#54533,#54534);
#47415=AXIS2_PLACEMENT_3D('',#76618,#54535,#54536);
#47416=AXIS2_PLACEMENT_3D('',#76619,#54537,#54538);
#47417=AXIS2_PLACEMENT_3D('',#76628,#54539,#54540);
#47418=AXIS2_PLACEMENT_3D('',#76629,#54541,#54542);
#47419=AXIS2_PLACEMENT_3D('',#76633,#54544,#54545);
#47420=AXIS2_PLACEMENT_3D('',#76635,#54546,#54547);
#47421=AXIS2_PLACEMENT_3D('',#76660,#54550,#54551);
#47422=AXIS2_PLACEMENT_3D('',#76661,#54552,#54553);
#47423=AXIS2_PLACEMENT_3D('',#76680,#54554,#54555);
#47424=AXIS2_PLACEMENT_3D('',#76688,#54557,#54558);
#47425=AXIS2_PLACEMENT_3D('',#76691,#54559,#54560);
#47426=AXIS2_PLACEMENT_3D('',#76692,#54561,#54562);
#47427=AXIS2_PLACEMENT_3D('',#76693,#54563,#54564);
#47428=AXIS2_PLACEMENT_3D('',#76702,#54565,#54566);
#47429=AXIS2_PLACEMENT_3D('',#76703,#54567,#54568);
#47430=AXIS2_PLACEMENT_3D('',#76707,#54570,#54571);
#47431=AXIS2_PLACEMENT_3D('',#76709,#54572,#54573);
#47432=AXIS2_PLACEMENT_3D('',#76752,#54576,#54577);
#47433=AXIS2_PLACEMENT_3D('',#76760,#54579,#54580);
#47434=AXIS2_PLACEMENT_3D('',#76763,#54581,#54582);
#47435=AXIS2_PLACEMENT_3D('',#76764,#54583,#54584);
#47436=AXIS2_PLACEMENT_3D('',#76765,#54585,#54586);
#47437=AXIS2_PLACEMENT_3D('',#76801,#54588,#54589);
#47438=AXIS2_PLACEMENT_3D('',#76803,#54590,#54591);
#47439=AXIS2_PLACEMENT_3D('',#76858,#54595,#54596);
#47440=AXIS2_PLACEMENT_3D('',#76861,#54597,#54598);
#47441=AXIS2_PLACEMENT_3D('',#76868,#54599,#54600);
#47442=AXIS2_PLACEMENT_3D('',#76877,#54601,#54602);
#47443=AXIS2_PLACEMENT_3D('',#76878,#54603,#54604);
#47444=AXIS2_PLACEMENT_3D('',#76882,#54606,#54607);
#47445=AXIS2_PLACEMENT_3D('',#76884,#54608,#54609);
#47446=AXIS2_PLACEMENT_3D('',#76927,#54612,#54613);
#47447=AXIS2_PLACEMENT_3D('',#76935,#54615,#54616);
#47448=AXIS2_PLACEMENT_3D('',#76938,#54617,#54618);
#47449=AXIS2_PLACEMENT_3D('',#76939,#54619,#54620);
#47450=AXIS2_PLACEMENT_3D('',#76940,#54621,#54622);
#47451=AXIS2_PLACEMENT_3D('',#76959,#54623,#54624);
#47452=AXIS2_PLACEMENT_3D('',#76960,#54625,#54626);
#47453=AXIS2_PLACEMENT_3D('',#76964,#54628,#54629);
#47454=AXIS2_PLACEMENT_3D('',#76966,#54630,#54631);
#47455=AXIS2_PLACEMENT_3D('',#77002,#54634,#54635);
#47456=AXIS2_PLACEMENT_3D('',#77010,#54637,#54638);
#47457=AXIS2_PLACEMENT_3D('',#77013,#54639,#54640);
#47458=AXIS2_PLACEMENT_3D('',#77014,#54641,#54642);
#47459=AXIS2_PLACEMENT_3D('',#77015,#54643,#54644);
#47460=AXIS2_PLACEMENT_3D('',#77030,#54645,#54646);
#47461=AXIS2_PLACEMENT_3D('',#77031,#54647,#54648);
#47462=AXIS2_PLACEMENT_3D('',#77035,#54650,#54651);
#47463=AXIS2_PLACEMENT_3D('',#77037,#54652,#54653);
#47464=AXIS2_PLACEMENT_3D('',#77071,#54656,#54657);
#47465=AXIS2_PLACEMENT_3D('',#77073,#54659,#54660);
#47466=AXIS2_PLACEMENT_3D('',#77074,#54661,#54662);
#47467=AXIS2_PLACEMENT_3D('',#77077,#54664,#54665);
#47468=AXIS2_PLACEMENT_3D('',#77078,#54666,#54667);
#47469=AXIS2_PLACEMENT_3D('',#77079,#54668,#54669);
#47470=AXIS2_PLACEMENT_3D('',#77098,#54670,#54671);
#47471=AXIS2_PLACEMENT_3D('',#77099,#54672,#54673);
#47472=AXIS2_PLACEMENT_3D('',#77109,#54674,#54675);
#47473=AXIS2_PLACEMENT_3D('',#77129,#54677,#54678);
#47474=AXIS2_PLACEMENT_3D('',#77137,#54680,#54681);
#47475=AXIS2_PLACEMENT_3D('',#77140,#54682,#54683);
#47476=AXIS2_PLACEMENT_3D('',#77141,#54684,#54685);
#47477=AXIS2_PLACEMENT_3D('',#77142,#54686,#54687);
#47478=AXIS2_PLACEMENT_3D('',#77151,#54688,#54689);
#47479=AXIS2_PLACEMENT_3D('',#77152,#54690,#54691);
#47480=AXIS2_PLACEMENT_3D('',#77156,#54693,#54694);
#47481=AXIS2_PLACEMENT_3D('',#77158,#54695,#54696);
#47482=AXIS2_PLACEMENT_3D('',#77183,#54699,#54700);
#47483=AXIS2_PLACEMENT_3D('',#77184,#54701,#54702);
#47484=AXIS2_PLACEMENT_3D('',#77203,#54703,#54704);
#47485=AXIS2_PLACEMENT_3D('',#77211,#54706,#54707);
#47486=AXIS2_PLACEMENT_3D('',#77214,#54708,#54709);
#47487=AXIS2_PLACEMENT_3D('',#77215,#54710,#54711);
#47488=AXIS2_PLACEMENT_3D('',#77216,#54712,#54713);
#47489=AXIS2_PLACEMENT_3D('',#77228,#54714,#54715);
#47490=AXIS2_PLACEMENT_3D('',#77229,#54716,#54717);
#47491=AXIS2_PLACEMENT_3D('',#77233,#54719,#54720);
#47492=AXIS2_PLACEMENT_3D('',#77235,#54721,#54722);
#47493=AXIS2_PLACEMENT_3D('',#77271,#54725,#54726);
#47494=AXIS2_PLACEMENT_3D('',#77279,#54728,#54729);
#47495=AXIS2_PLACEMENT_3D('',#77282,#54730,#54731);
#47496=AXIS2_PLACEMENT_3D('',#77283,#54732,#54733);
#47497=AXIS2_PLACEMENT_3D('',#77284,#54734,#54735);
#47498=AXIS2_PLACEMENT_3D('',#77320,#54737,#54738);
#47499=AXIS2_PLACEMENT_3D('',#77322,#54739,#54740);
#47500=AXIS2_PLACEMENT_3D('',#77377,#54744,#54745);
#47501=AXIS2_PLACEMENT_3D('',#77380,#54746,#54747);
#47502=AXIS2_PLACEMENT_3D('',#77387,#54748,#54749);
#47503=AXIS2_PLACEMENT_3D('',#77399,#54750,#54751);
#47504=AXIS2_PLACEMENT_3D('',#77400,#54752,#54753);
#47505=AXIS2_PLACEMENT_3D('',#77404,#54755,#54756);
#47506=AXIS2_PLACEMENT_3D('',#77406,#54757,#54758);
#47507=AXIS2_PLACEMENT_3D('',#77442,#54761,#54762);
#47508=AXIS2_PLACEMENT_3D('',#77450,#54764,#54765);
#47509=AXIS2_PLACEMENT_3D('',#77453,#54766,#54767);
#47510=AXIS2_PLACEMENT_3D('',#77454,#54768,#54769);
#47511=AXIS2_PLACEMENT_3D('',#77455,#54770,#54771);
#47512=AXIS2_PLACEMENT_3D('',#77474,#54772,#54773);
#47513=AXIS2_PLACEMENT_3D('',#77475,#54774,#54775);
#47514=AXIS2_PLACEMENT_3D('',#77479,#54777,#54778);
#47515=AXIS2_PLACEMENT_3D('',#77481,#54779,#54780);
#47516=AXIS2_PLACEMENT_3D('',#77524,#54783,#54784);
#47517=AXIS2_PLACEMENT_3D('',#77532,#54786,#54787);
#47518=AXIS2_PLACEMENT_3D('',#77535,#54788,#54789);
#47519=AXIS2_PLACEMENT_3D('',#77536,#54790,#54791);
#47520=AXIS2_PLACEMENT_3D('',#77537,#54792,#54793);
#47521=AXIS2_PLACEMENT_3D('',#77552,#54794,#54795);
#47522=AXIS2_PLACEMENT_3D('',#77553,#54796,#54797);
#47523=AXIS2_PLACEMENT_3D('',#77557,#54799,#54800);
#47524=AXIS2_PLACEMENT_3D('',#77559,#54801,#54802);
#47525=AXIS2_PLACEMENT_3D('',#77593,#54805,#54806);
#47526=AXIS2_PLACEMENT_3D('',#77595,#54808,#54809);
#47527=AXIS2_PLACEMENT_3D('',#77596,#54810,#54811);
#47528=AXIS2_PLACEMENT_3D('',#77599,#54813,#54814);
#47529=AXIS2_PLACEMENT_3D('',#77600,#54815,#54816);
#47530=AXIS2_PLACEMENT_3D('',#77601,#54817,#54818);
#47531=AXIS2_PLACEMENT_3D('',#77620,#54819,#54820);
#47532=AXIS2_PLACEMENT_3D('',#77621,#54821,#54822);
#47533=AXIS2_PLACEMENT_3D('',#77631,#54823,#54824);
#47534=AXIS2_PLACEMENT_3D('',#77651,#54826,#54827);
#47535=AXIS2_PLACEMENT_3D('',#77659,#54829,#54830);
#47536=AXIS2_PLACEMENT_3D('',#77662,#54831,#54832);
#47537=AXIS2_PLACEMENT_3D('',#77663,#54833,#54834);
#47538=AXIS2_PLACEMENT_3D('',#77664,#54835,#54836);
#47539=AXIS2_PLACEMENT_3D('',#77673,#54837,#54838);
#47540=AXIS2_PLACEMENT_3D('',#77674,#54839,#54840);
#47541=AXIS2_PLACEMENT_3D('',#77678,#54842,#54843);
#47542=AXIS2_PLACEMENT_3D('',#77680,#54844,#54845);
#47543=AXIS2_PLACEMENT_3D('',#77705,#54848,#54849);
#47544=AXIS2_PLACEMENT_3D('',#77706,#54850,#54851);
#47545=AXIS2_PLACEMENT_3D('',#77725,#54852,#54853);
#47546=AXIS2_PLACEMENT_3D('',#77733,#54855,#54856);
#47547=AXIS2_PLACEMENT_3D('',#77736,#54857,#54858);
#47548=AXIS2_PLACEMENT_3D('',#77737,#54859,#54860);
#47549=AXIS2_PLACEMENT_3D('',#77738,#54861,#54862);
#47550=AXIS2_PLACEMENT_3D('',#77750,#54863,#54864);
#47551=AXIS2_PLACEMENT_3D('',#77751,#54865,#54866);
#47552=AXIS2_PLACEMENT_3D('',#77755,#54868,#54869);
#47553=AXIS2_PLACEMENT_3D('',#77757,#54870,#54871);
#47554=AXIS2_PLACEMENT_3D('',#77793,#54874,#54875);
#47555=AXIS2_PLACEMENT_3D('',#77801,#54877,#54878);
#47556=AXIS2_PLACEMENT_3D('',#77804,#54879,#54880);
#47557=AXIS2_PLACEMENT_3D('',#77805,#54881,#54882);
#47558=AXIS2_PLACEMENT_3D('',#77806,#54883,#54884);
#47559=AXIS2_PLACEMENT_3D('',#77842,#54886,#54887);
#47560=AXIS2_PLACEMENT_3D('',#77844,#54888,#54889);
#47561=AXIS2_PLACEMENT_3D('',#77899,#54893,#54894);
#47562=AXIS2_PLACEMENT_3D('',#77902,#54895,#54896);
#47563=AXIS2_PLACEMENT_3D('',#77909,#54897,#54898);
#47564=AXIS2_PLACEMENT_3D('',#77921,#54899,#54900);
#47565=AXIS2_PLACEMENT_3D('',#77922,#54901,#54902);
#47566=AXIS2_PLACEMENT_3D('',#77926,#54904,#54905);
#47567=AXIS2_PLACEMENT_3D('',#77928,#54906,#54907);
#47568=AXIS2_PLACEMENT_3D('',#77964,#54910,#54911);
#47569=AXIS2_PLACEMENT_3D('',#77972,#54913,#54914);
#47570=AXIS2_PLACEMENT_3D('',#77975,#54915,#54916);
#47571=AXIS2_PLACEMENT_3D('',#77976,#54917,#54918);
#47572=AXIS2_PLACEMENT_3D('',#77977,#54919,#54920);
#47573=AXIS2_PLACEMENT_3D('',#77996,#54921,#54922);
#47574=AXIS2_PLACEMENT_3D('',#77997,#54923,#54924);
#47575=AXIS2_PLACEMENT_3D('',#78001,#54926,#54927);
#47576=AXIS2_PLACEMENT_3D('',#78003,#54928,#54929);
#47577=AXIS2_PLACEMENT_3D('',#78039,#54932,#54933);
#47578=AXIS2_PLACEMENT_3D('',#78047,#54935,#54936);
#47579=AXIS2_PLACEMENT_3D('',#78050,#54937,#54938);
#47580=AXIS2_PLACEMENT_3D('',#78051,#54939,#54940);
#47581=AXIS2_PLACEMENT_3D('',#78052,#54941,#54942);
#47582=AXIS2_PLACEMENT_3D('',#78064,#54943,#54944);
#47583=AXIS2_PLACEMENT_3D('',#78065,#54945,#54946);
#47584=AXIS2_PLACEMENT_3D('',#78069,#54948,#54949);
#47585=AXIS2_PLACEMENT_3D('',#78071,#54950,#54951);
#47586=AXIS2_PLACEMENT_3D('',#78112,#54954,#54955);
#47587=AXIS2_PLACEMENT_3D('',#78114,#54957,#54958);
#47588=AXIS2_PLACEMENT_3D('',#78115,#54959,#54960);
#47589=AXIS2_PLACEMENT_3D('',#78118,#54962,#54963);
#47590=AXIS2_PLACEMENT_3D('',#78119,#54964,#54965);
#47591=AXIS2_PLACEMENT_3D('',#78120,#54966,#54967);
#47592=AXIS2_PLACEMENT_3D('',#78139,#54968,#54969);
#47593=AXIS2_PLACEMENT_3D('',#78140,#54970,#54971);
#47594=AXIS2_PLACEMENT_3D('',#78150,#54972,#54973);
#47595=AXIS2_PLACEMENT_3D('',#78170,#54975,#54976);
#47596=AXIS2_PLACEMENT_3D('',#78178,#54978,#54979);
#47597=AXIS2_PLACEMENT_3D('',#78181,#54980,#54981);
#47598=AXIS2_PLACEMENT_3D('',#78182,#54982,#54983);
#47599=AXIS2_PLACEMENT_3D('',#78183,#54984,#54985);
#47600=AXIS2_PLACEMENT_3D('',#78192,#54986,#54987);
#47601=AXIS2_PLACEMENT_3D('',#78193,#54988,#54989);
#47602=AXIS2_PLACEMENT_3D('',#78197,#54991,#54992);
#47603=AXIS2_PLACEMENT_3D('',#78199,#54993,#54994);
#47604=AXIS2_PLACEMENT_3D('',#78224,#54997,#54998);
#47605=AXIS2_PLACEMENT_3D('',#78225,#54999,#55000);
#47606=AXIS2_PLACEMENT_3D('',#78244,#55001,#55002);
#47607=AXIS2_PLACEMENT_3D('',#78252,#55004,#55005);
#47608=AXIS2_PLACEMENT_3D('',#78255,#55006,#55007);
#47609=AXIS2_PLACEMENT_3D('',#78256,#55008,#55009);
#47610=AXIS2_PLACEMENT_3D('',#78257,#55010,#55011);
#47611=AXIS2_PLACEMENT_3D('',#78269,#55012,#55013);
#47612=AXIS2_PLACEMENT_3D('',#78270,#55014,#55015);
#47613=AXIS2_PLACEMENT_3D('',#78274,#55017,#55018);
#47614=AXIS2_PLACEMENT_3D('',#78276,#55019,#55020);
#47615=AXIS2_PLACEMENT_3D('',#78312,#55023,#55024);
#47616=AXIS2_PLACEMENT_3D('',#78320,#55026,#55027);
#47617=AXIS2_PLACEMENT_3D('',#78323,#55028,#55029);
#47618=AXIS2_PLACEMENT_3D('',#78324,#55030,#55031);
#47619=AXIS2_PLACEMENT_3D('',#78325,#55032,#55033);
#47620=AXIS2_PLACEMENT_3D('',#78361,#55035,#55036);
#47621=AXIS2_PLACEMENT_3D('',#78363,#55037,#55038);
#47622=AXIS2_PLACEMENT_3D('',#78418,#55042,#55043);
#47623=AXIS2_PLACEMENT_3D('',#78421,#55044,#55045);
#47624=AXIS2_PLACEMENT_3D('',#78428,#55046,#55047);
#47625=AXIS2_PLACEMENT_3D('',#78440,#55048,#55049);
#47626=AXIS2_PLACEMENT_3D('',#78441,#55050,#55051);
#47627=AXIS2_PLACEMENT_3D('',#78445,#55053,#55054);
#47628=AXIS2_PLACEMENT_3D('',#78447,#55055,#55056);
#47629=AXIS2_PLACEMENT_3D('',#78483,#55059,#55060);
#47630=AXIS2_PLACEMENT_3D('',#78491,#55062,#55063);
#47631=AXIS2_PLACEMENT_3D('',#78494,#55064,#55065);
#47632=AXIS2_PLACEMENT_3D('',#78495,#55066,#55067);
#47633=AXIS2_PLACEMENT_3D('',#78496,#55068,#55069);
#47634=AXIS2_PLACEMENT_3D('',#78515,#55070,#55071);
#47635=AXIS2_PLACEMENT_3D('',#78516,#55072,#55073);
#47636=AXIS2_PLACEMENT_3D('',#78520,#55075,#55076);
#47637=AXIS2_PLACEMENT_3D('',#78522,#55077,#55078);
#47638=AXIS2_PLACEMENT_3D('',#78558,#55081,#55082);
#47639=AXIS2_PLACEMENT_3D('',#78566,#55084,#55085);
#47640=AXIS2_PLACEMENT_3D('',#78569,#55086,#55087);
#47641=AXIS2_PLACEMENT_3D('',#78570,#55088,#55089);
#47642=AXIS2_PLACEMENT_3D('',#78571,#55090,#55091);
#47643=AXIS2_PLACEMENT_3D('',#78586,#55092,#55093);
#47644=AXIS2_PLACEMENT_3D('',#78587,#55094,#55095);
#47645=AXIS2_PLACEMENT_3D('',#78591,#55097,#55098);
#47646=AXIS2_PLACEMENT_3D('',#78593,#55099,#55100);
#47647=AXIS2_PLACEMENT_3D('',#78627,#55103,#55104);
#47648=AXIS2_PLACEMENT_3D('',#78629,#55106,#55107);
#47649=AXIS2_PLACEMENT_3D('',#78630,#55108,#55109);
#47650=AXIS2_PLACEMENT_3D('',#78633,#55111,#55112);
#47651=AXIS2_PLACEMENT_3D('',#78634,#55113,#55114);
#47652=AXIS2_PLACEMENT_3D('',#78635,#55115,#55116);
#47653=AXIS2_PLACEMENT_3D('',#78654,#55117,#55118);
#47654=AXIS2_PLACEMENT_3D('',#78655,#55119,#55120);
#47655=AXIS2_PLACEMENT_3D('',#78665,#55121,#55122);
#47656=AXIS2_PLACEMENT_3D('',#78685,#55124,#55125);
#47657=AXIS2_PLACEMENT_3D('',#78693,#55127,#55128);
#47658=AXIS2_PLACEMENT_3D('',#78696,#55129,#55130);
#47659=AXIS2_PLACEMENT_3D('',#78697,#55131,#55132);
#47660=AXIS2_PLACEMENT_3D('',#78698,#55133,#55134);
#47661=AXIS2_PLACEMENT_3D('',#78707,#55135,#55136);
#47662=AXIS2_PLACEMENT_3D('',#78708,#55137,#55138);
#47663=AXIS2_PLACEMENT_3D('',#78712,#55140,#55141);
#47664=AXIS2_PLACEMENT_3D('',#78714,#55142,#55143);
#47665=AXIS2_PLACEMENT_3D('',#78739,#55146,#55147);
#47666=AXIS2_PLACEMENT_3D('',#78740,#55148,#55149);
#47667=AXIS2_PLACEMENT_3D('',#78759,#55150,#55151);
#47668=AXIS2_PLACEMENT_3D('',#78767,#55153,#55154);
#47669=AXIS2_PLACEMENT_3D('',#78770,#55155,#55156);
#47670=AXIS2_PLACEMENT_3D('',#78771,#55157,#55158);
#47671=AXIS2_PLACEMENT_3D('',#78772,#55159,#55160);
#47672=AXIS2_PLACEMENT_3D('',#78784,#55161,#55162);
#47673=AXIS2_PLACEMENT_3D('',#78785,#55163,#55164);
#47674=AXIS2_PLACEMENT_3D('',#78789,#55166,#55167);
#47675=AXIS2_PLACEMENT_3D('',#78791,#55168,#55169);
#47676=AXIS2_PLACEMENT_3D('',#78827,#55172,#55173);
#47677=AXIS2_PLACEMENT_3D('',#78835,#55175,#55176);
#47678=AXIS2_PLACEMENT_3D('',#78838,#55177,#55178);
#47679=AXIS2_PLACEMENT_3D('',#78839,#55179,#55180);
#47680=AXIS2_PLACEMENT_3D('',#78840,#55181,#55182);
#47681=AXIS2_PLACEMENT_3D('',#78876,#55184,#55185);
#47682=AXIS2_PLACEMENT_3D('',#78878,#55186,#55187);
#47683=AXIS2_PLACEMENT_3D('',#78933,#55191,#55192);
#47684=AXIS2_PLACEMENT_3D('',#78936,#55193,#55194);
#47685=AXIS2_PLACEMENT_3D('',#78943,#55195,#55196);
#47686=AXIS2_PLACEMENT_3D('',#78955,#55197,#55198);
#47687=AXIS2_PLACEMENT_3D('',#78956,#55199,#55200);
#47688=AXIS2_PLACEMENT_3D('',#78960,#55202,#55203);
#47689=AXIS2_PLACEMENT_3D('',#78962,#55204,#55205);
#47690=AXIS2_PLACEMENT_3D('',#78998,#55208,#55209);
#47691=AXIS2_PLACEMENT_3D('',#79006,#55211,#55212);
#47692=AXIS2_PLACEMENT_3D('',#79009,#55213,#55214);
#47693=AXIS2_PLACEMENT_3D('',#79010,#55215,#55216);
#47694=AXIS2_PLACEMENT_3D('',#79011,#55217,#55218);
#47695=AXIS2_PLACEMENT_3D('',#79030,#55219,#55220);
#47696=AXIS2_PLACEMENT_3D('',#79031,#55221,#55222);
#47697=AXIS2_PLACEMENT_3D('',#79035,#55224,#55225);
#47698=AXIS2_PLACEMENT_3D('',#79037,#55226,#55227);
#47699=AXIS2_PLACEMENT_3D('',#79073,#55230,#55231);
#47700=AXIS2_PLACEMENT_3D('',#79081,#55233,#55234);
#47701=AXIS2_PLACEMENT_3D('',#79084,#55235,#55236);
#47702=AXIS2_PLACEMENT_3D('',#79085,#55237,#55238);
#47703=AXIS2_PLACEMENT_3D('',#79086,#55239,#55240);
#47704=AXIS2_PLACEMENT_3D('',#79101,#55241,#55242);
#47705=AXIS2_PLACEMENT_3D('',#79102,#55243,#55244);
#47706=AXIS2_PLACEMENT_3D('',#79106,#55246,#55247);
#47707=AXIS2_PLACEMENT_3D('',#79108,#55248,#55249);
#47708=AXIS2_PLACEMENT_3D('',#79142,#55252,#55253);
#47709=AXIS2_PLACEMENT_3D('',#79144,#55255,#55256);
#47710=AXIS2_PLACEMENT_3D('',#79145,#55257,#55258);
#47711=AXIS2_PLACEMENT_3D('',#79148,#55260,#55261);
#47712=AXIS2_PLACEMENT_3D('',#79149,#55262,#55263);
#47713=AXIS2_PLACEMENT_3D('',#79150,#55264,#55265);
#47714=AXIS2_PLACEMENT_3D('',#79169,#55266,#55267);
#47715=AXIS2_PLACEMENT_3D('',#79170,#55268,#55269);
#47716=AXIS2_PLACEMENT_3D('',#79180,#55270,#55271);
#47717=AXIS2_PLACEMENT_3D('',#79200,#55273,#55274);
#47718=AXIS2_PLACEMENT_3D('',#79208,#55276,#55277);
#47719=AXIS2_PLACEMENT_3D('',#79211,#55278,#55279);
#47720=AXIS2_PLACEMENT_3D('',#79212,#55280,#55281);
#47721=AXIS2_PLACEMENT_3D('',#79213,#55282,#55283);
#47722=AXIS2_PLACEMENT_3D('',#79222,#55284,#55285);
#47723=AXIS2_PLACEMENT_3D('',#79223,#55286,#55287);
#47724=AXIS2_PLACEMENT_3D('',#79227,#55289,#55290);
#47725=AXIS2_PLACEMENT_3D('',#79229,#55291,#55292);
#47726=AXIS2_PLACEMENT_3D('',#79254,#55295,#55296);
#47727=AXIS2_PLACEMENT_3D('',#79255,#55297,#55298);
#47728=AXIS2_PLACEMENT_3D('',#79274,#55299,#55300);
#47729=AXIS2_PLACEMENT_3D('',#79282,#55302,#55303);
#47730=AXIS2_PLACEMENT_3D('',#79285,#55304,#55305);
#47731=AXIS2_PLACEMENT_3D('',#79286,#55306,#55307);
#47732=AXIS2_PLACEMENT_3D('',#79287,#55308,#55309);
#47733=AXIS2_PLACEMENT_3D('',#79299,#55310,#55311);
#47734=AXIS2_PLACEMENT_3D('',#79300,#55312,#55313);
#47735=AXIS2_PLACEMENT_3D('',#79304,#55315,#55316);
#47736=AXIS2_PLACEMENT_3D('',#79306,#55317,#55318);
#47737=AXIS2_PLACEMENT_3D('',#79342,#55321,#55322);
#47738=AXIS2_PLACEMENT_3D('',#79350,#55324,#55325);
#47739=AXIS2_PLACEMENT_3D('',#79353,#55326,#55327);
#47740=AXIS2_PLACEMENT_3D('',#79354,#55328,#55329);
#47741=AXIS2_PLACEMENT_3D('',#79355,#55330,#55331);
#47742=AXIS2_PLACEMENT_3D('',#79391,#55333,#55334);
#47743=AXIS2_PLACEMENT_3D('',#79393,#55335,#55336);
#47744=AXIS2_PLACEMENT_3D('',#79448,#55340,#55341);
#47745=AXIS2_PLACEMENT_3D('',#79451,#55342,#55343);
#47746=AXIS2_PLACEMENT_3D('',#79458,#55344,#55345);
#47747=AXIS2_PLACEMENT_3D('',#79470,#55346,#55347);
#47748=AXIS2_PLACEMENT_3D('',#79471,#55348,#55349);
#47749=AXIS2_PLACEMENT_3D('',#79475,#55351,#55352);
#47750=AXIS2_PLACEMENT_3D('',#79477,#55353,#55354);
#47751=AXIS2_PLACEMENT_3D('',#79513,#55357,#55358);
#47752=AXIS2_PLACEMENT_3D('',#79521,#55360,#55361);
#47753=AXIS2_PLACEMENT_3D('',#79524,#55362,#55363);
#47754=AXIS2_PLACEMENT_3D('',#79525,#55364,#55365);
#47755=AXIS2_PLACEMENT_3D('',#79526,#55366,#55367);
#47756=AXIS2_PLACEMENT_3D('',#79545,#55368,#55369);
#47757=AXIS2_PLACEMENT_3D('',#79546,#55370,#55371);
#47758=AXIS2_PLACEMENT_3D('',#79550,#55373,#55374);
#47759=AXIS2_PLACEMENT_3D('',#79552,#55375,#55376);
#47760=AXIS2_PLACEMENT_3D('',#79588,#55379,#55380);
#47761=AXIS2_PLACEMENT_3D('',#79596,#55382,#55383);
#47762=AXIS2_PLACEMENT_3D('',#79599,#55384,#55385);
#47763=AXIS2_PLACEMENT_3D('',#79600,#55386,#55387);
#47764=AXIS2_PLACEMENT_3D('',#79601,#55388,#55389);
#47765=AXIS2_PLACEMENT_3D('',#79616,#55390,#55391);
#47766=AXIS2_PLACEMENT_3D('',#79617,#55392,#55393);
#47767=AXIS2_PLACEMENT_3D('',#79621,#55395,#55396);
#47768=AXIS2_PLACEMENT_3D('',#79623,#55397,#55398);
#47769=AXIS2_PLACEMENT_3D('',#79657,#55401,#55402);
#47770=AXIS2_PLACEMENT_3D('',#79659,#55404,#55405);
#47771=AXIS2_PLACEMENT_3D('',#79660,#55406,#55407);
#47772=AXIS2_PLACEMENT_3D('',#79663,#55409,#55410);
#47773=AXIS2_PLACEMENT_3D('',#79664,#55411,#55412);
#47774=AXIS2_PLACEMENT_3D('',#79665,#55413,#55414);
#47775=AXIS2_PLACEMENT_3D('',#79684,#55415,#55416);
#47776=AXIS2_PLACEMENT_3D('',#79685,#55417,#55418);
#47777=AXIS2_PLACEMENT_3D('',#79695,#55419,#55420);
#47778=AXIS2_PLACEMENT_3D('',#79715,#55422,#55423);
#47779=AXIS2_PLACEMENT_3D('',#79723,#55425,#55426);
#47780=AXIS2_PLACEMENT_3D('',#79726,#55427,#55428);
#47781=AXIS2_PLACEMENT_3D('',#79727,#55429,#55430);
#47782=AXIS2_PLACEMENT_3D('',#79728,#55431,#55432);
#47783=AXIS2_PLACEMENT_3D('',#79737,#55433,#55434);
#47784=AXIS2_PLACEMENT_3D('',#79738,#55435,#55436);
#47785=AXIS2_PLACEMENT_3D('',#79742,#55438,#55439);
#47786=AXIS2_PLACEMENT_3D('',#79744,#55440,#55441);
#47787=AXIS2_PLACEMENT_3D('',#79769,#55444,#55445);
#47788=AXIS2_PLACEMENT_3D('',#79770,#55446,#55447);
#47789=AXIS2_PLACEMENT_3D('',#79789,#55448,#55449);
#47790=AXIS2_PLACEMENT_3D('',#79797,#55451,#55452);
#47791=AXIS2_PLACEMENT_3D('',#79800,#55453,#55454);
#47792=AXIS2_PLACEMENT_3D('',#79801,#55455,#55456);
#47793=AXIS2_PLACEMENT_3D('',#79802,#55457,#55458);
#47794=AXIS2_PLACEMENT_3D('',#79814,#55459,#55460);
#47795=AXIS2_PLACEMENT_3D('',#79815,#55461,#55462);
#47796=AXIS2_PLACEMENT_3D('',#79819,#55464,#55465);
#47797=AXIS2_PLACEMENT_3D('',#79821,#55466,#55467);
#47798=AXIS2_PLACEMENT_3D('',#79857,#55470,#55471);
#47799=AXIS2_PLACEMENT_3D('',#79865,#55473,#55474);
#47800=AXIS2_PLACEMENT_3D('',#79868,#55475,#55476);
#47801=AXIS2_PLACEMENT_3D('',#79869,#55477,#55478);
#47802=AXIS2_PLACEMENT_3D('',#79870,#55479,#55480);
#47803=AXIS2_PLACEMENT_3D('',#79906,#55482,#55483);
#47804=AXIS2_PLACEMENT_3D('',#79908,#55484,#55485);
#47805=AXIS2_PLACEMENT_3D('',#79963,#55489,#55490);
#47806=AXIS2_PLACEMENT_3D('',#79966,#55491,#55492);
#47807=AXIS2_PLACEMENT_3D('',#79973,#55493,#55494);
#47808=AXIS2_PLACEMENT_3D('',#79985,#55495,#55496);
#47809=AXIS2_PLACEMENT_3D('',#79986,#55497,#55498);
#47810=AXIS2_PLACEMENT_3D('',#79990,#55500,#55501);
#47811=AXIS2_PLACEMENT_3D('',#79992,#55502,#55503);
#47812=AXIS2_PLACEMENT_3D('',#80028,#55506,#55507);
#47813=AXIS2_PLACEMENT_3D('',#80036,#55509,#55510);
#47814=AXIS2_PLACEMENT_3D('',#80039,#55511,#55512);
#47815=AXIS2_PLACEMENT_3D('',#80040,#55513,#55514);
#47816=AXIS2_PLACEMENT_3D('',#80041,#55515,#55516);
#47817=AXIS2_PLACEMENT_3D('',#80060,#55517,#55518);
#47818=AXIS2_PLACEMENT_3D('',#80061,#55519,#55520);
#47819=AXIS2_PLACEMENT_3D('',#80065,#55522,#55523);
#47820=AXIS2_PLACEMENT_3D('',#80067,#55524,#55525);
#47821=AXIS2_PLACEMENT_3D('',#80103,#55528,#55529);
#47822=AXIS2_PLACEMENT_3D('',#80111,#55531,#55532);
#47823=AXIS2_PLACEMENT_3D('',#80114,#55533,#55534);
#47824=AXIS2_PLACEMENT_3D('',#80115,#55535,#55536);
#47825=AXIS2_PLACEMENT_3D('',#80116,#55537,#55538);
#47826=AXIS2_PLACEMENT_3D('',#80131,#55539,#55540);
#47827=AXIS2_PLACEMENT_3D('',#80132,#55541,#55542);
#47828=AXIS2_PLACEMENT_3D('',#80136,#55544,#55545);
#47829=AXIS2_PLACEMENT_3D('',#80138,#55546,#55547);
#47830=AXIS2_PLACEMENT_3D('',#80172,#55550,#55551);
#47831=AXIS2_PLACEMENT_3D('',#80174,#55553,#55554);
#47832=AXIS2_PLACEMENT_3D('',#80175,#55555,#55556);
#47833=AXIS2_PLACEMENT_3D('',#80178,#55558,#55559);
#47834=AXIS2_PLACEMENT_3D('',#80179,#55560,#55561);
#47835=AXIS2_PLACEMENT_3D('',#80180,#55562,#55563);
#47836=AXIS2_PLACEMENT_3D('',#80199,#55564,#55565);
#47837=AXIS2_PLACEMENT_3D('',#80200,#55566,#55567);
#47838=AXIS2_PLACEMENT_3D('',#80210,#55568,#55569);
#47839=AXIS2_PLACEMENT_3D('',#80230,#55571,#55572);
#47840=AXIS2_PLACEMENT_3D('',#80238,#55574,#55575);
#47841=AXIS2_PLACEMENT_3D('',#80241,#55576,#55577);
#47842=AXIS2_PLACEMENT_3D('',#80242,#55578,#55579);
#47843=AXIS2_PLACEMENT_3D('',#80243,#55580,#55581);
#47844=AXIS2_PLACEMENT_3D('',#80252,#55582,#55583);
#47845=AXIS2_PLACEMENT_3D('',#80253,#55584,#55585);
#47846=AXIS2_PLACEMENT_3D('',#80257,#55587,#55588);
#47847=AXIS2_PLACEMENT_3D('',#80259,#55589,#55590);
#47848=AXIS2_PLACEMENT_3D('',#80284,#55593,#55594);
#47849=AXIS2_PLACEMENT_3D('',#80285,#55595,#55596);
#47850=AXIS2_PLACEMENT_3D('',#80304,#55597,#55598);
#47851=AXIS2_PLACEMENT_3D('',#80312,#55600,#55601);
#47852=AXIS2_PLACEMENT_3D('',#80315,#55602,#55603);
#47853=AXIS2_PLACEMENT_3D('',#80316,#55604,#55605);
#47854=AXIS2_PLACEMENT_3D('',#80317,#55606,#55607);
#47855=AXIS2_PLACEMENT_3D('',#80329,#55608,#55609);
#47856=AXIS2_PLACEMENT_3D('',#80330,#55610,#55611);
#47857=AXIS2_PLACEMENT_3D('',#80334,#55613,#55614);
#47858=AXIS2_PLACEMENT_3D('',#80336,#55615,#55616);
#47859=AXIS2_PLACEMENT_3D('',#80372,#55619,#55620);
#47860=AXIS2_PLACEMENT_3D('',#80380,#55622,#55623);
#47861=AXIS2_PLACEMENT_3D('',#80383,#55624,#55625);
#47862=AXIS2_PLACEMENT_3D('',#80384,#55626,#55627);
#47863=AXIS2_PLACEMENT_3D('',#80385,#55628,#55629);
#47864=AXIS2_PLACEMENT_3D('',#80421,#55631,#55632);
#47865=AXIS2_PLACEMENT_3D('',#80423,#55633,#55634);
#47866=AXIS2_PLACEMENT_3D('',#80478,#55638,#55639);
#47867=AXIS2_PLACEMENT_3D('',#80481,#55640,#55641);
#47868=AXIS2_PLACEMENT_3D('',#80488,#55642,#55643);
#47869=AXIS2_PLACEMENT_3D('',#80500,#55644,#55645);
#47870=AXIS2_PLACEMENT_3D('',#80501,#55646,#55647);
#47871=AXIS2_PLACEMENT_3D('',#80505,#55649,#55650);
#47872=AXIS2_PLACEMENT_3D('',#80507,#55651,#55652);
#47873=AXIS2_PLACEMENT_3D('',#80543,#55655,#55656);
#47874=AXIS2_PLACEMENT_3D('',#80551,#55658,#55659);
#47875=AXIS2_PLACEMENT_3D('',#80554,#55660,#55661);
#47876=AXIS2_PLACEMENT_3D('',#80555,#55662,#55663);
#47877=AXIS2_PLACEMENT_3D('',#80556,#55664,#55665);
#47878=AXIS2_PLACEMENT_3D('',#80575,#55666,#55667);
#47879=AXIS2_PLACEMENT_3D('',#80576,#55668,#55669);
#47880=AXIS2_PLACEMENT_3D('',#80580,#55671,#55672);
#47881=AXIS2_PLACEMENT_3D('',#80582,#55673,#55674);
#47882=AXIS2_PLACEMENT_3D('',#80618,#55677,#55678);
#47883=AXIS2_PLACEMENT_3D('',#80626,#55680,#55681);
#47884=AXIS2_PLACEMENT_3D('',#80629,#55682,#55683);
#47885=AXIS2_PLACEMENT_3D('',#80630,#55684,#55685);
#47886=AXIS2_PLACEMENT_3D('',#80631,#55686,#55687);
#47887=AXIS2_PLACEMENT_3D('',#80646,#55688,#55689);
#47888=AXIS2_PLACEMENT_3D('',#80647,#55690,#55691);
#47889=AXIS2_PLACEMENT_3D('',#80651,#55693,#55694);
#47890=AXIS2_PLACEMENT_3D('',#80653,#55695,#55696);
#47891=AXIS2_PLACEMENT_3D('',#80687,#55699,#55700);
#47892=AXIS2_PLACEMENT_3D('',#80689,#55702,#55703);
#47893=AXIS2_PLACEMENT_3D('',#80690,#55704,#55705);
#47894=AXIS2_PLACEMENT_3D('',#80693,#55707,#55708);
#47895=AXIS2_PLACEMENT_3D('',#80694,#55709,#55710);
#47896=AXIS2_PLACEMENT_3D('',#80695,#55711,#55712);
#47897=AXIS2_PLACEMENT_3D('',#80714,#55713,#55714);
#47898=AXIS2_PLACEMENT_3D('',#80715,#55715,#55716);
#47899=AXIS2_PLACEMENT_3D('',#80725,#55717,#55718);
#47900=AXIS2_PLACEMENT_3D('',#80745,#55720,#55721);
#47901=AXIS2_PLACEMENT_3D('',#80753,#55723,#55724);
#47902=AXIS2_PLACEMENT_3D('',#80756,#55725,#55726);
#47903=AXIS2_PLACEMENT_3D('',#80757,#55727,#55728);
#47904=AXIS2_PLACEMENT_3D('',#80758,#55729,#55730);
#47905=AXIS2_PLACEMENT_3D('',#80767,#55731,#55732);
#47906=AXIS2_PLACEMENT_3D('',#80768,#55733,#55734);
#47907=AXIS2_PLACEMENT_3D('',#80772,#55736,#55737);
#47908=AXIS2_PLACEMENT_3D('',#80774,#55738,#55739);
#47909=AXIS2_PLACEMENT_3D('',#80799,#55742,#55743);
#47910=AXIS2_PLACEMENT_3D('',#80800,#55744,#55745);
#47911=AXIS2_PLACEMENT_3D('',#80819,#55746,#55747);
#47912=AXIS2_PLACEMENT_3D('',#80827,#55749,#55750);
#47913=AXIS2_PLACEMENT_3D('',#80830,#55751,#55752);
#47914=AXIS2_PLACEMENT_3D('',#80831,#55753,#55754);
#47915=AXIS2_PLACEMENT_3D('',#80832,#55755,#55756);
#47916=AXIS2_PLACEMENT_3D('',#80844,#55757,#55758);
#47917=AXIS2_PLACEMENT_3D('',#80845,#55759,#55760);
#47918=AXIS2_PLACEMENT_3D('',#80849,#55762,#55763);
#47919=AXIS2_PLACEMENT_3D('',#80851,#55764,#55765);
#47920=AXIS2_PLACEMENT_3D('',#80887,#55768,#55769);
#47921=AXIS2_PLACEMENT_3D('',#80895,#55771,#55772);
#47922=AXIS2_PLACEMENT_3D('',#80898,#55773,#55774);
#47923=AXIS2_PLACEMENT_3D('',#80899,#55775,#55776);
#47924=AXIS2_PLACEMENT_3D('',#80900,#55777,#55778);
#47925=AXIS2_PLACEMENT_3D('',#80936,#55780,#55781);
#47926=AXIS2_PLACEMENT_3D('',#80938,#55782,#55783);
#47927=AXIS2_PLACEMENT_3D('',#80993,#55787,#55788);
#47928=AXIS2_PLACEMENT_3D('',#80996,#55789,#55790);
#47929=AXIS2_PLACEMENT_3D('',#81003,#55791,#55792);
#47930=AXIS2_PLACEMENT_3D('',#81015,#55793,#55794);
#47931=AXIS2_PLACEMENT_3D('',#81016,#55795,#55796);
#47932=AXIS2_PLACEMENT_3D('',#81020,#55798,#55799);
#47933=AXIS2_PLACEMENT_3D('',#81022,#55800,#55801);
#47934=AXIS2_PLACEMENT_3D('',#81058,#55804,#55805);
#47935=AXIS2_PLACEMENT_3D('',#81066,#55807,#55808);
#47936=AXIS2_PLACEMENT_3D('',#81069,#55809,#55810);
#47937=AXIS2_PLACEMENT_3D('',#81070,#55811,#55812);
#47938=AXIS2_PLACEMENT_3D('',#81071,#55813,#55814);
#47939=AXIS2_PLACEMENT_3D('',#81090,#55815,#55816);
#47940=AXIS2_PLACEMENT_3D('',#81091,#55817,#55818);
#47941=AXIS2_PLACEMENT_3D('',#81095,#55820,#55821);
#47942=AXIS2_PLACEMENT_3D('',#81097,#55822,#55823);
#47943=AXIS2_PLACEMENT_3D('',#81133,#55826,#55827);
#47944=AXIS2_PLACEMENT_3D('',#81141,#55829,#55830);
#47945=AXIS2_PLACEMENT_3D('',#81144,#55831,#55832);
#47946=AXIS2_PLACEMENT_3D('',#81145,#55833,#55834);
#47947=AXIS2_PLACEMENT_3D('',#81146,#55835,#55836);
#47948=AXIS2_PLACEMENT_3D('',#81161,#55837,#55838);
#47949=AXIS2_PLACEMENT_3D('',#81162,#55839,#55840);
#47950=AXIS2_PLACEMENT_3D('',#81166,#55842,#55843);
#47951=AXIS2_PLACEMENT_3D('',#81168,#55844,#55845);
#47952=AXIS2_PLACEMENT_3D('',#81202,#55848,#55849);
#47953=AXIS2_PLACEMENT_3D('',#81204,#55851,#55852);
#47954=AXIS2_PLACEMENT_3D('',#81205,#55853,#55854);
#47955=AXIS2_PLACEMENT_3D('',#81208,#55856,#55857);
#47956=AXIS2_PLACEMENT_3D('',#81209,#55858,#55859);
#47957=AXIS2_PLACEMENT_3D('',#81210,#55860,#55861);
#47958=AXIS2_PLACEMENT_3D('',#81229,#55862,#55863);
#47959=AXIS2_PLACEMENT_3D('',#81230,#55864,#55865);
#47960=AXIS2_PLACEMENT_3D('',#81240,#55866,#55867);
#47961=AXIS2_PLACEMENT_3D('',#81260,#55869,#55870);
#47962=AXIS2_PLACEMENT_3D('',#81268,#55872,#55873);
#47963=AXIS2_PLACEMENT_3D('',#81271,#55874,#55875);
#47964=AXIS2_PLACEMENT_3D('',#81272,#55876,#55877);
#47965=AXIS2_PLACEMENT_3D('',#81273,#55878,#55879);
#47966=AXIS2_PLACEMENT_3D('',#81282,#55880,#55881);
#47967=AXIS2_PLACEMENT_3D('',#81283,#55882,#55883);
#47968=AXIS2_PLACEMENT_3D('',#81287,#55885,#55886);
#47969=AXIS2_PLACEMENT_3D('',#81289,#55887,#55888);
#47970=AXIS2_PLACEMENT_3D('',#81314,#55891,#55892);
#47971=AXIS2_PLACEMENT_3D('',#81315,#55893,#55894);
#47972=AXIS2_PLACEMENT_3D('',#81334,#55895,#55896);
#47973=AXIS2_PLACEMENT_3D('',#81342,#55898,#55899);
#47974=AXIS2_PLACEMENT_3D('',#81345,#55900,#55901);
#47975=AXIS2_PLACEMENT_3D('',#81346,#55902,#55903);
#47976=AXIS2_PLACEMENT_3D('',#81347,#55904,#55905);
#47977=AXIS2_PLACEMENT_3D('',#81356,#55906,#55907);
#47978=AXIS2_PLACEMENT_3D('',#81357,#55908,#55909);
#47979=AXIS2_PLACEMENT_3D('',#81361,#55911,#55912);
#47980=AXIS2_PLACEMENT_3D('',#81363,#55913,#55914);
#47981=AXIS2_PLACEMENT_3D('',#81406,#55917,#55918);
#47982=AXIS2_PLACEMENT_3D('',#81414,#55920,#55921);
#47983=AXIS2_PLACEMENT_3D('',#81417,#55922,#55923);
#47984=AXIS2_PLACEMENT_3D('',#81418,#55924,#55925);
#47985=AXIS2_PLACEMENT_3D('',#81419,#55926,#55927);
#47986=AXIS2_PLACEMENT_3D('',#81455,#55929,#55930);
#47987=AXIS2_PLACEMENT_3D('',#81457,#55931,#55932);
#47988=AXIS2_PLACEMENT_3D('',#81512,#55936,#55937);
#47989=AXIS2_PLACEMENT_3D('',#81515,#55938,#55939);
#47990=AXIS2_PLACEMENT_3D('',#81522,#55940,#55941);
#47991=AXIS2_PLACEMENT_3D('',#81534,#55942,#55943);
#47992=AXIS2_PLACEMENT_3D('',#81535,#55944,#55945);
#47993=AXIS2_PLACEMENT_3D('',#81539,#55947,#55948);
#47994=AXIS2_PLACEMENT_3D('',#81541,#55949,#55950);
#47995=AXIS2_PLACEMENT_3D('',#81577,#55953,#55954);
#47996=AXIS2_PLACEMENT_3D('',#81585,#55956,#55957);
#47997=AXIS2_PLACEMENT_3D('',#81588,#55958,#55959);
#47998=AXIS2_PLACEMENT_3D('',#81589,#55960,#55961);
#47999=AXIS2_PLACEMENT_3D('',#81590,#55962,#55963);
#48000=AXIS2_PLACEMENT_3D('',#81609,#55964,#55965);
#48001=AXIS2_PLACEMENT_3D('',#81610,#55966,#55967);
#48002=AXIS2_PLACEMENT_3D('',#81614,#55969,#55970);
#48003=AXIS2_PLACEMENT_3D('',#81616,#55971,#55972);
#48004=AXIS2_PLACEMENT_3D('',#81652,#55975,#55976);
#48005=AXIS2_PLACEMENT_3D('',#81660,#55978,#55979);
#48006=AXIS2_PLACEMENT_3D('',#81663,#55980,#55981);
#48007=AXIS2_PLACEMENT_3D('',#81664,#55982,#55983);
#48008=AXIS2_PLACEMENT_3D('',#81665,#55984,#55985);
#48009=AXIS2_PLACEMENT_3D('',#81680,#55986,#55987);
#48010=AXIS2_PLACEMENT_3D('',#81681,#55988,#55989);
#48011=AXIS2_PLACEMENT_3D('',#81685,#55991,#55992);
#48012=AXIS2_PLACEMENT_3D('',#81687,#55993,#55994);
#48013=AXIS2_PLACEMENT_3D('',#81721,#55997,#55998);
#48014=AXIS2_PLACEMENT_3D('',#81723,#56000,#56001);
#48015=AXIS2_PLACEMENT_3D('',#81724,#56002,#56003);
#48016=AXIS2_PLACEMENT_3D('',#81727,#56005,#56006);
#48017=AXIS2_PLACEMENT_3D('',#81728,#56007,#56008);
#48018=AXIS2_PLACEMENT_3D('',#81729,#56009,#56010);
#48019=AXIS2_PLACEMENT_3D('',#81748,#56011,#56012);
#48020=AXIS2_PLACEMENT_3D('',#81749,#56013,#56014);
#48021=AXIS2_PLACEMENT_3D('',#81759,#56015,#56016);
#48022=AXIS2_PLACEMENT_3D('',#81779,#56018,#56019);
#48023=AXIS2_PLACEMENT_3D('',#81787,#56021,#56022);
#48024=AXIS2_PLACEMENT_3D('',#81790,#56023,#56024);
#48025=AXIS2_PLACEMENT_3D('',#81791,#56025,#56026);
#48026=AXIS2_PLACEMENT_3D('',#81792,#56027,#56028);
#48027=AXIS2_PLACEMENT_3D('',#81801,#56029,#56030);
#48028=AXIS2_PLACEMENT_3D('',#81802,#56031,#56032);
#48029=AXIS2_PLACEMENT_3D('',#81806,#56034,#56035);
#48030=AXIS2_PLACEMENT_3D('',#81808,#56036,#56037);
#48031=AXIS2_PLACEMENT_3D('',#81833,#56040,#56041);
#48032=AXIS2_PLACEMENT_3D('',#81834,#56042,#56043);
#48033=AXIS2_PLACEMENT_3D('',#81853,#56044,#56045);
#48034=AXIS2_PLACEMENT_3D('',#81861,#56047,#56048);
#48035=AXIS2_PLACEMENT_3D('',#81864,#56049,#56050);
#48036=AXIS2_PLACEMENT_3D('',#81865,#56051,#56052);
#48037=AXIS2_PLACEMENT_3D('',#81866,#56053,#56054);
#48038=AXIS2_PLACEMENT_3D('',#81878,#56055,#56056);
#48039=AXIS2_PLACEMENT_3D('',#81879,#56057,#56058);
#48040=AXIS2_PLACEMENT_3D('',#81883,#56060,#56061);
#48041=AXIS2_PLACEMENT_3D('',#81885,#56062,#56063);
#48042=AXIS2_PLACEMENT_3D('',#81921,#56066,#56067);
#48043=AXIS2_PLACEMENT_3D('',#81929,#56069,#56070);
#48044=AXIS2_PLACEMENT_3D('',#81932,#56071,#56072);
#48045=AXIS2_PLACEMENT_3D('',#81933,#56073,#56074);
#48046=AXIS2_PLACEMENT_3D('',#81934,#56075,#56076);
#48047=AXIS2_PLACEMENT_3D('',#81969,#56078,#56079);
#48048=AXIS2_PLACEMENT_3D('',#81971,#56080,#56081);
#48049=AXIS2_PLACEMENT_3D('',#82021,#56085,#56086);
#48050=AXIS2_PLACEMENT_3D('',#82024,#56087,#56088);
#48051=AXIS2_PLACEMENT_3D('',#82031,#56089,#56090);
#48052=AXIS2_PLACEMENT_3D('',#82043,#56091,#56092);
#48053=AXIS2_PLACEMENT_3D('',#82044,#56093,#56094);
#48054=AXIS2_PLACEMENT_3D('',#82048,#56096,#56097);
#48055=AXIS2_PLACEMENT_3D('',#82050,#56098,#56099);
#48056=AXIS2_PLACEMENT_3D('',#82086,#56102,#56103);
#48057=AXIS2_PLACEMENT_3D('',#82094,#56105,#56106);
#48058=AXIS2_PLACEMENT_3D('',#82097,#56107,#56108);
#48059=AXIS2_PLACEMENT_3D('',#82098,#56109,#56110);
#48060=AXIS2_PLACEMENT_3D('',#82099,#56111,#56112);
#48061=AXIS2_PLACEMENT_3D('',#82118,#56113,#56114);
#48062=AXIS2_PLACEMENT_3D('',#82119,#56115,#56116);
#48063=AXIS2_PLACEMENT_3D('',#82123,#56118,#56119);
#48064=AXIS2_PLACEMENT_3D('',#82125,#56120,#56121);
#48065=AXIS2_PLACEMENT_3D('',#82161,#56124,#56125);
#48066=AXIS2_PLACEMENT_3D('',#82169,#56127,#56128);
#48067=AXIS2_PLACEMENT_3D('',#82172,#56129,#56130);
#48068=AXIS2_PLACEMENT_3D('',#82173,#56131,#56132);
#48069=AXIS2_PLACEMENT_3D('',#82174,#56133,#56134);
#48070=AXIS2_PLACEMENT_3D('',#82189,#56135,#56136);
#48071=AXIS2_PLACEMENT_3D('',#82190,#56137,#56138);
#48072=AXIS2_PLACEMENT_3D('',#82194,#56140,#56141);
#48073=AXIS2_PLACEMENT_3D('',#82196,#56142,#56143);
#48074=AXIS2_PLACEMENT_3D('',#82230,#56146,#56147);
#48075=AXIS2_PLACEMENT_3D('',#82232,#56149,#56150);
#48076=AXIS2_PLACEMENT_3D('',#82233,#56151,#56152);
#48077=AXIS2_PLACEMENT_3D('',#82236,#56154,#56155);
#48078=AXIS2_PLACEMENT_3D('',#82237,#56156,#56157);
#48079=AXIS2_PLACEMENT_3D('',#82238,#56158,#56159);
#48080=AXIS2_PLACEMENT_3D('',#82257,#56160,#56161);
#48081=AXIS2_PLACEMENT_3D('',#82258,#56162,#56163);
#48082=AXIS2_PLACEMENT_3D('',#82268,#56164,#56165);
#48083=AXIS2_PLACEMENT_3D('',#82288,#56167,#56168);
#48084=AXIS2_PLACEMENT_3D('',#82296,#56170,#56171);
#48085=AXIS2_PLACEMENT_3D('',#82299,#56172,#56173);
#48086=AXIS2_PLACEMENT_3D('',#82300,#56174,#56175);
#48087=AXIS2_PLACEMENT_3D('',#82301,#56176,#56177);
#48088=AXIS2_PLACEMENT_3D('',#82310,#56178,#56179);
#48089=AXIS2_PLACEMENT_3D('',#82311,#56180,#56181);
#48090=AXIS2_PLACEMENT_3D('',#82315,#56183,#56184);
#48091=AXIS2_PLACEMENT_3D('',#82317,#56185,#56186);
#48092=AXIS2_PLACEMENT_3D('',#82342,#56189,#56190);
#48093=AXIS2_PLACEMENT_3D('',#82343,#56191,#56192);
#48094=AXIS2_PLACEMENT_3D('',#82362,#56193,#56194);
#48095=AXIS2_PLACEMENT_3D('',#82370,#56196,#56197);
#48096=AXIS2_PLACEMENT_3D('',#82373,#56198,#56199);
#48097=AXIS2_PLACEMENT_3D('',#82374,#56200,#56201);
#48098=AXIS2_PLACEMENT_3D('',#82375,#56202,#56203);
#48099=AXIS2_PLACEMENT_3D('',#82387,#56204,#56205);
#48100=AXIS2_PLACEMENT_3D('',#82388,#56206,#56207);
#48101=AXIS2_PLACEMENT_3D('',#82392,#56209,#56210);
#48102=AXIS2_PLACEMENT_3D('',#82394,#56211,#56212);
#48103=AXIS2_PLACEMENT_3D('',#82430,#56215,#56216);
#48104=AXIS2_PLACEMENT_3D('',#82438,#56218,#56219);
#48105=AXIS2_PLACEMENT_3D('',#82441,#56220,#56221);
#48106=AXIS2_PLACEMENT_3D('',#82442,#56222,#56223);
#48107=AXIS2_PLACEMENT_3D('',#82443,#56224,#56225);
#48108=AXIS2_PLACEMENT_3D('',#82479,#56227,#56228);
#48109=AXIS2_PLACEMENT_3D('',#82481,#56229,#56230);
#48110=AXIS2_PLACEMENT_3D('',#82536,#56234,#56235);
#48111=AXIS2_PLACEMENT_3D('',#82539,#56236,#56237);
#48112=AXIS2_PLACEMENT_3D('',#82546,#56238,#56239);
#48113=AXIS2_PLACEMENT_3D('',#82555,#56240,#56241);
#48114=AXIS2_PLACEMENT_3D('',#82556,#56242,#56243);
#48115=AXIS2_PLACEMENT_3D('',#82560,#56245,#56246);
#48116=AXIS2_PLACEMENT_3D('',#82562,#56247,#56248);
#48117=AXIS2_PLACEMENT_3D('',#82605,#56251,#56252);
#48118=AXIS2_PLACEMENT_3D('',#82613,#56254,#56255);
#48119=AXIS2_PLACEMENT_3D('',#82616,#56256,#56257);
#48120=AXIS2_PLACEMENT_3D('',#82617,#56258,#56259);
#48121=AXIS2_PLACEMENT_3D('',#82618,#56260,#56261);
#48122=AXIS2_PLACEMENT_3D('',#82637,#56262,#56263);
#48123=AXIS2_PLACEMENT_3D('',#82638,#56264,#56265);
#48124=AXIS2_PLACEMENT_3D('',#82642,#56267,#56268);
#48125=AXIS2_PLACEMENT_3D('',#82644,#56269,#56270);
#48126=AXIS2_PLACEMENT_3D('',#82680,#56273,#56274);
#48127=AXIS2_PLACEMENT_3D('',#82688,#56276,#56277);
#48128=AXIS2_PLACEMENT_3D('',#82691,#56278,#56279);
#48129=AXIS2_PLACEMENT_3D('',#82692,#56280,#56281);
#48130=AXIS2_PLACEMENT_3D('',#82693,#56282,#56283);
#48131=AXIS2_PLACEMENT_3D('',#82708,#56284,#56285);
#48132=AXIS2_PLACEMENT_3D('',#82709,#56286,#56287);
#48133=AXIS2_PLACEMENT_3D('',#82713,#56289,#56290);
#48134=AXIS2_PLACEMENT_3D('',#82715,#56291,#56292);
#48135=AXIS2_PLACEMENT_3D('',#82749,#56295,#56296);
#48136=AXIS2_PLACEMENT_3D('',#82751,#56298,#56299);
#48137=AXIS2_PLACEMENT_3D('',#82752,#56300,#56301);
#48138=AXIS2_PLACEMENT_3D('',#82755,#56303,#56304);
#48139=AXIS2_PLACEMENT_3D('',#82756,#56305,#56306);
#48140=AXIS2_PLACEMENT_3D('',#82757,#56307,#56308);
#48141=AXIS2_PLACEMENT_3D('',#82776,#56309,#56310);
#48142=AXIS2_PLACEMENT_3D('',#82777,#56311,#56312);
#48143=AXIS2_PLACEMENT_3D('',#82787,#56313,#56314);
#48144=AXIS2_PLACEMENT_3D('',#82807,#56316,#56317);
#48145=AXIS2_PLACEMENT_3D('',#82815,#56319,#56320);
#48146=AXIS2_PLACEMENT_3D('',#82818,#56321,#56322);
#48147=AXIS2_PLACEMENT_3D('',#82819,#56323,#56324);
#48148=AXIS2_PLACEMENT_3D('',#82820,#56325,#56326);
#48149=AXIS2_PLACEMENT_3D('',#82829,#56327,#56328);
#48150=AXIS2_PLACEMENT_3D('',#82830,#56329,#56330);
#48151=AXIS2_PLACEMENT_3D('',#82834,#56332,#56333);
#48152=AXIS2_PLACEMENT_3D('',#82836,#56334,#56335);
#48153=AXIS2_PLACEMENT_3D('',#82861,#56338,#56339);
#48154=AXIS2_PLACEMENT_3D('',#82862,#56340,#56341);
#48155=AXIS2_PLACEMENT_3D('',#82881,#56342,#56343);
#48156=AXIS2_PLACEMENT_3D('',#82889,#56345,#56346);
#48157=AXIS2_PLACEMENT_3D('',#82892,#56347,#56348);
#48158=AXIS2_PLACEMENT_3D('',#82893,#56349,#56350);
#48159=AXIS2_PLACEMENT_3D('',#82894,#56351,#56352);
#48160=AXIS2_PLACEMENT_3D('',#82906,#56353,#56354);
#48161=AXIS2_PLACEMENT_3D('',#82907,#56355,#56356);
#48162=AXIS2_PLACEMENT_3D('',#82911,#56358,#56359);
#48163=AXIS2_PLACEMENT_3D('',#82913,#56360,#56361);
#48164=AXIS2_PLACEMENT_3D('',#82949,#56364,#56365);
#48165=AXIS2_PLACEMENT_3D('',#82957,#56367,#56368);
#48166=AXIS2_PLACEMENT_3D('',#82960,#56369,#56370);
#48167=AXIS2_PLACEMENT_3D('',#82961,#56371,#56372);
#48168=AXIS2_PLACEMENT_3D('',#82962,#56373,#56374);
#48169=AXIS2_PLACEMENT_3D('',#82998,#56376,#56377);
#48170=AXIS2_PLACEMENT_3D('',#83000,#56378,#56379);
#48171=AXIS2_PLACEMENT_3D('',#83055,#56383,#56384);
#48172=AXIS2_PLACEMENT_3D('',#83058,#56385,#56386);
#48173=AXIS2_PLACEMENT_3D('',#83065,#56387,#56388);
#48174=AXIS2_PLACEMENT_3D('',#83077,#56389,#56390);
#48175=AXIS2_PLACEMENT_3D('',#83078,#56391,#56392);
#48176=AXIS2_PLACEMENT_3D('',#83082,#56394,#56395);
#48177=AXIS2_PLACEMENT_3D('',#83084,#56396,#56397);
#48178=AXIS2_PLACEMENT_3D('',#83120,#56400,#56401);
#48179=AXIS2_PLACEMENT_3D('',#83128,#56403,#56404);
#48180=AXIS2_PLACEMENT_3D('',#83131,#56405,#56406);
#48181=AXIS2_PLACEMENT_3D('',#83132,#56407,#56408);
#48182=AXIS2_PLACEMENT_3D('',#83133,#56409,#56410);
#48183=AXIS2_PLACEMENT_3D('',#83152,#56411,#56412);
#48184=AXIS2_PLACEMENT_3D('',#83153,#56413,#56414);
#48185=AXIS2_PLACEMENT_3D('',#83157,#56416,#56417);
#48186=AXIS2_PLACEMENT_3D('',#83159,#56418,#56419);
#48187=AXIS2_PLACEMENT_3D('',#83202,#56422,#56423);
#48188=AXIS2_PLACEMENT_3D('',#83210,#56425,#56426);
#48189=AXIS2_PLACEMENT_3D('',#83213,#56427,#56428);
#48190=AXIS2_PLACEMENT_3D('',#83214,#56429,#56430);
#48191=AXIS2_PLACEMENT_3D('',#83215,#56431,#56432);
#48192=AXIS2_PLACEMENT_3D('',#83230,#56433,#56434);
#48193=AXIS2_PLACEMENT_3D('',#83231,#56435,#56436);
#48194=AXIS2_PLACEMENT_3D('',#83235,#56438,#56439);
#48195=AXIS2_PLACEMENT_3D('',#83237,#56440,#56441);
#48196=AXIS2_PLACEMENT_3D('',#83271,#56444,#56445);
#48197=AXIS2_PLACEMENT_3D('',#83273,#56447,#56448);
#48198=AXIS2_PLACEMENT_3D('',#83274,#56449,#56450);
#48199=AXIS2_PLACEMENT_3D('',#83277,#56452,#56453);
#48200=AXIS2_PLACEMENT_3D('',#83278,#56454,#56455);
#48201=AXIS2_PLACEMENT_3D('',#83279,#56456,#56457);
#48202=AXIS2_PLACEMENT_3D('',#83298,#56458,#56459);
#48203=AXIS2_PLACEMENT_3D('',#83299,#56460,#56461);
#48204=AXIS2_PLACEMENT_3D('',#83309,#56462,#56463);
#48205=AXIS2_PLACEMENT_3D('',#83329,#56465,#56466);
#48206=AXIS2_PLACEMENT_3D('',#83337,#56468,#56469);
#48207=AXIS2_PLACEMENT_3D('',#83340,#56470,#56471);
#48208=AXIS2_PLACEMENT_3D('',#83341,#56472,#56473);
#48209=AXIS2_PLACEMENT_3D('',#83342,#56474,#56475);
#48210=AXIS2_PLACEMENT_3D('',#83351,#56476,#56477);
#48211=AXIS2_PLACEMENT_3D('',#83352,#56478,#56479);
#48212=AXIS2_PLACEMENT_3D('',#83356,#56481,#56482);
#48213=AXIS2_PLACEMENT_3D('',#83358,#56483,#56484);
#48214=AXIS2_PLACEMENT_3D('',#83383,#56487,#56488);
#48215=AXIS2_PLACEMENT_3D('',#83384,#56489,#56490);
#48216=AXIS2_PLACEMENT_3D('',#83403,#56491,#56492);
#48217=AXIS2_PLACEMENT_3D('',#83411,#56494,#56495);
#48218=AXIS2_PLACEMENT_3D('',#83414,#56496,#56497);
#48219=AXIS2_PLACEMENT_3D('',#83415,#56498,#56499);
#48220=AXIS2_PLACEMENT_3D('',#83416,#56500,#56501);
#48221=AXIS2_PLACEMENT_3D('',#83428,#56502,#56503);
#48222=AXIS2_PLACEMENT_3D('',#83429,#56504,#56505);
#48223=AXIS2_PLACEMENT_3D('',#83433,#56507,#56508);
#48224=AXIS2_PLACEMENT_3D('',#83435,#56509,#56510);
#48225=AXIS2_PLACEMENT_3D('',#83471,#56513,#56514);
#48226=AXIS2_PLACEMENT_3D('',#83479,#56516,#56517);
#48227=AXIS2_PLACEMENT_3D('',#83482,#56518,#56519);
#48228=AXIS2_PLACEMENT_3D('',#83483,#56520,#56521);
#48229=AXIS2_PLACEMENT_3D('',#83484,#56522,#56523);
#48230=AXIS2_PLACEMENT_3D('',#83520,#56525,#56526);
#48231=AXIS2_PLACEMENT_3D('',#83522,#56527,#56528);
#48232=AXIS2_PLACEMENT_3D('',#83577,#56532,#56533);
#48233=AXIS2_PLACEMENT_3D('',#83580,#56534,#56535);
#48234=AXIS2_PLACEMENT_3D('',#83587,#56536,#56537);
#48235=AXIS2_PLACEMENT_3D('',#83599,#56538,#56539);
#48236=AXIS2_PLACEMENT_3D('',#83600,#56540,#56541);
#48237=AXIS2_PLACEMENT_3D('',#83604,#56543,#56544);
#48238=AXIS2_PLACEMENT_3D('',#83606,#56545,#56546);
#48239=AXIS2_PLACEMENT_3D('',#83642,#56549,#56550);
#48240=AXIS2_PLACEMENT_3D('',#83650,#56552,#56553);
#48241=AXIS2_PLACEMENT_3D('',#83653,#56554,#56555);
#48242=AXIS2_PLACEMENT_3D('',#83654,#56556,#56557);
#48243=AXIS2_PLACEMENT_3D('',#83655,#56558,#56559);
#48244=AXIS2_PLACEMENT_3D('',#83674,#56560,#56561);
#48245=AXIS2_PLACEMENT_3D('',#83675,#56562,#56563);
#48246=AXIS2_PLACEMENT_3D('',#83679,#56565,#56566);
#48247=AXIS2_PLACEMENT_3D('',#83681,#56567,#56568);
#48248=AXIS2_PLACEMENT_3D('',#83717,#56571,#56572);
#48249=AXIS2_PLACEMENT_3D('',#83725,#56574,#56575);
#48250=AXIS2_PLACEMENT_3D('',#83728,#56576,#56577);
#48251=AXIS2_PLACEMENT_3D('',#83729,#56578,#56579);
#48252=AXIS2_PLACEMENT_3D('',#83730,#56580,#56581);
#48253=AXIS2_PLACEMENT_3D('',#83742,#56582,#56583);
#48254=AXIS2_PLACEMENT_3D('',#83743,#56584,#56585);
#48255=AXIS2_PLACEMENT_3D('',#83747,#56587,#56588);
#48256=AXIS2_PLACEMENT_3D('',#83749,#56589,#56590);
#48257=AXIS2_PLACEMENT_3D('',#83790,#56593,#56594);
#48258=AXIS2_PLACEMENT_3D('',#83792,#56596,#56597);
#48259=AXIS2_PLACEMENT_3D('',#83793,#56598,#56599);
#48260=AXIS2_PLACEMENT_3D('',#83796,#56601,#56602);
#48261=AXIS2_PLACEMENT_3D('',#83797,#56603,#56604);
#48262=AXIS2_PLACEMENT_3D('',#83798,#56605,#56606);
#48263=AXIS2_PLACEMENT_3D('',#83817,#56607,#56608);
#48264=AXIS2_PLACEMENT_3D('',#83818,#56609,#56610);
#48265=AXIS2_PLACEMENT_3D('',#83828,#56611,#56612);
#48266=AXIS2_PLACEMENT_3D('',#83848,#56614,#56615);
#48267=AXIS2_PLACEMENT_3D('',#83856,#56617,#56618);
#48268=AXIS2_PLACEMENT_3D('',#83859,#56619,#56620);
#48269=AXIS2_PLACEMENT_3D('',#83860,#56621,#56622);
#48270=AXIS2_PLACEMENT_3D('',#83861,#56623,#56624);
#48271=AXIS2_PLACEMENT_3D('',#83870,#56625,#56626);
#48272=AXIS2_PLACEMENT_3D('',#83871,#56627,#56628);
#48273=AXIS2_PLACEMENT_3D('',#83875,#56630,#56631);
#48274=AXIS2_PLACEMENT_3D('',#83877,#56632,#56633);
#48275=AXIS2_PLACEMENT_3D('',#83902,#56636,#56637);
#48276=AXIS2_PLACEMENT_3D('',#83903,#56638,#56639);
#48277=AXIS2_PLACEMENT_3D('',#83922,#56640,#56641);
#48278=AXIS2_PLACEMENT_3D('',#83930,#56643,#56644);
#48279=AXIS2_PLACEMENT_3D('',#83933,#56645,#56646);
#48280=AXIS2_PLACEMENT_3D('',#83934,#56647,#56648);
#48281=AXIS2_PLACEMENT_3D('',#83935,#56649,#56650);
#48282=AXIS2_PLACEMENT_3D('',#83947,#56651,#56652);
#48283=AXIS2_PLACEMENT_3D('',#83948,#56653,#56654);
#48284=AXIS2_PLACEMENT_3D('',#83952,#56656,#56657);
#48285=AXIS2_PLACEMENT_3D('',#83954,#56658,#56659);
#48286=AXIS2_PLACEMENT_3D('',#83990,#56662,#56663);
#48287=AXIS2_PLACEMENT_3D('',#83998,#56665,#56666);
#48288=AXIS2_PLACEMENT_3D('',#84001,#56667,#56668);
#48289=AXIS2_PLACEMENT_3D('',#84002,#56669,#56670);
#48290=AXIS2_PLACEMENT_3D('',#84003,#56671,#56672);
#48291=AXIS2_PLACEMENT_3D('',#84039,#56674,#56675);
#48292=AXIS2_PLACEMENT_3D('',#84041,#56676,#56677);
#48293=AXIS2_PLACEMENT_3D('',#84096,#56681,#56682);
#48294=AXIS2_PLACEMENT_3D('',#84099,#56683,#56684);
#48295=AXIS2_PLACEMENT_3D('',#84106,#56685,#56686);
#48296=AXIS2_PLACEMENT_3D('',#84118,#56687,#56688);
#48297=AXIS2_PLACEMENT_3D('',#84119,#56689,#56690);
#48298=AXIS2_PLACEMENT_3D('',#84123,#56692,#56693);
#48299=AXIS2_PLACEMENT_3D('',#84125,#56694,#56695);
#48300=AXIS2_PLACEMENT_3D('',#84161,#56698,#56699);
#48301=AXIS2_PLACEMENT_3D('',#84169,#56701,#56702);
#48302=AXIS2_PLACEMENT_3D('',#84172,#56703,#56704);
#48303=AXIS2_PLACEMENT_3D('',#84173,#56705,#56706);
#48304=AXIS2_PLACEMENT_3D('',#84174,#56707,#56708);
#48305=AXIS2_PLACEMENT_3D('',#84193,#56709,#56710);
#48306=AXIS2_PLACEMENT_3D('',#84194,#56711,#56712);
#48307=AXIS2_PLACEMENT_3D('',#84198,#56714,#56715);
#48308=AXIS2_PLACEMENT_3D('',#84200,#56716,#56717);
#48309=AXIS2_PLACEMENT_3D('',#84236,#56720,#56721);
#48310=AXIS2_PLACEMENT_3D('',#84244,#56723,#56724);
#48311=AXIS2_PLACEMENT_3D('',#84247,#56725,#56726);
#48312=AXIS2_PLACEMENT_3D('',#84248,#56727,#56728);
#48313=AXIS2_PLACEMENT_3D('',#84249,#56729,#56730);
#48314=AXIS2_PLACEMENT_3D('',#84264,#56731,#56732);
#48315=AXIS2_PLACEMENT_3D('',#84265,#56733,#56734);
#48316=AXIS2_PLACEMENT_3D('',#84269,#56736,#56737);
#48317=AXIS2_PLACEMENT_3D('',#84271,#56738,#56739);
#48318=AXIS2_PLACEMENT_3D('',#84305,#56742,#56743);
#48319=AXIS2_PLACEMENT_3D('',#84307,#56745,#56746);
#48320=AXIS2_PLACEMENT_3D('',#84308,#56747,#56748);
#48321=AXIS2_PLACEMENT_3D('',#84311,#56750,#56751);
#48322=AXIS2_PLACEMENT_3D('',#84312,#56752,#56753);
#48323=AXIS2_PLACEMENT_3D('',#84313,#56754,#56755);
#48324=AXIS2_PLACEMENT_3D('',#84332,#56756,#56757);
#48325=AXIS2_PLACEMENT_3D('',#84333,#56758,#56759);
#48326=AXIS2_PLACEMENT_3D('',#84343,#56760,#56761);
#48327=AXIS2_PLACEMENT_3D('',#84363,#56763,#56764);
#48328=AXIS2_PLACEMENT_3D('',#84371,#56766,#56767);
#48329=AXIS2_PLACEMENT_3D('',#84374,#56768,#56769);
#48330=AXIS2_PLACEMENT_3D('',#84375,#56770,#56771);
#48331=AXIS2_PLACEMENT_3D('',#84376,#56772,#56773);
#48332=AXIS2_PLACEMENT_3D('',#84385,#56774,#56775);
#48333=AXIS2_PLACEMENT_3D('',#84386,#56776,#56777);
#48334=AXIS2_PLACEMENT_3D('',#84390,#56779,#56780);
#48335=AXIS2_PLACEMENT_3D('',#84392,#56781,#56782);
#48336=AXIS2_PLACEMENT_3D('',#84417,#56785,#56786);
#48337=AXIS2_PLACEMENT_3D('',#84418,#56787,#56788);
#48338=AXIS2_PLACEMENT_3D('',#84437,#56789,#56790);
#48339=AXIS2_PLACEMENT_3D('',#84445,#56792,#56793);
#48340=AXIS2_PLACEMENT_3D('',#84448,#56794,#56795);
#48341=AXIS2_PLACEMENT_3D('',#84449,#56796,#56797);
#48342=AXIS2_PLACEMENT_3D('',#84450,#56798,#56799);
#48343=AXIS2_PLACEMENT_3D('',#84462,#56800,#56801);
#48344=AXIS2_PLACEMENT_3D('',#84463,#56802,#56803);
#48345=AXIS2_PLACEMENT_3D('',#84467,#56805,#56806);
#48346=AXIS2_PLACEMENT_3D('',#84469,#56807,#56808);
#48347=AXIS2_PLACEMENT_3D('',#84505,#56811,#56812);
#48348=AXIS2_PLACEMENT_3D('',#84513,#56814,#56815);
#48349=AXIS2_PLACEMENT_3D('',#84516,#56816,#56817);
#48350=AXIS2_PLACEMENT_3D('',#84517,#56818,#56819);
#48351=AXIS2_PLACEMENT_3D('',#84518,#56820,#56821);
#48352=AXIS2_PLACEMENT_3D('',#84554,#56823,#56824);
#48353=AXIS2_PLACEMENT_3D('',#84556,#56825,#56826);
#48354=AXIS2_PLACEMENT_3D('',#84611,#56830,#56831);
#48355=AXIS2_PLACEMENT_3D('',#84614,#56832,#56833);
#48356=AXIS2_PLACEMENT_3D('',#84621,#56834,#56835);
#48357=AXIS2_PLACEMENT_3D('',#84633,#56836,#56837);
#48358=AXIS2_PLACEMENT_3D('',#84634,#56838,#56839);
#48359=AXIS2_PLACEMENT_3D('',#84638,#56841,#56842);
#48360=AXIS2_PLACEMENT_3D('',#84640,#56843,#56844);
#48361=AXIS2_PLACEMENT_3D('',#84676,#56847,#56848);
#48362=AXIS2_PLACEMENT_3D('',#84684,#56850,#56851);
#48363=AXIS2_PLACEMENT_3D('',#84687,#56852,#56853);
#48364=AXIS2_PLACEMENT_3D('',#84688,#56854,#56855);
#48365=AXIS2_PLACEMENT_3D('',#84689,#56856,#56857);
#48366=AXIS2_PLACEMENT_3D('',#84708,#56858,#56859);
#48367=AXIS2_PLACEMENT_3D('',#84709,#56860,#56861);
#48368=AXIS2_PLACEMENT_3D('',#84713,#56863,#56864);
#48369=AXIS2_PLACEMENT_3D('',#84715,#56865,#56866);
#48370=AXIS2_PLACEMENT_3D('',#84751,#56869,#56870);
#48371=AXIS2_PLACEMENT_3D('',#84759,#56872,#56873);
#48372=AXIS2_PLACEMENT_3D('',#84762,#56874,#56875);
#48373=AXIS2_PLACEMENT_3D('',#84763,#56876,#56877);
#48374=AXIS2_PLACEMENT_3D('',#84764,#56878,#56879);
#48375=AXIS2_PLACEMENT_3D('',#84779,#56880,#56881);
#48376=AXIS2_PLACEMENT_3D('',#84780,#56882,#56883);
#48377=AXIS2_PLACEMENT_3D('',#84784,#56885,#56886);
#48378=AXIS2_PLACEMENT_3D('',#84786,#56887,#56888);
#48379=AXIS2_PLACEMENT_3D('',#84820,#56891,#56892);
#48380=AXIS2_PLACEMENT_3D('',#84822,#56894,#56895);
#48381=AXIS2_PLACEMENT_3D('',#84823,#56896,#56897);
#48382=AXIS2_PLACEMENT_3D('',#84826,#56899,#56900);
#48383=AXIS2_PLACEMENT_3D('',#84827,#56901,#56902);
#48384=AXIS2_PLACEMENT_3D('',#84828,#56903,#56904);
#48385=AXIS2_PLACEMENT_3D('',#84847,#56905,#56906);
#48386=AXIS2_PLACEMENT_3D('',#84848,#56907,#56908);
#48387=AXIS2_PLACEMENT_3D('',#84858,#56909,#56910);
#48388=AXIS2_PLACEMENT_3D('',#84878,#56912,#56913);
#48389=AXIS2_PLACEMENT_3D('',#84886,#56915,#56916);
#48390=AXIS2_PLACEMENT_3D('',#84889,#56917,#56918);
#48391=AXIS2_PLACEMENT_3D('',#84890,#56919,#56920);
#48392=AXIS2_PLACEMENT_3D('',#84891,#56921,#56922);
#48393=AXIS2_PLACEMENT_3D('',#84900,#56923,#56924);
#48394=AXIS2_PLACEMENT_3D('',#84901,#56925,#56926);
#48395=AXIS2_PLACEMENT_3D('',#84905,#56928,#56929);
#48396=AXIS2_PLACEMENT_3D('',#84907,#56930,#56931);
#48397=AXIS2_PLACEMENT_3D('',#84932,#56934,#56935);
#48398=AXIS2_PLACEMENT_3D('',#84933,#56936,#56937);
#48399=AXIS2_PLACEMENT_3D('',#84952,#56938,#56939);
#48400=AXIS2_PLACEMENT_3D('',#84960,#56941,#56942);
#48401=AXIS2_PLACEMENT_3D('',#84963,#56943,#56944);
#48402=AXIS2_PLACEMENT_3D('',#84964,#56945,#56946);
#48403=AXIS2_PLACEMENT_3D('',#84965,#56947,#56948);
#48404=AXIS2_PLACEMENT_3D('',#84977,#56949,#56950);
#48405=AXIS2_PLACEMENT_3D('',#84978,#56951,#56952);
#48406=AXIS2_PLACEMENT_3D('',#84982,#56954,#56955);
#48407=AXIS2_PLACEMENT_3D('',#84984,#56956,#56957);
#48408=AXIS2_PLACEMENT_3D('',#85020,#56960,#56961);
#48409=AXIS2_PLACEMENT_3D('',#85028,#56963,#56964);
#48410=AXIS2_PLACEMENT_3D('',#85031,#56965,#56966);
#48411=AXIS2_PLACEMENT_3D('',#85032,#56967,#56968);
#48412=AXIS2_PLACEMENT_3D('',#85033,#56969,#56970);
#48413=AXIS2_PLACEMENT_3D('',#85069,#56972,#56973);
#48414=AXIS2_PLACEMENT_3D('',#85071,#56974,#56975);
#48415=AXIS2_PLACEMENT_3D('',#85126,#56979,#56980);
#48416=AXIS2_PLACEMENT_3D('',#85129,#56981,#56982);
#48417=AXIS2_PLACEMENT_3D('',#85136,#56983,#56984);
#48418=AXIS2_PLACEMENT_3D('',#85148,#56985,#56986);
#48419=AXIS2_PLACEMENT_3D('',#85149,#56987,#56988);
#48420=AXIS2_PLACEMENT_3D('',#85153,#56990,#56991);
#48421=AXIS2_PLACEMENT_3D('',#85155,#56992,#56993);
#48422=AXIS2_PLACEMENT_3D('',#85191,#56996,#56997);
#48423=AXIS2_PLACEMENT_3D('',#85199,#56999,#57000);
#48424=AXIS2_PLACEMENT_3D('',#85202,#57001,#57002);
#48425=AXIS2_PLACEMENT_3D('',#85203,#57003,#57004);
#48426=AXIS2_PLACEMENT_3D('',#85204,#57005,#57006);
#48427=AXIS2_PLACEMENT_3D('',#85223,#57007,#57008);
#48428=AXIS2_PLACEMENT_3D('',#85224,#57009,#57010);
#48429=AXIS2_PLACEMENT_3D('',#85228,#57012,#57013);
#48430=AXIS2_PLACEMENT_3D('',#85230,#57014,#57015);
#48431=AXIS2_PLACEMENT_3D('',#85266,#57018,#57019);
#48432=AXIS2_PLACEMENT_3D('',#85274,#57021,#57022);
#48433=AXIS2_PLACEMENT_3D('',#85277,#57023,#57024);
#48434=AXIS2_PLACEMENT_3D('',#85278,#57025,#57026);
#48435=AXIS2_PLACEMENT_3D('',#85279,#57027,#57028);
#48436=AXIS2_PLACEMENT_3D('',#85294,#57029,#57030);
#48437=AXIS2_PLACEMENT_3D('',#85295,#57031,#57032);
#48438=AXIS2_PLACEMENT_3D('',#85299,#57034,#57035);
#48439=AXIS2_PLACEMENT_3D('',#85301,#57036,#57037);
#48440=AXIS2_PLACEMENT_3D('',#85335,#57040,#57041);
#48441=AXIS2_PLACEMENT_3D('',#85337,#57043,#57044);
#48442=AXIS2_PLACEMENT_3D('',#85338,#57045,#57046);
#48443=AXIS2_PLACEMENT_3D('',#85341,#57048,#57049);
#48444=AXIS2_PLACEMENT_3D('',#85342,#57050,#57051);
#48445=AXIS2_PLACEMENT_3D('',#85343,#57052,#57053);
#48446=AXIS2_PLACEMENT_3D('',#85362,#57054,#57055);
#48447=AXIS2_PLACEMENT_3D('',#85363,#57056,#57057);
#48448=AXIS2_PLACEMENT_3D('',#85373,#57058,#57059);
#48449=AXIS2_PLACEMENT_3D('',#85393,#57061,#57062);
#48450=AXIS2_PLACEMENT_3D('',#85401,#57064,#57065);
#48451=AXIS2_PLACEMENT_3D('',#85404,#57066,#57067);
#48452=AXIS2_PLACEMENT_3D('',#85405,#57068,#57069);
#48453=AXIS2_PLACEMENT_3D('',#85406,#57070,#57071);
#48454=AXIS2_PLACEMENT_3D('',#85415,#57072,#57073);
#48455=AXIS2_PLACEMENT_3D('',#85416,#57074,#57075);
#48456=AXIS2_PLACEMENT_3D('',#85420,#57077,#57078);
#48457=AXIS2_PLACEMENT_3D('',#85422,#57079,#57080);
#48458=AXIS2_PLACEMENT_3D('',#85447,#57083,#57084);
#48459=AXIS2_PLACEMENT_3D('',#85448,#57085,#57086);
#48460=AXIS2_PLACEMENT_3D('',#85467,#57087,#57088);
#48461=AXIS2_PLACEMENT_3D('',#85475,#57090,#57091);
#48462=AXIS2_PLACEMENT_3D('',#85478,#57092,#57093);
#48463=AXIS2_PLACEMENT_3D('',#85479,#57094,#57095);
#48464=AXIS2_PLACEMENT_3D('',#85480,#57096,#57097);
#48465=AXIS2_PLACEMENT_3D('',#85492,#57098,#57099);
#48466=AXIS2_PLACEMENT_3D('',#85493,#57100,#57101);
#48467=AXIS2_PLACEMENT_3D('',#85497,#57103,#57104);
#48468=AXIS2_PLACEMENT_3D('',#85499,#57105,#57106);
#48469=AXIS2_PLACEMENT_3D('',#85535,#57109,#57110);
#48470=AXIS2_PLACEMENT_3D('',#85543,#57112,#57113);
#48471=AXIS2_PLACEMENT_3D('',#85546,#57114,#57115);
#48472=AXIS2_PLACEMENT_3D('',#85547,#57116,#57117);
#48473=AXIS2_PLACEMENT_3D('',#85548,#57118,#57119);
#48474=AXIS2_PLACEMENT_3D('',#85584,#57121,#57122);
#48475=AXIS2_PLACEMENT_3D('',#85586,#57123,#57124);
#48476=AXIS2_PLACEMENT_3D('',#85641,#57128,#57129);
#48477=AXIS2_PLACEMENT_3D('',#85644,#57130,#57131);
#48478=AXIS2_PLACEMENT_3D('',#85651,#57132,#57133);
#48479=AXIS2_PLACEMENT_3D('',#85663,#57134,#57135);
#48480=AXIS2_PLACEMENT_3D('',#85664,#57136,#57137);
#48481=AXIS2_PLACEMENT_3D('',#85668,#57139,#57140);
#48482=AXIS2_PLACEMENT_3D('',#85670,#57141,#57142);
#48483=AXIS2_PLACEMENT_3D('',#85706,#57145,#57146);
#48484=AXIS2_PLACEMENT_3D('',#85714,#57148,#57149);
#48485=AXIS2_PLACEMENT_3D('',#85717,#57150,#57151);
#48486=AXIS2_PLACEMENT_3D('',#85718,#57152,#57153);
#48487=AXIS2_PLACEMENT_3D('',#85719,#57154,#57155);
#48488=AXIS2_PLACEMENT_3D('',#85738,#57156,#57157);
#48489=AXIS2_PLACEMENT_3D('',#85739,#57158,#57159);
#48490=AXIS2_PLACEMENT_3D('',#85743,#57161,#57162);
#48491=AXIS2_PLACEMENT_3D('',#85745,#57163,#57164);
#48492=AXIS2_PLACEMENT_3D('',#85781,#57167,#57168);
#48493=AXIS2_PLACEMENT_3D('',#85789,#57170,#57171);
#48494=AXIS2_PLACEMENT_3D('',#85792,#57172,#57173);
#48495=AXIS2_PLACEMENT_3D('',#85793,#57174,#57175);
#48496=AXIS2_PLACEMENT_3D('',#85794,#57176,#57177);
#48497=AXIS2_PLACEMENT_3D('',#85809,#57178,#57179);
#48498=AXIS2_PLACEMENT_3D('',#85810,#57180,#57181);
#48499=AXIS2_PLACEMENT_3D('',#85814,#57183,#57184);
#48500=AXIS2_PLACEMENT_3D('',#85816,#57185,#57186);
#48501=AXIS2_PLACEMENT_3D('',#85850,#57189,#57190);
#48502=AXIS2_PLACEMENT_3D('',#85852,#57192,#57193);
#48503=AXIS2_PLACEMENT_3D('',#85853,#57194,#57195);
#48504=AXIS2_PLACEMENT_3D('',#85856,#57197,#57198);
#48505=AXIS2_PLACEMENT_3D('',#85857,#57199,#57200);
#48506=AXIS2_PLACEMENT_3D('',#85858,#57201,#57202);
#48507=AXIS2_PLACEMENT_3D('',#85877,#57203,#57204);
#48508=AXIS2_PLACEMENT_3D('',#85878,#57205,#57206);
#48509=AXIS2_PLACEMENT_3D('',#85888,#57207,#57208);
#48510=AXIS2_PLACEMENT_3D('',#85908,#57210,#57211);
#48511=AXIS2_PLACEMENT_3D('',#85916,#57213,#57214);
#48512=AXIS2_PLACEMENT_3D('',#85919,#57215,#57216);
#48513=AXIS2_PLACEMENT_3D('',#85920,#57217,#57218);
#48514=AXIS2_PLACEMENT_3D('',#85921,#57219,#57220);
#48515=AXIS2_PLACEMENT_3D('',#85930,#57221,#57222);
#48516=AXIS2_PLACEMENT_3D('',#85931,#57223,#57224);
#48517=AXIS2_PLACEMENT_3D('',#85935,#57226,#57227);
#48518=AXIS2_PLACEMENT_3D('',#85937,#57228,#57229);
#48519=AXIS2_PLACEMENT_3D('',#85962,#57232,#57233);
#48520=AXIS2_PLACEMENT_3D('',#85963,#57234,#57235);
#48521=AXIS2_PLACEMENT_3D('',#85982,#57236,#57237);
#48522=AXIS2_PLACEMENT_3D('',#85990,#57239,#57240);
#48523=AXIS2_PLACEMENT_3D('',#85993,#57241,#57242);
#48524=AXIS2_PLACEMENT_3D('',#85994,#57243,#57244);
#48525=AXIS2_PLACEMENT_3D('',#85995,#57245,#57246);
#48526=AXIS2_PLACEMENT_3D('',#86007,#57247,#57248);
#48527=AXIS2_PLACEMENT_3D('',#86008,#57249,#57250);
#48528=AXIS2_PLACEMENT_3D('',#86012,#57252,#57253);
#48529=AXIS2_PLACEMENT_3D('',#86014,#57254,#57255);
#48530=AXIS2_PLACEMENT_3D('',#86050,#57258,#57259);
#48531=AXIS2_PLACEMENT_3D('',#86058,#57261,#57262);
#48532=AXIS2_PLACEMENT_3D('',#86061,#57263,#57264);
#48533=AXIS2_PLACEMENT_3D('',#86062,#57265,#57266);
#48534=AXIS2_PLACEMENT_3D('',#86063,#57267,#57268);
#48535=AXIS2_PLACEMENT_3D('',#86099,#57270,#57271);
#48536=AXIS2_PLACEMENT_3D('',#86101,#57272,#57273);
#48537=AXIS2_PLACEMENT_3D('',#86156,#57277,#57278);
#48538=AXIS2_PLACEMENT_3D('',#86159,#57279,#57280);
#48539=AXIS2_PLACEMENT_3D('',#86166,#57281,#57282);
#48540=AXIS2_PLACEMENT_3D('',#86178,#57283,#57284);
#48541=AXIS2_PLACEMENT_3D('',#86179,#57285,#57286);
#48542=AXIS2_PLACEMENT_3D('',#86183,#57288,#57289);
#48543=AXIS2_PLACEMENT_3D('',#86185,#57290,#57291);
#48544=AXIS2_PLACEMENT_3D('',#86221,#57294,#57295);
#48545=AXIS2_PLACEMENT_3D('',#86229,#57297,#57298);
#48546=AXIS2_PLACEMENT_3D('',#86232,#57299,#57300);
#48547=AXIS2_PLACEMENT_3D('',#86233,#57301,#57302);
#48548=AXIS2_PLACEMENT_3D('',#86234,#57303,#57304);
#48549=AXIS2_PLACEMENT_3D('',#86253,#57305,#57306);
#48550=AXIS2_PLACEMENT_3D('',#86254,#57307,#57308);
#48551=AXIS2_PLACEMENT_3D('',#86258,#57310,#57311);
#48552=AXIS2_PLACEMENT_3D('',#86260,#57312,#57313);
#48553=AXIS2_PLACEMENT_3D('',#86296,#57316,#57317);
#48554=AXIS2_PLACEMENT_3D('',#86304,#57319,#57320);
#48555=AXIS2_PLACEMENT_3D('',#86307,#57321,#57322);
#48556=AXIS2_PLACEMENT_3D('',#86308,#57323,#57324);
#48557=AXIS2_PLACEMENT_3D('',#86309,#57325,#57326);
#48558=AXIS2_PLACEMENT_3D('',#86324,#57327,#57328);
#48559=AXIS2_PLACEMENT_3D('',#86325,#57329,#57330);
#48560=AXIS2_PLACEMENT_3D('',#86329,#57332,#57333);
#48561=AXIS2_PLACEMENT_3D('',#86331,#57334,#57335);
#48562=AXIS2_PLACEMENT_3D('',#86365,#57338,#57339);
#48563=AXIS2_PLACEMENT_3D('',#86367,#57341,#57342);
#48564=AXIS2_PLACEMENT_3D('',#86368,#57343,#57344);
#48565=AXIS2_PLACEMENT_3D('',#86371,#57346,#57347);
#48566=AXIS2_PLACEMENT_3D('',#86372,#57348,#57349);
#48567=AXIS2_PLACEMENT_3D('',#86373,#57350,#57351);
#48568=AXIS2_PLACEMENT_3D('',#86392,#57352,#57353);
#48569=AXIS2_PLACEMENT_3D('',#86393,#57354,#57355);
#48570=AXIS2_PLACEMENT_3D('',#86403,#57356,#57357);
#48571=AXIS2_PLACEMENT_3D('',#86423,#57359,#57360);
#48572=AXIS2_PLACEMENT_3D('',#86431,#57362,#57363);
#48573=AXIS2_PLACEMENT_3D('',#86434,#57364,#57365);
#48574=AXIS2_PLACEMENT_3D('',#86435,#57366,#57367);
#48575=AXIS2_PLACEMENT_3D('',#86436,#57368,#57369);
#48576=AXIS2_PLACEMENT_3D('',#86445,#57370,#57371);
#48577=AXIS2_PLACEMENT_3D('',#86446,#57372,#57373);
#48578=AXIS2_PLACEMENT_3D('',#86450,#57375,#57376);
#48579=AXIS2_PLACEMENT_3D('',#86452,#57377,#57378);
#48580=AXIS2_PLACEMENT_3D('',#86477,#57381,#57382);
#48581=AXIS2_PLACEMENT_3D('',#86478,#57383,#57384);
#48582=AXIS2_PLACEMENT_3D('',#86497,#57385,#57386);
#48583=AXIS2_PLACEMENT_3D('',#86505,#57388,#57389);
#48584=AXIS2_PLACEMENT_3D('',#86508,#57390,#57391);
#48585=AXIS2_PLACEMENT_3D('',#86509,#57392,#57393);
#48586=AXIS2_PLACEMENT_3D('',#86510,#57394,#57395);
#48587=AXIS2_PLACEMENT_3D('',#86522,#57396,#57397);
#48588=AXIS2_PLACEMENT_3D('',#86523,#57398,#57399);
#48589=AXIS2_PLACEMENT_3D('',#86527,#57401,#57402);
#48590=AXIS2_PLACEMENT_3D('',#86529,#57403,#57404);
#48591=AXIS2_PLACEMENT_3D('',#86565,#57407,#57408);
#48592=AXIS2_PLACEMENT_3D('',#86573,#57410,#57411);
#48593=AXIS2_PLACEMENT_3D('',#86576,#57412,#57413);
#48594=AXIS2_PLACEMENT_3D('',#86577,#57414,#57415);
#48595=AXIS2_PLACEMENT_3D('',#86578,#57416,#57417);
#48596=AXIS2_PLACEMENT_3D('',#86614,#57419,#57420);
#48597=AXIS2_PLACEMENT_3D('',#86616,#57421,#57422);
#48598=AXIS2_PLACEMENT_3D('',#86671,#57426,#57427);
#48599=AXIS2_PLACEMENT_3D('',#86674,#57428,#57429);
#48600=AXIS2_PLACEMENT_3D('',#86681,#57430,#57431);
#48601=AXIS2_PLACEMENT_3D('',#86693,#57432,#57433);
#48602=AXIS2_PLACEMENT_3D('',#86694,#57434,#57435);
#48603=AXIS2_PLACEMENT_3D('',#86698,#57437,#57438);
#48604=AXIS2_PLACEMENT_3D('',#86700,#57439,#57440);
#48605=AXIS2_PLACEMENT_3D('',#86736,#57443,#57444);
#48606=AXIS2_PLACEMENT_3D('',#86744,#57446,#57447);
#48607=AXIS2_PLACEMENT_3D('',#86747,#57448,#57449);
#48608=AXIS2_PLACEMENT_3D('',#86748,#57450,#57451);
#48609=AXIS2_PLACEMENT_3D('',#86749,#57452,#57453);
#48610=AXIS2_PLACEMENT_3D('',#86768,#57454,#57455);
#48611=AXIS2_PLACEMENT_3D('',#86769,#57456,#57457);
#48612=AXIS2_PLACEMENT_3D('',#86773,#57459,#57460);
#48613=AXIS2_PLACEMENT_3D('',#86775,#57461,#57462);
#48614=AXIS2_PLACEMENT_3D('',#86811,#57465,#57466);
#48615=AXIS2_PLACEMENT_3D('',#86819,#57468,#57469);
#48616=AXIS2_PLACEMENT_3D('',#86822,#57470,#57471);
#48617=AXIS2_PLACEMENT_3D('',#86823,#57472,#57473);
#48618=AXIS2_PLACEMENT_3D('',#86824,#57474,#57475);
#48619=AXIS2_PLACEMENT_3D('',#86839,#57476,#57477);
#48620=AXIS2_PLACEMENT_3D('',#86840,#57478,#57479);
#48621=AXIS2_PLACEMENT_3D('',#86844,#57481,#57482);
#48622=AXIS2_PLACEMENT_3D('',#86846,#57483,#57484);
#48623=AXIS2_PLACEMENT_3D('',#86880,#57487,#57488);
#48624=AXIS2_PLACEMENT_3D('',#86882,#57490,#57491);
#48625=AXIS2_PLACEMENT_3D('',#86883,#57492,#57493);
#48626=AXIS2_PLACEMENT_3D('',#86886,#57495,#57496);
#48627=AXIS2_PLACEMENT_3D('',#86887,#57497,#57498);
#48628=AXIS2_PLACEMENT_3D('',#86888,#57499,#57500);
#48629=AXIS2_PLACEMENT_3D('',#86907,#57501,#57502);
#48630=AXIS2_PLACEMENT_3D('',#86908,#57503,#57504);
#48631=AXIS2_PLACEMENT_3D('',#86918,#57505,#57506);
#48632=AXIS2_PLACEMENT_3D('',#86938,#57508,#57509);
#48633=AXIS2_PLACEMENT_3D('',#86946,#57511,#57512);
#48634=AXIS2_PLACEMENT_3D('',#86949,#57513,#57514);
#48635=AXIS2_PLACEMENT_3D('',#86950,#57515,#57516);
#48636=AXIS2_PLACEMENT_3D('',#86951,#57517,#57518);
#48637=AXIS2_PLACEMENT_3D('',#86960,#57519,#57520);
#48638=AXIS2_PLACEMENT_3D('',#86961,#57521,#57522);
#48639=AXIS2_PLACEMENT_3D('',#86965,#57524,#57525);
#48640=AXIS2_PLACEMENT_3D('',#86967,#57526,#57527);
#48641=AXIS2_PLACEMENT_3D('',#86992,#57530,#57531);
#48642=AXIS2_PLACEMENT_3D('',#86993,#57532,#57533);
#48643=AXIS2_PLACEMENT_3D('',#87012,#57534,#57535);
#48644=AXIS2_PLACEMENT_3D('',#87020,#57537,#57538);
#48645=AXIS2_PLACEMENT_3D('',#87023,#57539,#57540);
#48646=AXIS2_PLACEMENT_3D('',#87024,#57541,#57542);
#48647=AXIS2_PLACEMENT_3D('',#87025,#57543,#57544);
#48648=AXIS2_PLACEMENT_3D('',#87037,#57545,#57546);
#48649=AXIS2_PLACEMENT_3D('',#87038,#57547,#57548);
#48650=AXIS2_PLACEMENT_3D('',#87042,#57550,#57551);
#48651=AXIS2_PLACEMENT_3D('',#87044,#57552,#57553);
#48652=AXIS2_PLACEMENT_3D('',#87080,#57556,#57557);
#48653=AXIS2_PLACEMENT_3D('',#87088,#57559,#57560);
#48654=AXIS2_PLACEMENT_3D('',#87091,#57561,#57562);
#48655=AXIS2_PLACEMENT_3D('',#87092,#57563,#57564);
#48656=AXIS2_PLACEMENT_3D('',#87093,#57565,#57566);
#48657=AXIS2_PLACEMENT_3D('',#87129,#57568,#57569);
#48658=AXIS2_PLACEMENT_3D('',#87131,#57570,#57571);
#48659=AXIS2_PLACEMENT_3D('',#87186,#57575,#57576);
#48660=AXIS2_PLACEMENT_3D('',#87189,#57577,#57578);
#48661=AXIS2_PLACEMENT_3D('',#87196,#57579,#57580);
#48662=AXIS2_PLACEMENT_3D('',#87208,#57581,#57582);
#48663=AXIS2_PLACEMENT_3D('',#87209,#57583,#57584);
#48664=AXIS2_PLACEMENT_3D('',#87213,#57586,#57587);
#48665=AXIS2_PLACEMENT_3D('',#87215,#57588,#57589);
#48666=AXIS2_PLACEMENT_3D('',#87251,#57592,#57593);
#48667=AXIS2_PLACEMENT_3D('',#87259,#57595,#57596);
#48668=AXIS2_PLACEMENT_3D('',#87262,#57597,#57598);
#48669=AXIS2_PLACEMENT_3D('',#87263,#57599,#57600);
#48670=AXIS2_PLACEMENT_3D('',#87264,#57601,#57602);
#48671=AXIS2_PLACEMENT_3D('',#87283,#57603,#57604);
#48672=AXIS2_PLACEMENT_3D('',#87284,#57605,#57606);
#48673=AXIS2_PLACEMENT_3D('',#87288,#57608,#57609);
#48674=AXIS2_PLACEMENT_3D('',#87290,#57610,#57611);
#48675=AXIS2_PLACEMENT_3D('',#87326,#57614,#57615);
#48676=AXIS2_PLACEMENT_3D('',#87334,#57617,#57618);
#48677=AXIS2_PLACEMENT_3D('',#87337,#57619,#57620);
#48678=AXIS2_PLACEMENT_3D('',#87338,#57621,#57622);
#48679=AXIS2_PLACEMENT_3D('',#87339,#57623,#57624);
#48680=AXIS2_PLACEMENT_3D('',#87354,#57625,#57626);
#48681=AXIS2_PLACEMENT_3D('',#87355,#57627,#57628);
#48682=AXIS2_PLACEMENT_3D('',#87359,#57630,#57631);
#48683=AXIS2_PLACEMENT_3D('',#87361,#57632,#57633);
#48684=AXIS2_PLACEMENT_3D('',#87395,#57636,#57637);
#48685=AXIS2_PLACEMENT_3D('',#87397,#57639,#57640);
#48686=AXIS2_PLACEMENT_3D('',#87398,#57641,#57642);
#48687=AXIS2_PLACEMENT_3D('',#87401,#57644,#57645);
#48688=AXIS2_PLACEMENT_3D('',#87402,#57646,#57647);
#48689=AXIS2_PLACEMENT_3D('',#87403,#57648,#57649);
#48690=AXIS2_PLACEMENT_3D('',#87422,#57650,#57651);
#48691=AXIS2_PLACEMENT_3D('',#87423,#57652,#57653);
#48692=AXIS2_PLACEMENT_3D('',#87433,#57654,#57655);
#48693=AXIS2_PLACEMENT_3D('',#87453,#57657,#57658);
#48694=AXIS2_PLACEMENT_3D('',#87461,#57660,#57661);
#48695=AXIS2_PLACEMENT_3D('',#87464,#57662,#57663);
#48696=AXIS2_PLACEMENT_3D('',#87465,#57664,#57665);
#48697=AXIS2_PLACEMENT_3D('',#87466,#57666,#57667);
#48698=AXIS2_PLACEMENT_3D('',#87475,#57668,#57669);
#48699=AXIS2_PLACEMENT_3D('',#87476,#57670,#57671);
#48700=AXIS2_PLACEMENT_3D('',#87480,#57673,#57674);
#48701=AXIS2_PLACEMENT_3D('',#87482,#57675,#57676);
#48702=AXIS2_PLACEMENT_3D('',#87507,#57679,#57680);
#48703=AXIS2_PLACEMENT_3D('',#87508,#57681,#57682);
#48704=AXIS2_PLACEMENT_3D('',#87527,#57683,#57684);
#48705=AXIS2_PLACEMENT_3D('',#87535,#57686,#57687);
#48706=AXIS2_PLACEMENT_3D('',#87538,#57688,#57689);
#48707=AXIS2_PLACEMENT_3D('',#87539,#57690,#57691);
#48708=AXIS2_PLACEMENT_3D('',#87540,#57692,#57693);
#48709=AXIS2_PLACEMENT_3D('',#87552,#57694,#57695);
#48710=AXIS2_PLACEMENT_3D('',#87553,#57696,#57697);
#48711=AXIS2_PLACEMENT_3D('',#87557,#57699,#57700);
#48712=AXIS2_PLACEMENT_3D('',#87559,#57701,#57702);
#48713=AXIS2_PLACEMENT_3D('',#87595,#57705,#57706);
#48714=AXIS2_PLACEMENT_3D('',#87603,#57708,#57709);
#48715=AXIS2_PLACEMENT_3D('',#87606,#57710,#57711);
#48716=AXIS2_PLACEMENT_3D('',#87607,#57712,#57713);
#48717=AXIS2_PLACEMENT_3D('',#87608,#57714,#57715);
#48718=AXIS2_PLACEMENT_3D('',#87644,#57717,#57718);
#48719=AXIS2_PLACEMENT_3D('',#87646,#57719,#57720);
#48720=AXIS2_PLACEMENT_3D('',#87701,#57724,#57725);
#48721=AXIS2_PLACEMENT_3D('',#87704,#57726,#57727);
#48722=AXIS2_PLACEMENT_3D('',#87711,#57728,#57729);
#48723=AXIS2_PLACEMENT_3D('',#87723,#57730,#57731);
#48724=AXIS2_PLACEMENT_3D('',#87724,#57732,#57733);
#48725=AXIS2_PLACEMENT_3D('',#87728,#57735,#57736);
#48726=AXIS2_PLACEMENT_3D('',#87730,#57737,#57738);
#48727=AXIS2_PLACEMENT_3D('',#87766,#57741,#57742);
#48728=AXIS2_PLACEMENT_3D('',#87774,#57744,#57745);
#48729=AXIS2_PLACEMENT_3D('',#87777,#57746,#57747);
#48730=AXIS2_PLACEMENT_3D('',#87778,#57748,#57749);
#48731=AXIS2_PLACEMENT_3D('',#87779,#57750,#57751);
#48732=AXIS2_PLACEMENT_3D('',#87798,#57752,#57753);
#48733=AXIS2_PLACEMENT_3D('',#87799,#57754,#57755);
#48734=AXIS2_PLACEMENT_3D('',#87803,#57757,#57758);
#48735=AXIS2_PLACEMENT_3D('',#87805,#57759,#57760);
#48736=AXIS2_PLACEMENT_3D('',#87841,#57763,#57764);
#48737=AXIS2_PLACEMENT_3D('',#87849,#57766,#57767);
#48738=AXIS2_PLACEMENT_3D('',#87852,#57768,#57769);
#48739=AXIS2_PLACEMENT_3D('',#87853,#57770,#57771);
#48740=AXIS2_PLACEMENT_3D('',#87854,#57772,#57773);
#48741=AXIS2_PLACEMENT_3D('',#87869,#57774,#57775);
#48742=AXIS2_PLACEMENT_3D('',#87870,#57776,#57777);
#48743=AXIS2_PLACEMENT_3D('',#87874,#57779,#57780);
#48744=AXIS2_PLACEMENT_3D('',#87876,#57781,#57782);
#48745=AXIS2_PLACEMENT_3D('',#87910,#57785,#57786);
#48746=AXIS2_PLACEMENT_3D('',#87912,#57788,#57789);
#48747=AXIS2_PLACEMENT_3D('',#87913,#57790,#57791);
#48748=AXIS2_PLACEMENT_3D('',#87916,#57793,#57794);
#48749=AXIS2_PLACEMENT_3D('',#87917,#57795,#57796);
#48750=AXIS2_PLACEMENT_3D('',#87918,#57797,#57798);
#48751=AXIS2_PLACEMENT_3D('',#87919,#57799,#57800);
#48752=AXIS2_PLACEMENT_3D('',#87922,#57801,#57802);
#48753=AXIS2_PLACEMENT_3D('',#87924,#57803,#57804);
#48754=AXIS2_PLACEMENT_3D('',#87926,#57805,#57806);
#48755=AXIS2_PLACEMENT_3D('',#87927,#57807,#57808);
#48756=AXIS2_PLACEMENT_3D('',#87946,#57809,#57810);
#48757=AXIS2_PLACEMENT_3D('',#87947,#57811,#57812);
#48758=AXIS2_PLACEMENT_3D('',#87957,#57813,#57814);
#48759=AXIS2_PLACEMENT_3D('',#87990,#57817,#57818);
#48760=AXIS2_PLACEMENT_3D('',#87991,#57819,#57820);
#48761=AXIS2_PLACEMENT_3D('',#87995,#57822,#57823);
#48762=AXIS2_PLACEMENT_3D('',#87997,#57824,#57825);
#48763=AXIS2_PLACEMENT_3D('',#88022,#57828,#57829);
#48764=AXIS2_PLACEMENT_3D('',#88023,#57830,#57831);
#48765=AXIS2_PLACEMENT_3D('',#88042,#57832,#57833);
#48766=AXIS2_PLACEMENT_3D('',#88050,#57835,#57836);
#48767=AXIS2_PLACEMENT_3D('',#88053,#57837,#57838);
#48768=AXIS2_PLACEMENT_3D('',#88054,#57839,#57840);
#48769=AXIS2_PLACEMENT_3D('',#88055,#57841,#57842);
#48770=AXIS2_PLACEMENT_3D('',#88067,#57843,#57844);
#48771=AXIS2_PLACEMENT_3D('',#88068,#57845,#57846);
#48772=AXIS2_PLACEMENT_3D('',#88072,#57848,#57849);
#48773=AXIS2_PLACEMENT_3D('',#88074,#57850,#57851);
#48774=AXIS2_PLACEMENT_3D('',#88110,#57854,#57855);
#48775=AXIS2_PLACEMENT_3D('',#88118,#57857,#57858);
#48776=AXIS2_PLACEMENT_3D('',#88121,#57859,#57860);
#48777=AXIS2_PLACEMENT_3D('',#88122,#57861,#57862);
#48778=AXIS2_PLACEMENT_3D('',#88123,#57863,#57864);
#48779=AXIS2_PLACEMENT_3D('',#88159,#57866,#57867);
#48780=AXIS2_PLACEMENT_3D('',#88161,#57868,#57869);
#48781=AXIS2_PLACEMENT_3D('',#88216,#57873,#57874);
#48782=AXIS2_PLACEMENT_3D('',#88219,#57875,#57876);
#48783=AXIS2_PLACEMENT_3D('',#88226,#57877,#57878);
#48784=AXIS2_PLACEMENT_3D('',#88238,#57879,#57880);
#48785=AXIS2_PLACEMENT_3D('',#88239,#57881,#57882);
#48786=AXIS2_PLACEMENT_3D('',#88243,#57884,#57885);
#48787=AXIS2_PLACEMENT_3D('',#88245,#57886,#57887);
#48788=AXIS2_PLACEMENT_3D('',#88281,#57890,#57891);
#48789=AXIS2_PLACEMENT_3D('',#88289,#57893,#57894);
#48790=AXIS2_PLACEMENT_3D('',#88292,#57895,#57896);
#48791=AXIS2_PLACEMENT_3D('',#88293,#57897,#57898);
#48792=AXIS2_PLACEMENT_3D('',#88294,#57899,#57900);
#48793=AXIS2_PLACEMENT_3D('',#88313,#57901,#57902);
#48794=AXIS2_PLACEMENT_3D('',#88314,#57903,#57904);
#48795=AXIS2_PLACEMENT_3D('',#88318,#57906,#57907);
#48796=AXIS2_PLACEMENT_3D('',#88320,#57908,#57909);
#48797=AXIS2_PLACEMENT_3D('',#88356,#57912,#57913);
#48798=AXIS2_PLACEMENT_3D('',#88364,#57915,#57916);
#48799=AXIS2_PLACEMENT_3D('',#88367,#57917,#57918);
#48800=AXIS2_PLACEMENT_3D('',#88368,#57919,#57920);
#48801=AXIS2_PLACEMENT_3D('',#88369,#57921,#57922);
#48802=AXIS2_PLACEMENT_3D('',#88384,#57923,#57924);
#48803=AXIS2_PLACEMENT_3D('',#88385,#57925,#57926);
#48804=AXIS2_PLACEMENT_3D('',#88389,#57928,#57929);
#48805=AXIS2_PLACEMENT_3D('',#88391,#57930,#57931);
#48806=AXIS2_PLACEMENT_3D('',#88425,#57934,#57935);
#48807=AXIS2_PLACEMENT_3D('',#88427,#57937,#57938);
#48808=AXIS2_PLACEMENT_3D('',#88428,#57939,#57940);
#48809=AXIS2_PLACEMENT_3D('',#88431,#57942,#57943);
#48810=AXIS2_PLACEMENT_3D('',#88432,#57944,#57945);
#48811=AXIS2_PLACEMENT_3D('',#88433,#57946,#57947);
#48812=AXIS2_PLACEMENT_3D('',#88434,#57948,#57949);
#48813=AXIS2_PLACEMENT_3D('',#88437,#57950,#57951);
#48814=AXIS2_PLACEMENT_3D('',#88439,#57952,#57953);
#48815=AXIS2_PLACEMENT_3D('',#88441,#57954,#57955);
#48816=AXIS2_PLACEMENT_3D('',#88442,#57956,#57957);
#48817=AXIS2_PLACEMENT_3D('',#88443,#57958,#57959);
#48818=AXIS2_PLACEMENT_3D('',#88446,#57960,#57961);
#48819=AXIS2_PLACEMENT_3D('',#88448,#57962,#57963);
#48820=AXIS2_PLACEMENT_3D('',#88450,#57964,#57965);
#48821=AXIS2_PLACEMENT_3D('',#88451,#57966,#57967);
#48822=AXIS2_PLACEMENT_3D('',#88470,#57968,#57969);
#48823=AXIS2_PLACEMENT_3D('',#88471,#57970,#57971);
#48824=AXIS2_PLACEMENT_3D('',#88481,#57972,#57973);
#48825=AXIS2_PLACEMENT_3D('',#88517,#57976,#57977);
#48826=AXIS2_PLACEMENT_3D('',#88518,#57978,#57979);
#48827=AXIS2_PLACEMENT_3D('',#88522,#57981,#57982);
#48828=AXIS2_PLACEMENT_3D('',#88524,#57983,#57984);
#48829=AXIS2_PLACEMENT_3D('',#88549,#57987,#57988);
#48830=AXIS2_PLACEMENT_3D('',#88550,#57989,#57990);
#48831=AXIS2_PLACEMENT_3D('',#88582,#57992,#57993);
#48832=AXIS2_PLACEMENT_3D('',#88583,#57994,#57995);
#48833=AXIS2_PLACEMENT_3D('',#88587,#57997,#57998);
#48834=AXIS2_PLACEMENT_3D('',#88589,#57999,#58000);
#48835=AXIS2_PLACEMENT_3D('',#88632,#58003,#58004);
#48836=AXIS2_PLACEMENT_3D('',#88640,#58006,#58007);
#48837=AXIS2_PLACEMENT_3D('',#88643,#58008,#58009);
#48838=AXIS2_PLACEMENT_3D('',#88644,#58010,#58011);
#48839=AXIS2_PLACEMENT_3D('',#88645,#58012,#58013);
#48840=AXIS2_PLACEMENT_3D('',#88681,#58015,#58016);
#48841=AXIS2_PLACEMENT_3D('',#88683,#58017,#58018);
#48842=AXIS2_PLACEMENT_3D('',#88738,#58022,#58023);
#48843=AXIS2_PLACEMENT_3D('',#88741,#58024,#58025);
#48844=AXIS2_PLACEMENT_3D('',#88748,#58026,#58027);
#48845=AXIS2_PLACEMENT_3D('',#88760,#58028,#58029);
#48846=AXIS2_PLACEMENT_3D('',#88761,#58030,#58031);
#48847=AXIS2_PLACEMENT_3D('',#88765,#58033,#58034);
#48848=AXIS2_PLACEMENT_3D('',#88767,#58035,#58036);
#48849=AXIS2_PLACEMENT_3D('',#88803,#58039,#58040);
#48850=AXIS2_PLACEMENT_3D('',#88811,#58042,#58043);
#48851=AXIS2_PLACEMENT_3D('',#88814,#58044,#58045);
#48852=AXIS2_PLACEMENT_3D('',#88815,#58046,#58047);
#48853=AXIS2_PLACEMENT_3D('',#88816,#58048,#58049);
#48854=AXIS2_PLACEMENT_3D('',#88835,#58050,#58051);
#48855=AXIS2_PLACEMENT_3D('',#88836,#58052,#58053);
#48856=AXIS2_PLACEMENT_3D('',#88840,#58055,#58056);
#48857=AXIS2_PLACEMENT_3D('',#88842,#58057,#58058);
#48858=AXIS2_PLACEMENT_3D('',#88878,#58061,#58062);
#48859=AXIS2_PLACEMENT_3D('',#88886,#58064,#58065);
#48860=AXIS2_PLACEMENT_3D('',#88889,#58066,#58067);
#48861=AXIS2_PLACEMENT_3D('',#88890,#58068,#58069);
#48862=AXIS2_PLACEMENT_3D('',#88891,#58070,#58071);
#48863=AXIS2_PLACEMENT_3D('',#88906,#58072,#58073);
#48864=AXIS2_PLACEMENT_3D('',#88907,#58074,#58075);
#48865=AXIS2_PLACEMENT_3D('',#88911,#58077,#58078);
#48866=AXIS2_PLACEMENT_3D('',#88913,#58079,#58080);
#48867=AXIS2_PLACEMENT_3D('',#88947,#58083,#58084);
#48868=AXIS2_PLACEMENT_3D('',#88949,#58086,#58087);
#48869=AXIS2_PLACEMENT_3D('',#88950,#58088,#58089);
#48870=AXIS2_PLACEMENT_3D('',#88953,#58091,#58092);
#48871=AXIS2_PLACEMENT_3D('',#88954,#58093,#58094);
#48872=AXIS2_PLACEMENT_3D('',#88955,#58095,#58096);
#48873=AXIS2_PLACEMENT_3D('',#88956,#58097,#58098);
#48874=AXIS2_PLACEMENT_3D('',#88959,#58099,#58100);
#48875=AXIS2_PLACEMENT_3D('',#88961,#58101,#58102);
#48876=AXIS2_PLACEMENT_3D('',#88963,#58103,#58104);
#48877=AXIS2_PLACEMENT_3D('',#88964,#58105,#58106);
#48878=AXIS2_PLACEMENT_3D('',#88965,#58107,#58108);
#48879=AXIS2_PLACEMENT_3D('',#88968,#58109,#58110);
#48880=AXIS2_PLACEMENT_3D('',#88970,#58111,#58112);
#48881=AXIS2_PLACEMENT_3D('',#88972,#58113,#58114);
#48882=AXIS2_PLACEMENT_3D('',#88973,#58115,#58116);
#48883=AXIS2_PLACEMENT_3D('',#88974,#58117,#58118);
#48884=AXIS2_PLACEMENT_3D('',#88977,#58119,#58120);
#48885=AXIS2_PLACEMENT_3D('',#88979,#58121,#58122);
#48886=AXIS2_PLACEMENT_3D('',#88981,#58123,#58124);
#48887=AXIS2_PLACEMENT_3D('',#88982,#58125,#58126);
#48888=AXIS2_PLACEMENT_3D('',#88991,#58127,#58128);
#48889=AXIS2_PLACEMENT_3D('',#88992,#58129,#58130);
#48890=AXIS2_PLACEMENT_3D('',#88996,#58132,#58133);
#48891=AXIS2_PLACEMENT_3D('',#88998,#58134,#58135);
#48892=AXIS2_PLACEMENT_3D('',#89023,#58138,#58139);
#48893=AXIS2_PLACEMENT_3D('',#89024,#58140,#58141);
#48894=AXIS2_PLACEMENT_3D('',#89062,#58143,#58144);
#48895=AXIS2_PLACEMENT_3D('',#89063,#58145,#58146);
#48896=AXIS2_PLACEMENT_3D('',#89067,#58148,#58149);
#48897=AXIS2_PLACEMENT_3D('',#89069,#58150,#58151);
#48898=AXIS2_PLACEMENT_3D('',#89144,#58156,#58157);
#48899=AXIS2_PLACEMENT_3D('',#89146,#58158,#58159);
#48900=AXIS2_PLACEMENT_3D('',#89207,#58163,#58164);
#48901=AXIS2_PLACEMENT_3D('',#89208,#58165,#58166);
#48902=AXIS2_PLACEMENT_3D('',#89218,#58167,#58168);
#48903=AXIS2_PLACEMENT_3D('',#89243,#58171,#58172);
#48904=AXIS2_PLACEMENT_3D('',#89246,#58173,#58174);
#48905=AXIS2_PLACEMENT_3D('',#89253,#58175,#58176);
#48906=AXIS2_PLACEMENT_3D('',#89265,#58177,#58178);
#48907=AXIS2_PLACEMENT_3D('',#89266,#58179,#58180);
#48908=AXIS2_PLACEMENT_3D('',#89270,#58182,#58183);
#48909=AXIS2_PLACEMENT_3D('',#89272,#58184,#58185);
#48910=AXIS2_PLACEMENT_3D('',#89308,#58188,#58189);
#48911=AXIS2_PLACEMENT_3D('',#89316,#58191,#58192);
#48912=AXIS2_PLACEMENT_3D('',#89319,#58193,#58194);
#48913=AXIS2_PLACEMENT_3D('',#89320,#58195,#58196);
#48914=AXIS2_PLACEMENT_3D('',#89321,#58197,#58198);
#48915=AXIS2_PLACEMENT_3D('',#89340,#58199,#58200);
#48916=AXIS2_PLACEMENT_3D('',#89341,#58201,#58202);
#48917=AXIS2_PLACEMENT_3D('',#89345,#58204,#58205);
#48918=AXIS2_PLACEMENT_3D('',#89347,#58206,#58207);
#48919=AXIS2_PLACEMENT_3D('',#89383,#58210,#58211);
#48920=AXIS2_PLACEMENT_3D('',#89391,#58213,#58214);
#48921=AXIS2_PLACEMENT_3D('',#89394,#58215,#58216);
#48922=AXIS2_PLACEMENT_3D('',#89395,#58217,#58218);
#48923=AXIS2_PLACEMENT_3D('',#89396,#58219,#58220);
#48924=AXIS2_PLACEMENT_3D('',#89411,#58221,#58222);
#48925=AXIS2_PLACEMENT_3D('',#89412,#58223,#58224);
#48926=AXIS2_PLACEMENT_3D('',#89416,#58226,#58227);
#48927=AXIS2_PLACEMENT_3D('',#89418,#58228,#58229);
#48928=AXIS2_PLACEMENT_3D('',#89452,#58232,#58233);
#48929=AXIS2_PLACEMENT_3D('',#89454,#58235,#58236);
#48930=AXIS2_PLACEMENT_3D('',#89455,#58237,#58238);
#48931=AXIS2_PLACEMENT_3D('',#89458,#58240,#58241);
#48932=AXIS2_PLACEMENT_3D('',#89459,#58242,#58243);
#48933=AXIS2_PLACEMENT_3D('',#89460,#58244,#58245);
#48934=AXIS2_PLACEMENT_3D('',#89461,#58246,#58247);
#48935=AXIS2_PLACEMENT_3D('',#89464,#58248,#58249);
#48936=AXIS2_PLACEMENT_3D('',#89466,#58250,#58251);
#48937=AXIS2_PLACEMENT_3D('',#89468,#58252,#58253);
#48938=AXIS2_PLACEMENT_3D('',#89469,#58254,#58255);
#48939=AXIS2_PLACEMENT_3D('',#89470,#58256,#58257);
#48940=AXIS2_PLACEMENT_3D('',#89473,#58258,#58259);
#48941=AXIS2_PLACEMENT_3D('',#89475,#58260,#58261);
#48942=AXIS2_PLACEMENT_3D('',#89477,#58262,#58263);
#48943=AXIS2_PLACEMENT_3D('',#89478,#58264,#58265);
#48944=AXIS2_PLACEMENT_3D('',#89479,#58266,#58267);
#48945=AXIS2_PLACEMENT_3D('',#89482,#58268,#58269);
#48946=AXIS2_PLACEMENT_3D('',#89497,#58270,#58271);
#48947=AXIS2_PLACEMENT_3D('',#89498,#58272,#58273);
#48948=AXIS2_PLACEMENT_3D('',#89501,#58274,#58275);
#48949=AXIS2_PLACEMENT_3D('',#89503,#58276,#58277);
#48950=AXIS2_PLACEMENT_3D('',#89505,#58278,#58279);
#48951=AXIS2_PLACEMENT_3D('',#89506,#58280,#58281);
#48952=AXIS2_PLACEMENT_3D('',#89515,#58282,#58283);
#48953=AXIS2_PLACEMENT_3D('',#89516,#58284,#58285);
#48954=AXIS2_PLACEMENT_3D('',#89520,#58287,#58288);
#48955=AXIS2_PLACEMENT_3D('',#89522,#58289,#58290);
#48956=AXIS2_PLACEMENT_3D('',#89610,#58295,#58296);
#48957=AXIS2_PLACEMENT_3D('',#89612,#58297,#58298);
#48958=AXIS2_PLACEMENT_3D('',#89667,#58302,#58303);
#48959=AXIS2_PLACEMENT_3D('',#89668,#58304,#58305);
#48960=AXIS2_PLACEMENT_3D('',#89672,#58307,#58308);
#48961=AXIS2_PLACEMENT_3D('',#89674,#58309,#58310);
#48962=AXIS2_PLACEMENT_3D('',#89717,#58313,#58314);
#48963=AXIS2_PLACEMENT_3D('',#89736,#58316,#58317);
#48964=AXIS2_PLACEMENT_3D('',#89737,#58318,#58319);
#48965=AXIS2_PLACEMENT_3D('',#89747,#58320,#58321);
#48966=AXIS2_PLACEMENT_3D('',#89786,#58324,#58325);
#48967=AXIS2_PLACEMENT_3D('',#89787,#58326,#58327);
#48968=AXIS2_PLACEMENT_3D('',#89791,#58329,#58330);
#48969=AXIS2_PLACEMENT_3D('',#89793,#58331,#58332);
#48970=AXIS2_PLACEMENT_3D('',#89818,#58335,#58336);
#48971=AXIS2_PLACEMENT_3D('',#89819,#58337,#58338);
#48972=AXIS2_PLACEMENT_3D('',#89843,#58340,#58341);
#48973=AXIS2_PLACEMENT_3D('',#89846,#58342,#58343);
#48974=AXIS2_PLACEMENT_3D('',#89847,#58344,#58345);
#48975=AXIS2_PLACEMENT_3D('',#89848,#58346,#58347);
#48976=AXIS2_PLACEMENT_3D('',#89867,#58348,#58349);
#48977=AXIS2_PLACEMENT_3D('',#89868,#58350,#58351);
#48978=AXIS2_PLACEMENT_3D('',#89872,#58353,#58354);
#48979=AXIS2_PLACEMENT_3D('',#89874,#58355,#58356);
#48980=AXIS2_PLACEMENT_3D('',#89910,#58359,#58360);
#48981=AXIS2_PLACEMENT_3D('',#89918,#58362,#58363);
#48982=AXIS2_PLACEMENT_3D('',#89921,#58364,#58365);
#48983=AXIS2_PLACEMENT_3D('',#89922,#58366,#58367);
#48984=AXIS2_PLACEMENT_3D('',#89923,#58368,#58369);
#48985=AXIS2_PLACEMENT_3D('',#89938,#58370,#58371);
#48986=AXIS2_PLACEMENT_3D('',#89939,#58372,#58373);
#48987=AXIS2_PLACEMENT_3D('',#89943,#58375,#58376);
#48988=AXIS2_PLACEMENT_3D('',#89945,#58377,#58378);
#48989=AXIS2_PLACEMENT_3D('',#89979,#58381,#58382);
#48990=AXIS2_PLACEMENT_3D('',#89981,#58384,#58385);
#48991=AXIS2_PLACEMENT_3D('',#89982,#58386,#58387);
#48992=AXIS2_PLACEMENT_3D('',#89985,#58389,#58390);
#48993=AXIS2_PLACEMENT_3D('',#89986,#58391,#58392);
#48994=AXIS2_PLACEMENT_3D('',#89987,#58393,#58394);
#48995=AXIS2_PLACEMENT_3D('',#89988,#58395,#58396);
#48996=AXIS2_PLACEMENT_3D('',#89991,#58397,#58398);
#48997=AXIS2_PLACEMENT_3D('',#89993,#58399,#58400);
#48998=AXIS2_PLACEMENT_3D('',#89995,#58401,#58402);
#48999=AXIS2_PLACEMENT_3D('',#89996,#58403,#58404);
#49000=AXIS2_PLACEMENT_3D('',#89997,#58405,#58406);
#49001=AXIS2_PLACEMENT_3D('',#90000,#58407,#58408);
#49002=AXIS2_PLACEMENT_3D('',#90002,#58409,#58410);
#49003=AXIS2_PLACEMENT_3D('',#90004,#58411,#58412);
#49004=AXIS2_PLACEMENT_3D('',#90005,#58413,#58414);
#49005=AXIS2_PLACEMENT_3D('',#90006,#58415,#58416);
#49006=AXIS2_PLACEMENT_3D('',#90009,#58417,#58418);
#49007=AXIS2_PLACEMENT_3D('',#90011,#58419,#58420);
#49008=AXIS2_PLACEMENT_3D('',#90013,#58421,#58422);
#49009=AXIS2_PLACEMENT_3D('',#90014,#58423,#58424);
#49010=AXIS2_PLACEMENT_3D('',#90015,#58425,#58426);
#49011=AXIS2_PLACEMENT_3D('',#90018,#58427,#58428);
#49012=AXIS2_PLACEMENT_3D('',#90020,#58429,#58430);
#49013=AXIS2_PLACEMENT_3D('',#90022,#58431,#58432);
#49014=AXIS2_PLACEMENT_3D('',#90023,#58433,#58434);
#49015=AXIS2_PLACEMENT_3D('',#90024,#58435,#58436);
#49016=AXIS2_PLACEMENT_3D('',#90027,#58437,#58438);
#49017=AXIS2_PLACEMENT_3D('',#90042,#58439,#58440);
#49018=AXIS2_PLACEMENT_3D('',#90077,#58442,#58443);
#49019=AXIS2_PLACEMENT_3D('',#90079,#58444,#58445);
#49020=AXIS2_PLACEMENT_3D('',#90135,#58449,#58450);
#49021=AXIS2_PLACEMENT_3D('',#90136,#58451,#58452);
#49022=AXIS2_PLACEMENT_3D('',#90140,#58454,#58455);
#49023=AXIS2_PLACEMENT_3D('',#90142,#58456,#58457);
#49024=AXIS2_PLACEMENT_3D('',#90201,#58461,#58462);
#49025=AXIS2_PLACEMENT_3D('',#90202,#58463,#58464);
#49026=AXIS2_PLACEMENT_3D('',#90206,#58466,#58467);
#49027=AXIS2_PLACEMENT_3D('',#90208,#58468,#58469);
#49028=AXIS2_PLACEMENT_3D('',#90251,#58472,#58473);
#49029=AXIS2_PLACEMENT_3D('',#90277,#58475,#58476);
#49030=AXIS2_PLACEMENT_3D('',#90278,#58477,#58478);
#49031=AXIS2_PLACEMENT_3D('',#90288,#58479,#58480);
#49032=AXIS2_PLACEMENT_3D('',#90320,#58483,#58484);
#49033=AXIS2_PLACEMENT_3D('',#90321,#58485,#58486);
#49034=AXIS2_PLACEMENT_3D('',#90325,#58488,#58489);
#49035=AXIS2_PLACEMENT_3D('',#90327,#58490,#58491);
#49036=AXIS2_PLACEMENT_3D('',#90352,#58494,#58495);
#49037=AXIS2_PLACEMENT_3D('',#90353,#58496,#58497);
#49038=AXIS2_PLACEMENT_3D('',#90391,#58499,#58500);
#49039=AXIS2_PLACEMENT_3D('',#90392,#58501,#58502);
#49040=AXIS2_PLACEMENT_3D('',#90396,#58504,#58505);
#49041=AXIS2_PLACEMENT_3D('',#90398,#58506,#58507);
#49042=AXIS2_PLACEMENT_3D('',#90439,#58511,#58512);
#49043=AXIS2_PLACEMENT_3D('',#90442,#58513,#58514);
#49044=AXIS2_PLACEMENT_3D('',#90443,#58515,#58516);
#49045=AXIS2_PLACEMENT_3D('',#90444,#58517,#58518);
#49046=AXIS2_PLACEMENT_3D('',#90459,#58519,#58520);
#49047=AXIS2_PLACEMENT_3D('',#90460,#58521,#58522);
#49048=AXIS2_PLACEMENT_3D('',#90464,#58524,#58525);
#49049=AXIS2_PLACEMENT_3D('',#90466,#58526,#58527);
#49050=AXIS2_PLACEMENT_3D('',#90500,#58530,#58531);
#49051=AXIS2_PLACEMENT_3D('',#90502,#58533,#58534);
#49052=AXIS2_PLACEMENT_3D('',#90503,#58535,#58536);
#49053=AXIS2_PLACEMENT_3D('',#90506,#58538,#58539);
#49054=AXIS2_PLACEMENT_3D('',#90507,#58540,#58541);
#49055=AXIS2_PLACEMENT_3D('',#90508,#58542,#58543);
#49056=AXIS2_PLACEMENT_3D('',#90509,#58544,#58545);
#49057=AXIS2_PLACEMENT_3D('',#90512,#58546,#58547);
#49058=AXIS2_PLACEMENT_3D('',#90514,#58548,#58549);
#49059=AXIS2_PLACEMENT_3D('',#90516,#58550,#58551);
#49060=AXIS2_PLACEMENT_3D('',#90517,#58552,#58553);
#49061=AXIS2_PLACEMENT_3D('',#90518,#58554,#58555);
#49062=AXIS2_PLACEMENT_3D('',#90521,#58556,#58557);
#49063=AXIS2_PLACEMENT_3D('',#90536,#58558,#58559);
#49064=AXIS2_PLACEMENT_3D('',#90537,#58560,#58561);
#49065=AXIS2_PLACEMENT_3D('',#90540,#58562,#58563);
#49066=AXIS2_PLACEMENT_3D('',#90542,#58564,#58565);
#49067=AXIS2_PLACEMENT_3D('',#90544,#58566,#58567);
#49068=AXIS2_PLACEMENT_3D('',#90545,#58568,#58569);
#49069=AXIS2_PLACEMENT_3D('',#90546,#58570,#58571);
#49070=AXIS2_PLACEMENT_3D('',#90549,#58572,#58573);
#49071=AXIS2_PLACEMENT_3D('',#90551,#58574,#58575);
#49072=AXIS2_PLACEMENT_3D('',#90553,#58576,#58577);
#49073=AXIS2_PLACEMENT_3D('',#90554,#58578,#58579);
#49074=AXIS2_PLACEMENT_3D('',#90555,#58580,#58581);
#49075=AXIS2_PLACEMENT_3D('',#90558,#58582,#58583);
#49076=AXIS2_PLACEMENT_3D('',#90560,#58584,#58585);
#49077=AXIS2_PLACEMENT_3D('',#90562,#58586,#58587);
#49078=AXIS2_PLACEMENT_3D('',#90563,#58588,#58589);
#49079=AXIS2_PLACEMENT_3D('',#90564,#58590,#58591);
#49080=AXIS2_PLACEMENT_3D('',#90567,#58592,#58593);
#49081=AXIS2_PLACEMENT_3D('',#90569,#58594,#58595);
#49082=AXIS2_PLACEMENT_3D('',#90571,#58596,#58597);
#49083=AXIS2_PLACEMENT_3D('',#90572,#58598,#58599);
#49084=AXIS2_PLACEMENT_3D('',#90581,#58600,#58601);
#49085=AXIS2_PLACEMENT_3D('',#90582,#58602,#58603);
#49086=AXIS2_PLACEMENT_3D('',#90586,#58605,#58606);
#49087=AXIS2_PLACEMENT_3D('',#90587,#58607,#58608);
#49088=AXIS2_PLACEMENT_3D('',#90649,#58612,#58613);
#49089=AXIS2_PLACEMENT_3D('',#90650,#58614,#58615);
#49090=AXIS2_PLACEMENT_3D('',#90654,#58617,#58618);
#49091=AXIS2_PLACEMENT_3D('',#90655,#58619,#58620);
#49092=AXIS2_PLACEMENT_3D('',#90707,#58624,#58625);
#49093=AXIS2_PLACEMENT_3D('',#90708,#58626,#58627);
#49094=AXIS2_PLACEMENT_3D('',#90712,#58629,#58630);
#49095=AXIS2_PLACEMENT_3D('',#90714,#58631,#58632);
#49096=AXIS2_PLACEMENT_3D('',#90755,#58635,#58636);
#49097=AXIS2_PLACEMENT_3D('',#90768,#58638,#58639);
#49098=AXIS2_PLACEMENT_3D('',#90769,#58640,#58641);
#49099=AXIS2_PLACEMENT_3D('',#90778,#58642,#58643);
#49100=AXIS2_PLACEMENT_3D('',#90807,#58646,#58647);
#49101=AXIS2_PLACEMENT_3D('',#90808,#58648,#58649);
#49102=AXIS2_PLACEMENT_3D('',#90812,#58651,#58652);
#49103=AXIS2_PLACEMENT_3D('',#90813,#58653,#58654);
#49104=AXIS2_PLACEMENT_3D('',#90838,#58657,#58658);
#49105=AXIS2_PLACEMENT_3D('',#90839,#58659,#58660);
#49106=AXIS2_PLACEMENT_3D('',#90870,#58662,#58663);
#49107=AXIS2_PLACEMENT_3D('',#90871,#58664,#58665);
#49108=AXIS2_PLACEMENT_3D('',#90875,#58667,#58668);
#49109=AXIS2_PLACEMENT_3D('',#90876,#58669,#58670);
#49110=AXIS2_PLACEMENT_3D('',#90957,#58675,#58676);
#49111=AXIS2_PLACEMENT_3D('',#90958,#58677,#58678);
#49112=AXIS2_PLACEMENT_3D('',#91005,#58682,#58683);
#49113=AXIS2_PLACEMENT_3D('',#91006,#58684,#58685);
#49114=AXIS2_PLACEMENT_3D('',#91009,#58687,#58688);
#49115=AXIS2_PLACEMENT_3D('',#91010,#58689,#58690);
#49116=AXIS2_PLACEMENT_3D('',#91011,#58691,#58692);
#49117=AXIS2_PLACEMENT_3D('',#91012,#58693,#58694);
#49118=AXIS2_PLACEMENT_3D('',#91013,#58695,#58696);
#49119=AXIS2_PLACEMENT_3D('',#91016,#58698,#58699);
#49120=AXIS2_PLACEMENT_3D('',#91017,#58700,#58701);
#49121=AXIS2_PLACEMENT_3D('',#91018,#58702,#58703);
#49122=AXIS2_PLACEMENT_3D('',#91019,#58704,#58705);
#49123=AXIS2_PLACEMENT_3D('',#91020,#58706,#58707);
#49124=AXIS2_PLACEMENT_3D('',#91021,#58708,#58709);
#49125=AXIS2_PLACEMENT_3D('',#91022,#58710,#58711);
#49126=AXIS2_PLACEMENT_3D('',#91023,#58712,#58713);
#49127=AXIS2_PLACEMENT_3D('',#91040,#58714,#58715);
#49128=AXIS2_PLACEMENT_3D('',#91057,#58716,#58717);
#49129=AXIS2_PLACEMENT_3D('',#91080,#58718,#58719);
#49130=AXIS2_PLACEMENT_3D('',#91128,#58720,#58721);
#49131=AXIS2_PLACEMENT_3D('',#91145,#58722,#58723);
#49132=AXIS2_PLACEMENT_3D('',#91168,#58724,#58725);
#49133=AXIS2_PLACEMENT_3D('',#91185,#58726,#58727);
#49134=AXIS2_PLACEMENT_3D('',#91208,#58728,#58729);
#49135=AXIS2_PLACEMENT_3D('',#91225,#58730,#58731);
#49136=AXIS2_PLACEMENT_3D('',#91232,#58732,#58733);
#49137=AXIS2_PLACEMENT_3D('',#91237,#58734,#58735);
#49138=AXIS2_PLACEMENT_3D('',#91254,#58736,#58737);
#49139=AXIS2_PLACEMENT_3D('',#91271,#58738,#58739);
#49140=AXIS2_PLACEMENT_3D('',#91294,#58740,#58741);
#49141=AXIS2_PLACEMENT_3D('',#91295,#58742,#58743);
#49142=AXIS2_PLACEMENT_3D('',#91328,#58744,#58745);
#49143=AXIS2_PLACEMENT_3D('',#91333,#58746,#58747);
#49144=AXIS2_PLACEMENT_3D('',#91350,#58748,#58749);
#49145=AXIS2_PLACEMENT_3D('',#91367,#58750,#58751);
#49146=AXIS2_PLACEMENT_3D('',#91405,#58752,#58753);
#49147=AXIS2_PLACEMENT_3D('',#91438,#58754,#58755);
#49148=AXIS2_PLACEMENT_3D('',#91455,#58756,#58757);
#49149=AXIS2_PLACEMENT_3D('',#91478,#58758,#58759);
#49150=AXIS2_PLACEMENT_3D('',#91495,#58760,#58761);
#49151=AXIS2_PLACEMENT_3D('',#91518,#58762,#58763);
#49152=AXIS2_PLACEMENT_3D('',#91535,#58764,#58765);
#49153=AXIS2_PLACEMENT_3D('',#91558,#58766,#58767);
#49154=AXIS2_PLACEMENT_3D('',#91575,#58768,#58769);
#49155=AXIS2_PLACEMENT_3D('',#91598,#58770,#58771);
#49156=AXIS2_PLACEMENT_3D('',#91599,#58772,#58773);
#49157=AXIS2_PLACEMENT_3D('',#91632,#58774,#58775);
#49158=AXIS2_PLACEMENT_3D('',#91637,#58776,#58777);
#49159=AXIS2_PLACEMENT_3D('',#91654,#58778,#58779);
#49160=AXIS2_PLACEMENT_3D('',#91671,#58780,#58781);
#49161=AXIS2_PLACEMENT_3D('',#91694,#58782,#58783);
#49162=AXIS2_PLACEMENT_3D('',#91711,#58784,#58785);
#49163=AXIS2_PLACEMENT_3D('',#91744,#58786,#58787);
#49164=AXIS2_PLACEMENT_3D('',#91761,#58788,#58789);
#49165=AXIS2_PLACEMENT_3D('',#91784,#58790,#58791);
#49166=AXIS2_PLACEMENT_3D('',#91801,#58792,#58793);
#49167=AXIS2_PLACEMENT_3D('',#91824,#58794,#58795);
#49168=AXIS2_PLACEMENT_3D('',#91841,#58796,#58797);
#49169=AXIS2_PLACEMENT_3D('',#91864,#58798,#58799);
#49170=AXIS2_PLACEMENT_3D('',#91881,#58800,#58801);
#49171=AXIS2_PLACEMENT_3D('',#91909,#58802,#58803);
#49172=AXIS2_PLACEMENT_3D('',#91936,#58804,#58805);
#49173=AXIS2_PLACEMENT_3D('',#91941,#58806,#58807);
#49174=AXIS2_PLACEMENT_3D('',#91958,#58808,#58809);
#49175=AXIS2_PLACEMENT_3D('',#91975,#58810,#58811);
#49176=AXIS2_PLACEMENT_3D('',#91998,#58812,#58813);
#49177=AXIS2_PLACEMENT_3D('',#92015,#58814,#58815);
#49178=AXIS2_PLACEMENT_3D('',#92048,#58816,#58817);
#49179=AXIS2_PLACEMENT_3D('',#92065,#58818,#58819);
#49180=AXIS2_PLACEMENT_3D('',#92088,#58820,#58821);
#49181=AXIS2_PLACEMENT_3D('',#92105,#58822,#58823);
#49182=AXIS2_PLACEMENT_3D('',#92128,#58824,#58825);
#49183=AXIS2_PLACEMENT_3D('',#92145,#58826,#58827);
#49184=AXIS2_PLACEMENT_3D('',#92168,#58828,#58829);
#49185=AXIS2_PLACEMENT_3D('',#92206,#58830,#58831);
#49186=AXIS2_PLACEMENT_3D('',#92207,#58832,#58833);
#49187=AXIS2_PLACEMENT_3D('',#92240,#58834,#58835);
#49188=AXIS2_PLACEMENT_3D('',#92245,#58836,#58837);
#49189=AXIS2_PLACEMENT_3D('',#92262,#58838,#58839);
#49190=AXIS2_PLACEMENT_3D('',#92279,#58840,#58841);
#49191=AXIS2_PLACEMENT_3D('',#92302,#58842,#58843);
#49192=AXIS2_PLACEMENT_3D('',#92319,#58844,#58845);
#49193=AXIS2_PLACEMENT_3D('',#92352,#58846,#58847);
#49194=AXIS2_PLACEMENT_3D('',#92369,#58848,#58849);
#49195=AXIS2_PLACEMENT_3D('',#92392,#58850,#58851);
#49196=AXIS2_PLACEMENT_3D('',#92440,#58852,#58853);
#49197=AXIS2_PLACEMENT_3D('',#92447,#58854,#58855);
#49198=AXIS2_PLACEMENT_3D('',#92480,#58856,#58857);
#49199=AXIS2_PLACEMENT_3D('',#92497,#58858,#58859);
#49200=AXIS2_PLACEMENT_3D('',#92510,#58860,#58861);
#49201=AXIS2_PLACEMENT_3D('',#92511,#58862,#58863);
#49202=AXIS2_PLACEMENT_3D('',#92544,#58864,#58865);
#49203=AXIS2_PLACEMENT_3D('',#92549,#58866,#58867);
#49204=AXIS2_PLACEMENT_3D('',#92566,#58868,#58869);
#49205=AXIS2_PLACEMENT_3D('',#92583,#58870,#58871);
#49206=AXIS2_PLACEMENT_3D('',#92606,#58872,#58873);
#49207=AXIS2_PLACEMENT_3D('',#92623,#58874,#58875);
#49208=AXIS2_PLACEMENT_3D('',#92656,#58876,#58877);
#49209=AXIS2_PLACEMENT_3D('',#92673,#58878,#58879);
#49210=AXIS2_PLACEMENT_3D('',#92696,#58880,#58881);
#49211=AXIS2_PLACEMENT_3D('',#92744,#58882,#58883);
#49212=AXIS2_PLACEMENT_3D('',#92761,#58884,#58885);
#49213=AXIS2_PLACEMENT_3D('',#92784,#58886,#58887);
#49214=AXIS2_PLACEMENT_3D('',#92801,#58888,#58889);
#49215=AXIS2_PLACEMENT_3D('',#92814,#58890,#58891);
#49216=AXIS2_PLACEMENT_3D('',#92815,#58892,#58893);
#49217=AXIS2_PLACEMENT_3D('',#92848,#58894,#58895);
#49218=AXIS2_PLACEMENT_3D('',#92853,#58896,#58897);
#49219=AXIS2_PLACEMENT_3D('',#92870,#58898,#58899);
#49220=AXIS2_PLACEMENT_3D('',#92887,#58900,#58901);
#49221=AXIS2_PLACEMENT_3D('',#92910,#58902,#58903);
#49222=AXIS2_PLACEMENT_3D('',#92927,#58904,#58905);
#49223=AXIS2_PLACEMENT_3D('',#92960,#58906,#58907);
#49224=AXIS2_PLACEMENT_3D('',#92977,#58908,#58909);
#49225=AXIS2_PLACEMENT_3D('',#93000,#58910,#58911);
#49226=AXIS2_PLACEMENT_3D('',#93048,#58912,#58913);
#49227=AXIS2_PLACEMENT_3D('',#93065,#58914,#58915);
#49228=AXIS2_PLACEMENT_3D('',#93088,#58916,#58917);
#49229=AXIS2_PLACEMENT_3D('',#93105,#58918,#58919);
#49230=AXIS2_PLACEMENT_3D('',#93118,#58920,#58921);
#49231=AXIS2_PLACEMENT_3D('',#93119,#58922,#58923);
#49232=AXIS2_PLACEMENT_3D('',#93152,#58924,#58925);
#49233=AXIS2_PLACEMENT_3D('',#93157,#58926,#58927);
#49234=AXIS2_PLACEMENT_3D('',#93174,#58928,#58929);
#49235=AXIS2_PLACEMENT_3D('',#93191,#58930,#58931);
#49236=AXIS2_PLACEMENT_3D('',#93214,#58932,#58933);
#49237=AXIS2_PLACEMENT_3D('',#93231,#58934,#58935);
#49238=AXIS2_PLACEMENT_3D('',#93264,#58936,#58937);
#49239=AXIS2_PLACEMENT_3D('',#93281,#58938,#58939);
#49240=AXIS2_PLACEMENT_3D('',#93304,#58940,#58941);
#49241=AXIS2_PLACEMENT_3D('',#93352,#58942,#58943);
#49242=AXIS2_PLACEMENT_3D('',#93369,#58944,#58945);
#49243=AXIS2_PLACEMENT_3D('',#93392,#58946,#58947);
#49244=AXIS2_PLACEMENT_3D('',#93409,#58948,#58949);
#49245=AXIS2_PLACEMENT_3D('',#93422,#58950,#58951);
#49246=AXIS2_PLACEMENT_3D('',#93423,#58952,#58953);
#49247=AXIS2_PLACEMENT_3D('',#93456,#58954,#58955);
#49248=AXIS2_PLACEMENT_3D('',#93461,#58956,#58957);
#49249=AXIS2_PLACEMENT_3D('',#93478,#58958,#58959);
#49250=AXIS2_PLACEMENT_3D('',#93495,#58960,#58961);
#49251=AXIS2_PLACEMENT_3D('',#93518,#58962,#58963);
#49252=AXIS2_PLACEMENT_3D('',#93535,#58964,#58965);
#49253=AXIS2_PLACEMENT_3D('',#93568,#58966,#58967);
#49254=AXIS2_PLACEMENT_3D('',#93585,#58968,#58969);
#49255=AXIS2_PLACEMENT_3D('',#93608,#58970,#58971);
#49256=AXIS2_PLACEMENT_3D('',#93656,#58972,#58973);
#49257=AXIS2_PLACEMENT_3D('',#93673,#58974,#58975);
#49258=AXIS2_PLACEMENT_3D('',#93696,#58976,#58977);
#49259=AXIS2_PLACEMENT_3D('',#93713,#58978,#58979);
#49260=AXIS2_PLACEMENT_3D('',#93726,#58980,#58981);
#49261=AXIS2_PLACEMENT_3D('',#93727,#58982,#58983);
#49262=AXIS2_PLACEMENT_3D('',#93760,#58984,#58985);
#49263=AXIS2_PLACEMENT_3D('',#93765,#58986,#58987);
#49264=AXIS2_PLACEMENT_3D('',#93782,#58988,#58989);
#49265=AXIS2_PLACEMENT_3D('',#93799,#58990,#58991);
#49266=AXIS2_PLACEMENT_3D('',#93822,#58992,#58993);
#49267=AXIS2_PLACEMENT_3D('',#93839,#58994,#58995);
#49268=AXIS2_PLACEMENT_3D('',#93872,#58996,#58997);
#49269=AXIS2_PLACEMENT_3D('',#93889,#58998,#58999);
#49270=AXIS2_PLACEMENT_3D('',#93912,#59000,#59001);
#49271=AXIS2_PLACEMENT_3D('',#93960,#59002,#59003);
#49272=AXIS2_PLACEMENT_3D('',#93977,#59004,#59005);
#49273=AXIS2_PLACEMENT_3D('',#94000,#59006,#59007);
#49274=AXIS2_PLACEMENT_3D('',#94017,#59008,#59009);
#49275=AXIS2_PLACEMENT_3D('',#94030,#59010,#59011);
#49276=AXIS2_PLACEMENT_3D('',#94031,#59012,#59013);
#49277=AXIS2_PLACEMENT_3D('',#94064,#59014,#59015);
#49278=AXIS2_PLACEMENT_3D('',#94069,#59016,#59017);
#49279=AXIS2_PLACEMENT_3D('',#94086,#59018,#59019);
#49280=AXIS2_PLACEMENT_3D('',#94103,#59020,#59021);
#49281=AXIS2_PLACEMENT_3D('',#94126,#59022,#59023);
#49282=AXIS2_PLACEMENT_3D('',#94143,#59024,#59025);
#49283=AXIS2_PLACEMENT_3D('',#94176,#59026,#59027);
#49284=AXIS2_PLACEMENT_3D('',#94193,#59028,#59029);
#49285=AXIS2_PLACEMENT_3D('',#94216,#59030,#59031);
#49286=AXIS2_PLACEMENT_3D('',#94264,#59032,#59033);
#49287=AXIS2_PLACEMENT_3D('',#94281,#59034,#59035);
#49288=AXIS2_PLACEMENT_3D('',#94304,#59036,#59037);
#49289=AXIS2_PLACEMENT_3D('',#94321,#59038,#59039);
#49290=AXIS2_PLACEMENT_3D('',#94334,#59040,#59041);
#49291=AXIS2_PLACEMENT_3D('',#94335,#59042,#59043);
#49292=AXIS2_PLACEMENT_3D('',#94368,#59044,#59045);
#49293=AXIS2_PLACEMENT_3D('',#94373,#59046,#59047);
#49294=AXIS2_PLACEMENT_3D('',#94390,#59048,#59049);
#49295=AXIS2_PLACEMENT_3D('',#94407,#59050,#59051);
#49296=AXIS2_PLACEMENT_3D('',#94430,#59052,#59053);
#49297=AXIS2_PLACEMENT_3D('',#94447,#59054,#59055);
#49298=AXIS2_PLACEMENT_3D('',#94480,#59056,#59057);
#49299=AXIS2_PLACEMENT_3D('',#94497,#59058,#59059);
#49300=AXIS2_PLACEMENT_3D('',#94520,#59060,#59061);
#49301=AXIS2_PLACEMENT_3D('',#94568,#59062,#59063);
#49302=AXIS2_PLACEMENT_3D('',#94585,#59064,#59065);
#49303=AXIS2_PLACEMENT_3D('',#94608,#59066,#59067);
#49304=AXIS2_PLACEMENT_3D('',#94625,#59068,#59069);
#49305=AXIS2_PLACEMENT_3D('',#94638,#59070,#59071);
#49306=AXIS2_PLACEMENT_3D('',#94639,#59072,#59073);
#49307=AXIS2_PLACEMENT_3D('',#94672,#59074,#59075);
#49308=AXIS2_PLACEMENT_3D('',#94677,#59076,#59077);
#49309=AXIS2_PLACEMENT_3D('',#94694,#59078,#59079);
#49310=AXIS2_PLACEMENT_3D('',#94711,#59080,#59081);
#49311=AXIS2_PLACEMENT_3D('',#94734,#59082,#59083);
#49312=AXIS2_PLACEMENT_3D('',#94751,#59084,#59085);
#49313=AXIS2_PLACEMENT_3D('',#94784,#59086,#59087);
#49314=AXIS2_PLACEMENT_3D('',#94801,#59088,#59089);
#49315=AXIS2_PLACEMENT_3D('',#94824,#59090,#59091);
#49316=AXIS2_PLACEMENT_3D('',#94872,#59092,#59093);
#49317=AXIS2_PLACEMENT_3D('',#94889,#59094,#59095);
#49318=AXIS2_PLACEMENT_3D('',#94912,#59096,#59097);
#49319=AXIS2_PLACEMENT_3D('',#94929,#59098,#59099);
#49320=AXIS2_PLACEMENT_3D('',#94942,#59100,#59101);
#49321=AXIS2_PLACEMENT_3D('',#94943,#59102,#59103);
#49322=AXIS2_PLACEMENT_3D('',#94976,#59104,#59105);
#49323=AXIS2_PLACEMENT_3D('',#94981,#59106,#59107);
#49324=AXIS2_PLACEMENT_3D('',#94998,#59108,#59109);
#49325=AXIS2_PLACEMENT_3D('',#95015,#59110,#59111);
#49326=AXIS2_PLACEMENT_3D('',#95038,#59112,#59113);
#49327=AXIS2_PLACEMENT_3D('',#95055,#59114,#59115);
#49328=AXIS2_PLACEMENT_3D('',#95088,#59116,#59117);
#49329=AXIS2_PLACEMENT_3D('',#95105,#59118,#59119);
#49330=AXIS2_PLACEMENT_3D('',#95128,#59120,#59121);
#49331=AXIS2_PLACEMENT_3D('',#95176,#59122,#59123);
#49332=AXIS2_PLACEMENT_3D('',#95193,#59124,#59125);
#49333=AXIS2_PLACEMENT_3D('',#95216,#59126,#59127);
#49334=AXIS2_PLACEMENT_3D('',#95233,#59128,#59129);
#49335=AXIS2_PLACEMENT_3D('',#95246,#59130,#59131);
#49336=AXIS2_PLACEMENT_3D('',#95247,#59132,#59133);
#49337=AXIS2_PLACEMENT_3D('',#95280,#59134,#59135);
#49338=AXIS2_PLACEMENT_3D('',#95285,#59136,#59137);
#49339=AXIS2_PLACEMENT_3D('',#95302,#59138,#59139);
#49340=AXIS2_PLACEMENT_3D('',#95319,#59140,#59141);
#49341=AXIS2_PLACEMENT_3D('',#95342,#59142,#59143);
#49342=AXIS2_PLACEMENT_3D('',#95359,#59144,#59145);
#49343=AXIS2_PLACEMENT_3D('',#95392,#59146,#59147);
#49344=AXIS2_PLACEMENT_3D('',#95409,#59148,#59149);
#49345=AXIS2_PLACEMENT_3D('',#95432,#59150,#59151);
#49346=AXIS2_PLACEMENT_3D('',#95480,#59152,#59153);
#49347=AXIS2_PLACEMENT_3D('',#95497,#59154,#59155);
#49348=AXIS2_PLACEMENT_3D('',#95520,#59156,#59157);
#49349=AXIS2_PLACEMENT_3D('',#95537,#59158,#59159);
#49350=AXIS2_PLACEMENT_3D('',#95550,#59160,#59161);
#49351=AXIS2_PLACEMENT_3D('',#95551,#59162,#59163);
#49352=AXIS2_PLACEMENT_3D('',#95584,#59164,#59165);
#49353=AXIS2_PLACEMENT_3D('',#95589,#59166,#59167);
#49354=AXIS2_PLACEMENT_3D('',#95606,#59168,#59169);
#49355=AXIS2_PLACEMENT_3D('',#95623,#59170,#59171);
#49356=AXIS2_PLACEMENT_3D('',#95646,#59172,#59173);
#49357=AXIS2_PLACEMENT_3D('',#95663,#59174,#59175);
#49358=AXIS2_PLACEMENT_3D('',#95696,#59176,#59177);
#49359=AXIS2_PLACEMENT_3D('',#95713,#59178,#59179);
#49360=AXIS2_PLACEMENT_3D('',#95736,#59180,#59181);
#49361=AXIS2_PLACEMENT_3D('',#95784,#59182,#59183);
#49362=AXIS2_PLACEMENT_3D('',#95801,#59184,#59185);
#49363=AXIS2_PLACEMENT_3D('',#95824,#59186,#59187);
#49364=AXIS2_PLACEMENT_3D('',#95841,#59188,#59189);
#49365=AXIS2_PLACEMENT_3D('',#95854,#59190,#59191);
#49366=AXIS2_PLACEMENT_3D('',#95855,#59192,#59193);
#49367=AXIS2_PLACEMENT_3D('',#95888,#59194,#59195);
#49368=AXIS2_PLACEMENT_3D('',#95893,#59196,#59197);
#49369=AXIS2_PLACEMENT_3D('',#95910,#59198,#59199);
#49370=AXIS2_PLACEMENT_3D('',#95927,#59200,#59201);
#49371=AXIS2_PLACEMENT_3D('',#95950,#59202,#59203);
#49372=AXIS2_PLACEMENT_3D('',#95967,#59204,#59205);
#49373=AXIS2_PLACEMENT_3D('',#96000,#59206,#59207);
#49374=AXIS2_PLACEMENT_3D('',#96017,#59208,#59209);
#49375=AXIS2_PLACEMENT_3D('',#96040,#59210,#59211);
#49376=AXIS2_PLACEMENT_3D('',#96088,#59212,#59213);
#49377=AXIS2_PLACEMENT_3D('',#96105,#59214,#59215);
#49378=AXIS2_PLACEMENT_3D('',#96128,#59216,#59217);
#49379=AXIS2_PLACEMENT_3D('',#96145,#59218,#59219);
#49380=AXIS2_PLACEMENT_3D('',#96158,#59220,#59221);
#49381=AXIS2_PLACEMENT_3D('',#96159,#59222,#59223);
#49382=AXIS2_PLACEMENT_3D('',#96192,#59224,#59225);
#49383=AXIS2_PLACEMENT_3D('',#96197,#59226,#59227);
#49384=AXIS2_PLACEMENT_3D('',#96214,#59228,#59229);
#49385=AXIS2_PLACEMENT_3D('',#96231,#59230,#59231);
#49386=AXIS2_PLACEMENT_3D('',#96254,#59232,#59233);
#49387=AXIS2_PLACEMENT_3D('',#96271,#59234,#59235);
#49388=AXIS2_PLACEMENT_3D('',#96304,#59236,#59237);
#49389=AXIS2_PLACEMENT_3D('',#96321,#59238,#59239);
#49390=AXIS2_PLACEMENT_3D('',#96344,#59240,#59241);
#49391=AXIS2_PLACEMENT_3D('',#96392,#59242,#59243);
#49392=AXIS2_PLACEMENT_3D('',#96409,#59244,#59245);
#49393=AXIS2_PLACEMENT_3D('',#96432,#59246,#59247);
#49394=AXIS2_PLACEMENT_3D('',#96449,#59248,#59249);
#49395=AXIS2_PLACEMENT_3D('',#96462,#59250,#59251);
#49396=AXIS2_PLACEMENT_3D('',#96463,#59252,#59253);
#49397=AXIS2_PLACEMENT_3D('',#96496,#59254,#59255);
#49398=AXIS2_PLACEMENT_3D('',#96501,#59256,#59257);
#49399=AXIS2_PLACEMENT_3D('',#96518,#59258,#59259);
#49400=AXIS2_PLACEMENT_3D('',#96535,#59260,#59261);
#49401=AXIS2_PLACEMENT_3D('',#96558,#59262,#59263);
#49402=AXIS2_PLACEMENT_3D('',#96575,#59264,#59265);
#49403=AXIS2_PLACEMENT_3D('',#96608,#59266,#59267);
#49404=AXIS2_PLACEMENT_3D('',#96625,#59268,#59269);
#49405=AXIS2_PLACEMENT_3D('',#96648,#59270,#59271);
#49406=AXIS2_PLACEMENT_3D('',#96696,#59272,#59273);
#49407=AXIS2_PLACEMENT_3D('',#96713,#59274,#59275);
#49408=AXIS2_PLACEMENT_3D('',#96736,#59276,#59277);
#49409=AXIS2_PLACEMENT_3D('',#96753,#59278,#59279);
#49410=AXIS2_PLACEMENT_3D('',#96766,#59280,#59281);
#49411=AXIS2_PLACEMENT_3D('',#96767,#59282,#59283);
#49412=AXIS2_PLACEMENT_3D('',#96800,#59284,#59285);
#49413=AXIS2_PLACEMENT_3D('',#96805,#59286,#59287);
#49414=AXIS2_PLACEMENT_3D('',#96822,#59288,#59289);
#49415=AXIS2_PLACEMENT_3D('',#96839,#59290,#59291);
#49416=AXIS2_PLACEMENT_3D('',#96862,#59292,#59293);
#49417=AXIS2_PLACEMENT_3D('',#96879,#59294,#59295);
#49418=AXIS2_PLACEMENT_3D('',#96912,#59296,#59297);
#49419=AXIS2_PLACEMENT_3D('',#96929,#59298,#59299);
#49420=AXIS2_PLACEMENT_3D('',#96952,#59300,#59301);
#49421=AXIS2_PLACEMENT_3D('',#97000,#59302,#59303);
#49422=AXIS2_PLACEMENT_3D('',#97017,#59304,#59305);
#49423=AXIS2_PLACEMENT_3D('',#97040,#59306,#59307);
#49424=AXIS2_PLACEMENT_3D('',#97057,#59308,#59309);
#49425=AXIS2_PLACEMENT_3D('',#97070,#59310,#59311);
#49426=AXIS2_PLACEMENT_3D('',#97071,#59312,#59313);
#49427=AXIS2_PLACEMENT_3D('',#97104,#59314,#59315);
#49428=AXIS2_PLACEMENT_3D('',#97109,#59316,#59317);
#49429=AXIS2_PLACEMENT_3D('',#97126,#59318,#59319);
#49430=AXIS2_PLACEMENT_3D('',#97143,#59320,#59321);
#49431=AXIS2_PLACEMENT_3D('',#97166,#59322,#59323);
#49432=AXIS2_PLACEMENT_3D('',#97183,#59324,#59325);
#49433=AXIS2_PLACEMENT_3D('',#97216,#59326,#59327);
#49434=AXIS2_PLACEMENT_3D('',#97233,#59328,#59329);
#49435=AXIS2_PLACEMENT_3D('',#97256,#59330,#59331);
#49436=AXIS2_PLACEMENT_3D('',#97304,#59332,#59333);
#49437=AXIS2_PLACEMENT_3D('',#97321,#59334,#59335);
#49438=AXIS2_PLACEMENT_3D('',#97344,#59336,#59337);
#49439=AXIS2_PLACEMENT_3D('',#97361,#59338,#59339);
#49440=AXIS2_PLACEMENT_3D('',#97374,#59340,#59341);
#49441=AXIS2_PLACEMENT_3D('',#97375,#59342,#59343);
#49442=AXIS2_PLACEMENT_3D('',#97408,#59344,#59345);
#49443=AXIS2_PLACEMENT_3D('',#97413,#59346,#59347);
#49444=AXIS2_PLACEMENT_3D('',#97430,#59348,#59349);
#49445=AXIS2_PLACEMENT_3D('',#97447,#59350,#59351);
#49446=AXIS2_PLACEMENT_3D('',#97470,#59352,#59353);
#49447=AXIS2_PLACEMENT_3D('',#97487,#59354,#59355);
#49448=AXIS2_PLACEMENT_3D('',#97520,#59356,#59357);
#49449=AXIS2_PLACEMENT_3D('',#97537,#59358,#59359);
#49450=AXIS2_PLACEMENT_3D('',#97560,#59360,#59361);
#49451=AXIS2_PLACEMENT_3D('',#97608,#59362,#59363);
#49452=AXIS2_PLACEMENT_3D('',#97625,#59364,#59365);
#49453=AXIS2_PLACEMENT_3D('',#97648,#59366,#59367);
#49454=AXIS2_PLACEMENT_3D('',#97665,#59368,#59369);
#49455=AXIS2_PLACEMENT_3D('',#97678,#59370,#59371);
#49456=AXIS2_PLACEMENT_3D('',#97679,#59372,#59373);
#49457=AXIS2_PLACEMENT_3D('',#97712,#59374,#59375);
#49458=AXIS2_PLACEMENT_3D('',#97717,#59376,#59377);
#49459=AXIS2_PLACEMENT_3D('',#97734,#59378,#59379);
#49460=AXIS2_PLACEMENT_3D('',#97751,#59380,#59381);
#49461=AXIS2_PLACEMENT_3D('',#97774,#59382,#59383);
#49462=AXIS2_PLACEMENT_3D('',#97791,#59384,#59385);
#49463=AXIS2_PLACEMENT_3D('',#97824,#59386,#59387);
#49464=AXIS2_PLACEMENT_3D('',#97841,#59388,#59389);
#49465=AXIS2_PLACEMENT_3D('',#97864,#59390,#59391);
#49466=AXIS2_PLACEMENT_3D('',#97912,#59392,#59393);
#49467=AXIS2_PLACEMENT_3D('',#97929,#59394,#59395);
#49468=AXIS2_PLACEMENT_3D('',#97952,#59396,#59397);
#49469=AXIS2_PLACEMENT_3D('',#97969,#59398,#59399);
#49470=AXIS2_PLACEMENT_3D('',#97982,#59400,#59401);
#49471=AXIS2_PLACEMENT_3D('',#97983,#59402,#59403);
#49472=AXIS2_PLACEMENT_3D('',#98016,#59404,#59405);
#49473=AXIS2_PLACEMENT_3D('',#98021,#59406,#59407);
#49474=AXIS2_PLACEMENT_3D('',#98038,#59408,#59409);
#49475=AXIS2_PLACEMENT_3D('',#98055,#59410,#59411);
#49476=AXIS2_PLACEMENT_3D('',#98078,#59412,#59413);
#49477=AXIS2_PLACEMENT_3D('',#98095,#59414,#59415);
#49478=AXIS2_PLACEMENT_3D('',#98128,#59416,#59417);
#49479=AXIS2_PLACEMENT_3D('',#98145,#59418,#59419);
#49480=AXIS2_PLACEMENT_3D('',#98168,#59420,#59421);
#49481=AXIS2_PLACEMENT_3D('',#98216,#59422,#59423);
#49482=AXIS2_PLACEMENT_3D('',#98233,#59424,#59425);
#49483=AXIS2_PLACEMENT_3D('',#98256,#59426,#59427);
#49484=AXIS2_PLACEMENT_3D('',#98273,#59428,#59429);
#49485=AXIS2_PLACEMENT_3D('',#98286,#59430,#59431);
#49486=AXIS2_PLACEMENT_3D('',#98287,#59432,#59433);
#49487=AXIS2_PLACEMENT_3D('',#98320,#59434,#59435);
#49488=AXIS2_PLACEMENT_3D('',#98325,#59436,#59437);
#49489=AXIS2_PLACEMENT_3D('',#98342,#59438,#59439);
#49490=AXIS2_PLACEMENT_3D('',#98359,#59440,#59441);
#49491=AXIS2_PLACEMENT_3D('',#98382,#59442,#59443);
#49492=AXIS2_PLACEMENT_3D('',#98399,#59444,#59445);
#49493=AXIS2_PLACEMENT_3D('',#98432,#59446,#59447);
#49494=AXIS2_PLACEMENT_3D('',#98449,#59448,#59449);
#49495=AXIS2_PLACEMENT_3D('',#98472,#59450,#59451);
#49496=AXIS2_PLACEMENT_3D('',#98520,#59452,#59453);
#49497=AXIS2_PLACEMENT_3D('',#98537,#59454,#59455);
#49498=AXIS2_PLACEMENT_3D('',#98560,#59456,#59457);
#49499=AXIS2_PLACEMENT_3D('',#98577,#59458,#59459);
#49500=AXIS2_PLACEMENT_3D('',#98590,#59460,#59461);
#49501=AXIS2_PLACEMENT_3D('',#98591,#59462,#59463);
#49502=AXIS2_PLACEMENT_3D('',#98624,#59464,#59465);
#49503=AXIS2_PLACEMENT_3D('',#98629,#59466,#59467);
#49504=AXIS2_PLACEMENT_3D('',#98646,#59468,#59469);
#49505=AXIS2_PLACEMENT_3D('',#98663,#59470,#59471);
#49506=AXIS2_PLACEMENT_3D('',#98686,#59472,#59473);
#49507=AXIS2_PLACEMENT_3D('',#98703,#59474,#59475);
#49508=AXIS2_PLACEMENT_3D('',#98736,#59476,#59477);
#49509=AXIS2_PLACEMENT_3D('',#98753,#59478,#59479);
#49510=AXIS2_PLACEMENT_3D('',#98776,#59480,#59481);
#49511=AXIS2_PLACEMENT_3D('',#98824,#59482,#59483);
#49512=AXIS2_PLACEMENT_3D('',#98841,#59484,#59485);
#49513=AXIS2_PLACEMENT_3D('',#98864,#59486,#59487);
#49514=AXIS2_PLACEMENT_3D('',#98881,#59488,#59489);
#49515=AXIS2_PLACEMENT_3D('',#98894,#59490,#59491);
#49516=AXIS2_PLACEMENT_3D('',#98895,#59492,#59493);
#49517=AXIS2_PLACEMENT_3D('',#98928,#59494,#59495);
#49518=AXIS2_PLACEMENT_3D('',#98933,#59496,#59497);
#49519=AXIS2_PLACEMENT_3D('',#98950,#59498,#59499);
#49520=AXIS2_PLACEMENT_3D('',#98967,#59500,#59501);
#49521=AXIS2_PLACEMENT_3D('',#98990,#59502,#59503);
#49522=AXIS2_PLACEMENT_3D('',#99007,#59504,#59505);
#49523=AXIS2_PLACEMENT_3D('',#99040,#59506,#59507);
#49524=AXIS2_PLACEMENT_3D('',#99057,#59508,#59509);
#49525=AXIS2_PLACEMENT_3D('',#99080,#59510,#59511);
#49526=AXIS2_PLACEMENT_3D('',#99128,#59512,#59513);
#49527=AXIS2_PLACEMENT_3D('',#99145,#59514,#59515);
#49528=AXIS2_PLACEMENT_3D('',#99168,#59516,#59517);
#49529=AXIS2_PLACEMENT_3D('',#99185,#59518,#59519);
#49530=AXIS2_PLACEMENT_3D('',#99198,#59520,#59521);
#49531=AXIS2_PLACEMENT_3D('',#99199,#59522,#59523);
#49532=AXIS2_PLACEMENT_3D('',#99232,#59524,#59525);
#49533=AXIS2_PLACEMENT_3D('',#99237,#59526,#59527);
#49534=AXIS2_PLACEMENT_3D('',#99254,#59528,#59529);
#49535=AXIS2_PLACEMENT_3D('',#99271,#59530,#59531);
#49536=AXIS2_PLACEMENT_3D('',#99294,#59532,#59533);
#49537=AXIS2_PLACEMENT_3D('',#99311,#59534,#59535);
#49538=AXIS2_PLACEMENT_3D('',#99344,#59536,#59537);
#49539=AXIS2_PLACEMENT_3D('',#99361,#59538,#59539);
#49540=AXIS2_PLACEMENT_3D('',#99384,#59540,#59541);
#49541=AXIS2_PLACEMENT_3D('',#99432,#59542,#59543);
#49542=AXIS2_PLACEMENT_3D('',#99449,#59544,#59545);
#49543=AXIS2_PLACEMENT_3D('',#99472,#59546,#59547);
#49544=AXIS2_PLACEMENT_3D('',#99489,#59548,#59549);
#49545=AXIS2_PLACEMENT_3D('',#99502,#59550,#59551);
#49546=AXIS2_PLACEMENT_3D('',#99503,#59552,#59553);
#49547=AXIS2_PLACEMENT_3D('',#99536,#59554,#59555);
#49548=AXIS2_PLACEMENT_3D('',#99541,#59556,#59557);
#49549=AXIS2_PLACEMENT_3D('',#99558,#59558,#59559);
#49550=AXIS2_PLACEMENT_3D('',#99575,#59560,#59561);
#49551=AXIS2_PLACEMENT_3D('',#99598,#59562,#59563);
#49552=AXIS2_PLACEMENT_3D('',#99615,#59564,#59565);
#49553=AXIS2_PLACEMENT_3D('',#99648,#59566,#59567);
#49554=AXIS2_PLACEMENT_3D('',#99665,#59568,#59569);
#49555=AXIS2_PLACEMENT_3D('',#99688,#59570,#59571);
#49556=AXIS2_PLACEMENT_3D('',#99736,#59572,#59573);
#49557=AXIS2_PLACEMENT_3D('',#99753,#59574,#59575);
#49558=AXIS2_PLACEMENT_3D('',#99776,#59576,#59577);
#49559=AXIS2_PLACEMENT_3D('',#99793,#59578,#59579);
#49560=AXIS2_PLACEMENT_3D('',#99806,#59580,#59581);
#49561=AXIS2_PLACEMENT_3D('',#99807,#59582,#59583);
#49562=AXIS2_PLACEMENT_3D('',#99840,#59584,#59585);
#49563=AXIS2_PLACEMENT_3D('',#99845,#59586,#59587);
#49564=AXIS2_PLACEMENT_3D('',#99862,#59588,#59589);
#49565=AXIS2_PLACEMENT_3D('',#99879,#59590,#59591);
#49566=AXIS2_PLACEMENT_3D('',#99902,#59592,#59593);
#49567=AXIS2_PLACEMENT_3D('',#99919,#59594,#59595);
#49568=AXIS2_PLACEMENT_3D('',#99952,#59596,#59597);
#49569=AXIS2_PLACEMENT_3D('',#99969,#59598,#59599);
#49570=AXIS2_PLACEMENT_3D('',#99992,#59600,#59601);
#49571=AXIS2_PLACEMENT_3D('',#100040,#59602,#59603);
#49572=AXIS2_PLACEMENT_3D('',#100057,#59604,#59605);
#49573=AXIS2_PLACEMENT_3D('',#100080,#59606,#59607);
#49574=AXIS2_PLACEMENT_3D('',#100097,#59608,#59609);
#49575=AXIS2_PLACEMENT_3D('',#100110,#59610,#59611);
#49576=AXIS2_PLACEMENT_3D('',#100111,#59612,#59613);
#49577=AXIS2_PLACEMENT_3D('',#100144,#59614,#59615);
#49578=AXIS2_PLACEMENT_3D('',#100149,#59616,#59617);
#49579=AXIS2_PLACEMENT_3D('',#100166,#59618,#59619);
#49580=AXIS2_PLACEMENT_3D('',#100183,#59620,#59621);
#49581=AXIS2_PLACEMENT_3D('',#100206,#59622,#59623);
#49582=AXIS2_PLACEMENT_3D('',#100223,#59624,#59625);
#49583=AXIS2_PLACEMENT_3D('',#100256,#59626,#59627);
#49584=AXIS2_PLACEMENT_3D('',#100273,#59628,#59629);
#49585=AXIS2_PLACEMENT_3D('',#100296,#59630,#59631);
#49586=AXIS2_PLACEMENT_3D('',#100344,#59632,#59633);
#49587=AXIS2_PLACEMENT_3D('',#100361,#59634,#59635);
#49588=AXIS2_PLACEMENT_3D('',#100384,#59636,#59637);
#49589=AXIS2_PLACEMENT_3D('',#100401,#59638,#59639);
#49590=AXIS2_PLACEMENT_3D('',#100414,#59640,#59641);
#49591=AXIS2_PLACEMENT_3D('',#100415,#59642,#59643);
#49592=AXIS2_PLACEMENT_3D('',#100448,#59644,#59645);
#49593=AXIS2_PLACEMENT_3D('',#100453,#59646,#59647);
#49594=AXIS2_PLACEMENT_3D('',#100470,#59648,#59649);
#49595=AXIS2_PLACEMENT_3D('',#100487,#59650,#59651);
#49596=AXIS2_PLACEMENT_3D('',#100510,#59652,#59653);
#49597=AXIS2_PLACEMENT_3D('',#100527,#59654,#59655);
#49598=AXIS2_PLACEMENT_3D('',#100560,#59656,#59657);
#49599=AXIS2_PLACEMENT_3D('',#100577,#59658,#59659);
#49600=AXIS2_PLACEMENT_3D('',#100600,#59660,#59661);
#49601=AXIS2_PLACEMENT_3D('',#100648,#59662,#59663);
#49602=AXIS2_PLACEMENT_3D('',#100665,#59664,#59665);
#49603=AXIS2_PLACEMENT_3D('',#100688,#59666,#59667);
#49604=AXIS2_PLACEMENT_3D('',#100705,#59668,#59669);
#49605=AXIS2_PLACEMENT_3D('',#100718,#59670,#59671);
#49606=AXIS2_PLACEMENT_3D('',#100719,#59672,#59673);
#49607=AXIS2_PLACEMENT_3D('',#100752,#59674,#59675);
#49608=AXIS2_PLACEMENT_3D('',#100757,#59676,#59677);
#49609=AXIS2_PLACEMENT_3D('',#100774,#59678,#59679);
#49610=AXIS2_PLACEMENT_3D('',#100791,#59680,#59681);
#49611=AXIS2_PLACEMENT_3D('',#100814,#59682,#59683);
#49612=AXIS2_PLACEMENT_3D('',#100831,#59684,#59685);
#49613=AXIS2_PLACEMENT_3D('',#100864,#59686,#59687);
#49614=AXIS2_PLACEMENT_3D('',#100881,#59688,#59689);
#49615=AXIS2_PLACEMENT_3D('',#100904,#59690,#59691);
#49616=AXIS2_PLACEMENT_3D('',#100952,#59692,#59693);
#49617=AXIS2_PLACEMENT_3D('',#100969,#59694,#59695);
#49618=AXIS2_PLACEMENT_3D('',#100992,#59696,#59697);
#49619=AXIS2_PLACEMENT_3D('',#101009,#59698,#59699);
#49620=AXIS2_PLACEMENT_3D('',#101022,#59700,#59701);
#49621=AXIS2_PLACEMENT_3D('',#101023,#59702,#59703);
#49622=AXIS2_PLACEMENT_3D('',#101056,#59704,#59705);
#49623=AXIS2_PLACEMENT_3D('',#101061,#59706,#59707);
#49624=AXIS2_PLACEMENT_3D('',#101078,#59708,#59709);
#49625=AXIS2_PLACEMENT_3D('',#101095,#59710,#59711);
#49626=AXIS2_PLACEMENT_3D('',#101118,#59712,#59713);
#49627=AXIS2_PLACEMENT_3D('',#101135,#59714,#59715);
#49628=AXIS2_PLACEMENT_3D('',#101168,#59716,#59717);
#49629=AXIS2_PLACEMENT_3D('',#101185,#59718,#59719);
#49630=AXIS2_PLACEMENT_3D('',#101208,#59720,#59721);
#49631=AXIS2_PLACEMENT_3D('',#101256,#59722,#59723);
#49632=AXIS2_PLACEMENT_3D('',#101273,#59724,#59725);
#49633=AXIS2_PLACEMENT_3D('',#101296,#59726,#59727);
#49634=AXIS2_PLACEMENT_3D('',#101313,#59728,#59729);
#49635=AXIS2_PLACEMENT_3D('',#101326,#59730,#59731);
#49636=AXIS2_PLACEMENT_3D('',#101327,#59732,#59733);
#49637=AXIS2_PLACEMENT_3D('',#101360,#59734,#59735);
#49638=AXIS2_PLACEMENT_3D('',#101365,#59736,#59737);
#49639=AXIS2_PLACEMENT_3D('',#101382,#59738,#59739);
#49640=AXIS2_PLACEMENT_3D('',#101399,#59740,#59741);
#49641=AXIS2_PLACEMENT_3D('',#101422,#59742,#59743);
#49642=AXIS2_PLACEMENT_3D('',#101439,#59744,#59745);
#49643=AXIS2_PLACEMENT_3D('',#101472,#59746,#59747);
#49644=AXIS2_PLACEMENT_3D('',#101489,#59748,#59749);
#49645=AXIS2_PLACEMENT_3D('',#101512,#59750,#59751);
#49646=AXIS2_PLACEMENT_3D('',#101560,#59752,#59753);
#49647=AXIS2_PLACEMENT_3D('',#101577,#59754,#59755);
#49648=AXIS2_PLACEMENT_3D('',#101600,#59756,#59757);
#49649=AXIS2_PLACEMENT_3D('',#101617,#59758,#59759);
#49650=AXIS2_PLACEMENT_3D('',#101630,#59760,#59761);
#49651=AXIS2_PLACEMENT_3D('',#101631,#59762,#59763);
#49652=AXIS2_PLACEMENT_3D('',#101664,#59764,#59765);
#49653=AXIS2_PLACEMENT_3D('',#101669,#59766,#59767);
#49654=AXIS2_PLACEMENT_3D('',#101686,#59768,#59769);
#49655=AXIS2_PLACEMENT_3D('',#101703,#59770,#59771);
#49656=AXIS2_PLACEMENT_3D('',#101726,#59772,#59773);
#49657=AXIS2_PLACEMENT_3D('',#101743,#59774,#59775);
#49658=AXIS2_PLACEMENT_3D('',#101776,#59776,#59777);
#49659=AXIS2_PLACEMENT_3D('',#101793,#59778,#59779);
#49660=AXIS2_PLACEMENT_3D('',#101816,#59780,#59781);
#49661=AXIS2_PLACEMENT_3D('',#101864,#59782,#59783);
#49662=AXIS2_PLACEMENT_3D('',#101881,#59784,#59785);
#49663=AXIS2_PLACEMENT_3D('',#101904,#59786,#59787);
#49664=AXIS2_PLACEMENT_3D('',#101921,#59788,#59789);
#49665=AXIS2_PLACEMENT_3D('',#101934,#59790,#59791);
#49666=AXIS2_PLACEMENT_3D('',#101935,#59792,#59793);
#49667=AXIS2_PLACEMENT_3D('',#101968,#59794,#59795);
#49668=AXIS2_PLACEMENT_3D('',#101973,#59796,#59797);
#49669=AXIS2_PLACEMENT_3D('',#101990,#59798,#59799);
#49670=AXIS2_PLACEMENT_3D('',#102007,#59800,#59801);
#49671=AXIS2_PLACEMENT_3D('',#102030,#59802,#59803);
#49672=AXIS2_PLACEMENT_3D('',#102047,#59804,#59805);
#49673=AXIS2_PLACEMENT_3D('',#102080,#59806,#59807);
#49674=AXIS2_PLACEMENT_3D('',#102097,#59808,#59809);
#49675=AXIS2_PLACEMENT_3D('',#102120,#59810,#59811);
#49676=AXIS2_PLACEMENT_3D('',#102168,#59812,#59813);
#49677=AXIS2_PLACEMENT_3D('',#102185,#59814,#59815);
#49678=AXIS2_PLACEMENT_3D('',#102208,#59816,#59817);
#49679=AXIS2_PLACEMENT_3D('',#102225,#59818,#59819);
#49680=AXIS2_PLACEMENT_3D('',#102238,#59820,#59821);
#49681=AXIS2_PLACEMENT_3D('',#102239,#59822,#59823);
#49682=AXIS2_PLACEMENT_3D('',#102272,#59824,#59825);
#49683=AXIS2_PLACEMENT_3D('',#102277,#59826,#59827);
#49684=AXIS2_PLACEMENT_3D('',#102294,#59828,#59829);
#49685=AXIS2_PLACEMENT_3D('',#102311,#59830,#59831);
#49686=AXIS2_PLACEMENT_3D('',#102334,#59832,#59833);
#49687=AXIS2_PLACEMENT_3D('',#102351,#59834,#59835);
#49688=AXIS2_PLACEMENT_3D('',#102384,#59836,#59837);
#49689=AXIS2_PLACEMENT_3D('',#102401,#59838,#59839);
#49690=AXIS2_PLACEMENT_3D('',#102424,#59840,#59841);
#49691=AXIS2_PLACEMENT_3D('',#102472,#59842,#59843);
#49692=AXIS2_PLACEMENT_3D('',#102489,#59844,#59845);
#49693=AXIS2_PLACEMENT_3D('',#102512,#59846,#59847);
#49694=AXIS2_PLACEMENT_3D('',#102529,#59848,#59849);
#49695=AXIS2_PLACEMENT_3D('',#102542,#59850,#59851);
#49696=AXIS2_PLACEMENT_3D('',#102543,#59852,#59853);
#49697=AXIS2_PLACEMENT_3D('',#102576,#59854,#59855);
#49698=AXIS2_PLACEMENT_3D('',#102581,#59856,#59857);
#49699=AXIS2_PLACEMENT_3D('',#102598,#59858,#59859);
#49700=AXIS2_PLACEMENT_3D('',#102615,#59860,#59861);
#49701=AXIS2_PLACEMENT_3D('',#102638,#59862,#59863);
#49702=AXIS2_PLACEMENT_3D('',#102655,#59864,#59865);
#49703=AXIS2_PLACEMENT_3D('',#102688,#59866,#59867);
#49704=AXIS2_PLACEMENT_3D('',#102705,#59868,#59869);
#49705=AXIS2_PLACEMENT_3D('',#102728,#59870,#59871);
#49706=AXIS2_PLACEMENT_3D('',#102776,#59872,#59873);
#49707=AXIS2_PLACEMENT_3D('',#102793,#59874,#59875);
#49708=AXIS2_PLACEMENT_3D('',#102816,#59876,#59877);
#49709=AXIS2_PLACEMENT_3D('',#102833,#59878,#59879);
#49710=AXIS2_PLACEMENT_3D('',#102846,#59880,#59881);
#49711=AXIS2_PLACEMENT_3D('',#102847,#59882,#59883);
#49712=AXIS2_PLACEMENT_3D('',#102880,#59884,#59885);
#49713=AXIS2_PLACEMENT_3D('',#102885,#59886,#59887);
#49714=AXIS2_PLACEMENT_3D('',#102902,#59888,#59889);
#49715=AXIS2_PLACEMENT_3D('',#102919,#59890,#59891);
#49716=AXIS2_PLACEMENT_3D('',#102942,#59892,#59893);
#49717=AXIS2_PLACEMENT_3D('',#102959,#59894,#59895);
#49718=AXIS2_PLACEMENT_3D('',#102992,#59896,#59897);
#49719=AXIS2_PLACEMENT_3D('',#103009,#59898,#59899);
#49720=AXIS2_PLACEMENT_3D('',#103032,#59900,#59901);
#49721=AXIS2_PLACEMENT_3D('',#103080,#59902,#59903);
#49722=AXIS2_PLACEMENT_3D('',#103097,#59904,#59905);
#49723=AXIS2_PLACEMENT_3D('',#103120,#59906,#59907);
#49724=AXIS2_PLACEMENT_3D('',#103137,#59908,#59909);
#49725=AXIS2_PLACEMENT_3D('',#103150,#59910,#59911);
#49726=AXIS2_PLACEMENT_3D('',#103151,#59912,#59913);
#49727=AXIS2_PLACEMENT_3D('',#103184,#59914,#59915);
#49728=AXIS2_PLACEMENT_3D('',#103189,#59916,#59917);
#49729=AXIS2_PLACEMENT_3D('',#103206,#59918,#59919);
#49730=AXIS2_PLACEMENT_3D('',#103223,#59920,#59921);
#49731=AXIS2_PLACEMENT_3D('',#103246,#59922,#59923);
#49732=AXIS2_PLACEMENT_3D('',#103263,#59924,#59925);
#49733=AXIS2_PLACEMENT_3D('',#103296,#59926,#59927);
#49734=AXIS2_PLACEMENT_3D('',#103313,#59928,#59929);
#49735=AXIS2_PLACEMENT_3D('',#103336,#59930,#59931);
#49736=AXIS2_PLACEMENT_3D('',#103384,#59932,#59933);
#49737=AXIS2_PLACEMENT_3D('',#103401,#59934,#59935);
#49738=AXIS2_PLACEMENT_3D('',#103424,#59936,#59937);
#49739=AXIS2_PLACEMENT_3D('',#103441,#59938,#59939);
#49740=AXIS2_PLACEMENT_3D('',#103454,#59940,#59941);
#49741=AXIS2_PLACEMENT_3D('',#103455,#59942,#59943);
#49742=AXIS2_PLACEMENT_3D('',#103488,#59944,#59945);
#49743=AXIS2_PLACEMENT_3D('',#103493,#59946,#59947);
#49744=AXIS2_PLACEMENT_3D('',#103510,#59948,#59949);
#49745=AXIS2_PLACEMENT_3D('',#103527,#59950,#59951);
#49746=AXIS2_PLACEMENT_3D('',#103550,#59952,#59953);
#49747=AXIS2_PLACEMENT_3D('',#103567,#59954,#59955);
#49748=AXIS2_PLACEMENT_3D('',#103600,#59956,#59957);
#49749=AXIS2_PLACEMENT_3D('',#103617,#59958,#59959);
#49750=AXIS2_PLACEMENT_3D('',#103640,#59960,#59961);
#49751=AXIS2_PLACEMENT_3D('',#103688,#59962,#59963);
#49752=AXIS2_PLACEMENT_3D('',#103705,#59964,#59965);
#49753=AXIS2_PLACEMENT_3D('',#103728,#59966,#59967);
#49754=AXIS2_PLACEMENT_3D('',#103745,#59968,#59969);
#49755=AXIS2_PLACEMENT_3D('',#103758,#59970,#59971);
#49756=AXIS2_PLACEMENT_3D('',#103759,#59972,#59973);
#49757=AXIS2_PLACEMENT_3D('',#103792,#59974,#59975);
#49758=AXIS2_PLACEMENT_3D('',#103797,#59976,#59977);
#49759=AXIS2_PLACEMENT_3D('',#103814,#59978,#59979);
#49760=AXIS2_PLACEMENT_3D('',#103831,#59980,#59981);
#49761=AXIS2_PLACEMENT_3D('',#103854,#59982,#59983);
#49762=AXIS2_PLACEMENT_3D('',#103871,#59984,#59985);
#49763=AXIS2_PLACEMENT_3D('',#103904,#59986,#59987);
#49764=AXIS2_PLACEMENT_3D('',#103921,#59988,#59989);
#49765=AXIS2_PLACEMENT_3D('',#103944,#59990,#59991);
#49766=AXIS2_PLACEMENT_3D('',#103992,#59992,#59993);
#49767=AXIS2_PLACEMENT_3D('',#104009,#59994,#59995);
#49768=AXIS2_PLACEMENT_3D('',#104032,#59996,#59997);
#49769=AXIS2_PLACEMENT_3D('',#104049,#59998,#59999);
#49770=AXIS2_PLACEMENT_3D('',#104062,#60000,#60001);
#49771=AXIS2_PLACEMENT_3D('',#104063,#60002,#60003);
#49772=AXIS2_PLACEMENT_3D('',#104112,#60004,#60005);
#49773=AXIS2_PLACEMENT_3D('',#104129,#60006,#60007);
#49774=AXIS2_PLACEMENT_3D('',#104136,#60008,#60009);
#49775=AXIS2_PLACEMENT_3D('',#104141,#60010,#60011);
#49776=AXIS2_PLACEMENT_3D('',#104158,#60012,#60013);
#49777=AXIS2_PLACEMENT_3D('',#104175,#60014,#60015);
#49778=AXIS2_PLACEMENT_3D('',#104208,#60016,#60017);
#49779=AXIS2_PLACEMENT_3D('',#104225,#60018,#60019);
#49780=AXIS2_PLACEMENT_3D('',#104248,#60020,#60021);
#49781=AXIS2_PLACEMENT_3D('',#104296,#60022,#60023);
#49782=AXIS2_PLACEMENT_3D('',#104313,#60024,#60025);
#49783=AXIS2_PLACEMENT_3D('',#104336,#60026,#60027);
#49784=AXIS2_PLACEMENT_3D('',#104353,#60028,#60029);
#49785=AXIS2_PLACEMENT_3D('',#104366,#60030,#60031);
#49786=AXIS2_PLACEMENT_3D('',#104367,#60032,#60033);
#49787=AXIS2_PLACEMENT_3D('',#104400,#60034,#60035);
#49788=AXIS2_PLACEMENT_3D('',#104405,#60036,#60037);
#49789=AXIS2_PLACEMENT_3D('',#104422,#60038,#60039);
#49790=AXIS2_PLACEMENT_3D('',#104439,#60040,#60041);
#49791=AXIS2_PLACEMENT_3D('',#104462,#60042,#60043);
#49792=AXIS2_PLACEMENT_3D('',#104479,#60044,#60045);
#49793=AXIS2_PLACEMENT_3D('',#104512,#60046,#60047);
#49794=AXIS2_PLACEMENT_3D('',#104529,#60048,#60049);
#49795=AXIS2_PLACEMENT_3D('',#104552,#60050,#60051);
#49796=AXIS2_PLACEMENT_3D('',#104600,#60052,#60053);
#49797=AXIS2_PLACEMENT_3D('',#104617,#60054,#60055);
#49798=AXIS2_PLACEMENT_3D('',#104640,#60056,#60057);
#49799=AXIS2_PLACEMENT_3D('',#104657,#60058,#60059);
#49800=AXIS2_PLACEMENT_3D('',#104670,#60060,#60061);
#49801=AXIS2_PLACEMENT_3D('',#104671,#60062,#60063);
#49802=AXIS2_PLACEMENT_3D('',#104704,#60064,#60065);
#49803=AXIS2_PLACEMENT_3D('',#104709,#60066,#60067);
#49804=AXIS2_PLACEMENT_3D('',#104726,#60068,#60069);
#49805=AXIS2_PLACEMENT_3D('',#104743,#60070,#60071);
#49806=AXIS2_PLACEMENT_3D('',#104766,#60072,#60073);
#49807=AXIS2_PLACEMENT_3D('',#104783,#60074,#60075);
#49808=AXIS2_PLACEMENT_3D('',#104816,#60076,#60077);
#49809=AXIS2_PLACEMENT_3D('',#104833,#60078,#60079);
#49810=AXIS2_PLACEMENT_3D('',#104856,#60080,#60081);
#49811=AXIS2_PLACEMENT_3D('',#104904,#60082,#60083);
#49812=AXIS2_PLACEMENT_3D('',#104921,#60084,#60085);
#49813=AXIS2_PLACEMENT_3D('',#104944,#60086,#60087);
#49814=AXIS2_PLACEMENT_3D('',#104961,#60088,#60089);
#49815=AXIS2_PLACEMENT_3D('',#104974,#60090,#60091);
#49816=AXIS2_PLACEMENT_3D('',#104975,#60092,#60093);
#49817=AXIS2_PLACEMENT_3D('',#105008,#60094,#60095);
#49818=AXIS2_PLACEMENT_3D('',#105013,#60096,#60097);
#49819=AXIS2_PLACEMENT_3D('',#105030,#60098,#60099);
#49820=AXIS2_PLACEMENT_3D('',#105047,#60100,#60101);
#49821=AXIS2_PLACEMENT_3D('',#105070,#60102,#60103);
#49822=AXIS2_PLACEMENT_3D('',#105087,#60104,#60105);
#49823=AXIS2_PLACEMENT_3D('',#105120,#60106,#60107);
#49824=AXIS2_PLACEMENT_3D('',#105137,#60108,#60109);
#49825=AXIS2_PLACEMENT_3D('',#105160,#60110,#60111);
#49826=AXIS2_PLACEMENT_3D('',#105208,#60112,#60113);
#49827=AXIS2_PLACEMENT_3D('',#105225,#60114,#60115);
#49828=AXIS2_PLACEMENT_3D('',#105248,#60116,#60117);
#49829=AXIS2_PLACEMENT_3D('',#105265,#60118,#60119);
#49830=AXIS2_PLACEMENT_3D('',#105278,#60120,#60121);
#49831=AXIS2_PLACEMENT_3D('',#105279,#60122,#60123);
#49832=AXIS2_PLACEMENT_3D('',#105312,#60124,#60125);
#49833=AXIS2_PLACEMENT_3D('',#105317,#60126,#60127);
#49834=AXIS2_PLACEMENT_3D('',#105334,#60128,#60129);
#49835=AXIS2_PLACEMENT_3D('',#105351,#60130,#60131);
#49836=AXIS2_PLACEMENT_3D('',#105374,#60132,#60133);
#49837=AXIS2_PLACEMENT_3D('',#105391,#60134,#60135);
#49838=AXIS2_PLACEMENT_3D('',#105424,#60136,#60137);
#49839=AXIS2_PLACEMENT_3D('',#105441,#60138,#60139);
#49840=AXIS2_PLACEMENT_3D('',#105464,#60140,#60141);
#49841=AXIS2_PLACEMENT_3D('',#105512,#60142,#60143);
#49842=AXIS2_PLACEMENT_3D('',#105529,#60144,#60145);
#49843=AXIS2_PLACEMENT_3D('',#105552,#60146,#60147);
#49844=AXIS2_PLACEMENT_3D('',#105569,#60148,#60149);
#49845=AXIS2_PLACEMENT_3D('',#105582,#60150,#60151);
#49846=AXIS2_PLACEMENT_3D('',#105583,#60152,#60153);
#49847=AXIS2_PLACEMENT_3D('',#105616,#60154,#60155);
#49848=AXIS2_PLACEMENT_3D('',#105621,#60156,#60157);
#49849=AXIS2_PLACEMENT_3D('',#105638,#60158,#60159);
#49850=AXIS2_PLACEMENT_3D('',#105655,#60160,#60161);
#49851=AXIS2_PLACEMENT_3D('',#105678,#60162,#60163);
#49852=AXIS2_PLACEMENT_3D('',#105695,#60164,#60165);
#49853=AXIS2_PLACEMENT_3D('',#105728,#60166,#60167);
#49854=AXIS2_PLACEMENT_3D('',#105745,#60168,#60169);
#49855=AXIS2_PLACEMENT_3D('',#105768,#60170,#60171);
#49856=AXIS2_PLACEMENT_3D('',#105816,#60172,#60173);
#49857=AXIS2_PLACEMENT_3D('',#105833,#60174,#60175);
#49858=AXIS2_PLACEMENT_3D('',#105856,#60176,#60177);
#49859=AXIS2_PLACEMENT_3D('',#105873,#60178,#60179);
#49860=AXIS2_PLACEMENT_3D('',#105886,#60180,#60181);
#49861=AXIS2_PLACEMENT_3D('',#105887,#60182,#60183);
#49862=AXIS2_PLACEMENT_3D('',#105920,#60184,#60185);
#49863=AXIS2_PLACEMENT_3D('',#105925,#60186,#60187);
#49864=AXIS2_PLACEMENT_3D('',#105942,#60188,#60189);
#49865=AXIS2_PLACEMENT_3D('',#105959,#60190,#60191);
#49866=AXIS2_PLACEMENT_3D('',#105982,#60192,#60193);
#49867=AXIS2_PLACEMENT_3D('',#105999,#60194,#60195);
#49868=AXIS2_PLACEMENT_3D('',#106032,#60196,#60197);
#49869=AXIS2_PLACEMENT_3D('',#106049,#60198,#60199);
#49870=AXIS2_PLACEMENT_3D('',#106072,#60200,#60201);
#49871=AXIS2_PLACEMENT_3D('',#106120,#60202,#60203);
#49872=AXIS2_PLACEMENT_3D('',#106137,#60204,#60205);
#49873=AXIS2_PLACEMENT_3D('',#106160,#60206,#60207);
#49874=AXIS2_PLACEMENT_3D('',#106177,#60208,#60209);
#49875=AXIS2_PLACEMENT_3D('',#106190,#60210,#60211);
#49876=AXIS2_PLACEMENT_3D('',#106191,#60212,#60213);
#49877=AXIS2_PLACEMENT_3D('',#106224,#60214,#60215);
#49878=AXIS2_PLACEMENT_3D('',#106225,#60216,#60217);
#49879=AXIS2_PLACEMENT_3D('',#106227,#60218,#60219);
#49880=AXIS2_PLACEMENT_3D('',#106230,#60221,#60222);
#49881=AXIS2_PLACEMENT_3D('',#106231,#60223,#60224);
#49882=AXIS2_PLACEMENT_3D('',#106233,#60225,#60226);
#49883=AXIS2_PLACEMENT_3D('',#106236,#60228,#60229);
#49884=AXIS2_PLACEMENT_3D('',#106237,#60230,#60231);
#49885=AXIS2_PLACEMENT_3D('',#106239,#60232,#60233);
#49886=AXIS2_PLACEMENT_3D('',#106242,#60235,#60236);
#49887=AXIS2_PLACEMENT_3D('',#106243,#60237,#60238);
#49888=AXIS2_PLACEMENT_3D('',#106244,#60239,#60240);
#49889=AXIS2_PLACEMENT_3D('',#106245,#60241,#60242);
#49890=AXIS2_PLACEMENT_3D('',#106246,#60243,#60244);
#49891=AXIS2_PLACEMENT_3D('',#106247,#60245,#60246);
#49892=AXIS2_PLACEMENT_3D('',#106249,#60247,#60248);
#49893=AXIS2_PLACEMENT_3D('',#106252,#60250,#60251);
#49894=AXIS2_PLACEMENT_3D('',#106253,#60252,#60253);
#49895=AXIS2_PLACEMENT_3D('',#106255,#60254,#60255);
#49896=AXIS2_PLACEMENT_3D('',#106258,#60257,#60258);
#49897=AXIS2_PLACEMENT_3D('',#106259,#60259,#60260);
#49898=AXIS2_PLACEMENT_3D('',#106260,#60261,#60262);
#49899=AXIS2_PLACEMENT_3D('',#106261,#60263,#60264);
#49900=AXIS2_PLACEMENT_3D('',#106262,#60265,#60266);
#49901=AXIS2_PLACEMENT_3D('',#106264,#60267,#60268);
#49902=AXIS2_PLACEMENT_3D('',#106267,#60270,#60271);
#49903=AXIS2_PLACEMENT_3D('',#106268,#60272,#60273);
#49904=AXIS2_PLACEMENT_3D('',#106270,#60274,#60275);
#49905=AXIS2_PLACEMENT_3D('',#106273,#60277,#60278);
#49906=AXIS2_PLACEMENT_3D('',#106274,#60279,#60280);
#49907=AXIS2_PLACEMENT_3D('',#106276,#60281,#60282);
#49908=AXIS2_PLACEMENT_3D('',#106279,#60284,#60285);
#49909=AXIS2_PLACEMENT_3D('',#106280,#60286,#60287);
#49910=AXIS2_PLACEMENT_3D('',#106282,#60288,#60289);
#49911=AXIS2_PLACEMENT_3D('',#106285,#60291,#60292);
#49912=AXIS2_PLACEMENT_3D('',#106286,#60293,#60294);
#49913=AXIS2_PLACEMENT_3D('',#106291,#60296,#60297);
#49914=AXIS2_PLACEMENT_3D('',#106294,#60299,#60300);
#49915=AXIS2_PLACEMENT_3D('',#106295,#60301,#60302);
#49916=AXIS2_PLACEMENT_3D('',#106300,#60304,#60305);
#49917=AXIS2_PLACEMENT_3D('',#106303,#60307,#60308);
#49918=AXIS2_PLACEMENT_3D('',#106304,#60309,#60310);
#49919=AXIS2_PLACEMENT_3D('',#106309,#60312,#60313);
#49920=AXIS2_PLACEMENT_3D('',#106312,#60315,#60316);
#49921=AXIS2_PLACEMENT_3D('',#106313,#60317,#60318);
#49922=AXIS2_PLACEMENT_3D('',#106318,#60320,#60321);
#49923=AXIS2_PLACEMENT_3D('',#106321,#60323,#60324);
#49924=AXIS2_PLACEMENT_3D('',#106322,#60325,#60326);
#49925=AXIS2_PLACEMENT_3D('',#106327,#60328,#60329);
#49926=AXIS2_PLACEMENT_3D('',#106330,#60331,#60332);
#49927=AXIS2_PLACEMENT_3D('',#106331,#60333,#60334);
#49928=AXIS2_PLACEMENT_3D('',#106336,#60336,#60337);
#49929=AXIS2_PLACEMENT_3D('',#106339,#60339,#60340);
#49930=AXIS2_PLACEMENT_3D('',#106340,#60341,#60342);
#49931=AXIS2_PLACEMENT_3D('',#106345,#60344,#60345);
#49932=AXIS2_PLACEMENT_3D('',#106348,#60347,#60348);
#49933=AXIS2_PLACEMENT_3D('',#106349,#60349,#60350);
#49934=AXIS2_PLACEMENT_3D('',#106354,#60352,#60353);
#49935=AXIS2_PLACEMENT_3D('',#106357,#60355,#60356);
#49936=AXIS2_PLACEMENT_3D('',#106358,#60357,#60358);
#49937=AXIS2_PLACEMENT_3D('',#106363,#60360,#60361);
#49938=AXIS2_PLACEMENT_3D('',#106366,#60363,#60364);
#49939=AXIS2_PLACEMENT_3D('',#106367,#60365,#60366);
#49940=AXIS2_PLACEMENT_3D('',#106372,#60368,#60369);
#49941=AXIS2_PLACEMENT_3D('',#106375,#60371,#60372);
#49942=AXIS2_PLACEMENT_3D('',#106376,#60373,#60374);
#49943=AXIS2_PLACEMENT_3D('',#106381,#60376,#60377);
#49944=AXIS2_PLACEMENT_3D('',#106384,#60379,#60380);
#49945=AXIS2_PLACEMENT_3D('',#106385,#60381,#60382);
#49946=AXIS2_PLACEMENT_3D('',#106390,#60384,#60385);
#49947=AXIS2_PLACEMENT_3D('',#106393,#60387,#60388);
#49948=AXIS2_PLACEMENT_3D('',#106394,#60389,#60390);
#49949=AXIS2_PLACEMENT_3D('',#106399,#60392,#60393);
#49950=AXIS2_PLACEMENT_3D('',#106402,#60395,#60396);
#49951=AXIS2_PLACEMENT_3D('',#106403,#60397,#60398);
#49952=AXIS2_PLACEMENT_3D('',#106408,#60400,#60401);
#49953=AXIS2_PLACEMENT_3D('',#106411,#60403,#60404);
#49954=AXIS2_PLACEMENT_3D('',#106412,#60405,#60406);
#49955=AXIS2_PLACEMENT_3D('',#106417,#60408,#60409);
#49956=AXIS2_PLACEMENT_3D('',#106420,#60411,#60412);
#49957=AXIS2_PLACEMENT_3D('',#106421,#60413,#60414);
#49958=AXIS2_PLACEMENT_3D('',#106426,#60416,#60417);
#49959=AXIS2_PLACEMENT_3D('',#106429,#60419,#60420);
#49960=AXIS2_PLACEMENT_3D('',#106430,#60421,#60422);
#49961=AXIS2_PLACEMENT_3D('',#106435,#60424,#60425);
#49962=AXIS2_PLACEMENT_3D('',#106438,#60427,#60428);
#49963=AXIS2_PLACEMENT_3D('',#106439,#60429,#60430);
#49964=AXIS2_PLACEMENT_3D('',#106444,#60432,#60433);
#49965=AXIS2_PLACEMENT_3D('',#106447,#60435,#60436);
#49966=AXIS2_PLACEMENT_3D('',#106448,#60437,#60438);
#49967=AXIS2_PLACEMENT_3D('',#106453,#60440,#60441);
#49968=AXIS2_PLACEMENT_3D('',#106456,#60443,#60444);
#49969=AXIS2_PLACEMENT_3D('',#106457,#60445,#60446);
#49970=AXIS2_PLACEMENT_3D('',#106462,#60448,#60449);
#49971=AXIS2_PLACEMENT_3D('',#106465,#60451,#60452);
#49972=AXIS2_PLACEMENT_3D('',#106466,#60453,#60454);
#49973=AXIS2_PLACEMENT_3D('',#106471,#60456,#60457);
#49974=AXIS2_PLACEMENT_3D('',#106474,#60459,#60460);
#49975=AXIS2_PLACEMENT_3D('',#106475,#60461,#60462);
#49976=AXIS2_PLACEMENT_3D('',#106480,#60464,#60465);
#49977=AXIS2_PLACEMENT_3D('',#106483,#60467,#60468);
#49978=AXIS2_PLACEMENT_3D('',#106484,#60469,#60470);
#49979=AXIS2_PLACEMENT_3D('',#106489,#60472,#60473);
#49980=AXIS2_PLACEMENT_3D('',#106492,#60475,#60476);
#49981=AXIS2_PLACEMENT_3D('',#106493,#60477,#60478);
#49982=AXIS2_PLACEMENT_3D('',#106498,#60480,#60481);
#49983=AXIS2_PLACEMENT_3D('',#106501,#60483,#60484);
#49984=AXIS2_PLACEMENT_3D('',#106502,#60485,#60486);
#49985=AXIS2_PLACEMENT_3D('',#106507,#60488,#60489);
#49986=AXIS2_PLACEMENT_3D('',#106510,#60491,#60492);
#49987=AXIS2_PLACEMENT_3D('',#106511,#60493,#60494);
#49988=AXIS2_PLACEMENT_3D('',#106516,#60496,#60497);
#49989=AXIS2_PLACEMENT_3D('',#106519,#60499,#60500);
#49990=AXIS2_PLACEMENT_3D('',#106520,#60501,#60502);
#49991=AXIS2_PLACEMENT_3D('',#106525,#60504,#60505);
#49992=AXIS2_PLACEMENT_3D('',#106528,#60507,#60508);
#49993=AXIS2_PLACEMENT_3D('',#106529,#60509,#60510);
#49994=AXIS2_PLACEMENT_3D('',#106534,#60512,#60513);
#49995=AXIS2_PLACEMENT_3D('',#106537,#60515,#60516);
#49996=AXIS2_PLACEMENT_3D('',#106538,#60517,#60518);
#49997=AXIS2_PLACEMENT_3D('',#106543,#60520,#60521);
#49998=AXIS2_PLACEMENT_3D('',#106546,#60523,#60524);
#49999=AXIS2_PLACEMENT_3D('',#106547,#60525,#60526);
#50000=AXIS2_PLACEMENT_3D('',#106552,#60528,#60529);
#50001=AXIS2_PLACEMENT_3D('',#106555,#60531,#60532);
#50002=AXIS2_PLACEMENT_3D('',#106556,#60533,#60534);
#50003=AXIS2_PLACEMENT_3D('',#106561,#60536,#60537);
#50004=AXIS2_PLACEMENT_3D('',#106564,#60539,#60540);
#50005=AXIS2_PLACEMENT_3D('',#106565,#60541,#60542);
#50006=AXIS2_PLACEMENT_3D('',#106570,#60544,#60545);
#50007=AXIS2_PLACEMENT_3D('',#106573,#60547,#60548);
#50008=AXIS2_PLACEMENT_3D('',#106574,#60549,#60550);
#50009=AXIS2_PLACEMENT_3D('',#106579,#60552,#60553);
#50010=AXIS2_PLACEMENT_3D('',#106582,#60555,#60556);
#50011=AXIS2_PLACEMENT_3D('',#106583,#60557,#60558);
#50012=AXIS2_PLACEMENT_3D('',#106588,#60560,#60561);
#50013=AXIS2_PLACEMENT_3D('',#106591,#60563,#60564);
#50014=AXIS2_PLACEMENT_3D('',#106592,#60565,#60566);
#50015=AXIS2_PLACEMENT_3D('',#106597,#60568,#60569);
#50016=AXIS2_PLACEMENT_3D('',#106600,#60571,#60572);
#50017=AXIS2_PLACEMENT_3D('',#106601,#60573,#60574);
#50018=AXIS2_PLACEMENT_3D('',#106606,#60576,#60577);
#50019=AXIS2_PLACEMENT_3D('',#106609,#60579,#60580);
#50020=AXIS2_PLACEMENT_3D('',#106610,#60581,#60582);
#50021=AXIS2_PLACEMENT_3D('',#106615,#60584,#60585);
#50022=AXIS2_PLACEMENT_3D('',#106618,#60587,#60588);
#50023=AXIS2_PLACEMENT_3D('',#106619,#60589,#60590);
#50024=AXIS2_PLACEMENT_3D('',#106624,#60592,#60593);
#50025=AXIS2_PLACEMENT_3D('',#106627,#60595,#60596);
#50026=AXIS2_PLACEMENT_3D('',#106628,#60597,#60598);
#50027=AXIS2_PLACEMENT_3D('',#106633,#60600,#60601);
#50028=AXIS2_PLACEMENT_3D('',#106636,#60603,#60604);
#50029=AXIS2_PLACEMENT_3D('',#106637,#60605,#60606);
#50030=AXIS2_PLACEMENT_3D('',#106642,#60608,#60609);
#50031=AXIS2_PLACEMENT_3D('',#106645,#60611,#60612);
#50032=AXIS2_PLACEMENT_3D('',#106646,#60613,#60614);
#50033=AXIS2_PLACEMENT_3D('',#106651,#60616,#60617);
#50034=AXIS2_PLACEMENT_3D('',#106654,#60619,#60620);
#50035=AXIS2_PLACEMENT_3D('',#106655,#60621,#60622);
#50036=AXIS2_PLACEMENT_3D('',#106660,#60624,#60625);
#50037=AXIS2_PLACEMENT_3D('',#106663,#60627,#60628);
#50038=AXIS2_PLACEMENT_3D('',#106664,#60629,#60630);
#50039=AXIS2_PLACEMENT_3D('',#106669,#60632,#60633);
#50040=AXIS2_PLACEMENT_3D('',#106672,#60635,#60636);
#50041=AXIS2_PLACEMENT_3D('',#106673,#60637,#60638);
#50042=AXIS2_PLACEMENT_3D('',#106678,#60640,#60641);
#50043=AXIS2_PLACEMENT_3D('',#106681,#60643,#60644);
#50044=AXIS2_PLACEMENT_3D('',#106682,#60645,#60646);
#50045=AXIS2_PLACEMENT_3D('',#106687,#60648,#60649);
#50046=AXIS2_PLACEMENT_3D('',#106690,#60651,#60652);
#50047=AXIS2_PLACEMENT_3D('',#106691,#60653,#60654);
#50048=AXIS2_PLACEMENT_3D('',#106696,#60656,#60657);
#50049=AXIS2_PLACEMENT_3D('',#106699,#60659,#60660);
#50050=AXIS2_PLACEMENT_3D('',#106700,#60661,#60662);
#50051=AXIS2_PLACEMENT_3D('',#106705,#60664,#60665);
#50052=AXIS2_PLACEMENT_3D('',#106708,#60667,#60668);
#50053=AXIS2_PLACEMENT_3D('',#106709,#60669,#60670);
#50054=AXIS2_PLACEMENT_3D('',#106714,#60672,#60673);
#50055=AXIS2_PLACEMENT_3D('',#106717,#60675,#60676);
#50056=AXIS2_PLACEMENT_3D('',#106718,#60677,#60678);
#50057=AXIS2_PLACEMENT_3D('',#106723,#60680,#60681);
#50058=AXIS2_PLACEMENT_3D('',#106726,#60683,#60684);
#50059=AXIS2_PLACEMENT_3D('',#106727,#60685,#60686);
#50060=AXIS2_PLACEMENT_3D('',#106732,#60688,#60689);
#50061=AXIS2_PLACEMENT_3D('',#106735,#60691,#60692);
#50062=AXIS2_PLACEMENT_3D('',#106736,#60693,#60694);
#50063=AXIS2_PLACEMENT_3D('',#106741,#60696,#60697);
#50064=AXIS2_PLACEMENT_3D('',#106744,#60699,#60700);
#50065=AXIS2_PLACEMENT_3D('',#106745,#60701,#60702);
#50066=AXIS2_PLACEMENT_3D('',#106899,#60805,#60806);
#50067=AXIS2_PLACEMENT_3D('',#107053,#60909,#60910);
#50068=AXIS2_PLACEMENT_3D('',#107054,#60911,#60912);
#50069=AXIS2_PLACEMENT_3D('',#107055,#60913,#60914);
#50070=AXIS2_PLACEMENT_3D('',#107056,#60915,#60916);
#50071=AXIS2_PLACEMENT_3D('',#107057,#60917,#60918);
#50072=AXIS2_PLACEMENT_3D('',#107059,#60920,#60921);
#50073=AXIS2_PLACEMENT_3D('',#107060,#60922,#60923);
#50074=AXIS2_PLACEMENT_3D('',#107062,#60925,#60926);
#50075=AXIS2_PLACEMENT_3D('',#107063,#60927,#60928);
#50076=AXIS2_PLACEMENT_3D('',#107065,#60930,#60931);
#50077=AXIS2_PLACEMENT_3D('',#107066,#60932,#60933);
#50078=AXIS2_PLACEMENT_3D('',#107068,#60935,#60936);
#50079=AXIS2_PLACEMENT_3D('',#107069,#60937,#60938);
#50080=AXIS2_PLACEMENT_3D('',#107071,#60940,#60941);
#50081=AXIS2_PLACEMENT_3D('',#107072,#60942,#60943);
#50082=AXIS2_PLACEMENT_3D('',#107074,#60945,#60946);
#50083=AXIS2_PLACEMENT_3D('',#107075,#60947,#60948);
#50084=AXIS2_PLACEMENT_3D('',#107077,#60950,#60951);
#50085=AXIS2_PLACEMENT_3D('',#107078,#60952,#60953);
#50086=AXIS2_PLACEMENT_3D('',#107080,#60955,#60956);
#50087=AXIS2_PLACEMENT_3D('',#107081,#60957,#60958);
#50088=AXIS2_PLACEMENT_3D('',#107083,#60960,#60961);
#50089=AXIS2_PLACEMENT_3D('',#107084,#60962,#60963);
#50090=AXIS2_PLACEMENT_3D('',#107086,#60965,#60966);
#50091=AXIS2_PLACEMENT_3D('',#107087,#60967,#60968);
#50092=AXIS2_PLACEMENT_3D('',#107089,#60970,#60971);
#50093=AXIS2_PLACEMENT_3D('',#107090,#60972,#60973);
#50094=AXIS2_PLACEMENT_3D('',#107092,#60975,#60976);
#50095=AXIS2_PLACEMENT_3D('',#107093,#60977,#60978);
#50096=AXIS2_PLACEMENT_3D('',#107095,#60980,#60981);
#50097=AXIS2_PLACEMENT_3D('',#107096,#60982,#60983);
#50098=AXIS2_PLACEMENT_3D('',#107098,#60985,#60986);
#50099=AXIS2_PLACEMENT_3D('',#107099,#60987,#60988);
#50100=AXIS2_PLACEMENT_3D('',#107101,#60990,#60991);
#50101=AXIS2_PLACEMENT_3D('',#107102,#60992,#60993);
#50102=AXIS2_PLACEMENT_3D('',#107104,#60995,#60996);
#50103=AXIS2_PLACEMENT_3D('',#107105,#60997,#60998);
#50104=AXIS2_PLACEMENT_3D('',#107107,#61000,#61001);
#50105=AXIS2_PLACEMENT_3D('',#107108,#61002,#61003);
#50106=AXIS2_PLACEMENT_3D('',#107110,#61005,#61006);
#50107=AXIS2_PLACEMENT_3D('',#107111,#61007,#61008);
#50108=AXIS2_PLACEMENT_3D('',#107113,#61010,#61011);
#50109=AXIS2_PLACEMENT_3D('',#107114,#61012,#61013);
#50110=AXIS2_PLACEMENT_3D('',#107116,#61015,#61016);
#50111=AXIS2_PLACEMENT_3D('',#107117,#61017,#61018);
#50112=AXIS2_PLACEMENT_3D('',#107119,#61020,#61021);
#50113=AXIS2_PLACEMENT_3D('',#107120,#61022,#61023);
#50114=AXIS2_PLACEMENT_3D('',#107122,#61025,#61026);
#50115=AXIS2_PLACEMENT_3D('',#107123,#61027,#61028);
#50116=AXIS2_PLACEMENT_3D('',#107125,#61030,#61031);
#50117=AXIS2_PLACEMENT_3D('',#107126,#61032,#61033);
#50118=AXIS2_PLACEMENT_3D('',#107128,#61035,#61036);
#50119=AXIS2_PLACEMENT_3D('',#107129,#61037,#61038);
#50120=AXIS2_PLACEMENT_3D('',#107131,#61040,#61041);
#50121=AXIS2_PLACEMENT_3D('',#107132,#61042,#61043);
#50122=AXIS2_PLACEMENT_3D('',#107134,#61045,#61046);
#50123=AXIS2_PLACEMENT_3D('',#107135,#61047,#61048);
#50124=AXIS2_PLACEMENT_3D('',#107137,#61050,#61051);
#50125=AXIS2_PLACEMENT_3D('',#107138,#61052,#61053);
#50126=AXIS2_PLACEMENT_3D('',#107140,#61055,#61056);
#50127=AXIS2_PLACEMENT_3D('',#107141,#61057,#61058);
#50128=AXIS2_PLACEMENT_3D('',#107143,#61060,#61061);
#50129=AXIS2_PLACEMENT_3D('',#107144,#61062,#61063);
#50130=AXIS2_PLACEMENT_3D('',#107146,#61065,#61066);
#50131=AXIS2_PLACEMENT_3D('',#107147,#61067,#61068);
#50132=AXIS2_PLACEMENT_3D('',#107149,#61070,#61071);
#50133=AXIS2_PLACEMENT_3D('',#107150,#61072,#61073);
#50134=AXIS2_PLACEMENT_3D('',#107152,#61075,#61076);
#50135=AXIS2_PLACEMENT_3D('',#107153,#61077,#61078);
#50136=AXIS2_PLACEMENT_3D('',#107155,#61080,#61081);
#50137=AXIS2_PLACEMENT_3D('',#107156,#61082,#61083);
#50138=AXIS2_PLACEMENT_3D('',#107158,#61085,#61086);
#50139=AXIS2_PLACEMENT_3D('',#107159,#61087,#61088);
#50140=AXIS2_PLACEMENT_3D('',#107161,#61090,#61091);
#50141=AXIS2_PLACEMENT_3D('',#107162,#61092,#61093);
#50142=AXIS2_PLACEMENT_3D('',#107164,#61095,#61096);
#50143=AXIS2_PLACEMENT_3D('',#107165,#61097,#61098);
#50144=AXIS2_PLACEMENT_3D('',#107167,#61100,#61101);
#50145=AXIS2_PLACEMENT_3D('',#107168,#61102,#61103);
#50146=AXIS2_PLACEMENT_3D('',#107170,#61105,#61106);
#50147=AXIS2_PLACEMENT_3D('',#107171,#61107,#61108);
#50148=AXIS2_PLACEMENT_3D('',#107173,#61110,#61111);
#50149=AXIS2_PLACEMENT_3D('',#107174,#61112,#61113);
#50150=AXIS2_PLACEMENT_3D('',#107176,#61115,#61116);
#50151=AXIS2_PLACEMENT_3D('',#107177,#61117,#61118);
#50152=AXIS2_PLACEMENT_3D('',#107179,#61120,#61121);
#50153=AXIS2_PLACEMENT_3D('',#107180,#61122,#61123);
#50154=AXIS2_PLACEMENT_3D('',#107182,#61125,#61126);
#50155=AXIS2_PLACEMENT_3D('',#107183,#61127,#61128);
#50156=AXIS2_PLACEMENT_3D('',#107185,#61130,#61131);
#50157=AXIS2_PLACEMENT_3D('',#107186,#61132,#61133);
#50158=AXIS2_PLACEMENT_3D('',#107188,#61135,#61136);
#50159=AXIS2_PLACEMENT_3D('',#107189,#61137,#61138);
#50160=AXIS2_PLACEMENT_3D('',#107191,#61140,#61141);
#50161=AXIS2_PLACEMENT_3D('',#107192,#61142,#61143);
#50162=AXIS2_PLACEMENT_3D('',#107194,#61145,#61146);
#50163=AXIS2_PLACEMENT_3D('',#107195,#61147,#61148);
#50164=AXIS2_PLACEMENT_3D('',#107197,#61150,#61151);
#50165=AXIS2_PLACEMENT_3D('',#107198,#61152,#61153);
#50166=AXIS2_PLACEMENT_3D('',#107200,#61155,#61156);
#50167=AXIS2_PLACEMENT_3D('',#107201,#61157,#61158);
#50168=AXIS2_PLACEMENT_3D('',#107203,#61160,#61161);
#50169=AXIS2_PLACEMENT_3D('',#107204,#61162,#61163);
#50170=AXIS2_PLACEMENT_3D('',#107206,#61165,#61166);
#50171=AXIS2_PLACEMENT_3D('',#107207,#61167,#61168);
#50172=AXIS2_PLACEMENT_3D('',#107209,#61170,#61171);
#50173=AXIS2_PLACEMENT_3D('',#107210,#61172,#61173);
#50174=AXIS2_PLACEMENT_3D('',#107211,#61174,#61175);
#50175=AXIS2_PLACEMENT_3D('',#107213,#61176,#61177);
#50176=AXIS2_PLACEMENT_3D('',#107217,#61179,#61180);
#50177=AXIS2_PLACEMENT_3D('',#107221,#61182,#61183);
#50178=AXIS2_PLACEMENT_3D('',#107224,#61185,#61186);
#50179=AXIS2_PLACEMENT_3D('',#107226,#61187,#61188);
#50180=AXIS2_PLACEMENT_3D('',#107229,#61190,#61191);
#50181=AXIS2_PLACEMENT_3D('',#107230,#61192,#61193);
#50182=AXIS2_PLACEMENT_3D('',#107232,#61194,#61195);
#50183=AXIS2_PLACEMENT_3D('',#107235,#61197,#61198);
#50184=AXIS2_PLACEMENT_3D('',#107279,#61199,#61200);
#50185=AXIS2_PLACEMENT_3D('',#107281,#61201,#61202);
#50186=AXIS2_PLACEMENT_3D('',#107284,#61204,#61205);
#50187=AXIS2_PLACEMENT_3D('',#107285,#61206,#61207);
#50188=AXIS2_PLACEMENT_3D('',#107288,#61208,#61209);
#50189=AXIS2_PLACEMENT_3D('',#107292,#61211,#61212);
#50190=AXIS2_PLACEMENT_3D('',#107294,#61214,#61215);
#50191=AXIS2_PLACEMENT_3D('',#107296,#61216,#61217);
#50192=AXIS2_PLACEMENT_3D('',#107299,#61219,#61220);
#50193=AXIS2_PLACEMENT_3D('',#107300,#61221,#61222);
#50194=AXIS2_PLACEMENT_3D('',#107303,#61223,#61224);
#50195=AXIS2_PLACEMENT_3D('',#107306,#61226,#61227);
#50196=AXIS2_PLACEMENT_3D('',#107308,#61228,#61229);
#50197=AXIS2_PLACEMENT_3D('',#107319,#61230,#61231);
#50198=AXIS2_PLACEMENT_3D('',#107321,#61232,#61233);
#50199=AXIS2_PLACEMENT_3D('',#107330,#61234,#61235);
#50200=AXIS2_PLACEMENT_3D('',#107333,#61237,#61238);
#50201=AXIS2_PLACEMENT_3D('',#107334,#61239,#61240);
#50202=AXIS2_PLACEMENT_3D('',#107336,#61241,#61242);
#50203=AXIS2_PLACEMENT_3D('',#107339,#61244,#61245);
#50204=AXIS2_PLACEMENT_3D('',#107340,#61246,#61247);
#50205=AXIS2_PLACEMENT_3D('',#107343,#61248,#61249);
#50206=AXIS2_PLACEMENT_3D('',#107347,#61251,#61252);
#50207=AXIS2_PLACEMENT_3D('',#107349,#61254,#61255);
#50208=AXIS2_PLACEMENT_3D('',#107352,#61256,#61257);
#50209=AXIS2_PLACEMENT_3D('',#107356,#61259,#61260);
#50210=AXIS2_PLACEMENT_3D('',#107360,#61262,#61263);
#50211=AXIS2_PLACEMENT_3D('',#107362,#61265,#61266);
#50212=AXIS2_PLACEMENT_3D('',#107364,#61267,#61268);
#50213=AXIS2_PLACEMENT_3D('',#107367,#61270,#61271);
#50214=AXIS2_PLACEMENT_3D('',#107368,#61272,#61273);
#50215=AXIS2_PLACEMENT_3D('',#107370,#61274,#61275);
#50216=AXIS2_PLACEMENT_3D('',#107373,#61277,#61278);
#50217=AXIS2_PLACEMENT_3D('',#107374,#61279,#61280);
#50218=AXIS2_PLACEMENT_3D('',#107376,#61281,#61282);
#50219=AXIS2_PLACEMENT_3D('',#107379,#61284,#61285);
#50220=AXIS2_PLACEMENT_3D('',#107380,#61286,#61287);
#50221=AXIS2_PLACEMENT_3D('',#107382,#61288,#61289);
#50222=AXIS2_PLACEMENT_3D('',#107385,#61291,#61292);
#50223=AXIS2_PLACEMENT_3D('',#107386,#61293,#61294);
#50224=AXIS2_PLACEMENT_3D('',#107388,#61295,#61296);
#50225=AXIS2_PLACEMENT_3D('',#107392,#61298,#61299);
#50226=AXIS2_PLACEMENT_3D('',#107396,#61301,#61302);
#50227=AXIS2_PLACEMENT_3D('',#107399,#61304,#61305);
#50228=AXIS2_PLACEMENT_3D('',#107401,#61307,#61308);
#50229=AXIS2_PLACEMENT_3D('',#107403,#61309,#61310);
#50230=AXIS2_PLACEMENT_3D('',#107406,#61312,#61313);
#50231=AXIS2_PLACEMENT_3D('',#107407,#61314,#61315);
#50232=AXIS2_PLACEMENT_3D('',#107410,#61317,#61318);
#50233=AXIS2_PLACEMENT_3D('',#107414,#61320,#61321);
#50234=AXIS2_PLACEMENT_3D('',#107416,#61323,#61324);
#50235=AXIS2_PLACEMENT_3D('',#107419,#61325,#61326);
#50236=AXIS2_PLACEMENT_3D('',#107422,#61328,#61329);
#50237=AXIS2_PLACEMENT_3D('',#107424,#61330,#61331);
#50238=AXIS2_PLACEMENT_3D('',#107428,#61333,#61334);
#50239=AXIS2_PLACEMENT_3D('',#107430,#61336,#61337);
#50240=AXIS2_PLACEMENT_3D('',#107439,#61342,#61343);
#50241=AXIS2_PLACEMENT_3D('',#107444,#61345,#61346);
#50242=AXIS2_PLACEMENT_3D('',#107448,#61348,#61349);
#50243=AXIS2_PLACEMENT_3D('',#107451,#61351,#61352);
#50244=AXIS2_PLACEMENT_3D('',#107452,#61353,#61354);
#50245=AXIS2_PLACEMENT_3D('',#107453,#61355,#61356);
#50246=AXIS2_PLACEMENT_3D('',#107457,#61358,#61359);
#50247=AXIS2_PLACEMENT_3D('',#107462,#61362,#61363);
#50248=AXIS2_PLACEMENT_3D('',#107473,#61370,#61371);
#50249=AXIS2_PLACEMENT_3D('',#107482,#61377,#61378);
#50250=AXIS2_PLACEMENT_3D('',#107492,#61384,#61385);
#50251=AXIS2_PLACEMENT_3D('',#107501,#61390,#61391);
#50252=AXIS2_PLACEMENT_3D('',#107502,#61392,#61393);
#50253=AXIS2_PLACEMENT_3D('',#107506,#61395,#61396);
#50254=AXIS2_PLACEMENT_3D('',#107510,#61398,#61399);
#50255=AXIS2_PLACEMENT_3D('',#107514,#61401,#61402);
#50256=AXIS2_PLACEMENT_3D('',#107518,#61404,#61405);
#50257=AXIS2_PLACEMENT_3D('',#107519,#61406,#61407);
#50258=AXIS2_PLACEMENT_3D('',#107520,#61408,#61409);
#50259=AXIS2_PLACEMENT_3D('',#107523,#61411,#61412);
#50260=AXIS2_PLACEMENT_3D('',#107524,#61413,#61414);
#50261=AXIS2_PLACEMENT_3D('',#107525,#61415,#61416);
#50262=AXIS2_PLACEMENT_3D('',#107527,#61417,#61418);
#50263=AXIS2_PLACEMENT_3D('',#107529,#61420,#61421);
#50264=AXIS2_PLACEMENT_3D('',#107535,#61425,#61426);
#50265=AXIS2_PLACEMENT_3D('',#107548,#61433,#61434);
#50266=AXIS2_PLACEMENT_3D('',#107581,#61451,#61452);
#50267=AXIS2_PLACEMENT_3D('',#107601,#61462,#61463);
#50268=AXIS2_PLACEMENT_3D('',#107605,#61465,#61466);
#50269=AXIS2_PLACEMENT_3D('',#107609,#61468,#61469);
#50270=AXIS2_PLACEMENT_3D('',#107617,#61473,#61474);
#50271=AXIS2_PLACEMENT_3D('',#107621,#61476,#61477);
#50272=AXIS2_PLACEMENT_3D('',#107625,#61479,#61480);
#50273=AXIS2_PLACEMENT_3D('',#107630,#61483,#61484);
#50274=AXIS2_PLACEMENT_3D('',#107633,#61486,#61487);
#50275=AXIS2_PLACEMENT_3D('',#107634,#61488,#61489);
#50276=AXIS2_PLACEMENT_3D('',#107635,#61490,#61491);
#50277=AXIS2_PLACEMENT_3D('',#107641,#61495,#61496);
#50278=AXIS2_PLACEMENT_3D('',#107648,#61502,#61503);
#50279=AXIS2_PLACEMENT_3D('',#107654,#61507,#61508);
#50280=AXIS2_PLACEMENT_3D('',#107663,#61515,#61516);
#50281=AXIS2_PLACEMENT_3D('',#107669,#61520,#61521);
#50282=AXIS2_PLACEMENT_3D('',#107674,#61525,#61526);
#50283=AXIS2_PLACEMENT_3D('',#107678,#61529,#61530);
#50284=AXIS2_PLACEMENT_3D('',#107682,#61533,#61534);
#50285=AXIS2_PLACEMENT_3D('',#107684,#61536,#61537);
#50286=AXIS2_PLACEMENT_3D('',#107687,#61540,#61541);
#50287=AXIS2_PLACEMENT_3D('',#107689,#61543,#61544);
#50288=AXIS2_PLACEMENT_3D('',#107691,#61546,#61547);
#50289=AXIS2_PLACEMENT_3D('',#107693,#61549,#61550);
#50290=AXIS2_PLACEMENT_3D('',#107695,#61552,#61553);
#50291=AXIS2_PLACEMENT_3D('',#107697,#61555,#61556);
#50292=AXIS2_PLACEMENT_3D('',#107699,#61558,#61559);
#50293=AXIS2_PLACEMENT_3D('',#107700,#61560,#61561);
#50294=AXIS2_PLACEMENT_3D('',#107701,#61562,#61563);
#50295=AXIS2_PLACEMENT_3D('',#107702,#61564,#61565);
#50296=AXIS2_PLACEMENT_3D('',#107703,#61566,#61567);
#50297=AXIS2_PLACEMENT_3D('',#107708,#61571,#61572);
#50298=AXIS2_PLACEMENT_3D('',#107711,#61574,#61575);
#50299=AXIS2_PLACEMENT_3D('',#107712,#61576,#61577);
#50300=AXIS2_PLACEMENT_3D('',#107716,#61580,#61581);
#50301=AXIS2_PLACEMENT_3D('',#107719,#61583,#61584);
#50302=AXIS2_PLACEMENT_3D('',#107720,#61585,#61586);
#50303=AXIS2_PLACEMENT_3D('',#107724,#61589,#61590);
#50304=AXIS2_PLACEMENT_3D('',#107727,#61592,#61593);
#50305=AXIS2_PLACEMENT_3D('',#107728,#61594,#61595);
#50306=AXIS2_PLACEMENT_3D('',#107732,#61598,#61599);
#50307=AXIS2_PLACEMENT_3D('',#107735,#61601,#61602);
#50308=AXIS2_PLACEMENT_3D('',#107736,#61603,#61604);
#50309=AXIS2_PLACEMENT_3D('',#107739,#61607,#61608);
#50310=AXIS2_PLACEMENT_3D('',#107740,#61609,#61610);
#50311=AXIS2_PLACEMENT_3D('',#107741,#61611,#61612);
#50312=AXIS2_PLACEMENT_3D('',#107745,#61615,#61616);
#50313=AXIS2_PLACEMENT_3D('',#107747,#61617,#61618);
#50314=AXIS2_PLACEMENT_3D('',#107749,#61620,#61621);
#50315=AXIS2_PLACEMENT_3D('',#107753,#61624,#61625);
#50316=AXIS2_PLACEMENT_3D('',#107754,#61626,#61627);
#50317=AXIS2_PLACEMENT_3D('',#107755,#61628,#61629);
#50318=AXIS2_PLACEMENT_3D('',#107761,#61633,#61634);
#50319=AXIS2_PLACEMENT_3D('',#107767,#61638,#61639);
#50320=AXIS2_PLACEMENT_3D('',#107773,#61644,#61645);
#50321=AXIS2_PLACEMENT_3D('',#107775,#61647,#61648);
#50322=AXIS2_PLACEMENT_3D('',#107777,#61650,#61651);
#50323=AXIS2_PLACEMENT_3D('',#107779,#61653,#61654);
#50324=AXIS2_PLACEMENT_3D('',#107781,#61656,#61657);
#50325=AXIS2_PLACEMENT_3D('',#107783,#61659,#61660);
#50326=AXIS2_PLACEMENT_3D('',#107784,#61661,#61662);
#50327=AXIS2_PLACEMENT_3D('',#107785,#61663,#61664);
#50328=AXIS2_PLACEMENT_3D('',#107786,#61665,#61666);
#50329=AXIS2_PLACEMENT_3D('',#107787,#61667,#61668);
#50330=AXIS2_PLACEMENT_3D('',#107788,#61669,#61670);
#50331=AXIS2_PLACEMENT_3D('',#107790,#61672,#61673);
#50332=AXIS2_PLACEMENT_3D('',#107791,#61674,#61675);
#50333=AXIS2_PLACEMENT_3D('',#107792,#61676,#61677);
#50334=AXIS2_PLACEMENT_3D('',#107793,#61678,#61679);
#50335=AXIS2_PLACEMENT_3D('',#107799,#61683,#61684);
#50336=AXIS2_PLACEMENT_3D('',#107803,#61687,#61688);
#50337=AXIS2_PLACEMENT_3D('',#107807,#61691,#61692);
#50338=AXIS2_PLACEMENT_3D('',#107811,#61695,#61696);
#50339=AXIS2_PLACEMENT_3D('',#107815,#61699,#61700);
#50340=AXIS2_PLACEMENT_3D('',#107819,#61703,#61704);
#50341=AXIS2_PLACEMENT_3D('',#107823,#61707,#61708);
#50342=AXIS2_PLACEMENT_3D('',#107825,#61710,#61711);
#50343=AXIS2_PLACEMENT_3D('',#107826,#61712,#61713);
#50344=AXIS2_PLACEMENT_3D('',#107827,#61714,#61715);
#50345=AXIS2_PLACEMENT_3D('',#107828,#61716,#61717);
#50346=AXIS2_PLACEMENT_3D('',#107829,#61718,#61719);
#50347=AXIS2_PLACEMENT_3D('',#107839,#61725,#61726);
#50348=AXIS2_PLACEMENT_3D('',#107840,#61727,#61728);
#50349=AXIS2_PLACEMENT_3D('',#107841,#61729,#61730);
#50350=AXIS2_PLACEMENT_3D('',#107845,#61733,#61734);
#50351=AXIS2_PLACEMENT_3D('',#107846,#61735,#61736);
#50352=AXIS2_PLACEMENT_3D('',#107847,#61737,#61738);
#50353=AXIS2_PLACEMENT_3D('',#107849,#61740,#61741);
#50354=AXIS2_PLACEMENT_3D('',#107853,#61744,#61745);
#50355=AXIS2_PLACEMENT_3D('',#107855,#61747,#61748);
#50356=AXIS2_PLACEMENT_3D('',#107856,#61749,#61750);
#50357=AXIS2_PLACEMENT_3D('',#107858,#61752,#61753);
#50358=AXIS2_PLACEMENT_3D('',#107859,#61754,#61755);
#50359=AXIS2_PLACEMENT_3D('',#107860,#61756,#61757);
#50360=AXIS2_PLACEMENT_3D('',#107863,#61758,#61759);
#50361=AXIS2_PLACEMENT_3D('',#107866,#61762,#61763);
#50362=AXIS2_PLACEMENT_3D('',#107869,#61764,#61765);
#50363=AXIS2_PLACEMENT_3D('',#107872,#61768,#61769);
#50364=AXIS2_PLACEMENT_3D('',#107875,#61772,#61773);
#50365=AXIS2_PLACEMENT_3D('',#107876,#61774,#61775);
#50366=AXIS2_PLACEMENT_3D('',#107877,#61776,#61777);
#50367=AXIS2_PLACEMENT_3D('',#107878,#61778,#61779);
#50368=AXIS2_PLACEMENT_3D('',#107879,#61780,#61781);
#50369=AXIS2_PLACEMENT_3D('',#107880,#61782,#61783);
#50370=AXIS2_PLACEMENT_3D('',#107881,#61784,#61785);
#50371=AXIS2_PLACEMENT_3D('',#107882,#61786,#61787);
#50372=AXIS2_PLACEMENT_3D('',#107883,#61788,#61789);
#50373=AXIS2_PLACEMENT_3D('',#107884,#61790,#61791);
#50374=AXIS2_PLACEMENT_3D('',#107885,#61792,#61793);
#50375=AXIS2_PLACEMENT_3D('',#107886,#61794,#61795);
#50376=DIRECTION('axis',(0.,0.,1.));
#50377=DIRECTION('refdir',(1.,0.,0.));
#50378=DIRECTION('axis',(0.,0.,1.));
#50379=DIRECTION('refdir',(1.,0.,0.));
#50380=DIRECTION('center_axis',(0.,1.,-1.45983193964168E-32));
#50381=DIRECTION('ref_axis',(-1.,0.,0.));
#50382=DIRECTION('center_axis',(0.,-1.,6.6666666666222E-12));
#50383=DIRECTION('ref_axis',(1.,0.,0.));
#50384=DIRECTION('',(0.,1.,-1.45983193964168E-32));
#50385=DIRECTION('center_axis',(0.,-1.,6.6666666666222E-12));
#50386=DIRECTION('ref_axis',(1.,0.,0.));
#50387=DIRECTION('center_axis',(0.,1.,-1.45983193964168E-32));
#50388=DIRECTION('ref_axis',(-1.,0.,0.));
#50389=DIRECTION('center_axis',(0.,-1.,2.49999999999375E-12));
#50390=DIRECTION('ref_axis',(1.,0.,0.));
#50391=DIRECTION('',(0.,-1.,1.45983193964168E-32));
#50392=DIRECTION('center_axis',(0.,-1.,2.49999999999375E-12));
#50393=DIRECTION('ref_axis',(1.,0.,0.));
#50394=DIRECTION('center_axis',(-1.19900741137893E-16,-1.,1.45983193964168E-32));
#50395=DIRECTION('ref_axis',(-1.,1.19900741137893E-16,0.));
#50396=DIRECTION('center_axis',(-1.19900741137893E-16,-1.,1.45983193964168E-32));
#50397=DIRECTION('ref_axis',(-1.,1.19900741137893E-16,0.));
#50398=DIRECTION('axis',(0.,0.,1.));
#50399=DIRECTION('refdir',(1.,0.,0.));
#50400=DIRECTION('center_axis',(-3.37541892033393E-34,1.,-4.11561597259898E-17));
#50401=DIRECTION('ref_axis',(1.,-1.28292706084425E-49,-8.20149144819841E-18));
#50402=DIRECTION('center_axis',(-1.19904736293711E-16,-1.,2.51898569257898E-21));
#50403=DIRECTION('ref_axis',(-1.,1.19904736293711E-16,0.));
#50404=DIRECTION('axis',(0.,0.,1.));
#50405=DIRECTION('refdir',(1.,0.,0.));
#50406=DIRECTION('center_axis',(0.,0.,-1.));
#50407=DIRECTION('ref_axis',(-1.,0.,0.));
#50408=DIRECTION('center_axis',(0.,0.,-1.));
#50409=DIRECTION('ref_axis',(-1.,0.,0.));
#50410=DIRECTION('center_axis',(0.,-1.,0.));
#50411=DIRECTION('ref_axis',(1.,0.,0.));
#50412=DIRECTION('center_axis',(0.,0.,1.));
#50413=DIRECTION('ref_axis',(-1.,0.,0.));
#50414=DIRECTION('center_axis',(0.,0.,-1.));
#50415=DIRECTION('ref_axis',(-1.,0.,0.));
#50416=DIRECTION('',(0.,0.,1.));
#50417=DIRECTION('center_axis',(0.,0.,-1.));
#50418=DIRECTION('ref_axis',(-1.,0.,0.));
#50419=DIRECTION('center_axis',(0.,0.,-1.));
#50420=DIRECTION('ref_axis',(0.,-1.,0.));
#50421=DIRECTION('center_axis',(0.,0.,-1.));
#50422=DIRECTION('ref_axis',(0.,-1.,0.));
#50423=DIRECTION('axis',(0.,0.,1.));
#50424=DIRECTION('refdir',(1.,0.,0.));
#50425=DIRECTION('center_axis',(0.,0.,-1.));
#50426=DIRECTION('ref_axis',(-1.,0.,0.));
#50427=DIRECTION('center_axis',(0.,0.,-1.));
#50428=DIRECTION('ref_axis',(-1.,0.,0.));
#50429=DIRECTION('',(0.,0.,1.));
#50430=DIRECTION('center_axis',(0.,0.,-1.));
#50431=DIRECTION('ref_axis',(-1.,0.,0.));
#50432=DIRECTION('center_axis',(0.,0.,-1.));
#50433=DIRECTION('ref_axis',(-1.,0.,0.));
#50434=DIRECTION('center_axis',(0.,0.,-1.));
#50435=DIRECTION('ref_axis',(0.,-1.,0.));
#50436=DIRECTION('',(1.,0.,0.));
#50437=DIRECTION('center_axis',(0.,0.,-1.));
#50438=DIRECTION('ref_axis',(0.,-1.,0.));
#50439=DIRECTION('center_axis',(1.,0.,0.));
#50440=DIRECTION('ref_axis',(0.,0.,-1.));
#50441=DIRECTION('axis',(0.,0.,1.));
#50442=DIRECTION('refdir',(1.,0.,0.));
#50443=DIRECTION('center_axis',(0.,-1.,1.45983193964168E-32));
#50444=DIRECTION('ref_axis',(1.,0.,0.));
#50445=DIRECTION('center_axis',(0.,1.,-5.71428571425305E-12));
#50446=DIRECTION('ref_axis',(1.,0.,0.));
#50447=DIRECTION('',(-1.01199007411378E-14,-1.,1.E-14));
#50448=DIRECTION('center_axis',(0.,-1.,5.71428571425305E-12));
#50449=DIRECTION('ref_axis',(1.,0.,0.));
#50450=DIRECTION('',(-1.01199007411378E-14,-1.,1.E-14));
#50451=DIRECTION('center_axis',(0.,8.34284178923119E-33,1.));
#50452=DIRECTION('ref_axis',(-0.288781765961724,0.95739495071158,-7.9873946035955E-33));
#50453=DIRECTION('center_axis',(0.,0.,-1.));
#50454=DIRECTION('ref_axis',(-1.,0.,0.));
#50455=DIRECTION('',(1.00521721346157E-14,1.E-14,1.));
#50456=DIRECTION('center_axis',(0.,-2.22222222221729E-12,-1.));
#50457=DIRECTION('ref_axis',(1.,0.,0.));
#50458=DIRECTION('',(1.00521721346157E-14,1.E-14,1.));
#50459=DIRECTION('center_axis',(1.18937267665668E-17,-1.,7.7223206752818E-33));
#50460=DIRECTION('ref_axis',(-7.5891469116954E-66,-7.7223206752818E-33,
-1.));
#50461=DIRECTION('',(1.,1.00118937267665E-14,-1.02086885384633E-14));
#50462=DIRECTION('',(-0.985460115744347,-1.00117207933559E-14,0.169906916507654));
#50463=DIRECTION('',(1.00521721346157E-14,1.E-14,1.));
#50464=DIRECTION('',(0.985460115744347,1.00117207933559E-14,0.169906916507654));
#50465=DIRECTION('',(1.,1.00118937267665E-14,0.));
#50466=DIRECTION('',(1.,1.00118937267665E-14,-1.E-14));
#50467=DIRECTION('center_axis',(0.,1.,-5.71428571425305E-12));
#50468=DIRECTION('ref_axis',(1.,0.,0.));
#50469=DIRECTION('',(-1.,-1.00118937267665E-14,1.E-14));
#50470=DIRECTION('center_axis',(0.,8.34284178923119E-33,1.));
#50471=DIRECTION('ref_axis',(1.,0.,0.));
#50472=DIRECTION('center_axis',(0.169906916507649,2.14440522290675E-14,
0.985460115744348));
#50473=DIRECTION('ref_axis',(0.985460115744348,-2.65533858744027E-12,-0.169906916507649));
#50474=DIRECTION('',(1.00521721346157E-14,1.E-14,1.));
#50475=DIRECTION('center_axis',(0.169906916507651,-2.62034553422522E-14,
-0.985460115744347));
#50476=DIRECTION('ref_axis',(-0.985460115744347,-7.81400541235329E-14,-0.169906916507651));
#50477=DIRECTION('center_axis',(0.,-1.,8.34284178923119E-33));
#50478=DIRECTION('ref_axis',(-1.,0.,0.));
#50479=DIRECTION('',(0.985460115744347,-9.99999999999989E-15,-0.169906916507654));
#50480=DIRECTION('',(1.00521721346157E-14,1.E-14,1.));
#50481=DIRECTION('',(-0.985460115744347,-9.99999999999989E-15,-0.169906916507654));
#50482=DIRECTION('center_axis',(-1.,0.,5.21721346158438E-17));
#50483=DIRECTION('ref_axis',(0.,1.,0.));
#50484=DIRECTION('',(-1.01199007411378E-14,-1.,1.E-14));
#50485=DIRECTION('',(-1.00521721346157E-14,-1.E-14,-1.));
#50486=DIRECTION('',(-1.01199007411378E-14,-1.,1.E-14));
#50487=DIRECTION('center_axis',(-2.66337519831924E-50,1.,-2.22131671000782E-34));
#50488=DIRECTION('ref_axis',(1.,2.37389193643995E-65,-1.19900741137893E-16));
#50489=DIRECTION('',(-0.985460115744347,1.01181573982395E-14,0.169906916507654));
#50490=DIRECTION('',(-1.,1.01199007411378E-14,1.02086885384633E-14));
#50491=DIRECTION('',(1.00521721346157E-14,1.E-14,1.));
#50492=DIRECTION('',(1.,-1.01199007411378E-14,0.));
#50493=DIRECTION('',(0.985460115744347,-1.01181573982395E-14,0.169906916507654));
#50494=DIRECTION('',(1.00521721346157E-14,1.E-14,1.));
#50495=DIRECTION('',(1.,-1.01334402673827E-14,0.));
#50496=DIRECTION('center_axis',(0.,-1.,5.71428571425305E-12));
#50497=DIRECTION('ref_axis',(1.,0.,0.));
#50498=DIRECTION('',(-1.,1.01334402673827E-14,0.));
#50499=DIRECTION('center_axis',(0.562571578885413,0.8267485824786,-2.93505601446575E-17));
#50500=DIRECTION('ref_axis',(-5.21721346158438E-17,6.35926162475305E-32,
-1.));
#50501=DIRECTION('',(-0.72055180024015,0.490308628911769,0.490308628911771));
#50502=DIRECTION('',(-0.826748582478598,0.562571578885415,1.0172532953354E-14));
#50503=DIRECTION('',(-0.826748582478598,0.562571578885415,0.));
#50504=DIRECTION('',(0.720551800240151,-0.490308628911769,0.49030862891177));
#50505=DIRECTION('center_axis',(0.,0.,-1.));
#50506=DIRECTION('ref_axis',(0.,-1.,0.));
#50507=DIRECTION('',(-1.01199007411378E-14,-1.,1.E-14));
#50508=DIRECTION('',(-1.,1.01199007411378E-14,0.));
#50509=DIRECTION('center_axis',(1.60527967783421E-47,7.69222732429044E-32,
1.));
#50510=DIRECTION('ref_axis',(1.,-2.08688538463375E-16,-3.50729211666941E-63));
#50511=DIRECTION('',(1.,-1.01199007411378E-14,-1.02086885384633E-14));
#50512=DIRECTION('',(-1.01199007411378E-14,-1.,1.E-14));
#50513=DIRECTION('center_axis',(-0.169906916507646,2.03719652137209E-17,
-0.985460115744348));
#50514=DIRECTION('ref_axis',(-0.985460115744348,-9.68087878944276E-35,0.169906916507646));
#50515=DIRECTION('',(0.985460115744347,-1.01181573982395E-14,-0.169906916507654));
#50516=DIRECTION('center_axis',(-0.169906916507646,2.03719652137209E-17,
0.985460115744348));
#50517=DIRECTION('ref_axis',(1.19900741137893E-16,1.,-3.62640108812244E-32));
#50518=DIRECTION('',(-0.985460115744347,1.01181573982395E-14,-0.169906916507654));
#50519=DIRECTION('center_axis',(0.,-1.,1.45983193964168E-32));
#50520=DIRECTION('ref_axis',(-1.,1.78777851217525E-48,1.22464679914735E-16));
#50521=DIRECTION('',(-1.01199007411378E-14,-1.,1.E-14));
#50522=DIRECTION('',(-1.01199007411378E-14,-1.,1.E-14));
#50523=DIRECTION('center_axis',(2.84375793746248E-80,1.45983193964168E-32,
1.));
#50524=DIRECTION('ref_axis',(1.,-1.94800364359783E-48,8.31581056687692E-97));
#50525=DIRECTION('center_axis',(-1.94800364359783E-48,-1.45983193964168E-32,
-1.));
#50526=DIRECTION('ref_axis',(0.,-1.,1.45983193964168E-32));
#50527=DIRECTION('center_axis',(-8.47826271278967E-17,-0.707106781186549,
-0.707106781186547));
#50528=DIRECTION('ref_axis',(-1.48909625690539E-32,0.707106781186547,-0.707106781186549));
#50529=DIRECTION('',(0.060400598363751,0.705815757729061,-0.705815757729064));
#50530=DIRECTION('center_axis',(-0.120142332833053,0.707106781186551,0.696825530431705));
#50531=DIRECTION('ref_axis',(0.985460115744348,6.9160230078685E-16,0.169906916507646));
#50532=DIRECTION('',(0.607508557019365,0.60750855701936,-0.511729133718712));
#50533=DIRECTION('center_axis',(-0.707106781186545,0.707106781186551,3.68912701758404E-17));
#50534=DIRECTION('ref_axis',(5.21721346158438E-17,4.12364695333908E-32,
1.));
#50535=DIRECTION('',(0.607508557019368,0.607508557019363,0.511729133718706));
#50536=DIRECTION('center_axis',(-0.120142332833053,0.707106781186546,-0.69682553043171));
#50537=DIRECTION('ref_axis',(-0.985460115744348,3.52718437708667E-16,0.169906916507646));
#50538=DIRECTION('',(0.0604005983636862,0.705815757729064,0.705815757729067));
#50539=DIRECTION('center_axis',(6.27824535754649E-17,-0.707106781186549,
0.707106781186546));
#50540=DIRECTION('ref_axis',(-1.,-8.87877973254815E-17,-2.5390518211582E-32));
#50541=DIRECTION('axis',(0.,0.,1.));
#50542=DIRECTION('refdir',(1.,0.,0.));
#50543=DIRECTION('center_axis',(0.,1.,-1.45983193964168E-32));
#50544=DIRECTION('ref_axis',(-1.,0.,0.));
#50545=DIRECTION('center_axis',(0.,-1.,6.6666666666222E-12));
#50546=DIRECTION('ref_axis',(1.,0.,0.));
#50547=DIRECTION('',(0.,-1.,1.45983193964168E-32));
#50548=DIRECTION('center_axis',(0.,-1.,6.6666666666222E-12));
#50549=DIRECTION('ref_axis',(1.,0.,0.));
#50550=DIRECTION('center_axis',(0.,-1.,0.));
#50551=DIRECTION('ref_axis',(0.,0.,-1.));
#50552=DIRECTION('',(8.65956056235495E-17,0.707106781186546,-0.707106781186549));
#50553=DIRECTION('center_axis',(0.,1.,-1.81818181817851E-12));
#50554=DIRECTION('ref_axis',(1.,0.,0.));
#50555=DIRECTION('center_axis',(0.470181317528933,0.878565373676135,0.0839786450478365));
#50556=DIRECTION('ref_axis',(-0.430724319865323,0.14537209543693,0.890698329483575));
#50557=DIRECTION('center_axis',(-0.431958871988205,0.885461953092126,0.171372875732875));
#50558=DIRECTION('ref_axis',(0.528713288045884,0.0946722161324461,0.843504256383026));
#50559=DIRECTION('center_axis',(0.476999112541715,0.878565373674465,0.0243871034496678));
#50560=DIRECTION('ref_axis',(-0.315693828177029,0.145372095444832,0.937658978902731));
#50561=DIRECTION('center_axis',(-0.407074030600313,0.885461953092291,0.224160351616429));
#50562=DIRECTION('ref_axis',(0.630263341829312,0.0946722161298985,0.770587627359278));
#50563=DIRECTION('center_axis',(0.47629434659331,0.878565373678942,-0.0355890372956794));
#50564=DIRECTION('ref_axis',(-0.195684656275447,0.145372095425782,0.969832186086788));
#50565=DIRECTION('center_axis',(-0.375769388577795,0.885461953092213,0.273412684844712));
#50566=DIRECTION('ref_axis',(0.721873766209692,0.0946722161311678,0.685518371125857));
#50567=DIRECTION('center_axis',(0.468078134286444,0.878565373674476,-0.0950039177252697));
#50568=DIRECTION('ref_axis',(-0.0725894203991882,0.145372095453218,0.986710560351743));
#50569=DIRECTION('center_axis',(-0.338538638842928,0.885461953090034,0.318353136689997));
#50570=DIRECTION('ref_axis',(0.802099810062447,0.0946722161536946,0.589638080678593));
#50571=DIRECTION('center_axis',(0.452480050181005,0.878565373677713,-0.152920529565967));
#50572=DIRECTION('ref_axis',(0.0516505940339392,0.145372095401793,0.988027919653303));
#50573=DIRECTION('center_axis',(-0.295968932481847,0.885461953094103,0.358272969435782));
#50574=DIRECTION('ref_axis',(0.869676260782141,0.0946722161116901,0.484458845443548));
#50575=DIRECTION('center_axis',(0.429746085383579,0.87856537367488,-0.208425493347162));
#50576=DIRECTION('ref_axis',(0.175076047702811,0.145372095419575,0.97376348842729));
#50577=DIRECTION('center_axis',(-0.248731619302135,0.885461953092945,0.392542623397975));
#50578=DIRECTION('ref_axis',(0.923537397331102,0.0946722161240135,0.371639404833586));
#50579=DIRECTION('center_axis',(0.400234768100223,0.878565373673598,-0.260643462579693));
#50580=DIRECTION('ref_axis',(0.295740447509778,0.145372095427147,0.94414222529121));
#50581=DIRECTION('center_axis',(-0.197571659886334,0.885461953093207,0.420621645703265));
#50582=DIRECTION('ref_axis',(0.962833797434217,0.0946722161215446,0.252958988796685));
#50583=DIRECTION('center_axis',(0.364411509455074,0.878565373679554,-0.3087509286593));
#50584=DIRECTION('ref_axis',(0.411740843713011,0.145372095421878,0.899631275296246));
#50585=DIRECTION('center_axis',(-0.143295877392587,0.885461953091437,0.442067213384781));
#50586=DIRECTION('ref_axis',(0.986945733379162,0.0946722161389514,0.130289258406083));
#50587=DIRECTION('center_axis',(0.322841263593088,0.878565373676854,-0.35198920821194));
#50588=DIRECTION('ref_axis',(0.521247840989627,0.145372095407339,0.840932602614819));
#50589=DIRECTION('center_axis',(-0.0867602332807392,0.885461953092501,0.456541117038417));
#50590=DIRECTION('ref_axis',(0.995492945540836,0.0946722161283294,0.0055647885656998));
#50591=DIRECTION('center_axis',(0.276179618172625,0.878565373680365,-0.389676407646017));
#50592=DIRECTION('ref_axis',(0.622534448311122,0.145372095417224,0.768971920514639));
#50593=DIRECTION('center_axis',(-0.0288563284685773,0.88546195309315,0.463815094549301));
#50594=DIRECTION('ref_axis',(0.988340639271075,0.0946722161237086,-0.11924744131204));
#50595=DIRECTION('center_axis',(0.225162455177494,0.878565373680138,-0.421218177372158));
#50596=DIRECTION('ref_axis',(0.714003315567455,0.145372095415238,0.684884091823766));
#50597=DIRECTION('center_axis',(0.0295026578968582,0.885461953094759,0.463774430945299));
#50598=DIRECTION('ref_axis',(0.965601610712996,0.09467221610468,-0.242179067812014));
#50599=DIRECTION('center_axis',(0.170594345751946,0.878565373678822,-0.446117084821976));
#50600=DIRECTION('ref_axis',(0.794211924045204,0.145372095394835,0.589995231832369));
#50601=DIRECTION('center_axis',(0.0873963697059013,0.885461953095116,0.45641976752022));
#50602=DIRECTION('ref_axis',(0.927634467930516,0.0946722161010694,-0.361291385734258));
#50603=DIRECTION('center_axis',(0.113335861610607,0.878565373681749,-0.463980459330379));
#50604=DIRECTION('ref_axis',(0.861895335995359,0.145372095376466,0.485801794639854));
#50605=DIRECTION('center_axis',(0.143911788527641,0.885461953092717,0.441867091723299));
#50606=DIRECTION('ref_axis',(0.875037975450806,0.0946722161263171,-0.474705922664428));
#50607=DIRECTION('center_axis',(0.0542900032060115,0.878565373680826,-0.474526584841104));
#50608=DIRECTION('ref_axis',(0.915986143629403,0.145372095381604,0.373946972929714));
#50609=DIRECTION('center_axis',(0.198157632482187,0.885461953090638,0.420345907935318));
#50610=DIRECTION('ref_axis',(0.808641611378265,0.0946722161478671,-0.580634063621154));
#50611=DIRECTION('center_axis',(-0.00561204098253765,0.878565373679935,
-0.47758914263899));
#50612=DIRECTION('ref_axis',(0.955631302573077,0.145372095420351,0.256194784130318));
#50613=DIRECTION('center_axis',(0.2492784122292,0.88546195309152,0.392195618057929));
#50614=DIRECTION('ref_axis',(0.729492486028889,0.0946722161374401,-0.677405258555775));
#50615=DIRECTION('center_axis',(-0.0654255799087193,0.878565373682163,-0.473119834355239));
#50616=DIRECTION('ref_axis',(0.980205585037586,0.145372095405399,0.134402250496665));
#50617=DIRECTION('center_axis',(0.296467922535388,0.885461953097206,0.357860168955463));
#50618=DIRECTION('ref_axis',(0.638838828380997,0.094672216080367,-0.763493367918299));
#50619=DIRECTION('center_axis',(-0.124207318411051,0.878565373676778,-0.461189143659432));
#50620=DIRECTION('ref_axis',(0.989321439874569,0.14537209543964,0.0104901130593315));
#50621=DIRECTION('center_axis',(0.338981956513975,0.885461953090639,0.317881051317736));
#50622=DIRECTION('ref_axis',(0.538110300825814,0.0946722161462289,-0.837540730732013));
#50623=DIRECTION('center_axis',(-0.181030233209146,0.878565373684908,-0.441985224669491));
#50624=DIRECTION('ref_axis',(0.982835104623311,0.145372095356493,-0.113587459746872));
#50625=DIRECTION('center_axis',(0.376150042589092,0.885461953090726,0.272888759550445));
#50626=DIRECTION('ref_axis',(0.428895452353032,0.0946722161448653,-0.898379575926072));
#50627=DIRECTION('center_axis',(-0.234998193211149,0.878565373675165,-0.415810934640389));
#50628=DIRECTION('ref_axis',(0.960848872626057,0.145372095417506,-0.23587369045139));
#50629=DIRECTION('center_axis',(0.407386017797145,0.885461953092542,0.223592849011155));
#50630=DIRECTION('ref_axis',(0.312916666379303,0.0946722161266354,-0.945050438545867));
#50631=DIRECTION('center_axis',(-0.285260091217153,0.878565373681205,-0.383079057802938));
#50632=DIRECTION('ref_axis',(0.923709479949017,0.145372095379356,-0.354440052106603));
#50633=DIRECTION('center_axis',(0.432197272136797,0.885461953093454,0.170770745683908));
#50634=DIRECTION('ref_axis',(0.192002997652503,0.0946722161181877,-0.976817291200214));
#50635=DIRECTION('center_axis',(-0.331023267233894,0.878565373679115,-0.344305795364926));
#50636=DIRECTION('ref_axis',(0.872002636966723,0.14537209540145,-0.467416682416955));
#50637=DIRECTION('center_axis',(0.450192517310335,0.885461953094449,0.115255485682668));
#50638=DIRECTION('ref_axis',(0.0680613269555309,0.0946722161089431,-0.993179151648923));
#50639=DIRECTION('center_axis',(-0.371566008536628,0.87856537368448,-0.300102624884903));
#50640=DIRECTION('ref_axis',(0.806543791497076,0.145372095359132,-0.573021872434566));
#50641=DIRECTION('center_axis',(0.46108795755193,0.885461953094479,0.057922577831964));
#50642=DIRECTION('ref_axis',(-0.0569537115214824,0.0946722161090591,-0.993877983577928));
#50643=DIRECTION('center_axis',(-0.406248931959853,0.87856537368365,-0.251166656715393));
#50644=DIRECTION('ref_axis',(0.728365268655383,0.145372095392437,-0.669590165174029));
#50645=DIRECTION('center_axis',(0.464711765269602,0.885461953090712,-0.000323803632485891));
#50646=DIRECTION('ref_axis',(-0.181070555926217,0.0946722161451853,-0.97890276599197));
#50647=DIRECTION('center_axis',(-0.434525067050534,0.878565373681443,-0.198269640320233));
#50648=DIRECTION('ref_axis',(0.638699990373455,0.145372095395856,-0.75559862107945));
#50649=DIRECTION('center_axis',(0.46100679083195,0.885461953093654,-0.0585650785912394));
#50650=DIRECTION('ref_axis',(-0.302331809531034,0.094672216116691,-0.9484896670187));
#50651=DIRECTION('center_axis',(-0.455948482255112,0.878565373679943,-0.142245793259001));
#50652=DIRECTION('ref_axis',(0.538962031740231,0.145372095419794,-0.829690835321025));
#50653=DIRECTION('center_axis',(0.450031463915207,0.885461953093974,-0.115882747246262));
#50654=DIRECTION('ref_axis',(-0.418825109881704,0.0946722161145024,-0.90311831939594));
#50655=DIRECTION('center_axis',(-0.470181317508262,0.878565373682988,-0.0839786450918718));
#50656=DIRECTION('ref_axis',(0.430724319845604,0.145372095368486,-0.890698329504281));
#50657=DIRECTION('center_axis',(0.431958824442153,0.885461961244214,-0.171372953455624));
#50658=DIRECTION('ref_axis',(-0.528713326932488,0.0946721347508802,-0.843504241142682));
#50659=DIRECTION('center_axis',(-0.476999112532178,0.878565373678833,-0.0243871034788126));
#50660=DIRECTION('ref_axis',(0.315693828207894,0.145372095426544,-0.937658978895174));
#50661=DIRECTION('center_axis',(0.407073973687001,0.885461961244578,-0.224160422768117));
#50662=DIRECTION('ref_axis',(-0.630263378499859,0.0946721347472922,-0.770587607364882));
#50663=DIRECTION('center_axis',(-0.476294346599364,0.878565373674358,0.0355890373278207));
#50664=DIRECTION('ref_axis',(0.195684656259467,0.145372095454662,-0.969832186085683));
#50665=DIRECTION('center_axis',(0.375769388575765,0.885461953092483,-0.273412684846627));
#50666=DIRECTION('ref_axis',(-0.721873766210669,0.0946722161286249,-0.68551837112518));
#50667=DIRECTION('center_axis',(-0.468078134283175,0.878565373681661,0.0950039176749343));
#50668=DIRECTION('ref_axis',(0.0725894203633281,0.145372095377612,-0.98671056036552));
#50669=DIRECTION('center_axis',(0.338538638809758,0.885461953093661,-0.318353136715184));
#50670=DIRECTION('ref_axis',(-0.802099810076275,0.0946722161163834,-0.589638080665773));
#50671=DIRECTION('center_axis',(-0.45248005018208,0.878565373679752,0.152920529551074));
#50672=DIRECTION('ref_axis',(-0.0516505939966993,0.145372095404103,-0.98802791965491));
#50673=DIRECTION('center_axis',(0.295968932486342,0.885461953093587,-0.358272969433345));
#50674=DIRECTION('ref_axis',(-0.869676260780677,0.0946722161163057,-0.484458845445274));
#50675=DIRECTION('center_axis',(-0.429746085391914,0.878565373681383,0.208425493302567));
#50676=DIRECTION('ref_axis',(-0.17507604768326,0.145372095379237,-0.973763488436827));
#50677=DIRECTION('center_axis',(0.248731619323381,0.885461953090817,-0.392542623389315));
#50678=DIRECTION('ref_axis',(-0.923537397325435,0.0946722161445156,-0.371639404842446));
#50679=DIRECTION('center_axis',(-0.400234768116551,0.878565373680973,0.260643462529762));
#50680=DIRECTION('ref_axis',(-0.295740447488144,0.145372095380758,-0.944142225305129));
#50681=DIRECTION('center_axis',(0.197571659905606,0.885461953091393,-0.420621645698031));
#50682=DIRECTION('ref_axis',(-0.962833797430249,0.0946722161392853,-0.252958988805146));
#50683=DIRECTION('center_axis',(-0.364411509442283,0.878565373675362,0.308750928686326));
#50684=DIRECTION('ref_axis',(-0.411740843782727,0.14537209541642,-0.89963127526522));
#50685=DIRECTION('center_axis',(0.143295877377764,0.885461953092811,-0.442067213386835));
#50686=DIRECTION('ref_axis',(-0.986945733381312,0.0946722161256203,-0.130289258399489));
#50687=DIRECTION('center_axis',(-0.32284126361482,0.878565373682674,0.35198920817748));
#50688=DIRECTION('ref_axis',(-0.521247840921593,0.145372095402714,-0.840932602657789));
#50689=DIRECTION('center_axis',(0.0867602333015312,0.885461953090746,-0.456541117037869));
#50690=DIRECTION('ref_axis',(-0.995492945539012,0.0946722161469667,-0.00556478857491395));
#50691=DIRECTION('center_axis',(-0.276179618153645,0.878565373676274,0.389676407668691));
#50692=DIRECTION('ref_axis',(-0.622534448319981,0.145372095443063,-0.768971920502582));
#50693=DIRECTION('center_axis',(0.0288563284973618,0.885461953090383,-0.463815094552793));
#50694=DIRECTION('ref_axis',(-0.988340639270242,0.0946722161494783,0.119247441298489));
#50695=DIRECTION('center_axis',(-0.225162455131814,0.878565373671252,0.42121817741511));
#50696=DIRECTION('ref_axis',(-0.714003315623988,0.145372095441861,-0.684884091759178));
#50697=DIRECTION('center_axis',(-0.0295026578689006,0.885461953092215,-0.463774430951935));
#50698=DIRECTION('ref_axis',(-0.965601610713841,0.0946722161302304,0.242179067798656));
#50699=DIRECTION('center_axis',(-0.170594345743913,0.878565373677633,0.446117084827388));
#50700=DIRECTION('ref_axis',(-0.794211924010337,0.145372095431894,-0.589995231870173));
#50701=DIRECTION('center_axis',(-0.0873963696730955,0.885461953092048,-0.456419767532454));
#50702=DIRECTION('ref_axis',(-0.927634467933496,0.0946722161323006,0.361291385718422));
#50703=DIRECTION('center_axis',(-0.113335861582412,0.878565373677204,0.463980459345873));
#50704=DIRECTION('ref_axis',(-0.861895335999343,0.145372095404732,-0.485801794624327));
#50705=DIRECTION('center_axis',(-0.143911788525932,0.885461953092382,-0.441867091724528));
#50706=DIRECTION('ref_axis',(-0.875037975451224,0.0946722161280739,0.474705922663308));
#50707=DIRECTION('center_axis',(-0.0542900031638738,0.878565373674397,0.474526584857829));
#50708=DIRECTION('ref_axis',(-0.915986143631796,0.145372095421936,-0.373946972908173));
#50709=DIRECTION('center_axis',(-0.198157632504344,0.885461953092994,-0.42034590791991));
#50710=DIRECTION('ref_axis',(-0.808641611372961,0.094672216123831,0.58063406363246));
#50711=DIRECTION('center_axis',(0.005612041014381,0.878565373675177,0.477589142647369));
#50712=DIRECTION('ref_axis',(-0.955631302593608,0.145372095417575,-0.25619478405531));
#50713=DIRECTION('center_axis',(-0.249278412244268,0.885461953093368,-0.392195618044179));
#50714=DIRECTION('ref_axis',(-0.729492486023782,0.0946722161193055,0.677405258563809));
#50715=DIRECTION('center_axis',(0.0654255799497689,0.8785653736764,0.473119834360264));
#50716=DIRECTION('ref_axis',(-0.980205585048038,0.145372095409979,-0.134402250415481));
#50717=DIRECTION('center_axis',(-0.296467922503249,0.88546195309275,-0.357860168993115));
#50718=DIRECTION('ref_axis',(-0.638838828395272,0.0946722161246698,0.763493367900862));
#50719=DIRECTION('center_axis',(0.124207318409077,0.878565373677123,0.461189143659306));
#50720=DIRECTION('ref_axis',(-0.989321439880191,0.145372095405823,-0.0104901129977411));
#50721=DIRECTION('center_axis',(-0.338981956504719,0.885461953089255,-0.31788105133146));
#50722=DIRECTION('ref_axis',(-0.538110300831041,0.0946722161611699,0.837540730726965));
#50723=DIRECTION('center_axis',(0.181030233273647,0.87856537367578,0.441985224661216));
#50724=DIRECTION('ref_axis',(-0.982835104611445,0.145372095414437,0.113587459775392));
#50725=DIRECTION('center_axis',(-0.376150042596336,0.885461953092368,-0.272888759535135));
#50726=DIRECTION('ref_axis',(-0.428895452346745,0.0946722161297347,0.898379575930667));
#50727=DIRECTION('center_axis',(0.234998193217866,0.878565373674249,0.415810934638528));
#50728=DIRECTION('ref_axis',(-0.960848872633557,0.145372095452043,0.235873690399552));
#50729=DIRECTION('center_axis',(-0.407386017798389,0.885461953092885,-0.22359284900753));
#50730=DIRECTION('ref_axis',(-0.312916666377336,0.0946722161234403,0.945050438546838));
#50731=DIRECTION('center_axis',(0.28526009123465,0.878565373678539,0.383079057796023));
#50732=DIRECTION('ref_axis',(-0.923709479959308,0.145372095424003,0.354440052061472));
#50733=DIRECTION('center_axis',(-0.432197272133671,0.885461953092218,-0.170770745698229));
#50734=DIRECTION('ref_axis',(-0.192002997658825,0.0946722161312271,0.976817291197708));
#50735=DIRECTION('center_axis',(0.331023267286328,0.878565373670557,0.344305795336355));
#50736=DIRECTION('ref_axis',(-0.87200263694079,0.14537209544692,0.467416682451193));
#50737=DIRECTION('center_axis',(-0.450192517308106,0.885461953091926,-0.115255485710757));
#50738=DIRECTION('ref_axis',(-0.0680613269678815,0.0946722161341875,0.99317915164567));
#50739=DIRECTION('center_axis',(0.371566008567699,0.878565373679051,0.300102624862328));
#50740=DIRECTION('ref_axis',(-0.806543791482632,0.145372095393174,0.573021872446261));
#50741=DIRECTION('center_axis',(-0.46108795755314,0.885461953092287,-0.0579225778558486));
#50742=DIRECTION('ref_axis',(0.056953711510405,0.0946722161303211,0.993877983576537));
#50743=DIRECTION('center_axis',(0.406248931974331,0.878565373680964,0.251166656701371));
#50744=DIRECTION('ref_axis',(-0.728365268650857,0.14537209541337,0.669590165174408));
#50745=DIRECTION('center_axis',(-0.464711749675408,0.885461961242092,0.000323893391809522));
#50746=DIRECTION('ref_axis',(0.181070597688607,0.0946721347711845,0.978902766136942));
#50747=DIRECTION('center_axis',(0.434525067034736,0.878565373684967,0.19826964033924));
#50748=DIRECTION('ref_axis',(-0.638699990404053,0.145372095388073,0.755598621055083));
#50749=DIRECTION('center_axis',(-0.461006790844013,0.885461953090007,0.0585650785514288));
#50750=DIRECTION('ref_axis',(0.302331809512097,0.0946722161538305,0.94848966702103));
#50751=DIRECTION('center_axis',(0.455948482273978,0.878565373675013,0.142245793228975));
#50752=DIRECTION('ref_axis',(-0.538962031724008,0.145372095451307,0.829690835326042));
#50753=DIRECTION('center_axis',(-0.450031463932584,0.885461953090173,0.115882747207818));
#50754=DIRECTION('ref_axis',(0.418825109863107,0.0946722161522763,0.903118319400605));
#50755=DIRECTION('center_axis',(0.,1.,0.));
#50756=DIRECTION('ref_axis',(0.,0.,1.));
#50757=DIRECTION('',(8.65956056235503E-17,-0.707106781186539,0.707106781186556));
#50758=DIRECTION('center_axis',(0.,-1.,1.81818181817852E-12));
#50759=DIRECTION('ref_axis',(1.,0.,0.));
#50760=DIRECTION('center_axis',(-0.458818968797312,-0.87926072867782,-0.12800673762236));
#50761=DIRECTION('ref_axis',(0.477771165970434,-0.122671608382798,-0.869877226661343));
#50762=DIRECTION('center_axis',(-0.0510528487249554,0.705424652954679,0.70694389143753));
#50763=DIRECTION('ref_axis',(-0.993134147532106,-0.110462470651433,0.0385046436583641));
#50764=DIRECTION('center_axis',(-0.0747813385372569,0.160364694830346,0.984220969121541));
#50765=DIRECTION('ref_axis',(-0.00205849356672293,-0.987007291747137,0.160662281330179));
#50766=DIRECTION('center_axis',(-0.0897986376521124,-0.137109889430621,
0.986477107132318));
#50767=DIRECTION('ref_axis',(0.0344440051966361,-0.99031373067732,-0.134507714789833));
#50768=DIRECTION('center_axis',(0.473783675120008,-0.879260729005327,-0.0492909689375137));
#50769=DIRECTION('ref_axis',(-0.342664178411406,-0.132503133709511,-0.930066761254694));
#50770=DIRECTION('center_axis',(-0.43915754583858,-0.879260728678471,-0.184502631246384));
#50771=DIRECTION('ref_axis',(0.583028323247161,-0.122671608378535,-0.80313737977349));
#50772=DIRECTION('center_axis',(-0.139253845558219,0.705424652962835,0.694970809091656));
#50773=DIRECTION('ref_axis',(-0.990128899650558,-0.110462470602953,-0.0862716909830027));
#50774=DIRECTION('center_axis',(-0.197547261949399,0.160364694810999,0.967087505841364));
#50775=DIRECTION('ref_axis',(-0.0221785849573792,-0.987007291750282,0.159137413580408));
#50776=DIRECTION('center_axis',(-0.212728914248208,-0.137109889396287,0.967443686874082));
#50777=DIRECTION('ref_axis',(0.0510306907533597,-0.990313730682094,-0.129130102701686));
#50778=DIRECTION('center_axis',(0.476225545845609,-0.879260729009032,0.0104785450591571));
#50779=DIRECTION('ref_axis',(-0.22339389441128,-0.132503133683585,-0.965680116551952));
#50780=DIRECTION('center_axis',(-0.412570346035416,-0.879260728680131,-0.238088808164313));
#50781=DIRECTION('ref_axis',(0.679090775560755,-0.122671608348556,-0.723731576659102));
#50782=DIRECTION('center_axis',(-0.225258726217264,0.705424652951847,0.672037621916171));
#50783=DIRECTION('ref_axis',(-0.971508727523255,-0.110462470666646,-0.209687469631274));
#50784=DIRECTION('center_axis',(-0.317197747029055,0.160364694845115,0.934702494875736));
#50785=DIRECTION('ref_axis',(-0.0419489068256087,-0.987007291744729,0.15510285380634));
#50786=DIRECTION('center_axis',(-0.332304328785672,-0.137109889416642,0.933153101744007));
#50787=DIRECTION('ref_axis',(0.0668125918448412,-0.990313730679244,-0.121716031808188));
#50788=DIRECTION('center_axis',(0.471157055240052,-0.879260729008505,0.0700828061720898));
#50789=DIRECTION('ref_axis',(-0.100600555230665,-0.132503133686602,-0.986064119543203));
#50790=DIRECTION('center_axis',(-0.379476665467412,-0.879260728673145,-0.287920182305626));
#50791=DIRECTION('ref_axis',(0.764443560670196,-0.122671608391771,-0.632912094247257));
#50792=DIRECTION('center_axis',(-0.307711142019788,0.705424652963427,0.638506000025298));
#50793=DIRECTION('ref_axis',(-0.937567282419065,-0.110462470446083,-0.329796351647918));
#50794=DIRECTION('center_axis',(-0.431845834156375,0.160364694827406,0.887576667209486));
#50795=DIRECTION('ref_axis',(-0.0610576693612533,-0.987007291747613,0.148622229323928));
#50796=DIRECTION('center_axis',(-0.446639105538544,-0.137109889604953,0.88414613474032));
#50797=DIRECTION('ref_axis',(0.0815408184091089,-0.99031373065616,-0.112382426593533));
#50798=DIRECTION('center_axis',(0.458658136415686,-0.879260729004838,0.128581819591928));
#50799=DIRECTION('ref_axis',(0.0237793148120579,-0.132503133713074,-0.990897302319107));
#50800=DIRECTION('center_axis',(-0.34039841113939,-0.879260728676267,-0.333210883227814));
#50801=DIRECTION('ref_axis',(0.837740614229303,-0.12267160839414,-0.532111209959632));
#50802=DIRECTION('center_axis',(-0.385310769468071,0.705424652953116,0.594904757030819));
#50803=DIRECTION('ref_axis',(-0.888839841209568,-0.110462470660403,-0.444704148006457));
#50804=DIRECTION('center_axis',(-0.539683454506372,0.160364694818675,0.826453225287301));
#50805=DIRECTION('ref_axis',(-0.0792035159775513,-0.987007291749035,0.139797743511935));
#50806=DIRECTION('center_axis',(-0.553930116811,-0.137109889434077,0.821195655071998));
#50807=DIRECTION('ref_axis',(0.0949830976385117,-0.990313730676833,-0.101276482936196));
#50808=DIRECTION('center_axis',(0.43892590479466,-0.879260729009627,0.185053020839027));
#50809=DIRECTION('ref_axis',(0.147784170781883,-0.132503133701823,-0.980103442716894));
#50810=DIRECTION('center_axis',(-0.295951870544099,-0.879260728675819,-0.373246649455714));
#50811=DIRECTION('ref_axis',(0.897825997808071,-0.122671608373307,-0.42291861410802));
#50812=DIRECTION('center_axis',(-0.456833815793938,0.705424652957863,0.541921510688059));
#50813=DIRECTION('ref_axis',(-0.826094864746202,-0.110462470633544,-0.552598694371863));
#50814=DIRECTION('center_axis',(-0.639009944386313,0.160364694822305,0.752296122301551));
#50815=DIRECTION('ref_axis',(-0.0961002758384732,-0.987007291748441,0.128768563784709));
#50816=DIRECTION('center_axis',(-0.652485319215739,-0.137109889569417,0.745294429329911));
#50817=DIRECTION('ref_axis',(0.106927436622317,-0.990313730661046,-0.0885733490480162));
#50818=DIRECTION('center_axis',(0.412271549450918,-0.879260729009111,0.238605825443777));
#50819=DIRECTION('ref_axis',(0.269458382201844,-0.132503133682721,-0.953852766324774));
#50820=DIRECTION('center_axis',(-0.246837992119163,-0.879260728680677,-0.407396093067306));
#50821=DIRECTION('ref_axis',(0.943752129107433,-0.12267160836025,-0.307056338979503));
#50822=DIRECTION('center_axis',(-0.521152320027383,0.705424652950378,0.480391838336077));
#50823=DIRECTION('ref_axis',(-0.750321878732873,-0.11046247067845,-0.651778429273618));
#50824=DIRECTION('center_axis',(-0.728258865719209,0.160364694810991,0.666274860068687));
#50825=DIRECTION('ref_axis',(-0.11148147693236,-0.987007291750285,0.115708626872619));
#50826=DIRECTION('center_axis',(-0.740750438384919,-0.137109889435947,0.6576394652478));
#50827=DIRECTION('ref_axis',(0.117185466079654,-0.990313730676577,-0.0744733601574021));
#50828=DIRECTION('center_axis',(0.379115425475678,-0.879260729003382,0.288395673682593));
#50829=DIRECTION('ref_axis',(0.386883073940472,-0.132503133722346,-0.9125592619946));
#50830=DIRECTION('center_axis',(-0.193831331191601,-0.87926072867378,-0.435120656899377));
#50831=DIRECTION('ref_axis',(0.974794725525188,-0.122671608410494,-0.186351602027606));
#50832=DIRECTION('center_axis',(-0.577251940727125,0.705424652962881,0.411286099836799));
#50833=DIRECTION('ref_axis',(-0.662715868563518,-0.110462470601243,-0.74067922891274));
#50834=DIRECTION('center_axis',(-0.806022709697782,0.160364694810026,0.56974604527801));
#50835=DIRECTION('ref_axis',(-0.12510454854524,-0.987007291750441,0.100823895802292));
#50836=DIRECTION('center_axis',(-0.817333480602069,-0.137109889640004,0.559613133914683));
#50837=DIRECTION('ref_axis',(0.125595410813388,-0.990313730651293,-0.0591988823047837));
#50838=DIRECTION('center_axis',(0.339980424795607,-0.87926072900711,0.333637349800174));
#50839=DIRECTION('ref_axis',(0.498206388459968,-0.132503133697411,-0.856874152987498));
#50840=DIRECTION('center_axis',(-0.137767834283508,-0.879260728679782,-0.455983108062493));
#50841=DIRECTION('ref_axis',(0.990464226825965,-0.122671608346041,-0.062707988995335));
#50842=DIRECTION('center_axis',(-0.624247953590279,0.70542465295917,0.335694133752414));
#50843=DIRECTION('ref_axis',(-0.564658433181154,-0.110462470627397,-0.817899074715393));
#50844=DIRECTION('center_axis',(-0.87107509404991,0.160364694808483,0.464231995003493));
#50845=DIRECTION('ref_axis',(-0.136754646693211,-0.987007291750693,0.0843491116656059));
#50846=DIRECTION('center_axis',(-0.881026685627242,-0.137109889424586,0.452761369194254));
#50847=DIRECTION('ref_axis',(0.132024640697849,-0.990313730678156,-0.0429908022595161));
#50848=DIRECTION('center_axis',(0.295483729709509,-0.87926072900682,0.373617365634084));
#50849=DIRECTION('ref_axis',(0.601672690632676,-0.132503133698707,-0.787675626706107));
#50850=DIRECTION('center_axis',(-0.0795316564451785,-0.879260728670998,
-0.469654433216628));
#50851=DIRECTION('ref_axis',(0.990513515580251,-0.122671608429301,0.0619245665162102));
#50852=DIRECTION('center_axis',(-0.661399203311531,0.705424652954368,0.254808070639612));
#50853=DIRECTION('ref_axis',(-0.457695996992253,-0.110462470652642,-0.882220163516218));
#50854=DIRECTION('center_axis',(-0.922390103810698,0.160364694827014,0.351396728848077));
#50855=DIRECTION('ref_axis',(-0.146248042387767,-0.987007291747676,0.0665440916585738));
#50856=DIRECTION('center_axis',(-0.930825573503264,-0.137109889365752,0.338769287200641));
#50857=DIRECTION('ref_axis',(0.136371763177505,-0.990313730686301,-0.0261047317940428));
#50858=DIRECTION('center_axis',(0.246327079714757,-0.879260729010737,0.407705212400709));
#50859=DIRECTION('ref_axis',(0.695650255042948,-0.132503133672225,-0.70605498527078));
#50860=DIRECTION('center_axis',(-0.0200412167434643,-0.879260728679161,
-0.4759190273923));
#50861=DIRECTION('ref_axis',(0.974941814511513,-0.12267160834986,0.185580534598479));
#50862=DIRECTION('center_axis',(-0.688119792457086,0.705424652960527,0.169903532112602));
#50863=DIRECTION('ref_axis',(-0.343515421574124,-0.110462470618877,-0.932628113304293));
#50864=DIRECTION('center_axis',(-0.95915847062965,0.160364694817076,0.233019726365851));
#50865=DIRECTION('ref_axis',(-0.153435019064046,-0.987007291749297,0.0476896315621617));
#50866=DIRECTION('center_axis',(-0.965944786020493,-0.137109889429341,0.219434611172664));
#50867=DIRECTION('ref_axis',(0.138568221601756,-0.99031373067749,-0.00880697415449896));
#50868=DIRECTION('center_axis',(0.193285704483541,-0.8792607290072,0.435363304457355));
#50869=DIRECTION('ref_axis',(0.778656999385461,-0.132503133696502,-0.613299434916287));
#50870=DIRECTION('center_axis',(0.0397652848177643,-0.879260728674355,-0.474678094222183));
#50871=DIRECTION('ref_axis',(0.943994698616188,-0.122671608384915,0.306309786785845));
#50872=DIRECTION('center_axis',(-0.703988321455513,0.705424652950248,0.0823195132655206));
#50873=DIRECTION('ref_axis',(-0.223917402658416,-0.110462470676263,-0.968327960640817));
#50874=DIRECTION('center_axis',(-0.980800335390021,0.160364694827208,0.110967863599328));
#50875=DIRECTION('ref_axis',(-0.158202233851104,-0.987007291747647,0.0280830774933107));
#50876=DIRECTION('center_axis',(-0.985830472241187,-0.137109889443731,0.0966393202451538));
#50877=DIRECTION('ref_axis',(0.138579376349179,-0.990313730675486,0.00862967474895586));
#50878=DIRECTION('center_axis',(0.13719609829506,-0.879260729013987,0.456155457082784));
#50879=DIRECTION('ref_axis',(0.84938385766004,-0.132503133672304,-0.51087178617885));
#50880=DIRECTION('center_axis',(0.0989446641324139,-0.879260728675946,-0.465951203934456));
#50881=DIRECTION('ref_axis',(0.89816022240913,-0.122671608372746,0.422208350676802));
#50882=DIRECTION('center_axis',(-0.708754534050761,0.705424652952351,-0.00656273338962056));
#50883=DIRECTION('ref_axis',(-0.100788072609723,-0.110462470665894,-0.988756697572261));
#50884=DIRECTION('center_axis',(-0.986974392960287,0.160364694833053,-0.012834028665036));
#50885=DIRECTION('ref_axis',(-0.160474504900988,-0.987007291746699,0.00803363651342823));
#50886=DIRECTION('center_axis',(-0.990169023015502,-0.137109889404239,-0.0276800304928161));
#50887=DIRECTION('ref_axis',(0.136405051494663,-0.990313730680973,0.0259302285271826));
#50888=DIRECTION('center_axis',(0.0789428275537311,-0.879260729002341,0.469753765724228));
#50889=DIRECTION('ref_axis',(0.906715425170266,-0.132503133730031,-0.400387384054525));
#50890=DIRECTION('center_axis',(0.156563626958717,-0.879260728673591,-0.449875984829061));
#50891=DIRECTION('ref_axis',(0.838161222937335,-0.122671608411932,0.531448436683957));
#50892=DIRECTION('center_axis',(-0.702343264258627,0.70542465295162,-0.0953414818356713));
#50893=DIRECTION('ref_axis',(0.0239307455634354,-0.110462470668693,-0.993592150729134));
#50894=DIRECTION('center_axis',(-0.977583274769392,0.160364694802967,-0.136433520631487));
#50895=DIRECTION('ref_axis',(-0.160215997110056,-0.987007291751593,-0.0121424997103922));
#50896=DIRECTION('center_axis',(-0.978892016790465,-0.137109889424122,-0.151562850613205));
#50897=DIRECTION('ref_axis',(0.132079537552637,-0.990313730678209,0.0428218471120587));
#50898=DIRECTION('center_axis',(0.0194445813316385,-0.879260729000878,0.475943776819996));
#50899=DIRECTION('ref_axis',(0.949747548726854,-0.132503133762174,-0.283588633817605));
#50900=DIRECTION('center_axis',(0.211713487886367,-0.879260728674883,-0.426705952685338));
#50901=DIRECTION('ref_axis',(0.764943920330387,-0.122671608382308,0.632307263319406));
#50902=DIRECTION('center_axis',(-0.684855621636837,0.705424652958876,-0.182616638098152));
#50903=DIRECTION('ref_axis',(0.14827216179308,-0.110462470380521,-0.982758062126503));
#50904=DIRECTION('center_axis',(-0.952775084346285,0.160364694830759,-0.257881374474325));
#50905=DIRECTION('ref_axis',(-0.15743078739333,-0.987007291747074,-0.0321271414667282));
#50906=DIRECTION('center_axis',(-0.952177298702754,-0.137109889415165,-0.273055434041677));
#50907=DIRECTION('ref_axis',(0.125671050374487,-0.990313730679455,0.059038139583782));
#50908=DIRECTION('center_axis',(-0.0403603174395375,-0.879260729014459,
0.474627870219545));
#50909=DIRECTION('ref_axis',(0.977801586111893,-0.132503133669077,-0.162317521435431));
#50910=DIRECTION('center_axis',(0.263524500644688,-0.879260728677615,-0.396806512755622));
#50911=DIRECTION('ref_axis',(0.679662995120437,-0.12267160836076,0.723194226723431));
#50912=DIRECTION('center_axis',(-0.65656739675031,0.705424652959475,-0.267011820939683));
#50913=DIRECTION('ref_axis',(0.270275237180936,-0.110462470438146,-0.956425291798314));
#50914=DIRECTION('center_axis',(-0.912941061687989,0.160364694825961,-0.375262284991956));
#50915=DIRECTION('ref_axis',(-0.152162800082905,-0.98700729174785,-0.0516051190048394));
#50916=DIRECTION('center_axis',(-0.910446175781508,-0.137109889642671,-0.390241770146408));
#50917=DIRECTION('ref_axis',(0.117280655931353,-0.990313730650938,0.0743233652933744));
#50918=DIRECTION('center_axis',(-0.099528710080768,-0.879260729003441,0.465826798608664));
#50919=DIRECTION('ref_axis',(0.990435108372055,-0.132503133721845,-0.038486564641797));
#50920=DIRECTION('center_axis',(0.311179574584837,-0.879260728676818,-0.360649197098664));
#50921=DIRECTION('ref_axis',(0.583663378466932,-0.122671608369214,0.802675985150096));
#50922=DIRECTION('center_axis',(-0.61792471178816,0.705424652955238,-0.347196067898963));
#50923=DIRECTION('ref_axis',(0.388015910533207,-0.110462470648107,-0.915009123315939));
#50924=DIRECTION('center_axis',(-0.858709413119038,0.160364694843852,-0.48672508510287));
#50925=DIRECTION('ref_axis',(-0.144495114537597,-0.987007291744945,-0.0702692529992742));
#50926=DIRECTION('center_axis',(-0.85435677284678,-0.137109889450976,-0.501273760439918));
#50927=DIRECTION('ref_axis',(0.107040674993316,-0.990313730674492,0.0884364672210806));
#50928=DIRECTION('center_axis',(-0.157127475408515,-0.879260729005603,0.449679360100375));
#50929=DIRECTION('ref_axis',(0.98744887731259,-0.132503133730221,0.0859513481323921));
#50930=DIRECTION('center_axis',(0.353927160734071,-0.879260728672657,-0.318804228185179));
#50931=DIRECTION('ref_axis',(0.478459041683958,-0.122671608397634,0.869499063785583));
#50932=DIRECTION('center_axis',(-0.569536984911877,0.705424652934478,-0.421904825582453));
#50933=DIRECTION('ref_axis',(0.499637341450765,-0.110462470774635,-0.859162714262191));
#50934=DIRECTION('center_axis',(-0.790935404138116,0.160364694856304,-0.590511939866181));
#50935=DIRECTION('ref_axis',(-0.134548654712423,-0.98700729174292,-0.0878251988974902));
#50936=DIRECTION('center_axis',(-0.784793653210681,-0.137109889462256,-0.604400364073253));
#50937=DIRECTION('ref_axis',(0.0951125989073771,-0.990313730672959,0.10115487318805));
#50938=DIRECTION('center_axis',(-0.212248246590896,-0.879260729007012,0.426440209461007));
#50939=DIRECTION('ref_axis',(0.96888998759003,-0.132503133720377,0.209033756848198));
#50940=DIRECTION('center_axis',(0.39109310415168,-0.879260728672932,-0.271931526121096));
#50941=DIRECTION('ref_axis',(0.365709119989659,-0.122671608393851,0.922609622782277));
#50942=DIRECTION('center_axis',(-0.512167319731713,0.705424652954773,-0.489959891830414));
#50943=DIRECTION('ref_axis',(0.60337919282722,-0.110462470649097,-0.789766796112162));
#50944=DIRECTION('center_axis',(-0.710687871354221,0.160364694851882,-0.684986068584661));
#50945=DIRECTION('ref_axis',(-0.122480282212692,-0.98700729174364,-0.103996088935997));
#50946=DIRECTION('center_axis',(-0.702853868861137,-0.137109889358614,-0.697995212925562));
#50947=DIRECTION('ref_axis',(0.0816845402343855,-0.990313730687279,0.112278006301063));
#50948=DIRECTION('center_axis',(-0.264021736139023,-0.879260729007782,0.396475841976331));
#50949=DIRECTION('ref_axis',(0.935051123976042,-0.132503133714817,0.328819578350948));
#50950=DIRECTION('center_axis',(0.422091275700155,-0.879260728678951,-0.220770301401197));
#50951=DIRECTION('ref_axis',(0.247191746984302,-0.122671608351982,0.961170076899602));
#50952=DIRECTION('center_axis',(-0.44672046979781,0.7054246529415,-0.550287998130059));
#50953=DIRECTION('ref_axis',(0.697605394040524,-0.110462470732661,-0.707915783667239));
#50954=DIRECTION('center_axis',(-0.619232366294704,0.160364694847693,-0.768657557810673));
#50955=DIRECTION('ref_axis',(-0.108480322497183,-0.987007291744323,-0.118526898527059));
#50956=DIRECTION('center_axis',(-0.609829659120054,-0.13710988941858,-0.780582260291088));
#50957=DIRECTION('ref_axis',(0.0669682676856494,-0.990313730678976,0.121630448292651));
#50958=DIRECTION('center_axis',(-0.311631445195416,-0.879260729007769,0.360258813618964));
#50959=DIRECTION('ref_axis',(0.886465945546352,-0.132503133692648,0.443419718718327));
#50960=DIRECTION('center_axis',(0.446432815664272,-0.879260728674888,-0.16612739722326));
#50961=DIRECTION('ref_axis',(0.124776012454926,-0.122671608403339,0.984572304712857));
#50962=DIRECTION('center_axis',(-0.374228571398007,0.70542465296098,-0.601937733776748));
#50963=DIRECTION('ref_axis',(0.780829941339811,-0.110462470613005,-0.614900516582429));
#50964=DIRECTION('center_axis',(-0.518011196904828,0.160364694872858,-0.840206858172178));
#50965=DIRECTION('ref_axis',(-0.0927695633096054,-0.987007291740231,-0.131188468147773));
#50966=DIRECTION('center_axis',(-0.50718807135462,-0.137109889581385,-0.850859059101189));
#50967=DIRECTION('ref_axis',(0.0511958657084904,-0.990313730659423,0.129064705484394));
#50968=DIRECTION('center_axis',(-0.354326540197732,-0.879260729008234,0.318360288565352));
#50969=DIRECTION('ref_axis',(0.82390066964127,-0.132503133711363,0.551026865153901));
#50970=DIRECTION('center_axis',(0.463733843447336,-0.87926072867611,-0.10886456471009));
#50971=DIRECTION('ref_axis',(0.000392485695471339,-0.122671608394846,0.99244723912599));
#50972=DIRECTION('center_axis',(-0.295834864707477,0.705424652953782,-0.644094551932048));
#50973=DIRECTION('ref_axis',(0.851740334110555,-0.110462470655033,-0.512187900897733));
#50974=DIRECTION('center_axis',(-0.408620681497454,0.160364694865246,-0.898505594469691));
#50975=DIRECTION('ref_axis',(-0.0755957726710143,-0.987007291741473,-0.14178111723158));
#50976=DIRECTION('center_axis',(-0.396547824745071,-0.137109889425071,-0.907717302309369));
#50977=DIRECTION('ref_axis',(0.034616073952146,-0.990313730678103,0.134463535036669));
#50978=DIRECTION('center_axis',(-0.391433693969208,-0.879260729013596,0.271441031607419));
#50979=DIRECTION('ref_axis',(0.748341987973332,-0.132503133651729,0.649943988824109));
#50980=DIRECTION('center_axis',(0.473721511152887,-0.879260729012473,-0.0498848703263812));
#50981=DIRECTION('ref_axis',(-0.123997232081177,-0.122671606019574,0.98467068785091));
#50982=DIRECTION('center_axis',(-0.21277567187849,0.705424653817806,-0.676093611301486));
#50983=DIRECTION('ref_axis',(0.909218271556588,-0.110462465555327,-0.401397780725167));
#50984=DIRECTION('center_axis',(-0.292785973845394,0.160364694840491,-0.94263436080387));
#50985=DIRECTION('ref_axis',(-0.0572297915357268,-0.987007291745495,-0.150137793383277));
#50986=DIRECTION('center_axis',(-0.279653782043359,-0.137109889431314,-0.950260301395875));
#50987=DIRECTION('ref_axis',(0.0174903662277315,-0.990313730677212,0.137741794388638));
#50988=DIRECTION('center_axis',(-0.422367704644081,-0.879260729003134,0.220240987344697));
#50989=DIRECTION('ref_axis',(0.660981506120526,-0.132503133747519,0.738611107494145));
#50990=DIRECTION('center_axis',(0.476238308330351,-0.879260728672218,0.00988153295016984));
#50991=DIRECTION('ref_axis',(-0.246431436826979,-0.122671608401111,0.961365291362069));
#50992=DIRECTION('center_axis',(-0.126360866737994,0.705424652922653,-0.697430276376197));
#50993=DIRECTION('ref_axis',(0.95235729655815,-0.110462470915775,-0.284277368447847));
#50994=DIRECTION('center_axis',(-0.172333856482792,0.160364694839762,-0.971897220162049));
#50995=DIRECTION('ref_axis',(-0.0379612624110037,-0.987007291745612,-0.156126706867071));
#50996=DIRECTION('center_axis',(-0.158349432088054,-0.137109891155577,-0.977817127639262));
#50997=DIRECTION('ref_axis',(8.88252939813159E-5,-0.990313730439543,0.138847785048893));
#50998=DIRECTION('center_axis',(-0.446640724223604,-0.879260729008031,0.165567611232637));
#50999=DIRECTION('ref_axis',(0.563196951084305,-0.13250313371093,0.815629887783746));
#51000=DIRECTION('center_axis',(0.471244542523149,-0.879260728680165,0.0694921012991661));
#51001=DIRECTION('ref_axis',(-0.364979272010298,-0.122671608366607,0.922898590043122));
#51002=DIRECTION('center_axis',(-0.0379532822265761,0.705424652970262,-0.707768046290602));
#51003=DIRECTION('ref_axis',(0.9804770766421,-0.110462470559006,-0.162673737208444));
#51004=DIRECTION('center_axis',(-0.0491639312551466,0.160364694821936,-0.985832679777967));
#51005=DIRECTION('ref_axis',(-0.0180940614984255,-0.987007291748523,-0.159653408901083));
#51006=DIRECTION('center_axis',(-0.0345478170780039,-0.137109891131492,
-0.989953193888002));
#51007=DIRECTION('ref_axis',(-0.0173141169948037,-0.990313730442863,0.137764061529232));
#51008=DIRECTION('center_axis',(-0.463852070615388,-0.879265855918343,0.10831810191284));
#51009=DIRECTION('ref_axis',(0.440180830784498,-0.122636854730908,0.889494821835169));
#51010=DIRECTION('center_axis',(0.458818968799936,-0.879260728677175,0.128006737617385));
#51011=DIRECTION('ref_axis',(-0.477771165967333,-0.122671608387466,0.869877226662388));
#51012=DIRECTION('center_axis',(0.0510528487577276,0.705424652951044,-0.70694389143879));
#51013=DIRECTION('ref_axis',(0.993134147530435,-0.110462470674624,-0.0385046436349503));
#51014=DIRECTION('center_axis',(0.0747813385357381,0.16036469488283,-0.984220969113105));
#51015=DIRECTION('ref_axis',(0.0020584935708628,-0.987007291738614,-0.160662281382488));
#51016=DIRECTION('center_axis',(0.0897986376532112,-0.137109889370473,-0.986477107140578));
#51017=DIRECTION('ref_axis',(-0.0344440051901882,-0.990313730685666,0.134507714730033));
#51018=DIRECTION('center_axis',(-0.473783675110741,-0.879260729008865,0.0492909689634806));
#51019=DIRECTION('ref_axis',(0.342664178424753,-0.132503133685172,0.930066761253244));
#51020=DIRECTION('center_axis',(0.439157545850119,-0.879260728675988,0.184502631230756));
#51021=DIRECTION('ref_axis',(-0.583028323238382,-0.122671608395633,0.803137379777252));
#51022=DIRECTION('center_axis',(0.139253845616515,0.705424652955838,-0.694970809087078));
#51023=DIRECTION('ref_axis',(0.990128899642354,-0.110462470644664,0.0862716910237555));
#51024=DIRECTION('center_axis',(0.197547261947256,0.16036469485379,-0.967087505834706));
#51025=DIRECTION('ref_axis',(0.0221785849666862,-0.987007291743339,-0.159137413622173));
#51026=DIRECTION('center_axis',(0.212728914246855,-0.137109889420509,-0.967443686870947));
#51027=DIRECTION('ref_axis',(-0.0510306907593974,-0.990313730678721,0.129130102725165));
#51028=DIRECTION('center_axis',(-0.47622554584437,-0.87926072900977,-0.0104785450535443));
#51029=DIRECTION('ref_axis',(0.223393894456238,-0.132503133701192,0.965680116539136));
#51030=DIRECTION('center_axis',(0.412570346078638,-0.879260728672076,0.23808880811916));
#51031=DIRECTION('ref_axis',(-0.679090775549037,-0.122671608414792,0.723731576658871));
#51032=DIRECTION('center_axis',(0.225258726238494,0.705424652949409,-0.672037621911614));
#51033=DIRECTION('ref_axis',(0.971508727518402,-0.110462470682718,0.209687469645291));
#51034=DIRECTION('center_axis',(0.317197747027847,0.160364694860719,-0.934702494873469));
#51035=DIRECTION('ref_axis',(0.0419489068324215,-0.987007291742214,-0.155102853820504));
#51036=DIRECTION('center_axis',(0.332304328786436,-0.137109889415776,-0.933153101743862));
#51037=DIRECTION('ref_axis',(-0.0668125918447864,-0.990313730679361,0.121716031807269));
#51038=DIRECTION('center_axis',(-0.471157055239204,-0.879260729009568,-0.0700828061644564));
#51039=DIRECTION('ref_axis',(0.10060055527342,-0.132503133700201,0.986064119537014));
#51040=DIRECTION('center_axis',(0.379476665444939,-0.879260728676914,0.287920182323735));
#51041=DIRECTION('ref_axis',(-0.764443560681583,-0.122671608366485,0.632912094238404));
#51042=DIRECTION('center_axis',(0.307711142173716,0.705424652944235,-0.63850599997232));
#51043=DIRECTION('ref_axis',(0.93756728240383,-0.110462470713733,0.329796351601583));
#51044=DIRECTION('center_axis',(0.431845834156531,0.160364694815792,-0.887576667211508));
#51045=DIRECTION('ref_axis',(0.0610576693579444,-0.987007291749521,-0.148622229312618));
#51046=DIRECTION('center_axis',(0.446639105450297,-0.137109891249355,-0.884146134529891));
#51047=DIRECTION('ref_axis',(-0.0815408191148127,-0.990313730429522,0.112382428078637));
#51048=DIRECTION('center_axis',(-0.458658136415822,-0.879260729004999,-0.128581819590344));
#51049=DIRECTION('ref_axis',(-0.0237793147674236,-0.132503133734286,0.990897302317342));
#51050=DIRECTION('center_axis',(0.340398408902727,-0.879260729007449,0.333210884638814));
#51051=DIRECTION('ref_axis',(-0.83774061513981,-0.122671606054293,0.53211120906558));
#51052=DIRECTION('center_axis',(0.385310763021079,0.705424653838188,-0.59490476015694));
#51053=DIRECTION('ref_axis',(0.888839843993657,-0.110462465576322,0.444704143704701));
#51054=DIRECTION('center_axis',(0.539683454502762,0.160364694851086,-0.826453225283369));
#51055=DIRECTION('ref_axis',(0.0792035159962911,-0.987007291743783,-0.139797743538397));
#51056=DIRECTION('center_axis',(0.553930116811889,-0.137109889420056,-0.821195655073739));
#51057=DIRECTION('ref_axis',(-0.0949830976305822,-0.990313730678775,0.101276482924643));
#51058=DIRECTION('center_axis',(-0.43892590478839,-0.879260729004544,-0.185053020878046));
#51059=DIRECTION('ref_axis',(-0.147784170842995,-0.132503133714334,0.980103442705988));
#51060=DIRECTION('center_axis',(0.2959518705077,-0.879260728681021,0.373246649472321));
#51061=DIRECTION('ref_axis',(-0.897825997836381,-0.122671608360944,0.422918614051506));
#51062=DIRECTION('center_axis',(0.45683381573245,0.70542465296641,-0.541921510728767));
#51063=DIRECTION('ref_axis',(0.826094864780288,-0.110462470581545,0.552598694331301));
#51064=DIRECTION('center_axis',(0.639009944383963,0.160364694842497,-0.752296122299243));
#51065=DIRECTION('ref_axis',(0.0961002758532159,-0.987007291745183,-0.128768563798679));
#51066=DIRECTION('center_axis',(0.652485319230149,-0.137109889417251,-0.745294429345289));
#51067=DIRECTION('ref_axis',(-0.106927436623215,-0.990313730679154,0.088573348844475));
#51068=DIRECTION('center_axis',(-0.412271549460581,-0.879260729013579,-0.238605825410616));
#51069=DIRECTION('ref_axis',(-0.269458382143699,-0.132503133675119,0.953852766342256));
#51070=DIRECTION('center_axis',(0.246837992152326,-0.87926072867621,0.407396093056855));
#51071=DIRECTION('ref_axis',(-0.943752129089521,-0.122671608371701,0.307056339029983));
#51072=DIRECTION('center_axis',(0.521152319951747,0.705424652961949,-0.480391838401139));
#51073=DIRECTION('ref_axis',(0.750321878785262,-0.110462470607681,0.651778429225302));
#51074=DIRECTION('center_axis',(0.728258865710466,0.160364694878353,-0.66627486006203));
#51075=DIRECTION('ref_axis',(0.111481476982423,-0.987007291739349,-0.115708626917674));
#51076=DIRECTION('center_axis',(0.740750438389486,-0.137109889397372,-0.657639465250699));
#51077=DIRECTION('ref_axis',(-0.117185466050305,-0.990313730681934,0.074473360132347));
#51078=DIRECTION('center_axis',(-0.379115425491949,-0.879260729008477,-0.288395673645669));
#51079=DIRECTION('ref_axis',(-0.386883073924451,-0.132503133686919,0.912559262006536));
#51080=DIRECTION('center_axis',(0.19383133116877,-0.879260728676786,0.435120656903474));
#51081=DIRECTION('ref_axis',(-0.974794725529707,-0.12267160838987,0.186351602017545));
#51082=DIRECTION('center_axis',(0.57725194078524,0.705424652952856,-0.41128609977243));
#51083=DIRECTION('ref_axis',(0.66271586851335,-0.110462470663156,0.740679228948394));
#51084=DIRECTION('center_axis',(0.806022709691879,0.160364694850647,-0.569746045274927));
#51085=DIRECTION('ref_axis',(0.125104548578956,-0.987007291743853,-0.100823895824952));
#51086=DIRECTION('center_axis',(0.817333480632928,-0.137109889377541,-0.559613133933918));
#51087=DIRECTION('ref_axis',(-0.125595410672812,-0.990313730684659,0.0591988820448487));
#51088=DIRECTION('center_axis',(-0.339980424780122,-0.879260729003266,-0.333637349826085));
#51089=DIRECTION('ref_axis',(-0.498206388471336,-0.132503133723577,0.856874152976842));
#51090=DIRECTION('center_axis',(0.137767834334762,-0.87926072867318,0.455983108059737));
#51091=DIRECTION('ref_axis',(-0.990464226818836,-0.122671608391281,0.0627079890194332));
#51092=DIRECTION('center_axis',(0.624247953561087,0.705424652964862,-0.335694133794737));
#51093=DIRECTION('ref_axis',(0.564658433212921,-0.110462470590227,0.817899074698481));
#51094=DIRECTION('center_axis',(0.871075094041514,0.160364694862904,-0.464231995000448));
#51095=DIRECTION('ref_axis',(0.136754646741252,-0.987007291741855,-0.0843491116911401));
#51096=DIRECTION('center_axis',(0.881026685614934,-0.137109889525777,-0.452761369187559));
#51097=DIRECTION('ref_axis',(-0.132024640726991,-0.990313730667086,0.0429908024250133));
#51098=DIRECTION('center_axis',(-0.295483729705123,-0.879260729005976,-0.37361736563954));
#51099=DIRECTION('ref_axis',(-0.601672690597617,-0.132503133727805,0.787675626727992));
#51100=DIRECTION('center_axis',(0.0795316564089272,-0.879260728675799,0.469654433213779));
#51101=DIRECTION('ref_axis',(-0.990513515588166,-0.122671608376523,-0.0619245664941464));
#51102=DIRECTION('center_axis',(0.661399203298246,0.70542465295776,-0.254808070664704));
#51103=DIRECTION('ref_axis',(0.457695997011179,-0.110462470632492,0.882220163508922));
#51104=DIRECTION('center_axis',(0.922390103807476,0.160364694846821,-0.351396728847495));
#51105=DIRECTION('ref_axis',(0.146248042406897,-0.987007291744476,-0.066544091663986));
#51106=DIRECTION('center_axis',(0.930825573497249,-0.137109889410855,-0.338769287198916));
#51107=DIRECTION('ref_axis',(-0.13637176322006,-0.990313730680047,0.0261047318089868));
#51108=DIRECTION('center_axis',(-0.246327079694008,-0.87926072900698,-0.407705212421348));
#51109=DIRECTION('ref_axis',(-0.695650255050645,-0.132503133697876,0.706054985258383));
#51110=DIRECTION('center_axis',(0.020041216796702,-0.879260728672416,0.475919027402519));
#51111=DIRECTION('ref_axis',(-0.974941814499448,-0.122671608420682,-0.185580534615046));
#51112=DIRECTION('center_axis',(0.68811979247493,0.705424652954293,-0.169903532066213));
#51113=DIRECTION('ref_axis',(0.343515421538055,-0.110462470652446,0.932628113313603));
#51114=DIRECTION('center_axis',(0.959158470620454,0.160364694873863,-0.233019726364624));
#51115=DIRECTION('ref_axis',(0.153435019119225,-0.987007291740073,-0.0476896315755246));
#51116=DIRECTION('center_axis',(0.965944786002725,-0.137109889560608,-0.219434611168856));
#51117=DIRECTION('ref_axis',(-0.138568221700355,-0.990313730662269,0.00880697431474339));
#51118=DIRECTION('center_axis',(-0.193285704507149,-0.879260729010939,-0.435363304439324));
#51119=DIRECTION('ref_axis',(-0.778656999349661,-0.132503133693184,0.613299434962456));
#51120=DIRECTION('center_axis',(-0.039765284845021,-0.879260728678037,0.47467809421308));
#51121=DIRECTION('ref_axis',(-0.943994698599503,-0.12267160838127,-0.306309786838725));
#51122=DIRECTION('center_axis',(0.703988321442307,0.705424652957028,-0.0823195133203546));
#51123=DIRECTION('ref_axis',(0.223917402698939,-0.110462470636748,0.968327960635954));
#51124=DIRECTION('center_axis',(0.980800335382066,0.160364694875923,-0.110967863599237));
#51125=DIRECTION('ref_axis',(0.1582022338996,-0.987007291739743,-0.0280830774979129));
#51126=DIRECTION('center_axis',(0.985830472224448,-0.137109889565211,-0.0966393202435602));
#51127=DIRECTION('ref_axis',(-0.138579376457204,-0.990313730661652,-0.0086296746018274));
#51128=DIRECTION('center_axis',(-0.137196098265259,-0.879260729009514,-0.45615545710037));
#51129=DIRECTION('ref_axis',(-0.849383857664955,-0.132503133702865,0.510871786162751));
#51130=DIRECTION('center_axis',(-0.0989446641002374,-0.879260728671348,
0.465951203949965));
#51131=DIRECTION('ref_axis',(-0.898160222391755,-0.122671608426907,-0.422208350698027));
#51132=DIRECTION('center_axis',(0.708754534051182,0.705424652951909,0.00656273339169857));
#51133=DIRECTION('ref_axis',(0.10078807260931,-0.110462470668518,0.98875669757201));
#51134=DIRECTION('center_axis',(0.986974392953023,0.160364694877827,0.0128340286641733));
#51135=DIRECTION('ref_axis',(0.160474504945745,-0.987007291739428,-0.00803363651259044));
#51136=DIRECTION('center_axis',(0.990169023015283,-0.137109889405871,0.027680030492564));
#51137=DIRECTION('ref_axis',(-0.136405051496291,-0.99031373068074,-0.0259302285275058));
#51138=DIRECTION('center_axis',(-0.0789428275667312,-0.87926072900407,-0.469753765718808));
#51139=DIRECTION('ref_axis',(-0.906715425169113,-0.132503133717594,0.400387384061252));
#51140=DIRECTION('center_axis',(-0.156563626986478,-0.879260728677805,0.449875984811163));
#51141=DIRECTION('ref_axis',(-0.838161222932035,-0.122671608382732,-0.531448436699056));
#51142=DIRECTION('center_axis',(0.70234326425919,0.705424652958555,0.0953414817802181));
#51143=DIRECTION('ref_axis',(-0.0239307455239352,-0.110462470629527,0.99359215073444));
#51144=DIRECTION('center_axis',(0.977583274764738,0.160364694832406,0.136433520630231));
#51145=DIRECTION('ref_axis',(0.160215997139136,-0.987007291746816,0.0121424997149576));
#51146=DIRECTION('center_axis',(0.978892016791562,-0.137109889415534,0.151562850613888));
#51147=DIRECTION('ref_axis',(-0.132079537544142,-0.9903137306794,-0.0428218471107381));
#51148=DIRECTION('center_axis',(-0.0194445814035528,-0.87926072901053,-0.475943776799227));
#51149=DIRECTION('ref_axis',(-0.949747548733399,-0.132503133684082,0.283588633832173));
#51150=DIRECTION('center_axis',(-0.211713487892645,-0.879260728675838,0.426705952680256));
#51151=DIRECTION('ref_axis',(-0.764943920330541,-0.122671608373738,-0.632307263320882));
#51152=DIRECTION('center_axis',(0.68485562163539,0.705424652957529,0.182616638108781));
#51153=DIRECTION('ref_axis',(-0.148272161548486,-0.110462470635442,0.982758062134752));
#51154=DIRECTION('center_axis',(0.952775084340861,0.160364694866168,0.257881374472347));
#51155=DIRECTION('ref_axis',(0.157430787427507,-0.987007291741322,0.0321271414759624));
#51156=DIRECTION('center_axis',(0.952177298703104,-0.137109889411569,0.27305543404226));
#51157=DIRECTION('ref_axis',(-0.125671050370933,-0.990313730679946,-0.0590381395830944));
#51158=DIRECTION('center_axis',(0.0403603174543297,-0.879260729012547,-0.47462787022183));
#51159=DIRECTION('ref_axis',(-0.977801586111239,-0.132503133682443,0.162317521428458));
#51160=DIRECTION('center_axis',(-0.263524500637211,-0.879260728676324,0.396806512763449));
#51161=DIRECTION('ref_axis',(-0.679662995110619,-0.122671608378878,-0.723194226729585));
#51162=DIRECTION('center_axis',(0.656567396744409,0.705424652956745,0.267011820961406));
#51163=DIRECTION('ref_axis',(-0.270275237259081,-0.110462470391246,0.956425291781648));
#51164=DIRECTION('center_axis',(0.912941061682396,0.160364694864044,0.375262284989289));
#51165=DIRECTION('ref_axis',(0.152162800118094,-0.987007291741665,0.0516051190193879));
#51166=DIRECTION('center_axis',(0.910446175811195,-0.137109889406173,0.390241770160241));
#51167=DIRECTION('ref_axis',(-0.117280655660036,-0.990313730680689,-0.0743233653251029));
#51168=DIRECTION('center_axis',(0.0995287100521309,-0.879260729007236,-0.465826798607619));
#51169=DIRECTION('ref_axis',(-0.990435108370254,-0.132503133718826,0.0384865646985363));
#51170=DIRECTION('center_axis',(-0.311179574561562,-0.87926072867168,0.360649197131272));
#51171=DIRECTION('ref_axis',(-0.583663378483035,-0.122671608402557,-0.802675985133291));
#51172=DIRECTION('center_axis',(0.617924711791022,0.705424652956328,0.347196067891656));
#51173=DIRECTION('ref_axis',(-0.38801591053027,-0.110462470640521,0.9150091233181));
#51174=DIRECTION('center_axis',(0.858709413117082,0.160364694858558,0.486725085101475));
#51175=DIRECTION('ref_axis',(0.144495114550315,-0.987007291742558,0.0702692530066537));
#51176=DIRECTION('center_axis',(0.854356772853503,-0.137109889390124,0.501273760445104));
#51177=DIRECTION('ref_axis',(-0.107040674940543,-0.990313730682904,-0.0884364671907566));
#51178=DIRECTION('center_axis',(0.157127475379704,-0.87926072900933,-0.449679360103155));
#51179=DIRECTION('ref_axis',(-0.987448877316381,-0.13250313368182,-0.0859513481634601));
#51180=DIRECTION('center_axis',(-0.353927160753815,-0.87926072867792,0.318804228148744));
#51181=DIRECTION('ref_axis',(-0.478459041636315,-0.122671608379725,-0.869499063814327));
#51182=DIRECTION('center_axis',(0.569536985000032,0.705424652955541,0.421904825428232));
#51183=DIRECTION('ref_axis',(-0.499637341350622,-0.110462470646596,0.85916271433689));
#51184=DIRECTION('center_axis',(0.790935404140268,0.160364694840428,0.59051193986761));
#51185=DIRECTION('ref_axis',(0.134548654699449,-0.987007291745503,0.0878251988883308));
#51186=DIRECTION('center_axis',(0.784793653213853,-0.13710988942998,0.604400364076457));
#51187=DIRECTION('ref_axis',(-0.095112598881028,-0.9903137306774,-0.101154873169351));
#51188=DIRECTION('center_axis',(0.212248246609885,-0.879260729004504,-0.426440209456727));
#51189=DIRECTION('ref_axis',(-0.968889987585865,-0.132503133737634,-0.209033756856564));
#51190=DIRECTION('center_axis',(-0.391093104159856,-0.879260728675769,0.271931526100164));
#51191=DIRECTION('ref_axis',(-0.365709119951303,-0.122671608390012,-0.922609622797991));
#51192=DIRECTION('center_axis',(0.512167319772571,0.705424652962821,0.489959891776117));
#51193=DIRECTION('ref_axis',(-0.603379192791661,-0.110462470601419,0.789766796145998));
#51194=DIRECTION('center_axis',(0.710687871353904,0.160364694855864,0.684986068584057));
#51195=DIRECTION('ref_axis',(0.122480282215561,-0.987007291742994,0.103996088938754));
#51196=DIRECTION('center_axis',(0.70285386885858,-0.137109889388095,0.697995212922345));
#51197=DIRECTION('ref_axis',(-0.0816845402554354,-0.990313730683201,-0.11227800632171));
#51198=DIRECTION('center_axis',(0.264021736112348,-0.879260729011344,-0.396475841986194));
#51199=DIRECTION('ref_axis',(-0.93505112398369,-0.132503133689779,-0.328819578339287));
#51200=DIRECTION('center_axis',(-0.422091275691081,-0.879260728674362,0.220770301436824));
#51201=DIRECTION('ref_axis',(-0.247191747000703,-0.122671608384156,-0.961170076891278));
#51202=DIRECTION('center_axis',(0.446720469914802,0.705424652961171,0.55028799800987));
#51203=DIRECTION('ref_axis',(-0.697605393966077,-0.110462470612296,0.707915783759383));
#51204=DIRECTION('center_axis',(0.619232366294981,0.160364694844356,0.768657557811146));
#51205=DIRECTION('ref_axis',(0.108480322495231,-0.987007291744863,0.118526898524347));
#51206=DIRECTION('center_axis',(0.609829659124712,-0.137109889358621,0.780582260297981));
#51207=DIRECTION('ref_axis',(-0.0669682676488701,-0.990313730687279,-0.1216304482453));
#51208=DIRECTION('center_axis',(0.31163144517232,-0.879260729011096,-0.360258813630823));
#51209=DIRECTION('ref_axis',(-0.88646594556642,-0.132503133685564,-0.443419718680325));
#51210=DIRECTION('center_axis',(-0.446432815665649,-0.879260728676026,0.166127397213536));
#51211=DIRECTION('ref_axis',(-0.124776012493544,-0.122671608372295,-0.98457230471183));
#51212=DIRECTION('center_axis',(0.374228571297439,0.705424652945905,0.601937733856939));
#51213=DIRECTION('ref_axis',(-0.780829941387608,-0.110462470705292,0.614900516505156));
#51214=DIRECTION('center_axis',(0.518011196907874,0.160364694830562,0.840206858178373));
#51215=DIRECTION('ref_axis',(0.0927695632868828,-0.987007291747108,0.131188468112105));
#51216=DIRECTION('center_axis',(0.507188071362947,-0.137109889457119,0.85085905911625));
#51217=DIRECTION('ref_axis',(-0.0511958655288825,-0.990313730673669,-0.129064705446333));
#51218=DIRECTION('center_axis',(0.354326540219259,-0.879260729004894,-0.318360288550618));
#51219=DIRECTION('ref_axis',(-0.823900669610395,-0.132503133712186,-0.551026865199868));
#51220=DIRECTION('center_axis',(-0.463733843447264,-0.879260728676205,0.10886456470963));
#51221=DIRECTION('ref_axis',(-0.000392485740395515,-0.122671608370983,-0.992447239128922));
#51222=DIRECTION('center_axis',(0.295834864657644,0.705424652947218,0.644094551962125));
#51223=DIRECTION('ref_axis',(-0.851740334128267,-0.110462470695732,0.512187900859501));
#51224=DIRECTION('center_axis',(0.408620681499501,0.160364694829131,0.898505594475206));
#51225=DIRECTION('ref_axis',(0.0755957726563047,-0.987007291747337,0.141781117198601));
#51226=DIRECTION('center_axis',(0.396547824746198,-0.137109889419203,0.907717302309762));
#51227=DIRECTION('ref_axis',(-0.0346160739492184,-0.990313730678898,-0.134463535031565));
#51228=DIRECTION('center_axis',(0.391433693991048,-0.879260729009837,-0.271441031588101));
#51229=DIRECTION('ref_axis',(-0.748341987988513,-0.132503133700379,-0.649943988796711));
#51230=DIRECTION('center_axis',(-0.473721511495587,-0.879260728677342,0.0498848729789476));
#51231=DIRECTION('ref_axis',(0.123997230797718,-0.122671608386178,-0.984670687717699));
#51232=DIRECTION('center_axis',(0.212775665524956,0.705424652954647,0.676093614201634));
#51233=DIRECTION('ref_axis',(-0.909218272985087,-0.110462470653129,0.401397776086544));
#51234=DIRECTION('center_axis',(0.292785973844741,0.160364694852788,0.942634360801981));
#51235=DIRECTION('ref_axis',(0.0572297915402712,-0.987007291743488,0.150137793394741));
#51236=DIRECTION('center_axis',(0.279653782042791,-0.137109889440163,0.950260301394765));
#51237=DIRECTION('ref_axis',(-0.0174903662316186,-0.99031373067602,-0.137741794396716));
#51238=DIRECTION('center_axis',(0.422367704615302,-0.879260729008736,-0.220240987377524));
#51239=DIRECTION('ref_axis',(-0.660981506108124,-0.132503133685961,-0.738611107516287));
#51240=DIRECTION('center_axis',(-0.476238308321661,-0.879260728676558,-0.00988153298285341));
#51241=DIRECTION('ref_axis',(0.246431436838738,-0.122671608368691,-0.961365291363191));
#51242=DIRECTION('center_axis',(0.126360866964444,0.705424652951288,0.697430276306204));
#51243=DIRECTION('ref_axis',(-0.952357296558165,-0.110462470671254,0.284277368542813));
#51244=DIRECTION('center_axis',(0.172333856482175,0.160364694835558,0.971897220162852));
#51245=DIRECTION('ref_axis',(0.0379612624105628,-0.98700729174629,0.156126706862887));
#51246=DIRECTION('center_axis',(0.158349432142159,-0.137109889429416,0.977817127872543));
#51247=DIRECTION('ref_axis',(-8.88249781092152E-5,-0.990313730677477,-0.138847783352057));
#51248=DIRECTION('center_axis',(0.446640724211219,-0.879260729010886,-0.165567611250882));
#51249=DIRECTION('ref_axis',(-0.563196951097272,-0.132503133693378,-0.815629887777644));
#51250=DIRECTION('center_axis',(-0.471244542531502,-0.879260728677323,-0.0694921012784819));
#51251=DIRECTION('ref_axis',(0.364979272000188,-0.122671608386658,-0.922898590044455));
#51252=DIRECTION('center_axis',(0.0379532820704627,0.705424652950965,0.707768046318206));
#51253=DIRECTION('ref_axis',(-0.980477076648027,-0.110462470672139,0.162673737095898));
#51254=DIRECTION('center_axis',(0.0491639312547749,0.160364694836564,0.985832679775606));
#51255=DIRECTION('ref_axis',(0.0180940615012009,-0.987007291746126,0.15965340891559));
#51256=DIRECTION('center_axis',(0.0345478171019963,-0.137109889427261,0.989953194123203));
#51257=DIRECTION('ref_axis',(0.017314117093875,-0.990313730677783,-0.137764059828063));
#51258=DIRECTION('center_axis',(-0.75633600629039,0.584827951390054,-0.293141796510861));
#51259=DIRECTION('ref_axis',(-0.343345849080795,0.0265489689972696,0.938833734036102));
#51260=DIRECTION('center_axis',(0.963047106314052,-1.31484110737795E-11,
0.269333011382066));
#51261=DIRECTION('ref_axis',(0.269299613072503,-0.0157477670567345,-0.96292768484021));
#51262=DIRECTION('center_axis',(-0.947192631974055,-0.000115441176542844,
-0.32066509727034));
#51263=DIRECTION('ref_axis',(0.00786439770681546,0.999690782633873,-0.0235900480199696));
#51264=DIRECTION('',(0.944235193661784,-6.06181771180169E-10,0.329271770807176));
#51265=DIRECTION('center_axis',(0.755847214530432,-0.601098527978643,0.259568002551347));
#51266=DIRECTION('ref_axis',(-0.304733775776946,0.0279220144013082,0.95202819654278));
#51267=DIRECTION('',(0.434844806368806,2.24206636476412E-10,0.900505410519046));
#51268=DIRECTION('center_axis',(-0.787112483927548,0.584827952222553,-0.19603623120378));
#51269=DIRECTION('ref_axis',(-0.243954870275565,-0.00326197145111748,0.969781099429703));
#51270=DIRECTION('center_axis',(0.978058326780646,-5.2326700288553E-10,
0.208331249252345));
#51271=DIRECTION('ref_axis',(0.208305626739765,-0.0156832196319802,-0.977938036120146));
#51272=DIRECTION('',(-0.978058312613197,8.32144303432302E-8,-0.208331315764625));
#51273=DIRECTION('center_axis',(-0.777850283233954,0.584827969931555,-0.230054737961631));
#51274=DIRECTION('ref_axis',(-0.278731662566012,0.0070448013555362,0.960343184000932));
#51275=DIRECTION('center_axis',(-0.96304708547139,5.92586886094829E-10,
-0.269333085908621));
#51276=DIRECTION('ref_axis',(0.269300010215738,0.0156715280545403,-0.96292881756973));
#51277=DIRECTION('',(0.963047106749921,-1.36557432027528E-11,0.26933300982354));
#51278=DIRECTION('center_axis',(-0.978058312798117,-2.50584992505245E-13,
-0.208331314896489));
#51279=DIRECTION('ref_axis',(0.00340963653580824,0.999866061277598,-0.0160073072037918));
#51280=DIRECTION('',(0.978058312887135,-6.06514838087569E-10,0.208331314478577));
#51281=DIRECTION('center_axis',(-0.787112480221453,0.584827951389699,-0.196036248568883));
#51282=DIRECTION('ref_axis',(-0.222971396850376,0.0265489690037058,0.974463395121352));
#51283=DIRECTION('center_axis',(0.989209569349546,-1.2561123777913E-11,
0.146507432942106));
#51284=DIRECTION('ref_axis',(0.146489265467591,-0.0157477670536161,-0.989086903631623));
#51285=DIRECTION('center_axis',(0.782419632888726,-0.601098528018349,0.162788444566697));
#51286=DIRECTION('ref_axis',(-0.205370608821025,-0.00227572672788967,0.978681630613522));
#51287=DIRECTION('',(0.490529942139282,5.19500677922187E-12,0.871424337429723));
#51288=DIRECTION('',(0.544279180131203,2.24062901110918E-10,0.838904150708355));
#51289=DIRECTION('center_axis',(0.78241963073013,-0.601098528002463,0.162788455000345));
#51290=DIRECTION('ref_axis',(-0.183010085949976,0.0279220138800812,0.982714439489653));
#51291=DIRECTION('center_axis',(0.,-1.,1.45983193964168E-32));
#51292=DIRECTION('ref_axis',(1.,0.,0.));
#51293=DIRECTION('center_axis',(-0.756949290928045,0.60109853604161,-0.256336343369729));
#51294=DIRECTION('ref_axis',(-0.302155559728147,0.0258666713804852,0.952907620410848));
#51295=DIRECTION('center_axis',(-0.780842226674104,-0.601098522914074,-0.170193956394304));
#51296=DIRECTION('ref_axis',(-0.232606079276408,0.0268944878410888,0.972199104302932));
#51297=DIRECTION('center_axis',(0.78010795135025,0.601098531832816,0.173528496992713));
#51298=DIRECTION('ref_axis',(-0.236757469743944,0.0268942924313918,0.971196477318086));
#51299=DIRECTION('',(-0.838904141906341,-3.07807852447804E-8,0.544279193697853));
#51300=DIRECTION('center_axis',(-0.115217253588766,0.793626260376509,0.59739630340023));
#51301=DIRECTION('ref_axis',(-2.69955750324411E-17,-0.601401446663863,0.798946994456211));
#51302=DIRECTION('center_axis',(-0.503978321595855,0.471546674544287,-0.723636362469196));
#51303=DIRECTION('ref_axis',(0.614174030924001,-0.393423319529449,-0.684111358909494));
#51304=DIRECTION('center_axis',(0.,-1.,1.45983193964168E-32));
#51305=DIRECTION('ref_axis',(1.,0.,0.));
#51306=DIRECTION('center_axis',(-0.783107990018738,0.601098526871089,-0.159444149978034));
#51307=DIRECTION('ref_axis',(-0.202698002714123,-0.00432816599900778,0.979231732877765));
#51308=DIRECTION('center_axis',(-0.780842215871236,-0.601098528389853,-0.170193986617777));
#51309=DIRECTION('ref_axis',(-0.210533861636455,-0.00330175297127346,0.977580989755713));
#51310=DIRECTION('center_axis',(0.78010795247552,0.601098527550831,0.173528506766684));
#51311=DIRECTION('ref_axis',(-0.214708427362672,-0.003301934692242,0.976672610677056));
#51312=DIRECTION('center_axis',(0.,-1.,1.45983193964168E-32));
#51313=DIRECTION('ref_axis',(1.,0.,0.));
#51314=DIRECTION('center_axis',(0.795705453891954,0.601098532045573,0.0743867287844844));
#51315=DIRECTION('ref_axis',(-0.113167377776585,0.0268942876583815,0.993211881674056));
#51316=DIRECTION('center_axis',(-0.783107979656637,0.601098535644099,-0.159444167797447));
#51317=DIRECTION('ref_axis',(-0.180341991740008,0.0258666807695524,0.983263790059012));
#51318=DIRECTION('center_axis',(-0.796016009810675,-0.601098523313665,-0.0709864592385278));
#51319=DIRECTION('ref_axis',(-0.10892306480896,0.0268944792246232,0.993686295034735));
#51320=DIRECTION('center_axis',(-0.805474420453926,0.584828255987311,-0.0958481559199371));
#51321=DIRECTION('ref_axis',(-0.141747987849753,-0.0330815410845231,0.989349846909585));
#51322=DIRECTION('center_axis',(0.989214559142771,-1.08101365926502E-7,
0.146473738192076));
#51323=DIRECTION('ref_axis',(0.146455740324152,-0.0156751635321152,-0.989093021598245));
#51324=DIRECTION('',(-0.989209569691844,-4.44089209849706E-13,-0.146507430630931));
#51325=DIRECTION('center_axis',(-0.80054981432474,0.584827952226173,-0.13075267140508));
#51326=DIRECTION('ref_axis',(-0.1773246910663,-0.0227607295940804,0.983889172176718));
#51327=DIRECTION('center_axis',(-0.978058297134577,5.77132968639425E-10,
-0.208331388432495));
#51328=DIRECTION('ref_axis',(0.208305732673441,0.0156933905082622,-0.97793785039221));
#51329=DIRECTION('',(0.978058312885186,-2.20379270384577E-11,0.208331314487726));
#51330=DIRECTION('center_axis',(-0.80055020562547,0.584827969931532,-0.130750196400547));
#51331=DIRECTION('ref_axis',(-0.156170863562451,0.00704480134783312,0.987704931722085));
#51332=DIRECTION('center_axis',(-0.989209560482432,4.66318822968212E-10,
-0.146507492812327));
#51333=DIRECTION('ref_axis',(0.146489500829708,0.0156715280542981,-0.989088079674963));
#51334=DIRECTION('',(0.989209569691789,-1.4432899319988E-11,0.146507430631303));
#51335=DIRECTION('center_axis',(-0.80547572164662,0.584827952222745,-0.0958390741650192));
#51336=DIRECTION('ref_axis',(-0.120485412206387,-0.00326197145934098,0.992709738537734));
#51337=DIRECTION('center_axis',(0.996456866177649,1.93578415386087E-10,
0.0841053734752966));
#51338=DIRECTION('ref_axis',(0.084095029421336,-0.0156832196296146,-0.996334312692619));
#51339=DIRECTION('',(-0.996456868143889,8.32140417651974E-8,-0.0841053501797939));
#51340=DIRECTION('',(-0.803073192437107,-1.43735365430951E-13,0.595880397050342));
#51341=DIRECTION('',(-0.764072860871016,-3.07812369845586E-8,0.645129958442778));
#51342=DIRECTION('center_axis',(0.796652822001855,-0.601098527974287,0.0634416335195257));
#51343=DIRECTION('ref_axis',(-0.103672281525895,-0.0324816871225219,0.994080981633232));
#51344=DIRECTION('',(0.544279180225795,8.00811321699502E-12,0.838904150646984));
#51345=DIRECTION('',(0.595880397048087,5.05127141378972E-12,0.80307319243878));
#51346=DIRECTION('center_axis',(0.796652822107589,-0.601098528033706,0.0634416316288104));
#51347=DIRECTION('ref_axis',(-0.0810898709684607,-0.00227572362146215,0.996704195791468));
#51348=DIRECTION('center_axis',(0.,-1.,1.45983193964168E-32));
#51349=DIRECTION('ref_axis',(1.,0.,0.));
#51350=DIRECTION('center_axis',(-0.796916614506406,0.601098515216612,-0.0600373594358867));
#51351=DIRECTION('ref_axis',(-0.100958817490252,-0.0345386959223724,0.994290900921331));
#51352=DIRECTION('center_axis',(-0.780842210528445,-0.601098532642785,-0.170193996109563));
#51353=DIRECTION('ref_axis',(-0.188148565998907,-0.033509922223831,0.981568745542108));
#51354=DIRECTION('center_axis',(0.780107924867447,0.601098517625842,0.173528665260302));
#51355=DIRECTION('ref_axis',(-0.19234048933514,-0.0335101945242414,0.980755934483838));
#51356=DIRECTION('center_axis',(0.,-1.,1.45983193964168E-32));
#51357=DIRECTION('ref_axis',(1.,0.,0.));
#51358=DIRECTION('center_axis',(0.795705456777408,0.601098527536453,0.0743867343560998));
#51359=DIRECTION('ref_axis',(-0.0906058539709184,-0.00330193705786042,0.995881356607235));
#51360=DIRECTION('center_axis',(-0.796916600686538,0.6010985268631,-0.0600374262708134));
#51361=DIRECTION('ref_axis',(-0.0783693870587833,-0.00432816741275879,0.996914994439785));
#51362=DIRECTION('center_axis',(-0.796016004324672,-0.601098528386779,-0.0709864777984713));
#51363=DIRECTION('ref_axis',(-0.0863503538729397,-0.00330175382353104,0.996259361214592));
#51364=DIRECTION('',(-0.996456868253698,-7.77156117236895E-13,-0.0841053488788494));
#51365=DIRECTION('center_axis',(-0.810624895144558,0.584827952146236,-0.0293861491236025));
#51366=DIRECTION('ref_axis',(-0.0740902026680098,-0.052656272846004,0.995860411301996));
#51367=DIRECTION('center_axis',(-0.989209555778179,7.0544820002307E-10,
-0.146507524575151));
#51368=DIRECTION('ref_axis',(0.146489298830423,0.01577299981401,-0.989086496624556));
#51369=DIRECTION('',(0.989209569692257,-1.77302617009905E-10,0.146507430628141));
#51370=DIRECTION('center_axis',(-0.810624895029856,0.58482795222639,-0.0293861506925126));
#51371=DIRECTION('ref_axis',(-0.0526124215066951,-0.0227607295861682,0.998355589102354));
#51372=DIRECTION('center_axis',(-0.996456861480342,6.15511979164734E-10,
-0.0841054291276525));
#51373=DIRECTION('ref_axis',(0.0840950716516077,0.0156933905097029,-0.99633414897725));
#51374=DIRECTION('',(0.996456868253725,-2.32591723655397E-11,0.0841053488785229));
#51375=DIRECTION('center_axis',(-0.81113612605453,0.584827952238869,0.00586952207091835));
#51376=DIRECTION('ref_axis',(-0.0166244013107426,-0.0330869090662063,0.999314207709219));
#51377=DIRECTION('center_axis',(0.999771608389312,-5.84500981991017E-10,
0.0213712671278065));
#51378=DIRECTION('ref_axis',(0.0213686413800553,-0.0156751701950672,-0.999648773422409));
#51379=DIRECTION('',(-0.999771606794424,-3.88578058618759E-13,-0.021371341738294));
#51380=DIRECTION('',(-0.764072871228432,0.,0.645129946175761));
#51381=DIRECTION('',(-0.72205710346861,0.,0.691833462135593));
#51382=DIRECTION('',(0.59588039702185,6.70833484120459E-11,0.803073192458248));
#51383=DIRECTION('',(0.645129946172589,8.00811321699427E-12,0.76407287123111));
#51384=DIRECTION('center_axis',(0.798322321538695,-0.601098527845071,-0.0369057008544292));
#51385=DIRECTION('ref_axis',(0.0217365923777059,-0.0324816894873403,0.99923593830479));
#51386=DIRECTION('center_axis',(0.,-1.,1.45983193964168E-32));
#51387=DIRECTION('ref_axis',(1.,0.,0.));
#51388=DIRECTION('center_axis',(-0.784612619000654,0.60109854236896,-0.151866982806818));
#51389=DIRECTION('ref_axis',(-0.151616329939511,0.0514848335721866,0.987097665080673));
#51390=DIRECTION('center_axis',(0.798967517066683,0.601098534860787,-0.0182059896878827));
#51391=DIRECTION('ref_axis',(-0.0167582471047594,0.0525165168369252,0.998479432243495));
#51392=DIRECTION('center_axis',(0.,-1.,1.45983193964168E-32));
#51393=DIRECTION('ref_axis',(1.,0.,0.));
#51394=DIRECTION('center_axis',(0.795705459175127,0.601098522337475,0.074386750719496));
#51395=DIRECTION('ref_axis',(-0.0679024024563864,-0.0335101098683029,0.997129046952933));
#51396=DIRECTION('center_axis',(-0.798157366407851,0.601098516594213,0.0403161480937846));
#51397=DIRECTION('ref_axis',(0.0244549337192487,-0.0345386712358531,0.99910411689976));
#51398=DIRECTION('center_axis',(-0.79601600041738,-0.601098532679962,-0.0709864852596231));
#51399=DIRECTION('ref_axis',(-0.0636417725517395,-0.0335099214952075,0.997410051056163));
#51400=DIRECTION('center_axis',(-0.806364311797864,0.584827908068084,-0.0880506365875126));
#51401=DIRECTION('ref_axis',(-0.0927703937601591,0.0219600677301591,0.995445332234208));
#51402=DIRECTION('center_axis',(0.999771754696857,-1.94678874097512E-8,
0.0213644216014981));
#51403=DIRECTION('ref_axis',(0.0213617749287953,-0.0157391387090833,-0.999647915060392));
#51404=DIRECTION('',(-0.999771606794415,-3.88578058618275E-13,-0.0213713417387115));
#51405=DIRECTION('center_axis',(-0.801776305997045,0.584827952320353,-0.123008216500021));
#51406=DIRECTION('ref_axis',(-0.128518655158662,0.032283433062828,0.991181484505177));
#51407=DIRECTION('center_axis',(-0.99645686226659,5.28005960808625E-10,
-0.0841054198124182));
#51408=DIRECTION('ref_axis',(0.0840950508622084,0.0157020800817931,-0.996334013823471));
#51409=DIRECTION('',(0.996456868253682,-7.77156117237624E-13,0.0841053488790393));
#51410=DIRECTION('center_axis',(-0.807915936815818,0.584827952145957,0.0724438087608944));
#51411=DIRECTION('ref_axis',(0.0513084262408636,-0.0526562728494161,0.997293719185223));
#51412=DIRECTION('center_axis',(-0.999771605207897,5.41160526128575E-10,
-0.0213714159574124));
#51413=DIRECTION('ref_axis',(0.0213687573297561,0.0157729998140531,-0.999647232120936));
#51414=DIRECTION('',(0.999771606794473,-1.77302617010133E-10,0.021371341736028));
#51415=DIRECTION('',(-0.999140703555321,7.77156117237103E-13,0.0414470083236203));
#51416=DIRECTION('',(-0.72205710346864,0.,0.691833462135562));
#51417=DIRECTION('',(-0.677191706198013,0.,0.735806627488924));
#51418=DIRECTION('center_axis',(0.797228847766677,-0.60109852812305,0.0557379922218206));
#51419=DIRECTION('ref_axis',(-0.0522531812709769,0.0232723689287435,0.998362660505443));
#51420=DIRECTION('',(0.64512994617573,0.,0.764072871228458));
#51421=DIRECTION('',(0.691833462110807,6.51326541667403E-11,0.722057103492359));
#51422=DIRECTION('center_axis',(0.,-1.,1.45983193964168E-32));
#51423=DIRECTION('ref_axis',(1.,0.,0.));
#51424=DIRECTION('center_axis',(-0.797459701698008,0.601098534578107,-0.052331404488862));
#51425=DIRECTION('ref_axis',(-0.0495338937900471,0.0212179603895841,0.998547040215383));
#51426=DIRECTION('center_axis',(-0.798882449897006,-0.601098524060562,0.0216193343739451));
#51427=DIRECTION('ref_axis',(0.0103159222699735,0.0222453126288138,0.999699318702262));
#51428=DIRECTION('center_axis',(0.798967520085859,0.601098531169166,-0.0182059790762032));
#51429=DIRECTION('ref_axis',(0.00604483790312725,0.0222451252052261,0.999734271863943));
#51430=DIRECTION('center_axis',(0.,-1.,1.45983193964168E-32));
#51431=DIRECTION('ref_axis',(1.,0.,0.));
#51432=DIRECTION('center_axis',(0.790385605091053,0.60109853538485,-0.118199602465651));
#51433=DIRECTION('ref_axis',(0.108516544623323,0.0525165107899705,0.992706490175954));
#51434=DIRECTION('center_axis',(-0.797459694190177,0.601098542402019,-0.0523314290295791));
#51435=DIRECTION('ref_axis',(-0.0267046471782287,0.0514848332083756,0.998316670084494));
#51436=DIRECTION('center_axis',(-0.811041494763648,0.584827953016302,0.0137098191932171));
#51437=DIRECTION('ref_axis',(0.0112444354981666,-0.00784645566785257,0.999905993483277));
#51438=DIRECTION('center_axis',(0.999140686056023,-1.52846821713024E-9,
-0.0414474301676266));
#51439=DIRECTION('ref_axis',(-0.0414423360944754,-0.0156778483090111,-0.999017886652402));
#51440=DIRECTION('',(-0.999140703563491,1.2575884663851E-8,0.0414470081266709));
#51441=DIRECTION('center_axis',(-0.810871087291932,0.584827953187666,-0.0215486650242196));
#51442=DIRECTION('ref_axis',(-0.0247910851729539,0.00246158313914707,0.999689623185315));
#51443=DIRECTION('center_axis',(-0.999771605317616,5.21632347592839E-10,
-0.0213714108246876));
#51444=DIRECTION('ref_axis',(0.0213687865604974,0.0156707406169895,-0.999648839767969));
#51445=DIRECTION('',(0.999771606794421,-6.46149800302255E-11,0.0213713417384283));
#51446=DIRECTION('center_axis',(-0.810871077874132,0.584827952320916,-0.0215490429339312));
#51447=DIRECTION('ref_axis',(-0.00327726666415344,0.0322834330552977,0.999473381072941));
#51448=DIRECTION('center_axis',(-0.999140706103433,4.51516519363189E-10,
0.0414469468976114));
#51449=DIRECTION('ref_axis',(-0.0414418370929418,0.0157020800815274,-0.999017526782927));
#51450=DIRECTION('',(0.999140703555301,-7.77156117237896E-13,-0.0414470083241067));
#51451=DIRECTION('center_axis',(-0.811041537039199,0.58482792304389,0.0137085967649634));
#51452=DIRECTION('ref_axis',(0.0327240637255072,0.0219596690916775,0.999223152547354));
#51453=DIRECTION('center_axis',(0.994566169398982,-1.3078163819384E-8,-0.104106362375384));
#51454=DIRECTION('ref_axis',(-0.104093467141315,-0.0157391391449197,-0.994442974532716));
#51455=DIRECTION('',(-0.994566648423267,7.77156117236963E-13,0.10410178597944));
#51456=DIRECTION('',(-0.677191704413373,-4.65201564659664E-9,0.735806629131398));
#51457=DIRECTION('',(-0.629653742642429,-1.43735365430928E-13,0.776875900241719));
#51458=DIRECTION('center_axis',(0.797928283300872,-0.601098528053661,-0.04462078305281));
#51459=DIRECTION('ref_axis',(0.0506350763003886,-0.0069195234725463,0.99869325082478));
#51460=DIRECTION('',(0.691833462126601,2.34493981894284E-11,0.722057103477226));
#51461=DIRECTION('',(0.735806627488914,0.,0.677191706198024));
#51462=DIRECTION('center_axis',(0.797928295444368,-0.601098524297468,-0.0446206164978998));
#51463=DIRECTION('ref_axis',(0.0732867338760961,0.023272472024472,0.997039340589751));
#51464=DIRECTION('center_axis',(0.,-1.,1.45983193964168E-32));
#51465=DIRECTION('ref_axis',(1.,0.,0.));
#51466=DIRECTION('center_axis',(-0.797730380563259,0.601098527999986,0.048029153257653));
#51467=DIRECTION('ref_axis',(0.053358553918965,-0.0089720006035093,0.998535111014554));
#51468=DIRECTION('center_axis',(-0.798882451489998,-0.601098528053305,0.0216191644954361));
#51469=DIRECTION('ref_axis',(0.0330247131478521,-0.00794574335897238,0.99942295024878));
#51470=DIRECTION('center_axis',(0.798967518742967,0.601098528198664,-0.0182061360839188));
#51471=DIRECTION('ref_axis',(0.0287548632853352,-0.00794573399547077,0.999554912522926));
#51472=DIRECTION('center_axis',(0.,-1.,1.45983193964168E-32));
#51473=DIRECTION('ref_axis',(1.,0.,0.));
#51474=DIRECTION('center_axis',(0.79038559015766,0.601098528086115,-0.118199739440638));
#51475=DIRECTION('ref_axis',(0.131297210925068,0.0222452083715773,0.991093433086812));
#51476=DIRECTION('center_axis',(-0.797730380655153,0.601098528105586,0.0480291504097525));
#51477=DIRECTION('ref_axis',(0.0760075873921403,0.0212181391866325,0.996881455955663));
#51478=DIRECTION('center_axis',(-0.789873402538101,-0.601098524330917,0.121575375837698));
#51479=DIRECTION('ref_axis',(0.135530123087635,0.0222453097977533,0.990523463592788));
#51480=DIRECTION('center_axis',(-0.80292169045898,0.584826536164717,0.115302565401089));
#51481=DIRECTION('ref_axis',(0.129132272514604,-0.0181846250656886,0.991460627360681));
#51482=DIRECTION('center_axis',(0.994566501061888,-4.70791329828775E-9,
-0.104103193829549));
#51483=DIRECTION('ref_axis',(-0.104090396391608,-0.0156795063510537,-0.994444237984023));
#51484=DIRECTION('',(-0.994566648759581,2.06170772008968E-7,0.104101782766161));
#51485=DIRECTION('center_axis',(-0.807177436659008,0.584827782536509,0.0802561556643659));
#51486=DIRECTION('ref_axis',(0.0792583150449474,-0.0273551074277302,0.996478709051956));
#51487=DIRECTION('center_axis',(-0.999140707616432,6.53531644443777E-10,
0.0414469104244949));
#51488=DIRECTION('ref_axis',(-0.0414418004598346,0.0157023279240177,-0.999017524407062));
#51489=DIRECTION('',(-0.999140703510251,-1.29267417449312E-5,0.0414470073942642));
#51490=DIRECTION('center_axis',(-0.807177928572345,0.584827952254024,0.0802499712649406));
#51491=DIRECTION('ref_axis',(0.100698427306123,0.00246180457994313,0.994913949171627));
#51492=DIRECTION('center_axis',(-0.994566654136008,4.10157440230847E-10,
0.1041017314011));
#51493=DIRECTION('ref_axis',(-0.104088948368872,0.0156707406194045,-0.994444527721834));
#51494=DIRECTION('',(0.994566648423206,-6.42264019716518E-11,-0.104101785980022));
#51495=DIRECTION('center_axis',(-0.802927900605498,0.58482795337543,0.115252120934729));
#51496=DIRECTION('ref_axis',(0.136477184444299,-0.00784642890627583,0.990612139880981));
#51497=DIRECTION('center_axis',(0.986067412984717,-1.20307368323152E-9,
-0.1663461963786));
#51498=DIRECTION('ref_axis',(-0.166325751615243,-0.0156778482801143,-0.985946220350243));
#51499=DIRECTION('',(-0.986067493104144,0.,0.166345721445757));
#51500=DIRECTION('',(-0.629653711784272,-7.62628872217157E-8,0.776875925252085));
#51501=DIRECTION('',(-0.579630823425917,0.,0.814879198737207));
#51502=DIRECTION('center_axis',(0.994566627728983,-1.61526260366513E-7,
-0.10410198368798));
#51503=DIRECTION('ref_axis',(-0.0803539506773033,-0.635772804014541,-0.767682345951786));
#51504=DIRECTION('',(-0.735806627488086,0.,-0.677191706198924));
#51505=DIRECTION('',(0.776875900233977,2.35931335548636E-11,0.629653742651982));
#51506=DIRECTION('center_axis',(0.786043912908388,-0.601098528034509,-0.144275869688652));
#51507=DIRECTION('ref_axis',(0.175405260409767,-0.00691952526967788,0.984471997971818));
#51508=DIRECTION('center_axis',(0.,-1.,1.45983193964168E-32));
#51509=DIRECTION('ref_axis',(1.,0.,0.));
#51510=DIRECTION('center_axis',(0.790385590374402,0.601098528024184,-0.118199738306259));
#51511=DIRECTION('ref_axis',(0.15380555625738,-0.00794574594539266,0.988069185829479));
#51512=DIRECTION('center_axis',(-0.78542038860029,0.601098527972214,0.147632560231834));
#51513=DIRECTION('ref_axis',(0.178087442540051,-0.00897200248407754,0.983973762851922));
#51514=DIRECTION('center_axis',(-0.789873424064263,-0.601098528093318,0.121575217380206));
#51515=DIRECTION('ref_axis',(0.158025217926938,-0.00794573996386805,0.987403107001173));
#51516=DIRECTION('center_axis',(-0.904842557875188,0.398564395022499,0.149687569551504));
#51517=DIRECTION('ref_axis',(-0.40310605101085,-0.915153272210966,2.27467263527814E-16));
#51518=DIRECTION('center_axis',(0.984879681053578,5.74456348530311E-5,-0.173239748752421));
#51519=DIRECTION('ref_axis',(0.1732397170712,0.000363132139149149,0.984879621356915));
#51520=DIRECTION('',(-0.986067643452147,5.94973695487231E-5,0.166344819567047));
#51521=DIRECTION('center_axis',(-0.804293392145717,0.590180063977743,0.069279372355438));
#51522=DIRECTION('ref_axis',(0.565263839752734,0.795824505360262,-0.217117820862523));
#51523=DIRECTION('center_axis',(-0.790753837980066,0.584827782536617,0.180789470083574));
#51524=DIRECTION('ref_axis',(0.203525238326007,-0.02735510741636,0.978687475889306));
#51525=DIRECTION('center_axis',(-0.986067496545839,4.69894213309026E-11,
0.166345701044009));
#51526=DIRECTION('ref_axis',(-0.16632519242299,0.0157023279237646,-0.985945925121266));
#51527=DIRECTION('',(-0.986067493175983,-1.29267417804204E-5,0.16634572051764));
#51528=DIRECTION('center_axis',(-0.78213916976026,0.584826536166289,0.215026141951326));
#51529=DIRECTION('ref_axis',(0.252376992392512,-0.018184624930405,0.967458098899922));
#51530=DIRECTION('center_axis',(0.973676800738548,7.17798744206148E-10,
-0.227933077247569));
#51531=DIRECTION('ref_axis',(-0.227905057190963,-0.0156795066151571,-0.973557105658979));
#51532=DIRECTION('',(-0.973676780617697,2.06170660986877E-7,0.227933163199029));
#51533=DIRECTION('center_axis',(-0.220379505183991,0.550037558020212,0.805538055253767));
#51534=DIRECTION('ref_axis',(2.93242547267914E-16,-0.825842037277522,0.563901524616942));
#51535=DIRECTION('center_axis',(-0.716151223202446,-0.477126089861736,-0.509389948741523));
#51536=DIRECTION('ref_axis',(0.61922185901425,-0.0976233195081025,-0.779123852033267));
#51537=DIRECTION('',(-0.52732033240823,-7.62630514906775E-8,0.849666562263614));
#51538=DIRECTION('',(-0.81487919873641,0.,-0.579630823427038));
#51539=DIRECTION('center_axis',(0.973676779882379,4.07347797860785E-12,
-0.227933166340226));
#51540=DIRECTION('ref_axis',(-0.175936196944572,-0.635772805085134,-0.751557978414747));
#51541=DIRECTION('center_axis',(-0.713631661728486,0.584827951390276,-0.385624323210159));
#51542=DIRECTION('ref_axis',(-0.458305532168383,0.0265489689922669,0.888398104134235));
#51543=DIRECTION('center_axis',(0.921696813429137,2.97646228428206E-11,
0.387911051807723));
#51544=DIRECTION('ref_axis',(0.387862949374495,-0.0157477670559207,-0.921582519547365));
#51545=DIRECTION('center_axis',(-0.899533742181365,-0.000115441197578976,
-0.436851271430586));
#51546=DIRECTION('ref_axis',(0.0107693567476671,0.99969019274119,-0.0224396856556493));
#51547=DIRECTION('',(0.895520921373541,-6.06958927296726E-10,0.445019414612761));
#51548=DIRECTION('center_axis',(0.717354636765597,-0.601098528005662,0.352254005996133));
#51549=DIRECTION('ref_axis',(-0.421651630621408,0.027922013862445,0.906327900671812));
#51550=DIRECTION('',(0.318552670246311,2.24206636476423E-10,0.947905162069996));
#51551=DIRECTION('center_axis',(0.,-1.,1.45983193964168E-32));
#51552=DIRECTION('ref_axis',(1.,0.,0.));
#51553=DIRECTION('center_axis',(-0.718853053469519,0.601098535825989,-0.349185964416385));
#51554=DIRECTION('ref_axis',(-0.419203972104053,0.0258666762854648,0.907523523017518));
#51555=DIRECTION('center_axis',(-0.753354093398353,-0.601098522929298,-0.266717407928618));
#51556=DIRECTION('ref_axis',(-0.352620768704926,0.0268944874816471,0.935379751769861));
#51557=DIRECTION('center_axis',(0.752207681322588,0.601098531694907,0.269933620272695));
#51558=DIRECTION('ref_axis',(-0.356613757471971,0.0268942954984485,0.933864725134944));
#51559=DIRECTION('center_axis',(-0.756336012135367,0.584827952222443,-0.293141779769575));
#51560=DIRECTION('ref_axis',(-0.363577014308828,-0.00326197144318428,0.931558433061814));
#51561=DIRECTION('center_axis',(0.944235222537388,-6.87901178487106E-10,
0.329271688002125));
#51562=DIRECTION('ref_axis',(0.329231191113268,-0.0156832196311381,-0.944119091757041));
#51563=DIRECTION('',(-0.944235193228753,8.32144303432336E-8,-0.329271772048945));
#51564=DIRECTION('center_axis',(-0.742883197204518,0.584827969931003,-0.325731178884637));
#51565=DIRECTION('ref_axis',(-0.396896696751271,0.00704480136778811,0.917836250581561));
#51566=DIRECTION('center_axis',(-0.921696788164321,5.28962013185638E-10,
-0.387911111838235));
#51567=DIRECTION('ref_axis',(0.387863474058534,0.0156715280546057,-0.921583598323928));
#51568=DIRECTION('',(0.921696815638088,-1.44328993199795E-11,0.387911046559141));
#51569=DIRECTION('',(-0.900505403486899,-3.07809289801569E-8,0.434844820931441));
#51570=DIRECTION('center_axis',(-0.189182341558766,0.793626260374901,0.57824510416059));
#51571=DIRECTION('ref_axis',(1.24306842251369E-16,-0.588879097818246,0.808221138150178));
#51572=DIRECTION('center_axis',(-0.409308616753587,0.4715466745495,-0.781095506306734));
#51573=DIRECTION('ref_axis',(0.695078489039964,-0.393415955336541,-0.601738963472167));
#51574=DIRECTION('center_axis',(0.75584721514625,-0.601098528044197,0.259568000606312));
#51575=DIRECTION('ref_axis',(-0.326412540790778,-0.00227572104232137,0.945224668694298));
#51576=DIRECTION('',(0.377443537014619,5.19500677922227E-12,0.926032600055686));
#51577=DIRECTION('center_axis',(-0.787110054750406,0.584828255987491,-0.196045078258655));
#51578=DIRECTION('ref_axis',(-0.264628678073429,-0.0330815410799287,0.96378279419218));
#51579=DIRECTION('center_axis',(0.96305628431587,-1.08237348364162E-7,0.269300191681512));
#51580=DIRECTION('ref_axis',(0.269267103038703,-0.0156751635310825,-0.962937960862183));
#51581=DIRECTION('',(-0.963047106749948,7.77156117236919E-13,-0.269333009823441));
#51582=DIRECTION('center_axis',(-0.777849584821009,0.584827952226153,-0.230057144398405));
#51583=DIRECTION('ref_axis',(-0.299240444333017,-0.0227607295926439,0.953906235257842));
#51584=DIRECTION('center_axis',(-0.944235167903987,5.97413398597196E-10,
-0.329271844671434));
#51585=DIRECTION('ref_axis',(0.329231295236,0.0156933905095839,-0.944118886439383));
#51586=DIRECTION('',(0.944235193658857,-2.20379270384694E-11,0.329271770815569));
#51587=DIRECTION('center_axis',(0.782419631380168,-0.601098527991307,0.162788451917224));
#51588=DIRECTION('ref_axis',(-0.227446178817791,-0.032481686875515,0.973248773828617));
#51589=DIRECTION('',(0.434844806470272,8.00811321699437E-12,0.900505410470049));
#51590=DIRECTION('center_axis',(0.,-1.,1.45983193964168E-32));
#51591=DIRECTION('ref_axis',(1.,0.,0.));
#51592=DIRECTION('center_axis',(-0.756949293860049,0.601098526927086,-0.256336356084852));
#51593=DIRECTION('ref_axis',(-0.323829959303373,-0.00432815696677943,0.946105398206165));
#51594=DIRECTION('center_axis',(-0.753354077033342,-0.601098528375901,-0.266717441877294));
#51595=DIRECTION('ref_axis',(-0.331397130446077,-0.00330175671303345,0.943485580353359));
#51596=DIRECTION('center_axis',(0.752207682272757,0.60109852758074,0.269933626786501));
#51597=DIRECTION('ref_axis',(-0.335424917255577,-0.00330192953264533,0.942061156266116));
#51598=DIRECTION('',(-0.871424337428488,0.,0.490529942141476));
#51599=DIRECTION('center_axis',(0.,-1.,1.45983193964168E-32));
#51600=DIRECTION('ref_axis',(1.,0.,0.));
#51601=DIRECTION('center_axis',(-0.783108000754804,0.601098516989598,-0.159444134500836));
#51602=DIRECTION('ref_axis',(-0.224780462152304,-0.0345386642712182,0.973797116706019));
#51603=DIRECTION('center_axis',(-0.753354077630504,-0.601098533169073,-0.26671742938826));
#51604=DIRECTION('ref_axis',(-0.309688131015092,-0.0335099124882587,0.950247518951462));
#51605=DIRECTION('center_axis',(0.752207680104345,0.60109852274501,0.269933643597471));
#51606=DIRECTION('ref_axis',(-0.313745024739697,-0.0335101026406503,0.948915766794977));
#51607=DIRECTION('',(-0.978058312885208,3.88578058618623E-13,-0.208331314487622));
#51608=DIRECTION('center_axis',(-0.800549814629415,0.584827952146848,-0.130752669894475));
#51609=DIRECTION('ref_axis',(-0.198320384831937,-0.05265627283548,0.978721789831609));
#51610=DIRECTION('center_axis',(-0.963047086493937,5.49753720943777E-10,
-0.269333082252329));
#51611=DIRECTION('ref_axis',(0.269299576821397,0.0157729998148347,-0.962927281990005));
#51612=DIRECTION('',(0.963047106750697,-1.76580972044047E-10,0.269333009820765));
#51613=DIRECTION('',(-0.838904150644731,-6.16008708989698E-13,0.544279180229266));
#51614=DIRECTION('',(0.490529942110868,6.72270837774838E-11,0.871424337445718));
#51615=DIRECTION('center_axis',(0.,-1.,1.45983193964168E-32));
#51616=DIRECTION('ref_axis',(1.,0.,0.));
#51617=DIRECTION('center_axis',(-0.759391731897356,0.601098541947915,-0.249007510718101));
#51618=DIRECTION('ref_axis',(-0.274136938268848,0.0514848384475658,0.960311538245069));
#51619=DIRECTION('center_axis',(0.794949235440494,0.601098534738984,0.0820747501197568));
#51620=DIRECTION('ref_axis',(-0.141768757368629,0.052516518220691,0.988505758581168));
#51621=DIRECTION('center_axis',(-0.788970434280454,0.584827930050748,-0.188419601060691));
#51622=DIRECTION('ref_axis',(-0.216800464321758,0.0219594825770514,0.975968923580468));
#51623=DIRECTION('center_axis',(0.989210085096209,-1.01053617270023E-8,
0.146503950608683));
#51624=DIRECTION('ref_axis',(0.146485803310934,-0.015739139347894,-0.989087553718546));
#51625=DIRECTION('',(-0.98920956969183,0.,-0.146507430631025));
#51626=DIRECTION('center_axis',(-0.780037042816505,0.584827952320453,-0.222527476997218));
#51627=DIRECTION('ref_axis',(-0.251733227677601,0.0322834330622996,0.967258063824091));
#51628=DIRECTION('center_axis',(-0.978058295676359,6.17736426195848E-10,
-0.208331395278425));
#51629=DIRECTION('ref_axis',(0.208305711097874,0.0157020800811686,-0.977937715503975));
#51630=DIRECTION('',(0.978058312885197,-7.77156117237441E-13,0.208331314487675));
#51631=DIRECTION('',(-0.803073192437192,-1.64268989063981E-13,0.595880397050227));
#51632=DIRECTION('center_axis',(0.783956636563995,-0.601098528016923,0.155217755437825));
#51633=DIRECTION('ref_axis',(-0.176969173465271,0.0232723717115823,0.983941211840391));
#51634=DIRECTION('',(0.544279180229423,0.,0.838904150644629));
#51635=DIRECTION('center_axis',(0.,-1.,1.45983193964168E-32));
#51636=DIRECTION('ref_axis',(1.,0.,0.));
#51637=DIRECTION('center_axis',(-0.784612628717512,0.601098534467104,-0.151866963881205));
#51638=DIRECTION('ref_axis',(-0.174294437728632,0.0212179634901381,0.98446495468462));
#51639=DIRECTION('center_axis',(-0.795292643209686,-0.601098524266774,-0.0786776701539809));
#51640=DIRECTION('ref_axis',(-0.115060977215054,0.0222453072138315,0.993109318166575));
#51641=DIRECTION('center_axis',(0.794949236451677,0.601098531229447,0.0820747660288937));
#51642=DIRECTION('ref_axis',(-0.119302758621563,0.0222451235580996,0.992608687380465));
#51643=DIRECTION('center_axis',(-0.806364486303598,0.584827953016318,-0.0880487399062475));
#51644=DIRECTION('ref_axis',(-0.114165681646991,-0.00784645567563293,0.993430737528998));
#51645=DIRECTION('center_axis',(0.996456902738626,-1.43266585541422E-9,
0.0841049403099755));
#51646=DIRECTION('ref_axis',(0.0840946033685045,-0.0156778483110181,-0.99633443318829));
#51647=DIRECTION('',(-0.996456868253666,0.,-0.0841053488792232));
#51648=DIRECTION('center_axis',(-0.801776305949045,0.584827952254045,-0.123008217128146));
#51649=DIRECTION('ref_axis',(-0.149890236715455,0.00246180457886108,0.988699578464359));
#51650=DIRECTION('center_axis',(-0.989209559600953,5.20282766649608E-10,
-0.14650749876402));
#51651=DIRECTION('ref_axis',(0.146489508589636,0.0156707406169381,-0.98908809100185));
#51652=DIRECTION('',(0.989209569691921,-6.41708908203814E-11,0.146507430630414));
#51653=DIRECTION('',(-0.76407287122841,0.,0.645129946175786));
#51654=DIRECTION('center_axis',(0.79722884753577,-0.601098528049182,0.0557379963211305));
#51655=DIRECTION('ref_axis',(-0.0749336502850237,-0.00691952391171873,0.997164514131844));
#51656=DIRECTION('',(0.595880397040365,2.35931335548661E-11,0.80307319244451));
#51657=DIRECTION('center_axis',(0.,-1.,1.45983193964168E-32));
#51658=DIRECTION('ref_axis',(1.,0.,0.));
#51659=DIRECTION('center_axis',(-0.797459710617155,0.601098525255623,-0.0523313756547448));
#51660=DIRECTION('ref_axis',(-0.0722115697536528,-0.00897219529730149,0.997348980500437));
#51661=DIRECTION('center_axis',(-0.795292639168737,-0.601098529139514,-0.0786776737730471));
#51662=DIRECTION('ref_axis',(-0.0924964820476553,-0.00794564883199728,0.995681308187236));
#51663=DIRECTION('center_axis',(0.794949237650369,0.601098526741823,0.0820747872851781));
#51664=DIRECTION('ref_axis',(-0.0967494703898303,-0.00794584267896273,0.995277048646963));
#51665=DIRECTION('center_axis',(-0.811041749443006,0.584825719451611,0.0137897979801614));
#51666=DIRECTION('ref_axis',(0.00387504240444698,-0.0182013008699368,0.999826833353159));
#51667=DIRECTION('center_axis',(0.999771637473267,-4.86463518547559E-9,
0.0213699065047608));
#51668=DIRECTION('ref_axis',(0.0213672794041909,-0.015679506350074,-0.999648734532026));
#51669=DIRECTION('',(-0.999771606725344,2.06171160587013E-7,-0.0213713449689478));
#51670=DIRECTION('center_axis',(-0.810871364980857,0.584827782536638,-0.0215428463151879));
#51671=DIRECTION('ref_axis',(-0.0462585592451372,-0.027355107413009,0.998554877708274));
#51672=DIRECTION('center_axis',(-0.996456860583546,6.00919128441484E-10,
-0.0841054397526283));
#51673=DIRECTION('ref_axis',(0.0840950704737484,0.0157023279254457,-0.996334008262157));
#51674=DIRECTION('',(-0.996456868092506,-1.29267420448973E-5,-0.0841053497952053));
#51675=DIRECTION('',(-0.722057075988495,-7.62629077544141E-8,0.691833490816208));
#51676=DIRECTION('center_axis',(0.999771611042803,-1.6152775507127E-7,0.0213711429936039));
#51677=DIRECTION('ref_axis',(0.0164957749902458,-0.635772804014574,-0.771699961826432));
#51678=DIRECTION('',(-0.645129946174611,0.,-0.764072871229403));
#51679=DIRECTION('center_axis',(-0.916468431161503,0.398564395017297,0.0351003947110158));
#51680=DIRECTION('ref_axis',(-0.398810145302877,-0.91703351520187,-1.87163520774561E-17));
#51681=DIRECTION('center_axis',(0.998826308492376,5.74456517323226E-5,-0.0484355464869609));
#51682=DIRECTION('ref_axis',(0.0484355225308032,0.000363221802276343,0.998826245263454));
#51683=DIRECTION('',(-0.999140739682403,5.94973695487116E-5,0.0414460947130521));
#51684=DIRECTION('center_axis',(-0.806634306274172,0.590180063977203,-0.0320716077777504));
#51685=DIRECTION('ref_axis',(0.588016977321403,0.795820729355314,-0.144587001871456));
#51686=DIRECTION('center_axis',(-0.319602436182492,0.550037558023316,0.771565271088561));
#51687=DIRECTION('ref_axis',(-8.09024547853229E-17,-0.814272451734368,0.580482880321634));
#51688=DIRECTION('center_axis',(-0.646660667342669,-0.477126090214631,-0.595130805242372));
#51689=DIRECTION('ref_axis',(0.711992768894656,-0.0976346405864383,-0.695365928126536));
#51690=DIRECTION('center_axis',(-0.659672919556613,0.584827951390368,-0.472025323977644));
#51691=DIRECTION('ref_axis',(-0.566037463239915,0.0265489689911301,0.823951905425572));
#51692=DIRECTION('center_axis',(0.865810812945574,1.21936651804102E-11,
0.50037149817563));
#51693=DIRECTION('ref_axis',(0.500309450222573,-0.0157477670562345,-0.865703449138751));
#51694=DIRECTION('center_axis',(-0.837688665629566,-0.000115441167396227,
-0.546148044168515));
#51695=DIRECTION('ref_axis',(0.0134844972654758,0.999690756780727,-0.0208939977188291));
#51696=DIRECTION('',(0.832683749197156,-6.06126260028676E-10,0.553748836407778));
#51697=DIRECTION('center_axis',(0.667548951037651,-0.601098528184639,0.439384748691613));
#51698=DIRECTION('ref_axis',(-0.531919783696298,0.0279220099678944,0.846334275018941));
#51699=DIRECTION('',(0.197236768219723,2.24206636476402E-10,0.980355882964059));
#51700=DIRECTION('center_axis',(0.,-1.,1.45983193964168E-32));
#51701=DIRECTION('ref_axis',(1.,0.,0.));
#51702=DIRECTION('center_axis',(-0.669420073431964,0.601098535677805,-0.436528711189015));
#51703=DIRECTION('ref_axis',(-0.52964128500097,0.0258666796488071,0.847827237181295));
#51704=DIRECTION('center_axis',(-0.71398511283608,-0.601098523128875,-0.359034572347476));
#51705=DIRECTION('ref_axis',(-0.46707442261457,0.0268944831968703,0.883808899317516));
#51706=DIRECTION('center_axis',(0.712444648251792,0.601098531545889,0.362081729103742));
#51707=DIRECTION('ref_axis',(-0.470846033187989,0.0268942988832825,0.8818053695225));
#51708=DIRECTION('center_axis',(-0.713631669633069,0.584827952222616,-0.385624307319729));
#51709=DIRECTION('ref_axis',(-0.477465331608741,-0.00326197145780636,0.878644533730202));
#51710=DIRECTION('center_axis',(0.895520951623367,-5.33044822369668E-10,
0.445019353740464));
#51711=DIRECTION('ref_axis',(0.44496462113546,-0.0156832196306143,-0.895410812174945));
#51712=DIRECTION('',(-0.895520920788556,8.32136531871802E-8,-0.445019415789929));
#51713=DIRECTION('center_axis',(-0.696200399396224,0.584827969931464,-0.416270644492716));
#51714=DIRECTION('ref_axis',(-0.508802432901024,0.00704480135282949,0.860854491216662));
#51715=DIRECTION('center_axis',(-0.86581078309822,4.76354188381577E-10,
-0.500371549821578));
#51716=DIRECTION('ref_axis',(0.500310101231311,0.0156715280534181,-0.865704456390509));
#51717=DIRECTION('',(0.865810815148979,-1.44328993199734E-11,0.500371494362999));
#51718=DIRECTION('',(-0.94790515691845,-3.07809289801676E-8,0.31855268557557));
#51719=DIRECTION('center_axis',(-0.260163910989382,0.79362626037384,0.54997463420029));
#51720=DIRECTION('ref_axis',(2.06655110892397E-16,-0.569588725712686,0.821929853175439));
#51721=DIRECTION('center_axis',(-0.308183870524933,0.471546674550742,-0.826236307401465));
#51722=DIRECTION('ref_axis',(0.765017150085957,-0.393413621124861,-0.509876929060126));
#51723=DIRECTION('center_axis',(0.717354637754989,-0.601098528042064,0.352254003919151));
#51724=DIRECTION('ref_axis',(-0.442306743760686,-0.00227572172927009,0.896860951047836));
#51725=DIRECTION('',(0.258404621837449,5.19500677922238E-12,0.966036775393693));
#51726=DIRECTION('center_axis',(0.,-1.,1.45983193964168E-32));
#51727=DIRECTION('ref_axis',(1.,0.,0.));
#51728=DIRECTION('center_axis',(-0.718853055774957,0.601098526949856,-0.349185974949911));
#51729=DIRECTION('ref_axis',(-0.43985491616893,-0.00432815365740093,0.898058416701242));
#51730=DIRECTION('center_axis',(-0.713985095789305,-0.60109852837797,-0.359034597459042));
#51731=DIRECTION('ref_axis',(-0.447034063521164,-0.00330175656877996,0.89451084088194));
#51732=DIRECTION('center_axis',(0.712444648108363,0.60109852759936,0.362081735937665));
#51733=DIRECTION('ref_axis',(-0.450851558771531,-0.00330192635974614,0.892592835079688));
#51734=DIRECTION('center_axis',(-0.756332493285849,0.584828255987547,-0.293150252598519));
#51735=DIRECTION('ref_axis',(-0.383336015959487,-0.033081541076345,0.92301631107382));
#51736=DIRECTION('center_axis',(0.921710028648617,-1.08128393816517E-7,
0.387879650263524));
#51737=DIRECTION('ref_axis',(0.387831992673483,-0.0156751635321966,-0.921596785317285));
#51738=DIRECTION('',(-0.921696815638291,3.88578058618578E-13,-0.38791104655866));
#51739=DIRECTION('center_axis',(-0.742882202695379,0.584827952226373,-0.3257334788031));
#51740=DIRECTION('ref_axis',(-0.416436997041045,-0.0227607295851117,0.908879627169732));
#51741=DIRECTION('center_axis',(-0.895520885907555,6.09172716946589E-10,
-0.445019485981622));
#51742=DIRECTION('ref_axis',(0.444964682358649,0.0156933905080377,-0.895410603548913));
#51743=DIRECTION('',(0.89552092136948,-2.16493489798338E-11,0.445019414620934));
#51744=DIRECTION('',(-0.926032600054708,0.,0.377443537017017));
#51745=DIRECTION('center_axis',(0.755847217242881,-0.601098527856549,0.259567994935592));
#51746=DIRECTION('ref_axis',(-0.347633110564671,-0.0324816893235681,0.937067852558084));
#51747=DIRECTION('',(0.318552670353073,8.15184858242943E-12,0.947905162034117));
#51748=DIRECTION('',(-0.944235193658598,7.77156117236542E-13,-0.329271770816312));
#51749=DIRECTION('center_axis',(-0.777849585318546,0.584827952146123,-0.230057142919619));
#51750=DIRECTION('ref_axis',(-0.319422936029011,-0.052656272845511,0.946148141079728));
#51751=DIRECTION('center_axis',(-0.921696780470485,6.71476112526404E-10,
-0.387911130119185));
#51752=DIRECTION('ref_axis',(0.387862873402704,0.0157729998154662,-0.921582120004842));
#51753=DIRECTION('',(0.921696815639179,-1.75748304775626E-10,0.38791104655655));
#51754=DIRECTION('',(0.377443536984304,6.72270837774768E-11,0.926032600068042));
#51755=DIRECTION('center_axis',(0.,-1.,1.45983193964168E-32));
#51756=DIRECTION('ref_axis',(1.,0.,0.));
#51757=DIRECTION('center_axis',(-0.756949309663079,0.601098517154981,-0.256336332334437));
#51758=DIRECTION('ref_axis',(-0.345057146162678,-0.0345386613841079,0.937945972192355));
#51759=DIRECTION('center_axis',(-0.713985090105492,-0.601098532579805,-0.359034601727267));
#51760=DIRECTION('ref_axis',(-0.42634375475666,-0.0335099233942814,0.903940312085982));
#51761=DIRECTION('center_axis',(0.712444636107614,0.601098522329735,0.362081768298954));
#51762=DIRECTION('ref_axis',(-0.430201741828989,-0.0335101101284208,0.902110599564424));
#51763=DIRECTION('',(-0.900505410468168,-1.43735365431037E-13,0.434844806474168));
#51764=DIRECTION('center_axis',(0.,-1.,1.45983193964168E-32));
#51765=DIRECTION('ref_axis',(1.,0.,0.));
#51766=DIRECTION('center_axis',(-0.722194785664401,0.601098542066865,-0.342221031329518));
#51767=DIRECTION('ref_axis',(-0.392334235304463,0.0514848370752,0.918380726800929));
#51768=DIRECTION('center_axis',(0.778394129727655,0.601098534684237,0.18106112339757));
#51769=DIRECTION('ref_axis',(-0.264543490688213,0.0525165188511361,0.962942758829544));
#51770=DIRECTION('center_axis',(-0.759133928885502,0.584827930050941,-0.285818071939465));
#51771=DIRECTION('ref_axis',(-0.337412268953248,0.0219594825745819,0.941100813879617));
#51772=DIRECTION('center_axis',(0.963048054265193,-1.01060003967696E-8,
0.269329621794607));
#51773=DIRECTION('ref_axis',(0.269296260339939,-0.0157391393484892,-0.962928763543541));
#51774=DIRECTION('',(-0.963047106750002,0.,-0.269333009823247));
#51775=DIRECTION('center_axis',(-0.745996129502959,0.584827952320933,-0.318537346241708));
#51776=DIRECTION('ref_axis',(-0.370977816810699,0.0322834330561264,0.928080405667784));
#51777=DIRECTION('center_axis',(-0.944235167368485,5.9634126920769E-10,
-0.329271846207066));
#51778=DIRECTION('ref_axis',(0.329231251851031,0.015702080083906,-0.944118757088133));
#51779=DIRECTION('',(0.944235193658916,-3.88578058618636E-13,0.3292717708154));
#51780=DIRECTION('',(-0.871424337428328,-1.64268989063966E-13,0.490529942141761));
#51781=DIRECTION('center_axis',(0.758320962041116,-0.601098528084844,0.252249634416525));
#51782=DIRECTION('ref_axis',(-0.298894250086174,0.0232723698954888,0.954002423511005));
#51783=DIRECTION('',(0.434844806474003,0.,0.900505410468248));
#51784=DIRECTION('center_axis',(0.,-1.,1.45983193964168E-32));
#51785=DIRECTION('ref_axis',(1.,0.,0.));
#51786=DIRECTION('center_axis',(-0.759391743085759,0.601098534241087,-0.249007495201229));
#51787=DIRECTION('ref_axis',(-0.296306257953441,0.021217969680861,0.954857266433183));
#51788=DIRECTION('center_axis',(-0.779160595905135,-0.601098524313,-0.177733873691787));
#51789=DIRECTION('ref_axis',(-0.238623290661855,0.0222453060519611,0.970857389894294));
#51790=DIRECTION('center_axis',(0.778394129827603,0.601098531103878,0.181061134854196));
#51791=DIRECTION('ref_axis',(-0.242768872812476,0.0222451269395338,0.96982907190948));
#51792=DIRECTION('center_axis',(-0.788970628195854,0.584827953016308,-0.188418717793627));
#51793=DIRECTION('ref_axis',(-0.237775337804514,-0.00784645567500136,0.971288485397253));
#51794=DIRECTION('center_axis',(0.978058403447699,-1.62597700528713E-9,
0.208330889321143));
#51795=DIRECTION('ref_axis',(0.208305284384794,-0.0156778483096643,-0.977938195168667));
#51796=DIRECTION('',(-0.978058312885179,0.,-0.208331314487758));
#51797=DIRECTION('center_axis',(-0.780037042689349,0.584827952253964,-0.222527477617686));
#51798=DIRECTION('ref_axis',(-0.272625222623443,0.00246180458055105,0.962117158930099));
#51799=DIRECTION('center_axis',(-0.9630470847767,6.1993888346627E-10,-0.269333088392605));
#51800=DIRECTION('ref_axis',(0.269300016023813,0.0156707406182653,-0.96292882876049));
#51801=DIRECTION('',(0.963047106750167,-6.41708908203662E-11,0.269333009822659));
#51802=DIRECTION('',(-0.838904150644707,0.,0.544279180229304));
#51803=DIRECTION('center_axis',(0.783956637020661,-0.601098528036003,0.155217753057459));
#51804=DIRECTION('ref_axis',(-0.199320627528099,-0.00691952505566824,0.979909897702237));
#51805=DIRECTION('',(0.490529942130914,2.35931335548666E-11,0.871424337434434));
#51806=DIRECTION('center_axis',(0.,-1.,1.45983193964168E-32));
#51807=DIRECTION('ref_axis',(1.,0.,0.));
#51808=DIRECTION('center_axis',(-0.784612638143514,0.60109852542789,-0.151866950960011));
#51809=DIRECTION('ref_axis',(-0.196643148413631,-0.00897218324522628,0.980434073311301));
#51810=DIRECTION('center_axis',(-0.779160598291669,-0.601098529343444,-0.177733846216521));
#51811=DIRECTION('ref_axis',(-0.216559054708591,-0.00794563115865621,0.976237185713192));
#51812=DIRECTION('center_axis',(0.778394127547434,0.601098526761477,0.181061159072981));
#51813=DIRECTION('ref_axis',(-0.220727860741832,-0.00794584115531741,0.975303068333464));
#51814=DIRECTION('center_axis',(-0.806374762979318,0.584825719450409,-0.0879694236616418));
#51815=DIRECTION('ref_axis',(-0.121467043420276,-0.0182013008530597,0.992428571742064));
#51816=DIRECTION('center_axis',(0.989209578813874,-4.87840080647454E-10,
0.146507369039505));
#51817=DIRECTION('ref_axis',(0.146489358731641,-0.01567950661673,-0.989087974272586));
#51818=DIRECTION('',(-0.989209569218337,2.06171160587046E-7,-0.146507433827873));
#51819=DIRECTION('center_axis',(-0.801777367483258,0.584827782536624,-0.123002104717406));
#51820=DIRECTION('ref_axis',(-0.171045908405215,-0.0273551074118827,0.984883239433142));
#51821=DIRECTION('center_axis',(-0.978058291785313,6.8004977939135E-10,
-0.20833141354581));
#51822=DIRECTION('ref_axis',(0.208305728553097,0.0157023279262274,-0.977937707806413));
#51823=DIRECTION('',(-0.97805831261045,-1.29267420804535E-5,-0.20833131537649));
#51824=DIRECTION('',(-0.803073168768253,-7.62642219063171E-8,0.595880428949056));
#51825=DIRECTION('center_axis',(0.989209569691421,2.03930294082373E-12,
0.146507430633788));
#51826=DIRECTION('ref_axis',(0.113085605681508,-0.635772805085229,-0.763547369913423));
#51827=DIRECTION('',(-0.544279180228737,0.,-0.838904150645075));
#51828=DIRECTION('center_axis',(-0.913641051314188,0.398564391558955,-0.0800403344242509));
#51829=DIRECTION('ref_axis',(-0.399847251243964,-0.916581788861554,-6.67217341138553E-17));
#51830=DIRECTION('center_axis',(0.997020848376458,5.74456518849634E-5,0.077132513265712));
#51831=DIRECTION('ref_axis',(0.077132529104784,-0.000363102228566342,-0.997020782687438));
#51832=DIRECTION('',(-0.996456789590132,5.94973691223711E-5,-0.0841062598133456));
#51833=DIRECTION('center_axis',(-0.796254114841391,0.590180063812382,-0.132916804342285));
#51834=DIRECTION('ref_axis',(0.601501199445676,0.795822082110392,-0.0697389467291665));
#51835=DIRECTION('center_axis',(-0.413785045848131,0.550037558019381,0.72542444168951));
#51836=DIRECTION('ref_axis',(3.87855366211629E-16,-0.796841686270309,0.604188155314129));
#51837=DIRECTION('center_axis',(-0.566971886742689,-0.477126089856525,-0.671486093691938));
#51838=DIRECTION('ref_axis',(0.793527238897196,-0.0976199624324114,-0.600653697285622));
#51839=DIRECTION('center_axis',(-0.595310741375292,0.584827951390672,-0.550982203410772));
#51840=DIRECTION('ref_axis',(-0.664842645381441,0.0265489689884084,0.746511492964348));
#51841=DIRECTION('center_axis',(0.796270460755438,-3.00458614992124E-11,
0.60494078497678));
#51842=DIRECTION('ref_axis',(0.604865770037167,-0.0157477670566697,-0.796171720214976));
#51843=DIRECTION('center_axis',(-0.762632744771221,-0.000115441241507041,
-0.646831727171784));
#51844=DIRECTION('ref_axis',(0.0160163222934664,0.99969000865124,-0.0190621096176581));
#51845=DIRECTION('',(0.756714656875199,-6.07736083413749E-10,0.653745308258691));
#51846=DIRECTION('center_axis',(0.607215616380602,-0.601098528161896,0.519586137868524));
#51847=DIRECTION('ref_axis',(-0.633799249129408,0.0279220104056515,0.772993449608666));
#51848=DIRECTION('',(0.0728103245348834,2.24206636476344E-10,0.997345805947528));
#51849=DIRECTION('center_axis',(0.,-1.,1.45983193964168E-32));
#51850=DIRECTION('ref_axis',(1.,0.,0.));
#51851=DIRECTION('center_axis',(-0.609429936565619,0.601098535479941,-0.516987140131643));
#51852=DIRECTION('ref_axis',(-0.631725838972641,0.0258666841461149,0.774760207435564));
#51853=DIRECTION('center_axis',(-0.66335616311592,-0.601098523127959,-0.44568954031872));
#51854=DIRECTION('ref_axis',(-0.574162028410077,0.0268944832644721,0.818299854516645));
#51855=DIRECTION('center_axis',(0.661445936087663,0.601098531516931,0.44851959716528));
#51856=DIRECTION('ref_axis',(-0.577652789222863,0.0268942995145629,0.815839415422341));
#51857=DIRECTION('center_axis',(-0.659672929381783,0.584827952222579,-0.472025309215514));
#51858=DIRECTION('ref_axis',(-0.583823735431116,-0.00326197144977297,0.81187388521218));
#51859=DIRECTION('center_axis',(0.832683801792781,-7.44626053212263E-10,
0.553748757318625));
#51860=DIRECTION('ref_axis',(0.553680652163339,-0.015683219631694,-0.832581390641157));
#51861=DIRECTION('',(-0.832683748468971,8.32144303432563E-8,-0.553748837502758));
#51862=DIRECTION('center_axis',(-0.638538105377738,0.584827969931015,-0.500245273407933));
#51863=DIRECTION('ref_axis',(-0.61268405077085,0.00704480136482595,0.790296542257875));
#51864=DIRECTION('center_axis',(-0.796270418241213,5.26330196580228E-10,
-0.60494084093733));
#51865=DIRECTION('ref_axis',(0.604866550617452,0.0156715280534126,-0.796172631501873));
#51866=DIRECTION('',(0.796270460894481,-1.40443212613737E-11,0.604940784793761));
#51867=DIRECTION('',(-0.980355879774395,-3.07807852448036E-8,0.19723678407379));
#51868=DIRECTION('center_axis',(-0.327042540108679,0.793626260381241,0.513030735719167));
#51869=DIRECTION('ref_axis',(-9.03584097610045E-18,-0.542884142424063,0.839807601718685));
#51870=DIRECTION('center_axis',(-0.202198880525624,0.471546674565983,-0.858346868357978));
#51871=DIRECTION('ref_axis',(0.822883322106636,-0.393422484402515,-0.409977788380418));
#51872=DIRECTION('center_axis',(0.667548955300865,-0.601098528008301,0.439384742455831));
#51873=DIRECTION('ref_axis',(-0.551225498185787,-0.00227572877616902,0.83435320530838));
#51874=DIRECTION('',(0.135290511410413,5.05127141378944E-12,0.990805973701365));
#51875=DIRECTION('center_axis',(0.,-1.,1.45983193964168E-32));
#51876=DIRECTION('ref_axis',(1.,0.,0.));
#51877=DIRECTION('center_axis',(-0.669420074346758,0.601098526972795,-0.436528721772939));
#51878=DIRECTION('ref_axis',(-0.54894309775187,-0.00432815035528203,0.835848516505882));
#51879=DIRECTION('center_axis',(-0.663356142061132,-0.601098528374394,-0.445689564580449));
#51880=DIRECTION('ref_axis',(-0.555621003655155,-0.00330175758509039,0.83142913028958));
#51881=DIRECTION('center_axis',(0.661445935961308,0.601098527608529,0.448519602589595));
#51882=DIRECTION('ref_axis',(-0.559168004095893,-0.00330192476536948,0.82904779143802));
#51883=DIRECTION('center_axis',(-0.713627116581051,0.584828255988157,-0.385632272350314));
#51884=DIRECTION('ref_axis',(-0.495997915892786,-0.0330815410631934,0.867693309338557));
#51885=DIRECTION('center_axis',(0.865827858828577,-1.0812546324535E-7,0.500342001911003));
#51886=DIRECTION('ref_axis',(0.500280526962411,-0.0156751635318979,-0.865721481534599));
#51887=DIRECTION('',(-0.865810815149254,3.88578058618869E-13,-0.500371494362523));
#51888=DIRECTION('center_axis',(-0.696199124466262,0.584827952226206,-0.416272801642521));
#51889=DIRECTION('ref_axis',(-0.527066089522084,-0.0227607295921243,0.84951944442981));
#51890=DIRECTION('center_axis',(-0.832683715238848,4.65217159593631E-10,
-0.553748887471596));
#51891=DIRECTION('ref_axis',(0.553680693946936,0.0156933905093404,-0.832581171204802));
#51892=DIRECTION('',(0.832683749192512,-2.28705943069147E-11,0.553748836414761));
#51893=DIRECTION('',(-0.966036775393065,0.,0.258404621839796));
#51894=DIRECTION('center_axis',(0.717354638086269,-0.601098527996424,0.35225400332239));
#51895=DIRECTION('ref_axis',(-0.462337666708267,-0.0324816867803975,0.886108809326855));
#51896=DIRECTION('',(0.197236768330282,8.15184858243042E-12,0.980355882941816));
#51897=DIRECTION('center_axis',(0.,-1.,1.45983193964168E-32));
#51898=DIRECTION('ref_axis',(1.,0.,0.));
#51899=DIRECTION('center_axis',(-0.718853072762017,0.601098517458356,-0.349185956318367));
#51900=DIRECTION('ref_axis',(-0.459892075508836,-0.0345386560330738,0.887302857046907));
#51901=DIRECTION('center_axis',(-0.663356131866617,-0.601098532278994,-0.445689574487668));
#51902=DIRECTION('ref_axis',(-0.536275675289761,-0.0335099289335965,0.84337742722661));
#51903=DIRECTION('center_axis',(0.661445920052673,0.601098522425337,0.448519632996985));
#51904=DIRECTION('ref_axis',(-0.539873909196622,-0.0335101084212974,0.841078613925209));
#51905=DIRECTION('',(-0.895520921369859,8.32667268468674E-13,-0.44501941462017));
#51906=DIRECTION('center_axis',(-0.742882203369472,0.584827952147132,-0.325733477408004));
#51907=DIRECTION('ref_axis',(-0.435487996740383,-0.0526562728318949,0.898653170932202));
#51908=DIRECTION('center_axis',(-0.865810776031052,5.73356427121151E-10,
-0.50037156205015));
#51909=DIRECTION('ref_axis',(0.500309315085384,0.015772999814506,-0.865703067867757));
#51910=DIRECTION('',(0.865810815150186,-1.7652546089277E-10,0.50037149436091));
#51911=DIRECTION('',(-0.947905162032818,-1.43735365431086E-13,0.31855267035694));
#51912=DIRECTION('',(0.258404621807034,6.51326541667456E-11,0.966036775401829));
#51913=DIRECTION('center_axis',(-0.717325427945312,0.584827930050931,-0.378709021090623));
#51914=DIRECTION('ref_axis',(-0.452702880547943,0.0219594825762896,0.891390982155741));
#51915=DIRECTION('center_axis',(0.921698179088528,-1.00810072301223E-8,
0.38790780691408));
#51916=DIRECTION('ref_axis',(0.387859757432562,-0.0157391393497043,-0.921584010308819));
#51917=DIRECTION('',(-0.921696815638489,1.60982338570588E-12,-0.387911046558189));
#51918=DIRECTION('center_axis',(-0.700190411576892,0.584827952319919,-0.409523691281803));
#51919=DIRECTION('ref_axis',(-0.484371864185748,0.0322834330701548,0.874266365093858));
#51920=DIRECTION('center_axis',(-0.895520892717308,4.74561357526579E-10,
-0.445019472278231));
#51921=DIRECTION('ref_axis',(0.444964607943966,0.0157020800824926,-0.895410488188716));
#51922=DIRECTION('',(0.895520921369544,0.,0.445019414620803));
#51923=DIRECTION('center_axis',(0.720726111367983,-0.601098528029885,0.345303391226748));
#51924=DIRECTION('ref_axis',(-0.416105590020171,0.0232723713891031,0.90901844573358));
#51925=DIRECTION('',(0.318552670357153,0.,0.947905162032746));
#51926=DIRECTION('center_axis',(0.,-1.,1.45983193964168E-32));
#51927=DIRECTION('ref_axis',(1.,0.,0.));
#51928=DIRECTION('center_axis',(-0.673608395900761,0.601098542100637,-0.430037523544739));
#51929=DIRECTION('ref_axis',(-0.504344188395324,0.0514848367856261,0.861966502372928));
#51930=DIRECTION('center_axis',(0.749563254147552,0.601098538699542,0.277192126159831));
#51931=DIRECTION('ref_axis',(-0.3831462732819,0.0525164728782138,0.922193555251078));
#51932=DIRECTION('',(-0.926032600054682,-1.64268989064055E-13,0.377443537017083));
#51933=DIRECTION('center_axis',(0.,-1.,1.45983193964168E-32));
#51934=DIRECTION('ref_axis',(1.,0.,0.));
#51935=DIRECTION('center_axis',(-0.722194799748368,0.601098534343069,-0.342221015174447));
#51936=DIRECTION('ref_axis',(-0.413645140020028,0.0212179668797318,0.910190911852729));
#51937=DIRECTION('center_axis',(-0.750740720407566,-0.601098524335125,-0.27398710693035));
#51938=DIRECTION('ref_axis',(-0.358422371524481,0.0222453054265748,0.933294460487817));
#51939=DIRECTION('center_axis',(0.749563276968541,0.601098531420702,0.277192080233288));
#51940=DIRECTION('ref_axis',(-0.362406391970458,0.0222451184080069,0.931754668228697));
#51941=DIRECTION('center_axis',(-0.759134231971544,0.584827953016391,-0.285817219949449));
#51942=DIRECTION('ref_axis',(-0.35763513484838,-0.00784645567247245,0.933828433629733));
#51943=DIRECTION('center_axis',(0.94423530926095,-9.70178035548998E-10,
0.329271439309392));
#51944=DIRECTION('ref_axis',(0.32923097018331,-0.0156778483086887,-0.944119258009583));
#51945=DIRECTION('',(-0.944235193658824,3.88578058618818E-13,-0.329271770815664));
#51946=DIRECTION('center_axis',(-0.74599612929426,0.58482795225407,-0.318537346853226));
#51947=DIRECTION('ref_axis',(-0.391060745912263,0.00246180458148873,0.920361577058032));
#51948=DIRECTION('center_axis',(-0.921696791818101,4.61753290138909E-10,
-0.387911103156664));
#51949=DIRECTION('ref_axis',(0.387863470164475,0.015670740618503,-0.921583613352819));
#51950=DIRECTION('',(0.92169681563878,-6.42264019716333E-11,0.387911046557498));
#51951=DIRECTION('',(-0.90050541046819,0.,0.434844806474122));
#51952=DIRECTION('center_axis',(0.758320961992543,-0.601098528033327,0.252249634685309));
#51953=DIRECTION('ref_axis',(-0.320564200670215,-0.00691952525868305,0.947201516795059));
#51954=DIRECTION('',(0.3774435370056,2.35931335548606E-11,0.926032600059362));
#51955=DIRECTION('center_axis',(0.,-1.,1.45983193964168E-32));
#51956=DIRECTION('ref_axis',(1.,0.,0.));
#51957=DIRECTION('center_axis',(-0.759391757226185,0.601098525421464,-0.249007473367908));
#51958=DIRECTION('ref_axis',(-0.317973530880616,-0.00897218348452268,0.94805713624382));
#51959=DIRECTION('center_axis',(-0.750740714555744,-0.601098529097443,-0.273987112516669));
#51960=DIRECTION('ref_axis',(-0.337206411814674,-0.00794565257757915,0.941397207578283));
#51961=DIRECTION('center_axis',(0.749563277928319,0.601098526787934,0.277192087684207));
#51962=DIRECTION('ref_axis',(-0.341225240450696,-0.00794583919521706,0.939947976708737));
#51963=DIRECTION('center_axis',(-0.788970653144117,0.584827952229847,-0.18841861576816));
#51964=DIRECTION('ref_axis',(-0.244956601238545,-0.0181546317064356,0.969364055892967));
#51965=DIRECTION('center_axis',(0.963047096323551,3.03853506791505E-10,
0.269333047104838));
#51966=DIRECTION('ref_axis',(0.26929993772326,-0.0156795066156373,-0.962928707960531));
#51967=DIRECTION('',(-0.963047105879734,2.06171549165051E-7,-0.269333012934965));
#51968=DIRECTION('center_axis',(-0.780038861941738,0.584827782536567,-0.222521546448878));
#51969=DIRECTION('ref_axis',(-0.293135761410684,-0.0273551074116156,0.955679404131259));
#51970=DIRECTION('center_axis',(-0.944235164423757,5.82024366209817E-10,
-0.329271854651504));
#51971=DIRECTION('ref_axis',(0.329231259012644,0.0157023279254938,-0.944118750468748));
#51972=DIRECTION('',(-0.944235193274803,-1.29267418160562E-5,-0.329271771663157));
#51973=DIRECTION('',(-0.871424317944096,-7.62629077544537E-8,0.490529976755408));
#51974=DIRECTION('center_axis',(0.963047106749398,1.61336649447084E-12,
0.269333009825408));
#51975=DIRECTION('ref_axis',(0.20789175275403,-0.635772805084664,-0.74335318621207));
#51976=DIRECTION('',(-0.434844806473195,0.,-0.900505410468638));
#51977=DIRECTION('center_axis',(-0.896405004805104,0.39856439155694,-0.193918779758972));
#51978=DIRECTION('ref_axis',(-0.40627649968951,-0.91375018785226,2.11715934575633E-16));
#51979=DIRECTION('center_axis',(0.979491773889296,5.74456562550402E-5,0.201484147225525));
#51980=DIRECTION('ref_axis',(0.201484154709456,-0.00036293807059144,-0.979491706793362));
#51981=DIRECTION('',(-0.978058120671607,5.94973691578955E-5,-0.20833220837976));
#51982=DIRECTION('center_axis',(-0.773316520430496,0.590180063812117,-0.231665818600838));
#51983=DIRECTION('ref_axis',(0.605499692316029,0.795821432315522,0.00619439040305992));
#51984=DIRECTION('center_axis',(-0.501442018156305,0.550037558016864,0.667843235496308));
#51985=DIRECTION('ref_axis',(-5.60351980611002E-16,-0.771902436601816,0.635741007304216));
#51986=DIRECTION('center_axis',(-0.478341620775355,-0.477126089438627,-0.737251645376943));
#51987=DIRECTION('ref_axis',(0.862552725675641,-0.0976242841602588,-0.496459761281536));
#51988=DIRECTION('center_axis',(-0.521560157177763,0.58482795139038,-0.621249764359906));
#51989=DIRECTION('ref_axis',(-0.753162861850607,0.0265489689898624,0.657298148312148));
#51990=DIRECTION('center_axis',(0.714172443316223,9.09561476418819E-12,
0.699969800211221));
#51991=DIRECTION('ref_axis',(0.699883001315757,-0.0157477670549617,-0.714083883239238));
#51992=DIRECTION('center_axis',(-0.675549637427138,-0.000115441124074375,
-0.73731450144793));
#51993=DIRECTION('ref_axis',(0.0187140380375274,0.999675144775611,-0.0173028812106884));
#51994=DIRECTION('',(0.668811722374505,-6.06625860390613E-10,0.743431826070453));
#51995=DIRECTION('center_axis',(0.53730612122198,-0.601098527862433,0.591593350113916));
#51996=DIRECTION('ref_axis',(-0.725683327143529,0.0279220169301707,0.687462049626341));
#51997=DIRECTION('',(-0.0527643814626423,2.24206636476439E-10,0.998606989785704));
#51998=DIRECTION('center_axis',(0.,-1.,1.45983193964168E-32));
#51999=DIRECTION('ref_axis',(1.,0.,0.));
#52000=DIRECTION('center_axis',(-0.53982872696825,0.60109853538561,-0.589292369114953));
#52001=DIRECTION('ref_axis',(-0.723847695975665,0.0258666862474939,0.689474747596527));
#52002=DIRECTION('center_axis',(-0.602265686714187,-0.601098523280458,-0.525315722129789));
#52003=DIRECTION('ref_axis',(-0.672194759395683,0.0268944799871021,0.739885729276625));
#52004=DIRECTION('center_axis',(0.600015829518251,0.601098531375124,0.52788404020788));
#52005=DIRECTION('ref_axis',(-0.675349613221344,0.0268943027491544,0.737007188839714));
#52006=DIRECTION('center_axis',(-0.595310752991289,0.584827952222906,-0.550982189976869));
#52007=DIRECTION('ref_axis',(-0.68097489015979,-0.00326197146842053,0.732299500555613));
#52008=DIRECTION('center_axis',(0.756714686154918,-3.50932338498322E-10,
0.653745274367214));
#52009=DIRECTION('ref_axis',(0.653664870720632,-0.0156832196319518,-0.756621618385145));
#52010=DIRECTION('',(-0.756714656015473,8.32132090980655E-8,-0.653745309253824));
#52011=DIRECTION('center_axis',(-0.570805683990802,0.584827969930714,-0.576330735524762));
#52012=DIRECTION('ref_axis',(-0.706903275156747,0.00704480137507825,0.707275144725339));
#52013=DIRECTION('center_axis',(-0.714172407611761,4.01813307213759E-10,
-0.699969836640137));
#52014=DIRECTION('ref_axis',(0.699883876193368,0.0156715280549141,-0.714084702996059));
#52015=DIRECTION('',(0.714172445802828,-1.60427227056679E-11,0.699969797674162));
#52016=DIRECTION('',(-0.997345804770054,-3.07807852448081E-8,0.0728103406637648));
#52017=DIRECTION('center_axis',(-0.38876351302317,0.793626260381023,0.467996036068166));
#52018=DIRECTION('ref_axis',(5.14608281189496E-16,-0.507952836951219,0.861384882287359));
#52019=DIRECTION('center_axis',(-0.0930250935211342,0.471546674525771,-0.876920786456263));
#52020=DIRECTION('ref_axis',(0.867779998855256,-0.393420034062469,-0.303609206686916));
#52021=DIRECTION('center_axis',(0.607215617952052,-0.601098528024132,0.51958613619142));
#52022=DIRECTION('ref_axis',(-0.651451109280604,-0.0022757251850946,0.7586872038541));
#52023=DIRECTION('',(0.0100427887997458,5.05127141378811E-12,0.999949569924966));
#52024=DIRECTION('center_axis',(0.,-1.,1.45983193964168E-32));
#52025=DIRECTION('ref_axis',(1.,0.,0.));
#52026=DIRECTION('center_axis',(-0.609429937620773,0.601098526993246,-0.516987148755257));
#52027=DIRECTION('ref_axis',(-0.64937411786308,-0.00432814735280087,0.760456785221908));
#52028=DIRECTION('center_axis',(-0.602265662641906,-0.601098528361773,-0.525315743913902));
#52029=DIRECTION('ref_axis',(-0.655445470963613,-0.00330176107082695,0.75523528318473));
#52030=DIRECTION('center_axis',(0.600015828005484,0.601098527623849,0.527884046198912));
#52031=DIRECTION('ref_axis',(-0.658666035184986,-0.00330192209803078,0.752428170262218));
#52032=DIRECTION('center_axis',(-0.659667413965905,0.584828255987831,-0.472032640767318));
#52033=DIRECTION('ref_axis',(-0.600837632369412,-0.0330815410726327,0.798686265794635));
#52034=DIRECTION('center_axis',(0.796291065774804,-1.08116165302368E-7,
0.604913662076842));
#52035=DIRECTION('ref_axis',(0.604839339266343,-0.0156751635312651,-0.796193232151669));
#52036=DIRECTION('',(-0.796270460894816,0.,-0.604940784793319));
#52037=DIRECTION('center_axis',(-0.638536570136217,0.584827952226412,-0.500247253758917));
#52038=DIRECTION('ref_axis',(-0.629383034939896,-0.0227607295784563,0.776761832558026));
#52039=DIRECTION('center_axis',(-0.756714605335634,6.02210338294383E-10,
-0.653745367916084));
#52040=DIRECTION('ref_axis',(0.653664859942376,0.0156933905078516,-0.756621416806901));
#52041=DIRECTION('',(0.756714656868826,-2.2482016248314E-11,0.653745308266067));
#52042=DIRECTION('',(-0.990805973701014,0.,0.13529051141298));
#52043=DIRECTION('center_axis',(0.667548949926352,-0.601098527953579,0.439384750696091));
#52044=DIRECTION('ref_axis',(-0.569750877659947,-0.0324816875124569,0.82117530246718));
#52045=DIRECTION('',(0.0728103246472944,8.15184858242776E-12,0.997345805939322));
#52046=DIRECTION('center_axis',(0.,-1.,1.45983193964168E-32));
#52047=DIRECTION('ref_axis',(1.,0.,0.));
#52048=DIRECTION('center_axis',(-0.669420094475072,0.601098517583778,-0.436528703834663));
#52049=DIRECTION('ref_axis',(-0.567474227812613,-0.0345386538450982,0.822666446476971));
#52050=DIRECTION('center_axis',(-0.602265649429205,-0.601098531988501,-0.525315754912117));
#52051=DIRECTION('ref_axis',(-0.637750206829724,-0.0335099342688502,0.769513975177801));
#52052=DIRECTION('center_axis',(0.600015812540529,0.60109852279929,0.527884069270744));
#52053=DIRECTION('ref_axis',(-0.641031937936639,-0.0335101017961318,0.766782320885667));
#52054=DIRECTION('',(-0.832683749192486,0.,-0.5537488364148));
#52055=DIRECTION('center_axis',(-0.696199125313164,0.58482795214638,-0.416272800338259));
#52056=DIRECTION('ref_axis',(-0.544685151566205,-0.0526562728418925,0.836985903461761));
#52057=DIRECTION('center_axis',(-0.796270413842743,5.69899567997189E-10,
-0.60494084672694));
#52058=DIRECTION('ref_axis',(0.604865591185688,0.0157729998149048,-0.796171356603858));
#52059=DIRECTION('',(0.796270460896058,-1.76914038951424E-10,0.604940784791685));
#52060=DIRECTION('',(-0.980355882940996,0.,0.197236768334354));
#52061=DIRECTION('',(0.135290511377995,6.7370819142914E-11,0.990805973705791));
#52062=DIRECTION('center_axis',(0.,-1.,1.45983193964168E-32));
#52063=DIRECTION('ref_axis',(1.,0.,0.));
#52064=DIRECTION('center_axis',(-0.614398793752247,0.601098541642861,-0.511072074633911));
#52065=DIRECTION('ref_axis',(-0.608400338225441,0.051484842085893,0.791958546568291));
#52066=DIRECTION('center_axis',(0.708911344827112,0.601098538035799,0.368951558807712));
#52067=DIRECTION('ref_axis',(-0.495706541700321,0.0525164805429546,0.866900826961706));
#52068=DIRECTION('center_axis',(-0.664203715286355,0.584827908067513,-0.465628330909084));
#52069=DIRECTION('ref_axis',(-0.56085476194302,0.0219600677391468,0.82762291620685));
#52070=DIRECTION('center_axis',(0.865814280566785,-1.94983737445407E-8,
0.500365497977848));
#52071=DIRECTION('ref_axis',(0.500303518481015,-0.0157391387106383,-0.865707034110365));
#52072=DIRECTION('',(-0.865810815149096,3.88578058618736E-13,-0.500371494362796));
#52073=DIRECTION('center_axis',(-0.643342272598766,0.584827952320221,-0.494051603046071));
#52074=DIRECTION('ref_axis',(-0.590127077891625,0.032283433066789,0.806664621691391));
#52075=DIRECTION('center_axis',(-0.832683710697438,5.14805201568008E-10,
-0.553748894300607));
#52076=DIRECTION('ref_axis',(0.553680625231442,0.0157020800817568,-0.832581053065961));
#52077=DIRECTION('',(0.832683749192297,-7.77156117237866E-13,0.553748836415085));
#52078=DIRECTION('',(-0.966036775393088,0.,0.258404621839711));
#52079=DIRECTION('center_axis',(0.671764979831684,-0.601098528016402,0.432911505377545));
#52080=DIRECTION('ref_axis',(-0.526754694709403,0.0232723717226879,0.849698704433521));
#52081=DIRECTION('',(0.197236768334356,1.43735365432692E-13,0.980355882940996));
#52082=DIRECTION('center_axis',(-0.717325835416885,0.584827953016236,-0.378708213819436));
#52083=DIRECTION('ref_axis',(-0.471854812183757,-0.00784645566122617,0.881641349615924));
#52084=DIRECTION('center_axis',(0.895521109945517,-1.54028260138715E-9,
0.445019035145632));
#52085=DIRECTION('ref_axis',(0.444964340052093,-0.0156778483093563,-0.895411045919356));
#52086=DIRECTION('',(-0.895520921369635,3.88578058618527E-13,-0.445019414620621));
#52087=DIRECTION('center_axis',(-0.7001904113086,0.584827952254159,-0.40952369183443));
#52088=DIRECTION('ref_axis',(-0.503329007621636,0.00246180457671532,0.864091343322478));
#52089=DIRECTION('center_axis',(-0.865810778099468,5.60508848932578E-10,
-0.500371558471097));
#52090=DIRECTION('ref_axis',(0.500310116056249,0.0156707406188733,-0.865704462077122));
#52091=DIRECTION('',(0.865810815149366,-6.46149800302453E-11,0.50037149436233));
#52092=DIRECTION('center_axis',(0.720726110244692,-0.60109852806954,0.345303393502279));
#52093=DIRECTION('ref_axis',(-0.436752288568508,-0.00691952239342252,0.899555200440761));
#52094=DIRECTION('',(0.258404621828094,2.35931335548689E-11,0.966036775396196));
#52095=DIRECTION('center_axis',(0.,-1.,1.45983193964168E-32));
#52096=DIRECTION('ref_axis',(1.,0.,0.));
#52097=DIRECTION('center_axis',(-0.673608405718115,0.601098534097765,-0.430037519353157));
#52098=DIRECTION('ref_axis',(-0.524460602283865,0.0212179736208634,0.851170296854554));
#52099=DIRECTION('center_axis',(-0.710481210982187,-0.601098524559535,-0.365919407265637));
#52100=DIRECTION('ref_axis',(-0.472568923490101,0.0222452996576803,0.881012916587803));
#52101=DIRECTION('center_axis',(0.708911378994718,0.601098530857045,0.368951504853022));
#52102=DIRECTION('ref_axis',(-0.476328516796978,0.0222451336537348,0.878985948758408));
#52103=DIRECTION('',(-0.947905162032792,1.64268989064054E-13,0.318552670357018));
#52104=DIRECTION('center_axis',(0.,-1.,1.45983193964168E-32));
#52105=DIRECTION('ref_axis',(1.,0.,0.));
#52106=DIRECTION('center_axis',(-0.722194816033392,0.601098525392591,-0.342220996529068));
#52107=DIRECTION('ref_axis',(-0.434289278687137,-0.00897218548941485,0.900728772886128));
#52108=DIRECTION('center_axis',(-0.710481209891288,-0.601098529111296,-0.365919401906551));
#52109=DIRECTION('ref_axis',(-0.452535793264877,-0.00794565142206212,0.891710840148087));
#52110=DIRECTION('center_axis',(0.708911366633865,0.601098526781341,0.368951535243596));
#52111=DIRECTION('ref_axis',(-0.456341297275093,-0.0079458395878439,0.889769343164019));
#52112=DIRECTION('center_axis',(-0.759134269503231,0.584827952230624,-0.285817121872591));
#52113=DIRECTION('ref_axis',(-0.364518576916482,-0.018154631692394,0.931019127854469));
#52114=DIRECTION('center_axis',(0.92169678288755,6.8097117849751E-10,0.387911124376114));
#52115=DIRECTION('ref_axis',(0.387863438075824,-0.0156795066142625,-0.921583477757894));
#52116=DIRECTION('',(-0.921696815638345,1.99840144432174E-12,-0.387911046558531));
#52117=DIRECTION('center_axis',(-0.745996131539549,0.58482795217557,-0.318537341739014));
#52118=DIRECTION('ref_axis',(-0.410607314150629,-0.0273514813181276,0.911401958542832));
#52119=DIRECTION('center_axis',(-0.895520883366674,5.55358532199175E-10,
-0.445019491094685));
#52120=DIRECTION('ref_axis',(0.444964625027153,0.0157023279249333,-0.895410475353166));
#52121=DIRECTION('',(-0.895520920882602,-1.29267412633629E-5,-0.445019415412942));
#52122=DIRECTION('',(-0.926032600054565,-7.39210450788166E-13,0.37744353701737));
#52123=DIRECTION('center_axis',(0.921696815868328,-4.81892124678041E-10,
0.38791104601208));
#52124=DIRECTION('ref_axis',(0.299419321991596,-0.635772805082133,-0.711435879005332));
#52125=DIRECTION('',(-0.318552670356402,0.,-0.947905162032999));
#52126=DIRECTION('center_axis',(-0.865032115883027,0.398564391556874,-0.304739010095249));
#52127=DIRECTION('ref_axis',(-0.418468469414644,-0.908231325217186,1.44167877428543E-16));
#52128=DIRECTION('center_axis',(0.946515529011113,5.74456512495677E-5,0.322658255807611));
#52129=DIRECTION('ref_axis',(0.322658254835461,-0.000362742142822936,-0.946515461577185));
#52130=DIRECTION('',(-0.944234890926654,5.94973683762808E-5,-0.329272633567979));
#52131=DIRECTION('center_axis',(-0.73818326258567,0.590180063815931,-0.326761324383104));
#52132=DIRECTION('ref_axis',(0.599952266514969,0.795819902379834,0.0820241481498212));
#52133=DIRECTION('center_axis',(-0.581190950296166,0.550037558009473,0.599729742528095));
#52134=DIRECTION('ref_axis',(0.718118878862159,-2.4451179902057E-16,0.695920452222634));
#52135=DIRECTION('center_axis',(-0.382167621418612,-0.477126090026257,-0.791390297739047));
#52136=DIRECTION('ref_axis',(0.917972909631245,-0.0976141048661876,-0.384444044971853));
#52137=DIRECTION('center_axis',(-0.439584257727902,0.584827951390055,-0.681719845413584));
#52138=DIRECTION('ref_axis',(-0.829605250075042,0.0265489689967324,0.557718819202955));
#52139=DIRECTION('center_axis',(0.62081150436806,-2.72556222406521E-11,
0.783959868899082));
#52140=DIRECTION('ref_axis',(0.783862654917877,-0.0157477670581149,-0.620734521400076));
#52141=DIRECTION('center_axis',(-0.577812718057188,-0.000115441154269082,
-0.816169375512647));
#52142=DIRECTION('ref_axis',(0.0202289007957235,0.999690764743852,-0.0144625882347842));
#52143=DIRECTION('',(0.570361227482597,-6.06126260028481E-10,0.821393979880876));
#52144=DIRECTION('center_axis',(0.458923006270181,-0.601098528268336,0.6542707647676));
#52145=DIRECTION('ref_axis',(-0.806122932258831,0.0279220081159775,0.591088977692188));
#52146=DIRECTION('',(-0.177506961644612,2.24206636476395E-10,0.98411954485606));
#52147=DIRECTION('center_axis',(0.,-1.,1.45983193964168E-32));
#52148=DIRECTION('ref_axis',(1.,0.,0.));
#52149=DIRECTION('center_axis',(-0.461714093721715,0.601098535245096,-0.652304105908383));
#52150=DIRECTION('ref_axis',(-0.804554042774789,0.0258666894925332,0.593315857389165));
#52151=DIRECTION('center_axis',(-0.531677123659475,-0.60109852328464,-0.596657356849148));
#52152=DIRECTION('ref_axis',(-0.759626573944644,0.0268944798668635,0.649803166435663));
#52153=DIRECTION('center_axis',(0.529123109915892,0.601098531435083,0.598923442569684));
#52154=DIRECTION('ref_axis',(-0.76239577523424,0.0268943012708223,0.646551914747869));
#52155=DIRECTION('center_axis',(-0.521560170386556,0.584827952222643,-0.621249752487208));
#52156=DIRECTION('ref_axis',(-0.767386664096021,-0.00326197146761128,0.641176315306269));
#52157=DIRECTION('center_axis',(0.668811781409396,-6.23322798646924E-10,
0.743431772961037));
#52158=DIRECTION('ref_axis',(0.743340338836695,-0.0156832196313301,-0.668729524755818));
#52159=DIRECTION('',(-0.668811721396591,8.32139862539898E-8,-0.743431826950207));
#52160=DIRECTION('center_axis',(-0.494071316001355,0.584827969930883,-0.643327117640172));
#52161=DIRECTION('ref_axis',(-0.789974212594529,0.00704480137084633,0.613099595668843));
#52162=DIRECTION('center_axis',(-0.620811426879039,7.50881692280034E-10,
-0.783959930262008));
#52163=DIRECTION('ref_axis',(0.78386365533596,0.0156715280539164,-0.620735187541195));
#52164=DIRECTION('',(0.620811504614624,-1.36557432027502E-11,0.78395986870383));
#52165=DIRECTION('',(-0.998606990638996,-3.07807852448225E-8,-0.0527643653134219));
#52166=DIRECTION('center_axis',(-0.444353453098131,0.793626260382086,0.415580759361779));
#52167=DIRECTION('ref_axis',(-0.872542221931499,-0.488538709773179,-1.44217452160079E-16));
#52168=DIRECTION('center_axis',(0.0176157549639931,0.471546674566232,-0.881665139881677));
#52169=DIRECTION('ref_axis',(0.898990386289206,-0.393418648488291,-0.192452727653393));
#52170=DIRECTION('center_axis',(0.537306130849713,-0.601098528023407,0.591593341206106));
#52171=DIRECTION('ref_axis',(-0.741402943245098,-0.00227572516403292,0.671056254588603));
#52172=DIRECTION('',(-0.115363314589492,5.19500677922248E-12,0.993323364089925));
#52173=DIRECTION('center_axis',(0.,-1.,1.45983193964168E-32));
#52174=DIRECTION('ref_axis',(1.,0.,0.));
#52175=DIRECTION('center_axis',(-0.539828728548569,0.601098526995621,-0.589292376225359));
#52176=DIRECTION('ref_axis',(-0.739564117538253,-0.00432814660592568,0.673072197610942));
#52177=DIRECTION('center_axis',(-0.531677101688084,-0.601098528380341,-0.596657371294068));
#52178=DIRECTION('ref_axis',(-0.744933164574353,-0.00330175743698294,0.667130930713805));
#52179=DIRECTION('center_axis',(0.529123113241154,0.601098527640399,0.598923443440423));
#52180=DIRECTION('ref_axis',(-0.747776509741548,-0.00330191911101335,0.66394230834383));
#52181=DIRECTION('center_axis',(-0.595304362154782,0.584828255987947,-0.5509887724787));
#52182=DIRECTION('ref_axis',(-0.696201780475317,-0.0330815410697006,0.717083462717871));
#52183=DIRECTION('center_axis',(0.714196283526239,-1.08070422970347E-7,
0.699945475445978));
#52184=DIRECTION('ref_axis',(0.699859476888709,-0.015675163530811,-0.714108536468614));
#52185=DIRECTION('',(-0.714172445803004,-1.60982338570655E-12,-0.699969797673982));
#52186=DIRECTION('center_axis',(-0.570803912671749,0.584827952226411,-0.576332507822772));
#52187=DIRECTION('ref_axis',(-0.721774233899328,-0.0227607295851833,0.691754222587609));
#52188=DIRECTION('center_axis',(-0.668811664780684,5.92864469603341E-10,
-0.743431877883435));
#52189=DIRECTION('ref_axis',(0.743340325119513,0.0156933905087102,-0.668729301395982));
#52190=DIRECTION('',(0.668811722367516,-2.32591723654911E-11,0.743431826076741));
#52191=DIRECTION('',(-0.999949569924939,0.,0.010042788802444));
#52192=DIRECTION('center_axis',(0.607215618103716,-0.601098527827829,0.519586136241278));
#52193=DIRECTION('ref_axis',(-0.668178775416595,-0.0324816898727424,0.7432913721454));
#52194=DIRECTION('',(-0.0527643813501558,8.17238220606145E-12,0.998606989791647));
#52195=DIRECTION('center_axis',(0.,-1.,1.45983193964168E-32));
#52196=DIRECTION('ref_axis',(1.,0.,0.));
#52197=DIRECTION('center_axis',(-0.609429958764808,0.601098517802545,-0.516987134516428));
#52198=DIRECTION('ref_axis',(-0.666106973868854,-0.0345386499370693,0.745056092535188));
#52199=DIRECTION('center_axis',(-0.531677091111748,-0.601098532367363,-0.596657376701866));
#52200=DIRECTION('ref_axis',(-0.729167024598296,-0.0335099273449384,0.683514838908275));
#52201=DIRECTION('center_axis',(0.529123081475363,0.601098522341261,0.598923476822515));
#52202=DIRECTION('ref_axis',(-0.732080524449355,-0.0335101098726774,0.680393399628684));
#52203=DIRECTION('',(-0.756714656869205,4.44089209849579E-13,-0.653745308265628));
#52204=DIRECTION('center_axis',(-0.638536571159005,0.584827952146087,-0.500247252547293));
#52205=DIRECTION('ref_axis',(-0.645292296180387,-0.0526562728463764,0.762118868300852));
#52206=DIRECTION('center_axis',(-0.714172381807117,6.7742520729511E-10,
-0.699969862968364));
#52207=DIRECTION('ref_axis',(0.699882785675474,0.0157729998148926,-0.714083537684477));
#52208=DIRECTION('',(0.714172445804168,-1.75692793624375E-10,0.699969797672794));
#52209=DIRECTION('',(-0.997345805939016,0.,0.0728103246514788));
#52210=DIRECTION('',(0.0100427887670809,6.72270837774816E-11,0.999949569925294));
#52211=DIRECTION('center_axis',(0.,-1.,1.45983193964168E-32));
#52212=DIRECTION('ref_axis',(1.,0.,0.));
#52213=DIRECTION('center_axis',(-0.545499755366481,0.601098541294413,-0.584046710930588));
#52214=DIRECTION('ref_axis',(-0.7028616489713,0.051484846090818,0.70946093129104));
#52215=DIRECTION('center_axis',(0.657079473241136,0.60109853820579,0.454892419382884));
#52216=DIRECTION('ref_axis',(-0.60044923356296,0.0525164785306523,0.797936549730862));
#52217=DIRECTION('center_axis',(-0.600608226829493,0.584827930050726,-0.545202760537138));
#52218=DIRECTION('ref_axis',(-0.660160309869158,0.0219594825803943,0.750803667011729));
#52219=DIRECTION('center_axis',(0.796272582239159,-1.00169709512767E-8,
0.604937992503515));
#52220=DIRECTION('ref_axis',(0.604863059963878,-0.0157391393487521,-0.796173949701756));
#52221=DIRECTION('',(-0.796270460894404,-3.88578058618498E-13,-0.604940784793862));
#52222=DIRECTION('center_axis',(-0.576348241677965,0.584827952320902,-0.570788025889523));
#52223=DIRECTION('ref_axis',(-0.686575635047655,0.0322834330554533,0.726341295335095));
#52224=DIRECTION('center_axis',(-0.756714608220924,5.53608283030036E-10,
-0.653745364576342));
#52225=DIRECTION('ref_axis',(0.653664767416266,0.0157020800830109,-0.756621316458706));
#52226=DIRECTION('',(0.75671465686865,-8.32667268468213E-13,0.653745308266271));
#52227=DIRECTION('',(-0.990805973700979,0.,0.135290511413238));
#52228=DIRECTION('center_axis',(0.612209714621429,-0.601098528058252,0.513692344589007));
#52229=DIRECTION('ref_axis',(-0.629096561700259,0.0232723706551922,0.776978708087294));
#52230=DIRECTION('',(0.0728103246514612,1.43735365432664E-13,0.997345805939018));
#52231=DIRECTION('center_axis',(0.,-1.,1.45983193964168E-32));
#52232=DIRECTION('ref_axis',(1.,0.,0.));
#52233=DIRECTION('center_axis',(-0.614398801971386,0.601098533841799,-0.511072073928291));
#52234=DIRECTION('ref_axis',(-0.627005006672677,0.0212179807364959,0.778726215624504));
#52235=DIRECTION('center_axis',(-0.659016991795236,-0.601098524564669,-0.452080931129964));
#52236=DIRECTION('ref_axis',(-0.579262774122748,0.0222452995525509,0.814837275266317));
#52237=DIRECTION('center_axis',(0.657079518485687,0.60109853076028,0.454892363866938));
#52238=DIRECTION('ref_axis',(-0.582738672468509,0.0222451363282048,0.812355090781968));
#52239=DIRECTION('center_axis',(-0.664204781937783,0.584827953016243,-0.465626752906031));
#52240=DIRECTION('ref_axis',(-0.578633057240995,-0.00784645566470083,0.815550254859528));
#52241=DIRECTION('center_axis',(0.832683926477417,-7.28256137447449E-10,
0.553748569827636));
#52242=DIRECTION('ref_axis',(0.553680511340963,-0.0156778483074527,-0.832581585451935));
#52243=DIRECTION('',(-0.8326837491923,0.,-0.55374883641508));
#52244=DIRECTION('center_axis',(-0.6433422722591,0.58482795225408,-0.49405160356667));
#52245=DIRECTION('ref_axis',(-0.607659470213678,0.00246180457784726,0.794193872916338));
#52246=DIRECTION('center_axis',(-0.796270419146702,5.21210358149189E-10,
-0.604940839745454));
#52247=DIRECTION('ref_axis',(0.604866556891538,0.0156707406191342,-0.796172642234474));
#52248=DIRECTION('',(0.796270460894934,-6.33937347031928E-11,0.604940784793165));
#52249=DIRECTION('',(-0.980355882941021,1.64268989064092E-13,0.197236768334231));
#52250=DIRECTION('center_axis',(0.671764979565829,-0.601098528057821,0.432911505732573));
#52251=DIRECTION('ref_axis',(-0.546052527331169,-0.00691952331713121,0.837722363072818));
#52252=DIRECTION('',(0.13529051140086,2.3613667178499E-11,0.990805973702669));
#52253=DIRECTION('center_axis',(-0.717325884960116,0.584827952229979,-0.378708121191871));
#52254=DIRECTION('ref_axis',(-0.478331876855593,-0.0181546317001112,0.877991472015326));
#52255=DIRECTION('center_axis',(0.865810846544381,-4.91898929192996E-10,
0.500371440038401));
#52256=DIRECTION('ref_axis',(0.500309928860263,-0.0156795066183271,-0.865704411537821));
#52257=DIRECTION('',(-0.865810813532527,2.06171160586968E-7,-0.500371497159962));
#52258=DIRECTION('center_axis',(-0.700193645032136,0.584827782588847,-0.409518405164925));
#52259=DIRECTION('ref_axis',(-0.521594170261362,-0.0273551035144114,0.852755076127417));
#52260=DIRECTION('center_axis',(-0.832683698962267,7.12366036531364E-10,
-0.553748911947027));
#52261=DIRECTION('ref_axis',(0.553680640722956,0.0157023279285975,-0.83258103808953));
#52262=DIRECTION('',(-0.83268374860965,-1.29267411567854E-5,-0.553748837140342));
#52263=DIRECTION('center_axis',(0.865810815155372,-1.00468440339018E-11,
0.500371494351937));
#52264=DIRECTION('ref_axis',(0.386224871041075,-0.635772805085301,-0.668298802410474));
#52265=DIRECTION('',(-0.197236768333327,0.,-0.980355882941203));
#52266=DIRECTION('center_axis',(0.,-1.,1.45983193964168E-32));
#52267=DIRECTION('ref_axis',(1.,0.,0.));
#52268=DIRECTION('center_axis',(-0.673608428738637,0.601098525416304,-0.430037495428723));
#52269=DIRECTION('ref_axis',(-0.543756029387751,-0.00897218398747796,0.83919537678598));
#52270=DIRECTION('center_axis',(-0.659016985594954,-0.601098529035859,-0.452080934223361));
#52271=DIRECTION('ref_axis',(-0.56072842327227,-0.00794565772609306,0.827961654823394));
#52272=DIRECTION('center_axis',(0.657079502595968,0.601098526821226,0.454892392024299));
#52273=DIRECTION('ref_axis',(-0.564260575522972,-0.00794583663500264,0.825558517968687));
#52274=DIRECTION('',(-0.966036765128978,-7.62629077544845E-8,0.258404660211721));
#52275=DIRECTION('center_axis',(-0.820017152393108,0.398564395010779,-0.410753323554162));
#52276=DIRECTION('ref_axis',(-0.447863103182219,-5.76011272065838E-16,0.894102142267869));
#52277=DIRECTION('center_axis',(0.898612168814772,5.74456501979234E-5,0.438743850963189));
#52278=DIRECTION('ref_axis',(0.438743841499205,-0.000363186155216258,-0.898612101878412));
#52279=DIRECTION('',(-0.895520512893129,5.94973688026089E-5,-0.445020232627338));
#52280=DIRECTION('center_axis',(-0.6914084161041,0.590180063979457,-0.416703604761975));
#52281=DIRECTION('ref_axis',(0.584945575469874,0.795818476300859,0.156561893564165));
#52282=DIRECTION('center_axis',(-0.651774153934771,0.550037558029746,0.52215815326325));
#52283=DIRECTION('ref_axis',(-0.644941563435971,-0.764231888730616,1.41890158173865E-16));
#52284=DIRECTION('center_axis',(-0.279966610619734,-0.477126089615033,-0.833048252832191));
#52285=DIRECTION('ref_axis',(0.95891877528538,-0.0976282465771925,-0.266352225212124));
#52286=DIRECTION('center_axis',(-0.350675851952374,0.584827951390166,-0.731438797255285));
#52287=DIRECTION('ref_axis',(-0.89296426791565,0.0265489689935778,0.449343931161027));
#52288=DIRECTION('center_axis',(0.517659993435585,-2.35082575115718E-11,
0.85558642532258));
#52289=DIRECTION('ref_axis',(0.855480329378303,-0.0157477670555638,-0.517595801644058));
#52290=DIRECTION('center_axis',(-0.470963348342342,-0.000115441184994627,
-0.882152770891473));
#52291=DIRECTION('ref_axis',(0.0218910266942953,0.99969051108519,-0.0118179946057292));
#52292=DIRECTION('',(0.462915795316803,-6.06958927296742E-10,0.886402259950984));
#52293=DIRECTION('center_axis',(0.37330239356122,-0.601098528356447,0.706629947121673));
#52294=DIRECTION('ref_axis',(-0.873849503844342,0.0279220061610186,0.485394073102404));
#52295=DIRECTION('',(-0.299450151004041,2.24350371841882E-10,0.954111946819479));
#52296=DIRECTION('center_axis',(0.,-1.,1.45983193964168E-32));
#52297=DIRECTION('ref_axis',(1.,0.,0.));
#52298=DIRECTION('center_axis',(-0.376317949464262,0.601098535010339,-0.705028617943582));
#52299=DIRECTION('ref_axis',(-0.872572092162209,0.0258666949039728,0.487800018526456));
#52300=DIRECTION('center_axis',(-0.452703687647038,-0.601098523524197,-0.658589353245103));
#52301=DIRECTION('ref_axis',(-0.835078627465076,0.0268944746709312,0.549472813870913));
#52302=DIRECTION('center_axis',(0.449885809662912,0.601098531270677,0.660517459245539));
#52303=DIRECTION('ref_axis',(-0.837418496166001,0.0268943050251962,0.545900136138731));
#52304=DIRECTION('center_axis',(-0.439584272333921,0.584827952222756,-0.68171983528103));
#52305=DIRECTION('ref_axis',(-0.841696291922646,-0.00326197147019357,0.539941396547621));
#52306=DIRECTION('center_axis',(0.570361301697443,-7.08808782319137E-10,
0.821393928347415));
#52307=DIRECTION('ref_axis',(0.821292905716089,-0.0156832196307858,-0.570291153396611));
#52308=DIRECTION('',(-0.570361226402818,8.3214818921328E-8,-0.821393980630651));
#52309=DIRECTION('center_axis',(-0.40954514820993,0.58482796993091,-0.700177846810506));
#52310=DIRECTION('ref_axis',(-0.860586784796277,0.00704480137018753,0.509255099736528));
#52311=DIRECTION('center_axis',(-0.517659939546137,4.83271880986753E-10,
-0.855586457927596));
#52312=DIRECTION('ref_axis',(0.855481386835343,0.0156715280552529,-0.517596367826022));
#52313=DIRECTION('',(0.517659995144269,-1.48214773786002E-11,0.855586424288766));
#52314=DIRECTION('',(-0.984119547726674,-3.07809289801987E-8,-0.177506945729585));
#52315=DIRECTION('center_axis',(-0.492935673776194,0.79362626038218,0.356611525824118));
#52316=DIRECTION('ref_axis',(-0.849477030546853,-0.527625600756161,-4.09521487904968E-16));
#52317=DIRECTION('center_axis',(0.127978792334609,0.47154667454649,-0.872505107398646));
#52318=DIRECTION('ref_axis',(0.916024775580547,-0.393413511721289,-0.078258669281638));
#52319=DIRECTION('center_axis',(0.458922996999573,-0.601098528053855,0.654270771467302));
#52320=DIRECTION('ref_axis',(-0.819662414427714,-0.00227571922525397,0.572842340855264));
#52321=DIRECTION('',(-0.238950069592984,5.051271413789E-12,0.971031855420567));
#52322=DIRECTION('center_axis',(0.,-1.,1.45983193964168E-32));
#52323=DIRECTION('ref_axis',(1.,0.,0.));
#52324=DIRECTION('center_axis',(-0.461714089613293,0.601098527038454,-0.652304116378833));
#52325=DIRECTION('ref_axis',(-0.818090753690027,-0.00432813989567482,0.575072852716877));
#52326=DIRECTION('center_axis',(-0.452703668569484,-0.601098528371206,-0.658589361934811));
#52327=DIRECTION('ref_axis',(-0.822672822304874,-0.00330175941561732,0.56850551960882));
#52328=DIRECTION('center_axis',(0.449885812549619,0.601098527660819,0.660517460564492));
#52329=DIRECTION('ref_axis',(-0.825094102333532,-0.00330191552492792,0.564985680923233));
#52330=DIRECTION('center_axis',(-0.521553004948764,0.584828255987703,-0.621255482090336));
#52331=DIRECTION('ref_axis',(-0.780586410601624,-0.0330815410779919,0.624171825080224));
#52332=DIRECTION('center_axis',(0.620838225739205,-1.08300056263464E-7,
0.783938707719541));
#52333=DIRECTION('ref_axis',(0.783842389664105,-0.0156751635317241,-0.620761949070591));
#52334=DIRECTION('',(-0.620811504614934,1.16573417585605E-12,-0.783959868703585));
#52335=DIRECTION('center_axis',(-0.49406933650575,0.584827952226459,-0.643328653970406));
#52336=DIRECTION('ref_axis',(-0.802782622036335,-0.0227607295775255,0.595837235279539));
#52337=DIRECTION('center_axis',(-0.570361157887498,6.48541563533731E-10,
-0.821394028206459));
#52338=DIRECTION('ref_axis',(0.821292874494091,0.0156933905080219,-0.570290918566652));
#52339=DIRECTION('',(0.570361227475292,-2.28150831556906E-11,0.821393979885949));
#52340=DIRECTION('',(-0.993323364090245,0.,-0.115363314586734));
#52341=DIRECTION('center_axis',(0.537306131419502,-0.601098527806004,0.5915933409095));
#52342=DIRECTION('ref_axis',(-0.756069097064001,-0.0324816901882255,0.653685291457092));
#52343=DIRECTION('',(-0.177506961533698,8.00811321699377E-12,0.984119544876065));
#52344=DIRECTION('center_axis',(0.,-1.,1.45983193964168E-32));
#52345=DIRECTION('ref_axis',(1.,0.,0.));
#52346=DIRECTION('center_axis',(-0.53982874725037,0.601098518028139,-0.589292368240478));
#52347=DIRECTION('ref_axis',(-0.754234814257284,-0.0345386459730884,0.655695757876034));
#52348=DIRECTION('center_axis',(-0.45270365302585,-0.601098532080463,-0.658589369233792));
#52349=DIRECTION('ref_axis',(-0.809084453718785,-0.0335099325942185,0.58673625349735));
#52350=DIRECTION('center_axis',(0.449885781508012,0.601098522737911,0.660517486187328));
#52351=DIRECTION('ref_axis',(-0.811583750412878,-0.0335101027780247,0.583274282887196));
#52352=DIRECTION('',(-0.668811722367349,-3.8857805861924E-13,-0.743431826076891));
#52353=DIRECTION('center_axis',(-0.570803913814109,0.58482795214713,-0.57633250677182));
#52354=DIRECTION('ref_axis',(-0.735722795822873,-0.0526562728337489,0.67523276330302));
#52355=DIRECTION('center_axis',(-0.620811448742737,5.19037977403783E-10,
-0.783959912948324));
#52356=DIRECTION('ref_axis',(0.783862387164722,0.0157729998154696,-0.620734218861216));
#52357=DIRECTION('',(0.620811504616689,-1.78523862336725E-10,0.783959868702195));
#52358=DIRECTION('',(-0.99860698979188,0.,-0.0527643813457488));
#52359=DIRECTION('',(-0.115363314620757,6.51326541667565E-11,0.993323364086294));
#52360=DIRECTION('center_axis',(0.,-1.,1.45983193964168E-32));
#52361=DIRECTION('ref_axis',(1.,0.,0.));
#52362=DIRECTION('center_axis',(-0.467997860236714,0.60109854104577,-0.647810579387605));
#52363=DIRECTION('ref_axis',(-0.786238409799018,0.0514848489886549,0.61577469360256));
#52364=DIRECTION('center_axis',(0.594885072803049,0.601098537808415,0.533659346400581));
#52365=DIRECTION('ref_axis',(-0.69572247542785,0.0525164831338593,0.716388341741961));
#52366=DIRECTION('center_axis',(-0.52754022664394,0.584827930050739,-0.616179845098027));
#52367=DIRECTION('ref_axis',(-0.749055400002377,0.0219594825787594,0.662143329538366));
#52368=DIRECTION('center_axis',(0.714174875099444,-9.73286011102838E-9,
0.699967319077608));
#52369=DIRECTION('ref_axis',(0.699880615468601,-0.0157391393466766,-0.714086411846577));
#52370=DIRECTION('',(-0.714172445802862,1.16573417585578E-12,-0.699969797674127));
#52371=DIRECTION('center_axis',(-0.500264854685563,0.584827952321108,-0.638522780604054));
#52372=DIRECTION('ref_axis',(-0.772196484307766,0.032283433051883,0.634563132850554));
#52373=DIRECTION('center_axis',(-0.668811663975281,5.85773660908862E-10,
-0.743431878607998));
#52374=DIRECTION('ref_axis',(0.743340224422381,0.0157020800826207,-0.668729209349168));
#52375=DIRECTION('',(0.668811722367304,-3.88578058619029E-13,0.743431826076931));
#52376=DIRECTION('',(-0.999949569924938,0.,0.0100427888025238));
#52377=DIRECTION('center_axis',(0.542999531328701,-0.601098527924313,0.586371954227037));
#52378=DIRECTION('ref_axis',(-0.721517204487967,0.0232723741764296,0.692005289161912));
#52379=DIRECTION('',(-0.0527643813459068,0.,0.998606989791872));
#52380=DIRECTION('center_axis',(0.,-1.,1.45983193964168E-32));
#52381=DIRECTION('ref_axis',(1.,0.,0.));
#52382=DIRECTION('center_axis',(-0.545499761809049,0.601098533647117,-0.584046712783795));
#52383=DIRECTION('ref_axis',(-0.719661164504588,0.0212179861508259,0.694001156603938));
#52384=DIRECTION('center_axis',(-0.597159676907081,-0.601098524704973,-0.531112873006986));
#52385=DIRECTION('ref_axis',(-0.676821308316238,0.0222452958767956,0.73581116016302));
#52386=DIRECTION('center_axis',(0.594885119307456,0.601098530760866,0.533659302498965));
#52387=DIRECTION('ref_axis',(-0.67995869433305,0.0222451362999726,0.732912906089046));
#52388=DIRECTION('center_axis',(-0.600608822257759,0.584827953016275,-0.545202079963881));
#52389=DIRECTION('ref_axis',(-0.676285913340346,-0.00784645565583719,0.736597445387272));
#52390=DIRECTION('center_axis',(0.756714871630385,-7.93392647660612E-10,
0.653745059678014));
#52391=DIRECTION('ref_axis',(0.65366471112118,-0.0156778483085135,-0.756621867584647));
#52392=DIRECTION('',(-0.756714656868892,3.88578058618794E-13,-0.65374530826599));
#52393=DIRECTION('center_axis',(-0.576348241270836,0.58482795225427,-0.57078802636889));
#52394=DIRECTION('ref_axis',(-0.702406779954916,0.00246180457067037,0.711771490712871));
#52395=DIRECTION('center_axis',(-0.714172408549139,3.97521702241774E-10,
-0.699969835683739));
#52396=DIRECTION('ref_axis',(0.699883883875737,0.0156707406191022,-0.714084712747348));
#52397=DIRECTION('',(0.714172445802881,-6.46149800301959E-11,0.699969797674108));
#52398=DIRECTION('',(-0.997345805939002,1.64268989064134E-13,0.0728103246516758));
#52399=DIRECTION('center_axis',(0.612209720657188,-0.601098527971134,0.513692337497635));
#52400=DIRECTION('ref_axis',(-0.646741185585192,-0.00691953024425702,0.762678149004584));
#52401=DIRECTION('',(0.0100427887901276,2.35931335548657E-11,0.999949569925062));
#52402=DIRECTION('center_axis',(0.,-1.,1.45983193964168E-32));
#52403=DIRECTION('ref_axis',(1.,0.,0.));
#52404=DIRECTION('center_axis',(-0.614398828791068,0.601098525500061,-0.511072051497454));
#52405=DIRECTION('ref_axis',(-0.644647426983502,-0.00897217798432998,0.764427364048258));
#52406=DIRECTION('center_axis',(-0.597159673304864,-0.601098529024544,-0.531112872168391));
#52407=DIRECTION('ref_axis',(-0.660078024723387,-0.00794565881973064,0.751155022470856));
#52408=DIRECTION('center_axis',(0.594885098139866,0.601098526797091,0.533659330559758));
#52409=DIRECTION('ref_axis',(-0.663281132608099,-0.00794583835980365,0.748328138438531));
#52410=DIRECTION('center_axis',(-0.664204842698312,0.584827952230054,-0.465626667220115));
#52411=DIRECTION('ref_axis',(-0.584601597363002,-0.0181546317022303,0.811117366173591));
#52412=DIRECTION('center_axis',(0.796270423924654,4.79391517388211E-10,
0.60494083345634));
#52413=DIRECTION('ref_axis',(0.604866467468704,-0.0156795066158151,-0.796172537584797));
#52414=DIRECTION('',(-0.796270458940246,2.06171937743057E-7,-0.604940787366042));
#52415=DIRECTION('center_axis',(-0.643346147146909,0.584827782537135,-0.494046758641251));
#52416=DIRECTION('ref_axis',(-0.624359791305129,-0.0273551073958671,0.780657766950907));
#52417=DIRECTION('center_axis',(-0.756714597939265,5.92328891388393E-10,
-0.65374537647743));
#52418=DIRECTION('ref_axis',(0.65366477677188,0.0157023279245459,-0.756621303232679));
#52419=DIRECTION('',(-0.756714656199794,-1.29267412633769E-5,-0.653745308912674));
#52420=DIRECTION('',(-0.990805968327174,-7.6263051489871E-8,0.135290550768501));
#52421=DIRECTION('center_axis',(0.796270460902336,-1.03532362406177E-11,
0.604940784783422));
#52422=DIRECTION('ref_axis',(0.466939422466012,-0.635772805085451,-0.614622254771892));
#52423=DIRECTION('',(-0.0728103246508497,0.,-0.997345805939062));
#52424=DIRECTION('center_axis',(-0.762070031246047,0.398564391552654,-0.510289813011108));
#52425=DIRECTION('ref_axis',(-0.556392281443859,9.44692024466823E-17,0.830919748922661));
#52426=DIRECTION('center_axis',(0.83653715793225,5.74456598775067E-5,0.547910193461146));
#52427=DIRECTION('ref_axis',(0.547910175655507,-0.0003633645381878,-0.836537092650029));
#52428=DIRECTION('',(-0.832683241412774,5.94973691934172E-5,-0.553749596776718));
#52429=DIRECTION('center_axis',(-0.633729640882618,0.59018006380588,-0.500074229042925));
#52430=DIRECTION('ref_axis',(0.560699752632307,0.795821258487725,0.228657630393309));
#52431=DIRECTION('center_axis',(-0.712078489837049,0.550037558028519,0.436351817997143));
#52432=DIRECTION('ref_axis',(-0.611304898379798,-0.791395173865032,-8.76719162497403E-17));
#52433=DIRECTION('center_axis',(-0.173350358948395,-0.477126090400623,-0.861568538719631));
#52434=DIRECTION('ref_axis',(0.984740390653664,-0.0976174117503724,-0.144073605974262));
#52435=DIRECTION('center_axis',(-0.256237078487173,0.58482795138957,-0.769622522332758));
#52436=DIRECTION('ref_axis',(-0.94224070582697,0.0265489690038872,0.333882620882736));
#52437=DIRECTION('center_axis',(0.406344677055198,-1.12068438201966E-11,
0.913719871420616));
#52438=DIRECTION('ref_axis',(0.913606566709862,-0.0157477670552894,-0.406294288782639));
#52439=DIRECTION('center_axis',(-0.356686602128754,-0.00011544118293406,
-0.934224092247239));
#52440=DIRECTION('ref_axis',(0.0231987777512836,0.999690532904092,-0.00898082027316364));
#52441=DIRECTION('',(0.348169904526055,-6.07736083413689E-10,0.937431446870819));
#52442=DIRECTION('center_axis',(0.281794559405976,-0.601098527852825,0.747845161849937));
#52443=DIRECTION('ref_axis',(-0.927794953421368,0.0279220172196599,0.372044198127354));
#52444=DIRECTION('',(-0.416670832598985,2.2420663647639E-10,0.909057433422811));
#52445=DIRECTION('center_axis',(0.,-1.,1.45983193964168E-32));
#52446=DIRECTION('ref_axis',(1.,0.,0.));
#52447=DIRECTION('center_axis',(-0.284987050396032,0.601098534917648,-0.746634403457561));
#52448=DIRECTION('ref_axis',(-0.926829155228736,0.0258666969731542,0.374591285277283));
#52449=DIRECTION('center_axis',(-0.366590846799548,-0.601098523644121,-0.710134998374005));
#52450=DIRECTION('ref_axis',(-0.897360989139196,0.0268944721096581,0.440476948932707));
#52451=DIRECTION('center_axis',(0.36355353887101,0.601098531205687,0.711694723991074));
#52452=DIRECTION('ref_axis',(-0.899234629581645,0.0268943064871736,0.43663918426973));
#52453=DIRECTION('center_axis',(-0.350675867677086,0.584827952222683,-0.731438789050694));
#52454=DIRECTION('ref_axis',(-0.902731866435013,-0.00326197144967307,0.430191279392108));
#52455=DIRECTION('center_axis',(0.462915873277324,-6.89120218774699E-10,
0.886402219236782));
#52456=DIRECTION('ref_axis',(0.886293201285704,-0.0156832196313558,-0.462858939609827));
#52457=DIRECTION('',(-0.462915794151209,8.32139862540845E-8,-0.886402260559701));
#52458=DIRECTION('center_axis',(-0.318560208793917,0.584827969931273,-0.745986353065016));
#52459=DIRECTION('ref_axis',(-0.917627389307625,0.0070448013615417,0.397379346678018));
#52460=DIRECTION('center_axis',(-0.406344585065271,7.73278930637216E-10,
-0.913719912329885));
#52461=DIRECTION('ref_axis',(0.913607702105341,0.0156715280544491,-0.406294683526916));
#52462=DIRECTION('',(0.406344678314967,-1.565414464706E-11,0.913719870860378));
#52463=DIRECTION('',(-0.954111951662124,-3.07809289802008E-8,-0.299450135574341));
#52464=DIRECTION('center_axis',(-0.533744004413321,0.793626260382327,0.292018315494759));
#52465=DIRECTION('ref_axis',(-0.829794751147533,-0.558068697355446,-2.23533872199617E-16));
#52466=DIRECTION('center_axis',(0.23632352768933,0.471546674520354,-0.849585148180726));
#52467=DIRECTION('ref_axis',(0.918610213450041,-0.393413126094722,0.0371670278829099));
#52468=DIRECTION('center_axis',(0.373302383932541,-0.601098528045228,0.706629952473105));
#52469=DIRECTION('ref_axis',(-0.884995312998488,-0.00227572143390278,0.465594369663835));
#52470=DIRECTION('',(-0.358768439257086,5.19500677922277E-12,0.933426594324928));
#52471=DIRECTION('center_axis',(0.,-1.,1.45983193964168E-32));
#52472=DIRECTION('ref_axis',(1.,0.,0.));
#52473=DIRECTION('center_axis',(-0.376317948744125,0.601098527048046,-0.705028625116515));
#52474=DIRECTION('ref_axis',(-0.883715605272235,-0.00432813772470444,0.468004269448648));
#52475=DIRECTION('center_axis',(-0.366590819735879,-0.601098528339074,-0.710135008370927));
#52476=DIRECTION('ref_axis',(-0.887438440940119,-0.00330176677718059,0.460914430103811));
#52477=DIRECTION('center_axis',(0.363553538492343,0.601098527658307,0.71169472718063));
#52478=DIRECTION('ref_axis',(-0.889399471565693,-0.00330191612723909,0.457118887521128));
#52479=DIRECTION('center_axis',(-0.439576445278285,0.584828255987864,-0.6817246216433));
#52480=DIRECTION('ref_axis',(-0.852660726744351,-0.0330815410735374,0.521416624886467));
#52481=DIRECTION('center_axis',(0.517689131149895,-1.08056920685984E-7,
0.855568795298926));
#52482=DIRECTION('ref_axis',(0.855463676738608,-0.0156751635310533,-0.517625527798946));
#52483=DIRECTION('',(-0.517659995144338,0.,-0.855586424288724));
#52484=DIRECTION('center_axis',(-0.409542991772211,0.584827952226587,-0.700179122928358));
#52485=DIRECTION('ref_axis',(-0.871130648656311,-0.0227607295796337,0.490523538844608));
#52486=DIRECTION('center_axis',(-0.462915703310323,7.97913436906672E-10,
-0.886402308000554));
#52487=DIRECTION('ref_axis',(0.886293148594207,0.0156933905085995,-0.462858695769359));
#52488=DIRECTION('',(0.4629157953087,-2.3259172365528E-11,0.886402259955216));
#52489=DIRECTION('',(-0.971031855421177,0.,-0.238950069590505));
#52490=DIRECTION('center_axis',(0.458923001955571,-0.601098527953781,0.654270768082974));
#52491=DIRECTION('ref_axis',(-0.83203575979251,-0.0324816874711891,0.553770199997729));
#52492=DIRECTION('',(-0.299450150896404,8.00811321699499E-12,0.954111946853262));
#52493=DIRECTION('center_axis',(0.,-1.,1.45983193964168E-32));
#52494=DIRECTION('ref_axis',(1.,0.,0.));
#52495=DIRECTION('center_axis',(-0.461714116117164,0.601098518117668,-0.652304105839362));
#52496=DIRECTION('ref_axis',(-0.830467918261611,-0.0345386443924794,0.555994711109518));
#52497=DIRECTION('center_axis',(-0.366590812751239,-0.601098532026415,-0.710135008855412));
#52498=DIRECTION('ref_axis',(-0.876242133670582,-0.0335099336422242,0.480704490854536));
#52499=DIRECTION('center_axis',(0.363553507319193,0.601098522813485,0.711694747196689));
#52500=DIRECTION('ref_axis',(-0.878287821258083,-0.033510101446702,0.476956576776924));
#52501=DIRECTION('',(-0.570361227475679,-3.88578058618649E-13,-0.82139397988568));
#52502=DIRECTION('center_axis',(-0.494069337794621,0.584827952146325,-0.643328653053415));
#52503=DIRECTION('ref_axis',(-0.814550507452863,-0.0526562728431611,0.57769783428584));
#52504=DIRECTION('center_axis',(-0.517659889573965,9.29479950426669E-10,
-0.855586488162518));
#52505=DIRECTION('ref_axis',(0.855480051928071,0.015772999815068,-0.517595491894953));
#52506=DIRECTION('',(0.517659995146304,-1.77302617009957E-10,0.855586424287534));
#52507=DIRECTION('',(-0.98411954487684,0.,-0.177506961529406));
#52508=DIRECTION('',(-0.238950069624714,6.73708191429337E-11,0.971031855412758));
#52509=DIRECTION('center_axis',(0.,-1.,1.45983193964168E-32));
#52510=DIRECTION('ref_axis',(1.,0.,0.));
#52511=DIRECTION('center_axis',(-0.383115352763055,0.601098540442394,-0.701358090532407));
#52512=DIRECTION('ref_axis',(-0.857215723028873,0.0514848559344195,0.512377315853756));
#52513=DIRECTION('center_axis',(0.523308968761393,0.601098538211298,0.604010157674628));
#52514=DIRECTION('ref_axis',(-0.780023767323197,0.0525164784582637,0.623542253501132));
#52515=DIRECTION('center_axis',(-0.446152601960881,0.584827930051338,-0.677439405404943));
#52516=DIRECTION('ref_axis',(-0.826137439006878,0.0219594825671946,0.563040596224232));
#52517=DIRECTION('center_axis',(0.620814204536648,-9.52273684387182E-9,
0.783957730649765));
#52518=DIRECTION('ref_axis',(0.783860623339077,-0.0157391393472892,-0.620737305686617));
#52519=DIRECTION('',(-0.620811504615104,-1.60982338570751E-12,-0.78395986870345));
#52520=DIRECTION('center_axis',(-0.416291992083781,0.584827952321421,-0.696187649639414));
#52521=DIRECTION('ref_axis',(-0.8456393337275,0.0322834330537012,0.532777530685349));
#52522=DIRECTION('center_axis',(-0.570361157976486,6.33614257171157E-10,
-0.821394028144667));
#52523=DIRECTION('ref_axis',(0.821292762374769,0.0157020800825937,-0.570290840845179));
#52524=DIRECTION('',(0.570361227475211,-1.99840144432419E-12,0.821393979886005));
#52525=DIRECTION('',(-0.99332336409025,0.,-0.115363314586692));
#52526=DIRECTION('center_axis',(0.46522593544058,-0.601098528225849,0.649804115374899));
#52527=DIRECTION('ref_axis',(-0.802559080156761,0.0232723661732835,0.596118545115508));
#52528=DIRECTION('',(-0.177506961529595,0.,0.984119544876806));
#52529=DIRECTION('center_axis',(0.,-1.,1.45983193964168E-32));
#52530=DIRECTION('ref_axis',(1.,0.,0.));
#52531=DIRECTION('center_axis',(-0.4679978757003,0.601098533795021,-0.64781057494416));
#52532=DIRECTION('ref_axis',(-0.800967827107389,0.0212179820057374,0.59833129383183));
#52533=DIRECTION('center_axis',(-0.525884798108242,-0.60109852478409,-0.601768844840812));
#52534=DIRECTION('ref_axis',(-0.763705963940892,0.022245293807787,0.64518086421136));
#52535=DIRECTION('center_axis',(0.523309032241945,0.601098530594663,0.604010110255562));
#52536=DIRECTION('ref_axis',(-0.76645535742454,0.0222451408421469,0.641912251623331));
#52537=DIRECTION('center_axis',(-0.527540902698841,0.584827953016229,-0.616179244498335));
#52538=DIRECTION('ref_axis',(-0.763273336564778,-0.00784645567575521,0.646028054207091));
#52539=DIRECTION('center_axis',(0.668811959513174,-7.18937375996525E-10,
0.743431612733914));
#52540=DIRECTION('ref_axis',(0.743340241251659,-0.0156778483086904,-0.668729759176556));
#52541=DIRECTION('',(-0.668811722367591,3.88578058618546E-13,-0.743431826076673));
#52542=DIRECTION('center_axis',(-0.500264854224869,0.584827952254413,-0.638522781026082));
#52543=DIRECTION('ref_axis',(-0.786076715181059,0.00246180456478883,0.618124046910036));
#52544=DIRECTION('center_axis',(-0.620811426908302,7.56581079087839E-10,
-0.783959930238834));
#52545=DIRECTION('ref_axis',(0.783863664988098,0.0156707406189149,-0.620735195232138));
#52546=DIRECTION('',(0.620811504615392,-6.42264019716503E-11,0.783959868703222));
#52547=DIRECTION('',(-0.998606989791874,1.64268989064165E-13,-0.0527643813458644));
#52548=DIRECTION('center_axis',(0.542999531338148,-0.601098528084606,0.586371954053971));
#52549=DIRECTION('ref_axis',(-0.737230364923761,-0.00691952120981509,0.675606031101414));
#52550=DIRECTION('',(-0.115363314599122,2.37574025439407E-11,0.993323364088807));
#52551=DIRECTION('center_axis',(0.,-1.,1.45983193964168E-32));
#52552=DIRECTION('ref_axis',(1.,0.,0.));
#52553=DIRECTION('center_axis',(-0.545499785857832,0.601098525638433,-0.584046698564731));
#52554=DIRECTION('ref_axis',(-0.735372351633788,-0.00897216828780553,0.677603870007254));
#52555=DIRECTION('center_axis',(-0.525884793701434,-0.601098528988418,-0.601768844492269));
#52556=DIRECTION('ref_axis',(-0.749017802714225,-0.00794566167936899,0.662502224658628));
#52557=DIRECTION('center_axis',(0.523309006927691,0.601098526850466,0.604010135913755));
#52558=DIRECTION('ref_axis',(-0.751841344649372,-0.00794583436748203,0.659296182449155));
#52559=DIRECTION('center_axis',(-0.600608893317819,0.584827952228866,-0.545202002526895));
#52560=DIRECTION('ref_axis',(-0.6816518014331,-0.0181546317269892,0.731451454950954));
#52561=DIRECTION('center_axis',(0.714172486918624,-4.60209657606995E-10,
0.699969755724109));
#52562=DIRECTION('ref_axis',(0.699883707722976,-0.0156795066181786,-0.714084692971464));
#52563=DIRECTION('',(-0.714172443541281,2.06170660986742E-7,-0.699969799981566));
#52564=DIRECTION('center_axis',(-0.576352692830911,0.584827782537096,-0.570783705302894));
#52565=DIRECTION('ref_axis',(-0.717278890098503,-0.0273551073999281,0.696249015739483));
#52566=DIRECTION('center_axis',(-0.668811641026249,7.44449369156047E-10,
-0.743431899253574));
#52567=DIRECTION('ref_axis',(0.743340242173521,0.0157023279256583,-0.66872918379799));
#52568=DIRECTION('',(-0.668811721622572,-1.29267404107118E-5,-0.743431826634528));
#52569=DIRECTION('',(-0.999949569526027,-7.62629077545172E-8,0.0100428285212935));
#52570=DIRECTION('center_axis',(0.714172445812284,-1.09814043632675E-11,
0.699969797664514));
#52571=DIRECTION('ref_axis',(0.540290060262428,-0.635772805085269,-0.551252747018671));
#52572=DIRECTION('',(0.0527643813464523,0.,-0.998606989791843));
#52573=DIRECTION('center_axis',(-0.692104609109857,0.398564391554928,-0.60177872663741));
#52574=DIRECTION('ref_axis',(-0.656146821083495,2.49882806495788E-16,0.754633254754933));
#52575=DIRECTION('center_axis',(0.76126945630972,5.74456474002762E-5,0.648435664958292));
#52576=DIRECTION('ref_axis',(0.648435639152938,-0.000363146004023474,-0.761269393842482));
#52577=DIRECTION('',(-0.756714057795,5.94973699394661E-5,-0.653745998990042));
#52578=DIRECTION('center_axis',(-0.566056573296636,0.590180063808837,-0.575558379411044));
#52579=DIRECTION('ref_axis',(0.527623534722438,0.795820516823244,0.297124739141971));
#52580=DIRECTION('center_axis',(-0.761152922577171,0.550037558029868,0.343663953897947));
#52581=DIRECTION('ref_axis',(-0.585711678833674,-0.81051948112173,-3.01370648851509E-16));
#52582=DIRECTION('center_axis',(-0.0640002687006948,-0.477126090261306,
-0.876501374555796));
#52583=DIRECTION('ref_axis',(0.995031847779778,-0.0976263647563779,-0.0195119145245918));
#52584=DIRECTION('center_axis',(-0.157757293237268,0.584827951389508,-0.795668840475736));
#52585=DIRECTION('ref_axis',(-0.97665744493467,0.0265489690060458,0.213155782230737));
#52586=DIRECTION('center_axis',(0.288621060453656,-9.51818097282618E-12,
0.957443410057538));
#52587=DIRECTION('ref_axis',(0.957324683463083,-0.015747767055969,-0.288585270353598));
#52588=DIRECTION('center_axis',(-0.236784693339787,-0.00011544116316845,
-0.971562141951466));
#52589=DIRECTION('ref_axis',(0.0241339308308979,0.999690725296098,-0.00600059493807027));
#52590=DIRECTION('',(0.227933166354572,-6.0612626002843E-10,0.973676779879021));
#52591=DIRECTION('center_axis',(0.185842683821483,-0.601098528165775,0.777266399831465));
#52592=DIRECTION('ref_axis',(-0.967108513356064,0.0279220103706326,0.252826985765141));
#52593=DIRECTION('',(-0.527320366256967,2.24206636476404E-10,0.849666541256403));
#52594=DIRECTION('center_axis',(0.,-1.,1.45983193964168E-32));
#52595=DIRECTION('ref_axis',(1.,0.,0.));
#52596=DIRECTION('center_axis',(-0.189161725627372,0.601098534572865,-0.776465320083279));
#52597=DIRECTION('ref_axis',(-0.966469570041807,0.025866704851165,0.255475015927873));
#52598=DIRECTION('center_axis',(-0.274696652837102,-0.601098523645616,-0.750481388037807));
#52599=DIRECTION('ref_axis',(-0.94549143003686,0.0268944720827181,0.324534502169254));
#52600=DIRECTION('center_axis',(0.271487805717504,0.601098531311225,0.751648140423551));
#52601=DIRECTION('ref_axis',(-0.946869297906245,0.0268943040459628,0.320492166975135));
#52602=DIRECTION('center_axis',(-0.256237095134423,0.584827952222713,-0.769622516157149));
#52603=DIRECTION('ref_axis',(-0.949530820132141,-0.00326197145096664,0.313656788801768));
#52604=DIRECTION('center_axis',(0.348169990616235,-7.19927070234003E-10,
0.9374314148962));
#52605=DIRECTION('ref_axis',(0.937316120903577,-0.0156832196315479,-0.348127169460041));
#52606=DIRECTION('',(-0.348169903293503,8.32132090980276E-8,-0.937431447328596));
#52607=DIRECTION('center_axis',(-0.222551384603853,0.584827969931453,-0.780030208900119));
#52608=DIRECTION('ref_axis',(-0.960196461724811,0.00704480134305794,0.279236683953222));
#52609=DIRECTION('center_axis',(-0.288620999812851,4.93139200386861E-10,
-0.957443428337691));
#52610=DIRECTION('ref_axis',(0.957325848603127,0.015671528054376,-0.288585555433297));
#52611=DIRECTION('',(0.288621063170277,-1.40443212613482E-11,0.957443409238613));
#52612=DIRECTION('',(-0.909057440161158,-3.07809289802204E-8,-0.416670817897825));
#52613=DIRECTION('center_axis',(-0.566134873256367,0.793626260383097,0.222819801887843));
#52614=DIRECTION('ref_axis',(-0.814092839857193,-0.580734748480966,-1.58476235549859E-16));
#52615=DIRECTION('center_axis',(0.340941299925238,0.471546674535792,-0.813266723615029));
#52616=DIRECTION('ref_axis',(0.90670649220367,-0.393419297900025,0.152001950762374));
#52617=DIRECTION('center_axis',(0.281794570900451,-0.601098528027835,0.747845157378051));
#52618=DIRECTION('ref_axis',(-0.936371307102128,-0.00227572440954448,0.351003698433882));
#52619=DIRECTION('',(-0.472928816316283,5.19500677922167E-12,0.881100638234748));
#52620=DIRECTION('center_axis',(0.,-1.,1.45983193964168E-32));
#52621=DIRECTION('ref_axis',(1.,0.,0.));
#52622=DIRECTION('center_axis',(-0.284987038209989,0.60109852710865,-0.746634414395767));
#52623=DIRECTION('ref_axis',(-0.93540373637898,-0.00432812888194756,0.353554970646186));
#52624=DIRECTION('center_axis',(-0.274696621413743,-0.601098528330619,-0.750481395787156));
#52625=DIRECTION('ref_axis',(-0.938208620668851,-0.00330176892258368,0.346054450086448));
#52626=DIRECTION('center_axis',(0.271487805197435,0.601098527639148,0.751648143547982));
#52627=DIRECTION('ref_axis',(-0.939678480413728,-0.00330191842797677,0.342043053988882));
#52628=DIRECTION('center_axis',(-0.350667502455631,0.58482825598845,-0.731442556677582));
#52629=DIRECTION('ref_axis',(-0.911288073877589,-0.0330815410569061,0.410438373023008));
#52630=DIRECTION('center_axis',(0.406375835800862,-1.08414464411254E-7,
0.913706014031395));
#52631=DIRECTION('ref_axis',(0.913593752748676,-0.0156751635316695,-0.406325908830394));
#52632=DIRECTION('',(-0.40634467831564,-4.44089209849844E-13,-0.913719870860079));
#52633=DIRECTION('center_axis',(-0.318557909437256,0.584827952226086,-0.745987348840453));
#52634=DIRECTION('ref_axis',(-0.925740424549813,-0.0227607295990099,0.377473993200132));
#52635=DIRECTION('center_axis',(-0.348169818716519,7.02758491966354E-10,
-0.937431478741196));
#52636=DIRECTION('ref_axis',(0.937316035149934,0.0156933905084249,-0.348126941998399));
#52637=DIRECTION('',(0.348169904517226,-2.20379270384261E-11,0.937431446874098));
#52638=DIRECTION('',(-0.933426594325903,-1.43735365431306E-13,-0.358768439254552));
#52639=DIRECTION('center_axis',(0.373302387671571,-0.601098527899086,0.706629950622146));
#52640=DIRECTION('ref_axis',(-0.894880718438291,-0.032481688583243,0.445121825654673));
#52641=DIRECTION('',(-0.416670832496686,8.17238220606245E-12,0.9090574334697));
#52642=DIRECTION('center_axis',(0.,-1.,1.45983193964168E-32));
#52643=DIRECTION('ref_axis',(1.,0.,0.));
#52644=DIRECTION('center_axis',(-0.376317985627075,0.601098517887626,-0.705028613239832));
#52645=DIRECTION('ref_axis',(-0.893604043109341,-0.0345386484892894,0.447525301965344));
#52646=DIRECTION('center_axis',(-0.27469661328818,-0.601098531871184,-0.750481395925516));
#52647=DIRECTION('ref_axis',(-0.92958095227624,-0.0335099365428258,0.367091728751949));
#52648=DIRECTION('center_axis',(0.27148778682652,0.601098523227746,0.751648153711203));
#52649=DIRECTION('ref_axis',(-0.931140766145985,-0.0335100940379686,0.363116988336589));
#52650=DIRECTION('',(-0.46291579530913,-3.8857805861882E-13,-0.886402259954991));
#52651=DIRECTION('center_axis',(-0.409542993149134,0.584827952146895,-0.700179122189542));
#52652=DIRECTION('ref_axis',(-0.880532271007807,-0.0526562728339964,0.471052265300854));
#52653=DIRECTION('center_axis',(-0.406344618832969,4.69796662330587E-10,
-0.913719897312896));
#52654=DIRECTION('ref_axis',(0.913606229190611,0.0157729998145959,-0.406294068946325));
#52655=DIRECTION('',(0.406344678317545,-1.76525460892821E-10,0.913719870859232));
#52656=DIRECTION('',(-0.954111946854531,0.,-0.299450150892358));
#52657=DIRECTION('',(-0.358768439286625,6.5132654166774E-11,0.933426594313575));
#52658=DIRECTION('center_axis',(0.,-1.,1.45983193964168E-32));
#52659=DIRECTION('ref_axis',(1.,0.,0.));
#52660=DIRECTION('center_axis',(-0.292190888656869,0.601098540001039,-0.743844761892243));
#52661=DIRECTION('ref_axis',(-0.914674229293506,0.0514848610180654,0.40089944294334));
#52662=DIRECTION('center_axis',(0.443479987208326,0.601098537465326,0.664835354958466));
#52663=DIRECTION('ref_axis',(-0.852023607513652,0.0525164870226359,0.520862545044489));
#52664=DIRECTION('center_axis',(-0.357728884201083,0.58482793005104,-0.728015341624381));
#52665=DIRECTION('ref_axis',(-0.890190797102062,0.0219594825743353,0.455058376342929));
#52666=DIRECTION('center_axis',(0.51766303052389,-1.03400239175962E-8,0.855584587769568));
#52667=DIRECTION('ref_axis',(0.855478608197473,-0.0157391393486956,-0.517598908817509));
#52668=DIRECTION('',(-0.517659995144606,0.,-0.855586424288562));
#52669=DIRECTION('center_axis',(-0.325753956097604,0.58482795232135,-0.74287322355189));
#52670=DIRECTION('ref_axis',(-0.90574594568893,0.0322834330483309,0.422589708604789));
#52671=DIRECTION('center_axis',(-0.462915741151528,4.48487702201447E-10,
-0.886402288238321));
#52672=DIRECTION('ref_axis',(0.88629300790583,0.0157020800818683,-0.462858670458207));
#52673=DIRECTION('',(0.462915795308233,-8.32667268468716E-13,0.88640225995546));
#52674=DIRECTION('',(-0.971031855421231,0.,-0.238950069590282));
#52675=DIRECTION('center_axis',(0.380115437938402,-0.601098528198227,0.702988487273314));
#52676=DIRECTION('ref_axis',(-0.870944127416965,0.0232723669164295,0.490830646818236));
#52677=DIRECTION('',(-0.299450150892453,1.43735365432663E-13,0.954111946854502));
#52678=DIRECTION('center_axis',(0.,-1.,1.45983193964168E-32));
#52679=DIRECTION('ref_axis',(1.,0.,0.));
#52680=DIRECTION('center_axis',(-0.38311537327739,0.601098533661765,-0.701358085137829));
#52681=DIRECTION('ref_axis',(-0.869642754686168,0.0212179856622501,0.493225380841547));
#52682=DIRECTION('center_axis',(-0.446316399920546,-0.601098524901484,-0.662934562776164));
#52683=DIRECTION('ref_axis',(-0.838546520538259,0.0222452907237038,0.544375679043248));
#52684=DIRECTION('center_axis',(0.443480040215139,0.601098530690299,0.664835325725659));
#52685=DIRECTION('ref_axis',(-0.840864568154533,0.0222451381343953,0.540788250474871));
#52686=DIRECTION('center_axis',(-0.446153347918924,0.584827953016325,-0.677438894300786));
#52687=DIRECTION('ref_axis',(-0.838223483347709,-0.00784645565821609,0.545270414655001));
#52688=DIRECTION('center_axis',(0.57036150323578,-8.49799438812077E-10,
0.82139378840275));
#52689=DIRECTION('ref_axis',(0.821292834977943,-0.0156778483083717,-0.570291402956694));
#52690=DIRECTION('',(-0.570361227475616,-7.7715611723776E-13,-0.821393979885724));
#52691=DIRECTION('center_axis',(-0.416291991565607,0.584827952254239,-0.696187650005697));
#52692=DIRECTION('ref_axis',(-0.857349751040828,0.00246180457236924,0.514728417622806));
#52693=DIRECTION('center_axis',(-0.517659944790757,4.41968251467754E-10,
-0.855586454754416));
#52694=DIRECTION('ref_axis',(0.855481394221478,0.0156707406182415,-0.517596379459277));
#52695=DIRECTION('',(0.517659995144688,-6.50590692400118E-11,0.855586424288512));
#52696=DIRECTION('',(-0.984119544876815,1.64268989064223E-13,-0.177506961529541));
#52697=DIRECTION('center_axis',(0.465225925216188,-0.601098528074967,0.649804122834605));
#52698=DIRECTION('ref_axis',(-0.816092971536365,-0.00691952152621577,0.577879210588851));
#52699=DIRECTION('',(-0.238950069602231,2.34493981894294E-11,0.971031855418291));
#52700=DIRECTION('center_axis',(0.,-1.,1.45983193964168E-32));
#52701=DIRECTION('ref_axis',(1.,0.,0.));
#52702=DIRECTION('center_axis',(-0.467997902155121,0.601098525572697,-0.647810563461832));
#52703=DIRECTION('ref_axis',(-0.814500001467842,-0.00897217296524106,0.580094171424922));
#52704=DIRECTION('center_axis',(-0.446316403197408,-0.601098529023294,-0.662934556832694));
#52705=DIRECTION('ref_axis',(-0.826145117889556,-0.00794565927750685,0.563401376183887));
#52706=DIRECTION('center_axis',(0.443480015076013,0.601098526843241,0.664835345973019));
#52707=DIRECTION('ref_axis',(-0.828544573820292,-0.00794583479468556,0.559866727804365));
#52708=DIRECTION('center_axis',(-0.527540982838747,0.5848279522305,-0.616179176632422));
#52709=DIRECTION('ref_axis',(-0.767951949450662,-0.0181546316971145,0.640250117284542));
#52710=DIRECTION('center_axis',(0.620811582090657,-7.74860921390325E-10,
0.783959807351178));
#52711=DIRECTION('ref_axis',(0.783863434364948,-0.0156795066180816,-0.620735265099223));
#52712=DIRECTION('',(-0.620811502082354,2.06171549165036E-7,-0.783959870709088));
#52713=DIRECTION('center_axis',(-0.50026981225926,0.584827782536682,-0.638519051959542));
#52714=DIRECTION('ref_axis',(-0.798886072311127,-0.0273551074082388,0.600860001635976));
#52715=DIRECTION('center_axis',(-0.570361141665806,7.05271550366232E-10,
-0.821394039470508));
#52716=DIRECTION('ref_axis',(0.821292770502868,0.0157023279247815,-0.570290822315655));
#52717=DIRECTION('',(-0.570361226666628,-1.29267412278592E-5,-0.821393980345753));
#52718=DIRECTION('',(-0.993323368672574,-7.62630514899115E-8,-0.115363275131056));
#52719=DIRECTION('center_axis',(0.620811504614919,1.410173336424E-14,0.783959868703597));
#52720=DIRECTION('ref_axis',(0.605120001066379,-0.635772805085093,-0.47918965412836));
#52721=DIRECTION('',(0.17750696153003,0.,-0.984119544876727));
#52722=DIRECTION('center_axis',(-0.61122428384635,0.398564391552574,-0.68377723026059));
#52723=DIRECTION('ref_axis',(-0.745553533391341,-2.17675110791388E-16,0.666445743363769));
#52724=DIRECTION('center_axis',(0.673996080582493,5.74456607852808E-5,0.738734918668012));
#52725=DIRECTION('ref_axis',(0.73873488531722,-0.000362796013170164,-0.673996021942568));
#52726=DIRECTION('',(-0.668811041446666,5.94973683763053E-5,-0.743432436270499));
#52727=DIRECTION('center_axis',(-0.489456455415781,0.590180063811213,-0.641965630335154));
#52728=DIRECTION('ref_axis',(0.486222843277527,0.795820632489076,0.360911163002481));
#52729=DIRECTION('center_axis',(-0.798223519039003,0.550037558029662,0.24555630395035));
#52730=DIRECTION('ref_axis',(-0.567410340630547,-0.82343518588018,3.06798539265314E-16));
#52731=DIRECTION('center_axis',(0.0463591440219179,-0.477126090531288,-0.877611259898074));
#52732=DIRECTION('ref_axis',(0.989629241963715,-0.0976390452529731,0.105359291438438));
#52733=DIRECTION('center_axis',(-0.0567895812488869,0.584827951389893,-0.809166985692494));
#52734=DIRECTION('ref_axis',(-0.995671712707148,0.0265489689991942,0.0890673495726409));
#52735=DIRECTION('center_axis',(0.16634571851791,2.36699141555689E-12,0.98606749359806));
#52736=DIRECTION('ref_axis',(0.985945217509321,-0.015747767056103,-0.166325091021305));
#52737=DIRECTION('center_axis',(-0.113148552631875,-0.00011544118542266,
-0.993578075296876));
#52738=DIRECTION('ref_axis',(0.024707162564102,0.999690438280507,-0.00292980008858347));
#52739=DIRECTION('',(0.104101785988569,-6.06903416145004E-10,0.994566648422312));
#52740=DIRECTION('center_axis',(0.0869599339253347,-0.601098527785029,0.794429688384298));
#52741=DIRECTION('ref_axis',(-0.991170198717985,0.0279220186133635,0.129622521383846));
#52742=DIRECTION('',(-0.629653742733209,2.24350371841873E-10,0.776875900168143));
#52743=DIRECTION('center_axis',(0.,-1.,1.45983193964168E-32));
#52744=DIRECTION('ref_axis',(1.,0.,0.));
#52745=DIRECTION('center_axis',(-0.0903532208711649,0.601098534606634,-0.794050909685244));
#52746=DIRECTION('ref_axis',(-0.990868178537547,0.0258667040795945,0.132329763778762));
#52747=DIRECTION('center_axis',(-0.178470325633292,-0.601098523730062,-0.778992238496564));
#52748=DIRECTION('ref_axis',(-0.97871090680517,0.0268944702660908,0.20347395010101));
#52749=DIRECTION('center_axis',(0.175140560780707,0.601098531055857,0.779747612969678));
#52750=DIRECTION('ref_axis',(-0.979571268606861,0.0268943098413773,0.199290807159039));
#52751=DIRECTION('center_axis',(-0.15775731054866,0.584827952222719,-0.795668836430984));
#52752=DIRECTION('ref_axis',(-0.981355105571386,-0.00326197146141438,0.19217574329545));
#52753=DIRECTION('center_axis',(0.227933218521286,-4.1940118515531E-10,
0.973676767667036));
#52754=DIRECTION('ref_axis',(0.973557015888024,-0.015683219630834,-0.227905185191599));
#52755=DIRECTION('',(-0.22793316507402,8.32144303433845E-8,-0.973676780178788));
#52756=DIRECTION('center_axis',(-0.123032792071934,0.584827969931186,-0.801772522390954));
#52757=DIRECTION('ref_axis',(-0.98762266236098,0.00704480136197383,0.15669029186513));
#52758=DIRECTION('center_axis',(-0.166345664255104,4.29216190013688E-10,
-0.986067502751981));
#52759=DIRECTION('ref_axis',(0.985946407810043,0.0156715280543889,-0.166325236013402));
#52760=DIRECTION('',(0.166345721445477,-1.44328993199749E-11,0.986067493104191));
#52761=DIRECTION('',(-0.849666549784077,-3.07807852448522E-8,-0.527320352516401));
#52762=DIRECTION('center_axis',(-0.58959745695761,0.793626260382879,0.150107286897758));
#52763=DIRECTION('ref_axis',(-0.802721322940073,-0.59635432227606,1.12566621593397E-16));
#52764=DIRECTION('center_axis',(0.440182224109369,0.47154667450417,-0.764122597062924));
#52765=DIRECTION('ref_axis',(0.88050646203643,-0.39341697707929,0.264445556699071));
#52766=DIRECTION('center_axis',(0.185842684630873,-0.601098528028628,0.777266399744004));
#52767=DIRECTION('ref_axis',(-0.972980168207799,-0.00227572432940167,0.230877485591603));
#52768=DIRECTION('',(-0.579630823428198,5.19500677922228E-12,0.814879198735585));
#52769=DIRECTION('center_axis',(0.,-1.,1.45983193964168E-32));
#52770=DIRECTION('ref_axis',(1.,0.,0.));
#52771=DIRECTION('center_axis',(-0.189161721372458,0.601098527118791,-0.776465326890408));
#52772=DIRECTION('ref_axis',(-0.972339986917059,-0.00432812674195253,0.233529906352568));
#52773=DIRECTION('center_axis',(-0.17847030044431,-0.601098528344443,-0.778992240706839));
#52774=DIRECTION('ref_axis',(-0.974182687949423,-0.00330176646215566,0.22573699040668));
#52775=DIRECTION('center_axis',(0.175140559098384,0.601098527670136,0.779747615957561));
#52776=DIRECTION('ref_axis',(-0.975138195345261,-0.00330191308371978,0.2215730068144));
#52777=DIRECTION('center_axis',(-0.256228323701883,0.584828255987388,-0.769625205623928));
#52778=DIRECTION('ref_axis',(-0.955543863686363,-0.0330815410800097,0.292987262882038));
#52779=DIRECTION('center_axis',(0.288653685344861,-1.08198123761921E-7,
0.957433574686421));
#52780=DIRECTION('ref_axis',(0.9573159411088,-0.0156751635316667,-0.288618222133026));
#52781=DIRECTION('',(-0.288621063170684,3.88578058619192E-13,-0.957443409238491));
#52782=DIRECTION('center_axis',(-0.22254897853054,0.584827952226241,-0.78003090865034));
#52783=DIRECTION('ref_axis',(-0.965750720954388,-0.0227607295905163,0.258471457156465));
#52784=DIRECTION('center_axis',(-0.227933086768831,6.25622020348082E-10,
-0.973676798509666));
#52785=DIRECTION('ref_axis',(0.973556891347874,0.0156933905084927,-0.227905017065031));
#52786=DIRECTION('',(0.227933166345219,-2.28705943068783E-11,0.97367677988121));
#52787=DIRECTION('',(-0.881100638236051,0.,-0.472928816313854));
#52788=DIRECTION('center_axis',(0.281794569239125,-0.601098527928147,0.747845158084179));
#52789=DIRECTION('ref_axis',(-0.943612874711639,-0.0324816879688959,0.329453612250841));
#52790=DIRECTION('',(-0.52732036616135,8.17238220606277E-12,0.849666541315745));
#52791=DIRECTION('center_axis',(0.,-1.,1.45983193964168E-32));
#52792=DIRECTION('ref_axis',(1.,0.,0.));
#52793=DIRECTION('center_axis',(-0.284987069308705,0.601098518635038,-0.746634409347439));
#52794=DIRECTION('ref_axis',(-0.942647507793442,-0.0345386352562879,0.331998130605347));
#52795=DIRECTION('center_axis',(-0.178470279873277,-0.601098531582791,-0.77899224292092));
#52796=DIRECTION('ref_axis',(-0.968259723758394,-0.0335099418156356,0.247689707389773));
#52797=DIRECTION('center_axis',(0.175140532367362,0.601098523279556,0.779747625346313));
#52798=DIRECTION('ref_axis',(-0.969309069137841,-0.033510093144419,0.243550820455579));
#52799=DIRECTION('',(-0.348169904517746,7.77156117238016E-13,-0.937431446873905));
#52800=DIRECTION('center_axis',(-0.31855791089476,0.584827952145615,-0.745987348281143));
#52801=DIRECTION('ref_axis',(-0.932627514626529,-0.0526562728524064,0.356977920732972));
#52802=DIRECTION('center_axis',(-0.288620975689055,6.76985696212227E-10,
-0.9574434356098));
#52803=DIRECTION('ref_axis',(0.957324328213855,0.0157729998150228,-0.288585070796683));
#52804=DIRECTION('',(0.288621063172828,-1.76914038951305E-10,0.957443409237844));
#52805=DIRECTION('',(-0.909057433471482,0.,-0.416670832492798));
#52806=DIRECTION('',(-0.472928816344037,6.51531877903919E-11,0.881100638219851));
#52807=DIRECTION('center_axis',(0.,-1.,1.45983193964168E-32));
#52808=DIRECTION('ref_axis',(1.,0.,0.));
#52809=DIRECTION('center_axis',(-0.196658414391181,0.601098540407601,-0.774600550457459));
#52810=DIRECTION('ref_axis',(-0.957707771787014,0.0514848563389987,0.283099158293531));
#52811=DIRECTION('center_axis',(0.356657049198021,0.601098537525625,0.715175710886434));
#52812=DIRECTION('ref_axis',(-0.910586534296204,0.0525164863478813,0.409968513693552));
#52813=DIRECTION('center_axis',(-0.263663568245725,0.584827930050699,-0.767110041006209));
#52814=DIRECTION('ref_axis',(-0.940205314548717,0.0219594825774785,0.339899614032258));
#52815=DIRECTION('center_axis',(0.406347874870001,-9.95120379307527E-9,
0.913718449298598));
#52816=DIRECTION('ref_axis',(0.913605268826287,-0.0157391393485702,-0.406297541544881));
#52817=DIRECTION('',(-0.406344678315089,4.44089209849855E-13,-0.913719870860324));
#52818=DIRECTION('center_axis',(-0.230078585608708,0.584827952321108,-0.777843242966214));
#52819=DIRECTION('ref_axis',(-0.951568403027054,0.0322834330550571,0.30573739436111));
#52820=DIRECTION('center_axis',(-0.348169832796153,5.70023818185921E-10,
-0.937431473511904));
#52821=DIRECTION('ref_axis',(0.93731590203293,0.0157020800826772,-0.348126908579719));
#52822=DIRECTION('',(0.348169904517199,-8.32667268468792E-13,0.937431446874109));
#52823=DIRECTION('',(-0.933426594325893,0.,-0.358768439254578));
#52824=DIRECTION('center_axis',(0.289010303054396,-0.601098528424121,0.74508630631274));
#52825=DIRECTION('ref_axis',(-0.925593862075092,0.0232723609802456,0.377802064186156));
#52826=DIRECTION('',(-0.416670832492792,0.,0.909057433471485));
#52827=DIRECTION('center_axis',(0.,-1.,1.45983193964168E-32));
#52828=DIRECTION('ref_axis',(1.,0.,0.));
#52829=DIRECTION('center_axis',(-0.292190908012313,0.60109853343636,-0.743844759594095));
#52830=DIRECTION('ref_axis',(-0.924602896651822,0.0212179917817949,0.380341005319974));
#52831=DIRECTION('center_axis',(-0.359709332547123,-0.601098524824285,-0.713645401815616));
#52832=DIRECTION('ref_axis',(-0.900162693631838,0.0222452928133851,0.434985369801238));
#52833=DIRECTION('center_axis',(0.356657114723764,0.601098530486833,0.71517568412488));
#52834=DIRECTION('ref_axis',(-0.902012836724754,0.0222451436298874,0.431135704817691));
#52835=DIRECTION('center_axis',(-0.357729647164783,0.584827953375185,-0.728014947985515));
#52836=DIRECTION('ref_axis',(-0.899954361421966,-0.0078464288985307,0.435913501638939));
#52837=DIRECTION('center_axis',(0.46291631123801,-1.99076621249946E-9,0.886401990515474));
#52838=DIRECTION('ref_axis',(0.886293047250042,-0.0156778482806867,-0.462859416528954));
#52839=DIRECTION('',(-0.462915795308943,0.,-0.886402259955089));
#52840=DIRECTION('center_axis',(-0.325753955539869,0.584827952254261,-0.742873223849276));
#52841=DIRECTION('ref_axis',(-0.915101869160062,0.00246180456567018,0.403215213723443));
#52842=DIRECTION('center_axis',(-0.406344585355985,7.77170922148946E-10,
-0.9137199122006));
#52843=DIRECTION('ref_axis',(0.913607713252797,0.0156707406185981,-0.406294688832453));
#52844=DIRECTION('',(0.406344678315861,-6.37823127618327E-11,0.913719870859981));
#52845=DIRECTION('',(-0.954111946854573,1.64268989064276E-13,-0.299450150892225));
#52846=DIRECTION('center_axis',(0.380115435494561,-0.6010985280191,0.702988488747897));
#52847=DIRECTION('ref_axis',(-0.882085301519085,-0.00691952667751051,0.471038895415808));
#52848=DIRECTION('',(-0.358768439266198,2.35931335548739E-11,0.933426594321426));
#52849=DIRECTION('center_axis',(0.,-1.,1.45983193964168E-32));
#52850=DIRECTION('ref_axis',(1.,0.,0.));
#52851=DIRECTION('center_axis',(-0.38311538656434,0.601098525760556,-0.701358084651587));
#52852=DIRECTION('ref_axis',(-0.880782512520894,-0.00897215952289311,0.473436021011157));
#52853=DIRECTION('center_axis',(-0.35970932549862,-0.601098528958347,-0.713645401886286));
#52854=DIRECTION('ref_axis',(-0.890243636339669,-0.00794566461597056,0.455415342704365));
#52855=DIRECTION('center_axis',(0.356657089597931,0.601098526944953,0.715175699632014));
#52856=DIRECTION('ref_axis',(-0.892181155505171,-0.0079458276464437,0.451607849338861));
#52857=DIRECTION('center_axis',(-0.446153435948076,0.584827952230776,-0.677438837003964));
#52858=DIRECTION('ref_axis',(-0.842141036447412,-0.0181546316901292,0.538951652821915));
#52859=DIRECTION('center_axis',(0.517659926830274,6.26752252576661E-10,
0.855586465621141));
#52860=DIRECTION('ref_axis',(0.855481287509428,-0.0156795066150229,-0.517596290359118));
#52861=DIRECTION('',(-0.517659992379576,2.06170327919809E-7,-0.855586425961478));
#52862=DIRECTION('center_axis',(-0.416297377895457,0.584827782536603,-0.69618457174135));
#52863=DIRECTION('ref_axis',(-0.867894343937951,-0.0273551074107471,0.495995066365645));
#52864=DIRECTION('center_axis',(-0.462915705502022,6.80458439970798E-10,
-0.886402306855959));
#52865=DIRECTION('ref_axis',(0.886293023072826,0.0157023279257069,-0.462858633008119));
#52866=DIRECTION('',(-0.46291579444854,-1.29267404107022E-5,-0.886402260310169));
#52867=DIRECTION('',(-0.971031864912521,-7.62630514899288E-8,-0.238950031020097));
#52868=DIRECTION('center_axis',(0.517659995141469,1.97424267101112E-12,
0.85558642429046));
#52869=DIRECTION('ref_axis',(0.660406837962033,-0.635772805084829,-0.399569454147282));
#52870=DIRECTION('',(0.299450150892762,0.,-0.954111946854405));
#52871=DIRECTION('center_axis',(-0.520704586498207,0.398564391553765,-0.754992158492463));
#52872=DIRECTION('ref_axis',(-0.823202421105205,4.20107565333048E-17,0.567747984484779));
#52873=DIRECTION('center_axis',(0.576093384093487,5.7445652595911E-5,0.817383881357903));
#52874=DIRECTION('ref_axis',(0.817383840831677,-0.000363133212873767,-0.576093330009579));
#52875=DIRECTION('',(-0.570360475446356,5.94973691578862E-5,-0.821394499925991));
#52876=DIRECTION('center_axis',(-0.405137316619699,0.590180063805294,-0.698248699940766));
#52877=DIRECTION('ref_axis',(0.437157251884037,0.795820196456205,0.41900328404155));
#52878=DIRECTION('center_axis',(-0.822705653767276,0.550037558032886,0.143576084403282));
#52879=DIRECTION('ref_axis',(-0.555796003831724,-0.831318712723758,1.13199349268201E-16));
#52880=DIRECTION('center_axis',(0.155987445281772,-0.477126091130184,-0.864880691238565));
#52881=DIRECTION('ref_axis',(0.968621986494132,-0.0976332342635064,0.228558961424418));
#52882=DIRECTION('center_axis',(0.0450737363500213,0.584827951390675,-0.809904084175179));
#52883=DIRECTION('ref_axis',(-0.998983642787651,0.0265489689862998,-0.0364257283864013));
#52884=DIRECTION('center_axis',(0.0414470066457046,-1.35743970630672E-11,
0.999140703624925));
#52885=DIRECTION('ref_axis',(0.999016806408817,-0.0157477670559316,-0.0414418670607522));
#52886=DIRECTION('center_axis',(0.0122720119993164,-0.000115441169559691,
-0.999924689361567));
#52887=DIRECTION('ref_axis',(0.0248707036530095,0.99969065818745,0.000189822410529044));
#52888=DIRECTION('',(-0.0213713417294297,-6.06514838087198E-10,0.999771606794614));
#52889=DIRECTION('center_axis',(-0.0132941993870834,-0.601098528157791,
0.799064342659084));
#52890=DIRECTION('ref_axis',(-0.999600535579284,0.0279220105392125,0.00437385379914484));
#52891=DIRECTION('',(-0.722057103549597,2.24206636476414E-10,0.691833462051068));
#52892=DIRECTION('center_axis',(0.,-1.,1.45983193964168E-32));
#52893=DIRECTION('ref_axis',(1.,0.,0.));
#52894=DIRECTION('center_axis',(0.00988022332258178,0.601098534236258,-0.799113842531912));
#52895=DIRECTION('ref_axis',(-0.999640204045365,0.0258667124555254,0.0070975800723927));
#52896=DIRECTION('center_axis',(-0.079429416547992,-0.60109852376284,-0.795217915113197));
#52897=DIRECTION('ref_axis',(-0.996495527177138,0.0268944696049595,0.0792044936895975));
#52898=DIRECTION('center_axis',(0.0760312438730437,0.601098530830715,0.795550002318065));
#52899=DIRECTION('ref_axis',(-0.996824817208516,0.0268943149207247,0.0749465117410669));
#52900=DIRECTION('center_axis',(-0.0567895989104308,0.58482795222283,-0.80916698385095));
#52901=DIRECTION('ref_axis',(-0.997702834767716,-0.00326197145638583,0.0676639714965141));
#52902=DIRECTION('center_axis',(0.104101880233295,-7.42459677259694E-10,
0.994566638557665));
#52903=DIRECTION('ref_axis',(0.994444317549335,-0.0156832196312127,-0.104089076832476));
#52904=DIRECTION('',(-0.104101784680852,8.32143748321909E-8,-0.994566648559188));
#52905=DIRECTION('center_axis',(-0.0215738989994039,0.584827969932201,-0.810870404236672));
#52906=DIRECTION('ref_axis',(-0.999473463626067,0.00704480132966553,0.031672800342533));
#52907=DIRECTION('center_axis',(-0.0414469282271476,6.03116713776065E-10,
-0.999140706877932));
#52908=DIRECTION('ref_axis',(0.999018006468192,0.0156715280543576,-0.0414418382888709));
#52909=DIRECTION('',(0.0414470083234698,-1.48214773785843E-11,0.999140703555327));
#52910=DIRECTION('',(-0.776875910350776,-3.07809289802272E-8,-0.629653730169728));
#52911=DIRECTION('center_axis',(-0.603761736552382,0.793626260383761,0.075027490325471));
#52912=DIRECTION('ref_axis',(-0.795869445650856,-0.605468269589249,3.41264943846719E-17));
#52913=DIRECTION('center_axis',(0.532481211718397,0.471546674499199,-0.702927800656408));
#52914=DIRECTION('ref_axis',(0.840419115869136,-0.393420680742697,0.372714203708004));
#52915=DIRECTION('center_axis',(0.086959942795448,-0.601098528044268,0.794429687217205));
#52916=DIRECTION('ref_axis',(-0.994244551277268,-0.00227572098346056,0.107110192556405));
#52917=DIRECTION('',(-0.677191706199959,5.05127141378919E-12,0.735806627487133));
#52918=DIRECTION('center_axis',(0.,-1.,1.45983193964168E-32));
#52919=DIRECTION('ref_axis',(1.,0.,0.));
#52920=DIRECTION('center_axis',(-0.0903532064474036,0.601098527152084,-0.794050916969603));
#52921=DIRECTION('ref_axis',(-0.993941854728559,-0.00432812185830315,0.109821932144412));
#52922=DIRECTION('center_axis',(-0.0794293726861269,-0.601098528292757,
-0.795217916070161));
#52923=DIRECTION('ref_axis',(-0.994793314994779,-0.00330177835730735,0.101859504717909));
#52924=DIRECTION('center_axis',(0.0760312337800567,0.601098527673595,0.795550005668103));
#52925=DIRECTION('ref_axis',(-0.995219400801409,-0.00330191285651983,0.0976086145787));
#52926=DIRECTION('center_axis',(-0.157748271170264,0.584828255987902,-0.795670405344413));
#52927=DIRECTION('ref_axis',(-0.984730155966502,-0.033081541071693,0.17091556854339));
#52928=DIRECTION('center_axis',(0.166379301644552,-1.08060781329185E-7,
0.986061827668154));
#52929=DIRECTION('ref_axis',(0.985940676947419,-0.0156751635313546,-0.166358861467401));
#52930=DIRECTION('',(-0.166345721445974,0.,-0.986067493104107));
#52931=DIRECTION('center_axis',(-0.123030317275551,0.584827952226511,-0.801772915061131));
#52932=DIRECTION('ref_axis',(-0.990530551576628,-0.0227607295753553,0.135392671819783));
#52933=DIRECTION('center_axis',(-0.104101721443439,4.93313746308513E-10,
-0.994566655178281));
#52934=DIRECTION('ref_axis',(0.994444175453534,0.0156933905082854,-0.104088901429955));
#52935=DIRECTION('',(0.104101785979735,-2.28705943069056E-11,0.994566648423236));
#52936=DIRECTION('',(-0.814879198737184,1.43735365431383E-13,-0.579630823425951));
#52937=DIRECTION('center_axis',(0.185842686022657,-0.601098527830234,0.77726639956466));
#52938=DIRECTION('ref_axis',(-0.977463691313877,-0.0324816898131399,0.208589721678543));
#52939=DIRECTION('',(-0.629653742645588,8.00811321699454E-12,0.776875900239159));
#52940=DIRECTION('center_axis',(0.,-1.,1.45983193964168E-32));
#52941=DIRECTION('ref_axis',(1.,0.,0.));
#52942=DIRECTION('center_axis',(-0.189161734660047,0.6010985193897,-0.776465329636754));
#52943=DIRECTION('ref_axis',(-0.9768248540831,-0.0345386219249532,0.211235148687562));
#52944=DIRECTION('center_axis',(-0.0794293717565466,-0.601098531586404,
-0.795217913673371));
#52945=DIRECTION('ref_axis',(-0.991668458571965,-0.0335099417813519,0.124381478023516));
#52946=DIRECTION('center_axis',(0.076031206768239,0.601098523311899,0.795550011545233));
#52947=DIRECTION('ref_axis',(-0.992190789392835,-0.0335100925034672,0.120143710382328));
#52948=DIRECTION('',(-0.227933166345721,0.,-0.973676779881093));
#52949=DIRECTION('center_axis',(-0.222548980029614,0.584827952147113,-0.780030908281969));
#52950=DIRECTION('ref_axis',(-0.970014665235007,-0.0526562728337964,0.237273821059698));
#52951=DIRECTION('center_axis',(-0.166345655494771,4.83957742611337E-10,
-0.986067504229814));
#52952=DIRECTION('ref_axis',(0.985944835955002,0.015772999814884,-0.166324961838274));
#52953=DIRECTION('',(0.166345721448234,-1.76914038951275E-10,0.986067493103726));
#52954=DIRECTION('',(-0.849666541317971,0.,-0.527320366157762));
#52955=DIRECTION('',(-0.579630823453725,6.51326541667441E-11,0.814879198717428));
#52956=DIRECTION('center_axis',(0.,-1.,1.45983193964168E-32));
#52957=DIRECTION('ref_axis',(1.,0.,0.));
#52958=DIRECTION('center_axis',(-0.098024518104039,0.601098540713194,-0.793140427795065));
#52959=DIRECTION('ref_axis',(-0.985637692309511,0.051484852820372,0.160834229655403));
#52960=DIRECTION('center_axis',(0.264209415125226,0.601098537645921,0.754237318752606));
#52961=DIRECTION('ref_axis',(-0.954788967611246,0.0525164848971561,0.292609032912346));
#52962=DIRECTION('center_axis',(-0.165440120329679,0.584827930051102,-0.794106956786959));
#52963=DIRECTION('ref_axis',(-0.975392232529833,0.0219594825708578,0.219380431774778));
#52964=DIRECTION('center_axis',(0.288624384642661,-9.72083670309824E-9,
0.957442407975355));
#52965=DIRECTION('ref_axis',(0.957323811526494,-0.015739139347579,-0.288588633485421));
#52966=DIRECTION('',(-0.288621063170532,3.88578058618535E-13,-0.957443409238537));
#52967=DIRECTION('center_axis',(-0.130774738400328,0.584827952321201,-0.800546209771876));
#52968=DIRECTION('ref_axis',(-0.982384058205275,0.0322834330508441,0.184063418784358));
#52969=DIRECTION('center_axis',(-0.227933087277152,6.06662003836226E-10,
-0.973676798390671));
#52970=DIRECTION('ref_axis',(0.973556758396492,0.0157020800821283,-0.227904986478159));
#52971=DIRECTION('',(0.227933166345052,-3.88578058618627E-13,0.973676779881249));
#52972=DIRECTION('',(-0.881100638236031,-1.64268989064337E-13,-0.472928816313892));
#52973=DIRECTION('center_axis',(0.193347282237507,-0.601098528136115,0.775433677321256));
#52974=DIRECTION('ref_axis',(-0.965646434806065,0.0232723685696349,0.258815300566825));
#52975=DIRECTION('',(-0.527320366157789,0.,0.849666541317955));
#52976=DIRECTION('center_axis',(0.,-1.,1.45983193964168E-32));
#52977=DIRECTION('ref_axis',(1.,0.,0.));
#52978=DIRECTION('center_axis',(-0.196658433615245,0.601098533602547,-0.77460055085758));
#52979=DIRECTION('ref_axis',(-0.964981493238737,0.0212179873045292,0.26145843784717));
#52980=DIRECTION('center_axis',(-0.267429420305788,-0.601098525088523,-0.753101632113032));
#52981=DIRECTION('ref_axis',(-0.947582767948786,0.0222452859069907,0.318735070460458));
#52982=DIRECTION('center_axis',(0.264209492842463,0.601098530326073,0.754237297361887));
#52983=DIRECTION('ref_axis',(-0.948935826115031,0.0222451481022262,0.314683891073716));
#52984=DIRECTION('center_axis',(-0.263664252983005,0.584827954381707,-0.767109787105224));
#52985=DIRECTION('ref_axis',(-0.947492435019574,-0.00784635387838365,0.319681904885925));
#52986=DIRECTION('center_axis',(0.348170767516168,-2.42832855999574E-9,
0.937431126348599));
#52987=DIRECTION('ref_axis',(0.937315911348809,-0.0156778481980674,-0.348127975618494));
#52988=DIRECTION('',(-0.348169904517986,0.,-0.937431446873816));
#52989=DIRECTION('center_axis',(-0.230078585026532,0.584827952254463,-0.777843243188524));
#52990=DIRECTION('ref_axis',(-0.958422284152977,0.00246180456700299,0.285343065023952));
#52991=DIRECTION('center_axis',(-0.288621003383784,4.69944830746473E-10,
-0.957443427261234));
#52992=DIRECTION('ref_axis',(0.957325859343011,0.0156707406186114,-0.288585562566163));
#52993=DIRECTION('',(0.288621063170873,-6.42264019715572E-11,0.957443409238434));
#52994=DIRECTION('',(-0.90905743347151,1.64268989064311E-13,-0.416670832492738));
#52995=DIRECTION('center_axis',(0.28901028694578,-0.601098528046295,0.745086312865895));
#52996=DIRECTION('ref_axis',(-0.934166624693501,-0.00691952387371952,0.356770006444086));
#52997=DIRECTION('',(-0.472928816324628,2.3449398189427E-11,0.881100638230269));
#52998=DIRECTION('center_axis',(0.,-1.,1.45983193964168E-32));
#52999=DIRECTION('ref_axis',(1.,0.,0.));
#53000=DIRECTION('center_axis',(-0.292190927015802,0.601098525790784,-0.743844758307668));
#53001=DIRECTION('ref_axis',(-0.933174547879557,-0.00897215717209348,0.359311513293776));
#53002=DIRECTION('center_axis',(-0.26742942804773,-0.60109852898886,-0.753101626250729));
#53003=DIRECTION('ref_axis',(-0.940302475780628,-0.00794566216052988,0.340247146194722));
#53004=DIRECTION('center_axis',(0.264209457521186,0.601098526927667,0.754237312443338));
#53005=DIRECTION('ref_axis',(-0.941747513064489,-0.00794582853994121,0.336226836296069));
#53006=DIRECTION('center_axis',(-0.357729782847908,0.58482795223096,-0.728014882233139));
#53007=DIRECTION('ref_axis',(-0.903049056228438,-0.0181546316809015,0.429153598835497));
#53008=DIRECTION('center_axis',(0.406344760815415,-7.08143957842295E-10,
0.91371983417121));
#53009=DIRECTION('ref_axis',(0.913607509655577,-0.0156795066176049,-0.406294808449681));
#53010=DIRECTION('',(-0.406344675363295,2.06171937743088E-7,-0.913719872173007));
#53011=DIRECTION('center_axis',(-0.325759685202577,0.584827782536742,-0.742870844945389));
#53012=DIRECTION('ref_axis',(-0.923215403305287,-0.0273551074156397,0.383307992609254));
#53013=DIRECTION('center_axis',(-0.34816980557852,7.1282886651966E-10,-0.937431483620758));
#53014=DIRECTION('ref_axis',(0.937315908492689,0.0157023279253457,-0.348126880008208));
#53015=DIRECTION('',(-0.348169903619823,-1.29267404106986E-5,-0.937431447118275));
#53016=DIRECTION('',(-0.933426608576392,-7.6262907754578E-8,-0.358768402178298));
#53017=DIRECTION('center_axis',(0.406344678308733,5.73812350350916E-12,
0.91371987086315));
#53018=DIRECTION('ref_axis',(0.70527866451459,-0.635772805084979,-0.313647805181057));
#53019=DIRECTION('',(0.416670832493319,0.,-0.909057433471244));
#53020=DIRECTION('center_axis',(-0.421973066766652,0.398564391555568,-0.814300409374505));
#53021=DIRECTION('ref_axis',(-0.887868914881341,-7.97986771087996E-17,0.460096500733737));
#53022=DIRECTION('center_axis',(0.469105350796176,5.74456488072083E-5,0.883142211964978));
#53023=DIRECTION('ref_axis',(0.883142165012923,-0.000363020440370894,-0.469105302242948));
#53024=DIRECTION('',(-0.462914984031325,5.94973683763289E-5,-0.886402681640428));
#53025=DIRECTION('center_axis',(-0.314428920608558,0.590180063809988,-0.743519970253775));
#53026=DIRECTION('ref_axis',(0.381196510278465,0.795819976664742,0.470488879032066));
#53027=DIRECTION('center_axis',(-0.834213228879005,0.550037558031181,0.0393315842340603));
#53028=DIRECTION('ref_axis',(-0.550463499052738,-0.834859231374138,7.73147444792113E-19));
#53029=DIRECTION('center_axis',(0.26315573158457,-0.477126089798436,-0.838510438437021));
#53030=DIRECTION('ref_axis',(0.932339990205128,-0.0976265035258249,0.348154001088059));
#53031=DIRECTION('center_axis',(0.14622621420636,0.584827951391204,-0.797868511441856));
#53032=DIRECTION('ref_axis',(-0.986541004061149,0.0265489689768779,-0.16134435085334));
#53033=DIRECTION('center_axis',(-0.0841053527532984,9.82782766916969E-12,
0.996456867926677));
#53034=DIRECTION('ref_axis',(0.996333303516304,-0.0157477670566241,0.0840949233724572));
#53035=DIRECTION('center_axis',(0.137499035826066,-0.000115441193923135,
-0.990501893900377));
#53036=DIRECTION('ref_axis',(0.0246629893145987,0.999690351939331,0.00330714340248807));
#53037=DIRECTION('',(-0.14650743062218,-6.06126260029117E-10,0.98920956969314));
#53038=DIRECTION('center_axis',(-0.113338700331315,-0.601098527834891,0.791097275208261));
#53039=DIRECTION('ref_axis',(-0.992266574683714,0.0279220176816331,-0.120943812136201));
#53040=DIRECTION('',(-0.803073192506799,2.24206636476386E-10,0.595880396956418));
#53041=DIRECTION('center_axis',(0.,-1.,1.45983193964168E-32));
#53042=DIRECTION('ref_axis',(1.,0.,0.));
#53043=DIRECTION('center_axis',(0.109957851633899,0.601098533843261,-0.791574269083792));
#53044=DIRECTION('ref_axis',(-0.992647303462575,0.0258667215027917,-0.118246537569502));
#53045=DIRECTION('center_axis',(0.0208641544658999,-0.601098524137728,-0.79890252930997));
#53046=DIRECTION('ref_axis',(-0.998564817328578,0.0268944613826216,-0.0463140749716835));
#53047=DIRECTION('center_axis',(-0.0242771357386957,0.601098530732607,0.79880609476357));
#53048=DIRECTION('ref_axis',(-0.998357844538717,0.0268943171535404,-0.0505797385605408));
#53049=DIRECTION('center_axis',(0.0450737186086209,0.584827952222913,-0.809904084561589));
#53050=DIRECTION('ref_axis',(-0.998316194260093,-0.00326197146239322,-0.0579149015385696));
#53051=DIRECTION('center_axis',(-0.0213712893727949,-4.10500129431464E-10,
0.9997716079138));
#53052=DIRECTION('ref_axis',(0.999648646751534,-0.0156832196310207,0.0213686609274604));
#53053=DIRECTION('',(0.0213713430443167,8.32140417652696E-8,-0.999771606766503));
#53054=DIRECTION('center_axis',(0.080225227444987,0.584827969931439,-0.807180375422539));
#53055=DIRECTION('ref_axis',(-0.995561971316665,0.00704480135439165,-0.0938441902408085));
#53056=DIRECTION('center_axis',(0.0841054060144577,4.23273412101713E-10,
-0.996456863431199));
#53057=DIRECTION('ref_axis',(0.996334492612421,0.0156715280540825,0.0840950773779236));
#53058=DIRECTION('',(-0.0841053488789075,-1.40443212613677E-11,0.996456868253693));
#53059=DIRECTION('',(-0.69183347372805,-3.07809289802329E-8,-0.722057092361385));
#53060=DIRECTION('center_axis',(-0.608404332892848,0.79362626038425,-0.00123553458889862));
#53061=DIRECTION('ref_axis',(-0.793626866138329,-0.608404797271895,-2.90994740798271E-19));
#53062=DIRECTION('center_axis',(0.616382652636135,0.471546674578011,-0.630647412762204));
#53063=DIRECTION('ref_axis',(0.78707911312239,-0.393406599041741,0.475118635202708));
#53064=DIRECTION('center_axis',(-0.0132942036922927,-0.601098528044386,
0.799064342672766));
#53065=DIRECTION('ref_axis',(-0.999829102807158,-0.00227572108321212,-0.0183462877276236));
#53066=DIRECTION('',(-0.764072871230124,5.05127141378843E-12,0.645129946173757));
#53067=DIRECTION('center_axis',(0.,-1.,1.45983193964168E-32));
#53068=DIRECTION('ref_axis',(1.,0.,0.));
#53069=DIRECTION('center_axis',(0.00988022742892383,0.601098527162617,-0.79911384780198));
#53070=DIRECTION('ref_axis',(-0.999868664172006,-0.00432812016876069,-0.015617995476148));
#53071=DIRECTION('center_axis',(0.0208641859867265,-0.601098528288371,-0.798902525363805));
#53072=DIRECTION('ref_axis',(-0.999715453639247,-0.00330177928429916,-0.0236243520214359));
#53073=DIRECTION('center_axis',(-0.0242771432463745,0.60109852769626,0.798806096820238));
#53074=DIRECTION('ref_axis',(-0.999605402018444,-0.00330190886658757,-0.0278951188092559));
#53075=DIRECTION('center_axis',(-0.0567768155313816,0.584828375911606,-0.809167574700512));
#53076=DIRECTION('ref_axis',(-0.998386871228108,-0.0330794214893115,0.0461455006829729));
#53077=DIRECTION('center_axis',(0.0414944557150844,-1.50624413674013E-7,
0.999138734183039));
#53078=DIRECTION('ref_axis',(0.999015977020359,-0.0156751609036203,-0.0414893599456838));
#53079=DIRECTION('',(-0.041447008323888,-4.4408920985015E-13,-0.99914070355531));
#53080=DIRECTION('center_axis',(-0.0215713945108209,0.584827952225678,-0.810870483637417));
#53081=DIRECTION('ref_axis',(-0.999689123679031,-0.0227607296123229,0.0101786632406399));
#53082=DIRECTION('center_axis',(0.0213714187153477,5.88437628125681E-10,
-0.999771605148943));
#53083=DIRECTION('ref_axis',(0.999648484439658,0.0156933905086753,0.0213687868592492));
#53084=DIRECTION('',(-0.0213713417386148,-2.36477504241347E-11,0.999771606794418));
#53085=DIRECTION('',(-0.735806627489112,0.,-0.677191706197809));
#53086=DIRECTION('center_axis',(0.0869599425730912,-0.601098528069535,0.794429687222427));
#53087=DIRECTION('ref_axis',(-0.995899323085398,-0.0324816854912687,0.0844362385809061));
#53088=DIRECTION('',(-0.722057103471557,8.1518485824276E-12,0.691833462132518));
#53089=DIRECTION('center_axis',(0.,-1.,1.45983193964168E-32));
#53090=DIRECTION('ref_axis',(1.,0.,0.));
#53091=DIRECTION('center_axis',(-0.090353228593366,0.601098519348321,-0.794050920357134));
#53092=DIRECTION('ref_axis',(-0.99559708246167,-0.0345386226702202,0.0871408798317705));
#53093=DIRECTION('center_axis',(0.0208641849024253,-0.601098531590183,-0.798902522907822));
#53094=DIRECTION('ref_axis',(-0.999437989418741,-0.033509941682649,-0.000888321478876713));
#53095=DIRECTION('center_axis',(-0.0242771705949099,0.601098523543119,0.79880609911429));
#53096=DIRECTION('ref_axis',(-0.999425068545745,-0.0335100884017672,-0.00515813315444326));
#53097=DIRECTION('',(-0.104101785979609,-4.44089209850367E-13,-0.99456664842325));
#53098=DIRECTION('center_axis',(-0.123030318860491,0.584827952146009,-0.801772914876645));
#53099=DIRECTION('ref_axis',(-0.992104105100685,-0.0526562728490771,0.113827771532309));
#53100=DIRECTION('center_axis',(-0.0414469425911784,4.75766052612418E-10,
-0.999140706282075));
#53101=DIRECTION('ref_axis',(0.99901641168037,0.0157729998146264,-0.0414417865218749));
#53102=DIRECTION('',(0.0414470083264018,-1.77746706219692E-10,0.999140703555206));
#53103=DIRECTION('',(-0.776875900241758,0.,-0.629653742642381));
#53104=DIRECTION('',(-0.677191706222999,6.51326541667412E-11,0.735806627465928));
#53105=DIRECTION('center_axis',(0.,-1.,1.45983193964168E-32));
#53106=DIRECTION('ref_axis',(1.,0.,0.));
#53107=DIRECTION('center_axis',(0.00215530640688391,0.601098539803382,-0.799172009082234));
#53108=DIRECTION('ref_axis',(-0.998023518743271,0.0514848633080921,0.0360328306610393));
#53109=DIRECTION('center_axis',(0.167595042660841,0.601098537659878,0.781404152598812));
#53110=DIRECTION('ref_axis',(-0.98393380773214,0.0525164847285,0.170634934387698));
#53111=DIRECTION('center_axis',(-0.0646072654724011,0.584827923044615,-0.808580361915562));
#53112=DIRECTION('ref_axis',(-0.995196652942778,0.021959669079551,0.0954012311524769));
#53113=DIRECTION('center_axis',(0.166350249831606,-1.30064135257624E-8,
0.986066729172505));
#53114=DIRECTION('ref_axis',(0.985944587101618,-0.0157391391447165,-0.166329644573669));
#53115=DIRECTION('',(-0.166345721445869,3.88578058619102E-13,-0.986067493104125));
#53116=DIRECTION('center_axis',(-0.0294084954082734,0.584827952319998,-0.81062408463049));
#53117=DIRECTION('ref_axis',(-0.997706929940489,0.0322834330689216,0.0594866531081364));
#53118=DIRECTION('center_axis',(-0.104101714517271,5.33328897972409E-10,
-0.994566655903245));
#53119=DIRECTION('ref_axis',(0.994444040496267,0.0157020800824344,-0.104088880302097));
#53120=DIRECTION('',(0.104101785979298,-1.22124532708759E-12,0.994566648423282));
#53121=DIRECTION('',(-0.814879198737126,0.,-0.579630823426032));
#53122=DIRECTION('center_axis',(0.0946350700368982,-0.601098528112436,0.793551991378116));
#53123=DIRECTION('ref_axis',(-0.990470182848417,0.023272369138899,0.135746873713121));
#53124=DIRECTION('',(-0.629653742642369,0.,0.776875900241768));
#53125=DIRECTION('center_axis',(0.,-1.,1.45983193964168E-32));
#53126=DIRECTION('ref_axis',(1.,0.,0.));
#53127=DIRECTION('center_axis',(-0.0980245238225754,0.601098533435455,-0.7931404326039));
#53128=DIRECTION('ref_axis',(-0.990141758144127,0.0212179918813064,0.138452503046286));
#53129=DIRECTION('center_axis',(-0.170932004530704,-0.60109852490719,-0.780680993224195));
#53130=DIRECTION('ref_axis',(-0.980058890457948,0.0222452907071548,0.197458143097949));
#53131=DIRECTION('center_axis',(0.167595116543381,0.601098530461403,0.781404142289988));
#53132=DIRECTION('ref_axis',(-0.980893534367322,0.0222451443138458,0.193269314146968));
#53133=DIRECTION('center_axis',(-0.165440957226946,0.584827953375188,-0.794106765254409));
#53134=DIRECTION('ref_axis',(-0.980087919791214,-0.0078464289079487,0.198408928813002));
#53135=DIRECTION('center_axis',(0.227933641184126,-1.25033758461367E-9,
0.973676668723528));
#53136=DIRECTION('ref_axis',(0.973556998972359,-0.0156778482793224,-0.22790562701536));
#53137=DIRECTION('',(-0.227933166345836,3.88578058618775E-13,-0.973676779881066));
#53138=DIRECTION('center_axis',(-0.130774737773183,0.584827952254203,-0.800546209923269));
#53139=DIRECTION('ref_axis',(-0.986627807192036,0.00246180457580221,0.162970885723999));
#53140=DIRECTION('center_axis',(-0.166345641911318,6.12618273329711E-10,
-0.986067506521289));
#53141=DIRECTION('ref_axis',(0.985946423748941,0.0156707406188289,-0.166325215722484));
#53142=DIRECTION('',(0.16634572144638,-6.41708908203574E-11,0.986067493104039));
#53143=DIRECTION('',(-0.849666541318022,1.64268989064345E-13,-0.527320366157681));
#53144=DIRECTION('center_axis',(0.193347264597227,-0.60109852814683,0.775433681711392));
#53145=DIRECTION('ref_axis',(-0.971515582976909,-0.00691951581125515,0.23687463421391));
#53146=DIRECTION('',(-0.579630823436063,2.36136671785042E-11,0.814879198729991));
#53147=DIRECTION('center_axis',(0.,-1.,1.45983193964168E-32));
#53148=DIRECTION('ref_axis',(1.,0.,0.));
#53149=DIRECTION('center_axis',(-0.196658430624571,0.60109852592005,-0.774600557578565));
#53150=DIRECTION('ref_axis',(-0.970849864666905,-0.00897214799424333,0.239520439287802));
#53151=DIRECTION('center_axis',(-0.17093200004291,-0.60109852895254,-0.780680991092023));
#53152=DIRECTION('ref_axis',(-0.975532185834689,-0.00794566528748167,0.219713041951845));
#53153=DIRECTION('center_axis',(0.167595094659997,0.601098527004474,0.781404149642781));
#53154=DIRECTION('ref_axis',(-0.976461947719334,-0.00794582307778729,0.215543333350353));
#53155=DIRECTION('center_axis',(-0.263664517425136,0.584827952230139,-0.767109697853751));
#53156=DIRECTION('ref_axis',(-0.949715452919976,-0.0181546317036599,0.312587536272178));
#53157=DIRECTION('center_axis',(0.288621117749965,-4.46288586079944E-10,
0.957443392785579));
#53158=DIRECTION('ref_axis',(0.957325693290781,-0.0156795066178608,-0.288585637268293));
#53159=DIRECTION('',(-0.288621060077174,2.06171493654015E-7,-0.957443410171006));
#53160=DIRECTION('center_axis',(-0.230084567678364,0.58482778253655,-0.777841601156458));
#53161=DIRECTION('ref_axis',(-0.96397680426132,-0.0273551074224977,0.264575922835083));
#53162=DIRECTION('center_axis',(-0.227933076190557,6.11666218383047E-10,
-0.973676800985989));
#53163=DIRECTION('ref_axis',(0.9735567572018,0.0157023279251935,-0.227904974505702));
#53164=DIRECTION('',(-0.227933165424191,-1.29267396645822E-5,-0.973676780011009));
#53165=DIRECTION('',(-0.881100657021103,-7.62629077545992E-8,-0.472928781315934));
#53166=DIRECTION('center_axis',(0.288621063162946,6.19194292263073E-12,
0.957443409240823));
#53167=DIRECTION('ref_axis',(0.739027825212226,-0.635772805085107,-0.222779742966684));
#53168=DIRECTION('',(0.527320366158135,0.,-0.84966654131774));
#53169=DIRECTION('center_axis',(-0.316586779698294,0.398564391555877,-0.860766656361617));
#53170=DIRECTION('ref_axis',(2.94490590170337E-16,0.907442263779439,0.420176793631974));
#53171=DIRECTION('center_axis',(0.35471924586863,5.74456547725441E-5,0.934972862339002));
#53172=DIRECTION('ref_axis',(0.93497280964334,-0.000363109780049791,-0.354719203566606));
#53173=DIRECTION('',(-0.348169046786133,5.94973699394781E-5,-0.937431763554073));
#53174=DIRECTION('center_axis',(-0.218761792525728,0.590180063808641,-0.777065486567097));
#53175=DIRECTION('ref_axis',(0.319217807250868,0.795820705788151,0.514557475674775));
#53176=DIRECTION('center_axis',(-0.832564763033601,0.550037558033772,-0.0655331985107512));
#53177=DIRECTION('ref_axis',(-0.551222471627934,-0.834358308385787,-6.13931407995218E-17));
#53178=DIRECTION('center_axis',(0.366173894521264,-0.477126090432259,-0.798916374096788));
#53179=DIRECTION('ref_axis',(0.881350386866143,-0.0976339845307942,0.462265184321229));
#53180=DIRECTION('center_axis',(0.245072617384947,0.584827951389285,-0.773250075642999));
#53181=DIRECTION('ref_axis',(-0.95854002435476,0.026548969010481,-0.283718476582785));
#53182=DIRECTION('center_axis',(-0.208331315235233,-3.25592671745016E-11,
0.978058312725963));
#53183=DIRECTION('ref_axis',(0.977937029805949,-0.015747767057039,0.208305481365794));
#53184=DIRECTION('center_axis',(0.260557615828758,-0.00011544123373398,
-0.965458292991963));
#53185=DIRECTION('ref_axis',(0.0240700430029388,0.999689938683564,0.00637648215625154));
#53186=DIRECTION('',(-0.269333009814431,-6.06514838087046E-10,0.963047106752468));
#53187=DIRECTION('center_axis',(-0.211595760985938,-0.601098528097979,0.770654133480918));
#53188=DIRECTION('ref_axis',(-0.969283979365573,0.0279220118464045,-0.244354104937259));
#53189=DIRECTION('',(-0.871424337485721,2.24206636476429E-10,0.490529942039803));
#53190=DIRECTION('center_axis',(0.,-1.,1.45983193964168E-32));
#53191=DIRECTION('ref_axis',(1.,0.,0.));
#53192=DIRECTION('center_axis',(0.208301364394399,0.601098533826222,-0.771551096314041));
#53193=DIRECTION('ref_axis',(-0.969999761963384,0.0258667218163505,-0.241725825044521));
#53194=DIRECTION('center_axis',(0.120828674064531,-0.60109852420491,-0.789987971884691));
#53195=DIRECTION('ref_axis',(-0.984886142419322,0.026894459919668,-0.171102234047416));
#53196=DIRECTION('center_axis',(-0.124202644056001,0.601098530459505,0.789464539981957));
#53197=DIRECTION('ref_axis',(-0.984146173822937,0.0268943232999321,-0.175308311052021));
#53198=DIRECTION('center_axis',(0.146226196685621,0.58482795222256,-0.797868514043527));
#53199=DIRECTION('ref_axis',(-0.983185511002024,-0.00326197145263899,-0.182580422000639));
#53200=DIRECTION('center_axis',(-0.146507360718647,-5.54529865880287E-10,
0.989209580046239));
#53201=DIRECTION('ref_axis',(0.989087917901018,-0.015683219631045,0.146489341879311));
#53202=DIRECTION('',(0.146507431922858,8.32148189213204E-8,-0.989209569500499));
#53203=DIRECTION('center_axis',(0.180759154061358,0.584827969932013,-0.790760629905298));
#53204=DIRECTION('ref_axis',(-0.975949872003341,0.00704480134002263,-0.217881201829672));
#53205=DIRECTION('center_axis',(0.208331415279698,7.80545475967607E-10,
-0.978058291415986));
#53206=DIRECTION('ref_axis',(0.977938180049076,0.0156715280545262,0.208305830957121));
#53207=DIRECTION('',(-0.208331314487837,-1.44328993199869E-11,0.978058312885162));
#53208=DIRECTION('',(-0.595880409943332,-3.07809289802393E-8,-0.803073182870507));
#53209=DIRECTION('center_axis',(-0.603452029460871,0.793626260384574,-0.0774790743849719));
#53210=DIRECTION('ref_axis',(-0.796019110999669,-0.605271488609282,-3.39050861409775E-17));
#53211=DIRECTION('center_axis',(0.690563370785492,0.4715466745671,-0.548421338602072));
#53212=DIRECTION('ref_axis',(0.721326027536678,-0.393427780058085,0.570002933217648));
#53213=DIRECTION('center_axis',(-0.113338608937478,-0.601098527844478,0.791097288294758));
#53214=DIRECTION('ref_axis',(-0.989645761738707,-0.00227577203245932,-0.143513369183052));
#53215=DIRECTION('',(-0.838904150647018,7.57690712069459E-12,0.544279180225742));
#53216=DIRECTION('center_axis',(0.,-1.,1.45983193964168E-32));
#53217=DIRECTION('ref_axis',(1.,0.,0.));
#53218=DIRECTION('center_axis',(0.109957852882409,0.601098527208925,-0.791574273948284));
#53219=DIRECTION('ref_axis',(-0.990026945959674,-0.00432811321328217,-0.140811624909925));
#53220=DIRECTION('center_axis',(0.120828705633355,-0.60109852827952,-0.789987963955884));
#53221=DIRECTION('ref_axis',(-0.988871481869316,-0.00330178122241446,-0.148735639933211));
#53222=DIRECTION('center_axis',(-0.124202642833808,0.601098527766976,0.78946454222433));
#53223=DIRECTION('ref_axis',(-0.988227031801981,-0.00330189731720042,-0.152958919615538));
#53224=DIRECTION('center_axis',(0.0450828641671435,0.584828255987828,-0.809903356183145));
#53225=DIRECTION('ref_axis',(-0.996298020780763,-0.0330815410749405,-0.0793464897045918));
#53226=DIRECTION('center_axis',(-0.0840714188105122,-1.08029305018116E-7,
0.99645973151913));
#53227=DIRECTION('ref_axis',(0.99633730370572,-0.0156751635313067,0.0840610878628315));
#53228=DIRECTION('',(0.0841053488787466,4.44089209849881E-13,-0.996456868253706));
#53229=DIRECTION('center_axis',(0.0802277221187175,0.584827952226099,-0.807180140302442));
#53230=DIRECTION('ref_axis',(-0.993082001121473,-0.0227607295978636,-0.115195869009022));
#53231=DIRECTION('center_axis',(0.146507493237112,4.80800404034445E-10,
-0.989209560419519));
#53232=DIRECTION('ref_axis',(0.989087740412835,0.0156933905088255,0.14648945101737));
#53233=DIRECTION('',(-0.146507430631075,-2.24820162482982E-11,0.989209569691823));
#53234=DIRECTION('',(-0.645129946175771,0.,-0.764072871228423));
#53235=DIRECTION('center_axis',(-0.0132941449757976,-0.601098526145228,
0.799064345078291));
#53236=DIRECTION('ref_axis',(-0.998629027060397,-0.0324817210721147,-0.0410488015488608));
#53237=DIRECTION('',(-0.803073192440483,1.02462781930395E-11,0.595880397045793));
#53238=DIRECTION('center_axis',(0.,-1.,1.45983193964168E-32));
#53239=DIRECTION('ref_axis',(1.,0.,0.));
#53240=DIRECTION('center_axis',(0.00988020448522983,0.601098519395469,-0.799113853928153));
#53241=DIRECTION('ref_axis',(-0.998668150326737,-0.0345386218180123,-0.0383276548445816));
#53242=DIRECTION('center_axis',(0.120828713187755,-0.601098531192363,-0.789987960584068));
#53243=DIRECTION('ref_axis',(-0.991445784674722,-0.0335099490343529,-0.126144121410551));
#53244=DIRECTION('center_axis',(-0.124202696628462,0.601098523288246,0.789464537171182));
#53245=DIRECTION('ref_axis',(-0.990897816933698,-0.0335100928779197,-0.130378641162362));
#53246=DIRECTION('',(0.021371341738508,-7.77156117237601E-13,-0.99977160679442));
#53247=DIRECTION('center_axis',(-0.0215713960520066,0.58482795214548,-0.810870483654259));
#53248=DIRECTION('ref_axis',(-0.99854747058022,-0.0526562728540313,-0.0114134099622345));
#53249=DIRECTION('center_axis',(0.0841054675363998,8.95626188632988E-10,
-0.996456858238471));
#53250=DIRECTION('ref_axis',(0.996332897509981,0.0157729998150688,0.084095004704203));
#53251=DIRECTION('',(-0.0841053488765219,-1.77302617009861E-10,0.996456868253894));
#53252=DIRECTION('',(-0.691833462135605,0.,-0.722057103468599));
#53253=DIRECTION('',(-0.764072871250423,6.51326541667476E-11,0.645129946149715));
#53254=DIRECTION('center_axis',(0.,-1.,1.45983193964168E-32));
#53255=DIRECTION('ref_axis',(1.,0.,0.));
#53256=DIRECTION('center_axis',(0.102301128745808,0.601098539514464,-0.792600167077267));
#53257=DIRECTION('ref_axis',(-0.994669915818139,0.0514848666272864,-0.0893368181362392));
#53258=DIRECTION('center_axis',(0.0683376233553293,0.601098536259686,0.796247774841857));
#53259=DIRECTION('ref_axis',(-0.997561422019287,0.0525165008945674,0.0459698426432973));
#53260=DIRECTION('center_axis',(0.0372448546931241,0.584827908068242,-0.810301881241437));
#53261=DIRECTION('ref_axis',(-0.999306149480362,0.021960067725517,-0.0300828029981178));
#53262=DIRECTION('center_axis',(0.0414539038352585,-1.93069262314765E-8,
0.99914041748736));
#53263=DIRECTION('ref_axis',(0.999016656034164,-0.0157391387097842,-0.0414487693302229));
#53264=DIRECTION('',(-0.0414470083237126,-1.60982338570645E-12,-0.999140703555317));
#53265=DIRECTION('center_axis',(0.0724215370721092,0.584827952320769,-0.807917933426663));
#53266=DIRECTION('ref_axis',(-0.997295367386826,0.0322834330562048,-0.0660282525808609));
#53267=DIRECTION('center_axis',(0.0213714252574956,6.25304076798456E-10,
-0.999771605009096));
#53268=DIRECTION('ref_axis',(0.999648347907534,0.0157020800826177,0.021368790485612));
#53269=DIRECTION('',(-0.0213713417391225,-1.60982338570518E-12,0.999771606794407));
#53270=DIRECTION('',(-0.735806627488928,0.,-0.677191706198008));
#53271=DIRECTION('center_axis',(-0.00556959565550501,-0.601098528052763,
0.799155516265161));
#53272=DIRECTION('ref_axis',(-0.9996736242306,0.0232723708321993,0.0105376360491782));
#53273=DIRECTION('',(-0.722057103468721,0.,0.691833462135478));
#53274=DIRECTION('center_axis',(0.,-1.,1.45983193964168E-32));
#53275=DIRECTION('ref_axis',(1.,0.,0.));
#53276=DIRECTION('center_axis',(0.00215530436841184,0.601098532989542,-0.799172014212772));
#53277=DIRECTION('ref_axis',(-0.999686894498085,0.0212180041744757,0.0132630791156127));
#53278=DIRECTION('center_axis',(-0.0717388699212962,-0.601098525174619,
-0.79594855209072));
#53279=DIRECTION('ref_axis',(-0.997078901768021,0.0222452838102306,0.0730671677108043));
#53280=DIRECTION('center_axis',(0.0683376830885089,0.601098530194654,0.796247774293857));
#53281=DIRECTION('ref_axis',(-0.997381963140672,0.0222451515272063,0.0688067789915375));
#53282=DIRECTION('center_axis',(-0.0646084828443836,0.584827953016101,-0.808580242966364));
#53283=DIRECTION('ref_axis',(-0.997226863463135,-0.0078464556861505,0.0740068640103327));
#53284=DIRECTION('center_axis',(0.104102207062556,-1.53723582553726E-9,
0.994566604348198));
#53285=DIRECTION('ref_axis',(0.994444367120634,-0.0156778483100078,-0.104089412403035));
#53286=DIRECTION('',(-0.104101785979623,0.,-0.994566648423248));
#53287=DIRECTION('center_axis',(-0.0294084948096632,0.584827952254358,-0.810624084699563));
#53288=DIRECTION('ref_axis',(-0.999273620325167,0.00246180456904867,0.038028558222716));
#53289=DIRECTION('center_axis',(-0.0414469199711997,6.73631675134276E-10,
-0.99914070722041));
#53290=DIRECTION('ref_axis',(0.999018019141589,0.0156707406190299,-0.0414418305443513));
#53291=DIRECTION('',(0.0414470083242613,-6.4614980030209E-11,0.999140703555294));
#53292=DIRECTION('',(-0.776875900241837,1.64268989064397E-13,-0.629653742642284));
#53293=DIRECTION('center_axis',(0.0946350652757326,-0.601098528055325,0.79355199198917));
#53294=DIRECTION('ref_axis',(-0.993543155106225,-0.00691952328441555,0.113243627366327));
#53295=DIRECTION('',(-0.677191706207015,2.34699318130683E-11,0.735806627480639));
#53296=DIRECTION('center_axis',(0.,-1.,1.45983193964168E-32));
#53297=DIRECTION('ref_axis',(1.,0.,0.));
#53298=DIRECTION('center_axis',(-0.09802452438425,0.601098525946293,-0.793140438210305));
#53299=DIRECTION('ref_axis',(-0.993214294979514,-0.00897214607806965,0.115951993700411));
#53300=DIRECTION('center_axis',(-0.0717388784411376,-0.601098528963249,
-0.795948548461662));
#53301=DIRECTION('ref_axis',(-0.995377169084396,-0.00794566452399397,0.0957139367114593));
#53302=DIRECTION('center_axis',(0.0683376456977897,0.601098526979802,0.796247779929838));
#53303=DIRECTION('ref_axis',(-0.995776996739739,-0.00794582476184027,0.0914605741991623));
#53304=DIRECTION('center_axis',(-0.165441105016554,0.58482795223037,-0.794106735307625));
#53305=DIRECTION('ref_axis',(-0.981404269601245,-0.0181546317005234,0.191091781498484));
#53306=DIRECTION('center_axis',(0.166345793588914,-5.72962025682916E-10,
0.986067480933873));
#53307=DIRECTION('ref_axis',(0.985946262651246,-0.0156795066181454,-0.166325344539709));
#53308=DIRECTION('',(-0.166345718259955,2.06171882231989E-7,-0.986067493641555));
#53309=DIRECTION('center_axis',(-0.130780879077022,0.584827782536271,-0.800545330660013));
#53310=DIRECTION('ref_axis',(-0.989535715164436,-0.0273551074289179,0.14167133270906));
#53311=DIRECTION('center_axis',(-0.104101642227122,1.01911928448842E-9,
-0.994566663469883));
#53312=DIRECTION('ref_axis',(0.99444404419175,0.0157023279255542,-0.104088807608093));
#53313=DIRECTION('',(-0.104101785049298,-1.29267396645623E-5,-0.994566648436619));
#53314=DIRECTION('',(-0.814879221760667,-7.6262887221002E-8,-0.579630791058173));
#53315=DIRECTION('center_axis',(0.166345721445505,1.76912654930784E-13,
0.986067493104186));
#53316=DIRECTION('ref_axis',(0.761122075630443,-0.635772805085226,-0.128398311134019));
#53317=DIRECTION('',(0.6296537426427,0.,-0.7768759002415));
#53318=DIRECTION('center_axis',(-0.206207729994026,0.398564391559433,-0.893658098979453));
#53319=DIRECTION('ref_axis',(1.81224450895921E-16,0.913286229134016,0.407318381213235));
#53320=DIRECTION('center_axis',(0.234739006587026,5.74456419399389E-5,0.972058432135916));
#53321=DIRECTION('ref_axis',(0.972058374626882,-0.000362894799268911,-0.234738971253411));
#53322=DIRECTION('',(-0.227932275687093,5.94973683762914E-5,-0.973676986561851));
#53323=DIRECTION('center_axis',(-0.1196446603478,0.590180063809313,-0.798356215941414));
#53324=DIRECTION('ref_axis',(0.252206560643778,0.795821124358454,0.550509390286017));
#53325=DIRECTION('center_axis',(-0.817786253526483,0.550037558034545,-0.169364483568763));
#53326=DIRECTION('ref_axis',(-0.558100160398776,-0.829773590181599,6.40047726430736E-17));
#53327=DIRECTION('center_axis',(0.463417276847617,-0.477126089246125,-0.746722922160447));
#53328=DIRECTION('ref_axis',(0.816468152271752,-0.0976221507206682,0.569077913834848));
#53329=DIRECTION('center_axis',(0.340054078907099,0.584827951390133,-0.736437024253577));
#53330=DIRECTION('ref_axis',(-0.915422295877618,0.026548968994854,-0.401618192386079));
#53331=DIRECTION('center_axis',(-0.329271771466537,-4.74095418533005E-11,
0.944235193431853));
#53332=DIRECTION('ref_axis',(0.944118104706356,-0.0157477670569709,0.329230940524122));
#53333=DIRECTION('center_axis',(0.379507057814437,-0.000115441161244248,
-0.925188834639917));
#53334=DIRECTION('ref_axis',(0.0230516160204343,0.99969073081804,0.00933090110008984));
#53335=DIRECTION('',(-0.387911046549999,-6.0690341614628E-10,0.921696815641936));
#53336=DIRECTION('center_axis',(-0.306515843341055,-0.601098527987144,0.738057313108278));
#53337=DIRECTION('ref_axis',(-0.931015194377809,0.0279220141825818,-0.36391079808332));
#53338=DIRECTION('',(-0.926032600098767,2.24062901110949E-10,0.377443536908922));
#53339=DIRECTION('center_axis',(0.,-1.,1.45983193964168E-32));
#53340=DIRECTION('ref_axis',(1.,0.,0.));
#53341=DIRECTION('center_axis',(0.30335983449366,0.601098533973444,-0.739360103921598));
#53342=DIRECTION('ref_axis',(-0.932054746514114,0.0258667184698823,-0.361392947324807));
#53343=DIRECTION('center_axis',(0.218887642670481,-0.601098523971291,-0.768614834859239));
#53344=DIRECTION('ref_axis',(-0.95567522663093,0.0268944650784618,-0.293192000150183));
#53345=DIRECTION('center_axis',(-0.222169422774876,0.601098530737144,0.767672654149883));
#53346=DIRECTION('ref_axis',(-0.954413927449797,0.0268943169511852,-0.297272183033635));
#53347=DIRECTION('center_axis',(0.245072600276168,0.58482795222252,-0.773250080435231));
#53348=DIRECTION('ref_axis',(-0.952549404908864,-0.00326197145103078,-0.304366540128876));
#53349=DIRECTION('center_axis',(-0.269332908043605,-8.28266897459133E-10,
0.963047135214458));
#53350=DIRECTION('ref_axis',(0.962928690770987,-0.0156832196310515,0.269299782978149));
#53351=DIRECTION('',(0.269333011080688,8.3214818921303E-8,-0.963047106398334));
#53352=DIRECTION('center_axis',(0.278442400844468,0.584827969932124,-0.761870116881506));
#53353=DIRECTION('ref_axis',(-0.940946460207726,0.00704480132855519,-0.338482096715308));
#53354=DIRECTION('center_axis',(0.329271851494279,6.43150047631334E-10,
-0.944235165524738));
#53355=DIRECTION('ref_axis',(0.944119207837706,0.0156715280545467,0.329231414965733));
#53356=DIRECTION('',(-0.329271770815784,-1.48214773786022E-11,0.944235193658782));
#53357=DIRECTION('',(-0.490529956132129,-3.07809289802454E-8,-0.871424329553066));
#53358=DIRECTION('center_axis',(-0.588982927039396,0.793626260385285,-0.152500722893282));
#53359=DIRECTION('ref_axis',(-0.803018883943793,-0.595953582109937,3.751356198321E-17));
#53360=DIRECTION('center_axis',(0.753853492055292,0.47154667454953,-0.457546332339493));
#53361=DIRECTION('ref_axis',(0.644196855355331,-0.393421735031793,0.655919011734586));
#53362=DIRECTION('center_axis',(-0.211595771064685,-0.601098528069342,0.770654130735969));
#53363=DIRECTION('ref_axis',(-0.96385509500095,-0.0022757160895087,-0.266417298531812));
#53364=DIRECTION('',(-0.900505410469423,5.19500677922231E-12,0.43484480647157));
#53365=DIRECTION('center_axis',(0.,-1.,1.45983193964168E-32));
#53366=DIRECTION('ref_axis',(1.,0.,0.));
#53367=DIRECTION('center_axis',(0.208301378683891,0.601098527259043,-0.771551097572546));
#53368=DIRECTION('ref_axis',(-0.964571908712687,-0.00432810514597244,-0.26378457200566));
#53369=DIRECTION('center_axis',(0.21888768672917,-0.601098528263956,-0.76861481895502));
#53370=DIRECTION('ref_axis',(-0.962432414917285,-0.00330178468193749,-0.271501279802502));
#53371=DIRECTION('center_axis',(-0.222169419447295,0.601098527734523,0.767672657464001));
#53372=DIRECTION('ref_axis',(-0.961263728712235,-0.00330190212277808,-0.275610488379203));
#53373=DIRECTION('center_axis',(0.146235178796552,0.584828255987166,-0.797866645174086));
#53374=DIRECTION('ref_axis',(-0.978497161184359,-0.0330815410904191,-0.203590071450535));
#53375=DIRECTION('center_axis',(-0.208297965837032,-1.08390100212757E-7,
0.97806541572031));
#53376=DIRECTION('ref_axis',(0.977945248097851,-0.0156751635316394,0.208272372078222));
#53377=DIRECTION('',(0.208331314487311,3.88578058618561E-13,-0.978058312885274));
#53378=DIRECTION('center_axis',(0.180761599638725,0.584827952226355,-0.790760083964016));
#53379=DIRECTION('ref_axis',(-0.970813382163765,-0.0227607295866176,-0.23875369358491));
#53380=DIRECTION('center_axis',(0.269333103715099,7.48422893903147E-10,
-0.963047080491495));
#53381=DIRECTION('ref_axis',(0.9629284823617,0.0156933905083944,0.269299935668288));
#53382=DIRECTION('',(-0.269333009823168,-2.20934381896949E-11,0.963047106750025));
#53383=DIRECTION('',(-0.544279180229307,0.,-0.838904150644705));
#53384=DIRECTION('center_axis',(-0.113338678411945,-0.601098527569091,0.791097278550561));
#53385=DIRECTION('ref_axis',(-0.98560975486667,-0.0324816945160823,-0.165886559530982));
#53386=DIRECTION('',(-0.871424337430412,8.00811321699429E-12,0.490529942138059));
#53387=DIRECTION('center_axis',(0.,-1.,1.45983193964168E-32));
#53388=DIRECTION('ref_axis',(1.,0.,0.));
#53389=DIRECTION('center_axis',(0.10995783127813,0.601098519808573,-0.791574282568953));
#53390=DIRECTION('ref_axis',(-0.985989623433843,-0.0345386145953561,-0.163191747899895));
#53391=DIRECTION('center_axis',(0.218887680548057,-0.601098531456249,-0.768614818218744));
#53392=DIRECTION('ref_axis',(-0.967817889648016,-0.0335099442410043,-0.249410537295892));
#53393=DIRECTION('center_axis',(-0.222169453489029,0.601098523668802,0.767672650795619));
#53394=DIRECTION('ref_axis',(-0.966743517525389,-0.0335100860343741,-0.253542985421816));
#53395=DIRECTION('',(0.146507430630888,0.,-0.98920956969185));
#53396=DIRECTION('center_axis',(0.080227720602025,0.58482795214713,-0.807180140510406));
#53397=DIRECTION('ref_axis',(-0.989243145943592,-0.0526562728337357,-0.136474595199564));
#53398=DIRECTION('center_axis',(0.208331373152654,4.29367531478973E-10,
-0.978058300389261));
#53399=DIRECTION('ref_axis',(0.977936628468742,0.0157729998144705,0.208305456424077));
#53400=DIRECTION('',(-0.208331314485257,-1.76081371683112E-10,0.978058312885712));
#53401=DIRECTION('',(-0.595880397050137,0.,-0.803073192437259));
#53402=DIRECTION('',(-0.83890415066404,6.73708191429374E-11,0.544279180199506));
#53403=DIRECTION('center_axis',(0.,-1.,1.45983193964168E-32));
#53404=DIRECTION('ref_axis',(1.,0.,0.));
#53405=DIRECTION('center_axis',(0.200833593520141,0.601098539633411,-0.773528547220054));
#53406=DIRECTION('ref_axis',(-0.97562977458375,0.051484865311369,-0.21329756583124));
#53407=DIRECTION('center_axis',(-0.0319975640352948,0.601098537119618,0.798534097311106));
#53408=DIRECTION('ref_axis',(-0.995456900744133,0.0525164909496035,-0.0794202552200983));
#53409=DIRECTION('center_axis',(0.138507934572584,0.584827930050219,-0.799244545989282));
#53410=DIRECTION('ref_axis',(-0.987656085635407,0.0219594825865639,-0.155091062385544));
#53411=DIRECTION('center_axis',(-0.0841018096930555,-1.0371211046821E-8,
0.996457166970238));
#53412=DIRECTION('ref_axis',(0.996333737901996,-0.0157391393485509,0.0840913920137152));
#53413=DIRECTION('',(0.08410534887882,-3.88578058619033E-13,-0.9964568682537));
#53414=DIRECTION('center_axis',(0.173109438633622,0.584827952322477,-0.792470433794379));
#53415=DIRECTION('ref_axis',(-0.981155861141504,0.0322834330334646,-0.190501853269852));
#53416=DIRECTION('center_axis',(0.146507522183494,6.95832293934272E-10,
-0.989209556132397));
#53417=DIRECTION('ref_axis',(0.989087601174383,0.0157020800821761,0.146489459976472));
#53418=DIRECTION('',(-0.146507430631413,-1.16573417585542E-12,0.989209569691773));
#53419=DIRECTION('',(-0.645129946175793,-1.64268989064484E-13,-0.764072871228405));
#53420=DIRECTION('center_axis',(-0.105686420127036,-0.601098528110706,0.792155881189981));
#53421=DIRECTION('ref_axis',(-0.993111615389959,0.0232723692717861,-0.114837782136476));
#53422=DIRECTION('',(-0.803073192437354,1.43735365432664E-13,0.595880397050009));
#53423=DIRECTION('center_axis',(0.,-1.,1.45983193964168E-32));
#53424=DIRECTION('ref_axis',(1.,0.,0.));
#53425=DIRECTION('center_axis',(0.102301118167672,0.601098533074067,-0.792600173326911));
#53426=DIRECTION('ref_axis',(-0.993466369715916,0.0212180019323403,-0.112135492318351));
#53427=DIRECTION('center_axis',(0.0285856187492689,-0.601098525185125,-0.798663524533949));
#53428=DIRECTION('ref_axis',(-0.998374381198037,0.0222452835218335,-0.052476111979347));
#53429=DIRECTION('center_axis',(-0.0319974908985116,0.601098530253856,0.79853410540994));
#53430=DIRECTION('ref_axis',(-0.998141084474372,0.0222451499143489,-0.0567408916885656));
#53431=DIRECTION('center_axis',(0.0372429508152893,0.584827953016182,-0.810301936308604));
#53432=DIRECTION('ref_axis',(-0.998638951358832,-0.00784645567012263,-0.0515623696347268));
#53433=DIRECTION('center_axis',(-0.0213710049213545,-8.58526880578322E-10,
0.999771613994242));
#53434=DIRECTION('ref_axis',(0.999648737047707,-0.0156778483081366,0.0213683783041829));
#53435=DIRECTION('',(0.0213713417385381,-3.88578058618843E-13,-0.999771606794419));
#53436=DIRECTION('center_axis',(0.0724215377014447,0.584827952254335,-0.807917933418339));
#53437=DIRECTION('ref_axis',(-0.996160291529796,0.00246180457187916,-0.087513502372616));
#53438=DIRECTION('center_axis',(0.0841054050042859,4.22320839248603E-10,
-0.996456863516462));
#53439=DIRECTION('ref_axis',(0.99633450499547,0.0156707406185972,0.0840950774058495));
#53440=DIRECTION('',(-0.0841053488781393,-6.50035580887595E-11,0.996456868253758));
#53441=DIRECTION('',(-0.691833462135694,1.64268989064481E-13,-0.722057103468513));
#53442=DIRECTION('center_axis',(-0.00556958958256345,-0.601098527996718,
0.799155516349641));
#53443=DIRECTION('ref_axis',(-0.999901960614497,-0.00691952812673157,-0.012173302337035));
#53444=DIRECTION('',(-0.764072871236518,2.36136671785041E-11,0.645129946166184));
#53445=DIRECTION('center_axis',(0.,-1.,1.45983193964168E-32));
#53446=DIRECTION('ref_axis',(1.,0.,0.));
#53447=DIRECTION('center_axis',(0.00215529775560142,0.601098526063912,-0.79917201943973));
#53448=DIRECTION('ref_axis',(-0.999915141883942,-0.00897213785214235,-0.00944509256586728));
#53449=DIRECTION('center_axis',(0.028585614071655,-0.601098528930697,-0.798663521882337));
#53450=DIRECTION('ref_axis',(-0.999524459852295,-0.0079456673545495,-0.029794639237111));
#53451=DIRECTION('center_axis',(-0.0319975271426687,0.601098526968027,0.798534106431042));
#53452=DIRECTION('ref_axis',(-0.999388047168573,-0.00794582543224992,-0.0340645715485336));
#53453=DIRECTION('center_axis',(-0.0646085875882672,0.584827952229195,-0.808580235166094));
#53454=DIRECTION('ref_axis',(-0.997615754686242,-0.0181546317615242,0.066582395176232));
#53455=DIRECTION('center_axis',(0.0414484569980076,-4.97663449248963E-9,
0.99914064345941));
#53456=DIRECTION('ref_axis',(0.999017818082041,-0.0156795063500311,-0.0414433617750534));
#53457=DIRECTION('',(-0.0414470050956686,2.06171493653918E-7,-0.999140703689204));
#53458=DIRECTION('center_axis',(-0.0294146978379073,0.584827782536786,-0.810623982080601));
#53459=DIRECTION('ref_axis',(-0.999489056723302,-0.0273551074064042,0.0165325009949378));
#53460=DIRECTION('center_axis',(0.0213714460906926,7.0386369386079E-10,
-0.999771604563759));
#53461=DIRECTION('ref_axis',(0.999648343570961,0.0157023279251134,0.021368811234293));
#53462=DIRECTION('',(0.0213713426633156,-1.29267396290012E-5,-0.999771606691082));
#53463=DIRECTION('',(-0.735806654387649,-7.62629077546487E-8,-0.677191676971039));
#53464=DIRECTION('center_axis',(0.041447206939856,-1.61525101140892E-7,
0.99914069531616));
#53465=DIRECTION('ref_axis',(0.771212966511889,-0.635772804014362,-0.0319922171730482));
#53466=DIRECTION('',(0.722057103468862,0.,-0.69183346213533));
#53467=DIRECTION('center_axis',(-0.0925766612059187,0.398564391554733,-0.912456019534405));
#53468=DIRECTION('ref_axis',(-6.9062910639093E-17,0.916391407641987,0.400283384616372));
#53469=DIRECTION('center_axis',(0.111056792872745,5.7445687582888E-5,0.99381405980033));
#53470=DIRECTION('ref_axis',(0.993813998268466,-0.000363029792981438,-0.111056765012375));
#53471=DIRECTION('',(-0.10410087644023,5.9497368305179E-5,-0.994566741845131));
#53472=DIRECTION('center_axis',(-0.0186406604881565,0.590180063812162,-0.807056390876894));
#53473=DIRECTION('ref_axis',(0.181223283205387,0.795820770431835,0.577778004923639));
#53474=DIRECTION('center_axis',(-0.790110766279426,0.550037558035771,-0.270524789546882));
#53475=DIRECTION('ref_axis',(-0.571341150200151,-0.820712672064936,-1.98680099173155E-16));
#53476=DIRECTION('center_axis',(0.553352291168644,-0.477126090543816,-0.682753202541582));
#53477=DIRECTION('ref_axis',(0.738701542742593,-0.0976315438263697,0.666924367825762));
#53478=DIRECTION('center_axis',(0.429672684498432,0.584827951389853,-0.688009921054238));
#53479=DIRECTION('ref_axis',(-0.857867810937999,0.0265489689994253,-0.513184149405954));
#53480=DIRECTION('center_axis',(-0.44501941753188,-2.58199235088207E-13,
0.895520919922916));
#53481=DIRECTION('ref_axis',(0.895409871950847,-0.0157477670569058,0.444964233445442));
#53482=DIRECTION('center_axis',(0.492471434687182,-0.000115441210406181,
-0.870328600409337));
#53483=DIRECTION('ref_axis',(0.0217249806890136,0.999690027137922,0.0121603805467594));
#53484=DIRECTION('',(-0.50037149435502,-6.06903416145897E-10,0.86581081515359));
#53485=DIRECTION('center_axis',(-0.396601982854688,-0.601098528025573,0.693820889568208));
#53486=DIRECTION('ref_axis',(-0.878063744941495,0.0279220134200669,-0.477728396671044));
#53487=DIRECTION('',(-0.966036775423284,2.24206636476442E-10,0.258404621726826));
#53488=DIRECTION('center_axis',(0.,-1.,1.45983193964168E-32));
#53489=DIRECTION('ref_axis',(1.,0.,0.));
#53490=DIRECTION('center_axis',(0.393634151697023,0.60109853374655,-0.695508955618483));
#53491=DIRECTION('ref_axis',(-0.879410666406445,0.0258667235993845,-0.475360697177213));
#53492=DIRECTION('center_axis',(0.313494643752222,-0.601098524363107,-0.735120175445595));
#53493=DIRECTION('ref_axis',(-0.911392736151507,0.0268944565563492,-0.410657970453282));
#53494=DIRECTION('center_axis',(-0.316632441871935,0.601098530599997,0.733774115968082));
#53495=DIRECTION('ref_axis',(-0.909630006253576,0.0268943200603761,-0.41454788296602));
#53496=DIRECTION('center_axis',(0.340054062537767,0.584827952222704,-0.736437031151041));
#53497=DIRECTION('ref_axis',(-0.906891025682966,-0.00326197146399792,-0.421352616080481));
#53498=DIRECTION('center_axis',(-0.387910988888561,-4.91125118611069E-10,
0.921696839909685));
#53499=DIRECTION('ref_axis',(0.921583481107603,-0.015683219630754,0.387863279999029));
#53500=DIRECTION('',(0.387911047762143,8.3213597675953E-8,-0.921696815131782));
#53501=DIRECTION('center_axis',(0.371734444692853,0.584827969931374,-0.720964456970553));
#53502=DIRECTION('ref_axis',(-0.891103760619904,0.0070448013553493,-0.453744926784783));
#53503=DIRECTION('center_axis',(0.445019483355182,5.75499300180527E-10,
-0.895520887212737));
#53504=DIRECTION('ref_axis',(0.89541091192758,0.0156715280541854,0.444964832328877));
#53505=DIRECTION('',(-0.445019414620638,-1.44328993199847E-11,0.895520921369626));
#53506=DIRECTION('',(-0.377443551884409,-3.07809289802548E-8,-0.926032593994877));
#53507=DIRECTION('center_axis',(-0.565225212017908,0.793626260385261,-0.225117343903613));
#53508=DIRECTION('ref_axis',(-0.814533996880245,-0.58011582285462,-1.01709000961919E-17));
#53509=DIRECTION('center_axis',(0.805254893431975,0.471546674524301,-0.359455547111087));
#53510=DIRECTION('ref_axis',(0.556909986835466,-0.39342664753178,0.731482562727797));
#53511=DIRECTION('center_axis',(-0.306515839351534,-0.601098528038064,0.738057314723659));
#53512=DIRECTION('ref_axis',(-0.922863871513281,-0.00227572262241581,-0.385119586287253));
#53513=DIRECTION('',(-0.947905162033643,5.19500677922257E-12,0.318552670354485));
#53514=DIRECTION('center_axis',(0.,-1.,1.45983193964168E-32));
#53515=DIRECTION('ref_axis',(1.,0.,0.));
#53516=DIRECTION('center_axis',(0.303359854367542,0.601098527259698,-0.739360101225597));
#53517=DIRECTION('ref_axis',(-0.923904997618405,-0.00432810492030727,-0.382597468475071));
#53518=DIRECTION('center_axis',(0.313494662811144,-0.601098528298344,-0.735120164100055));
#53519=DIRECTION('ref_axis',(-0.920815217868027,-0.0033017783155422,-0.389985169977799));
#53520=DIRECTION('center_axis',(-0.316632443585747,0.601098527734296,0.733774117576097));
#53521=DIRECTION('ref_axis',(-0.919140723420251,-0.00330190204970445,-0.393915508698696));
#53522=DIRECTION('center_axis',(0.24507260052094,0.584827952239687,-0.77325008034467));
#53523=DIRECTION('ref_axis',(-0.945267066533668,-0.0330869090465625,-0.324615818124407));
#53524=DIRECTION('center_axis',(-0.329271704502654,-5.5048012952267E-10,
0.944235216783359));
#53525=DIRECTION('ref_axis',(0.944119205188345,-0.0156751701945281,0.329231249175864));
#53526=DIRECTION('',(0.329271770815259,3.88578058618359E-13,-0.944235193658965));
#53527=DIRECTION('center_axis',(0.278444758722175,0.584827952226138,-0.761869268729965));
#53528=DIRECTION('ref_axis',(-0.933234456237909,-0.0227607295922861,-0.358546229765089));
#53529=DIRECTION('center_axis',(0.387911135664321,7.42148139023014E-10,
-0.921696778136724));
#53530=DIRECTION('ref_axis',(0.921583272247153,0.0156933905090626,0.387863364870362));
#53531=DIRECTION('',(-0.387911046558538,-2.20379270384585E-11,0.921696815638342));
#53532=DIRECTION('',(-0.434844806474186,0.,-0.900505410468159));
#53533=DIRECTION('center_axis',(-0.211595749425156,-0.601098527583133,0.770654137056693));
#53534=DIRECTION('ref_axis',(-0.957046828571228,-0.0324816942905735,-0.28810815236256));
#53535=DIRECTION('',(-0.926032600056252,8.17238220606226E-12,0.37744353701323));
#53536=DIRECTION('center_axis',(0.,-1.,1.45983193964168E-32));
#53537=DIRECTION('ref_axis',(1.,0.,0.));
#53538=DIRECTION('center_axis',(0.208301341754461,0.601098519678007,-0.771551113448876));
#53539=DIRECTION('ref_axis',(-0.957761452083959,-0.0345386168713349,-0.285482197074776));
#53540=DIRECTION('center_axis',(0.313494679133752,-0.601098531002521,-0.735120154928048));
#53541=DIRECTION('ref_axis',(-0.928926923074171,-0.0335099525260047,-0.368743616445977));
#53542=DIRECTION('center_axis',(-0.31663247868647,0.601098523595813,0.733774105819901));
#53543=DIRECTION('ref_axis',(-0.927343093225053,-0.0335100873639033,-0.372708815957785));
#53544=DIRECTION('',(0.269333009822791,8.32667268467739E-13,-0.96304710675013));
#53545=DIRECTION('center_axis',(0.180761598115075,0.584827952145732,-0.790760084371937));
#53546=DIRECTION('ref_axis',(-0.96433786595444,-0.0526562728494128,-0.259383494494242));
#53547=DIRECTION('center_axis',(0.329271876752694,8.41810918162305E-10,
-0.944235156716672));
#53548=DIRECTION('ref_axis',(0.944117692442974,0.0157729998149326,0.329230914850038));
#53549=DIRECTION('',(-0.329271770813475,-1.76136882834204E-10,0.944235193659588));
#53550=DIRECTION('',(-0.490529942141654,0.,-0.871424337428388));
#53551=DIRECTION('',(-0.900505410483609,6.73708191429276E-11,0.434844806442192));
#53552=DIRECTION('center_axis',(0.,-1.,1.45983193964168E-32));
#53553=DIRECTION('ref_axis',(1.,0.,0.));
#53554=DIRECTION('center_axis',(0.296198809704822,0.601098538800504,-0.742257914596635));
#53555=DIRECTION('ref_axis',(-0.941203364053214,0.0514848748675469,-0.333894497041784));
#53556=DIRECTION('center_axis',(-0.131828106546344,0.601098536710114,0.788227060871019));
#53557=DIRECTION('ref_axis',(-0.977653429390555,0.0525164956588446,-0.203557828846257));
#53558=DIRECTION('center_axis',(0.237588622522883,0.584827908067953,-0.775582338886427));
#53559=DIRECTION('ref_axis',(-0.960429820312543,0.0219600677334787,-0.277655029991458));
#53560=DIRECTION('center_axis',(-0.208324618392494,-1.88734789164305E-8,
0.978059739163013));
#53561=DIRECTION('ref_axis',(0.977938589004,-0.0157391387081356,0.20829881336578));
#53562=DIRECTION('',(0.20833131448726,8.32667268468638E-13,-0.978058312885285));
#53563=DIRECTION('center_axis',(0.271067301054217,0.584827952319284,-0.764525201994817));
#53564=DIRECTION('ref_axis',(-0.949542940826784,0.032283433081186,-0.311971126026936));
#53565=DIRECTION('center_axis',(0.269333078423088,5.28470611559298E-10,
-0.963047087564852));
#53566=DIRECTION('ref_axis',(0.962928358052914,0.0157020800824718,0.269299873632726));
#53567=DIRECTION('',(-0.26933300982351,0.,0.963047106749929));
#53568=DIRECTION('',(-0.544279180229341,0.,-0.838904150644683));
#53569=DIRECTION('center_axis',(-0.204136505045659,-0.601098528206328,0.772663475709788));
#53570=DIRECTION('ref_axis',(-0.970887643980288,0.0232723666889749,-0.238402138654625));
#53571=DIRECTION('',(-0.871424337428441,0.,0.49052994214156));
#53572=DIRECTION('center_axis',(0.,-1.,1.45983193964168E-32));
#53573=DIRECTION('ref_axis',(1.,0.,0.));
#53574=DIRECTION('center_axis',(0.200833592354618,0.601098532928243,-0.773528552733158));
#53575=DIRECTION('ref_axis',(-0.971578285480988,0.0212180058948169,-0.235765628130294));
#53576=DIRECTION('center_axis',(0.128459301139359,-0.601098525336866,-0.78878309489278));
#53577=DIRECTION('ref_axis',(-0.983924899358624,0.0222452795628364,-0.177191816851943));
#53578=DIRECTION('center_axis',(-0.131828036158469,0.601098530106885,0.788227077678726));
#53579=DIRECTION('ref_axis',(-0.983158925334848,0.0222451538963128,-0.181393717263182));
#53580=DIRECTION('center_axis',(0.138507040834489,0.58482795301623,-0.799244684067476));
#53581=DIRECTION('ref_axis',(-0.984301906436154,-0.00784645568808815,-0.17631843386126));
#53582=DIRECTION('center_axis',(-0.146507111242795,-7.49259406551241E-10,
0.989209616994948));
#53583=DIRECTION('ref_axis',(0.989088038172257,-0.0156778483085329,0.146489104772234));
#53584=DIRECTION('',(0.146507430631052,-4.44089209850505E-13,-0.989209569691826));
#53585=DIRECTION('center_axis',(0.173109439256193,0.584827952254779,-0.792470433708342));
#53586=DIRECTION('ref_axis',(-0.977336919866491,0.0024618045487747,-0.211675422721308));
#53587=DIRECTION('center_axis',(0.208331416101965,7.95303813231119E-10,
-0.978058291240839));
#53588=DIRECTION('ref_axis',(0.977938191944633,0.0156707406189369,0.208305834350639));
#53589=DIRECTION('',(-0.208331314486965,-6.3837823912962E-11,0.978058312885348));
#53590=DIRECTION('',(-0.595880397050185,1.64268989064468E-13,-0.803073192437223));
#53591=DIRECTION('center_axis',(-0.105686432079547,-0.60109852811121,0.792155879594939));
#53592=DIRECTION('ref_axis',(-0.990491714011746,-0.00691951878544824,-0.137398270490755));
#53593=DIRECTION('',(-0.838904150651509,2.34493981894382E-11,0.54427918021882));
#53594=DIRECTION('center_axis',(0.,-1.,1.45983193964168E-32));
#53595=DIRECTION('ref_axis',(1.,0.,0.));
#53596=DIRECTION('center_axis',(0.102301118391204,0.601098526083832,-0.79260017859937));
#53597=DIRECTION('ref_axis',(-0.990846728085701,-0.00897213638327582,-0.134693215161644));
#53598=DIRECTION('center_axis',(0.128459309556313,-0.601098528782676,-0.788783090896108));
#53599=DIRECTION('ref_axis',(-0.987908649882266,-0.00794567944767794,-0.154833348042058));
#53600=DIRECTION('center_axis',(-0.131828062205383,0.601098527104583,0.788227075612019));
#53601=DIRECTION('ref_axis',(-0.987238153221425,-0.00794581535552585,-0.159052484552382));
#53602=DIRECTION('center_axis',(0.037242845866466,0.584827952228643,-0.810301941700634));
#53603=DIRECTION('ref_axis',(-0.998094243374912,-0.0181546317616234,-0.0589770352549358));
#53604=DIRECTION('center_axis',(-0.084103933977164,-4.74152240553405E-9,
0.996456987676621));
#53605=DIRECTION('ref_axis',(0.996334492213274,-0.0156795063497496,0.0840935949210542));
#53606=DIRECTION('',(0.0841053520983884,2.06170327919954E-7,-0.996456867981933));
#53607=DIRECTION('center_axis',(0.0724153707322235,0.584827782537017,-0.807918609053257));
#53608=DIRECTION('ref_axis',(-0.993679858785782,-0.0273551073987626,-0.108867058115254));
#53609=DIRECTION('center_axis',(0.146507538530465,7.41923804238371E-10,
-0.989209553711318));
#53610=DIRECTION('ref_axis',(0.989087594903337,0.0157023279249282,0.146489475751914));
#53611=DIRECTION('',(0.146507431535495,-1.29267395934322E-5,-0.989209569473411));
#53612=DIRECTION('',(-0.645129976525437,-7.62630514900407E-8,-0.764072845603273));
#53613=DIRECTION('center_axis',(-0.0841051507916142,-1.61528648367539E-7,
0.9964568849731));
#53614=DIRECTION('ref_axis',(0.769141409948316,-0.635772804014554,0.0649186658688223));
#53615=DIRECTION('',(0.803073192437323,0.,-0.59588039705005));
#53616=DIRECTION('center_axis',(0.0225143968323005,0.398564391561196,-0.916863963581693));
#53617=DIRECTION('ref_axis',(3.39181432986796E-17,0.917096430247481,0.39866544574032));
#53618=DIRECTION('center_axis',(-0.0143768528108244,5.7445659478889E-5,
0.999896646060608));
#53619=DIRECTION('ref_axis',(0.999896581537589,-0.000362987245248623,0.0143768727372876));
#53620=DIRECTION('',(0.0213722558148867,5.94973683407431E-5,-0.999771585484128));
#53621=DIRECTION('center_axis',(0.0826573141490685,0.590180063802952,-0.803028804406919));
#53622=DIRECTION('ref_axis',(0.107376602486449,0.795821166339074,0.595935345859921));
#53623=DIRECTION('center_axis',(-0.749974760259059,0.550037558037291,-0.367418757989764));
#53624=DIRECTION('ref_axis',(-0.591402864747467,-0.806376246902455,1.34536393528168E-16));
#53625=DIRECTION('center_axis',(0.634560609589244,-0.477126090761952,-0.608016057577384));
#53626=DIRECTION('ref_axis',(0.64929247946224,-0.0976240300752894,0.754247190823828));
#53627=DIRECTION('center_axis',(0.512515095169429,0.584827951389991,-0.628732490409441));
#53628=DIRECTION('ref_axis',(-0.786784238160081,0.0265489689956428,-0.616656885819115));
#53629=DIRECTION('center_axis',(-0.553748840165996,1.08058537688362E-11,
0.832683746697877));
#53630=DIRECTION('ref_axis',(0.832580490772235,-0.0157477670557757,0.553680173221167));
#53631=DIRECTION('center_axis',(0.597669253808723,-0.000115441150256891,
-0.801742757825143));
#53632=DIRECTION('ref_axis',(0.0190168739071945,0.999720685825276,0.0140324210255403));
#53633=DIRECTION('',(-0.604940784786227,-6.06181771179997E-10,0.796270460900204));
#53634=DIRECTION('center_axis',(-0.480433469444791,-0.601098528159146,0.638642498493601));
#53635=DIRECTION('ref_axis',(-0.811264707648814,0.0279220105145261,-0.584011930916065));
#53636=DIRECTION('',(-0.990805973716841,2.24350371841859E-10,0.135290511297072));
#53637=DIRECTION('center_axis',(0.,-1.,1.45983193964168E-32));
#53638=DIRECTION('ref_axis',(1.,0.,0.));
#53639=DIRECTION('center_axis',(0.477700620491674,0.601098533573279,-0.640689214922433));
#53640=DIRECTION('ref_axis',(-0.812897754247503,0.0258667274892258,-0.581831722707145));
#53641=DIRECTION('center_axis',(0.403157636441818,-0.601098524456693,-0.690032234083766));
#53642=DIRECTION('ref_axis',(-0.852737039489665,0.0268944544782255,-0.521647610749557));
#53643=DIRECTION('center_axis',(-0.406101978505186,0.60109853045139,0.688303522977584));
#53644=DIRECTION('ref_axis',(-0.850500677540323,0.0268943233501674,-0.525285915359424));
#53645=DIRECTION('center_axis',(0.429672669126836,0.584827952222689,-0.6880099299461));
#53646=DIRECTION('ref_axis',(-0.84693043322058,-0.00326197145677045,-0.531693709598878));
#53647=DIRECTION('center_axis',(-0.500371404828997,-8.11024626575273E-10,
0.865810866892681));
#53648=DIRECTION('ref_axis',(0.865704381467998,-0.0156832196312531,0.500309864513093));
#53649=DIRECTION('',(0.50037149549337,8.32135976759965E-8,-0.865810814495708));
#53650=DIRECTION('center_axis',(0.459164014243506,0.584827969931117,-0.668688756904166));
#53651=DIRECTION('ref_axis',(-0.827207822419288,0.00704480135620463,-0.561851928271312));
#53652=DIRECTION('center_axis',(0.55374888242709,4.06970665576237E-10,-0.83268371859353));
#53653=DIRECTION('ref_axis',(0.832581460086186,0.0156715280544909,0.553680878782347));
#53654=DIRECTION('',(-0.55374883641498,-1.32116539928992E-11,0.832683749192366));
#53655=DIRECTION('',(-0.258404637349593,-3.0780928980269E-8,-0.966036771244358));
#53656=DIRECTION('center_axis',(-0.532553557753611,0.793626260385853,-0.2941837299205));
#53657=DIRECTION('ref_axis',(-0.830371106917834,-0.557210754379392,1.99771634101076E-17));
#53658=DIRECTION('center_axis',(0.843956944123754,0.471546674539063,-0.255695933085463));
#53659=DIRECTION('ref_axis',(0.460837498610183,-0.39342086414382,0.795517959276244));
#53660=DIRECTION('center_axis',(-0.396601983388789,-0.601098528044585,0.693820889246434));
#53661=DIRECTION('ref_axis',(-0.867318529731536,-0.00227572042476273,-0.497748319013611));
#53662=DIRECTION('',(-0.980355882941529,5.05127141378872E-12,0.197236768331708));
#53663=DIRECTION('center_axis',(0.,-1.,1.45983193964168E-32));
#53664=DIRECTION('ref_axis',(1.,0.,0.));
#53665=DIRECTION('center_axis',(0.393634171246799,0.601098527296137,-0.695508950128797));
#53666=DIRECTION('ref_axis',(-0.868667549393486,-0.00432809960814291,-0.495376580173606));
#53667=DIRECTION('center_axis',(0.40315766119088,-0.601098528266436,-0.69003221630517));
#53668=DIRECTION('ref_axis',(-0.864676207687786,-0.00330178542044302,-0.502318777343339));
#53669=DIRECTION('center_axis',(-0.406101983502883,0.601098527737377,0.688303522399081));
#53670=DIRECTION('ref_axis',(-0.862522320557366,-0.00330190096595632,-0.506008244982577));
#53671=DIRECTION('center_axis',(0.340062297717029,0.584828255987335,-0.736432987223025));
#53672=DIRECTION('ref_axis',(-0.897125081634952,-0.0330815410846242,-0.44053626359353));
#53673=DIRECTION('center_axis',(-0.444988893932816,-1.08268168110917E-7,
0.895536087646075));
#53674=DIRECTION('ref_axis',(0.895426060219439,-0.0156751635312524,0.444934219776545));
#53675=DIRECTION('',(0.445019414620048,3.8857805861828E-13,-0.89552092136992));
#53676=DIRECTION('center_axis',(0.371736677655948,0.584827952226369,-0.72096331999626));
#53677=DIRECTION('ref_axis',(-0.88093786543938,-0.0227607295790456,-0.472684277741643));
#53678=DIRECTION('center_axis',(0.500371546002264,4.5264802562808E-10,-0.865810785305487));
#53679=DIRECTION('ref_axis',(0.865704161711832,0.015693390508689,0.500309925835133));
#53680=DIRECTION('',(-0.50037149436294,-2.12607709212252E-11,0.865810815149013));
#53681=DIRECTION('',(-0.318552670357103,0.,-0.947905162032763));
#53682=DIRECTION('center_axis',(-0.306515838597793,-0.601098527943026,0.73805731511409));
#53683=DIRECTION('ref_axis',(-0.91339069879748,-0.0324816877714825,-0.405786115225456));
#53684=DIRECTION('',(-0.966036775394095,8.00811321699466E-12,0.258404621835947));
#53685=DIRECTION('center_axis',(0.,-1.,1.45983193964168E-32));
#53686=DIRECTION('ref_axis',(1.,0.,0.));
#53687=DIRECTION('center_axis',(0.303359823568943,0.601098519834244,-0.73936011989916));
#53688=DIRECTION('ref_axis',(-0.914428808686088,-0.0345386141111437,-0.403270427852358));
#53689=DIRECTION('center_axis',(0.40315766702957,-0.601098530966851,-0.690032210541485));
#53690=DIRECTION('ref_axis',(-0.875386226563281,-0.0335099532194896,-0.482261378692642));
#53691=DIRECTION('center_axis',(-0.406102014405697,0.60109852375045,0.68830350764809));
#53692=DIRECTION('ref_axis',(-0.873317916729201,-0.0335100846096989,-0.485996800966035));
#53693=DIRECTION('',(0.387911046558289,7.77156117236932E-13,-0.921696815638447));
#53694=DIRECTION('center_axis',(0.278444757278483,0.584827952146073,-0.76186926931906));
#53695=DIRECTION('ref_axis',(-0.924224401747177,-0.0526562728447773,-0.378201761160852));
#53696=DIRECTION('center_axis',(0.44501947109597,4.54565369276803E-10,-0.89552089330482));
#53697=DIRECTION('ref_axis',(0.895409489159723,0.0157729998144009,0.444964110012907));
#53698=DIRECTION('',(-0.445019414618126,-1.75304215565769E-10,0.895520921370875));
#53699=DIRECTION('',(-0.37744353701714,-1.43735365431523E-13,-0.926032600054658));
#53700=DIRECTION('',(-0.947905162043636,6.51326541667543E-11,0.31855267032475));
#53701=DIRECTION('center_axis',(0.,-1.,1.45983193964168E-32));
#53702=DIRECTION('ref_axis',(1.,0.,0.));
#53703=DIRECTION('center_axis',(0.386892778599255,0.601098538778694,-0.699281434435283));
#53704=DIRECTION('ref_axis',(-0.891933617243813,0.0514848751370183,-0.449225700581002));
#53705=DIRECTION('center_axis',(-0.229579642912527,0.601098536382064,0.765489214241127));
#53706=DIRECTION('ref_axis',(-0.944431780630213,0.0525164994541969,-0.324485175348155));
#53707=DIRECTION('center_axis',(0.332920489062412,0.584827930050483,-0.73968928625154));
#53708=DIRECTION('ref_axis',(-0.918057474730095,0.0219594825824973,-0.395838671957289));
#53709=DIRECTION('center_axis',(-0.329268426587499,-1.02921683725058E-8,
0.944236359844606));
#53710=DIRECTION('ref_axis',(0.944119399299011,-0.0157391393486129,0.329227640637658));
#53711=DIRECTION('',(0.32927177081541,1.16573417585652E-12,-0.944235193658913));
#53712=DIRECTION('center_axis',(0.364750270111432,0.584827952319838,-0.724522951078172));
#53713=DIRECTION('ref_axis',(-0.902955161127037,0.0322834330697393,-0.428520427684933));
#53714=DIRECTION('center_axis',(0.387911115801846,5.59178227092144E-10,
-0.92169678649617));
#53715=DIRECTION('ref_axis',(0.92158315486564,0.0157020800826605,0.387863292087524));
#53716=DIRECTION('',(-0.387911046558911,0.,0.921696815638185));
#53717=DIRECTION('',(-0.434844806474091,-1.64268989064544E-13,-0.900505410468205));
#53718=DIRECTION('center_axis',(-0.299367242653868,-0.601098528133014,0.740985703979601));
#53719=DIRECTION('ref_axis',(-0.933352193011291,0.0232723686584569,-0.35820675685704));
#53720=DIRECTION('',(-0.926032600054671,0.,0.377443537017109));
#53721=DIRECTION('center_axis',(0.,-1.,1.45983193964168E-32));
#53722=DIRECTION('ref_axis',(1.,0.,0.));
#53723=DIRECTION('center_axis',(0.296198799055564,0.601098532815511,-0.742257923693026));
#53724=DIRECTION('ref_axis',(-0.934367830445983,0.0212180089737124,-0.3556775977242));
#53725=DIRECTION('center_axis',(0.226307099698326,-0.60109852540265,-0.766463084163153));
#53726=DIRECTION('ref_axis',(-0.95395833364752,0.0222452778845224,-0.299113097801297));
#53727=DIRECTION('center_axis',(-0.22957958291146,0.601098530145375,0.765489237133527));
#53728=DIRECTION('ref_axis',(-0.952671761995156,0.0222451527836799,-0.303185862260555));
#53729=DIRECTION('center_axis',(0.237586792125608,0.584827953016327,-0.775582865706945));
#53730=DIRECTION('ref_axis',(-0.954441832450582,-0.0078464556792525,-0.298293851095942));
#53731=DIRECTION('center_axis',(-0.269332588157193,-1.65064812737033E-9,
0.963047224676209));
#53732=DIRECTION('ref_axis',(0.962928861348009,-0.0156778483098861,0.269299485806043));
#53733=DIRECTION('',(0.269333009823076,7.77156117237388E-13,-0.96304710675005));
#53734=DIRECTION('center_axis',(0.271067301623241,0.584827952254122,-0.764525201842912));
#53735=DIRECTION('ref_axis',(-0.943100361129656,0.00246180457329884,-0.332499095269981));
#53736=DIRECTION('center_axis',(0.329271815799476,3.54739971595345E-10,
-0.94423517797216));
#53737=DIRECTION('ref_axis',(0.944119231938393,0.0156707406186497,0.329231383334763));
#53738=DIRECTION('',(-0.329271770814866,-6.33937347031782E-11,0.944235193659102));
#53739=DIRECTION('',(-0.49052994214159,1.64268989064518E-13,-0.871424337428425));
#53740=DIRECTION('center_axis',(-0.204136514467861,-0.60109852806508,0.772663473330341));
#53741=DIRECTION('ref_axis',(-0.965460822828727,-0.00691952277231014,-0.260456368298956));
#53742=DIRECTION('',(-0.900505410473572,2.35931335548655E-11,0.434844806462977));
#53743=DIRECTION('center_axis',(0.,-1.,1.45983193964168E-32));
#53744=DIRECTION('ref_axis',(1.,0.,0.));
#53745=DIRECTION('center_axis',(0.200833585503954,0.601098526072395,-0.773528559839402));
#53746=DIRECTION('ref_axis',(-0.966152069761189,-0.00897213720975653,-0.257817142273473));
#53747=DIRECTION('center_axis',(0.226307095413984,-0.601098528854831,-0.766463082720782));
#53748=DIRECTION('ref_axis',(-0.960712933164148,-0.00794567351718236,-0.277430218836191));
#53749=DIRECTION('center_axis',(-0.229579616820753,0.601098527017376,0.765489229419969));
#53750=DIRECTION('ref_axis',(-0.95951892089988,-0.0079458216776583,-0.281532066296179));
#53751=DIRECTION('center_axis',(0.138506937414431,0.584827952228472,-0.799244702566321));
#53752=DIRECTION('ref_axis',(-0.982832189620029,-0.0181546317366621,-0.183606362616349));
#53753=DIRECTION('center_axis',(-0.208331222268825,-7.38316845110491E-10,
0.978058332528269));
#53754=DIRECTION('ref_axis',(0.977938098822323,-0.015679506618582,0.208305611887868));
#53755=DIRECTION('',(0.208331317647447,2.06171549165144E-7,-0.978058312212128));
#53756=DIRECTION('center_axis',(0.173103405619857,0.584827782536667,-0.792471876937));
#53757=DIRECTION('ref_axis',(-0.972199735881759,-0.0273551074073029,-0.232549718662854));
#53758=DIRECTION('center_axis',(0.269333098110424,6.04766748526227E-10,
-0.963047082058941));
#53759=DIRECTION('ref_axis',(0.96292834879903,0.0157023279251934,0.269299892270502));
#53760=DIRECTION('',(0.269333010693047,-1.2926740481586E-5,-0.963047106419991));
#53761=DIRECTION('',(-0.544279213551348,-7.6263051490058E-8,-0.838904129025433));
#53762=DIRECTION('center_axis',(-0.208331314516526,2.31191508624251E-11,
0.978058312879051));
#53763=DIRECTION('ref_axis',(0.754939979655494,-0.635772805085298,0.160805993146194));
#53764=DIRECTION('',(0.871424337428539,0.,-0.490529942141387));
#53765=DIRECTION('center_axis',(0.137250389382567,0.398564391564464,-0.906812415216721));
#53766=DIRECTION('ref_axis',(-4.29084615902504E-17,0.915476128559304,0.402372287860469));
#53767=DIRECTION('center_axis',(-0.139583766916631,5.7445652467052E-5,0.990210264900017));
#53768=DIRECTION('ref_axis',(0.990210198381314,-0.000363006345283363,0.139583778599206));
#53769=DIRECTION('',(0.146508334828672,5.9497368376234E-5,-0.989209433985439));
#53770=DIRECTION('center_axis',(0.182651732966148,0.590180063810584,-0.786336974028945));
#53771=DIRECTION('ref_axis',(0.0318357966482478,0.795821663447861,0.604693610052935));
#53772=DIRECTION('center_axis',(-0.698011204256667,0.550037558037817,-0.458518313134768));
#53773=DIRECTION('ref_axis',(-0.618934249318816,-0.785442801876849,1.08964565723535E-17));
#53774=DIRECTION('center_axis',(0.70576152845033,-0.477126090197719,-0.523690136447205));
#53775=DIRECTION('ref_axis',(0.54964196122163,-0.0976209307608887,0.829676966259651));
#53776=DIRECTION('center_axis',(0.587274836641366,0.584827951389706,-0.559539572792825));
#53777=DIRECTION('ref_axis',(-0.703292607934828,0.0265489690024795,-0.71040457478055));
#53778=DIRECTION('center_axis',(-0.653745311499404,2.14805049941619E-11,
0.756714654075463));
#53779=DIRECTION('ref_axis',(0.756620818603737,-0.0157477670561346,0.653664244615045));
#53780=DIRECTION('center_axis',(0.693441464837208,-0.000115441142812938,
-0.720512957217127));
#53781=DIRECTION('ref_axis',(0.017310355292461,0.999714013427519,0.016499786552871));
#53782=DIRECTION('',(-0.699969797667544,-6.06958927296982E-10,0.714172445809314));
#53783=DIRECTION('center_axis',(-0.556688241105297,-0.601098528020006,0.573392328015707));
#53784=DIRECTION('ref_axis',(-0.731671536606546,0.0279220135032058,-0.681085254341733));
#53785=DIRECTION('',(-0.999949569926115,2.24206636476405E-10,0.0100427886853574));
#53786=DIRECTION('center_axis',(0.,-1.,1.45983193964168E-32));
#53787=DIRECTION('ref_axis',(1.,0.,0.));
#53788=DIRECTION('center_axis',(0.554233466834936,0.60109853330817,-0.575765418807777));
#53789=DIRECTION('ref_axis',(-0.733564955864417,0.0258667335491262,-0.679126915696275));
#53790=DIRECTION('center_axis',(0.486462590005111,-0.601098524487545,-0.63406207297426));
#53791=DIRECTION('ref_axis',(-0.780633170909662,0.0268944538704173,-0.624410554704626));
#53792=DIRECTION('center_axis',(-0.489167050999535,0.601098530508858,0.631977968632222));
#53793=DIRECTION('ref_axis',(-0.777958442290685,0.0268943220480753,-0.627739880452265));
#53794=DIRECTION('center_axis',(0.512515081052865,0.584827952222668,-0.628732501142112));
#53795=DIRECTION('ref_axis',(-0.77361324188928,-0.0032619714457999,-0.633649675700892));
#53796=DIRECTION('center_axis',(-0.604940734512417,-4.95210567798345E-10,
0.796270499094106));
#53797=DIRECTION('ref_axis',(0.796172566385581,-0.015683219631898,0.604866333297676));
#53798=DIRECTION('',(0.604940785833409,8.32148189212586E-8,-0.796270460104637));
#53799=DIRECTION('center_axis',(0.539352292991265,0.584827969931393,-0.605867435691167));
#53800=DIRECTION('ref_axis',(-0.750266322713667,0.00704480135244388,-0.661098189209149));
#53801=DIRECTION('center_axis',(0.653745360770694,5.17440208614981E-10,
-0.756714611508721));
#53802=DIRECTION('ref_axis',(0.756621682456946,0.0156715280541952,0.653665076965617));
#53803=DIRECTION('',(-0.653745308265973,-1.48214773786071E-11,0.756714656868907));
#53804=DIRECTION('',(-0.135290527320362,-3.07809289802733E-8,-0.990805971528925));
#53805=DIRECTION('center_axis',(-0.491483215751795,0.793626260386506,-0.358610662779573));
#53806=DIRECTION('ref_axis',(-0.850173673706501,-0.526502349981832,-3.01975261095387E-16));
#53807=DIRECTION('center_axis',(0.869349289640561,0.471546674565597,-0.147903841422661));
#53808=DIRECTION('ref_axis',(0.3574942912207,-0.393410391429238,0.84701009182896));
#53809=DIRECTION('center_axis',(-0.480433476380654,-0.601098528055858,0.638642493373155));
#53810=DIRECTION('ref_axis',(-0.798095056225195,-0.00227571851785752,-0.602527262731015));
#53811=DIRECTION('',(-0.997345805939199,5.19500677922194E-12,0.0728103246489838));
#53812=DIRECTION('center_axis',(0.,-1.,1.45983193964168E-32));
#53813=DIRECTION('ref_axis',(1.,0.,0.));
#53814=DIRECTION('center_axis',(0.477700635629862,0.60109852730126,-0.640689209519782));
#53815=DIRECTION('ref_axis',(-0.799730696663546,-0.00432809833535144,-0.600343302102089));
#53816=DIRECTION('center_axis',(0.486462610921983,-0.601098528267777,-0.634062053342794));
#53817=DIRECTION('ref_axis',(-0.794900741263355,-0.0033017849475055,-0.606730508343803));
#53818=DIRECTION('center_axis',(-0.489167051144032,0.601098527750881,0.631977971143595));
#53819=DIRECTION('ref_axis',(-0.792301426769745,-0.00330189864368045,-0.61012092785281));
#53820=DIRECTION('center_axis',(0.429680332517662,0.584828255987283,-0.688004885772176));
#53821=DIRECTION('ref_axis',(-0.834837147990686,-0.0330815410860676,-0.549502090964309));
#53822=DIRECTION('center_axis',(-0.553720478367964,-1.08069513787359E-7,
0.832702607078867));
#53823=DIRECTION('ref_axis',(0.832600299740156,-0.0156751635310958,0.553652445240582));
#53824=DIRECTION('',(0.553748836414939,1.16573417585621E-12,-0.832683749192394));
#53825=DIRECTION('center_axis',(0.459166087091293,0.584827952226198,-0.668687349035544));
#53826=DIRECTION('ref_axis',(-0.814748358265621,-0.0227607295829982,-0.579367812268101));
#53827=DIRECTION('center_axis',(0.604940842662418,5.5376368860139E-10,-0.796270416930633));
#53828=DIRECTION('ref_axis',(0.796172357150687,0.0156933905073754,0.604866344908941));
#53829=DIRECTION('',(-0.604940784793415,-2.24265050970792E-11,0.796270460894743));
#53830=DIRECTION('',(-0.197236768334464,0.,-0.980355882940974));
#53831=DIRECTION('center_axis',(-0.39660197790353,-0.601098527876615,0.69382089252744));
#53832=DIRECTION('ref_axis',(-0.855329855112446,-0.0324816889100509,-0.517064578983005));
#53833=DIRECTION('',(-0.99080597370157,8.1518485824271E-12,0.135290511408906));
#53834=DIRECTION('center_axis',(0.,-1.,1.45983193964168E-32));
#53835=DIRECTION('ref_axis',(1.,0.,0.));
#53836=DIRECTION('center_axis',(0.393634150632677,0.601098520441866,-0.695508967719533));
#53837=DIRECTION('ref_axis',(-0.856675070654286,-0.0345386033944676,-0.514698851946489));
#53838=DIRECTION('center_axis',(0.486462608228835,-0.601098531310315,-0.634062052524657));
#53839=DIRECTION('ref_axis',(-0.808040171738806,-0.0335099469771996,-0.588173583485272));
#53840=DIRECTION('center_axis',(-0.489167083046666,0.601098523747394,0.631977950258014));
#53841=DIRECTION('ref_axis',(-0.805519993522239,-0.0335100846374624,-0.591620329488027));
#53842=DIRECTION('',(0.500371494362523,1.60982338570607E-12,-0.865810815149254));
#53843=DIRECTION('center_axis',(0.371736676294122,0.584827952147084,-0.720963320762747));
#53844=DIRECTION('ref_axis',(-0.869535366613621,-0.0526562728332215,-0.491055560134929));
#53845=DIRECTION('center_axis',(0.553748893832433,4.99550230227221E-10,
-0.832683711008782));
#53846=DIRECTION('ref_axis',(0.832580123902208,0.0157729998146186,0.553680006646287));
#53847=DIRECTION('',(-0.553748836412657,-1.76525460892907E-10,0.832683749193911));
#53848=DIRECTION('',(-0.258404621839997,0.,-0.966036775393012));
#53849=DIRECTION('',(-0.98035588294767,6.51326541667506E-11,0.197236768301184));
#53850=DIRECTION('center_axis',(0.,-1.,1.45983193964168E-32));
#53851=DIRECTION('ref_axis',(1.,0.,0.));
#53852=DIRECTION('center_axis',(0.47148522438417,0.601098538304408,-0.645276863397188));
#53853=DIRECTION('ref_axis',(-0.828597540311574,0.0514848806124787,-0.557472352012123));
#53854=DIRECTION('center_axis',(-0.323710583623996,0.60109853674469,0.730679141055228));
#53855=DIRECTION('ref_axis',(-0.896315875410475,0.0525164952408666,-0.440295206895068));
#53856=DIRECTION('center_axis',(0.423002961639728,0.584827930050679,-0.692130613884878));
#53857=DIRECTION('ref_axis',(-0.861206576608442,0.0219594825779789,-0.507780477698066));
#53858=DIRECTION('center_axis',(-0.445016265398051,-1.00945786707435E-8,
0.89552248633475));
#53859=DIRECTION('ref_axis',(0.89541155989297,-0.015739139348497,0.44496114201423));
#53860=DIRECTION('',(0.445019414620412,1.60982338570637E-12,-0.895520921369739));
#53861=DIRECTION('center_axis',(0.452680909523334,0.584827952320435,-0.673094540415991));
#53862=DIRECTION('ref_axis',(-0.842127239138703,0.0322834330609294,-0.538311706217157));
#53863=DIRECTION('center_axis',(0.500371556578268,5.32646000511302E-10,
-0.865810779193376));
#53864=DIRECTION('ref_axis',(0.865704037482965,0.0157020800820386,0.500309868148521));
#53865=DIRECTION('',(-0.500371494363197,-4.44089209850264E-13,0.865810815148864));
#53866=DIRECTION('',(-0.318552670357111,-1.64268989064552E-13,-0.94790516203276));
#53867=DIRECTION('center_axis',(-0.389876779295978,-0.601098528066563,0.697622144518082));
#53868=DIRECTION('ref_axis',(-0.88109721997925,0.0232723703365245,-0.472362239942777));
#53869=DIRECTION('',(-0.966036775392989,0.,0.258404621840081));
#53870=DIRECTION('center_axis',(0.,-1.,1.45983193964168E-32));
#53871=DIRECTION('ref_axis',(1.,0.,0.));
#53872=DIRECTION('center_axis',(0.386892787612457,0.60109853235182,-0.699281434973037));
#53873=DIRECTION('ref_axis',(-0.882421829328887,0.0212180217980572,-0.469980330093545));
#53874=DIRECTION('center_axis',(0.320585907961959,-0.601098525668862,-0.732055488371562));
#53875=DIRECTION('ref_axis',(-0.908947271769225,0.0222452708710491,-0.416317192855587));
#53876=DIRECTION('center_axis',(-0.323710520662284,0.60109853014702,0.730679174376584));
#53877=DIRECTION('ref_axis',(-0.907160396119142,0.022245152793508,-0.420196583625039));
#53878=DIRECTION('center_axis',(0.332919657819598,0.584827953016086,-0.739689642220504));
#53879=DIRECTION('ref_axis',(-0.909529640592536,-0.00784645564255627,-0.41556499614075));
#53880=DIRECTION('center_axis',(-0.387910658915138,-1.51457921573024E-9,
0.921696978784255));
#53881=DIRECTION('ref_axis',(0.921583697610959,-0.0156778483096378,0.387862982727266));
#53882=DIRECTION('',(0.387911046558196,1.22124532708725E-12,-0.921696815638486));
#53883=DIRECTION('center_axis',(0.364750270664268,0.584827952254338,-0.724522950852725));
#53884=DIRECTION('ref_axis',(-0.893990546328477,0.00246180456674765,-0.448079058418921));
#53885=DIRECTION('center_axis',(0.445019479869039,5.51522626024051E-10,
-0.895520888945138));
#53886=DIRECTION('ref_axis',(0.895410924712026,0.0156707406188141,0.444964834335043));
#53887=DIRECTION('',(-0.445019414619707,-6.38378239129916E-11,0.895520921370089));
#53888=DIRECTION('',(-0.377443537017128,1.64268989064547E-13,-0.926032600054663));
#53889=DIRECTION('center_axis',(-0.299367251286446,-0.601098528085944,0.740985700530117));
#53890=DIRECTION('ref_axis',(-0.925204036176552,-0.00691952105771956,-0.379406920958157));
#53891=DIRECTION('',(-0.947905162036754,2.35931335548688E-11,0.318552670345227));
#53892=DIRECTION('center_axis',(0.,-1.,1.45983193964168E-32));
#53893=DIRECTION('ref_axis',(1.,0.,0.));
#53894=DIRECTION('center_axis',(0.296198808422639,0.601098526255464,-0.74225792526757));
#53895=DIRECTION('ref_axis',(-0.926220609588028,-0.0089721241941348,-0.376875156201396));
#53896=DIRECTION('center_axis',(0.320585901750229,-0.601098528786845,-0.73205548853163));
#53897=DIRECTION('ref_axis',(-0.918366195244468,-0.00794567929387724,-0.395651864159336));
#53898=DIRECTION('center_axis',(-0.323710545522671,0.601098527087631,0.730679165879592));
#53899=DIRECTION('ref_axis',(-0.91666750615744,-0.00794581654303214,-0.399571704647068));
#53900=DIRECTION('center_axis',(0.237586691867558,0.584827952229731,-0.775582897012441));
#53901=DIRECTION('ref_axis',(-0.952070285106708,-0.0181546317102868,-0.305340108017759));
#53902=DIRECTION('center_axis',(-0.329271743027232,-2.29656697345778E-10,
0.944235203349149));
#53903=DIRECTION('ref_axis',(0.944119127553756,-0.0156795066177309,0.329231265312635));
#53904=DIRECTION('',(0.329271773866349,2.06172326321069E-7,-0.944235192594973));
#53905=DIRECTION('center_axis',(0.271061496426085,0.584827782537064,-0.764527389913555));
#53906=DIRECTION('ref_axis',(-0.935387442372695,-0.0273551073963662,-0.35256493125494));
#53907=DIRECTION('center_axis',(0.387911113057852,4.51452499428076E-10,
-0.921696787651025));
#53908=DIRECTION('ref_axis',(0.921583152433633,0.0157023279244598,0.387863287832504));
#53909=DIRECTION('',(0.387911047380125,-1.29267404815429E-5,-0.921696815201915));
#53910=DIRECTION('',(-0.434844842242925,-7.62630514900653E-8,-0.900505393195799));
#53911=DIRECTION('center_axis',(-0.329271770804114,-1.01359413495107E-11,
0.944235193662852));
#53912=DIRECTION('ref_axis',(0.728832717346511,-0.635772805085059,0.254157058606634));
#53913=DIRECTION('',(0.92603260005471,0.,-0.377443537017014));
#53914=DIRECTION('center_axis',(0.249821861302329,0.398564391568801,-0.882459893359937));
#53915=DIRECTION('ref_axis',(-4.0408704040895E-16,0.91135738249489,0.411615987750794));
#53916=DIRECTION('center_axis',(-0.262589361671171,5.74456459349265E-5,
0.96490767632822));
#53917=DIRECTION('ref_axis',(0.964907608885033,-0.000362964710733412,0.262589364926279));
#53918=DIRECTION('',(0.269333889882249,5.94973682696981E-5,-0.963046858787754));
#53919=DIRECTION('center_axis',(0.279765625248216,0.590180063806943,-0.757244139768877));
#53920=DIRECTION('ref_axis',(-0.0441970528704828,0.79582076062354,0.603917161105837));
#53921=DIRECTION('center_axis',(-0.635039594591643,0.550037558039011,-0.542386760575297));
#53922=DIRECTION('ref_axis',(-0.654706135033812,-0.755883507393228,-4.32073907844199E-16));
#53923=DIRECTION('center_axis',(0.76583216617711,-0.477126090214006,-0.431105308811632));
#53924=DIRECTION('ref_axis',(-0.441323162917497,0.0976183354969225,-0.89202271632919));
#53925=DIRECTION('center_axis',(0.652772903104731,0.584827951389971,-0.481522381873607));
#53926=DIRECTION('ref_axis',(-0.608709633166722,0.0265489689982835,-0.792948759211567));
#53927=DIRECTION('center_axis',(-0.743431828170876,-3.27000309038643E-12,
0.668811720039735));
#53928=DIRECTION('ref_axis',(0.668728784863672,-0.01574776705564,0.743339639819859));
#53929=DIRECTION('center_axis',(0.778277686855452,-0.000115441219111835,
-0.627920240807901));
#53930=DIRECTION('ref_axis',(0.0157248311762356,0.999689948221239,0.0193064007493675));
#53931=DIRECTION('',(-0.783959868697913,-6.06570349238166E-10,0.620811504622097));
#53932=DIRECTION('center_axis',(-0.624163700784653,-0.601098528100592,0.499099423099355));
#53933=DIRECTION('ref_axis',(-0.640539472529953,0.0279220117807904,-0.767417451840368));
#53934=DIRECTION('',(-0.99332336407675,2.24206636476409E-10,-0.115363314702931));
#53935=DIRECTION('center_axis',(0.,-1.,1.45983193964168E-32));
#53936=DIRECTION('ref_axis',(1.,0.,0.));
#53937=DIRECTION('center_axis',(0.622025706030483,0.601098533560836,-0.501761471207477));
#53938=DIRECTION('ref_axis',(-0.642663410630348,0.0258667278601001,-0.765711860314818));
#53939=DIRECTION('center_axis',(0.562095733968384,-0.601098524369219,-0.568092377924304));
#53940=DIRECTION('ref_axis',(-0.696218253805938,0.0268944565437029,-0.717326167984014));
#53941=DIRECTION('center_axis',(-0.564517655764164,0.601098530153958,0.565685754971154));
#53942=DIRECTION('ref_axis',(-0.693147346115239,0.0268943300857719,-0.720294003572596));
#53943=DIRECTION('center_axis',(0.587274823952193,0.584827952222734,-0.559539585240297));
#53944=DIRECTION('ref_axis',(-0.688095707625187,-0.0032619714632092,-0.725612607863153));
#53945=DIRECTION('center_axis',(-0.699969746350645,-5.63643803412786E-10,
0.714172496105677));
#53946=DIRECTION('ref_axis',(0.714084660570638,-0.0156832196315775,0.699883657588677));
#53947=DIRECTION('',(0.699969798606842,8.32135976760244E-8,-0.714172444888691));
#53948=DIRECTION('center_axis',(0.611034663886251,0.58482796993141,-0.533491223091179));
#53949=DIRECTION('ref_axis',(-0.661492674912475,0.00704480134835528,-0.74991853678323));
#53950=DIRECTION('center_axis',(0.743431876282904,5.62385146219574E-10,
-0.668811666559787));
#53951=DIRECTION('ref_axis',(0.668729532510225,0.0156715280548055,0.743340578441056));
#53952=DIRECTION('',(-0.743431826076989,-1.44328993199839E-11,0.66881172236724));
#53953=DIRECTION('',(-0.0100428048565106,-3.07809289802904E-8,-0.999949569763702));
#53954=DIRECTION('center_axis',(-0.442661889839964,0.793626260386774,-0.417382091263887));
#53955=DIRECTION('ref_axis',(-0.873334555251418,-0.487120882947763,4.49831660585486E-16));
#53956=DIRECTION('center_axis',(0.881031477541083,0.471546674544276,-0.0377792179380582));
#53957=DIRECTION('ref_axis',(0.248517210562371,-0.393411140887218,0.885136639327576));
#53958=DIRECTION('center_axis',(-0.556688238442204,-0.601098528035278,0.573392330585209));
#53959=DIRECTION('ref_axis',(-0.716285152269076,-0.0022757229430359,-0.697803985173453));
#53960=DIRECTION('',(-0.998606989791731,5.05127141378911E-12,-0.0527643813485665));
#53961=DIRECTION('center_axis',(0.,-1.,1.45983193964168E-32));
#53962=DIRECTION('ref_axis',(1.,0.,0.));
#53963=DIRECTION('center_axis',(0.554233477834988,0.601098527323786,-0.575765414466786));
#53964=DIRECTION('ref_axis',(-0.718181610818199,-0.00432809493829295,-0.695842253299397));
#53965=DIRECTION('center_axis',(0.562095757374046,-0.601098528262797,-0.568092350645912));
#53966=DIRECTION('ref_axis',(-0.712589213394155,-0.00330178665336215,-0.70157373893212));
#53967=DIRECTION('center_axis',(-0.564517663858828,0.601098527757849,0.565685749439314));
#53968=DIRECTION('ref_axis',(-0.70958546592687,-0.00330189725113067,-0.704611640565134));
#53969=DIRECTION('center_axis',(0.512522051794119,0.584828255986954,-0.62872653628108));
#53970=DIRECTION('ref_axis',(-0.759383333816913,-0.0330815410895385,-0.649801942102555));
#53971=DIRECTION('center_axis',(-0.653719533738691,-1.0810677741567E-7,
0.756736923381209));
#53972=DIRECTION('ref_axis',(0.756643949578265,-0.0156751635310768,0.653639214563263));
#53973=DIRECTION('',(0.65374530826584,0.,-0.756714656869022));
#53974=DIRECTION('center_axis',(0.539354173045247,0.58482795222633,-0.605865779123921));
#53975=DIRECTION('ref_axis',(-0.735709782773397,-0.0227607295838477,-0.676914370301246));
#53976=DIRECTION('center_axis',(0.699969849654639,5.54772316281761E-10,
-0.714172394856075));
#53977=DIRECTION('ref_axis',(0.7140844453511,0.0156933905089797,0.699883649188881));
#53978=DIRECTION('',(-0.699969797674486,-2.28150831557062E-11,0.71417244580251));
#53979=DIRECTION('',(-0.0728103246514917,-1.4373536543164E-13,-0.997345805939016));
#53980=DIRECTION('center_axis',(-0.480433477524117,-0.601098528245212,0.638642492334737));
#53981=DIRECTION('ref_axis',(-0.783779942752042,-0.0324816822283564,-0.62018863393263));
#53982=DIRECTION('',(-0.999949569924982,8.00811321699498E-12,0.0100427887981127));
#53983=DIRECTION('center_axis',(0.,-1.,1.45983193964168E-32));
#53984=DIRECTION('ref_axis',(1.,0.,0.));
#53985=DIRECTION('center_axis',(0.477700614898206,0.601098520407419,-0.640689231445236));
#53986=DIRECTION('ref_axis',(-0.785411060893115,-0.0345386039953625,-0.618010153849274));
#53987=DIRECTION('center_axis',(0.562095763024861,-0.601098530840434,-0.568092342327346));
#53988=DIRECTION('ref_axis',(-0.727950828462085,-0.0335099556139018,-0.684809954816749));
#53989=DIRECTION('center_axis',(-0.564517689922951,0.601098523962191,0.565685727462282));
#53990=DIRECTION('ref_axis',(-0.725018542428448,-0.0335100808076772,-0.687913648373974));
#53991=DIRECTION('',(0.604940784793647,0.,-0.796270460894567));
#53992=DIRECTION('center_axis',(0.459166085830651,0.584827952146512,-0.668687349970878));
#53993=DIRECTION('ref_axis',(-0.801133239325096,-0.0526562728411134,-0.596165119559137));
#53994=DIRECTION('center_axis',(0.653745376981871,6.72256483690371E-10,
-0.756714597503465));
#53995=DIRECTION('ref_axis',(0.756620461065956,0.0157729998144629,0.653664050084746));
#53996=DIRECTION('',(-0.653745308264173,-1.77302617010168E-10,0.756714656870463));
#53997=DIRECTION('',(-0.135290511413073,-1.43735365431586E-13,-0.990805973701001));
#53998=DIRECTION('',(-0.9973458059415,6.51326541667556E-11,0.0728103246174644));
#53999=DIRECTION('center_axis',(0.,-1.,1.45983193964168E-32));
#54000=DIRECTION('ref_axis',(1.,0.,0.));
#54001=DIRECTION('center_axis',(0.548642066116338,0.601098537770836,-0.581095888109148));
#54002=DIRECTION('ref_axis',(-0.752193983083953,0.0514848867700612,-0.656927331024195));
#54003=DIRECTION('center_axis',(-0.412736402430169,0.601098536370573,0.684345827547854));
#54004=DIRECTION('ref_axis',(-0.834064537983385,0.0525164995610771,-0.549161509714959));
#54005=DIRECTION('center_axis',(0.506414424843185,0.58482793005016,-0.63365662826486));
#54006=DIRECTION('ref_axis',(-0.79077393630234,0.0219594825879678,-0.611714281989044));
#54007=DIRECTION('center_axis',(-0.55374598213335,-9.39659742892925E-9,
0.832685647331075));
#54008=DIRECTION('ref_axis',(0.832582504369383,-0.0157391393474978,0.553677390644233));
#54009=DIRECTION('',(0.553748836414868,3.88578058618135E-13,-0.832683749192441));
#54010=DIRECTION('center_axis',(0.533472500561931,0.58482795232209,-0.611051026778412));
#54011=DIRECTION('ref_axis',(-0.768018467538781,0.0322834330421544,-0.639613487561352));
#54012=DIRECTION('center_axis',(0.604940834163369,4.55365815109069E-10,
-0.796270423387512));
#54013=DIRECTION('ref_axis',(0.796172254977744,0.0157020800819334,0.604866253881596));
#54014=DIRECTION('',(-0.604940784794057,-1.16573417585723E-12,0.796270460894256));
#54015=DIRECTION('',(-0.197236768334425,0.,-0.980355882940982));
#54016=DIRECTION('center_axis',(-0.47423772019324,-0.601098528163163,0.64325667053362));
#54017=DIRECTION('ref_axis',(-0.814946820275726,0.0232723678061855,-0.579068283554865));
#54018=DIRECTION('',(-0.990805973700986,0.,0.135290511413188));
#54019=DIRECTION('center_axis',(0.,-1.,1.45983193964168E-32));
#54020=DIRECTION('ref_axis',(1.,0.,0.));
#54021=DIRECTION('center_axis',(0.471485217112986,0.601098532584745,-0.645276874038104));
#54022=DIRECTION('ref_axis',(-0.816559520194112,0.021218015378734,-0.576871169156293));
#54023=DIRECTION('center_axis',(0.409808866426316,-0.601098525471459,-0.686102948306168));
#54024=DIRECTION('ref_axis',(-0.849601574644904,0.0222452761089785,-0.526955702172142));
#54025=DIRECTION('center_axis',(-0.412736344185965,0.601098529989856,0.684345868280096));
#54026=DIRECTION('ref_axis',(-0.847342571781816,0.0222451570215671,-0.530580549054772));
#54027=DIRECTION('center_axis',(0.423002181533233,0.584827953016183,-0.692131071249533));
#54028=DIRECTION('ref_axis',(-0.85027362301044,-0.00784645566944904,-0.526282432868634));
#54029=DIRECTION('center_axis',(-0.500371129583691,-1.52148457841835E-9,
0.865811025963022));
#54030=DIRECTION('ref_axis',(0.865704613456417,-0.0156778483093056,0.500309631441038));
#54031=DIRECTION('',(0.50037149436275,3.88578058618399E-13,-0.865810815149123));
#54032=DIRECTION('center_axis',(0.452680910063766,0.584827952254225,-0.673094540110058));
#54033=DIRECTION('ref_axis',(-0.830781966560561,0.0024618045719596,-0.55659254716176));
#54034=DIRECTION('center_axis',(0.553748900359298,5.82366288656275E-10,
-0.832683706668305));
#54035=DIRECTION('ref_axis',(0.832581458437494,0.0156707406186236,0.553680903548749));
#54036=DIRECTION('',(-0.55374883641417,-6.4170890820376E-11,0.832683749192905));
#54037=DIRECTION('',(-0.258404621839981,1.64268989064578E-13,-0.966036775393016));
#54038=DIRECTION('center_axis',(-0.38987678399407,-0.601098528077048,0.697622141883447));
#54039=DIRECTION('ref_axis',(-0.870356230200551,-0.00691952173119867,-0.492373996845991));
#54040=DIRECTION('',(-0.980355882943439,2.3449398189433E-11,0.197236768322213));
#54041=DIRECTION('center_axis',(0.,-1.,1.45983193964168E-32));
#54042=DIRECTION('ref_axis',(1.,0.,0.));
#54043=DIRECTION('center_axis',(0.386892766875141,0.601098526142014,-0.699281451784327));
#54044=DIRECTION('ref_axis',(-0.871682106507819,-0.00897213204655847,-0.489989597890231));
#54045=DIRECTION('center_axis',(0.409808864115314,-0.601098528821877,-0.686102946751208));
#54046=DIRECTION('ref_axis',(-0.861536277690818,-0.00794567680510276,-0.507633833035939));
#54047=DIRECTION('center_axis',(-0.412736369131606,0.60109852713163,0.684345855745649));
#54048=DIRECTION('ref_axis',(-0.859359697506052,-0.00794581332026708,-0.511309861388362));
#54049=DIRECTION('center_axis',(0.332919562152049,0.584827952227919,-0.739689685901721));
#54050=DIRECTION('ref_axis',(-0.90629366348865,-0.0181546317530755,-0.42225845742416));
#54051=DIRECTION('center_axis',(-0.445019481897012,6.08170420604607E-10,
0.895520887937359));
#54052=DIRECTION('ref_axis',(0.895410800637064,-0.0156795066141847,0.444964775206789));
#54053=DIRECTION('',(0.445019417513644,2.06171882231856E-7,-0.895520919931955));
#54054=DIRECTION('center_axis',(0.364744785491104,0.584827782537139,-0.724525849248833));
#54055=DIRECTION('ref_axis',(-0.883823530127309,-0.0273551073961588,-0.467019984254042));
#54056=DIRECTION('center_axis',(0.500371579043315,6.52716079657588E-10,
-0.865810766210319));
#54057=DIRECTION('ref_axis',(0.865704021130687,0.0157023279252462,0.500309888664902));
#54058=DIRECTION('',(0.500371495123498,-1.29267395933215E-5,-0.86581081461297));
#54059=DIRECTION('',(-0.318552708008709,-7.62629077547213E-8,-0.947905149379574));
#54060=DIRECTION('center_axis',(-0.445019414093066,-4.78825638661493E-10,
0.895520921631798));
#54061=DIRECTION('ref_axis',(0.691231328023145,-0.635772805081915,0.343499914814592));
#54062=DIRECTION('',(0.966036775393033,0.,-0.258404621839916));
#54063=DIRECTION('center_axis',(0.35845349323297,0.398564391571384,-0.844190451829689));
#54064=DIRECTION('ref_axis',(-3.77661288183636E-16,0.904282187137336,0.426935271471116));
#54065=DIRECTION('center_axis',(-0.38145376525024,5.74456466242848E-5,0.924387917314161));
#54066=DIRECTION('ref_axis',(0.924387849993085,-0.000362969539878445,0.381453760026396));
#54067=DIRECTION('',(0.387911888600281,5.94973684118082E-5,-0.921696459330634));
#54068=DIRECTION('center_axis',(0.37246744627126,0.590180063809394,-0.716209113143714));
#54069=DIRECTION('ref_axis',(-0.119540363498291,0.795820897101943,0.59361536471907));
#54070=DIRECTION('center_axis',(-0.562053031166013,0.550037558040921,-0.617701444794714));
#54071=DIRECTION('ref_axis',(-0.73963826964566,-4.1371342815621E-16,0.673004628569205));
#54072=DIRECTION('center_axis',(0.813825173309153,-0.477126089925489,-0.33172169299089));
#54073=DIRECTION('ref_axis',(-0.326037099188356,0.0976292430140872,-0.940302260372343));
#54074=DIRECTION('center_axis',(0.70797635094518,0.584827951389921,-0.395911295336993));
#54075=DIRECTION('ref_axis',(-0.504526943851804,0.026548969000283,-0.862987668030419));
#54076=DIRECTION('center_axis',(-0.821393980625655,-2.78574751580884E-11,
0.570361226410019));
#54077=DIRECTION('ref_axis',(0.57029049946684,-0.0157477670569905,0.82129212467342));
#54078=DIRECTION('center_axis',(0.85084000898608,-0.000115441208927885,
-0.52542484313353));
#54079=DIRECTION('ref_axis',(0.0131765282484206,0.999690165025676,0.0211176005799707));
#54080=DIRECTION('',(-0.855586424283945,-6.07347505355654E-10,0.517659995152236));
#54081=DIRECTION('center_axis',(-0.681795727521764,-0.601098528130143,0.416935421153978));
#54082=DIRECTION('ref_axis',(-0.539305717521858,0.0279220110851815,-0.841647018853624));
#54083=DIRECTION('',(-0.971031855393334,2.24206636476412E-10,-0.23895006970365));
#54084=DIRECTION('center_axis',(0.,-1.,1.45983193964168E-32));
#54085=DIRECTION('ref_axis',(1.,0.,0.));
#54086=DIRECTION('center_axis',(0.680008247647369,0.601098532952695,-0.419844419771982));
#54087=DIRECTION('ref_axis',(-0.54162665863951,0.0258667416307407,-0.840221086576865));
#54088=DIRECTION('center_axis',(0.628864298647871,-0.601098524492875,-0.493163520283698));
#54089=DIRECTION('ref_axis',(-0.600823553899494,0.0268944537977208,-0.798929124162152));
#54090=DIRECTION('center_axis',(-0.630965493733841,0.60109853030328,0.490472326012841));
#54091=DIRECTION('ref_axis',(-0.597404892030046,0.0268943266317125,-0.801488671269654));
#54092=DIRECTION('center_axis',(0.652772892098893,0.584827952222548,-0.481522395782406));
#54093=DIRECTION('ref_axis',(-0.591726492967278,-0.00326197144519419,-0.806132195773706));
#54094=DIRECTION('center_axis',(-0.783959817463517,-6.47203937932624E-10,
0.620811569320812));
#54095=DIRECTION('ref_axis',(0.620735216178117,-0.0156832196310024,0.78386339882553));
#54096=DIRECTION('',(0.783959869514184,8.32140417652251E-8,-0.620811503591305));
#54097=DIRECTION('center_axis',(0.673080653132819,0.584827969931241,-0.452701535191125));
#54098=DIRECTION('ref_axis',(-0.562286892455316,0.00704480135906427,-0.826912221065063));
#54099=DIRECTION('center_axis',(0.821394025877762,6.05711839516913E-10,
-0.570361161241124));
#54100=DIRECTION('ref_axis',(0.57029111749682,0.0156715280541059,0.821293153820654));
#54101=DIRECTION('',(-0.821393979885835,-1.5210055437211E-11,0.570361227475456));
#54102=DIRECTION('',(0.11536329863905,-3.07809289802874E-8,-0.993323365942389));
#54103=DIRECTION('center_axis',(-0.386859521492136,0.793626260387047,-0.469571154836993));
#54104=DIRECTION('ref_axis',(-2.69928171055445E-16,0.509219680892889,0.860636576373178));
#54105=DIRECTION('center_axis',(0.878819272722778,0.471546674561253,0.0729412064695383));
#54106=DIRECTION('ref_axis',(0.135633310371155,-0.393433170232164,0.909293102183686));
#54107=DIRECTION('center_axis',(-0.624163700568947,-0.601098528038163,0.4990994234443));
#54108=DIRECTION('ref_axis',(-0.623178999774232,-0.0022757226821621,-0.782075926829781));
#54109=DIRECTION('',(-0.984119544876305,5.19500677922197E-12,-0.177506961532368));
#54110=DIRECTION('center_axis',(0.,-1.,1.45983193964168E-32));
#54111=DIRECTION('ref_axis',(1.,0.,0.));
#54112=DIRECTION('center_axis',(0.622025724926714,0.601098527339717,-0.501761455234875));
#54113=DIRECTION('ref_axis',(-0.625306372224195,-0.00432809260108738,-0.780367354820954));
#54114=DIRECTION('center_axis',(0.628864322227214,-0.601098528236074,-0.493163485653725));
#54115=DIRECTION('ref_axis',(-0.619039722698785,-0.00330179299804888,-0.785352735962643));
#54116=DIRECTION('center_axis',(-0.630965496664613,0.601098527762398,0.490472325356545));
#54117=DIRECTION('ref_axis',(-0.615678918250599,-0.00330189631434547,-0.787990207491503));
#54118=DIRECTION('center_axis',(0.587280992156649,0.584828255987147,-0.559532793722169));
#54119=DIRECTION('ref_axis',(-0.671953590829443,-0.0330815410858397,-0.739854028448047));
#54120=DIRECTION('center_axis',(-0.743409036258055,-1.0821547404186E-7,
0.668837054004829));
#54121=DIRECTION('ref_axis',(0.668754879990046,-0.0156751635329546,0.743317697715932));
#54122=DIRECTION('',(0.743431826076993,0.,-0.668811722367235));
#54123=DIRECTION('center_axis',(0.611036321497906,0.584827952226251,-0.533489343947148));
#54124=DIRECTION('ref_axis',(-0.645068624513626,-0.0227607295831316,-0.763785584347428));
#54125=DIRECTION('center_axis',(0.783959924147141,6.84547634730646E-10,
-0.620811434600886));
#54126=DIRECTION('ref_axis',(0.620734982387142,0.0156933905081134,0.783863380401964));
#54127=DIRECTION('',(-0.783959868704082,-2.28705943069331E-11,0.620811504614306));
#54128=DIRECTION('',(0.0527643813458746,0.,-0.998606989791874));
#54129=DIRECTION('center_axis',(-0.556688234994435,-0.601098527787945,0.573392334191822));
#54130=DIRECTION('ref_axis',(-0.699869364617338,-0.0324816905828272,-0.713531927980105));
#54131=DIRECTION('',(-0.993323364089748,8.17238220606141E-12,-0.115363314591021));
#54132=DIRECTION('center_axis',(0.,-1.,1.45983193964168E-32));
#54133=DIRECTION('ref_axis',(1.,0.,0.));
#54134=DIRECTION('center_axis',(0.55423346574626,0.601098520880261,-0.575765432830464));
#54135=DIRECTION('ref_axis',(-0.701760641393952,-0.0345385956231396,-0.711575075169677));
#54136=DIRECTION('center_axis',(0.628864320118186,-0.601098530849351,-0.493163485157857));
#54137=DIRECTION('ref_axis',(-0.636381272887134,-0.0335099554704704,-0.770646454869493));
#54138=DIRECTION('center_axis',(-0.630965517497451,0.601098524134483,0.490472303002444));
#54139=DIRECTION('ref_axis',(-0.633083115930161,-0.0335100777499132,-0.773358159595768));
#54140=DIRECTION('',(0.699969797674222,0.,-0.714172445802769));
#54141=DIRECTION('center_axis',(0.539354171899053,0.584827952145603,-0.60586578022221));
#54142=DIRECTION('ref_axis',(-0.720096762283953,-0.0526562728523631,-0.69187279891427));
#54143=DIRECTION('center_axis',(0.743431873707654,5.17806860950093E-10,
-0.668811669422363));
#54144=DIRECTION('ref_axis',(0.668728468241762,0.0157729998153311,0.743339389673285));
#54145=DIRECTION('',(-0.743431826075324,-1.7769119506863E-10,0.668811722369091));
#54146=DIRECTION('',(-0.0100427888024932,-1.43735365431651E-13,-0.999949569924938));
#54147=DIRECTION('',(-0.998606989790074,6.51326541667587E-11,-0.0527643813799327));
#54148=DIRECTION('center_axis',(0.,-1.,1.45983193964168E-32));
#54149=DIRECTION('ref_axis',(1.,0.,0.));
#54150=DIRECTION('center_axis',(0.617146485119927,0.601098537856876,-0.507750690487413));
#54151=DIRECTION('ref_axis',(-0.663927883266848,0.0514848857726378,-0.746022166130324));
#54152=DIRECTION('center_axis',(-0.495253123111622,0.601098536029601,0.627219972602321));
#54153=DIRECTION('ref_axis',(-0.758659505446537,0.0525165034839058,-0.649367208640413));
#54154=DIRECTION('center_axis',(0.581839430013544,0.584827930051117,-0.56518949911834));
#54155=DIRECTION('ref_axis',(-0.70787031866,0.0219594825710829,-0.706000986603702));
#54156=DIRECTION('center_axis',(-0.653742635283663,-1.02194371156788E-8,
0.756716966119018));
#54157=DIRECTION('ref_axis',(0.756623233263496,-0.0157391393489811,0.653661657418));
#54158=DIRECTION('',(0.653745308265769,0.,-0.756714656869083));
#54159=DIRECTION('center_axis',(0.605850911637909,0.584827952320374,-0.539370873381454));
#54160=DIRECTION('ref_axis',(-0.681797585877112,0.032283433062499,-0.730828182161745));
#54161=DIRECTION('center_axis',(0.699969850606534,5.5076297820919E-10,-0.714172393923111));
#54162=DIRECTION('ref_axis',(0.71408434698844,0.0157020800825275,0.699883554648325));
#54163=DIRECTION('',(-0.699969797674564,-1.22124532708828E-12,0.714172445802433));
#54164=DIRECTION('',(-0.0728103246515018,-1.6426898906465E-13,-0.997345805939015));
#54165=DIRECTION('center_axis',(-0.551119654299467,-0.601098528114907,0.578746651085713));
#54166=DIRECTION('ref_axis',(-0.73594421951875,0.0232723691575943,-0.676642078643304));
#54167=DIRECTION('',(-0.99994956992494,0.,0.0100427888023022));
#54168=DIRECTION('center_axis',(0.,-1.,1.45983193964168E-32));
#54169=DIRECTION('ref_axis',(1.,0.,0.));
#54170=DIRECTION('center_axis',(0.548642063374605,0.601098532266458,-0.581095896391607));
#54171=DIRECTION('ref_axis',(-0.73781956742827,0.0212180242146453,-0.674664421300239));
#54172=DIRECTION('center_axis',(0.492568906019118,-0.601098525584716,-0.629330148144049));
#54173=DIRECTION('ref_axis',(-0.776857147932723,0.0222452731343194,-0.629283814768039));
#54174=DIRECTION('center_axis',(-0.495253075494428,0.601098529992903,0.627220015986163));
#54175=DIRECTION('ref_axis',(-0.774161646564126,0.0222451569315223,-0.632596947496756));
#54176=DIRECTION('center_axis',(0.506413708192182,0.58482795301627,-0.633657179810853));
#54177=DIRECTION('ref_axis',(-0.777608282452322,-0.00784645567321364,-0.628700081274782));
#54178=DIRECTION('center_axis',(-0.604940525637679,-7.70162739777139E-10,
0.796270657779884));
#54179=DIRECTION('ref_axis',(0.796172792128776,-0.0156778483076014,0.604866175402719));
#54180=DIRECTION('',(0.604940784793799,0.,-0.796270460894452));
#54181=DIRECTION('center_axis',(0.533472501095234,0.584827952254122,-0.611051026377869));
#54182=DIRECTION('ref_axis',(-0.754471458890974,0.0024618045796853,-0.656328238945375));
#54183=DIRECTION('center_axis',(0.653745370650952,6.26092348591291E-10,
-0.75671460297291));
#54184=DIRECTION('ref_axis',(0.756621683260073,0.015670740619388,0.653665094914156));
#54185=DIRECTION('',(-0.653745308265284,-6.46149800302507E-11,0.756714656869502));
#54186=DIRECTION('',(-0.13529051141302,1.64268989064603E-13,-0.990805973701009));
#54187=DIRECTION('center_axis',(-0.474237728369273,-0.601098528079538,0.643256664584025));
#54188=DIRECTION('ref_axis',(-0.801782385968023,-0.00691952141559517,-0.59757604183468));
#54189=DIRECTION('',(-0.997345805939891,2.36136671784977E-11,0.0728103246395067));
#54190=DIRECTION('center_axis',(0.,-1.,1.45983193964168E-32));
#54191=DIRECTION('ref_axis',(1.,0.,0.));
#54192=DIRECTION('center_axis',(0.471485217296396,0.601098526249266,-0.645276879805818));
#54193=DIRECTION('ref_axis',(-0.80339664619811,-0.00897212462668922,-0.595376628578341));
#54194=DIRECTION('center_axis',(0.492568909358048,-0.601098528730169,-0.62933014252636));
#54195=DIRECTION('ref_axis',(-0.791119411035074,-0.00794568415793535,-0.611610123842616));
#54196=DIRECTION('center_axis',(-0.495253100626083,0.601098527106587,0.627219998908312));
#54197=DIRECTION('ref_axis',(-0.788499270034972,-0.00794581489403096,-0.614984361736122));
#54198=DIRECTION('center_axis',(0.423002092228966,0.584827952231097,-0.69213112649201));
#54199=DIRECTION('ref_axis',(-0.846224249338951,-0.0181546316873852,-0.532517538846397));
#54200=DIRECTION('center_axis',(-0.553748779401505,-5.17795029430526E-10,
0.832683787107293));
#54201=DIRECTION('ref_axis',(0.83258142444458,-0.0156795066178101,0.553680706492521));
#54202=DIRECTION('',(0.553748839105272,2.06171493653695E-7,-0.832683747403251));
#54203=DIRECTION('center_axis',(0.452675831374959,0.584827782536344,-0.673098103148875));
#54204=DIRECTION('ref_axis',(-0.81832119285553,-0.0273551074146088,-0.574109853095937));
#54205=DIRECTION('center_axis',(0.604940866149408,6.8645898744654E-10,-0.796270399087147));
#54206=DIRECTION('ref_axis',(0.79617222757896,0.0157023279254072,0.604866283512049));
#54207=DIRECTION('',(0.604940785481077,-1.29267396288052E-5,-0.796270460267387));
#54208=DIRECTION('',(-0.197236807274973,-7.62630514901014E-8,-0.98035587510657));
#54209=DIRECTION('center_axis',(-0.553748835937082,-4.67000694238083E-10,
0.832683749510177));
#54210=DIRECTION('ref_axis',(0.642728807477492,-0.635772805082059,0.42742557288568));
#54211=DIRECTION('',(0.990805973701098,0.,-0.135290511412364));
#54212=DIRECTION('center_axis',(0.461432099445187,0.398564391573976,-0.79260762257934));
#54213=DIRECTION('ref_axis',(-0.864216279017837,1.03620976188408E-16,-0.503120485649872));
#54214=DIRECTION('center_axis',(-0.494302415132049,5.74456528004925E-5,
0.869290008624637));
#54215=DIRECTION('ref_axis',(0.869289942541571,-0.000362817023473896,0.494302401531572));
#54216=DIRECTION('',(0.500372285107575,5.9497368376275E-5,-0.865810356115175));
#54217=DIRECTION('center_axis',(0.459295233292948,0.590180063808867,-0.663879040908009));
#54218=DIRECTION('ref_axis',(-0.192989148209777,0.79581959433691,0.573956759645446));
#54219=DIRECTION('center_axis',(-0.480202555684534,0.550037558040659,-0.683274608235013));
#54220=DIRECTION('ref_axis',(-4.07701821964641E-16,0.778964448248472,0.627068089097949));
#54221=DIRECTION('center_axis',(0.848983671137801,-0.477126089978748,-0.22710662782705));
#54222=DIRECTION('ref_axis',(-0.205617355534998,0.0976251537602208,-0.973750908834537));
#54223=DIRECTION('center_axis',(0.752014588807973,0.584827951389544,-0.304056451162418));
#54224=DIRECTION('ref_axis',(-0.392387563238403,0.02654896900435,-0.919416745801725));
#54225=DIRECTION('center_axis',(-0.886402263734747,5.45006096916998E-11,
0.462915788071564));
#54226=DIRECTION('ref_axis',(0.462858384766917,-0.0157477670565849,0.886292346510841));
#54227=DIRECTION('center_axis',(0.909984076723602,-0.000115441199351685,
-0.414643180075138));
#54228=DIRECTION('ref_axis',(0.0104254267660666,0.999690192852031,0.0226015219004144));
#54229=DIRECTION('',(-0.913719870856715,-6.06958927297027E-10,0.406344678323204));
#54230=DIRECTION('center_axis',(-0.728675430621122,-0.601098528034678,0.328196094436946));
#54231=DIRECTION('ref_axis',(-0.429566785864648,0.0279220132424748,-0.902603311349124));
#54232=DIRECTION('',(-0.933426594283892,2.24206636476396E-10,-0.358768439363852));
#54233=DIRECTION('center_axis',(0.,-1.,1.45983193964168E-32));
#54234=DIRECTION('ref_axis',(1.,0.,0.));
#54235=DIRECTION('center_axis',(0.727266639106194,0.601098532901112,-0.331306186762807));
#54236=DIRECTION('ref_axis',(-0.432048143497244,0.0258667428545896,-0.901479513530219));
#54237=DIRECTION('center_axis',(0.685715297905327,-0.601098524686556,-0.410457176619259));
#54238=DIRECTION('ref_axis',(-0.495953505479251,0.0268944496490568,-0.867932491027336));
#54239=DIRECTION('center_axis',(-0.687462619750625,0.601098530023253,0.407523868809536));
#54240=DIRECTION('ref_axis',(-0.492241016448715,0.0268943329637461,-0.870043376263489));
#54241=DIRECTION('center_axis',(0.707976341754609,0.584827952222725,-0.39591131054156));
#54242=DIRECTION('ref_axis',(-0.48602539807284,-0.00326197146067777,-0.873938597368446));
#54243=DIRECTION('center_axis',(-0.855586379305734,-6.81865596053655E-10,
0.517660069492041));
#54244=DIRECTION('ref_axis',(0.517596402876359,-0.0156832196314315,0.85548115137123));
#54245=DIRECTION('',(0.855586424964706,8.32132090979335E-8,-0.517659994027071));
#54246=DIRECTION('center_axis',(0.724511758384335,0.584827969931324,-0.364772473672077));
#54247=DIRECTION('ref_axis',(-0.454213509827986,0.00704480135380958,-0.890865005634202));
#54248=DIRECTION('center_axis',(0.886402299924587,6.50267358417405E-10,
-0.462915718774382));
#54249=DIRECTION('ref_axis',(0.462858869967012,0.0156715280551234,0.886293444464799));
#54250=DIRECTION('',(-0.886402259955359,-1.44328993199847E-11,0.462915795308425));
#54251=DIRECTION('',(0.238950054000536,-3.0781093249293E-8,-0.971031859257532));
#54252=DIRECTION('center_axis',(-0.324956147391805,0.793626260387304,-0.514354800790212));
#54253=DIRECTION('ref_axis',(-1.18555920776032E-18,0.543871187776492,0.839168714327809));
#54254=DIRECTION('center_axis',(0.8627475630211,0.471546674539849,0.1825113043939));
#54255=DIRECTION('ref_axis',(0.0205917296021878,-0.393421568437244,0.919127548363321));
#54256=DIRECTION('center_axis',(-0.681795727685446,-0.601098528036579,0.416935421021206));
#54257=DIRECTION('ref_axis',(-0.520244942803458,-0.00227572300687119,-0.854014063451078));
#54258=DIRECTION('',(-0.954111946853705,5.05127141378909E-12,-0.299450150894991));
#54259=DIRECTION('center_axis',(0.,-1.,1.45983193964168E-32));
#54260=DIRECTION('ref_axis',(1.,0.,0.));
#54261=DIRECTION('center_axis',(0.680008254497479,0.601098527358381,-0.419844416686559));
#54262=DIRECTION('ref_axis',(-0.522569677456327,-0.00432808968609659,-0.852585596783607));
#54263=DIRECTION('center_axis',(0.685715309048858,-0.601098528261091,-0.410457152767959));
#54264=DIRECTION('ref_axis',(-0.515727617683695,-0.0033017877527314,-0.856746241635139));
#54265=DIRECTION('center_axis',(-0.687462624690007,0.601098527784663,0.40752386377909));
#54266=DIRECTION('ref_axis',(-0.512062749502158,-0.00330189269620656,-0.858941696552748));
#54267=DIRECTION('center_axis',(0.652772892221425,0.584827952239017,-0.481522395596295));
#54268=DIRECTION('ref_axis',(-0.573932730512764,-0.0330869090627003,-0.818233754678234));
#54269=DIRECTION('center_axis',(-0.82139394258747,-5.1287838017996E-10,
0.570361281189925));
#54270=DIRECTION('ref_axis',(0.570291204882479,-0.0156751701947647,0.821293023635934));
#54271=DIRECTION('',(0.821393979885559,-8.32667268468003E-13,-0.570361227475854));
#54272=DIRECTION('center_axis',(0.673082062143511,0.584827952226365,-0.452699463126869));
#54273=DIRECTION('ref_axis',(-0.544254348701349,-0.0227607295837561,-0.838611443463828));
#54274=DIRECTION('center_axis',(0.855586476863532,7.80700868016979E-10,
-0.517659908248889));
#54275=DIRECTION('ref_axis',(0.517596159023445,0.0156933905086436,0.855481112391454));
#54276=DIRECTION('',(-0.855586424288594,-2.28705943069067E-11,0.517659995144553));
#54277=DIRECTION('',(0.177506961529544,0.,-0.984119544876815));
#54278=DIRECTION('center_axis',(-0.624163698886024,-0.601098527870402,0.499099425750974));
#54279=DIRECTION('ref_axis',(-0.60492142024746,-0.0324816890410056,-0.795622407428825));
#54280=DIRECTION('',(-0.971031855420269,8.00811321699544E-12,-0.238950069594192));
#54281=DIRECTION('center_axis',(0.,-1.,1.45983193964168E-32));
#54282=DIRECTION('ref_axis',(1.,0.,0.));
#54283=DIRECTION('center_axis',(0.622025719321274,0.601098521249722,-0.501761469479523));
#54284=DIRECTION('ref_axis',(-0.607043037353427,-0.0345385891650894,-0.793918028929442));
#54285=DIRECTION('center_axis',(0.685715312759475,-0.601098530765051,-0.410457142901999));
#54286=DIRECTION('ref_axis',(-0.534775602600504,-0.0335099570183753,-0.844329401148565));
#54287=DIRECTION('center_axis',(-0.687462640971433,0.601098524430712,0.407523841260609));
#54288=DIRECTION('ref_axis',(-0.531163593663202,-0.0335100724645697,-0.846606349970405));
#54289=DIRECTION('',(0.783959868703576,-3.88578058618413E-13,-0.620811504614945));
#54290=DIRECTION('center_axis',(0.611036320517163,0.584827952146974,-0.533489345157354));
#54291=DIRECTION('ref_axis',(-0.627703929108623,-0.0526562728345706,-0.776669230955346));
#54292=DIRECTION('center_axis',(0.821394034568631,7.121806854496E-10,-0.570361148725144));
#54293=DIRECTION('ref_axis',(0.570290194933799,0.0157729998139083,0.821291851925514));
#54294=DIRECTION('',(-0.821393979884609,-1.76914038951462E-10,0.570361227477222));
#54295=DIRECTION('',(0.115363314586777,-1.43735365431646E-13,-0.99332336409024));
#54296=DIRECTION('',(-0.984119544870761,6.51326541667581E-11,-0.177506961563108));
#54297=DIRECTION('center_axis',(0.,-1.,1.45983193964168E-32));
#54298=DIRECTION('ref_axis',(1.,0.,0.));
#54299=DIRECTION('center_axis',(0.675918141245002,0.60109853743272,-0.426397953362991));
#54300=DIRECTION('ref_axis',(-0.565191237695565,0.051484890664322,-0.823351790467136));
#54301=DIRECTION('center_axis',(-0.569959409941816,0.601098535897603,0.560202482287017));
#54302=DIRECTION('ref_axis',(-0.671289958056372,0.0525165049909385,-0.739332001820705));
#54303=DIRECTION('center_axis',(0.648089094031815,0.584827908067798,-0.487808204258665));
#54304=DIRECTION('ref_axis',(-0.613802514678574,0.0219600677380753,-0.789154122082118));
#54305=DIRECTION('center_axis',(-0.743427237289871,-1.89899202024935E-8,
0.668816823095495));
#54306=DIRECTION('ref_axis',(0.668733978372119,-0.0157391387083452,0.743335150307933));
#54307=DIRECTION('',(0.743431826076532,-7.77156117236683E-13,-0.668811722367748));
#54308=DIRECTION('center_axis',(0.668674691879153,0.584827952321432,-0.459184519146543));
#54309=DIRECTION('ref_axis',(-0.584824349033833,0.0322834330501032,-0.810517279721817));
#54310=DIRECTION('center_axis',(0.783959913257619,5.32263755173338E-10,
-0.62081144835216));
#54311=DIRECTION('ref_axis',(0.620734911445354,0.0157020800825522,0.783863262561788));
#54312=DIRECTION('',(-0.783959868704053,-8.32667268469007E-13,0.620811504614342));
#54313=DIRECTION('',(0.0527643813458762,0.,-0.998606989791874));
#54314=DIRECTION('center_axis',(-0.619310106536488,-0.601098527900125,0.50510944526713));
#54315=DIRECTION('ref_axis',(-0.645335333969567,0.0232723748746104,-0.76354482730098));
#54316=DIRECTION('',(-0.993323364090226,0.,-0.115363314586904));
#54317=DIRECTION('center_axis',(0.,-1.,1.45983193964168E-32));
#54318=DIRECTION('ref_axis',(1.,0.,0.));
#54319=DIRECTION('center_axis',(0.617146491191372,0.601098532042902,-0.507750689990714));
#54320=DIRECTION('ref_axis',(-0.647443759929067,0.0212180303810229,-0.761817808216415));
#54321=DIRECTION('center_axis',(0.567560843501483,-0.60109852584814,-0.562632429875027));
#54322=DIRECTION('ref_axis',(-0.691861215403394,0.0222452661870624,-0.721687748789464));
#54323=DIRECTION('center_axis',(-0.569959361942305,0.601098529742556,0.5602025377269));
#54324=DIRECTION('ref_axis',(-0.688771736305674,0.022245163805164,-0.724636907667384));
#54325=DIRECTION('center_axis',(0.581838788174164,0.584827953016256,-0.565190136101858));
#54326=DIRECTION('ref_axis',(-0.692679594745998,-0.00784645566272457,-0.721202753846692));
#54327=DIRECTION('center_axis',(-0.699969556481948,-8.6612246402921E-10,
0.714172682198406));
#54328=DIRECTION('ref_axis',(0.714084906802545,-0.0156778483080594,0.699883526702286));
#54329=DIRECTION('',(0.69996979767401,-3.88578058618449E-13,-0.714172445802976));
#54330=DIRECTION('center_axis',(0.605850912066346,0.584827952254572,-0.539370872971558));
#54331=DIRECTION('ref_axis',(-0.666262485644979,0.00246180455746111,-0.745713242299274));
#54332=DIRECTION('center_axis',(0.743431873636875,5.37764966112024E-10,
-0.668811669501039));
#54333=DIRECTION('ref_axis',(0.668729543705554,0.0156707406195515,0.743340584970171));
#54334=DIRECTION('',(-0.743431826076294,-6.42264019716035E-11,0.668811722368012));
#54335=DIRECTION('',(-0.0100427888024313,1.64268989064697E-13,-0.999949569924939));
#54336=DIRECTION('center_axis',(-0.551119660015009,-0.601098528080819,0.578746645678412));
#54337=DIRECTION('ref_axis',(-0.720563954751441,-0.00691952141674007,-0.693353955304451));
#54338=DIRECTION('',(-0.998606989791231,2.34493981894322E-11,-0.0527643813580464));
#54339=DIRECTION('center_axis',(0.,-1.,1.45983193964168E-32));
#54340=DIRECTION('ref_axis',(1.,0.,0.));
#54341=DIRECTION('center_axis',(0.548642054612441,0.601098526265418,-0.58109591087202));
#54342=DIRECTION('ref_axis',(-0.722441144725833,-0.00897212363898524,-0.691374206493585));
#54343=DIRECTION('center_axis',(0.567560837458516,-0.601098528740018,-0.562632432881339));
#54344=DIRECTION('ref_axis',(-0.708226124218215,-0.00794568359613293,-0.7059409487252));
#54345=DIRECTION('center_axis',(-0.569959387553192,0.601098527165284,0.560202514435375));
#54346=DIRECTION('ref_axis',(-0.705203743225232,-0.00794581057331358,-0.708960185507941));
#54347=DIRECTION('center_axis',(0.506413626493858,0.584827952229861,-0.633657245829295));
#54348=DIRECTION('ref_axis',(-0.772809373322586,-0.018154631707971,-0.634378500465061));
#54349=DIRECTION('center_axis',(-0.653745273667852,-3.58579868904279E-10,
0.756714686759115));
#54350=DIRECTION('ref_axis',(0.756621663054565,-0.0156795066181202,0.653664908090343));
#54351=DIRECTION('',(0.653745310710866,2.06170660986647E-7,-0.756714654756673));
#54352=DIRECTION('center_axis',(0.533467909010792,0.584827782536611,-0.611055197857742));
#54353=DIRECTION('ref_axis',(-0.739913441519287,-0.0273551074141563,-0.672145666621042));
#54354=DIRECTION('center_axis',(0.699969873412294,7.17574584943481E-10,
-0.714172371570882));
#54355=DIRECTION('ref_axis',(0.714084321857467,0.0157023279247992,0.699883574728757));
#54356=DIRECTION('',(0.699969798277374,-1.29267396287503E-5,-0.714172445094622));
#54357=DIRECTION('',(-0.0728103642668903,-7.62630514901185E-8,-0.997345803046926));
#54358=DIRECTION('center_axis',(-0.653745308271402,5.55864689695122E-12,
0.756714656864217));
#54359=DIRECTION('ref_axis',(0.584090069207158,-0.635772805085269,0.504610474888885));
#54360=DIRECTION('',(0.999949569924943,0.,-0.0100427888020118));
#54361=DIRECTION('center_axis',(0.557133645802655,0.39856439157781,-0.728524897639642));
#54362=DIRECTION('ref_axis',(-0.794343958189859,8.99985877814131E-17,-0.607468251094053));
#54363=DIRECTION('center_axis',(-0.599355620645822,5.74456453289826E-5,
0.800482877206165));
#54364=DIRECTION('ref_axis',(0.800482813270424,-0.000363058141650564,0.59935559882882));
#54365=DIRECTION('',(0.604941511770917,5.94973675946086E-5,-0.7962699063737));
#54366=DIRECTION('center_axis',(0.538879660101934,0.590180063808305,-0.601079199616531));
#54367=DIRECTION('ref_axis',(-0.263407883652486,0.795820382742406,0.545239585174673));
#54368=DIRECTION('center_axis',(-0.390778999041342,0.550037558041802,-0.738072122933564));
#54369=DIRECTION('ref_axis',(1.23414151848966E-16,0.801830011437534,0.597552200864563));
#54370=DIRECTION('center_axis',(0.870753189285527,-0.47712609008213,-0.118909955479017));
#54371=DIRECTION('ref_axis',(-0.0819527892227191,0.0976249050665862,-0.9918432931917));
#54372=DIRECTION('center_axis',(0.784193107367589,0.584827951389862,-0.207406455131711));
#54373=DIRECTION('ref_axis',(-0.274059996363077,0.0265489690005161,-0.961346072254149));
#54374=DIRECTION('center_axis',(-0.937431447214792,-3.39662097952973E-11,
0.348169903599926));
#54375=DIRECTION('ref_axis',(0.348126729219042,-0.0157477670578398,0.937315202179045));
#54376=DIRECTION('center_axis',(0.954777148801951,-0.000115441274343246,
-0.297322355027215));
#54377=DIRECTION('ref_axis',(0.00751840455574443,0.999689530367805,0.0237553460495545));
#54378=DIRECTION('',(-0.957443409235868,-6.06958927296624E-10,0.288621063179385));
#54379=DIRECTION('center_axis',(-0.764063486277657,-0.601098527918401,0.234280918283082));
#54380=DIRECTION('ref_axis',(-0.31305332861039,0.027922015765269,-0.949325009931561));
#54381=DIRECTION('',(-0.881100638180729,2.24206636476402E-10,-0.472928816416923));
#54382=DIRECTION('center_axis',(0.,-1.,1.45983193964168E-32));
#54383=DIRECTION('ref_axis',(1.,0.,0.));
#54384=DIRECTION('center_axis',(0.763055601588081,0.601098532777718,-0.237543054576486));
#54385=DIRECTION('ref_axis',(-0.315655968867838,0.0258667456400521,-0.948521070292115));
#54386=DIRECTION('center_axis',(0.731752155373931,-0.601098524847347,-0.32127767823481));
#54387=DIRECTION('ref_axis',(-0.383261974100595,0.0268944461499746,-0.92324804249714));
#54388=DIRECTION('center_axis',(-0.733118057082605,0.601098530103798,0.318148505397211));
#54389=DIRECTION('ref_axis',(-0.379314197018005,0.0268943310871904,-0.924876983655642));
#54390=DIRECTION('center_axis',(0.752014581597193,0.584827952222676,-0.304056467394184));
#54391=DIRECTION('ref_axis',(-0.372659392285939,-0.00326197145339533,-0.92796246523408));
#54392=DIRECTION('center_axis',(-0.913719837201684,-6.49433504233456E-10,
0.406344754000995));
#54393=DIRECTION('ref_axis',(0.406294777972886,-0.0156832196303141,0.91360745947808));
#54394=DIRECTION('',(0.913719871390962,8.3214485854382E-8,-0.40634467712187));
#54395=DIRECTION('center_axis',(0.764516880406742,0.584827969931339,-0.271090732337225));
#54396=DIRECTION('ref_axis',(-0.338976908815281,0.00704480134988046,-0.940768316889965));
#54397=DIRECTION('center_axis',(0.937431473544162,5.74387473960981E-10,
-0.348169832709298));
#54398=DIRECTION('ref_axis',(0.348127075378515,0.0156715280548011,0.937316351397344));
#54399=DIRECTION('',(-0.937431446874083,-1.40443212613657E-11,0.348169904517268));
#54400=DIRECTION('',(0.358768424268607,-3.07809289803191E-8,-0.933426600085845));
#54401=DIRECTION('center_axis',(-0.257928020727969,0.793626260387635,-0.551026764274196));
#54402=DIRECTION('ref_axis',(-2.1533635937977E-16,0.570324175992147,0.821419706531854));
#54403=DIRECTION('center_axis',(0.833069808817712,0.471546674569471,0.289203090126806));
#54404=DIRECTION('ref_axis',(-0.0947771047399993,-0.39340819536142,0.914465577394564));
#54405=DIRECTION('center_axis',(-0.728675431885439,-0.601098528055605,0.328196091591526));
#54406=DIRECTION('ref_axis',(-0.409106307232236,-0.00227571910488544,-0.912483890534709));
#54407=DIRECTION('',(-0.909057433470373,5.21554040285535E-12,-0.416670832495219));
#54408=DIRECTION('center_axis',(0.,-1.,1.45983193964168E-32));
#54409=DIRECTION('ref_axis',(1.,0.,0.));
#54410=DIRECTION('center_axis',(0.727266651289212,0.601098527417744,-0.331306169967894));
#54411=DIRECTION('ref_axis',(-0.411591737982606,-0.00432808000034288,-0.911358057487818));
#54412=DIRECTION('center_axis',(0.731752164393736,-0.601098528240813,-0.321277651341967));
#54413=DIRECTION('ref_axis',(-0.404282168821871,-0.00330179248364486,-0.914628354108421));
#54414=DIRECTION('center_axis',(-0.733118059057979,0.60109852779211,0.318148505212928));
#54415=DIRECTION('ref_axis',(-0.400371043525822,-0.00330189103679421,-0.916347164027709));
#54416=DIRECTION('center_axis',(0.707980627187698,0.58482825598716,-0.395903198428518));
#54417=DIRECTION('ref_axis',(-0.466848718286939,-0.0330815410881358,-0.883718216329773));
#54418=DIRECTION('center_axis',(-0.886386486654161,-1.08201782972538E-7,
0.462945997149647));
#54419=DIRECTION('ref_axis',(0.462889119754394,-0.015675163531169,0.88627758183386));
#54420=DIRECTION('',(0.886402259955066,0.,-0.462915795308987));
#54421=DIRECTION('center_axis',(0.724512896584358,0.584827952226229,-0.364770241354499));
#54422=DIRECTION('ref_axis',(-0.434856856697224,-0.022760729591192,-0.900211899150354));
#54423=DIRECTION('center_axis',(0.913719906847962,6.78823475718525E-10,
-0.406344597392105));
#54424=DIRECTION('ref_axis',(0.406294556518327,0.0156933905092881,0.913607383309646));
#54425=DIRECTION('',(-0.91371987086029,-2.24820162483051E-11,0.406344678315164));
#54426=DIRECTION('',(0.299450150892431,-1.43735365431748E-13,-0.954111946854509));
#54427=DIRECTION('center_axis',(-0.68179572955443,-0.601098528064928,0.416935417924071));
#54428=DIRECTION('ref_axis',(-0.500433501112916,-0.032481685474193,-0.865165447225341));
#54429=DIRECTION('',(-0.933426594324375,8.00811321699499E-12,-0.358768439258525));
#54430=DIRECTION('center_axis',(0.,-1.,1.45983193964168E-32));
#54431=DIRECTION('ref_axis',(1.,0.,0.));
#54432=DIRECTION('center_axis',(0.680008250771264,0.601098521421985,-0.419844431221028));
#54433=DIRECTION('ref_axis',(-0.502752004436133,-0.034538586081331,-0.863740417085453));
#54434=DIRECTION('center_axis',(0.731752165467864,-0.6010985306281,-0.321277644428976));
#54435=DIRECTION('ref_axis',(-0.424736200095745,-0.0335099595817295,-0.904696768501501));
#54436=DIRECTION('center_axis',(-0.733118072971343,0.601098524471746,0.31814847942537));
#54437=DIRECTION('ref_axis',(-0.420867299587536,-0.0335100717230877,-0.906503056382607));
#54438=DIRECTION('',(0.855586424288569,0.,-0.517659995144593));
#54439=DIRECTION('center_axis',(0.673082061319651,0.584827952146743,-0.452699464454661));
#54440=DIRECTION('ref_axis',(-0.525411830020171,-0.0526562728378581,-0.84921712524282));
#54441=DIRECTION('center_axis',(0.886402301749942,6.68497750786553E-10,
-0.462915715279147));
#54442=DIRECTION('ref_axis',(0.46285812786071,0.0157729998138629,0.886292031979387));
#54443=DIRECTION('',(-0.886402259954249,-1.7691403895149E-10,0.46291579531055));
#54444=DIRECTION('',(0.238950069590302,0.,-0.971031855421227));
#54445=DIRECTION('',(-0.954111946844362,6.51326541667565E-11,-0.299450150924759));
#54446=DIRECTION('center_axis',(0.,-1.,1.45983193964168E-32));
#54447=DIRECTION('ref_axis',(1.,0.,0.));
#54448=DIRECTION('center_axis',(0.724030162875529,0.60109853700323,-0.338320664546244));
#54449=DIRECTION('ref_axis',(-0.457541187731248,0.0514848956254042,-0.887696663873375));
#54450=DIRECTION('center_axis',(-0.635677097276993,0.601098535801653,0.484350264018309));
#54451=DIRECTION('ref_axis',(-0.573333766911368,0.052516506081434,-0.817637088388375));
#54452=DIRECTION('center_axis',(0.704117297543295,0.58482790806807,-0.40273458908449));
#54453=DIRECTION('ref_axis',(-0.510055260623721,0.0219600677308701,-0.85986126005032));
#54454=DIRECTION('center_axis',(-0.821390062079794,-1.90520203153216E-8,
0.570366869581809));
#54455=DIRECTION('ref_axis',(0.57029621967304,-0.0157391387082167,0.82128831803415));
#54456=DIRECTION('',(0.821393979885973,3.88578058618525E-13,-0.570361227475258));
#54457=DIRECTION('center_axis',(0.720953072804471,0.584827952320772,-0.371756550713075));
#54458=DIRECTION('ref_axis',(-0.478628082825391,0.0322834330580714,-0.877424035618398));
#54459=DIRECTION('center_axis',(0.855586464117781,5.7300538042428E-10,-0.517659929315022));
#54460=DIRECTION('ref_axis',(0.51759610946881,0.0157020800836657,0.855480982923523));
#54461=DIRECTION('',(-0.855586424289036,-7.77156117237386E-13,0.517659995143822));
#54462=DIRECTION('',(0.177506961529499,0.,-0.984119544876823));
#54463=DIRECTION('center_axis',(-0.677733658023607,-0.60109852804148,0.423506373468341));
#54464=DIRECTION('ref_axis',(-0.544549134192793,0.0232723710871578,-0.838406009755334));
#54465=DIRECTION('',(-0.971031855421207,0.,-0.238950069590381));
#54466=DIRECTION('center_axis',(0.,-1.,1.45983193964168E-32));
#54467=DIRECTION('ref_axis',(1.,0.,0.));
#54468=DIRECTION('center_axis',(0.675918145787789,0.601098531915386,-0.426397953939702));
#54469=DIRECTION('ref_axis',(-0.546857379262444,0.0212180338772051,-0.836956869727824));
#54470=DIRECTION('center_axis',(0.633601998742522,-0.60109852586306,-0.48706166898529));
#54471=DIRECTION('ref_axis',(-0.595954223605553,0.0222452659052586,-0.802710228856906));
#54472=DIRECTION('center_axis',(-0.63567705631572,0.601098529692435,0.484350325359005));
#54473=DIRECTION('ref_axis',(-0.59251948005633,0.022245165155015,-0.805248917031872));
#54474=DIRECTION('center_axis',(0.648087922879121,0.584827953016226,-0.4878097063293));
#54475=DIRECTION('ref_axis',(-0.596826936052606,-0.00784645566273247,-0.80233162815359));
#54476=DIRECTION('center_axis',(-0.783959669330724,-7.36093815513976E-10,
0.620811756382611));
#54477=DIRECTION('ref_axis',(0.620735455512434,-0.0156778483077018,0.783863316747386));
#54478=DIRECTION('',(0.783959868703302,0.,-0.620811504615291));
#54479=DIRECTION('center_axis',(0.668674692288739,0.584827952254013,-0.45918451863596));
#54480=DIRECTION('ref_axis',(-0.567546154946495,0.0024618045803074,-0.823337902397101));
#54481=DIRECTION('center_axis',(0.821394021188847,5.47809383740317E-10,
-0.570361167993768));
#54482=DIRECTION('ref_axis',(0.570291131288506,0.0156707406187205,0.82129315926905));
#54483=DIRECTION('',(-0.821393979885388,-6.42264019716009E-11,0.5703612274761));
#54484=DIRECTION('',(0.115363314586857,1.64268989064744E-13,-0.993323364090231));
#54485=DIRECTION('center_axis',(-0.619310103632507,-0.601098528057576,0.505109448640301));
#54486=DIRECTION('ref_axis',(-0.62798180126612,-0.0069195231192547,-0.778197261289425));
#54487=DIRECTION('',(-0.984119544874669,2.3449398189432E-11,-0.17750696154144));
#54488=DIRECTION('center_axis',(0.,-1.,1.45983193964168E-32));
#54489=DIRECTION('ref_axis',(1.,0.,0.));
#54490=DIRECTION('center_axis',(0.617146484443659,0.601098526356143,-0.507750704924479));
#54491=DIRECTION('ref_axis',(-0.630092308969899,-0.00897211717893297,-0.77646840456667));
#54492=DIRECTION('center_axis',(0.633601991244654,-0.601098528762654,-0.487061675160531));
#54493=DIRECTION('ref_axis',(-0.614163689544919,-0.00794568202695358,-0.789138662455274));
#54494=DIRECTION('center_axis',(-0.635677075874747,0.601098527221414,0.484350302755741));
#54495=DIRECTION('ref_axis',(-0.610786732984478,-0.00794580638708497,-0.791755284776178));
#54496=DIRECTION('center_axis',(0.581838715418155,0.584827952231152,-0.565190211813394));
#54497=DIRECTION('ref_axis',(-0.687206831789029,-0.0181546316769224,-0.726234934226632));
#54498=DIRECTION('center_axis',(-0.74343177523546,-5.95613149885961E-10,
0.668811778881214));
#54499=DIRECTION('ref_axis',(0.668729561174049,-0.015679506618148,0.743340384402849));
#54500=DIRECTION('',(0.743431828237445,2.06171493653824E-7,-0.668811719965707));
#54501=DIRECTION('center_axis',(0.605846879048239,0.584827782536647,-0.539375587064132));
#54502=DIRECTION('ref_axis',(-0.649836813202612,-0.0273551074096476,-0.759581341467311));
#54503=DIRECTION('center_axis',(0.783959932758504,6.94783626924064E-10,
-0.620811423726467));
#54504=DIRECTION('ref_axis',(0.620734884404402,0.0157023279250529,0.78386327901056));
#54505=DIRECTION('',(0.783959869213733,-1.29267396286675E-5,-0.620811503836137));
#54506=DIRECTION('',(0.0527643416803934,-7.62629077547763E-8,-0.998606991887714));
#54507=DIRECTION('center_axis',(-0.743431826069816,-8.3225866364936E-12,
0.668811722375213));
#54508=DIRECTION('ref_axis',(0.516239882061012,-0.63577280508478,0.573837367626284));
#54509=DIRECTION('',(0.993323364090158,0.,0.115363314587482));
#54510=DIRECTION('center_axis',(0.644048861750526,0.398564391578944,-0.652952899865801));
#54511=DIRECTION('ref_axis',(-0.711944358623389,-3.14655782804113E-17,-0.702235879334239));
#54512=DIRECTION('center_axis',(-0.694956629961929,5.74456601172877E-5,
0.719051652645312));
#54513=DIRECTION('ref_axis',(0.719051591920785,-0.000363148938065183,0.694956600284531));
#54514=DIRECTION('',(0.699970449419168,5.94973683762338E-5,-0.71417180454005));
#54515=DIRECTION('center_axis',(0.609965632634555,0.590180063812721,-0.528799980411062));
#54516=DIRECTION('ref_axis',(-0.329667854669152,0.795820454315329,0.507926087232368));
#54517=DIRECTION('center_axis',(-0.295192624143355,0.550037558042699,-0.78122979935086));
#54518=DIRECTION('ref_axis',(1.61303840242307E-17,0.817666865860829,0.575691667885969));
#54519=DIRECTION('center_axis',(0.878790409519382,-0.477126090101351,-0.0088380021133009));
#54520=DIRECTION('ref_axis',(0.0430060492887833,0.097628009236126,-0.994293342800384));
#54521=DIRECTION('center_axis',(0.804004432172478,0.584827951389866,-0.107485535399622));
#54522=DIRECTION('ref_axis',(-0.151410339624816,0.0265489689996098,-0.988114396868984));
#54523=DIRECTION('center_axis',(-0.973676780225177,-1.7969074443091E-11,
0.227933164875875));
#54524=DIRECTION('ref_axis',(0.227904900303916,-0.0157477670572438,0.973556040631546));
#54525=DIRECTION('center_axis',(0.984512820719522,-0.000115441120459348,
-0.175312556630262));
#54526=DIRECTION('ref_axis',(0.00445422974340059,0.999693435572462,0.024355588901113));
#54527=DIRECTION('',(-0.986067493102614,-6.06126260028834E-10,0.166345721454827));
#54528=DIRECTION('center_axis',(-0.787401801638329,-0.601098528045545,0.136671000428739));
#54529=DIRECTION('ref_axis',(-0.191602840052081,0.02792201296917,-0.981075284000023));
#54530=DIRECTION('',(-0.814879198669324,2.24206636476394E-10,-0.579630823521352));
#54531=DIRECTION('center_axis',(0.,-1.,1.45983193964168E-32));
#54532=DIRECTION('ref_axis',(1.,0.,0.));
#54533=DIRECTION('center_axis',(0.786810721571387,0.601098532483053,-0.140033719750047));
#54534=DIRECTION('ref_axis',(-0.194285705633603,0.0258667523495679,-0.980603883180838));
#54535=DIRECTION('center_axis',(0.766248842216283,-0.601098524937294,-0.227031440819144));
#54536=DIRECTION('ref_axis',(-0.264526173897541,0.0268944441817508,-0.964003419182361));
#54537=DIRECTION('center_axis',(-0.767211782381243,0.601098530024342,0.223755755630937));
#54538=DIRECTION('ref_axis',(-0.260405370577914,0.0268943328939305,-0.965124726567696));
#54539=DIRECTION('center_axis',(0.784193102256011,0.584827952222485,-0.207406472110561));
#54540=DIRECTION('ref_axis',(-0.253416325257633,-0.00326197144058285,-0.96735181068484));
#54541=DIRECTION('center_axis',(-0.957443383072194,-7.10515928356689E-10,
0.288621149972196));
#54542=DIRECTION('ref_axis',(0.288585652683465,-0.0156832196316195,0.957325627823284));
#54543=DIRECTION('',(0.957443409615542,8.32140417652626E-8,-0.28862106191988));
#54544=DIRECTION('center_axis',(0.792465114525967,0.584827969931577,-0.173133728213359));
#54545=DIRECTION('ref_axis',(-0.218394439457572,0.0070448013461047,-0.975835149801444));
#54546=DIRECTION('center_axis',(0.973676798398358,6.10870585646325E-10,
-0.227933087244314));
#54547=DIRECTION('ref_axis',(0.227905095698771,0.0156715280541824,0.973557225109537));
#54548=DIRECTION('',(-0.973676779881279,-1.44328993199777E-11,0.227933166344924));
#54549=DIRECTION('',(0.472928802167947,-3.07809289803151E-8,-0.881100645828835));
#54550=DIRECTION('center_axis',(-0.186832215098181,0.793626260387618,-0.579008706518885));
#54551=DIRECTION('ref_axis',(-2.13507208284854E-16,0.589386723415692,0.807851032221483));
#54552=DIRECTION('center_axis',(0.790254046116485,0.471546674563101,0.391333970292646));
#54553=DIRECTION('ref_axis',(-0.208633832128906,-0.393420324212994,0.895372756223546));
#54554=DIRECTION('center_axis',(-0.764063484811556,-0.601098528043994,0.234280922742262));
#54555=DIRECTION('ref_axis',(-0.291515827985554,-0.00227572128403759,-0.956563298023991));
#54556=DIRECTION('',(-0.849666541316623,5.19500677922216E-12,-0.527320366159934));
#54557=DIRECTION('center_axis',(0.,-1.,1.45983193964168E-32));
#54558=DIRECTION('ref_axis',(1.,0.,0.));
#54559=DIRECTION('center_axis',(0.763055610642251,0.601098527425935,-0.237543039034519));
#54560=DIRECTION('ref_axis',(-0.294122760511087,-0.00432807889280782,-0.955757850860999));
#54561=DIRECTION('center_axis',(0.766248848566382,-0.601098528229855,-0.227031410669529));
#54562=DIRECTION('ref_axis',(-0.286460949644773,-0.00330179593875977,-0.958086229142343));
#54563=DIRECTION('center_axis',(-0.767211782659897,0.601098527823099,0.22375576058892));
#54564=DIRECTION('ref_axis',(-0.28236525175776,-0.00330188583807953,-0.959301288516642));
#54565=DIRECTION('center_axis',(0.752014581679907,0.584827952239308,-0.304056467157619));
#54566=DIRECTION('ref_axis',(-0.352415118259546,-0.0330869090552597,-0.935258702643969));
#54567=DIRECTION('center_axis',(-0.937431425362165,-4.83895775299484E-10,
0.348169962437112));
#54568=DIRECTION('ref_axis',(0.348127185228387,-0.0156751701945908,0.937316249696084));
#54569=DIRECTION('',(0.937431446874013,8.32667268468572E-13,-0.348169904517457));
#54570=DIRECTION('center_axis',(0.764517729849789,0.58482795222609,-0.271088374963522));
#54571=DIRECTION('ref_axis',(-0.318601412284451,-0.022760729592207,-0.9476154754323));
#54572=DIRECTION('center_axis',(0.957443431034098,5.76612977251272E-10,
-0.288620990868051));
#54573=DIRECTION('ref_axis',(0.288585447520421,0.0156933905081676,0.957325522992987));
#54574=DIRECTION('',(-0.957443409238604,-2.20934381896848E-11,0.288621063170307));
#54575=DIRECTION('',(0.416670832492647,-1.43735365431753E-13,-0.909057433471552));
#54576=DIRECTION('center_axis',(-0.728675429110272,-0.601098527932451,0.328196097978636));
#54577=DIRECTION('ref_axis',(-0.388053453397706,-0.0324816879404024,-0.921064306796576));
#54578=DIRECTION('',(-0.881100638234071,8.00811321699558E-12,-0.472928816317543));
#54579=DIRECTION('center_axis',(0.,-1.,1.45983193964168E-32));
#54580=DIRECTION('ref_axis',(1.,0.,0.));
#54581=DIRECTION('center_axis',(0.727266646009034,0.601098521703302,-0.331306191926556));
#54582=DIRECTION('ref_axis',(-0.390532269241283,-0.0345385811012187,-0.919941103058652));
#54583=DIRECTION('center_axis',(0.766248846196635,-0.601098530728883,-0.227031412051072));
#54584=DIRECTION('ref_axis',(-0.30799845922305,-0.0335099577670905,-0.950796524944572));
#54585=DIRECTION('center_axis',(-0.767211793970439,0.601098524659991,0.223755730304821));
#54586=DIRECTION('ref_axis',(-0.303933680231947,-0.0335100683557745,-0.952103667328015));
#54587=DIRECTION('',(0.913719870860091,3.88578058618523E-13,-0.406344678315612));
#54588=DIRECTION('center_axis',(0.724512895936988,0.584827952146467,-0.364770242768198));
#54589=DIRECTION('ref_axis',(-0.414833672506597,-0.0526562728409388,-0.908372358168824));
#54590=DIRECTION('center_axis',(0.937431473538846,5.60668931630099E-10,
-0.348169832723611));
#54591=DIRECTION('ref_axis',(0.348126519866068,0.0157729998148864,0.937314855660988));
#54592=DIRECTION('',(-0.937431446873068,-1.76136882834246E-10,0.34816990452));
#54593=DIRECTION('',(0.358768439254553,0.,-0.933426594325902));
#54594=DIRECTION('',(-0.909057433457263,6.5132654166753E-11,-0.416670832523821));
#54595=DIRECTION('center_axis',(0.,-1.,1.45983193964168E-32));
#54596=DIRECTION('ref_axis',(1.,0.,0.));
#54597=DIRECTION('center_axis',(0.760723794998593,0.601098536495491,-0.244907854398175));
#54598=DIRECTION('ref_axis',(-0.342675438066658,0.0514849014682537,-0.938042029477693));
#54599=DIRECTION('center_axis',(-0.691369775202577,0.601098535458906,0.400859557208627));
#54600=DIRECTION('ref_axis',(-0.466335763285318,0.0525165100196524,-0.883047548015653));
#54601=DIRECTION('center_axis',(0.749041150657826,0.584827908068299,-0.311309608855329));
#54602=DIRECTION('ref_axis',(-0.398264130414358,0.0219600677272139,-0.917007872294841));
#54603=DIRECTION('center_axis',(-0.886399045287157,-1.96457150103562E-8,
0.462921950780061));
#54604=DIRECTION('ref_axis',(0.462864609877147,-0.0157391387108218,0.886289248742146));
#54605=DIRECTION('',(0.886402259955037,0.,-0.462915795309042));
#54606=DIRECTION('center_axis',(0.761861593086633,0.584827952320782,-0.278465759409983));
#54607=DIRECTION('ref_axis',(-0.364883565842199,0.0322834330579322,-0.930493290318783));
#54608=DIRECTION('center_axis',(0.913719904256589,6.14490181019606E-10,
-0.406344603219152));
#54609=DIRECTION('ref_axis',(0.406294506910647,0.0157020800829072,0.913607256065375));
#54610=DIRECTION('',(-0.91371987086035,-3.88578058618498E-13,0.406344678315031));
#54611=DIRECTION('',(0.299450150892393,0.,-0.95411194685452));
#54612=DIRECTION('center_axis',(-0.725468945452924,-0.601098528222859,0.335224355546754));
#54613=DIRECTION('ref_axis',(-0.435175071162971,0.0232723662834079,-0.90004502909903));
#54614=DIRECTION('',(-0.933426594325924,1.43735365432682E-13,-0.358768439254497));
#54615=DIRECTION('center_axis',(0.,-1.,1.45983193964168E-32));
#54616=DIRECTION('ref_axis',(1.,0.,0.));
#54617=DIRECTION('center_axis',(0.724030164751593,0.601098531862174,-0.338320669665511));
#54618=DIRECTION('ref_axis',(-0.43764673286923,0.0212180353560184,-0.898896619297525));
#54619=DIRECTION('center_axis',(0.689650872581711,-0.601098525907596,-0.403809653300909));
#54620=DIRECTION('ref_axis',(-0.490648676648319,0.0222452647620465,-0.871073489608609));
#54621=DIRECTION('center_axis',(-0.691369747346035,0.601098529780441,0.400859613768302));
#54622=DIRECTION('ref_axis',(-0.486922833503873,0.0222451626493677,-0.873161672859765));
#54623=DIRECTION('center_axis',(0.704116346373504,0.584827953375381,-0.402736186256451));
#54624=DIRECTION('ref_axis',(-0.491561927845562,-0.00784642891601187,-0.870807271815079));
#54625=DIRECTION('center_axis',(-0.85558611995522,-2.03617710913708E-9,
0.517660498145235));
#54626=DIRECTION('ref_axis',(0.517596875100651,-0.0156778482803438,0.855480964112785));
#54627=DIRECTION('',(0.855586424288614,3.88578058618633E-13,-0.51765999514452));
#54628=DIRECTION('center_axis',(0.720953073132771,0.584827952254103,-0.37175655018128));
#54629=DIRECTION('ref_axis',(-0.459879282384634,0.00246180457136728,-0.887978031908248));
#54630=DIRECTION('center_axis',(0.886402295876551,5.88964994383866E-10,
-0.462915726525661));
#54631=DIRECTION('ref_axis',(0.462858883431285,0.0156707406183786,0.886293451356387));
#54632=DIRECTION('',(-0.886402259954842,-6.37823127617598E-11,0.462915795309415));
#54633=DIRECTION('',(0.23895006959035,1.64268989064786E-13,-0.971031855421215));
#54634=DIRECTION('center_axis',(-0.677733660142661,-0.601098528074642,0.42350637003017));
#54635=DIRECTION('ref_axis',(-0.525495996600591,-0.00691952178971143,-0.850767934148292));
#54636=DIRECTION('',(-0.954111946850841,2.34493981894321E-11,-0.299450150904116));
#54637=DIRECTION('center_axis',(0.,-1.,1.45983193964168E-32));
#54638=DIRECTION('ref_axis',(1.,0.,0.));
#54639=DIRECTION('center_axis',(0.675918144140183,0.601098526458222,-0.426397964244489));
#54640=DIRECTION('ref_axis',(-0.52780653885738,-0.00897210993944167,-0.849317230946498));
#54641=DIRECTION('center_axis',(0.689650870426024,-0.601098528684547,-0.403809652848841));
#54642=DIRECTION('ref_axis',(-0.510415517766898,-0.00794568844090066,-0.859891193848355));
#54643=DIRECTION('center_axis',(-0.691369757445448,0.601098527295095,0.400859600076498));
#54644=DIRECTION('ref_axis',(-0.506737253187209,-0.00794580112719611,-0.862063930620421));
#54645=DIRECTION('center_axis',(0.648087860131304,0.584827952228637,-0.487809790638203));
#54646=DIRECTION('ref_axis',(-0.590766628087855,-0.0181546317314174,-0.806638209164681));
#54647=DIRECTION('center_axis',(-0.821393943279879,-5.02776464207159E-10,
0.570361280192766));
#54648=DIRECTION('ref_axis',(0.570291165105354,-0.015679506617579,0.821292968480193));
#54649=DIRECTION('',(0.821393981728486,2.06171105075815E-7,-0.570361224821762));
#54650=DIRECTION('center_axis',(0.66867128189068,0.584827782537022,-0.45918970104686));
#54651=DIRECTION('ref_axis',(-0.549511870141489,-0.0273551074001155,-0.835037964809224));
#54652=DIRECTION('center_axis',(0.855586473862625,6.3690949927931E-10,-0.517659913208778));
#54653=DIRECTION('ref_axis',(0.517596091348888,0.0157023279254066,0.855480989337622));
#54654=DIRECTION('',(0.855586424697114,-1.2926739628574E-5,-0.517659994307953));
#54655=DIRECTION('',(0.1775069224395,-7.62629077547996E-8,-0.984119551927535));
#54656=DIRECTION('center_axis',(-0.821393979889483,4.55998777965875E-12,
0.570361227470202));
#54657=DIRECTION('ref_axis',(0.440248283555354,-0.635772805085312,0.634014502310885));
#54658=DIRECTION('',(0.971031855420999,0.,0.238950069591228));
#54659=DIRECTION('center_axis',(0.720807042410979,0.39856439158468,-0.567083444804617));
#54660=DIRECTION('ref_axis',(-0.618316971226317,2.54116158780968E-16,-0.785928828262149));
#54661=DIRECTION('center_axis',(-0.779597758073224,5.74456515223888E-5,
0.626280553990941));
#54662=DIRECTION('ref_axis',(0.626280497544892,-0.00036285465843142,0.77959772109173));
#54663=DIRECTION('',(0.783960434937778,5.94973676301789E-5,-0.620810786723486));
#54664=DIRECTION('center_axis',(0.6714320830097,0.590180063806611,-0.448181269343644));
#54665=DIRECTION('ref_axis',(-0.390731048633041,0.795821036217624,0.462599314685649));
#54666=DIRECTION('center_axis',(-0.194950885223199,0.550037558043462,-0.812067015148551));
#54667=DIRECTION('ref_axis',(1.05327946492612E-16,0.827952943471004,0.560797577917114));
#54668=DIRECTION('center_axis',(0.872968580073513,-0.477126090041954,0.101373331827024));
#54669=DIRECTION('ref_axis',(0.16728754861143,0.097632994085021,-0.981062013608504));
#54670=DIRECTION('center_axis',(0.811136126793024,0.584827951390207,-0.0058695045741029));
#54671=DIRECTION('ref_axis',(-0.026372851389724,0.0265489689940623,-0.999299567174392));
#54672=DIRECTION('center_axis',(-0.994566648465754,-2.99637009883098E-11,
0.104101785573529));
#54673=DIRECTION('ref_axis',(0.104088876559904,-0.0157477670567439,0.994443318449686));
#54674=DIRECTION('center_axis',(0.998722132125226,-0.000115441216901894,
-0.0505380003222111));
#54675=DIRECTION('ref_axis',(0.00137352177937294,0.999690005520608,0.0248597325031408));
#54676=DIRECTION('',(-0.999140703554944,-6.06958927296906E-10,0.0414470083327064));
#54677=DIRECTION('center_axis',(-0.798322321672281,-0.60109852804191,0.0369056947587686));
#54678=DIRECTION('ref_axis',(-0.067130656640417,0.0279220130298706,-0.997353415859888));
#54679=DIRECTION('',(-0.735806627409701,2.24062901110931E-10,-0.677191706284094));
#54680=DIRECTION('center_axis',(0.,-1.,1.45983193964168E-32));
#54681=DIRECTION('ref_axis',(1.,0.,0.));
#54682=DIRECTION('center_axis',(0.798157363031323,0.601098532444239,-0.0403159786222247));
#54683=DIRECTION('ref_axis',(-0.0698514481007516,0.0258667532426018,-0.997221984452266));
#54684=DIRECTION('center_axis',(0.78866132617452,-0.601098525006615,-0.129204782541199));
#54685=DIRECTION('ref_axis',(-0.14161863837021,0.0268944426871824,-0.989555885343882));
#54686=DIRECTION('center_axis',(-0.789206120912546,0.601098530062168,0.125834239661842));
#54687=DIRECTION('ref_axis',(-0.137389792491866,0.0268943319889687,-0.990151877151131));
#54688=DIRECTION('center_axis',(0.804004429227664,0.584827952222659,-0.107485552895957));
#54689=DIRECTION('ref_axis',(-0.130176731423392,-0.00326197144762294,-0.991485440204846));
#54690=DIRECTION('center_axis',(-0.986067481533857,-5.45168758924053E-10,
0.166345790032317));
#54691=DIRECTION('ref_axis',(0.16632533129643,-0.0156832196306599,0.985946205830292));
#54692=DIRECTION('',(0.986067493321353,8.32139862540711E-8,-0.166345720158157));
#54693=DIRECTION('center_axis',(0.807915700397312,0.584827969931308,-0.0724463017520282));
#54694=DIRECTION('ref_axis',(-0.0943677593111905,0.00704480135220278,-0.995512479467984));
#54695=DIRECTION('center_axis',(0.994566654888419,4.60698908371065E-10,
-0.104101724212714));
#54696=DIRECTION('ref_axis',(0.104088939895806,0.0156715280552417,0.994444516199763));
#54697=DIRECTION('',(-0.99456664842325,-1.40443212613684E-11,0.104101785979601));
#54698=DIRECTION('',(0.579630810343267,-3.07809289803229E-8,-0.814879208043012));
#54699=DIRECTION('center_axis',(-0.112789953828636,0.793626260387895,-0.597859335578244));
#54700=DIRECTION('ref_axis',(-7.60995088010986E-17,0.601698864092707,0.798723028934026));
#54701=DIRECTION('center_axis',(0.734975505022815,0.471546674564434,0.487293279990277));
#54702=DIRECTION('ref_axis',(-0.319217348238282,-0.393408855917977,0.86216573619521));
#54703=DIRECTION('center_axis',(-0.787401802043575,-0.601098528049665,0.13667099807588));
#54704=DIRECTION('ref_axis',(-0.169327965428505,-0.00227571981498317,-0.985557132399318));
#54705=DIRECTION('',(-0.776875900240117,5.05127141378907E-12,-0.629653742644406));
#54706=DIRECTION('center_axis',(0.,-1.,1.45983193964168E-32));
#54707=DIRECTION('ref_axis',(1.,0.,0.));
#54708=DIRECTION('center_axis',(0.786810727775904,0.601098527454823,-0.140033706472389));
#54709=DIRECTION('ref_axis',(-0.172015286604093,-0.00432807421381841,-0.985084772467888));
#54710=DIRECTION('center_axis',(0.788661328976348,-0.601098528218721,-0.129204750495282));
#54711=DIRECTION('ref_axis',(-0.164122071343041,-0.00330179825181832,-0.986434510662707));
#54712=DIRECTION('center_axis',(-0.789206121376638,0.601098527829134,0.125834247418145));
#54713=DIRECTION('ref_axis',(-0.159906386064952,-0.00330188499779538,-0.987126661199619));
#54714=DIRECTION('center_axis',(0.784195235648826,0.584828255987593,-0.207397549127737));
#54715=DIRECTION('ref_axis',(-0.232410023808953,-0.033081541078036,-0.972055138597098));
#54716=DIRECTION('center_axis',(-0.973669012885895,-1.08205910182348E-7,
0.227966342572307));
#54717=DIRECTION('ref_axis',(0.227938335612477,-0.015675163532481,0.973549384677759));
#54718=DIRECTION('',(0.973676779881262,3.88578058618882E-13,-0.227933166344996));
#54719=DIRECTION('center_axis',(0.792465661815022,0.584827952226149,-0.173131282959057));
#54720=DIRECTION('ref_axis',(-0.197321433276741,-0.0227607295932086,-0.980074589588975));
#54721=DIRECTION('center_axis',(0.986067506826153,6.31299538322982E-10,
-0.166345640104134));
#54722=DIRECTION('ref_axis',(0.16632515482247,0.0156933905090719,0.98594607376246));
#54723=DIRECTION('',(-0.98606749310408,-2.28705943069118E-11,0.166345721446137));
#54724=DIRECTION('',(0.527320366157672,0.,-0.849666541318027));
#54725=DIRECTION('center_axis',(-0.764063484700029,-0.601098528029406,0.234280923143411));
#54726=DIRECTION('ref_axis',(-0.269553565881082,-0.0324816861699376,-0.962437434425922));
#54727=DIRECTION('',(-0.814879198734831,8.1518485824293E-12,-0.579630823429258));
#54728=DIRECTION('center_axis',(0.,-1.,1.45983193964168E-32));
#54729=DIRECTION('ref_axis',(1.,0.,0.));
#54730=DIRECTION('center_axis',(0.763055608651005,0.601098521833866,-0.237543059581597));
#54731=DIRECTION('ref_axis',(-0.272153609616772,-0.0345385788119736,-0.96163376570616));
#54732=DIRECTION('center_axis',(0.788661328100161,-0.601098530387989,-0.129204745751426));
#54733=DIRECTION('ref_axis',(-0.186403388257063,-0.0335099640094169,-0.981901654524716));
#54734=DIRECTION('center_axis',(-0.789206129626374,0.601098524547363,0.125834211354237));
#54735=DIRECTION('ref_axis',(-0.18220683847475,-0.0335100703121061,-0.982689036878256));
#54736=DIRECTION('',(0.957443409238448,3.88578058618626E-13,-0.288621063170825));
#54737=DIRECTION('center_axis',(0.764517729385345,0.584827952146375,-0.271088376445309));
#54738=DIRECTION('ref_axis',(-0.297713340163934,-0.0526562728410443,-0.953202016373719));
#54739=DIRECTION('center_axis',(0.973676797912358,5.80360093127206E-10,
-0.227933089320392));
#54740=DIRECTION('ref_axis',(0.227904734093392,0.0157729998154154,0.973555671060799));
#54741=DIRECTION('',(-0.973676779880651,-1.76914038951436E-10,0.227933166347607));
#54742=DIRECTION('',(0.472928816313919,0.,-0.881100638236016));
#54743=DIRECTION('',(-0.84966654129999,6.52763895321867E-11,-0.527320366186736));
#54744=DIRECTION('center_axis',(0.,-1.,1.45983193964168E-32));
#54745=DIRECTION('ref_axis',(1.,0.,0.));
#54746=DIRECTION('center_axis',(0.785420354371214,0.601098536404089,-0.147632708002865));
#54747=DIRECTION('ref_axis',(-0.222405497715741,0.0514849025470141,-0.973593908873478));
#54748=DIRECTION('center_axis',(-0.736159142124515,0.601098535395105,0.311047051444564));
#54749=DIRECTION('ref_axis',(-0.351983362770681,0.0525165107314909,-0.934531823124945));
#54750=DIRECTION('center_axis',(0.782151897001614,0.584827930050724,-0.21497605040879));
#54751=DIRECTION('ref_axis',(-0.280192919620054,0.0219594825788432,-0.959692507483339));
#54752=DIRECTION('center_axis',(-0.937430242585242,-9.64037678221773E-9,
0.348173146992377));
#54753=DIRECTION('ref_axis',(0.348130019649239,-0.0157391393477757,0.937314124993117));
#54754=DIRECTION('',(0.937431446873851,3.88578058618657E-13,-0.348169904517893));
#54755=DIRECTION('center_axis',(0.790755100932567,0.584827952320671,-0.180783396730828));
#54756=DIRECTION('ref_axis',(-0.245384617052312,0.0322834330591902,-0.968888109981748));
#54757=DIRECTION('center_axis',(0.957443430073302,5.35836324334506E-10,
-0.2886209940553));
#54758=DIRECTION('ref_axis',(0.288585411333215,0.0157020800824498,0.957325391414394));
#54759=DIRECTION('',(-0.957443409238708,-8.32667268468881E-13,0.288621063169962));
#54760=DIRECTION('',(0.416670832492843,0.,-0.909057433471462));
#54761=DIRECTION('center_axis',(-0.761763160213927,-0.601098528106845,0.2416556377341));
#54762=DIRECTION('ref_axis',(-0.318938027994497,0.0232723693707062,-0.947489805287031));
#54763=DIRECTION('',(-0.881100638235951,1.43735365432651E-13,-0.472928816314041));
#54764=DIRECTION('center_axis',(0.,-1.,1.45983193964168E-32));
#54765=DIRECTION('ref_axis',(1.,0.,0.));
#54766=DIRECTION('center_axis',(0.760723795872547,0.601098531745845,-0.244907863340997));
#54767=DIRECTION('ref_axis',(-0.321534133665856,0.0212180385557474,-0.946660232463366));
#54768=DIRECTION('center_axis',(0.734823540351965,-0.601098525986883,-0.314189316497238));
#54769=DIRECTION('ref_axis',(-0.377605305630028,0.0222452626969263,-0.925699401235411));
#54770=DIRECTION('center_axis',(-0.736159118843831,0.601098529596128,0.311047117749781));
#54771=DIRECTION('ref_axis',(-0.373647131821486,0.0222451677062268,-0.927304142876165));
#54772=DIRECTION('center_axis',(0.749040407179186,0.584827953375494,-0.311311312617244));
#54773=DIRECTION('ref_axis',(-0.378544724015712,-0.00784642890189125,-0.925549742300951));
#54774=DIRECTION('center_axis',(-0.913719631733798,-2.04042747348083E-9,
0.406345216022352));
#54775=DIRECTION('ref_axis',(0.406295274186236,-0.0156778482801616,0.913607330994687));
#54776=DIRECTION('',(0.91371987086025,3.88578058618712E-13,-0.406344678315255));
#54777=DIRECTION('center_axis',(0.761861593344965,0.584827952254111,-0.278465758843226));
#54778=DIRECTION('ref_axis',(-0.344959838812461,0.0024618045699357,-0.938614217410295));
#54779=DIRECTION('center_axis',(0.937431472565835,5.58909274130683E-10,
-0.3481698353434));
#54780=DIRECTION('ref_axis',(0.348127082309473,0.0156707406182684,0.937316361988399));
#54781=DIRECTION('',(-0.937431446873651,-6.41708908203805E-11,0.348169904518431));
#54782=DIRECTION('',(0.358768439254525,1.642689890648E-13,-0.933426594325913));
#54783=DIRECTION('center_axis',(-0.725468949669201,-0.601098528058629,0.335224346716666));
#54784=DIRECTION('ref_axis',(-0.414722809127897,-0.00691952313171273,-0.909921486606782));
#54785=DIRECTION('',(-0.909057433466375,2.34493981894292E-11,-0.416670832503941));
#54786=DIRECTION('center_axis',(0.,-1.,1.45983193964168E-32));
#54787=DIRECTION('ref_axis',(1.,0.,0.));
#54788=DIRECTION('center_axis',(0.724030164855667,0.601098526489808,-0.338320678987934));
#54789=DIRECTION('ref_axis',(-0.417196949127517,-0.008972107745217,-0.908771812349668));
#54790=DIRECTION('center_axis',(0.734823539271242,-0.60109852864006,-0.314189313948835));
#54791=DIRECTION('ref_axis',(-0.398617790674048,-0.0079456920901308,-0.917082724150526));
#54792=DIRECTION('center_axis',(-0.736159130438184,0.601098527290318,0.311047094765258));
#54793=DIRECTION('ref_axis',(-0.394696218349555,-0.00794580135155318,-0.918777317668129));
#54794=DIRECTION('center_axis',(0.704116272234799,0.584827952230113,-0.40273631753854));
#54795=DIRECTION('ref_axis',(-0.485009681656924,-0.0181546316947643,-0.874320317759502));
#54796=DIRECTION('center_axis',(-0.886402227433596,-5.50280066249969E-10,
0.462915857581872));
#54797=DIRECTION('ref_axis',(0.462858950871009,-0.0156795066187817,0.886293261099722));
#54798=DIRECTION('',(0.886402261451109,2.06171493653986E-7,-0.462915792444281));
#54799=DIRECTION('center_axis',(0.720950339158042,0.584827782536829,-0.371762119158151));
#54800=DIRECTION('ref_axis',(-0.440520796642366,-0.0273551074055604,-0.89732554060631));
#54801=DIRECTION('center_axis',(0.91371990856544,6.13568318143281E-10,-0.406344593530127));
#54802=DIRECTION('ref_axis',(0.406294495641273,0.0157023279256281,0.913607256817348));
#54803=DIRECTION('',(0.91371987116043,-1.29267404456195E-5,-0.406344677434645));
#54804=DIRECTION('',(0.299450112994266,-7.62629077548155E-8,-0.954111958748928));
#54805=DIRECTION('center_axis',(-0.886402259959937,8.07131938721877E-12,
0.462915795299659));
#54806=DIRECTION('ref_axis',(0.357313706637834,-0.635772805085138,0.684192849540908));
#54807=DIRECTION('',(0.933426594325498,0.,0.358768439255605));
#54808=DIRECTION('center_axis',(0.78619766542402,0.398564391587654,-0.472270745060694));
#54809=DIRECTION('ref_axis',(-0.514938355828296,-1.84676138194459E-16,-0.857227210077265));
#54810=DIRECTION('center_axis',(-0.85194416385074,5.74456496553722E-5,0.523632636855898));
#54811=DIRECTION('ref_axis',(0.523632585551374,-0.000362597540125659,0.851944120158011));
#54812=DIRECTION('',(0.855586896082549,5.94973692289276E-5,-0.517659211945361));
#54813=DIRECTION('center_axis',(0.722309648105342,0.590180063812333,-0.360494472263318));
#54814=DIRECTION('ref_axis',(-0.445629721318181,0.795821199110888,0.409978987904977));
#54815=DIRECTION('center_axis',(-0.0916346543850253,0.5500375580439,-0.830097449012368));
#54816=DIRECTION('ref_axis',(-4.21286816843194E-17,0.833604678689015,0.552361511754561));
#54817=DIRECTION('center_axis',(0.853379514663138,-0.477126089924881,0.209985947782943));
#54818=DIRECTION('ref_axis',(0.288924638246151,0.0976260041170478,-0.952361127269729));
#54819=DIRECTION('center_axis',(0.805475720145869,0.584827951390078,0.0958390918591059));
#54820=DIRECTION('ref_axis',(0.0990805524777462,0.0265489689969947,-0.994725186353448));
#54821=DIRECTION('center_axis',(-0.999771606733593,7.98851526112104E-15,
-0.0213713445840403));
#54822=DIRECTION('ref_axis',(-0.0213686944566971,-0.015747767056506,0.999647631283119));
#54823=DIRECTION('center_axis',(0.997181000919987,-0.000115441232581829,
0.0750335796662666));
#54824=DIRECTION('ref_axis',(0.001753101083015,-0.99968999170467,-0.0248364071900295));
#54825=DIRECTION('',(-0.996456868254473,-6.06514838087359E-10,-0.0841053488696623));
#54826=DIRECTION('center_axis',(-0.79665282157886,-0.601098527948266,-0.0634416390777339));
#54827=DIRECTION('ref_axis',(0.0584002199716004,0.0279220150878775,-0.997902688332234));
#54828=DIRECTION('',(-0.645129946086362,2.24206636476389E-10,-0.764072871303914));
#54829=DIRECTION('center_axis',(0.,-1.,1.45983193964168E-32));
#54830=DIRECTION('ref_axis',(1.,0.,0.));
#54831=DIRECTION('center_axis',(0.79691658507517,0.601098532103177,0.0600375810266817));
#54832=DIRECTION('ref_axis',(0.0556844176437354,0.0258667610074719,-0.998113298331738));
#54833=DIRECTION('center_axis',(0.798636149364674,-0.601098525218913,-0.0293404824025407));
#54834=DIRECTION('ref_axis',(-0.0164776880985398,0.0268944380938454,-0.9995024637261));
#54835=DIRECTION('center_axis',(-0.798754206951309,0.601098529797617,0.0259282539467715));
#54836=DIRECTION('ref_axis',(-0.0122075043862703,0.0268943379739908,-0.999563740549646));
#54837=DIRECTION('center_axis',(0.811136126064599,0.584827952222597,-0.00586952230073281));
#54838=DIRECTION('ref_axis',(-0.00488417276898191,-0.00326197145228212,
-0.999982752050558));
#54839=DIRECTION('center_axis',(-0.999140700839568,-5.13744792983439E-10,
0.0414470737907721));
#54840=DIRECTION('ref_axis',(0.0414419762542119,-0.0156832196311383,0.999017817271618));
#54841=DIRECTION('',(0.999140703609452,8.32140417652197E-8,-0.0414470070186271));
#54842=DIRECTION('center_axis',(0.810624973045492,0.584827969931702,0.0293836461413375));
#54843=DIRECTION('ref_axis',(0.0311471567522389,0.00704480134473847,-0.999489982641279));
#54844=DIRECTION('center_axis',(0.999771605383917,4.91098306320819E-10,
0.0213714077230609));
#54845=DIRECTION('ref_axis',(-0.0213687831950173,0.0156715280538888,0.999648827495546));
#54846=DIRECTION('',(-0.99977160679441,-1.44884104712086E-11,-0.0213713417389639));
#54847=DIRECTION('',(0.677191694384778,-3.07809289803371E-8,-0.735806638361106));
#54848=DIRECTION('center_axis',(-0.0369689276092246,0.793626260387842,-0.60728136577227));
#54849=DIRECTION('ref_axis',(-6.40118045451157E-18,0.607696777838784,0.794169142062546));
#54850=DIRECTION('center_axis',(0.668105961119928,0.471546674587854,0.575567683596947));
#54851=DIRECTION('ref_axis',(-0.424747386385162,-0.393422882089557,0.815357647665931));
#54852=DIRECTION('center_axis',(-0.79832232140634,-0.601098528027703,0.0369057007428594));
#54853=DIRECTION('ref_axis',(-0.0444697081985339,-0.00227572478171658,-0.999008141172761));
#54854=DIRECTION('',(-0.691833462133681,5.19500677922273E-12,-0.722057103470442));
#54855=DIRECTION('center_axis',(0.,-1.,1.45983193964168E-32));
#54856=DIRECTION('ref_axis',(1.,0.,0.));
#54857=DIRECTION('center_axis',(0.79815736744895,0.601098527458077,-0.0403159655061622));
#54858=DIRECTION('ref_axis',(-0.0471950343009395,-0.00432807382640624,-0.998876316925317));
#54859=DIRECTION('center_axis',(0.798636148022719,-0.601098528218913,-0.0293404574690105));
#54860=DIRECTION('ref_axis',(-0.0391948925249827,-0.00330179850900792,-0.999226129825757));
#54861=DIRECTION('center_axis',(-0.798754208373615,0.601098527841249,0.025928255485519));
#54862=DIRECTION('ref_axis',(-0.0349257031272392,-0.00330188269111536,-0.99938445696927));
#54863=DIRECTION('center_axis',(0.804005427453076,0.584828255987368,-0.107476432880749));
#54864=DIRECTION('ref_axis',(-0.1087465876337,-0.03308154108069,-0.993518893286762));
#54865=DIRECTION('center_axis',(-0.994563102620099,-1.08065969665897E-7,
0.104135656269459));
#54866=DIRECTION('ref_axis',(0.104122863543029,-0.0156751635318716,0.994440907513286));
#54867=DIRECTION('',(0.994566648423216,0.,-0.10410178597993));
#54868=DIRECTION('center_axis',(0.807915936897985,0.584827952226251,-0.0724438071963501));
#54869=DIRECTION('ref_axis',(-0.0729295773905037,-0.0227607295923756,-0.997077342000141));
#54870=DIRECTION('center_axis',(0.999140706524478,5.45925022813738E-10,
-0.0414469367476885));
#54871=DIRECTION('ref_axis',(0.0414418325971275,0.0156933905076496,0.999017663510193));
#54872=DIRECTION('',(-0.99914070355531,-2.24820162482996E-11,0.0414470083238722));
#54873=DIRECTION('',(0.629653742642299,0.,-0.776875900241824));
#54874=DIRECTION('center_axis',(-0.787401800997156,-0.601098527900108,0.136671004762377));
#54875=DIRECTION('ref_axis',(-0.146802662815299,-0.0324816885186914,-0.988632347286549));
#54876=DIRECTION('',(-0.735806627485984,8.17238220606064E-12,-0.677191706201208));
#54877=DIRECTION('center_axis',(0.,-1.,1.45983193964168E-32));
#54878=DIRECTION('ref_axis',(1.,0.,0.));
#54879=DIRECTION('center_axis',(0.786810728237449,0.601098522108102,-0.140033726830044));
#54880=DIRECTION('ref_axis',(-0.14948292141722,-0.0345385739796511,-0.988160889284749));
#54881=DIRECTION('center_axis',(0.798636146090112,-0.601098530631398,-0.0293404606492082));
#54882=DIRECTION('ref_axis',(-0.0618686383501138,-0.0335099595911008,-0.997521605879745));
#54883=DIRECTION('center_axis',(-0.798754211564724,0.601098524902521,0.0259282253081593));
#54884=DIRECTION('ref_axis',(-0.0576064969356273,-0.0335100640083441,-0.997776812278659));
#54885=DIRECTION('',(0.986067493104221,0.,-0.166345721445301));
#54886=DIRECTION('center_axis',(0.792465661535211,0.584827952145566,-0.173131284512027));
#54887=DIRECTION('ref_axis',(-0.175897890623464,-0.0526562728562727,-0.982999109360279));
#54888=DIRECTION('center_axis',(0.994566658297495,7.04166480481068E-10,
-0.10410169164309));
#54889=DIRECTION('ref_axis',(0.104088741225509,0.015772999814322,0.994442932715069));
#54890=DIRECTION('',(-0.994566648422976,-1.76969550102655E-10,0.104101785982223));
#54891=DIRECTION('',(0.579630823425986,0.,-0.814879198737159));
#54892=DIRECTION('',(-0.776875900220307,6.49889188013141E-11,-0.629653742668848));
#54893=DIRECTION('center_axis',(0.,-1.,1.45983193964168E-32));
#54894=DIRECTION('ref_axis',(1.,0.,0.));
#54895=DIRECTION('center_axis',(0.797730365318786,0.601098536214713,-0.0480293036477394));
#54896=DIRECTION('ref_axis',(-0.0986280882349215,0.0514849047391242,-0.993791630471463));
#54897=DIRECTION('center_axis',(-0.769338840674988,0.601098535510728,0.216329144674784));
#54898=DIRECTION('ref_axis',(-0.232079971852678,0.0525165093863018,-0.971277974066507));
#54899=DIRECTION('center_axis',(0.802928089510673,0.58482792304435,-0.115250958791558));
#54900=DIRECTION('ref_axis',(-0.157701893482256,0.0219596690837393,-0.987242566812151));
#54901=DIRECTION('center_axis',(-0.973675747383018,-1.25141579433899E-8,
0.227937576889204));
#54902=DIRECTION('ref_axis',(0.227909342926954,-0.0157391391449199,0.973555140146454));
#54903=DIRECTION('',(0.973676779881215,0.,-0.227933166345199));
#54904=DIRECTION('center_axis',(0.807177928460976,0.584827952320853,-0.0802499718981004));
#54905=DIRECTION('ref_axis',(-0.122015806272558,0.0322834330565352,-0.992002985363321));
#54906=DIRECTION('center_axis',(0.986067504831869,5.22694560534451E-10,
-0.1663456519259));
#54907=DIRECTION('ref_axis',(0.166325143951013,0.015702080081768,0.985945937245436));
#54908=DIRECTION('',(-0.986067493104268,-8.32667268468834E-13,0.16634572144502));
#54909=DIRECTION('',(0.527320366157604,0.,-0.849666541318069));
#54910=DIRECTION('center_axis',(-0.786043912893678,-0.601098528080546,0.144275869576991));
#54911=DIRECTION('ref_axis',(-0.197671144361105,0.0232723701079249,-0.97999209970108));
#54912=DIRECTION('',(-0.814879198737222,0.,-0.579630823425897));
#54913=DIRECTION('center_axis',(0.,-1.,1.45983193964168E-32));
#54914=DIRECTION('ref_axis',(1.,0.,0.));
#54915=DIRECTION('center_axis',(0.785420358017335,0.601098531523994,-0.147632708474847));
#54916=DIRECTION('ref_axis',(-0.200350744918924,0.0212180447058338,-0.979494447962465));
#54917=DIRECTION('center_axis',(0.768407600938775,-0.601098526051774,-0.219614026869643));
#54918=DIRECTION('ref_axis',(-0.258606873673701,0.0222452610627766,-0.965726479521486));
#54919=DIRECTION('center_axis',(-0.769338824807468,0.60109852954767,0.216329217674113));
#54920=DIRECTION('ref_axis',(-0.254478787566266,0.0222451690245878,-0.966822475500994));
#54921=DIRECTION('center_axis',(0.782151653292242,0.584827953375421,-0.214976873646746));
#54922=DIRECTION('ref_axis',(-0.259557643786552,-0.00784642891152066,-0.965695740440699));
#54923=DIRECTION('center_axis',(-0.957443242555532,-1.95480487174851E-9,
0.288621616107921));
#54924=DIRECTION('ref_axis',(0.288586143092863,-0.0156778482815104,0.957325567969459));
#54925=DIRECTION('',(0.957443409238456,0.,-0.2886210631708));
#54926=DIRECTION('center_axis',(0.790755101116753,0.584827952254255,-0.180783396140045));
#54927=DIRECTION('ref_axis',(-0.224600172512662,0.00246180456921715,-0.974447896003448));
#54928=DIRECTION('center_axis',(0.973676796191129,5.41348134919956E-10,
-0.22793309667308));
#54929=DIRECTION('ref_axis',(0.227905107940483,0.0156707406184557,0.973557234918988));
#54930=DIRECTION('',(-0.973676779881,-6.42264019716094E-11,0.227933166346118));
#54931=DIRECTION('',(0.472928816313867,1.64268989064855E-13,-0.881100638236044));
#54932=DIRECTION('center_axis',(-0.761763162109401,-0.601098528069507,0.241655631851939));
#54933=DIRECTION('ref_axis',(-0.297409192544541,-0.00691952221419285,-0.954725034972023));
#54934=DIRECTION('',(-0.849666541311454,2.36136671784956E-11,-0.527320366168264));
#54935=DIRECTION('center_axis',(0.,-1.,1.45983193964168E-32));
#54936=DIRECTION('ref_axis',(1.,0.,0.));
#54937=DIRECTION('center_axis',(0.760723795752158,0.601098526498427,-0.244907876594135));
#54938=DIRECTION('ref_axis',(-0.300007915937367,-0.00897210709785068,-0.953894518104147));
#54939=DIRECTION('center_axis',(0.768407598352854,-0.601098528653796,-0.219614028795614));
#54940=DIRECTION('ref_axis',(-0.280533628432852,-0.00794569101660869,-0.959811309223103));
#54941=DIRECTION('center_axis',(-0.769338832903073,0.601098527321917,0.21632919506798));
#54942=DIRECTION('ref_axis',(-0.276430591656974,-0.00794579897947787,-0.961001036562788));
#54943=DIRECTION('center_axis',(0.749021847101764,0.584826536164618,-0.311358627890662));
#54944=DIRECTION('ref_axis',(-0.371641576340283,-0.018184624961436,-0.928198178273542));
#54945=DIRECTION('center_axis',(-0.937431424039985,-5.13910947046991E-10,
0.348169965997019));
#54946=DIRECTION('ref_axis',(0.348127165115549,-0.0156795066182876,0.937316184636123));
#54947=DIRECTION('',(0.937431447998912,2.06171160587093E-7,-0.348169901488658));
#54948=DIRECTION('center_axis',(0.761859578895022,0.584827782536468,-0.278471626596639));
#54949=DIRECTION('ref_axis',(-0.324582447047109,-0.0273551074266564,-0.945461756585948));
#54950=DIRECTION('center_axis',(0.957443440341857,7.30692533559346E-10,
-0.288620959991386));
#54951=DIRECTION('ref_axis',(0.288585376147215,0.0157023279247365,0.957325397956053));
#54952=DIRECTION('',(0.957443409426106,-1.29267410337996E-5,-0.288621062258828));
#54953=DIRECTION('',(0.416670796384349,-7.62630514902167E-8,-0.909057450021959));
#54954=DIRECTION('center_axis',(-0.937431446875436,3.17801790996086E-12,
0.348169904513626));
#54955=DIRECTION('ref_axis',(0.268744079129297,-0.635772805085123,0.723581066810858));
#54956=DIRECTION('',(0.8811006382356,0.,0.472928816314695));
#54957=DIRECTION('center_axis',(0.839189481601217,0.398564391590654,-0.370010053547));
#54958=DIRECTION('ref_axis',(-0.42901236436663,0.903298616859648,2.02564385446472E-16));
#54959=DIRECTION('center_axis',(-0.910854901243392,5.744564612845E-5,0.412726720216767));
#54960=DIRECTION('ref_axis',(0.412726674767955,-0.00036272125224494,0.910854851427097));
#54961=DIRECTION('',(0.91372024077296,5.94973683052012E-5,-0.406343842160635));
#54962=DIRECTION('center_axis',(0.761795958734543,0.59018006380744,-0.267122461691196));
#54963=DIRECTION('ref_axis',(0.493508984532234,-0.795824167217403,-0.350874303787966));
#54964=DIRECTION('center_axis',(0.0131267096924739,0.550037558044511,-0.835036750229043));
#54965=DIRECTION('ref_axis',(-1.16798815570368E-17,0.835108702330798,0.550084952794903));
#54966=DIRECTION('center_axis',(0.820332144110193,-0.477126090614814,0.315286959759198));
#54967=DIRECTION('ref_axis',(0.40600907759125,0.0976264307245231,-0.908639482378733));
#54968=DIRECTION('center_axis',(0.787112480220966,0.58482795138957,0.196036248571223));
#54969=DIRECTION('ref_axis',(0.22297139685242,0.0265489690048779,-0.974463395120852));
#54970=DIRECTION('center_axis',(-0.989209569180196,-1.7727863172603E-12,
-0.146507434085546));
#54971=DIRECTION('ref_axis',(-0.146489266611052,-0.0157477670559463,0.989086903462232));
#54972=DIRECTION('center_axis',(0.97991372776366,-0.00011544114226027,0.199421846380157));
#54973=DIRECTION('ref_axis',(0.00484665943939179,-0.999690671402767,-0.0243940854012324));
#54974=DIRECTION('',(-0.978058312887152,-6.06514838087335E-10,-0.208331314478496));
#54975=DIRECTION('center_axis',(-0.782419630478694,-0.601098527966524,-0.162788456341543));
#54976=DIRECTION('ref_axis',(0.183010087021585,0.0279220146957969,-0.982714439266911));
#54977=DIRECTION('',(-0.5442791801312,2.24206636476379E-10,-0.838904150708357));
#54978=DIRECTION('center_axis',(0.,-1.,1.45983193964168E-32));
#54979=DIRECTION('ref_axis',(1.,0.,0.));
#54980=DIRECTION('center_axis',(0.783107954819573,0.601098531987497,0.159444303569561));
#54981=DIRECTION('ref_axis',(0.180342099955132,0.0258667636464215,-0.983263768030854));
#54982=DIRECTION('center_axis',(0.796016001373979,-0.601098525456467,0.0709865356996868));
#54983=DIRECTION('ref_axis',(0.108923126008378,0.0268944328893104,-0.993686289580432));
#54984=DIRECTION('center_axis',(-0.795705463599409,0.601098529740564,-0.0743866435711483));
#54985=DIRECTION('ref_axis',(0.113167309509515,0.0268943392310359,-0.99321188805597));
#54986=DIRECTION('center_axis',(0.805475721645465,0.584827952222615,0.0958390741755142));
#54987=DIRECTION('ref_axis',(0.120485412214686,-0.00326197145288064,-0.992709738536748));
#54988=DIRECTION('center_axis',(-0.996456874308969,-5.64487442434603E-10,
-0.0841052771376477));
#54989=DIRECTION('ref_axis',(-0.0840949330836856,-0.0156832196320191,0.996334320823901));
#54990=DIRECTION('',(0.996456868143877,8.32144303432584E-8,0.0841053501799309));
#54991=DIRECTION('center_axis',(0.80055020562484,0.584827969931446,0.130750196404785));
#54992=DIRECTION('ref_axis',(0.156170863565598,0.00704480135073622,-0.987704931721566));
#54993=DIRECTION('center_axis',(0.989209560314072,4.75626585929023E-10,
0.146507493949079));
#54994=DIRECTION('ref_axis',(-0.146489501966464,0.0156715280545244,0.9890880795066));
#54995=DIRECTION('',(-0.989209569691783,-1.4432899319981E-11,-0.146507430631343));
#54996=DIRECTION('',(0.764072860870889,-3.07809495139578E-8,-0.645129958442928));
#54997=DIRECTION('center_axis',(0.0394351206968075,0.793626260381199,-0.607126206063436));
#54998=DIRECTION('ref_axis',(1.38549959453206E-18,0.607598837093761,0.794244076567341));
#54999=DIRECTION('center_axis',(0.590699987184514,0.471546674567145,0.654765040945897));
#55000=DIRECTION('ref_axis',(-0.523586731929217,-0.393426487751019,0.755693411962536));
#55001=DIRECTION('center_axis',(-0.796652821640193,-0.601098528049027,-0.0634416373528684));
#55002=DIRECTION('ref_axis',(0.0810898755505838,-0.00227572017840687,-0.996704195426537));
#55003=DIRECTION('',(-0.595880397048102,5.19500677922242E-12,-0.803073192438769));
#55004=DIRECTION('center_axis',(0.,-1.,1.45983193964168E-32));
#55005=DIRECTION('ref_axis',(1.,0.,0.));
#55006=DIRECTION('center_axis',(0.796916587647907,0.601098527501541,0.0600375929488731));
#55007=DIRECTION('ref_axis',(0.0783695203868449,-0.00432806703985685,-0.996914984394374));
#55008=DIRECTION('center_axis',(0.796015997482586,-0.601098528209201,0.0709865560267364));
#55009=DIRECTION('ref_axis',(0.0863504162892312,-0.00330180114940477,-0.996259355647838));
#55010=DIRECTION('center_axis',(-0.795705465563001,0.601098527863717,-0.074386637733132));
#55011=DIRECTION('ref_axis',(0.0906057767860851,-0.00330187871639367,-0.995881363822987));
#55012=DIRECTION('center_axis',(0.811135913073174,0.584828375911389,-0.00585672705487716));
#55013=DIRECTION('ref_axis',(0.0166347872562848,-0.0330794214899682,-0.999314282759347));
#55014=DIRECTION('center_axis',(-0.999772620560389,-1.50627415268376E-7,
-0.0213238640445531));
#55015=DIRECTION('ref_axis',(-0.0213212417725825,-0.0156751609036356,0.99964978566492));
#55016=DIRECTION('',(0.99977160679441,3.88578058618689E-13,0.0213713417389563));
#55017=DIRECTION('center_axis',(0.810624895030398,0.584827952226214,0.029386150681072));
#55018=DIRECTION('ref_axis',(0.0526124214975072,-0.0227607295930021,-0.998355589102682));
#55019=DIRECTION('center_axis',(0.996456862410338,5.28963084084849E-10,
0.0841054181093271));
#55020=DIRECTION('ref_axis',(-0.0840950606332875,0.0156933905084143,0.996334149907266));
#55021=DIRECTION('',(-0.996456868253738,-2.24820162483037E-11,-0.0841053488783731));
#55022=DIRECTION('',(0.722057103468553,0.,-0.691833462135653));
#55023=DIRECTION('center_axis',(-0.798322321646307,-0.601098528011999,0.0369056958078118));
#55024=DIRECTION('ref_axis',(-0.0217365883386131,-0.0324816864609622,-0.99923593849103));
#55025=DIRECTION('',(-0.645129946172534,8.00811321699476E-12,-0.764072871231157));
#55026=DIRECTION('center_axis',(0.,-1.,1.45983193964168E-32));
#55027=DIRECTION('ref_axis',(1.,0.,0.));
#55028=DIRECTION('center_axis',(0.798157370548727,0.601098522271916,-0.0403159814622186));
#55029=DIRECTION('ref_axis',(-0.0244548005322686,-0.034538571078463,-0.99910412362215));
#55030=DIRECTION('center_axis',(0.796015995627959,-0.601098530265478,0.0709865594117118));
#55031=DIRECTION('ref_axis',(0.0636418316459174,-0.0335099662987225,-0.997410045780275));
#55032=DIRECTION('center_axis',(-0.795705464507517,0.601098524981808,-0.0743866723114541));
#55033=DIRECTION('ref_axis',(0.0679023398853725,-0.0335100626041385,-0.997129052802273));
#55034=DIRECTION('',(0.999140703555293,3.88578058618659E-13,-0.0414470083242979));
#55035=DIRECTION('center_axis',(0.807915936815926,0.584827952146018,-0.0724438087592005));
#55036=DIRECTION('ref_axis',(-0.051308426239449,-0.0526562728484819,-0.997293719185345));
#55037=DIRECTION('center_axis',(0.999771605233908,5.32086166830061E-10,
0.0213714147406051));
#55038=DIRECTION('ref_axis',(-0.0213687561129565,0.0157729998156971,0.99964723214692));
#55039=DIRECTION('',(-0.999771606794473,-1.76525460892867E-10,-0.0213713417360126));
#55040=DIRECTION('',(0.677191706197975,-1.43735365431834E-13,-0.735806627488959));
#55041=DIRECTION('',(-0.691833462110934,6.51326541667552E-11,-0.722057103492237));
#55042=DIRECTION('center_axis',(0.,-1.,1.45983193964168E-32));
#55043=DIRECTION('ref_axis',(1.,0.,0.));
#55044=DIRECTION('center_axis',(0.797459690717028,0.60109853555185,0.0523315606390982));
#55045=DIRECTION('ref_axis',(0.0267047523711035,0.0514849123724737,-0.998316663187987));
#55046=DIRECTION('center_axis',(-0.79038560520097,0.60109853544184,0.118199601440836));
#55047=DIRECTION('ref_axis',(-0.108516543809086,0.0525165101673011,-0.992706490297902));
#55048=DIRECTION('center_axis',(0.811041537039342,0.584827923043801,-0.0137085967602897));
#55049=DIRECTION('ref_axis',(-0.032724063722221,0.0219596690951161,-0.999223152547386));
#55050=DIRECTION('center_axis',(-0.994566168142843,-1.31729277523896E-8,
0.104106374375744));
#55051=DIRECTION('ref_axis',(0.104093479141674,-0.0157391391440287,0.994442973276591));
#55052=DIRECTION('',(0.994566648423253,0.,-0.104101785979579));
#55053=DIRECTION('center_axis',(0.810871077874088,0.584827952321184,0.0215490429283152));
#55054=DIRECTION('ref_axis',(0.00327726665943345,0.0322834330522339,-0.999473381073055));
#55055=DIRECTION('center_axis',(0.999140706846209,5.92341332246755E-10,
-0.0414469289918896));
#55056=DIRECTION('ref_axis',(0.0414418191872178,0.0157020800820226,0.999017527525695));
#55057=DIRECTION('',(-0.999140703555343,-1.16573417585624E-12,0.0414470083230859));
#55058=DIRECTION('',(0.629653742642216,0.,-0.776875900241892));
#55059=DIRECTION('center_axis',(-0.797928283125533,-0.601098528079163,0.0446207858447481));
#55060=DIRECTION('ref_axis',(-0.0732868695549994,0.0232723701520699,-0.997039332994608));
#55061=DIRECTION('',(-0.735806627488915,1.43735365432665E-13,-0.677191706198023));
#55062=DIRECTION('center_axis',(0.,-1.,1.45983193964168E-32));
#55063=DIRECTION('ref_axis',(1.,0.,0.));
#55064=DIRECTION('center_axis',(0.797730369155652,0.60109853137464,-0.0480293004949925));
#55065=DIRECTION('ref_axis',(-0.0760077075841752,0.0212180487987468,-0.996881448715429));
#55066=DIRECTION('center_axis',(0.789873413751279,-0.601098526075908,-0.121575294358155));
#55067=DIRECTION('ref_axis',(-0.135530058031665,0.0222452604497166,-0.990523473602447));
#55068=DIRECTION('center_axis',(-0.79038559828228,0.601098529468463,0.118199678082531));
#55069=DIRECTION('ref_axis',(-0.131297161989445,0.022245171162852,-0.991093440404815));
#55070=DIRECTION('center_axis',(0.80292790060668,0.584827953375448,-0.1152521209264));
#55071=DIRECTION('ref_axis',(-0.136477184437087,-0.0078464289019961,-0.990612139882008));
#55072=DIRECTION('center_axis',(-0.98606739651783,-1.97928475987955E-9,
0.166346293991028));
#55073=DIRECTION('ref_axis',(0.166325849227674,-0.0156778482801063,0.985946203883355));
#55074=DIRECTION('',(0.986067493104167,3.88578058618637E-13,-0.166345721445622));
#55075=DIRECTION('center_axis',(0.807177928571927,0.584827952254115,-0.0802499712684867));
#55076=DIRECTION('ref_axis',(-0.100698427309043,0.00246180457790776,-0.994913949171337));
#55077=DIRECTION('center_axis',(0.994566655474391,5.112341101984E-10,-0.104101718614458));
#55078=DIRECTION('ref_axis',(0.104088935582225,0.0156707406191776,0.994444529060222));
#55079=DIRECTION('',(-0.994566648423222,-6.41708908203981E-11,0.104101785979871));
#55080=DIRECTION('',(0.579630823425857,1.64268989064856E-13,-0.81487919873725));
#55081=DIRECTION('center_axis',(-0.786043913859459,-0.601098528073676,0.144275864343844));
#55082=DIRECTION('ref_axis',(-0.175405256149202,-0.00691952199720874,-0.984471998753932));
#55083=DIRECTION('',(-0.776875900234022,2.3593133554863E-11,-0.629653742651926));
#55084=DIRECTION('center_axis',(0.,-1.,1.45983193964168E-32));
#55085=DIRECTION('ref_axis',(1.,0.,0.));
#55086=DIRECTION('center_axis',(0.785420358955231,0.60109852656773,-0.147632723664982));
#55087=DIRECTION('ref_axis',(-0.178087573082603,-0.00897210222286303,-0.983973738315841));
#55088=DIRECTION('center_axis',(0.789873411738925,-0.601098528636561,-0.121575294771892));
#55089=DIRECTION('ref_axis',(-0.158025279743992,-0.00794569274266845,-0.987403097487886));
#55090=DIRECTION('center_axis',(-0.790385604202826,0.601098527305987,0.118199649489781));
#55091=DIRECTION('ref_axis',(-0.153805485205631,-0.00794579997179938,-0.988069196455121));
#55092=DIRECTION('center_axis',(0.782151614114705,0.584827952228535,-0.214977019306578));
#55093=DIRECTION('ref_axis',(-0.252337589513471,-0.0181546317291736,-0.967468940207028));
#55094=DIRECTION('center_axis',(-0.973676763012146,-5.60776949172076E-10,
0.227933238405875));
#55095=DIRECTION('ref_axis',(0.22790521834897,-0.0156795066172466,0.973557067932614));
#55096=DIRECTION('',(0.973676780617487,2.06171160587071E-7,-0.227933163199926));
#55097=DIRECTION('center_axis',(0.790753837977295,0.584827782536514,-0.180789470096029));
#55098=DIRECTION('ref_axis',(-0.20352523833637,-0.0273551074234324,-0.978687475886953));
#55099=DIRECTION('center_axis',(0.986067510177297,6.90490385794096E-10,
-0.166345620239144));
#55100=DIRECTION('ref_axis',(0.166325111618119,0.0157023279257334,0.985945938752695));
#55101=DIRECTION('',(0.986067493175933,-1.2926740480983E-5,-0.166345720517936));
#55102=DIRECTION('',(0.527320332408238,-7.62629077548565E-8,-0.849666562263609));
#55103=DIRECTION('center_axis',(-0.973676779746441,-4.80402468853765E-10,
0.227933166920922));
#55104=DIRECTION('ref_axis',(0.175936197693315,-0.635772805081887,0.751557978242216));
#55105=DIRECTION('',(0.814879198736464,0.,0.579630823426963));
#55106=DIRECTION('center_axis',(0.878946778346926,0.398564391591961,-0.261914082455468));
#55107=DIRECTION('ref_axis',(-0.412981067411442,0.910739610404481,-3.93877995988757E-17));
#55108=DIRECTION('center_axis',(-0.955400912706611,5.74456610291878E-5,
0.295311856686064));
#55109=DIRECTION('ref_axis',(0.295311817849053,-0.000362660813026997,0.955400857606807));
#55110=DIRECTION('',(0.957443671436224,5.94973684118189E-5,-0.288620187247509));
#55111=DIRECTION('center_axis',(0.789268291915765,0.590180063811103,-0.169537770589014));
#55112=DIRECTION('ref_axis',(0.533587214447737,-0.795821262434452,-0.286274698209849));
#55113=DIRECTION('center_axis',(0.117681057716851,0.550037558044731,-0.82680702306816));
#55114=DIRECTION('ref_axis',(1.5271491548741E-16,0.83259233830046,0.553886268292843));
#55115=DIRECTION('center_axis',(0.774347646173993,-0.477126090177126,0.415615708241503));
#55116=DIRECTION('ref_axis',(0.51669272472535,0.0976322306155627,-0.850586019025074));
#55117=DIRECTION('center_axis',(0.756336006288325,0.584827951389734,0.293141796516828));
#55118=DIRECTION('ref_axis',(0.343345849085406,0.0265489690012112,-0.938833734034304));
#55119=DIRECTION('center_axis',(-0.9630471056442,7.61707667613043E-12,-0.269333013777237));
#55120=DIRECTION('ref_axis',(-0.269299615467692,-0.0157477670567472,0.962927684170353));
#55121=DIRECTION('center_axis',(0.947192633567712,-0.000115441243345257,
0.320665092562912));
#55122=DIRECTION('ref_axis',(0.00787578078550292,-0.999689899016347,-0.023623672062273));
#55123=DIRECTION('',(-0.944235193661842,-6.06570349238513E-10,-0.329271770807008));
#55124=DIRECTION('center_axis',(-0.755847216535123,-0.601098528159584,-0.259567996294784));
#55125=DIRECTION('ref_axis',(0.304733770807828,0.027922010452604,-0.952028198249152));
#55126=DIRECTION('',(-0.434844806368847,2.24350371841866E-10,-0.900505410519026));
#55127=DIRECTION('center_axis',(0.,-1.,1.45983193964168E-32));
#55128=DIRECTION('ref_axis',(1.,0.,0.));
#55129=DIRECTION('center_axis',(0.756949243714246,0.601098531914126,0.256336492468616));
#55130=DIRECTION('ref_axis',(0.302155678236854,0.0258667653067949,-0.952907580283518));
#55131=DIRECTION('center_axis',(0.780842206360819,-0.601098525344159,0.170194041008038));
#55132=DIRECTION('ref_axis',(0.232606147173315,0.0268944354086559,-0.972199089508541));
#55133=DIRECTION('center_axis',(-0.780107969953459,0.601098529720276,-0.173528420678617));
#55134=DIRECTION('ref_axis',(0.236757408448613,0.026894339668752,-0.971196490952515));
#55135=DIRECTION('center_axis',(0.787112483925137,0.58482795222257,0.196036231213407));
#55136=DIRECTION('ref_axis',(0.243954870283373,-0.00326197144530851,-0.969781099427759));
#55137=DIRECTION('center_axis',(-0.978058329448275,-6.23278424207892E-10,
-0.208331236728554));
#55138=DIRECTION('ref_axis',(-0.208305614215986,-0.0156832196301943,0.977938038787802));
#55139=DIRECTION('',(0.978058312613238,8.3214430343242E-8,0.208331315764432));
#55140=DIRECTION('center_axis',(0.777850283241406,0.584827969931775,0.230054737935873));
#55141=DIRECTION('ref_axis',(0.278731662545331,0.00704480133959886,-0.960343184007051));
#55142=DIRECTION('center_axis',(0.963047084611284,6.17958183329108E-10,
0.269333088984082));
#55143=DIRECTION('ref_axis',(-0.2693000132912,0.015671528055328,0.96292881670961));
#55144=DIRECTION('',(-0.963047106749995,-1.40443212613654E-11,-0.269333009823273));
#55145=DIRECTION('',(0.838904141906417,-3.07810727157134E-8,-0.544279193697736));
#55146=DIRECTION('center_axis',(0.115217253574516,0.793626260383203,-0.597396303394086));
#55147=DIRECTION('ref_axis',(2.53029610822811E-17,0.601401446656677,0.79894699446162));
#55148=DIRECTION('center_axis',(0.503978321585131,0.471546674548375,0.723636362474001));
#55149=DIRECTION('ref_axis',(0.614178693886623,0.39341725961525,-0.684110657578544));
#55150=DIRECTION('center_axis',(-0.782419630395453,-0.601098528053825,-0.162788456419267));
#55151=DIRECTION('ref_axis',(0.205370618307549,-0.002275719460754,-0.978681628639728));
#55152=DIRECTION('',(-0.4905299421393,5.05127141378903E-12,-0.871424337429714));
#55153=DIRECTION('center_axis',(0.,-1.,1.45983193964168E-32));
#55154=DIRECTION('ref_axis',(1.,0.,0.));
#55155=DIRECTION('center_axis',(0.783107955385302,0.601098527525842,0.159444317611245));
#55156=DIRECTION('ref_axis',(0.202698136851968,-0.00432806322786716,-0.979231705565867));
#55157=DIRECTION('center_axis',(0.780842198431431,-0.601098528204078,0.17019406728691));
#55158=DIRECTION('ref_axis',(0.210533925993421,-0.00330180270151346,-0.977580975727698));
#55159=DIRECTION('center_axis',(-0.780107972007283,0.60109852785516,-0.173528417906242));
#55160=DIRECTION('ref_axis',(0.214708356390796,-0.00330187999745221,-0.976672626464183));
#55161=DIRECTION('center_axis',(0.805474420452859,0.584828255987408,0.0958481559283075));
#55162=DIRECTION('ref_axis',(0.141747987856584,-0.0330815410796403,-0.98934984690877));
#55163=DIRECTION('center_axis',(-0.989214558882193,-1.08087088037379E-7,
-0.146473739951897));
#55164=DIRECTION('ref_axis',(-0.146455742083979,-0.0156751635316721,0.989093021337673));
#55165=DIRECTION('',(0.989209569691817,3.88578058618681E-13,0.146507430631113));
#55166=DIRECTION('center_axis',(0.800549814323794,0.58482795222629,0.130752671410353));
#55167=DIRECTION('ref_axis',(0.177324691070629,-0.0227607295910026,-0.983889172176008));
#55168=DIRECTION('center_axis',(0.978058296034405,6.18594720556444E-10,
0.208331393597502));
#55169=DIRECTION('ref_axis',(-0.208305737838454,0.015693390506422,0.977937849292065));
#55170=DIRECTION('',(-0.978058312885219,-2.24265050970653E-11,-0.208331314487569));
#55171=DIRECTION('',(0.803073192437117,-1.43735365431889E-13,-0.595880397050329));
#55172=DIRECTION('center_axis',(-0.796652821848156,-0.601098528024524,-0.0634416349735795));
#55173=DIRECTION('ref_axis',(0.103672282694559,-0.0324816862473311,-0.99408098153995));
#55174=DIRECTION('',(-0.544279180225778,8.17238220606129E-12,-0.838904150646995));
#55175=DIRECTION('center_axis',(0.,-1.,1.45983193964168E-32));
#55176=DIRECTION('ref_axis',(1.,0.,0.));
#55177=DIRECTION('center_axis',(0.796916592183571,0.601098522752696,0.0600375802897754));
#55178=DIRECTION('ref_axis',(0.100958994621709,-0.0345385625894204,-0.99429088756723));
#55179=DIRECTION('center_axis',(0.780842196599987,-0.601098530248933,0.17019406846738));
#55180=DIRECTION('ref_axis',(0.188148623470608,-0.0335099666683606,-0.981568733008545));
#55181=DIRECTION('center_axis',(-0.780107967744112,0.601098525096341,-0.173528446628081));
#55182=DIRECTION('ref_axis',(0.192340315430215,-0.0335100605282662,-0.980755973167432));
#55183=DIRECTION('',(0.996456868253704,3.88578058618601E-13,0.0841053488787717));
#55184=DIRECTION('center_axis',(0.810624895144929,0.584827952145969,0.0293861491186781));
#55185=DIRECTION('ref_axis',(0.0740902026644828,-0.0526562728495679,-0.99586041130207));
#55186=DIRECTION('center_axis',(0.989209556839538,6.48209010908156E-10,
0.146507517408919));
#55187=DIRECTION('ref_axis',(-0.146489291664188,0.0157729998144143,0.98908649768591));
#55188=DIRECTION('',(-0.989209569692122,-1.76969550102591E-10,-0.146507430629054));
#55189=DIRECTION('',(0.764072871228435,0.,-0.645129946175758));
#55190=DIRECTION('',(-0.595880397021771,6.72270837774884E-11,-0.803073192458307));
#55191=DIRECTION('center_axis',(0.,-1.,1.45983193964168E-32));
#55192=DIRECTION('ref_axis',(1.,0.,0.));
#55193=DIRECTION('center_axis',(0.784612598448139,0.601098535311237,0.151867116925111));
#55194=DIRECTION('ref_axis',(0.151616436599874,0.0514849151660113,-0.987097644442081));
#55195=DIRECTION('center_axis',(-0.798967517010862,0.601098535033961,0.0182059864199733));
#55196=DIRECTION('ref_axis',(0.0167582497254366,0.0525165148770827,-0.998479432302591));
#55197=DIRECTION('center_axis',(0.806364404619297,0.58482793005053,0.0880496405204397));
#55198=DIRECTION('ref_axis',(0.0927695868605033,0.0219594825816756,-0.995445420341305));
#55199=DIRECTION('center_axis',(-0.999771680335281,-9.50272957164279E-9,
-0.0213679011502948));
#55200=DIRECTION('ref_axis',(-0.0213652542031799,-0.0157391393478712,0.999647840694623));
#55201=DIRECTION('',(0.999771606794418,3.88578058618524E-13,0.0213713417386143));
#55202=DIRECTION('center_axis',(0.801776305997875,0.584827952320729,0.123008216492823));
#55203=DIRECTION('ref_axis',(0.128518655152663,0.0322834330588407,-0.991181484506085));
#55204=DIRECTION('center_axis',(0.996456862274223,5.27118926555364E-10,
0.084105419721982));
#55205=DIRECTION('ref_axis',(-0.0840950507717687,0.0157020800823933,0.996334013831095));
#55206=DIRECTION('',(-0.996456868253673,-4.44089209850033E-13,-0.0841053488791432));
#55207=DIRECTION('',(0.722057103468734,-1.64268989064969E-13,-0.691833462135463));
#55208=DIRECTION('center_axis',(-0.797228847712849,-0.601098528101694,-0.0557379932220375));
#55209=DIRECTION('ref_axis',(0.0522531820751103,0.0232723695238065,-0.998362660449484));
#55210=DIRECTION('',(-0.645129946175722,1.43735365432679E-13,-0.764072871228465));
#55211=DIRECTION('center_axis',(0.,-1.,1.45983193964168E-32));
#55212=DIRECTION('ref_axis',(1.,0.,0.));
#55213=DIRECTION('center_axis',(0.79745969424158,0.601098531278079,0.0523315560198833));
#55214=DIRECTION('ref_axis',(0.0495340149003826,0.0212180514793412,-0.998547032272025));
#55215=DIRECTION('center_axis',(0.798882450803113,-0.601098526263612,-0.0216192396380311));
#55216=DIRECTION('ref_axis',(-0.0103158466528301,0.0222452555462506,-0.999699320752754));
#55217=DIRECTION('center_axis',(-0.798967519598811,0.60109852937561,0.0182060596671171));
#55218=DIRECTION('ref_axis',(-0.00604490231352095,0.0222451736562014,-0.999734270396402));
#55219=DIRECTION('center_axis',(0.811041496720708,0.584827954381744,-0.0137096451704552));
#55220=DIRECTION('ref_axis',(-0.0112442943397282,-0.00784635389251968,-0.999905995869309));
#55221=DIRECTION('center_axis',(-0.999140665572378,-2.39543322650626E-9,
0.0414479239478296));
#55222=DIRECTION('ref_axis',(0.0414428298276432,-0.0156778481977069,0.999017866172456));
#55223=DIRECTION('',(0.999140703555307,0.,-0.0414470083239631));
#55224=DIRECTION('center_axis',(0.810871077905441,0.584827952254198,0.0215490435664711));
#55225=DIRECTION('ref_axis',(0.0247913922286098,0.00246180457413497,-0.999689615025387));
#55226=DIRECTION('center_axis',(0.999771605140397,5.87028746314927E-10,
0.021371419115121));
#55227=DIRECTION('ref_axis',(-0.0213687948509366,0.0156707406192051,0.999648839590716));
#55228=DIRECTION('',(-0.999771606794419,-6.41708908203814E-11,-0.0213713417385345));
#55229=DIRECTION('',(0.677191706198009,1.64268989064928E-13,-0.735806627488928));
#55230=DIRECTION('center_axis',(-0.797928283093221,-0.601098528023317,0.0446207871748926));
#55231=DIRECTION('ref_axis',(-0.0506350795953401,-0.00691952595144905,-0.998693250640546));
#55232=DIRECTION('',(-0.691833462126744,2.36136671785025E-11,-0.722057103477089));
#55233=DIRECTION('center_axis',(0.,-1.,1.45983193964168E-32));
#55234=DIRECTION('ref_axis',(1.,0.,0.));
#55235=DIRECTION('center_axis',(0.797730371835312,0.601098526624151,-0.0480293154414078));
#55236=DIRECTION('ref_axis',(-0.0533586835760229,-0.00897209812163425,-0.998535103209862));
#55237=DIRECTION('center_axis',(0.798882448921765,-0.601098528604706,-0.0216192440668271));
#55238=DIRECTION('ref_axis',(-0.0330247766656794,-0.00794569538969458,-0.999422948531279));
#55239=DIRECTION('center_axis',(-0.798967521824576,0.601098527331365,0.0182060294836761));
#55240=DIRECTION('ref_axis',(-0.0287547780917037,-0.00794579812142253,-0.999554914463988));
#55241=DIRECTION('center_axis',(0.802927879994109,0.58482795222914,-0.115252270344828));
#55242=DIRECTION('ref_axis',(-0.129091821551966,-0.0181546317646192,-0.991466444693862));
#55243=DIRECTION('center_axis',(-0.994566499546172,-4.82169677984236E-9,
0.104103208310188));
#55244=DIRECTION('ref_axis',(0.104090410872243,-0.0156795063499374,0.994444236468325));
#55245=DIRECTION('',(0.994566648759578,2.06171493653893E-7,-0.104101782766194));
#55246=DIRECTION('center_axis',(0.80717743665864,0.584827782536333,-0.0802561556693508));
#55247=DIRECTION('ref_axis',(-0.0792583150492463,-0.0273551074302921,-0.996478709051544));
#55248=DIRECTION('center_axis',(0.999140707823812,6.92958397042268E-10,
-0.041446905425273));
#55249=DIRECTION('ref_axis',(0.0414417954606099,0.0157023279249861,0.999017524614427));
#55250=DIRECTION('',(0.999140703510251,-1.29267396282542E-5,-0.0414470073942771));
#55251=DIRECTION('',(0.629653711784213,-7.62630514902441E-8,-0.776875925252133));
#55252=DIRECTION('center_axis',(-0.994566627728716,-1.61528326269501E-7,
0.104101983690535));
#55253=DIRECTION('ref_axis',(0.0803539506805691,-0.635772804014687,0.767682345951323));
#55254=DIRECTION('',(0.735806627488049,0.,0.677191706198964));
#55255=DIRECTION('center_axis',(0.904842559340681,0.39856439159295,-0.149687569824443));
#55256=DIRECTION('ref_axis',(-0.403106047559068,0.915153273731404,-2.21620707676059E-17));
#55257=DIRECTION('center_axis',(-0.984879681052153,5.74456494182127E-5,
0.173239748760516));
#55258=DIRECTION('ref_axis',(0.173239717104257,-0.000362923152739352,0.984879621428133));
#55259=DIRECTION('',(0.986067643452047,5.94973683762695E-5,-0.166344819567638));
#55260=DIRECTION('center_axis',(0.80429339270289,0.590180063807686,-0.0692793673356712));
#55261=DIRECTION('ref_axis',(0.565257933865613,-0.795820139095679,-0.217149198505803));
#55262=DIRECTION('center_axis',(0.220379505161487,0.550037558045268,-0.805538055242815));
#55263=DIRECTION('ref_axis',(-1.78365250524718E-16,0.82584203726199,0.56390152463969));
#55264=DIRECTION('center_axis',(0.716151222799951,-0.477126090775243,0.509389948451743));
#55265=DIRECTION('ref_axis',(0.619221586313834,0.0976225795884288,-0.779124161477155));
#55266=DIRECTION('center_axis',(0.713631661727888,0.584827951390377,0.385624323211112));
#55267=DIRECTION('ref_axis',(0.458305532169128,0.0265489689930021,-0.888398104133829));
#55268=DIRECTION('center_axis',(-0.921696814299896,-7.64602880816405E-12,
-0.387911049738756));
#55269=DIRECTION('ref_axis',(-0.387862947305241,-0.0157477670559312,0.921582520418244));
#55270=DIRECTION('center_axis',(0.899533739617671,-0.000115441140596853,
0.43685127670958));
#55271=DIRECTION('ref_axis',(0.0107128862560727,-0.99969340280687,-0.0223234059338097));
#55272=DIRECTION('',(-0.895520921373816,-6.06903416145823E-10,-0.445019414612207));
#55273=DIRECTION('center_axis',(-0.717354638076182,-0.601098528089715,-0.352254003183738));
#55274=DIRECTION('ref_axis',(0.421651628388622,0.0279220120055917,-0.906327901767778));
#55275=DIRECTION('',(-0.318552670246172,2.24206636476366E-10,-0.947905162070043));
#55276=DIRECTION('center_axis',(0.,-1.,1.45983193964168E-32));
#55277=DIRECTION('ref_axis',(1.,0.,0.));
#55278=DIRECTION('center_axis',(0.718852989379429,0.601098531789471,0.349186103304242));
#55279=DIRECTION('ref_axis',(0.419204082182475,0.0258667681431969,-0.907523469551821));
#55280=DIRECTION('center_axis',(0.753354059151887,-0.601098525631524,0.26671749856915));
#55281=DIRECTION('ref_axis',(0.352620841655527,0.0268944291101661,-0.935379725947161));
#55282=DIRECTION('center_axis',(-0.752207708651457,0.601098529635836,-0.269933548702196));
#55283=DIRECTION('ref_axis',(0.356613699824013,0.0268943415657175,-0.933864745822207));
#55284=DIRECTION('center_axis',(0.756336012141187,0.58482795222267,0.293141779754106));
#55285=DIRECTION('ref_axis',(0.363577014296436,-0.00326197145300851,-0.931558433066616));
#55286=DIRECTION('center_axis',(-0.94423522144996,-6.61920013744243E-10,
-0.329271691120486));
#55287=DIRECTION('ref_axis',(-0.32923119423163,-0.0156832196310547,0.944119090669614));
#55288=DIRECTION('',(0.94423519322909,8.32144303432419E-8,0.329271772047978));
#55289=DIRECTION('center_axis',(0.742883197217908,0.584827969931451,0.325731178853293));
#55290=DIRECTION('ref_axis',(0.396896696726391,0.00704480134718826,-0.917836250592478));
#55291=DIRECTION('center_axis',(0.921696784377478,6.05482782476995E-10,
0.387911120835967));
#55292=DIRECTION('ref_axis',(-0.387863483056267,0.0156715280544747,0.921583594537087));
#55293=DIRECTION('',(-0.921696815638182,-1.44328993199795E-11,-0.387911046558918));
#55294=DIRECTION('',(0.900505403486833,-3.07809289803555E-8,-0.434844820931577));
#55295=DIRECTION('center_axis',(0.189182341537265,0.793626260384412,-0.578245104154571));
#55296=DIRECTION('ref_axis',(7.61514585110326E-17,0.588879097809632,0.808221138156454));
#55297=DIRECTION('center_axis',(0.409308616765261,0.471546674544237,0.781095506303794));
#55298=DIRECTION('ref_axis',(0.695084368764266,0.393408104074107,-0.601737304767121));
#55299=DIRECTION('center_axis',(-0.75584721418306,-0.601098528053673,-0.259568003389123));
#55300=DIRECTION('ref_axis',(0.326412543019652,-0.00227571927650737,-0.945224667928857));
#55301=DIRECTION('',(-0.377443537014696,5.05127141378908E-12,-0.926032600055655));
#55302=DIRECTION('center_axis',(0.,-1.,1.45983193964168E-32));
#55303=DIRECTION('ref_axis',(1.,0.,0.));
#55304=DIRECTION('center_axis',(0.756949242071626,0.60109852753972,0.256336507576995));
#55305=DIRECTION('ref_axis',(0.323830080576638,-0.00432806085017039,-0.946105357136828));
#55306=DIRECTION('center_axis',(0.753354050301488,-0.601098528194456,0.266717517791394));
#55307=DIRECTION('ref_axis',(0.331397190998648,-0.00330180520380201,-0.94348555891471));
#55308=DIRECTION('center_axis',(-0.752207710703613,0.601098527861535,-0.269933546934659));
#55309=DIRECTION('ref_axis',(0.335424853501877,-0.0033018785742854,-0.9420611791445));
#55310=DIRECTION('center_axis',(0.787110054748738,0.584828255987617,0.196045078264979));
#55311=DIRECTION('ref_axis',(0.264628678078428,-0.0330815410758865,-0.963782794190946));
#55312=DIRECTION('center_axis',(-0.963056284291006,-1.0823643437071E-7,
-0.269300191770429));
#55313=DIRECTION('ref_axis',(-0.269267103127621,-0.0156751635316013,0.96293796083731));
#55314=DIRECTION('',(0.963047106749919,3.88578058618612E-13,0.269333009823547));
#55315=DIRECTION('center_axis',(0.77784958482566,0.584827952226003,0.230057144383061));
#55316=DIRECTION('ref_axis',(0.29924044432063,-0.0227607296021428,-0.953906235261501));
#55317=DIRECTION('center_axis',(0.944235165175771,6.62804140859967E-10,
0.329271852494993));
#55318=DIRECTION('ref_axis',(-0.329231303059565,0.0156933905093517,0.944118883711168));
#55319=DIRECTION('',(-0.944235193658685,-2.28705943069057E-11,-0.329271770816064));
#55320=DIRECTION('',(0.87142433742843,0.,-0.49052994214158));
#55321=DIRECTION('center_axis',(-0.782419630834816,-0.601098528069948,-0.162788454247995));
#55322=DIRECTION('ref_axis',(0.227446180684351,-0.0324816854257597,-0.973248773440791));
#55323=DIRECTION('',(-0.43484480647018,8.1518485824254E-12,-0.900505410470094));
#55324=DIRECTION('center_axis',(0.,-1.,1.45983193964168E-32));
#55325=DIRECTION('ref_axis',(1.,0.,0.));
#55326=DIRECTION('center_axis',(0.78310796246243,0.601098522796805,0.159444300680334));
#55327=DIRECTION('ref_axis',(0.224780595854182,-0.0345385618110103,-0.973797089477816));
#55328=DIRECTION('center_axis',(0.7533540488904,-0.601098530160528,0.266717517346152));
#55329=DIRECTION('ref_axis',(0.309688200669007,-0.0335099682690439,-0.950247494283989));
#55330=DIRECTION('center_axis',(-0.752207704481693,0.601098525353629,-0.269933569857612));
#55331=DIRECTION('ref_axis',(0.31374496629142,-0.033510055923605,-0.948915787769806));
#55332=DIRECTION('',(0.978058312885182,0.,0.208331314487746));
#55333=DIRECTION('center_axis',(0.800549814629832,0.584827952146791,0.130752669892176));
#55334=DIRECTION('ref_axis',(0.198320384830501,-0.0526562728374665,-0.978721789831793));
#55335=DIRECTION('center_axis',(0.963047084639028,6.04071551872731E-10,
0.269333088884878));
#55336=DIRECTION('ref_axis',(-0.269299583453945,0.0157729998151177,0.962927280135091));
#55337=DIRECTION('',(-0.963047106750702,-1.7691403895138E-10,-0.269333009820746));
#55338=DIRECTION('',(0.838904150644647,0.,-0.544279180229396));
#55339=DIRECTION('',(-0.490529942111875,6.5132654166756E-11,-0.871424337445151));
#55340=DIRECTION('center_axis',(0.,-1.,1.45983193964168E-32));
#55341=DIRECTION('ref_axis',(1.,0.,0.));
#55342=DIRECTION('center_axis',(0.759391695701333,0.601098535079257,0.249007637684921));
#55343=DIRECTION('ref_axis',(0.274137038722192,0.0514849178358315,-0.960311505312763));
#55344=DIRECTION('center_axis',(-0.794949234662874,0.601098535026273,-0.0820747555474917));
#55345=DIRECTION('ref_axis',(0.141768761737848,0.0525165149262143,-0.988505758129573));
#55346=DIRECTION('center_axis',(0.788970434278718,0.584827930050502,0.188419601068719));
#55347=DIRECTION('ref_axis',(0.216800464328143,0.0219594825819946,-0.975968923578939));
#55348=DIRECTION('center_axis',(-0.989210085707457,-1.01383751197917E-8,
-0.146503946481472));
#55349=DIRECTION('ref_axis',(-0.146485799183718,-0.0157391393489173,0.989087554329779));
#55350=DIRECTION('',(0.989209569691852,0.,0.146507430630876));
#55351=DIRECTION('center_axis',(0.780037042821315,0.584827952321357,0.222527476977982));
#55352=DIRECTION('ref_axis',(0.251733227661971,0.0322834330509041,-0.967258063828539));
#55353=DIRECTION('center_axis',(0.978058297637846,5.43689378628934E-10,
0.208331386069788));
#55354=DIRECTION('ref_axis',(-0.20830570188923,0.0157020800826578,0.977937717465439));
#55355=DIRECTION('',(-0.978058312885196,-7.77156117237457E-13,-0.208331314487679));
#55356=DIRECTION('',(0.803073192437116,0.,-0.59588039705033));
#55357=DIRECTION('center_axis',(-0.783956636806604,-0.601098528048292,-0.155217754091001));
#55358=DIRECTION('ref_axis',(0.176969172392052,0.0232723708888864,-0.983941212052876));
#55359=DIRECTION('',(-0.54427918022921,0.,-0.838904150644768));
#55360=DIRECTION('center_axis',(0.,-1.,1.45983193964168E-32));
#55361=DIRECTION('ref_axis',(1.,0.,0.));
#55362=DIRECTION('center_axis',(0.784612601745812,0.601098531093903,0.151867116580321));
#55363=DIRECTION('ref_axis',(0.174294559514057,0.0212180565961819,-0.984464931116432));
#55364=DIRECTION('center_axis',(0.795292633422098,-0.601098526236438,0.0786777540409415));
#55365=DIRECTION('ref_axis',(0.115061044311964,0.0222452563148451,-0.993109311532888));
#55366=DIRECTION('center_axis',(-0.794949246499047,0.601098529356507,-0.0820746824303406));
#55367=DIRECTION('ref_axis',(0.119302691667852,0.0222451741801302,-0.992608694293225));
#55368=DIRECTION('center_axis',(0.806364486303306,0.584827953016348,0.0880487399087191));
#55369=DIRECTION('ref_axis',(0.114165681649204,-0.00784645567446514,-0.993430737528753));
#55370=DIRECTION('center_axis',(-0.996456903954996,-1.54610479594417E-9,
-0.0841049258986923));
#55371=DIRECTION('ref_axis',(-0.0840945889572224,-0.0156778483095254,0.996334434404683));
#55372=DIRECTION('',(0.996456868253732,3.88578058618602E-13,0.0841053488784387));
#55373=DIRECTION('center_axis',(0.801776305949548,0.584827952254047,0.123008217124855));
#55374=DIRECTION('ref_axis',(0.149890236712957,0.00246180457667358,-0.988699578464743));
#55375=DIRECTION('center_axis',(0.98920956001149,4.98288762736695E-10,0.146507495992097));
#55376=DIRECTION('ref_axis',(-0.146489505817707,0.0156707406191989,0.989088091412352));
#55377=DIRECTION('',(-0.989209569691896,-6.37823127618053E-11,-0.146507430630582));
#55378=DIRECTION('',(0.76407287122843,1.64268989064961E-13,-0.645129946175764));
#55379=DIRECTION('center_axis',(-0.797228847335996,-0.601098528067765,-0.0557379989781326));
#55380=DIRECTION('ref_axis',(0.0749336524077195,-0.00691952230795232,-0.99716451398346));
#55381=DIRECTION('',(-0.595880397040262,2.34493981894256E-11,-0.803073192444586));
#55382=DIRECTION('center_axis',(0.,-1.,1.45983193964168E-32));
#55383=DIRECTION('ref_axis',(1.,0.,0.));
#55384=DIRECTION('center_axis',(0.797459698279166,0.60109852670928,0.0523315469715389));
#55385=DIRECTION('ref_axis',(0.0722117068174117,-0.00897209216443674,-0.997348971504312));
#55386=DIRECTION('center_axis',(0.795292631668755,-0.601098528582469,0.0786777538404375));
#55387=DIRECTION('ref_axis',(0.0924965459119079,-0.00794569729621685,-0.995681301867642));
#55388=DIRECTION('center_axis',(-0.794949245543195,0.601098527392003,-0.0820747060760524));
#55389=DIRECTION('ref_axis',(0.0967494055274045,-0.00794579363142727,-0.995277055343717));
#55390=DIRECTION('center_axis',(0.811041493555078,0.584827952230365,-0.0137099242151991));
#55391=DIRECTION('ref_axis',(-0.00381019848136195,-0.018154631726411,-0.999827931063346));
#55392=DIRECTION('center_axis',(-0.999771634704107,-3.84875494615878E-9,
-0.0213700360570086));
#55393=DIRECTION('ref_axis',(-0.0213674089564386,-0.0156795063471331,0.999648731762912));
#55394=DIRECTION('',(0.999771606725356,2.06171160587047E-7,0.0213713449683962));
#55395=DIRECTION('center_axis',(0.810871364980605,0.584827782536739,0.0215428463219416));
#55396=DIRECTION('ref_axis',(0.0462585592507087,-0.0273551074091835,-0.998554877708121));
#55397=DIRECTION('center_axis',(0.996456858641484,7.82376094411192E-10,
0.0841054627616138));
#55398=DIRECTION('ref_axis',(-0.0840950934827374,0.015702327924652,0.996334006320108));
#55399=DIRECTION('',(0.996456868092494,-1.29267395926603E-5,0.0841053497953458));
#55400=DIRECTION('',(0.722057075988427,-7.62630514902547E-8,-0.691833490816278));
#55401=DIRECTION('center_axis',(-0.999771611042796,-1.61527610287435E-7,
-0.0213711429938946));
#55402=DIRECTION('ref_axis',(-0.016495774990561,-0.635772804014641,0.771699961826371));
#55403=DIRECTION('',(0.645129946174821,0.,0.764072871229226));
#55404=DIRECTION('center_axis',(0.916468432647469,0.398564391592776,-0.0351003947979456));
#55405=DIRECTION('ref_axis',(-0.398810141877463,0.917033516691554,5.53686176681803E-17));
#55406=DIRECTION('center_axis',(-0.998826308491894,5.74456525261277E-5,
0.048435546496896));
#55407=DIRECTION('ref_axis',(0.0484355225642264,-0.000362908471667172,0.998826245375727));
#55408=DIRECTION('',(0.999140739682401,5.94973683407417E-5,-0.0414460947131014));
#55409=DIRECTION('center_axis',(0.806634306200451,0.590180063810972,0.0320716126908823));
#55410=DIRECTION('ref_axis',(0.588016972727278,-0.795820717445797,-0.144587086106277));
#55411=DIRECTION('center_axis',(0.31960243616028,0.550037558046786,-0.77156527108103));
#55412=DIRECTION('ref_axis',(-1.40687696057311E-16,0.814272451719983,0.580482880341814));
#55413=DIRECTION('center_axis',(0.64666066718635,-0.477126090607359,0.595130805097369));
#55414=DIRECTION('ref_axis',(0.711989593230198,0.0976245058129954,-0.695370602626158));
#55415=DIRECTION('center_axis',(0.659672919556294,0.584827951390327,0.472025323978142));
#55416=DIRECTION('ref_axis',(0.566037463240398,0.0265489689913246,-0.823951905425234));
#55417=DIRECTION('center_axis',(-0.865810814540078,-2.02897135812954E-11,
-0.500371495416602));
#55418=DIRECTION('ref_axis',(-0.500309447463457,-0.0157477670546732,0.865703450733334));
#55419=DIRECTION('center_axis',(0.837688665200949,-0.000115441160790834,
0.546148044825934));
#55420=DIRECTION('ref_axis',(0.0127915959477522,-0.999721510045263,-0.0198312235106537));
#55421=DIRECTION('',(-0.832683749197209,-6.07014438448021E-10,-0.553748836407698));
#55422=DIRECTION('center_axis',(-0.667548946793382,-0.601098527962809,-0.439384755443325));
#55423=DIRECTION('ref_axis',(0.531919789020974,0.0279220147650522,-0.846334271514124));
#55424=DIRECTION('',(-0.197236768219774,2.24206636476456E-10,-0.980355882964049));
#55425=DIRECTION('center_axis',(0.,-1.,1.45983193964168E-32));
#55426=DIRECTION('ref_axis',(1.,0.,0.));
#55427=DIRECTION('center_axis',(0.669419990798359,0.601098531560112,0.436528843578293));
#55428=DIRECTION('ref_axis',(0.529641389590394,0.0258667733636549,-0.84782716898464));
#55429=DIRECTION('center_axis',(0.713985067372484,-0.601098525837634,0.359034658222479));
#55430=DIRECTION('ref_axis',(0.467074491946653,0.0268944246589108,-0.883808864458284));
#55431=DIRECTION('center_axis',(-0.712444686287866,0.601098529375266,-0.362081657866117));
#55432=DIRECTION('ref_axis',(0.470845975634754,0.0268943474458885,-0.881805398772324));
#55433=DIRECTION('center_axis',(0.713631669624092,0.584827952222598,0.385624307336369));
#55434=DIRECTION('ref_axis',(0.477465331622029,-0.00326197144642527,-0.878644533723023));
#55435=DIRECTION('center_axis',(-0.895520966472167,-7.947455469195E-10,
-0.445019323859937));
#55436=DIRECTION('ref_axis',(-0.444964591254928,-0.0156832196312974,0.895410827023736));
#55437=DIRECTION('',(0.895520920788632,8.32139862540598E-8,0.445019415789777));
#55438=DIRECTION('center_axis',(0.69620039940266,0.58482796993151,0.416270644481887));
#55439=DIRECTION('ref_axis',(0.50880243289223,0.00704480134550057,-0.86085449122192));
#55440=DIRECTION('center_axis',(0.865810765649482,7.49484263326867E-10,
0.500371580013751));
#55441=DIRECTION('ref_axis',(-0.50031013142348,0.0156715280536838,0.865704438941769));
#55442=DIRECTION('',(-0.865810815148925,-1.48214773785942E-11,-0.500371494363093));
#55443=DIRECTION('',(0.947905156918536,-3.07810316484846E-8,-0.318552685575313));
#55444=DIRECTION('center_axis',(0.260163910959887,0.793626260386302,-0.54997463419626));
#55445=DIRECTION('ref_axis',(-1.5872085081592E-17,0.569588725703824,0.82192985318158));
#55446=DIRECTION('center_axis',(0.308183870415267,0.471546674597968,0.826236307415417));
#55447=DIRECTION('ref_axis',(0.765014665445126,0.393417088882177,-0.509877981314505));
#55448=DIRECTION('center_axis',(-0.717354637119605,-0.6010985280463,-0.352254005205861));
#55449=DIRECTION('ref_axis',(0.442306744791282,-0.00227572086838956,-0.89686095054176));
#55450=DIRECTION('',(-0.258404621837415,5.05127141378918E-12,-0.966036775393702));
#55451=DIRECTION('center_axis',(0.,-1.,1.45983193964168E-32));
#55452=DIRECTION('ref_axis',(1.,0.,0.));
#55453=DIRECTION('center_axis',(0.71885298669406,0.601098527551182,0.349186116128391));
#55454=DIRECTION('ref_axis',(0.439855029239441,-0.0043280593061185,-0.898058361775789));
#55455=DIRECTION('center_axis',(0.713985057703359,-0.601098528184557,0.3590346735215));
#55456=DIRECTION('ref_axis',(0.447034124176754,-0.00330180781928047,-0.894510810379979));
#55457=DIRECTION('center_axis',(-0.712444684573304,0.601098527865069,-0.362081663746858));
#55458=DIRECTION('ref_axis',(0.450851501151844,-0.00330187774175132,-0.892592864363427));
#55459=DIRECTION('center_axis',(0.756332493291777,0.584828255987081,0.293150252584156));
#55460=DIRECTION('ref_axis',(0.383336015948029,-0.0330815410858942,-0.923016311078236));
#55461=DIRECTION('center_axis',(-0.921710034200493,-1.08240530837605E-7,
-0.387879637070721));
#55462=DIRECTION('ref_axis',(-0.387831979480682,-0.0156751635319584,0.921596790869164));
#55463=DIRECTION('',(0.921696815638239,0.,0.387911046558782));
#55464=DIRECTION('center_axis',(0.742882202703939,0.584827952226054,0.325733478784151));
#55465=DIRECTION('ref_axis',(0.416436997026077,-0.0227607295980158,-0.908879627176266));
#55466=DIRECTION('center_axis',(0.895520879251373,7.26913384781663E-10,
0.44501949937598));
#55467=DIRECTION('ref_axis',(-0.444964695753017,0.0156933905072713,0.895410596892739));
#55468=DIRECTION('',(-0.895520921369782,-2.24820162482919E-11,-0.445019414620325));
#55469=DIRECTION('',(0.926032600054683,-1.43735365431985E-13,-0.377443537017079));
#55470=DIRECTION('center_axis',(-0.755847215917792,-0.601098527981938,-0.259567998503803));
#55471=DIRECTION('ref_axis',(0.347633113441175,-0.0324816870314175,-0.937067851570413));
#55472=DIRECTION('',(-0.318552670353025,8.15184858242886E-12,-0.947905162034134));
#55473=DIRECTION('center_axis',(0.,-1.,1.45983193964168E-32));
#55474=DIRECTION('ref_axis',(1.,0.,0.));
#55475=DIRECTION('center_axis',(0.756949252602283,0.601098522786963,0.256336487625497));
#55476=DIRECTION('ref_axis',(0.345057271550156,-0.0345385619991088,-0.937945929723774));
#55477=DIRECTION('center_axis',(0.713985059025465,-0.601098530219434,0.359034667485523));
#55478=DIRECTION('ref_axis',(0.426343806632472,-0.0335099672547986,-0.903940285992784));
#55479=DIRECTION('center_axis',(-0.712444668004794,0.601098524805671,-0.362081701426605));
#55480=DIRECTION('ref_axis',(0.430201689006238,-0.0335100655799265,-0.902110626409538));
#55481=DIRECTION('',(0.944235193658814,-3.88578058618719E-13,0.329271770815693));
#55482=DIRECTION('center_axis',(0.777849585313836,0.584827952146828,0.230057142933752));
#55483=DIRECTION('ref_axis',(0.319422936040306,-0.0526562728363321,-0.946148141076426));
#55484=DIRECTION('center_axis',(0.921696777606893,7.30033026013869E-10,
0.387911136923225));
#55485=DIRECTION('ref_axis',(-0.38786288020675,0.0157729998153751,0.92158211714125));
#55486=DIRECTION('',(-0.921696815639174,-1.76914038951287E-10,-0.387911046556562));
#55487=DIRECTION('',(0.90050541046818,0.,-0.434844806474143));
#55488=DIRECTION('',(-0.377443536985532,6.51326541667579E-11,-0.926032600067542));
#55489=DIRECTION('center_axis',(0.,-1.,1.45983193964168E-32));
#55490=DIRECTION('ref_axis',(1.,0.,0.));
#55491=DIRECTION('center_axis',(0.722194730403783,0.601098534741279,0.342221160814019));
#55492=DIRECTION('ref_axis',(0.392334337172448,0.0514849217340168,-0.918380678536683));
#55493=DIRECTION('center_axis',(-0.778394128429977,0.601098534940886,-0.181061128124333));
#55494=DIRECTION('ref_axis',(0.264543494507129,0.0525165158982934,-0.962942757941437));
#55495=DIRECTION('center_axis',(0.759133928885952,0.58482793005096,0.285818071938233));
#55496=DIRECTION('ref_axis',(0.337412268951842,0.0219594825744128,-0.941100813880125));
#55497=DIRECTION('center_axis',(-0.963048054619894,-1.01164058154922E-8,
-0.269329620526294));
#55498=DIRECTION('ref_axis',(-0.269296259071625,-0.0157391393485634,0.962928763898241));
#55499=DIRECTION('',(0.963047106750035,0.,0.269333009823132));
#55500=DIRECTION('center_axis',(0.745996129500833,0.584827952320648,0.318537346247209));
#55501=DIRECTION('ref_axis',(0.370977816814879,0.0322834330599069,-0.928080405665981));
#55502=DIRECTION('center_axis',(0.944235168505604,5.6877892465971E-10,0.329271842946209));
#55503=DIRECTION('ref_axis',(-0.329231248590178,0.0157020800818962,0.944118758225285));
#55504=DIRECTION('',(-0.944235193658622,-3.88578058618715E-13,-0.329271770816244));
#55505=DIRECTION('',(0.87142433742845,-1.43735365431918E-13,-0.490529942141545));
#55506=DIRECTION('center_axis',(-0.758320962878211,-0.601098528151806,-0.252249631740454));
#55507=DIRECTION('ref_axis',(0.298894247961264,0.0232723682068303,-0.954002424217945));
#55508=DIRECTION('',(-0.434844806473994,1.43735365432644E-13,-0.900505410468252));
#55509=DIRECTION('center_axis',(0.,-1.,1.45983193964168E-32));
#55510=DIRECTION('ref_axis',(1.,0.,0.));
#55511=DIRECTION('center_axis',(0.759391699445769,0.60109853103519,0.249007636027903));
#55512=DIRECTION('ref_axis',(0.296306370032838,0.0212180581951432,-0.954857229686402));
#55513=DIRECTION('center_axis',(0.779160575653599,-0.601098526282654,0.177733955810289));
#55514=DIRECTION('ref_axis',(0.23862335649232,0.0222452550770015,-0.970857374882067));
#55515=DIRECTION('center_axis',(-0.778394148784845,0.601098529365771,-0.181061059125989));
#55516=DIRECTION('ref_axis',(0.242768812035222,0.0222451738801953,-0.969829086046633));
#55517=DIRECTION('center_axis',(0.788970628196199,0.584827953016268,0.188418717792304));
#55518=DIRECTION('ref_axis',(0.237775337803774,-0.00784645567628602,-0.971288485397424));
#55519=DIRECTION('center_axis',(-0.97805838109112,-7.84599393169719E-10,
-0.208330994279336));
#55520=DIRECTION('ref_axis',(-0.208305389342993,-0.015677848308091,0.977938172812112));
#55521=DIRECTION('',(0.978058312885159,3.88578058618636E-13,0.208331314487851));
#55522=DIRECTION('center_axis',(0.780037042689973,0.58482795225398,0.222527477615458));
#55523=DIRECTION('ref_axis',(0.2726252226216,0.00246180457925343,-0.962117158930625));
#55524=DIRECTION('center_axis',(0.963047086738829,5.62745578224248E-10,
0.269333081376674));
#55525=DIRECTION('ref_axis',(-0.269300009007876,0.0156707406191654,0.962928830722606));
#55526=DIRECTION('',(-0.963047106750114,-6.41708908203849E-11,-0.269333009822849));
#55527=DIRECTION('',(0.838904150644651,1.6426898906501E-13,-0.544279180229389));
#55528=DIRECTION('center_axis',(-0.783956636830115,-0.601098528045093,-0.155217753984645));
#55529=DIRECTION('ref_axis',(0.199320628268647,-0.00691952448456596,-0.979909897555637));
#55530=DIRECTION('',(-0.490529942130889,2.35931335548681E-11,-0.871424337434448));
#55531=DIRECTION('center_axis',(0.,-1.,1.45983193964168E-32));
#55532=DIRECTION('ref_axis',(1.,0.,0.));
#55533=DIRECTION('center_axis',(0.784612606923713,0.601098526770815,0.151867106940017));
#55534=DIRECTION('ref_axis',(0.196643273319265,-0.00897208774518776,-0.980434049133228));
#55535=DIRECTION('center_axis',(0.779160573919315,-0.601098528567099,0.177733955687123));
#55536=DIRECTION('ref_axis',(0.216559142005727,-0.00794569869411633,-0.976237165798356));
#55537=DIRECTION('center_axis',(-0.778394144807355,0.601098527383943,-0.181061082804895));
#55538=DIRECTION('ref_axis',(0.220727799876673,-0.00794579414360136,-0.9753030824913));
#55539=DIRECTION('center_axis',(0.806364498274801,0.584827952228293,0.0880486355061219));
#55540=DIRECTION('ref_axis',(0.121531513603223,-0.0181546317370622,-0.992421533698157));
#55541=DIRECTION('center_axis',(-0.989209558181874,6.15894848857748E-10,
-0.14650750834555));
#55542=DIRECTION('ref_axis',(-0.146489498037684,-0.0156795066150825,0.989087953640613));
#55543=DIRECTION('',(0.989209569218361,2.06171493653842E-7,0.146507433827718));
#55544=DIRECTION('center_axis',(0.801777367482884,0.584827782536652,0.123002104719708));
#55545=DIRECTION('ref_axis',(0.171045908407409,-0.0273551074109777,-0.984883239432786));
#55546=DIRECTION('center_axis',(0.978058291383363,6.95105897126313E-10,
0.208331415432856));
#55547=DIRECTION('ref_axis',(-0.208305730440146,0.0157023279250068,0.977937707404481));
#55548=DIRECTION('',(0.978058312610443,-1.29267404452746E-5,0.208331315376523));
#55549=DIRECTION('',(0.80307316876836,-7.6262907754909E-8,-0.595880428948912));
#55550=DIRECTION('center_axis',(-0.989209569691202,3.16135222513024E-12,
-0.146507430635265));
#55551=DIRECTION('ref_axis',(-0.113085605683379,-0.635772805085027,0.763547369913315));
#55552=DIRECTION('',(0.544279180228156,0.,0.838904150645451));
#55553=DIRECTION('center_axis',(0.913641051300077,0.398564391591664,0.0800403344224422));
#55554=DIRECTION('ref_axis',(-0.39984725127672,0.916581788847264,-1.13151217873397E-16));
#55555=DIRECTION('center_axis',(-0.997020848376335,5.7445662141833E-5,-0.0771325132672888));
#55556=DIRECTION('ref_axis',(0.077132529100234,0.000362892818154704,-0.997020782764032));
#55557=DIRECTION('',(0.996456789590153,5.94973683407411E-5,0.0841062598131004));
#55558=DIRECTION('center_axis',(0.796254114848551,0.590180063812527,0.13291680429875));
#55559=DIRECTION('ref_axis',(0.601502357066498,-0.795819654738625,-0.0697566597189352));
#55560=DIRECTION('center_axis',(0.413785045843809,0.550037558024795,-0.72542444168787));
#55561=DIRECTION('ref_axis',(-2.3512701952177E-16,0.796841686266789,0.604188155318772));
#55562=DIRECTION('center_axis',(0.56697188662127,-0.477126090203707,0.671486093547768));
#55563=DIRECTION('ref_axis',(0.793529116258299,0.0976273805452995,-0.60065001141945));
#55564=DIRECTION('center_axis',(0.595310741352729,0.584827951389405,0.550982203436496));
#55565=DIRECTION('ref_axis',(0.664842645401608,0.0265489690088179,-0.746511492945661));
#55566=DIRECTION('center_axis',(-0.796270459217244,-1.33926730831543E-11,
-0.604940787001471));
#55567=DIRECTION('ref_axis',(-0.604865772061812,-0.0157477670570415,0.796171718676809));
#55568=DIRECTION('center_axis',(0.762632738812627,-0.000115441153842097,
0.64683173419715));
#55569=DIRECTION('ref_axis',(0.0152930708773917,-0.999717230246732,-0.0182093803008533));
#55570=DIRECTION('',(-0.756714656874731,-6.07014438447633E-10,-0.653745308259232));
#55571=DIRECTION('center_axis',(-0.607215615508909,-0.601098528125524,-0.519586138929307));
#55572=DIRECTION('ref_axis',(0.633799249965789,0.0279220112272639,-0.772993448893215));
#55573=DIRECTION('',(-0.0728103245348818,2.24206636476418E-10,-0.997345805947529));
#55574=DIRECTION('center_axis',(0.,-1.,1.45983193964168E-32));
#55575=DIRECTION('ref_axis',(1.,0.,0.));
#55576=DIRECTION('center_axis',(0.609429838331448,0.601098531375975,0.516987260702768));
#55577=DIRECTION('ref_axis',(0.631725933862725,0.0258667775350435,-0.774760126945896));
#55578=DIRECTION('center_axis',(0.66335610523484,-0.601098525931305,0.445689622686996));
#55579=DIRECTION('ref_axis',(0.574162095150205,0.0268944226164245,-0.818299809681547));
#55580=DIRECTION('center_axis',(-0.661445984060744,0.601098529285794,-0.448519529407996));
#55581=DIRECTION('ref_axis',(0.577652734288884,0.0268943494357593,-0.815839452672524));
#55582=DIRECTION('center_axis',(0.659672929384356,0.584827952222519,0.472025309211994));
#55583=DIRECTION('ref_axis',(0.583823735428411,-0.00326197145261643,-0.811873885214114));
#55584=DIRECTION('center_axis',(-0.832683791162331,-5.94454085157781E-10,
-0.553748773303858));
#55585=DIRECTION('ref_axis',(-0.553680668148574,-0.0156832196308938,0.832581380010721));
#55586=DIRECTION('',(0.832683748469071,8.32136531871631E-8,0.553748837502608));
#55587=DIRECTION('center_axis',(0.638538105402631,0.584827969931605,0.500245273375468));
#55588=DIRECTION('ref_axis',(0.612684050745061,0.00704480134031414,-0.790296542278086));
#55589=DIRECTION('center_axis',(0.79627042978386,3.77540322483168E-10,0.604940825743995));
#55590=DIRECTION('ref_axis',(-0.604866535424114,0.0156715280546595,0.796172643044497));
#55591=DIRECTION('',(-0.796270460894472,-1.48769885298212E-11,-0.604940784793772));
#55592=DIRECTION('',(0.980355879774379,-3.07809289803698E-8,-0.197236784073871));
#55593=DIRECTION('center_axis',(0.327042540097583,0.793626260386024,-0.513030735718841));
#55594=DIRECTION('ref_axis',(1.25736257823514E-16,0.542884142421512,0.839807601720334));
#55595=DIRECTION('center_axis',(0.202198880588061,0.471546674539153,0.858346868358009));
#55596=DIRECTION('ref_axis',(0.82289066041759,0.393411577749833,-0.409973525352419));
#55597=DIRECTION('center_axis',(-0.667548947904293,-0.601098528046553,-0.439384753640974));
#55598=DIRECTION('ref_axis',(0.551225507145412,-0.00227572072850447,-0.834353199411046));
#55599=DIRECTION('',(-0.135290511410435,5.19500677922224E-12,-0.990805973701361));
#55600=DIRECTION('center_axis',(0.,-1.,1.45983193964168E-32));
#55601=DIRECTION('ref_axis',(1.,0.,0.));
#55602=DIRECTION('center_axis',(0.669419981668909,0.601098527615754,0.436528863009733));
#55603=DIRECTION('ref_axis',(0.548943210914805,-0.00432804893558317,-0.83584844271133));
#55604=DIRECTION('center_axis',(0.663356092189077,-0.601098528168137,0.445689639087264));
#55605=DIRECTION('ref_axis',(0.555621063060828,-0.00330181158883881,-0.831429090375954));
#55606=DIRECTION('center_axis',(-0.661445983008431,0.60109852788511,-0.448519532837048));
#55607=DIRECTION('ref_axis',(0.559167948443955,-0.00330187419158931,-0.829047829175013));
#55608=DIRECTION('center_axis',(0.713627116595045,0.58482825598741,0.385632272325549));
#55609=DIRECTION('ref_axis',(0.495997915872523,-0.0330815410799037,-0.867693309349503));
#55610=DIRECTION('center_axis',(-0.86582787538343,-1.08385228015312E-7,
-0.500341973263291));
#55611=DIRECTION('ref_axis',(-0.5002804983147,-0.0156751635309624,0.865721498089468));
#55612=DIRECTION('',(0.865810815149328,0.,0.500371494362396));
#55613=DIRECTION('center_axis',(0.696199124465904,0.584827952226065,0.416272801643317));
#55614=DIRECTION('ref_axis',(0.527066089522502,-0.0227607295913177,-0.849519444429572));
#55615=DIRECTION('center_axis',(0.832683703923129,6.25710847379276E-10,
0.553748904487276));
#55616=DIRECTION('ref_axis',(-0.553680710962633,0.0156933905077011,0.832581159889104));
#55617=DIRECTION('',(-0.832683749191998,-2.24820162482884E-11,-0.553748836415534));
#55618=DIRECTION('',(0.966036775392944,0.,-0.258404621840249));
#55619=DIRECTION('center_axis',(-0.71735463898416,-0.601098527931815,-0.352254001604114));
#55620=DIRECTION('ref_axis',(0.462337665315646,-0.0324816879447406,-0.88610881001079));
#55621=DIRECTION('',(-0.197236768330209,8.17238220606182E-12,-0.98035588294183));
#55622=DIRECTION('center_axis',(0.,-1.,1.45983193964168E-32));
#55623=DIRECTION('ref_axis',(1.,0.,0.));
#55624=DIRECTION('center_axis',(0.718852993768966,0.601098523304961,0.349186108873178));
#55625=DIRECTION('ref_axis',(0.459892199152257,-0.034538552828122,-0.887302796979385));
#55626=DIRECTION('center_axis',(0.663356092770367,-0.60109852991426,0.445689635867099));
#55627=DIRECTION('ref_axis',(0.53627572350735,-0.0335099728267182,-0.843377394822639));
#55628=DIRECTION('center_axis',(-0.661445962688288,0.601098525066399,-0.448519566581396));
#55629=DIRECTION('ref_axis',(0.539873856959319,-0.0335100609617226,-0.841078649346309));
#55630=DIRECTION('',(0.895520921369855,3.88578058618721E-13,0.445019414620179));
#55631=DIRECTION('center_axis',(0.742882203366681,0.584827952147364,0.325733477413953));
#55632=DIRECTION('ref_axis',(0.435487996745506,-0.0526562728284316,-0.898653170929922));
#55633=DIRECTION('center_axis',(0.865810771633002,6.42926458855253E-10,
0.500371569660253));
#55634=DIRECTION('ref_axis',(-0.500309322695488,0.0157729998147222,0.865703063469702));
#55635=DIRECTION('',(-0.865810815150161,-1.76914038951315E-10,-0.500371494360954));
#55636=DIRECTION('',(0.947905162032747,-1.43735365431978E-13,-0.318552670357151));
#55637=DIRECTION('',(-0.258404621806973,6.51326541667439E-11,-0.966036775401845));
#55638=DIRECTION('center_axis',(0.,-1.,1.45983193964168E-32));
#55639=DIRECTION('ref_axis',(1.,0.,0.));
#55640=DIRECTION('center_axis',(0.67360832250785,0.601098534529477,0.430037649089794));
#55641=DIRECTION('ref_axis',(0.504344286576578,0.0514849241852926,-0.86196643970586));
#55642=DIRECTION('center_axis',(-0.749563283555236,0.601098534670828,-0.277192055374023));
#55643=DIRECTION('ref_axis',(0.383146215747937,0.0525165190175251,-0.922193576527357));
#55644=DIRECTION('center_axis',(0.717324974950354,0.584827908067301,0.378709913070808));
#55645=DIRECTION('ref_axis',(0.452703598373547,0.0219600677454818,-0.891390603183731));
#55646=DIRECTION('center_axis',(-0.921699486410975,-1.91782754834668E-8,
-0.387904700602795));
#55647=DIRECTION('ref_axis',(-0.387856651377982,-0.0157391387101182,0.921585317534151));
#55648=DIRECTION('',(0.92169681563843,4.44089209850062E-13,0.38791104655833));
#55649=DIRECTION('center_axis',(0.700190411583638,0.584827952320447,0.409523691269515));
#55650=DIRECTION('ref_axis',(0.484371864175863,0.0322834330620492,-0.874266365099635));
#55651=DIRECTION('center_axis',(0.895520891779626,4.91459824244294E-10,
0.445019474165146));
#55652=DIRECTION('ref_axis',(-0.444964609830889,0.0157020800820199,0.895410487251039));
#55653=DIRECTION('',(-0.895520921369562,-8.32667268468546E-13,-0.445019414620768));
#55654=DIRECTION('',(0.926032600054668,0.,-0.377443537017117));
#55655=DIRECTION('center_axis',(-0.720726113507914,-0.601098528148682,-0.345303386553429));
#55656=DIRECTION('ref_axis',(0.416105586312613,0.0232723683016273,-0.909018447509769));
#55657=DIRECTION('',(-0.318552670356925,0.,-0.947905162032823));
#55658=DIRECTION('center_axis',(0.,-1.,1.45983193964168E-32));
#55659=DIRECTION('ref_axis',(1.,0.,0.));
#55660=DIRECTION('center_axis',(0.722194735685976,0.601098530972697,0.342221156286295));
#55661=DIRECTION('ref_axis',(0.413645252066319,0.0212180599124248,-0.910190858763449));
#55662=DIRECTION('center_axis',(0.750740685581025,-0.601098526591847,0.273987197406091));
#55663=DIRECTION('ref_axis',(0.358422444249889,0.0222452470260503,-0.93329443395034));
#55664=DIRECTION('center_axis',(-0.749563311433282,0.601098529303308,-0.277191991627778));
#55665=DIRECTION('ref_axis',(0.362406320684363,0.0222451755618634,-0.931754694590934));
#55666=DIRECTION('center_axis',(0.759134231974123,0.58482795301644,0.2858172199425));
#55667=DIRECTION('ref_axis',(0.357635134842662,-0.00784645567666929,-0.933828433631888));
#55668=DIRECTION('center_axis',(-0.944235336028488,-1.60783837117334E-9,
-0.329271362549446));
#55669=DIRECTION('ref_axis',(-0.329230893423353,-0.0156778483097205,0.944119284777108));
#55670=DIRECTION('',(0.944235193658949,3.88578058618655E-13,0.329271770815305));
#55671=DIRECTION('center_axis',(0.745996129292408,0.584827952253851,0.318537346857968));
#55672=DIRECTION('ref_axis',(0.391060745915754,0.00246180458492519,-0.920361577056539));
#55673=DIRECTION('center_axis',(0.921696792401348,4.50063191212345E-10,
0.387911101770839));
#55674=DIRECTION('ref_axis',(-0.387863468778648,0.0156707406191547,0.921583613936056));
#55675=DIRECTION('',(-0.921696815638753,-6.4226401971644E-11,-0.387911046557562));
#55676=DIRECTION('',(0.900505410468141,0.,-0.434844806474224));
#55677=DIRECTION('center_axis',(-0.758320961486058,-0.601098528044341,-0.252249636181676));
#55678=DIRECTION('ref_axis',(0.320564201865843,-0.00691952430573698,-0.947201516397381));
#55679=DIRECTION('',(-0.377443537005826,2.34493981894312E-11,-0.92603260005927));
#55680=DIRECTION('center_axis',(0.,-1.,1.45983193964168E-32));
#55681=DIRECTION('ref_axis',(1.,0.,0.));
#55682=DIRECTION('center_axis',(0.75939170473741,0.601098526820475,0.249007630064353));
#55683=DIRECTION('ref_axis',(0.31797365645609,-0.00897208425772004,-0.948057095065491));
#55684=DIRECTION('center_axis',(0.750740687421923,-0.601098528539803,0.273987188088317));
#55685=DIRECTION('ref_axis',(0.337206472014744,-0.00794570095967736,-0.941397185606388));
#55686=DIRECTION('center_axis',(-0.749563305959255,0.601098527443124,-0.277192010464118));
#55687=DIRECTION('ref_axis',(0.341225178879087,-0.00794578980304227,-0.939947999478344));
#55688=DIRECTION('center_axis',(0.788970653153501,0.584827952228961,0.188418615731616));
#55689=DIRECTION('ref_axis',(0.244956601208456,-0.0181546317280604,-0.969364055900166));
#55690=DIRECTION('center_axis',(-0.963047127164173,-5.9401172880047E-10,
-0.269332936828812));
#55691=DIRECTION('ref_axis',(-0.269299827447224,-0.0156795066176967,0.962928738801123));
#55692=DIRECTION('',(0.963047105879958,2.0617149365389E-7,0.269333012934164));
#55693=DIRECTION('center_axis',(0.780038861938788,0.584827782536756,0.222521546458721));
#55694=DIRECTION('ref_axis',(0.293135761418687,-0.0273551074055863,-0.955679404128976));
#55695=DIRECTION('center_axis',(0.94423516594774,5.45508720203076E-10,0.329271850281259));
#55696=DIRECTION('ref_axis',(-0.329231254642399,0.0157023279249513,0.94411875199274));
#55697=DIRECTION('',(0.944235193275004,-1.29267404097053E-5,0.329271771662581));
#55698=DIRECTION('',(0.871424317944201,-7.62629077549355E-8,-0.490529976755221));
#55699=DIRECTION('center_axis',(-0.963047106747145,8.30207502439632E-12,
-0.269333009833466));
#55700=DIRECTION('ref_axis',(-0.207891752764345,-0.635772805084664,0.743353186209185));
#55701=DIRECTION('',(0.434844806472752,0.,0.900505410468851));
#55702=DIRECTION('center_axis',(0.896405004789995,0.398564391592692,0.19391877975533));
#55703=DIRECTION('ref_axis',(-0.406276499725655,0.913750187836188,-3.10333992776203E-16));
#55704=DIRECTION('center_axis',(-0.979491773889536,5.74456556182148E-5,
-0.201484147224359));
#55705=DIRECTION('ref_axis',(0.201484154706541,0.000363041689850167,-0.979491706755561));
#55706=DIRECTION('',(0.978058120671662,5.94973683762348E-5,0.208332208379502));
#55707=DIRECTION('center_axis',(0.773316520448395,0.59018006381252,0.231665818540062));
#55708=DIRECTION('ref_axis',(0.60549942861941,-0.795821622328588,0.00619575466446112));
#55709=DIRECTION('center_axis',(0.501442018148417,0.550037558025294,-0.667843235495288));
#55710=DIRECTION('ref_axis',(-4.66273618249888E-16,0.771902436596558,0.6357410073106));
#55711=DIRECTION('center_axis',(0.478341620466137,-0.477126090494331,0.73725164489435));
#55712=DIRECTION('ref_axis',(0.862552891155475,0.0976251602361496,-0.496459301502346));
#55713=DIRECTION('center_axis',(0.521560157167445,0.584827951390025,0.621249764368902));
#55714=DIRECTION('ref_axis',(0.753162861857848,0.0265489689976712,-0.657298148303536));
#55715=DIRECTION('center_axis',(-0.714172445357471,-3.3520060503145E-11,
-0.699969798128555));
#55716=DIRECTION('ref_axis',(-0.699882999232859,-0.0157477670559804,0.714083885280692));
#55717=DIRECTION('center_axis',(0.675549640303332,-0.000115441165281704,
0.737314498812668));
#55718=DIRECTION('ref_axis',(0.0182582712999792,-0.999690713313198,-0.0168852966952043));
#55719=DIRECTION('',(-0.668811722373935,-6.06903416145164E-10,-0.743431826070966));
#55720=DIRECTION('center_axis',(-0.537306126172887,-0.601098528049546,-0.591593345427207));
#55721=DIRECTION('ref_axis',(0.725683323477494,0.0279220128337455,-0.687462053662579));
#55722=DIRECTION('',(0.0527643814626838,2.24062901110916E-10,-0.998606989785702));
#55723=DIRECTION('center_axis',(0.,-1.,1.45983193964168E-32));
#55724=DIRECTION('ref_axis',(1.,0.,0.));
#55725=DIRECTION('center_axis',(0.539828613186025,0.601098531243132,0.589292477572048));
#55726=DIRECTION('ref_axis',(0.723847780931745,0.0258667806383051,-0.68947465486383));
#55727=DIRECTION('center_axis',(0.602265620307525,-0.601098526029287,0.525315795118528));
#55728=DIRECTION('ref_axis',(0.672194818786008,0.0268944205332519,-0.739885677480938));
#55729=DIRECTION('center_axis',(-0.600015879953058,0.601098529364232,-0.527883985171283));
#55730=DIRECTION('ref_axis',(0.67534956841233,0.0268943476353437,-0.737007228262077));
#55731=DIRECTION('center_axis',(0.595310752969356,0.584827952222556,0.550982190000939));
#55732=DIRECTION('ref_axis',(0.680974890179038,-0.00326197144911916,-0.7322995005378));
#55733=DIRECTION('center_axis',(-0.756714706390063,-5.93515005629862E-10,
-0.653745250944893));
#55734=DIRECTION('ref_axis',(-0.653664847298321,-0.0156832196311885,0.756621638620297));
#55735=DIRECTION('',(0.75671465601544,8.32135976761057E-8,0.653745309253861));
#55736=DIRECTION('center_axis',(0.570805684013776,0.584827969931209,0.576330735501505));
#55737=DIRECTION('ref_axis',(0.706903275138169,0.00704480135579719,-0.7072751447441));
#55738=DIRECTION('center_axis',(0.714172389847507,6.00847554702783E-10,
0.699969854764832));
#55739=DIRECTION('ref_axis',(-0.699883894318067,0.0156715280547506,0.714084685231805));
#55740=DIRECTION('',(-0.714172445802532,-1.48214773785851E-11,-0.699969797674464));
#55741=DIRECTION('',(0.997345804770064,-3.07809289803779E-8,-0.0728103406636272));
#55742=DIRECTION('center_axis',(0.388763513015119,0.793626260384467,-0.467996036069014));
#55743=DIRECTION('ref_axis',(-5.74087223566324E-17,0.507952836950267,0.861384882287921));
#55744=DIRECTION('center_axis',(0.0930250935242046,0.471546674524122,0.876920786456824));
#55745=DIRECTION('ref_axis',(0.867787458195339,0.393407974295759,-0.303603513088007));
#55746=DIRECTION('center_axis',(-0.607215611590486,-0.601098528053039,-0.519586143592438));
#55747=DIRECTION('ref_axis',(0.651451115212137,-0.00227571932839452,-0.758687198778523));
#55748=DIRECTION('',(-0.0100427887997432,5.1950067792211E-12,-0.999949569924966));
#55749=DIRECTION('center_axis',(0.,-1.,1.45983193964168E-32));
#55750=DIRECTION('ref_axis',(1.,0.,0.));
#55751=DIRECTION('center_axis',(0.609429829516059,0.60109852762544,0.516987275455166));
#55752=DIRECTION('ref_axis',(0.649374219434502,-0.00432804735943733,-0.760456699056485));
#55753=DIRECTION('center_axis',(0.602265607328405,-0.601098528165844,0.525315807554088));
#55754=DIRECTION('ref_axis',(0.655445521675757,-0.00330181187803222,-0.755235238951094));
#55755=DIRECTION('center_axis',(-0.600015883320388,0.601098527900785,-0.527883983010249));
#55756=DIRECTION('ref_axis',(0.65866598479739,-0.00330187161489854,-0.752428214592411));
#55757=DIRECTION('center_axis',(0.659667413981856,0.584828255987001,0.472032640746055));
#55758=DIRECTION('ref_axis',(0.600837632351962,-0.0330815410883527,-0.798686265807112));
#55759=DIRECTION('center_axis',(-0.796291055960073,-1.07988306620361E-7,
-0.604913674996673));
#55760=DIRECTION('ref_axis',(-0.604839352186181,-0.0156751635314749,0.796193222336929));
#55761=DIRECTION('',(0.796270460894843,0.,0.604940784793284));
#55762=DIRECTION('center_axis',(0.63853657013902,0.584827952226448,0.500247253755297));
#55763=DIRECTION('ref_axis',(0.629383034937091,-0.0227607295813455,-0.776761832560214));
#55764=DIRECTION('center_axis',(0.756714603597912,6.23929002742358E-10,
0.653745369927508));
#55765=DIRECTION('ref_axis',(-0.653664861953803,0.0156933905085894,0.756621415069162));
#55766=DIRECTION('',(-0.756714656868878,-2.20379270384426E-11,-0.653745308266007));
#55767=DIRECTION('',(0.99080597370102,0.,-0.135290511412935));
#55768=DIRECTION('center_axis',(-0.667548948507381,-0.601098528036872,-0.439384752737956));
#55769=DIRECTION('ref_axis',(0.569750879323193,-0.0324816860210763,-0.821175301372172));
#55770=DIRECTION('',(-0.0728103246472255,8.1518485824278E-12,-0.997345805939327));
#55771=DIRECTION('center_axis',(0.,-1.,1.45983193964168E-32));
#55772=DIRECTION('ref_axis',(1.,0.,0.));
#55773=DIRECTION('center_axis',(0.669419994709514,0.601098523566272,0.436528848587996));
#55774=DIRECTION('ref_axis',(0.567474345638155,-0.0345385482279327,-0.822666369635258));
#55775=DIRECTION('center_axis',(0.602265611301596,-0.601098530053937,0.525315800838421));
#55776=DIRECTION('ref_axis',(0.637750242713869,-0.0335099703073872,-0.769513943868725));
#55777=DIRECTION('center_axis',(-0.600015867092371,0.601098525646047,-0.527884004023175));
#55778=DIRECTION('ref_axis',(0.64103188687302,-0.0335100506535652,-0.76678236581002));
#55779=DIRECTION('',(0.832683749192558,0.,0.553748836414691));
#55780=DIRECTION('center_axis',(0.696199125316928,0.584827952146109,0.416272800332345));
#55781=DIRECTION('ref_axis',(0.544685151561283,-0.0526562728459283,-0.83698590346471));
#55782=DIRECTION('center_axis',(0.796270393925419,8.30266888503259E-10,
0.604940872943678));
#55783=DIRECTION('ref_axis',(-0.604865617402429,0.0157729998155413,0.796171336686519));
#55784=DIRECTION('',(-0.796270460895877,-1.756927936244E-10,-0.604940784791923));
#55785=DIRECTION('',(0.980355882941038,0.,-0.197236768334149));
#55786=DIRECTION('',(-0.135290511379306,6.51326541667664E-11,-0.990805973705612));
#55787=DIRECTION('center_axis',(0.,-1.,1.45983193964168E-32));
#55788=DIRECTION('ref_axis',(1.,0.,0.));
#55789=DIRECTION('center_axis',(0.614398707753774,0.601098534286894,0.511072186670964));
#55790=DIRECTION('ref_axis',(0.608400425199828,0.0514849269706017,-0.791958474234287));
#55791=DIRECTION('center_axis',(-0.708911379310895,0.601098534382717,-0.368951498501462));
#55792=DIRECTION('ref_axis',(0.495706492384409,0.0525165223579738,-0.866900852628125));
#55793=DIRECTION('center_axis',(0.664204276505397,0.584827930051153,0.465627502735853));
#55794=DIRECTION('ref_axis',(0.560854097273766,0.0219594825688793,-0.827623382159141));
#55795=DIRECTION('center_axis',(-0.865812541374247,-9.56935734198916E-9,
-0.500368507401363));
#55796=DIRECTION('ref_axis',(-0.500306527662049,-0.0157391393472365,0.865705295046387));
#55797=DIRECTION('',(0.86581081514902,0.,0.500371494362928));
#55798=DIRECTION('center_axis',(0.643342272591299,0.584827952319625,0.494051603056501));
#55799=DIRECTION('ref_axis',(0.590127077899819,0.032283433074407,-0.806664621685091));
#55800=DIRECTION('center_axis',(0.832683701355471,6.47954253504361E-10,
0.553748908348317));
#55801=DIRECTION('ref_axis',(-0.553680639279151,0.0157020800829031,0.832581043723973));
#55802=DIRECTION('',(-0.832683749192111,-3.88578058618584E-13,-0.553748836415365));
#55803=DIRECTION('',(0.966036775392978,0.,-0.258404621840121));
#55804=DIRECTION('center_axis',(-0.671764981849494,-0.601098528105988,-0.432911502122043));
#55805=DIRECTION('ref_axis',(0.526754692134173,0.0232723694222049,-0.849698706092995));
#55806=DIRECTION('',(-0.197236768334325,0.,-0.980355882941002));
#55807=DIRECTION('center_axis',(0.,-1.,1.45983193964168E-32));
#55808=DIRECTION('ref_axis',(1.,0.,0.));
#55809=DIRECTION('center_axis',(0.67360832555935,0.601098530772093,0.430037649561942));
#55810=DIRECTION('ref_axis',(0.524460705381175,0.0212180654376879,-0.851170231040867));
#55811=DIRECTION('center_axis',(0.710481175414537,-0.601098526313104,0.365919473444354));
#55812=DIRECTION('ref_axis',(0.472568976800901,0.0222452543572108,-0.881012889136097));
#55813=DIRECTION('center_axis',(-0.708911410112214,0.601098529398319,-0.368951447439755));
#55814=DIRECTION('ref_axis',(0.476328470483819,0.0222451729067309,-0.87898597286242));
#55815=DIRECTION('center_axis',(0.717325835414934,0.584827953016227,0.378708213823145));
#55816=DIRECTION('ref_axis',(0.471854812187027,-0.00784645565919282,-0.881641349614192));
#55817=DIRECTION('center_axis',(-0.895521107072002,-1.4892603257905E-9,
-0.445019040928066));
#55818=DIRECTION('ref_axis',(-0.444964345834529,-0.0156778483098858,0.895411043045831));
#55819=DIRECTION('',(0.895520921369927,0.,0.445019414620034));
#55820=DIRECTION('center_axis',(0.700190411309518,0.584827952254178,0.409523691832833));
#55821=DIRECTION('ref_axis',(0.503329007620302,0.00246180457570976,-0.864091343323259));
#55822=DIRECTION('center_axis',(0.865810773374916,6.35123262430197E-10,
0.500371566646158));
#55823=DIRECTION('ref_axis',(-0.500310124231316,0.0156707406190989,0.865704457352562));
#55824=DIRECTION('',(-0.865810815149511,-6.37823127617821E-11,-0.500371494362078));
#55825=DIRECTION('',(0.947905162032825,1.64268989065083E-13,-0.31855267035692));
#55826=DIRECTION('center_axis',(-0.720726111162175,-0.601098528053417,-0.345303391615352));
#55827=DIRECTION('ref_axis',(0.436752287053821,-0.00691952365102899,-0.899555201166498));
#55828=DIRECTION('',(-0.25840462182816,2.3449398189435E-11,-0.966036775396178));
#55829=DIRECTION('center_axis',(0.,-1.,1.45983193964168E-32));
#55830=DIRECTION('ref_axis',(1.,0.,0.));
#55831=DIRECTION('center_axis',(0.722194739844622,0.601098526879159,0.342221154700384));
#55832=DIRECTION('ref_axis',(0.434289405563679,-0.00897208007322183,-0.900728712762231));
#55833=DIRECTION('center_axis',(0.710481170796042,-0.601098528513992,0.365919478796359));
#55834=DIRECTION('ref_axis',(0.452535854473705,-0.00794570338777936,-0.891710808622071));
#55835=DIRECTION('center_axis',(-0.708911406887304,0.601098527487534,-0.368951456749235));
#55836=DIRECTION('ref_axis',(0.456341234740237,-0.00794578655635072,-0.889769375710221));
#55837=DIRECTION('center_axis',(0.759134269518841,0.5848279522295,0.285817121833429));
#55838=DIRECTION('ref_axis',(0.364518576884325,-0.0181546317168159,-0.931019127866583));
#55839=DIRECTION('center_axis',(-0.921696778591536,7.48645501603821E-10,
-0.387911134583663));
#55840=DIRECTION('ref_axis',(-0.387863448283094,-0.015679506614589,0.921583473461992));
#55841=DIRECTION('',(0.921696814384977,2.06171049564735E-7,0.387911049536543));
#55842=DIRECTION('center_axis',(0.745998677573766,0.584827782536733,0.318531690466364));
#55843=DIRECTION('ref_axis',(0.410602688348994,-0.0273551074101987,-0.91140393373035));
#55844=DIRECTION('center_axis',(0.895520876536056,6.75843163070039E-10,
0.445019504840063));
#55845=DIRECTION('ref_axis',(-0.444964638772521,0.0157023279262793,0.89541046852253));
#55846=DIRECTION('',(0.895520920882366,-1.29267412267966E-5,0.445019415413417));
#55847=DIRECTION('',(0.926032585062198,-7.62629077549361E-8,-0.377443573800134));
#55848=DIRECTION('center_axis',(-0.921696815639292,-2.06910887724944E-12,
-0.387911046556281));
#55849=DIRECTION('ref_axis',(-0.29941932269188,-0.635772805085085,0.711435878707968));
#55850=DIRECTION('',(0.318552670355559,0.,0.947905162033282));
#55851=DIRECTION('center_axis',(0.865032115867938,0.398564391594533,0.304739010088827));
#55852=DIRECTION('ref_axis',(-0.41846846945328,0.908231325199384,-2.63657958565185E-16));
#55853=DIRECTION('center_axis',(-0.94651552901007,5.74456447744061E-5,-0.322658255810672));
#55854=DIRECTION('ref_axis',(0.32265825482549,0.00036294994602284,-0.946515461500923));
#55855=DIRECTION('',(0.94423489092648,5.94973683407405E-5,0.329272633568477));
#55856=DIRECTION('center_axis',(0.73818326248297,0.590180063806695,0.326761324631792));
#55857=DIRECTION('ref_axis',(0.599945994337841,-0.79582265730166,0.082043293469382));
#55858=DIRECTION('center_axis',(0.581190950280199,0.550037558025492,-0.599729742528877));
#55859=DIRECTION('ref_axis',(-0.718118878872167,-8.71609914090751E-16,-0.695920452212307));
#55860=DIRECTION('center_axis',(0.382167621345336,-0.47712609034057,0.791390297584934));
#55861=DIRECTION('ref_axis',(0.917974674576926,0.0976286238898018,-0.384436143764828));
#55862=DIRECTION('center_axis',(0.439584257719342,0.584827951389649,0.681719845419452));
#55863=DIRECTION('ref_axis',(0.829605250079619,0.0265489690027765,-0.557718819195858));
#55864=DIRECTION('center_axis',(-0.620811502736929,-1.44144189845694E-11,
-0.783959870190762));
#55865=DIRECTION('ref_axis',(-0.783862656209556,-0.0157477670553342,0.620734519769016));
#55866=DIRECTION('center_axis',(0.577812722908943,-0.000115441210598508,
0.816169372077806));
#55867=DIRECTION('ref_axis',(0.0202499730413635,-0.999690122184594,-0.0144775066353077));
#55868=DIRECTION('',(-0.570361227482914,-6.06570349238548E-10,-0.821393979880656));
#55869=DIRECTION('center_axis',(-0.458922997514026,-0.601098527969961,-0.654270771183528));
#55870=DIRECTION('ref_axis',(0.806122937243544,0.0279220146409949,-0.591088970585841));
#55871=DIRECTION('',(0.177506961644642,2.24206636476394E-10,-0.984119544856054));
#55872=DIRECTION('center_axis',(0.,-1.,1.45983193964168E-32));
#55873=DIRECTION('ref_axis',(1.,0.,0.));
#55874=DIRECTION('center_axis',(0.461713971852301,0.601098531247332,0.652304195853954));
#55875=DIRECTION('ref_axis',(0.804554112791792,0.0258667804468661,-0.593315758478675));
#55876=DIRECTION('center_axis',(0.531677054547471,-0.601098525820599,0.596657415879521));
#55877=DIRECTION('ref_axis',(0.759626622235968,0.0268944251012258,-0.649803112249278));
#55878=DIRECTION('center_axis',(-0.529123173962527,0.601098529180198,-0.598923388250304));
#55879=DIRECTION('ref_axis',(0.762395730785078,0.0268943517741113,-0.646551965060301));
#55880=DIRECTION('center_axis',(0.521560170384467,0.584827952222769,0.621249752488843));
#55881=DIRECTION('ref_axis',(0.767386664097426,-0.0032619714661072,-0.641176315304596));
#55882=DIRECTION('center_axis',(-0.668811782515035,-6.34029621191083E-10,
-0.743431771966373));
#55883=DIRECTION('ref_axis',(-0.743340337842035,-0.015683219631839,0.668729525861441));
#55884=DIRECTION('',(0.668811721396846,8.32135976761153E-8,0.743431826949977));
#55885=DIRECTION('center_axis',(0.494071316040898,0.584827969931514,0.64332711760923));
#55886=DIRECTION('ref_axis',(0.789974212569877,0.00704480134113012,-0.613099595700948));
#55887=DIRECTION('center_axis',(0.620811451437247,5.06106120414513E-10,
0.783959910814564));
#55888=DIRECTION('ref_axis',(-0.783863635888522,0.0156715280540463,0.620735212099393));
#55889=DIRECTION('',(-0.620811504614948,-1.44328993199751E-11,-0.783959868703574));
#55890=DIRECTION('',(0.998606990639008,-3.07809289803829E-8,0.0527643653131774));
#55891=DIRECTION('center_axis',(0.444353453097782,0.793626260382252,-0.415580759361835));
#55892=DIRECTION('ref_axis',(-0.872542221931706,0.488538709772809,-1.67697309061468E-16));
#55893=DIRECTION('center_axis',(-0.0176157550387083,0.471546674599121,0.881665139862594));
#55894=DIRECTION('ref_axis',(0.898991141509732,0.393417286499192,-0.192451984065224));
#55895=DIRECTION('center_axis',(-0.537306120944992,-0.601098528063561,-0.591593350161127));
#55896=DIRECTION('ref_axis',(0.741402950424546,-0.00227571714743173,-0.671056246683722));
#55897=DIRECTION('',(0.115363314589441,5.0512714137876E-12,-0.993323364089931));
#55898=DIRECTION('center_axis',(0.,-1.,1.45983193964168E-32));
#55899=DIRECTION('ref_axis',(1.,0.,0.));
#55900=DIRECTION('center_axis',(0.539828601331174,0.601098527651807,0.589292492095104));
#55901=DIRECTION('ref_axis',(0.739564210493411,-0.00432804329610699,-0.673072096137171));
#55902=DIRECTION('center_axis',(0.531677029917933,-0.601098528156719,0.596657435473213));
#55903=DIRECTION('ref_axis',(0.744933215704376,-0.00330181543041807,-0.667130873333862));
#55904=DIRECTION('center_axis',(-0.529123179217502,0.601098527932195,-0.598923384860293));
#55905=DIRECTION('ref_axis',(0.747776463056216,-0.00330186607709241,-0.663942361187735));
#55906=DIRECTION('center_axis',(0.595310752812087,0.584827952238646,0.550982190153782));
#55907=DIRECTION('ref_axis',(0.696196315803167,-0.0330869090691157,-0.717088520554017));
#55908=DIRECTION('center_axis',(-0.714172494850206,-5.48807989469595E-10,
-0.69996974763159));
#55909=DIRECTION('ref_axis',(-0.699883747222762,-0.0156751701944172,0.714084749461015));
#55910=DIRECTION('',(0.714172445802503,3.88578058618675E-13,0.699969797674493));
#55911=DIRECTION('center_axis',(0.570803912686522,0.584827952226004,0.576332507808553));
#55912=DIRECTION('ref_axis',(0.721774233887805,-0.022760729597555,-0.691754222599226));
#55913=DIRECTION('center_axis',(0.668811671170596,5.24710583738528E-10,
0.743431872134895));
#55914=DIRECTION('ref_axis',(-0.743340319370965,0.0156933905087981,0.668729307785901));
#55915=DIRECTION('',(-0.668811722367453,-2.20379270384528E-11,-0.743431826076797));
#55916=DIRECTION('',(0.999949569924938,0.,-0.0100427888024681));
#55917=DIRECTION('center_axis',(-0.607215610045583,-0.601098528222621,-0.519586145201708));
#55918=DIRECTION('ref_axis',(0.668178782739805,-0.032481682628503,-0.743291365878801));
#55919=DIRECTION('',(0.0527643813501149,8.17238220606147E-12,-0.99860698979165));
#55920=DIRECTION('center_axis',(0.,-1.,1.45983193964168E-32));
#55921=DIRECTION('ref_axis',(1.,0.,0.));
#55922=DIRECTION('center_axis',(0.609429841859766,0.601098523778736,0.516987265376823));
#55923=DIRECTION('ref_axis',(0.666107080935483,-0.034538544519953,-0.745056001700579));
#55924=DIRECTION('center_axis',(0.531677035164203,-0.601098529878237,0.596657429063969));
#55925=DIRECTION('ref_axis',(0.729167065292789,-0.0335099735574638,-0.683514793230169));
#55926=DIRECTION('center_axis',(-0.529123151656913,0.601098525557496,-0.598923411592216));
#55927=DIRECTION('ref_axis',(0.732080473725266,-0.0335100522421239,-0.680393457044467));
#55928=DIRECTION('',(0.756714656868998,7.7715611723784E-13,0.653745308265868));
#55929=DIRECTION('center_axis',(0.638536571144397,0.584827952147131,0.500247252564718));
#55930=DIRECTION('ref_axis',(0.645292296194971,-0.0526562728331614,-0.762118868289417));
#55931=DIRECTION('center_axis',(0.714172398215871,4.92767641735136E-10,
0.699969846226673));
#55932=DIRECTION('ref_axis',(-0.699882768933784,0.0157729998150548,0.714083554093227));
#55933=DIRECTION('',(-0.714172445804273,-1.76525460892683E-10,-0.699969797672688));
#55934=DIRECTION('',(0.997345805939024,-1.43735365432053E-13,-0.0728103246513699));
#55935=DIRECTION('',(-0.0100427887682085,6.51326541667426E-11,-0.999949569925282));
#55936=DIRECTION('center_axis',(0.,-1.,1.45983193964168E-32));
#55937=DIRECTION('ref_axis',(1.,0.,0.));
#55938=DIRECTION('center_axis',(0.545499654375564,0.601098533820789,0.584046812947933));
#55939=DIRECTION('ref_axis',(0.70286172745956,0.0514849323635992,-0.709460847272123));
#55940=DIRECTION('center_axis',(-0.657079521879776,0.601098533955509,-0.454892354742068));
#55941=DIRECTION('ref_axis',(0.60044918033672,0.0525165272278878,-0.79793658657871));
#55942=DIRECTION('center_axis',(0.600608226843436,0.584827930051093,0.545202760521384));
#55943=DIRECTION('ref_axis',(0.660160309856493,0.0219594825681387,-0.750803667023223));
#55944=DIRECTION('center_axis',(-0.796272568887257,-9.84282189124006E-9,
-0.604938010078462));
#55945=DIRECTION('ref_axis',(-0.604863077538847,-0.0157391393470823,0.796173936349871));
#55946=DIRECTION('',(0.796270460894685,1.22124532708776E-12,0.604940784793492));
#55947=DIRECTION('center_axis',(0.576348241675388,0.584827952320947,0.570788025892079));
#55948=DIRECTION('ref_axis',(0.686575635049832,0.0322834330574119,-0.72634129533295));
#55949=DIRECTION('center_axis',(0.756714599701,6.55778036687605E-10,0.653745374438211));
#55950=DIRECTION('ref_axis',(-0.653664777278155,0.015702080080864,0.756621307938809));
#55951=DIRECTION('',(-0.756714656868477,-3.88578058618553E-13,-0.653745308266471));
#55952=DIRECTION('',(0.990805973700973,0.,-0.135290511413283));
#55953=DIRECTION('center_axis',(-0.612209713153376,-0.601098528006665,-0.513692346398972));
#55954=DIRECTION('ref_axis',(0.629096563127882,0.0232723720554988,-0.776978706889447));
#55955=DIRECTION('',(-0.0728103246514208,0.,-0.997345805939021));
#55956=DIRECTION('center_axis',(0.,-1.,1.45983193964168E-32));
#55957=DIRECTION('ref_axis',(1.,0.,0.));
#55958=DIRECTION('center_axis',(0.614398710488254,0.601098530667225,0.511072187640919));
#55959=DIRECTION('ref_axis',(0.627005096438769,0.0212180683557757,-0.778726140960389));
#55960=DIRECTION('center_axis',(0.659016935312657,-0.601098526825138,0.452081010461357));
#55961=DIRECTION('ref_axis',(0.579262838249883,0.0222452408855797,-0.814837231280354));
#55962=DIRECTION('center_axis',(-0.657079561225306,0.601098529124045,-0.454892304292861));
#55963=DIRECTION('ref_axis',(0.582738624272725,0.0222451803996117,-0.812355124148128));
#55964=DIRECTION('center_axis',(0.664204681256843,0.584827954381872,0.465626894809578));
#55965=DIRECTION('ref_axis',(0.578633172815619,-0.00784635391407085,-0.815550173838241));
#55966=DIRECTION('center_axis',(-0.832684316109069,-3.23656056986375E-9,
-0.553747983929488));
#55967=DIRECTION('ref_axis',(-0.553679925483015,-0.0156778481997066,0.832581975058882));
#55968=DIRECTION('',(0.832683749192755,3.88578058619072E-13,0.553748836414396));
#55969=DIRECTION('center_axis',(0.643342272241462,0.584827952253614,0.49405160359019));
#55970=DIRECTION('ref_axis',(0.60765947023258,0.00246180459506116,-0.794193872901823));
#55971=DIRECTION('center_axis',(0.796270420373333,5.05988671369472E-10,
0.604940838130867));
#55972=DIRECTION('ref_axis',(-0.604866555276953,0.0156707406197974,0.79617264346109));
#55973=DIRECTION('',(-0.796270460895025,-6.37823127617811E-11,-0.604940784793044));
#55974=DIRECTION('',(0.980355882941001,1.6426898906513E-13,-0.197236768334329));
#55975=DIRECTION('center_axis',(-0.671764980350506,-0.601098528045241,-0.432911504532425));
#55976=DIRECTION('ref_axis',(0.54605252636692,-0.00691952417752918,-0.837722363694238));
#55977=DIRECTION('',(-0.135290511400882,2.34493981894302E-11,-0.990805973702666));
#55978=DIRECTION('center_axis',(0.,-1.,1.45983193964168E-32));
#55979=DIRECTION('ref_axis',(1.,0.,0.));
#55980=DIRECTION('center_axis',(0.673608335974524,0.601098526858151,0.430037638718511));
#55981=DIRECTION('ref_axis',(0.543756144444565,-0.00897208149114492,-0.839195303330814));
#55982=DIRECTION('center_axis',(0.659016940608251,-0.601098528480747,0.452081000540414));
#55983=DIRECTION('ref_axis',(0.56072847601211,-0.0079457060119668,-0.827961618642499));
#55984=DIRECTION('center_axis',(-0.657079549965281,0.601098527488736,-0.454892322718572));
#55985=DIRECTION('ref_axis',(0.564260520362422,-0.00794578617095023,-0.825558556156045));
#55986=DIRECTION('center_axis',(0.717325884976863,0.58482795222916,0.378708121161413));
#55987=DIRECTION('ref_axis',(0.478331876830556,-0.018154631720293,-0.877991472028549));
#55988=DIRECTION('center_axis',(-0.865810784279634,4.83825714184073E-10,
-0.500371547777334));
#55989=DIRECTION('ref_axis',(-0.500310036599232,-0.015679506613961,0.865704349273133));
#55990=DIRECTION('',(0.865810813532333,2.06171882231919E-7,0.500371497160298));
#55991=DIRECTION('center_axis',(0.700193648426392,0.584827782536454,0.409518399436254));
#55992=DIRECTION('ref_axis',(0.521594165603633,-0.0273551074133822,-0.85275507885128));
#55993=DIRECTION('center_axis',(0.832683694838208,6.55764680054239E-10,
0.55374891814846));
#55994=DIRECTION('ref_axis',(-0.55368064692291,0.0157023279256327,0.83258103396651));
#55995=DIRECTION('',(0.832683748609624,-1.29267411912356E-5,0.55374883714038));
#55996=DIRECTION('',(0.966036765128944,-7.62629077549575E-8,-0.258404660211845));
#55997=DIRECTION('center_axis',(-0.8658108151466,3.96258707532583E-12,-0.500371494367116));
#55998=DIRECTION('ref_axis',(-0.386224871060518,-0.635772805085263,0.668298802399273));
#55999=DIRECTION('',(0.197236768332891,0.,0.980355882941291));
#56000=DIRECTION('center_axis',(0.820017153734806,0.398564391592048,0.410753324192914));
#56001=DIRECTION('ref_axis',(0.447863103153179,1.17847903490295E-17,-0.894102142282415));
#56002=DIRECTION('center_axis',(-0.898612168819394,5.74456518964492E-5,
-0.438743850953722));
#56003=DIRECTION('ref_axis',(0.438743841501099,0.000363080670879633,-0.898612101920114));
#56004=DIRECTION('',(0.895520512892924,5.94973684117939E-5,0.445020232627751));
#56005=DIRECTION('center_axis',(0.691408413580748,0.590180063808505,0.416703609190925));
#56006=DIRECTION('ref_axis',(0.584935624845923,-0.795821655632749,0.156582908428919));
#56007=DIRECTION('center_axis',(0.651774153940385,0.550037558024768,-0.522158153261486));
#56008=DIRECTION('ref_axis',(-0.644941563429318,0.764231888736231,-6.88734724809203E-18));
#56009=DIRECTION('center_axis',(0.279966610551229,-0.477126090010582,0.833048252628664));
#56010=DIRECTION('ref_axis',(0.958919043818676,0.0976333725527449,-0.266349379510922));
#56011=DIRECTION('center_axis',(0.350675851921805,0.584827951388939,0.731438797270922));
#56012=DIRECTION('ref_axis',(0.892964267927599,0.0265489690139539,-0.449343931136078));
#56013=DIRECTION('center_axis',(-0.517659995335373,-4.43418987557268E-11,
-0.855586424173141));
#56014=DIRECTION('ref_axis',(-0.855480328228814,-0.0157477670572569,0.517595803543877));
#56015=DIRECTION('center_axis',(0.470963347117226,-0.00011544117072539,
0.882152771545539));
#56016=DIRECTION('ref_axis',(0.0218840739070157,-0.999690707186623,-0.0118142826249362));
#56017=DIRECTION('',(-0.46291579531665,-6.06514838086686E-10,-0.886402259951064));
#56018=DIRECTION('center_axis',(-0.373302379157644,-0.601098527901457,-0.706629955117914));
#56019=DIRECTION('ref_axis',(0.873849509997278,0.0279220160657003,-0.48539406145558));
#56020=DIRECTION('',(0.299450151003895,2.24350371841883E-10,-0.954111946819525));
#56021=DIRECTION('center_axis',(0.,-1.,1.45983193964168E-32));
#56022=DIRECTION('ref_axis',(1.,0.,0.));
#56023=DIRECTION('center_axis',(0.376317811527839,0.601098530834626,0.705028695129037));
#56024=DIRECTION('ref_axis',(0.872572151713197,0.0258667898253148,-0.487799906968763));
#56025=DIRECTION('center_axis',(0.452703617578686,-0.601098525867147,0.658589399270528));
#56026=DIRECTION('ref_axis',(0.835078665382949,0.02689442413629,-0.549472758717491));
#56027=DIRECTION('center_axis',(-0.449885876190126,0.601098529134951,-0.660517415876706));
#56028=DIRECTION('ref_axis',(0.837418460426783,0.0268943527820764,-0.545900188610399));
#56029=DIRECTION('center_axis',(0.439584272309975,0.584827952222484,0.681719835296705));
#56030=DIRECTION('ref_axis',(0.841696291935165,-0.00326197145329843,-0.539941396528208));
#56031=DIRECTION('center_axis',(-0.570361291815053,-6.14013338689065E-10,
-0.82139393520957));
#56032=DIRECTION('ref_axis',(-0.821292912578248,-0.0156832196307606,0.570291143514215));
#56033=DIRECTION('',(0.570361226402489,8.32143748320893E-8,0.82139398063088));
#56034=DIRECTION('center_axis',(0.409545148242126,0.584827969931487,0.700177846791193));
#56035=DIRECTION('ref_axis',(0.860586784780955,0.00704480134808137,-0.509255099762726));
#56036=DIRECTION('center_axis',(0.517659921081644,6.52385431013528E-10,
0.855586469099264));
#56037=DIRECTION('ref_axis',(-0.855481398007026,0.015671528054159,0.517596349361538));
#56038=DIRECTION('',(-0.517659995144111,-1.36557432027408E-11,-0.855586424288861));
#56039=DIRECTION('',(0.984119547726679,-3.07809289803933E-8,0.177506945729556));
#56040=DIRECTION('center_axis',(0.49293567378062,0.793626260380211,-0.356611525822383));
#56041=DIRECTION('ref_axis',(-0.849477030544143,0.527625600760525,2.24172534152986E-16));
#56042=DIRECTION('center_axis',(-0.127978792423019,0.471546674587275,0.872505107363635));
#56043=DIRECTION('ref_axis',(0.91601707681542,0.393429494163488,-0.078268436197456));
#56044=DIRECTION('center_axis',(-0.458923008330418,-0.6010985280139,-0.654270763556253));
#56045=DIRECTION('ref_axis',(0.819662408082402,-0.00227572752435393,-0.572842349901604));
#56046=DIRECTION('',(0.238950069593058,5.19500677922368E-12,-0.971031855420548));
#56047=DIRECTION('center_axis',(0.,-1.,1.45983193964168E-32));
#56048=DIRECTION('ref_axis',(1.,0.,0.));
#56049=DIRECTION('center_axis',(0.461713950440732,0.601098527686159,0.652304214291112));
#56050=DIRECTION('ref_axis',(0.818090832306808,-0.00432803772398581,-0.575072741646667));
#56051=DIRECTION('center_axis',(0.452703595008796,-0.601098528162513,0.658589412689706));
#56052=DIRECTION('ref_axis',(0.822672862713188,-0.00330181325403135,-0.568505460822079));
#56053=DIRECTION('center_axis',(-0.449885881652066,0.60109852793641,-0.660517413247239));
#56054=DIRECTION('ref_axis',(0.825094064654831,-0.00330186518387631,-0.564985736242674));
#56055=DIRECTION('center_axis',(0.521553004954773,0.584828255987234,0.621255482085734));
#56056=DIRECTION('ref_axis',(0.780586410597556,-0.0330815410821509,-0.624171825085092));
#56057=DIRECTION('center_axis',(-0.620838200118697,-1.08043366079622E-7,
-0.783938728009636));
#56058=DIRECTION('ref_axis',(-0.783842409954205,-0.015675163531732,0.620761923450076));
#56059=DIRECTION('',(0.620811504614969,0.,0.783959868703557));
#56060=DIRECTION('center_axis',(0.494069336524158,0.584827952226326,0.643328653956391));
#56061=DIRECTION('ref_axis',(0.802782622024964,-0.022760729591192,-0.595837235294338));
#56062=DIRECTION('center_axis',(0.57036116034183,6.26445488212079E-10,0.821394026502215));
#56063=DIRECTION('ref_axis',(-0.821292872789849,0.0156933905088762,0.570290921020959));
#56064=DIRECTION('',(-0.570361227475226,-2.2482016248264E-11,-0.821393979885994));
#56065=DIRECTION('',(0.993323364090225,0.,0.115363314586913));
#56066=DIRECTION('center_axis',(-0.537306125094688,-0.601098528082298,-0.591593346373188));
#56067=DIRECTION('ref_axis',(0.756069101559276,-0.0324816851659188,-0.653685286507301));
#56068=DIRECTION('',(0.177506961533666,8.17238220606035E-12,-0.984119544876071));
#56069=DIRECTION('center_axis',(0.,-1.,1.45983193964168E-32));
#56070=DIRECTION('ref_axis',(1.,0.,0.));
#56071=DIRECTION('center_axis',(0.539828616369953,0.60109852393486,0.589292482110059));
#56072=DIRECTION('ref_axis',(0.754234908019797,-0.0345385417563714,-0.655695655512305));
#56073=DIRECTION('center_axis',(0.452703592957575,-0.601098529677169,0.658589412717247));
#56074=DIRECTION('ref_axis',(0.809084487247631,-0.0335099773181815,-0.586736204708191));
#56075=DIRECTION('center_axis',(-0.449885864064448,0.601098526155993,-0.660517426846618));
#56076=DIRECTION('ref_axis',(0.811583704649522,-0.0335100416239802,-0.583274350076974));
#56077=DIRECTION('',(0.668811722367532,4.44089209849998E-13,0.743431826076726));
#56078=DIRECTION('center_axis',(0.570803913820623,0.584827952146655,0.576332506765851));
#56079=DIRECTION('ref_axis',(0.735722795817769,-0.0526562728388038,-0.675232763308188));
#56080=DIRECTION('center_axis',(0.620811434513497,6.62050482000029E-10,
0.783959924216343));
#56081=DIRECTION('ref_axis',(-0.783862398432757,0.0157729998141104,0.620734204631991));
#56082=DIRECTION('',(-0.620811504616735,-1.75748304775537E-10,-0.783959868702159));
#56083=DIRECTION('',(0.998606989791864,-1.43735365432102E-13,0.0527643813460516));
#56084=DIRECTION('',(0.11536331462071,6.51326541667568E-11,-0.9933233640863));
#56085=DIRECTION('center_axis',(0.,-1.,1.45983193964168E-32));
#56086=DIRECTION('ref_axis',(1.,0.,0.));
#56087=DIRECTION('center_axis',(0.467997749689556,0.601098533729295,0.647810666039086));
#56088=DIRECTION('ref_axis',(0.786238475690617,0.0514849334007102,-0.61577460241262));
#56089=DIRECTION('center_axis',(-0.594885124104481,0.601098533936693,-0.533659293574426));
#56090=DIRECTION('ref_axis',(0.695722431559084,0.0525165274531211,-0.716388381096303));
#56091=DIRECTION('center_axis',(0.527540226646797,0.584827930050718,0.616179845095601));
#56092=DIRECTION('ref_axis',(0.749055400000351,0.0219594825766691,-0.662143329540727));
#56093=DIRECTION('center_axis',(-0.714174894398227,-9.94930068197513E-9,
-0.699967299387108));
#56094=DIRECTION('ref_axis',(-0.699880595778083,-0.0157391393488182,0.714086431145329));
#56095=DIRECTION('',(0.714172445802415,0.,0.699969797674583));
#56096=DIRECTION('center_axis',(0.500264854672132,0.584827952320526,0.638522780615109));
#56097=DIRECTION('ref_axis',(0.772196484316485,0.0322834330620383,-0.634563132839428));
#56098=DIRECTION('center_axis',(0.668811663491213,5.91155253666298E-10,
0.743431879043478));
#56099=DIRECTION('ref_axis',(-0.743340224857858,0.0157020800830934,0.668729208865093));
#56100=DIRECTION('',(-0.668811722367217,0.,-0.743431826077009));
#56101=DIRECTION('',(0.999949569924937,0.,-0.010042788802629));
#56102=DIRECTION('center_axis',(-0.542999537080384,-0.601098528106974,-0.586371948713543));
#56103=DIRECTION('ref_axis',(0.721517200158609,0.0232723693894611,-0.692005293836892));
#56104=DIRECTION('',(0.0527643813459379,1.43735365432659E-13,-0.99860698979187));
#56105=DIRECTION('center_axis',(0.,-1.,1.45983193964168E-32));
#56106=DIRECTION('ref_axis',(1.,0.,0.));
#56107=DIRECTION('center_axis',(0.545499660483158,0.601098530583077,0.584046810575681));
#56108=DIRECTION('ref_axis',(0.719661241409237,0.0212180706883322,-0.694001074271201));
#56109=DIRECTION('center_axis',(0.597159614763651,-0.601098526838636,0.531112940463467));
#56110=DIRECTION('ref_axis',(0.67682136303877,0.0222452406144092,-0.73581111149829));
#56111=DIRECTION('center_axis',(-0.594885168938924,0.601098529130676,-0.533659249009558));
#56112=DIRECTION('ref_axis',(0.679958650910506,0.0222451801649955,-0.732912945042855));
#56113=DIRECTION('center_axis',(0.600608822281924,0.584827953016299,0.545202079937235));
#56114=DIRECTION('ref_axis',(0.676285913318753,-0.00784645567689399,-0.736597445406872));
#56115=DIRECTION('center_axis',(-0.756714879539488,-8.8798175969817E-10,
-0.653745050523167));
#56116=DIRECTION('ref_axis',(-0.653664701966337,-0.0156778483084326,0.756621875493748));
#56117=DIRECTION('',(0.756714656869119,8.32667268468655E-13,0.653745308265727));
#56118=DIRECTION('center_axis',(0.576348241262515,0.584827952254101,0.570788026377464));
#56119=DIRECTION('ref_axis',(0.702406779961722,0.00246180457781366,-0.71177149070613));
#56120=DIRECTION('center_axis',(0.714172377412268,7.46039727085603E-10,
0.699969867452385));
#56121=DIRECTION('ref_axis',(-0.699883915644385,0.0156707406188272,0.71408468161048));
#56122=DIRECTION('',(-0.714172445803038,-6.33937347031602E-11,-0.699969797673947));
#56123=DIRECTION('',(0.99734580593901,1.64268989065177E-13,-0.0728103246515634));
#56124=DIRECTION('center_axis',(-0.612209711118165,-0.60109852808043,-0.513692348738184));
#56125=DIRECTION('ref_axis',(0.646741194614692,-0.00691952138882007,-0.762678141428028));
#56126=DIRECTION('',(-0.0100427887902123,2.36136671784991E-11,-0.999949569925061));
#56127=DIRECTION('center_axis',(0.,-1.,1.45983193964168E-32));
#56128=DIRECTION('ref_axis',(1.,0.,0.));
#56129=DIRECTION('center_axis',(0.614398716792201,0.601098526967397,0.511072184414025));
#56130=DIRECTION('ref_axis',(0.644647533842544,-0.0089720736175879,-0.764427275158158));
#56131=DIRECTION('center_axis',(0.597159621283849,-0.601098528479525,0.531112931275336));
#56132=DIRECTION('ref_axis',(0.660078071675325,-0.00794570627140616,-0.751154980709862));
#56133=DIRECTION('center_axis',(-0.594885156756865,0.601098527501109,-0.533659264424743));
#56134=DIRECTION('ref_axis',(0.663281080036902,-0.00794578523321746,-0.748328185599145));
#56135=DIRECTION('center_axis',(0.66420484270576,0.584827952229765,0.465626667209855));
#56136=DIRECTION('ref_axis',(0.584601597354615,-0.0181546317097263,-0.811117366179467));
#56137=DIRECTION('center_axis',(-0.796270496767386,-4.64388117108289E-10,
-0.60494073757503));
#56138=DIRECTION('ref_axis',(-0.604866371587384,-0.0156795066172821,0.796172610427508));
#56139=DIRECTION('',(0.796270458939758,2.0617116058701E-7,0.604940787366685));
#56140=DIRECTION('center_axis',(0.64334614715523,0.584827782537056,0.494046758630508));
#56141=DIRECTION('ref_axis',(0.624359791296606,-0.0273551074042075,-0.780657766957431));
#56142=DIRECTION('center_axis',(0.756714577676916,8.3606101144566E-10,0.653745399931233));
#56143=DIRECTION('ref_axis',(-0.653664800225672,0.0157023279260372,0.756621282970308));
#56144=DIRECTION('',(0.756714656200049,-1.29267412622836E-5,0.653745308912378));
#56145=DIRECTION('',(0.990805968327137,-7.62630514903484E-8,-0.135290550768773));
#56146=DIRECTION('center_axis',(-0.796270460895142,-8.75589444335316E-13,
-0.604940784792891));
#56147=DIRECTION('ref_axis',(-0.466939422478211,-0.635772805085266,0.614622254762815));
#56148=DIRECTION('',(0.0728103246501242,-3.74249790574711E-13,0.997345805939115));
#56149=DIRECTION('center_axis',(0.762070031231707,0.398564391593391,0.510289813000706));
#56150=DIRECTION('ref_axis',(0.556392281443257,2.67730606825651E-16,-0.830919748923064));
#56151=DIRECTION('center_axis',(-0.836537157930299,5.74456560985943E-5,
-0.547910193464124));
#56152=DIRECTION('ref_axis',(0.547910175674295,0.000363259836001831,-0.836537092683196));
#56153=DIRECTION('',(0.832683241412888,5.94973691578637E-5,0.553749596776548));
#56154=DIRECTION('center_axis',(0.63372964100381,0.59018006381091,0.500074228883405));
#56155=DIRECTION('ref_axis',(0.560701812787564,-0.795820734737636,0.228654401441101));
#56156=DIRECTION('center_axis',(0.712078489846112,0.550037558019866,-0.43635181799326));
#56157=DIRECTION('ref_axis',(-0.611304898368902,0.791395173873449,5.31197026603917E-16));
#56158=DIRECTION('center_axis',(0.173350359018707,-0.477126089715379,0.861568539084963));
#56159=DIRECTION('ref_axis',(0.984740254929913,0.0976251248572319,-0.144069307339142));
#56160=DIRECTION('center_axis',(0.256237078464303,0.584827951388878,0.769622522340898));
#56161=DIRECTION('ref_axis',(0.942240705833203,0.0265489690180492,-0.333882620864018));
#56162=DIRECTION('center_axis',(-0.406344674439861,1.212629090089E-11,-0.913719872583695));
#56163=DIRECTION('ref_axis',(-0.913606567872938,-0.0157477670558653,0.406294286167287));
#56164=DIRECTION('center_axis',(0.356686603111286,-0.000115441196879581,
0.934224091872107));
#56165=DIRECTION('ref_axis',(0.023208648645243,-0.999690269928019,-0.0089845889892695));
#56166=DIRECTION('',(-0.348169904526061,-6.0695892729679E-10,-0.937431446870817));
#56167=DIRECTION('center_axis',(-0.281794560966275,-0.601098527898774,-0.74784516122507));
#56168=DIRECTION('ref_axis',(0.927794952947662,0.0279220162086369,-0.372044199384548));
#56169=DIRECTION('',(0.416670832599042,2.24206636476383E-10,-0.909057433422785));
#56170=DIRECTION('center_axis',(0.,-1.,1.45983193964168E-32));
#56171=DIRECTION('ref_axis',(1.,0.,0.));
#56172=DIRECTION('center_axis',(0.284986911706633,0.60109853096743,0.746634459574907));
#56173=DIRECTION('ref_axis',(0.926829197919476,0.0258667868113062,-0.374591173446464));
#56174=DIRECTION('center_axis',(0.366590771873736,-0.601098525971635,0.710135035082587));
#56175=DIRECTION('ref_axis',(0.89736101970089,0.0268944218182806,-0.440476889741606));
#56176=DIRECTION('center_axis',(-0.363553605776339,0.601098529201857,-0.711694691506397));
#56177=DIRECTION('ref_axis',(0.899234602532466,0.0268943512091051,-0.436639237221438));
#56178=DIRECTION('center_axis',(0.350675867701933,0.58482795222295,0.731438789038568));
#56179=DIRECTION('ref_axis',(0.90273186642539,-0.00326197146607218,-0.430191279412179));
#56180=DIRECTION('center_axis',(-0.462915866366431,-6.27932174290943E-10,
-0.886402222845936));
#56181=DIRECTION('ref_axis',(-0.886293204894859,-0.0156832196313113,0.462858932698934));
#56182=DIRECTION('',(0.462915794151349,8.32143748321858E-8,0.886402260559628));
#56183=DIRECTION('center_axis',(0.318560208828588,0.584827969931739,0.745986353049844));
#56184=DIRECTION('ref_axis',(0.917627389295675,0.00704480133904469,-0.397379346706013));
#56185=DIRECTION('center_axis',(0.406344605395894,5.99603447787589E-10,
0.91371990328856));
#56186=DIRECTION('ref_axis',(-0.913607693064028,0.015671528053928,0.406294703857532));
#56187=DIRECTION('',(-0.406344678315143,-1.44328993199831E-11,-0.9137198708603));
#56188=DIRECTION('',(0.954111951662165,-3.07809289804025E-8,0.29945013557421));
#56189=DIRECTION('center_axis',(0.533744004419719,0.793626260379228,-0.292018315491485));
#56190=DIRECTION('ref_axis',(-0.829794751143426,0.558068697361553,1.37353446782025E-17));
#56191=DIRECTION('center_axis',(-0.236323527865057,0.471546674606097,0.849585148084255));
#56192=DIRECTION('ref_axis',(0.918611650451755,0.393409545157626,0.0371694152923138));
#56193=DIRECTION('center_axis',(-0.373302383231254,-0.601098528046985,-0.70662995284209));
#56194=DIRECTION('ref_axis',(0.884995313294357,-0.00227572095771443,-0.465594369103779));
#56195=DIRECTION('',(0.358768439256913,5.19500677922131E-12,-0.933426594324995));
#56196=DIRECTION('center_axis',(0.,-1.,1.45983193964168E-32));
#56197=DIRECTION('ref_axis',(1.,0.,0.));
#56198=DIRECTION('center_axis',(0.376317791083764,0.60109852773164,0.705028708686882));
#56199=DIRECTION('ref_axis',(0.883715672465122,-0.00432803058542384,-0.468004143561539));
#56200=DIRECTION('center_axis',(0.366590750308916,-0.601098528165542,0.710135044357878));
#56201=DIRECTION('ref_axis',(0.887438469564525,-0.00330181390545426,-0.460914374653153));
#56202=DIRECTION('center_axis',(-0.363553611789512,0.601098527926897,-0.711694689511534));
#56203=DIRECTION('ref_axis',(0.889399441604279,-0.0033018665924906,-0.457118946173752));
#56204=DIRECTION('center_axis',(0.439576445276083,0.584828255987649,0.681724621644904));
#56205=DIRECTION('ref_axis',(0.852660726745465,-0.033081541071735,-0.521416624884761));
#56206=DIRECTION('center_axis',(-0.517689160600361,-1.08326166762735E-7,
-0.855568777478984));
#56207=DIRECTION('ref_axis',(-0.855463658918661,-0.0156751635317574,0.517625557249398));
#56208=DIRECTION('',(0.517659995144627,1.16573417585677E-12,0.855586424288549));
#56209=DIRECTION('center_axis',(0.409542991805253,0.584827952225948,0.700179122909564));
#56210=DIRECTION('ref_axis',(0.871130648640799,-0.0227607296020412,-0.490523538871116));
#56211=DIRECTION('center_axis',(0.462915725331666,6.03583660258034E-10,
0.886402296500104));
#56212=DIRECTION('ref_axis',(-0.886293137093757,0.0156933905088725,0.462858717790691));
#56213=DIRECTION('',(-0.462915795308633,-2.16493489798453E-11,-0.886402259955251));
#56214=DIRECTION('',(0.971031855421239,0.,0.238950069590253));
#56215=DIRECTION('center_axis',(-0.458923003741332,-0.601098527885463,-0.65427076689316));
#56216=DIRECTION('ref_axis',(0.832035758807123,-0.0324816887614031,-0.553770201402587));
#56217=DIRECTION('',(0.299450150896321,8.17238220605966E-12,-0.954111946853288));
#56218=DIRECTION('center_axis',(0.,-1.,1.45983193964168E-32));
#56219=DIRECTION('ref_axis',(1.,0.,0.));
#56220=DIRECTION('center_axis',(0.461713957455863,0.601098524618822,0.652304212152214));
#56221=DIRECTION('ref_axis',(0.830468006537055,-0.0345385296351385,-0.555994586384627));
#56222=DIRECTION('center_axis',(0.366590743436293,-0.601098529457339,0.71013504681226));
#56223=DIRECTION('ref_axis',(0.876242162608083,-0.0335099812939027,-0.48070443478461));
#56224=DIRECTION('center_axis',(-0.363553589130721,0.601098525939916,-0.711694702764487));
#56225=DIRECTION('ref_axis',(0.878287787393539,-0.0335100454515292,-0.476956643070623));
#56226=DIRECTION('',(0.570361227475854,8.32667268470211E-13,0.821393979885559));
#56227=DIRECTION('center_axis',(0.494069337780756,0.584827952146981,0.643328653063466));
#56228=DIRECTION('ref_axis',(0.814550507461375,-0.0526562728332638,-0.57769783427474));
#56229=DIRECTION('center_axis',(0.517659905315428,7.85228749101234E-10,
0.855586478638379));
#56230=DIRECTION('ref_axis',(-0.855480042403958,0.0157729998136923,0.517595507636417));
#56231=DIRECTION('',(-0.51765999514652,-1.76914038951223E-10,-0.855586424287404));
#56232=DIRECTION('',(0.984119544876793,-1.43735365432129E-13,0.177506961529667));
#56233=DIRECTION('',(0.23895006962348,6.51326541667397E-11,-0.971031855413062));
#56234=DIRECTION('center_axis',(0.,-1.,1.45983193964168E-32));
#56235=DIRECTION('ref_axis',(1.,0.,0.));
#56236=DIRECTION('center_axis',(0.383115227651307,0.601098532850742,0.701358165380836));
#56237=DIRECTION('ref_axis',(0.857215779016419,0.0514849435566238,-0.512377213381163));
#56238=DIRECTION('center_axis',(-0.523309027811023,0.601098534236298,-0.604010110470393));
#56239=DIRECTION('ref_axis',(0.780023727708288,0.0525165239653635,-0.62354229922489));
#56240=DIRECTION('center_axis',(0.446152601933338,0.584827930050342,0.677439405423942));
#56241=DIRECTION('ref_axis',(0.826137439021757,0.0219594825869006,-0.563040596201631));
#56242=DIRECTION('center_axis',(-0.620814224972045,-9.72756495102324E-9,
-0.783957714467023));
#56243=DIRECTION('ref_axis',(-0.783860607156331,-0.0157391393478925,0.620737326122004));
#56244=DIRECTION('',(0.620811504615245,1.165734175857E-12,0.783959868703339));
#56245=DIRECTION('center_axis',(0.416291992044271,0.584827952319077,0.696187649665008));
#56246=DIRECTION('ref_axis',(0.845639333746944,0.0322834330816786,-0.532777530652791));
#56247=DIRECTION('center_axis',(0.570361160563746,6.0878364447281E-10,0.82139402634812));
#56248=DIRECTION('ref_axis',(-0.82129276057823,0.0157020800819259,0.570290843432447));
#56249=DIRECTION('',(-0.57036122747518,-8.3266726846866E-13,-0.821393979886027));
#56250=DIRECTION('',(0.993323364090257,-1.64268989065282E-13,0.115363314586632));
#56251=DIRECTION('center_axis',(-0.465225930454903,-0.601098528085867,-0.649804119073874));
#56252=DIRECTION('ref_axis',(0.802559083046984,0.0232723699029421,-0.596118541078773));
#56253=DIRECTION('',(0.177506961529538,0.,-0.984119544876816));
#56254=DIRECTION('center_axis',(0.,-1.,1.45983193964168E-32));
#56255=DIRECTION('ref_axis',(1.,0.,0.));
#56256=DIRECTION('center_axis',(0.467997751365031,0.601098530417989,0.647810667901207));
#56257=DIRECTION('ref_axis',(0.800967899836253,0.0212180752187776,-0.598331193166387));
#56258=DIRECTION('center_axis',(0.52588472722959,-0.601098526940685,0.601768904627348));
#56259=DIRECTION('ref_axis',(0.763706012663099,0.0222452379388547,-0.645180808464786));
#56260=DIRECTION('center_axis',(-0.523309087003531,0.60109852899713,-0.604010064400435));
#56261=DIRECTION('ref_axis',(0.766455320034414,0.0222451837789128,-0.641912294779891));
#56262=DIRECTION('center_axis',(0.527540769866512,0.584827954381971,0.616179356926251));
#56263=DIRECTION('ref_axis',(0.763273428376044,-0.00784635390595337,-0.646027946969373));
#56264=DIRECTION('center_axis',(-0.66881247587959,-3.15689300772054E-9,
-0.743431148195859));
#56265=DIRECTION('ref_axis',(-0.743339776746405,-0.0156778481997067,0.668730275509066));
#56266=DIRECTION('',(0.668811722367582,4.44089209850169E-13,0.743431826076681));
#56267=DIRECTION('center_axis',(0.500264854202378,0.584827952253931,0.638522781044144));
#56268=DIRECTION('ref_axis',(0.786076715195562,0.00246180458149666,-0.618124046891526));
#56269=DIRECTION('center_axis',(0.620811458452108,4.4207282963584E-10,0.783959905259552));
#56270=DIRECTION('ref_axis',(-0.783863640008822,0.0156707406190849,0.620735226775933));
#56271=DIRECTION('',(-0.62081150461559,-6.42264019716283E-11,-0.783959868703066));
#56272=DIRECTION('',(0.998606989791871,1.64268989065234E-13,0.0527643813459203));
#56273=DIRECTION('center_axis',(-0.542999538349175,-0.601098528013067,-0.586371947634867));
#56274=DIRECTION('ref_axis',(0.737230359758982,-0.00691952691788106,-0.675606036678829));
#56275=DIRECTION('',(0.11536331459892,2.34493981894245E-11,-0.99332336408883));
#56276=DIRECTION('center_axis',(0.,-1.,1.45983193964168E-32));
#56277=DIRECTION('ref_axis',(1.,0.,0.));
#56278=DIRECTION('center_axis',(0.545499656932936,0.601098527119734,0.584046817456046));
#56279=DIRECTION('ref_axis',(0.735372447364012,-0.00897206298346596,-0.677603767509954));
#56280=DIRECTION('center_axis',(0.525884739928065,-0.601098528496697,0.601768891975896));
#56281=DIRECTION('ref_axis',(0.749017840375685,-0.00794570493064833,-0.662502181560257));
#56282=DIRECTION('center_axis',(-0.523309064580667,0.601098527455218,-0.604010085361889));
#56283=DIRECTION('ref_axis',(0.751841304520338,-0.00794578827969788,-0.659296228766531));
#56284=DIRECTION('center_axis',(0.600608893325141,0.584827952228797,0.545202002518902));
#56285=DIRECTION('ref_axis',(0.681651801426565,-0.0181546317332704,-0.731451454956888));
#56286=DIRECTION('center_axis',(-0.714172423332152,2.70738924708545E-10,
-0.699969820600775));
#56287=DIRECTION('ref_axis',(-0.699883772599899,-0.0156795066139273,0.714084629384835));
#56288=DIRECTION('',(0.714172443541394,2.06172326321031E-7,0.699969799981451));
#56289=DIRECTION('center_axis',(0.576352692844794,0.584827782536587,0.570783705289397));
#56290=DIRECTION('ref_axis',(0.71727889008742,-0.0273551074114228,-0.696249015750449));
#56291=DIRECTION('center_axis',(0.668811635346391,8.0403432168573E-10,0.743431904363329));
#56292=DIRECTION('ref_axis',(-0.743340247283272,0.0157023279256694,0.668729178118137));
#56293=DIRECTION('',(0.668811721622696,-1.29267412267558E-5,0.743431826634416));
#56294=DIRECTION('',(0.999949569526026,-7.62630514903833E-8,-0.0100428285213587));
#56295=DIRECTION('center_axis',(-0.714172446213903,-4.77179581778534E-10,
-0.699969797254746));
#56296=DIRECTION('ref_axis',(-0.540290059736212,-0.635772805082231,0.551252747537926));
#56297=DIRECTION('',(-0.0527643813476595,0.,0.998606989791779));
#56298=DIRECTION('center_axis',(0.692104609098264,0.398564391591702,0.601778726626387));
#56299=DIRECTION('ref_axis',(0.65614682108291,-1.14922775163484E-16,-0.754633254755442));
#56300=DIRECTION('center_axis',(-0.761269456311017,5.7445664986067E-5,-0.648435664956766));
#56301=DIRECTION('ref_axis',(0.648435639191338,0.000362937741181404,-0.761269393909093));
#56302=DIRECTION('',(0.75671405779511,5.94973691933618E-5,0.653745998989915));
#56303=DIRECTION('center_axis',(0.566056573281352,0.590180063806646,0.575558379428322));
#56304=DIRECTION('ref_axis',(0.527619938303713,-0.795821286109522,0.297129065019519));
#56305=DIRECTION('center_axis',(0.761152922591209,0.550037558015138,-0.343663953890433));
#56306=DIRECTION('ref_axis',(-0.585711678816273,0.810519481134305,-4.28907078704251E-17));
#56307=DIRECTION('center_axis',(0.0640002686815192,-0.477126090766273,0.876501374282316));
#56308=DIRECTION('ref_axis',(0.995031674671247,0.0976283473316997,-0.0195108225919653));
#56309=DIRECTION('center_axis',(0.157757293231697,0.584827951389322,0.795668840476977));
#56310=DIRECTION('ref_axis',(0.976657444935551,0.026548969009499,-0.213155782226273));
#56311=DIRECTION('center_axis',(-0.288621061342871,-1.43925814653302E-11,
-0.957443409789485));
#56312=DIRECTION('ref_axis',(-0.95732468319503,-0.0157477670566732,0.288585271242773));
#56313=DIRECTION('center_axis',(0.236784694176708,-0.000115441177377208,
0.971562141747494));
#56314=DIRECTION('ref_axis',(0.0241396323370541,-0.999690579295746,-0.00600198450246929));
#56315=DIRECTION('',(-0.227933166354412,-6.07014438448248E-10,-0.973676779879058));
#56316=DIRECTION('center_axis',(-0.185842674628182,-0.601098527904035,-0.77726640223198));
#56317=DIRECTION('ref_axis',(0.967108515123235,0.0279220160808943,-0.252826978374757));
#56318=DIRECTION('',(0.527320366257025,2.24206636476405E-10,-0.849666541256367));
#56319=DIRECTION('center_axis',(0.,-1.,1.45983193964168E-32));
#56320=DIRECTION('ref_axis',(1.,0.,0.));
#56321=DIRECTION('center_axis',(0.189161578622374,0.601098530555737,0.776465359006327));
#56322=DIRECTION('ref_axis',(0.966469598843853,0.0258667961724589,-0.255474897722603));
#56323=DIRECTION('center_axis',(0.274696560809731,-0.601098526354879,0.750481419552342));
#56324=DIRECTION('ref_axis',(0.945491456743476,0.0268944134769082,-0.32453442921951));
#56325=DIRECTION('center_axis',(-0.271487881944521,0.601098529144406,-0.751648114623931));
#56326=DIRECTION('ref_axis',(0.946869276050077,0.0268943524351229,-0.320492227486875));
#56327=DIRECTION('center_axis',(0.256237095127745,0.584827952222611,0.76962251615945));
#56328=DIRECTION('ref_axis',(0.949530820133915,-0.0032619714466773,-0.313656788796442));
#56329=DIRECTION('center_axis',(-0.348169975729648,-5.95365837681765E-10,
-0.937431420425205));
#56330=DIRECTION('ref_axis',(-0.937316126432585,-0.0156832196313476,0.348127154573454));
#56331=DIRECTION('',(0.34816990329345,8.32135976760844E-8,0.937431447328615));
#56332=DIRECTION('center_axis',(0.22255138460994,0.584827969931679,0.780030208898213));
#56333=DIRECTION('ref_axis',(0.96019646172339,0.00704480133933188,-0.2792366839582));
#56334=DIRECTION('center_axis',(0.288620987568787,5.92193446020471E-10,
0.957443432028659));
#56335=DIRECTION('ref_axis',(-0.957325852294089,0.0156715280544834,0.28858554318925));
#56336=DIRECTION('',(-0.288621063170319,-1.48214773785991E-11,-0.957443409238601));
#56337=DIRECTION('',(0.909057440161087,-3.07809289804079E-8,0.41667081789798));
#56338=DIRECTION('center_axis',(0.566134873267341,0.793626260377381,-0.222819801880318));
#56339=DIRECTION('ref_axis',(-0.814092839849893,0.580734748491199,1.14572618823004E-16));
#56340=DIRECTION('center_axis',(-0.340941299947114,0.471546674547623,0.813266723598999));
#56341=DIRECTION('ref_axis',(0.906703761223004,0.393427978814542,0.151995772539772));
#56342=DIRECTION('center_axis',(-0.2817945677677,-0.601098528040889,-0.747845158548006));
#56343=DIRECTION('ref_axis',(0.936371308045141,-0.00227572240193344,-0.351003695931227));
#56344=DIRECTION('',(0.472928816316381,5.05127141379E-12,-0.881100638234695));
#56345=DIRECTION('center_axis',(0.,-1.,1.45983193964168E-32));
#56346=DIRECTION('ref_axis',(1.,0.,0.));
#56347=DIRECTION('center_axis',(0.284986893316741,0.601098527699123,0.746634469225483));
#56348=DIRECTION('ref_axis',(0.935403780561703,-0.00432803588139098,-0.353554854889991));
#56349=DIRECTION('center_axis',(0.274696550152684,-0.601098528163608,0.750481422004408));
#56350=DIRECTION('ref_axis',(0.938208641494535,-0.00330181468705492,-0.346054393188053));
#56351=DIRECTION('center_axis',(-0.27148789264536,0.60109852795299,-0.751648111711677));
#56352=DIRECTION('ref_axis',(0.939678455149161,-0.0033018624838774,-0.342043123937061));
#56353=DIRECTION('center_axis',(0.350667502483558,0.584828255987638,0.731442556664843));
#56354=DIRECTION('ref_axis',(0.911288073866872,-0.0330815410750519,-0.41043837304534));
#56355=DIRECTION('center_axis',(-0.406375812556749,-1.08214501188567E-7,
-0.913706024369343));
#56356=DIRECTION('ref_axis',(-0.913593763086638,-0.0156751635309797,0.406325885586278));
#56357=DIRECTION('',(0.406344678315595,3.88578058618905E-13,0.913719870860099));
#56358=DIRECTION('center_axis',(0.318557909444986,0.584827952226065,0.745987348837169));
#56359=DIRECTION('ref_axis',(0.925740424547197,-0.0227607296041559,-0.377473993206236));
#56360=DIRECTION('center_axis',(0.348169826705523,6.35249530183533E-10,
0.937431475774014));
#56361=DIRECTION('ref_axis',(-0.93731603218275,0.0156933905083093,0.348126949987413));
#56362=DIRECTION('',(-0.348169904517709,-2.28705943069384E-11,-0.937431446873919));
#56363=DIRECTION('',(0.933426594325848,0.,0.358768439254693));
#56364=DIRECTION('center_axis',(-0.373302380556704,-0.601098528158341,-0.70662995416029));
#56365=DIRECTION('ref_axis',(0.894880721407181,-0.0324816838077035,-0.445121820034447));
#56366=DIRECTION('',(0.416670832496624,8.17238220605976E-12,-0.909057433469729));
#56367=DIRECTION('center_axis',(0.,-1.,1.45983193964168E-32));
#56368=DIRECTION('ref_axis',(1.,0.,0.));
#56369=DIRECTION('center_axis',(0.376317810921175,0.601098524538565,0.705028700820793));
#56370=DIRECTION('ref_axis',(0.89360411672998,-0.034538531061908,-0.447525164024682));
#56371=DIRECTION('center_axis',(0.274696540277618,-0.601098529320043,0.750481424692703));
#56372=DIRECTION('ref_axis',(0.929580973804702,-0.0335099838657365,-0.367091669915867));
#56373=DIRECTION('center_axis',(-0.271487875923072,0.601098526440157,-0.751648118961426));
#56374=DIRECTION('ref_axis',(0.931140740168084,-0.0335100365203316,-0.363117060259688));
#56375=DIRECTION('',(0.462915795308873,1.22124532708699E-12,0.886402259955125));
#56376=DIRECTION('center_axis',(0.409542993165234,0.58482795214625,0.700179122180664));
#56377=DIRECTION('ref_axis',(0.880532271000263,-0.0526562728447166,-0.471052265313756));
#56378=DIRECTION('center_axis',(0.406344580513227,8.00067216176833E-10,
0.913719914354246));
#56379=DIRECTION('ref_axis',(-0.913606246231954,0.0157729998148722,0.406294030626588));
#56380=DIRECTION('',(-0.406344678317571,-1.75692793624627E-10,-0.91371987085922));
#56381=DIRECTION('',(0.954111946854583,0.,0.299450150892195));
#56382=DIRECTION('',(0.3587684392876,6.73708191429265E-11,-0.9334265943132));
#56383=DIRECTION('center_axis',(0.,-1.,1.45983193964168E-32));
#56384=DIRECTION('ref_axis',(1.,0.,0.));
#56385=DIRECTION('center_axis',(0.292190758314825,0.601098532593968,0.743844819077733));
#56386=DIRECTION('ref_axis',(0.914674270984079,0.051484946561636,-0.400899336838176));
#56387=DIRECTION('center_axis',(-0.443480041513362,0.601098534115099,-0.664835321763206));
#56388=DIRECTION('ref_axis',(0.852023579248202,0.052516525333457,-0.520862587418202));
#56389=DIRECTION('center_axis',(0.357728884211842,0.584827930051393,0.728015341618811));
#56390=DIRECTION('ref_axis',(0.890190797097705,0.0219594825673074,-0.455058376351791));
#56391=DIRECTION('center_axis',(-0.517662994394784,-1.00068004579382E-8,
-0.855584609629127));
#56392=DIRECTION('ref_axis',(-0.855478630057052,-0.0157391393477768,0.517598872688398));
#56393=DIRECTION('',(0.517659995144392,0.,0.855586424288691));
#56394=DIRECTION('center_axis',(0.325753956081705,0.584827952320803,0.742873223559293));
#56395=DIRECTION('ref_axis',(0.905745945694596,0.0322834330587411,-0.422589708591849));
#56396=DIRECTION('center_axis',(0.462915721400744,6.23428967396594E-10,
0.886402298552993));
#56397=DIRECTION('ref_axis',(-0.886293018220489,0.0157020800827689,0.462858650707417));
#56398=DIRECTION('',(-0.462915795308241,-1.60982338570617E-12,-0.886402259955456));
#56399=DIRECTION('',(0.971031855421229,0.,0.238950069590293));
#56400=DIRECTION('center_axis',(-0.380115429407096,-0.601098527976857,-0.702988492075592));
#56401=DIRECTION('ref_axis',(0.870944131140459,0.0232723727996506,-0.490830639932213));
#56402=DIRECTION('',(0.299450150892508,0.,-0.954111946854484));
#56403=DIRECTION('center_axis',(0.,-1.,1.45983193964168E-32));
#56404=DIRECTION('ref_axis',(1.,0.,0.));
#56405=DIRECTION('center_axis',(0.38311523762894,0.601098530269338,0.701358162142969));
#56406=DIRECTION('ref_axis',(0.869642814507809,0.0212180793202286,-0.493225271336432));
#56407=DIRECTION('center_axis',(0.446316331932025,-0.601098526794362,0.662934606832672));
#56408=DIRECTION('ref_axis',(0.83854655666011,0.022245241894255,-0.54437562539715));
#56409=DIRECTION('center_axis',(-0.443480105976362,0.601098528947103,-0.664835283435547));
#56410=DIRECTION('ref_axis',(0.840864533470763,0.0222451851397701,-0.540788302470655));
#56411=DIRECTION('center_axis',(0.446153347929533,0.584827953016334,0.677438894293791));
#56412=DIRECTION('ref_axis',(0.838223483341985,-0.00784645566550682,-0.545270414663695));
#56413=DIRECTION('center_axis',(-0.570361573111646,-1.51695271097795E-9,
-0.821393739882164));
#56414=DIRECTION('ref_axis',(-0.821292786457333,-0.0156778483100648,0.570291472832548));
#56415=DIRECTION('',(0.570361227475778,0.,0.821393979885611));
#56416=DIRECTION('center_axis',(0.416291991554971,0.584827952254014,0.696187650012245));
#56417=DIRECTION('ref_axis',(0.85734975104592,0.00246180457996112,-0.514728417614288));
#56418=DIRECTION('center_axis',(0.517659917881015,6.88305756872033E-10,
0.855586471035758));
#56419=DIRECTION('ref_axis',(-0.855481410502806,0.0156707406191949,0.517596352549529));
#56420=DIRECTION('',(-0.517659995144781,-6.46149800302453E-11,-0.855586424288456));
#56421=DIRECTION('',(0.984119544876784,1.64268989065259E-13,0.177506961529715));
#56422=DIRECTION('center_axis',(-0.465225922666287,-0.601098528102663,-0.649804124634581));
#56423=DIRECTION('ref_axis',(0.816092972990407,-0.00691951965448234,-0.577879208557835));
#56424=DIRECTION('',(0.238950069602214,2.34493981894305E-11,-0.971031855418295));
#56425=DIRECTION('center_axis',(0.,-1.,1.45983193964168E-32));
#56426=DIRECTION('ref_axis',(1.,0.,0.));
#56427=DIRECTION('center_axis',(0.467997750909437,0.601098527138387,0.64781067127346));
#56428=DIRECTION('ref_axis',(0.814500088444679,-0.00897206142817162,-0.580094051027365));
#56429=DIRECTION('center_axis',(0.446316335307023,-0.601098528453655,0.662934603055958));
#56430=DIRECTION('ref_axis',(0.826145154494294,-0.00794570877144874,-0.563401321810411));
#56431=DIRECTION('center_axis',(-0.44348009084144,0.601098527573114,-0.664835294773602));
#56432=DIRECTION('ref_axis',(0.828544533267035,-0.00794577982429505,-0.559866788599122));
#56433=DIRECTION('center_axis',(0.527540982864664,0.584827952229474,0.616179176611206));
#56434=DIRECTION('ref_axis',(0.767951949432859,-0.018154631716425,-0.640250117305349));
#56435=DIRECTION('center_axis',(-0.620811438041664,6.65490569819036E-10,
-0.783959921422417));
#56436=DIRECTION('ref_axis',(-0.783863548436222,-0.0156795066150567,0.620735121050262));
#56437=DIRECTION('',(0.620811502081951,2.06171105075976E-7,0.783959870709407));
#56438=DIRECTION('center_axis',(0.500269812260683,0.584827782536768,0.638519051958349));
#56439=DIRECTION('ref_axis',(0.798886072310224,-0.0273551074093783,-0.600860001637124));
#56440=DIRECTION('center_axis',(0.570361134901209,7.69554369147915E-10,
0.821394044167722));
#56441=DIRECTION('ref_axis',(-0.821292775200073,0.0157023279251403,0.57029081555106));
#56442=DIRECTION('',(0.570361226666348,-1.29267404451664E-5,0.821393980345947));
#56443=DIRECTION('',(0.993323368672551,-7.62630514903932E-8,0.115363275131251));
#56444=DIRECTION('center_axis',(-0.620811504599348,1.56670257677117E-11,
-0.783959868715927));
#56445=DIRECTION('ref_axis',(-0.605120001082122,-0.63577280508502,0.479189654108577));
#56446=DIRECTION('',(-0.177506961531102,0.,0.984119544876534));
#56447=DIRECTION('center_axis',(0.611224283835664,0.398564391591621,0.683777230247381));
#56448=DIRECTION('ref_axis',(0.745553533390733,2.85036533746566E-16,-0.666445743364449));
#56449=DIRECTION('center_axis',(-0.673996080620018,5.7445664793789E-5,-0.738734918633775));
#56450=DIRECTION('ref_axis',(0.738734885246909,0.000362953305560281,-0.673996021934948));
#56451=DIRECTION('',(0.668811041446531,5.94973700105111E-5,0.74343243627062));
#56452=DIRECTION('center_axis',(0.489456455373912,0.590180063808601,0.641965630369478));
#56453=DIRECTION('ref_axis',(0.486218742096034,-0.795821400074055,0.360914995558124));
#56454=DIRECTION('center_axis',(0.798223519056493,0.550037558009713,-0.245556303938181));
#56455=DIRECTION('ref_axis',(-0.567410340608164,0.823435185895604,7.65040472392408E-17));
#56456=DIRECTION('center_axis',(-0.046359144049487,-0.477126089681845,0.87761126035843));
#56457=DIRECTION('ref_axis',(0.989631716015808,0.0976231510478723,0.105350780894548));
#56458=DIRECTION('center_axis',(0.0567895812678342,0.584827951390709,0.809166985690575));
#56459=DIRECTION('ref_axis',(0.995671712706078,0.0265489689879054,-0.0890673495879593));
#56460=DIRECTION('center_axis',(-0.166345718370956,-5.79615458256036E-12,
-0.986067493622851));
#56461=DIRECTION('ref_axis',(-0.985945217534087,-0.0157477670560628,0.166325090874496));
#56462=DIRECTION('center_axis',(0.113148551236963,-0.000115441160388845,
0.993578075455731));
#56463=DIRECTION('ref_axis',(0.0247034058069071,-0.999690532374862,-0.00292937222011708));
#56464=DIRECTION('',(-0.10410178598878,-6.0812466147161E-10,-0.99456664842229));
#56465=DIRECTION('center_axis',(-0.0869599381853343,-0.601098527906027,
-0.794429687826437));
#56466=DIRECTION('ref_axis',(0.991170198344495,0.0279220160276409,-0.129622524796762));
#56467=DIRECTION('',(0.629653742733083,2.24062901110922E-10,-0.776875900168245));
#56468=DIRECTION('center_axis',(0.,-1.,1.45983193964168E-32));
#56469=DIRECTION('ref_axis',(1.,0.,0.));
#56470=DIRECTION('center_axis',(0.0903530626196487,0.601098530391009,0.794050930883542));
#56471=DIRECTION('ref_axis',(0.990868192983961,0.0258667999664512,-0.132329636862627));
#56472=DIRECTION('center_axis',(0.178470234888878,-0.601098526314079,0.778992257292556));
#56473=DIRECTION('ref_axis',(0.978710923336046,0.0268944144261749,-0.203473877968101));
#56474=DIRECTION('center_axis',(-0.175140634157931,0.60109852903841,-0.779747598043506));
#56475=DIRECTION('ref_axis',(0.979571255487549,0.02689435486768,-0.199290865567886));
#56476=DIRECTION('center_axis',(0.157757310542433,0.584827952222822,0.795668836432142));
#56477=DIRECTION('ref_axis',(0.981355105572388,-0.00326197145772807,-0.192175743290398));
#56478=DIRECTION('center_axis',(-0.227933249196464,-6.67224254800419E-10,
-0.973676760486119));
#56479=DIRECTION('ref_axis',(-0.973557008707097,-0.0156832196312757,0.227905215866787));
#56480=DIRECTION('',(0.227933165074045,8.32139862540016E-8,0.973676780178783));
#56481=DIRECTION('center_axis',(0.12303279206818,0.58482796993107,0.801772522391615));
#56482=DIRECTION('ref_axis',(0.987622662361441,0.00704480136426823,-0.15669029186212));
#56483=DIRECTION('center_axis',(0.166345636865383,6.46213028799582E-10,
0.986067507372518));
#56484=DIRECTION('ref_axis',(-0.985946412430586,0.0156715280538572,0.166325208623692));
#56485=DIRECTION('',(-0.16634572144554,-1.52655665884468E-11,-0.98606749310418));
#56486=DIRECTION('',(0.849666549784065,-3.07809289804128E-8,0.527320352516421));
#56487=DIRECTION('center_axis',(0.589597456970291,0.793626260375601,-0.150107286886432));
#56488=DIRECTION('ref_axis',(-0.802721322931315,0.596354322287849,8.06103090759229E-17));
#56489=DIRECTION('center_axis',(-0.440182224162468,0.47154667453567,0.764122597012897));
#56490=DIRECTION('ref_axis',(0.880508648889467,0.393407165948483,0.264452871058772));
#56491=DIRECTION('center_axis',(-0.185842683725629,-0.601098528037002,-0.777266399953971));
#56492=DIRECTION('ref_axis',(0.972980168381012,-0.00227572377380966,-0.23087748486711));
#56493=DIRECTION('',(0.579630823428158,5.19500677922247E-12,-0.814879198735614));
#56494=DIRECTION('center_axis',(0.,-1.,1.45983193964168E-32));
#56495=DIRECTION('ref_axis',(1.,0.,0.));
#56496=DIRECTION('center_axis',(0.189161557158541,0.601098527764655,0.776465366396029));
#56497=DIRECTION('ref_axis',(0.972340018886731,-0.00432802533413876,-0.233529775120988));
#56498=DIRECTION('center_axis',(0.178470202136203,-0.601098528104808,0.778992263414532));
#56499=DIRECTION('ref_axis',(0.974182705936134,-0.00330182722881675,-0.225736911895026));
#56500=DIRECTION('center_axis',(-0.175140642259538,0.60109852795263,-0.779747597060804));
#56501=DIRECTION('ref_axis',(0.97513818040934,-0.00330186181908194,-0.221573073311016));
#56502=DIRECTION('center_axis',(0.256228323716209,0.584828255987086,0.769625205619388));
#56503=DIRECTION('ref_axis',(0.955543863682515,-0.0330815410888132,-0.292987262893595));
#56504=DIRECTION('center_axis',(-0.288653681746295,-1.08169872562643E-7,
-0.957433575771341));
#56505=DIRECTION('ref_axis',(-0.957315942193711,-0.0156751635319026,0.288618218534477));
#56506=DIRECTION('',(0.288621063170579,0.,0.957443409238522));
#56507=DIRECTION('center_axis',(0.222548978555872,0.58482795222586,0.780030908643398));
#56508=DIRECTION('ref_axis',(0.96575072094856,-0.0227607296059838,-0.25847145717688));
#56509=DIRECTION('center_axis',(0.227933079194689,6.8622169776503E-10,0.973676800282736));
#56510=DIRECTION('ref_axis',(-0.973556893120938,0.0156933905088043,0.227905009490895));
#56511=DIRECTION('',(-0.227933166345564,-2.28705943069234E-11,-0.97367677988113));
#56512=DIRECTION('',(0.881100638236175,0.,0.472928816313623));
#56513=DIRECTION('center_axis',(-0.281794563711666,-0.601098528121939,-0.747845160011209));
#56514=DIRECTION('ref_axis',(0.943612876362721,-0.0324816844511772,-0.329453607868675));
#56515=DIRECTION('',(0.527320366161225,8.00811321699381E-12,-0.849666541315822));
#56516=DIRECTION('center_axis',(0.,-1.,1.45983193964168E-32));
#56517=DIRECTION('ref_axis',(1.,0.,0.));
#56518=DIRECTION('center_axis',(0.284986892580716,0.601098525015561,0.746634471666896));
#56519=DIRECTION('ref_axis',(0.942647561254193,-0.034538522663551,-0.331997990526662));
#56520=DIRECTION('center_axis',(0.178470203895147,-0.601098529032738,0.778992262295527));
#56521=DIRECTION('ref_axis',(0.96825973773138,-0.0335099891008813,-0.247689646369844));
#56522=DIRECTION('center_axis',(-0.175140622244973,0.601098526387723,-0.779747602762684));
#56523=DIRECTION('ref_axis',(0.969309052898517,-0.0335100374068191,-0.243550892755443));
#56524=DIRECTION('',(0.348169904517632,0.,0.937431446873948));
#56525=DIRECTION('center_axis',(0.318557910873374,0.584827952146795,0.745987348289352));
#56526=DIRECTION('ref_axis',(0.932627514633883,-0.0526562728392143,-0.356977920715706));
#56527=DIRECTION('center_axis',(0.288620968373058,7.36716723334152E-10,
0.957443437815205));
#56528=DIRECTION('ref_axis',(-0.957324330419263,0.0157729998146348,0.288585063480696));
#56529=DIRECTION('',(-0.288621063172965,-1.76525460893015E-10,-0.957443409237803));
#56530=DIRECTION('',(0.909057433471482,0.,0.4166708324928));
#56531=DIRECTION('',(0.472928816344016,6.51326541667589E-11,-0.881100638219862));
#56532=DIRECTION('center_axis',(0.,-1.,1.45983193964168E-32));
#56533=DIRECTION('ref_axis',(1.,0.,0.));
#56534=DIRECTION('center_axis',(0.196658269195918,0.601098532523592,0.774600593438225));
#56535=DIRECTION('ref_axis',(0.957707801639643,0.0514849473548277,-0.283099040751522));
#56536=DIRECTION('center_axis',(-0.356657108101514,0.601098534122288,-0.71517568437182));
#56537=DIRECTION('ref_axis',(0.910586511224675,0.0525165252266949,-0.409968559957699));
#56538=DIRECTION('center_axis',(0.263662627420127,0.584827908067115,0.767110381136742));
#56539=DIRECTION('ref_axis',(0.940205578398073,0.0219600677488413,-0.339898846384644));
#56540=DIRECTION('center_axis',(-0.406351027183781,-1.96778055995898E-8,
-0.913717047398529));
#56541=DIRECTION('ref_axis',(-0.913603867046846,-0.0157391387099202,0.406300693612155));
#56542=DIRECTION('',(0.406344678315241,1.1657341758555E-12,0.913719870860256));
#56543=DIRECTION('center_axis',(0.230078585587962,0.584827952320172,0.777843242973054));
#56544=DIRECTION('ref_axis',(0.951568403032065,0.0322834330679206,-0.305737394344157));
#56545=DIRECTION('center_axis',(0.348169842990746,4.83512735164658E-10,
0.937431469725547));
#56546=DIRECTION('ref_axis',(-0.937315898246574,0.0157020800822315,0.348126918774331));
#56547=DIRECTION('',(-0.3481699045172,-7.77156117238184E-13,-0.937431446874108));
#56548=DIRECTION('',(0.933426594325828,-1.64268989065341E-13,0.358768439254745));
#56549=DIRECTION('center_axis',(-0.289010284359285,-0.601098527964732,-0.745086313934968));
#56550=DIRECTION('ref_axis',(0.925593867913443,0.0232723731127603,-0.377802049135169));
#56551=DIRECTION('',(0.41667083249282,0.,-0.909057433471472));
#56552=DIRECTION('center_axis',(0.,-1.,1.45983193964168E-32));
#56553=DIRECTION('ref_axis',(1.,0.,0.));
#56554=DIRECTION('center_axis',(0.292190763392168,0.601098530037678,0.743844819149025));
#56555=DIRECTION('ref_axis',(0.924602942398734,0.0212180856973082,-0.380340888870688));
#56556=DIRECTION('center_axis',(0.359709254122371,-0.601098526854637,0.713645439635056));
#56557=DIRECTION('ref_axis',(0.900162724924359,0.0222452403493355,-0.43498530772723));
#56558=DIRECTION('center_axis',(-0.356657179733677,0.601098528884004,-0.715175653051686));
#56559=DIRECTION('ref_axis',(0.90201281102059,0.0222451869553289,-0.431135756359939));
#56560=DIRECTION('center_axis',(0.357729647163817,0.58482795337547,0.728014947985761));
#56561=DIRECTION('ref_axis',(0.899954361422345,-0.00784642889805246,-0.435913501638165));
#56562=DIRECTION('center_axis',(-0.462916327110225,-2.13103238692194E-9,
-0.886401982226337));
#56563=DIRECTION('ref_axis',(-0.886293038960898,-0.0156778482812414,0.462859432401163));
#56564=DIRECTION('',(0.462915795308865,-8.3266726846851E-13,0.88640225995513));
#56565=DIRECTION('center_axis',(0.325753955500558,0.584827952253567,0.742873223867061));
#56566=DIRECTION('ref_axis',(0.915101869174067,0.00246180459107409,-0.403215213691503));
#56567=DIRECTION('center_axis',(0.406344609651634,5.69456944890493E-10,
0.91371990139597));
#56568=DIRECTION('ref_axis',(-0.913607702448164,0.0156707406190495,0.40629471312809));
#56569=DIRECTION('',(-0.406344678315647,-6.46149800302078E-11,-0.913719870860076));
#56570=DIRECTION('',(0.954111946854455,1.64268989065293E-13,0.2994501508926));
#56571=DIRECTION('center_axis',(-0.380115429527852,-0.601098528065762,-0.702988491934279));
#56572=DIRECTION('ref_axis',(0.882085304090706,-0.00691952261253271,-0.471038890659807));
#56573=DIRECTION('',(0.358768439266062,2.34493981894336E-11,-0.933426594321478));
#56574=DIRECTION('center_axis',(0.,-1.,1.45983193964168E-32));
#56575=DIRECTION('ref_axis',(1.,0.,0.));
#56576=DIRECTION('center_axis',(0.383115245013786,0.601098527119973,0.701358160808175));
#56577=DIRECTION('ref_axis',(0.880782574146974,-0.00897206302439092,-0.47343590819045));
#56578=DIRECTION('center_axis',(0.359709246947306,-0.601098528345563,0.713645441995814));
#56579=DIRECTION('ref_axis',(0.890243668023657,-0.0079457177559491,-0.455415279841518));
#56580=DIRECTION('center_axis',(-0.356657173644811,0.60109852769709,-0.715175657085786));
#56581=DIRECTION('ref_axis',(0.892181121906817,-0.00794577101805003,-0.451607916710969));
#56582=DIRECTION('center_axis',(0.446196308910663,0.584826536165555,0.677411821945188));
#56583=DIRECTION('ref_axis',(0.84211854955642,-0.018184624938029,-0.538985777093287));
#56584=DIRECTION('center_axis',(-0.517660059578906,-5.71097183739979E-10,
-0.855586385303532));
#56585=DIRECTION('ref_axis',(-0.85548120719194,-0.0156795066172793,0.517596423107483));
#56586=DIRECTION('',(0.517659992380242,2.06171049564757E-7,0.855586425961074));
#56587=DIRECTION('center_axis',(0.416297377870238,0.584827782537028,0.696184571756073));
#56588=DIRECTION('ref_axis',(0.867894343950115,-0.0273551073936917,-0.495995066345301));
#56589=DIRECTION('center_axis',(0.462915689858085,8.19138286898656E-10,
0.886402315025865));
#56590=DIRECTION('ref_axis',(-0.88629303124274,0.0157023279251941,0.462858617364184));
#56591=DIRECTION('',(0.462915794448414,-1.2926741850564E-5,0.886402260310235));
#56592=DIRECTION('',(0.971031864912497,-7.62629077550481E-8,0.238950031020196));
#56593=DIRECTION('center_axis',(-0.517659995654058,-4.84222756609793E-10,
-0.855586423980325));
#56594=DIRECTION('ref_axis',(-0.66040683756443,-0.635772805082279,0.399569454808496));
#56595=DIRECTION('',(-0.299450150894097,0.,0.954111946853985));
#56596=DIRECTION('center_axis',(0.520704586489422,0.398564391591113,0.754992158478806));
#56597=DIRECTION('ref_axis',(0.823202421104882,-3.43454409686757E-16,-0.567747984485247));
#56598=DIRECTION('center_axis',(-0.576093384133844,5.74456620606364E-5,
-0.817383881329459));
#56599=DIRECTION('ref_axis',(0.817383840858432,0.000362923848892853,-0.57609333010355));
#56600=DIRECTION('',(0.57036047544634,5.94973683763054E-5,0.821394499926003));
#56601=DIRECTION('center_axis',(0.405137316878508,0.590180063814461,0.698248699782851));
#56602=DIRECTION('ref_axis',(0.43716135183174,-0.795819504651481,0.419000320382833));
#56603=DIRECTION('center_axis',(0.82270565378683,0.550037558008124,-0.143576084386098));
#56604=DIRECTION('ref_axis',(-0.555796003805303,0.831318712741422,-1.57794878871776E-16));
#56605=DIRECTION('center_axis',(-0.155987445342299,-0.477126090515431,0.864880691566787));
#56606=DIRECTION('ref_axis',(0.96862208907624,0.0976327713137033,0.228558724443385));
#56607=DIRECTION('center_axis',(-0.0450737364009293,0.584827951389048,0.80990408417352));
#56608=DIRECTION('ref_axis',(0.998983642785354,0.0265489690160679,0.036425728427699));
#56609=DIRECTION('center_axis',(-0.0414470086426727,-3.87595059013494E-11,
-0.999140703542086));
#56610=DIRECTION('ref_axis',(-0.999016806325967,-0.0157477670562018,0.0414418690578688));
#56611=DIRECTION('center_axis',(-0.0122720118683925,-0.000115441168890837,
0.999924689363173));
#56612=DIRECTION('ref_axis',(0.0248716549244404,-0.999690634518669,0.000189834085567114));
#56613=DIRECTION('',(0.0213713417293984,-6.05404615063059E-10,-0.999771606794615));
#56614=DIRECTION('center_axis',(0.0132941942386101,-0.601098528297747,-0.799064342639458));
#56615=DIRECTION('ref_axis',(0.999600535647751,0.027922007443411,-0.00437385791473135));
#56616=DIRECTION('',(0.72205710354946,2.24206636476366E-10,-0.691833462051211));
#56617=DIRECTION('center_axis',(0.,-1.,1.45983193964168E-32));
#56618=DIRECTION('ref_axis',(1.,0.,0.));
#56619=DIRECTION('center_axis',(-0.00988037512737149,0.601098530231419,
0.799113843667453));
#56620=DIRECTION('ref_axis',(0.999640202548808,0.0258668036150491,-0.00709745862388935));
#56621=DIRECTION('center_axis',(0.0794293293740866,-0.601098526204097,0.795217921975131));
#56622=DIRECTION('ref_axis',(0.996495534121554,0.02689441690441,-0.0792044242146213));
#56623=DIRECTION('center_axis',(-0.0760313169023642,0.60109852885632,-0.795549996830407));
#56624=DIRECTION('ref_axis',(0.996824811638328,0.0268943589583594,-0.0749465700244607));
#56625=DIRECTION('center_axis',(0.0567895988978252,0.584827952222578,0.809166983852017));
#56626=DIRECTION('ref_axis',(0.99770283476844,-0.00326197144910447,-0.0676639714861966));
#56627=DIRECTION('center_axis',(-0.104101854023608,-5.35833916009832E-10,
-0.994566641301048));
#56628=DIRECTION('ref_axis',(-0.994444320292724,-0.0156832196308266,0.10408905062279));
#56629=DIRECTION('',(0.104101784680632,8.32123764308129E-8,0.994566648559211));
#56630=DIRECTION('center_axis',(0.021573898985439,0.584827969931933,0.810870404237237));
#56631=DIRECTION('ref_axis',(0.999473463626372,0.00704480133771679,-0.0316728003311105));
#56632=DIRECTION('center_axis',(0.0414469425202581,4.90387004565544E-10,
0.999140706285017));
#56633=DIRECTION('ref_axis',(-0.999018005875278,0.0156715280542373,0.0414418525819914));
#56634=DIRECTION('',(-0.0414470083234317,-1.52100554371989E-11,-0.999140703555329));
#56635=DIRECTION('',(0.776875910350839,-3.07809289804261E-8,0.62965373016965));
#56636=DIRECTION('center_axis',(0.603761736567746,0.793626260373733,-0.0750274903079059));
#56637=DIRECTION('ref_axis',(-0.795869445639745,0.605468269603854,1.93408423312097E-18));
#56638=DIRECTION('center_axis',(-0.532481211769311,0.471546674534408,0.70292780059422));
#56639=DIRECTION('ref_axis',(0.840418742351967,0.393423605136949,0.37271195905764));
#56640=DIRECTION('center_axis',(-0.0869599531970929,-0.601098528018402,
-0.79442968609819));
#56641=DIRECTION('ref_axis',(0.994244550367405,-0.00227572727050743,-0.107110200868581));
#56642=DIRECTION('',(0.677191706199972,5.19500677922242E-12,-0.735806627487121));
#56643=DIRECTION('center_axis',(0.,-1.,1.45983193964168E-32));
#56644=DIRECTION('ref_axis',(1.,0.,0.));
#56645=DIRECTION('center_axis',(0.0903530431260819,0.601098527779805,0.794050935078354));
#56646=DIRECTION('ref_axis',(0.993941869584976,-0.00432802320240801,-0.109821801574556));
#56647=DIRECTION('center_axis',(0.0794293017766313,-0.601098528134647,0.795217923272381));
#56648=DIRECTION('ref_axis',(0.994793320646601,-0.00330182131864235,-0.101859448127744));
#56649=DIRECTION('center_axis',(-0.0760313175229954,0.601098527951306,-0.795549997454899));
#56650=DIRECTION('ref_axis',(0.995219394403722,-0.0033018622772266,-0.0976086815206026));
#56651=DIRECTION('center_axis',(0.157748271217537,0.584828255986589,0.795670405336005));
#56652=DIRECTION('ref_axis',(0.984730155958913,-0.0330815410996522,-0.170915568581701));
#56653=DIRECTION('center_axis',(-0.166379306364509,-1.08098869174227E-7,
-0.98606182687175));
#56654=DIRECTION('ref_axis',(-0.985940676151014,-0.0156751635313622,0.166358866187367));
#56655=DIRECTION('',(0.166345721446008,-4.44089209849642E-13,0.986067493104101));
#56656=DIRECTION('center_axis',(0.123030317359083,0.584827952225381,0.801772915049137));
#56657=DIRECTION('ref_axis',(0.990530551566245,-0.0227607296247098,-0.135392671887445));
#56658=DIRECTION('center_axis',(0.104101719042027,5.12252965996456E-10,
0.994566655429637));
#56659=DIRECTION('ref_axis',(-0.994444175704888,0.0156933905084582,0.104088899028543));
#56660=DIRECTION('',(-0.104101785979457,-2.24265050970633E-11,-0.994566648423266));
#56661=DIRECTION('',(0.814879198737199,0.,0.579630823425929));
#56662=DIRECTION('center_axis',(-0.185842672560432,-0.601098528282589,-0.77726640243362));
#56663=DIRECTION('ref_axis',(0.977463693873356,-0.0324816815353087,-0.208589710973703));
#56664=DIRECTION('',(0.62965374264558,8.0081132169946E-12,-0.776875900239165));
#56665=DIRECTION('center_axis',(0.,-1.,1.45983193964168E-32));
#56666=DIRECTION('ref_axis',(1.,0.,0.));
#56667=DIRECTION('center_axis',(0.189161568512983,0.601098525178652,0.776465365631821));
#56668=DIRECTION('ref_axis',(0.976824886273939,-0.0345385197933366,-0.211235016525178));
#56669=DIRECTION('center_axis',(0.0794293062798579,-0.601098529449489,0.795217921828704));
#56670=DIRECTION('ref_axis',(0.99166846380021,-0.0335099815858313,-0.124381425615923));
#56671=DIRECTION('center_axis',(-0.076031303748593,0.601098526592688,-0.795549999797868));
#56672=DIRECTION('ref_axis',(0.992190781961022,-0.0335100337510252,-0.120143788143963));
#56673=DIRECTION('',(0.227933166345836,0.,0.973676779881066));
#56674=DIRECTION('center_axis',(0.222548980042715,0.584827952146603,0.780030908278613));
#56675=DIRECTION('ref_axis',(0.970014665232009,-0.0526562728418158,-0.237273821070177));
#56676=DIRECTION('center_axis',(0.166345654650758,4.90609543879989E-10,
0.986067504372196));
#56677=DIRECTION('ref_axis',(-0.985944836097383,0.015772999814921,0.166324960994262));
#56678=DIRECTION('',(-0.166345721448132,-1.76525460892848E-10,-0.986067493103743));
#56679=DIRECTION('',(0.849666541318092,0.,0.527320366157567));
#56680=DIRECTION('',(0.579630823453911,6.52763895321938E-11,-0.814879198717295));
#56681=DIRECTION('center_axis',(0.,-1.,1.45983193964168E-32));
#56682=DIRECTION('ref_axis',(1.,0.,0.));
#56683=DIRECTION('center_axis',(0.0980243614840752,0.601098532447537,0.793140453416075));
#56684=DIRECTION('ref_axis',(0.985637707909252,0.0514849482174098,-0.160834103518025));
#56685=DIRECTION('center_axis',(-0.264209488022563,0.601098533639632,-0.754237296409519));
#56686=DIRECTION('ref_axis',(0.954788947439151,0.0525165307922483,-0.292609090497177));
#56687=DIRECTION('center_axis',(0.165440120299829,0.584827930050204,0.794106956793839));
#56688=DIRECTION('ref_axis',(0.975392232534895,0.0219594825888217,-0.219380431750472));
#56689=DIRECTION('center_axis',(-0.288624441049067,-1.01852615899359E-8,
-0.957442390971443));
#56690=DIRECTION('ref_axis',(-0.95732379452256,-0.0157391393488549,0.288588689891833));
#56691=DIRECTION('',(0.288621063170527,0.,0.957443409238538));
#56692=DIRECTION('center_axis',(0.130774738411927,0.58482795232171,0.80054620976961));
#56693=DIRECTION('ref_axis',(0.982384058203747,0.0322834330438129,-0.184063418793747));
#56694=DIRECTION('center_axis',(0.227933095961805,5.36713694051927E-10,
0.973676796357635));
#56695=DIRECTION('ref_axis',(-0.973556756363443,0.0157020800829616,0.227904995162808));
#56696=DIRECTION('',(-0.227933166345239,0.,-0.973676779881206));
#56697=DIRECTION('',(0.881100638235996,0.,0.472928816313958));
#56698=DIRECTION('center_axis',(-0.193347279669351,-0.601098528077531,-0.775433678007015));
#56699=DIRECTION('ref_axis',(0.965646435319799,0.0232723701693565,-0.258815298506224));
#56700=DIRECTION('',(0.527320366157741,1.43735365432636E-13,-0.849666541317984));
#56701=DIRECTION('center_axis',(0.,-1.,1.45983193964168E-32));
#56702=DIRECTION('ref_axis',(1.,0.,0.));
#56703=DIRECTION('center_axis',(0.196658274352736,0.601098530012063,0.774600594077968));
#56704=DIRECTION('ref_axis',(0.964981525726815,0.0212180863974566,-0.261458309899644));
#56705=DIRECTION('center_axis',(0.267429327870916,-0.601098527355575,0.753101663127542));
#56706=DIRECTION('ref_axis',(0.947582794004111,0.022245227166339,-0.318734997098971));
#56707=DIRECTION('center_axis',(-0.26420956622361,0.601098528605351,-0.754237273027802));
#56708=DIRECTION('ref_axis',(0.948935805683094,0.0222451945820041,-0.314683949400961));
#56709=DIRECTION('center_axis',(0.263664374551296,0.584827953375635,0.767109746087833));
#56710=DIRECTION('ref_axis',(0.947492401188789,-0.00784642890954199,-0.319682003314027));
#56711=DIRECTION('center_axis',(-0.348170453906574,-2.02285230155265E-9,
-0.937431242826102));
#56712=DIRECTION('ref_axis',(-0.937316027812998,-0.0156778482804679,0.348127662041035));
#56713=DIRECTION('',(0.348169904517851,0.,0.937431446873866));
#56714=DIRECTION('center_axis',(0.230078585025473,0.584827952254169,0.777843243189058));
#56715=DIRECTION('ref_axis',(0.958422284153197,0.00246180456792404,-0.285343065023208));
#56716=DIRECTION('center_axis',(0.288620995923767,5.31164864483657E-10,
0.957443429510054));
#56717=DIRECTION('ref_axis',(-0.957325861591825,0.0156707406190328,0.288585555106142));
#56718=DIRECTION('',(-0.288621063171154,-6.3837823913025E-11,-0.957443409238349));
#56719=DIRECTION('',(0.909057433471483,1.64268989065371E-13,0.416670832492798));
#56720=DIRECTION('center_axis',(-0.289010286880025,-0.601098528051554,-0.745086312887158));
#56721=DIRECTION('ref_axis',(0.934166624713937,-0.00691952383404778,-0.356770006391346));
#56722=DIRECTION('',(0.472928816324657,2.3593133554862E-11,-0.881100638230253));
#56723=DIRECTION('center_axis',(0.,-1.,1.45983193964168E-32));
#56724=DIRECTION('ref_axis',(1.,0.,0.));
#56725=DIRECTION('center_axis',(0.292190763391757,0.601098527273705,0.743844821382743));
#56726=DIRECTION('ref_axis',(0.933174599151579,-0.00897205187960923,-0.359311382763417));
#56727=DIRECTION('center_axis',(0.267429334256417,-0.601098528288515,0.753101660115387));
#56728=DIRECTION('ref_axis',(0.940302502417433,-0.00794572222091479,-0.34024707117902));
#56729=DIRECTION('center_axis',(-0.264209542754952,0.601098527650592,-0.754237282009787));
#56730=DIRECTION('ref_axis',(0.941747489151797,-0.00794577413585423,-0.336226904559507));
#56731=DIRECTION('center_axis',(0.357729782879291,0.584827952230029,0.728014882218466));
#56732=DIRECTION('ref_axis',(0.903049056216021,-0.0181546317010865,-0.429153598860771));
#56733=DIRECTION('center_axis',(-0.406344608639772,5.97918690298626E-10,
-0.91371990184596));
#56734=DIRECTION('ref_axis',(-0.91360757733036,-0.015679506615491,0.406294656274047));
#56735=DIRECTION('',(0.406344675363134,2.06170716497958E-7,0.913719872173079));
#56736=DIRECTION('center_axis',(0.325759685235944,0.584827782535944,0.742870844931385));
#56737=DIRECTION('ref_axis',(0.923215403293511,-0.0273551074368675,-0.383307992636101));
#56738=DIRECTION('center_axis',(0.348169814866188,6.35675375795079E-10,
0.937431480171241));
#56739=DIRECTION('ref_axis',(-0.937315905043182,0.0157023279249446,0.348126889295869));
#56740=DIRECTION('',(0.348169903620024,-1.29267404452099E-5,0.9374314471182));
#56741=DIRECTION('',(0.933426608576421,-7.62630514904304E-8,0.358768402178222));
#56742=DIRECTION('center_axis',(-0.406344678303629,9.72635009398676E-12,
-0.91371987086542));
#56743=DIRECTION('ref_axis',(-0.705278664517349,-0.63577280508501,0.31364780517479));
#56744=DIRECTION('',(-0.416670832494401,0.,0.909057433470748));
#56745=DIRECTION('center_axis',(0.42197306675971,0.398564391592602,0.814300409359976));
#56746=DIRECTION('ref_axis',(0.88786891488108,-3.68203022609066E-16,-0.460096500734241));
#56747=DIRECTION('center_axis',(-0.469105350786784,5.74456587699608E-5,
-0.883142211969966));
#56748=DIRECTION('ref_axis',(0.883142165048644,0.000362915771362469,-0.469105302256685));
#56749=DIRECTION('',(0.462914984031396,5.94973683407511E-5,0.88640268164039));
#56750=DIRECTION('center_axis',(0.31442892067083,0.59018006381212,0.743519970225749));
#56751=DIRECTION('ref_axis',(0.381193945724401,-0.795820376348163,0.470490280805172));
#56752=DIRECTION('center_axis',(0.834213228884336,0.550037558023509,-0.039331584228274));
#56753=DIRECTION('ref_axis',(-0.550463499044935,0.834859231379283,-4.10782205454431E-17));
#56754=DIRECTION('center_axis',(-0.263155731641066,-0.477126089454373,0.838510438615068));
#56755=DIRECTION('ref_axis',(0.932338856151779,0.0976304978256445,0.348155917950433));
#56756=DIRECTION('center_axis',(-0.146226214258538,0.584827951389492,0.797868511433548));
#56757=DIRECTION('ref_axis',(0.98654100405341,0.0265489690076915,0.161344350895589));
#56758=DIRECTION('center_axis',(0.0841053503384132,-1.04564632314426E-11,
-0.996456868130504));
#56759=DIRECTION('ref_axis',(-0.996333303720138,-0.015747767056287,-0.0840949209575536));
#56760=DIRECTION('center_axis',(-0.137499037186064,-0.000115441183750491,
0.990501893711586));
#56761=DIRECTION('ref_axis',(0.0246541028855363,-0.999690575213707,0.00330590982899623));
#56762=DIRECTION('',(0.14650743062224,-6.06570349238291E-10,-0.989209569693131));
#56763=DIRECTION('center_axis',(0.113338698242169,-0.601098527890642,-0.791097275465207));
#56764=DIRECTION('ref_axis',(0.992266574922364,0.0279220164159767,0.120943810470426));
#56765=DIRECTION('',(0.803073192506942,2.24206636476422E-10,-0.595880396956225));
#56766=DIRECTION('center_axis',(0.,-1.,1.45983193964168E-32));
#56767=DIRECTION('ref_axis',(1.,0.,0.));
#56768=DIRECTION('center_axis',(-0.109958002712627,0.601098529822913,0.791574251150316));
#56769=DIRECTION('ref_axis',(0.992647286720043,0.0258668128628887,0.118246658133127));
#56770=DIRECTION('center_axis',(-0.020864243568711,-0.601098526625939,0.798902525110812));
#56771=DIRECTION('ref_axis',(0.998564815473844,0.0268944076276533,0.0463141461763672));
#56772=DIRECTION('center_axis',(0.024277065154547,0.601098528826007,-0.798806098343454));
#56773=DIRECTION('ref_axis',(0.998357846255219,0.0268943596500547,0.0505796820833543));
#56774=DIRECTION('center_axis',(-0.0450737186594267,0.584827952222493,0.809904084559065));
#56775=DIRECTION('ref_axis',(0.998316194257801,-0.00326197143264825,0.0579149015797671));
#56776=DIRECTION('center_axis',(0.0213712886453174,-4.16287320721315E-10,
-0.99977160792935));
#56777=DIRECTION('ref_axis',(-0.999648646767079,-0.01568321963139,-0.0213686601999815));
#56778=DIRECTION('',(-0.0213713430443371,8.32155960773552E-8,0.999771606766503));
#56779=DIRECTION('center_axis',(-0.0802252274000674,0.584827969932243,0.807180375426422));
#56780=DIRECTION('ref_axis',(0.99556197132029,0.0070448013281525,0.0938441902043184));
#56781=DIRECTION('center_axis',(-0.0841054090067981,4.46159887102019E-10,
0.996456863178632));
#56782=DIRECTION('ref_axis',(-0.99633449235985,0.0156715280544274,-0.0840950803702535));
#56783=DIRECTION('',(0.0841053488789417,-1.28230759343022E-11,-0.99645686825369));
#56784=DIRECTION('',(0.691833473728012,-3.07809289804253E-8,0.722057092361422));
#56785=DIRECTION('center_axis',(0.608404332907485,0.793626260372994,0.0012355346107901));
#56786=DIRECTION('ref_axis',(-0.793626866127095,0.608404797286549,2.59767481348948E-19));
#56787=DIRECTION('center_axis',(-0.616382652520224,0.471546674485576,0.630647412944608));
#56788=DIRECTION('ref_axis',(0.787078545591813,0.393425210691968,0.475104164011491));
#56789=DIRECTION('center_axis',(0.0132942125182302,-0.601098528073487,-0.799064342504036));
#56790=DIRECTION('ref_axis',(0.999829102689717,-0.00227571578226521,0.0183462947854261));
#56791=DIRECTION('',(0.764072871230274,5.0512714137896E-12,-0.645129946173579));
#56792=DIRECTION('center_axis',(0.,-1.,1.45983193964168E-32));
#56793=DIRECTION('ref_axis',(1.,0.,0.));
#56794=DIRECTION('center_axis',(-0.00988040017072651,0.601098527820397,
0.799113845171399));
#56795=DIRECTION('ref_axis',(0.999868662463102,-0.00432801644249017,0.0156181336247414));
#56796=DIRECTION('center_axis',(-0.0208642534513744,-0.601098528142146,
0.798902523711912));
#56797=DIRECTION('ref_axis',(0.999715452232994,-0.00330181997161638,0.0236244058434362));
#56798=DIRECTION('center_axis',(0.024277053557954,0.601098527995585,-0.798806099320784));
#56799=DIRECTION('ref_axis',(0.999605404196658,-0.00330185493271657,0.0278950471381458));
#56800=DIRECTION('center_axis',(0.0567768155390874,0.584828375911211,0.809167574700257));
#56801=DIRECTION('ref_axis',(0.99838687122767,-0.0330794214939016,-0.0461455006891631));
#56802=DIRECTION('center_axis',(-0.0414944532586696,-1.506057891401E-7,
-0.999138734285055));
#56803=DIRECTION('ref_axis',(-0.999015977122379,-0.0156751609033304,0.0414893574892793));
#56804=DIRECTION('',(0.0414470083239282,-8.32667268469771E-13,0.999140703555308));
#56805=DIRECTION('center_axis',(0.0215713944646267,0.584827952226312,0.810870483638189));
#56806=DIRECTION('ref_axis',(0.999689123680026,-0.0227607295853948,-0.0101786632031094));
#56807=DIRECTION('center_axis',(-0.0213714117579914,5.34377304442964E-10,
0.999771605297665));
#56808=DIRECTION('ref_axis',(-0.999648484588385,0.0156933905084443,-0.0213687799019016));
#56809=DIRECTION('',(0.0213713417387848,-2.40918396339775E-11,-0.999771606794414));
#56810=DIRECTION('',(0.735806627489012,0.,0.677191706197917));
#56811=DIRECTION('center_axis',(-0.0869599395448373,-0.601098528164396,
-0.79442968748213));
#56812=DIRECTION('ref_axis',(0.995899323349845,-0.0324816836639048,-0.0844362361648036));
#56813=DIRECTION('',(0.722057103471606,8.00811321699473E-12,-0.691833462132467));
#56814=DIRECTION('center_axis',(0.,-1.,1.45983193964168E-32));
#56815=DIRECTION('ref_axis',(1.,0.,0.));
#56816=DIRECTION('center_axis',(0.0903530450352583,0.601098525620875,0.794050936495428));
#56817=DIRECTION('ref_axis',(0.995597099123901,-0.034538511957999,-0.0871407333444038));
#56818=DIRECTION('center_axis',(-0.0208642636661934,-0.601098529032989,
0.798902522774866));
#56819=DIRECTION('ref_axis',(0.999437987770463,-0.0335099891761658,0.000888384343415163));
#56820=DIRECTION('center_axis',(0.024277072871618,0.601098526825379,-0.798806099614384));
#56821=DIRECTION('ref_axis',(0.999425070919505,-0.0335100296281867,0.00515805504620711));
#56822=DIRECTION('',(0.104101785979659,3.88578058618678E-13,0.994566648423244));
#56823=DIRECTION('center_axis',(0.123030318886438,0.584827952145045,0.801772914873366));
#56824=DIRECTION('ref_axis',(0.992104105097463,-0.0526562728642782,-0.113827771553362));
#56825=DIRECTION('center_axis',(0.0414469144126123,6.97494215856958E-10,
0.999140707450994));
#56826=DIRECTION('ref_axis',(-0.999016412849288,0.0157729998147174,0.0414417583433199));
#56827=DIRECTION('',(-0.0414470083263993,-1.77358128161261E-10,-0.999140703555206));
#56828=DIRECTION('',(0.776875900241836,0.,0.629653742642285));
#56829=DIRECTION('',(0.677191706223117,6.51326541667497E-11,-0.735806627465819));
#56830=DIRECTION('center_axis',(0.,-1.,1.45983193964168E-32));
#56831=DIRECTION('ref_axis',(1.,0.,0.));
#56832=DIRECTION('center_axis',(-0.00215546144630236,0.601098531722126,
0.799172014742419));
#56833=DIRECTION('ref_axis',(0.99802351841858,0.0514849565616084,-0.0360327064102555));
#56834=DIRECTION('center_axis',(-0.167595112513565,0.601098533934261,-0.78140414048279));
#56835=DIRECTION('ref_axis',(0.983933795834039,0.052516527403456,-0.170634989861697));
#56836=DIRECTION('center_axis',(0.0646072654303257,0.584827923043277,0.808580361919891));
#56837=DIRECTION('ref_axis',(0.995196652945506,0.0219596691043631,-0.0954012311183076));
#56838=DIRECTION('center_axis',(-0.166350265005554,-1.31282301405503E-8,
-0.986066726612648));
#56839=DIRECTION('ref_axis',(-0.98594458454176,-0.0157391391446185,0.166329659747629));
#56840=DIRECTION('',(0.166345721446039,8.32667268468167E-13,0.986067493104096));
#56841=DIRECTION('center_axis',(0.0294084954526384,0.584827952321989,0.810624084627444));
#56842=DIRECTION('ref_axis',(0.997706929939182,0.0322834330428721,-0.0594866531442022));
#56843=DIRECTION('center_axis',(0.104101705406296,6.05294299319807E-10,
0.994566656856895));
#56844=DIRECTION('ref_axis',(-0.994444041449916,0.0157020800824323,0.104088871191121));
#56845=DIRECTION('',(-0.104101785979012,-8.32667268468189E-13,-0.994566648423312));
#56846=DIRECTION('',(0.814879198737093,0.,0.579630823426078));
#56847=DIRECTION('center_axis',(-0.0946350612128965,-0.601098527914393,
-0.793551992580436));
#56848=DIRECTION('ref_axis',(0.990470183691813,0.023272374490036,-0.135746866641933));
#56849=DIRECTION('',(0.629653742642401,1.43735365432657E-13,-0.776875900241742));
#56850=DIRECTION('center_axis',(0.,-1.,1.45983193964168E-32));
#56851=DIRECTION('ref_axis',(1.,0.,0.));
#56852=DIRECTION('center_axis',(0.0980243639847826,0.601098529928312,0.793140455016261));
#56853=DIRECTION('ref_axis',(0.990141773984808,0.0212180887973301,-0.13845237490923));
#56854=DIRECTION('center_axis',(0.170931915613415,-0.601098527019728,0.780681011066263));
#56855=DIRECTION('ref_axis',(0.980058905949232,0.0222452360632367,-0.19745807236496));
#56856=DIRECTION('center_axis',(-0.167595193935718,0.601098528699735,-0.78140412704609));
#56857=DIRECTION('ref_axis',(0.980893521143664,0.0222451917353439,-0.193269375802382));
#56858=DIRECTION('center_axis',(0.165440957208147,0.584827953375401,0.794106765258168));
#56859=DIRECTION('ref_axis',(0.980087919794378,-0.00784642889667977,-0.198408928797817));
#56860=DIRECTION('center_axis',(-0.22793372461516,-1.92270791500281E-9,
-0.973676649192667));
#56861=DIRECTION('ref_axis',(-0.973556979441473,-0.0156778482808568,0.227905710446399));
#56862=DIRECTION('',(0.227933166345677,7.77156117236961E-13,0.973676779881103));
#56863=DIRECTION('center_axis',(0.13077473776379,0.584827952253972,0.800546209924973));
#56864=DIRECTION('ref_axis',(0.986627807193293,0.00246180458131422,-0.162970885716307));
#56865=DIRECTION('center_axis',(0.16634562963675,7.10084872101303E-10,0.986067508591959));
#56866=DIRECTION('ref_axis',(-0.985946425819607,0.0156707406190697,0.166325203447917));
#56867=DIRECTION('',(-0.166345721446248,-6.37823127617725E-11,-0.986067493104061));
#56868=DIRECTION('',(0.849666541317975,1.64268989065366E-13,0.527320366157756));
#56869=DIRECTION('center_axis',(-0.19334727172034,-0.601098528097524,-0.77543367997353));
#56870=DIRECTION('ref_axis',(0.971515581559539,-0.00691952022034624,-0.236874639898302));
#56871=DIRECTION('',(0.579630823435965,2.34493981894383E-11,-0.814879198730061));
#56872=DIRECTION('center_axis',(0.,-1.,1.45983193964168E-32));
#56873=DIRECTION('ref_axis',(1.,0.,0.));
#56874=DIRECTION('center_axis',(0.196658270544328,0.601098527316492,0.774600597136652));
#56875=DIRECTION('ref_axis',(0.970849897117024,-0.008972048994066,-0.239520311465881));
#56876=DIRECTION('center_axis',(0.17093190968256,-0.601098528304482,0.780681011375619));
#56877=DIRECTION('ref_axis',(0.975532201644004,-0.00794572107663697,-0.219712969740464));
#56878=DIRECTION('center_axis',(-0.167595173693706,0.601098527646255,-0.781404132197982));
#56879=DIRECTION('ref_axis',(0.976461934154753,-0.0079457744237133,-0.215543396594667));
#56880=DIRECTION('center_axis',(0.263664517464618,0.584827952228799,0.767109697841202));
#56881=DIRECTION('ref_axis',(0.949715452909033,-0.0181546317278219,-0.312587536304022));
#56882=DIRECTION('center_axis',(-0.28862099104446,6.09872333951937E-10,
-0.957443430980919));
#56883=DIRECTION('ref_axis',(-0.957325731486259,-0.0156795066142757,0.288585510562525));
#56884=DIRECTION('',(0.28862106007695,2.06171937743006E-7,0.957443410171074));
#56885=DIRECTION('center_axis',(0.230084567703631,0.584827782535973,0.777841601149418));
#56886=DIRECTION('ref_axis',(0.963976804255236,-0.0273551074375476,-0.264575922855696));
#56887=DIRECTION('center_axis',(0.22793305193534,8.06705954572667E-10,0.973676806664019));
#56888=DIRECTION('ref_axis',(-0.97355676287983,0.0157023279251005,0.227904950250493));
#56889=DIRECTION('',(0.227933165424189,-1.29267412268658E-5,0.97367678001101));
#56890=DIRECTION('',(0.881100657021104,-7.62629077550825E-8,0.472928781315933));
#56891=DIRECTION('center_axis',(-0.288621063731909,-4.7686293377351E-10,
-0.95744340906931));
#56892=DIRECTION('ref_axis',(-0.739027824993722,-0.635772805081909,0.222779743700656));
#56893=DIRECTION('',(-0.527320366159318,0.,0.849666541317005));
#56894=DIRECTION('center_axis',(0.316586779693368,0.398564391592836,0.860766656346315));
#56895=DIRECTION('ref_axis',(4.1601212236768E-16,-0.907442263761735,0.420176793670209));
#56896=DIRECTION('center_axis',(-0.354719245873589,5.74456553038096E-5,
-0.934972862337121));
#56897=DIRECTION('ref_axis',(0.934972809691412,0.000362953207812999,-0.354719203600136));
#56898=DIRECTION('',(0.348169046786044,5.94973691579315E-5,0.937431763554106));
#56899=DIRECTION('center_axis',(0.218761792620593,0.590180063812006,0.777065486537834));
#56900=DIRECTION('ref_axis',(0.319216405899052,-0.795820911703122,0.51455802656348));
#56901=DIRECTION('center_axis',(0.83256476303904,0.550037558024637,0.065533198518315));
#56902=DIRECTION('ref_axis',(-0.551222471619054,0.834358308391653,-2.53035028927643E-17));
#56903=DIRECTION('center_axis',(-0.36617389431988,-0.477126091316635,0.798916373660925));
#56904=DIRECTION('ref_axis',(0.881353683148659,0.0976243413979602,0.462260936232889));
#56905=DIRECTION('center_axis',(-0.245072617360243,0.58482795139018,0.773250075650152));
#56906=DIRECTION('ref_axis',(0.958540024361042,0.0265489689952938,0.283718476562983));
#56907=DIRECTION('center_axis',(0.208331313444156,-5.80606616147636E-11,
-0.978058313107472));
#56908=DIRECTION('ref_axis',(-0.977937030187507,-0.0157477670561977,-0.208305479574549));
#56909=DIRECTION('center_axis',(-0.260557623648053,-0.000115441151282437,
0.965458290881704));
#56910=DIRECTION('ref_axis',(0.0229724391951117,-0.999717608876927,0.00608025812175752));
#56911=DIRECTION('',(0.269333009814414,-6.06958927297125E-10,-0.963047106752473));
#56912=DIRECTION('center_axis',(0.211595763952694,-0.60109852801139,-0.770654132733885));
#56913=DIRECTION('ref_axis',(0.969283978718163,0.0279220136873786,0.244354107294985));
#56914=DIRECTION('',(0.871424337485884,2.24206636476427E-10,-0.490529942039513));
#56915=DIRECTION('center_axis',(0.,-1.,1.45983193964168E-32));
#56916=DIRECTION('ref_axis',(1.,0.,0.));
#56917=DIRECTION('center_axis',(-0.208301504811785,0.601098530007901,0.771551061379275));
#56918=DIRECTION('ref_axis',(0.969999731793433,0.0258668087052201,0.241725936812905));
#56919=DIRECTION('center_axis',(-0.120828758075573,-0.601098526589866,0.789987957220493));
#56920=DIRECTION('ref_axis',(0.984886132128416,0.026894408524338,0.171102301361652));
#56921=DIRECTION('center_axis',(0.124202588650017,0.601098528934584,-0.789464549859785));
#56922=DIRECTION('ref_axis',(0.9841461808156,0.0268943571417947,0.175308266604853));
#56923=DIRECTION('center_axis',(-0.146226196689905,0.584827952222654,0.797868514042673));
#56924=DIRECTION('ref_axis',(0.983185511001358,-0.00326197145028403,0.182580422004266));
#56925=DIRECTION('center_axis',(0.146507367971168,-4.95981624200213E-10,
-0.989209578972101));
#56926=DIRECTION('ref_axis',(-0.989087916826879,-0.0156832196309275,-0.146489349131849));
#56927=DIRECTION('',(-0.146507431922664,8.32140417652522E-8,0.989209569500528));
#56928=DIRECTION('center_axis',(-0.180759154061673,0.584827969931817,0.790760629905371));
#56929=DIRECTION('ref_axis',(0.975949872003266,0.0070448013400457,0.217881201830008));
#56930=DIRECTION('center_axis',(-0.208331363027332,3.62541623983424E-10,
0.978058302546006));
#56931=DIRECTION('ref_axis',(-0.977938191179099,0.0156715280542195,-0.208305778704765));
#56932=DIRECTION('',(0.20833131448783,-1.48214773786036E-11,-0.978058312885164));
#56933=DIRECTION('',(0.595880409943404,-3.07809289804292E-8,0.803073182870453));
#56934=DIRECTION('center_axis',(0.603452029474063,0.793626260371976,0.077479074411271));
#56935=DIRECTION('ref_axis',(-0.796019110988665,0.605271488623754,1.14284199043117E-17));
#56936=DIRECTION('center_axis',(-0.690563370774189,0.471546674556346,0.548421338625551));
#56937=DIRECTION('ref_axis',(0.721325537428693,0.393420484789212,0.570008588708476));
#56938=DIRECTION('center_axis',(0.113338614706024,-0.60109852786219,-0.791097287454854));
#56939=DIRECTION('ref_axis',(0.989645761078243,-0.0022757685263134,0.143513373793104));
#56940=DIRECTION('',(0.838904150646891,7.72064248612649E-12,-0.544279180225937));
#56941=DIRECTION('center_axis',(0.,-1.,1.45983193964168E-32));
#56942=DIRECTION('ref_axis',(1.,0.,0.));
#56943=DIRECTION('center_axis',(-0.109958008733103,0.601098527808738,0.791574251843514));
#56944=DIRECTION('ref_axis',(0.990026928638139,-0.00432801871030212,0.140811749599867));
#56945=DIRECTION('center_axis',(-0.120828788033283,-0.601098528090992,0.789987951496256));
#56946=DIRECTION('ref_axis',(0.988871471812975,-0.0033018314369469,0.148735705678233));
#56947=DIRECTION('center_axis',(0.124202574739973,0.601098527983157,-0.789464552772601));
#56948=DIRECTION('ref_axis',(0.988227040359869,-0.00330185589360348,0.15295886521948));
#56949=DIRECTION('center_axis',(-0.0450828641579298,0.584828255987395,0.809903356183971));
#56950=DIRECTION('ref_axis',(0.996298020781173,-0.0330815410804403,0.0793464896971532));
#56951=DIRECTION('center_axis',(0.0840714036549145,-1.08148586559602E-7,
-0.996459732797809));
#56952=DIRECTION('ref_axis',(-0.9963373049844,-0.0156751635312903,-0.0840610727072327));
#56953=DIRECTION('',(-0.0841053488787986,1.16573417585502E-12,0.996456868253702));
#56954=DIRECTION('center_axis',(-0.0802277221050548,0.58482795222607,0.807180140303821));
#56955=DIRECTION('ref_axis',(0.993082001122573,-0.0227607296058987,0.115195868997946));
#56956=DIRECTION('center_axis',(-0.146507507156355,5.90512572813898E-10,
0.989209558358001));
#56957=DIRECTION('ref_axis',(-0.989087738351328,0.0156933905081884,-0.146489464936603));
#56958=DIRECTION('',(0.146507430631042,-2.16493489798574E-11,-0.989209569691827));
#56959=DIRECTION('',(0.64512994617575,0.,0.764072871228441));
#56960=DIRECTION('center_axis',(0.0132942055902067,-0.601098528115421,-0.799064342587754));
#56961=DIRECTION('ref_axis',(0.998629026253513,-0.0324816845862958,0.0410488500496337));
#56962=DIRECTION('',(0.803073192439769,8.15184858242782E-12,-0.595880397046754));
#56963=DIRECTION('center_axis',(0.,-1.,1.45983193964168E-32));
#56964=DIRECTION('ref_axis',(1.,0.,0.));
#56965=DIRECTION('center_axis',(-0.00988039429928425,0.601098525863136,
0.799113846716259));
#56966=DIRECTION('ref_axis',(0.998668148441378,-0.0345385076908348,0.0383278068138463));
#56967=DIRECTION('center_axis',(-0.12082876902967,-0.601098529374135,0.789987953426523));
#56968=DIRECTION('ref_axis',(0.991445777876212,-0.033509983014987,0.126144165817402));
#56969=DIRECTION('center_axis',(0.124202600035381,0.601098526561387,-0.789464549875535));
#56970=DIRECTION('ref_axis',(0.990897829041076,-0.033510034284593,0.130378564204122));
#56971=DIRECTION('',(-0.0213713417384466,-1.22124532708752E-12,0.999771606794421));
#56972=DIRECTION('center_axis',(0.0215713960453859,0.584827952145866,0.810870483654157));
#56973=DIRECTION('ref_axis',(0.998547470580346,-0.052656272850442,0.011413409967822));
#56974=DIRECTION('center_axis',(-0.0841054139654099,4.72602757267682E-10,
0.996456862760103));
#56975=DIRECTION('ref_axis',(-0.996332902031619,0.015772999814619,-0.0840949511332293));
#56976=DIRECTION('',(0.0841053488763018,-1.77691195068295E-10,-0.996456868253913));
#56977=DIRECTION('',(0.691833462135556,-1.43735365432298E-13,0.722057103468645));
#56978=DIRECTION('',(0.764072871250519,6.52763895321776E-11,-0.645129946149602));
#56979=DIRECTION('center_axis',(0.,-1.,1.45983193964168E-32));
#56980=DIRECTION('ref_axis',(1.,0.,0.));
#56981=DIRECTION('center_axis',(-0.102301277609593,0.601098531733207,0.792600153764575));
#56982=DIRECTION('ref_axis',(0.994669900505696,0.051484956462993,0.0893369368514132));
#56983=DIRECTION('center_axis',(-0.0683376730294128,0.601098533636227,-0.796247772559084));
#56984=DIRECTION('ref_axis',(0.997561418616392,0.0525165308253309,-0.0459698822939941));
#56985=DIRECTION('center_axis',(-0.037243854755886,0.584827930051135,0.810301911336156));
#56986=DIRECTION('ref_axis',(0.999306186748226,0.0219594825721155,0.030081992152864));
#56987=DIRECTION('center_axis',(-0.041450461752033,-9.62093338242311E-9,
-0.999140560291966));
#56988=DIRECTION('ref_axis',(-0.999016798817377,-0.0157391393471299,0.0414453275206271));
#56989=DIRECTION('',(0.0414470083237992,-3.88578058618537E-13,0.999140703555314));
#56990=DIRECTION('center_axis',(-0.0724215370767206,0.584827952320712,0.807917933426291));
#56991=DIRECTION('ref_axis',(0.997295367386491,0.0322834330589318,0.0660282525845819));
#56992=DIRECTION('center_axis',(-0.0213713965116663,3.99570979461207E-10,
0.999771605623575));
#56993=DIRECTION('ref_axis',(-0.999648348522012,0.0157020800826844,-0.0213687617397829));
#56994=DIRECTION('',(0.0213713417389734,-8.32667268468203E-13,-0.99977160679441));
#56995=DIRECTION('',(0.735806627488868,0.,0.677191706198074));
#56996=DIRECTION('center_axis',(0.0055695912840324,-0.601098528152127,-0.799155516220889));
#56997=DIRECTION('ref_axis',(0.999673624254888,0.023272368205861,-0.0105376395453706));
#56998=DIRECTION('',(0.722057103468578,1.43735365432649E-13,-0.691833462135626));
#56999=DIRECTION('center_axis',(0.,-1.,1.45983193964168E-32));
#57000=DIRECTION('ref_axis',(1.,0.,0.));
#57001=DIRECTION('center_axis',(-0.0021554625750434,0.601098529555253,0.799172016369192));
#57002=DIRECTION('ref_axis',(0.99968689416083,0.0212180991799879,-0.0132629525469103));
#57003=DIRECTION('center_axis',(0.0717387755805213,-0.601098527369297,0.795948558936236));
#57004=DIRECTION('ref_axis',(0.997078908551603,0.0222452268180101,-0.0730670924928601));
#57005=DIRECTION('center_axis',(-0.0683377528351415,0.601098528633598,-0.796247769486337));
#57006=DIRECTION('ref_axis',(0.997381958361871,0.0222451935625928,-0.0688068346721553));
#57007=DIRECTION('center_axis',(0.0646084828042011,0.584827953016284,0.808580242969443));
#57008=DIRECTION('ref_axis',(0.997226863465737,-0.00784645566254045,-0.0740068639777763));
#57009=DIRECTION('center_axis',(-0.104102226223653,-1.68828436960849E-9,
-0.994566602342588));
#57010=DIRECTION('ref_axis',(-0.994444365115028,-0.0156778483097638,0.104089431564132));
#57011=DIRECTION('',(0.1041017859799,0.,0.994566648423219));
#57012=DIRECTION('center_axis',(0.0294084947975279,0.584827952254149,0.810624084700154));
#57013=DIRECTION('ref_axis',(0.999273620325529,0.00246180457596316,-0.0380285582127298));
#57014=DIRECTION('center_axis',(0.0414469484098936,4.50535560692295E-10,
0.9991407060407));
#57015=DIRECTION('ref_axis',(-0.999018017961886,0.0156707406185484,0.0414418589830465));
#57016=DIRECTION('',(-0.0414470083243479,-6.41708908203792E-11,-0.999140703555291));
#57017=DIRECTION('',(0.776875900241734,1.64268989065426E-13,0.629653742642411));
#57018=DIRECTION('center_axis',(-0.0946350669774392,-0.601098528044088,
-0.793551991794744));
#57019=DIRECTION('ref_axis',(0.993543154944051,-0.00691952431293544,-0.11324362872632));
#57020=DIRECTION('',(0.677191706207041,2.34493981894341E-11,-0.735806627480616));
#57021=DIRECTION('center_axis',(0.,-1.,1.45983193964168E-32));
#57022=DIRECTION('ref_axis',(1.,0.,0.));
#57023=DIRECTION('center_axis',(0.0980243639266851,0.601098527314582,0.793140457004313));
#57024=DIRECTION('ref_axis',(0.993214310825923,-0.00897204908649078,-0.115951865469155));
#57025=DIRECTION('center_axis',(0.0717387832098065,-0.601098528296013,0.795948557548755));
#57026=DIRECTION('ref_axis',(0.995377175937633,-0.00794572215068903,-0.0957138606573088));
#57027=DIRECTION('center_axis',(-0.0683377344053666,0.601098527687643,-0.796247771782182));
#57028=DIRECTION('ref_axis',(0.995776990652027,-0.00794577121283169,-0.0914606451312635));
#57029=DIRECTION('center_axis',(0.165441105021194,0.584827952230366,0.794106735306661));
#57030=DIRECTION('ref_axis',(0.981404269600449,-0.0181546317031915,-0.191091781502323));
#57031=DIRECTION('center_axis',(-0.166345660993045,4.80436704184032E-10,
-0.986067503302277));
#57032=DIRECTION('ref_axis',(-0.98594628501969,-0.0156795066154144,0.16632521194386));
#57033=DIRECTION('',(0.166345718259841,2.06171493653946E-7,0.986067493641574));
#57034=DIRECTION('center_axis',(0.130780879082784,0.58482778253619,0.800545330659131));
#57035=DIRECTION('ref_axis',(0.989535715163695,-0.0273551074326196,-0.141671332713516));
#57036=DIRECTION('center_axis',(0.104101686357031,6.71216382327904E-10,
0.994566658850789));
#57037=DIRECTION('ref_axis',(-0.994444039572659,0.0157023279254252,0.104088851737994));
#57038=DIRECTION('',(0.104101785049356,-1.29267411913885E-5,0.994566648436613));
#57039=DIRECTION('',(0.814879221760606,-7.62629077551079E-8,0.57963079105826));
#57040=DIRECTION('center_axis',(-0.166345721435314,8.38219850921266E-12,
-0.986067493105906));
#57041=DIRECTION('ref_axis',(-0.761122075632713,-0.635772805085135,0.128398311121022));
#57042=DIRECTION('',(-0.629653742643417,0.,0.776875900240919));
#57043=DIRECTION('center_axis',(0.206207729991539,0.398564391592221,0.893658098965404));
#57044=DIRECTION('ref_axis',(7.977868849158E-17,-0.913286229119169,0.407318381246525));
#57045=DIRECTION('center_axis',(-0.234739006541716,5.74456595838224E-5,
-0.972058432146856));
#57046=DIRECTION('ref_axis',(0.972058374620108,0.000362947015312071,-0.234738971200731));
#57047=DIRECTION('',(0.227932275687214,5.94973691934203E-5,0.973676986561822));
#57048=DIRECTION('center_axis',(0.119644660393128,0.590180063811167,0.798356215933251));
#57049=DIRECTION('ref_axis',(0.252209298373921,-0.795820738081259,0.550508694439547));
#57050=DIRECTION('center_axis',(0.817786253531608,0.550037558024095,0.169364483577954));
#57051=DIRECTION('ref_axis',(-0.558100160389067,0.829773590188129,8.72788992253708E-17));
#57052=DIRECTION('center_axis',(-0.463417276442099,-0.477126090650508,0.746722921514768));
#57053=DIRECTION('ref_axis',(0.816467047629943,0.097624951635498,0.569079018197482));
#57054=DIRECTION('center_axis',(-0.340054078922432,0.584827951389632,0.736437024246896));
#57055=DIRECTION('ref_axis',(0.915422295871966,0.0265489690047848,0.401618192398304));
#57056=DIRECTION('center_axis',(0.329271775058143,2.52786593772104E-11,
-0.944235192179396));
#57057=DIRECTION('ref_axis',(-0.944118103453684,-0.0157477670564997,-0.329230944116365));
#57058=DIRECTION('center_axis',(-0.379507052682398,-0.000115441210108468,
0.925188836745043));
#57059=DIRECTION('ref_axis',(0.0230779722542089,-0.999690021762026,0.00934171215969518));
#57060=DIRECTION('',(0.387911046550329,-6.06126260028195E-10,-0.921696815641797));
#57061=DIRECTION('center_axis',(0.306515840649688,-0.601098528069313,-0.738057314159084));
#57062=DIRECTION('ref_axis',(0.931015195264333,0.0279220124474747,0.3639107959484));
#57063=DIRECTION('',(0.926032600098742,2.24206636476434E-10,-0.377443536908983));
#57064=DIRECTION('center_axis',(0.,-1.,1.45983193964168E-32));
#57065=DIRECTION('ref_axis',(1.,0.,0.));
#57066=DIRECTION('center_axis',(-0.30335997485622,0.60109852999791,0.739360049562854));
#57067=DIRECTION('ref_axis',(0.932054700806224,0.0258668088583444,0.361393058738691));
#57068=DIRECTION('center_axis',(-0.218887725620292,-0.601098526393931,0.768614809341988));
#57069=DIRECTION('ref_axis',(0.955675207654525,0.0268944127803095,0.293192066802092));
#57070=DIRECTION('center_axis',(0.222169359871822,0.60109852895906,-0.767672673746694));
#57071=DIRECTION('ref_axis',(0.954413942092609,0.0268943565695278,0.297272132437531));
#57072=DIRECTION('center_axis',(-0.245072600278341,0.584827952222495,0.773250080434561));
#57073=DIRECTION('ref_axis',(0.952549404908284,-0.00326197144980148,0.304366540130703));
#57074=DIRECTION('center_axis',(0.269332938029609,-5.8483345689954E-10,
-0.963047126828349));
#57075=DIRECTION('ref_axis',(-0.962928682384874,-0.0156832196315011,-0.269299812964139));
#57076=DIRECTION('',(-0.269333011080849,8.32135976759878E-8,0.963047106398288));
#57077=DIRECTION('center_axis',(-0.278442400876454,0.584827969931489,0.761870116870303));
#57078=DIRECTION('ref_axis',(0.940946460198289,0.00704480134837665,0.338482096741131));
#57079=DIRECTION('center_axis',(-0.329271851742164,6.46313079915493E-10,
0.944235165438296));
#57080=DIRECTION('ref_axis',(-0.944119207751262,0.015671528054241,-0.329231415213636));
#57081=DIRECTION('',(0.329271770815587,-1.32671651441181E-11,-0.944235193658851));
#57082=DIRECTION('',(0.490529956132169,-3.07809289804332E-8,0.871424329553044));
#57083=DIRECTION('center_axis',(0.588982927050323,0.793626260371225,0.15250072292425));
#57084=DIRECTION('ref_axis',(-0.803018883933449,0.595953582123875,-1.43142346962412E-16));
#57085=DIRECTION('center_axis',(-0.753853492062759,0.471546674560884,0.457546332315489));
#57086=DIRECTION('ref_axis',(0.64419412264145,0.39340505448244,0.655931700302616));
#57087=DIRECTION('center_axis',(0.211595757716834,-0.601098528031622,-0.770654134430262));
#57088=DIRECTION('ref_axis',(0.963855097930843,-0.00227572441773332,0.26641728786079));
#57089=DIRECTION('',(0.900505410469431,5.19500677922309E-12,-0.434844806471553));
#57090=DIRECTION('center_axis',(0.,-1.,1.45983193964168E-32));
#57091=DIRECTION('ref_axis',(1.,0.,0.));
#57092=DIRECTION('center_axis',(-0.208301530005171,0.601098527857505,0.771551056252952));
#57093=DIRECTION('ref_axis',(0.96457187601466,-0.0043280109716603,0.263784693116541));
#57094=DIRECTION('center_axis',(-0.218887748539973,-0.601098528126118,0.768614801460209));
#57095=DIRECTION('ref_axis',(0.962432400878757,-0.00330182340838835,0.271501329096068));
#57096=DIRECTION('center_axis',(0.222169344354683,0.601098527988436,-0.767672678997465));
#57097=DIRECTION('ref_axis',(0.961263746067348,-0.00330185516210308,0.275610428411295));
#57098=DIRECTION('center_axis',(-0.146235178803069,0.584828255987149,0.797866645172904));
#57099=DIRECTION('ref_axis',(0.978497161183396,-0.0330815410865203,0.203590071455794));
#57100=DIRECTION('center_axis',(0.208297997691912,-1.08134170125211E-7,
-0.978065408936196));
#57101=DIRECTION('ref_axis',(-0.977945241313742,-0.0156751635311632,-0.208272403933114));
#57102=DIRECTION('',(-0.20833131448759,0.,0.978058312885215));
#57103=DIRECTION('center_axis',(-0.180761599633245,0.584827952226279,0.790760083965325));
#57104=DIRECTION('ref_axis',(0.970813382164798,-0.0227607295898355,0.238753693580401));
#57105=DIRECTION('center_axis',(-0.269333108956724,7.92216648094451E-10,
0.963047079025582));
#57106=DIRECTION('ref_axis',(-0.962928480895791,0.0156933905078548,-0.269299940909932));
#57107=DIRECTION('',(0.269333009823161,-2.16493489798119E-11,-0.963047106750027));
#57108=DIRECTION('',(0.544279180229334,0.,0.838904150644687));
#57109=DIRECTION('center_axis',(0.113338686509647,-0.601098527841723,-0.791097277183269));
#57110=DIRECTION('ref_axis',(0.985609753935629,-0.0324816895753882,0.165886566030155));
#57111=DIRECTION('',(0.871424337430542,8.17238220606246E-12,-0.490529942137829));
#57112=DIRECTION('center_axis',(0.,-1.,1.45983193964168E-32));
#57113=DIRECTION('ref_axis',(1.,0.,0.));
#57114=DIRECTION('center_axis',(-0.109958010163819,0.60109852597944,0.791574253033889));
#57115=DIRECTION('ref_axis',(0.985989603468124,-0.034538505663073,0.163191891585745));
#57116=DIRECTION('center_axis',(-0.218887753379354,-0.601098529013112,0.768614799388362));
#57117=DIRECTION('ref_axis',(0.967817873192568,-0.0335099896073441,0.249410595054682));
#57118=DIRECTION('center_axis',(0.222169363956345,0.601098526776724,-0.767672674273408));
#57119=DIRECTION('ref_axis',(0.966743538100934,-0.0335100303655534,0.25354291432613));
#57120=DIRECTION('',(-0.146507430631127,1.1657341758556E-12,0.989209569691815));
#57121=DIRECTION('center_axis',(-0.0802277205987724,0.584827952146903,0.807180140510893));
#57122=DIRECTION('ref_axis',(0.989243145943866,-0.0526562728355991,0.136474595196858));
#57123=DIRECTION('center_axis',(-0.208331408096651,7.10677786846695E-10,
0.978058292946012));
#57124=DIRECTION('ref_axis',(-0.977936621025492,0.0157729998146215,-0.208305491368066));
#57125=DIRECTION('',(0.208331314485092,-1.75748304775633E-10,-0.978058312885747));
#57126=DIRECTION('',(0.59588039705036,0.,0.803073192437093));
#57127=DIRECTION('',(0.838904150663342,6.51326541667559E-11,-0.544279180200581));
#57128=DIRECTION('center_axis',(0.,-1.,1.45983193964168E-32));
#57129=DIRECTION('ref_axis',(1.,0.,0.));
#57130=DIRECTION('center_axis',(-0.200833745921226,0.60109853150529,0.773528513967929));
#57131=DIRECTION('ref_axis',(0.975629743199405,0.0514849590709439,0.213297686752872));
#57132=DIRECTION('center_axis',(0.0319974973800043,0.601098533599825,-0.798534102631539));
#57133=DIRECTION('ref_axis',(0.995456902887003,0.0525165311962358,0.0794202017482328));
#57134=DIRECTION('center_axis',(-0.138507934550866,0.584827930050956,0.799244545992506));
#57135=DIRECTION('ref_axis',(0.987656085638451,0.0219594825737406,0.155091062367971));
#57136=DIRECTION('center_axis',(0.08410187096805,-9.88649956170652E-9,-0.996457161798576));
#57137=DIRECTION('ref_axis',(-0.996333732730334,-0.0157391393484628,-0.0840914532887217));
#57138=DIRECTION('',(-0.0841053488788927,-7.77156117238321E-13,0.996456868253694));
#57139=DIRECTION('center_axis',(-0.17310943869208,0.584827952319961,0.792470433783466));
#57140=DIRECTION('ref_axis',(0.981155861131183,0.0322834330681012,0.190501853317139));
#57141=DIRECTION('center_axis',(-0.146507509371627,5.94611736450723E-10,
0.989209558029906));
#57142=DIRECTION('ref_axis',(-0.989087603071883,0.0157020800827092,-0.146489447164611));
#57143=DIRECTION('',(0.146507430631453,-1.22124532708676E-12,-0.989209569691767));
#57144=DIRECTION('',(0.645129946175734,0.,0.764072871228454));
#57145=DIRECTION('center_axis',(0.105686425993003,-0.601098527976467,-0.792155880509228));
#57146=DIRECTION('ref_axis',(0.993111614765757,0.0232723728235476,0.114837786814762));
#57147=DIRECTION('',(0.803073192437276,0.,-0.595880397050114));
#57148=DIRECTION('center_axis',(0.,-1.,1.45983193964168E-32));
#57149=DIRECTION('ref_axis',(1.,0.,0.));
#57150=DIRECTION('center_axis',(-0.10230128097518,0.601098529510368,0.792600155015952));
#57151=DIRECTION('ref_axis',(0.993466352943827,0.0212181003141552,0.112135622295283));
#57152=DIRECTION('center_axis',(-0.0285857038531819,-0.601098527168134,
0.798663519995448));
#57153=DIRECTION('ref_axis',(0.998374378768266,0.0222452321645403,0.0524761799774345));
#57154=DIRECTION('center_axis',(0.0319974136827314,0.601098528532173,-0.798534109799996));
#57155=DIRECTION('ref_axis',(0.998141086949402,0.0222451964194356,0.056740829917499));
#57156=DIRECTION('center_axis',(-0.0372429508028461,0.584827953016271,0.810301936309112));
#57157=DIRECTION('ref_axis',(0.9986389513593,-0.00784645567732753,0.0515623696245816));
#57158=DIRECTION('center_axis',(0.0213710252196031,-6.99985568850361E-10,
-0.999771613560349));
#57159=DIRECTION('ref_axis',(-0.999648736613809,-0.0156778483084573,-0.0213683986024217));
#57160=DIRECTION('',(-0.0213713417383099,-4.44089209849764E-13,0.999771606794424));
#57161=DIRECTION('center_axis',(-0.0724215376820377,0.584827952254425,0.807917933420013));
#57162=DIRECTION('ref_axis',(0.99616029153121,0.00246180456054646,0.0875135023568358));
#57163=DIRECTION('center_axis',(-0.084105442047678,7.13530268223119E-10,
0.996456860389834));
#57164=DIRECTION('ref_axis',(-0.996334501868839,0.0156707406187732,-0.0840951144492399));
#57165=DIRECTION('',(0.0841053488781944,-6.4226401971558E-11,-0.996456868253753));
#57166=DIRECTION('',(0.691833462135674,1.64268989065485E-13,0.722057103468532));
#57167=DIRECTION('center_axis',(0.00556959465845934,-0.601098528032363,
-0.799155516287454));
#57168=DIRECTION('ref_axis',(0.999901960586244,-0.0069195250739992,0.0121733063928809));
#57169=DIRECTION('',(0.764072871236398,2.34493981894309E-11,-0.645129946166326));
#57170=DIRECTION('center_axis',(0.,-1.,1.45983193964168E-32));
#57171=DIRECTION('ref_axis',(1.,0.,0.));
#57172=DIRECTION('center_axis',(-0.00215545266561574,0.601098527372563,
0.799172018037633));
#57173=DIRECTION('ref_axis',(0.999915141548093,-0.00897204484915501,0.00944521646556398));
#57174=DIRECTION('center_axis',(-0.0285856996086749,-0.601098528338824,
0.798663519266269));
#57175=DIRECTION('ref_axis',(0.999524457407752,-0.00794571891958214,0.0297947074929481));
#57176=DIRECTION('center_axis',(0.0319974503381975,0.6010985275747,-0.798534109051944));
#57177=DIRECTION('ref_axis',(0.99938804962766,-0.00794577923852444,0.0340645101786992));
#57178=DIRECTION('center_axis',(0.0646085875664995,0.584827952230155,0.808580235167139));
#57179=DIRECTION('ref_axis',(0.997615754687303,-0.0181546317371957,-0.0665823951669649));
#57180=DIRECTION('center_axis',(-0.0414482896573108,-3.66455749607626E-9,
-0.999140650401376));
#57181=DIRECTION('ref_axis',(-0.999017825024053,-0.0156795063469686,0.0414431944343749));
#57182=DIRECTION('',(0.0414470050956375,2.06171105075987E-7,0.999140703689205));
#57183=DIRECTION('center_axis',(0.0294146978912214,0.584827782535925,0.810623982079288));
#57184=DIRECTION('ref_axis',(0.999489056721735,-0.0273551074375189,-0.0165325010382245));
#57185=DIRECTION('center_axis',(-0.0213714686382134,8.82110719332692E-10,
0.999771604081775));
#57186=DIRECTION('ref_axis',(-0.999648343088967,0.0157023279257171,-0.021368833781832));
#57187=DIRECTION('',(-0.0213713426633531,-1.29267419730502E-5,0.999771606691081));
#57188=DIRECTION('',(0.735806654387714,-7.62629077551357E-8,0.677191676970969));
#57189=DIRECTION('center_axis',(-0.0414472069397243,-1.61525008678803E-7,
-0.999140695316165));
#57190=DIRECTION('ref_axis',(-0.771212966511826,-0.635772804014447,0.0319922171728849));
#57191=DIRECTION('',(-0.722057103469967,0.,0.691833462134176));
#57192=DIRECTION('center_axis',(0.0925766612049255,0.39856439159139,0.912456019518494));
#57193=DIRECTION('ref_axis',(-1.04051723405416E-16,-0.916391407625922,0.40028338465315));
#57194=DIRECTION('center_axis',(-0.111056792829436,5.74456674606717E-5,
-0.993814059805171));
#57195=DIRECTION('ref_axis',(0.993813998287295,0.000362990317359139,-0.111056764972918));
#57196=DIRECTION('',(0.104100876440593,5.94973699395232E-5,0.994566741845093));
#57197=DIRECTION('center_axis',(0.0186406606636707,0.590180063817314,0.807056390869072));
#57198=DIRECTION('ref_axis',(0.181219010772305,-0.795821359149822,0.577778534090387));
#57199=DIRECTION('center_axis',(0.790110766284182,0.550037558023235,0.270524789558478));
#57200=DIRECTION('ref_axis',(-0.571341150189064,0.820712672072655,1.13123986132218E-16));
#57201=DIRECTION('center_axis',(-0.553352291407227,-0.477126089849265,0.682753202833588));
#57202=DIRECTION('ref_axis',(0.73870537475839,0.0976228476931799,0.666921396351429));
#57203=DIRECTION('center_axis',(-0.429672684490192,0.584827951390324,0.688009921058984));
#57204=DIRECTION('ref_axis',(0.857867810942039,0.0265489689937178,0.513184149399496));
#57205=DIRECTION('center_axis',(0.44501941704254,-1.263031542495E-11,-0.895520920166088));
#57206=DIRECTION('ref_axis',(-0.895409872194088,-0.0157477670560035,-0.444964232955994));
#57207=DIRECTION('center_axis',(-0.492471439238968,-0.000115441170765423,
0.870328597833736));
#57208=DIRECTION('ref_axis',(0.0217041865571253,-0.999690621869625,0.0121486143990027));
#57209=DIRECTION('',(0.500371494355022,-6.08124661472372E-10,-0.865810815153589));
#57210=DIRECTION('center_axis',(0.396601983992574,-0.601098527988962,-0.693820888949488));
#57211=DIRECTION('ref_axis',(0.878063744427938,0.0279220141999334,0.47772839756938));
#57212=DIRECTION('',(0.966036775423212,2.24062901110976E-10,-0.258404621727094));
#57213=DIRECTION('center_axis',(0.,-1.,1.45983193964168E-32));
#57214=DIRECTION('ref_axis',(1.,0.,0.));
#57215=DIRECTION('center_axis',(-0.393634287432195,0.601098529677143,0.69550888231404));
#57216=DIRECTION('ref_axis',(0.879410605621152,0.0258668162395267,0.475360804588124));
#57217=DIRECTION('center_axis',(-0.313494723667525,-0.601098526808639,0.735120139365741));
#57218=DIRECTION('ref_axis',(0.911392708689532,0.0268944037202345,0.410658034861234));
#57219=DIRECTION('center_axis',(0.316632373895327,0.601098528588605,-0.733774146948517));
#57220=DIRECTION('ref_axis',(0.909630029913998,0.0268943649857957,0.414547828134064));
#57221=DIRECTION('center_axis',(-0.340054062561776,0.584827952222567,0.736437031140063));
#57222=DIRECTION('ref_axis',(0.906891025673923,-0.00326197144877692,0.421352616100064));
#57223=DIRECTION('center_axis',(0.387910953050161,-7.94897451911712E-10,
-0.921696854992853));
#57224=DIRECTION('ref_axis',(-0.921583496190756,-0.0156832196313773,-0.387863244160642));
#57225=DIRECTION('',(-0.387911047762012,8.32148189213521E-8,0.921696815131837));
#57226=DIRECTION('center_axis',(-0.371734444666745,0.584827969931767,0.720964456983695));
#57227=DIRECTION('ref_axis',(0.891103760630804,0.00704480133835922,0.453744926763641));
#57228=DIRECTION('center_axis',(-0.445019486730157,6.04376373905928E-10,
0.895520885535579));
#57229=DIRECTION('ref_axis',(-0.895410910250426,0.0156715280542697,-0.444964835703843));
#57230=DIRECTION('',(0.44501941462051,-1.52100554372157E-11,-0.89552092136969));
#57231=DIRECTION('',(0.377443551884433,-3.07807852450739E-8,0.926032593994867));
#57232=DIRECTION('center_axis',(0.565225212024928,0.793626260371114,0.22511734393586));
#57233=DIRECTION('ref_axis',(-0.814533996871954,0.580115822866261,8.98799277858797E-17));
#57234=DIRECTION('center_axis',(-0.805254893437658,0.471546674537444,0.359455547081114));
#57235=DIRECTION('ref_axis',(0.556903411321164,0.393401148446506,0.731501282883237));
#57236=DIRECTION('center_axis',(0.306515838186029,-0.601098528034889,-0.738057315210279));
#57237=DIRECTION('ref_axis',(0.922863871900687,-0.00227572338068341,0.38511958535443));
#57238=DIRECTION('',(0.947905162033646,5.19500677922244E-12,-0.318552670354477));
#57239=DIRECTION('center_axis',(0.,-1.,1.45983193964168E-32));
#57240=DIRECTION('ref_axis',(1.,0.,0.));
#57241=DIRECTION('center_axis',(-0.303359993099232,0.601098527830073,0.73936004384018));
#57242=DIRECTION('ref_axis',(0.92390495204079,-0.0043280147898287,0.38259757955649));
#57243=DIRECTION('center_axis',(-0.31349473879885,-0.601098528107193,0.735120131851119));
#57244=DIRECTION('ref_axis',(0.920815192023725,-0.00330182805213655,0.389985230579088));
#57245=DIRECTION('center_axis',(0.316632370525574,0.601098527993511,-0.733774148890099));
#57246=DIRECTION('ref_axis',(0.919140748588481,-0.00330185426789301,0.393915450373046));
#57247=DIRECTION('center_axis',(-0.245081277370425,0.584828255988135,0.773247100531491));
#57248=DIRECTION('ref_axis',(0.945264816817517,-0.0330815410633406,0.32462291620867));
#57249=DIRECTION('center_axis',(0.329239579421866,-1.08354798316671E-7,
-0.944246418760538));
#57250=DIRECTION('ref_axis',(-0.944130406444208,-0.0156751635322327,-0.329199126480815));
#57251=DIRECTION('',(-0.329271770815384,1.22124532708837E-12,0.944235193658922));
#57252=DIRECTION('center_axis',(-0.278444758713474,0.584827952226039,0.761869268733222));
#57253=DIRECTION('ref_axis',(0.933234456240481,-0.0227607295977756,0.358546229758049));
#57254=DIRECTION('center_axis',(-0.387911125646508,6.56837119634826E-10,
0.921696782352884));
#57255=DIRECTION('ref_axis',(-0.921583276463325,0.0156933905082965,-0.387863354852553));
#57256=DIRECTION('',(0.387911046558472,-2.28705943069176E-11,-0.92169681563837));
#57257=DIRECTION('',(0.434844806474066,0.,0.900505410468217));
#57258=DIRECTION('center_axis',(0.211595754170762,-0.601098527745205,-0.770654135627296));
#57259=DIRECTION('ref_axis',(0.957046827522298,-0.0324816913084358,0.288108156183139));
#57260=DIRECTION('',(0.926032600056353,8.00811321699569E-12,-0.377443537012983));
#57261=DIRECTION('center_axis',(0.,-1.,1.45983193964168E-32));
#57262=DIRECTION('ref_axis',(1.,0.,0.));
#57263=DIRECTION('center_axis',(-0.208301522446814,0.601098526095677,0.771551059666141));
#57264=DIRECTION('ref_axis',(0.957761412761915,-0.0345385035991132,0.28548234269992));
#57265=DIRECTION('center_axis',(-0.313494748360086,-0.601098528584498,0.735120127383408));
#57266=DIRECTION('ref_axis',(0.928926899735521,-0.0335099974581725,0.36874367115668));
#57267=DIRECTION('center_axis',(0.316632396784893,0.601098526555786,-0.733774138736653));
#57268=DIRECTION('ref_axis',(0.927343121189809,-0.0335100342769605,0.372708751151217));
#57269=DIRECTION('',(-0.269333009823004,1.16573417585691E-12,0.96304710675007));
#57270=DIRECTION('center_axis',(-0.180761598123538,0.5848279521463,0.790760084369583));
#57271=DIRECTION('ref_axis',(0.964337865952839,-0.0526562728443061,0.25938349450123));
#57272=DIRECTION('center_axis',(-0.329271845805718,5.83638447949411E-10,
0.944235167508442));
#57273=DIRECTION('ref_axis',(-0.944117703234743,0.0157729998148134,-0.329230883903067));
#57274=DIRECTION('',(0.329271770813222,-1.76914038951379E-10,-0.944235193659676));
#57275=DIRECTION('',(0.490529942141599,0.,0.871424337428419));
#57276=DIRECTION('',(0.900505410483596,6.72270837774942E-11,-0.434844806442219));
#57277=DIRECTION('center_axis',(0.,-1.,1.45983193964168E-32));
#57278=DIRECTION('ref_axis',(1.,0.,0.));
#57279=DIRECTION('center_axis',(-0.296198939617034,0.601098531624116,0.74225786856663));
#57280=DIRECTION('ref_axis',(0.941203323148457,0.0514849577008644,0.333894599574238));
#57281=DIRECTION('center_axis',(0.13182805295787,0.601098533827196,-0.788227072031995));
#57282=DIRECTION('ref_axis',(0.977653436616125,0.0525165286099951,0.203557785641906));
#57283=DIRECTION('center_axis',(-0.237587661479048,0.584827930050785,0.775582616711741));
#57284=DIRECTION('ref_axis',(0.960430058059983,0.0219594825764484,0.277654253883985));
#57285=DIRECTION('center_axis',(0.208327868813298,-1.01451858201418E-8,
-0.978059046824735));
#57286=DIRECTION('ref_axis',(-0.977937896713006,-0.0157391393483165,-0.208302063516224));
#57287=DIRECTION('',(-0.208331314487397,1.22124532708716E-12,0.978058312885256));
#57288=DIRECTION('center_axis',(-0.271067301023581,0.584827952320365,0.764525202004853));
#57289=DIRECTION('ref_axis',(0.94954294083552,0.0322834330622836,0.311971126002302));
#57290=DIRECTION('center_axis',(-0.269333079626839,5.38133350324857E-10,
0.963047087228201));
#57291=DIRECTION('ref_axis',(-0.962928357716265,0.0157020800824384,-0.269299874836475));
#57292=DIRECTION('',(0.269333009823372,0.,-0.963047106749968));
#57293=DIRECTION('',(0.544279180229277,0.,0.838904150644725));
#57294=DIRECTION('center_axis',(0.204136518769429,-0.601098527889654,-0.772663472330347));
#57295=DIRECTION('ref_axis',(0.970887641095373,0.0232723751933657,0.238402149573196));
#57296=DIRECTION('',(0.871424337428443,0.,-0.490529942141556));
#57297=DIRECTION('center_axis',(0.,-1.,1.45983193964168E-32));
#57298=DIRECTION('ref_axis',(1.,0.,0.));
#57299=DIRECTION('center_axis',(-0.200833748756779,0.601098529431724,0.773528514843065));
#57300=DIRECTION('ref_axis',(0.971578253134806,0.0212181025282827,0.235765752730581));
#57301=DIRECTION('center_axis',(-0.128459387649655,-0.601098527378134,0.788783079248353));
#57302=DIRECTION('ref_axis',(0.983924888080242,0.0222452265883128,0.177191886130033));
#57303=DIRECTION('center_axis',(0.131827962105105,0.6010985284313,-0.788227091341664));
#57304=DIRECTION('ref_axis',(0.983158935264301,0.0222451991726764,0.18139365789281));
#57305=DIRECTION('center_axis',(-0.13850704083771,0.584827953016387,0.799244684066803));
#57306=DIRECTION('ref_axis',(0.98430190643568,-0.00784645568629959,0.176318433863986));
#57307=DIRECTION('center_axis',(0.146507087593992,-9.36218342805786E-10,
-0.989209620497459));
#57308=DIRECTION('ref_axis',(-0.989088041674773,-0.015677848308132,-0.146489081123439));
#57309=DIRECTION('',(-0.14650743063097,-3.88578058618891E-13,0.989209569691838));
#57310=DIRECTION('center_axis',(-0.173109439351868,0.584827952253358,0.792470433688492));
#57311=DIRECTION('ref_axis',(0.977336919849494,0.00246180460537174,0.211675422799128));
#57312=DIRECTION('center_axis',(-0.208331386153898,5.54965824874705E-10,
0.97805829761993));
#57313=DIRECTION('ref_axis',(-0.977938198323729,0.0156707406186644,-0.208305804402567));
#57314=DIRECTION('',(0.208331314486879,-6.46149800301645E-11,-0.978058312885366));
#57315=DIRECTION('',(0.595880397050194,1.64268989065517E-13,0.803073192437217));
#57316=DIRECTION('center_axis',(0.105686416211157,-0.601098527992137,-0.792155881802394));
#57317=DIRECTION('ref_axis',(0.990491715704822,-0.00691952841778068,0.137398257800428));
#57318=DIRECTION('',(0.838904150651368,2.34493981894334E-11,-0.544279180219037));
#57319=DIRECTION('center_axis',(0.,-1.,1.45983193964168E-32));
#57320=DIRECTION('ref_axis',(1.,0.,0.));
#57321=DIRECTION('center_axis',(-0.102301275627061,0.601098527426145,0.792600157286886));
#57322=DIRECTION('ref_axis',(0.99084671183987,-0.00897204111701711,0.134693341016966));
#57323=DIRECTION('center_axis',(-0.128459379962898,-0.601098528294563,0.788783079801829));
#57324=DIRECTION('ref_axis',(0.987908640739109,-0.00794572241207701,0.154833404174798));
#57325=DIRECTION('center_axis',(0.131827982572337,0.601098527746006,-0.7882270884412));
#57326=DIRECTION('ref_axis',(0.987238163854929,-0.00794576686894387,0.159052420972501));
#57327=DIRECTION('center_axis',(-0.0372428459221002,0.584827952230008,0.810301941697092));
#57328=DIRECTION('ref_axis',(0.99809424337453,-0.0181546317010637,0.0589770352800358));
#57329=DIRECTION('center_axis',(0.0841052618395418,-6.64941428738438E-10,
-0.996456875600195));
#57330=DIRECTION('ref_axis',(-0.996334380141064,-0.0156795066176087,-0.0840949226835356));
#57331=DIRECTION('',(-0.0841053520982985,2.0617116058726E-7,0.996456867981941));
#57332=DIRECTION('center_axis',(-0.0724153706974204,0.584827782536221,0.807918609056953));
#57333=DIRECTION('ref_axis',(0.993679858788329,-0.0273551074191281,0.108867058086894));
#57334=DIRECTION('center_axis',(-0.146507522166042,6.11855090107436E-10,
0.989209556134981));
#57335=DIRECTION('ref_axis',(-0.989087597326991,0.0157023279255864,-0.146489459387487));
#57336=DIRECTION('',(-0.146507431535708,-1.29267420441721E-5,0.98920956947338));
#57337=DIRECTION('',(0.645129976525409,-7.62630514905186E-8,0.764072845603297));
#57338=DIRECTION('center_axis',(0.0841053482901251,-4.80180366554845E-10,
-0.996456868303389));
#57339=DIRECTION('ref_axis',(-0.769141387593958,-0.635772805081689,-0.0649189202667612));
#57340=DIRECTION('',(-0.803073192438327,0.,0.595880397048698));
#57341=DIRECTION('center_axis',(-0.0225143968314784,0.398564391590973,0.916863963568769));
#57342=DIRECTION('ref_axis',(1.32509733837405E-17,-0.917096430234536,0.398665445770097));
#57343=DIRECTION('center_axis',(0.0143768528772085,5.74456683306679E-5,
-0.999896646059653));
#57344=DIRECTION('ref_axis',(0.99989658156764,0.000362902000896798,0.0143768727992233));
#57345=DIRECTION('',(-0.0213722558148664,5.94973699395278E-5,0.999771585484128));
#57346=DIRECTION('center_axis',(-0.0826573138804223,0.590180063811489,0.803028804428297));
#57347=DIRECTION('ref_axis',(0.107377222157672,-0.795821081622156,0.595935347338487));
#57348=DIRECTION('center_axis',(0.749974760262434,0.550037558024859,0.367418758001486));
#57349=DIRECTION('ref_axis',(-0.591402864737045,0.806376246910099,3.44718433429239E-16));
#57350=DIRECTION('center_axis',(-0.634560609802729,-0.477126090219829,0.608016057779997));
#57351=DIRECTION('ref_axis',(0.649293907906614,0.097621054247684,0.754246346310626));
#57352=DIRECTION('center_axis',(-0.512515095180752,0.584827951389499,0.628732490400669));
#57353=DIRECTION('ref_axis',(0.786784238152812,0.0265489690042029,0.616656885828021));
#57354=DIRECTION('center_axis',(0.55374883837593,-1.94416449583736E-11,
-0.832683747888301));
#57355=DIRECTION('ref_axis',(-0.832580491962753,-0.0157477670575025,-0.553680171430911));
#57356=DIRECTION('center_axis',(-0.597669249882254,-0.000115441202897984,
0.801742760752171));
#57357=DIRECTION('ref_axis',(0.0200236790427926,-0.999690210189126,0.0147829607864248));
#57358=DIRECTION('',(0.604940784786562,-6.06070748877474E-10,-0.79627046089995));
#57359=DIRECTION('center_axis',(0.480433465069761,-0.601098528305781,-0.638642501646804));
#57360=DIRECTION('ref_axis',(0.811264710240501,0.0279220072711538,0.58401192747096));
#57361=DIRECTION('',(0.990805973716838,2.24350371841898E-10,-0.135290511297095));
#57362=DIRECTION('center_axis',(0.,-1.,1.45983193964168E-32));
#57363=DIRECTION('ref_axis',(1.,0.,0.));
#57364=DIRECTION('center_axis',(-0.477700744076694,0.601098529565722,0.640689126536809));
#57365=DIRECTION('ref_axis',(0.812897681593187,0.0258668187358074,0.581831820158464));
#57366=DIRECTION('center_axis',(-0.403157705739844,-0.601098526727984,0.690032191617197));
#57367=DIRECTION('ref_axis',(0.852737006755842,0.0268944054952872,0.521647666784911));
#57368=DIRECTION('center_axis',(0.406101919085641,0.601098528571327,-0.688303559677229));
#57369=DIRECTION('ref_axis',(0.850500705913757,0.0268943653428166,0.52528586726944));
#57370=DIRECTION('center_axis',(-0.429672669136689,0.584827952222573,0.688009929940045));
#57371=DIRECTION('ref_axis',(0.846930433215634,-0.00326197144994845,0.531693709606798));
#57372=DIRECTION('center_axis',(0.500371425977371,-6.18913571759043E-10,
-0.865810854670564));
#57373=DIRECTION('ref_axis',(-0.86570436924588,-0.015683219630985,-0.500309885661476));
#57374=DIRECTION('',(-0.500371495493563,8.32124319419546E-8,0.865810814495596));
#57375=DIRECTION('center_axis',(-0.459164014240661,0.584827969931258,0.668688756905995));
#57376=DIRECTION('ref_axis',(0.827207822420984,0.00704480135458538,0.561851928268835));
#57377=DIRECTION('center_axis',(-0.553748923309602,7.92180262186616E-10,
0.832683691405961));
#57378=DIRECTION('ref_axis',(-0.83258143289862,0.0156715280539033,-0.55368091966487));
#57379=DIRECTION('',(0.553748836415073,-1.48214773785855E-11,-0.832683749192304));
#57380=DIRECTION('',(0.258404637349547,-3.07809289804395E-8,0.96603677124437));
#57381=DIRECTION('center_axis',(0.532553557756658,0.793626260371024,0.294183729954989));
#57382=DIRECTION('ref_axis',(-0.830371106911542,0.557210754388769,8.10631680189143E-17));
#57383=DIRECTION('center_axis',(-0.843956944130239,0.471546674587893,0.25569593297401));
#57384=DIRECTION('ref_axis',(0.460838052815712,0.393422457595482,0.795516850190211));
#57385=DIRECTION('center_axis',(0.396601985414726,-0.601098528055261,-0.693820888079118));
#57386=DIRECTION('ref_axis',(0.867318528806137,-0.00227571901415262,0.497748320632553));
#57387=DIRECTION('',(0.980355882941517,5.19500677922323E-12,-0.197236768331765));
#57388=DIRECTION('center_axis',(0.,-1.,1.45983193964168E-32));
#57389=DIRECTION('ref_axis',(1.,0.,0.));
#57390=DIRECTION('center_axis',(-0.393634297367351,0.601098527846508,0.695508878273221));
#57391=DIRECTION('ref_axis',(0.868667492214279,-0.00432801246559104,0.495376681201541));
#57392=DIRECTION('center_axis',(-0.403157732486128,-0.601098528075926,0.690032174816218));
#57393=DIRECTION('ref_axis',(0.864676174475855,-0.00330183512154052,0.502318834186645));
#57394=DIRECTION('center_axis',(0.406101923931813,0.601098527962152,-0.688303557349963));
#57395=DIRECTION('ref_axis',(0.862522348605138,-0.00330185944770726,0.506008197444334));
#57396=DIRECTION('center_axis',(-0.340062297712719,0.584828255986933,0.736432987225334));
#57397=DIRECTION('ref_axis',(0.897125081636666,-0.0330815410873473,0.440536263589834));
#57398=DIRECTION('center_axis',(0.444988920947186,-1.08032394082146E-7,
-0.895536074222724));
#57399=DIRECTION('ref_axis',(-0.895426046796085,-0.0156751635317822,-0.444934246790902));
#57400=DIRECTION('',(-0.445019414620402,-4.44089209849761E-13,0.895520921369744));
#57401=DIRECTION('center_axis',(-0.371736677613563,0.584827952225974,0.720963320018434));
#57402=DIRECTION('ref_axis',(0.880937865457384,-0.0227607296063951,0.472684277706771));
#57403=DIRECTION('center_axis',(-0.500371604875772,9.85772978998244E-10,
0.865810751281158));
#57404=DIRECTION('ref_axis',(-0.86570412768751,0.0156933905084823,-0.500309984708637));
#57405=DIRECTION('',(0.500371494362832,-2.20379270384489E-11,-0.865810815149076));
#57406=DIRECTION('',(0.318552670357025,0.,0.947905162032789));
#57407=DIRECTION('center_axis',(0.306515842391656,-0.601098528076755,-0.738057313429582));
#57408=DIRECTION('ref_axis',(0.913390697523814,-0.0324816852769616,0.405786118292049));
#57409=DIRECTION('',(0.966036775394096,8.17238220606244E-12,-0.258404621835945));
#57410=DIRECTION('center_axis',(0.,-1.,1.45983193964168E-32));
#57411=DIRECTION('ref_axis',(1.,0.,0.));
#57412=DIRECTION('center_axis',(-0.303359997774148,0.601098526315498,0.739360043153406));
#57413=DIRECTION('ref_axis',(0.91442875086526,-0.0345384997365875,0.403270568758676));
#57414=DIRECTION('center_axis',(-0.403157730677928,-0.601098528603427,0.69003217541316));
#57415=DIRECTION('ref_axis',(0.875386197278205,-0.0335099970597739,0.482261428803774));
#57416=DIRECTION('center_axis',(0.406101946483679,0.601098526349531,-0.688303545452578));
#57417=DIRECTION('ref_axis',(0.873317948314018,-0.0335100378554978,0.485996747433064));
#57418=DIRECTION('',(-0.387911046558245,0.,0.921696815638465));
#57419=DIRECTION('center_axis',(-0.278444757256321,0.584827952145246,0.761869269327794));
#57420=DIRECTION('ref_axis',(0.924224401753873,-0.0526562728585254,0.378201761142575));
#57421=DIRECTION('center_axis',(-0.445019520156076,8.85968837443965E-10,
0.895520868924927));
#57422=DIRECTION('ref_axis',(-0.895409464779819,0.015772999815539,-0.444964159072995));
#57423=DIRECTION('',(0.445019414618192,-1.76525460892714E-10,-0.895520921370842));
#57424=DIRECTION('',(0.377443537017177,0.,0.926032600054643));
#57425=DIRECTION('',(0.947905162043632,6.51326541667647E-11,-0.31855267032476));
#57426=DIRECTION('center_axis',(0.,-1.,1.45983193964168E-32));
#57427=DIRECTION('ref_axis',(1.,0.,0.));
#57428=DIRECTION('center_axis',(-0.386892908655361,0.601098531195128,0.699281368997669));
#57429=DIRECTION('ref_axis',(0.891933560802797,0.0514849626451757,0.449225802614975));
#57430=DIRECTION('center_axis',(0.229579573086911,0.601098532501136,-0.765489238230174));
#57431=DIRECTION('ref_axis',(0.944431797604197,0.0525165438942013,0.32448511875202));
#57432=DIRECTION('center_axis',(-0.332920489065193,0.584827930050222,0.739689286250494));
#57433=DIRECTION('ref_axis',(0.918057474729132,0.0219594825843356,0.395838671959421));
#57434=DIRECTION('center_axis',(0.329268495354959,-9.71829046692891E-9,
-0.944236335864428));
#57435=DIRECTION('ref_axis',(-0.94411937531885,-0.0157391393472326,-0.329227709405136));
#57436=DIRECTION('',(-0.32927177081575,0.,0.944235193658794));
#57437=DIRECTION('center_axis',(-0.364750270081651,0.584827952321338,0.724522951091954));
#57438=DIRECTION('ref_axis',(0.902955161139128,0.0322834330509239,0.428520427660874));
#57439=DIRECTION('center_axis',(-0.387911153478514,8.80631342479224E-10,
0.92169677063933));
#57440=DIRECTION('ref_axis',(-0.9215831390088,0.0157020800823732,-0.387863329764201));
#57441=DIRECTION('',(0.387911046558865,-7.7715611723626E-13,-0.921696815638204));
#57442=DIRECTION('',(0.434844806474141,0.,0.900505410468181));
#57443=DIRECTION('center_axis',(0.299367248971426,-0.601098527980864,-0.740985701550657));
#57444=DIRECTION('ref_axis',(0.933352190985876,0.0232723727333417,0.35820676186977));
#57445=DIRECTION('',(0.926032600054566,2.46403483598868E-13,-0.377443537017367));
#57446=DIRECTION('center_axis',(0.,-1.,1.45983193964168E-32));
#57447=DIRECTION('ref_axis',(1.,0.,0.));
#57448=DIRECTION('center_axis',(-0.296198957591961,0.601098529132487,0.742257863411494));
#57449=DIRECTION('ref_axis',(0.934367780165617,0.0212181108285934,0.355677723734903));
#57450=DIRECTION('center_axis',(-0.22630718595971,-0.601098527503902,0.766463057045569));
#57451=DIRECTION('ref_axis',(0.953958313206604,0.022245223402675,0.299113167045142));
#57452=DIRECTION('center_axis',(0.229579503858799,0.601098528301044,-0.765489262290639));
#57453=DIRECTION('ref_axis',(0.952671781045117,0.0222452026643455,0.303185798741871));
#57454=DIRECTION('center_axis',(-0.237586792098395,0.584827953016338,0.775582865715273));
#57455=DIRECTION('ref_axis',(0.954441832457449,-0.00784645569542236,0.298293851073547));
#57456=DIRECTION('center_axis',(0.269332611586817,-1.45997421325207E-9,
-0.963047218123714));
#57457=DIRECTION('ref_axis',(-0.96292885479551,-0.0156778483101916,-0.269299509235665));
#57458=DIRECTION('',(-0.269333009823076,7.77156117237388E-13,0.96304710675005));
#57459=DIRECTION('center_axis',(-0.27106730162798,0.584827952254156,0.764525201841206));
#57460=DIRECTION('ref_axis',(0.943100361128264,0.00246180457613212,0.332499095273908));
#57461=DIRECTION('center_axis',(-0.329271852152496,6.5516650383206E-10,
0.944235165295206));
#57462=DIRECTION('ref_axis',(-0.944119219261441,0.0156707406189448,-0.329231419687763));
#57463=DIRECTION('',(0.329271770814934,-6.33937347031766E-11,-0.944235193659079));
#57464=DIRECTION('',(0.490529942141632,1.64268989065528E-13,0.871424337428401));
#57465=DIRECTION('center_axis',(0.204136512687545,-0.601098528048857,-0.772663473813319));
#57466=DIRECTION('ref_axis',(0.965460823204787,-0.00691952388372738,0.260456366875447));
#57467=DIRECTION('',(0.900505410473539,2.34493981894349E-11,-0.434844806463045));
#57468=DIRECTION('center_axis',(0.,-1.,1.45983193964168E-32));
#57469=DIRECTION('ref_axis',(1.,0.,0.));
#57470=DIRECTION('center_axis',(-0.200833749216353,0.601098527505302,0.773528516220741));
#57471=DIRECTION('ref_axis',(0.966152035710377,-0.00897203548261672,0.257817273416643));
#57472=DIRECTION('center_axis',(-0.226307184425563,-0.601098528211325,0.766463056943747));
#57473=DIRECTION('ref_axis',(0.960712912217245,-0.00794572934697725,0.277430289774215));
#57474=DIRECTION('center_axis',(0.229579534945688,0.60109852769211,-0.765489253445468));
#57475=DIRECTION('ref_axis',(0.959518940489111,-0.00794577038205849,0.281532000979798));
#57476=DIRECTION('center_axis',(-0.138506937461519,0.584827952229457,0.79924470255744));
#57477=DIRECTION('ref_axis',(0.982832189613404,-0.0181546317085302,0.183606362654589));
#57478=DIRECTION('center_axis',(0.208331388704263,5.95656447432217E-10,
-0.978058297076689));
#57479=DIRECTION('ref_axis',(-0.977938063370797,-0.0156795066151041,-0.208305778323314));
#57480=DIRECTION('',(-0.208331317647729,2.06170772009129E-7,0.978058312212068));
#57481=DIRECTION('center_axis',(-0.173103405649599,0.584827782537418,0.79247187692995));
#57482=DIRECTION('ref_axis',(0.972199735876484,-0.0273551073893314,0.232549718687021));
#57483=DIRECTION('center_axis',(-0.269333131312943,8.75931129577168E-10,
0.963047072773271));
#57484=DIRECTION('ref_axis',(-0.962928339513347,0.0157023279258724,-0.269299925473025));
#57485=DIRECTION('',(-0.269333010693124,-1.29267411915878E-5,0.96304710641997));
#57486=DIRECTION('',(0.544279213551341,-7.62630514905437E-8,0.838904129025437));
#57487=DIRECTION('center_axis',(0.208331314469237,-1.49811687359948E-11,
-0.978058312889124));
#57488=DIRECTION('ref_axis',(-0.754939979668634,-0.635772805084903,-0.160805993086069));
#57489=DIRECTION('',(-0.871424337429238,0.,0.490529942140145));
#57490=DIRECTION('center_axis',(-0.137250389380106,0.398564391593955,0.906812415204131));
#57491=DIRECTION('ref_axis',(-4.38221259861562E-17,-0.915476128546279,0.402372287890104));
#57492=DIRECTION('center_axis',(0.13958376690986,5.74456497710768E-5,-0.990210264900971));
#57493=DIRECTION('ref_axis',(0.990210198391864,0.000362980231419196,0.139583778592271));
#57494=DIRECTION('',(-0.146508334828668,5.94973691934673E-5,0.98920943398544));
#57495=DIRECTION('center_axis',(-0.18265173307186,0.590180063808731,0.786336974005781));
#57496=DIRECTION('ref_axis',(0.0318446813635314,-0.795820438448205,0.604694754414954));
#57497=DIRECTION('center_axis',(0.698011204258703,0.550037558024481,0.458518313147666));
#57498=DIRECTION('ref_axis',(-0.618934249308444,0.785442801885021,1.77536854630035E-16));
#57499=DIRECTION('center_axis',(-0.705761528390122,-0.477126090336105,0.523690136402264));
#57500=DIRECTION('ref_axis',(0.549640180293908,0.0976244106121075,0.829677736629782));
#57501=DIRECTION('center_axis',(-0.58727483662782,0.584827951390493,0.55953957280622));
#57502=DIRECTION('ref_axis',(0.703292607946138,0.0265489689915622,0.710404574769761));
#57503=DIRECTION('center_axis',(0.653745308372474,-5.67375835137551E-11,
-0.756714656776898));
#57504=DIRECTION('ref_axis',(-0.756620821305633,-0.015747767056935,-0.653664241487562));
#57505=DIRECTION('center_axis',(-0.693441462764553,-0.000115441186732093,
0.720512959211901));
#57506=DIRECTION('ref_axis',(0.0180067889625396,-0.999690424427228,0.0171700570694068));
#57507=DIRECTION('',(0.699969797667289,-6.06570349238745E-10,-0.714172445809564));
#57508=DIRECTION('center_axis',(0.556688242552792,-0.601098527968652,-0.573392326664217));
#57509=DIRECTION('ref_axis',(0.731671535505592,0.0279220146977377,0.681085255475486));
#57510=DIRECTION('',(0.999949569926111,2.24062901110943E-10,-0.0100427886856853));
#57511=DIRECTION('center_axis',(0.,-1.,1.45983193964168E-32));
#57512=DIRECTION('ref_axis',(1.,0.,0.));
#57513=DIRECTION('center_axis',(-0.554233567212543,0.601098529702217,0.575765325948595));
#57514=DIRECTION('ref_axis',(0.733564879997119,0.0258668156642469,0.679126994517377));
#57515=DIRECTION('center_axis',(-0.486462658812862,-0.601098526942828,0.634062017856206));
#57516=DIRECTION('ref_axis',(0.780633128058457,0.0268944007484411,0.624410610564916));
#57517=DIRECTION('center_axis',(0.489166992764132,0.601098528495421,-0.631978015622961));
#57518=DIRECTION('ref_axis',(0.777958478909273,0.0268943670421948,0.627739833143134));
#57519=DIRECTION('center_axis',(-0.512515081039449,0.58482795222263,0.628732501153084));
#57520=DIRECTION('ref_axis',(0.773613241898176,-0.00326197145590633,0.633649675689979));
#57521=DIRECTION('center_axis',(0.604940694421974,-8.90032992022572E-10,
-0.796270529551522));
#57522=DIRECTION('ref_axis',(-0.796172596843005,-0.015683219631179,-0.60486629320724));
#57523=DIRECTION('',(-0.604940785833219,8.32148189212505E-8,0.796270460104782));
#57524=DIRECTION('center_axis',(-0.539352292982029,0.584827969931407,0.605867435699376));
#57525=DIRECTION('ref_axis',(0.750266322720323,0.00704480134519892,0.661098189201673));
#57526=DIRECTION('center_axis',(-0.653745384148104,7.59107307410203E-10,
0.756714591312371));
#57527=DIRECTION('ref_axis',(-0.756621662260592,0.0156715280548858,-0.653665100343015));
#57528=DIRECTION('',(0.653745308266017,-1.44328993199912E-11,-0.756714656868869));
#57529=DIRECTION('',(0.135290527320277,-3.07809289804497E-8,0.990805971528937));
#57530=DIRECTION('center_axis',(0.491483215750491,0.793626260371511,0.358610662814545));
#57531=DIRECTION('ref_axis',(-0.850173673702674,0.526502349988012,1.8687162403211E-16));
#57532=DIRECTION('center_axis',(-0.869349289638193,0.471546674578613,0.147903841395081));
#57533=DIRECTION('ref_axis',(0.357497665685219,0.393418196486003,0.847005042312807));
#57534=DIRECTION('center_axis',(0.480433470466423,-0.601098528037282,-0.638642497839756));
#57535=DIRECTION('ref_axis',(0.798095059786291,-0.00227572297195063,0.602527257997238));
#57536=DIRECTION('',(0.997345805939219,5.19500677922227E-12,-0.0728103246487009));
#57537=DIRECTION('center_axis',(0.,-1.,1.45983193964168E-32));
#57538=DIRECTION('ref_axis',(1.,0.,0.));
#57539=DIRECTION('center_axis',(-0.477700756092285,0.60109852787616,0.640689119163087));
#57540=DIRECTION('ref_axis',(0.799730624680367,-0.00432800792574344,0.600343398644264));
#57541=DIRECTION('center_axis',(-0.48646267173064,-0.601098528094992,0.634062006853211));
#57542=DIRECTION('ref_axis',(0.794900704079075,-0.00330183107163924,0.606730556809335));
#57543=DIRECTION('center_axis',(0.489166986034203,0.601098528025653,-0.63197802127891));
#57544=DIRECTION('ref_axis',(0.792301466969707,-0.00330184925236548,0.610120875916539));
#57545=DIRECTION('center_axis',(-0.429680332528739,0.584828255987421,0.68800488576514));
#57546=DIRECTION('ref_axis',(0.834837147984965,-0.0330815410785944,0.549502090973451));
#57547=DIRECTION('center_axis',(0.553720447696691,-1.0835760102034E-7,-0.832702627474277));
#57548=DIRECTION('ref_axis',(-0.832600320135553,-0.0156751635316961,-0.553652414569312));
#57549=DIRECTION('',(-0.553748836414874,-3.88578058618755E-13,0.832683749192437));
#57550=DIRECTION('center_axis',(-0.459166087066968,0.584827952226069,0.668687349052359));
#57551=DIRECTION('ref_axis',(0.814748358279444,-0.0227607295997188,0.579367812248005));
#57552=DIRECTION('center_axis',(-0.604940859635535,7.21040668407962E-10,
0.796270404035853));
#57553=DIRECTION('ref_axis',(-0.79617234425589,0.0156933905087076,-0.604866361882046));
#57554=DIRECTION('',(0.604940784793816,-2.32591723655392E-11,-0.796270460894439));
#57555=DIRECTION('',(0.197236768334392,0.,0.980355882940989));
#57556=DIRECTION('center_axis',(0.396601986956849,-0.601098528226986,-0.693820887048835));
#57557=DIRECTION('ref_axis',(0.855329850916094,-0.0324816825391389,0.517064586324842));
#57558=DIRECTION('',(0.990805973701574,8.1723822060613E-12,-0.135290511408879));
#57559=DIRECTION('center_axis',(0.,-1.,1.45983193964168E-32));
#57560=DIRECTION('ref_axis',(1.,0.,0.));
#57561=DIRECTION('center_axis',(-0.393634294321039,0.601098526148187,0.695508881465115));
#57562=DIRECTION('ref_axis',(0.85667500460091,-0.0345385027092639,0.514698968643452));
#57563=DIRECTION('center_axis',(-0.486462676856388,-0.601098528542966,0.634062002495969));
#57564=DIRECTION('ref_axis',(0.80804013045387,-0.0335099981759193,0.588173637286084));
#57565=DIRECTION('center_axis',(0.489167013021502,0.601098526659551,-0.631978001689409));
#57566=DIRECTION('ref_axis',(0.805520036045076,-0.0335100323791407,0.591620274551074));
#57567=DIRECTION('',(-0.500371494362924,1.2212453270872E-12,0.865810815149022));
#57568=DIRECTION('center_axis',(-0.37173667630522,0.584827952147585,0.720963320756618));
#57569=DIRECTION('ref_axis',(0.869535366608895,-0.0526562728258266,0.49105556014409));
#57570=DIRECTION('center_axis',(-0.553748908457271,6.38498716108382E-10,
0.832683701283015));
#57571=DIRECTION('ref_axis',(-0.832580114176435,0.0157729998147555,-0.553680021271129));
#57572=DIRECTION('',(0.55374883641321,-1.7652546089297E-10,-0.832683749193544));
#57573=DIRECTION('',(0.258404621839954,0.,0.966036775393023));
#57574=DIRECTION('',(0.980355882947729,6.51326541667623E-11,-0.197236768300891));
#57575=DIRECTION('center_axis',(0.,-1.,1.45983193964168E-32));
#57576=DIRECTION('ref_axis',(1.,0.,0.));
#57577=DIRECTION('center_axis',(-0.471485344333914,0.601098530776743,0.645276782765638));
#57578=DIRECTION('ref_axis',(0.828597472026194,0.051484967479824,0.557472445485336));
#57579=DIRECTION('center_axis',(0.323710518197072,0.601098532913274,-0.730679173193059));
#57580=DIRECTION('ref_axis',(0.896315899040263,0.0525165391159678,0.440295153558299));
#57581=DIRECTION('center_axis',(-0.423002961639147,0.584827930050675,0.692130613885236));
#57582=DIRECTION('ref_axis',(0.861206576608726,0.0219594825775692,0.5077804776976));
#57583=DIRECTION('center_axis',(0.44501630379855,-9.7571629034851E-9,-0.895522467252205));
#57584=DIRECTION('ref_axis',(-0.895411540810433,-0.0157391393480044,-0.444961180414731));
#57585=DIRECTION('',(-0.445019414620135,8.32667268468322E-13,0.895520921369877));
#57586=DIRECTION('center_axis',(-0.452680909511843,0.58482795232107,0.673094540423167));
#57587=DIRECTION('ref_axis',(0.842127239144872,0.0322834330530846,0.538311706207976));
#57588=DIRECTION('center_axis',(-0.50037154967943,4.71272382541235E-10,
0.86581078318037));
#57589=DIRECTION('ref_axis',(-0.865704041469944,0.0157020800824796,-0.500309861249696));
#57590=DIRECTION('',(0.500371494363191,-1.60982338570577E-12,-0.865810815148868));
#57591=DIRECTION('',(0.318552670357066,0.,0.947905162032776));
#57592=DIRECTION('center_axis',(0.389876781786075,-0.601098528007569,-0.697622143177284));
#57593=DIRECTION('ref_axis',(0.881097218878822,0.0232723720441225,0.472362241911274));
#57594=DIRECTION('',(0.966036775393002,0.,-0.258404621840034));
#57595=DIRECTION('center_axis',(0.,-1.,1.45983193964168E-32));
#57596=DIRECTION('ref_axis',(1.,0.,0.));
#57597=DIRECTION('center_axis',(-0.386892919518056,0.601098529104829,0.699281364784452));
#57598=DIRECTION('ref_axis',(0.882421771467431,0.0212181115163354,0.469980434682084));
#57599=DIRECTION('center_axis',(-0.320585978010544,-0.601098527464425,0.732055456221127));
#57600=DIRECTION('ref_axis',(0.908947247090312,0.0222452244191775,0.41631724921925));
#57601=DIRECTION('center_axis',(0.323710438814069,0.601098528144864,-0.730679212284625));
#57602=DIRECTION('ref_axis',(0.907160425325583,0.0222452070252269,0.420196517700363));
#57603=DIRECTION('center_axis',(-0.332919816036326,0.58482795438189,0.739689569930409));
#57604=DIRECTION('ref_axis',(0.909529582677385,-0.00784635391606152,0.415565124817912));
#57605=DIRECTION('center_axis',(0.387910088892421,-3.35595830138579E-9,
-0.921697218687067));
#57606=DIRECTION('ref_axis',(-0.921583937497068,-0.0156778482000772,-0.387862412748666));
#57607=DIRECTION('',(-0.387911046558218,3.885780586189E-13,0.921696815638477));
#57608=DIRECTION('center_axis',(-0.36475027068107,0.58482795225389,0.724522950844629));
#57609=DIRECTION('ref_axis',(0.893990546321623,0.00246180457749375,0.448079058432537));
#57610=DIRECTION('center_axis',(-0.445019470826524,4.72904638593461E-10,
0.895520893438718));
#57611=DIRECTION('ref_axis',(-0.89541092920561,0.0156707406183176,-0.444964825292539));
#57612=DIRECTION('',(0.445019414619957,-6.46149800302003E-11,-0.895520921369965));
#57613=DIRECTION('',(0.37744353701708,1.642689890656E-13,0.926032600054683));
#57614=DIRECTION('center_axis',(0.299367244840995,-0.60109852803596,-0.740985703174706));
#57615=DIRECTION('ref_axis',(0.925204038262238,-0.00691952524571913,0.37940691579572));
#57616=DIRECTION('',(0.94790516203665,2.37574025439352E-11,-0.318552670345537));
#57617=DIRECTION('center_axis',(0.,-1.,1.45983193964168E-32));
#57618=DIRECTION('ref_axis',(1.,0.,0.));
#57619=DIRECTION('center_axis',(-0.296198948099129,0.601098527530323,0.742257868497093));
#57620=DIRECTION('ref_axis',(0.926220564894495,-0.00897203367556791,0.376875268196584));
#57621=DIRECTION('center_axis',(-0.320585971320242,-0.601098528265885,0.732055458492896));
#57622=DIRECTION('ref_axis',(0.918366170984935,-0.0079457249634534,0.395651919552117));
#57623=DIRECTION('center_axis',(0.323710475898501,0.60109852768299,-0.730679196235193));
#57624=DIRECTION('ref_axis',(0.916667530744144,-0.00794577088209146,0.399571649150091));
#57625=DIRECTION('center_axis',(-0.23758669196574,0.584827952232603,0.775582896980199));
#57626=DIRECTION('ref_axis',(0.952070285082109,-0.0181546316499588,0.305340108098044));
#57627=DIRECTION('center_axis',(0.329271828552448,4.79123238521358E-10,
-0.944235173524968));
#57628=DIRECTION('ref_axis',(-0.944119097729614,-0.0156795066156232,-0.329231350837842));
#57629=DIRECTION('',(-0.329271773866148,2.06172326320939E-7,0.944235192595043));
#57630=DIRECTION('center_axis',(-0.271061496415139,0.584827782536856,0.764527389917595));
#57631=DIRECTION('ref_axis',(0.935387442375913,-0.027355107402994,0.352564931245888));
#57632=DIRECTION('center_axis',(-0.387911138367906,6.66509159556812E-10,
0.921696776998876));
#57633=DIRECTION('ref_axis',(-0.92158314178148,0.0157023279249487,-0.387863313142547));
#57634=DIRECTION('',(-0.387911047380046,-1.29267419732928E-5,0.921696815201949));
#57635=DIRECTION('',(0.434844842242892,-7.62630514905467E-8,0.900505393195815));
#57636=DIRECTION('center_axis',(0.329271770822495,5.67466570329746E-12,
-0.944235193656442));
#57637=DIRECTION('ref_axis',(-0.728832717338233,-0.635772805085086,-0.254157058630306));
#57638=DIRECTION('',(-0.926032600055416,0.,0.377443537015281));
#57639=DIRECTION('center_axis',(-0.249821861299389,0.398564391590108,0.882459893351146));
#57640=DIRECTION('ref_axis',(-4.2359305722015E-16,-0.911357382485098,0.411615987772476));
#57641=DIRECTION('center_axis',(0.262589361637465,5.74456695676028E-5,-0.964907676337391));
#57642=DIRECTION('ref_axis',(0.96490760891343,0.000362912078006155,0.262589364894681));
#57643=DIRECTION('',(-0.269333889882224,5.94973691579809E-5,0.963046858787761));
#57644=DIRECTION('center_axis',(-0.279765625258245,0.590180063806458,0.75724413976555));
#57645=DIRECTION('ref_axis',(-0.0441943955513831,-0.795820385214085,0.603917850273987));
#57646=DIRECTION('center_axis',(0.635039594592039,0.550037558023176,0.54238676059089));
#57647=DIRECTION('ref_axis',(-0.65470613502281,0.755883507402757,2.94999188131179E-16));
#57648=DIRECTION('center_axis',(-0.765832166685461,-0.477126089142097,0.431105309094913));
#57649=DIRECTION('ref_axis',(-0.441318377353577,-0.0976272725723773,-0.892024105873874));
#57650=DIRECTION('center_axis',(-0.652772903110501,0.584827951389779,0.481522381866018));
#57651=DIRECTION('ref_axis',(0.608709633160469,0.0265489690038084,0.792948759216182));
#57652=DIRECTION('center_axis',(0.743431825330591,-5.08120091142919E-11,
-0.668811723196914));
#57653=DIRECTION('ref_axis',(-0.668728788021033,-0.0157477670540756,-0.743339636979444));
#57654=DIRECTION('center_axis',(-0.778277689636587,-0.00011544118093089,
0.627920237360821));
#57655=DIRECTION('ref_axis',(0.015710992834112,-0.999690496894265,0.0192892489087636));
#57656=DIRECTION('',(0.783959868698026,-6.07291994204368E-10,-0.620811504621954));
#57657=DIRECTION('center_axis',(0.624163700015786,-0.60109852813265,-0.499099424022274));
#57658=DIRECTION('ref_axis',(0.640539473279341,0.0279220110573426,0.767417451241199));
#57659=DIRECTION('',(0.993323364076756,2.24206636476405E-10,0.115363314702887));
#57660=DIRECTION('center_axis',(0.,-1.,1.45983193964168E-32));
#57661=DIRECTION('ref_axis',(1.,0.,0.));
#57662=DIRECTION('center_axis',(-0.622025798805131,0.601098529751936,0.501761360759175));
#57663=DIRECTION('ref_axis',(0.64266332081354,0.0258668144821308,0.765711932772018));
#57664=DIRECTION('center_axis',(-0.562095789923428,-0.601098526612776,0.568092320185995));
#57665=DIRECTION('ref_axis',(0.696218208653023,0.0268944080891951,0.71732621362495));
#57666=DIRECTION('center_axis',(0.564517616921446,0.60109852864008,-0.565685795342311));
#57667=DIRECTION('ref_axis',(0.693147377749455,0.0268943637794391,0.720293971872564));
#57668=DIRECTION('center_axis',(-0.587274823972098,0.584827952222541,0.559539585219608));
#57669=DIRECTION('ref_axis',(0.688095707608259,-0.0032619714465507,0.725612607879281));
#57670=DIRECTION('center_axis',(0.699969721790153,-8.33585723815394E-10,
-0.714172520177735));
#57671=DIRECTION('ref_axis',(-0.714084684642701,-0.0156832196312858,-0.699883633028184));
#57672=DIRECTION('',(-0.699969798606644,8.32140417651395E-8,0.714172444888885));
#57673=DIRECTION('center_axis',(-0.611034663879005,0.584827969931641,0.533491223099225));
#57674=DIRECTION('ref_axis',(0.661492674919247,0.00704480134231119,0.749918536777314));
#57675=DIRECTION('center_axis',(-0.743431879511351,5.99257470412741E-10,
0.668811662971139));
#57676=DIRECTION('ref_axis',(-0.66872952892159,0.0156715280544964,-0.743340581669496));
#57677=DIRECTION('',(0.743431826076751,-1.48214773786022E-11,-0.668811722367505));
#57678=DIRECTION('',(0.0100428048565612,-3.07809289804534E-8,0.999949569763702));
#57679=DIRECTION('center_axis',(0.442661889834435,0.793626260372119,0.417382091297616));
#57680=DIRECTION('ref_axis',(-0.873334555250179,0.487120882949984,-5.16666451419685E-16));
#57681=DIRECTION('center_axis',(-0.881031477526049,0.471546674578495,0.0377792178615387));
#57682=DIRECTION('ref_axis',(0.248516531292135,0.393409809153091,0.885137421950204));
#57683=DIRECTION('center_axis',(0.556688232289915,-0.601098528013371,-0.573392336581236));
#57684=DIRECTION('ref_axis',(0.716285157056349,-0.00227572809784918,0.697803980242579));
#57685=DIRECTION('',(0.998606989791734,5.19500677922203E-12,0.0527643813485244));
#57686=DIRECTION('center_axis',(0.,-1.,1.45983193964168E-32));
#57687=DIRECTION('ref_axis',(1.,0.,0.));
#57688=DIRECTION('center_axis',(-0.554233581699321,0.601098527875221,0.575765313910958));
#57689=DIRECTION('ref_axis',(0.718181530636935,-0.0043280081485485,0.695842336594616));
#57690=DIRECTION('center_axis',(-0.56209581458741,-0.601098528076768,0.568092294233303));
#57691=DIRECTION('ref_axis',(0.712589168289662,-0.00330183506205464,0.701573784516975));
#57692=DIRECTION('center_axis',(0.564517607904078,0.601098528021518,-0.565685804998342));
#57693=DIRECTION('ref_axis',(0.709585510442279,-0.00330184985540807,0.70461159595759));
#57694=DIRECTION('center_axis',(-0.512522051817965,0.584828255987753,0.628726536260899));
#57695=DIRECTION('ref_axis',(0.759383333800813,-0.0330815410714352,0.649801942122292));
#57696=DIRECTION('center_axis',(0.653719519633801,-1.08253155343526E-7,
-0.756736935565948));
#57697=DIRECTION('ref_axis',(-0.75664396176299,-0.01567516353247,-0.653639200458355));
#57698=DIRECTION('',(-0.6537453082656,0.,0.75671465686923));
#57699=DIRECTION('center_axis',(-0.539354173031852,0.584827952226096,0.605865779136071));
#57700=DIRECTION('ref_axis',(0.735709782783262,-0.0227607295942035,0.676914370290175));
#57701=DIRECTION('center_axis',(-0.699969862671832,6.97646258222362E-10,
0.714172382097752));
#57702=DIRECTION('ref_axis',(-0.714084432592782,0.0156933905086662,-0.699883662206075));
#57703=DIRECTION('',(0.699969797674119,-2.3259172365536E-11,-0.71417244580287));
#57704=DIRECTION('',(0.0728103246514921,0.,0.997345805939015));
#57705=DIRECTION('center_axis',(0.480433476314609,-0.601098528193226,-0.638642493293547));
#57706=DIRECTION('ref_axis',(0.783779943492905,-0.0324816831588366,0.620188632947612));
#57707=DIRECTION('',(0.999949569924982,8.00811321699464E-12,-0.0100427887981123));
#57708=DIRECTION('center_axis',(0.,-1.,1.45983193964168E-32));
#57709=DIRECTION('ref_axis',(1.,0.,0.));
#57710=DIRECTION('center_axis',(-0.477700756802861,0.601098526553358,0.64068911987434));
#57711=DIRECTION('ref_axis',(0.785410974555097,-0.0345384955415771,0.618010269634848));
#57712=DIRECTION('center_axis',(-0.562095813790538,-0.601098528572725,0.568092294496993));
#57713=DIRECTION('ref_axis',(0.727950789289693,-0.0335099976713577,0.684809994398868));
#57714=DIRECTION('center_axis',(0.564517632497287,0.601098526611315,-0.565685781954402));
#57715=DIRECTION('ref_axis',(0.725018587143443,-0.0335100331949467,0.687913603566464));
#57716=DIRECTION('',(-0.604940784793116,-3.88578058618287E-13,0.79627046089497));
#57717=DIRECTION('center_axis',(-0.459166085817877,0.584827952145803,0.66868734998027));
#57718=DIRECTION('ref_axis',(0.801133239332449,-0.0526562728502562,0.596165119548449));
#57719=DIRECTION('center_axis',(-0.653745378516728,6.88166267249251E-10,
0.756714596177463));
#57720=DIRECTION('ref_axis',(-0.756620459739955,0.0157729998143454,-0.653664051619603));
#57721=DIRECTION('',(0.653745308264166,-1.76914038951625E-10,-0.756714656870468));
#57722=DIRECTION('',(0.135290511413065,0.,0.990805973701002));
#57723=DIRECTION('',(0.997345805941503,6.5132654166752E-11,-0.0728103246174193));
#57724=DIRECTION('center_axis',(0.,-1.,1.45983193964168E-32));
#57725=DIRECTION('ref_axis',(1.,0.,0.));
#57726=DIRECTION('center_axis',(-0.548642170750967,0.601098530535707,0.581095796802455));
#57727=DIRECTION('ref_axis',(0.752193906731871,0.0514849702321019,0.65692741190762));
#57728=DIRECTION('center_axis',(0.412736343893058,0.601098532682348,-0.684345866091788));
#57729=DIRECTION('ref_axis',(0.834064566950636,0.052516541749496,0.549161461685105));
#57730=DIRECTION('center_axis',(-0.506414424847036,0.584827930049987,0.633656628261943));
#57731=DIRECTION('ref_axis',(0.790773936299874,0.0219594825907513,0.611714281992132));
#57732=DIRECTION('center_axis',(0.553745940067887,-9.79389565979201E-9,
-0.832685675305113));
#57733=DIRECTION('ref_axis',(-0.832582532343421,-0.0157391393472531,-0.553677348578776));
#57734=DIRECTION('',(-0.553748836414763,3.8857805861822E-13,0.832683749192511));
#57735=DIRECTION('center_axis',(-0.533472500586727,0.584827952320527,0.61105102675826));
#57736=DIRECTION('ref_axis',(0.768018467521465,0.0322834330602798,0.639613487581229));
#57737=DIRECTION('center_axis',(-0.604940838723149,5.00351481251069E-10,
0.796270419923365));
#57738=DIRECTION('ref_axis',(-0.796172251513586,0.0157020800827631,-0.604866258441369));
#57739=DIRECTION('',(0.604940784793812,-1.16573417585636E-12,-0.796270460894442));
#57740=DIRECTION('',(0.197236768334319,-1.64268989065584E-13,0.980355882941003));
#57741=DIRECTION('center_axis',(0.474237720943464,-0.601098528144826,-0.643256669997655));
#57742=DIRECTION('ref_axis',(0.814946819839827,0.0232723683639434,0.579068284145908));
#57743=DIRECTION('',(0.990805973701026,0.,-0.135290511412896));
#57744=DIRECTION('center_axis',(0.,-1.,1.45983193964168E-32));
#57745=DIRECTION('ref_axis',(1.,0.,0.));
#57746=DIRECTION('center_axis',(-0.471485348678522,0.601098529086282,0.645276781165882));
#57747=DIRECTION('ref_axis',(0.816559444195094,0.0212181120796413,0.576871273175892));
#57748=DIRECTION('center_axis',(-0.409808942054769,-0.601098527542422,0.686102901318951));
#57749=DIRECTION('ref_axis',(0.849601538195442,0.0222452224588818,0.526955763203795));
#57750=DIRECTION('center_axis',(0.412736271713158,0.601098528090446,-0.684345913657575));
#57751=DIRECTION('ref_axis',(0.847342607083042,0.0222452084305431,0.530580490522971));
#57752=DIRECTION('center_axis',(-0.423002181530047,0.584827953016395,0.692131071251301));
#57753=DIRECTION('ref_axis',(0.850273623012057,-0.00784645567137288,0.526282432865992));
#57754=DIRECTION('center_axis',(0.500371211619023,-7.78002359410976E-10,
-0.865810978553004));
#57755=DIRECTION('ref_axis',(-0.865704566046401,-0.0156778483087253,-0.500309713476384));
#57756=DIRECTION('',(-0.500371494362507,-3.88578058618512E-13,0.865810815149263));
#57757=DIRECTION('center_axis',(-0.452680910074828,0.584827952254067,0.673094540102756));
#57758=DIRECTION('ref_axis',(0.830781966554501,0.0024618045795608,0.556592547170772));
#57759=DIRECTION('center_axis',(-0.553748911662773,6.88113040807786E-10,
0.832683699151301));
#57760=DIRECTION('ref_axis',(-0.832581450920485,0.0156707406193936,-0.55368091485221));
#57761=DIRECTION('',(0.553748836414603,-6.50035580888534E-11,-0.832683749192617));
#57762=DIRECTION('',(0.258404621840001,1.64268989065638E-13,0.966036775393011));
#57763=DIRECTION('center_axis',(0.389876788530882,-0.601098528116778,-0.697622139313747));
#57764=DIRECTION('ref_axis',(0.870356228170294,-0.00691951858998903,0.492374000478967));
#57765=DIRECTION('',(0.980355882943393,2.34493981894308E-11,-0.197236768322441));
#57766=DIRECTION('center_axis',(0.,-1.,1.45983193964168E-32));
#57767=DIRECTION('ref_axis',(1.,0.,0.));
#57768=DIRECTION('center_axis',(-0.386892915864324,0.601098527591087,0.699281368107165));
#57769=DIRECTION('ref_axis',(0.87168204034931,-0.00897202944535721,0.489989717463638));
#57770=DIRECTION('center_axis',(-0.409808933300045,-0.601098528262936,0.686102905916898));
#57771=DIRECTION('ref_axis',(0.861536244811326,-0.00794572521358364,0.507633888080011));
#57772=DIRECTION('center_axis',(0.412736294851897,0.601098527818209,-0.684345899941477));
#57773=DIRECTION('ref_axis',(0.859359733181087,-0.00794576136272164,0.511309802236666));
#57774=DIRECTION('center_axis',(-0.332919562188109,0.584827952228835,0.739689685884767));
#57775=DIRECTION('ref_axis',(0.906293663475364,-0.0181546317298205,0.422258457453677));
#57776=DIRECTION('center_axis',(0.445019476003258,5.37775435232845E-10,
-0.895520890866196));
#57777=DIRECTION('ref_axis',(-0.89541080356602,-0.0156795066150552,-0.444964769312765));
#57778=DIRECTION('',(-0.445019417513705,2.06170716497847E-7,0.895520919931924));
#57779=DIRECTION('center_axis',(-0.364744785454799,0.584827782536393,0.724525849267711));
#57780=DIRECTION('ref_axis',(0.883823530142337,-0.0273551074198127,0.467019984224217));
#57781=DIRECTION('center_axis',(-0.500371575167866,6.17478624361332E-10,
0.865810768450029));
#57782=DIRECTION('ref_axis',(-0.865704023370405,0.0157023279246887,-0.500309884789456));
#57783=DIRECTION('',(-0.500371495123144,-1.29267411917713E-5,0.865810814613174));
#57784=DIRECTION('',(0.318552708008686,-7.62630514905686E-8,0.947905149379582));
#57785=DIRECTION('center_axis',(0.445019414614705,-5.06252227775145E-12,
-0.895520921372575));
#57786=DIRECTION('ref_axis',(-0.691231327686734,-0.635772805085008,-0.343499915485835));
#57787=DIRECTION('',(-0.96603677539344,0.,0.258404621838397));
#57788=DIRECTION('center_axis',(-0.358453493229671,0.398564391588364,0.844190451823073));
#57789=DIRECTION('ref_axis',(1.45643262671735E-16,-0.904282187129022,0.426935271488726));
#57790=DIRECTION('center_axis',(0.3814537653021,5.74456535097432E-5,-0.924387917292761));
#57791=DIRECTION('ref_axis',(0.924387849953043,0.000363021687504849,0.381453760073807));
#57792=DIRECTION('',(-0.387911888599863,5.94973691934224E-5,0.921696459330809));
#57793=DIRECTION('center_axis',(-0.372467446133925,0.59018006381471,0.716209113210755));
#57794=DIRECTION('ref_axis',(-0.119533762394807,-0.79581992529521,0.593617996821919));
#57795=DIRECTION('center_axis',(0.562053031164479,0.550037558024463,0.617701444810766));
#57796=DIRECTION('ref_axis',(0.73963826965528,1.66905152560888E-16,-0.673004628558633));
#57797=DIRECTION('center_axis',(-0.813825173144071,-0.47712609025277,0.331721692925152));
#57798=DIRECTION('ref_axis',(-0.326038799174341,-0.0976261562960603,-0.940301991404789));
#57799=DIRECTION('center_axis',(0.,-1.,1.45983193964168E-32));
#57800=DIRECTION('ref_axis',(1.,0.,0.));
#57801=DIRECTION('center_axis',(-0.680008321123557,0.601098529378286,0.41984430588253));
#57802=DIRECTION('ref_axis',(0.541626566377255,0.02586682302227,0.840221143545626));
#57803=DIRECTION('center_axis',(-0.62886435068494,-0.601098526908652,0.493163450983402));
#57804=DIRECTION('ref_axis',(0.600823499447581,0.0268944015745013,0.79892916686995));
#57805=DIRECTION('center_axis',(0.681795728548397,-0.601098528078482,-0.41693541954965));
#57806=DIRECTION('ref_axis',(0.539305716225786,0.0279220122353789,0.841647019645956));
#57807=DIRECTION('center_axis',(0.630965454817298,0.601098528548254,-0.490472378227687));
#57808=DIRECTION('ref_axis',(0.597404933134226,0.0268943657915818,0.801488639317838));
#57809=DIRECTION('center_axis',(-0.70797635094031,0.584827951390237,0.395911295345234));
#57810=DIRECTION('ref_axis',(0.504526943858353,0.0265489689943019,0.862987668026774));
#57811=DIRECTION('center_axis',(0.821393979803529,-3.34035840811973E-11,
-0.570361227593987));
#57812=DIRECTION('ref_axis',(-0.570290500650736,-0.0157477670566653,-0.82129212385135));
#57813=DIRECTION('center_axis',(-0.850840010906561,-0.000115441176905437,
0.525424840023631));
#57814=DIRECTION('ref_axis',(0.0131676303921038,-0.999690586528358,0.0211031920913415));
#57815=DIRECTION('',(0.855586424284002,-6.06570349238516E-10,-0.517659995152141));
#57816=DIRECTION('',(0.971031855393319,2.2406290111098E-10,0.238950069703709));
#57817=DIRECTION('center_axis',(-0.652772892093047,0.58482795222276,0.481522395790074));
#57818=DIRECTION('ref_axis',(0.59172649297372,-0.00326197145057506,0.806132195768955));
#57819=DIRECTION('center_axis',(0.783959821523761,-5.96131969645808E-10,
-0.620811564193543));
#57820=DIRECTION('ref_axis',(-0.620735211050847,-0.0156832196313396,-0.783863402885768));
#57821=DIRECTION('',(-0.783959869513934,8.321320909793E-8,0.620811503591621));
#57822=DIRECTION('center_axis',(-0.673080653115289,0.584827969931677,0.452701535216626));
#57823=DIRECTION('ref_axis',(0.562286892476256,0.00704480134115208,0.826912221050976));
#57824=DIRECTION('center_axis',(-0.821394020464315,5.31114300248357E-10,
0.570361169037189));
#57825=DIRECTION('ref_axis',(-0.570291125292885,0.0156715280545383,-0.8212931484072));
#57826=DIRECTION('',(0.821393979886223,-1.44328993199867E-11,-0.570361227474896));
#57827=DIRECTION('',(-0.115363298639103,-3.07809289804514E-8,0.993323365942382));
#57828=DIRECTION('center_axis',(0.386859521482828,0.793626260373017,0.469571154868373));
#57829=DIRECTION('ref_axis',(-2.13687929229864E-16,-0.509219680924762,0.860636576354319));
#57830=DIRECTION('center_axis',(-0.878819272724478,0.471546674559146,-0.0729412064626718));
#57831=DIRECTION('ref_axis',(0.135626041762887,0.393420630700766,0.909299611863297));
#57832=DIRECTION('center_axis',(0.624163699479745,-0.601098528034406,-0.499099424810959));
#57833=DIRECTION('ref_axis',(0.623179000875404,-0.00227572371504448,0.782075925949332));
#57834=DIRECTION('',(0.984119544876364,5.19500677922209E-12,0.177506961532043));
#57835=DIRECTION('center_axis',(0.,-1.,1.45983193964168E-32));
#57836=DIRECTION('ref_axis',(1.,0.,0.));
#57837=DIRECTION('center_axis',(-0.622025817027204,0.60109852790029,0.501761340387782));
#57838=DIRECTION('ref_axis',(0.625306280590028,-0.00432800421432909,0.780367428737378));
#57839=DIRECTION('center_axis',(-0.628864362189718,-0.601098528093964,0.493163434868188));
#57840=DIRECTION('ref_axis',(0.619039682119636,-0.00330183194536081,0.785352767784659));
#57841=DIRECTION('center_axis',(0.630965447315775,0.601098528031762,-0.490472388510966));
#57842=DIRECTION('ref_axis',(0.615678968825533,-0.00330184814314328,0.787990168177731));
#57843=DIRECTION('center_axis',(-0.587280992141335,0.584828255986637,0.559532793738774));
#57844=DIRECTION('ref_axis',(0.671953590842899,-0.0330815410987143,0.73985402843525));
#57845=DIRECTION('center_axis',(0.743409038173406,-1.08193554509994E-7,
-0.668837051875925));
#57846=DIRECTION('ref_axis',(-0.668754877861165,-0.0156751635313557,-0.743317699631297));
#57847=DIRECTION('',(-0.743431826102458,2.44243513872084E-9,0.668811722338929));
#57848=DIRECTION('center_axis',(-0.611036274076432,0.58482795055301,0.53348940009597));
#57849=DIRECTION('ref_axis',(0.645068669434817,-0.0227607725733292,0.763785545127335));
#57850=DIRECTION('center_axis',(-0.783959920609502,6.39561847536878E-10,
0.620811439068211));
#57851=DIRECTION('ref_axis',(-0.620734986854462,0.0156933905089844,-0.783863376864313));
#57852=DIRECTION('',(0.783959868703813,-2.2870594306917E-11,-0.620811504614646));
#57853=DIRECTION('',(-0.0527643808758776,-9.0376691099926E-10,0.998606989816707));
#57854=DIRECTION('center_axis',(0.556688242465508,-0.601098528137483,-0.573392326571969));
#57855=DIRECTION('ref_axis',(0.699869358675761,-0.0324816841607832,0.71353193410026));
#57856=DIRECTION('',(0.993323364089752,8.00811321699503E-12,0.115363314590982));
#57857=DIRECTION('center_axis',(0.,-1.,1.45983193964168E-32));
#57858=DIRECTION('ref_axis',(1.,0.,0.));
#57859=DIRECTION('center_axis',(-0.55423357818793,0.601098526332382,0.575765318901758));
#57860=DIRECTION('ref_axis',(0.701760552571379,-0.0345384994452432,0.711575167435447));
#57861=DIRECTION('center_axis',(-0.628864360507214,-0.601098528788258,0.493163436167407));
#57862=DIRECTION('ref_axis',(0.636381232999916,-0.0335099937670627,0.770646486142147));
#57863=DIRECTION('center_axis',(0.630965472559523,0.601098526509254,-0.490472357902198));
#57864=DIRECTION('ref_axis',(0.63308316071494,-0.0335100350712062,0.773358124783536));
#57865=DIRECTION('',(-0.69996979767421,-3.88578058618464E-13,0.714172445802781));
#57866=DIRECTION('center_axis',(-0.539354171922836,0.584827952147118,0.605865780199576));
#57867=DIRECTION('ref_axis',(0.720096762266244,-0.0526562728331108,0.691872798934167));
#57868=DIRECTION('center_axis',(-0.743431897726421,8.01204384872099E-10,
0.668811642723789));
#57869=DIRECTION('ref_axis',(-0.668728441543193,0.0157729998147021,-0.743339413692061));
#57870=DIRECTION('',(0.743431826075426,-1.76525460892892E-10,-0.668811722368977));
#57871=DIRECTION('',(0.010042788802475,0.,0.999949569924938));
#57872=DIRECTION('',(0.998606989790074,6.51326541667596E-11,0.0527643813799335));
#57873=DIRECTION('center_axis',(0.,-1.,1.45983193964168E-32));
#57874=DIRECTION('ref_axis',(1.,0.,0.));
#57875=DIRECTION('center_axis',(-0.617146580610682,0.601098530377361,0.507750583277577));
#57876=DIRECTION('ref_axis',(0.663927794474839,0.0514849720612138,0.746022239196414));
#57877=DIRECTION('center_axis',(0.495253069852363,0.601098532340813,-0.62722001819101));
#57878=DIRECTION('ref_axis',(0.758659540214554,0.0525165456835235,0.649367164607906));
#57879=DIRECTION('center_axis',(-0.581839430006672,0.584827930051382,0.565189499125141));
#57880=DIRECTION('ref_axis',(0.707870318665559,0.0219594825652875,0.706000986598309));
#57881=DIRECTION('center_axis',(0.653742689345644,-9.65698928568759E-9,
-0.756716919413809));
#57882=DIRECTION('ref_axis',(-0.756623186558303,-0.0157391393474532,-0.653661711479999));
#57883=DIRECTION('',(-0.653745308266206,0.,0.756714656868706));
#57884=DIRECTION('center_axis',(-0.605850911623636,0.584827952321254,0.539370873396533));
#57885=DIRECTION('ref_axis',(0.681797585889768,0.0322834330504779,0.730828182150469));
#57886=DIRECTION('center_axis',(-0.699969848687725,5.29825396220384E-10,
0.714172395803761));
#57887=DIRECTION('ref_axis',(-0.714084348869081,0.0157020800831493,-0.699883552729511));
#57888=DIRECTION('',(0.699969797674381,-3.88578058618674E-13,-0.714172445802613));
#57889=DIRECTION('',(0.0728103246515104,0.,0.997345805939014));
#57890=DIRECTION('center_axis',(0.551119652024366,-0.601098528185188,-0.578746653179215));
#57891=DIRECTION('ref_axis',(0.735944221221984,0.0232723672963963,0.676642076854809));
#57892=DIRECTION('',(0.99994956992494,0.,-0.0100427888023433));
#57893=DIRECTION('center_axis',(0.,-1.,1.45983193964168E-32));
#57894=DIRECTION('ref_axis',(1.,0.,0.));
#57895=DIRECTION('center_axis',(-0.548642181723866,0.601098528779788,0.581095788258743));
#57896=DIRECTION('ref_axis',(0.73781947939277,0.0212181204735827,0.674664514549379));
#57897=DIRECTION('center_axis',(-0.492568970194462,-0.601098527513249,0.629330096072778));
#57898=DIRECTION('ref_axis',(0.776857107271133,0.0222452233282606,0.629283866725823));
#57899=DIRECTION('center_axis',(0.495253018968578,0.601098528368869,-0.627220062175382));
#57900=DIRECTION('ref_axis',(0.774161682723275,0.0222452008249728,0.632596901702279));
#57901=DIRECTION('center_axis',(-0.506413843524673,0.584827954381722,0.633657070393962));
#57902=DIRECTION('ref_axis',(0.777608194314138,-0.00784635389937767,0.628700191558736));
#57903=DIRECTION('center_axis',(0.604939965639439,-3.27650173372792E-9,
-0.796271083219876));
#57904=DIRECTION('ref_axis',(-0.796173217541591,-0.0156778482002054,-0.604865615443036));
#57905=DIRECTION('',(-0.604940784793658,0.,0.796270460894559));
#57906=DIRECTION('center_axis',(-0.533472501099667,0.584827952254068,0.61105102637405));
#57907=DIRECTION('ref_axis',(0.75447145888779,0.00246180458297537,0.656328238949022));
#57908=DIRECTION('center_axis',(-0.653745361478494,5.31761636790432E-10,
0.756714610897235));
#57909=DIRECTION('ref_axis',(-0.7566216911844,0.0156707406186724,-0.653665085741713));
#57910=DIRECTION('',(0.653745308265349,-6.38378239129687E-11,-0.756714656869446));
#57911=DIRECTION('',(0.135290511412992,1.64268989065632E-13,0.990805973701012));
#57912=DIRECTION('center_axis',(0.474237725950656,-0.601098528057081,-0.643256666388123));
#57913=DIRECTION('ref_axis',(0.801782387397817,-0.00691952323199839,0.597576039895258));
#57914=DIRECTION('',(0.997345805939914,2.3449398189431E-11,-0.0728103246391816));
#57915=DIRECTION('center_axis',(0.,-1.,1.45983193964168E-32));
#57916=DIRECTION('ref_axis',(1.,0.,0.));
#57917=DIRECTION('center_axis',(-0.471485353517794,0.601098527683139,0.645276778937042));
#57918=DIRECTION('ref_axis',(0.803396566223726,-0.00897202285469235,0.595376738028805));
#57919=DIRECTION('center_axis',(-0.492568963228535,-0.601098528265706,0.629330100806221));
#57920=DIRECTION('ref_axis',(0.791119377524039,-0.00794572522958855,0.611610166655651));
#57921=DIRECTION('center_axis',(0.495253024655371,0.601098527880305,-0.627220058153306));
#57922=DIRECTION('ref_axis',(0.788499317751901,-0.00794575698719568,0.614984301304259));
#57923=DIRECTION('center_axis',(-0.423002092231914,0.584827952231039,0.692131126490257));
#57924=DIRECTION('ref_axis',(0.846224249337463,-0.0181546316854976,0.532517538848826));
#57925=DIRECTION('center_axis',(0.553748791295796,-4.24684809762998E-10,
-0.832683779197389));
#57926=DIRECTION('ref_axis',(-0.832581416534835,-0.0156795066181781,-0.553680718386562));
#57927=DIRECTION('',(-0.553748839105298,2.06170327919852E-7,0.832683747403234));
#57928=DIRECTION('center_axis',(-0.452675831355118,0.584827782536082,0.673098103162446));
#57929=DIRECTION('ref_axis',(0.818321192866598,-0.0273551074282337,0.574109853079511));
#57930=DIRECTION('center_axis',(-0.604940865737854,6.83049984403924E-10,
0.796270399399812));
#57931=DIRECTION('ref_axis',(-0.796172227891624,0.0157023279250567,-0.604866283100507));
#57932=DIRECTION('',(-0.604940785481047,-1.29267420445158E-5,0.79627046026741));
#57933=DIRECTION('',(0.197236807274931,-7.62630514905909E-8,0.980355875106579));
#57934=DIRECTION('center_axis',(0.553748836409908,-5.14328675068677E-12,
-0.832683749195739));
#57935=DIRECTION('ref_axis',(-0.642728807070213,-0.635772805084933,-0.427425573493839));
#57936=DIRECTION('',(-0.990805973701214,0.,0.135290511411514));
#57937=DIRECTION('center_axis',(-0.46143209944248,0.398564391585333,0.792607622575205));
#57938=DIRECTION('ref_axis',(0.864216279017979,-2.46944013809118E-16,0.503120485649628));
#57939=DIRECTION('center_axis',(0.49430241515009,5.74456554432761E-5,-0.869290008614378));
#57940=DIRECTION('ref_axis',(0.869289942423636,0.000363130101863143,0.494302401509076));
#57941=DIRECTION('',(-0.500372285107574,5.94973691578971E-5,0.865810356115176));
#57942=DIRECTION('center_axis',(-0.459295233458345,0.590180063803156,0.663879040798658));
#57943=DIRECTION('ref_axis',(-0.193006876961119,-0.795822364586091,0.573946957018084));
#57944=DIRECTION('center_axis',(0.480202555681032,0.550037558023931,0.68327460825094));
#57945=DIRECTION('ref_axis',(-2.67200776655505E-16,-0.778964448264928,0.627068089077508));
#57946=DIRECTION('center_axis',(-0.848983670875502,-0.477126090478573,0.227106627757515));
#57947=DIRECTION('ref_axis',(-0.205617745019631,-0.0976244547999203,-0.973750896666114));
#57948=DIRECTION('center_axis',(0.,-1.,1.45983193964168E-32));
#57949=DIRECTION('ref_axis',(1.,0.,0.));
#57950=DIRECTION('center_axis',(-0.680008328143395,0.601098527896,0.419844296634939));
#57951=DIRECTION('ref_axis',(0.522569581621024,-0.00432800512230333,0.852585655952579));
#57952=DIRECTION('center_axis',(-0.685715352438027,-0.601098528063218,0.410457080571191));
#57953=DIRECTION('ref_axis',(0.515727559994683,-0.00330183849355368,0.856746276166108));
#57954=DIRECTION('center_axis',(0.681795728152809,-0.601098528038952,-0.416935420253529));
#57955=DIRECTION('ref_axis',(0.520244942189748,-0.00227572246809452,0.854014063826371));
#57956=DIRECTION('center_axis',(0.687462588098602,0.601098528021724,-0.407523925156412));
#57957=DIRECTION('ref_axis',(0.512062798628297,-0.00330184974610516,0.858941667431037));
#57958=DIRECTION('center_axis',(0.,-1.,1.45983193964168E-32));
#57959=DIRECTION('ref_axis',(1.,0.,0.));
#57960=DIRECTION('center_axis',(-0.727266694147858,0.601098529543099,0.331306072030638));
#57961=DIRECTION('ref_axis',(0.432048050851811,0.0258668192715915,0.901479555739298));
#57962=DIRECTION('center_axis',(-0.685715334700198,-0.601098526757656,0.4104571121162));
#57963=DIRECTION('ref_axis',(0.495953454603779,0.0268944048963865,0.867932521485309));
#57964=DIRECTION('center_axis',(0.728675431061478,-0.601098528004021,-0.3281960935154));
#57965=DIRECTION('ref_axis',(0.429566785113303,0.0279220138465334,0.902603311688017));
#57966=DIRECTION('center_axis',(0.68746259021791,0.601098528408167,-0.407523921011294));
#57967=DIRECTION('ref_axis',(0.492241057688875,0.0268943690384856,0.87004335181608));
#57968=DIRECTION('center_axis',(-0.752014588816605,0.584827951388868,0.304056451142372));
#57969=DIRECTION('ref_axis',(0.392387563221727,0.0265489690167294,0.919416745808485));
#57970=DIRECTION('center_axis',(0.886402261674847,6.96815599083177E-12,
-0.46291579201591));
#57971=DIRECTION('ref_axis',(-0.462858388711434,-0.0157477670569393,-0.886292344450845));
#57972=DIRECTION('center_axis',(-0.909984078160621,-0.000115441171811356,
0.414643176921436));
#57973=DIRECTION('ref_axis',(0.010417872471279,-0.999690646286046,0.0225849432445623));
#57974=DIRECTION('',(0.913719870856373,-6.06514838087195E-10,-0.406344678323974));
#57975=DIRECTION('',(0.933426594283893,2.24206636476395E-10,0.358768439363851));
#57976=DIRECTION('center_axis',(-0.707976341755816,0.584827952222755,0.395911310539358));
#57977=DIRECTION('ref_axis',(0.486025398070987,-0.00326197145932844,0.873938597369482));
#57978=DIRECTION('center_axis',(0.855586388865124,-5.36828188002314E-10,
-0.517660053692322));
#57979=DIRECTION('ref_axis',(-0.517596387076646,-0.0156832196303758,-0.855481160930636));
#57980=DIRECTION('',(-0.85558642496489,8.32136531871927E-8,0.517659994026766));
#57981=DIRECTION('center_axis',(-0.724511758384697,0.584827969931394,0.364772473671245));
#57982=DIRECTION('ref_axis',(0.45421350982732,0.00704480135432238,0.890865005634538));
#57983=DIRECTION('center_axis',(-0.886402280378725,3.19828384669413E-10,
0.462915756201273));
#57984=DIRECTION('ref_axis',(-0.462858907393903,0.0156715280543384,-0.886293424918951));
#57985=DIRECTION('',(0.886402259955283,-1.40443212613674E-11,-0.462915795308571));
#57986=DIRECTION('',(-0.238950054000525,-3.07809289804526E-8,0.971031859257535));
#57987=DIRECTION('center_axis',(0.324956147379585,0.793626260374256,0.514354800818064));
#57988=DIRECTION('ref_axis',(1.18768397098885E-16,-0.543871187803528,0.839168714310287));
#57989=DIRECTION('center_axis',(-0.862747562988294,0.471546674573188,-0.182511304462839));
#57990=DIRECTION('ref_axis',(0.0205860831513606,0.393412747962545,0.919131450294812));
#57991=DIRECTION('',(0.954111946853708,5.05127141378893E-12,0.299450150894981));
#57992=DIRECTION('center_axis',(-0.652772892223738,0.584827952239051,0.481522395593117));
#57993=DIRECTION('ref_axis',(0.573932730509739,-0.033086909061157,0.818233754680418));
#57994=DIRECTION('center_axis',(0.821393938657068,-5.66605482047647E-10,
-0.570361286850211));
#57995=DIRECTION('ref_axis',(-0.570291210542767,-0.0156751701942392,-0.821293019705542));
#57996=DIRECTION('',(-0.821393979885579,0.,0.570361227475824));
#57997=DIRECTION('center_axis',(-0.673082062129668,0.584827952225996,0.452699463147927));
#57998=DIRECTION('ref_axis',(0.544254348718667,-0.0227607295979204,0.838611443452205));
#57999=DIRECTION('center_axis',(-0.85558645437424,4.39716529147059E-10,
0.517659945419111));
#58000=DIRECTION('ref_axis',(-0.517596196193671,0.0156933905082907,-0.855481089902166));
#58001=DIRECTION('',(0.855586424288824,-2.20934381896938E-11,-0.517659995144173));
#58002=DIRECTION('',(-0.177506961529562,0.,0.984119544876812));
#58003=DIRECTION('center_axis',(0.624163703184407,-0.601098528102421,-0.499099420096067));
#58004=DIRECTION('ref_axis',(0.6049214158146,-0.0324816847642132,0.795622410973785));
#58005=DIRECTION('',(0.971031855420263,8.00811321699492E-12,0.238950069594217));
#58006=DIRECTION('center_axis',(0.,-1.,1.45983193964168E-32));
#58007=DIRECTION('ref_axis',(1.,0.,0.));
#58008=DIRECTION('center_axis',(-0.622025811482655,0.60109852640924,0.501761349047517));
#58009=DIRECTION('ref_axis',(0.607042942905174,-0.0345384980589837,0.793918105109624));
#58010=DIRECTION('center_axis',(-0.685715346712145,-0.60109852870395,0.410457089198603));
#58011=DIRECTION('ref_axis',(0.534775559073474,-0.0335099953326465,0.84432942719679));
#58012=DIRECTION('center_axis',(0.687462605265226,0.601098526679091,-0.407523898177978));
#58013=DIRECTION('ref_axis',(0.53116363987613,-0.0335100320481414,0.846606322576009));
#58014=DIRECTION('',(-0.783959868703477,3.88578058618491E-13,0.62081150461507));
#58015=DIRECTION('center_axis',(-0.611036320506081,0.584827952146277,0.533489345170812));
#58016=DIRECTION('ref_axis',(0.627703929119516,-0.0526562728443811,0.776669230945877));
#58017=DIRECTION('center_axis',(-0.821394029079472,6.36178315555462E-10,
0.570361156630246));
#58018=DIRECTION('ref_axis',(-0.570290202838897,0.0157729998144146,-0.821291846436347));
#58019=DIRECTION('',(0.821393979884557,-1.76525460892916E-10,-0.570361227477296));
#58020=DIRECTION('',(-0.115363314586811,-1.4373536543246E-13,0.993323364090236));
#58021=DIRECTION('',(0.98411954487057,6.73708191429274E-11,0.177506961564164));
#58022=DIRECTION('center_axis',(0.,-1.,1.45983193964168E-32));
#58023=DIRECTION('ref_axis',(1.,0.,0.));
#58024=DIRECTION('center_axis',(-0.675918217257937,0.601098530441075,0.426397842724881));
#58025=DIRECTION('ref_axis',(0.565191146769487,0.0514849713402289,0.823351847838752));
#58026=DIRECTION('center_axis',(0.569959358794219,0.601098531899161,-0.560202538615773));
#58027=DIRECTION('ref_axis',(0.671290001483131,0.0525165507868081,0.739331959137595));
#58028=DIRECTION('center_axis',(-0.648088479825358,0.584827930050975,0.487808993920723));
#58029=DIRECTION('ref_axis',(0.613803163212554,0.0219594825743171,0.789153633936593));
#58030=DIRECTION('center_axis',(0.743429504550853,-9.7370770992602E-9,-0.668814302899746));
#58031=DIRECTION('ref_axis',(-0.668731458373539,-0.0157391393482095,-0.743337417377988));
#58032=DIRECTION('',(-0.743431826076801,3.88578058618555E-13,0.668811722367449));
#58033=DIRECTION('center_axis',(-0.668674691896985,0.58482795232003,0.459184519122361));
#58034=DIRECTION('ref_axis',(0.584824349013597,0.0322834330674684,0.810517279735726));
#58035=DIRECTION('center_axis',(-0.783959911974966,5.16098504643952E-10,
0.620811449971893));
#58036=DIRECTION('ref_axis',(-0.620734913065085,0.0157020800826335,-0.783863261279134));
#58037=DIRECTION('',(0.783959868703571,-3.88578058618765E-13,-0.620811504614952));
#58038=DIRECTION('',(-0.0527643813458578,0.,0.998606989791875));
#58039=DIRECTION('center_axis',(0.619310100008391,-0.601098528130847,-0.505109452996602));
#58040=DIRECTION('ref_axis',(0.645335340235233,0.0232723687883982,0.763544822190848));
#58041=DIRECTION('',(0.993323364090227,1.43735365432655E-13,0.115363314586895));
#58042=DIRECTION('center_axis',(0.,-1.,1.45983193964168E-32));
#58043=DIRECTION('ref_axis',(1.,0.,0.));
#58044=DIRECTION('center_axis',(-0.617146593637132,0.601098528605606,0.507750569542034));
#58045=DIRECTION('ref_axis',(0.647443662249848,0.0212181253246192,0.761817888586382));
#58046=DIRECTION('center_axis',(-0.567560897639404,-0.60109852767921,0.56263237330662));
#58047=DIRECTION('ref_axis',(0.691861171014227,0.0222452189954519,0.721687792798705));
#58048=DIRECTION('center_axis',(0.569959306223684,0.601098527946005,-0.560202596343646));
#58049=DIRECTION('ref_axis',(0.688771782411489,0.0222452124300358,0.724636862350821));
#58050=DIRECTION('center_axis',(-0.581838788167143,0.584827953016251,0.565190136109091));
#58051=DIRECTION('ref_axis',(0.692679594751913,-0.0078464556685245,0.721202753840948));
#58052=DIRECTION('center_axis',(0.699969489842962,-1.59750556575904E-9,
-0.714172747512102));
#58053=DIRECTION('ref_axis',(-0.714084972116213,-0.0156778483104737,-0.699883460063275));
#58054=DIRECTION('',(-0.69996979767378,4.44089209849797E-13,0.714172445803202));
#58055=DIRECTION('center_axis',(-0.605850912090104,0.584827952254016,0.539370872945475));
#58056=DIRECTION('ref_axis',(0.66626248562324,0.00246180457741594,0.74571324231863));
#58057=DIRECTION('center_axis',(-0.743431866551407,4.54777387042457E-10,
0.668811677377041));
#58058=DIRECTION('ref_axis',(-0.668729551581567,0.0156707406185188,-0.743340577884716));
#58059=DIRECTION('',(0.743431826076476,-6.42264019716054E-11,-0.66881172236781));
#58060=DIRECTION('',(0.0100427888024243,1.64268989065715E-13,0.999949569924939));
#58061=DIRECTION('center_axis',(0.551119657779422,-0.601098528057545,-0.578746647831454));
#58062=DIRECTION('ref_axis',(0.720563956462457,-0.00691952328167995,0.693353953507676));
#58063=DIRECTION('',(0.998606989791215,2.33056628239968E-11,0.0527643813583316));
#58064=DIRECTION('center_axis',(0.,-1.,1.45983193964168E-32));
#58065=DIRECTION('ref_axis',(1.,0.,0.));
#58066=DIRECTION('center_axis',(-0.548642174934512,0.601098527672761,0.581095795814053));
#58067=DIRECTION('ref_axis',(0.722441053324715,-0.00897202367764671,0.691374303299019));
#58068=DIRECTION('center_axis',(-0.567560894235305,-0.601098528183147,0.562632376202148));
#58069=DIRECTION('ref_axis',(0.708226078745709,-0.00794573193760378,0.705940993800794));
#58070=DIRECTION('center_axis',(0.569959316685545,0.601098527973058,-0.560202585670549));
#58071=DIRECTION('ref_axis',(0.705203800501899,-0.00794575017932217,0.708960129211626));
#58072=DIRECTION('center_axis',(-0.506413626476593,0.584827952229078,0.633657245843815));
#58073=DIRECTION('ref_axis',(0.772809373333965,-0.0181546317213056,0.634378500450818));
#58074=DIRECTION('center_axis',(0.653745352984885,4.63890099005459E-10,
-0.756714618235084));
#58075=DIRECTION('ref_axis',(-0.756621594530565,-0.0156795066149336,-0.653664987407417));
#58076=DIRECTION('',(-0.653745310710569,2.06171937743035E-7,0.75671465475693));
#58077=DIRECTION('center_axis',(-0.53346790901253,0.584827782536522,0.61105519785631));
#58078=DIRECTION('ref_axis',(0.739913441518089,-0.027355107412841,0.672145666622414));
#58079=DIRECTION('center_axis',(-0.699969862169507,5.94033433643584E-10,
0.714172382590087));
#58080=DIRECTION('ref_axis',(-0.714084332876665,0.0157023279254008,-0.699883563485964));
#58081=DIRECTION('',(-0.699969798277329,-1.29267419735568E-5,0.714172445094667));
#58082=DIRECTION('',(0.0728103642669414,-7.62629077552247E-8,0.997345803046922));
#58083=DIRECTION('center_axis',(0.653745308269215,3.24852657677469E-12,
-0.756714656866107));
#58084=DIRECTION('ref_axis',(-0.584090069209569,-0.635772805085282,-0.504610474886078));
#58085=DIRECTION('',(-0.999949569924953,0.,0.0100427888010589));
#58086=DIRECTION('center_axis',(-0.557133645801549,0.398564391581777,0.728524897638319));
#58087=DIRECTION('ref_axis',(0.794343958189908,-3.09877856731042E-16,0.607468251093989));
#58088=DIRECTION('center_axis',(0.599355620640818,5.74456531717371E-5,-0.80048287720991));
#58089=DIRECTION('ref_axis',(0.800482813240499,0.000363161708211434,0.599355598806042));
#58090=DIRECTION('',(-0.604941511771255,5.94973699394858E-5,0.796269906373443));
#58091=DIRECTION('center_axis',(-0.538879660020742,0.590180063812166,0.60107919968553));
#58092=DIRECTION('ref_axis',(-0.263409456277491,-0.795820649045882,0.545238436737349));
#58093=DIRECTION('center_axis',(0.390778999035457,0.550037558023876,0.738072122950039));
#58094=DIRECTION('ref_axis',(7.53656174059586E-17,-0.801830011453256,0.597552200843467));
#58095=DIRECTION('center_axis',(-0.870753189088995,-0.47712609044742,0.118909955452456));
#58096=DIRECTION('ref_axis',(-0.0819536582661743,-0.0976233394778846,-0.991843375481218));
#58097=DIRECTION('center_axis',(0.,-1.,1.45983193964168E-32));
#58098=DIRECTION('ref_axis',(1.,0.,0.));
#58099=DIRECTION('center_axis',(-0.763055658654184,0.601098528025735,0.237542883288733));
#58100=DIRECTION('ref_axis',(0.3156558309711,0.0258668540830143,0.948521113225105));
#58101=DIRECTION('center_axis',(-0.731752133462375,-0.601098523429036,0.321277730794861));
#58102=DIRECTION('ref_axis',(0.383262015888094,0.0268944802402911,0.923248024157105));
#58103=DIRECTION('center_axis',(0.764063590022611,-0.601098518825436,-0.234280603268019));
#58104=DIRECTION('ref_axis',(0.313053074944991,0.0279222149704815,0.949325087722129));
#58105=DIRECTION('center_axis',(0.733118084397875,0.601098531882569,-0.318148439093156));
#58106=DIRECTION('ref_axis',(0.37931414459962,0.0268942877291573,0.924877006414474));
#58107=DIRECTION('center_axis',(0.,-1.,1.45983193964168E-32));
#58108=DIRECTION('ref_axis',(1.,0.,0.));
#58109=DIRECTION('center_axis',(-0.680008326307634,0.601098526530791,0.419844301562856));
#58110=DIRECTION('ref_axis',(0.502751902272055,-0.0345384959278909,0.863740480156435));
#58111=DIRECTION('center_axis',(-0.731752192868383,-0.601098528530253,0.321277585945668));
#58112=DIRECTION('ref_axis',(0.424736152881488,-0.0335099985284445,0.904696789225018));
#58113=DIRECTION('center_axis',(0.681795729173495,-0.60109852804082,-0.416935418581753));
#58114=DIRECTION('ref_axis',(0.500433501629634,-0.0324816859338729,0.8651654469092));
#58115=DIRECTION('center_axis',(0.733118040771723,0.601098527035837,-0.318148548779305));
#58116=DIRECTION('ref_axis',(0.420867355674219,-0.0335100257314689,0.906503032043063));
#58117=DIRECTION('center_axis',(0.,-1.,1.45983193964168E-32));
#58118=DIRECTION('ref_axis',(1.,0.,0.));
#58119=DIRECTION('center_axis',(-0.727266707321978,0.60109852793785,0.331306046023914));
#58120=DIRECTION('ref_axis',(0.411591638996172,-0.00432799832780596,0.911358102580385));
#58121=DIRECTION('center_axis',(-0.731752194190079,-0.601098528072251,0.321277583792239));
#58122=DIRECTION('ref_axis',(0.40428211487033,-0.00330183696942516,0.914628377795376));
#58123=DIRECTION('center_axis',(0.728675428745706,-0.601098528032884,-0.328196098604113));
#58124=DIRECTION('ref_axis',(0.409106312832959,-0.00227572372044445,0.91248388801215));
#58125=DIRECTION('center_axis',(0.733118028917691,0.601098528044534,-0.318148574189064));
#58126=DIRECTION('ref_axis',(0.400371098715705,-0.00330184579683318,0.916347140077118));
#58127=DIRECTION('center_axis',(-0.752014581596804,0.584827952222568,0.304056467395354));
#58128=DIRECTION('ref_axis',(0.372659392286658,-0.00326197145442373,0.927962465233788));
#58129=DIRECTION('center_axis',(0.913719848261096,-4.35909436812389E-10,
-0.406344729132445));
#58130=DIRECTION('ref_axis',(-0.406294753104332,-0.0156832196307687,-0.913607470537486));
#58131=DIRECTION('',(-0.913719871391209,8.32139862540962E-8,0.406344677121314));
#58132=DIRECTION('center_axis',(-0.764516880406,0.584827969931467,0.271090732339042));
#58133=DIRECTION('ref_axis',(0.338976908816905,0.00704480134891643,0.940768316889387));
#58134=DIRECTION('center_axis',(-0.937431471416932,5.26575514447819E-10,
0.348169838436769));
#58135=DIRECTION('ref_axis',(-0.348127081105987,0.0156715280544189,-0.937316349270119));
#58136=DIRECTION('',(0.937431446874141,-1.44328993199741E-11,-0.348169904517111));
#58137=DIRECTION('',(-0.358768424268643,-3.07809289805637E-8,0.933426600085831));
#58138=DIRECTION('center_axis',(0.257928020713531,0.793626260375571,0.551026764298329));
#58139=DIRECTION('ref_axis',(3.86526474988473E-16,-0.570324176014851,0.821419706516091));
#58140=DIRECTION('center_axis',(-0.833069808886043,0.471546674515063,-0.289203090018688));
#58141=DIRECTION('ref_axis',(-0.0947709949961845,0.393417043001799,0.914462404248066));
#58142=DIRECTION('',(0.909057433470377,5.19500677922194E-12,0.416670832495209));
#58143=DIRECTION('center_axis',(-0.707980627189437,0.584828255987165,0.3959031984254));
#58144=DIRECTION('ref_axis',(0.466848718284166,-0.0330815410864286,0.883718216331303));
#58145=DIRECTION('center_axis',(0.886386495251401,-1.08055804801194E-7,
-0.462945980688812));
#58146=DIRECTION('ref_axis',(-0.462889103293546,-0.0156751635321578,-0.886277590431089));
#58147=DIRECTION('',(-0.886402259955067,3.8857805861861E-13,0.462915795308984));
#58148=DIRECTION('center_axis',(-0.724512896583829,0.584827952226093,0.364770241355767));
#58149=DIRECTION('ref_axis',(0.434856856698299,-0.0227607295918755,0.900211899149817));
#58150=DIRECTION('center_axis',(-0.913719892390152,3.99854364386318E-10,
0.406344629902412));
#58151=DIRECTION('ref_axis',(-0.406294589028634,0.0156933905087666,-0.913607368851846));
#58152=DIRECTION('',(0.91371987086034,-2.24265050970685E-11,-0.406344678315053));
#58153=DIRECTION('',(-0.299450150892402,0.,0.954111946854518));
#58154=DIRECTION('',(0.933426594324386,8.00811321699435E-12,0.358768439258496));
#58155=DIRECTION('',(-0.855586424288614,8.32667268468143E-13,0.517659995144519));
#58156=DIRECTION('center_axis',(-0.673082061317715,0.584827952146517,0.452699464457831));
#58157=DIRECTION('ref_axis',(0.525411830022407,-0.052656272840452,0.849217125241276));
#58158=DIRECTION('center_axis',(-0.886402289863428,4.66216806888189E-10,
0.462915738039734));
#58159=DIRECTION('ref_axis',(-0.462858150621278,0.0157729998159349,-0.886292020092845));
#58160=DIRECTION('',(0.886402259954025,-1.76136882834176E-10,-0.462915795310981));
#58161=DIRECTION('',(-0.238950069590315,0.,0.971031855421223));
#58162=DIRECTION('',(0.95411194684388,6.73708191429212E-11,0.299450150926296));
#58163=DIRECTION('center_axis',(-0.784193107368798,0.58482795138977,0.207406455127399));
#58164=DIRECTION('ref_axis',(0.274059996359373,0.0265489690028562,0.961346072255141));
#58165=DIRECTION('center_axis',(0.937431447265939,-2.66968652048685E-11,
-0.348169903462213));
#58166=DIRECTION('ref_axis',(-0.348126729081251,-0.015747767055638,-0.937315202230259));
#58167=DIRECTION('center_axis',(-0.957443409380817,7.95312786477369E-12,
0.288621062698544));
#58168=DIRECTION('ref_axis',(0.00472526695421307,-0.999865971929401,0.0156751405061303));
#58169=DIRECTION('',(0.957443409235807,-6.06126260028942E-10,-0.288621063179587));
#58170=DIRECTION('',(0.881100638180641,2.24206636473677E-10,0.472928816417088));
#58171=DIRECTION('center_axis',(0.,-1.,1.45983193964168E-32));
#58172=DIRECTION('ref_axis',(1.,0.,0.));
#58173=DIRECTION('center_axis',(-0.724030222887723,0.601098530184123,0.338320548231469));
#58174=DIRECTION('ref_axis',(0.457541092754366,0.0514849742756542,0.887696708265259));
#58175=DIRECTION('center_axis',(0.635677057400638,0.601098532148273,-0.484350320887329));
#58176=DIRECTION('ref_axis',(0.573333811124451,0.0525165478891726,0.817637054700505));
#58177=DIRECTION('center_axis',(-0.704116787165796,0.58482793005043,0.402735449475516));
#58178=DIRECTION('ref_axis',(0.510055965204231,0.0219594825838839,0.859860857048527));
#58179=DIRECTION('center_axis',(0.821392007966856,-9.6282449769448E-9,-0.570364067283499));
#58180=DIRECTION('ref_axis',(-0.570293417594276,-0.0157391393474235,-0.821290263756513));
#58181=DIRECTION('',(-0.821393979885945,4.44089209849773E-13,0.570361227475297));
#58182=DIRECTION('center_axis',(-0.720953072810683,0.584827952320198,0.371756550701933));
#58183=DIRECTION('ref_axis',(0.478628082816279,0.032283433065689,0.877424035623088));
#58184=DIRECTION('center_axis',(-0.855586463236559,5.60123081497593E-10,
0.517659930771502));
#58185=DIRECTION('ref_axis',(-0.517596110925291,0.0157020800827716,-0.855480982042317));
#58186=DIRECTION('',(0.855586424289034,-3.88578058618695E-13,-0.517659995143825));
#58187=DIRECTION('',(-0.177506961529512,-1.6426898906565E-13,0.984119544876821));
#58188=DIRECTION('center_axis',(0.677733657883253,-0.601098528047542,-0.423506373684346));
#58189=DIRECTION('ref_axis',(0.544549134368899,0.0232723709346554,0.838406009645185));
#58190=DIRECTION('',(0.971031855421274,0.,0.23895006959011));
#58191=DIRECTION('center_axis',(0.,-1.,1.45983193964168E-32));
#58192=DIRECTION('ref_axis',(1.,0.,0.));
#58193=DIRECTION('center_axis',(-0.675918226413701,0.601098528713118,0.426397830647251));
#58194=DIRECTION('ref_axis',(0.546857279595311,0.0212181223337183,0.836956932606599));
#58195=DIRECTION('center_axis',(-0.633602050443839,-0.601098527883255,0.487061599235606));
#58196=DIRECTION('ref_axis',(0.595954168650271,0.0222452135891341,0.802710271107041));
#58197=DIRECTION('center_axis',(0.635677009826813,0.601098527945971,-0.484350388539979));
#58198=DIRECTION('ref_axis',(0.592519529931851,0.0222452123180939,0.805248879029497));
#58199=DIRECTION('center_axis',(-0.64808802673632,0.584827954381773,0.487809566710878));
#58200=DIRECTION('ref_axis',(0.596826823270977,-0.00784635390048773,0.802331713043142));
#58201=DIRECTION('center_axis',(0.783959299467165,-2.39970101787109E-9,
-0.620812223445183));
#58202=DIRECTION('ref_axis',(-0.620735922539111,-0.015677848198522,-0.783862946914435));
#58203=DIRECTION('',(-0.783959868703779,7.77156117237062E-13,0.620811504614689));
#58204=DIRECTION('center_axis',(-0.668674692280572,0.584827952254079,0.459184518647769));
#58205=DIRECTION('ref_axis',(0.567546154955955,0.00246180457167309,0.823337902390605));
#58206=DIRECTION('center_axis',(-0.821394026637575,6.22329750071602E-10,
0.570361160146894));
#58207=DIRECTION('ref_axis',(-0.570291123441637,0.0156707406185681,-0.821293164717776));
#58208=DIRECTION('',(0.821393979885603,-6.37823127618236E-11,-0.57036122747579));
#58209=DIRECTION('',(-0.115363314586758,1.6426898906571E-13,0.993323364090243));
#58210=DIRECTION('center_axis',(0.619310103140169,-0.601098528052553,-0.50510944924993));
#58211=DIRECTION('ref_axis',(0.627981801754453,-0.00691952358516004,0.778197260891212));
#58212=DIRECTION('',(0.984119544874613,2.34493981894299E-11,0.177506961541753));
#58213=DIRECTION('center_axis',(0.,-1.,1.45983193964168E-32));
#58214=DIRECTION('ref_axis',(1.,0.,0.));
#58215=DIRECTION('center_axis',(-0.617146594133584,0.601098527826761,0.507750569860653));
#58216=DIRECTION('ref_axis',(0.630092201514216,-0.00897201270892481,0.776468492972458));
#58217=DIRECTION('center_axis',(-0.63360204568641,-0.601098528143562,0.487061605103133));
#58218=DIRECTION('ref_axis',(0.614163633400353,-0.00794573548312544,0.789138705612714));
#58219=DIRECTION('center_axis',(0.635677020797868,0.601098527942322,-0.484350374145742));
#58220=DIRECTION('ref_axis',(0.610786790306842,-0.00794575219278953,0.791755241099645));
#58221=DIRECTION('center_axis',(-0.58183871533142,0.584827952227705,0.56519021190625));
#58222=DIRECTION('ref_axis',(0.687206831862969,-0.0181546317512861,0.726234934154806));
#58223=DIRECTION('center_axis',(0.743431881697495,6.52231953694037E-10,
-0.668811660541084));
#58224=DIRECTION('ref_axis',(-0.668729442833958,-0.0156795066147268,-0.743340490864922));
#58225=DIRECTION('',(-0.743431828237324,2.06171160587007E-7,0.668811719965842));
#58226=DIRECTION('center_axis',(-0.605846879053264,0.58482778253678,0.539375587058343));
#58227=DIRECTION('ref_axis',(0.649836813198125,-0.0273551074048852,0.759581341471321));
#58228=DIRECTION('center_axis',(-0.78395992854951,6.42204840304423E-10,
0.620811429041579));
#58229=DIRECTION('ref_axis',(-0.620734889719503,0.0157023279254214,-0.783863274801568));
#58230=DIRECTION('',(-0.783959869213338,-1.29267420091223E-5,0.620811503836636));
#58231=DIRECTION('',(-0.0527643416803028,-7.62630514906024E-8,0.998606991887719));
#58232=DIRECTION('center_axis',(0.74343182608437,8.46488594574043E-12,-0.668811722359036));
#58233=DIRECTION('ref_axis',(-0.516239882040292,-0.635772805085321,-0.573837367644325));
#58234=DIRECTION('',(-0.993323364090019,0.,-0.115363314588682));
#58235=DIRECTION('center_axis',(-0.644048861750252,0.398564391579836,0.652952899865527));
#58236=DIRECTION('ref_axis',(0.711944358623391,-1.48341292504493E-16,0.702235879334237));
#58237=DIRECTION('center_axis',(0.694956629954641,5.74456464726726E-5,-0.719051652652357));
#58238=DIRECTION('ref_axis',(0.719051591959292,0.000363044425646409,0.694956600299294));
#58239=DIRECTION('',(-0.699970449419061,5.94973699395165E-5,0.714171804540155));
#58240=DIRECTION('center_axis',(-0.60996563275169,0.590180063807912,0.528799980281315));
#58241=DIRECTION('ref_axis',(-0.329667630782392,-0.795820412202847,0.507926298527272));
#58242=DIRECTION('center_axis',(0.295192624134886,0.550037558023661,0.781229799367464));
#58243=DIRECTION('ref_axis',(-2.99006832900842E-16,-0.817666865875968,0.575691667864467));
#58244=DIRECTION('center_axis',(-0.878790409509715,-0.477126090119163,0.00883800211288844));
#58245=DIRECTION('ref_axis',(0.0430053759461772,-0.09762677183074,-0.994293493422157));
#58246=DIRECTION('center_axis',(0.,-1.,1.45983193964168E-32));
#58247=DIRECTION('ref_axis',(1.,0.,0.));
#58248=DIRECTION('center_axis',(-0.786810691452641,0.601098536565918,0.140033871453045));
#58249=DIRECTION('ref_axis',(0.194285827458928,0.0258666594739602,0.98060386149365));
#58250=DIRECTION('center_axis',(-0.766248820041582,-0.601098522588609,0.227031521878956));
#58251=DIRECTION('ref_axis',(0.264526238238669,0.0268944948231608,0.964003400114079));
#58252=DIRECTION('center_axis',(0.787401802212211,-0.601098527961809,-0.136670997490725));
#58253=DIRECTION('ref_axis',(0.191602837697934,0.0279220147745897,0.981075284408402));
#58254=DIRECTION('center_axis',(0.767211803203183,0.601098532171143,-0.223755678469661));
#58255=DIRECTION('ref_axis',(0.26040530923369,0.0268942848435636,0.96512474445828));
#58256=DIRECTION('center_axis',(0.,-1.,1.45983193964168E-32));
#58257=DIRECTION('ref_axis',(1.,0.,0.));
#58258=DIRECTION('center_axis',(-0.763055658742142,0.601098528049379,0.237542882946354));
#58259=DIRECTION('ref_axis',(0.294122635795175,-0.0043279808307652,0.955757889684845));
#58260=DIRECTION('center_axis',(-0.766248826143083,-0.601098528566415,0.227031485458818));
#58261=DIRECTION('ref_axis',(0.286461009557513,-0.00330174912324799,0.958086211390195));
#58262=DIRECTION('center_axis',(0.76406357716492,-0.601098528929575,-0.234280619276642));
#58263=DIRECTION('ref_axis',(0.29151558545289,-0.00227553083980164,0.956563372389648));
#58264=DIRECTION('center_axis',(0.767211806619316,0.601098527379421,-0.223755679628956));
#58265=DIRECTION('ref_axis',(0.28236518714665,-0.00330193682016637,0.959301307359097));
#58266=DIRECTION('center_axis',(0.,-1.,1.45983193964168E-32));
#58267=DIRECTION('ref_axis',(1.,0.,0.));
#58268=DIRECTION('center_axis',(-0.760723836756566,0.60109853016227,0.244907740235234));
#58269=DIRECTION('ref_axis',(0.34267534538575,0.0514849745188543,0.93804205932546));
#58270=DIRECTION('center_axis',(0.691369743499754,0.601098531888471,-0.40085961724101));
#58271=DIRECTION('ref_axis',(0.466335810284432,0.0525165508876074,0.88304752076501));
#58272=DIRECTION('center_axis',(0.,-1.,1.45983193964168E-32));
#58273=DIRECTION('ref_axis',(1.,0.,0.));
#58274=DIRECTION('center_axis',(-0.727266700096615,0.601098526413129,0.331306064651021));
#58275=DIRECTION('ref_axis',(0.390532168548934,-0.0345384980101142,0.919941148924034));
#58276=DIRECTION('center_axis',(-0.766248865328599,-0.601098528706299,0.227031352834265));
#58277=DIRECTION('ref_axis',(0.307998411581329,-0.0335099952893715,0.950796539055062));
#58278=DIRECTION('center_axis',(0.72867543016971,-0.601098528022213,-0.328196095462021));
#58279=DIRECTION('ref_axis',(0.388053451412226,-0.0324816862907586,0.921064307691253));
#58280=DIRECTION('center_axis',(0.767211772309541,0.601098527048624,-0.223755798158681));
#58281=DIRECTION('ref_axis',(0.30393373490876,-0.0335100255164653,0.952103651381664));
#58282=DIRECTION('center_axis',(-0.75201458167613,0.584827952239124,0.304056467167315));
#58283=DIRECTION('ref_axis',(0.352415118267461,-0.0330869090612141,0.935258702640775));
#58284=DIRECTION('center_axis',(0.937431427900636,-4.26563368083218E-10,
-0.348169955602397));
#58285=DIRECTION('ref_axis',(-0.348127178393669,-0.0156751701946118,-0.937316252234555));
#58286=DIRECTION('',(-0.93743144687371,3.88578058618708E-13,0.348169904518272));
#58287=DIRECTION('center_axis',(-0.764517729851838,0.584827952226204,0.271088374957497));
#58288=DIRECTION('ref_axis',(0.318601412279502,-0.0227607295886048,0.94761547543405));
#58289=DIRECTION('center_axis',(-0.957443432644625,6.20247471359333E-10,
0.288620985525443));
#58290=DIRECTION('ref_axis',(-0.288585442177813,0.0156933905085329,-0.957325524603508));
#58291=DIRECTION('',(0.957443409238553,-2.2482016248302E-11,-0.288621063170478));
#58292=DIRECTION('',(-0.416670832492711,-1.43735365432645E-13,0.909057433471522));
#58293=DIRECTION('',(0.881100638234107,8.00811321699514E-12,0.472928816317476));
#58294=DIRECTION('',(-0.913719870860275,3.88578058618767E-13,0.4063446783152));
#58295=DIRECTION('center_axis',(-0.724512895938863,0.584827952146669,0.364770242764149));
#58296=DIRECTION('ref_axis',(0.414833672503379,-0.0526562728382997,0.908372358170446));
#58297=DIRECTION('center_axis',(-0.937431470815378,4.98983339446778E-10,
0.348169840056427));
#58298=DIRECTION('ref_axis',(-0.348126527198881,0.015772999815457,-0.937314852937511));
#58299=DIRECTION('',(0.937431446873072,-1.7691403895138E-10,-0.348169904519991));
#58300=DIRECTION('',(-0.358768439254574,0.,0.933426594325894));
#58301=DIRECTION('',(0.909057433457252,6.51326541667565E-11,0.416670832523844));
#58302=DIRECTION('center_axis',(-0.749040752138178,0.584827930050797,0.311310526434255));
#58303=DIRECTION('ref_axis',(0.398264879952269,0.0219594825763105,0.917007560776674));
#58304=DIRECTION('center_axis',(0.886400663547062,-9.55911743639789E-9,
-0.462918852136449));
#58305=DIRECTION('ref_axis',(-0.462861511471999,-0.015739139347479,-0.886290866866209));
#58306=DIRECTION('',(-0.886402259955305,7.77156117237576E-13,0.462915795308529));
#58307=DIRECTION('center_axis',(-0.761861593087581,0.584827952320615,0.278465759407741));
#58308=DIRECTION('ref_axis',(0.36488356584029,0.0322834330592784,0.930493290319485));
#58309=DIRECTION('center_axis',(-0.913719901723408,5.65380501737239E-10,
0.406344608915347));
#58310=DIRECTION('ref_axis',(-0.406294512606847,0.0157020800825024,-0.913607253532199));
#58311=DIRECTION('',(0.913719870860467,-3.88578058618884E-13,-0.406344678314768));
#58312=DIRECTION('',(-0.299450150892451,-1.64268989065695E-13,0.954111946854502));
#58313=DIRECTION('center_axis',(0.72546894837819,-0.601098528071751,-0.335224349487053));
#58314=DIRECTION('ref_axis',(0.435175066285531,0.0232723703371241,0.900045031352474));
#58315=DIRECTION('',(0.933426594325836,0.,0.358768439254726));
#58316=DIRECTION('center_axis',(-0.804004432171644,0.584827951390059,0.10748553540481));
#58317=DIRECTION('ref_axis',(0.151410339629092,0.0265489689966038,0.988114396868409));
#58318=DIRECTION('center_axis',(0.973676780287623,-1.28906918013669E-11,
-0.22793316460912));
#58319=DIRECTION('ref_axis',(-0.227904900037124,-0.0157477670551488,-0.973556040694035));
#58320=DIRECTION('center_axis',(-0.98606749399318,4.96891179130181E-11,
0.166345716175714));
#58321=DIRECTION('ref_axis',(0.00272900050446146,-0.999865419160101,0.0161770245732108));
#58322=DIRECTION('',(0.986067493102596,-6.06514838087271E-10,-0.166345721454935));
#58323=DIRECTION('',(0.814879198669332,2.24062901110924E-10,0.579630823521341));
#58324=DIRECTION('center_axis',(-0.784193102249395,0.584827952222746,0.207406472134837));
#58325=DIRECTION('ref_axis',(0.253416325277267,-0.00326197145543368,0.967351810679646));
#58326=DIRECTION('center_axis',(0.957443386600224,-6.15197396809075E-10,
-0.288621138268657));
#58327=DIRECTION('ref_axis',(-0.288585640979932,-0.0156832196320613,-0.957325631351305));
#58328=DIRECTION('',(-0.957443409615588,8.32144303432537E-8,0.288621061919726));
#58329=DIRECTION('center_axis',(-0.792465114529435,0.584827969931237,0.173133728198635));
#58330=DIRECTION('ref_axis',(0.218394439445317,0.00704480135457211,0.975835149804126));
#58331=DIRECTION('center_axis',(-0.973676797222046,5.70223093254237E-10,
0.227933092269243));
#58332=DIRECTION('ref_axis',(-0.227905100723701,0.0156715280547446,-0.973557223933215));
#58333=DIRECTION('',(0.973676779881275,-1.40998324126016E-11,-0.227933166344942));
#58334=DIRECTION('',(-0.472928802167949,-3.07808057783763E-8,0.881100645828834));
#58335=DIRECTION('center_axis',(0.186832215081918,0.793626260376337,0.579008706539594));
#58336=DIRECTION('ref_axis',(-9.49913119975713E-19,-0.589386723434917,0.807851032207457));
#58337=DIRECTION('center_axis',(-0.790254046147588,0.471546674542655,-0.391333970254474));
#58338=DIRECTION('ref_axis',(-0.208641931036127,0.393409230472831,0.895375743468792));
#58339=DIRECTION('',(0.849666541316565,4.90753604829622E-12,0.527320366160028));
#58340=DIRECTION('center_axis',(0.,-1.,1.45983193964168E-32));
#58341=DIRECTION('ref_axis',(1.,0.,0.));
#58342=DIRECTION('center_axis',(-0.72403023283582,0.6010985284829,0.338320529964412));
#58343=DIRECTION('ref_axis',(0.437646620241063,0.0212181286726185,0.89889667193021));
#58344=DIRECTION('center_axis',(-0.689650913839443,-0.601098527866504,0.403809579922447));
#58345=DIRECTION('ref_axis',(0.490648618647226,0.0222452140406601,0.871073523574132));
#58346=DIRECTION('center_axis',(0.691369707533585,0.601098527966793,-0.400859685153146));
#58347=DIRECTION('ref_axis',(0.486922890027579,0.0222452117933845,0.873161640087022));
#58348=DIRECTION('center_axis',(-0.704116346384031,0.584827953375261,0.402736186238222));
#58349=DIRECTION('ref_axis',(0.491561927830823,-0.00784642890357389,0.870807271823511));
#58350=DIRECTION('center_axis',(0.855586176495259,-1.17960254227111E-9,
-0.51766040469619));
#58351=DIRECTION('ref_axis',(-0.517596781651614,-0.015677848278934,-0.855481020652846));
#58352=DIRECTION('',(-0.85558642428887,3.88578058618816E-13,0.517659995144097));
#58353=DIRECTION('center_axis',(-0.720953073140382,0.584827952253987,0.371756550166701));
#58354=DIRECTION('ref_axis',(0.459879282372611,0.0024618045807253,0.887978031914449));
#58355=DIRECTION('center_axis',(-0.886402301307037,6.8040664922404E-10,
0.462915716127234));
#58356=DIRECTION('ref_axis',(-0.462858873032855,0.0156707406196535,-0.886293456786852));
#58357=DIRECTION('',(0.886402259955158,-6.3782312761799E-11,-0.462915795308811));
#58358=DIRECTION('',(-0.238950069590406,1.64268989065784E-13,0.971031855421201));
#58359=DIRECTION('center_axis',(0.677733656698397,-0.60109852802926,-0.423506375606408));
#58360=DIRECTION('ref_axis',(0.525496001044302,-0.0069195257270167,0.850767931371511));
#58361=DIRECTION('',(0.954111946850913,2.37574025439388E-11,0.299450150903886));
#58362=DIRECTION('center_axis',(0.,-1.,1.45983193964168E-32));
#58363=DIRECTION('ref_axis',(1.,0.,0.));
#58364=DIRECTION('center_axis',(-0.675918227587769,0.601098527795593,0.426397830079587));
#58365=DIRECTION('ref_axis',(0.527806431987649,-0.00897201507403433,0.849317298362619));
#58366=DIRECTION('center_axis',(-0.689650908208436,-0.601098528172786,0.403809589083505));
#58367=DIRECTION('ref_axis',(0.510415466722804,-0.0079457331077057,0.859891223734446));
#58368=DIRECTION('center_axis',(0.691369715830186,0.601098527946894,-0.400859670873694));
#58369=DIRECTION('ref_axis',(0.506737309962297,-0.00794575175649518,0.86206389770202));
#58370=DIRECTION('center_axis',(-0.648087860160526,0.584827952230098,0.487809790597627));
#58371=DIRECTION('ref_axis',(0.590766628055431,-0.0181546317021972,0.806638209189085));
#58372=DIRECTION('center_axis',(0.82139394033835,-5.4349324088216E-10,-0.570361284428947));
#58373=DIRECTION('ref_axis',(-0.570291169341544,-0.0156795066169794,-0.82129296553867));
#58374=DIRECTION('',(-0.821393981728642,2.06171937742879E-7,0.570361224821538));
#58375=DIRECTION('center_axis',(-0.668671281884745,0.584827782536624,0.45918970105601));
#58376=DIRECTION('ref_axis',(0.549511870148897,-0.0273551074063184,0.835037964804146));
#58377=DIRECTION('center_axis',(-0.855586480187597,7.32921391904566E-10,
0.517659902754887));
#58378=DIRECTION('ref_axis',(-0.517596080894988,0.0157023279262901,-0.855480995662583));
#58379=DIRECTION('',(-0.855586424696769,-1.29267420091793E-5,0.517659994308522));
#58380=DIRECTION('',(-0.177506922439442,-7.62631952260005E-8,0.984119551927545));
#58381=DIRECTION('center_axis',(0.82139397988059,-7.72262198065806E-12,
-0.570361227483009));
#58382=DIRECTION('ref_axis',(-0.440248283571863,-0.635772805084867,-0.634014502299867));
#58383=DIRECTION('',(-0.971031855420821,0.,-0.23895006959195));
#58384=DIRECTION('center_axis',(-0.720807042413305,0.39856439157804,0.567083444806328));
#58385=DIRECTION('ref_axis',(0.618316971226236,-4.58880547466017E-16,0.785928828262212));
#58386=DIRECTION('center_axis',(0.779597758089364,5.74456436517556E-5,-0.62628055397085));
#58387=DIRECTION('ref_axis',(0.626280497553244,0.000362750097935672,0.77959772113368));
#58388=DIRECTION('',(-0.783960434937737,5.9497369157871E-5,0.620810786723538));
#58389=DIRECTION('center_axis',(-0.671432082927573,0.590180063811423,0.448181269460343));
#58390=DIRECTION('ref_axis',(-0.390733176690629,-0.795821494105799,0.462596729509043));
#58391=DIRECTION('center_axis',(0.194950885198616,0.550037558002531,0.812067015182176));
#58392=DIRECTION('ref_axis',(1.0056084917372E-16,-0.827952943501162,0.560797577872588));
#58393=DIRECTION('center_axis',(-0.872968580275457,-0.47712608966723,-0.101373331851685));
#58394=DIRECTION('ref_axis',(0.167281242125899,-0.0976209729541355,-0.98106428518844));
#58395=DIRECTION('center_axis',(0.,-1.,1.45983193964168E-32));
#58396=DIRECTION('ref_axis',(1.,0.,0.));
#58397=DIRECTION('center_axis',(-0.786810699055945,0.601098526818443,0.140033870573491));
#58398=DIRECTION('ref_axis',(0.172015417774543,-0.0043281742326977,0.985084749123476));
#58399=DIRECTION('center_axis',(-0.788661315181863,-0.601098528412519,0.12920483379471));
#58400=DIRECTION('ref_axis',(0.164122137841156,-0.00330174737487977,0.986434499769103));
#58401=DIRECTION('center_axis',(0.787401802179485,-0.601098528054466,-0.136670997271746));
#58402=DIRECTION('ref_axis',(0.169327964798454,-0.00227571930843304,0.985557132508736));
#58403=DIRECTION('center_axis',(0.789206135165619,0.601098527541506,-0.125834162310476));
#58404=DIRECTION('ref_axis',(0.159906318021571,-0.0033019368237457,0.987126672048728));
#58405=DIRECTION('center_axis',(0.,-1.,1.45983193964168E-32));
#58406=DIRECTION('ref_axis',(1.,0.,0.));
#58407=DIRECTION('center_axis',(-0.763055658010031,0.601098527992998,0.237542885440774));
#58408=DIRECTION('ref_axis',(0.272153471330359,-0.0345384700759067,0.961633808748242));
#58409=DIRECTION('center_axis',(-0.788661313920426,-0.601098533000795,0.129204820148475));
#58410=DIRECTION('ref_axis',(0.186403448113438,-0.0335099185808696,0.981901644711997));
#58411=DIRECTION('center_axis',(0.76406356176432,-0.601098537476189,-0.234280647574671));
#58412=DIRECTION('ref_axis',(0.26955334695223,-0.032481514321347,0.962437501541914));
#58413=DIRECTION('center_axis',(0.789206140541634,0.601098522388829,-0.125834153207089));
#58414=DIRECTION('ref_axis',(0.182206791918155,-0.0335101061238788,0.982689044289424));
#58415=DIRECTION('center_axis',(0.,-1.,1.45983193964168E-32));
#58416=DIRECTION('ref_axis',(1.,0.,0.));
#58417=DIRECTION('center_axis',(-0.798157352253882,0.601098536492064,0.0403161316369818));
#58418=DIRECTION('ref_axis',(0.0698515706646391,0.0258666611243446,0.997221978256577));
#58419=DIRECTION('center_axis',(-0.788661314308054,-0.601098522653569,0.129204865920715));
#58420=DIRECTION('ref_axis',(0.141618704730856,0.0268944934460804,0.989555874467245));
#58421=DIRECTION('center_axis',(0.798322321900873,-0.601098527948964,-0.0369056913278559));
#58422=DIRECTION('ref_axis',(0.0671306538928277,0.027922015095456,0.997353415986996));
#58423=DIRECTION('center_axis',(0.789206130815412,0.601098532003673,-0.125834168278713));
#58424=DIRECTION('ref_axis',(0.137389735591166,0.0268942886600805,0.99015188622335));
#58425=DIRECTION('center_axis',(0.,-1.,1.45983193964168E-32));
#58426=DIRECTION('ref_axis',(1.,0.,0.));
#58427=DIRECTION('center_axis',(-0.760723846485499,0.601098528328861,0.244907714515458));
#58428=DIRECTION('ref_axis',(0.321534013967133,0.0212181329446819,0.946660271003556));
#58429=DIRECTION('center_axis',(-0.734823571847927,-0.60109852793342,0.314189239110651));
#58430=DIRECTION('ref_axis',(0.377605244297892,0.0222452123488197,0.925699427463518));
#58431=DIRECTION('center_axis',(0.761763160169678,-0.601098528110665,-0.241655637864085));
#58432=DIRECTION('ref_axis',(0.318938028103574,0.0232723692944289,0.947489805252187));
#58433=DIRECTION('center_axis',(0.73615909432316,0.601098528132069,-0.31104717861245));
#58434=DIRECTION('ref_axis',(0.373647180134697,0.0222452071622992,0.927304122462364));
#58435=DIRECTION('center_axis',(0.,-1.,1.45983193964168E-32));
#58436=DIRECTION('ref_axis',(1.,0.,0.));
#58437=DIRECTION('center_axis',(-0.785420383285721,0.601098529650706,0.147632581671769));
#58438=DIRECTION('ref_axis',(0.22240539569108,0.0514849804187075,0.973593928061787));
#58439=DIRECTION('center_axis',(0.736159119253747,0.601098531981097,-0.311047112170677));
#58440=DIRECTION('ref_axis',(0.351983410607425,0.0525165497891723,0.934531802912777));
#58441=DIRECTION('',(-0.957443409238448,3.88578058618629E-13,0.288621063170827));
#58442=DIRECTION('center_axis',(-0.764517729382288,0.58482795214616,0.271088376454395));
#58443=DIRECTION('ref_axis',(0.29771334017134,-0.0526562728465342,0.953202016371102));
#58444=DIRECTION('center_axis',(-0.973676803711829,7.80713441197243E-10,
0.227933064546407));
#58445=DIRECTION('ref_axis',(-0.227904709319416,0.0157729998142581,-0.973555676860287));
#58446=DIRECTION('',(0.973676779880511,-1.76914038951382E-10,-0.227933166348205));
#58447=DIRECTION('',(-0.472928816313912,0.,0.88110063823602));
#58448=DIRECTION('',(0.849666541299393,6.73708191429312E-11,0.527320366187697));
#58449=DIRECTION('center_axis',(-0.782151896996921,0.584827930051179,0.214976050424628));
#58450=DIRECTION('ref_axis',(0.280192919632944,0.0219594825691283,0.959692507479798));
#58451=DIRECTION('center_axis',(0.937430225687632,-1.00225340753624E-8,
-0.348173192487928));
#58452=DIRECTION('ref_axis',(-0.348130065144794,-0.0157391393476006,-0.937314108095508));
#58453=DIRECTION('',(-0.937431446873868,0.,0.348169904517848));
#58454=DIRECTION('center_axis',(-0.790755100933366,0.584827952320552,0.180783396727721));
#58455=DIRECTION('ref_axis',(0.245384617050075,0.0322834330615039,0.968888109982237));
#58456=DIRECTION('center_axis',(-0.957443430531097,5.48477399997537E-10,
0.288620992536655));
#58457=DIRECTION('ref_axis',(-0.28858540981457,0.0157020800817192,-0.957325391872201));
#58458=DIRECTION('',(0.95744340923852,-1.22124532708705E-12,-0.288621063170588));
#58459=DIRECTION('',(-0.41667083249281,0.,0.909057433471477));
#58460=DIRECTION('',(0.881100638236075,1.43735365432681E-13,0.47292881631381));
#58461=DIRECTION('center_axis',(-0.749040407174815,0.584827953375321,0.311311312628085));
#58462=DIRECTION('ref_axis',(0.378544724024558,-0.00784642890859345,0.925549742297276));
#58463=DIRECTION('center_axis',(0.913719640106859,-1.87941711854915E-9,
-0.406345197194444));
#58464=DIRECTION('ref_axis',(-0.406295255358328,-0.0156778482813538,-0.913607339367728));
#58465=DIRECTION('',(-0.913719870860235,3.88578058618638E-13,0.406344678315288));
#58466=DIRECTION('center_axis',(-0.76186159335239,0.584827952253948,0.278465758823256));
#58467=DIRECTION('ref_axis',(0.344959838796073,0.00246180458216537,0.938614217416286));
#58468=DIRECTION('center_axis',(-0.937431470422838,5.10643621529069E-10,
0.348169841113322));
#58469=DIRECTION('ref_axis',(-0.348127088079396,0.0156707406182868,-0.937316359845402));
#58470=DIRECTION('',(0.937431446873923,-6.41708908203887E-11,-0.348169904517699));
#58471=DIRECTION('',(-0.35876843925459,1.64268989065808E-13,0.933426594325888));
#58472=DIRECTION('center_axis',(0.725468946368522,-0.601098528002572,-0.335224353960282));
#58473=DIRECTION('ref_axis',(0.414722814901041,-0.00691952791939243,0.909921483939098));
#58474=DIRECTION('',(0.909057433466349,2.35931335548692E-11,0.416670832503999));
#58475=DIRECTION('center_axis',(-0.811136126793454,0.584827951389749,0.00586950456028211));
#58476=DIRECTION('ref_axis',(0.0263728513782388,0.0265489690017877,0.99929956717449));
#58477=DIRECTION('center_axis',(0.994566648832187,8.50721872347641E-12,
-0.104101782072709));
#58478=DIRECTION('ref_axis',(-0.104088873058919,-0.0157477670547349,-0.994443318816168));
#58479=DIRECTION('center_axis',(-0.998722132347498,-0.000115441181840488,
0.0505379959297901));
#58480=DIRECTION('ref_axis',(0.00137233352454056,-0.999690590777516,0.0248362519635856));
#58481=DIRECTION('',(0.999140703554945,-6.069034161454E-10,-0.041447008332686));
#58482=DIRECTION('',(0.735806627409681,2.24206636476401E-10,0.677191706284115));
#58483=DIRECTION('center_axis',(-0.80400442922631,0.584827952222711,0.107485552905802));
#58484=DIRECTION('ref_axis',(0.130176731431605,-0.00326197145312202,0.991485440203749));
#58485=DIRECTION('center_axis',(0.986067481394172,-5.51759956911657E-10,
-0.166345790860347));
#58486=DIRECTION('ref_axis',(-0.166325332124458,-0.0156832196314432,-0.985946205690595));
#58487=DIRECTION('',(-0.986067493321454,8.32135976760707E-8,0.16634572015756));
#58488=DIRECTION('center_axis',(-0.807915700396783,0.584827969931553,0.0724463017559439));
#58489=DIRECTION('ref_axis',(0.0943677593143437,0.00704480134984,0.995512479467702));
#58490=DIRECTION('center_axis',(-0.994566657124383,6.29001243004044E-10,
0.104101702850767));
#58491=DIRECTION('ref_axis',(-0.104088918533863,0.0156715280532925,-0.994444518435758));
#58492=DIRECTION('',(0.994566648423263,-1.40443212613673E-11,-0.104101785979482));
#58493=DIRECTION('',(-0.579630810343145,-3.07808057783809E-8,0.814879208043099));
#58494=DIRECTION('center_axis',(0.112789953813512,0.793626260378774,0.597859335593205));
#58495=DIRECTION('ref_axis',(-8.52455597729631E-17,-0.601698864106725,0.798723028923467));
#58496=DIRECTION('center_axis',(-0.734975505034963,0.4715466745576,-0.487293279978568));
#58497=DIRECTION('ref_axis',(-0.319218617798124,0.393407181090822,0.862166030366094));
#58498=DIRECTION('',(0.776875900240113,5.05127141378944E-12,0.629653742644411));
#58499=DIRECTION('center_axis',(-0.784195235649416,0.584828255987556,0.207397549125613));
#58500=DIRECTION('ref_axis',(0.232410023807321,-0.0330815410766171,0.972055138597537));
#58501=DIRECTION('center_axis',(0.973669013264507,-1.08193100855599E-7,
-0.227966340955215));
#58502=DIRECTION('ref_axis',(-0.227938333995393,-0.0156751635311225,-0.973549385056391));
#58503=DIRECTION('',(-0.973676779881119,7.77156117237206E-13,0.22793316634561));
#58504=DIRECTION('center_axis',(-0.792465661813423,0.584827952226059,0.17313128296668));
#58505=DIRECTION('ref_axis',(0.197321433282868,-0.022760729597827,0.980074589587634));
#58506=DIRECTION('center_axis',(-0.986067510765312,8.16820737104964E-10,
0.166345616753496));
#58507=DIRECTION('ref_axis',(-0.166325131471838,0.015693390508592,-0.985946077701626));
#58508=DIRECTION('',(0.986067493104091,-2.20934381896923E-11,-0.166345721446069));
#58509=DIRECTION('',(-0.527320366157622,0.,0.849666541318058));
#58510=DIRECTION('',(0.814879198734754,8.17238220596398E-12,0.579630823429366));
#58511=DIRECTION('center_axis',(0.,-1.,1.45983193964168E-32));
#58512=DIRECTION('ref_axis',(1.,0.,0.));
#58513=DIRECTION('center_axis',(-0.724030231397888,0.601098527836107,0.338320534190856));
#58514=DIRECTION('ref_axis',(0.417196833668173,-0.00897201206616011,0.908771866299092));
#58515=DIRECTION('center_axis',(-0.734823570967135,-0.601098528090507,0.314189240870107));
#58516=DIRECTION('ref_axis',(0.398617732222085,-0.00794574009299561,0.917082749141263));
#58517=DIRECTION('center_axis',(0.736159098339688,0.601098527936454,-0.311047169484511));
#58518=DIRECTION('ref_axis',(0.394696278215606,-0.00794575246477388,0.91877729237314));
#58519=DIRECTION('center_axis',(-0.704116272226526,0.584827952230066,0.402736317553072));
#58520=DIRECTION('ref_axis',(0.485009681668631,-0.0181546317046172,0.874320317752804));
#58521=DIRECTION('center_axis',(0.886402227295928,-5.52722010689124E-10,
-0.462915857845481));
#58522=DIRECTION('ref_axis',(-0.462858951134617,-0.015679506619194,-0.886293260962048));
#58523=DIRECTION('',(-0.88640226145087,2.06171882231894E-7,0.462915792444739));
#58524=DIRECTION('center_axis',(-0.720950339151385,0.584827782536519,0.37176211917155));
#58525=DIRECTION('ref_axis',(0.440520796653547,-0.0273551074137171,0.897325540600572));
#58526=DIRECTION('center_axis',(-0.913719924310483,9.17652330754914E-10,
0.406344558125301));
#58527=DIRECTION('ref_axis',(-0.406294460236443,0.0157023279264494,-0.913607272562378));
#58528=DIRECTION('',(-0.91371987116053,-1.29267419736916E-5,0.406344677434421));
#58529=DIRECTION('',(-0.299450112994252,-7.6263051490643E-8,0.954111958748932));
#58530=DIRECTION('center_axis',(0.886402259958573,5.51249576955609E-12,
-0.462915795302272));
#58531=DIRECTION('ref_axis',(-0.357313706641208,-0.635772805085359,-0.68419284953894));
#58532=DIRECTION('',(-0.933426594325549,0.,-0.358768439255471));
#58533=DIRECTION('center_axis',(-0.786197665429277,0.398564391573593,0.472270745063811));
#58534=DIRECTION('ref_axis',(0.514938355828264,6.04616573156442E-16,0.857227210077284));
#58535=DIRECTION('center_axis',(0.85194416384702,5.74456530678644E-5,-0.52363263686195));
#58536=DIRECTION('ref_axis',(0.523632585407709,0.000363224037420787,0.851944119979437));
#58537=DIRECTION('',(-0.855586896082275,5.94973699395157E-5,0.517659211945815));
#58538=DIRECTION('center_axis',(-0.722309648058218,0.590180063816037,0.360494472351674));
#58539=DIRECTION('ref_axis',(-0.445631531500632,-0.795821662861919,0.409976120099806));
#58540=DIRECTION('center_axis',(0.0916346543585759,0.550037558005875,0.830097449040484));
#58541=DIRECTION('ref_axis',(-1.25152671372798E-16,-0.833604678715212,0.552361511715025));
#58542=DIRECTION('center_axis',(-0.853379514155569,-0.477126090889111,-0.209985947654791));
#58543=DIRECTION('ref_axis',(0.288925961123907,-0.0976286666970697,-0.952360452994337));
#58544=DIRECTION('center_axis',(0.,-1.,1.45983193964168E-32));
#58545=DIRECTION('ref_axis',(1.,0.,0.));
#58546=DIRECTION('center_axis',(-0.786810702938747,0.601098516361292,0.140033893644677));
#58547=DIRECTION('ref_axis',(0.149483054325176,-0.0345386753521871,0.988160865636022));
#58548=DIRECTION('center_axis',(-0.798636142119035,-0.601098532740246,0.0293405255363244));
#58549=DIRECTION('ref_axis',(0.0618686902012185,-0.0335099203682645,0.997521603981437));
#58550=DIRECTION('center_axis',(0.787401802117191,-0.60109852815296,-0.136670997197453));
#58551=DIRECTION('ref_axis',(0.1468026567879,-0.0324816839227375,0.988632348332563));
#58552=DIRECTION('center_axis',(0.798754216513376,0.601098522019537,-0.0259281396947761));
#58553=DIRECTION('ref_axis',(0.057606428403082,-0.0335101155912361,0.997776814502974));
#58554=DIRECTION('center_axis',(0.,-1.,1.45983193964168E-32));
#58555=DIRECTION('ref_axis',(1.,0.,0.));
#58556=DIRECTION('center_axis',(-0.797730380527669,0.60109852822162,0.0480291510749676));
#58557=DIRECTION('ref_axis',(0.0986279656220281,0.051484996853496,0.993791637867946));
#58558=DIRECTION('center_axis',(0.769338807450739,0.601098527991798,-0.216329283723609));
#58559=DIRECTION('ref_axis',(0.232080081996,0.0525165954341669,0.971277943095968));
#58560=DIRECTION('center_axis',(0.,-1.,1.45983193964168E-32));
#58561=DIRECTION('ref_axis',(1.,0.,0.));
#58562=DIRECTION('center_axis',(-0.798157359514994,0.60109852682156,0.0403161320689704));
#58563=DIRECTION('ref_axis',(0.047195167488092,-0.00432817393868725,0.998876310198679));
#58564=DIRECTION('center_axis',(-0.79863614492077,-0.601098528403341,0.0293405381243889));
#58565=DIRECTION('ref_axis',(0.0391949569049173,-0.00330174988199066,0.999226127461116));
#58566=DIRECTION('center_axis',(0.798322321310044,-0.601098528021013,-0.036905702934847));
#58567=DIRECTION('ref_axis',(0.0444697099494423,-0.00227572610152403,0.999008141091815));
#58568=DIRECTION('center_axis',(0.798754211449592,0.601098527548076,-0.0259281675225105));
#58569=DIRECTION('ref_axis',(0.03492563283816,-0.00330193561822562,0.999384459250807));
#58570=DIRECTION('center_axis',(0.,-1.,1.45983193964168E-32));
#58571=DIRECTION('ref_axis',(1.,0.,0.));
#58572=DIRECTION('center_axis',(-0.796916594028537,0.601098536374166,-0.0600374194214937));
#58573=DIRECTION('ref_axis',(-0.0556842885238396,0.0258666638057379,0.998113308054328));
#58574=DIRECTION('center_axis',(-0.798636147949864,-0.601098522706458,0.0293405723856551));
#58575=DIRECTION('ref_axis',(0.0164777599185274,0.0268944923173048,0.999502461083044));
#58576=DIRECTION('center_axis',(0.796652821507865,-0.601098527915204,0.0634416402824783));
#58577=DIRECTION('ref_axis',(-0.0584002209349251,0.0279220158115366,0.99790268825561));
#58578=DIRECTION('center_axis',(0.798754207866941,0.601098531819143,-0.025928178874069));
#58579=DIRECTION('ref_axis',(0.0122074444057763,0.0268942928144612,0.999563742497241));
#58580=DIRECTION('center_axis',(0.,-1.,1.45983193964168E-32));
#58581=DIRECTION('ref_axis',(1.,0.,0.));
#58582=DIRECTION('center_axis',(-0.760723845934306,0.601098527910175,0.24490771725517));
#58583=DIRECTION('ref_axis',(0.300007788767924,-0.00897200679300414,0.953894559043444));
#58584=DIRECTION('center_axis',(-0.768407619804461,-0.601098528125849,0.219613955183591));
#58585=DIRECTION('ref_axis',(0.280533569597203,-0.00794573722101145,0.959811326037084));
#58586=DIRECTION('center_axis',(0.761763161499585,-0.601098528053865,-0.241655633813147));
#58587=DIRECTION('ref_axis',(0.297409194101466,-0.00691952345940434,0.954725034477996));
#58588=DIRECTION('center_axis',(0.769338810340699,0.601098527970217,-0.216329273505912));
#58589=DIRECTION('ref_axis',(0.276430654457888,-0.00794574992649899,0.961001018903773));
#58590=DIRECTION('center_axis',(0.,-1.,1.45983193964168E-32));
#58591=DIRECTION('ref_axis',(1.,0.,0.));
#58592=DIRECTION('center_axis',(-0.785420387740065,0.601098528306397,0.147632563447667));
#58593=DIRECTION('ref_axis',(0.200350628531198,0.0212181335979679,0.979494469843384));
#58594=DIRECTION('center_axis',(-0.768407622369157,-0.601098527984367,0.219613946597221));
#58595=DIRECTION('ref_axis',(0.258606809898566,0.0222452109926528,0.965726497752847));
#58596=DIRECTION('center_axis',(0.786043913939973,-0.601098527958986,-0.144275864383021));
#58597=DIRECTION('ref_axis',(0.197671140201316,0.0232723733017627,0.979992100464292));
#58598=DIRECTION('center_axis',(0.769338810009928,0.601098528244495,-0.216329273920128));
#58599=DIRECTION('ref_axis',(0.254478832329244,0.0222452039836464,0.966822462914506));
#58600=DIRECTION('center_axis',(-0.802928197021279,0.584827908067885,0.115250285783159));
#58601=DIRECTION('ref_axis',(0.157701346099928,0.021960067734333,0.987242645383279));
#58602=DIRECTION('center_axis',(0.973675213540049,-1.90745723150787E-8,
-0.227939857282003));
#58603=DIRECTION('ref_axis',(-0.227911623139389,-0.0157391387082283,-0.973554606352767));
#58604=DIRECTION('',(-0.973676779881003,0.,0.227933166346105));
#58605=DIRECTION('center_axis',(-0.807177928462317,0.584827952320411,0.0802499718878338));
#58606=DIRECTION('ref_axis',(0.122015806264322,0.0322834330627758,0.992002985364131));
#58607=DIRECTION('center_axis',(-0.986067506113591,5.83269785121389E-10,
0.166345644328079));
#58608=DIRECTION('ref_axis',(-0.16632513635319,0.015702080082056,-0.985945938527153));
#58609=DIRECTION('',(0.986067493104161,-4.44089209849969E-13,-0.166345721445658));
#58610=DIRECTION('',(-0.527320366157736,0.,0.849666541317987));
#58611=DIRECTION('',(0.814879198737098,1.43735365432635E-13,0.579630823426072));
#58612=DIRECTION('center_axis',(-0.782151653290743,0.58482795337546,0.214976873652094));
#58613=DIRECTION('ref_axis',(0.259557643791007,-0.00784642891460876,0.965695740439476));
#58614=DIRECTION('center_axis',(0.957443242800339,-1.9481252264197E-9,-0.288621615295826));
#58615=DIRECTION('ref_axis',(-0.28858614228077,-0.0156778482810863,-0.957325568214272));
#58616=DIRECTION('',(-0.95744340923868,-3.88578058618785E-13,0.288621063170055));
#58617=DIRECTION('center_axis',(-0.790755101119389,0.584827952254179,0.180783396128763));
#58618=DIRECTION('ref_axis',(0.224600172503117,0.00246180457544701,0.974447896005632));
#58619=DIRECTION('center_axis',(-0.97367679496501,4.99433705161115E-10,
0.227933101910772));
#58620=DIRECTION('ref_axis',(-0.227905113178174,0.0156707406176226,-0.973557233692883));
#58621=DIRECTION('',(0.973676779880786,-6.4614980030186E-11,-0.227933166347032));
#58622=DIRECTION('',(-0.472928816313917,1.64268989065853E-13,0.881100638236018));
#58623=DIRECTION('',(0.849666541311608,2.34493981894313E-11,0.527320366168015));
#58624=DIRECTION('center_axis',(-0.749021847116042,0.584826536165524,0.311358627854613));
#58625=DIRECTION('ref_axis',(0.371641576311207,-0.0181846249388088,0.928198178285627));
#58626=DIRECTION('center_axis',(0.93743142220389,-5.5501891853302E-10,-0.348169970940619));
#58627=DIRECTION('ref_axis',(-0.348127170059145,-0.0156795066183704,-0.937316182800028));
#58628=DIRECTION('',(-0.937431447998895,2.06171549165055E-7,0.348169901488703));
#58629=DIRECTION('center_axis',(-0.761859578893809,0.584827782536394,0.278471626600113));
#58630=DIRECTION('ref_axis',(0.32458244704978,-0.0273551074290013,0.945461756584963));
#58631=DIRECTION('center_axis',(-0.957443434474091,5.7096507072109E-10,
0.288620979456547));
#58632=DIRECTION('ref_axis',(-0.288585395612374,0.0157023279254197,-0.957325392088276));
#58633=DIRECTION('',(-0.957443409425798,-1.29267425264385E-5,0.288621062259848));
#58634=DIRECTION('',(-0.416670796384237,-7.6262907755298E-8,0.90905745002201));
#58635=DIRECTION('center_axis',(0.937431446872798,-2.82675655164576E-12,
-0.348169904520728));
#58636=DIRECTION('ref_axis',(-0.268744079138403,-0.635772805084965,-0.723581066807615));
#58637=DIRECTION('',(-0.8811006382351,0.,-0.472928816315627));
#58638=DIRECTION('center_axis',(-0.80547572014595,0.584827951390055,-0.0958390918585707));
#58639=DIRECTION('ref_axis',(-0.099080552477698,0.0265489689961426,0.994725186353475));
#58640=DIRECTION('center_axis',(0.999771606780537,-3.77560611900383E-11,
0.0213713423879551));
#58641=DIRECTION('ref_axis',(0.0213686922602901,-0.0157477670553484,-0.999647631330088));
#58642=DIRECTION('center_axis',(-0.996456868435036,-1.82930342323839E-11,
-0.0841053467304035));
#58643=DIRECTION('ref_axis',(0.00137653801704517,0.999866054443186,-0.0163088416297004));
#58644=DIRECTION('',(0.996456868254416,-6.06792393843473E-10,0.0841053488703394));
#58645=DIRECTION('',(0.645129946086367,2.242066364764E-10,0.76407287130391));
#58646=DIRECTION('center_axis',(-0.81113612606466,0.584827952222608,0.00586952229118291));
#58647=DIRECTION('ref_axis',(0.00488417276115256,-0.00326197144681202,0.999982752050614));
#58648=DIRECTION('center_axis',(0.999140699079624,-8.46367557917498E-10,
-0.0414471162167002));
#58649=DIRECTION('ref_axis',(-0.0414420186801338,-0.0156832196316866,-0.999017815511665));
#58650=DIRECTION('',(-0.999140703609447,8.32139862541118E-8,0.041447007018758));
#58651=DIRECTION('center_axis',(-0.810624973045738,0.584827969931961,-0.0293836461293935));
#58652=DIRECTION('ref_axis',(-0.0311471567426006,0.0070448013376867,0.999489982641629));
#58653=DIRECTION('center_axis',(-0.999771605135594,5.82131145152661E-10,
-0.021371419339818));
#58654=DIRECTION('ref_axis',(0.0213687948117744,0.0156715280532176,-0.999648827247234));
#58655=DIRECTION('',(0.99977160679441,-1.48769885298236E-11,0.0213713417389642));
#58656=DIRECTION('',(-0.677191694384739,-3.07809495137633E-8,0.735806638361142));
#58657=DIRECTION('center_axis',(0.0369689275944231,0.793626260379842,0.607281365783626));
#58658=DIRECTION('ref_axis',(2.85820292298768E-17,-0.607696777849814,0.794169142054105));
#58659=DIRECTION('center_axis',(-0.668105961212897,0.471546674538878,-0.575567683529154));
#58660=DIRECTION('ref_axis',(-0.424756903944142,0.393410586642562,0.815358622245048));
#58661=DIRECTION('',(0.691833462133554,5.05127141378853E-12,0.722057103470564));
#58662=DIRECTION('center_axis',(-0.804005427452842,0.584828255987393,0.107476432882369));
#58663=DIRECTION('ref_axis',(0.108746587635101,-0.0330815410815246,0.993518893286581));
#58664=DIRECTION('center_axis',(0.994563100012491,-1.08262028849995E-7,
-0.104135681173802));
#58665=DIRECTION('ref_axis',(-0.10412288844737,-0.0156751635309253,-0.994440904905694));
#58666=DIRECTION('',(-0.994566648423227,3.88578058618661E-13,0.104101785979821));
#58667=DIRECTION('center_axis',(-0.807915936897736,0.584827952226153,0.0724438071999103));
#58668=DIRECTION('ref_axis',(0.0729295773933777,-0.0227607295944781,0.997077341999882));
#58669=DIRECTION('center_axis',(-0.999140706646079,5.68849416964949E-10,
0.0414469338163077));
#58670=DIRECTION('ref_axis',(-0.0414418296657482,0.0156933905078002,-0.999017663631792));
#58671=DIRECTION('',(0.999140703555315,-2.24820162483055E-11,-0.041447008323772));
#58672=DIRECTION('',(-0.62965374264226,0.,0.776875900241856));
#58673=DIRECTION('',(0.735806627486024,8.0286468406269E-12,0.677191706201164));
#58674=DIRECTION('',(-0.986067493104082,7.77156117237022E-13,0.166345721446123));
#58675=DIRECTION('center_axis',(-0.792465661535707,0.584827952145603,0.173131284509631));
#58676=DIRECTION('ref_axis',(0.175897890621741,-0.0526562728545463,0.98299910936068));
#58677=DIRECTION('center_axis',(-0.994566657961751,6.7861735203041E-10,
0.104101694850723));
#58678=DIRECTION('ref_axis',(-0.104088744433143,0.0157729998146477,-0.994442932379319));
#58679=DIRECTION('',(0.994566648423056,-1.76525460892884E-10,-0.104101785981459));
#58680=DIRECTION('',(-0.579630823425941,0.,0.814879198737191));
#58681=DIRECTION('',(0.776875900220228,6.51531877903912E-11,0.629653742668945));
#58682=DIRECTION('center_axis',(-0.83918948161091,0.39856439156716,0.370010053550321));
#58683=DIRECTION('ref_axis',(-0.429012364341953,-0.903298616871369,3.62132827148377E-16));
#58684=DIRECTION('center_axis',(0.910854901238292,5.74456698535606E-5,-0.412726720228018));
#58685=DIRECTION('ref_axis',(0.412726674652397,0.000363348493937081,0.910854851229463));
#58686=DIRECTION('',(-0.913720240772838,5.94973707566566E-5,0.406343842160909));
#58687=DIRECTION('center_axis',(-0.761795958691224,0.590180063811968,0.267122461804732));
#58688=DIRECTION('ref_axis',(0.493495347852432,0.795819764955679,-0.350903467286796));
#58689=DIRECTION('center_axis',(-0.0131267097189408,0.550037558010457,0.835036750251058));
#58690=DIRECTION('ref_axis',(6.76045893512397E-18,-0.835108702353105,0.550084952761038));
#58691=DIRECTION('center_axis',(-0.820332144360729,-0.477126090118974,-0.315286959857698));
#58692=DIRECTION('ref_axis',(0.406006491071471,-0.0976208218760109,-0.908641240723798));
#58693=DIRECTION('center_axis',(-0.87894677835708,0.398564391567542,0.261914082458552));
#58694=DIRECTION('ref_axis',(-0.412981067386498,-0.910739610415792,-1.42150438893369E-16));
#58695=DIRECTION('center_axis',(0.955400912707171,5.74456423295275E-5,-0.295311856684258));
#58696=DIRECTION('ref_axis',(0.295311817796603,0.000362973412833882,0.955400857504308));
#58697=DIRECTION('',(-0.957443671436405,5.94973691223933E-5,0.288620187246907));
#58698=DIRECTION('center_axis',(-0.789268291903739,0.590180063813734,0.169537770635844));
#58699=DIRECTION('ref_axis',(0.533588748824947,0.795821946541685,-0.2862699364761));
#58700=DIRECTION('center_axis',(-0.117681057741536,0.550037558015597,0.826807023084028));
#58701=DIRECTION('ref_axis',(4.25184181647116E-17,-0.832592338318892,0.553886268265137));
#58702=DIRECTION('center_axis',(-0.774347645955717,-0.477126090634454,-0.415615708123167));
#58703=DIRECTION('ref_axis',(0.516691144115654,-0.0976284509969061,-0.850587412996689));
#58704=DIRECTION('center_axis',(-0.0394351207028803,0.793626260377946,0.607126206067294));
#58705=DIRECTION('ref_axis',(-1.39708533644483E-17,-0.607598837097768,0.794244076564276));
#58706=DIRECTION('center_axis',(-0.590699987197054,0.471546674561303,-0.654765040938791));
#58707=DIRECTION('ref_axis',(-0.523594102005531,0.3934170135974,0.75569323786648));
#58708=DIRECTION('center_axis',(-1.19900741137893E-16,-1.,1.45983193964168E-32));
#58709=DIRECTION('ref_axis',(-1.,1.19900741137893E-16,0.));
#58710=DIRECTION('center_axis',(-1.19900741137893E-16,-1.,1.45983193964168E-32));
#58711=DIRECTION('ref_axis',(-1.,1.19900741137893E-16,0.));
#58712=DIRECTION('center_axis',(-1.19900741137893E-16,-1.,1.45983193964168E-32));
#58713=DIRECTION('ref_axis',(-1.,1.19900741137893E-16,0.));
#58714=DIRECTION('center_axis',(-0.796301631197733,-0.584827952229447,0.154531480426938));
#58715=DIRECTION('ref_axis',(0.174895616737967,0.0219588922001345,0.984342079918962));
#58716=DIRECTION('center_axis',(-0.78883375237848,-0.58482795222954,0.188990945284396));
#58717=DIRECTION('ref_axis',(0.210169515934559,0.0322834340869575,0.977131799940717));
#58718=DIRECTION('center_axis',(-0.811140170796249,-0.584827952229906,-0.00528106156067749));
#58719=DIRECTION('ref_axis',(0.0314665010204262,-0.0526562713691229,0.998116815006657));
#58720=DIRECTION('center_axis',(-0.811140170796482,-0.584827952229454,-0.00528106157488254));
#58721=DIRECTION('ref_axis',(0.00990171161333319,-0.0227607290413202,0.999691905199114));
#58722=DIRECTION('center_axis',(-0.81014435690596,-0.584827952229489,-0.0405263773916719));
#58723=DIRECTION('ref_axis',(-0.0260944005329791,-0.0330869094618765,0.999111774869602));
#58724=DIRECTION('center_axis',(-0.811140170796523,-0.584827952229448,-0.00528106156919257));
#58725=DIRECTION('ref_axis',(-0.0115903885860303,0.00704626726206911,0.999908002273257));
#58726=DIRECTION('center_axis',(-0.810144356905825,-0.584827952229486,-0.0405263773944057));
#58727=DIRECTION('ref_axis',(-0.0476118958772688,-0.00326197171456771,0.998860584321709));
#58728=DIRECTION('center_axis',(-0.810144356905296,-0.584827952229881,-0.0405263773992749));
#58729=DIRECTION('ref_axis',(-0.0690517656280587,0.0265489589827359,0.997259748731784));
#58730=DIRECTION('center_axis',(-0.811140170795812,-0.584827952230272,-0.00528106158720195));
#58731=DIRECTION('ref_axis',(-0.0330971952597666,0.0368858773873733,0.99877124894307));
#58732=DIRECTION('center_axis',(0.814941485545711,-0.572651970021063,0.0891072183807034));
#58733=DIRECTION('ref_axis',(0.574939054737167,0.81819623767036,-3.64197201067138E-17));
#58734=DIRECTION('center_axis',(0.876234650030245,-0.398672303280863,-0.270690289229419));
#58735=DIRECTION('ref_axis',(0.414133355848299,0.910216218034938,7.98171504109407E-18));
#58736=DIRECTION('center_axis',(-0.788833752377747,-0.584827952229584,0.18899094528732));
#58737=DIRECTION('ref_axis',(0.252033915040477,-0.0273514773899239,0.967331795380446));
#58738=DIRECTION('center_axis',(-0.796301631197723,-0.584827952229588,0.154531480426454));
#58739=DIRECTION('ref_axis',(0.216973405116302,-0.0376838387932248,0.975449880704305));
#58740=DIRECTION('center_axis',(-0.796301631197232,-0.584827952229512,0.154531480429274));
#58741=DIRECTION('ref_axis',(0.196052058349387,-0.0078465155714681,0.980562095234338));
#58742=DIRECTION('center_axis',(-0.788833752378357,-0.584827952229601,0.18899094528472));
#58743=DIRECTION('ref_axis',(0.231262112084199,0.0024618052359846,0.972888367198075));
#58744=DIRECTION('center_axis',(0.819683524323173,-0.572651970037011,-0.0137346702134645));
#58745=DIRECTION('ref_axis',(0.572705990547634,0.819760848291045,1.96554044353146E-18));
#58746=DIRECTION('center_axis',(0.835398788851755,-0.39867230328298,-0.378377137496526));
#58747=DIRECTION('ref_axis',(0.430693725907008,0.902498152055914,1.54228934430356E-17));
#58748=DIRECTION('center_axis',(-0.758926716337915,-0.584827952229656,0.286367780169868));
#58749=DIRECTION('ref_axis',(0.371285374189789,-0.0273514773865269,0.928115869704598));
#58750=DIRECTION('center_axis',(-0.770654624865961,-0.58482795222928,0.253116011868101));
#58751=DIRECTION('ref_axis',(0.337518792731011,-0.0376838387990361,0.940564188584048));
#58752=DIRECTION('center_axis',(-0.805405980798282,-0.584827952229224,0.0964234016498613));
#58753=DIRECTION('ref_axis',(0.156315586147125,-0.0526562713792445,0.986302567477098));
#58754=DIRECTION('center_axis',(-0.805405980797294,-0.584827952229503,0.0964234016564226));
#58755=DIRECTION('ref_axis',(0.135118252709478,-0.0227607290393984,0.990568022398428));
#58756=DIRECTION('center_axis',(-0.808835428595534,-0.584827952229771,0.0613311971137978));
#58757=DIRECTION('ref_axis',(0.0993332710549336,-0.0330869094570363,0.994503975700504));
#58758=DIRECTION('center_axis',(-0.805405980797101,-0.5848279522295,0.0964234016580494));
#58759=DIRECTION('ref_axis',(0.113822708281416,0.00704626726155522,0.993476089897066));
#58760=DIRECTION('center_axis',(-0.808835428596934,-0.584827952229517,0.0613311970977501));
#58761=DIRECTION('ref_axis',(0.0779539650531781,-0.0032619717164415,0.996951623135751));
#58762=DIRECTION('center_axis',(-0.808835428596281,-0.584827952229553,0.0613311971060317));
#58763=DIRECTION('ref_axis',(0.0564825171890357,0.0265489589884549,0.998050538814854));
#58764=DIRECTION('center_axis',(-0.80540598079873,-0.584827952230285,0.0964234016396851));
#58765=DIRECTION('ref_axis',(0.0923430162306484,0.0368858773872494,0.995043817830551));
#58766=DIRECTION('center_axis',(-0.758926716341125,-0.584827952229569,0.286367780161537));
#58767=DIRECTION('ref_axis',(0.351373786213101,0.00246180523518679,0.93623202352689));
#58768=DIRECTION('center_axis',(-0.770654624866236,-0.584827952229576,0.25311601186658));
#58769=DIRECTION('ref_axis',(0.317403147406832,-0.00784651558018333,0.948258231817413));
#58770=DIRECTION('center_axis',(-0.770654624861251,-0.584827952229353,0.253116011882271));
#58771=DIRECTION('ref_axis',(0.2968872883741,0.02195889220305,0.954660015427005));
#58772=DIRECTION('center_axis',(-0.75892671634115,-0.584827952229477,0.286367780161659));
#58773=DIRECTION('ref_axis',(0.330979354631449,0.0322834340865671,0.943085598814513));
#58774=DIRECTION('center_axis',(0.811498664278269,-0.572651970034831,-0.116359954837616));
#58775=DIRECTION('ref_axis',(0.576568537396316,0.817048787824003,-1.47601094058414E-16));
#58776=DIRECTION('center_axis',(0.781388189730918,-0.398672303283029,-0.480096752274001));
#58777=DIRECTION('ref_axis',(-0.523498180784514,8.42991561846578E-17,-0.852026792252042));
#58778=DIRECTION('center_axis',(-0.717050952619425,-0.584827952229777,0.379228424090681));
#58779=DIRECTION('ref_axis',(0.484681441192821,-0.0273514773836963,0.874263002332924));
#58780=DIRECTION('center_axis',(-0.732853934721158,-0.584827952229817,0.347708752628398));
#58781=DIRECTION('ref_axis',(0.452741307384835,-0.0376838387856906,0.890845237334659));
#58782=DIRECTION('center_axis',(-0.717050952628536,-0.584827952229634,0.379228424073675));
#58783=DIRECTION('ref_axis',(0.465944085829832,0.00246180523198907,0.884810741568615));
#58784=DIRECTION('center_axis',(-0.73285393472127,-0.584827952229536,0.347708752628632));
#58785=DIRECTION('ref_axis',(0.433748599251106,-0.00784651556579437,0.900999769612168));
#58786=DIRECTION('center_axis',(-0.794770682400051,-0.584827952229808,0.162221541997498));
#58787=DIRECTION('ref_axis',(0.223194397613665,-0.0330869094539688,0.974212254745678));
#58788=DIRECTION('center_axis',(-0.786970057354105,-0.584827952229501,0.196607210241956));
#58789=DIRECTION('ref_axis',(0.258203898243506,-0.0227607290377056,0.96582229014738));
#58790=DIRECTION('center_axis',(-0.786970057353186,-0.584827952229392,0.196607210245963));
#58791=DIRECTION('ref_axis',(0.237440753049131,0.00704626726436888,0.971376466108327));
#58792=DIRECTION('center_axis',(-0.794770682404231,-0.584827952229529,0.162221541978031));
#58793=DIRECTION('ref_axis',(0.202290445390172,-0.00326197171572208,0.979320139302961));
#58794=DIRECTION('center_axis',(-0.794770682403762,-0.58482795222973,0.162221541979603));
#58795=DIRECTION('ref_axis',(0.181126036956144,0.0265489589848099,0.983101475694846));
#58796=DIRECTION('center_axis',(-0.786970057355164,-0.584827952229715,0.196607210237081));
#58797=DIRECTION('ref_axis',(0.216326923204146,0.0368858773959806,0.97562395129771));
#58798=DIRECTION('center_axis',(-0.7170509526256,-0.58482795222946,0.379228424079493));
#58799=DIRECTION('ref_axis',(0.446569451189646,0.0322834340870415,0.894166374422415));
#58800=DIRECTION('center_axis',(-0.732853934732519,-0.584827952229878,0.34770875260435));
#58801=DIRECTION('ref_axis',(0.41419687010375,0.021958892191509,0.909922392212643));
#58802=DIRECTION('center_axis',(-0.786970057358417,-0.584827952228838,0.196607210226671));
#58803=DIRECTION('ref_axis',(0.278699481110547,-0.0526562713830886,0.95893373927125));
#58804=DIRECTION('center_axis',(0.790515985532476,-0.572651970032463,-0.217150173464257));
#58805=DIRECTION('ref_axis',(0.586650501972613,0.809840224078356,9.70824530985733E-17));
#58806=DIRECTION('center_axis',(0.715054632080185,-0.398672303280797,-0.574244954472788));
#58807=DIRECTION('ref_axis',(-0.626157514223935,-2.26629648864061E-16,-0.779696586744422));
#58808=DIRECTION('center_axis',(-0.663866867041266,-0.584827952229466,0.4661084092096));
#58809=DIRECTION('ref_axis',(0.590433792322176,-0.0273514773905273,0.806622485161807));
#58810=DIRECTION('center_axis',(-0.683495700249331,-0.584827952229789,0.436817918624441));
#58811=DIRECTION('ref_axis',(0.560823821147073,-0.0376838387877329,0.827077124534475));
#58812=DIRECTION('center_axis',(-0.663866867041324,-0.584827952229674,0.466108409209256));
#58813=DIRECTION('ref_axis',(0.573166168880506,0.00246180523643346,0.819435465650481));
#58814=DIRECTION('center_axis',(-0.683495700253782,-0.584827952229443,0.436817918617939));
#58815=DIRECTION('ref_axis',(0.543253576549997,-0.00784651557252715,0.839532002820028));
#58816=DIRECTION('center_axis',(-0.663866867043481,-0.584827952229547,0.466108409206343));
#58817=DIRECTION('ref_axis',(0.555116880732246,0.0322834340855692,0.831145612158149));
#58818=DIRECTION('center_axis',(-0.683495700251026,-0.584827952229332,0.4368179186224));
#58819=DIRECTION('ref_axis',(0.524974319790862,0.0219588922038162,0.850834749298183));
#58820=DIRECTION('center_axis',(-0.768171927774257,-0.584827952229491,0.260553556242555));
#58821=DIRECTION('ref_axis',(0.323436684567506,-0.00326197171076301,0.946244191853529));
#58822=DIRECTION('center_axis',(-0.756123145994201,-0.58482795222951,0.293690405670444));
#58823=DIRECTION('ref_axis',(0.357314215292318,0.0070462672613232,0.93395765517914));
#58824=DIRECTION('center_axis',(-0.768171927771648,-0.584827952229115,0.260553556251089));
#58825=DIRECTION('ref_axis',(0.302913090937847,0.0265489589946694,0.952648315022275));
#58826=DIRECTION('center_axis',(-0.756123145985551,-0.584827952228401,0.293690405694923));
#58827=DIRECTION('ref_axis',(0.336899225382093,0.036885877413158,0.94081791223616));
#58828=DIRECTION('center_axis',(-0.756123145993946,-0.584827952229542,0.293690405671039));
#58829=DIRECTION('ref_axis',(0.396688118786568,-0.0526562713743675,0.916441953152802));
#58830=DIRECTION('center_axis',(-0.768171927778807,-0.584827952229177,0.260553556229844));
#58831=DIRECTION('ref_axis',(0.343535615169486,-0.033086909467639,0.93855662457414));
#58832=DIRECTION('center_axis',(-0.756123145992398,-0.584827952229551,0.293690405675006));
#58833=DIRECTION('ref_axis',(0.377217514059134,-0.0227607290356258,0.925844963425742));
#58834=DIRECTION('center_axis',(0.757066397461466,-0.572651970032553,-0.31451580413797));
#58835=DIRECTION('ref_axis',(0.603266389976478,0.797539756203255,-8.73256628124952E-19));
#58836=DIRECTION('center_axis',(0.637444235727302,-0.398672303282526,-0.659336970701205));
#58837=DIRECTION('ref_axis',(-0.7189419696157,-2.63290852888377E-16,-0.695070100295717));
#58838=DIRECTION('center_axis',(-0.600213204385386,-0.584827952229503,0.545637586290088));
#58839=DIRECTION('ref_axis',(0.686874649850214,-0.0273514773867845,0.726261049539286));
#58840=DIRECTION('center_axis',(-0.623358330286889,-0.584827952229631,0.519038205099431));
#58841=DIRECTION('ref_axis',(0.66006180822835,-0.037683838791864,0.750265511410614));
#58842=DIRECTION('center_axis',(-0.600213204401377,-0.584827952229736,0.545637586272247));
#58843=DIRECTION('ref_axis',(0.671349079039191,0.00246180522602489,0.741137202944407));
#58844=DIRECTION('center_axis',(-0.623358330292484,-0.584827952229444,0.519038205092922));
#58845=DIRECTION('ref_axis',(0.644191120426613,-0.00784651557700974,0.764824314831063));
#58846=DIRECTION('center_axis',(-0.60021320438963,-0.584827952229362,0.54563758628557));
#58847=DIRECTION('ref_axis',(0.654909785459053,0.0322834340879301,0.755017187084815));
#58848=DIRECTION('center_axis',(-0.623358330277944,-0.584827952229089,0.519038205110784));
#58849=DIRECTION('ref_axis',(0.627472610842218,0.0219588922095925,0.778328934124755));
#58850=DIRECTION('center_axis',(-0.713351720932154,-0.58482795222982,0.386141927966661));
#58851=DIRECTION('ref_axis',(0.508420747851833,-0.0526562713708326,0.85949732997788));
#58852=DIRECTION('center_axis',(-0.729458642968396,-0.584827952230075,0.354776485253861));
#58853=DIRECTION('ref_axis',(0.419923024492709,0.0265489589792049,0.907171321348959));
#58854=DIRECTION('center_axis',(-0.713351720928075,-0.584827952228853,0.38614192797566));
#58855=DIRECTION('ref_axis',(0.452158425492064,0.0368858774076047,0.891174612690694));
#58856=DIRECTION('center_axis',(-0.713351720932402,-0.584827952229603,0.386141927966532));
#58857=DIRECTION('ref_axis',(0.490282184337812,-0.0227607290347429,0.871266508557945));
#58858=DIRECTION('center_axis',(-0.729458642960928,-0.584827952229548,0.354776485270086));
#58859=DIRECTION('ref_axis',(0.458459070886996,-0.0330869094602276,0.888099395756918));
#58860=DIRECTION('center_axis',(-0.729458642954225,-0.584827952229394,0.354776485284121));
#58861=DIRECTION('ref_axis',(0.439482134022233,-0.00326197170103793,0.898245408235347));
#58862=DIRECTION('center_axis',(-0.713351720929657,-0.584827952229258,0.386141927972125));
#58863=DIRECTION('ref_axis',(0.471552618924881,0.00704626726875167,0.881809774102478));
#58864=DIRECTION('center_axis',(0.711677420049753,-0.572651970035769,-0.406921332698939));
#58865=DIRECTION('ref_axis',(0.626902064777995,0.779098069036939,-3.10242901956412E-17));
#58866=DIRECTION('center_axis',(0.549780962987417,-0.39867230327996,-0.734030849034344));
#58867=DIRECTION('ref_axis',(-0.800388280671653,2.40386410672042E-16,-0.599481943150479));
#58868=DIRECTION('center_axis',(-0.527093820965332,-0.584827952229272,0.616561732668744));
#58869=DIRECTION('ref_axis',(0.772483083816642,-0.0273514773988447,0.634446043333262));
#58870=DIRECTION('center_axis',(-0.553390227092773,-0.584827952228929,0.593072949012115));
#58871=DIRECTION('ref_axis',(0.748890226283988,-0.037683838805149,0.661621762995463));
#58872=DIRECTION('center_axis',(-0.527093820963167,-0.584827952229652,0.616561732670234));
#58873=DIRECTION('ref_axis',(0.758944413191785,0.00246180522996503,0.651150763802045));
#58874=DIRECTION('center_axis',(-0.553390227069166,-0.584827952229485,0.593072949033594));
#58875=DIRECTION('ref_axis',(0.734969385527659,-0.00784651556621632,0.678054890499703));
#58876=DIRECTION('center_axis',(-0.527093820963804,-0.584827952229951,0.616561732669406));
#58877=DIRECTION('ref_axis',(0.74437437163618,0.0322834340803733,0.666981689954995));
#58878=DIRECTION('center_axis',(-0.553390227069857,-0.584827952229117,0.593072949033312));
#58879=DIRECTION('ref_axis',(0.720075283975828,0.0219588922066651,0.693548406717359));
#58880=DIRECTION('center_axis',(-0.659330313116227,-0.584827952228385,0.47250376135901));
#58881=DIRECTION('ref_axis',(0.612135277983495,-0.0526562713886202,0.788997920486181));
#58882=DIRECTION('center_axis',(-0.659330313105025,-0.584827952229428,0.47250376137335));
#58883=DIRECTION('ref_axis',(0.595614811680486,-0.0227607290416661,0.802947660386598));
#58884=DIRECTION('center_axis',(-0.679241359589837,-0.584827952229611,0.443404377192501));
#58885=DIRECTION('ref_axis',(0.566152353175322,-0.0330869094578101,0.823636308947448));
#58886=DIRECTION('center_axis',(-0.659330313103211,-0.584827952229385,0.472503761375935));
#58887=DIRECTION('ref_axis',(0.57835435604605,0.00704626726010693,0.815755226131134));
#58888=DIRECTION('center_axis',(-0.679241359601283,-0.58482795222964,0.443404377174929));
#58889=DIRECTION('ref_axis',(0.548596687653687,-0.0032619717215567,0.836080757962944));
#58890=DIRECTION('center_axis',(-0.679241359595714,-0.584827952229845,0.443404377183191));
#58891=DIRECTION('ref_axis',(0.530310521127004,0.0265489589845896,0.84738769400956));
#58892=DIRECTION('center_axis',(-0.65933031310547,-0.584827952230006,0.472503761372014));
#58893=DIRECTION('ref_axis',(0.560286817117969,0.0368858773936832,0.827476957149088));
#58894=DIRECTION('center_axis',(0.65506486458811,-0.572651970038989,-0.492909468759352));
#58895=DIRECTION('ref_axis',(0.658159678661854,0.752878368253282,-3.22303153492065E-17));
#58896=DIRECTION('center_axis',(0.453447316037979,-0.398672303276905,-0.797148622389728));
#58897=DIRECTION('ref_axis',(-0.869211990412565,-4.27068266829703E-16,-0.494439597648718));
#58898=DIRECTION('center_axis',(-0.445661853072599,-0.584827952229858,0.677762332242305));
#58899=DIRECTION('ref_axis',(0.845908998121008,-0.0273514773765865,0.532625443987828));
#58900=DIRECTION('center_axis',(-0.474694829399016,-0.584827952229825,0.657754578267995));
#58901=DIRECTION('ref_axis',(0.825908198133754,-0.0376838387877635,0.562543844113215));
#58902=DIRECTION('center_axis',(-0.445661853116207,-0.5848279522299,0.677762332213594));
#58903=DIRECTION('ref_axis',(0.834570740565636,0.0024618052198936,0.550895288150829));
#58904=DIRECTION('center_axis',(-0.47469482939812,-0.584827952229606,0.657754578268837));
#58905=DIRECTION('ref_axis',(0.814156744357949,-0.00784651556705881,0.580592135504711));
#58906=DIRECTION('center_axis',(-0.445661853115868,-0.584827952230675,0.677762332213148));
#58907=DIRECTION('ref_axis',(0.822099729305151,0.0322834340707679,0.568427493143141));
#58908=DIRECTION('center_axis',(-0.474694829418479,-0.584827952230029,0.657754578253768));
#58909=DIRECTION('ref_axis',(0.801321939720788,0.0219588921910951,0.597830206643871));
#58910=DIRECTION('center_axis',(-0.594910872368468,-0.584827952229229,0.55141392821469));
#58911=DIRECTION('ref_axis',(0.706196069142412,-0.0526562713766156,0.706055542441611));
#58912=DIRECTION('center_axis',(-0.594910872346582,-0.584827952229776,0.551413928237722));
#58913=DIRECTION('ref_axis',(0.691554237667827,-0.0227607290218153,0.721965847930541));
#58914=DIRECTION('center_axis',(-0.618312034235857,-0.584827952229107,0.52503951718954));
#58915=DIRECTION('ref_axis',(0.664917074636038,-0.0330869094734788,0.746183985541735));
#58916=DIRECTION('center_axis',(-0.594910872357871,-0.584827952229404,0.551413928225937));
#58917=DIRECTION('ref_axis',(0.676035099498984,0.00704626726817664,0.736835730921746));
#58918=DIRECTION('center_axis',(-0.618312034234228,-0.584827952229657,0.525039517190846));
#58919=DIRECTION('ref_axis',(0.649059543819316,-0.00326197170423922,0.760730614684109));
#58920=DIRECTION('center_axis',(-0.618312034217777,-0.584827952229191,0.525039517210739));
#58921=DIRECTION('ref_axis',(0.632334704053358,0.0265489589935709,0.774240256526428));
#58922=DIRECTION('center_axis',(-0.594910872361907,-0.584827952229308,0.551413928221684));
#58923=DIRECTION('ref_axis',(0.659579150962401,0.0368858774011951,0.750729495666757));
#58924=DIRECTION('center_axis',(0.588121544899005,-0.57265197003845,-0.571124128046338));
#58925=DIRECTION('ref_axis',(0.697621253169909,0.716466738324708,1.05871245547361E-16));
#58926=DIRECTION('center_axis',(0.349962534037925,-0.398672303273708,-0.847694885776829));
#58927=DIRECTION('ref_axis',(2.03396851858332E-16,0.904918591666238,-0.425584706558861));
#58928=DIRECTION('center_axis',(-0.357201531544164,-0.584827952230252,0.728274214944257));
#58929=DIRECTION('ref_axis',(0.905994422190039,-0.0273514773660029,0.422405023225855));
#58930=DIRECTION('center_axis',(-0.388513210696198,-0.58482795222995,0.712063024882668));
#58931=DIRECTION('ref_axis',(0.889901104310132,-0.0376838387861378,0.454594272777328));
#58932=DIRECTION('center_axis',(-0.357201531572555,-0.584827952229513,0.728274214930926));
#58933=DIRECTION('ref_axis',(0.897035388835196,0.0024618052425906,0.441951864677859));
#58934=DIRECTION('center_axis',(-0.388513210688937,-0.584827952229398,0.712063024887083));
#58935=DIRECTION('ref_axis',(0.880504364980544,-0.00784651556111698,0.473973095696115));
#58936=DIRECTION('center_axis',(-0.357201531589311,-0.584827952229665,0.728274214922585));
#58937=DIRECTION('ref_axis',(0.886860083159802,0.0322834340828434,0.460908855178124));
#58938=DIRECTION('center_axis',(-0.38851321069286,-0.5848279522291,0.712063024885188));
#58939=DIRECTION('ref_axis',(0.869931269815895,0.0219588922094773,0.492683867048067));
#58940=DIRECTION('center_axis',(-0.5211093317958,-0.584827952229009,0.621627968005751));
#58941=DIRECTION('ref_axis',(0.789119726415041,-0.0526562713785744,0.611978246727085));
#58942=DIRECTION('center_axis',(-0.521109331771439,-0.584827952229721,0.621627968025504));
#58943=DIRECTION('ref_axis',(0.776587440188631,-0.0227607290239678,0.629598202789341));
#58944=DIRECTION('center_axis',(-0.547631558727778,-0.584827952229038,0.598394470376335));
#58945=DIRECTION('ref_axis',(0.753195656642439,-0.0330869094743024,0.656963894926049));
#58946=DIRECTION('center_axis',(-0.521109331759202,-0.584827952228686,0.621627968036734));
#58947=DIRECTION('ref_axis',(0.763054365594531,0.00704626728573874,0.646295896060361));
#58948=DIRECTION('center_axis',(-0.547631558700224,-0.584827952229441,0.598394470401158));
#58949=DIRECTION('ref_axis',(0.739286343288302,-0.00326197170241592,0.673383295135856));
#58950=DIRECTION('center_axis',(-0.547631558691036,-0.584827952228464,0.59839447041052));
#58951=DIRECTION('ref_axis',(0.724386590960141,0.026548959005902,0.688882587683016));
#58952=DIRECTION('center_axis',(-0.52110933176397,-0.584827952227933,0.621627968033447));
#58953=DIRECTION('ref_axis',(0.748469527589275,0.036885877418764,0.662142581561808));
#58954=DIRECTION('center_axis',(0.511903197111928,-0.572651970045343,-0.640331818661055));
#58955=DIRECTION('ref_axis',(2.78623697967282E-17,0.745401236176701,-0.666616079243702));
#58956=DIRECTION('center_axis',(0.240958633818126,-0.398672303272877,-0.884872494425949));
#58957=DIRECTION('ref_axis',(2.16461393462878E-16,0.91173645657313,-0.41077564893196));
#58958=DIRECTION('center_axis',(-0.263107928487425,-0.584827952230399,0.767300778220024));
#58959=DIRECTION('ref_axis',(0.951791773000886,-0.0273514773604094,0.305523022919768));
#58960=DIRECTION('center_axis',(-0.296204506617227,-0.584827952228624,0.755141812212593));
#58961=DIRECTION('ref_axis',(0.939859738456232,-0.0376838388117045,0.339475478232811));
#58962=DIRECTION('center_axis',(-0.263107928520809,-0.584827952229402,0.767300778209336));
#58963=DIRECTION('ref_axis',(0.945353253144115,0.00246180524621462,0.326038596311492));
#58964=DIRECTION('center_axis',(-0.296204506602731,-0.584827952229629,0.755141812217501));
#58965=DIRECTION('ref_axis',(0.932965905764073,-0.00784651558281844,0.359879217064603));
#58966=DIRECTION('center_axis',(-0.263107928561358,-0.584827952230673,0.767300778194463));
#58967=DIRECTION('ref_axis',(0.937634123704886,0.0322834340717656,0.346121409260833));
#58968=DIRECTION('center_axis',(-0.29620450658635,-0.584827952229493,0.755141812224032));
#58969=DIRECTION('ref_axis',(0.924821264095292,0.0219588922008965,0.379767608585166));
#58970=DIRECTION('center_axis',(-0.439089585745395,-0.584827952229949,0.682038563411529));
#58971=DIRECTION('ref_axis',(0.859598494215755,-0.0526562713668447,0.508249688467931));
#58972=DIRECTION('center_axis',(-0.439089585734235,-0.584827952229727,0.682038563418904));
#58973=DIRECTION('ref_axis',(0.849373394870101,-0.0227607290228192,0.52730141788278));
#58974=DIRECTION('center_axis',(-0.468314606414701,-0.584827952228701,0.662312385291585));
#58975=DIRECTION('ref_axis',(0.829595893198059,-0.0330869094862335,0.557383091248349));
#58976=DIRECTION('center_axis',(-0.439089585749168,-0.584827952229422,0.682038563409552));
#58977=DIRECTION('ref_axis',(0.838039808487152,0.00704626726651889,0.545563588877068));
#58978=DIRECTION('center_axis',(-0.468314606376331,-0.58482795222944,0.662312385318063));
#58979=DIRECTION('ref_axis',(0.817854155460095,-0.00326197170855117,0.575416318796424));
#58980=DIRECTION('center_axis',(-0.468314606377336,-0.584827952229433,0.662312385317358));
#58981=DIRECTION('ref_axis',(0.805014468575665,0.0265489589911354,0.592660828940404));
#58982=DIRECTION('center_axis',(-0.439089585747537,-0.584827952229093,0.682038563410884));
#58983=DIRECTION('ref_axis',(0.825556092624422,0.036885877404233,0.563113283433109));
#58984=DIRECTION('center_axis',(0.427611830115045,-0.57265197004781,-0.699441093978631));
#58985=DIRECTION('ref_axis',(2.4296297475095E-16,0.773750158489481,-0.633490877785547));
#58986=DIRECTION('center_axis',(0.128154672001504,-0.398672303267734,-0.908095135242661));
#58987=DIRECTION('ref_axis',(1.3304126858695E-16,0.915645369915158,-0.401987010428115));
#58988=DIRECTION('center_axis',(-0.16486495623335,-0.584827952230397,0.794226549856007));
#58989=DIRECTION('ref_axis',(0.982578798975358,-0.0273514773601188,0.18382274203798));
#58990=DIRECTION('center_axis',(-0.199224480487903,-0.584827952228576,0.786311562083666));
#58991=DIRECTION('ref_axis',(0.974996223098389,-0.0376838388125904,0.219002952574214));
#58992=DIRECTION('center_axis',(-0.164864956274359,-0.5848279522295,0.794226549848155));
#58993=DIRECTION('ref_axis',(0.97876233192126,0.00246180524259714,0.204983504524156));
#58994=DIRECTION('center_axis',(-0.19922448045893,-0.584827952229542,0.786311562090289));
#58995=DIRECTION('ref_axis',(0.970714016903537,-0.00784651557515089,0.240109828162715));
#58996=DIRECTION('center_axis',(-0.164864956292685,-0.58482795222969,0.794226549844211));
#58997=DIRECTION('ref_axis',(0.973621114013237,0.0322834340827729,0.225875421928651));
#58998=DIRECTION('center_axis',(-0.199224480444615,-0.584827952229133,0.78631156209422));
#58999=DIRECTION('ref_axis',(0.965126274586139,0.0219588922067689,0.260862188054405));
#59000=DIRECTION('center_axis',(-0.350145134677076,-0.584827952228389,0.731693003215366));
#59001=DIRECTION('ref_axis',(0.916520880240436,-0.0526562713881566,0.396505729046623));
#59002=DIRECTION('center_axis',(-0.350145134629644,-0.584827952229829,0.731693003236914));
#59003=DIRECTION('ref_axis',(0.908764223723316,-0.0227607290213395,0.416688774620791));
#59004=DIRECTION('center_axis',(-0.381612052959433,-0.584827952229268,0.715785238271514));
#59005=DIRECTION('ref_axis',(0.892912906963496,-0.0330869094685037,0.449012023224125));
#59006=DIRECTION('center_axis',(-0.350145134628676,-0.584827952228926,0.731693003238098));
#59007=DIRECTION('ref_axis',(0.899808863003385,0.00704626727932487,0.436227417957633));
#59008=DIRECTION('center_axis',(-0.381612052930085,-0.584827952229394,0.715785238287057));
#59009=DIRECTION('ref_axis',(0.883523919049835,-0.00326197169889307,0.468374683354531));
#59010=DIRECTION('center_axis',(-0.381612052925238,-0.584827952228613,0.71578523829028));
#59011=DIRECTION('ref_axis',(0.87294678715174,0.0265489590050242,0.487092454855548));
#59012=DIRECTION('center_axis',(-0.350145134606279,-0.584827952227175,0.731693003250216));
#59013=DIRECTION('ref_axis',(0.889623144943821,0.0368858774309471,0.455203352389253));
#59014=DIRECTION('center_axis',(0.336576769114371,-0.572651970050439,-0.747519765417533));
#59015=DIRECTION('ref_axis',(1.19211448397068E-16,0.793835266537866,-0.608132855222241));
#59016=DIRECTION('center_axis',(0.0133296344508691,-0.398672303267143,-0.916996573304981));
#59017=DIRECTION('ref_axis',(5.21908896690381E-18,0.917078049750596,-0.398707725866508));
#59018=DIRECTION('center_axis',(-0.06402196519388,-0.584827952229365,0.808626894348636));
#59019=DIRECTION('ref_axis',(0.997869970321849,-0.0273514773948857,0.0592234667525383));
#59020=DIRECTION('center_axis',(-0.0991025652750874,-0.584827952228812,
0.805080708902996));
#59021=DIRECTION('ref_axis',(0.994756434869629,-0.0376838388044832,0.095076619515121));
#59022=DIRECTION('center_axis',(-0.0640219651807408,-0.584827952229592,
0.808626894349513));
#59023=DIRECTION('ref_axis',(0.996735744040993,0.00246180523994048,0.080695700418357));
#59024=DIRECTION('center_axis',(-0.0991025652440291,-0.584827952229419,
0.805080708906379));
#59025=DIRECTION('ref_axis',(0.993153388117747,-0.00784651556606208,0.116553763833314));
#59026=DIRECTION('center_axis',(-0.0640219652106609,-0.584827952230345,
0.808626894346599));
#59027=DIRECTION('ref_axis',(0.994253517734721,0.0322834340735004,0.102067244288046));
#59028=DIRECTION('center_axis',(-0.0991025652547514,-0.584827952229472,
0.80508070890502));
#59029=DIRECTION('ref_axis',(0.990210667184292,0.0219588922006542,0.137842815002304));
#59030=DIRECTION('center_axis',(-0.25567868561861,-0.584827952229395,0.769808207290305));
#59031=DIRECTION('ref_axis',(0.95898918450145,-0.0526562713766554,0.278508637377643));
#59032=DIRECTION('center_axis',(-0.255678685641103,-0.584827952229286,0.769808207282917));
#59033=DIRECTION('ref_axis',(0.953823297883429,-0.0227607290544355,0.299504700510177));
#59034=DIRECTION('center_axis',(-0.288891249511358,-0.584827952228646,0.757969730429794));
#59035=DIRECTION('ref_axis',(0.942148150765216,-0.0330869094820139,0.333559767404004));
#59036=DIRECTION('center_axis',(-0.255678685610651,-0.584827952229358,0.769808207292976));
#59037=DIRECTION('ref_axis',(0.947387394214282,0.00704626726439204,0.320011680101699));
#59038=DIRECTION('center_axis',(-0.288891249468051,-0.584827952229451,0.757969730445679));
#59039=DIRECTION('ref_axis',(0.935259982633899,-0.00326197170485859,0.353946499381242));
#59040=DIRECTION('center_axis',(-0.288891249461548,-0.584827952228912,0.757969730448573));
#59041=DIRECTION('ref_axis',(0.9271122134078,0.0265489589997462,0.373842341804832));
#59042=DIRECTION('center_axis',(-0.255678685595091,-0.584827952228579,0.769808207298736));
#59043=DIRECTION('ref_axis',(0.939660308803962,0.0368858774105686,0.34011459260975));
#59044=DIRECTION('center_axis',(0.240233691412443,-0.572651970044448,-0.783809603612104));
#59045=DIRECTION('ref_axis',(1.40955751182557E-16,0.807455881609291,-0.589927961071995));
#59046=DIRECTION('center_axis',(-0.101705619397937,-0.398672303265427,-0.911436427619569));
#59047=DIRECTION('ref_axis',(-2.04923865621488E-17,0.916187281044667,-0.400750378729677));
#59048=DIRECTION('center_axis',(0.0378306905445431,-0.584827952229437,0.810274709678173));
#59049=DIRECTION('ref_axis',(0.997424136147349,-0.0273514773922417,-0.0663097980329947));
#59050=DIRECTION('center_axis',(0.00258225663246541,-0.584827952230405,
0.811153252006472));
#59051=DIRECTION('ref_axis',(0.99882874342139,-0.0376838387736332,-0.030349128661775));
#59052=DIRECTION('center_axis',(0.0378306905688722,-0.584827952229421,0.810274709677048));
#59053=DIRECTION('ref_axis',(0.998990038056263,0.00246180524922385,-0.044864723104699));
#59054=DIRECTION('center_axis',(0.00258225662327451,-0.584827952229373,
0.811153252007245));
#59055=DIRECTION('ref_axis',(0.999930137117185,-0.0078465155589794,-0.00884042297572202));
#59056=DIRECTION('center_axis',(0.0378306905186115,-0.584827952230635,0.810274709678518));
#59057=DIRECTION('ref_axis',(0.999205949546035,0.0322834340709376,-0.02335059477601));
#59058=DIRECTION('center_axis',(0.00258225662696415,-0.584827952228561,
0.811153252007819));
#59059=DIRECTION('ref_axis',(0.999678846039727,0.0219588922164569,0.0126495783845262));
#59060=DIRECTION('center_axis',(-0.157180030979881,-0.584827952228931,0.795783076065883));
#59061=DIRECTION('ref_axis',(0.986333656442174,-0.0526562713819141,0.156119298145892));
#59062=DIRECTION('center_axis',(-0.157180030981607,-0.584827952229301,0.79578307606527));
#59063=DIRECTION('ref_axis',(0.983840008871071,-0.0227607290469234,0.177597258306043));
#59064=DIRECTION('center_axis',(-0.191614458434911,-0.584827952229383,0.788200587166669));
#59065=DIRECTION('ref_axis',(0.976525155431572,-0.0330869094653137,0.2128470747541));
#59066=DIRECTION('center_axis',(-0.157180030964318,-0.584827952229441,0.795783076068582));
#59067=DIRECTION('ref_axis',(0.980025060285253,0.00704626726332402,0.198749166867535));
#59068=DIRECTION('center_axis',(-0.19161445842515,-0.584827952229539,0.788200587168926));
#59069=DIRECTION('ref_axis',(0.972246437596987,-0.00326197170944447,0.233936367674064));
#59070=DIRECTION('center_axis',(-0.191614458432366,-0.584827952229689,0.788200587167061));
#59071=DIRECTION('ref_axis',(0.966656526227481,0.0265489589867337,0.254696511712548));
#59072=DIRECTION('center_axis',(-0.157180030995559,-0.584827952230838,0.795783076061385));
#59073=DIRECTION('ref_axis',(0.974878468272374,0.0368858773811864,0.219662022545385));
#59074=DIRECTION('center_axis',(0.140101984886909,-0.572651970039226,-0.807738296133681));
#59075=DIRECTION('ref_axis',(-2.73695913613894E-16,0.815784312933643,-0.578356252470209));
#59076=DIRECTION('center_axis',(-0.215136914873053,-0.398672303262503,-0.891502385005377));
#59077=DIRECTION('ref_axis',(-1.40757177117324E-16,0.912878440606828,-0.408231493977676));
#59078=DIRECTION('center_axis',(0.139086733702938,-0.584827952229738,0.799144008798552));
#59079=DIRECTION('ref_axis',(0.98124832751129,-0.0273514773842728,-0.190797317699161));
#59080=DIRECTION('center_axis',(0.104226354693529,-0.584827952228692,0.804433423770602));
#59081=DIRECTION('ref_axis',(0.987148926019581,-0.037683838811534,-0.155296252855032));
#59082=DIRECTION('center_axis',(0.13908673371138,-0.58482795222936,0.799144008797359));
#59083=DIRECTION('ref_axis',(0.985489662402947,0.00246180524800965,-0.169717603128984));
#59084=DIRECTION('center_axis',(0.104226354730604,-0.584827952229458,0.804433423765242));
#59085=DIRECTION('ref_axis',(0.990937390525656,-0.00784651556961726,-0.13409519100855));
#59086=DIRECTION('center_axis',(0.139086733689145,-0.584827952229692,0.799144008800986));
#59087=DIRECTION('ref_axis',(0.98840030663301,0.0322834340858216,-0.1484001810356));
#59088=DIRECTION('center_axis',(0.104226354733429,-0.584827952229202,0.804433423765062));
#59089=DIRECTION('ref_axis',(0.993381492313261,0.0219588922051712,-0.112743149603864));
#59090=DIRECTION('center_axis',(-0.0562025533330101,-0.584827952229683,
0.809207970357241));
#59091=DIRECTION('ref_axis',(0.998123057416868,-0.0526562713724056,0.0312678643012303));
#59092=DIRECTION('center_axis',(-0.0562025533235253,-0.58482795222968,0.809207970357902));
#59093=DIRECTION('ref_axis',(0.998340975199547,-0.0227607290307561,0.052889001234716));
#59094=DIRECTION('center_axis',(-0.0913157929052481,-0.584827952229324,
0.806001049786749));
#59095=DIRECTION('ref_axis',(0.995501775041207,-0.0330869094618318,0.0887776566038487));
#59096=DIRECTION('center_axis',(-0.0562025533135293,-0.584827952229175,
0.809207970358962));
#59097=DIRECTION('ref_axis',(0.997207145718442,0.00704626727498444,0.0743522605276269));
#59098=DIRECTION('center_axis',(-0.0913157929007026,-0.584827952229465,
0.806001049787162));
#59099=DIRECTION('ref_axis',(0.993899985449488,-0.00326197170932218,0.110236919696055));
#59100=DIRECTION('center_axis',(-0.0913157928690418,-0.584827952228333,
0.80600104979157));
#59101=DIRECTION('ref_axis',(0.990956088185965,0.0265489590098869,0.131533965433503));
#59102=DIRECTION('center_axis',(-0.0562025532929524,-0.584827952227329,
0.809207970361725));
#59103=DIRECTION('ref_axis',(0.994722211948922,0.0368858774239052,0.095745251068202));
#59104=DIRECTION('center_axis',(0.037760786365144,-0.572651970035092,-0.818928473206308));
#59105=DIRECTION('ref_axis',(3.16831373149503E-17,0.819512943950104,-0.573060672789744));
#59106=DIRECTION('center_axis',(-0.325175372684327,-0.398672303260341,-0.857508817221551));
#59107=DIRECTION('ref_axis',(-3.37422109478849E-16,0.90678944104826,-0.421583810888634));
#59108=DIRECTION('center_axis',(0.238149295968193,-0.584827952229663,0.775410329516388));
#59109=DIRECTION('ref_axis',(0.949597646582202,-0.0273514773858706,-0.312275849675177));
#59110=DIRECTION('center_axis',(0.204226740955095,-0.584827952228983,0.785027199892154));
#59111=DIRECTION('ref_axis',(0.95990118035779,-0.0376838388049021,-0.277794262432916));
#59112=DIRECTION('center_axis',(0.238149295966526,-0.584827952229582,0.775410329516961));
#59113=DIRECTION('ref_axis',(0.956447526073562,0.00246180524043142,-0.291893935159196));
#59114=DIRECTION('center_axis',(0.204226740979238,-0.584827952229625,0.785027199885395));
#59115=DIRECTION('ref_axis',(0.966316969328394,-0.00784651557037047,-0.257235197788701));
#59116=DIRECTION('center_axis',(0.238149295946062,-0.584827952230011,0.775410329522922));
#59117=DIRECTION('ref_axis',(0.962007000446442,0.0322834340790003,-0.271109407760236));
#59118=DIRECTION('center_axis',(0.204226740987369,-0.584827952229167,0.78502719988362));
#59119=DIRECTION('ref_axis',(0.971417919034731,0.0219588922077158,-0.236357850792486));
#59120=DIRECTION('center_axis',(0.0456612721466382,-0.584827952230221,0.809871171555178));
#59121=DIRECTION('ref_axis',(0.994171461523332,-0.052656271367303,-0.0940766824364801));
#59122=DIRECTION('center_axis',(0.0456612721394024,-0.5848279522294,0.809871171556179));
#59123=DIRECTION('ref_axis',(0.997097507965193,-0.0227607290354471,-0.0726533469523378));
#59124=DIRECTION('center_axis',(0.0104229772374144,-0.584827952229693,0.811090394368182));
#59125=DIRECTION('ref_axis',(0.998778736973264,-0.0330869094538148,-0.0366918382325957));
#59126=DIRECTION('center_axis',(0.0456612721423449,-0.584827952229337,0.809871171556059));
#59127=DIRECTION('ref_axis',(0.998662678758543,0.00704626726621081,-0.0512172253487444));
#59128=DIRECTION('center_axis',(0.010422977223353,-0.584827952229428,0.811090394368554));
#59129=DIRECTION('ref_axis',(0.999879136804397,-0.00326197171151358,-0.0152010303548121));
#59130=DIRECTION('center_axis',(0.0104229772140677,-0.584827952229834,0.81109039436838));
#59131=DIRECTION('ref_axis',(0.999627680658168,0.0265489589835582,0.00629705001267351));
#59132=DIRECTION('center_axis',(0.0456612721716982,-0.584827952227699,0.809871171555587));
#59133=DIRECTION('ref_axis',(0.99887859211368,0.0368858774200037,-0.0296814801509117));
#59134=DIRECTION('center_axis',(-0.065175922335569,-0.572651970056052,-0.817203659034045));
#59135=DIRECTION('ref_axis',(-3.98584692492418E-17,0.818944908553334,-0.573872143211858));
#59136=DIRECTION('center_axis',(-0.430085620617851,-0.398672303259856,-0.809991823138505));
#59137=DIRECTION('ref_axis',(-0.883216234749031,-3.21399618696842E-16,0.468965971767402));
#59138=DIRECTION('center_axis',(0.333456101558182,-0.584827952229417,0.73944796613742));
#59139=DIRECTION('ref_axis',(0.902971243510296,-0.0273514773966886,-0.428829604945471));
#59140=DIRECTION('center_axis',(0.301006349518998,-0.584827952229591,0.753240628113082));
#59141=DIRECTION('ref_axis',(0.917515219660035,-0.0376838387937564,-0.395911290551259));
#59142=DIRECTION('center_axis',(0.333456101576296,-0.58482795222948,0.739447966129201));
#59143=DIRECTION('ref_axis',(0.912321640901148,0.00246180524209912,-0.409466925475535));
#59144=DIRECTION('center_axis',(0.301006349521064,-0.584827952229532,0.753240628112302));
#59145=DIRECTION('ref_axis',(0.926457152276119,-0.00784651557254989,-0.376318451832746));
#59146=DIRECTION('center_axis',(0.333456101560606,-0.584827952229806,0.739447966136019));
#59147=DIRECTION('ref_axis',(0.920442269183709,0.0322834340832547,-0.389543077186254));
#59148=DIRECTION('center_axis',(0.301006349541005,-0.584827952228975,0.753240628104766));
#59149=DIRECTION('ref_axis',(0.934134504873787,0.0219588922130655,-0.356245047484144));
#59150=DIRECTION('center_axis',(0.146804992065436,-0.584827952229486,0.797762220586895));
#59151=DIRECTION('ref_axis',(0.974541187793879,-0.0526562713753265,-0.217937583675104));
#59152=DIRECTION('center_axis',(0.146804992111045,-0.584827952229952,0.79776222057816));
#59153=DIRECTION('ref_axis',(0.980129217387624,-0.0227607290121625,-0.197049908495181));
#59154=DIRECTION('center_axis',(0.111997370786089,-0.584827952229844,0.803388358907229));
#59155=DIRECTION('ref_axis',(0.986304361580666,-0.0330869094541399,-0.161582680847079));
#59156=DIRECTION('center_axis',(0.146804992081053,-0.584827952229384,0.797762220584096));
#59157=DIRECTION('ref_axis',(0.984368704782361,0.00704626726995306,-0.175978985002918));
#59158=DIRECTION('center_axis',(0.111997370781047,-0.584827952229584,0.803388358908122));
#59159=DIRECTION('ref_axis',(0.990089596872588,-0.00326197170726883,-0.140399251085102));
#59160=DIRECTION('center_axis',(0.111997370753232,-0.584827952230296,0.80338835891148));
#59161=DIRECTION('ref_axis',(0.992534547463153,0.0265489589767518,-0.119039173675579));
#59162=DIRECTION('center_axis',(0.146804992125695,-0.584827952226961,0.797762220577657));
#59163=DIRECTION('ref_axis',(0.98728206017675,0.0368858774329538,-0.154640116719929));
#59164=DIRECTION('center_axis',(-0.167084767789042,-0.572651970057299,-0.802591054997734));
#59165=DIRECTION('ref_axis',(1.04024676683625E-16,0.814034314690017,-0.580816782218932));
#59166=DIRECTION('center_axis',(-0.528213161393386,-0.398672303260503,-0.749700774138436));
#59167=DIRECTION('ref_axis',(-0.817474789260881,-2.1562309484241E-16,0.57596438164428));
#59168=DIRECTION('center_axis',(0.423504105275545,-0.584827952229947,0.691824066584335));
#59169=DIRECTION('ref_axis',(0.842104444500713,-0.0273514773774933,-0.538620461213101));
#59170=DIRECTION('center_axis',(0.393038908107982,-0.584827952229038,0.709575001676973));
#59171=DIRECTION('ref_axis',(0.86065949586068,-0.0376838388021038,-0.507784561086665));
#59172=DIRECTION('center_axis',(0.423504105240179,-0.584827952229838,0.691824066606078));
#59173=DIRECTION('ref_axis',(0.853807898469918,0.00246180522579648,-0.520582377751507));
#59174=DIRECTION('center_axis',(0.393038908152261,-0.584827952229443,0.709575001652113));
#59175=DIRECTION('ref_axis',(0.871986552479397,-0.00784651555265927,-0.489466939117218));
#59176=DIRECTION('center_axis',(0.423504105258982,-0.584827952229269,0.691824066595048));
#59177=DIRECTION('ref_axis',(0.864361613487515,0.0322834340894379,-0.501833419585277));
#59178=DIRECTION('center_axis',(0.39303890813514,-0.584827952229147,0.70957500166184));
#59179=DIRECTION('ref_axis',(0.88211923155067,0.0219588922095178,-0.470514046954377));
#59180=DIRECTION('center_axis',(0.24563350955146,-0.584827952228278,0.773072082847332));
#59181=DIRECTION('ref_axis',(0.93954181737605,-0.0526562713904792,-0.338361479020532));
#59182=DIRECTION('center_axis',(0.245633509623877,-0.584827952230061,0.773072082822973));
#59183=DIRECTION('ref_axis',(0.947703703551881,-0.0227607290100421,-0.31833887523986));
#59184=DIRECTION('center_axis',(0.211805498867834,-0.584827952229117,0.783016409113402));
#59185=DIRECTION('ref_axis',(0.958275377222213,-0.0330869094709953,-0.283925268039469));
#59186=DIRECTION('center_axis',(0.245633509610189,-0.584827952228881,0.773072082828215));
#59187=DIRECTION('ref_axis',(0.954550648293822,0.00704626728150651,-0.297965450949));
#59188=DIRECTION('center_axis',(0.211805498906855,-0.584827952229244,0.783016409102751));
#59189=DIRECTION('ref_axis',(0.964685752543678,-0.00326197169741844,-0.26338329176294));
#59190=DIRECTION('center_axis',(0.211805498865265,-0.584827952230204,0.783016409113284));
#59191=DIRECTION('ref_axis',(0.969788551542686,0.0265489589781888,-0.242498078495303));
#59192=DIRECTION('center_axis',(0.245633509565711,-0.584827952229986,0.773072082841512));
#59193=DIRECTION('ref_axis',(0.960115500395768,0.0368858773910101,-0.277159986197286));
#59194=DIRECTION('center_axis',(-0.266358586643225,-0.572651970059613,-0.775321110578235));
#59195=DIRECTION('ref_axis',(-2.48492576229079E-16,0.804380141111197,-0.594114962432299));
#59196=DIRECTION('center_axis',(-0.618010465074973,-0.39867230325935,-0.677586496081276));
#59197=DIRECTION('ref_axis',(-0.738841278010305,-1.09179488801154E-16,0.673879489158187));
#59198=DIRECTION('center_axis',(0.506873196223756,-0.584827952229664,0.633289688247623));
#59199=DIRECTION('ref_axis',(0.767957155370104,-0.0273514773849234,-0.639916951018427));
#59200=DIRECTION('center_axis',(0.478873008347111,-0.584827952229356,0.654718953573062));
#59201=DIRECTION('ref_axis',(0.790230657669329,-0.0376838387963876,-0.611649765775372));
#59202=DIRECTION('center_axis',(0.506873196218676,-0.584827952229412,0.633289688251922));
#59203=DIRECTION('ref_axis',(0.781829095418921,0.00246180523862598,-0.623487934984631));
#59204=DIRECTION('center_axis',(0.478873008373498,-0.584827952229322,0.654718953553793));
#59205=DIRECTION('ref_axis',(0.803764203864772,-0.00784651555737207,-0.594896240347203));
#59206=DIRECTION('center_axis',(0.506873196212247,-0.584827952229583,0.633289688256909));
#59207=DIRECTION('ref_axis',(0.794649458809522,0.0322834340848596,-0.606209549163837));
#59208=DIRECTION('center_axis',(0.478873008348126,-0.584827952229779,0.654718953571943));
#59209=DIRECTION('ref_axis',(0.816192411000741,0.0219588921980096,-0.57736275882519));
#59210=DIRECTION('center_axis',(0.340588239909505,-0.584827952229418,0.736190136531651));
#59211=DIRECTION('ref_axis',(0.889725311229054,-0.0526562713735081,-0.453449211757394));
#59212=DIRECTION('center_axis',(0.340588239911442,-0.584827952229579,0.736190136530627));
#59213=DIRECTION('ref_axis',(0.900332336196276,-0.0227607290358304,-0.434607447719333));
#59214=DIRECTION('center_axis',(0.308273327752867,-0.584827952229647,0.750295822783955));
#59215=DIRECTION('ref_axis',(0.915133817709533,-0.033086909459052,-0.401790184184263));
#59216=DIRECTION('center_axis',(0.340588239920696,-0.58482795222925,0.736190136526607));
#59217=DIRECTION('ref_axis',(0.909678757870439,0.00704626726974534,-0.415252823707268));
#59218=DIRECTION('center_axis',(0.308273327749158,-0.584827952229474,0.750295822785613));
#59219=DIRECTION('ref_axis',(0.924068237631228,-0.0032619717112851,-0.382213620560115));
#59220=DIRECTION('center_axis',(0.308273327756663,-0.584827952229327,0.750295822782644));
#59221=DIRECTION('ref_axis',(0.931748410832705,0.0265489589938174,-0.362132643774451));
#59222=DIRECTION('center_axis',(0.340588239932968,-0.584827952228373,0.736190136521626));
#59223=DIRECTION('ref_axis',(0.917807345604216,0.0368858774140981,-0.39530887721165));
#59224=DIRECTION('center_axis',(-0.361431771470631,-0.572651970061988,-0.735823889090131));
#59225=DIRECTION('ref_axis',(1.05608455141898E-18,0.789173129075047,-0.614170800629515));
#59226=DIRECTION('center_axis',(-0.698061374540006,-0.398672303260801,-0.594786274209522));
#59227=DIRECTION('ref_axis',(-0.648555798443099,3.71019517064062E-16,0.76116711457198));
#59228=DIRECTION('center_axis',(0.582248594100823,-0.58482795222998,0.5647679531968));
#59229=DIRECTION('ref_axis',(0.6816987231266,-0.0273514773733327,-0.731121568258699));
#59230=DIRECTION('center_axis',(0.557154995178035,-0.584827952229649,0.589537596459326));
#59231=DIRECTION('ref_axis',(0.707339409944258,-0.0376838387904544,-0.705868888274391));
#59232=DIRECTION('center_axis',(0.582248594074075,-0.584827952229764,0.5647679532246));
#59233=DIRECTION('ref_axis',(0.697520380507347,0.00246180523187029,-0.716560715007379));
#59234=DIRECTION('center_axis',(0.557154995173542,-0.584827952229435,0.589537596463785));
#59235=DIRECTION('ref_axis',(0.722866013622932,-0.00784651557421879,-0.690943672481508));
#59236=DIRECTION('center_axis',(0.582248594082303,-0.584827952229179,0.564767953216724));
#59237=DIRECTION('ref_axis',(0.712405207457628,0.0322834340894324,-0.70102539202988));
#59238=DIRECTION('center_axis',(0.557154995173226,-0.584827952229562,0.589537596463957));
#59239=DIRECTION('ref_axis',(0.737393748550908,0.0219588921987813,-0.675106115104464));
#59240=DIRECTION('center_axis',(0.430171690230978,-0.584827952229147,0.687698031998992));
#59241=DIRECTION('ref_axis',(0.825877305439295,-0.0526562713786458,-0.561385779517817));
#59242=DIRECTION('center_axis',(0.430171690255798,-0.584827952229872,0.687698031982849));
#59243=DIRECTION('ref_axis',(0.838762190047532,-0.0227607290251598,-0.544022001173584));
#59244=DIRECTION('center_axis',(0.39987950204304,-0.584827952228486,0.705742623155245));
#59245=DIRECTION('ref_axis',(0.857560051241502,-0.0330869094880703,-0.513318629055288));
#59246=DIRECTION('center_axis',(0.430171690277,-0.584827952228745,0.687698031970545));
#59247=DIRECTION('ref_axis',(0.850460690000747,0.00704626728869317,-0.525991411413484));
#59248=DIRECTION('center_axis',(0.39987950209059,-0.584827952229427,0.705742623127523));
#59249=DIRECTION('ref_axis',(0.868877614590822,-0.00326197170616806,-0.495016212263348));
#59250=DIRECTION('center_axis',(0.399879502092047,-0.584827952229158,0.705742623126921));
#59251=DIRECTION('ref_axis',(0.879014041089011,0.0265489589953712,-0.476056160914475));
#59252=DIRECTION('center_axis',(0.430171690237065,-0.584827952229516,0.68769803199487));
#59253=DIRECTION('ref_axis',(0.86102482072266,0.0368858773983956,-0.50722351103637));
#59254=DIRECTION('center_axis',(-0.450804961352599,-0.572651970064768,-0.684722285310491));
#59255=DIRECTION('ref_axis',(3.11886164380238E-16,0.767090570529824,-0.641538819249645));
#59256=DIRECTION('center_axis',(-0.767103439127705,-0.398672303259429,-0.502605917486323));
#59257=DIRECTION('ref_axis',(-0.548042206506147,4.1389735132999E-17,0.83645067988966));
#59258=DIRECTION('center_axis',(0.648441583792624,-0.584827952229372,0.487339490191091));
#59259=DIRECTION('ref_axis',(0.584689494827209,-0.0273514773949,-0.810795961585293));
#59260=DIRECTION('center_axis',(0.62665031490309,-0.58482795222999,0.515058879277248));
#59261=DIRECTION('ref_axis',(0.613292997180565,-0.0376838387864848,-0.788956036736898));
#59262=DIRECTION('center_axis',(0.648441583795839,-0.584827952229595,0.487339490186545));
#59263=DIRECTION('ref_axis',(0.602211352506359,0.0024618052356761,-0.798332904512549));
#59264=DIRECTION('center_axis',(0.62665031489973,-0.584827952229372,0.515058879282038));
#59265=DIRECTION('ref_axis',(0.630567794508368,-0.00784651556989916,-0.776094510174028));
#59266=DIRECTION('center_axis',(0.648441583795029,-0.584827952229575,0.487339490187648));
#59267=DIRECTION('ref_axis',(0.618925900421918,0.0322834340860392,-0.784785645683285));
#59268=DIRECTION('center_axis',(0.626650314909146,-0.584827952228887,0.515058879271132));
#59269=DIRECTION('ref_axis',(0.646965946175702,0.0219588922115843,-0.762202644669919));
#59270=DIRECTION('center_axis',(0.512971076023869,-0.584827952228682,0.628360518695216));
#59271=DIRECTION('ref_axis',(0.74900472119103,-0.0526562713861267,-0.660468958178398));
#59272=DIRECTION('center_axis',(0.512971076037276,-0.584827952229498,0.628360518683511));
#59273=DIRECTION('ref_axis',(0.763964263128389,-0.0227607290396375,-0.644857002657397));
#59274=DIRECTION('center_axis',(0.485179337823022,-0.584827952230446,0.650059440697201));
#59275=DIRECTION('ref_axis',(0.786462050426737,-0.0330869094385312,-0.616751732597793));
#59276=DIRECTION('center_axis',(0.512971076019171,-0.584827952229899,0.628360518697919));
#59277=DIRECTION('ref_axis',(0.777830349057598,0.00704626724669506,-0.628434800279889));
#59278=DIRECTION('center_axis',(0.485179337808214,-0.584827952229516,0.65005944070909));
#59279=DIRECTION('ref_axis',(0.799984272523417,-0.00326197169936234,-0.600012102591116));
#59280=DIRECTION('center_axis',(0.48517933779427,-0.584827952229414,0.650059440719588));
#59281=DIRECTION('ref_axis',(0.812417094824369,0.0265489589910001,-0.582471988007686));
#59282=DIRECTION('center_axis',(0.512971076053233,-0.584827952228724,0.628360518671205));
#59283=DIRECTION('ref_axis',(0.790663420048422,0.0368858774084628,-0.611138927123072));
#59284=DIRECTION('center_axis',(-0.533068687695661,-0.572651970068508,-0.622822202056961));
#59285=DIRECTION('ref_axis',(3.61729072720274E-16,0.736133834918718,-0.676836004574122));
#59286=DIRECTION('center_axis',(-0.824047824234184,-0.398672303260603,-0.402499165201362));
#59287=DIRECTION('ref_axis',(-0.438885661587862,2.2735551145057E-16,0.898542918314192));
#59288=DIRECTION('center_axis',(0.704408262379738,-0.584827952229673,0.402225392264096));
#59289=DIRECTION('ref_axis',(0.478459363886856,-0.027351477387215,-0.877683618278091));
#59290=DIRECTION('center_axis',(0.68626298482074,-0.584827952230173,0.432457375882516));
#59291=DIRECTION('ref_axis',(0.509574587483431,-0.0376838387798185,-0.859600877201686));
#59292=DIRECTION('center_axis',(0.704408262376566,-0.584827952229622,0.402225392269725));
#59293=DIRECTION('ref_axis',(0.49740509173617,0.00246180523631316,-0.867514907209041));
#59294=DIRECTION('center_axis',(0.686262984799087,-0.584827952229561,0.432457375917704));
#59295=DIRECTION('ref_axis',(0.528325144612044,-0.00784651558329287,-0.849005873809989));
#59296=DIRECTION('center_axis',(0.704408262374531,-0.584827952229628,0.402225392273281));
#59297=DIRECTION('ref_axis',(0.515685762206007,0.0322834340851825,-0.856169360898694));
#59298=DIRECTION('center_axis',(0.686262984814354,-0.584827952229256,0.43245737589389));
#59299=DIRECTION('ref_axis',(0.546335104369736,0.0219588922059708,-0.837278783193744));
#59300=DIRECTION('center_axis',(0.587680601530481,-0.584827952229076,0.559113384633491));
#59301=DIRECTION('ref_axis',(0.660319885045023,-0.05265627138097,-0.749136146837396));
#59302=DIRECTION('center_axis',(0.587680601544024,-0.584827952229498,0.559113384618814));
#59303=DIRECTION('ref_axis',(0.677118163392339,-0.0227607290334116,-0.735522224013696));
#59304=DIRECTION('center_axis',(0.56282760551461,-0.584827952229546,0.584124432601211));
#59305=DIRECTION('ref_axis',(0.702961073322399,-0.0330869094577009,-0.710458292805397));
#59306=DIRECTION('center_axis',(0.587680601535344,-0.584827952229505,0.55911338462793));
#59307=DIRECTION('ref_axis',(0.692933158812551,0.00704626725934919,-0.720967396999178));
#59308=DIRECTION('center_axis',(0.562827605520547,-0.584827952229568,0.584124432595469));
#59309=DIRECTION('ref_axis',(0.718474700600097,-0.00326197170431984,-0.695545443618316));
#59310=DIRECTION('center_axis',(0.562827605513519,-0.584827952229463,0.584124432602346));
#59311=DIRECTION('ref_axis',(0.733007845657271,0.0265489589905533,-0.679701883903086));
#59312=DIRECTION('center_axis',(0.58768060156272,-0.584827952227991,0.559113384600739));
#59313=DIRECTION('ref_axis',(0.707832784918237,0.0368858774180847,-0.705416317249602));
#59314=DIRECTION('center_axis',(-0.606925602392853,-0.572651970070417,-0.551099840622861));
#59315=DIRECTION('ref_axis',(0.686271561910537,-0.7273454085322,-1.7200576857839E-16));
#59316=DIRECTION('center_axis',(-0.867996482891093,-0.398672303259356,-0.296044760640299));
#59317=DIRECTION('ref_axis',(0.417381833030164,-0.908731206384143,-2.70851097314861E-16));
#59318=DIRECTION('center_axis',(0.749266001871889,-0.584827952229832,0.310767959625145));
#59319=DIRECTION('ref_axis',(0.364683642961482,-0.0273514773819596,-0.930729680004547));
#59320=DIRECTION('center_axis',(0.73505287750409,-0.5848279522301,0.343035761347566));
#59321=DIRECTION('ref_axis',(0.397819882148946,-0.0376838387832597,-0.916689298323896));
#59322=DIRECTION('center_axis',(0.749266001868941,-0.584827952229526,0.310767959632829));
#59323=DIRECTION('ref_axis',(0.384754455528877,0.00246180524083023,-0.923015681592482));
#59324=DIRECTION('center_axis',(0.735052877494717,-0.584827952229498,0.343035761368678));
#59325=DIRECTION('ref_axis',(0.417750491554942,-0.00784651557676579,-0.908527907661018));
#59326=DIRECTION('center_axis',(0.749266001867358,-0.584827952229307,0.310767959637058));
#59327=DIRECTION('ref_axis',(0.404312951457465,0.0322834340889155,-0.914050773845294));
#59328=DIRECTION('center_axis',(0.735052877499929,-0.584827952229289,0.343035761357865));
#59329=DIRECTION('ref_axis',(0.437088231600138,0.0219588922034376,-0.899150535144067));
#59330=DIRECTION('center_axis',(0.65312205288754,-0.584827952229456,0.481048698494307));
#59331=DIRECTION('ref_axis',(0.561221409852641,-0.0526562713746137,-0.825989010948655));
#59332=DIRECTION('center_axis',(0.653122052890733,-0.584827952229576,0.481048698489826));
#59333=DIRECTION('ref_axis',(0.579593505736634,-0.0227607290348539,-0.814587820509072));
#59334=DIRECTION('center_axis',(0.631599745689671,-0.584827952230062,0.508977433227776));
#59335=DIRECTION('ref_axis',(0.608373980132682,-0.0330869094484406,-0.792960501362249));
#59336=DIRECTION('center_axis',(0.65312205289568,-0.584827952229212,0.481048698483552));
#59337=DIRECTION('ref_axis',(0.597107998714186,0.00704626726938554,-0.802129907177826));
#59338=DIRECTION('center_axis',(0.631599745685247,-0.584827952229501,0.508977433233911));
#59339=DIRECTION('ref_axis',(0.625634353446796,-0.00326197170274169,-0.780109617507578));
#59340=DIRECTION('center_axis',(0.631599745674331,-0.584827952229705,0.508977433247222));
#59341=DIRECTION('ref_axis',(0.642038624889269,0.0265489589877621,-0.766212475053077));
#59342=DIRECTION('center_axis',(0.653122052899692,-0.584827952228688,0.481048698478743));
#59343=DIRECTION('ref_axis',(0.61383920394949,0.0368858774095715,-0.788568870639961));
#59344=DIRECTION('center_axis',(-0.671210937779911,-0.572651970073183,-0.470686305490095));
#59345=DIRECTION('ref_axis',(0.649044045255814,-0.760750831296272,-1.68693210803163E-16));
#59346=DIRECTION('center_axis',(-0.898256318494365,-0.398672303264004,-0.184921553354722));
#59347=DIRECTION('ref_axis',(0.405668756710548,-0.914020163797779,-1.89095079954371E-16));
#59348=DIRECTION('center_axis',(0.782307368915401,-0.584827952229458,0.21440953064582));
#59349=DIRECTION('ref_axis',(0.245156643157,-0.0273514773929348,-0.96909757867844));
#59350=DIRECTION('center_axis',(0.772250547205598,-0.584827952229256,0.248204267956837));
#59351=DIRECTION('ref_axis',(0.279791319643253,-0.037683838798696,-0.95932098160401));
#59352=DIRECTION('center_axis',(0.782307368913366,-0.584827952229746,0.214409530652459));
#59353=DIRECTION('ref_axis',(0.266036011735809,0.00246180523015953,-0.9639599472876));
#59354=DIRECTION('center_axis',(0.772250547211137,-0.584827952229511,0.248204267939002));
#59355=DIRECTION('ref_axis',(0.300587663690744,-0.00784651556811171,-0.953721913678395));
#59356=DIRECTION('center_axis',(0.782307368912528,-0.584827952230018,0.214409530654777));
#59357=DIRECTION('ref_axis',(0.2865638839574,0.0322834340798274,-0.957517060054422));
#59358=DIRECTION('center_axis',(0.77225054720522,-0.584827952229822,0.248204267956682));
#59359=DIRECTION('ref_axis',(0.320948216323777,0.0219588921948035,-0.94684214602655));
#59360=DIRECTION('center_axis',(0.708263379303267,-0.584827952229123,0.395397587030329));
#59361=DIRECTION('ref_axis',(0.45327213778181,-0.052656271378629,-0.889815534925755));
#59362=DIRECTION('center_axis',(0.708263379307223,-0.584827952229426,0.395397587022796));
#59363=DIRECTION('ref_axis',(0.472928312264079,-0.0227607290376266,-0.880806880464001));
#59364=DIRECTION('center_axis',(0.690411180536856,-0.584827952228857,0.425803555740798));
#59365=DIRECTION('ref_axis',(0.504192465897799,-0.0330869094779533,-0.862957249087749));
#59366=DIRECTION('center_axis',(0.70826337931017,-0.584827952229283,0.395397587017728));
#59367=DIRECTION('ref_axis',(0.491866088796126,0.00704626726564717,-0.870642349538559));
#59368=DIRECTION('center_axis',(0.690411180559335,-0.584827952229379,0.425803555703633));
#59369=DIRECTION('ref_axis',(0.522927378805018,-0.00326197170296729,-0.852370996712536));
#59370=DIRECTION('center_axis',(0.690411180556875,-0.584827952229177,0.4258035557079));
#59371=DIRECTION('ref_axis',(0.540944071460083,0.0265489589947329,-0.840639437766563));
#59372=DIRECTION('center_axis',(0.708263379302448,-0.584827952229935,0.395397587030597));
#59373=DIRECTION('ref_axis',(0.510165012055972,0.036885877393939,-0.859285221869205));
#59374=DIRECTION('center_axis',(-0.724910875715219,-0.572651970076974,-0.382849766144314));
#59375=DIRECTION('ref_axis',(0.619880264826496,-0.784696410899548,-6.375267076676E-18));
#59376=DIRECTION('center_axis',(-0.914350115364004,-0.398672303265294,-0.070882022706601));
#59377=DIRECTION('ref_axis',(0.399677609928807,-0.916655774062214,1.06579819070638E-17));
#59378=DIRECTION('center_axis',(0.803011281433564,-0.584827952229893,0.114669735244374));
#59379=DIRECTION('ref_axis',(0.121763376606092,-0.0273514773793618,-0.992182229634581));
#59380=DIRECTION('center_axis',(0.79726936447069,-0.584827952229677,0.149458444951582));
#59381=DIRECTION('ref_axis',(0.157350280855911,-0.0376838387905617,-0.986823599945083));
#59382=DIRECTION('center_axis',(0.803011281429913,-0.584827952229658,0.114669735271145));
#59383=DIRECTION('ref_axis',(0.143122021098843,0.00246180523247351,-0.989701988778228));
#59384=DIRECTION('center_axis',(0.797269364468822,-0.584827952229543,0.149458444962072));
#59385=DIRECTION('ref_axis',(0.178684388830733,-0.00784651557677228,-0.983875155383797));
#59386=DIRECTION('center_axis',(0.803011281429729,-0.584827952229772,0.114669735271848));
#59387=DIRECTION('ref_axis',(0.164295532805841,0.0322834340834813,-0.985882730239161));
#59388=DIRECTION('center_axis',(0.797269364472123,-0.584827952229213,0.149458444945752));
#59389=DIRECTION('ref_axis',(0.199746655922415,0.021958892206408,-0.979601490658768));
#59390=DIRECTION('center_axis',(0.752234969135609,-0.584827952229195,0.303510819413338));
#59391=DIRECTION('ref_axis',(0.338174493321089,-0.0526562713785287,-0.939609136370829));
#59392=DIRECTION('center_axis',(0.752234969141854,-0.584827952229689,0.303510819396908));
#59393=DIRECTION('ref_axis',(0.358804756783703,-0.0227607290319074,-0.933135089750312));
#59394=DIRECTION('center_axis',(0.738334418684743,-0.584827952229868,0.335914501735312));
#59395=DIRECTION('ref_axis',(0.392059535219292,-0.0330869094523403,-0.919344645531003));
#59396=DIRECTION('center_axis',(0.752234969145643,-0.584827952229108,0.303510819388636));
#59397=DIRECTION('ref_axis',(0.378867156817279,0.00704626727295211,-0.925424241957552));
#59398=DIRECTION('center_axis',(0.738334418680268,-0.584827952229459,0.335914501745859));
#59399=DIRECTION('ref_axis',(0.411973527025067,-0.00326197170852844,-0.911189976114256));
#59400=DIRECTION('center_axis',(0.73833441867766,-0.584827952229559,0.335914501751417));
#59401=DIRECTION('ref_axis',(0.43131850689555,0.0265489589884161,-0.901809014362811));
#59402=DIRECTION('center_axis',(0.752234969147248,-0.584827952228465,0.303510819385897));
#59403=DIRECTION('ref_axis',(0.398445213122471,0.0368858774114973,-0.916450131860634));
#59404=DIRECTION('center_axis',(-0.767178536098743,-0.572651970080584,-0.288975457283513));
#59405=DIRECTION('ref_axis',(0.598172081278793,-0.801367681640954,1.80237087757503E-16));
#59406=DIRECTION('center_axis',(-0.916024064707328,-0.398672303268271,0.0442753597821266));
#59407=DIRECTION('ref_axis',(0.399063638865775,-0.916923231320488,-3.58065846580494E-17));
#59408=DIRECTION('center_axis',(0.811051226341725,-0.584827952229574,0.0131215296572828));
#59409=DIRECTION('ref_axis',(-0.00355017109927834,-0.0273514773886332,-0.999619574122989));
#59410=DIRECTION('center_axis',(0.809714767587711,-0.584827952229316,0.0483555730153735));
#59411=DIRECTION('ref_axis',(0.0324277341660284,-0.0376838387987105,-0.998763420610832));
#59412=DIRECTION('center_axis',(0.811051226341597,-0.584827952229581,0.0131215296648961));
#59413=DIRECTION('ref_axis',(0.0179509106930064,0.00246180523465447,-0.99983583868567));
#59414=DIRECTION('center_axis',(0.809714767588841,-0.584827952229489,0.0483555729943428));
#59415=DIRECTION('ref_axis',(0.0539631543924302,-0.00784651556639407,-0.998512098154792));
#59416=DIRECTION('center_axis',(0.811051226341607,-0.584827952229582,0.0131215296642423));
#59417=DIRECTION('ref_axis',(0.0394361429572599,0.0322834340863139,-0.998700440829105));
#59418=DIRECTION('center_axis',(0.809714767588954,-0.584827952229199,0.0483555729959739));
#59419=DIRECTION('ref_axis',(0.0753949714509705,0.0219588922059928,-0.996911934592516));
#59420=DIRECTION('center_axis',(0.784343364141097,-0.584827952229295,0.206837504865814));
#59421=DIRECTION('ref_axis',(0.217743635085388,-0.0526562713782781,-0.974584540439842));
#59422=DIRECTION('center_axis',(0.784343364146169,-0.5848279522297,0.206837504845436));
#59423=DIRECTION('ref_axis',(0.239022635952717,-0.0227607290302773,-0.97074720124048));
#59424=DIRECTION('center_axis',(0.774613681968537,-0.584827952229984,0.240727875406297));
#59425=DIRECTION('ref_axis',(0.273743591493593,-0.033086909449576,-0.961233427705916));
#59426=DIRECTION('center_axis',(0.784343364145265,-0.584827952229309,0.206837504849971));
#59427=DIRECTION('ref_axis',(0.25989326346829,0.00704626726723805,-0.96561164125201));
#59428=DIRECTION('center_axis',(0.774613681964187,-0.584827952229543,0.240727875421367));
#59429=DIRECTION('ref_axis',(0.294522606615922,-0.00326197170818176,-0.955638945278361));
#59430=DIRECTION('center_axis',(0.77461368196608,-0.584827952229136,0.240727875416265));
#59431=DIRECTION('ref_axis',(0.314890791803105,0.0265489589951922,-0.948756524095558));
#59432=DIRECTION('center_axis',(0.784343364146824,-0.584827952228856,0.206837504845337));
#59433=DIRECTION('ref_axis',(0.280441695187659,0.0368858774073383,-0.959162075797497));
#59434=DIRECTION('center_axis',(-0.797347332677702,-0.572651970082362,-0.190543832837863));
#59435=DIRECTION('ref_axis',(0.583339514953269,-0.812228422485993,1.43682251946218E-17));
#59436=DIRECTION('center_axis',(-0.903251767344807,-0.398672303269224,0.158734493398553));
#59437=DIRECTION('ref_axis',(0.403791856799519,-0.914850882047122,-3.65899417434021E-17));
#59438=DIRECTION('center_axis',(0.806300408914237,-0.584827952229579,-0.0886336103049619));
#59439=DIRECTION('ref_axis',(-0.128807730497183,-0.0273514773898677,-0.991292320785729));
#59440=DIRECTION('center_axis',(0.809390485122122,-0.584827952229272,-0.0535098952072579));
#59441=DIRECTION('ref_axis',(-0.0930062172741409,-0.0376838387986781,-0.994952145503366));
#59442=DIRECTION('center_axis',(0.806300408914354,-0.584827952229474,-0.0886336103045866));
#59443=DIRECTION('ref_axis',(-0.107503296299766,0.0024618052375083,-0.994201680143248));
#59444=DIRECTION('center_axis',(0.809390485121829,-0.584827952229487,-0.0535098952093429));
#59445=DIRECTION('ref_axis',(-0.0716091111974473,-0.00784651557791117,-0.997401908654078));
#59446=DIRECTION('center_axis',(0.806300408914507,-0.584827952229418,-0.0886336103035621));
#59447=DIRECTION('ref_axis',(-0.0860451784234849,0.0322834340877071,-0.995768048871611));
#59448=DIRECTION('center_axis',(0.809390485121477,-0.584827952229612,-0.0535098952133025));
#59449=DIRECTION('ref_axis',(-0.0501457367486247,0.0219588921980094,-0.998500481792259));
#59450=DIRECTION('center_axis',(0.804082195749088,-0.584827952228849,0.106902239317689));
#59451=DIRECTION('ref_axis',(0.0938788296586372,-0.0526562713838044,-0.994190164116443));
#59452=DIRECTION('center_axis',(0.804082195752539,-0.584827952229685,0.106902239287161));
#59453=DIRECTION('ref_axis',(0.115470985370648,-0.022760729030197,-0.993050049469585));
#59454=DIRECTION('center_axis',(0.798676824751148,-0.584827952229572,0.141744826700622));
#59455=DIRECTION('ref_axis',(0.15111054782177,-0.0330869094600406,-0.987962984508725));
#59456=DIRECTION('center_axis',(0.80408219575091,-0.584827952229495,0.106902239300454));
#59457=DIRECTION('ref_axis',(0.136820698101175,0.00704626726231543,-0.99057076813763));
#59458=DIRECTION('center_axis',(0.798676824749585,-0.584827952229556,0.141744826709496));
#59459=DIRECTION('ref_axis',(0.172426888770446,-0.00326197171537725,-0.985016917402677));
#59460=DIRECTION('center_axis',(0.798676824752703,-0.584827952229169,0.141744826693526));
#59461=DIRECTION('ref_axis',(0.193497060827057,0.0265489589948573,-0.980741576679392));
#59462=DIRECTION('center_axis',(0.804082195751867,-0.584827952229202,0.106902239294854));
#59463=DIRECTION('ref_axis',(0.15801544419156,0.0368858774025659,-0.986747460825305));
#59464=DIRECTION('center_axis',(-0.814941485506432,-0.572651970086207,-0.089107218321276));
#59465=DIRECTION('ref_axis',(0.574939054799503,-0.818196237626558,-1.3031285787327E-18));
#59466=DIRECTION('center_axis',(-0.876234650033272,-0.398672303273934,0.270690289229825));
#59467=DIRECTION('ref_axis',(0.41413335584115,-0.910216218038191,-5.40282558576922E-17));
#59468=DIRECTION('center_axis',(0.788833752374882,-0.584827952229736,-0.188990945298809));
#59469=DIRECTION('ref_axis',(-0.252033915049667,-0.0273514773827825,-0.967331795378254));
#59470=DIRECTION('center_axis',(0.79630163119712,-0.584827952229675,-0.154531480429235));
#59471=DIRECTION('ref_axis',(-0.216973405118666,-0.0376838387916993,-0.975449880703838));
#59472=DIRECTION('center_axis',(0.788833752376995,-0.584827952229461,-0.188990945290837));
#59473=DIRECTION('ref_axis',(-0.231262112088917,0.00246180523997023,-0.972888367196943));
#59474=DIRECTION('center_axis',(0.796301631196168,-0.584827952229549,-0.154531480434615));
#59475=DIRECTION('ref_axis',(-0.196052058353707,-0.00784651556825947,-0.9805620952335));
#59476=DIRECTION('center_axis',(0.788833752376159,-0.584827952229035,-0.188990945295645));
#59477=DIRECTION('ref_axis',(-0.210169515943608,0.0322834340937078,-0.977131799938548));
#59478=DIRECTION('center_axis',(0.796301631197679,-0.584827952229497,-0.154531480427026));
#59479=DIRECTION('ref_axis',(-0.174895616738131,0.0219588922000665,-0.984342079918935));
#59480=DIRECTION('center_axis',(0.811140170796625,-0.584827952229234,0.00528106157723248));
#59481=DIRECTION('ref_axis',(-0.0314665010067795,-0.0526562713785295,-0.998116815006591));
#59482=DIRECTION('center_axis',(0.811140170796457,-0.584827952229611,0.00528106156134455));
#59483=DIRECTION('ref_axis',(-0.00990171162426306,-0.0227607290333322,-0.999691905199187));
#59484=DIRECTION('center_axis',(0.810144356906057,-0.58482795222952,0.0405263773892647));
#59485=DIRECTION('ref_axis',(0.0260944005297899,-0.033086909462181,-0.999111774869675));
#59486=DIRECTION('center_axis',(0.811140170796392,-0.584827952229608,0.00528106157163474));
#59487=DIRECTION('ref_axis',(0.0115903885878127,0.00704626726036128,-0.999908002273249));
#59488=DIRECTION('center_axis',(0.810144356906541,-0.584827952229447,0.0405263773806528));
#59489=DIRECTION('ref_axis',(0.0476118958662175,-0.00326197170636763,-0.998860584322262));
#59490=DIRECTION('center_axis',(0.810144356906329,-0.584827952229399,0.0405263773855901));
#59491=DIRECTION('ref_axis',(0.0690517656170743,0.0265489589909614,-0.997259748732325));
#59492=DIRECTION('center_axis',(0.811140170795799,-0.584827952230299,0.00528106158617268));
#59493=DIRECTION('ref_axis',(0.0330971952593657,0.0368858773885729,-0.998771248943039));
#59494=DIRECTION('center_axis',(-0.819683524284951,-0.572651970090649,0.0137346702581644));
#59495=DIRECTION('ref_axis',(0.572705990601629,-0.819760848253323,6.03749681350753E-18));
#59496=DIRECTION('center_axis',(-0.835398788855164,-0.39867230327499,0.378377137497418));
#59497=DIRECTION('ref_axis',(0.430693725898546,-0.902498152059952,2.31475229891537E-16));
#59498=DIRECTION('center_axis',(0.758926716336079,-0.584827952229742,-0.286367780174555));
#59499=DIRECTION('ref_axis',(-0.371285374193801,-0.0273514773838731,-0.928115869703071));
#59500=DIRECTION('center_axis',(0.770654624860523,-0.584827952229746,-0.25311601188358));
#59501=DIRECTION('ref_axis',(-0.337518792743693,-0.0376838387894886,-0.94056418857988));
#59502=DIRECTION('center_axis',(0.758926716343912,-0.584827952229653,-0.286367780153981));
#59503=DIRECTION('ref_axis',(-0.351373786207065,0.00246180523036329,-0.936232023529167));
#59504=DIRECTION('center_axis',(0.770654624862685,-0.584827952229546,-0.253116011877459));
#59505=DIRECTION('ref_axis',(-0.317403147415658,-0.00784651557350236,-0.948258231814514));
#59506=DIRECTION('center_axis',(0.758926716336075,-0.584827952228924,-0.286367780176238));
#59507=DIRECTION('ref_axis',(-0.330979354643143,0.0322834340956424,-0.943085598810098));
#59508=DIRECTION('center_axis',(0.7706546248633,-0.584827952229544,-0.25311601187559));
#59509=DIRECTION('ref_axis',(-0.296887288368979,0.0219588921985787,-0.9546600154287));
#59510=DIRECTION('center_axis',(0.805405980797642,-0.584827952229345,-0.0964234016544657));
#59511=DIRECTION('ref_axis',(-0.156315586151049,-0.0526562713767823,-0.986302567476608));
#59512=DIRECTION('center_axis',(0.805405980796604,-0.584827952229569,-0.0964234016617822));
#59513=DIRECTION('ref_axis',(-0.135118252713833,-0.0227607290362419,-0.990568022397907));
#59514=DIRECTION('center_axis',(0.808835428597436,-0.584827952229255,-0.0613311970936381));
#59515=DIRECTION('ref_axis',(-0.0993332710383858,-0.0330869094686513,-0.994503975701771));
#59516=DIRECTION('center_axis',(0.805405980795944,-0.584827952229344,-0.0964234016686599));
#59517=DIRECTION('ref_axis',(-0.113822708290088,0.00704626726769293,-0.993476089896029));
#59518=DIRECTION('center_axis',(0.808835428596014,-0.584827952229492,-0.0613311971101359));
#59519=DIRECTION('ref_axis',(-0.077953965063628,-0.003261971709741,-0.996951623134956));
#59520=DIRECTION('center_axis',(0.808835428596344,-0.584827952229524,-0.0613311971054644));
#59521=DIRECTION('ref_axis',(-0.0564825171882718,0.0265489589885428,-0.998050538814895));
#59522=DIRECTION('center_axis',(0.805405980796467,-0.584827952229193,-0.0964234016652054));
#59523=DIRECTION('ref_axis',(-0.0923430162513425,0.0368858774021895,-0.995043817828077));
#59524=DIRECTION('center_axis',(-0.811498664230888,-0.572651970093207,0.116359954880761));
#59525=DIRECTION('ref_axis',(0.576568537458026,-0.817048787780456,6.33336117189426E-17));
#59526=DIRECTION('center_axis',(-0.781388189732742,-0.398672303278799,0.480096752274545));
#59527=DIRECTION('ref_axis',(0.523498180784058,-3.57703746127638E-16,0.852026792252322));
#59528=DIRECTION('center_axis',(0.717050952625024,-0.584827952229473,-0.379228424080563));
#59529=DIRECTION('ref_axis',(-0.484681441184531,-0.0273514773904689,-0.874263002337308));
#59530=DIRECTION('center_axis',(0.732853934726112,-0.584827952229606,-0.347708752618311));
#59531=DIRECTION('ref_axis',(-0.452741307376777,-0.0376838387925448,-0.890845237338464));
#59532=DIRECTION('center_axis',(0.717050952631686,-0.584827952229711,-0.379228424067599));
#59533=DIRECTION('ref_axis',(-0.465944085825003,0.00246180522786322,-0.884810741571169));
#59534=DIRECTION('center_axis',(0.732853934727818,-0.584827952229481,-0.347708752614925));
#59535=DIRECTION('ref_axis',(-0.433748599240115,-0.00784651557489748,-0.900999769617379));
#59536=DIRECTION('center_axis',(0.717050952622112,-0.584827952229132,-0.379228424086595));
#59537=DIRECTION('ref_axis',(-0.44656945119513,0.0322834340919662,-0.894166374419498));
#59538=DIRECTION('center_axis',(0.732853934728052,-0.58482795222954,-0.347708752614334));
#59539=DIRECTION('ref_axis',(-0.414196870111794,0.0219588921978709,-0.909922392208828));
#59540=DIRECTION('center_axis',(0.786970057351451,-0.584827952229999,-0.196607210251102));
#59541=DIRECTION('ref_axis',(-0.278699481130594,-0.0526562713682668,-0.958933739266238));
#59542=DIRECTION('center_axis',(0.786970057355849,-0.584827952229471,-0.196607210235065));
#59543=DIRECTION('ref_axis',(-0.258203898238116,-0.022760729042155,-0.965822290148716));
#59544=DIRECTION('center_axis',(0.794770682406187,-0.584827952229128,-0.162221541969888));
#59545=DIRECTION('ref_axis',(-0.223194397591495,-0.0330869094709643,-0.97421225475018));
#59546=DIRECTION('center_axis',(0.786970057353973,-0.584827952229482,-0.196607210242542));
#59547=DIRECTION('ref_axis',(-0.237440753046596,0.00704626726199184,-0.971376466108963));
#59548=DIRECTION('center_axis',(0.794770682402583,-0.584827952229557,-0.162221541986002));
#59549=DIRECTION('ref_axis',(-0.202290445396925,-0.00326197171136405,-0.979320139301581));
#59550=DIRECTION('center_axis',(0.794770682401897,-0.584827952229347,-0.162221541990116));
#59551=DIRECTION('ref_axis',(-0.181126036964189,0.0265489589916822,-0.983101475693179));
#59552=DIRECTION('center_axis',(0.786970057353212,-0.584827952229266,-0.196607210246233));
#59553=DIRECTION('ref_axis',(-0.216326923211641,0.0368858774012871,-0.975623951295848));
#59554=DIRECTION('center_axis',(-0.790515985477339,-0.572651970093842,0.217150173503114));
#59555=DIRECTION('ref_axis',(0.586650502040687,-0.809840224029042,2.50717685812128E-16));
#59556=DIRECTION('center_axis',(-0.715054632079823,-0.398672303282021,0.57424495447239));
#59557=DIRECTION('ref_axis',(0.626157514223864,1.11353316466764E-16,0.77969658674448));
#59558=DIRECTION('center_axis',(0.663866867044535,-0.584827952229405,-0.46610840920502));
#59559=DIRECTION('ref_axis',(-0.590433792318414,-0.0273514773937692,-0.806622485164451));
#59560=DIRECTION('center_axis',(0.683495700250236,-0.584827952229823,-0.436817918622978));
#59561=DIRECTION('ref_axis',(-0.560823821146066,-0.0376838387890247,-0.827077124535099));
#59562=DIRECTION('center_axis',(0.663866867042483,-0.584827952229439,-0.466108409207899));
#59563=DIRECTION('ref_axis',(-0.573166168879147,0.0024618052356994,-0.819435465651434));
#59564=DIRECTION('center_axis',(0.683495700255293,-0.584827952229569,-0.436817918615406));
#59565=DIRECTION('ref_axis',(-0.543253576548145,-0.00784651557452022,-0.839532002821207));
#59566=DIRECTION('center_axis',(0.663866867031427,-0.584827952228639,-0.466108409224651));
#59567=DIRECTION('ref_axis',(-0.555116880746585,0.032283434098762,-0.83114561214806));
#59568=DIRECTION('center_axis',(0.68349570025321,-0.584827952229423,-0.436817918618862));
#59569=DIRECTION('ref_axis',(-0.524974319787969,0.0219588922014649,-0.850834749300029));
#59570=DIRECTION('center_axis',(0.756123145990597,-0.584827952229889,-0.293690405678969));
#59571=DIRECTION('ref_axis',(-0.396688118793096,-0.0526562713693517,-0.916441953150265));
#59572=DIRECTION('center_axis',(0.756123146001629,-0.584827952229234,-0.29369040565187));
#59573=DIRECTION('ref_axis',(-0.377217514040846,-0.0227607290510223,-0.925844963432815));
#59574=DIRECTION('center_axis',(0.768171927774616,-0.584827952229541,-0.260553556241384));
#59575=DIRECTION('ref_axis',(-0.343535615178875,-0.0330869094603869,-0.938556624570959));
#59576=DIRECTION('center_axis',(0.756123145995835,-0.584827952229549,-0.293690405666161));
#59577=DIRECTION('ref_axis',(-0.357314215289047,0.0070462672583536,-0.933957655180414));
#59578=DIRECTION('center_axis',(0.768171927772525,-0.584827952229534,-0.260553556247562));
#59579=DIRECTION('ref_axis',(-0.323436684571794,-0.00326197170798405,-0.946244191852073));
#59580=DIRECTION('center_axis',(0.768171927771508,-0.58482795222913,-0.260553556251471));
#59581=DIRECTION('ref_axis',(-0.302913090938082,0.0265489589950167,-0.95264831502219));
#59582=DIRECTION('center_axis',(0.75612314599938,-0.584827952230302,-0.293690405655535));
#59583=DIRECTION('ref_axis',(-0.336899225350735,0.0368858773883775,-0.940817912248361));
#59584=DIRECTION('center_axis',(-0.75706639739712,-0.572651970098847,0.314515804172152));
#59585=DIRECTION('ref_axis',(0.603266390053514,-0.797539756144985,-4.43056783040492E-17));
#59586=DIRECTION('center_axis',(-0.637444235726239,-0.398672303285474,0.65933697070045));
#59587=DIRECTION('ref_axis',(0.718941969615881,5.05113636903814E-16,0.69507010029553));
#59588=DIRECTION('center_axis',(0.600213204389163,-0.584827952229446,-0.545637586285995));
#59589=DIRECTION('ref_axis',(-0.686874649847015,-0.0273514773903244,-0.726261049542179));
#59590=DIRECTION('center_axis',(0.623358330292039,-0.584827952229342,-0.519038205093572));
#59591=DIRECTION('ref_axis',(-0.6600618082234,-0.037683838796267,-0.750265511414747));
#59592=DIRECTION('center_axis',(0.600213204391252,-0.584827952229486,-0.545637586283653));
#59593=DIRECTION('ref_axis',(-0.671349079048087,0.00246180523542522,-0.741137202936317));
#59594=DIRECTION('center_axis',(0.623358330295149,-0.58482795222947,-0.519038205089691));
#59595=DIRECTION('ref_axis',(-0.644191120423901,-0.00784651557927282,-0.764824314833324));
#59596=DIRECTION('center_axis',(0.600213204390774,-0.584827952229604,-0.545637586284054));
#59597=DIRECTION('ref_axis',(-0.654909785457995,0.0322834340866717,-0.755017187085787));
#59598=DIRECTION('center_axis',(0.623358330287479,-0.584827952229354,-0.519038205099034));
#59599=DIRECTION('ref_axis',(-0.6274726108324,0.0219588922014093,-0.778328934132901));
#59600=DIRECTION('center_axis',(0.713351720938627,-0.584827952229213,-0.386141927955623));
#59601=DIRECTION('ref_axis',(-0.508420747842796,-0.0526562713784942,-0.859497329982756));
#59602=DIRECTION('center_axis',(0.713351720938112,-0.584827952229473,-0.38614192795618));
#59603=DIRECTION('ref_axis',(-0.490282184329536,-0.0227607290419115,-0.871266508562414));
#59604=DIRECTION('center_axis',(0.729458642964286,-0.584827952229379,-0.354776485263458));
#59605=DIRECTION('ref_axis',(-0.458459070881828,-0.0330869094649778,-0.888099395759409));
#59606=DIRECTION('center_axis',(0.713351720936875,-0.584827952229576,-0.386141927958309));
#59607=DIRECTION('ref_axis',(-0.471552618913885,0.00704626725944046,-0.881809774108433));
#59608=DIRECTION('center_axis',(0.729458642961595,-0.584827952229519,-0.354776485268762));
#59609=DIRECTION('ref_axis',(-0.439482134009922,-0.00326197171117806,-0.898245408241334));
#59610=DIRECTION('center_axis',(0.729458642961771,-0.58482795222943,-0.354776485268546));
#59611=DIRECTION('ref_axis',(-0.419923024504176,0.0265489589890718,-0.907171321343362));
#59612=DIRECTION('center_axis',(0.713351720934301,-0.584827952229366,-0.386141927963382));
#59613=DIRECTION('ref_axis',(-0.452158425482432,0.0368858773992535,-0.891174612695927));
#59614=DIRECTION('center_axis',(-0.711677419984127,-0.572651970099548,0.406921332723959));
#59615=DIRECTION('ref_axis',(0.626902064855465,-0.779098068974602,-1.93769385385326E-16));
#59616=DIRECTION('center_axis',(-0.549780962986053,-0.39867230328459,0.734030849032851));
#59617=DIRECTION('ref_axis',(0.800388280671782,3.1365307998394E-16,0.599481943150308));
#59618=DIRECTION('center_axis',(0.527093820944015,-0.58482795222981,-0.616561732686457));
#59619=DIRECTION('ref_axis',(-0.772483083831191,-0.0273514773824917,-0.634446043316253));
#59620=DIRECTION('center_axis',(0.553390227073648,-0.584827952229816,-0.593072949029086));
#59621=DIRECTION('ref_axis',(-0.748890226298068,-0.0376838387900128,-0.661621762980388));
#59622=DIRECTION('center_axis',(0.52709382095827,-0.584827952229528,-0.616561732674538));
#59623=DIRECTION('ref_axis',(-0.758944413195169,0.00246180523388964,-0.651150763798087));
#59624=DIRECTION('center_axis',(0.553390227071032,-0.584827952229476,-0.593072949031862));
#59625=DIRECTION('ref_axis',(-0.734969385526333,-0.00784651556787667,-0.678054890501121));
#59626=DIRECTION('center_axis',(0.527093820954421,-0.584827952229462,-0.616561732677892));
#59627=DIRECTION('ref_axis',(-0.744374371642847,0.0322834340877894,-0.666981689947195));
#59628=DIRECTION('center_axis',(0.553390227083124,-0.584827952229677,-0.593072949020381));
#59629=DIRECTION('ref_axis',(-0.720075283965554,0.0219588921958596,-0.693548406728368));
#59630=DIRECTION('center_axis',(0.659330313101025,-0.584827952229551,-0.472503761378779));
#59631=DIRECTION('ref_axis',(-0.61213527799987,-0.0526562713738629,-0.788997920474461));
#59632=DIRECTION('center_axis',(0.659330313100206,-0.584827952229568,-0.472503761379902));
#59633=DIRECTION('ref_axis',(-0.595614811685905,-0.0227607290370077,-0.80294766038271));
#59634=DIRECTION('center_axis',(0.679241359593035,-0.584827952229435,-0.443404377187834));
#59635=DIRECTION('ref_axis',(-0.566152353171553,-0.0330869094612513,-0.823636308949901));
#59636=DIRECTION('center_axis',(0.659330313104009,-0.584827952229546,-0.472503761374621));
#59637=DIRECTION('ref_axis',(-0.578354356045136,0.00704626725904472,-0.815755226131792));
#59638=DIRECTION('center_axis',(0.679241359593601,-0.584827952229575,-0.443404377186782));
#59639=DIRECTION('ref_axis',(-0.54859668766339,-0.00326197171347784,-0.836080757956609));
#59640=DIRECTION('center_axis',(0.679241359592077,-0.584827952229497,-0.443404377189219));
#59641=DIRECTION('ref_axis',(-0.530310521131489,0.0265489589891908,-0.847387694006609));
#59642=DIRECTION('center_axis',(0.659330313101111,-0.584827952229377,-0.472503761378876));
#59643=DIRECTION('ref_axis',(-0.560286817122907,0.0368858773991434,-0.827476957145501));
#59644=DIRECTION('center_axis',(-0.655064864523098,-0.572651970099649,0.492909468775278));
#59645=DIRECTION('ref_axis',(0.658159678738397,-0.75287836818637,3.33585939142612E-17));
#59646=DIRECTION('center_axis',(-0.453447316035864,-0.398672303285154,0.797148622386806));
#59647=DIRECTION('ref_axis',(0.869211990412778,-3.92406044704623E-16,0.494439597648345));
#59648=DIRECTION('center_axis',(0.445661853117017,-0.584827952228927,-0.677762332213901));
#59649=DIRECTION('ref_axis',(-0.845908998097638,-0.0273514774077798,-0.532625444023342));
#59650=DIRECTION('center_axis',(0.474694829402545,-0.584827952229701,-0.657754578265559));
#59651=DIRECTION('ref_axis',(-0.825908198131717,-0.0376838387902702,-0.562543844116038));
#59652=DIRECTION('center_axis',(0.445661853094375,-0.584827952229501,-0.677762332228294));
#59653=DIRECTION('ref_axis',(-0.834570740577306,0.00246180523543606,-0.550895288133081));
#59654=DIRECTION('center_axis',(0.474694829395997,-0.584827952229462,-0.657754578270496));
#59655=DIRECTION('ref_axis',(-0.814156744359243,-0.00784651556552523,-0.580592135502918));
#59656=DIRECTION('center_axis',(0.44566185310384,-0.584827952230146,-0.677762332221514));
#59657=DIRECTION('ref_axis',(-0.822099729311578,0.0322834340795859,-0.568427493133345));
#59658=DIRECTION('center_axis',(0.47469482941652,-0.584827952229831,-0.657754578255358));
#59659=DIRECTION('ref_axis',(-0.801321939721966,0.0219588921926168,-0.597830206642236));
#59660=DIRECTION('center_axis',(0.594910872379941,-0.584827952228667,-0.551413928202908));
#59661=DIRECTION('ref_axis',(-0.706196069132843,-0.0526562713866946,-0.706055542450431));
#59662=DIRECTION('center_axis',(0.59491087235748,-0.584827952229707,-0.551413928226038));
#59663=DIRECTION('ref_axis',(-0.691554237658444,-0.0227607290313939,-0.721965847939227));
#59664=DIRECTION('center_axis',(0.618312034230551,-0.584827952229208,-0.525039517195676));
#59665=DIRECTION('ref_axis',(-0.664917074641091,-0.0330869094688109,-0.746183985537439));
#59666=DIRECTION('center_axis',(0.594910872366718,-0.584827952229429,-0.551413928216366));
#59667=DIRECTION('ref_axis',(-0.676035099491233,0.00704626726054901,-0.73683573092893));
#59668=DIRECTION('center_axis',(0.618312034217811,-0.584827952229436,-0.525039517210426));
#59669=DIRECTION('ref_axis',(-0.649059543844922,-0.00326197170724836,-0.760730614662249));
#59670=DIRECTION('center_axis',(0.618312034220884,-0.584827952229394,-0.525039517206855));
#59671=DIRECTION('ref_axis',(-0.632334704050471,0.0265489589903301,-0.774240256528898));
#59672=DIRECTION('center_axis',(0.594910872389116,-0.584827952230958,-0.551413928190579));
#59673=DIRECTION('ref_axis',(-0.659579150937677,0.0368858773772172,-0.750729495689657));
#59674=DIRECTION('center_axis',(-0.588121544827873,-0.572651970103301,0.571124128054562));
#59675=DIRECTION('ref_axis',(0.697621253253775,-0.716466738243048,-6.26947218563319E-16));
#59676=DIRECTION('center_axis',(-0.349962534036297,-0.398672303280935,0.847694885774102));
#59677=DIRECTION('ref_axis',(8.44177824649252E-17,-0.90491859166274,-0.4255847065663));
#59678=DIRECTION('center_axis',(0.357201531611052,-0.584827952228913,-0.728274214912525));
#59679=DIRECTION('ref_axis',(-0.905994422163722,-0.0273514774097695,-0.422405023279467));
#59680=DIRECTION('center_axis',(0.388513210693687,-0.584827952230087,-0.712063024883926));
#59681=DIRECTION('ref_axis',(-0.889901104311223,-0.0376838387844891,-0.454594272775329));
#59682=DIRECTION('center_axis',(0.357201531563024,-0.58482795222909,-0.72827421493594));
#59683=DIRECTION('ref_axis',(-0.897035388838967,0.00246180524912005,-0.441951864670168));
#59684=DIRECTION('center_axis',(0.388513210718662,-0.584827952229685,-0.712063024870629));
#59685=DIRECTION('ref_axis',(-0.88050436496746,-0.00784651558132259,-0.473973095720087));
#59686=DIRECTION('center_axis',(0.357201531562618,-0.58482795222851,-0.728274214936605));
#59687=DIRECTION('ref_axis',(-0.886860083170569,0.0322834341005172,-0.460908855156168));
#59688=DIRECTION('center_axis',(0.388513210725782,-0.584827952230155,-0.712063024866358));
#59689=DIRECTION('ref_axis',(-0.869931269801255,0.0219588921870204,-0.492683867074917));
#59690=DIRECTION('center_axis',(0.521109331790668,-0.584827952229543,-0.62162796800955));
#59691=DIRECTION('ref_axis',(-0.789119726418472,-0.0526562713750646,-0.611978246722963));
#59692=DIRECTION('center_axis',(0.521109331792446,-0.584827952229465,-0.621627968008134));
#59693=DIRECTION('ref_axis',(-0.776587440174645,-0.022760729040405,-0.629598202805998));
#59694=DIRECTION('center_axis',(0.547631558707113,-0.584827952229693,-0.598394470394607));
#59695=DIRECTION('ref_axis',(-0.753195656657539,-0.0330869094581457,-0.656963894909551));
#59696=DIRECTION('center_axis',(0.521109331798352,-0.58482795222975,-0.621627968002915));
#59697=DIRECTION('ref_axis',(-0.76305436556791,0.00704626725475995,-0.64629589609213));
#59698=DIRECTION('center_axis',(0.547631558727812,-0.584827952229681,-0.598394470375676));
#59699=DIRECTION('ref_axis',(-0.73928634326801,-0.00326197172494508,-0.673383295158025));
#59700=DIRECTION('center_axis',(0.547631558699565,-0.584827952228912,-0.598394470402278));
#59701=DIRECTION('ref_axis',(-0.724386590953742,0.0265489589987662,-0.688882587690019));
#59702=DIRECTION('center_axis',(0.521109331796591,-0.584827952229941,-0.621627968004211));
#59703=DIRECTION('ref_axis',(-0.748469527566617,0.0368858773927419,-0.66214258158887));
#59704=DIRECTION('center_axis',(-0.511903197047791,-0.572651970103374,0.640331818660431));
#59705=DIRECTION('ref_axis',(-3.39450182657419E-16,-0.745401236142811,-0.666616079281597));
#59706=DIRECTION('center_axis',(-0.240958633816367,-0.398672303283347,0.884872494421711));
#59707=DIRECTION('ref_axis',(3.01927584586609E-17,-0.911736456568353,-0.410775648942563));
#59708=DIRECTION('center_axis',(0.263107928563467,-0.584827952229085,-0.767300778194951));
#59709=DIRECTION('ref_axis',(-0.951791772979906,-0.0273514774076893,-0.305523022980894));
#59710=DIRECTION('center_axis',(0.296204506578728,-0.584827952229886,-0.755141812226717));
#59711=DIRECTION('ref_axis',(-0.939859738468349,-0.0376838387875407,-0.339475478201949));
#59712=DIRECTION('center_axis',(0.26310792852108,-0.584827952229321,-0.767300778209305));
#59713=DIRECTION('ref_axis',(-0.94535325314404,0.00246180524608073,-0.326038596311711));
#59714=DIRECTION('center_axis',(0.296204506588777,-0.584827952229501,-0.755141812223074));
#59715=DIRECTION('ref_axis',(-0.932965905768518,-0.00784651557401198,-0.359879217053272));
#59716=DIRECTION('center_axis',(0.263107928504294,-0.584827952228226,-0.767300778215896));
#59717=DIRECTION('ref_axis',(-0.93763412372089,0.0322834341076045,-0.346121409214134));
#59718=DIRECTION('center_axis',(0.296204506582971,-0.584827952229374,-0.75514181222545));
#59719=DIRECTION('ref_axis',(-0.924821264096414,0.0219588922029174,-0.379767608582316));
#59720=DIRECTION('center_axis',(0.43908958573722,-0.584827952230541,-0.682038563416284));
#59721=DIRECTION('ref_axis',(-0.859598494219977,-0.0526562713614962,-0.508249688461343));
#59722=DIRECTION('center_axis',(0.439089585757463,-0.584827952229602,-0.682038563404057));
#59723=DIRECTION('ref_axis',(-0.849373394858158,-0.0227607290393782,-0.527301417901302));
#59724=DIRECTION('center_axis',(0.468314606413799,-0.584827952228568,-0.66231238529234));
#59725=DIRECTION('ref_axis',(-0.829595893198619,-0.0330869094855917,-0.557383091247553));
#59726=DIRECTION('center_axis',(0.439089585767504,-0.584827952229721,-0.682038563397491));
#59727=DIRECTION('ref_axis',(-0.838039808477603,0.00704626725346033,-0.545563588891904));
#59728=DIRECTION('center_axis',(0.468314606372224,-0.584827952229452,-0.662312385320956));
#59729=DIRECTION('ref_axis',(-0.817854155462514,-0.00326197170577599,-0.575416318793));
#59730=DIRECTION('center_axis',(0.468314606377903,-0.584827952229227,-0.662312385317139));
#59731=DIRECTION('ref_axis',(-0.805014468575387,0.0265489589908086,-0.592660828940796));
#59732=DIRECTION('center_axis',(0.439089585738317,-0.584827952228573,-0.682038563417265));
#59733=DIRECTION('ref_axis',(-0.825556092629325,0.0368858774108551,-0.563113283425487));
#59734=DIRECTION('center_axis',(-0.427611830052617,-0.572651970104803,0.699441093970135));
#59735=DIRECTION('ref_axis',(-1.75302949851223E-16,-0.773750158454805,-0.6334908778279));
#59736=DIRECTION('center_axis',(-0.128154671999727,-0.398672303284917,0.908095135235368));
#59737=DIRECTION('ref_axis',(-2.92400519014607E-17,-0.915645369907592,-0.401987010445348));
#59738=DIRECTION('center_axis',(0.1648649562964,-0.584827952229255,-0.79422654984376));
#59739=DIRECTION('ref_axis',(-0.982578798964788,-0.0273514773978768,-0.183822742088859));
#59740=DIRECTION('center_axis',(0.199224480465946,-0.584827952229349,-0.786311562088655));
#59741=DIRECTION('ref_axis',(-0.974996223102871,-0.0376838387993657,-0.219002952556533));
#59742=DIRECTION('center_axis',(0.164864956283302,-0.584827952229486,-0.794226549846309));
#59743=DIRECTION('ref_axis',(-0.978762331919751,0.00246180523728022,-0.204983504531425));
#59744=DIRECTION('center_axis',(0.199224480450776,-0.584827952229559,-0.786311562092342));
#59745=DIRECTION('ref_axis',(-0.970714016905226,-0.00784651557031847,-0.240109828156044));
#59746=DIRECTION('center_axis',(0.164864956289079,-0.584827952229657,-0.794226549844983));
#59747=DIRECTION('ref_axis',(-0.97362111401387,0.0322834340847991,-0.225875421925633));
#59748=DIRECTION('center_axis',(0.199224480466149,-0.58482795222989,-0.786311562088201));
#59749=DIRECTION('ref_axis',(-0.965126274581717,0.0219588921935203,-0.26086218807188));
#59750=DIRECTION('center_axis',(0.350145134649513,-0.584827952229794,-0.731693003227434));
#59751=DIRECTION('ref_axis',(-0.916520880250958,-0.0526562713704369,-0.396505729024655));
#59752=DIRECTION('center_axis',(0.350145134667601,-0.584827952229321,-0.731693003219155));
#59753=DIRECTION('ref_axis',(-0.908764223708701,-0.0227607290460544,-0.416688774651315));
#59754=DIRECTION('center_axis',(0.381612052951492,-0.584827952229456,-0.715785238275594));
#59755=DIRECTION('ref_axis',(-0.892912906966885,-0.0330869094632203,-0.449012023217774));
#59756=DIRECTION('center_axis',(0.350145134675522,-0.584827952229961,-0.731693003214853));
#59757=DIRECTION('ref_axis',(-0.899808862985237,0.00704626724822561,-0.436227417995569));
#59758=DIRECTION('center_axis',(0.381612052944737,-0.584827952229599,-0.715785238279079));
#59759=DIRECTION('ref_axis',(-0.883523919043546,-0.00326197170887951,-0.468374683366324));
#59760=DIRECTION('center_axis',(0.381612052960543,-0.584827952229905,-0.715785238270402));
#59761=DIRECTION('ref_axis',(-0.872946787136347,0.0265489589811143,-0.487092454884438));
#59762=DIRECTION('center_axis',(0.350145134633492,-0.584827952228301,-0.731693003236293));
#59763=DIRECTION('ref_axis',(-0.889623144933142,0.0368858774129701,-0.455203352411579));
#59764=DIRECTION('center_axis',(-0.336576769080192,-0.572651970082322,0.747519765408497));
#59765=DIRECTION('ref_axis',(4.05335326092723E-16,-0.793835266517972,-0.60813285524821));
#59766=DIRECTION('center_axis',(-0.01332963444991,-0.398672303291145,0.91699657329456));
#59767=DIRECTION('ref_axis',(1.50046340237098E-17,-0.917078049740163,-0.398707725890507));
#59768=DIRECTION('center_axis',(0.0640219651873326,-0.584827952229454,-0.808626894349091));
#59769=DIRECTION('ref_axis',(-0.997869970322272,-0.0273514773912274,-0.0592234667471015));
#59770=DIRECTION('center_axis',(0.0991025652636654,-0.584827952229383,-0.805080708903988));
#59771=DIRECTION('ref_axis',(-0.994756434870767,-0.037683838797787,-0.0950766195058686));
#59772=DIRECTION('center_axis',(0.0640219651883166,-0.584827952229605,-0.808626894348903));
#59773=DIRECTION('ref_axis',(-0.996735744040505,0.0024618052355194,-0.0806957004245199));
#59774=DIRECTION('center_axis',(0.0991025652509091,-0.584827952229481,-0.805080708905487));
#59775=DIRECTION('ref_axis',(-0.993153388117073,-0.00784651557029387,-0.116553763838773));
#59776=DIRECTION('center_axis',(0.0640219652154374,-0.584827952230895,-0.808626894345823));
#59777=DIRECTION('ref_axis',(-0.994253517734423,0.0322834340705456,-0.102067244291878));
#59778=DIRECTION('center_axis',(0.0991025652721308,-0.584827952229959,-0.805080708902527));
#59779=DIRECTION('ref_axis',(-0.990210667182516,0.0219588921906706,-0.137842815016649));
#59780=DIRECTION('center_axis',(0.255678685621909,-0.584827952229304,-0.769808207289278));
#59781=DIRECTION('ref_axis',(-0.958989184500568,-0.0526562713786804,-0.278508637380299));
#59782=DIRECTION('center_axis',(0.255678685634193,-0.584827952229256,-0.769808207285234));
#59783=DIRECTION('ref_axis',(-0.953823297885295,-0.0227607290501976,-0.299504700504554));
#59784=DIRECTION('center_axis',(0.288891249491466,-0.58482795222929,-0.757969730436879));
#59785=DIRECTION('ref_axis',(-0.942148150771053,-0.0330869094683896,-0.333559767388869));
#59786=DIRECTION('center_axis',(0.255678685607245,-0.584827952229379,-0.769808207294092));
#59787=DIRECTION('ref_axis',(-0.947387394215224,0.00704626726637755,-0.320011680098865));
#59788=DIRECTION('center_axis',(0.288891249475173,-0.58482795222939,-0.757969730443012));
#59789=DIRECTION('ref_axis',(-0.935259982631717,-0.00326197170936511,-0.353946499386967));
#59790=DIRECTION('center_axis',(0.288891249477309,-0.584827952229552,-0.757969730442073));
#59791=DIRECTION('ref_axis',(-0.927112213402921,0.0265489589896012,-0.373842341817651));
#59792=DIRECTION('center_axis',(0.255678685630505,-0.584827952230323,-0.769808207285649));
#59793=DIRECTION('ref_axis',(-0.939660308794284,0.0368858773885189,-0.340114592638878));
#59794=DIRECTION('center_axis',(-0.240233691368199,-0.572651970087536,0.783809603594185));
#59795=DIRECTION('ref_axis',(1.07498383400422E-17,-0.807455881581724,-0.589927961109729));
#59796=DIRECTION('center_axis',(0.101705619397328,-0.398672303296703,0.911436427605956));
#59797=DIRECTION('ref_axis',(1.56250901277415E-16,-0.916187281030926,-0.400750378761092));
#59798=DIRECTION('center_axis',(-0.0378306905315764,-0.584827952229299,
-0.810274709678878));
#59799=DIRECTION('ref_axis',(-0.997424136147838,-0.0273514773998618,0.0663097980224935));
#59800=DIRECTION('center_axis',(-0.00258225658073046,-0.584827952229025,
-0.811153252007632));
#59801=DIRECTION('ref_axis',(-0.998828743421528,-0.0376838388038362,0.030349128619739));
#59802=DIRECTION('center_axis',(-0.0378306905364861,-0.584827952229633,
-0.810274709678407));
#59803=DIRECTION('ref_axis',(-0.998990038057491,0.00246180523032482,0.0448647230783922));
#59804=DIRECTION('center_axis',(-0.00258225661252645,-0.584827952229595,
-0.81115325200712));
#59805=DIRECTION('ref_axis',(-0.999930137117214,-0.00784651556523036,0.00884042296698303));
#59806=DIRECTION('center_axis',(-0.0378306905424066,-0.584827952229676,
-0.8102747096781));
#59807=DIRECTION('ref_axis',(-0.999205949545135,0.0322834340848084,0.0233505947953502));
#59808=DIRECTION('center_axis',(-0.00258225660711838,-0.584827952229256,
-0.811153252007381));
#59809=DIRECTION('ref_axis',(-0.99967884603978,0.0219588922047833,-0.0126495784005934));
#59810=DIRECTION('center_axis',(0.157180030989646,-0.584827952228585,-0.795783076064208));
#59811=DIRECTION('ref_axis',(-0.986333656440618,-0.0526562713877413,-0.156119298153757));
#59812=DIRECTION('center_axis',(0.157180030957695,-0.584827952229673,-0.79578307606972));
#59813=DIRECTION('ref_axis',(-0.983840008874882,-0.0227607290325835,-0.177597258286768));
#59814=DIRECTION('center_axis',(0.191614458464428,-0.584827952228724,-0.788200587159982));
#59815=DIRECTION('ref_axis',(-0.976525155425776,-0.0330869094830448,-0.212847074777938));
#59816=DIRECTION('center_axis',(0.157180030967844,-0.584827952229568,-0.795783076067793));
#59817=DIRECTION('ref_axis',(-0.980025060284695,0.00704626726114766,-0.198749166870366));
#59818=DIRECTION('center_axis',(0.191614458419219,-0.584827952229447,-0.788200587170436));
#59819=DIRECTION('ref_axis',(-0.972246437598155,-0.00326197170583667,-0.233936367669261));
#59820=DIRECTION('center_axis',(0.191614458440564,-0.584827952229784,-0.788200587164998));
#59821=DIRECTION('ref_axis',(-0.966656526225866,0.0265489589817698,-0.254696511719196));
#59822=DIRECTION('center_axis',(0.157180030962411,-0.584827952229387,-0.795783076068999));
#59823=DIRECTION('ref_axis',(-0.974878468277728,0.0368858774010781,-0.219662022518284));
#59824=DIRECTION('center_axis',(-0.140101984835677,-0.572651970092198,0.807738296105012));
#59825=DIRECTION('ref_axis',(4.34107268269613E-17,-0.815784312898716,-0.578356252519474));
#59826=DIRECTION('center_axis',(0.215136914870904,-0.398672303292247,0.891502384992595));
#59827=DIRECTION('ref_axis',(-2.23020076991194E-16,-0.912878440593297,-0.408231494007935));
#59828=DIRECTION('center_axis',(-0.139086733705889,-0.584827952229799,-0.799144008797993));
#59829=DIRECTION('ref_axis',(-0.981248327510859,-0.0273514773825953,0.190797317701617));
#59830=DIRECTION('center_axis',(-0.104226354737577,-0.584827952229801,-0.804433423764089));
#59831=DIRECTION('ref_axis',(-0.987148926014928,-0.0376838387855637,0.155296252890911));
#59832=DIRECTION('center_axis',(-0.139086733679773,-0.584827952229591,-0.799144008802691));
#59833=DIRECTION('ref_axis',(-0.98548966240741,0.00246180522930748,0.169717603103337));
#59834=DIRECTION('center_axis',(-0.104226354689701,-0.584827952229773,-0.804433423770312));
#59835=DIRECTION('ref_axis',(-0.990937390529949,-0.00784651559373285,0.13409519097541));
#59836=DIRECTION('center_axis',(-0.139086733682762,-0.584827952229986,-0.799144008801882));
#59837=DIRECTION('ref_axis',(-0.988400306633913,0.0322834340821356,0.148400181030382));
#59838=DIRECTION('center_axis',(-0.104226354709108,-0.584827952229878,-0.804433423767722));
#59839=DIRECTION('ref_axis',(-0.993381492315826,0.021958892191087,0.112743149584011));
#59840=DIRECTION('center_axis',(0.0562025533357102,-0.584827952229681,-0.809207970357055));
#59841=DIRECTION('ref_axis',(-0.998123057416714,-0.0526562713740524,-0.0312678643033671));
#59842=DIRECTION('center_axis',(0.0562025533502697,-0.584827952229286,-0.80920797035633));
#59843=DIRECTION('ref_axis',(-0.998340975198042,-0.0227607290464764,-0.0528890012563592));
#59844=DIRECTION('center_axis',(0.0913157928915538,-0.584827952229636,-0.806001049788074));
#59845=DIRECTION('ref_axis',(-0.995501775042467,-0.0330869094538936,-0.0887776565926787));
#59846=DIRECTION('center_axis',(0.0562025533307129,-0.584827952229465,-0.809207970357558));
#59847=DIRECTION('ref_axis',(-0.997207145717477,0.00704626726482406,-0.0743522605415241));
#59848=DIRECTION('center_axis',(0.0913157928957569,-0.584827952229292,-0.806001049787848));
#59849=DIRECTION('ref_axis',(-0.993899985449946,-0.00326197170642138,-0.11023691969202));
#59850=DIRECTION('center_axis',(0.0913157929462842,-0.584827952230976,-0.806001049780901));
#59851=DIRECTION('ref_axis',(-0.990956088178859,0.0265489589641095,-0.131533965496278));
#59852=DIRECTION('center_axis',(0.0562025533008339,-0.584827952227875,-0.809207970360782));
#59853=DIRECTION('ref_axis',(-0.994722211948487,0.036885877419139,-0.095745251074552));
#59854=DIRECTION('center_axis',(-0.0377607863096941,-0.572651970097324,
0.818928473165348));
#59855=DIRECTION('ref_axis',(-2.66091658816507E-19,-0.819512943907396,-0.573060672850819));
#59856=DIRECTION('center_axis',(0.325175372679881,-0.398672303295285,0.857508817206991));
#59857=DIRECTION('ref_axis',(-1.86469491306704E-16,-0.906789441031397,-0.421583810924905));
#59858=DIRECTION('center_axis',(-0.238149295947369,-0.584827952229357,-0.775410329523014));
#59859=DIRECTION('ref_axis',(-0.949597646587419,-0.0273514773986001,0.312275849658199));
#59860=DIRECTION('center_axis',(-0.204226740992109,-0.584827952230219,-0.785027199881604));
#59861=DIRECTION('ref_axis',(-0.95990118034991,-0.0376838387824492,0.277794262463191));
#59862=DIRECTION('center_axis',(-0.238149295926173,-0.584827952229801,-0.775410329529189));
#59863=DIRECTION('ref_axis',(-0.956447526083613,0.00246180521581662,0.29189393512647));
#59864=DIRECTION('center_axis',(-0.20422674096961,-0.584827952229362,-0.785027199888095));
#59865=DIRECTION('ref_axis',(-0.966316969330447,-0.00784651557616204,0.257235197780811));
#59866=DIRECTION('center_axis',(-0.238149295974102,-0.584827952228874,-0.775410329515168));
#59867=DIRECTION('ref_axis',(-0.962007000439502,0.0322834340959872,0.271109407782839));
#59868=DIRECTION('center_axis',(-0.204226740951319,-0.58482795223023,-0.785027199892207));
#59869=DIRECTION('ref_axis',(-0.971417919042336,0.0219588921862599,0.236357850763224));
#59870=DIRECTION('center_axis',(-0.0456612721227857,-0.584827952229086,
-0.809871171557343));
#59871=DIRECTION('ref_axis',(-0.994171461524437,-0.0526562713812391,0.0940766824170002));
#59872=DIRECTION('center_axis',(-0.045661272150223,-0.584827952229654,-0.809871171555386));
#59873=DIRECTION('ref_axis',(-0.997097507964699,-0.0227607290290802,0.0726533469611127));
#59874=DIRECTION('center_axis',(-0.0104229772031832,-0.584827952228972,
-0.811090394369141));
#59875=DIRECTION('ref_axis',(-0.998778736973622,-0.0330869094738195,0.0366918382047993));
#59876=DIRECTION('center_axis',(-0.045661272103643,-0.584827952229944,-0.809871171557803));
#59877=DIRECTION('ref_axis',(-0.998662678760311,0.00704626724351014,0.0512172253173974));
#59878=DIRECTION('center_axis',(-0.0104229772141451,-0.584827952229454,
-0.811090394368653));
#59879=DIRECTION('ref_axis',(-0.999879136804493,-0.00326197171688232,0.0152010303473315));
#59880=DIRECTION('center_axis',(-0.0104229772060856,-0.584827952230127,
-0.811090394368271));
#59881=DIRECTION('ref_axis',(-0.999627680658252,0.026548958978832,-0.00629705001911262));
#59882=DIRECTION('center_axis',(-0.0456612721438079,-0.584827952229114,
-0.809871171556137));
#59883=DIRECTION('ref_axis',(-0.998878592114955,0.0368858774036614,0.0296814801283008));
#59884=DIRECTION('center_axis',(0.0651759223724451,-0.572651970102054,0.817203658998868));
#59885=DIRECTION('ref_axis',(-1.00418082817833E-16,-0.818944908520059,-0.573872143259343));
#59886=DIRECTION('center_axis',(0.430085620611463,-0.398672303296099,0.809991823124059));
#59887=DIRECTION('ref_axis',(0.883216234748452,-1.85852527887398E-17,-0.468965971768493));
#59888=DIRECTION('center_axis',(-0.333456101556104,-0.584827952229228,-0.739447966138506));
#59889=DIRECTION('ref_axis',(-0.902971243511053,-0.0273514773981376,0.428829604943784));
#59890=DIRECTION('center_axis',(-0.301006349552527,-0.58482795223066,-0.753240628098854));
#59891=DIRECTION('ref_axis',(-0.917515219648999,-0.0376838387726605,0.395911290578843));
#59892=DIRECTION('center_axis',(-0.333456101558463,-0.584827952229472,-0.73944796613725));
#59893=DIRECTION('ref_axis',(-0.912321640907653,0.00246180523059358,0.409466925461109));
#59894=DIRECTION('center_axis',(-0.301006349518084,-0.584827952229521,-0.753240628113502));
#59895=DIRECTION('ref_axis',(-0.926457152277091,-0.00784651557441018,0.376318451830314));
#59896=DIRECTION('center_axis',(-0.333456101577383,-0.584827952229164,-0.739447966128961));
#59897=DIRECTION('ref_axis',(-0.920442269177619,0.0322834340938364,0.389543077199768));
#59898=DIRECTION('center_axis',(-0.30100634950513,-0.584827952230014,-0.753240628118295));
#59899=DIRECTION('ref_axis',(-0.934134504885361,0.0219588921907591,0.356245047455169));
#59900=DIRECTION('center_axis',(-0.146804992071868,-0.584827952229856,-0.79776222058544));
#59901=DIRECTION('ref_axis',(-0.974541187792916,-0.0526562713714318,0.217937583680351));
#59902=DIRECTION('center_axis',(-0.14680499205743,-0.584827952229402,-0.79776222058843));
#59903=DIRECTION('ref_axis',(-0.980129217395657,-0.0227607290439648,0.197049908451549));
#59904=DIRECTION('center_axis',(-0.111997370784885,-0.584827952229807,-0.803388358907424));
#59905=DIRECTION('ref_axis',(-0.986304361580781,-0.033086909454995,0.161582680846199));
#59906=DIRECTION('center_axis',(-0.146804992063548,-0.584827952229562,-0.797762220587186));
#59907=DIRECTION('ref_axis',(-0.98436870478496,0.00704626725946665,0.175978984988801));
#59908=DIRECTION('center_axis',(-0.111997370782148,-0.58482795222945,-0.803388358908065));
#59909=DIRECTION('ref_axis',(-0.990089596872472,-0.00326197170656146,0.140399251085937));
#59910=DIRECTION('center_axis',(-0.11199737074419,-0.584827952230717,-0.803388358912434));
#59911=DIRECTION('ref_axis',(-0.992534547464178,0.0265489589715222,0.119039173668203));
#59912=DIRECTION('center_axis',(-0.146804992029651,-0.584827952231123,-0.79776222059228));
#59913=DIRECTION('ref_axis',(-0.987282060191029,0.0368858773761462,0.154640116642314));
#59914=DIRECTION('center_axis',(0.167084767814961,-0.572651970094166,0.802591054966034));
#59915=DIRECTION('ref_axis',(1.54173804028222E-16,-0.814034314661491,-0.580816782258912));
#59916=DIRECTION('center_axis',(0.528213161385387,-0.398672303295916,0.74970077412524));
#59917=DIRECTION('ref_axis',(0.817474789260215,5.18362180146966E-17,-0.575964381645226));
#59918=DIRECTION('center_axis',(-0.423504105258802,-0.584827952229492,-0.691824066594969));
#59919=DIRECTION('ref_axis',(-0.842104444509155,-0.0273514773890005,0.538620461199319));
#59920=DIRECTION('center_axis',(-0.393038908136311,-0.584827952230094,-0.709575001660411));
#59921=DIRECTION('ref_axis',(-0.860659495847695,-0.037683838783106,0.507784561110084));
#59922=DIRECTION('center_axis',(-0.423504105256182,-0.584827952229402,-0.69182406659665));
#59923=DIRECTION('ref_axis',(-0.853807898461964,0.00246180523642254,0.520582377764501));
#59924=DIRECTION('center_axis',(-0.39303890811573,-0.584827952229416,-0.709575001672369));
#59925=DIRECTION('ref_axis',(-0.871986552495883,-0.00784651557689437,0.489466939087459));
#59926=DIRECTION('center_axis',(-0.423504105251284,-0.584827952229727,-0.691824066599373));
#59927=DIRECTION('ref_axis',(-0.864361613491274,0.0322834340843171,0.501833419579131));
#59928=DIRECTION('center_axis',(-0.393038908128715,-0.584827952229044,-0.709575001665483));
#59929=DIRECTION('ref_axis',(-0.88211923155341,0.0219588922046995,0.470514046949466));
#59930=DIRECTION('center_axis',(-0.245633509582242,-0.584827952229828,-0.773072082836379));
#59931=DIRECTION('ref_axis',(-0.939541817367972,-0.0526562713714979,0.338361479045916));
#59932=DIRECTION('center_axis',(-0.24563350958476,-0.584827952229614,-0.773072082835741));
#59933=DIRECTION('ref_axis',(-0.947703703562037,-0.0227607290339116,0.31833887520792));
#59934=DIRECTION('center_axis',(-0.211805498835859,-0.584827952228281,-0.783016409122675));
#59935=DIRECTION('ref_axis',(-0.958275377229305,-0.033086909490308,0.283925268013282));
#59936=DIRECTION('center_axis',(-0.245633509587554,-0.584827952229358,-0.773072082835046));
#59937=DIRECTION('ref_axis',(-0.95455064829962,0.00704626726762763,0.297965450930756));
#59938=DIRECTION('center_axis',(-0.211805498854265,-0.584827952229578,-0.783016409116728));
#59939=DIRECTION('ref_axis',(-0.964685752555244,-0.00326197172903191,0.263383291720189));
#59940=DIRECTION('center_axis',(-0.211805498885655,-0.584827952229335,-0.783016409108418));
#59941=DIRECTION('ref_axis',(-0.969788551538211,0.0265489589902435,0.242498078511879));
#59942=DIRECTION('center_axis',(-0.245633509521976,-0.584827952232075,-0.773072082853827));
#59943=DIRECTION('ref_axis',(-0.960115500406961,0.0368858773645434,0.277159986162033));
#59944=DIRECTION('center_axis',(0.266358586659695,-0.572651970087279,0.775321110552143));
#59945=DIRECTION('ref_axis',(1.19124006870652E-16,-0.804380141087925,-0.594114962463807));
#59946=DIRECTION('center_axis',(0.61801046506436,-0.39867230329826,0.677586496068062));
#59947=DIRECTION('ref_axis',(0.738841278009524,-2.52796011405891E-16,-0.673879489159044));
#59948=DIRECTION('center_axis',(-0.506873196214637,-0.584827952229441,-0.633289688255127));
#59949=DIRECTION('ref_axis',(-0.76795715537621,-0.0273514773915847,0.639916951010815));
#59950=DIRECTION('center_axis',(-0.47887300834826,-0.584827952229484,-0.654718953572108));
#59951=DIRECTION('ref_axis',(-0.790230657668672,-0.037683838795387,0.611649765776283));
#59952=DIRECTION('center_axis',(-0.506873196222743,-0.584827952229388,-0.633289688248689));
#59953=DIRECTION('ref_axis',(-0.781829095416187,0.00246180524143953,0.623487934988048));
#59954=DIRECTION('center_axis',(-0.478873008346566,-0.584827952229558,-0.654718953573281));
#59955=DIRECTION('ref_axis',(-0.803764203880813,-0.0078465155765271,0.594896240325278));
#59956=DIRECTION('center_axis',(-0.506873196212754,-0.584827952229607,-0.633289688256482));
#59957=DIRECTION('ref_axis',(-0.794649458809219,0.032283434085324,0.606209549164209));
#59958=DIRECTION('center_axis',(-0.478873008327432,-0.584827952230354,-0.654718953586565));
#59959=DIRECTION('ref_axis',(-0.816192411012875,0.0219588921831804,0.5773627588086));
#59960=DIRECTION('center_axis',(-0.340588239910082,-0.584827952229608,-0.736190136531233));
#59961=DIRECTION('ref_axis',(-0.889725311228872,-0.0526562713729305,0.453449211757819));
#59962=DIRECTION('center_axis',(-0.340588239919936,-0.584827952229746,-0.736190136526565));
#59963=DIRECTION('ref_axis',(-0.900332336193019,-0.0227607290304719,0.434607447726361));
#59964=DIRECTION('center_axis',(-0.308273327736802,-0.584827952229275,-0.750295822790845));
#59965=DIRECTION('ref_axis',(-0.915133817714972,-0.0330869094691202,0.401790184171045));
#59966=DIRECTION('center_axis',(-0.340588239870387,-0.584827952230211,-0.736190136549119));
#59967=DIRECTION('ref_axis',(-0.909678757889288,0.00704626723776923,0.415252823666518));
#59968=DIRECTION('center_axis',(-0.308273327748204,-0.584827952229549,-0.750295822785946));
#59969=DIRECTION('ref_axis',(-0.924068237631525,-0.00326197171192395,0.382213620559391));
#59970=DIRECTION('center_axis',(-0.308273327756411,-0.584827952229156,-0.750295822782881));
#59971=DIRECTION('ref_axis',(-0.931748410832772,0.0265489589935049,0.362132643774301));
#59972=DIRECTION('center_axis',(-0.340588239917826,-0.584827952229112,-0.736190136528045));
#59973=DIRECTION('ref_axis',(-0.917807345609863,0.0368858774046296,0.395308877199423));
#59974=DIRECTION('center_axis',(0.361431771479317,-0.572651970079971,0.735823889071869));
#59975=DIRECTION('ref_axis',(-1.63914301419145E-16,-0.789173129058311,-0.61417080065102));
#59976=DIRECTION('center_axis',(0.698061374528685,-0.398672303296788,0.594786274198688));
#59977=DIRECTION('ref_axis',(0.648555798442348,-1.26241681070733E-16,-0.76116711457262));
#59978=DIRECTION('center_axis',(-0.582248594085411,-0.584827952229698,-0.564767953212982));
#59979=DIRECTION('ref_axis',(-0.6816987231398,-0.0273514773860545,0.731121568245916));
#59980=DIRECTION('center_axis',(-0.557154995166819,-0.584827952229244,-0.589537596470328));
#59981=DIRECTION('ref_axis',(-0.707339409953029,-0.0376838387996158,0.705868888265112));
#59982=DIRECTION('center_axis',(-0.582248594079238,-0.584827952229526,-0.564767953219524));
#59983=DIRECTION('ref_axis',(-0.697520380503128,0.00246180523609652,0.716560715011471));
#59984=DIRECTION('center_axis',(-0.557154995173368,-0.584827952229518,-0.589537596463867));
#59985=DIRECTION('ref_axis',(-0.72286601362311,-0.00784651557417456,0.690943672481324));
#59986=DIRECTION('center_axis',(-0.58224859407526,-0.584827952229825,-0.564767953223315));
#59987=DIRECTION('ref_axis',(-0.712405207463399,0.0322834340840874,0.701025392024262));
#59988=DIRECTION('center_axis',(-0.557154995166649,-0.58482795222981,-0.589537596469928));
#59989=DIRECTION('ref_axis',(-0.737393748555925,0.0219588921937242,0.675106115099149));
#59990=DIRECTION('center_axis',(-0.430171690231809,-0.584827952229279,-0.68769803199836));
#59991=DIRECTION('ref_axis',(-0.825877305438824,-0.0526562713780784,0.561385779518564));
#59992=DIRECTION('center_axis',(-0.430171690235322,-0.58482795222936,-0.687698031996093));
#59993=DIRECTION('ref_axis',(-0.838762190057943,-0.0227607290396216,0.544022001156927));
#59994=DIRECTION('center_axis',(-0.399879502055293,-0.584827952228838,-0.70574262314801));
#59995=DIRECTION('ref_axis',(-0.857560051235848,-0.033086909479653,0.513318629065277));
#59996=DIRECTION('center_axis',(-0.430171690229828,-0.584827952229611,-0.687698031999316));
#59997=DIRECTION('ref_axis',(-0.850460690024639,0.00704626725670269,0.525991411375283));
#59998=DIRECTION('center_axis',(-0.399879502057685,-0.584827952229754,-0.705742623145897));
#59999=DIRECTION('ref_axis',(-0.868877614606056,-0.00326197172774871,0.495016212236466));
#60000=DIRECTION('center_axis',(-0.399879502062724,-0.584827952230319,-0.705742623142573));
#60001=DIRECTION('ref_axis',(-0.879014041102351,0.0265489589760492,0.476056160890921));
#60002=DIRECTION('center_axis',(-0.430171690221956,-0.584827952230244,-0.687698032003702));
#60003=DIRECTION('ref_axis',(-0.861024820730134,0.0368858773879713,0.50722351102444));
#60004=DIRECTION('center_axis',(-0.648441583796989,-0.58482795222928,-0.487339490185394));
#60005=DIRECTION('ref_axis',(-0.584689494821897,-0.0273514773918109,0.810795961589228));
#60006=DIRECTION('center_axis',(-0.626650314901459,-0.584827952229821,-0.515058879279423));
#60007=DIRECTION('ref_axis',(-0.613292997182075,-0.0376838387884075,0.788956036735632));
#60008=DIRECTION('center_axis',(0.450804961350449,-0.572651970056101,0.684722285319155));
#60009=DIRECTION('ref_axis',(1.61865499994955E-17,-0.767090570538598,-0.641538819239155));
#60010=DIRECTION('center_axis',(0.767103439114685,-0.398672303296782,0.502605917476567));
#60011=DIRECTION('ref_axis',(0.548042206505212,9.68883205373909E-18,-0.836450679890272));
#60012=DIRECTION('center_axis',(-0.648441583787969,-0.584827952229667,-0.487339490196932));
#60013=DIRECTION('ref_axis',(-0.602211352514835,0.0024618052280988,0.798332904506179));
#60014=DIRECTION('center_axis',(-0.626650314887279,-0.584827952229558,-0.515058879296975));
#60015=DIRECTION('ref_axis',(-0.630567794520706,-0.00784651558099585,0.776094510163891));
#60016=DIRECTION('center_axis',(-0.648441583795828,-0.584827952229534,-0.487339490186635));
#60017=DIRECTION('ref_axis',(-0.618925900421077,0.0322834340867861,0.784785645683918));
#60018=DIRECTION('center_axis',(-0.626650314895806,-0.584827952229403,-0.515058879286777));
#60019=DIRECTION('ref_axis',(-0.646965946188594,0.0219588921995646,0.762202644659322));
#60020=DIRECTION('center_axis',(-0.512971076047556,-0.584827952230014,-0.628360518674639));
#60021=DIRECTION('ref_axis',(-0.749004721174768,-0.0526562713680577,0.66046895819828));
#60022=DIRECTION('center_axis',(-0.512971076038393,-0.584827952229598,-0.628360518682507));
#60023=DIRECTION('ref_axis',(-0.763964263127642,-0.0227607290387081,0.644857002658314));
#60024=DIRECTION('center_axis',(-0.48517933779571,-0.584827952229707,-0.65005944071825));
#60025=DIRECTION('ref_axis',(-0.786462050443622,-0.0330869094583757,0.616751732575197));
#60026=DIRECTION('center_axis',(-0.512971076036445,-0.584827952229604,-0.628360518684092));
#60027=DIRECTION('ref_axis',(-0.777830349046253,0.00704626725964967,0.628434800293785));
#60028=DIRECTION('center_axis',(-0.485179337811888,-0.584827952229374,-0.650059440706475));
#60029=DIRECTION('ref_axis',(-0.79998427252114,-0.00326197169693252,0.600012102594165));
#60030=DIRECTION('center_axis',(-0.485179337790077,-0.584827952229588,-0.650059440722562));
#60031=DIRECTION('ref_axis',(-0.812417094826833,0.0265489589879128,0.58247198800439));
#60032=DIRECTION('center_axis',(-0.512971076046306,-0.584827952229162,-0.628360518676453));
#60033=DIRECTION('ref_axis',(-0.790663420052944,0.0368858774035164,0.611138927117521));
#60034=DIRECTION('center_axis',(0.533068687695702,-0.572651970066448,0.622822202058821));
#60035=DIRECTION('ref_axis',(-4.08993525798431E-16,-0.736133834920939,-0.676836004571707));
#60036=DIRECTION('center_axis',(0.824047824221018,-0.398672303295535,0.402499165193716));
#60037=DIRECTION('ref_axis',(0.438885661586792,-5.28466665497678E-17,-0.898542918314715));
#60038=DIRECTION('center_axis',(-0.704408262376733,-0.584827952229495,-0.402225392269618));
#60039=DIRECTION('ref_axis',(-0.478459363891251,-0.027351477390948,0.877683618275579));
#60040=DIRECTION('center_axis',(-0.686262984817355,-0.58482795222998,-0.432457375888148));
#60041=DIRECTION('ref_axis',(-0.509574587487999,-0.0376838387835741,0.859600877198813));
#60042=DIRECTION('center_axis',(-0.704408262374728,-0.584827952229583,-0.402225392273001));
#60043=DIRECTION('ref_axis',(-0.497405091738635,0.00246180523382742,0.867514907207634));
#60044=DIRECTION('center_axis',(-0.686262984804124,-0.584827952229589,-0.432457375909674));
#60045=DIRECTION('ref_axis',(-0.52832514460542,-0.00784651557794266,0.849005873814161));
#60046=DIRECTION('center_axis',(-0.704408262374556,-0.584827952229765,-0.402225392273037));
#60047=DIRECTION('ref_axis',(-0.515685762205737,0.0322834340851159,0.856169360898859));
#60048=DIRECTION('center_axis',(-0.686262984807675,-0.584827952229569,-0.432457375904064));
#60049=DIRECTION('ref_axis',(-0.546335104378128,0.0219588921989141,0.837278783188453));
#60050=DIRECTION('center_axis',(-0.587680601548565,-0.584827952230265,-0.559113384613239));
#60051=DIRECTION('ref_axis',(-0.660319885028862,-0.0526562713654081,0.749136146852736));
#60052=DIRECTION('center_axis',(-0.587680601532822,-0.58482795222935,-0.559113384630743));
#60053=DIRECTION('ref_axis',(-0.677118163401999,-0.0227607290428999,0.735522224004509));
#60054=DIRECTION('center_axis',(-0.56282760550518,-0.584827952229442,-0.584124432610402));
#60055=DIRECTION('ref_axis',(-0.702961073329084,-0.033086909466746,0.710458292798361));
#60056=DIRECTION('center_axis',(-0.587680601533554,-0.58482795222962,-0.559113384629692));
#60057=DIRECTION('ref_axis',(-0.692933158813929,0.00704626725769116,0.720967396997869));
#60058=DIRECTION('center_axis',(-0.562827605502354,-0.584827952229588,-0.584124432612979));
#60059=DIRECTION('ref_axis',(-0.718474700614503,-0.0032619717187004,0.695545443603368));
#60060=DIRECTION('center_axis',(-0.562827605517478,-0.584827952229182,-0.584124432598812));
#60061=DIRECTION('ref_axis',(-0.733007845654138,0.0265489589933554,0.679701883906355));
#60062=DIRECTION('center_axis',(-0.587680601554992,-0.584827952228574,-0.559113384608252));
#60063=DIRECTION('ref_axis',(-0.707832784924696,0.0368858774120165,0.705416317243438));
#60064=DIRECTION('center_axis',(0.60692560239257,-0.572651970058496,0.551099840635561));
#60065=DIRECTION('ref_axis',(0.686271561903148,0.727345408539171,-3.55494846067791E-17));
#60066=DIRECTION('center_axis',(0.867996482877091,-0.398672303294177,0.296044760634463));
#60067=DIRECTION('ref_axis',(0.417381833065828,0.908731206367763,3.03903854002256E-16));
#60068=DIRECTION('center_axis',(-0.749266001865758,-0.584827952229527,-0.3107679596405));
#60069=DIRECTION('ref_axis',(-0.364683642974061,-0.0273514773913525,0.930729679999342));
#60070=DIRECTION('center_axis',(-0.73505287749892,-0.5848279522297,-0.343035761359327));
#60071=DIRECTION('ref_axis',(-0.397819882158354,-0.0376838387908347,0.916689298319501));
#60072=DIRECTION('center_axis',(-0.74926600186879,-0.584827952229442,-0.31076795963335));
#60073=DIRECTION('ref_axis',(-0.38475445552896,0.00246180524003201,0.923015681592449));
#60074=DIRECTION('center_axis',(-0.735052877495005,-0.584827952229528,-0.343035761368011));
#60075=DIRECTION('ref_axis',(-0.417750490545346,-0.00784651710898623,0.908527908112008));
#60076=DIRECTION('center_axis',(-0.74926600186846,-0.584827952229323,-0.31076795963437));
#60077=DIRECTION('ref_axis',(-0.404312951455422,0.0322834340908156,0.91405077384613));
#60078=DIRECTION('center_axis',(-0.735052877496047,-0.584827952229571,-0.343035761365705));
#60079=DIRECTION('ref_axis',(-0.437088231606847,0.0219588921987504,0.89915053514092));
#60080=DIRECTION('center_axis',(-0.653122052884241,-0.584827952229301,-0.481048698498975));
#60081=DIRECTION('ref_axis',(-0.561221409856519,-0.0526562713777249,0.825989010945821));
#60082=DIRECTION('center_axis',(-0.653122052875048,-0.584827952229324,-0.481048698511428));
#60083=DIRECTION('ref_axis',(-0.57959350575428,-0.0227607290501129,0.814587820496091));
#60084=DIRECTION('center_axis',(-0.631599745679082,-0.584827952229646,-0.508977433241395));
#60085=DIRECTION('ref_axis',(-0.608373980143524,-0.0330869094586271,0.792960501353506));
#60086=DIRECTION('center_axis',(-0.653122052875627,-0.584827952229884,-0.481048698509961));
#60087=DIRECTION('ref_axis',(-0.597107998736065,0.0070462672503748,0.802129907161706));
#60088=DIRECTION('center_axis',(-0.631599745672695,-0.584827952229487,-0.508977433249503));
#60089=DIRECTION('ref_axis',(-0.62563435345937,-0.00326197171456914,0.780109617497445));
#60090=DIRECTION('center_axis',(-0.631599745668354,-0.584827952229863,-0.508977433254457));
#60091=DIRECTION('ref_axis',(-0.642038624895127,0.0265489589821433,0.766212475048363));
#60092=DIRECTION('center_axis',(-0.653122052893968,-0.584827952229045,-0.481048698486079));
#60093=DIRECTION('ref_axis',(-0.613839203955641,0.0368858774042529,0.788568870635421));
#60094=DIRECTION('center_axis',(0.67121093778181,-0.572651970054142,0.470686305510552));
#60095=DIRECTION('ref_axis',(0.649044045242262,0.760750831307834,-7.92593106383196E-16));
#60096=DIRECTION('center_axis',(0.898256318482264,-0.398672303292889,0.184921553351231));
#60097=DIRECTION('ref_axis',(0.405668756739668,0.914020163784854,4.40549150587367E-17));
#60098=DIRECTION('center_axis',(-0.782307368915369,-0.584827952229426,-0.214409530646024));
#60099=DIRECTION('ref_axis',(-0.245156643157368,-0.0273514773927631,0.969097578678352));
#60100=DIRECTION('center_axis',(-0.772250547206547,-0.584827952229391,-0.248204267953567));
#60101=DIRECTION('ref_axis',(-0.279791319640618,-0.0376838387967089,0.959320981604856));
#60102=DIRECTION('center_axis',(-0.782307368914677,-0.584827952229587,-0.214409530648112));
#60103=DIRECTION('ref_axis',(-0.266036011731999,0.00246180523244144,0.963959947288646));
#60104=DIRECTION('center_axis',(-0.772250547207055,-0.584827952229545,-0.248204267951624));
#60105=DIRECTION('ref_axis',(-0.300587663701301,-0.00784651557541538,0.953721913675007));
#60106=DIRECTION('center_axis',(-0.782307368917322,-0.584827952229332,-0.214409530639156));
#60107=DIRECTION('ref_axis',(-0.286563883944476,0.0322834340891994,0.957517060057974));
#60108=DIRECTION('center_axis',(-0.772250547207065,-0.584827952229574,-0.248204267951522));
#60109=DIRECTION('ref_axis',(-0.320948216319338,0.0219588921977076,0.946842146027988));
#60110=DIRECTION('center_axis',(-0.708263379304496,-0.58482795222933,-0.395397587027824));
#60111=DIRECTION('ref_axis',(-0.453272137779791,-0.0526562713770493,0.889815534926877));
#60112=DIRECTION('center_axis',(-0.708263379298612,-0.584827952229271,-0.395397587038451));
#60113=DIRECTION('ref_axis',(-0.472928312276866,-0.0227607290478678,0.880806880456871));
#60114=DIRECTION('center_axis',(-0.690411180541906,-0.584827952229035,-0.425803555732365));
#60115=DIRECTION('ref_axis',(-0.504192465890993,-0.0330869094722355,0.862957249091944));
#60116=DIRECTION('center_axis',(-0.708263379302418,-0.584827952229702,-0.395397587030994));
#60117=DIRECTION('ref_axis',(-0.491866088807356,0.00704626725721685,0.870642349532283));
#60118=DIRECTION('center_axis',(-0.690411180544678,-0.584827952229611,-0.42580355572708));
#60119=DIRECTION('ref_axis',(-0.522927378824416,-0.00326197171863667,0.852370996700576));
#60120=DIRECTION('center_axis',(-0.690411180551283,-0.584827952229555,-0.425803555716447));
#60121=DIRECTION('ref_axis',(-0.540944071467078,0.0265489589886524,0.840639437762255));
#60122=DIRECTION('center_axis',(-0.708263379298778,-0.58482795223008,-0.395397587036955));
#60123=DIRECTION('ref_axis',(-0.510165012061082,0.0368858773894978,0.859285221866362));
#60124=DIRECTION('center_axis',(0.724910875721522,-0.572651970049502,0.38284976617347));
#60125=DIRECTION('ref_axis',(0.619880264804866,0.784696410916635,-2.87690912095748E-16));
#60126=DIRECTION('center_axis',(0.914350115353379,-0.398672303289966,0.0708820227048915));
#60127=DIRECTION('ref_axis',(0.399677609953492,0.916655774051451,9.93161652328719E-17));
#60128=DIRECTION('center_axis',(-0.803011281431714,-0.5848279522296,-0.114669735258827));
#60129=DIRECTION('ref_axis',(-0.12176337661821,-0.0273514773873073,0.992182229632875));
#60130=DIRECTION('center_axis',(-0.797269364471594,-0.584827952229905,-0.149458444945867));
#60131=DIRECTION('ref_axis',(-0.157350280851449,-0.0376838387869603,0.986823599945932));
#60132=DIRECTION('center_axis',(-0.803011281430099,-0.584827952229649,-0.114669735269889));
#60133=DIRECTION('ref_axis',(-0.143122021097682,0.00246180523301818,0.989701988778395));
#60134=DIRECTION('center_axis',(-0.79726936446997,-0.584827952229467,-0.149458444956243));
#60135=DIRECTION('ref_axis',(-0.178684388826315,-0.00784651557285187,0.983875155384631));
#60136=DIRECTION('center_axis',(-0.803011281431542,-0.584827952229375,-0.114669735261181));
#60137=DIRECTION('ref_axis',(-0.164295532796555,0.0322834340889757,0.985882730240529));
#60138=DIRECTION('center_axis',(-0.797269364469036,-0.58482795222959,-0.149458444960745));
#60139=DIRECTION('ref_axis',(-0.199746655934583,0.0219588921973963,0.979601490656488));
#60140=DIRECTION('center_axis',(-0.75223496913832,-0.584827952229617,-0.303510819405804));
#60141=DIRECTION('ref_axis',(-0.338174493315121,-0.0526562713737487,0.939609136373245));
#60142=DIRECTION('center_axis',(-0.752234969135657,-0.584827952229478,-0.303510819412674));
#60143=DIRECTION('ref_axis',(-0.35880475679657,-0.0227607290416326,0.933135089745128));
#60144=DIRECTION('center_axis',(-0.738334418673682,-0.584827952229299,-0.335914501760613));
#60145=DIRECTION('ref_axis',(-0.392059535240024,-0.0330869094679849,0.919344645521598));
#60146=DIRECTION('center_axis',(-0.752234969136256,-0.584827952229545,-0.303510819411061));
#60147=DIRECTION('ref_axis',(-0.378867156835913,0.00704626725925369,0.925424241950027));
#60148=DIRECTION('center_axis',(-0.738334418678639,-0.584827952229531,-0.335914501749314));
#60149=DIRECTION('ref_axis',(-0.411973527028004,-0.00326197171058358,0.911189976112921));
#60150=DIRECTION('center_axis',(-0.738334418681027,-0.584827952229172,-0.335914501744689));
#60151=DIRECTION('ref_axis',(-0.431318506889835,0.0265489589925769,0.901809014365422));
#60152=DIRECTION('center_axis',(-0.752234969138981,-0.58482795222936,-0.303510819404664));
#60153=DIRECTION('ref_axis',(-0.398445213138042,0.0368858773996949,0.916450131854339));
#60154=DIRECTION('center_axis',(0.767178536111651,-0.572651970044602,0.288975457320548));
#60155=DIRECTION('ref_axis',(0.598172081248193,0.801367681663795,-4.17053780108495E-16));
#60156=DIRECTION('center_axis',(0.916024064699777,-0.398672303285569,-0.0442753597825917));
#60157=DIRECTION('ref_axis',(0.399063638883099,0.916923231312949,8.19224667888075E-18));
#60158=DIRECTION('center_axis',(-0.811051226341668,-0.584827952229427,-0.0131215296673966));
#60159=DIRECTION('ref_axis',(0.0035501710909852,-0.0273514773944228,0.99961957412286));
#60160=DIRECTION('center_axis',(-0.809714767588102,-0.58482795222959,-0.0483555730055123));
#60161=DIRECTION('ref_axis',(-0.0324277341580232,-0.0376838387929533,0.998763420611309));
#60162=DIRECTION('center_axis',(-0.811051226342032,-0.584827952229353,-0.0131215296481657));
#60163=DIRECTION('ref_axis',(-0.0179509106794282,0.00246180524443599,0.99983583868589));
#60164=DIRECTION('center_axis',(-0.809714767588315,-0.584827952229458,-0.0483555730035268));
#60165=DIRECTION('ref_axis',(-0.0539631543998079,-0.00784651557187224,0.99851209815435));
#60166=DIRECTION('center_axis',(-0.811051226341268,-0.584827952229893,-0.0131215296713105));
#60167=DIRECTION('ref_axis',(-0.0394361429627812,0.0322834340818623,0.998700440829031));
#60168=DIRECTION('center_axis',(-0.809714767588765,-0.58482795222925,-0.0483555729985027));
#60169=DIRECTION('ref_axis',(-0.0753949714532756,0.0219588922048596,0.996911934592367));
#60170=DIRECTION('center_axis',(-0.784343364140843,-0.584827952229176,-0.206837504867116));
#60171=DIRECTION('ref_axis',(-0.217743635086438,-0.0526562713790471,0.974584540439566));
#60172=DIRECTION('center_axis',(-0.784343364142726,-0.58482795222944,-0.206837504859228));
#60173=DIRECTION('ref_axis',(-0.239022635964213,-0.0227607290381041,0.970747201237466));
#60174=DIRECTION('center_axis',(-0.7746136819609,-0.584827952229385,-0.240727875432328));
#60175=DIRECTION('ref_axis',(-0.273743591514971,-0.0330869094649303,0.961233427699299));
#60176=DIRECTION('center_axis',(-0.784343364141514,-0.58482795222953,-0.20683750486357));
#60177=DIRECTION('ref_axis',(-0.259893263479541,0.00704626725925445,0.96561164124904));
#60178=DIRECTION('center_axis',(-0.774613681957867,-0.584827952229589,-0.240727875441592));
#60179=DIRECTION('ref_axis',(-0.29452260663248,-0.00326197172036406,0.955638945273216));
#60180=DIRECTION('center_axis',(-0.774613681963109,-0.584827952229387,-0.240727875425216));
#60181=DIRECTION('ref_axis',(-0.314890791810213,0.0265489589893783,0.948756524093362));
#60182=DIRECTION('center_axis',(-0.784343364140797,-0.584827952229724,-0.206837504865741));
#60183=DIRECTION('ref_axis',(-0.280441695204173,0.0368858773946116,0.959162075793158));
#60184=DIRECTION('center_axis',(0.797347332705084,-0.572651970025819,0.190543832893213));
#60185=DIRECTION('ref_axis',(0.583339514902054,0.812228422522775,1.92994765983885E-17));
#60186=DIRECTION('center_axis',(0.903251767338709,-0.398672303283214,-0.158734493398112));
#60187=DIRECTION('ref_axis',(0.40379185681366,0.91485088204088,-1.37857755134463E-16));
#60188=DIRECTION('center_axis',(-0.806300408914473,-0.584827952229552,0.0886336103029912));
#60189=DIRECTION('ref_axis',(0.128807730495229,-0.0273514773905314,0.991292320785965));
#60190=DIRECTION('center_axis',(-0.809390485121178,-0.584827952229607,0.0535098952178855));
#60191=DIRECTION('ref_axis',(0.0930062172828468,-0.0376838387925279,0.994952145502785));
#60192=DIRECTION('center_axis',(-0.806300408913409,-0.584827952229407,0.0886336103136302));
#60193=DIRECTION('ref_axis',(0.107503296306928,0.0024618052430626,0.99420168014246));
#60194=DIRECTION('center_axis',(-0.809390485121514,-0.584827952229481,0.0535098952141856));
#60195=DIRECTION('ref_axis',(0.0716091112012576,-0.00784651557490987,0.997401908653828));
#60196=DIRECTION('center_axis',(-0.806300408914069,-0.584827952229266,0.0886336103085555));
#60197=DIRECTION('ref_axis',(0.0860451784273227,0.0322834340909248,0.995768048871175));
#60198=DIRECTION('center_axis',(-0.809390485121174,-0.58482795222938,0.0535098952204267));
#60199=DIRECTION('ref_axis',(0.0501457366864746,0.0219588922963099,0.998500481793219));
#60200=DIRECTION('center_axis',(-0.804082195749635,-0.584827952229121,-0.106902239312084));
#60201=DIRECTION('ref_axis',(-0.093878829653998,-0.0526562713806529,0.994190164117048));
#60202=DIRECTION('center_axis',(-0.804082195750617,-0.584827952229495,-0.10690223930266));
#60203=DIRECTION('ref_axis',(-0.115470985383714,-0.0227607290386235,0.993050049467873));
#60204=DIRECTION('center_axis',(-0.798676824748701,-0.584827952229234,-0.141744826715803));
#60205=DIRECTION('ref_axis',(-0.15111054783433,-0.0330869094686492,0.987962984506516));
#60206=DIRECTION('center_axis',(-0.804082195750302,-0.584827952229587,-0.106902239304525));
#60207=DIRECTION('ref_axis',(-0.136820698104582,0.00704626726004378,0.990570768137176));
#60208=DIRECTION('center_axis',(-0.798676824749339,-0.584827952229491,-0.14174482671115));
#60209=DIRECTION('ref_axis',(-0.172426888771917,-0.0032619717161641,0.985016917402417));
#60210=DIRECTION('center_axis',(-0.798676824749257,-0.584827952229734,-0.141744826710606));
#60211=DIRECTION('ref_axis',(-0.193497060841072,0.0265489589847928,0.980741576676899));
#60212=DIRECTION('center_axis',(-0.804082195752222,-0.584827952229105,-0.10690223929272));
#60213=DIRECTION('ref_axis',(-0.158015444189677,0.0368858774036313,0.986747460825567));
#60214=DIRECTION('axis',(0.,0.,1.));
#60215=DIRECTION('refdir',(1.,0.,0.));
#60216=DIRECTION('center_axis',(1.,0.,0.));
#60217=DIRECTION('ref_axis',(0.,0.,-1.));
#60218=DIRECTION('center_axis',(1.,0.,0.));
#60219=DIRECTION('ref_axis',(0.,0.,-1.));
#60220=DIRECTION('',(1.,0.,0.));
#60221=DIRECTION('center_axis',(1.,0.,0.));
#60222=DIRECTION('ref_axis',(0.,0.,-1.));
#60223=DIRECTION('center_axis',(-1.,0.,0.));
#60224=DIRECTION('ref_axis',(0.,0.,1.));
#60225=DIRECTION('center_axis',(1.,0.,0.));
#60226=DIRECTION('ref_axis',(0.,0.,-1.));
#60227=DIRECTION('',(1.,0.,0.));
#60228=DIRECTION('center_axis',(1.,0.,0.));
#60229=DIRECTION('ref_axis',(0.,0.,-1.));
#60230=DIRECTION('center_axis',(-1.,0.,0.));
#60231=DIRECTION('ref_axis',(0.,0.,1.));
#60232=DIRECTION('center_axis',(1.,0.,0.));
#60233=DIRECTION('ref_axis',(0.,0.,-1.));
#60234=DIRECTION('',(1.,0.,0.));
#60235=DIRECTION('center_axis',(1.,0.,0.));
#60236=DIRECTION('ref_axis',(0.,0.,-1.));
#60237=DIRECTION('center_axis',(1.,0.,0.));
#60238=DIRECTION('ref_axis',(0.,1.,0.));
#60239=DIRECTION('center_axis',(1.,0.,0.));
#60240=DIRECTION('ref_axis',(0.,1.,0.));
#60241=DIRECTION('center_axis',(1.,0.,0.));
#60242=DIRECTION('ref_axis',(0.,1.,0.));
#60243=DIRECTION('axis',(0.,0.,1.));
#60244=DIRECTION('refdir',(1.,0.,0.));
#60245=DIRECTION('center_axis',(1.,0.,0.));
#60246=DIRECTION('ref_axis',(0.,0.,-1.));
#60247=DIRECTION('center_axis',(1.,0.,0.));
#60248=DIRECTION('ref_axis',(0.,0.,-1.));
#60249=DIRECTION('',(1.,0.,0.));
#60250=DIRECTION('center_axis',(1.,0.,0.));
#60251=DIRECTION('ref_axis',(0.,0.,-1.));
#60252=DIRECTION('center_axis',(-1.,0.,0.));
#60253=DIRECTION('ref_axis',(0.,0.,1.));
#60254=DIRECTION('center_axis',(1.,0.,0.));
#60255=DIRECTION('ref_axis',(0.,0.,-1.));
#60256=DIRECTION('',(1.,0.,0.));
#60257=DIRECTION('center_axis',(1.,0.,0.));
#60258=DIRECTION('ref_axis',(0.,0.,-1.));
#60259=DIRECTION('center_axis',(1.,0.,0.));
#60260=DIRECTION('ref_axis',(0.,1.,0.));
#60261=DIRECTION('center_axis',(1.,0.,0.));
#60262=DIRECTION('ref_axis',(0.,1.,0.));
#60263=DIRECTION('axis',(0.,0.,1.));
#60264=DIRECTION('refdir',(1.,0.,0.));
#60265=DIRECTION('center_axis',(0.,0.,1.));
#60266=DIRECTION('ref_axis',(1.,0.,0.));
#60267=DIRECTION('center_axis',(0.,0.,-1.));
#60268=DIRECTION('ref_axis',(-1.,0.,0.));
#60269=DIRECTION('',(0.,0.,-1.));
#60270=DIRECTION('center_axis',(0.,0.,-1.));
#60271=DIRECTION('ref_axis',(-1.,0.,0.));
#60272=DIRECTION('center_axis',(0.,0.,-1.));
#60273=DIRECTION('ref_axis',(-1.,0.,0.));
#60274=DIRECTION('center_axis',(0.,0.,1.));
#60275=DIRECTION('ref_axis',(1.,0.,0.));
#60276=DIRECTION('',(0.,0.,1.));
#60277=DIRECTION('center_axis',(0.,0.,1.));
#60278=DIRECTION('ref_axis',(1.,0.,0.));
#60279=DIRECTION('center_axis',(0.,0.,1.));
#60280=DIRECTION('ref_axis',(1.,0.,0.));
#60281=DIRECTION('center_axis',(0.,0.,1.));
#60282=DIRECTION('ref_axis',(1.,0.,0.));
#60283=DIRECTION('',(0.,0.,1.));
#60284=DIRECTION('center_axis',(0.,0.,1.));
#60285=DIRECTION('ref_axis',(1.,0.,0.));
#60286=DIRECTION('center_axis',(0.,0.,-1.));
#60287=DIRECTION('ref_axis',(-1.,0.,0.));
#60288=DIRECTION('center_axis',(0.,0.,-1.));
#60289=DIRECTION('ref_axis',(-1.,0.,0.));
#60290=DIRECTION('',(0.,0.,-1.));
#60291=DIRECTION('center_axis',(0.,0.,-1.));
#60292=DIRECTION('ref_axis',(-1.,0.,0.));
#60293=DIRECTION('center_axis',(0.,0.,-1.));
#60294=DIRECTION('ref_axis',(-1.,0.,0.));
#60295=DIRECTION('',(0.,0.,-1.));
#60296=DIRECTION('center_axis',(0.,0.,-1.));
#60297=DIRECTION('ref_axis',(-1.,0.,0.));
#60298=DIRECTION('',(0.,0.,-1.));
#60299=DIRECTION('center_axis',(0.,0.,-1.));
#60300=DIRECTION('ref_axis',(-1.,0.,0.));
#60301=DIRECTION('center_axis',(0.,0.,-1.));
#60302=DIRECTION('ref_axis',(-1.,0.,0.));
#60303=DIRECTION('',(0.,0.,-1.));
#60304=DIRECTION('center_axis',(0.,0.,-1.));
#60305=DIRECTION('ref_axis',(-1.,0.,0.));
#60306=DIRECTION('',(0.,0.,-1.));
#60307=DIRECTION('center_axis',(0.,0.,-1.));
#60308=DIRECTION('ref_axis',(-1.,0.,0.));
#60309=DIRECTION('center_axis',(0.,0.,-1.));
#60310=DIRECTION('ref_axis',(-1.,0.,0.));
#60311=DIRECTION('',(0.,0.,-1.));
#60312=DIRECTION('center_axis',(0.,0.,-1.));
#60313=DIRECTION('ref_axis',(-1.,0.,0.));
#60314=DIRECTION('',(0.,0.,-1.));
#60315=DIRECTION('center_axis',(0.,0.,-1.));
#60316=DIRECTION('ref_axis',(-1.,0.,0.));
#60317=DIRECTION('center_axis',(0.,0.,-1.));
#60318=DIRECTION('ref_axis',(-1.,0.,0.));
#60319=DIRECTION('',(0.,0.,-1.));
#60320=DIRECTION('center_axis',(0.,0.,-1.));
#60321=DIRECTION('ref_axis',(-1.,0.,0.));
#60322=DIRECTION('',(0.,0.,-1.));
#60323=DIRECTION('center_axis',(0.,0.,-1.));
#60324=DIRECTION('ref_axis',(-1.,0.,0.));
#60325=DIRECTION('center_axis',(0.,0.,-1.));
#60326=DIRECTION('ref_axis',(-1.,0.,0.));
#60327=DIRECTION('',(0.,0.,-1.));
#60328=DIRECTION('center_axis',(0.,0.,-1.));
#60329=DIRECTION('ref_axis',(-1.,0.,0.));
#60330=DIRECTION('',(0.,0.,-1.));
#60331=DIRECTION('center_axis',(0.,0.,-1.));
#60332=DIRECTION('ref_axis',(-1.,0.,0.));
#60333=DIRECTION('center_axis',(0.,0.,-1.));
#60334=DIRECTION('ref_axis',(-1.,0.,0.));
#60335=DIRECTION('',(0.,0.,-1.));
#60336=DIRECTION('center_axis',(0.,0.,-1.));
#60337=DIRECTION('ref_axis',(-1.,0.,0.));
#60338=DIRECTION('',(0.,0.,-1.));
#60339=DIRECTION('center_axis',(0.,0.,-1.));
#60340=DIRECTION('ref_axis',(-1.,0.,0.));
#60341=DIRECTION('center_axis',(0.,0.,-1.));
#60342=DIRECTION('ref_axis',(-1.,0.,0.));
#60343=DIRECTION('',(0.,0.,-1.));
#60344=DIRECTION('center_axis',(0.,0.,-1.));
#60345=DIRECTION('ref_axis',(-1.,0.,0.));
#60346=DIRECTION('',(0.,0.,-1.));
#60347=DIRECTION('center_axis',(0.,0.,-1.));
#60348=DIRECTION('ref_axis',(-1.,0.,0.));
#60349=DIRECTION('center_axis',(0.,0.,-1.));
#60350=DIRECTION('ref_axis',(-1.,0.,0.));
#60351=DIRECTION('',(0.,0.,-1.));
#60352=DIRECTION('center_axis',(0.,0.,-1.));
#60353=DIRECTION('ref_axis',(-1.,0.,0.));
#60354=DIRECTION('',(0.,0.,-1.));
#60355=DIRECTION('center_axis',(0.,0.,-1.));
#60356=DIRECTION('ref_axis',(-1.,0.,0.));
#60357=DIRECTION('center_axis',(0.,0.,-1.));
#60358=DIRECTION('ref_axis',(-1.,0.,0.));
#60359=DIRECTION('',(0.,0.,-1.));
#60360=DIRECTION('center_axis',(0.,0.,-1.));
#60361=DIRECTION('ref_axis',(-1.,0.,0.));
#60362=DIRECTION('',(0.,0.,-1.));
#60363=DIRECTION('center_axis',(0.,0.,-1.));
#60364=DIRECTION('ref_axis',(-1.,0.,0.));
#60365=DIRECTION('center_axis',(0.,0.,-1.));
#60366=DIRECTION('ref_axis',(-1.,0.,0.));
#60367=DIRECTION('',(0.,0.,-1.));
#60368=DIRECTION('center_axis',(0.,0.,-1.));
#60369=DIRECTION('ref_axis',(-1.,0.,0.));
#60370=DIRECTION('',(0.,0.,-1.));
#60371=DIRECTION('center_axis',(0.,0.,-1.));
#60372=DIRECTION('ref_axis',(-1.,0.,0.));
#60373=DIRECTION('center_axis',(0.,0.,-1.));
#60374=DIRECTION('ref_axis',(-1.,0.,0.));
#60375=DIRECTION('',(0.,0.,-1.));
#60376=DIRECTION('center_axis',(0.,0.,-1.));
#60377=DIRECTION('ref_axis',(-1.,0.,0.));
#60378=DIRECTION('',(0.,0.,-1.));
#60379=DIRECTION('center_axis',(0.,0.,-1.));
#60380=DIRECTION('ref_axis',(-1.,0.,0.));
#60381=DIRECTION('center_axis',(0.,0.,-1.));
#60382=DIRECTION('ref_axis',(-1.,0.,0.));
#60383=DIRECTION('',(0.,0.,-1.));
#60384=DIRECTION('center_axis',(0.,0.,-1.));
#60385=DIRECTION('ref_axis',(-1.,0.,0.));
#60386=DIRECTION('',(0.,0.,-1.));
#60387=DIRECTION('center_axis',(0.,0.,-1.));
#60388=DIRECTION('ref_axis',(-1.,0.,0.));
#60389=DIRECTION('center_axis',(0.,0.,-1.));
#60390=DIRECTION('ref_axis',(-1.,0.,0.));
#60391=DIRECTION('',(0.,0.,-1.));
#60392=DIRECTION('center_axis',(0.,0.,-1.));
#60393=DIRECTION('ref_axis',(-1.,0.,0.));
#60394=DIRECTION('',(0.,0.,-1.));
#60395=DIRECTION('center_axis',(0.,0.,-1.));
#60396=DIRECTION('ref_axis',(-1.,0.,0.));
#60397=DIRECTION('center_axis',(0.,0.,-1.));
#60398=DIRECTION('ref_axis',(-1.,0.,0.));
#60399=DIRECTION('',(0.,0.,-1.));
#60400=DIRECTION('center_axis',(0.,0.,-1.));
#60401=DIRECTION('ref_axis',(-1.,0.,0.));
#60402=DIRECTION('',(0.,0.,-1.));
#60403=DIRECTION('center_axis',(0.,0.,-1.));
#60404=DIRECTION('ref_axis',(-1.,0.,0.));
#60405=DIRECTION('center_axis',(0.,0.,-1.));
#60406=DIRECTION('ref_axis',(-1.,0.,0.));
#60407=DIRECTION('',(0.,0.,-1.));
#60408=DIRECTION('center_axis',(0.,0.,-1.));
#60409=DIRECTION('ref_axis',(-1.,0.,0.));
#60410=DIRECTION('',(0.,0.,-1.));
#60411=DIRECTION('center_axis',(0.,0.,-1.));
#60412=DIRECTION('ref_axis',(-1.,0.,0.));
#60413=DIRECTION('center_axis',(0.,0.,-1.));
#60414=DIRECTION('ref_axis',(-1.,0.,0.));
#60415=DIRECTION('',(0.,0.,-1.));
#60416=DIRECTION('center_axis',(0.,0.,-1.));
#60417=DIRECTION('ref_axis',(-1.,0.,0.));
#60418=DIRECTION('',(0.,0.,-1.));
#60419=DIRECTION('center_axis',(0.,0.,-1.));
#60420=DIRECTION('ref_axis',(-1.,0.,0.));
#60421=DIRECTION('center_axis',(0.,0.,-1.));
#60422=DIRECTION('ref_axis',(-1.,0.,0.));
#60423=DIRECTION('',(0.,0.,-1.));
#60424=DIRECTION('center_axis',(0.,0.,-1.));
#60425=DIRECTION('ref_axis',(-1.,0.,0.));
#60426=DIRECTION('',(0.,0.,-1.));
#60427=DIRECTION('center_axis',(0.,0.,-1.));
#60428=DIRECTION('ref_axis',(-1.,0.,0.));
#60429=DIRECTION('center_axis',(0.,0.,-1.));
#60430=DIRECTION('ref_axis',(-1.,0.,0.));
#60431=DIRECTION('',(0.,0.,-1.));
#60432=DIRECTION('center_axis',(0.,0.,-1.));
#60433=DIRECTION('ref_axis',(-1.,0.,0.));
#60434=DIRECTION('',(0.,0.,-1.));
#60435=DIRECTION('center_axis',(0.,0.,-1.));
#60436=DIRECTION('ref_axis',(-1.,0.,0.));
#60437=DIRECTION('center_axis',(0.,0.,-1.));
#60438=DIRECTION('ref_axis',(-1.,0.,0.));
#60439=DIRECTION('',(0.,0.,-1.));
#60440=DIRECTION('center_axis',(0.,0.,-1.));
#60441=DIRECTION('ref_axis',(-1.,0.,0.));
#60442=DIRECTION('',(0.,0.,-1.));
#60443=DIRECTION('center_axis',(0.,0.,-1.));
#60444=DIRECTION('ref_axis',(-1.,0.,0.));
#60445=DIRECTION('center_axis',(0.,0.,-1.));
#60446=DIRECTION('ref_axis',(-1.,0.,0.));
#60447=DIRECTION('',(0.,0.,-1.));
#60448=DIRECTION('center_axis',(0.,0.,-1.));
#60449=DIRECTION('ref_axis',(-1.,0.,0.));
#60450=DIRECTION('',(0.,0.,-1.));
#60451=DIRECTION('center_axis',(0.,0.,-1.));
#60452=DIRECTION('ref_axis',(-1.,0.,0.));
#60453=DIRECTION('center_axis',(0.,0.,-1.));
#60454=DIRECTION('ref_axis',(-1.,0.,0.));
#60455=DIRECTION('',(0.,0.,-1.));
#60456=DIRECTION('center_axis',(0.,0.,-1.));
#60457=DIRECTION('ref_axis',(-1.,0.,0.));
#60458=DIRECTION('',(0.,0.,-1.));
#60459=DIRECTION('center_axis',(0.,0.,-1.));
#60460=DIRECTION('ref_axis',(-1.,0.,0.));
#60461=DIRECTION('center_axis',(0.,0.,-1.));
#60462=DIRECTION('ref_axis',(-1.,0.,0.));
#60463=DIRECTION('',(0.,0.,-1.));
#60464=DIRECTION('center_axis',(0.,0.,-1.));
#60465=DIRECTION('ref_axis',(-1.,0.,0.));
#60466=DIRECTION('',(0.,0.,-1.));
#60467=DIRECTION('center_axis',(0.,0.,-1.));
#60468=DIRECTION('ref_axis',(-1.,0.,0.));
#60469=DIRECTION('center_axis',(0.,0.,-1.));
#60470=DIRECTION('ref_axis',(-1.,0.,0.));
#60471=DIRECTION('',(0.,0.,-1.));
#60472=DIRECTION('center_axis',(0.,0.,-1.));
#60473=DIRECTION('ref_axis',(-1.,0.,0.));
#60474=DIRECTION('',(0.,0.,-1.));
#60475=DIRECTION('center_axis',(0.,0.,-1.));
#60476=DIRECTION('ref_axis',(-1.,0.,0.));
#60477=DIRECTION('center_axis',(0.,0.,-1.));
#60478=DIRECTION('ref_axis',(-1.,0.,0.));
#60479=DIRECTION('',(0.,0.,-1.));
#60480=DIRECTION('center_axis',(0.,0.,-1.));
#60481=DIRECTION('ref_axis',(-1.,0.,0.));
#60482=DIRECTION('',(0.,0.,-1.));
#60483=DIRECTION('center_axis',(0.,0.,-1.));
#60484=DIRECTION('ref_axis',(-1.,0.,0.));
#60485=DIRECTION('center_axis',(0.,0.,-1.));
#60486=DIRECTION('ref_axis',(-1.,0.,0.));
#60487=DIRECTION('',(0.,0.,-1.));
#60488=DIRECTION('center_axis',(0.,0.,-1.));
#60489=DIRECTION('ref_axis',(-1.,0.,0.));
#60490=DIRECTION('',(0.,0.,-1.));
#60491=DIRECTION('center_axis',(0.,0.,-1.));
#60492=DIRECTION('ref_axis',(-1.,0.,0.));
#60493=DIRECTION('center_axis',(0.,0.,-1.));
#60494=DIRECTION('ref_axis',(-1.,0.,0.));
#60495=DIRECTION('',(0.,0.,-1.));
#60496=DIRECTION('center_axis',(0.,0.,-1.));
#60497=DIRECTION('ref_axis',(-1.,0.,0.));
#60498=DIRECTION('',(0.,0.,-1.));
#60499=DIRECTION('center_axis',(0.,0.,-1.));
#60500=DIRECTION('ref_axis',(-1.,0.,0.));
#60501=DIRECTION('center_axis',(0.,0.,-1.));
#60502=DIRECTION('ref_axis',(-1.,0.,0.));
#60503=DIRECTION('',(0.,0.,-1.));
#60504=DIRECTION('center_axis',(0.,0.,-1.));
#60505=DIRECTION('ref_axis',(-1.,0.,0.));
#60506=DIRECTION('',(0.,0.,-1.));
#60507=DIRECTION('center_axis',(0.,0.,-1.));
#60508=DIRECTION('ref_axis',(-1.,0.,0.));
#60509=DIRECTION('center_axis',(0.,0.,-1.));
#60510=DIRECTION('ref_axis',(-1.,0.,0.));
#60511=DIRECTION('',(0.,0.,-1.));
#60512=DIRECTION('center_axis',(0.,0.,-1.));
#60513=DIRECTION('ref_axis',(-1.,0.,0.));
#60514=DIRECTION('',(0.,0.,-1.));
#60515=DIRECTION('center_axis',(0.,0.,-1.));
#60516=DIRECTION('ref_axis',(-1.,0.,0.));
#60517=DIRECTION('center_axis',(0.,0.,-1.));
#60518=DIRECTION('ref_axis',(-1.,0.,0.));
#60519=DIRECTION('',(0.,0.,-1.));
#60520=DIRECTION('center_axis',(0.,0.,-1.));
#60521=DIRECTION('ref_axis',(-1.,0.,0.));
#60522=DIRECTION('',(0.,0.,-1.));
#60523=DIRECTION('center_axis',(0.,0.,-1.));
#60524=DIRECTION('ref_axis',(-1.,0.,0.));
#60525=DIRECTION('center_axis',(0.,0.,-1.));
#60526=DIRECTION('ref_axis',(-1.,0.,0.));
#60527=DIRECTION('',(0.,0.,-1.));
#60528=DIRECTION('center_axis',(0.,0.,-1.));
#60529=DIRECTION('ref_axis',(-1.,0.,0.));
#60530=DIRECTION('',(0.,0.,-1.));
#60531=DIRECTION('center_axis',(0.,0.,-1.));
#60532=DIRECTION('ref_axis',(-1.,0.,0.));
#60533=DIRECTION('center_axis',(0.,0.,-1.));
#60534=DIRECTION('ref_axis',(-1.,0.,0.));
#60535=DIRECTION('',(0.,0.,-1.));
#60536=DIRECTION('center_axis',(0.,0.,-1.));
#60537=DIRECTION('ref_axis',(-1.,0.,0.));
#60538=DIRECTION('',(0.,0.,-1.));
#60539=DIRECTION('center_axis',(0.,0.,-1.));
#60540=DIRECTION('ref_axis',(-1.,0.,0.));
#60541=DIRECTION('center_axis',(0.,0.,-1.));
#60542=DIRECTION('ref_axis',(-1.,0.,0.));
#60543=DIRECTION('',(0.,0.,-1.));
#60544=DIRECTION('center_axis',(0.,0.,-1.));
#60545=DIRECTION('ref_axis',(-1.,0.,0.));
#60546=DIRECTION('',(0.,0.,-1.));
#60547=DIRECTION('center_axis',(0.,0.,-1.));
#60548=DIRECTION('ref_axis',(-1.,0.,0.));
#60549=DIRECTION('center_axis',(0.,0.,-1.));
#60550=DIRECTION('ref_axis',(-1.,0.,0.));
#60551=DIRECTION('',(0.,0.,-1.));
#60552=DIRECTION('center_axis',(0.,0.,-1.));
#60553=DIRECTION('ref_axis',(-1.,0.,0.));
#60554=DIRECTION('',(0.,0.,-1.));
#60555=DIRECTION('center_axis',(0.,0.,-1.));
#60556=DIRECTION('ref_axis',(-1.,0.,0.));
#60557=DIRECTION('center_axis',(0.,0.,-1.));
#60558=DIRECTION('ref_axis',(-1.,0.,0.));
#60559=DIRECTION('',(0.,0.,-1.));
#60560=DIRECTION('center_axis',(0.,0.,-1.));
#60561=DIRECTION('ref_axis',(-1.,0.,0.));
#60562=DIRECTION('',(0.,0.,-1.));
#60563=DIRECTION('center_axis',(0.,0.,-1.));
#60564=DIRECTION('ref_axis',(-1.,0.,0.));
#60565=DIRECTION('center_axis',(0.,0.,-1.));
#60566=DIRECTION('ref_axis',(-1.,0.,0.));
#60567=DIRECTION('',(0.,0.,-1.));
#60568=DIRECTION('center_axis',(0.,0.,-1.));
#60569=DIRECTION('ref_axis',(-1.,0.,0.));
#60570=DIRECTION('',(0.,0.,-1.));
#60571=DIRECTION('center_axis',(0.,0.,-1.));
#60572=DIRECTION('ref_axis',(-1.,0.,0.));
#60573=DIRECTION('center_axis',(0.,0.,-1.));
#60574=DIRECTION('ref_axis',(-1.,0.,0.));
#60575=DIRECTION('',(0.,0.,-1.));
#60576=DIRECTION('center_axis',(0.,0.,-1.));
#60577=DIRECTION('ref_axis',(-1.,0.,0.));
#60578=DIRECTION('',(0.,0.,-1.));
#60579=DIRECTION('center_axis',(0.,0.,-1.));
#60580=DIRECTION('ref_axis',(-1.,0.,0.));
#60581=DIRECTION('center_axis',(0.,0.,-1.));
#60582=DIRECTION('ref_axis',(-1.,0.,0.));
#60583=DIRECTION('',(0.,0.,-1.));
#60584=DIRECTION('center_axis',(0.,0.,-1.));
#60585=DIRECTION('ref_axis',(-1.,0.,0.));
#60586=DIRECTION('',(0.,0.,-1.));
#60587=DIRECTION('center_axis',(0.,0.,-1.));
#60588=DIRECTION('ref_axis',(-1.,0.,0.));
#60589=DIRECTION('center_axis',(0.,0.,-1.));
#60590=DIRECTION('ref_axis',(-1.,0.,0.));
#60591=DIRECTION('',(0.,0.,-1.));
#60592=DIRECTION('center_axis',(0.,0.,-1.));
#60593=DIRECTION('ref_axis',(-1.,0.,0.));
#60594=DIRECTION('',(0.,0.,-1.));
#60595=DIRECTION('center_axis',(0.,0.,-1.));
#60596=DIRECTION('ref_axis',(-1.,0.,0.));
#60597=DIRECTION('center_axis',(0.,0.,-1.));
#60598=DIRECTION('ref_axis',(-1.,0.,0.));
#60599=DIRECTION('',(0.,0.,-1.));
#60600=DIRECTION('center_axis',(0.,0.,-1.));
#60601=DIRECTION('ref_axis',(-1.,0.,0.));
#60602=DIRECTION('',(0.,0.,-1.));
#60603=DIRECTION('center_axis',(0.,0.,-1.));
#60604=DIRECTION('ref_axis',(-1.,0.,0.));
#60605=DIRECTION('center_axis',(0.,0.,-1.));
#60606=DIRECTION('ref_axis',(-1.,0.,0.));
#60607=DIRECTION('',(0.,0.,-1.));
#60608=DIRECTION('center_axis',(0.,0.,-1.));
#60609=DIRECTION('ref_axis',(-1.,0.,0.));
#60610=DIRECTION('',(0.,0.,-1.));
#60611=DIRECTION('center_axis',(0.,0.,-1.));
#60612=DIRECTION('ref_axis',(-1.,0.,0.));
#60613=DIRECTION('center_axis',(0.,0.,-1.));
#60614=DIRECTION('ref_axis',(-1.,0.,0.));
#60615=DIRECTION('',(0.,0.,-1.));
#60616=DIRECTION('center_axis',(0.,0.,-1.));
#60617=DIRECTION('ref_axis',(-1.,0.,0.));
#60618=DIRECTION('',(0.,0.,-1.));
#60619=DIRECTION('center_axis',(0.,0.,-1.));
#60620=DIRECTION('ref_axis',(-1.,0.,0.));
#60621=DIRECTION('center_axis',(0.,0.,-1.));
#60622=DIRECTION('ref_axis',(-1.,0.,0.));
#60623=DIRECTION('',(0.,0.,-1.));
#60624=DIRECTION('center_axis',(0.,0.,-1.));
#60625=DIRECTION('ref_axis',(-1.,0.,0.));
#60626=DIRECTION('',(0.,0.,-1.));
#60627=DIRECTION('center_axis',(0.,0.,-1.));
#60628=DIRECTION('ref_axis',(-1.,0.,0.));
#60629=DIRECTION('center_axis',(0.,0.,-1.));
#60630=DIRECTION('ref_axis',(-1.,0.,0.));
#60631=DIRECTION('',(0.,0.,-1.));
#60632=DIRECTION('center_axis',(0.,0.,-1.));
#60633=DIRECTION('ref_axis',(-1.,0.,0.));
#60634=DIRECTION('',(0.,0.,-1.));
#60635=DIRECTION('center_axis',(0.,0.,-1.));
#60636=DIRECTION('ref_axis',(-1.,0.,0.));
#60637=DIRECTION('center_axis',(0.,0.,-1.));
#60638=DIRECTION('ref_axis',(-1.,0.,0.));
#60639=DIRECTION('',(0.,0.,-1.));
#60640=DIRECTION('center_axis',(0.,0.,-1.));
#60641=DIRECTION('ref_axis',(-1.,0.,0.));
#60642=DIRECTION('',(0.,0.,-1.));
#60643=DIRECTION('center_axis',(0.,0.,-1.));
#60644=DIRECTION('ref_axis',(-1.,0.,0.));
#60645=DIRECTION('center_axis',(0.,0.,-1.));
#60646=DIRECTION('ref_axis',(-1.,0.,0.));
#60647=DIRECTION('',(0.,0.,-1.));
#60648=DIRECTION('center_axis',(0.,0.,-1.));
#60649=DIRECTION('ref_axis',(-1.,0.,0.));
#60650=DIRECTION('',(0.,0.,-1.));
#60651=DIRECTION('center_axis',(0.,0.,-1.));
#60652=DIRECTION('ref_axis',(-1.,0.,0.));
#60653=DIRECTION('center_axis',(0.,0.,-1.));
#60654=DIRECTION('ref_axis',(-1.,0.,0.));
#60655=DIRECTION('',(0.,0.,-1.));
#60656=DIRECTION('center_axis',(0.,0.,-1.));
#60657=DIRECTION('ref_axis',(-1.,0.,0.));
#60658=DIRECTION('',(0.,0.,-1.));
#60659=DIRECTION('center_axis',(0.,0.,-1.));
#60660=DIRECTION('ref_axis',(-1.,0.,0.));
#60661=DIRECTION('center_axis',(0.,0.,-1.));
#60662=DIRECTION('ref_axis',(-1.,0.,0.));
#60663=DIRECTION('',(0.,0.,-1.));
#60664=DIRECTION('center_axis',(0.,0.,-1.));
#60665=DIRECTION('ref_axis',(-1.,0.,0.));
#60666=DIRECTION('',(0.,0.,-1.));
#60667=DIRECTION('center_axis',(0.,0.,-1.));
#60668=DIRECTION('ref_axis',(-1.,0.,0.));
#60669=DIRECTION('center_axis',(0.,0.,-1.));
#60670=DIRECTION('ref_axis',(-1.,0.,0.));
#60671=DIRECTION('',(0.,0.,-1.));
#60672=DIRECTION('center_axis',(0.,0.,-1.));
#60673=DIRECTION('ref_axis',(-1.,0.,0.));
#60674=DIRECTION('',(0.,0.,-1.));
#60675=DIRECTION('center_axis',(0.,0.,-1.));
#60676=DIRECTION('ref_axis',(-1.,0.,0.));
#60677=DIRECTION('center_axis',(0.,0.,-1.));
#60678=DIRECTION('ref_axis',(-1.,0.,0.));
#60679=DIRECTION('',(0.,0.,-1.));
#60680=DIRECTION('center_axis',(0.,0.,-1.));
#60681=DIRECTION('ref_axis',(-1.,0.,0.));
#60682=DIRECTION('',(0.,0.,-1.));
#60683=DIRECTION('center_axis',(0.,0.,-1.));
#60684=DIRECTION('ref_axis',(-1.,0.,0.));
#60685=DIRECTION('center_axis',(0.,0.,-1.));
#60686=DIRECTION('ref_axis',(-1.,0.,0.));
#60687=DIRECTION('',(0.,0.,-1.));
#60688=DIRECTION('center_axis',(0.,0.,-1.));
#60689=DIRECTION('ref_axis',(-1.,0.,0.));
#60690=DIRECTION('',(0.,0.,-1.));
#60691=DIRECTION('center_axis',(0.,0.,-1.));
#60692=DIRECTION('ref_axis',(-1.,0.,0.));
#60693=DIRECTION('center_axis',(0.,0.,-1.));
#60694=DIRECTION('ref_axis',(-1.,0.,0.));
#60695=DIRECTION('',(0.,0.,-1.));
#60696=DIRECTION('center_axis',(0.,0.,-1.));
#60697=DIRECTION('ref_axis',(-1.,0.,0.));
#60698=DIRECTION('',(0.,0.,-1.));
#60699=DIRECTION('center_axis',(0.,0.,-1.));
#60700=DIRECTION('ref_axis',(-1.,0.,0.));
#60701=DIRECTION('center_axis',(0.,0.,-1.));
#60702=DIRECTION('ref_axis',(0.,-1.,0.));
#60703=DIRECTION('',(0.699017620280163,0.715104444495948,0.));
#60704=DIRECTION('',(0.40853671249629,-0.912741888237153,0.));
#60705=DIRECTION('',(0.605841460157257,0.79558539777608,0.));
#60706=DIRECTION('',(0.517605502898811,-0.855619391650791,0.));
#60707=DIRECTION('',(0.503481361059147,0.864006087401026,0.));
#60708=DIRECTION('',(0.618827921495384,-0.785526577257386,0.));
#60709=DIRECTION('',(0.393488997748033,0.919329325460277,0.));
#60710=DIRECTION('',(0.710669539600526,-0.703525980674471,0.));
#60711=DIRECTION('',(0.277531742331645,0.960716468058272,0.));
#60712=DIRECTION('',(0.791738131901976,-0.61086064735942,0.));
#60713=DIRECTION('',(0.157367388601791,0.987540128300948,0.));
#60714=DIRECTION('',(0.860804781177204,-0.508935289307458,0.));
#60715=DIRECTION('',(0.0348175056722151,0.99939368684156,0.));
#60716=DIRECTION('',(0.916822507425865,-0.399294991049663,0.));
#60717=DIRECTION('',(-0.0882601751523597,0.996097455815481,0.));
#60718=DIRECTION('',(0.958942139019354,-0.283601787746457,0.));
#60719=DIRECTION('',(-0.209999921689072,0.977701402725077,0.));
#60720=DIRECTION('',(0.986525185277102,-0.16360947042876,0.));
#60721=DIRECTION('',(-0.328556283475113,0.944484392983294,0.));
#60722=DIRECTION('',(0.999153515334452,-0.0411370003136725,0.));
#60723=DIRECTION('',(-0.442132066915505,0.896949962598262,0.));
#60724=DIRECTION('',(0.996635696580343,0.0819590647934408,0.));
#60725=DIRECTION('',(-0.54900557890607,0.835818685080689,0.));
#60726=DIRECTION('',(0.979009896580564,0.203812714022735,0.));
#60727=DIRECTION('',(-0.647556725945892,0.762017248283946,0.));
#60728=DIRECTION('',(0.946543304496363,0.322576770262686,0.));
#60729=DIRECTION('',(-0.736291573103355,0.676664406760831,0.));
#60730=DIRECTION('',(0.899728080769114,0.436450891482109,0.));
#60731=DIRECTION('',(-0.813864990546873,0.581054022584939,0.));
#60732=DIRECTION('',(0.83927389646971,0.543708862080205,0.));
#60733=DIRECTION('',(-0.879101044341991,0.476635451720516,0.));
#60734=DIRECTION('',(0.766097175408529,0.64272476055546,0.));
#60735=DIRECTION('',(-0.931010822411148,0.364991573263437,0.));
#60736=DIRECTION('',(0.681307202084615,0.731997606818242,0.));
#60737=DIRECTION('',(-0.968807425432727,0.247814794607607,0.));
#60738=DIRECTION('',(0.58618930606342,0.810174115518933,0.));
#60739=DIRECTION('',(-0.991917895432659,0.126881396274019,0.));
#60740=DIRECTION('',(0.482185377690781,0.876069210474377,0.));
#60741=DIRECTION('',(-0.99999190124326,0.00402460530868911,0.));
#60742=DIRECTION('',(0.370872010505059,0.928683989214811,0.));
#60743=DIRECTION('',(-0.992907049166627,-0.118893194570683,0.));
#60744=DIRECTION('',(0.253936601686191,0.967220865327082,0.));
#60745=DIRECTION('',(-0.970770738338343,-0.240008694813393,0.));
#60746=DIRECTION('',(0.13315177283448,0.991095659051655,0.));
#60747=DIRECTION('',(-0.933918532666054,-0.357485907894123,0.));
#60748=DIRECTION('',(0.0103484988340414,0.999946452852292,0.));
#60749=DIRECTION('',(-0.882909074022679,-0.469543999012249,0.));
#60750=DIRECTION('',(-0.112611647860063,0.993639077716975,0.));
#60751=DIRECTION('',(-0.818515613805076,-0.574484281732146,0.));
#60752=DIRECTION('',(-0.233864716762581,0.972269147023373,0.));
#60753=DIRECTION('',(-0.741714291231062,-0.670715968338017,0.));
#60754=DIRECTION('',(-0.351572634947544,0.936160607137494,0.));
#60755=DIRECTION('',(-0.653669336063903,-0.756780284554095,0.));
#60756=DIRECTION('',(-0.463951070360114,0.885860826716988,0.));
#60757=DIRECTION('',(-0.555715420075847,-0.831372583075678,0.));
#60758=DIRECTION('',(-0.569296480471704,0.822132299160257,0.));
#60759=DIRECTION('',(-0.449337424784549,-0.893362120692382,0.));
#60760=DIRECTION('',(-0.666011936248222,0.745941083983778,0.));
#60761=DIRECTION('',(-0.336147932162868,-0.941809199202592,0.));
#60762=DIRECTION('',(-0.752631329966403,0.658442162344578,0.));
#60763=DIRECTION('',(-0.217862779539932,-0.975979410280327,0.));
#60764=DIRECTION('',(-0.827841599912427,0.560961928703217,0.));
#60765=DIRECTION('',(-0.0962750492562598,-0.995354768356843,0.));
#60766=DIRECTION('',(-0.89050263505904,0.45497808403582,0.));
#60767=DIRECTION('',(0.0267721126367755,-0.999641562753852,0.));
#60768=DIRECTION('',(-0.939664557986563,0.342097235393562,0.));
#60769=DIRECTION('',(0.149413436592207,-0.988774810038012,0.));
#60770=DIRECTION('',(-0.974582124056318,0.224030541377457,0.));
#60771=DIRECTION('',(0.269789805152571,-0.962919239103539,0.));
#60772=DIRECTION('',(-0.994726018559695,0.102567772718229,0.));
#60773=DIRECTION('',(0.386076435275407,-0.922466794050081,0.));
#60774=DIRECTION('',(-0.999790880589577,-0.0204498188235966,0.));
#60775=DIRECTION('',(0.496510540184115,-0.868030692709698,0.));
#60776=DIRECTION('',(-0.989699932000427,-0.143157411957434,0.));
#60777=DIRECTION('',(0.599418051418609,-0.800436130889603,0.));
#60778=DIRECTION('',(-0.964606141286711,-0.263694884652627,0.));
#60779=DIRECTION('',(0.693238996006715,-0.720707773244886,0.));
#60780=DIRECTION('',(-0.924889904736447,-0.38023501169225,0.));
#60781=DIRECTION('',(0.77655114406428,-0.63005422040683,0.));
#60782=DIRECTION('',(-0.871153280011235,-0.491011163544849,0.));
#60783=DIRECTION('',(0.848091568350481,-0.529849687829314,0.));
#60784=DIRECTION('',(-0.804210859565811,-0.594344086667328,0.));
#60785=DIRECTION('',(0.906775788957432,-0.421613174083337,0.));
#60786=DIRECTION('',(-0.72507742225678,-0.688667359276932,0.));
#60787=DIRECTION('',(0.951714212920132,-0.306985434387063,0.));
#60788=DIRECTION('',(-0.634952550329563,-0.772551136708751,0.));
#60789=DIRECTION('',(0.982225619539013,-0.187704108429203,0.));
#60790=DIRECTION('',(-0.535202444974341,-0.844723826403333,0.));
#60791=DIRECTION('',(0.997847486991349,-0.0655773795225872,0.));
#60792=DIRECTION('',(-0.427339216108641,-0.904091363953695,0.));
#60793=DIRECTION('',(0.998343003690616,0.0575434356117104,0.));
#60794=DIRECTION('',(-0.312997960332345,-0.949753798006511,0.));
#60795=DIRECTION('',(0.983704658108754,0.179791950918663,0.));
#60796=DIRECTION('',(-0.193911974529963,-0.981018932607262,0.));
#60797=DIRECTION('',(0.954154352643279,0.299315003519512,0.));
#60798=DIRECTION('',(-0.0718864808566897,-0.997412820185324,0.));
#60799=DIRECTION('',(0.910140039803124,0.414300745771919,0.));
#60800=DIRECTION('',(0.0512287385893474,-0.998686946116021,0.));
#60801=DIRECTION('',(0.852328931705225,0.523006111033351,0.));
#60802=DIRECTION('',(0.173567382578051,-0.984821995949017,0.));
#60803=DIRECTION('',(0.781597385818949,0.623783236774591,0.));
#60804=DIRECTION('',(0.293274921971719,-0.956028148195691,0.));
#60805=DIRECTION('center_axis',(0.,0.,-1.));
#60806=DIRECTION('ref_axis',(0.,-1.,0.));
#60807=DIRECTION('',(-0.40853671249629,0.912741888237153,0.));
#60808=DIRECTION('',(-0.699017620280163,-0.715104444495948,0.));
#60809=DIRECTION('',(-0.293274921971719,0.956028148195691,0.));
#60810=DIRECTION('',(-0.781597385818949,-0.623783236774591,0.));
#60811=DIRECTION('',(-0.173567382578051,0.984821995949017,0.));
#60812=DIRECTION('',(-0.852328931705225,-0.523006111033351,0.));
#60813=DIRECTION('',(-0.0512287385893474,0.998686946116021,0.));
#60814=DIRECTION('',(-0.910140039803124,-0.414300745771919,0.));
#60815=DIRECTION('',(0.0718864808566897,0.997412820185324,0.));
#60816=DIRECTION('',(-0.954154352643279,-0.299315003519512,0.));
#60817=DIRECTION('',(0.193911974529963,0.981018932607262,0.));
#60818=DIRECTION('',(-0.983704658108754,-0.179791950918663,0.));
#60819=DIRECTION('',(0.312997960332345,0.949753798006511,0.));
#60820=DIRECTION('',(-0.998343003690616,-0.0575434356117104,0.));
#60821=DIRECTION('',(0.427339216108641,0.904091363953695,0.));
#60822=DIRECTION('',(-0.997847486991349,0.0655773795225872,0.));
#60823=DIRECTION('',(0.535202444974341,0.844723826403333,0.));
#60824=DIRECTION('',(-0.982225619539013,0.187704108429203,0.));
#60825=DIRECTION('',(0.634952550329563,0.772551136708751,0.));
#60826=DIRECTION('',(-0.951714212920132,0.306985434387063,0.));
#60827=DIRECTION('',(0.72507742225678,0.688667359276932,0.));
#60828=DIRECTION('',(-0.906775788957432,0.421613174083337,0.));
#60829=DIRECTION('',(0.804210859565811,0.594344086667328,0.));
#60830=DIRECTION('',(-0.848091568350481,0.529849687829314,0.));
#60831=DIRECTION('',(0.871153280011235,0.491011163544849,0.));
#60832=DIRECTION('',(-0.77655114406428,0.63005422040683,0.));
#60833=DIRECTION('',(0.924889904736447,0.38023501169225,0.));
#60834=DIRECTION('',(-0.693238996006715,0.720707773244886,0.));
#60835=DIRECTION('',(0.964606141286711,0.263694884652627,0.));
#60836=DIRECTION('',(-0.599418051418609,0.800436130889603,0.));
#60837=DIRECTION('',(0.989699932000427,0.143157411957434,0.));
#60838=DIRECTION('',(-0.496510540184115,0.868030692709698,0.));
#60839=DIRECTION('',(0.999790880589577,0.0204498188235966,0.));
#60840=DIRECTION('',(-0.386076435275407,0.922466794050081,0.));
#60841=DIRECTION('',(0.994726018559695,-0.102567772718229,0.));
#60842=DIRECTION('',(-0.269789805152571,0.962919239103539,0.));
#60843=DIRECTION('',(0.974582124056318,-0.224030541377457,0.));
#60844=DIRECTION('',(-0.149413436592207,0.988774810038012,0.));
#60845=DIRECTION('',(0.939664557986563,-0.342097235393562,0.));
#60846=DIRECTION('',(-0.0267721126367755,0.999641562753852,0.));
#60847=DIRECTION('',(0.89050263505904,-0.45497808403582,0.));
#60848=DIRECTION('',(0.0962750492562598,0.995354768356843,0.));
#60849=DIRECTION('',(0.827841599912427,-0.560961928703217,0.));
#60850=DIRECTION('',(0.217862779539932,0.975979410280327,0.));
#60851=DIRECTION('',(0.752631329966403,-0.658442162344578,0.));
#60852=DIRECTION('',(0.336147932162868,0.941809199202592,0.));
#60853=DIRECTION('',(0.666011936248222,-0.745941083983778,0.));
#60854=DIRECTION('',(0.449337424784549,0.893362120692382,0.));
#60855=DIRECTION('',(0.569296480471704,-0.822132299160257,0.));
#60856=DIRECTION('',(0.555715420075847,0.831372583075678,0.));
#60857=DIRECTION('',(0.463951070360114,-0.885860826716988,0.));
#60858=DIRECTION('',(0.653669336063903,0.756780284554095,0.));
#60859=DIRECTION('',(0.351572634947544,-0.936160607137494,0.));
#60860=DIRECTION('',(0.741714291231062,0.670715968338017,0.));
#60861=DIRECTION('',(0.233864716762581,-0.972269147023373,0.));
#60862=DIRECTION('',(0.818515613805076,0.574484281732146,0.));
#60863=DIRECTION('',(0.112611647860063,-0.993639077716975,0.));
#60864=DIRECTION('',(0.88290907402268,0.469543999012249,0.));
#60865=DIRECTION('',(-0.0103484988340414,-0.999946452852292,0.));
#60866=DIRECTION('',(0.933918532666054,0.357485907894123,0.));
#60867=DIRECTION('',(-0.13315177283448,-0.991095659051655,0.));
#60868=DIRECTION('',(0.970770738338343,0.240008694813393,0.));
#60869=DIRECTION('',(-0.253936601686191,-0.967220865327082,0.));
#60870=DIRECTION('',(0.992907049166627,0.118893194570683,0.));
#60871=DIRECTION('',(-0.370872010505059,-0.928683989214811,0.));
#60872=DIRECTION('',(0.99999190124326,-0.00402460530868912,0.));
#60873=DIRECTION('',(-0.482185377690781,-0.876069210474377,0.));
#60874=DIRECTION('',(0.991917895432659,-0.126881396274019,0.));
#60875=DIRECTION('',(-0.58618930606342,-0.810174115518933,0.));
#60876=DIRECTION('',(0.968807425432727,-0.247814794607607,0.));
#60877=DIRECTION('',(-0.681307202084615,-0.731997606818242,0.));
#60878=DIRECTION('',(0.931010822411148,-0.364991573263437,0.));
#60879=DIRECTION('',(-0.766097175408529,-0.64272476055546,0.));
#60880=DIRECTION('',(0.879101044341991,-0.476635451720516,0.));
#60881=DIRECTION('',(-0.83927389646971,-0.543708862080205,0.));
#60882=DIRECTION('',(0.813864990546873,-0.581054022584939,0.));
#60883=DIRECTION('',(-0.899728080769114,-0.436450891482109,0.));
#60884=DIRECTION('',(0.736291573103355,-0.676664406760831,0.));
#60885=DIRECTION('',(-0.946543304496363,-0.322576770262686,0.));
#60886=DIRECTION('',(0.647556725945892,-0.762017248283946,0.));
#60887=DIRECTION('',(-0.979009896580564,-0.203812714022735,0.));
#60888=DIRECTION('',(0.54900557890607,-0.835818685080689,0.));
#60889=DIRECTION('',(-0.996635696580343,-0.0819590647934408,0.));
#60890=DIRECTION('',(0.442132066915505,-0.896949962598262,0.));
#60891=DIRECTION('',(-0.999153515334452,0.0411370003136725,0.));
#60892=DIRECTION('',(0.328556283475113,-0.944484392983294,0.));
#60893=DIRECTION('',(-0.986525185277102,0.16360947042876,0.));
#60894=DIRECTION('',(0.209999921689072,-0.977701402725077,0.));
#60895=DIRECTION('',(-0.958942139019354,0.283601787746457,0.));
#60896=DIRECTION('',(0.0882601751523597,-0.996097455815481,0.));
#60897=DIRECTION('',(-0.916822507425865,0.399294991049663,0.));
#60898=DIRECTION('',(-0.0348175056722151,-0.99939368684156,0.));
#60899=DIRECTION('',(-0.860804781177204,0.508935289307458,0.));
#60900=DIRECTION('',(-0.157367388601791,-0.987540128300948,0.));
#60901=DIRECTION('',(-0.791738131901976,0.61086064735942,0.));
#60902=DIRECTION('',(-0.277531742331645,-0.960716468058272,0.));
#60903=DIRECTION('',(-0.710669539600526,0.703525980674471,0.));
#60904=DIRECTION('',(-0.393488997748033,-0.919329325460277,0.));
#60905=DIRECTION('',(-0.618827921495384,0.785526577257386,0.));
#60906=DIRECTION('',(-0.503481361059147,-0.864006087401026,0.));
#60907=DIRECTION('',(-0.517605502898811,0.855619391650791,0.));
#60908=DIRECTION('',(-0.605841460157257,-0.79558539777608,0.));
#60909=DIRECTION('center_axis',(0.,0.,-1.));
#60910=DIRECTION('ref_axis',(0.,-1.,0.));
#60911=DIRECTION('center_axis',(0.,0.,1.));
#60912=DIRECTION('ref_axis',(1.,0.,0.));
#60913=DIRECTION('center_axis',(0.,0.,1.));
#60914=DIRECTION('ref_axis',(1.,0.,0.));
#60915=DIRECTION('center_axis',(0.,0.,-1.));
#60916=DIRECTION('ref_axis',(0.,-1.,0.));
#60917=DIRECTION('center_axis',(-0.785526577257387,-0.618827921495382,0.));
#60918=DIRECTION('ref_axis',(-0.618827921495382,0.785526577257387,0.));
#60919=DIRECTION('',(0.,0.,-1.));
#60920=DIRECTION('center_axis',(0.864006087401028,-0.503481361059144,0.));
#60921=DIRECTION('ref_axis',(0.,0.,-1.));
#60922=DIRECTION('center_axis',(-0.855619391650793,-0.517605502898808,0.));
#60923=DIRECTION('ref_axis',(-0.517605502898808,0.855619391650792,0.));
#60924=DIRECTION('',(0.,0.,-1.));
#60925=DIRECTION('center_axis',(0.795585397776081,-0.605841460157256,0.));
#60926=DIRECTION('ref_axis',(0.,0.,-1.));
#60927=DIRECTION('center_axis',(-0.703525980674471,-0.710669539600526,0.));
#60928=DIRECTION('ref_axis',(-0.710669539600526,0.703525980674471,0.));
#60929=DIRECTION('',(0.,0.,-1.));
#60930=DIRECTION('center_axis',(0.91932932546028,-0.393488997748027,0.));
#60931=DIRECTION('ref_axis',(0.,0.,-1.));
#60932=DIRECTION('center_axis',(0.203812714022727,-0.979009896580566,0.));
#60933=DIRECTION('ref_axis',(0.,0.,-1.));
#60934=DIRECTION('',(0.,0.,-1.));
#60935=DIRECTION('center_axis',(0.83581868508069,0.549005578906067,0.));
#60936=DIRECTION('ref_axis',(0.,0.,-1.));
#60937=DIRECTION('center_axis',(0.0819590647934317,-0.996635696580343,0.));
#60938=DIRECTION('ref_axis',(0.,0.,-1.));
#60939=DIRECTION('',(0.,0.,-1.));
#60940=DIRECTION('center_axis',(0.896949962598264,0.442132066915501,0.));
#60941=DIRECTION('ref_axis',(0.,0.,-1.));
#60942=DIRECTION('center_axis',(-0.0411370003136629,-0.999153515334452,
0.));
#60943=DIRECTION('ref_axis',(-0.999153515334452,0.0411370003136629,0.));
#60944=DIRECTION('',(0.,0.,-1.));
#60945=DIRECTION('center_axis',(0.944484392983296,0.328556283475108,0.));
#60946=DIRECTION('ref_axis',(0.,0.,-1.));
#60947=DIRECTION('center_axis',(-0.163609470428752,-0.986525185277104,0.));
#60948=DIRECTION('ref_axis',(-0.986525185277104,0.163609470428752,0.));
#60949=DIRECTION('',(0.,0.,-1.));
#60950=DIRECTION('center_axis',(0.977701402725079,0.209999921689065,0.));
#60951=DIRECTION('ref_axis',(0.,0.,-1.));
#60952=DIRECTION('center_axis',(-0.283601787746451,-0.958942139019356,0.));
#60953=DIRECTION('ref_axis',(-0.958942139019356,0.283601787746451,0.));
#60954=DIRECTION('',(0.,0.,-1.));
#60955=DIRECTION('center_axis',(0.996097455815482,0.0882601751523507,0.));
#60956=DIRECTION('ref_axis',(0.,0.,-1.));
#60957=DIRECTION('center_axis',(-0.399294991049658,-0.916822507425867,0.));
#60958=DIRECTION('ref_axis',(-0.916822507425867,0.399294991049658,0.));
#60959=DIRECTION('',(0.,0.,-1.));
#60960=DIRECTION('center_axis',(0.99939368684156,-0.0348175056722054,0.));
#60961=DIRECTION('ref_axis',(0.,0.,-1.));
#60962=DIRECTION('center_axis',(-0.508935289307455,-0.860804781177206,0.));
#60963=DIRECTION('ref_axis',(-0.860804781177206,0.508935289307455,0.));
#60964=DIRECTION('',(0.,0.,-1.));
#60965=DIRECTION('center_axis',(0.98754012830095,-0.157367388601782,0.));
#60966=DIRECTION('ref_axis',(0.,0.,-1.));
#60967=DIRECTION('center_axis',(-0.610860647359419,-0.791738131901977,0.));
#60968=DIRECTION('ref_axis',(-0.791738131901977,0.610860647359419,0.));
#60969=DIRECTION('',(0.,0.,-1.));
#60970=DIRECTION('center_axis',(0.960716468058274,-0.277531742331638,0.));
#60971=DIRECTION('ref_axis',(0.,0.,-1.));
#60972=DIRECTION('center_axis',(0.322576770262681,-0.946543304496365,0.));
#60973=DIRECTION('ref_axis',(0.,0.,-1.));
#60974=DIRECTION('',(0.,0.,-1.));
#60975=DIRECTION('center_axis',(0.762017248283947,0.647556725945891,0.));
#60976=DIRECTION('ref_axis',(0.,0.,-1.));
#60977=DIRECTION('center_axis',(0.436450891482105,-0.899728080769115,0.));
#60978=DIRECTION('ref_axis',(0.,0.,-1.));
#60979=DIRECTION('',(0.,0.,-1.));
#60980=DIRECTION('center_axis',(0.676664406760831,0.736291573103355,0.));
#60981=DIRECTION('ref_axis',(0.,0.,-1.));
#60982=DIRECTION('center_axis',(0.543708862080202,-0.839273896469711,0.));
#60983=DIRECTION('ref_axis',(0.,0.,-1.));
#60984=DIRECTION('',(0.,0.,-1.));
#60985=DIRECTION('center_axis',(0.581054022584937,0.813864990546874,0.));
#60986=DIRECTION('ref_axis',(0.,0.,-1.));
#60987=DIRECTION('center_axis',(0.642724760555459,-0.76609717540853,0.));
#60988=DIRECTION('ref_axis',(0.,0.,-1.));
#60989=DIRECTION('',(0.,0.,-1.));
#60990=DIRECTION('center_axis',(0.476635451720513,0.879101044341993,0.));
#60991=DIRECTION('ref_axis',(0.,0.,-1.));
#60992=DIRECTION('center_axis',(0.731997606818242,-0.681307202084615,0.));
#60993=DIRECTION('ref_axis',(0.,0.,-1.));
#60994=DIRECTION('',(0.,0.,-1.));
#60995=DIRECTION('center_axis',(0.364991573263432,0.93101082241115,0.));
#60996=DIRECTION('ref_axis',(0.,0.,-1.));
#60997=DIRECTION('center_axis',(0.810174115518934,-0.586189306063419,0.));
#60998=DIRECTION('ref_axis',(0.,0.,-1.));
#60999=DIRECTION('',(0.,0.,-1.));
#61000=DIRECTION('center_axis',(0.2478147946076,0.968807425432729,0.));
#61001=DIRECTION('ref_axis',(0.,0.,-1.));
#61002=DIRECTION('center_axis',(0.876069210474379,-0.482185377690778,0.));
#61003=DIRECTION('ref_axis',(0.,0.,-1.));
#61004=DIRECTION('',(0.,0.,-1.));
#61005=DIRECTION('center_axis',(0.12688139627401,0.99191789543266,0.));
#61006=DIRECTION('ref_axis',(0.,0.,-1.));
#61007=DIRECTION('center_axis',(0.928683989214813,-0.370872010505054,0.));
#61008=DIRECTION('ref_axis',(0.,0.,-1.));
#61009=DIRECTION('',(0.,0.,-1.));
#61010=DIRECTION('center_axis',(0.00402460530867915,0.99999190124326,0.));
#61011=DIRECTION('ref_axis',(0.,0.,-1.));
#61012=DIRECTION('center_axis',(0.991095659051657,-0.133151772834472,0.));
#61013=DIRECTION('ref_axis',(0.,0.,-1.));
#61014=DIRECTION('',(0.,0.,-1.));
#61015=DIRECTION('center_axis',(-0.240008694813385,0.970770738338345,0.));
#61016=DIRECTION('ref_axis',(0.,0.,1.));
#61017=DIRECTION('center_axis',(0.967220865327084,-0.253936601686184,0.));
#61018=DIRECTION('ref_axis',(0.,0.,-1.));
#61019=DIRECTION('',(0.,0.,-1.));
#61020=DIRECTION('center_axis',(-0.118893194570674,0.992907049166628,0.));
#61021=DIRECTION('ref_axis',(0.,0.,1.));
#61022=DIRECTION('center_axis',(0.999946452852293,-0.0103484988340315,0.));
#61023=DIRECTION('ref_axis',(0.,0.,-1.));
#61024=DIRECTION('',(0.,0.,-1.));
#61025=DIRECTION('center_axis',(-0.357485907894118,0.933918532666056,0.));
#61026=DIRECTION('ref_axis',(0.,0.,1.));
#61027=DIRECTION('center_axis',(0.993639077716976,0.112611647860054,0.));
#61028=DIRECTION('ref_axis',(0.,0.,-1.));
#61029=DIRECTION('',(0.,0.,-1.));
#61030=DIRECTION('center_axis',(-0.469543999012245,0.882909074022681,0.));
#61031=DIRECTION('ref_axis',(0.,0.,1.));
#61032=DIRECTION('center_axis',(0.972269147023375,0.233864716762574,0.));
#61033=DIRECTION('ref_axis',(0.,0.,-1.));
#61034=DIRECTION('',(0.,0.,-1.));
#61035=DIRECTION('center_axis',(-0.574484281732144,0.818515613805077,0.));
#61036=DIRECTION('ref_axis',(0.,0.,1.));
#61037=DIRECTION('center_axis',(0.936160607137496,0.351572634947539,0.));
#61038=DIRECTION('ref_axis',(0.,0.,-1.));
#61039=DIRECTION('',(0.,0.,-1.));
#61040=DIRECTION('center_axis',(-0.670715968338016,0.741714291231062,0.));
#61041=DIRECTION('ref_axis',(0.,0.,1.));
#61042=DIRECTION('center_axis',(0.88586082671699,0.46395107036011,0.));
#61043=DIRECTION('ref_axis',(0.,0.,-1.));
#61044=DIRECTION('',(0.,0.,-1.));
#61045=DIRECTION('center_axis',(-0.756780284554095,0.653669336063902,0.));
#61046=DIRECTION('ref_axis',(0.,0.,1.));
#61047=DIRECTION('center_axis',(0.822132299160259,0.569296480471702,0.));
#61048=DIRECTION('ref_axis',(0.,0.,-1.));
#61049=DIRECTION('',(0.,0.,-1.));
#61050=DIRECTION('center_axis',(-0.831372583075679,0.555715420075845,0.));
#61051=DIRECTION('ref_axis',(0.,0.,1.));
#61052=DIRECTION('center_axis',(0.745941083983779,0.666011936248222,0.));
#61053=DIRECTION('ref_axis',(0.,0.,-1.));
#61054=DIRECTION('',(0.,0.,-1.));
#61055=DIRECTION('center_axis',(-0.893362120692384,0.449337424784545,0.));
#61056=DIRECTION('ref_axis',(0.,0.,1.));
#61057=DIRECTION('center_axis',(0.658442162344578,0.752631329966403,0.));
#61058=DIRECTION('ref_axis',(0.,0.,-1.));
#61059=DIRECTION('',(0.,0.,-1.));
#61060=DIRECTION('center_axis',(-0.941809199202594,0.336147932162862,0.));
#61061=DIRECTION('ref_axis',(0.,0.,1.));
#61062=DIRECTION('center_axis',(0.560961928703215,0.827841599912429,0.));
#61063=DIRECTION('ref_axis',(0.,0.,-1.));
#61064=DIRECTION('',(0.,0.,-1.));
#61065=DIRECTION('center_axis',(-0.975979410280329,0.217862779539925,0.));
#61066=DIRECTION('ref_axis',(0.,0.,1.));
#61067=DIRECTION('center_axis',(0.454978084035816,0.890502635059042,0.));
#61068=DIRECTION('ref_axis',(0.,0.,-1.));
#61069=DIRECTION('',(0.,0.,-1.));
#61070=DIRECTION('center_axis',(-0.995354768356844,0.0962750492562509,0.));
#61071=DIRECTION('ref_axis',(0.,0.,1.));
#61072=DIRECTION('center_axis',(-0.0204498188235867,0.999790880589577,0.));
#61073=DIRECTION('ref_axis',(0.,0.,1.));
#61074=DIRECTION('',(0.,0.,-1.));
#61075=DIRECTION('center_axis',(-0.922466794050083,-0.386076435275401,0.));
#61076=DIRECTION('ref_axis',(-0.386076435275401,0.922466794050083,0.));
#61077=DIRECTION('center_axis',(0.10256777271822,0.994726018559695,0.));
#61078=DIRECTION('ref_axis',(0.,0.,-1.));
#61079=DIRECTION('',(0.,0.,-1.));
#61080=DIRECTION('center_axis',(-0.96291923910354,-0.269789805152565,0.));
#61081=DIRECTION('ref_axis',(-0.269789805152565,0.96291923910354,0.));
#61082=DIRECTION('center_axis',(0.224030541377449,0.974582124056319,0.));
#61083=DIRECTION('ref_axis',(0.,0.,-1.));
#61084=DIRECTION('',(0.,0.,-1.));
#61085=DIRECTION('center_axis',(-0.988774810038013,-0.149413436592199,0.));
#61086=DIRECTION('ref_axis',(-0.149413436592199,0.988774810038013,0.));
#61087=DIRECTION('center_axis',(0.342097235393556,0.939664557986565,0.));
#61088=DIRECTION('ref_axis',(0.,0.,-1.));
#61089=DIRECTION('',(0.,0.,-1.));
#61090=DIRECTION('center_axis',(-0.999641562753853,-0.0267721126367658,
0.));
#61091=DIRECTION('ref_axis',(-0.0267721126367658,0.999641562753853,0.));
#61092=DIRECTION('center_axis',(-0.143157411957425,0.989699932000428,0.));
#61093=DIRECTION('ref_axis',(0.,0.,1.));
#61094=DIRECTION('',(0.,0.,-1.));
#61095=DIRECTION('center_axis',(-0.8680306927097,-0.496510540184112,0.));
#61096=DIRECTION('ref_axis',(-0.496510540184112,0.8680306927097,0.));
#61097=DIRECTION('center_axis',(-0.26369488465262,0.964606141286713,0.));
#61098=DIRECTION('ref_axis',(0.,0.,1.));
#61099=DIRECTION('',(0.,0.,-1.));
#61100=DIRECTION('center_axis',(-0.800436130889604,-0.599418051418608,0.));
#61101=DIRECTION('ref_axis',(-0.599418051418608,0.800436130889604,0.));
#61102=DIRECTION('center_axis',(-0.380235011692245,0.924889904736449,0.));
#61103=DIRECTION('ref_axis',(0.,0.,1.));
#61104=DIRECTION('',(0.,0.,-1.));
#61105=DIRECTION('center_axis',(-0.720707773244887,-0.693238996006714,0.));
#61106=DIRECTION('ref_axis',(-0.693238996006714,0.720707773244887,0.));
#61107=DIRECTION('center_axis',(-0.491011163544846,0.871153280011237,0.));
#61108=DIRECTION('ref_axis',(0.,0.,1.));
#61109=DIRECTION('',(0.,0.,-1.));
#61110=DIRECTION('center_axis',(-0.630054220406829,-0.776551144064281,0.));
#61111=DIRECTION('ref_axis',(-0.776551144064281,0.630054220406829,0.));
#61112=DIRECTION('center_axis',(-0.594344086667326,0.804210859565812,0.));
#61113=DIRECTION('ref_axis',(0.,0.,1.));
#61114=DIRECTION('',(0.,0.,-1.));
#61115=DIRECTION('center_axis',(-0.529849687829311,-0.848091568350483,0.));
#61116=DIRECTION('ref_axis',(-0.848091568350483,0.529849687829311,0.));
#61117=DIRECTION('center_axis',(-0.688667359276932,0.72507742225678,0.));
#61118=DIRECTION('ref_axis',(0.,0.,1.));
#61119=DIRECTION('',(0.,0.,-1.));
#61120=DIRECTION('center_axis',(-0.421613174083333,-0.906775788957434,0.));
#61121=DIRECTION('ref_axis',(-0.906775788957434,0.421613174083333,0.));
#61122=DIRECTION('center_axis',(-0.772551136708752,0.634952550329562,0.));
#61123=DIRECTION('ref_axis',(0.,0.,1.));
#61124=DIRECTION('',(0.,0.,-1.));
#61125=DIRECTION('center_axis',(-0.306985434387057,-0.951714212920134,0.));
#61126=DIRECTION('ref_axis',(-0.951714212920134,0.306985434387057,0.));
#61127=DIRECTION('center_axis',(-0.844723826403334,0.535202444974339,0.));
#61128=DIRECTION('ref_axis',(0.,0.,1.));
#61129=DIRECTION('',(0.,0.,-1.));
#61130=DIRECTION('center_axis',(-0.187704108429195,-0.982225619539015,0.));
#61131=DIRECTION('ref_axis',(-0.982225619539015,0.187704108429195,0.));
#61132=DIRECTION('center_axis',(-0.904091363953697,0.427339216108637,0.));
#61133=DIRECTION('ref_axis',(0.,0.,1.));
#61134=DIRECTION('',(0.,0.,-1.));
#61135=DIRECTION('center_axis',(-0.0655773795225779,-0.99784748699135,0.));
#61136=DIRECTION('ref_axis',(-0.99784748699135,0.0655773795225779,0.));
#61137=DIRECTION('center_axis',(-0.949753798006513,0.312997960332339,0.));
#61138=DIRECTION('ref_axis',(0.,0.,1.));
#61139=DIRECTION('',(0.,0.,-1.));
#61140=DIRECTION('center_axis',(0.057543435611701,-0.998343003690616,0.));
#61141=DIRECTION('ref_axis',(0.,0.,-1.));
#61142=DIRECTION('center_axis',(-0.981018932607263,0.193911974529956,0.));
#61143=DIRECTION('ref_axis',(0.,0.,1.));
#61144=DIRECTION('',(0.,0.,-1.));
#61145=DIRECTION('center_axis',(0.179791950918655,-0.983704658108756,0.));
#61146=DIRECTION('ref_axis',(0.,0.,-1.));
#61147=DIRECTION('center_axis',(-0.997412820185324,0.0718864808566805,0.));
#61148=DIRECTION('ref_axis',(0.,0.,1.));
#61149=DIRECTION('',(0.,0.,-1.));
#61150=DIRECTION('center_axis',(0.299315003519506,-0.954154352643281,0.));
#61151=DIRECTION('ref_axis',(0.,0.,-1.));
#61152=DIRECTION('center_axis',(-0.998686946116022,-0.051228738589338,0.));
#61153=DIRECTION('ref_axis',(-0.051228738589338,0.998686946116021,0.));
#61154=DIRECTION('',(0.,0.,-1.));
#61155=DIRECTION('center_axis',(0.414300745771915,-0.910140039803126,0.));
#61156=DIRECTION('ref_axis',(0.,0.,-1.));
#61157=DIRECTION('center_axis',(-0.984821995949018,-0.173567382578043,0.));
#61158=DIRECTION('ref_axis',(-0.173567382578043,0.984821995949018,0.));
#61159=DIRECTION('',(0.,0.,-1.));
#61160=DIRECTION('center_axis',(0.523006111033348,-0.852328931705227,0.));
#61161=DIRECTION('ref_axis',(0.,0.,-1.));
#61162=DIRECTION('center_axis',(-0.956028148195693,-0.293274921971712,0.));
#61163=DIRECTION('ref_axis',(-0.293274921971712,0.956028148195693,0.));
#61164=DIRECTION('',(0.,0.,-1.));
#61165=DIRECTION('center_axis',(0.62378323677459,-0.78159738581895,0.));
#61166=DIRECTION('ref_axis',(0.,0.,-1.));
#61167=DIRECTION('center_axis',(-0.912741888237155,-0.408536712496285,0.));
#61168=DIRECTION('ref_axis',(-0.408536712496285,0.912741888237155,0.));
#61169=DIRECTION('',(0.,0.,-1.));
#61170=DIRECTION('center_axis',(0.715104444495948,-0.699017620280163,0.));
#61171=DIRECTION('ref_axis',(0.,0.,-1.));
#61172=DIRECTION('axis',(0.,0.,1.));
#61173=DIRECTION('refdir',(1.,0.,0.));
#61174=DIRECTION('center_axis',(-1.,0.,0.));
#61175=DIRECTION('ref_axis',(0.,0.,1.));
#61176=DIRECTION('center_axis',(-1.,0.,0.));
#61177=DIRECTION('ref_axis',(0.,0.,1.));
#61178=DIRECTION('',(-1.,0.,0.));
#61179=DIRECTION('center_axis',(-1.,0.,0.));
#61180=DIRECTION('ref_axis',(0.,0.,1.));
#61181=DIRECTION('',(-1.,0.,0.));
#61182=DIRECTION('center_axis',(-1.,0.,0.));
#61183=DIRECTION('ref_axis',(0.,0.,1.));
#61184=DIRECTION('',(-1.,0.,0.));
#61185=DIRECTION('center_axis',(-1.,0.,0.));
#61186=DIRECTION('ref_axis',(0.,0.,1.));
#61187=DIRECTION('center_axis',(-1.,0.,0.));
#61188=DIRECTION('ref_axis',(0.,0.,1.));
#61189=DIRECTION('',(-1.,0.,0.));
#61190=DIRECTION('center_axis',(-1.,0.,0.));
#61191=DIRECTION('ref_axis',(0.,0.,1.));
#61192=DIRECTION('center_axis',(1.,0.,0.));
#61193=DIRECTION('ref_axis',(0.,0.,-1.));
#61194=DIRECTION('center_axis',(-1.,0.,0.));
#61195=DIRECTION('ref_axis',(0.,0.,-1.));
#61196=DIRECTION('',(1.,0.,0.));
#61197=DIRECTION('center_axis',(-1.,0.,0.));
#61198=DIRECTION('ref_axis',(0.,0.,1.));
#61199=DIRECTION('center_axis',(0.,0.,1.));
#61200=DIRECTION('ref_axis',(1.,0.,0.));
#61201=DIRECTION('center_axis',(0.,0.,-1.));
#61202=DIRECTION('ref_axis',(-1.,0.,0.));
#61203=DIRECTION('',(0.,0.,1.));
#61204=DIRECTION('center_axis',(0.,0.,1.));
#61205=DIRECTION('ref_axis',(-1.,0.,0.));
#61206=DIRECTION('center_axis',(0.,0.,1.));
#61207=DIRECTION('ref_axis',(1.,0.,0.));
#61208=DIRECTION('center_axis',(0.,0.,-1.));
#61209=DIRECTION('ref_axis',(-1.,0.,0.));
#61210=DIRECTION('',(0.,0.,-1.));
#61211=DIRECTION('center_axis',(0.,0.,-1.));
#61212=DIRECTION('ref_axis',(-1.,0.,0.));
#61213=DIRECTION('',(0.,0.,1.));
#61214=DIRECTION('center_axis',(0.,0.,-1.));
#61215=DIRECTION('ref_axis',(-1.,0.,0.));
#61216=DIRECTION('center_axis',(0.,0.,-1.));
#61217=DIRECTION('ref_axis',(-1.,0.,0.));
#61218=DIRECTION('',(0.,0.,-1.));
#61219=DIRECTION('center_axis',(0.,0.,-1.));
#61220=DIRECTION('ref_axis',(-1.,0.,0.));
#61221=DIRECTION('center_axis',(0.,0.,-1.));
#61222=DIRECTION('ref_axis',(-1.,0.,0.));
#61223=DIRECTION('center_axis',(0.,0.,1.));
#61224=DIRECTION('ref_axis',(-1.,0.,0.));
#61225=DIRECTION('',(0.64018439966448,-7.83999775913175E-17,-0.768221279597376));
#61226=DIRECTION('center_axis',(0.,0.,-1.));
#61227=DIRECTION('ref_axis',(-1.,0.,0.));
#61228=DIRECTION('center_axis',(0.,0.,1.));
#61229=DIRECTION('ref_axis',(-1.,0.,0.));
#61230=DIRECTION('center_axis',(0.,0.,-1.));
#61231=DIRECTION('ref_axis',(-1.,0.,0.));
#61232=DIRECTION('center_axis',(0.,0.,-1.));
#61233=DIRECTION('ref_axis',(-1.,0.,0.));
#61234=DIRECTION('center_axis',(0.,0.,-1.));
#61235=DIRECTION('ref_axis',(-1.,0.,0.));
#61236=DIRECTION('',(0.,0.,-1.));
#61237=DIRECTION('center_axis',(0.,0.,-1.));
#61238=DIRECTION('ref_axis',(-1.,0.,0.));
#61239=DIRECTION('center_axis',(0.,0.,1.));
#61240=DIRECTION('ref_axis',(1.,0.,0.));
#61241=DIRECTION('center_axis',(0.,0.,-1.));
#61242=DIRECTION('ref_axis',(-1.,0.,0.));
#61243=DIRECTION('',(0.,0.,1.));
#61244=DIRECTION('center_axis',(0.,0.,1.));
#61245=DIRECTION('ref_axis',(-1.,0.,0.));
#61246=DIRECTION('center_axis',(0.,0.,1.));
#61247=DIRECTION('ref_axis',(1.,0.,0.));
#61248=DIRECTION('center_axis',(0.,0.,-1.));
#61249=DIRECTION('ref_axis',(-1.,0.,0.));
#61250=DIRECTION('',(0.,0.,-1.));
#61251=DIRECTION('center_axis',(0.,0.,1.));
#61252=DIRECTION('ref_axis',(-1.,0.,0.));
#61253=DIRECTION('',(0.,0.,-1.));
#61254=DIRECTION('center_axis',(0.,0.,-1.));
#61255=DIRECTION('ref_axis',(-1.,0.,0.));
#61256=DIRECTION('center_axis',(0.,0.,1.));
#61257=DIRECTION('ref_axis',(-1.,0.,0.));
#61258=DIRECTION('',(0.,0.,-1.));
#61259=DIRECTION('center_axis',(0.,0.,1.));
#61260=DIRECTION('ref_axis',(-1.,0.,0.));
#61261=DIRECTION('',(0.,0.,-1.));
#61262=DIRECTION('center_axis',(0.,0.,1.));
#61263=DIRECTION('ref_axis',(-1.,0.,0.));
#61264=DIRECTION('',(0.,0.,-1.));
#61265=DIRECTION('center_axis',(0.,0.,1.));
#61266=DIRECTION('ref_axis',(1.,0.,0.));
#61267=DIRECTION('center_axis',(0.,0.,1.));
#61268=DIRECTION('ref_axis',(1.,0.,0.));
#61269=DIRECTION('',(0.,0.,1.));
#61270=DIRECTION('center_axis',(0.,0.,1.));
#61271=DIRECTION('ref_axis',(1.,0.,0.));
#61272=DIRECTION('center_axis',(0.,0.,1.));
#61273=DIRECTION('ref_axis',(1.,0.,0.));
#61274=DIRECTION('center_axis',(0.,0.,1.));
#61275=DIRECTION('ref_axis',(1.,0.,0.));
#61276=DIRECTION('',(0.,0.,1.));
#61277=DIRECTION('center_axis',(0.,0.,1.));
#61278=DIRECTION('ref_axis',(1.,0.,0.));
#61279=DIRECTION('center_axis',(0.,0.,1.));
#61280=DIRECTION('ref_axis',(1.,0.,0.));
#61281=DIRECTION('center_axis',(0.,0.,1.));
#61282=DIRECTION('ref_axis',(1.,0.,0.));
#61283=DIRECTION('',(0.,0.,1.));
#61284=DIRECTION('center_axis',(0.,0.,1.));
#61285=DIRECTION('ref_axis',(1.,0.,0.));
#61286=DIRECTION('center_axis',(0.,0.,-1.));
#61287=DIRECTION('ref_axis',(-1.,0.,0.));
#61288=DIRECTION('center_axis',(0.,0.,1.));
#61289=DIRECTION('ref_axis',(1.,0.,0.));
#61290=DIRECTION('',(0.,0.,-1.));
#61291=DIRECTION('center_axis',(0.,0.,1.));
#61292=DIRECTION('ref_axis',(1.,0.,0.));
#61293=DIRECTION('center_axis',(0.,0.,-1.));
#61294=DIRECTION('ref_axis',(-1.,0.,0.));
#61295=DIRECTION('center_axis',(0.,0.,1.));
#61296=DIRECTION('ref_axis',(1.,0.,0.));
#61297=DIRECTION('',(0.,0.,-1.));
#61298=DIRECTION('center_axis',(0.,0.,-1.));
#61299=DIRECTION('ref_axis',(-1.,0.,0.));
#61300=DIRECTION('',(0.,0.,1.));
#61301=DIRECTION('center_axis',(0.,0.,-1.));
#61302=DIRECTION('ref_axis',(-1.,0.,0.));
#61303=DIRECTION('',(0.,0.,-1.));
#61304=DIRECTION('center_axis',(0.,0.,1.));
#61305=DIRECTION('ref_axis',(1.,0.,0.));
#61306=DIRECTION('',(0.,0.,1.));
#61307=DIRECTION('center_axis',(0.,0.,-1.));
#61308=DIRECTION('ref_axis',(-1.,0.,0.));
#61309=DIRECTION('center_axis',(0.,0.,1.));
#61310=DIRECTION('ref_axis',(1.,0.,0.));
#61311=DIRECTION('',(0.,0.,-1.));
#61312=DIRECTION('center_axis',(0.,0.,1.));
#61313=DIRECTION('ref_axis',(1.,0.,0.));
#61314=DIRECTION('center_axis',(0.,0.,1.));
#61315=DIRECTION('ref_axis',(1.,0.,0.));
#61316=DIRECTION('',(0.,0.,1.));
#61317=DIRECTION('center_axis',(0.,0.,-1.));
#61318=DIRECTION('ref_axis',(-1.,0.,0.));
#61319=DIRECTION('',(0.,0.,1.));
#61320=DIRECTION('center_axis',(0.,0.,-1.));
#61321=DIRECTION('ref_axis',(-1.,0.,0.));
#61322=DIRECTION('',(0.,0.,-1.));
#61323=DIRECTION('center_axis',(0.,0.,-1.));
#61324=DIRECTION('ref_axis',(-1.,0.,0.));
#61325=DIRECTION('center_axis',(0.,0.,1.));
#61326=DIRECTION('ref_axis',(1.,0.,0.));
#61327=DIRECTION('',(0.,0.,-1.));
#61328=DIRECTION('center_axis',(0.,0.,-1.));
#61329=DIRECTION('ref_axis',(-1.,0.,0.));
#61330=DIRECTION('center_axis',(0.,0.,-1.));
#61331=DIRECTION('ref_axis',(-1.,0.,0.));
#61332=DIRECTION('',(0.,0.,1.));
#61333=DIRECTION('center_axis',(0.,0.,1.));
#61334=DIRECTION('ref_axis',(1.,0.,0.));
#61335=DIRECTION('',(0.,0.,-1.));
#61336=DIRECTION('center_axis',(-4.08908562752743E-48,1.,2.5571182003049E-32));
#61337=DIRECTION('ref_axis',(1.,8.50802870020078E-63,1.59909918401107E-16));
#61338=DIRECTION('',(1.01043442692316E-14,1.E-14,1.));
#61339=DIRECTION('',(0.984628016341329,1.01574517857485E-14,0.17466444811621));
#61340=DIRECTION('',(0.,0.,1.));
#61341=DIRECTION('',(-0.984628016341329,-1.01574517857485E-14,0.174664448116209));
#61342=DIRECTION('center_axis',(0.,0.,1.));
#61343=DIRECTION('ref_axis',(1.,0.,0.));
#61344=DIRECTION('',(0.,0.,1.));
#61345=DIRECTION('center_axis',(0.,0.,1.));
#61346=DIRECTION('ref_axis',(-1.,0.,0.));
#61347=DIRECTION('',(0.,0.,-1.));
#61348=DIRECTION('center_axis',(0.,0.,1.));
#61349=DIRECTION('ref_axis',(-1.,0.,0.));
#61350=DIRECTION('',(0.,0.,1.));
#61351=DIRECTION('center_axis',(0.,0.,1.));
#61352=DIRECTION('ref_axis',(-1.,0.,0.));
#61353=DIRECTION('center_axis',(0.,0.,1.));
#61354=DIRECTION('ref_axis',(-1.,0.,0.));
#61355=DIRECTION('center_axis',(0.,0.,1.));
#61356=DIRECTION('ref_axis',(1.,0.,0.));
#61357=DIRECTION('',(1.,-1.00901155052454E-14,0.));
#61358=DIRECTION('center_axis',(0.,0.,1.));
#61359=DIRECTION('ref_axis',(-1.,0.,0.));
#61360=DIRECTION('',(0.,-1.,0.));
#61361=DIRECTION('',(0.,1.,0.));
#61362=DIRECTION('center_axis',(0.,0.,1.));
#61363=DIRECTION('ref_axis',(-1.,0.,0.));
#61364=DIRECTION('',(1.0838294844996E-14,1.,0.));
#61365=DIRECTION('',(0.707106781186546,-0.707106781186549,0.));
#61366=DIRECTION('',(0.225189398770639,-0.97431500793189,0.));
#61367=DIRECTION('',(0.,-1.,0.));
#61368=DIRECTION('',(-0.707106781186549,0.707106781186546,0.));
#61369=DIRECTION('',(0.,-1.,0.));
#61370=DIRECTION('center_axis',(0.,0.,-1.));
#61371=DIRECTION('ref_axis',(0.,-1.,0.));
#61372=DIRECTION('',(-0.707106781186551,-0.707106781186544,0.));
#61373=DIRECTION('',(1.,1.0159909918401E-14,0.));
#61374=DIRECTION('',(1.0159909918401E-14,-1.,0.));
#61375=DIRECTION('',(0.,-1.,0.));
#61376=DIRECTION('',(1.,-1.00901155052454E-14,0.));
#61377=DIRECTION('center_axis',(1.60527967783421E-47,7.69222732429044E-32,
1.));
#61378=DIRECTION('ref_axis',(1.,-2.08688538463375E-16,-3.50729211666941E-63));
#61379=DIRECTION('',(-0.707106781186551,-0.707106781186544,0.));
#61380=DIRECTION('',(1.,-1.00901155052454E-14,0.));
#61381=DIRECTION('',(0.,-1.,0.));
#61382=DIRECTION('',(1.0159909918401E-14,-1.,0.));
#61383=DIRECTION('',(-1.,-1.0159909918401E-14,1.02086885384633E-14));
#61384=DIRECTION('center_axis',(-0.707106781186549,0.707106781186546,0.));
#61385=DIRECTION('ref_axis',(0.,0.,1.));
#61386=DIRECTION('',(0.,0.,-1.));
#61387=DIRECTION('',(0.701608823197059,0.701608823197062,-0.124459304288878));
#61388=DIRECTION('',(0.,0.,-1.));
#61389=DIRECTION('',(-0.707106781186546,-0.707106781186549,0.));
#61390=DIRECTION('center_axis',(0.,0.,-1.));
#61391=DIRECTION('ref_axis',(0.,-1.,0.));
#61392=DIRECTION('center_axis',(0.,0.,1.));
#61393=DIRECTION('ref_axis',(-1.,-6.4252467419967E-13,0.));
#61394=DIRECTION('',(-1.10484358065218E-14,-1.,0.));
#61395=DIRECTION('center_axis',(0.,0.,1.));
#61396=DIRECTION('ref_axis',(-1.,0.,0.));
#61397=DIRECTION('',(0.640406508926595,-0.768036134126807,0.));
#61398=DIRECTION('center_axis',(0.,0.,-1.));
#61399=DIRECTION('ref_axis',(-1.,0.,0.));
#61400=DIRECTION('',(-1.15041237245925E-14,-1.,0.));
#61401=DIRECTION('center_axis',(0.,0.,1.));
#61402=DIRECTION('ref_axis',(1.,0.,0.));
#61403=DIRECTION('',(0.707106781186548,-0.707106781186547,0.));
#61404=DIRECTION('center_axis',(0.,0.,1.));
#61405=DIRECTION('ref_axis',(-1.,0.,0.));
#61406=DIRECTION('center_axis',(0.,0.,-1.));
#61407=DIRECTION('ref_axis',(-1.,0.,0.));
#61408=DIRECTION('center_axis',(0.,0.,-1.));
#61409=DIRECTION('ref_axis',(-1.,0.,0.));
#61410=DIRECTION('',(0.,0.,-1.));
#61411=DIRECTION('center_axis',(0.,0.,1.));
#61412=DIRECTION('ref_axis',(-1.,0.,0.));
#61413=DIRECTION('center_axis',(0.,0.,-1.));
#61414=DIRECTION('ref_axis',(-1.,0.,0.));
#61415=DIRECTION('center_axis',(0.,0.,1.));
#61416=DIRECTION('ref_axis',(1.,0.,0.));
#61417=DIRECTION('center_axis',(0.,0.,1.));
#61418=DIRECTION('ref_axis',(-1.,0.,0.));
#61419=DIRECTION('',(0.,0.,1.));
#61420=DIRECTION('center_axis',(0.,-1.,0.));
#61421=DIRECTION('ref_axis',(0.,0.,-1.));
#61422=DIRECTION('',(-1.,0.,0.));
#61423=DIRECTION('',(0.,0.,-1.));
#61424=DIRECTION('',(-1.,0.,0.));
#61425=DIRECTION('center_axis',(0.,-1.,0.));
#61426=DIRECTION('ref_axis',(0.,0.,-1.));
#61427=DIRECTION('',(-1.,0.,0.));
#61428=DIRECTION('',(0.,0.,-1.));
#61429=DIRECTION('',(-1.,0.,0.));
#61430=DIRECTION('',(0.,0.,-1.));
#61431=DIRECTION('',(-1.,1.0031973271849E-14,0.));
#61432=DIRECTION('',(0.,0.,1.));
#61433=DIRECTION('center_axis',(0.,0.,-1.));
#61434=DIRECTION('ref_axis',(0.,-1.,0.));
#61435=DIRECTION('',(0.,1.,0.));
#61436=DIRECTION('',(-0.707106781186547,0.707106781186548,0.));
#61437=DIRECTION('',(-1.,0.,0.));
#61438=DIRECTION('',(-0.707106781186548,-0.707106781186548,0.));
#61439=DIRECTION('',(-1.0000695223269E-14,-1.,0.));
#61440=DIRECTION('',(0.707106781186547,-0.707106781186548,0.));
#61441=DIRECTION('',(1.,1.0159909918401E-14,0.));
#61442=DIRECTION('',(0.707106781186546,0.707106781186549,0.));
#61443=DIRECTION('',(0.,-1.,0.));
#61444=DIRECTION('',(-0.309086072337564,-0.951034068730946,0.));
#61445=DIRECTION('',(-1.,0.,0.));
#61446=DIRECTION('',(-0.309086072337565,0.951034068730946,0.));
#61447=DIRECTION('',(0.,1.,0.));
#61448=DIRECTION('',(0.309086072337565,0.951034068730946,0.));
#61449=DIRECTION('',(1.,0.,0.));
#61450=DIRECTION('',(0.309086072337564,-0.951034068730946,0.));
#61451=DIRECTION('center_axis',(0.,0.,-1.));
#61452=DIRECTION('ref_axis',(0.,-1.,0.));
#61453=DIRECTION('',(-0.707106781186547,-0.707106781186548,0.));
#61454=DIRECTION('',(1.0159909918401E-14,-1.,0.));
#61455=DIRECTION('',(1.,1.0159909918401E-14,0.));
#61456=DIRECTION('',(0.707106781186547,-0.707106781186548,0.));
#61457=DIRECTION('',(-1.0000695223269E-14,-1.,0.));
#61458=DIRECTION('',(-0.707106781186548,-0.707106781186548,0.));
#61459=DIRECTION('',(-1.,0.,0.));
#61460=DIRECTION('',(-0.707106781186547,0.707106781186548,0.));
#61461=DIRECTION('',(1.0838294844996E-14,1.,0.));
#61462=DIRECTION('center_axis',(0.,0.,-1.));
#61463=DIRECTION('ref_axis',(1.,0.,0.));
#61464=DIRECTION('',(-0.640406508926594,0.768036134126808,0.));
#61465=DIRECTION('center_axis',(0.,0.,1.));
#61466=DIRECTION('ref_axis',(-1.,0.,0.));
#61467=DIRECTION('',(-1.15041237245925E-14,1.,0.));
#61468=DIRECTION('center_axis',(0.,0.,-1.));
#61469=DIRECTION('ref_axis',(-1.,0.,0.));
#61470=DIRECTION('',(-0.707106781186549,0.707106781186546,0.));
#61471=DIRECTION('',(1.0159909918401E-14,-1.,0.));
#61472=DIRECTION('',(0.707106781186548,-0.707106781186547,0.));
#61473=DIRECTION('center_axis',(0.,0.,1.));
#61474=DIRECTION('ref_axis',(1.,0.,0.));
#61475=DIRECTION('',(-1.15041237245925E-14,-1.,0.));
#61476=DIRECTION('center_axis',(0.,0.,-1.));
#61477=DIRECTION('ref_axis',(-1.,0.,0.));
#61478=DIRECTION('',(0.640406508926595,-0.768036134126807,0.));
#61479=DIRECTION('center_axis',(0.,0.,1.));
#61480=DIRECTION('ref_axis',(-1.,0.,0.));
#61481=DIRECTION('',(-1.10484358065218E-14,-1.,0.));
#61482=DIRECTION('',(1.,0.,0.));
#61483=DIRECTION('center_axis',(0.,0.,1.));
#61484=DIRECTION('ref_axis',(-1.,0.,0.));
#61485=DIRECTION('',(1.01439313087194E-14,1.,0.));
#61486=DIRECTION('center_axis',(0.,0.,1.));
#61487=DIRECTION('ref_axis',(-1.,0.,0.));
#61488=DIRECTION('center_axis',(0.,0.,-1.));
#61489=DIRECTION('ref_axis',(-1.,0.,0.));
#61490=DIRECTION('center_axis',(0.707106781186548,0.707106781186548,0.));
#61491=DIRECTION('ref_axis',(0.,0.,-1.));
#61492=DIRECTION('',(0.,0.,-1.));
#61493=DIRECTION('',(-0.707106781186547,0.707106781186548,0.));
#61494=DIRECTION('',(0.,0.,-1.));
#61495=DIRECTION('center_axis',(-4.08908562752742E-48,1.,2.55711820030489E-32));
#61496=DIRECTION('ref_axis',(1.,1.39774757217584E-62,1.59909918401107E-16));
#61497=DIRECTION('',(-0.984628016341329,-1.01574517857485E-14,0.174664448116209));
#61498=DIRECTION('',(-1.,-1.0159909918401E-14,0.));
#61499=DIRECTION('',(0.,0.,-1.));
#61500=DIRECTION('',(0.984628016341329,1.01574517857485E-14,0.17466444811621));
#61501=DIRECTION('',(0.,0.,-1.));
#61502=DIRECTION('center_axis',(-0.707106781186549,0.707106781186546,0.));
#61503=DIRECTION('ref_axis',(0.,0.,1.));
#61504=DIRECTION('',(0.,0.,-1.));
#61505=DIRECTION('',(-0.701608823197059,-0.701608823197062,-0.124459304288878));
#61506=DIRECTION('',(0.577350269189623,0.577350269189625,0.577350269189629));
#61507=DIRECTION('center_axis',(-1.,0.,0.));
#61508=DIRECTION('ref_axis',(0.,0.,1.));
#61509=DIRECTION('',(1.0159909918401E-14,-1.,0.));
#61510=DIRECTION('',(1.0159909918401E-14,-1.,0.));
#61511=DIRECTION('',(1.0159909918401E-14,-1.,0.));
#61512=DIRECTION('',(0.,0.,-1.));
#61513=DIRECTION('',(0.,0.,-1.));
#61514=DIRECTION('',(0.,-1.,0.));
#61515=DIRECTION('center_axis',(-0.974315007931891,-0.225189398770632,0.));
#61516=DIRECTION('ref_axis',(-0.225189398770632,0.974315007931891,0.));
#61517=DIRECTION('',(0.,0.,-1.));
#61518=DIRECTION('',(0.1989949751698,-0.860980986979965,0.468094798001619));
#61519=DIRECTION('',(0.219688060005901,-0.950512657770367,-0.219688060005904));
#61520=DIRECTION('center_axis',(-0.707106781186549,-0.707106781186547,0.));
#61521=DIRECTION('ref_axis',(-0.707106781186547,0.707106781186549,0.));
#61522=DIRECTION('',(0.,0.,-1.));
#61523=DIRECTION('',(0.,0.,-1.));
#61524=DIRECTION('',(0.707106781186547,-0.707106781186548,0.));
#61525=DIRECTION('center_axis',(0.,-1.,0.));
#61526=DIRECTION('ref_axis',(0.,0.,-1.));
#61527=DIRECTION('',(0.,0.,-1.));
#61528=DIRECTION('',(1.,0.,0.));
#61529=DIRECTION('center_axis',(0.707106781186548,-0.707106781186548,0.));
#61530=DIRECTION('ref_axis',(0.,0.,-1.));
#61531=DIRECTION('',(0.,0.,-1.));
#61532=DIRECTION('',(0.707106781186548,0.707106781186548,0.));
#61533=DIRECTION('center_axis',(1.,-6.95223269150415E-19,0.));
#61534=DIRECTION('ref_axis',(0.,0.,1.));
#61535=DIRECTION('',(1.0000695223269E-14,1.,0.));
#61536=DIRECTION('center_axis',(0.500000000000001,0.500000000000001,-0.707106781186546));
#61537=DIRECTION('ref_axis',(-1.20310517779348E-15,-0.816496580927725,-0.577350269189628));
#61538=DIRECTION('',(0.678598344545843,0.281084637714825,0.67859834454585));
#61539=DIRECTION('',(-0.281084637714825,-0.678598344545842,-0.67859834454585));
#61540=DIRECTION('center_axis',(-1.13073387680411E-16,0.707106781186552,
-0.707106781186544));
#61541=DIRECTION('ref_axis',(-1.,1.02474602976116E-31,1.59909918401109E-16));
#61542=DIRECTION('',(0.28108463771482,-0.678598344545843,-0.678598344545851));
#61543=DIRECTION('center_axis',(0.707106781186552,-4.91597088054941E-19,
-0.707106781186544));
#61544=DIRECTION('ref_axis',(4.41380838164238E-34,-1.,6.95223269150422E-19));
#61545=DIRECTION('',(0.678598344545842,-0.281084637714827,0.67859834454585));
#61546=DIRECTION('center_axis',(-0.500000000000002,0.500000000000002,-0.707106781186545));
#61547=DIRECTION('ref_axis',(-0.816496580927723,2.47688303890596E-15,0.57735026918963));
#61548=DIRECTION('',(0.678598344545844,-0.281084637714819,-0.678598344545851));
#61549=DIRECTION('center_axis',(0.500000000000001,-0.500000000000001,-0.707106781186546));
#61550=DIRECTION('ref_axis',(8.28813430912774E-16,-0.816496580927725,0.577350269189628));
#61551=DIRECTION('',(0.281084637714827,-0.678598344545842,0.67859834454585));
#61552=DIRECTION('center_axis',(-0.707106781186552,0.,-0.707106781186544));
#61553=DIRECTION('ref_axis',(-0.707106781186544,0.,0.707106781186552));
#61554=DIRECTION('',(0.678598344545843,0.281084637714824,-0.67859834454585));
#61555=DIRECTION('center_axis',(0.,-0.707106781186552,-0.707106781186544));
#61556=DIRECTION('ref_axis',(0.,0.707106781186544,-0.707106781186552));
#61557=DIRECTION('',(-0.281084637714825,-0.678598344545843,0.67859834454585));
#61558=DIRECTION('center_axis',(-0.500000000000001,-0.500000000000001,-0.707106781186546));
#61559=DIRECTION('ref_axis',(-0.816496580927724,-1.85046612426036E-15,0.577350269189628));
#61560=DIRECTION('center_axis',(0.,0.,1.));
#61561=DIRECTION('ref_axis',(1.,0.,0.));
#61562=DIRECTION('center_axis',(0.,0.,1.));
#61563=DIRECTION('ref_axis',(1.,0.,0.));
#61564=DIRECTION('center_axis',(0.,0.,1.));
#61565=DIRECTION('ref_axis',(1.,0.,0.));
#61566=DIRECTION('center_axis',(-0.707106781186546,-0.707106781186549,0.));
#61567=DIRECTION('ref_axis',(-0.707106781186549,0.707106781186546,0.));
#61568=DIRECTION('',(-0.577350269189625,0.577350269189622,-0.577350269189631));
#61569=DIRECTION('',(0.,0.,-1.));
#61570=DIRECTION('',(0.707106781186549,-0.707106781186546,0.));
#61571=DIRECTION('center_axis',(0.,0.,-1.));
#61572=DIRECTION('ref_axis',(-1.,0.,0.));
#61573=DIRECTION('',(0.,0.,-1.));
#61574=DIRECTION('center_axis',(0.,0.,1.));
#61575=DIRECTION('ref_axis',(-1.,-3.33694734056382E-12,0.));
#61576=DIRECTION('center_axis',(-1.,-1.50412372459265E-15,0.));
#61577=DIRECTION('ref_axis',(-1.50412372459265E-15,1.,0.));
#61578=DIRECTION('',(0.,0.,-1.));
#61579=DIRECTION('',(1.15041237245925E-14,-1.,0.));
#61580=DIRECTION('center_axis',(0.,0.,-1.));
#61581=DIRECTION('ref_axis',(-1.,0.,0.));
#61582=DIRECTION('',(0.,0.,-1.));
#61583=DIRECTION('center_axis',(0.,0.,-1.));
#61584=DIRECTION('ref_axis',(-1.,0.,0.));
#61585=DIRECTION('center_axis',(-0.768036134126809,-0.640406508926593,0.));
#61586=DIRECTION('ref_axis',(-0.640406508926593,0.768036134126809,0.));
#61587=DIRECTION('',(0.,0.,-1.));
#61588=DIRECTION('',(0.640406508926594,-0.768036134126808,0.));
#61589=DIRECTION('center_axis',(0.,0.,-1.));
#61590=DIRECTION('ref_axis',(-1.,0.,0.));
#61591=DIRECTION('',(0.,0.,-1.));
#61592=DIRECTION('center_axis',(0.,0.,1.));
#61593=DIRECTION('ref_axis',(-1.,0.,0.));
#61594=DIRECTION('center_axis',(-1.,8.38294844996084E-16,0.));
#61595=DIRECTION('ref_axis',(0.,0.,1.));
#61596=DIRECTION('',(0.,0.,-1.));
#61597=DIRECTION('',(-1.0838294844996E-14,-1.,0.));
#61598=DIRECTION('center_axis',(0.,0.,1.));
#61599=DIRECTION('ref_axis',(1.,0.,0.));
#61600=DIRECTION('',(0.,0.,1.));
#61601=DIRECTION('center_axis',(0.,0.,1.));
#61602=DIRECTION('ref_axis',(-1.,0.,0.));
#61603=DIRECTION('center_axis',(0.,0.,-1.));
#61604=DIRECTION('ref_axis',(0.,-1.,0.));
#61605=DIRECTION('',(0.,1.,0.));
#61606=DIRECTION('',(0.,-1.,0.));
#61607=DIRECTION('center_axis',(1.,0.,0.));
#61608=DIRECTION('ref_axis',(0.,1.,0.));
#61609=DIRECTION('center_axis',(-1.,0.,0.));
#61610=DIRECTION('ref_axis',(0.,0.,1.));
#61611=DIRECTION('center_axis',(0.,1.,0.));
#61612=DIRECTION('ref_axis',(1.,0.,0.));
#61613=DIRECTION('',(1.,0.,0.));
#61614=DIRECTION('',(0.,0.,-1.));
#61615=DIRECTION('center_axis',(0.,0.,-1.));
#61616=DIRECTION('ref_axis',(0.707106781186543,-0.707106781186553,0.));
#61617=DIRECTION('center_axis',(0.,0.,1.));
#61618=DIRECTION('ref_axis',(-1.,0.,0.));
#61619=DIRECTION('',(0.,0.,-1.));
#61620=DIRECTION('center_axis',(-1.,1.43931308719534E-16,0.));
#61621=DIRECTION('ref_axis',(0.,0.,1.));
#61622=DIRECTION('',(1.02398855145324E-14,1.,0.));
#61623=DIRECTION('',(0.,0.,-1.));
#61624=DIRECTION('center_axis',(0.,0.,-1.));
#61625=DIRECTION('ref_axis',(0.707106781186539,0.707106781186556,0.));
#61626=DIRECTION('center_axis',(0.,0.,1.));
#61627=DIRECTION('ref_axis',(1.,0.,0.));
#61628=DIRECTION('center_axis',(0.707106781186548,-0.707106781186547,0.));
#61629=DIRECTION('ref_axis',(0.,0.,-1.));
#61630=DIRECTION('',(0.,0.,-1.));
#61631=DIRECTION('',(-0.577350269189624,-0.577350269189624,-0.57735026918963));
#61632=DIRECTION('',(-0.707106781186547,-0.707106781186548,0.));
#61633=DIRECTION('center_axis',(1.,0.,0.));
#61634=DIRECTION('ref_axis',(0.,1.,0.));
#61635=DIRECTION('',(0.,0.,-1.));
#61636=DIRECTION('',(0.,-1.,-1.0159909918401E-14));
#61637=DIRECTION('',(0.,-1.,0.));
#61638=DIRECTION('center_axis',(0.707106781186547,0.707106781186548,0.));
#61639=DIRECTION('ref_axis',(0.,0.,-1.));
#61640=DIRECTION('',(0.577350269189624,-0.577350269189624,0.57735026918963));
#61641=DIRECTION('',(0.707106781186548,-0.707106781186547,0.));
#61642=DIRECTION('',(0.,0.,-1.));
#61643=DIRECTION('',(0.,0.,-1.));
#61644=DIRECTION('center_axis',(0.,0.,-1.));
#61645=DIRECTION('ref_axis',(-1.,0.,0.));
#61646=DIRECTION('',(0.,0.,-1.));
#61647=DIRECTION('center_axis',(1.,-1.50412372459265E-15,0.));
#61648=DIRECTION('ref_axis',(0.,0.,1.));
#61649=DIRECTION('',(0.,0.,-1.));
#61650=DIRECTION('center_axis',(0.,0.,-1.));
#61651=DIRECTION('ref_axis',(-1.,0.,0.));
#61652=DIRECTION('',(0.,0.,-1.));
#61653=DIRECTION('center_axis',(0.768036134126808,0.640406508926594,0.));
#61654=DIRECTION('ref_axis',(0.,0.,-1.));
#61655=DIRECTION('',(0.,0.,-1.));
#61656=DIRECTION('center_axis',(0.,0.,-1.));
#61657=DIRECTION('ref_axis',(-1.,0.,0.));
#61658=DIRECTION('',(0.,0.,-1.));
#61659=DIRECTION('center_axis',(1.,-1.0484358065219E-15,0.));
#61660=DIRECTION('ref_axis',(0.,0.,1.));
#61661=DIRECTION('center_axis',(-0.707106781186551,-1.13073387680411E-16,
0.707106781186544));
#61662=DIRECTION('ref_axis',(-1.59909918401107E-16,1.,2.60143314432367E-31));
#61663=DIRECTION('center_axis',(0.,0.,1.));
#61664=DIRECTION('ref_axis',(-0.914066015001456,-0.405565432722463,0.));
#61665=DIRECTION('center_axis',(0.,0.,1.));
#61666=DIRECTION('ref_axis',(-1.,0.,0.));
#61667=DIRECTION('center_axis',(0.,0.,-1.));
#61668=DIRECTION('ref_axis',(0.,-1.,0.));
#61669=DIRECTION('center_axis',(0.,0.,1.));
#61670=DIRECTION('ref_axis',(1.,0.,0.));
#61671=DIRECTION('',(0.766044443118981,0.642787609686536,0.));
#61672=DIRECTION('center_axis',(0.,0.,-1.));
#61673=DIRECTION('ref_axis',(0.,-1.,0.));
#61674=DIRECTION('center_axis',(0.,0.,-1.));
#61675=DIRECTION('ref_axis',(0.,-1.,0.));
#61676=DIRECTION('center_axis',(0.,0.,-1.));
#61677=DIRECTION('ref_axis',(0.,-1.,0.));
#61678=DIRECTION('center_axis',(-0.951034068730948,0.309086072337558,0.));
#61679=DIRECTION('ref_axis',(0.,0.,1.));
#61680=DIRECTION('',(0.,0.,1.));
#61681=DIRECTION('',(-0.309086072337564,-0.951034068730946,0.));
#61682=DIRECTION('',(0.,0.,1.));
#61683=DIRECTION('center_axis',(0.,1.,0.));
#61684=DIRECTION('ref_axis',(1.,0.,0.));
#61685=DIRECTION('',(-1.,0.,0.));
#61686=DIRECTION('',(0.,0.,1.));
#61687=DIRECTION('center_axis',(0.951034068730948,0.309086072337558,0.));
#61688=DIRECTION('ref_axis',(0.,0.,-1.));
#61689=DIRECTION('',(-0.309086072337565,0.951034068730946,0.));
#61690=DIRECTION('',(0.,0.,1.));
#61691=DIRECTION('center_axis',(1.,0.,0.));
#61692=DIRECTION('ref_axis',(0.,1.,0.));
#61693=DIRECTION('',(0.,1.,0.));
#61694=DIRECTION('',(0.,0.,1.));
#61695=DIRECTION('center_axis',(0.951034068730948,-0.309086072337558,0.));
#61696=DIRECTION('ref_axis',(0.,0.,-1.));
#61697=DIRECTION('',(0.309086072337565,0.951034068730946,0.));
#61698=DIRECTION('',(0.,0.,1.));
#61699=DIRECTION('center_axis',(0.,-1.,0.));
#61700=DIRECTION('ref_axis',(0.,0.,-1.));
#61701=DIRECTION('',(1.,0.,0.));
#61702=DIRECTION('',(0.,0.,1.));
#61703=DIRECTION('center_axis',(-0.951034068730948,-0.309086072337558,0.));
#61704=DIRECTION('ref_axis',(-0.309086072337558,0.951034068730948,0.));
#61705=DIRECTION('',(0.309086072337564,-0.951034068730946,0.));
#61706=DIRECTION('',(0.,0.,1.));
#61707=DIRECTION('center_axis',(-1.,0.,0.));
#61708=DIRECTION('ref_axis',(0.,0.,1.));
#61709=DIRECTION('',(0.,-1.,0.));
#61710=DIRECTION('center_axis',(0.,0.,-1.));
#61711=DIRECTION('ref_axis',(0.,-1.,0.));
#61712=DIRECTION('center_axis',(0.,0.,-1.));
#61713=DIRECTION('ref_axis',(-1.,0.,0.));
#61714=DIRECTION('center_axis',(0.,0.,1.));
#61715=DIRECTION('ref_axis',(-1.,0.,0.));
#61716=DIRECTION('center_axis',(0.,0.,-1.));
#61717=DIRECTION('ref_axis',(0.,-1.,0.));
#61718=DIRECTION('center_axis',(0.642787609686535,-0.766044443118982,0.));
#61719=DIRECTION('ref_axis',(0.,0.,-1.));
#61720=DIRECTION('',(-0.766044443118981,-0.642787609686536,0.));
#61721=DIRECTION('',(0.,0.,-1.));
#61722=DIRECTION('',(0.766044443118981,0.642787609686536,0.));
#61723=DIRECTION('',(0.,0.,1.));
#61724=DIRECTION('',(-0.766044443118981,-0.642787609686536,0.));
#61725=DIRECTION('center_axis',(0.,0.,-1.));
#61726=DIRECTION('ref_axis',(-1.,0.,0.));
#61727=DIRECTION('center_axis',(0.,0.,1.));
#61728=DIRECTION('ref_axis',(1.,0.,0.));
#61729=DIRECTION('center_axis',(0.,0.,-1.));
#61730=DIRECTION('ref_axis',(0.,-1.,0.));
#61731=DIRECTION('',(-1.0159909918401E-14,1.,0.));
#61732=DIRECTION('',(1.,1.0159909918401E-14,0.));
#61733=DIRECTION('center_axis',(0.174664448116201,2.79305776458362E-17,
0.98462801634133));
#61734=DIRECTION('ref_axis',(1.59909918401107E-16,-1.,1.11324494830527E-31));
#61735=DIRECTION('center_axis',(0.174664448116202,2.79305776458363E-17,
-0.98462801634133));
#61736=DIRECTION('ref_axis',(1.74870334563606E-32,-1.,-2.8366629003327E-17));
#61737=DIRECTION('center_axis',(-0.707106781186544,0.707106781186551,7.37825403516808E-17));
#61738=DIRECTION('ref_axis',(1.04344269231688E-16,3.03340043204828E-31,
1.));
#61739=DIRECTION('',(1.01043442692316E-14,1.E-14,1.));
#61740=DIRECTION('center_axis',(0.,0.,-1.));
#61741=DIRECTION('ref_axis',(0.,-1.,0.));
#61742=DIRECTION('',(0.,1.,0.));
#61743=DIRECTION('',(1.,1.13010426069825E-14,0.));
#61744=DIRECTION('center_axis',(1.,0.,-1.04344269231688E-16));
#61745=DIRECTION('ref_axis',(0.,1.,0.));
#61746=DIRECTION('',(1.01043442692316E-14,1.E-14,1.));
#61747=DIRECTION('center_axis',(1.30104260698259E-15,-1.,-1.19070656486426E-31));
#61748=DIRECTION('ref_axis',(1.04509199371491E-63,1.19070656486426E-31,
-1.));
#61749=DIRECTION('center_axis',(-9.01155052455486E-17,-1.,2.60887201197534E-32));
#61750=DIRECTION('ref_axis',(-1.,9.01155052455486E-17,0.));
#61751=DIRECTION('',(1.01043442692316E-14,1.E-14,1.));
#61752=DIRECTION('center_axis',(-1.,0.,1.04344269231688E-16));
#61753=DIRECTION('ref_axis',(0.,1.,0.));
#61754=DIRECTION('center_axis',(1.,0.,0.));
#61755=DIRECTION('ref_axis',(0.,1.,0.));
#61756=DIRECTION('center_axis',(1.,0.,0.));
#61757=DIRECTION('ref_axis',(0.,1.,0.));
#61758=DIRECTION('center_axis',(-1.,0.,0.));
#61759=DIRECTION('ref_axis',(0.,0.,1.));
#61760=DIRECTION('',(0.,0.,-1.));
#61761=DIRECTION('',(0.,0.,1.));
#61762=DIRECTION('center_axis',(-1.,0.,0.));
#61763=DIRECTION('ref_axis',(0.,1.89882151931499E-15,-1.));
#61764=DIRECTION('center_axis',(-1.,0.,0.));
#61765=DIRECTION('ref_axis',(0.,0.,1.));
#61766=DIRECTION('',(1.,0.,0.));
#61767=DIRECTION('',(-1.,0.,0.));
#61768=DIRECTION('center_axis',(-1.,0.,0.));
#61769=DIRECTION('ref_axis',(0.,0.,1.));
#61770=DIRECTION('',(0.,0.,1.));
#61771=DIRECTION('',(0.,0.,-1.));
#61772=DIRECTION('center_axis',(0.,1.,0.));
#61773=DIRECTION('ref_axis',(1.,0.,0.));
#61774=DIRECTION('center_axis',(0.,-1.,0.));
#61775=DIRECTION('ref_axis',(0.,0.,-1.));
#61776=DIRECTION('',(6.0876171481807E-5,-0.999999998147046,-8.56383677439378E-17));
#61777=DIRECTION('',(-3.19183904829461E-16,-8.56577985967824E-17,1.));
#61778=DIRECTION('',(6.0876171481807E-5,-0.999999998147046,-8.56383677439378E-17));
#61779=DIRECTION('',(-3.19183904829461E-16,-8.56577985967824E-17,1.));
#61780=DIRECTION('',(6.0876171481807E-5,-0.999999998147046,-8.56383677439378E-17));
#61781=DIRECTION('',(-3.19183904829461E-16,-8.56577985967824E-17,1.));
#61782=DIRECTION('',(6.0876171481807E-5,-0.999999998147046,-8.56383677439378E-17));
#61783=DIRECTION('',(-3.19183904829461E-16,-8.56577985967824E-17,1.));
#61784=DIRECTION('',(6.0876171481807E-5,-0.999999998147046,-8.56383677439378E-17));
#61785=DIRECTION('',(-3.19183904829461E-16,-8.56577985967824E-17,1.));
#61786=DIRECTION('',(6.0876171481807E-5,-0.999999998147046,-8.56383677439378E-17));
#61787=DIRECTION('',(-3.19183904829461E-16,-8.56577985967824E-17,1.));
#61788=DIRECTION('',(6.0876171481807E-5,-0.999999998147046,-8.56383677439378E-17));
#61789=DIRECTION('',(-3.19183904829461E-16,-8.56577985967824E-17,1.));
#61790=DIRECTION('',(6.0876171481807E-5,-0.999999998147046,-8.56383677439378E-17));
#61791=DIRECTION('',(-3.19183904829461E-16,-8.56577985967824E-17,1.));
#61792=DIRECTION('',(6.0876171481807E-5,-0.999999998147046,-8.56383677439378E-17));
#61793=DIRECTION('',(-3.19183904829461E-16,-8.56577985967824E-17,1.));
#61794=DIRECTION('',(6.0876171481807E-5,-0.999999998147046,-8.56383677439378E-17));
#61795=DIRECTION('',(-3.19183904829461E-16,-8.56577985967824E-17,1.));
#61796=CARTESIAN_POINT('',(0.,0.,0.));
#61797=CARTESIAN_POINT('',(0.,0.,0.));
#61798=CARTESIAN_POINT('Origin',(0.00812378219310841,-0.0211741814719619,
0.07415));
#61799=CARTESIAN_POINT('',(0.00962378219312842,-0.0211741814719719,0.07415000000001));
#61800=CARTESIAN_POINT('Origin',(0.00812378219311841,-0.0211741814719719,
0.07415000000001));
#61801=CARTESIAN_POINT('',(0.00962378219312842,-0.0201741814719718,0.07415000000001));
#61802=CARTESIAN_POINT('',(0.00962378219310841,-0.0211741814719619,0.07415));
#61803=CARTESIAN_POINT('Origin',(0.00812378219311841,-0.0201741814719718,
0.07415000000001));
#61804=CARTESIAN_POINT('Origin',(0.00812378219310841,-0.0211741814719619,
0.07415));
#61805=CARTESIAN_POINT('',(0.0121237821931284,-0.0201741814719718,0.07415000000001));
#61806=CARTESIAN_POINT('Origin',(0.00812378219311841,-0.0201741814719718,
0.07415000000001));
#61807=CARTESIAN_POINT('',(0.0121237821931284,-0.0211741814719719,0.07415000000001));
#61808=CARTESIAN_POINT('',(0.0121237821931084,-0.0211741814719619,0.07415));
#61809=CARTESIAN_POINT('Origin',(0.00812378219311841,-0.0211741814719719,
0.07415000000001));
#61810=CARTESIAN_POINT('Origin',(0.00812378219310841,-0.0211741814719619,
0.07415));
#61811=CARTESIAN_POINT('Origin',(0.00812378219310841,-0.0201741814719619,
0.07415));
#61812=CARTESIAN_POINT('',(0.,0.,0.));
#61813=CARTESIAN_POINT('Ctrl Pts',(0.00815067148752137,-0.0203072579114564,
0.0762656663521488));
#61814=CARTESIAN_POINT('Ctrl Pts',(0.0083771381325318,-0.0203255606965017,
0.0762649347079084));
#61815=CARTESIAN_POINT('Ctrl Pts',(0.00860198035030984,-0.0203438634815471,
0.0762288078613937));
#61816=CARTESIAN_POINT('Ctrl Pts',(0.00953656982276594,-0.0204246662665928,
0.0759073888491967));
#61817=CARTESIAN_POINT('Ctrl Pts',(0.0100801851138304,-0.0204871662665918,
0.0752518676024789));
#61818=CARTESIAN_POINT('Ctrl Pts',(0.0103422385382883,-0.0206121662665931,
0.0738034800723812));
#61819=CARTESIAN_POINT('Ctrl Pts',(0.0100648920002843,-0.020674666266593,
0.0730378901277388));
#61820=CARTESIAN_POINT('Ctrl Pts',(0.00900362893656076,-0.0207996662665919,
0.0720931661776728));
#61821=CARTESIAN_POINT('Ctrl Pts',(0.008241028020177,-0.0208621662665925,
0.0719231783970233));
#61822=CARTESIAN_POINT('Ctrl Pts',(0.00691275415584957,-0.0209871662665924,
0.0722775972279668));
#61823=CARTESIAN_POINT('Ctrl Pts',(0.00636364311727103,-0.0210496662665924,
0.0727913084945308));
#61824=CARTESIAN_POINT('Ctrl Pts',(0.00590286642913209,-0.0211746662665925,
0.0740419937307385));
#61825=CARTESIAN_POINT('Ctrl Pts',(0.00599202908596152,-0.0212371662665924,
0.0747620631556615));
#61826=CARTESIAN_POINT('Ctrl Pts',(0.00669689975963152,-0.0213621662665925,
0.0758479396774564));
#61827=CARTESIAN_POINT('Ctrl Pts',(0.00730138706368173,-0.0214246662665922,
0.0762043156608544));
#61828=CARTESIAN_POINT('Ctrl Pts',(0.00855547426588603,-0.0215496662665927,
0.0763202968801402));
#61829=CARTESIAN_POINT('Ctrl Pts',(0.00919252612250013,-0.0216121662665926,
0.0760823999614819));
#61830=CARTESIAN_POINT('Ctrl Pts',(0.0100589999732895,-0.0217371662665924,
0.075213633090309));
#61831=CARTESIAN_POINT('Ctrl Pts',(0.0102830084237745,-0.0217996662665926,
0.0745926208223076));
#61832=CARTESIAN_POINT('Ctrl Pts',(0.0101959629269755,-0.0219246662665924,
0.0733988421450626));
#61833=CARTESIAN_POINT('Ctrl Pts',(0.00988830420246689,-0.0219871662665922,
0.0728354269849725));
#61834=CARTESIAN_POINT('Ctrl Pts',(0.00896597799697031,-0.0221121662665928,
0.0721171826520367));
#61835=CARTESIAN_POINT('Ctrl Pts',(0.00835948988205837,-0.022174666266592,
0.0719657358996911));
#61836=CARTESIAN_POINT('Ctrl Pts',(0.00723038395375605,-0.0222996662665929,
0.0721429107222321));
#61837=CARTESIAN_POINT('Ctrl Pts',(0.00671499560243656,-0.0223621662665927,
0.0724683075554325));
#61838=CARTESIAN_POINT('Ctrl Pts',(0.00606901592181546,-0.0224871662665922,
0.0733814268319492));
#61839=CARTESIAN_POINT('Ctrl Pts',(0.00594091088577522,-0.0225496662665926,
0.0739624842354635));
#61840=CARTESIAN_POINT('Ctrl Pts',(0.00612305344798784,-0.0226746662665923,
0.0750428459007938));
#61841=CARTESIAN_POINT('Ctrl Pts',(0.00643067872875265,-0.0227371662665921,
0.0755362893544149));
#61842=CARTESIAN_POINT('Ctrl Pts',(0.00729424742007936,-0.0228621662665928,
0.0761749122408133));
#61843=CARTESIAN_POINT('Ctrl Pts',(0.00784480408877878,-0.0229246662665925,
0.0763178915621161));
#61844=CARTESIAN_POINT('Ctrl Pts',(0.00889151097164585,-0.0230496662665924,
0.0761965031486893));
#61845=CARTESIAN_POINT('Ctrl Pts',(0.00938270763587042,-0.0231121662665924,
0.0759340000649118));
#61846=CARTESIAN_POINT('Ctrl Pts',(0.0100625879641978,-0.0232371662665925,
0.0751542816790953));
#61847=CARTESIAN_POINT('Ctrl Pts',(0.0102490546008787,-0.0232996662665926,
0.0746413589041057));
#61848=CARTESIAN_POINT('Ctrl Pts',(0.0102410178141923,-0.0234246662665924,
0.0736250907589115));
#61849=CARTESIAN_POINT('Ctrl Pts',(0.0100475843126518,-0.0234871662665927,
0.0731260381541277));
#61850=CARTESIAN_POINT('Ctrl Pts',(0.00938855725198137,-0.0236121662665922,
0.0723752164881653));
#61851=CARTESIAN_POINT('Ctrl Pts',(0.0089262758271642,-0.0236746662665927,
0.0721258013564626));
#61852=CARTESIAN_POINT('Ctrl Pts',(0.00795468689116961,-0.0237996662665922,
0.0719791054916663));
#61853=CARTESIAN_POINT('Ctrl Pts',(0.00744911026789867,-0.0238621662665923,
0.0720815291713897));
#61854=CARTESIAN_POINT('Ctrl Pts',(0.00661942895548025,-0.0239871662665926,
0.0725781618664859));
#61855=CARTESIAN_POINT('Ctrl Pts',(0.00629781787585632,-0.0240496662665925,
0.0729699778138594));
#61856=CARTESIAN_POINT('Ctrl Pts',(0.00596869167054677,-0.0241746662665925,
0.07386332441141));
#61857=CARTESIAN_POINT('Ctrl Pts',(0.00596159400885685,-0.0242371662665925,
0.0743616829432692));
#61858=CARTESIAN_POINT('Ctrl Pts',(0.00625226027464946,-0.0243621662665925,
0.0752533010137793));
#61859=CARTESIAN_POINT('Ctrl Pts',(0.0065485129249735,-0.0244246662665925,
0.0756440052932471));
#61860=CARTESIAN_POINT('Ctrl Pts',(0.00731262787164867,-0.0245496662665925,
0.0761638405487234));
#61861=CARTESIAN_POINT('Ctrl Pts',(0.00777792798085125,-0.0246121662665926,
0.0762919438047406));
#61862=CARTESIAN_POINT('Ctrl Pts',(0.00868784969457759,-0.0247371662665924,
0.07624508144423));
#61863=CARTESIAN_POINT('Ctrl Pts',(0.00912998835433636,-0.024799666266592,
0.0760707882292855));
#61864=CARTESIAN_POINT('Ctrl Pts',(0.00982231809848441,-0.024924666266593,
0.07549790728317));
#61865=CARTESIAN_POINT('Ctrl Pts',(0.010071019077723,-0.0249871662665926,
0.0751012030151419));
#61866=CARTESIAN_POINT('Ctrl Pts',(0.0102889821151069,-0.0251121662665924,
0.0742418039415068));
#61867=CARTESIAN_POINT('Ctrl Pts',(0.0102581523851926,-0.0251746662665924,
0.0737813536046464));
#61868=CARTESIAN_POINT('Ctrl Pts',(0.00993809892066803,-0.0252996662665926,
0.0729669145852015));
#61869=CARTESIAN_POINT('Ctrl Pts',(0.00965002750714532,-0.0253621662665928,
0.0726146871985494));
#61870=CARTESIAN_POINT('Ctrl Pts',(0.00892808254078336,-0.0254871662665921,
0.07214009674052));
#61871=CARTESIAN_POINT('Ctrl Pts',(0.00849604407482765,-0.0255496662665926,
0.0720184647612599));
#61872=CARTESIAN_POINT('Ctrl Pts',(0.00764304374228332,-0.0256746662665924,
0.0720402815521564));
#61873=CARTESIAN_POINT('Ctrl Pts',(0.00722389165927775,-0.0257371662665915,
0.0721833149981475));
#61874=CARTESIAN_POINT('Ctrl Pts',(0.00654039915241529,-0.0258621662665935,
0.0726767209970879));
#61875=CARTESIAN_POINT('Ctrl Pts',(0.00627724799864211,-0.0259246662665926,
0.0730258105884879));
#61876=CARTESIAN_POINT('Ctrl Pts',(0.00589186280469173,-0.0260919420154909,
0.0740718608505132));
#61877=CARTESIAN_POINT('Ctrl Pts',(0.00599991759097347,-0.0261967177643892,
0.0748547737082654));
#61878=CARTESIAN_POINT('Ctrl Pts',(0.00685580966361203,-0.0264062692621874,
0.0759938417732247));
#61879=CARTESIAN_POINT('Ctrl Pts',(0.00759343482402584,-0.0265110450110865,
0.0763289629385248));
#61880=CARTESIAN_POINT('Ctrl Pts',(0.00904218730885863,-0.0267205965088817,
0.0761958934123178));
#61881=CARTESIAN_POINT('Ctrl Pts',(0.00972755157183108,-0.0268253722577806,
0.0757250048942655));
#61882=CARTESIAN_POINT('Ctrl Pts',(0.010359884849577,-0.0270349237555792,
0.0743792630330001));
#61883=CARTESIAN_POINT('Ctrl Pts',(0.0102896623256786,-0.0271396995044774,
0.0735275482799331));
#61884=CARTESIAN_POINT('Ctrl Pts',(0.00940073146439328,-0.0273492510022741,
0.0722931522835415));
#61885=CARTESIAN_POINT('Ctrl Pts',(0.00859517611493118,-0.0274540267511745,
0.0719398966766563));
#61886=CARTESIAN_POINT('Ctrl Pts',(0.00705289958900958,-0.0276635782489686,
0.0721600303097132));
#61887=CARTESIAN_POINT('Ctrl Pts',(0.00635232687879448,-0.0277683539978693,
0.0727358184526565));
#61888=CARTESIAN_POINT('Ctrl Pts',(0.00598272505460037,-0.0279255176212164,
0.073875472823177));
#61889=CARTESIAN_POINT('Ctrl Pts',(0.00596897958949985,-0.0279779054956661,
0.0742932638294421));
#61890=CARTESIAN_POINT('Ctrl Pts',(0.00617298034709087,-0.0280826812445643,
0.0750763211850444));
#61891=CARTESIAN_POINT('Ctrl Pts',(0.00639068647810172,-0.0281350691190143,
0.075440160464901));
#61892=CARTESIAN_POINT('Ctrl Pts',(0.00699633121784709,-0.028239844867912,
0.0759930922591544));
#61893=CARTESIAN_POINT('Ctrl Pts',(0.00738340683150901,-0.0282922327423619,
0.0761809264433306));
#61894=CARTESIAN_POINT('Ctrl Pts',(0.00820473003409823,-0.0283970084912602,
0.076310154007468));
#61895=CARTESIAN_POINT('Ctrl Pts',(0.00863746583537968,-0.0284493963657099,
0.0762509280036797));
#61896=CARTESIAN_POINT('Ctrl Pts',(0.00940183247449225,-0.0285541721146081,
0.0758948085378461));
#61897=CARTESIAN_POINT('Ctrl Pts',(0.00973174559026465,-0.028606559989058,
0.0755982633195131));
#61898=CARTESIAN_POINT('Ctrl Pts',(0.0101673721494254,-0.0287113357379557,
0.0748618658679991));
#61899=CARTESIAN_POINT('Ctrl Pts',(0.0102717693088642,-0.0287637236124047,
0.0744233616342778));
#61900=CARTESIAN_POINT('Ctrl Pts',(0.0102064021029961,-0.0288684993613048,
0.0735573200377487));
#61901=CARTESIAN_POINT('Ctrl Pts',(0.0100362994783456,-0.0289208872357529,
0.0731317839731108));
#61902=CARTESIAN_POINT('Ctrl Pts',(0.00947201428442268,-0.0290256629846524,
0.072453899629834));
#61903=CARTESIAN_POINT('Ctrl Pts',(0.00907878062310723,-0.0290780508591023,
0.0722035268267701));
#61904=CARTESIAN_POINT('Ctrl Pts',(0.00821001945932422,-0.0291828266079989,
0.0719835875408627));
#61905=CARTESIAN_POINT('Ctrl Pts',(0.00773657577545569,-0.0292352144824501,
0.0720151544508798));
#61906=CARTESIAN_POINT('Ctrl Pts',(0.00689428236856863,-0.0293399902313469,
0.0723623130857159));
#61907=CARTESIAN_POINT('Ctrl Pts',(0.00652798278812114,-0.029392378105796,
0.0726775538261953));
#61908=CARTESIAN_POINT('Ctrl Pts',(0.00605938394721744,-0.0294971538546968,
0.0734769967671513));
#61909=CARTESIAN_POINT('Ctrl Pts',(0.00595907161542407,-0.0295495417291453,
0.0739592244029917));
#61910=CARTESIAN_POINT('Ctrl Pts',(0.00608211280228693,-0.0296543174780434,
0.0748942803942386));
#61911=CARTESIAN_POINT('Ctrl Pts',(0.00630586837465766,-0.0297067053524937,
0.0753440780020337));
#61912=CARTESIAN_POINT('Ctrl Pts',(0.00699741885923872,-0.0298114811013907,
0.0760106285387534));
#61913=CARTESIAN_POINT('Ctrl Pts',(0.00746350290246076,-0.02986386897584,
0.0762245043065757));
#61914=CARTESIAN_POINT('Ctrl Pts',(0.00843911221849071,-0.0299686447247403,
0.0763040900230327));
#61915=CARTESIAN_POINT('Ctrl Pts',(0.0089451874363639,-0.0300210325991884,
0.0761685265237053));
#61916=CARTESIAN_POINT('Ctrl Pts',(0.00975909850238958,-0.0301258083480876,
0.0755904500898765));
#61917=CARTESIAN_POINT('Ctrl Pts',(0.0100631115942824,-0.0301781962225362,
0.0751492903863319));
#61918=CARTESIAN_POINT('Ctrl Pts',(0.0103054074683059,-0.0302829719714357,
0.0741595369305542));
#61919=CARTESIAN_POINT('Ctrl Pts',(0.0102414483775728,-0.0303353598458849,
0.0736148328055268));
#61920=CARTESIAN_POINT('Ctrl Pts',(0.00975323921825422,-0.0304401355947827,
0.0726954265952984));
#61921=CARTESIAN_POINT('Ctrl Pts',(0.00932997882757754,-0.0304925234692313,
0.0723256171343211));
#61922=CARTESIAN_POINT('Ctrl Pts',(0.00832584380498464,-0.0305972992181321,
0.0719722823282605));
#61923=CARTESIAN_POINT('Ctrl Pts',(0.0077494649754808,-0.0306496870925817,
0.0719920559628832));
#61924=CARTESIAN_POINT('Ctrl Pts',(0.00675592000443203,-0.0307544628414776,
0.0724395062495526));
#61925=CARTESIAN_POINT('Ctrl Pts',(0.00634496891942769,-0.0308068507159279,
0.0728664214919276));
#61926=CARTESIAN_POINT('Ctrl Pts',(0.00594354974162806,-0.0309116264648272,
0.0739084696771727));
#61927=CARTESIAN_POINT('Ctrl Pts',(0.00595750536674637,-0.030964014339277,
0.0745180867156372));
#61928=CARTESIAN_POINT('Ctrl Pts',(0.00638267793035737,-0.0310568507159276,
0.0754400513829074));
#61929=CARTESIAN_POINT('Ctrl Pts',(0.00669956413626623,-0.0310972992181319,
0.0757857300068678));
#61930=CARTESIAN_POINT('Ctrl Pts',(0.00748945302262128,-0.0311781962225358,
0.0762240386264647));
#61931=CARTESIAN_POINT('Ctrl Pts',(0.00796079155782699,-0.0312186447247393,
0.0763148367595518));
#61932=CARTESIAN_POINT('Ctrl Pts',(0.00887509295304323,-0.0312995417291452,
0.0761868152287656));
#61933=CARTESIAN_POINT('Ctrl Pts',(0.00931534986442847,-0.031339990231348,
0.075967462485304));
#61934=CARTESIAN_POINT('Ctrl Pts',(0.00997379973563606,-0.0314208872357532,
0.0752903676969252));
#61935=CARTESIAN_POINT('Ctrl Pts',(0.0101892230058022,-0.0314613357379553,
0.0748339923228011));
#61936=CARTESIAN_POINT('Ctrl Pts',(0.0102708978512695,-0.0315328667545812,
0.0739826395793677));
#61937=CARTESIAN_POINT('Ctrl Pts',(0.0102055680523813,-0.0315639492690025,
0.0735997686615574));
#61938=CARTESIAN_POINT('Ctrl Pts',(0.0100469390803206,-0.0315950317834238,
0.0732561803273014));
#61939=CARTESIAN_POINT('Ctrl Pts',(0.00815332628724061,-0.0203072579114564,
0.0764745476396777));
#61940=CARTESIAN_POINT('Ctrl Pts',(0.00840215214987724,-0.0203255606965017,
0.0764737437596658));
#61941=CARTESIAN_POINT('Ctrl Pts',(0.00864919320439181,-0.0203438634815471,
0.0764340500831514));
#61942=CARTESIAN_POINT('Ctrl Pts',(0.00967605537954476,-0.0204246662665928,
0.0760808971366146));
#61943=CARTESIAN_POINT('Ctrl Pts',(0.0102733422062002,-0.0204871662665918,
0.0753606557973937));
#61944=CARTESIAN_POINT('Ctrl Pts',(0.0105612683570671,-0.0206121662665931,
0.0737692679062889));
#61945=CARTESIAN_POINT('Ctrl Pts',(0.0102565391923597,-0.020674666266593,
0.0729280907060315));
#61946=CARTESIAN_POINT('Ctrl Pts',(0.00909049684955361,-0.0207996662665919,
0.0718900934688763));
#61947=CARTESIAN_POINT('Ctrl Pts',(0.00825260378650262,-0.0208621662665925,
0.0717033226702191));
#61948=CARTESIAN_POINT('Ctrl Pts',(0.00679318847130807,-0.0209871662665924,
0.0720927335317618));
#61949=CARTESIAN_POINT('Ctrl Pts',(0.00618986329796383,-0.0210496662665924,
0.0726571638876892));
#61950=CARTESIAN_POINT('Ctrl Pts',(0.00568359379013531,-0.0211746662665925,
0.0740313301927182));
#61951=CARTESIAN_POINT('Ctrl Pts',(0.00578155954133694,-0.0212371662665924,
0.0748224925990252));
#61952=CARTESIAN_POINT('Ctrl Pts',(0.00655602261255478,-0.0213621662665925,
0.076015578504634));
#61953=CARTESIAN_POINT('Ctrl Pts',(0.00722019139059382,-0.0214246662665922,
0.0764071397497255));
#61954=CARTESIAN_POINT('Ctrl Pts',(0.00859809554021233,-0.0215496662665927,
0.0765345718796849));
#61955=CARTESIAN_POINT('Ctrl Pts',(0.00929804399292574,-0.0216121662665926,
0.0762731872241167));
#61956=CARTESIAN_POINT('Ctrl Pts',(0.010250065441227,-0.0217371662665924,
0.0753186463638511));
#61957=CARTESIAN_POINT('Ctrl Pts',(0.0104961904099933,-0.0217996662665926,
0.0746363211000744));
#61958=CARTESIAN_POINT('Ctrl Pts',(0.0104005508475817,-0.0219246662665924,
0.0733246797802278));
#61959=CARTESIAN_POINT('Ctrl Pts',(0.0100625167520088,-0.0219871662665922,
0.0727056382289851));
#61960=CARTESIAN_POINT('Ctrl Pts',(0.00904912860513842,-0.0221121662665928,
0.0719164811073332));
#61961=CARTESIAN_POINT('Ctrl Pts',(0.00838276147471677,-0.022174666266592,
0.0717500819062757));
#61962=CARTESIAN_POINT('Ctrl Pts',(0.00714217809165384,-0.0222996662665929,
0.0719447493287309));
#61963=CARTESIAN_POINT('Ctrl Pts',(0.0065759050711654,-0.0223621662665927,
0.0723022728294504));
#61964=CARTESIAN_POINT('Ctrl Pts',(0.00586614734384593,-0.0224871662665922,
0.0733055450405034));
#61965=CARTESIAN_POINT('Ctrl Pts',(0.00572539440382979,-0.0225496662665926,
0.073943970666777));
#61966=CARTESIAN_POINT('Ctrl Pts',(0.00592552003453053,-0.0226746662665923,
0.0751309972301058));
#61967=CARTESIAN_POINT('Ctrl Pts',(0.00626351738443437,-0.0227371662665921,
0.0756731587170833));
#61968=CARTESIAN_POINT('Ctrl Pts',(0.00721234684475271,-0.0228621662665928,
0.0763748333085017));
#61969=CARTESIAN_POINT('Ctrl Pts',(0.00781726037633776,-0.0229246662665925,
0.0765319290828517));
#61970=CARTESIAN_POINT('Ctrl Pts',(0.00896730939589689,-0.0230496662665924,
0.076398555902516));
#61971=CARTESIAN_POINT('Ctrl Pts',(0.00950700226631619,-0.0231121662665924,
0.0761101356971356));
#61972=CARTESIAN_POINT('Ctrl Pts',(0.010254007677104,-0.0232371662665925,
0.0752534351443655));
#61973=CARTESIAN_POINT('Ctrl Pts',(0.0104588843013103,-0.0232996662665926,
0.0746898711283627));
#61974=CARTESIAN_POINT('Ctrl Pts',(0.0104500540367917,-0.0234246662665924,
0.0735732660853268));
#61975=CARTESIAN_POINT('Ctrl Pts',(0.0102375227040588,-0.0234871662665927,
0.0730249416515866));
#61976=CARTESIAN_POINT('Ctrl Pts',(0.00951342941930744,-0.0236121662665922,
0.0721999908129729));
#61977=CARTESIAN_POINT('Ctrl Pts',(0.00900550661104702,-0.0236746662665927,
0.0719259507427556));
#61978=CARTESIAN_POINT('Ctrl Pts',(0.00793799198823834,-0.0237996662665922,
0.0717647714878526));
#61979=CARTESIAN_POINT('Ctrl Pts',(0.0073824994148905,-0.0238621662665923,
0.071877307532445));
#61980=CARTESIAN_POINT('Ctrl Pts',(0.00647090305920422,-0.0239871662665926,
0.0724229731370429));
#61981=CARTESIAN_POINT('Ctrl Pts',(0.0061175390822829,-0.0240496662665925,
0.0728534733596938));
#61982=CARTESIAN_POINT('Ctrl Pts',(0.0057559180058162,-0.0241746662665925,
0.0738350207207137));
#61983=CARTESIAN_POINT('Ctrl Pts',(0.00574811958679247,-0.0242371662665925,
0.0743825825552014));
#61984=CARTESIAN_POINT('Ctrl Pts',(0.00606748354576255,-0.0243621662665925,
0.075362230730441));
#61985=CARTESIAN_POINT('Ctrl Pts',(0.00639298543709791,-0.0244246662665925,
0.0757915095294001));
#61986=CARTESIAN_POINT('Ctrl Pts',(0.00723254201175921,-0.0245496662665925,
0.0763626685001477));
#61987=CARTESIAN_POINT('Ctrl Pts',(0.00774378154132399,-0.0246121662665926,
0.0765034194843978));
#61988=CARTESIAN_POINT('Ctrl Pts',(0.00874354049187196,-0.0247371662665924,
0.0764519303687327));
#61989=CARTESIAN_POINT('Ctrl Pts',(0.00922933182513614,-0.024799666266592,
0.0762604290571012));
#61990=CARTESIAN_POINT('Ctrl Pts',(0.00999001579168093,-0.024924666266593,
0.0756309871558503));
#61991=CARTESIAN_POINT('Ctrl Pts',(0.0102632712006387,-0.0249871662665926,
0.0751951159850686));
#61992=CARTESIAN_POINT('Ctrl Pts',(0.0105027538882435,-0.0251121662665924,
0.0742508678118485));
#61993=CARTESIAN_POINT('Ctrl Pts',(0.0104688803165286,-0.0251746662665924,
0.0737449568761991));
#61994=CARTESIAN_POINT('Ctrl Pts',(0.0101172277391856,-0.0252996662665926,
0.0728501076962283));
#61995=CARTESIAN_POINT('Ctrl Pts',(0.00980071482414927,-0.0253621662665928,
0.0724631046418761));
#61996=CARTESIAN_POINT('Ctrl Pts',(0.00900749170282425,-0.0254871662665921,
0.0719416575205446));
#61997=CARTESIAN_POINT('Ctrl Pts',(0.00853279776289023,-0.0255496662665926,
0.0718080167269426));
#61998=CARTESIAN_POINT('Ctrl Pts',(0.0075955800831525,-0.0256746662665924,
0.0718319875055733));
#61999=CARTESIAN_POINT('Ctrl Pts',(0.0071350448081896,-0.0257371662665915,
0.0719891427483816));
#62000=CARTESIAN_POINT('Ctrl Pts',(0.0063840705858361,-0.0258621662665935,
0.0725312630827505));
#62001=CARTESIAN_POINT('Ctrl Pts',(0.00609493832603504,-0.0259246662665926,
0.0729148185450287));
#62002=CARTESIAN_POINT('Ctrl Pts',(0.00567150376979967,-0.0260919420154909,
0.0740641461150897));
#62003=CARTESIAN_POINT('Ctrl Pts',(0.00579022688422278,-0.0261967177643892,
0.0749243565323479));
#62004=CARTESIAN_POINT('Ctrl Pts',(0.00673062180767083,-0.0264062692621874,
0.0761758856211119));
#62005=CARTESIAN_POINT('Ctrl Pts',(0.00754107324008372,-0.0265110450110865,
0.076544093544357));
#62006=CARTESIAN_POINT('Ctrl Pts',(0.00913286211817163,-0.0267205965088817,
0.0763978859664261));
#62007=CARTESIAN_POINT('Ctrl Pts',(0.00988589289648584,-0.0268253722577806,
0.0758805062803154));
#62008=CARTESIAN_POINT('Ctrl Pts',(0.0105806569015859,-0.0270349237555792,
0.0744018983400594));
#62009=CARTESIAN_POINT('Ctrl Pts',(0.0105035012565028,-0.0271396995044774,
0.0734660931660017));
#62010=CARTESIAN_POINT('Ctrl Pts',(0.00952680560062186,-0.0273492510022741,
0.072109824349359));
#62011=CARTESIAN_POINT('Ctrl Pts',(0.00864171718187381,-0.0274540267511745,
0.0717216915578374));
#62012=CARTESIAN_POINT('Ctrl Pts',(0.00694717056566465,-0.0276635782489686,
0.0719635591456149));
#62013=CARTESIAN_POINT('Ctrl Pts',(0.0061774297989796,-0.0277683539978693,
0.0725961952733644));
#62014=CARTESIAN_POINT('Ctrl Pts',(0.00577133691614923,-0.0279255176212164,
0.0738483685540666));
#62015=CARTESIAN_POINT('Ctrl Pts',(0.00575623435121828,-0.0279779054956661,
0.0743074083721862));
#62016=CARTESIAN_POINT('Ctrl Pts',(0.00598037625292647,-0.0280826812445643,
0.0751677775536731));
#62017=CARTESIAN_POINT('Ctrl Pts',(0.006219576669604,-0.0281350691190143,
0.0755675389519453));
#62018=CARTESIAN_POINT('Ctrl Pts',(0.00688501715781157,-0.028239844867912,
0.0761750621069688));
#62019=CARTESIAN_POINT('Ctrl Pts',(0.00731030903013384,-0.0282922327423619,
0.0763814412976357));
#62020=CARTESIAN_POINT('Ctrl Pts',(0.00821272207368966,-0.0283970084912602,
0.0765234275937696));
#62021=CARTESIAN_POINT('Ctrl Pts',(0.0086881821973765,-0.0284493963657099,
0.0764583541632762));
#62022=CARTESIAN_POINT('Ctrl Pts',(0.00952801531425379,-0.0285541721146081,
0.0760670747619161));
#62023=CARTESIAN_POINT('Ctrl Pts',(0.00989050099342927,-0.028606559989058,
0.0757412514171181));
#62024=CARTESIAN_POINT('Ctrl Pts',(0.0103691372816368,-0.0287113357379557,
0.0749321489062033));
#62025=CARTESIAN_POINT('Ctrl Pts',(0.0104838416490414,-0.0287637236124047,
0.0744503508285196));
#62026=CARTESIAN_POINT('Ctrl Pts',(0.0104120206910918,-0.0288684993613048,
0.0734988043112581));
#62027=CARTESIAN_POINT('Ctrl Pts',(0.0102251237098014,-0.0289208872357529,
0.0730312547594835));
#62028=CARTESIAN_POINT('Ctrl Pts',(0.00960512622564884,-0.0290256629846524,
0.0722864423988114));
#62029=CARTESIAN_POINT('Ctrl Pts',(0.00917306831712077,-0.0290780508591023,
0.0720113501056385));
#62030=CARTESIAN_POINT('Ctrl Pts',(0.00821853372773986,-0.0291828266079989,
0.0717696960530468));
#62031=CARTESIAN_POINT('Ctrl Pts',(0.00769834660242158,-0.0292352144824501,
0.0718043795871957));
#62032=CARTESIAN_POINT('Ctrl Pts',(0.00677289295094829,-0.0293399902313469,
0.072185813448155));
#62033=CARTESIAN_POINT('Ctrl Pts',(0.00637042834480692,-0.029392378105796,
0.0725321781376852));
#62034=CARTESIAN_POINT('Ctrl Pts',(0.00585556439734561,-0.0294971538546968,
0.0734105506653613));
#62035=CARTESIAN_POINT('Ctrl Pts',(0.00574534815560973,-0.0295495417291453,
0.0739403889886591));
#62036=CARTESIAN_POINT('Ctrl Pts',(0.00588053728891275,-0.0296543174780434,
0.0749677637423445));
#62037=CARTESIAN_POINT('Ctrl Pts',(0.00612638441272354,-0.0297067053524937,
0.0754619701971907));
#62038=CARTESIAN_POINT('Ctrl Pts',(0.0068862121828339,-0.0298114811013907,
0.0761943297562885));
#62039=CARTESIAN_POINT('Ctrl Pts',(0.00739831304479771,-0.02986386897584,
0.0764293216352161));
#62040=CARTESIAN_POINT('Ctrl Pts',(0.00847024498270537,-0.0299686447247403,
0.0765167649077124));
#62041=CARTESIAN_POINT('Ctrl Pts',(0.00902628537726555,-0.0300210325991884,
0.0763678171248695));
#62042=CARTESIAN_POINT('Ctrl Pts',(0.00992055447858949,-0.0301258083480876,
0.0757326667816004));
#62043=CARTESIAN_POINT('Ctrl Pts',(0.0102545830055701,-0.0301781962225362,
0.0752479510576141));
#62044=CARTESIAN_POINT('Ctrl Pts',(0.0105208009285865,-0.0302829719714357,
0.0741604785186885));
#62045=CARTESIAN_POINT('Ctrl Pts',(0.0104505271100099,-0.0303353598458849,
0.073561995356696));
#62046=CARTESIAN_POINT('Ctrl Pts',(0.00991411670304272,-0.0304401355947827,
0.0725518154983641));
#62047=CARTESIAN_POINT('Ctrl Pts',(0.00944906750418523,-0.0304925234692313,
0.072145494478619));
#62048=CARTESIAN_POINT('Ctrl Pts',(0.00834579349582601,-0.0305972992181321,
0.0717572746685295));
#62049=CARTESIAN_POINT('Ctrl Pts',(0.00771250836259956,-0.0306496870925817,
0.0717790005685719));
#62050=CARTESIAN_POINT('Ctrl Pts',(0.00662086996932487,-0.0307544628414776,
0.0722706279495596));
#62051=CARTESIAN_POINT('Ctrl Pts',(0.00616934538289875,-0.0308068507159279,
0.0727396928462987));
#62052=CARTESIAN_POINT('Ctrl Pts',(0.00572829379585245,-0.0309116264648272,
0.0738846232116097));
#62053=CARTESIAN_POINT('Ctrl Pts',(0.00574362727005372,-0.030964014339277,
0.0745544281864965));
#62054=CARTESIAN_POINT('Ctrl Pts',(0.00621077743207889,-0.0310568507159276,
0.0755674191002066));
#62055=CARTESIAN_POINT('Ctrl Pts',(0.0065589500450449,-0.0310972992181319,
0.0759472268277333));
#62056=CARTESIAN_POINT('Ctrl Pts',(0.00742682523931609,-0.0311781962225358,
0.076428809978167));
#62057=CARTESIAN_POINT('Ctrl Pts',(0.00794469937310318,-0.0312186447247393,
0.0765285726773943));
#62058=CARTESIAN_POINT('Ctrl Pts',(0.00894927041430031,-0.0312995417291452,
0.0763879114871669));
#62059=CARTESIAN_POINT('Ctrl Pts',(0.00943299421279664,-0.031339990231348,
0.0761469018867863));
#62060=CARTESIAN_POINT('Ctrl Pts',(0.0101564533217469,-0.0314208872357532,
0.0754029570343451));
#62061=CARTESIAN_POINT('Ctrl Pts',(0.0103931454890576,-0.0314613357379553,
0.0749015233854856));
#62062=CARTESIAN_POINT('Ctrl Pts',(0.0104828841518005,-0.0315328667545812,
0.0739661159625376));
#62063=CARTESIAN_POINT('Ctrl Pts',(0.0104111042940494,-0.0315639492690025,
0.0735454439187662));
#62064=CARTESIAN_POINT('Ctrl Pts',(0.0102368137674672,-0.0315950317834238,
0.0731679328567764));
#62065=CARTESIAN_POINT('Ctrl Pts',(0.00815574178150025,-0.0204978184012171,
0.0766646002253042));
#62066=CARTESIAN_POINT('Ctrl Pts',(0.00842491138661719,-0.0205161211862624,
0.0766637306209027));
#62067=CARTESIAN_POINT('Ctrl Pts',(0.00869215025956532,-0.0205344239713078,
0.0766207916308805));
#62068=CARTESIAN_POINT('Ctrl Pts',(0.00980296761298115,-0.0206152267563535,
0.0762387652685163));
#62069=CARTESIAN_POINT('Ctrl Pts',(0.0104490879863571,-0.0206777267563525,
0.0754596377501276));
#62070=CARTESIAN_POINT('Ctrl Pts',(0.0107605546784065,-0.0208027267563538,
0.0737381396482117));
#62071=CARTESIAN_POINT('Ctrl Pts',(0.0104309111756661,-0.0208652267563538,
0.0728281886791785));
#62072=CARTESIAN_POINT('Ctrl Pts',(0.00916953442954738,-0.0209902267563526,
0.0717053258727286));
#62073=CARTESIAN_POINT('Ctrl Pts',(0.00826313610534649,-0.0210527267563532,
0.071503284888768));
#62074=CARTESIAN_POINT('Ctrl Pts',(0.00668440051922231,-0.0211777267563531,
0.0719245335753756));
#62075=CARTESIAN_POINT('Ctrl Pts',(0.0060317481102427,-0.0212402267563531,
0.0725351111673153));
#62076=CARTESIAN_POINT('Ctrl Pts',(0.00548408653655842,-0.0213652267563533,
0.0740216278732971));
#62077=CARTESIAN_POINT('Ctrl Pts',(0.00559006186519377,-0.0214277267563531,
0.0748774748910969));
#62078=CARTESIAN_POINT('Ctrl Pts',(0.00642784422772027,-0.0215527267563532,
0.0761681062534498));
#62079=CARTESIAN_POINT('Ctrl Pts',(0.0071463147509265,-0.0216152267563529,
0.0765916811367176));
#62080=CARTESIAN_POINT('Ctrl Pts',(0.00863687490376476,-0.0217402267563534,
0.076729531984443));
#62081=CARTESIAN_POINT('Ctrl Pts',(0.00939405041045344,-0.0218027267563532,
0.0764467767926095));
#62082=CARTESIAN_POINT('Ctrl Pts',(0.0104239081374065,-0.0219277267563531,
0.0754141936692029));
#62083=CARTESIAN_POINT('Ctrl Pts',(0.0106901560263932,-0.0219902267563532,
0.0746760822049604));
#62084=CARTESIAN_POINT('Ctrl Pts',(0.0105866970733117,-0.0221152267563531,
0.0732572024616046));
#62085=CARTESIAN_POINT('Ctrl Pts',(0.0102210256633657,-0.0221777267563529,
0.0725875487200949));
#62086=CARTESIAN_POINT('Ctrl Pts',(0.00912478396070292,-0.0223027267563535,
0.0717338709369279));
#62087=CARTESIAN_POINT('Ctrl Pts',(0.00840393535012082,-0.0223652267563527,
0.0715538671110964));
#62088=CARTESIAN_POINT('Ctrl Pts',(0.00706192316619711,-0.0224902267563536,
0.0717644503385637));
#62089=CARTESIAN_POINT('Ctrl Pts',(0.00644935225536766,-0.0225527267563534,
0.0721512045870529));
#62090=CARTESIAN_POINT('Ctrl Pts',(0.00568156547803287,-0.0226777267563529,
0.073236503285558));
#62091=CARTESIAN_POINT('Ctrl Pts',(0.00552930472474256,-0.0227402267563533,
0.0739271259238148));
#62092=CARTESIAN_POINT('Ctrl Pts',(0.00574579241785726,-0.022865226756353,
0.0752112025383953));
#62093=CARTESIAN_POINT('Ctrl Pts',(0.00611142407784697,-0.0229277267563529,
0.0757976905819331));
#62094=CARTESIAN_POINT('Ctrl Pts',(0.00713782884321568,-0.0230527267563535,
0.0765567333546231));
#62095=CARTESIAN_POINT('Ctrl Pts',(0.00779219947294575,-0.0231152267563532,
0.0767266731153024));
#62096=CARTESIAN_POINT('Ctrl Pts',(0.00903627529842336,-0.0232402267563531,
0.0765823954831315));
#62097=CARTESIAN_POINT('Ctrl Pts',(0.00962009289389314,-0.0233027267563532,
0.0762703943431882));
#62098=CARTESIAN_POINT('Ctrl Pts',(0.0104281726863687,-0.0234277267563531,
0.0753436508485646));
#62099=CARTESIAN_POINT('Ctrl Pts',(0.0106497998092528,-0.0234902267563532,
0.0747340104275962));
#62100=CARTESIAN_POINT('Ctrl Pts',(0.0106402475915358,-0.0236152267563531,
0.0735261129232099));
#62101=CARTESIAN_POINT('Ctrl Pts',(0.0104103399191558,-0.0236777267563534,
0.0729329580568231));
#62102=CARTESIAN_POINT('Ctrl Pts',(0.00962704552419596,-0.0238027267563529,
0.0720405600998036));
#62103=CARTESIAN_POINT('Ctrl Pts',(0.00907759547796414,-0.0238652267563534,
0.0717441147998457));
#62104=CARTESIAN_POINT('Ctrl Pts',(0.00792280197525823,-0.0239902267563529,
0.0715697576975107));
#62105=CARTESIAN_POINT('Ctrl Pts',(0.00732189290966092,-0.024052726756353,
0.0716914945714972));
#62106=CARTESIAN_POINT('Ctrl Pts',(0.00633576538864637,-0.0241777267563532,
0.0722817732256498));
#62107=CARTESIAN_POINT('Ctrl Pts',(0.00595351074227404,-0.0242402267563532,
0.0727474706965873));
#62108=CARTESIAN_POINT('Ctrl Pts',(0.00556232390452704,-0.0243652267563532,
0.0738092683440253));
#62109=CARTESIAN_POINT('Ctrl Pts',(0.0055538878949141,-0.0244277267563531,
0.0744015982618417));
#62110=CARTESIAN_POINT('Ctrl Pts',(0.00589936271740101,-0.0245527267563532,
0.0754613414480549));
#62111=CARTESIAN_POINT('Ctrl Pts',(0.00625147730318875,-0.0246152267563531,
0.075925717632976));
#62112=CARTESIAN_POINT('Ctrl Pts',(0.00715967514597056,-0.0247402267563532,
0.0765435739642516));
#62113=CARTESIAN_POINT('Ctrl Pts',(0.00771271308517418,-0.0248027267563532,
0.0766958326018746));
#62114=CARTESIAN_POINT('Ctrl Pts',(0.00879421128266716,-0.0249277267563531,
0.0766401337899241));
#62115=CARTESIAN_POINT('Ctrl Pts',(0.00931972040763655,-0.0249902267563527,
0.0764329755311924));
#62116=CARTESIAN_POINT('Ctrl Pts',(0.0101425971002925,-0.0251152267563537,
0.0757520711179273));
#62117=CARTESIAN_POINT('Ctrl Pts',(0.0104381935859063,-0.0251777267563533,
0.0752805635757531));
#62118=CARTESIAN_POINT('Ctrl Pts',(0.0106972561277655,-0.025302726756353,
0.0742591146587279));
#62119=CARTESIAN_POINT('Ctrl Pts',(0.0106606130882285,-0.0253652267563531,
0.0737118409737093));
#62120=CARTESIAN_POINT('Ctrl Pts',(0.0102802097636754,-0.0254902267563532,
0.0727438298599943));
#62121=CARTESIAN_POINT('Ctrl Pts',(0.00993781908349455,-0.0255527267563535,
0.0723251858403766));
#62122=CARTESIAN_POINT('Ctrl Pts',(0.00907974286877045,-0.0256777267563528,
0.0717611057473714));
#62123=CARTESIAN_POINT('Ctrl Pts',(0.00856623844841187,-0.0257402267563532,
0.0716165386221529));
#62124=CARTESIAN_POINT('Ctrl Pts',(0.00755239483066854,-0.0258652267563531,
0.0716424692265927));
#62125=CARTESIAN_POINT('Ctrl Pts',(0.00705420667293192,-0.0259277267563522,
0.0718124733178095));
#62126=CARTESIAN_POINT('Ctrl Pts',(0.0062418335830046,-0.0260527267563541,
0.0723989168441442));
#62127=CARTESIAN_POINT('Ctrl Pts',(0.00592906217181541,-0.0261152267563532,
0.072813831400163));
#62128=CARTESIAN_POINT('Ctrl Pts',(0.0054710080487956,-0.0262825025052516,
0.0740571267911857));
#62129=CARTESIAN_POINT('Ctrl Pts',(0.00559943784097573,-0.0263872782541498,
0.0749876671131497));
#62130=CARTESIAN_POINT('Ctrl Pts',(0.00661671847055469,-0.0265968297519482,
0.0763415199122333));
#62131=CARTESIAN_POINT('Ctrl Pts',(0.00749343156507586,-0.0267016055008472,
0.0767398321304675));
#62132=CARTESIAN_POINT('Ctrl Pts',(0.00921536343825145,-0.0269111569986424,
0.0765816707737669));
#62133=CARTESIAN_POINT('Ctrl Pts',(0.0100299612260055,-0.0270159327475413,
0.0760219906652354));
#62134=CARTESIAN_POINT('Ctrl Pts',(0.0107815284100618,-0.0272254842453399,
0.0744224932850827));
#62135=CARTESIAN_POINT('Ctrl Pts',(0.0106980646000727,-0.027330259994239,
0.0734101776580076));
#62136=CARTESIAN_POINT('Ctrl Pts',(0.0096415153281149,-0.0275398114920338,
0.0719430217203579));
#62137=CARTESIAN_POINT('Ctrl Pts',(0.00868406300525948,-0.0276445872409343,
0.0715231555974404));
#62138=CARTESIAN_POINT('Ctrl Pts',(0.00685097202868609,-0.0278541387387302,
0.0717847980264181));
#62139=CARTESIAN_POINT('Ctrl Pts',(0.00601829806137571,-0.0279589144876299,
0.0724691578228018));
#62140=CARTESIAN_POINT('Ctrl Pts',(0.00557900344885459,-0.028116078110977,
0.0738237074822833));
#62141=CARTESIAN_POINT('Ctrl Pts',(0.00556266611399862,-0.0281684659854268,
0.0743202779161881));
#62142=CARTESIAN_POINT('Ctrl Pts',(0.00580513362333878,-0.028273241734325,
0.0752509899827782));
#62143=CARTESIAN_POINT('Ctrl Pts',(0.00606389081609463,-0.028325629608775,
0.0756834354551811));
#62144=CARTESIAN_POINT('Ctrl Pts',(0.00678373702316377,-0.0284304053576727,
0.0763406290684345));
#62145=CARTESIAN_POINT('Ctrl Pts',(0.00724380031449291,-0.0284827932321226,
0.0765638816060427));
#62146=CARTESIAN_POINT('Ctrl Pts',(0.00821999370537458,-0.0285875689810209,
0.076717476553358));
#62147=CARTESIAN_POINT('Ctrl Pts',(0.00873432695186883,-0.0286399568554705,
0.0766470827871961));
#62148=CARTESIAN_POINT('Ctrl Pts',(0.00964282394666933,-0.0287447326043687,
0.0762238127909082));
#62149=CARTESIAN_POINT('Ctrl Pts',(0.010034946076139,-0.0287971204788187,
0.0758713504699588));
#62150=CARTESIAN_POINT('Ctrl Pts',(0.0105527151670457,-0.0289018962277164,
0.0749960965833477));
#62151=CARTESIAN_POINT('Ctrl Pts',(0.0106767976436514,-0.0289542841021654,
0.0744749071983615));
#62152=CARTESIAN_POINT('Ctrl Pts',(0.0105991046792403,-0.0290590598510655,
0.0734455632323137));
#62153=CARTESIAN_POINT('Ctrl Pts',(0.0103969271960863,-0.0291114477255137,
0.0729397873178239));
#62154=CARTESIAN_POINT('Ctrl Pts',(0.00972623936559113,-0.0292162234744131,
0.0721340798769493));
#62155=CARTESIAN_POINT('Ctrl Pts',(0.00925885685400708,-0.0292686113488629,
0.0718364963253867));
#62156=CARTESIAN_POINT('Ctrl Pts',(0.00822628051418617,-0.0293733870977596,
0.0715750848900085));
#62157=CARTESIAN_POINT('Ctrl Pts',(0.0076635634331514,-0.0294257749722108,
0.0716126041136615));
#62158=CARTESIAN_POINT('Ctrl Pts',(0.0066624456583287,-0.0295305507211076,
0.072025223608455));
#62159=CARTESIAN_POINT('Ctrl Pts',(0.00622707596660661,-0.0295829385955566,
0.0723999067130141));
#62160=CARTESIAN_POINT('Ctrl Pts',(0.00567011728088695,-0.0296877143444575,
0.0733500940605625));
#62161=CARTESIAN_POINT('Ctrl Pts',(0.00555088987441427,-0.0297401022189059,
0.0739232514114372));
#62162=CARTESIAN_POINT('Ctrl Pts',(0.00569713192996942,-0.029844877967804,
0.0750346232512706));
#62163=CARTESIAN_POINT('Ctrl Pts',(0.00596307925768723,-0.0298972658422544,
0.075569235509368));
#62164=CARTESIAN_POINT('Ctrl Pts',(0.00678502975218297,-0.0300020415911513,
0.0763614720206259));
#62165=CARTESIAN_POINT('Ctrl Pts',(0.00733899944542236,-0.0300544294656007,
0.0766156765899838));
#62166=CARTESIAN_POINT('Ctrl Pts',(0.00849857141829326,-0.0301592052145009,
0.076710269133052));
#62167=CARTESIAN_POINT('Ctrl Pts',(0.00910007309439272,-0.0302115930889491,
0.0765491435351497));
#62168=CARTESIAN_POINT('Ctrl Pts',(0.0100674567028369,-0.0303163688378483,
0.0758620639636131));
#62169=CARTESIAN_POINT('Ctrl Pts',(0.010428795053089,-0.0303687567122968,
0.0753377183886118));
#62170=CARTESIAN_POINT('Ctrl Pts',(0.0107167786752658,-0.0304735324611964,
0.0741613352314253));
#62171=CARTESIAN_POINT('Ctrl Pts',(0.0106407593427259,-0.0305259203356456,
0.0735139207115853));
#62172=CARTESIAN_POINT('Ctrl Pts',(0.0100604925814896,-0.0306306960845434,
0.072421149603779));
#62173=CARTESIAN_POINT('Ctrl Pts',(0.00955742144615823,-0.0306830839589921,
0.0719816082021071));
#62174=CARTESIAN_POINT('Ctrl Pts',(0.0083639449079113,-0.0307878597078928,
0.0715616479460749));
#62175=CARTESIAN_POINT('Ctrl Pts',(0.00767888304404099,-0.0308402475823424,
0.0715851501329989));
#62176=CARTESIAN_POINT('Ctrl Pts',(0.00649799343660759,-0.0309450233312383,
0.0721169724548543));
#62177=CARTESIAN_POINT('Ctrl Pts',(0.00600955267188516,-0.0309974112056886,
0.0726243876073294));
#62178=CARTESIAN_POINT('Ctrl Pts',(0.00553244116802694,-0.0311021869545879,
0.0738629262827373));
#62179=CARTESIAN_POINT('Ctrl Pts',(0.00554902829105363,-0.0311545748290377,
0.0745874938123549));
#62180=CARTESIAN_POINT('Ctrl Pts',(0.00605437216210567,-0.0312474112056882,
0.0756833058044895));
#62181=CARTESIAN_POINT('Ctrl Pts',(0.00643101100403122,-0.0312878597078925,
0.0760941662148802));
#62182=CARTESIAN_POINT('Ctrl Pts',(0.00736984276716638,-0.0313687567122965,
0.076615123100389));
#62183=CARTESIAN_POINT('Ctrl Pts',(0.00793005774889972,-0.0314092052144999,
0.0767230422936426));
#62184=CARTESIAN_POINT('Ctrl Pts',(0.00901676146854406,-0.0314901022189058,
0.076570880791508));
#62185=CARTESIAN_POINT('Ctrl Pts',(0.00954003401926395,-0.0315305507211086,
0.0763101664980802));
#62186=CARTESIAN_POINT('Ctrl Pts',(0.0103226423888721,-0.0316114477255139,
0.075505397492003));
#62187=CARTESIAN_POINT('Ctrl Pts',(0.0105786862604142,-0.0316518962277159,
0.0749629671520629));
#62188=CARTESIAN_POINT('Ctrl Pts',(0.0106757618624369,-0.0317234272443419,
0.0739510817958126));
#62189=CARTESIAN_POINT('Ctrl Pts',(0.0105981133585333,-0.0317545097587632,
0.0734960160453883));
#62190=CARTESIAN_POINT('Ctrl Pts',(0.0104095730206495,-0.0317855922731845,
0.0730876400735085));
#62191=CARTESIAN_POINT('Ctrl Pts',(0.00815574178150025,-0.0209166974216957,
0.0766646002253042));
#62192=CARTESIAN_POINT('Ctrl Pts',(0.00842491138661719,-0.020935000206741,
0.0766637306209027));
#62193=CARTESIAN_POINT('Ctrl Pts',(0.00869215025956532,-0.0209533029917864,
0.0766207916308805));
#62194=CARTESIAN_POINT('Ctrl Pts',(0.00980296761298115,-0.0210341057768321,
0.0762387652685163));
#62195=CARTESIAN_POINT('Ctrl Pts',(0.0104490879863571,-0.0210966057768311,
0.0754596377501276));
#62196=CARTESIAN_POINT('Ctrl Pts',(0.0107605546784065,-0.0212216057768325,
0.0737381396482117));
#62197=CARTESIAN_POINT('Ctrl Pts',(0.0104309111756661,-0.0212841057768323,
0.0728281886791785));
#62198=CARTESIAN_POINT('Ctrl Pts',(0.00916953442954738,-0.0214091057768312,
0.0717053258727286));
#62199=CARTESIAN_POINT('Ctrl Pts',(0.00826313610534649,-0.0214716057768319,
0.071503284888768));
#62200=CARTESIAN_POINT('Ctrl Pts',(0.00668440051922231,-0.0215966057768317,
0.0719245335753756));
#62201=CARTESIAN_POINT('Ctrl Pts',(0.0060317481102427,-0.0216591057768317,
0.0725351111673153));
#62202=CARTESIAN_POINT('Ctrl Pts',(0.00548408653655842,-0.0217841057768319,
0.0740216278732971));
#62203=CARTESIAN_POINT('Ctrl Pts',(0.00559006186519377,-0.0218466057768317,
0.0748774748910969));
#62204=CARTESIAN_POINT('Ctrl Pts',(0.00642784422772027,-0.0219716057768319,
0.0761681062534498));
#62205=CARTESIAN_POINT('Ctrl Pts',(0.0071463147509265,-0.0220341057768316,
0.0765916811367176));
#62206=CARTESIAN_POINT('Ctrl Pts',(0.00863687490376476,-0.0221591057768321,
0.076729531984443));
#62207=CARTESIAN_POINT('Ctrl Pts',(0.00939405041045344,-0.0222216057768319,
0.0764467767926095));
#62208=CARTESIAN_POINT('Ctrl Pts',(0.0104239081374065,-0.0223466057768317,
0.0754141936692029));
#62209=CARTESIAN_POINT('Ctrl Pts',(0.0106901560263932,-0.0224091057768319,
0.0746760822049604));
#62210=CARTESIAN_POINT('Ctrl Pts',(0.0105866970733117,-0.0225341057768317,
0.0732572024616046));
#62211=CARTESIAN_POINT('Ctrl Pts',(0.0102210256633657,-0.0225966057768315,
0.0725875487200949));
#62212=CARTESIAN_POINT('Ctrl Pts',(0.00912478396070292,-0.0227216057768321,
0.0717338709369279));
#62213=CARTESIAN_POINT('Ctrl Pts',(0.00840393535012082,-0.0227841057768314,
0.0715538671110964));
#62214=CARTESIAN_POINT('Ctrl Pts',(0.00706192316619711,-0.0229091057768322,
0.0717644503385637));
#62215=CARTESIAN_POINT('Ctrl Pts',(0.00644935225536766,-0.0229716057768321,
0.0721512045870529));
#62216=CARTESIAN_POINT('Ctrl Pts',(0.00568156547803287,-0.0230966057768316,
0.073236503285558));
#62217=CARTESIAN_POINT('Ctrl Pts',(0.00552930472474256,-0.023159105776832,
0.0739271259238148));
#62218=CARTESIAN_POINT('Ctrl Pts',(0.00574579241785726,-0.0232841057768316,
0.0752112025383953));
#62219=CARTESIAN_POINT('Ctrl Pts',(0.00611142407784697,-0.0233466057768315,
0.0757976905819331));
#62220=CARTESIAN_POINT('Ctrl Pts',(0.00713782884321568,-0.0234716057768321,
0.0765567333546231));
#62221=CARTESIAN_POINT('Ctrl Pts',(0.00779219947294575,-0.0235341057768318,
0.0767266731153024));
#62222=CARTESIAN_POINT('Ctrl Pts',(0.00903627529842336,-0.0236591057768317,
0.0765823954831315));
#62223=CARTESIAN_POINT('Ctrl Pts',(0.00962009289389314,-0.0237216057768318,
0.0762703943431882));
#62224=CARTESIAN_POINT('Ctrl Pts',(0.0104281726863687,-0.0238466057768318,
0.0753436508485646));
#62225=CARTESIAN_POINT('Ctrl Pts',(0.0106497998092528,-0.0239091057768318,
0.0747340104275962));
#62226=CARTESIAN_POINT('Ctrl Pts',(0.0106402475915358,-0.0240341057768317,
0.0735261129232099));
#62227=CARTESIAN_POINT('Ctrl Pts',(0.0104103399191558,-0.0240966057768321,
0.0729329580568231));
#62228=CARTESIAN_POINT('Ctrl Pts',(0.00962704552419596,-0.0242216057768316,
0.0720405600998036));
#62229=CARTESIAN_POINT('Ctrl Pts',(0.00907759547796414,-0.0242841057768321,
0.0717441147998457));
#62230=CARTESIAN_POINT('Ctrl Pts',(0.00792280197525823,-0.0244091057768316,
0.0715697576975107));
#62231=CARTESIAN_POINT('Ctrl Pts',(0.00732189290966092,-0.0244716057768317,
0.0716914945714972));
#62232=CARTESIAN_POINT('Ctrl Pts',(0.00633576538864637,-0.0245966057768319,
0.0722817732256498));
#62233=CARTESIAN_POINT('Ctrl Pts',(0.00595351074227404,-0.0246591057768318,
0.0727474706965873));
#62234=CARTESIAN_POINT('Ctrl Pts',(0.00556232390452704,-0.0247841057768317,
0.0738092683440253));
#62235=CARTESIAN_POINT('Ctrl Pts',(0.0055538878949141,-0.0248466057768317,
0.0744015982618417));
#62236=CARTESIAN_POINT('Ctrl Pts',(0.00589936271740101,-0.0249716057768318,
0.0754613414480549));
#62237=CARTESIAN_POINT('Ctrl Pts',(0.00625147730318875,-0.0250341057768317,
0.075925717632976));
#62238=CARTESIAN_POINT('Ctrl Pts',(0.00715967514597056,-0.0251591057768318,
0.0765435739642516));
#62239=CARTESIAN_POINT('Ctrl Pts',(0.00771271308517418,-0.0252216057768319,
0.0766958326018746));
#62240=CARTESIAN_POINT('Ctrl Pts',(0.00879421128266716,-0.0253466057768317,
0.0766401337899241));
#62241=CARTESIAN_POINT('Ctrl Pts',(0.00931972040763655,-0.0254091057768313,
0.0764329755311924));
#62242=CARTESIAN_POINT('Ctrl Pts',(0.0101425971002925,-0.0255341057768323,
0.0757520711179273));
#62243=CARTESIAN_POINT('Ctrl Pts',(0.0104381935859063,-0.025596605776832,
0.0752805635757531));
#62244=CARTESIAN_POINT('Ctrl Pts',(0.0106972561277655,-0.0257216057768316,
0.0742591146587279));
#62245=CARTESIAN_POINT('Ctrl Pts',(0.0106606130882285,-0.0257841057768317,
0.0737118409737093));
#62246=CARTESIAN_POINT('Ctrl Pts',(0.0102802097636754,-0.0259091057768319,
0.0727438298599943));
#62247=CARTESIAN_POINT('Ctrl Pts',(0.00993781908349455,-0.0259716057768321,
0.0723251858403766));
#62248=CARTESIAN_POINT('Ctrl Pts',(0.00907974286877045,-0.0260966057768315,
0.0717611057473714));
#62249=CARTESIAN_POINT('Ctrl Pts',(0.00856623844841187,-0.0261591057768319,
0.0716165386221529));
#62250=CARTESIAN_POINT('Ctrl Pts',(0.00755239483066854,-0.0262841057768317,
0.0716424692265927));
#62251=CARTESIAN_POINT('Ctrl Pts',(0.00705420667293192,-0.0263466057768309,
0.0718124733178095));
#62252=CARTESIAN_POINT('Ctrl Pts',(0.0062418335830046,-0.0264716057768327,
0.0723989168441442));
#62253=CARTESIAN_POINT('Ctrl Pts',(0.00592906217181541,-0.0265341057768319,
0.072813831400163));
#62254=CARTESIAN_POINT('Ctrl Pts',(0.0054710080487956,-0.0267013815257303,
0.0740571267911857));
#62255=CARTESIAN_POINT('Ctrl Pts',(0.00559943784097573,-0.0268061572746284,
0.0749876671131497));
#62256=CARTESIAN_POINT('Ctrl Pts',(0.00661671847055469,-0.0270157087724267,
0.0763415199122333));
#62257=CARTESIAN_POINT('Ctrl Pts',(0.00749343156507586,-0.0271204845213259,
0.0767398321304675));
#62258=CARTESIAN_POINT('Ctrl Pts',(0.00921536343825145,-0.027330036019121,
0.0765816707737669));
#62259=CARTESIAN_POINT('Ctrl Pts',(0.0100299612260055,-0.0274348117680204,
0.0760219906652354));
#62260=CARTESIAN_POINT('Ctrl Pts',(0.0107815284100618,-0.027644363265818,
0.0744224932850827));
#62261=CARTESIAN_POINT('Ctrl Pts',(0.0106980646000727,-0.0277491390147176,
0.0734101776580076));
#62262=CARTESIAN_POINT('Ctrl Pts',(0.0096415153281149,-0.0279586905125125,
0.0719430217203579));
#62263=CARTESIAN_POINT('Ctrl Pts',(0.00868406300525948,-0.028063466261413,
0.0715231555974404));
#62264=CARTESIAN_POINT('Ctrl Pts',(0.00685097202868609,-0.0282730177592087,
0.0717847980264181));
#62265=CARTESIAN_POINT('Ctrl Pts',(0.00601829806137571,-0.0283777935081086,
0.0724691578228018));
#62266=CARTESIAN_POINT('Ctrl Pts',(0.00557900344885459,-0.0285349571314557,
0.0738237074822833));
#62267=CARTESIAN_POINT('Ctrl Pts',(0.00556266611399862,-0.0285873450059055,
0.0743202779161881));
#62268=CARTESIAN_POINT('Ctrl Pts',(0.00580513362333878,-0.0286921207548037,
0.0752509899827782));
#62269=CARTESIAN_POINT('Ctrl Pts',(0.00606389081609463,-0.0287445086292537,
0.0756834354551811));
#62270=CARTESIAN_POINT('Ctrl Pts',(0.00678373702316377,-0.0288492843781513,
0.0763406290684345));
#62271=CARTESIAN_POINT('Ctrl Pts',(0.00724380031449291,-0.0289016722526012,
0.0765638816060427));
#62272=CARTESIAN_POINT('Ctrl Pts',(0.00821999370537458,-0.0290064480014996,
0.076717476553358));
#62273=CARTESIAN_POINT('Ctrl Pts',(0.00873432695186883,-0.0290588358759492,
0.0766470827871961));
#62274=CARTESIAN_POINT('Ctrl Pts',(0.00964282394666933,-0.0291636116248473,
0.0762238127909082));
#62275=CARTESIAN_POINT('Ctrl Pts',(0.010034946076139,-0.0292159994992974,
0.0758713504699588));
#62276=CARTESIAN_POINT('Ctrl Pts',(0.0105527151670457,-0.029320775248195,
0.0749960965833477));
#62277=CARTESIAN_POINT('Ctrl Pts',(0.0106767976436514,-0.029373163122644,
0.0744749071983615));
#62278=CARTESIAN_POINT('Ctrl Pts',(0.0105991046792403,-0.0294779388715441,
0.0734455632323137));
#62279=CARTESIAN_POINT('Ctrl Pts',(0.0103969271960863,-0.0295303267459923,
0.0729397873178239));
#62280=CARTESIAN_POINT('Ctrl Pts',(0.00972623936559113,-0.0296351024948917,
0.0721340798769493));
#62281=CARTESIAN_POINT('Ctrl Pts',(0.00925885685400708,-0.0296874903693416,
0.0718364963253867));
#62282=CARTESIAN_POINT('Ctrl Pts',(0.00822628051418617,-0.0297922661182383,
0.0715750848900085));
#62283=CARTESIAN_POINT('Ctrl Pts',(0.0076635634331514,-0.0298446539926894,
0.0716126041136615));
#62284=CARTESIAN_POINT('Ctrl Pts',(0.0066624456583287,-0.0299494297415862,
0.072025223608455));
#62285=CARTESIAN_POINT('Ctrl Pts',(0.00622707596660661,-0.0300018176160353,
0.0723999067130141));
#62286=CARTESIAN_POINT('Ctrl Pts',(0.00567011728088695,-0.0301065933649361,
0.0733500940605625));
#62287=CARTESIAN_POINT('Ctrl Pts',(0.00555088987441427,-0.0301589812393846,
0.0739232514114372));
#62288=CARTESIAN_POINT('Ctrl Pts',(0.00569713192996942,-0.0302637569882826,
0.0750346232512706));
#62289=CARTESIAN_POINT('Ctrl Pts',(0.00596307925768723,-0.0303161448627331,
0.075569235509368));
#62290=CARTESIAN_POINT('Ctrl Pts',(0.00678502975218297,-0.03042092061163,
0.0763614720206259));
#62291=CARTESIAN_POINT('Ctrl Pts',(0.00733899944542236,-0.0304733084860793,
0.0766156765899838));
#62292=CARTESIAN_POINT('Ctrl Pts',(0.00849857141829326,-0.0305780842349796,
0.076710269133052));
#62293=CARTESIAN_POINT('Ctrl Pts',(0.00910007309439272,-0.0306304721094278,
0.0765491435351497));
#62294=CARTESIAN_POINT('Ctrl Pts',(0.0100674567028369,-0.030735247858327,
0.0758620639636131));
#62295=CARTESIAN_POINT('Ctrl Pts',(0.010428795053089,-0.0307876357327754,
0.0753377183886118));
#62296=CARTESIAN_POINT('Ctrl Pts',(0.0107167786752658,-0.030892411481675,
0.0741613352314253));
#62297=CARTESIAN_POINT('Ctrl Pts',(0.0106407593427259,-0.0309447993561243,
0.0735139207115853));
#62298=CARTESIAN_POINT('Ctrl Pts',(0.0100604925814896,-0.031049575105022,
0.072421149603779));
#62299=CARTESIAN_POINT('Ctrl Pts',(0.00955742144615823,-0.0311019629794706,
0.0719816082021071));
#62300=CARTESIAN_POINT('Ctrl Pts',(0.0083639449079113,-0.0312067387283715,
0.0715616479460749));
#62301=CARTESIAN_POINT('Ctrl Pts',(0.00767888304404099,-0.031259126602821,
0.0715851501329989));
#62302=CARTESIAN_POINT('Ctrl Pts',(0.00649799343660759,-0.0313639023517169,
0.0721169724548543));
#62303=CARTESIAN_POINT('Ctrl Pts',(0.00600955267188516,-0.0314162902261672,
0.0726243876073294));
#62304=CARTESIAN_POINT('Ctrl Pts',(0.00553244116802694,-0.0315210659750665,
0.0738629262827373));
#62305=CARTESIAN_POINT('Ctrl Pts',(0.00554902829105363,-0.0315734538495163,
0.0745874938123549));
#62306=CARTESIAN_POINT('Ctrl Pts',(0.00605437216210567,-0.0316662902261669,
0.0756833058044895));
#62307=CARTESIAN_POINT('Ctrl Pts',(0.00643101100403122,-0.0317067387283712,
0.0760941662148802));
#62308=CARTESIAN_POINT('Ctrl Pts',(0.00736984276716638,-0.0317876357327751,
0.076615123100389));
#62309=CARTESIAN_POINT('Ctrl Pts',(0.00793005774889972,-0.0318280842349786,
0.0767230422936426));
#62310=CARTESIAN_POINT('Ctrl Pts',(0.00901676146854406,-0.0319089812393844,
0.076570880791508));
#62311=CARTESIAN_POINT('Ctrl Pts',(0.00954003401926395,-0.0319494297415873,
0.0763101664980802));
#62312=CARTESIAN_POINT('Ctrl Pts',(0.0103226423888721,-0.0320303267459926,
0.075505397492003));
#62313=CARTESIAN_POINT('Ctrl Pts',(0.0105786862604142,-0.0320707752481946,
0.0749629671520629));
#62314=CARTESIAN_POINT('Ctrl Pts',(0.0106757618624369,-0.0321423062648206,
0.0739510817958126));
#62315=CARTESIAN_POINT('Ctrl Pts',(0.0105981133585333,-0.0321733887792418,
0.0734960160453883));
#62316=CARTESIAN_POINT('Ctrl Pts',(0.0104095730206495,-0.0322044712936632,
0.0730876400735085));
#62317=CARTESIAN_POINT('Ctrl Pts',(0.00815332628724061,-0.0211072579114564,
0.0764745476396777));
#62318=CARTESIAN_POINT('Ctrl Pts',(0.00840215214987724,-0.0211255606965017,
0.0764737437596658));
#62319=CARTESIAN_POINT('Ctrl Pts',(0.00864919320439181,-0.0211438634815471,
0.0764340500831514));
#62320=CARTESIAN_POINT('Ctrl Pts',(0.00967605537954476,-0.0212246662665928,
0.0760808971366146));
#62321=CARTESIAN_POINT('Ctrl Pts',(0.0102733422062002,-0.0212871662665918,
0.0753606557973937));
#62322=CARTESIAN_POINT('Ctrl Pts',(0.0105612683570671,-0.0214121662665932,
0.0737692679062889));
#62323=CARTESIAN_POINT('Ctrl Pts',(0.0102565391923597,-0.021474666266593,
0.0729280907060315));
#62324=CARTESIAN_POINT('Ctrl Pts',(0.00909049684955361,-0.0215996662665919,
0.0718900934688763));
#62325=CARTESIAN_POINT('Ctrl Pts',(0.00825260378650262,-0.0216621662665925,
0.0717033226702191));
#62326=CARTESIAN_POINT('Ctrl Pts',(0.00679318847130807,-0.0217871662665924,
0.0720927335317618));
#62327=CARTESIAN_POINT('Ctrl Pts',(0.00618986329796383,-0.0218496662665923,
0.0726571638876892));
#62328=CARTESIAN_POINT('Ctrl Pts',(0.00568359379013531,-0.0219746662665926,
0.0740313301927182));
#62329=CARTESIAN_POINT('Ctrl Pts',(0.00578155954133694,-0.0220371662665924,
0.0748224925990252));
#62330=CARTESIAN_POINT('Ctrl Pts',(0.00655602261255478,-0.0221621662665925,
0.076015578504634));
#62331=CARTESIAN_POINT('Ctrl Pts',(0.00722019139059382,-0.0222246662665922,
0.0764071397497255));
#62332=CARTESIAN_POINT('Ctrl Pts',(0.00859809554021233,-0.0223496662665927,
0.0765345718796849));
#62333=CARTESIAN_POINT('Ctrl Pts',(0.00929804399292574,-0.0224121662665926,
0.0762731872241167));
#62334=CARTESIAN_POINT('Ctrl Pts',(0.010250065441227,-0.0225371662665923,
0.0753186463638511));
#62335=CARTESIAN_POINT('Ctrl Pts',(0.0104961904099933,-0.0225996662665926,
0.0746363211000744));
#62336=CARTESIAN_POINT('Ctrl Pts',(0.0104005508475817,-0.0227246662665924,
0.0733246797802278));
#62337=CARTESIAN_POINT('Ctrl Pts',(0.0100625167520088,-0.0227871662665921,
0.0727056382289851));
#62338=CARTESIAN_POINT('Ctrl Pts',(0.00904912860513842,-0.0229121662665928,
0.0719164811073332));
#62339=CARTESIAN_POINT('Ctrl Pts',(0.00838276147471677,-0.0229746662665921,
0.0717500819062757));
#62340=CARTESIAN_POINT('Ctrl Pts',(0.00714217809165384,-0.0230996662665929,
0.0719447493287309));
#62341=CARTESIAN_POINT('Ctrl Pts',(0.0065759050711654,-0.0231621662665927,
0.0723022728294504));
#62342=CARTESIAN_POINT('Ctrl Pts',(0.00586614734384593,-0.0232871662665922,
0.0733055450405034));
#62343=CARTESIAN_POINT('Ctrl Pts',(0.00572539440382979,-0.0233496662665926,
0.073943970666777));
#62344=CARTESIAN_POINT('Ctrl Pts',(0.00592552003453053,-0.0234746662665924,
0.0751309972301058));
#62345=CARTESIAN_POINT('Ctrl Pts',(0.00626351738443437,-0.0235371662665921,
0.0756731587170833));
#62346=CARTESIAN_POINT('Ctrl Pts',(0.00721234684475271,-0.0236621662665928,
0.0763748333085017));
#62347=CARTESIAN_POINT('Ctrl Pts',(0.00781726037633776,-0.0237246662665926,
0.0765319290828517));
#62348=CARTESIAN_POINT('Ctrl Pts',(0.00896730939589689,-0.0238496662665925,
0.076398555902516));
#62349=CARTESIAN_POINT('Ctrl Pts',(0.00950700226631619,-0.0239121662665925,
0.0761101356971356));
#62350=CARTESIAN_POINT('Ctrl Pts',(0.010254007677104,-0.0240371662665925,
0.0752534351443655));
#62351=CARTESIAN_POINT('Ctrl Pts',(0.0104588843013103,-0.0240996662665926,
0.0746898711283627));
#62352=CARTESIAN_POINT('Ctrl Pts',(0.0104500540367917,-0.0242246662665924,
0.0735732660853268));
#62353=CARTESIAN_POINT('Ctrl Pts',(0.0102375227040588,-0.0242871662665928,
0.0730249416515866));
#62354=CARTESIAN_POINT('Ctrl Pts',(0.00951342941930744,-0.0244121662665922,
0.0721999908129729));
#62355=CARTESIAN_POINT('Ctrl Pts',(0.00900550661104702,-0.0244746662665927,
0.0719259507427556));
#62356=CARTESIAN_POINT('Ctrl Pts',(0.00793799198823834,-0.0245996662665922,
0.0717647714878526));
#62357=CARTESIAN_POINT('Ctrl Pts',(0.0073824994148905,-0.0246621662665923,
0.071877307532445));
#62358=CARTESIAN_POINT('Ctrl Pts',(0.00647090305920422,-0.0247871662665926,
0.0724229731370429));
#62359=CARTESIAN_POINT('Ctrl Pts',(0.0061175390822829,-0.0248496662665925,
0.0728534733596938));
#62360=CARTESIAN_POINT('Ctrl Pts',(0.0057559180058162,-0.0249746662665924,
0.0738350207207137));
#62361=CARTESIAN_POINT('Ctrl Pts',(0.00574811958679247,-0.0250371662665924,
0.0743825825552014));
#62362=CARTESIAN_POINT('Ctrl Pts',(0.00606748354576255,-0.0251621662665925,
0.075362230730441));
#62363=CARTESIAN_POINT('Ctrl Pts',(0.00639298543709791,-0.0252246662665924,
0.0757915095294001));
#62364=CARTESIAN_POINT('Ctrl Pts',(0.00723254201175921,-0.0253496662665925,
0.0763626685001477));
#62365=CARTESIAN_POINT('Ctrl Pts',(0.00774378154132399,-0.0254121662665926,
0.0765034194843978));
#62366=CARTESIAN_POINT('Ctrl Pts',(0.00874354049187196,-0.0255371662665924,
0.0764519303687327));
#62367=CARTESIAN_POINT('Ctrl Pts',(0.00922933182513614,-0.025599666266592,
0.0762604290571012));
#62368=CARTESIAN_POINT('Ctrl Pts',(0.00999001579168093,-0.0257246662665929,
0.0756309871558503));
#62369=CARTESIAN_POINT('Ctrl Pts',(0.0102632712006387,-0.0257871662665926,
0.0751951159850686));
#62370=CARTESIAN_POINT('Ctrl Pts',(0.0105027538882435,-0.0259121662665923,
0.0742508678118485));
#62371=CARTESIAN_POINT('Ctrl Pts',(0.0104688803165286,-0.0259746662665924,
0.0737449568761991));
#62372=CARTESIAN_POINT('Ctrl Pts',(0.0101172277391856,-0.0260996662665926,
0.0728501076962283));
#62373=CARTESIAN_POINT('Ctrl Pts',(0.00980071482414927,-0.0261621662665928,
0.0724631046418761));
#62374=CARTESIAN_POINT('Ctrl Pts',(0.00900749170282425,-0.0262871662665921,
0.0719416575205446));
#62375=CARTESIAN_POINT('Ctrl Pts',(0.00853279776289023,-0.0263496662665926,
0.0718080167269426));
#62376=CARTESIAN_POINT('Ctrl Pts',(0.0075955800831525,-0.0264746662665923,
0.0718319875055733));
#62377=CARTESIAN_POINT('Ctrl Pts',(0.0071350448081896,-0.0265371662665915,
0.0719891427483816));
#62378=CARTESIAN_POINT('Ctrl Pts',(0.0063840705858361,-0.0266621662665934,
0.0725312630827505));
#62379=CARTESIAN_POINT('Ctrl Pts',(0.00609493832603504,-0.0267246662665926,
0.0729148185450287));
#62380=CARTESIAN_POINT('Ctrl Pts',(0.00567150376979967,-0.0268919420154909,
0.0740641461150897));
#62381=CARTESIAN_POINT('Ctrl Pts',(0.00579022688422278,-0.0269967177643891,
0.0749243565323479));
#62382=CARTESIAN_POINT('Ctrl Pts',(0.00673062180767083,-0.0272062692621875,
0.0761758856211119));
#62383=CARTESIAN_POINT('Ctrl Pts',(0.00754107324008372,-0.0273110450110865,
0.076544093544357));
#62384=CARTESIAN_POINT('Ctrl Pts',(0.00913286211817163,-0.0275205965088817,
0.0763978859664261));
#62385=CARTESIAN_POINT('Ctrl Pts',(0.00988589289648584,-0.0276253722577802,
0.0758805062803154));
#62386=CARTESIAN_POINT('Ctrl Pts',(0.0105806569015859,-0.0278349237555796,
0.0744018983400594));
#62387=CARTESIAN_POINT('Ctrl Pts',(0.0105035012565028,-0.0279396995044774,
0.0734660931660017));
#62388=CARTESIAN_POINT('Ctrl Pts',(0.00952680560062186,-0.028149251002274,
0.072109824349359));
#62389=CARTESIAN_POINT('Ctrl Pts',(0.00864171718187381,-0.0282540267511745,
0.0717216915578374));
#62390=CARTESIAN_POINT('Ctrl Pts',(0.00694717056566465,-0.0284635782489686,
0.0719635591456149));
#62391=CARTESIAN_POINT('Ctrl Pts',(0.0061774297989796,-0.0285683539978693,
0.0725961952733644));
#62392=CARTESIAN_POINT('Ctrl Pts',(0.00577133691614923,-0.0287255176212164,
0.0738483685540666));
#62393=CARTESIAN_POINT('Ctrl Pts',(0.00575623435121828,-0.0287779054956661,
0.0743074083721862));
#62394=CARTESIAN_POINT('Ctrl Pts',(0.00598037625292647,-0.0288826812445643,
0.0751677775536731));
#62395=CARTESIAN_POINT('Ctrl Pts',(0.006219576669604,-0.0289350691190143,
0.0755675389519453));
#62396=CARTESIAN_POINT('Ctrl Pts',(0.00688501715781157,-0.0290398448679119,
0.0761750621069688));
#62397=CARTESIAN_POINT('Ctrl Pts',(0.00731030903013384,-0.0290922327423619,
0.0763814412976357));
#62398=CARTESIAN_POINT('Ctrl Pts',(0.00821272207368966,-0.0291970084912602,
0.0765234275937696));
#62399=CARTESIAN_POINT('Ctrl Pts',(0.0086881821973765,-0.0292493963657099,
0.0764583541632762));
#62400=CARTESIAN_POINT('Ctrl Pts',(0.00952801531425379,-0.0293541721146081,
0.0760670747619161));
#62401=CARTESIAN_POINT('Ctrl Pts',(0.00989050099342927,-0.029406559989058,
0.0757412514171181));
#62402=CARTESIAN_POINT('Ctrl Pts',(0.0103691372816368,-0.0295113357379557,
0.0749321489062033));
#62403=CARTESIAN_POINT('Ctrl Pts',(0.0104838416490414,-0.0295637236124048,
0.0744503508285196));
#62404=CARTESIAN_POINT('Ctrl Pts',(0.0104120206910918,-0.0296684993613048,
0.0734988043112581));
#62405=CARTESIAN_POINT('Ctrl Pts',(0.0102251237098014,-0.0297208872357529,
0.0730312547594835));
#62406=CARTESIAN_POINT('Ctrl Pts',(0.00960512622564884,-0.0298256629846524,
0.0722864423988114));
#62407=CARTESIAN_POINT('Ctrl Pts',(0.00917306831712077,-0.0298780508591023,
0.0720113501056385));
#62408=CARTESIAN_POINT('Ctrl Pts',(0.00821853372773986,-0.0299828266079989,
0.0717696960530468));
#62409=CARTESIAN_POINT('Ctrl Pts',(0.00769834660242158,-0.03003521448245,
0.0718043795871957));
#62410=CARTESIAN_POINT('Ctrl Pts',(0.00677289295094829,-0.030139990231347,
0.072185813448155));
#62411=CARTESIAN_POINT('Ctrl Pts',(0.00637042834480692,-0.030192378105796,
0.0725321781376852));
#62412=CARTESIAN_POINT('Ctrl Pts',(0.00585556439734561,-0.0302971538546968,
0.0734105506653613));
#62413=CARTESIAN_POINT('Ctrl Pts',(0.00574534815560973,-0.0303495417291453,
0.0739403889886591));
#62414=CARTESIAN_POINT('Ctrl Pts',(0.00588053728891275,-0.0304543174780433,
0.0749677637423445));
#62415=CARTESIAN_POINT('Ctrl Pts',(0.00612638441272354,-0.0305067053524937,
0.0754619701971907));
#62416=CARTESIAN_POINT('Ctrl Pts',(0.0068862121828339,-0.0306114811013907,
0.0761943297562885));
#62417=CARTESIAN_POINT('Ctrl Pts',(0.00739831304479771,-0.03066386897584,
0.0764293216352161));
#62418=CARTESIAN_POINT('Ctrl Pts',(0.00847024498270537,-0.0307686447247403,
0.0765167649077124));
#62419=CARTESIAN_POINT('Ctrl Pts',(0.00902628537726555,-0.0308210325991885,
0.0763678171248695));
#62420=CARTESIAN_POINT('Ctrl Pts',(0.00992055447858949,-0.0309258083480876,
0.0757326667816004));
#62421=CARTESIAN_POINT('Ctrl Pts',(0.0102545830055701,-0.0309781962225361,
0.0752479510576141));
#62422=CARTESIAN_POINT('Ctrl Pts',(0.0105208009285865,-0.0310829719714357,
0.0741604785186885));
#62423=CARTESIAN_POINT('Ctrl Pts',(0.0104505271100099,-0.031135359845885,
0.073561995356696));
#62424=CARTESIAN_POINT('Ctrl Pts',(0.00991411670304271,-0.0312401355947827,
0.0725518154983641));
#62425=CARTESIAN_POINT('Ctrl Pts',(0.00944906750418523,-0.0312925234692314,
0.072145494478619));
#62426=CARTESIAN_POINT('Ctrl Pts',(0.00834579349582601,-0.0313972992181321,
0.0717572746685295));
#62427=CARTESIAN_POINT('Ctrl Pts',(0.00771250836259956,-0.0314496870925817,
0.0717790005685719));
#62428=CARTESIAN_POINT('Ctrl Pts',(0.00662086996932487,-0.0315544628414776,
0.0722706279495596));
#62429=CARTESIAN_POINT('Ctrl Pts',(0.00616934538289875,-0.0316068507159279,
0.0727396928462987));
#62430=CARTESIAN_POINT('Ctrl Pts',(0.00572829379585245,-0.0317116264648272,
0.0738846232116097));
#62431=CARTESIAN_POINT('Ctrl Pts',(0.00574362727005372,-0.031764014339277,
0.0745544281864965));
#62432=CARTESIAN_POINT('Ctrl Pts',(0.00621077743207889,-0.0318568507159276,
0.0755674191002066));
#62433=CARTESIAN_POINT('Ctrl Pts',(0.0065589500450449,-0.0318972992181318,
0.0759472268277333));
#62434=CARTESIAN_POINT('Ctrl Pts',(0.00742682523931609,-0.0319781962225358,
0.076428809978167));
#62435=CARTESIAN_POINT('Ctrl Pts',(0.00794469937310318,-0.0320186447247393,
0.0765285726773943));
#62436=CARTESIAN_POINT('Ctrl Pts',(0.00894927041430031,-0.0320995417291451,
0.0763879114871669));
#62437=CARTESIAN_POINT('Ctrl Pts',(0.00943299421279664,-0.032139990231348,
0.0761469018867863));
#62438=CARTESIAN_POINT('Ctrl Pts',(0.0101564533217469,-0.0322208872357532,
0.0754029570343451));
#62439=CARTESIAN_POINT('Ctrl Pts',(0.0103931454890576,-0.0322613357379553,
0.0749015233854856));
#62440=CARTESIAN_POINT('Ctrl Pts',(0.0104828841518005,-0.0323328667545812,
0.0739661159625376));
#62441=CARTESIAN_POINT('Ctrl Pts',(0.0104111042940494,-0.0323639492690025,
0.0735454439187662));
#62442=CARTESIAN_POINT('Ctrl Pts',(0.0102368137674672,-0.0323950317834238,
0.0731679328567764));
#62443=CARTESIAN_POINT('Ctrl Pts',(0.00814801668780212,-0.0211072579114564,
0.07605678506462));
#62444=CARTESIAN_POINT('Ctrl Pts',(0.00835212411518636,-0.0211255606965017,
0.076056125656151));
#62445=CARTESIAN_POINT('Ctrl Pts',(0.00855476749622787,-0.0211438634815471,
0.0760235656396361));
#62446=CARTESIAN_POINT('Ctrl Pts',(0.00939708426598712,-0.0212246662665928,
0.0757338805617789));
#62447=CARTESIAN_POINT('Ctrl Pts',(0.00988702802146066,-0.0212871662665918,
0.0751430794075642));
#62448=CARTESIAN_POINT('Ctrl Pts',(0.0101232087195095,-0.0214121662665932,
0.0738376922384734));
#62449=CARTESIAN_POINT('Ctrl Pts',(0.00987324480820894,-0.021474666266593,
0.073147689549446));
#62450=CARTESIAN_POINT('Ctrl Pts',(0.0089167610235679,-0.0215996662665919,
0.0722962388864693));
#62451=CARTESIAN_POINT('Ctrl Pts',(0.00822945225385138,-0.0216621662665925,
0.0721430341238275));
#62452=CARTESIAN_POINT('Ctrl Pts',(0.00703231984039108,-0.0217871662665924,
0.0724624609241718));
#62453=CARTESIAN_POINT('Ctrl Pts',(0.00653742293657822,-0.0218496662665923,
0.0729254531013723));
#62454=CARTESIAN_POINT('Ctrl Pts',(0.00612213906812888,-0.0219746662665926,
0.0740526572687589));
#62455=CARTESIAN_POINT('Ctrl Pts',(0.0062024986305861,-0.0220371662665924,
0.0747016337122979));
#62456=CARTESIAN_POINT('Ctrl Pts',(0.00683777690670826,-0.0221621662665925,
0.0756803008502788));
#62457=CARTESIAN_POINT('Ctrl Pts',(0.00738258273676963,-0.0222246662665922,
0.0760014915719832));
#62458=CARTESIAN_POINT('Ctrl Pts',(0.00851285299155973,-0.0223496662665927,
0.0761060218805955));
#62459=CARTESIAN_POINT('Ctrl Pts',(0.00908700825207452,-0.0224121662665926,
0.0758916126988471));
#62460=CARTESIAN_POINT('Ctrl Pts',(0.009867934505352,-0.0225371662665923,
0.0751086198167669));
#62461=CARTESIAN_POINT('Ctrl Pts',(0.0100698264375556,-0.0225996662665926,
0.0745489205445409));
#62462=CARTESIAN_POINT('Ctrl Pts',(0.00999137500636933,-0.0227246662665924,
0.0734730045098974));
#62463=CARTESIAN_POINT('Ctrl Pts',(0.00971409165292503,-0.0227871662665921,
0.0729652157409598));
#62464=CARTESIAN_POINT('Ctrl Pts',(0.00888282738880219,-0.0229121662665928,
0.0723178841967402));
#62465=CARTESIAN_POINT('Ctrl Pts',(0.00833621828939995,-0.0229746662665921,
0.0721813898931065));
#62466=CARTESIAN_POINT('Ctrl Pts',(0.00731858981585824,-0.0230996662665929,
0.0723410721157334));
#62467=CARTESIAN_POINT('Ctrl Pts',(0.00685408613370773,-0.0231621662665927,
0.0726343422814147));
#62468=CARTESIAN_POINT('Ctrl Pts',(0.00627188449978499,-0.0232871662665922,
0.0734573086233949));
#62469=CARTESIAN_POINT('Ctrl Pts',(0.00615642736772064,-0.0233496662665926,
0.07398099780415));
#62470=CARTESIAN_POINT('Ctrl Pts',(0.00632058686144516,-0.0234746662665924,
0.0749546945714818));
#62471=CARTESIAN_POINT('Ctrl Pts',(0.00659784007307093,-0.0235371662665921,
0.0753994199917464));
#62472=CARTESIAN_POINT('Ctrl Pts',(0.007376147995406,-0.0236621662665928,
0.075974991173125));
#62473=CARTESIAN_POINT('Ctrl Pts',(0.00787234780121979,-0.0237246662665926,
0.0761038540413805));
#62474=CARTESIAN_POINT('Ctrl Pts',(0.00881571254739481,-0.0238496662665925,
0.0759944503948627));
#62475=CARTESIAN_POINT('Ctrl Pts',(0.00925841300542465,-0.0239121662665925,
0.0757578644326881));
#62476=CARTESIAN_POINT('Ctrl Pts',(0.0098711682512917,-0.0240371662665925,
0.0750551282138252));
#62477=CARTESIAN_POINT('Ctrl Pts',(0.0100392249004471,-0.0240996662665926,
0.0745928466798487));
#62478=CARTESIAN_POINT('Ctrl Pts',(0.0100319815915929,-0.0242246662665924,
0.0736769154324963));
#62479=CARTESIAN_POINT('Ctrl Pts',(0.0098576459212449,-0.0242871662665928,
0.0732271346566689));
#62480=CARTESIAN_POINT('Ctrl Pts',(0.00926368508465529,-0.0244121662665922,
0.0725504421633576));
#62481=CARTESIAN_POINT('Ctrl Pts',(0.00884704504328137,-0.0244746662665927,
0.0723256519701696));
#62482=CARTESIAN_POINT('Ctrl Pts',(0.00797138179410088,-0.0245996662665922,
0.07219343949548));
#62483=CARTESIAN_POINT('Ctrl Pts',(0.00751572112090685,-0.0246621662665923,
0.0722857508103344));
#62484=CARTESIAN_POINT('Ctrl Pts',(0.00676795485175628,-0.0247871662665926,
0.0727333505959289));
#62485=CARTESIAN_POINT('Ctrl Pts',(0.00647809666942974,-0.0248496662665925,
0.073086482268025));
#62486=CARTESIAN_POINT('Ctrl Pts',(0.00618146533527733,-0.0249746662665924,
0.0738916281021063));
#62487=CARTESIAN_POINT('Ctrl Pts',(0.00617506843092123,-0.0250371662665924,
0.0743407833313369));
#62488=CARTESIAN_POINT('Ctrl Pts',(0.00643703700353636,-0.0251621662665925,
0.0751443712971177));
#62489=CARTESIAN_POINT('Ctrl Pts',(0.00670404041284908,-0.0252246662665924,
0.0754965010570941));
#62490=CARTESIAN_POINT('Ctrl Pts',(0.00739271373153814,-0.0253496662665925,
0.0759650125972991));
#62491=CARTESIAN_POINT('Ctrl Pts',(0.00781207442037852,-0.0254121662665926,
0.0760804681250833));
#62492=CARTESIAN_POINT('Ctrl Pts',(0.00863215889728322,-0.0255371662665924,
0.0760382325197273));
#62493=CARTESIAN_POINT('Ctrl Pts',(0.0090306448835366,-0.025599666266592,
0.0758811474014697));
#62494=CARTESIAN_POINT('Ctrl Pts',(0.0096546204052879,-0.0257246662665929,
0.0753648274104897));
#62495=CARTESIAN_POINT('Ctrl Pts',(0.00987876695480732,-0.0257871662665926,
0.0750072900452153));
#62496=CARTESIAN_POINT('Ctrl Pts',(0.0100752103419703,-0.0259121662665923,
0.0742327400711651));
#62497=CARTESIAN_POINT('Ctrl Pts',(0.0100474244538565,-0.0259746662665924,
0.0738177503330937));
#62498=CARTESIAN_POINT('Ctrl Pts',(0.00975897010215047,-0.0260996662665926,
0.0730837214741746));
#62499=CARTESIAN_POINT('Ctrl Pts',(0.00949934019014137,-0.0261621662665928,
0.0727662697552228));
#62500=CARTESIAN_POINT('Ctrl Pts',(0.00884867337874248,-0.0262871662665921,
0.0723385359604954));
#62501=CARTESIAN_POINT('Ctrl Pts',(0.00845929038676506,-0.0263496662665926,
0.0722289127955772));
#62502=CARTESIAN_POINT('Ctrl Pts',(0.00769050740141413,-0.0264746662665923,
0.0722485755987396));
#62503=CARTESIAN_POINT('Ctrl Pts',(0.0073127385103659,-0.0265371662665915,
0.0723774872479133));
#62504=CARTESIAN_POINT('Ctrl Pts',(0.00669672771899448,-0.0266621662665934,
0.0728221789114253));
#62505=CARTESIAN_POINT('Ctrl Pts',(0.00645955767124918,-0.0267246662665926,
0.0731368026319471));
#62506=CARTESIAN_POINT('Ctrl Pts',(0.00611222183958379,-0.0268919420154909,
0.0740795755859367));
#62507=CARTESIAN_POINT('Ctrl Pts',(0.00620960829772417,-0.0269967177643891,
0.0747851908841829));
#62508=CARTESIAN_POINT('Ctrl Pts',(0.00698099751955323,-0.0272062692621875,
0.0758117979253375));
#62509=CARTESIAN_POINT('Ctrl Pts',(0.00764579640796796,-0.0273110450110865,
0.0761138323326925));
#62510=CARTESIAN_POINT('Ctrl Pts',(0.00895151249954563,-0.0275205965088817,
0.0759939008582095));
#62511=CARTESIAN_POINT('Ctrl Pts',(0.00956921024717631,-0.0276253722577802,
0.0755695035082156));
#62512=CARTESIAN_POINT('Ctrl Pts',(0.0101391127975682,-0.0278349237555796,
0.0743566277259409));
#62513=CARTESIAN_POINT('Ctrl Pts',(0.0100758233948543,-0.0279396995044774,
0.0735890033938645));
#62514=CARTESIAN_POINT('Ctrl Pts',(0.00927465732816471,-0.028149251002274,
0.0724764802177239));
#62515=CARTESIAN_POINT('Ctrl Pts',(0.00854863504798854,-0.0282540267511745,
0.0721581017954751));
#62516=CARTESIAN_POINT('Ctrl Pts',(0.0071586286123545,-0.0284635782489686,
0.0723565014738116));
#62517=CARTESIAN_POINT('Ctrl Pts',(0.00652722395860935,-0.0285683539978693,
0.0728754416319487));
#62518=CARTESIAN_POINT('Ctrl Pts',(0.0061941131930515,-0.0287255176212164,
0.0739025770922874));
#62519=CARTESIAN_POINT('Ctrl Pts',(0.00618172482778142,-0.0287779054956661,
0.0742791192866981));
#62520=CARTESIAN_POINT('Ctrl Pts',(0.00636558444125528,-0.0288826812445643,
0.0749848648164158));
#62521=CARTESIAN_POINT('Ctrl Pts',(0.00656179628659944,-0.0289350691190143,
0.0753127819778567));
#62522=CARTESIAN_POINT('Ctrl Pts',(0.0071076452778826,-0.0290398448679119,
0.0758111224113399));
#62523=CARTESIAN_POINT('Ctrl Pts',(0.00745650463288417,-0.0290922327423619,
0.0759804115890255));
#62524=CARTESIAN_POINT('Ctrl Pts',(0.00819673799450679,-0.0291970084912602,
0.0760968804211664));
#62525=CARTESIAN_POINT('Ctrl Pts',(0.00858674947338286,-0.0292493963657099,
0.0760435018440831));
#62526=CARTESIAN_POINT('Ctrl Pts',(0.00927564963473071,-0.0293541721146081,
0.0757225423137761));
#62527=CARTESIAN_POINT('Ctrl Pts',(0.00957299018710003,-0.029406559989058,
0.0754552752219081));
#62528=CARTESIAN_POINT('Ctrl Pts',(0.00996560701721403,-0.0295113357379557,
0.0747915828297948));
#62529=CARTESIAN_POINT('Ctrl Pts',(0.010059696968687,-0.0295637236124048,
0.074396372440036));
#62530=CARTESIAN_POINT('Ctrl Pts',(0.0100007835149004,-0.0296684993613048,
0.0736158357642392));
#62531=CARTESIAN_POINT('Ctrl Pts',(0.00984747524688978,-0.0297208872357529,
0.073232313186738));
#62532=CARTESIAN_POINT('Ctrl Pts',(0.00933890234319653,-0.0298256629846524,
0.0726213568608565));
#62533=CARTESIAN_POINT('Ctrl Pts',(0.00898449292909369,-0.0298780508591023,
0.0723957035479018));
#62534=CARTESIAN_POINT('Ctrl Pts',(0.00820150519090858,-0.0299828266079989,
0.0721974790286785));
#62535=CARTESIAN_POINT('Ctrl Pts',(0.00777480494848981,-0.03003521448245,
0.072225929314564));
#62536=CARTESIAN_POINT('Ctrl Pts',(0.00701567178618897,-0.030139990231347,
0.0725388127232768));
#62537=CARTESIAN_POINT('Ctrl Pts',(0.00668553723143537,-0.030192378105796,
0.0728229295147053));
#62538=CARTESIAN_POINT('Ctrl Pts',(0.00626320349708927,-0.0302971538546968,
0.0735434428689412));
#62539=CARTESIAN_POINT('Ctrl Pts',(0.00617279507523841,-0.0303495417291453,
0.0739780598173242));
#62540=CARTESIAN_POINT('Ctrl Pts',(0.00628368831566111,-0.0304543174780433,
0.0748207970461326));
#62541=CARTESIAN_POINT('Ctrl Pts',(0.00648535233659179,-0.0305067053524937,
0.0752261858068767));
#62542=CARTESIAN_POINT('Ctrl Pts',(0.00710862553564354,-0.0306114811013907,
0.0758269273212183));
#62543=CARTESIAN_POINT('Ctrl Pts',(0.00752869276012381,-0.03066386897584,
0.0760196869779353));
#62544=CARTESIAN_POINT('Ctrl Pts',(0.00840797945427604,-0.0307686447247403,
0.076091415138353));
#62545=CARTESIAN_POINT('Ctrl Pts',(0.00886408949546226,-0.0308210325991885,
0.075969235922541));
#62546=CARTESIAN_POINT('Ctrl Pts',(0.00959764252618967,-0.0309258083480876,
0.0754482333981525));
#62547=CARTESIAN_POINT('Ctrl Pts',(0.00987164018299474,-0.0309781962225361,
0.0750506297150497));
#62548=CARTESIAN_POINT('Ctrl Pts',(0.0100900140080253,-0.0310829719714357,
0.07415859534242));
#62549=CARTESIAN_POINT('Ctrl Pts',(0.0100323696451357,-0.031135359845885,
0.0736676702543576));
#62550=CARTESIAN_POINT('Ctrl Pts',(0.00959236173346572,-0.0312401355947827,
0.0728390376922328));
#62551=CARTESIAN_POINT('Ctrl Pts',(0.00921089015096985,-0.0312925234692314,
0.0725057397900231));
#62552=CARTESIAN_POINT('Ctrl Pts',(0.00830589411414326,-0.0313972992181321,
0.0721872899879916));
#62553=CARTESIAN_POINT('Ctrl Pts',(0.00778642158836204,-0.0314496870925817,
0.0722051113571944));
#62554=CARTESIAN_POINT('Ctrl Pts',(0.00689097003953919,-0.0315544628414776,
0.0726083845495457));
#62555=CARTESIAN_POINT('Ctrl Pts',(0.00652059245595663,-0.0316068507159279,
0.0729931501375565));
#62556=CARTESIAN_POINT('Ctrl Pts',(0.00615880568740368,-0.0317116264648272,
0.0739323161427358));
#62557=CARTESIAN_POINT('Ctrl Pts',(0.00617138346343902,-0.031764014339277,
0.0744817452447779));
#62558=CARTESIAN_POINT('Ctrl Pts',(0.00655457842863585,-0.0318568507159276,
0.0753126836656081));
#62559=CARTESIAN_POINT('Ctrl Pts',(0.00684017822748756,-0.0318972992181318,
0.0756242331860024));
#62560=CARTESIAN_POINT('Ctrl Pts',(0.00755208080592647,-0.0319781962225358,
0.0760192672747625));
#62561=CARTESIAN_POINT('Ctrl Pts',(0.0079768837425508,-0.0320186447247393,
0.0761011008417093));
#62562=CARTESIAN_POINT('Ctrl Pts',(0.00880091549178614,-0.0320995417291451,
0.0759857189703642));
#62563=CARTESIAN_POINT('Ctrl Pts',(0.00919770551606028,-0.032139990231348,
0.0757880230838218));
#62564=CARTESIAN_POINT('Ctrl Pts',(0.00979114614952519,-0.0322208872357532,
0.0751777783595053));
#62565=CARTESIAN_POINT('Ctrl Pts',(0.00998530052254685,-0.0322613357379553,
0.0747664612601165));
#62566=CARTESIAN_POINT('Ctrl Pts',(0.0100589115507385,-0.0323328667545812,
0.0739991631961976));
#62567=CARTESIAN_POINT('Ctrl Pts',(0.0100000318107133,-0.0323639492690025,
0.0736540934043486));
#62568=CARTESIAN_POINT('Ctrl Pts',(0.00985706439317406,-0.0323950317834238,
0.0733444277978263));
#62569=CARTESIAN_POINT('Ctrl Pts',(0.0081456011935425,-0.0209166974216957,
0.0758667324789935));
#62570=CARTESIAN_POINT('Ctrl Pts',(0.00832936487844643,-0.020935000206741,
0.0758661387949141));
#62571=CARTESIAN_POINT('Ctrl Pts',(0.00851181044105437,-0.0209533029917864,
0.075836824091907));
#62572=CARTESIAN_POINT('Ctrl Pts',(0.00927017203255066,-0.0210341057768321,
0.075576012429877));
#62573=CARTESIAN_POINT('Ctrl Pts',(0.0097112822413036,-0.0210966057768311,
0.0750440974548303));
#62574=CARTESIAN_POINT('Ctrl Pts',(0.00992392239817022,-0.0212216057768325,
0.0738688204965506));
#62575=CARTESIAN_POINT('Ctrl Pts',(0.00969887282490249,-0.0212841057768323,
0.0732475915762989));
#62576=CARTESIAN_POINT('Ctrl Pts',(0.00883772344357415,-0.0214091057768312,
0.0724810064826171));
#62577=CARTESIAN_POINT('Ctrl Pts',(0.00821891993500742,-0.0214716057768319,
0.0723430719052785));
#62578=CARTESIAN_POINT('Ctrl Pts',(0.00714110779247693,-0.0215966057768317,
0.072630660880558));
#62579=CARTESIAN_POINT('Ctrl Pts',(0.00669553812429927,-0.0216591057768317,
0.0730475058217461));
#62580=CARTESIAN_POINT('Ctrl Pts',(0.00632164632170585,-0.0217841057768319,
0.07406235958818));
#62581=CARTESIAN_POINT('Ctrl Pts',(0.00639399630672924,-0.0218466057768317,
0.0746466514202262));
#62582=CARTESIAN_POINT('Ctrl Pts',(0.00696595529154281,-0.0219716057768319,
0.075527773101463));
#62583=CARTESIAN_POINT('Ctrl Pts',(0.00745645937643706,-0.0220341057768316,
0.0758169501849909));
#62584=CARTESIAN_POINT('Ctrl Pts',(0.00847407362800718,-0.0221591057768321,
0.0759110617758377));
#62585=CARTESIAN_POINT('Ctrl Pts',(0.00899100183454682,-0.0222216057768319,
0.0757180231303543));
#62586=CARTESIAN_POINT('Ctrl Pts',(0.00969409180917257,-0.0223466057768317,
0.0750130725114152));
#62587=CARTESIAN_POINT('Ctrl Pts',(0.00987586082115598,-0.0224091057768319,
0.0745091594396549));
#62588=CARTESIAN_POINT('Ctrl Pts',(0.00980522878063905,-0.0225341057768317,
0.0735404818285206));
#62589=CARTESIAN_POINT('Ctrl Pts',(0.00955558274156816,-0.0225966057768315,
0.07308330524985));
#62590=CARTESIAN_POINT('Ctrl Pts',(0.00880717203323765,-0.0227216057768321,
0.0725004943671456));
#62591=CARTESIAN_POINT('Ctrl Pts',(0.00831504441399582,-0.0227841057768314,
0.072377604688286));
#62592=CARTESIAN_POINT('Ctrl Pts',(0.00739884474131507,-0.0229091057768322,
0.0725213711059004));
#62593=CARTESIAN_POINT('Ctrl Pts',(0.00698063894950555,-0.0229716057768321,
0.0727854105238122));
#62594=CARTESIAN_POINT('Ctrl Pts',(0.00645646636559797,-0.0230966057768316,
0.0735263503783403));
#62595=CARTESIAN_POINT('Ctrl Pts',(0.00635251704680801,-0.023159105776832,
0.0739978425471124));
#62596=CARTESIAN_POINT('Ctrl Pts',(0.00650031447811829,-0.0232841057768316,
0.0748744892631922));
#62597=CARTESIAN_POINT('Ctrl Pts',(0.00674993337965833,-0.0233466057768315,
0.0752748881268966));
#62598=CARTESIAN_POINT('Ctrl Pts',(0.00745066599694304,-0.0234716057768321,
0.0757930911270036));
#62599=CARTESIAN_POINT('Ctrl Pts',(0.00789740870461186,-0.0235341057768318,
0.0759091100089296));
#62600=CARTESIAN_POINT('Ctrl Pts',(0.00874674664486829,-0.0236591057768317,
0.0758106108142473));
#62601=CARTESIAN_POINT('Ctrl Pts',(0.00914532237784772,-0.0237216057768318,
0.0755976057866355));
#62602=CARTESIAN_POINT('Ctrl Pts',(0.00969700324202693,-0.0238466057768318,
0.0749649125096261));
#62603=CARTESIAN_POINT('Ctrl Pts',(0.00984830939250459,-0.0239091057768318,
0.0745487073806151));
#62604=CARTESIAN_POINT('Ctrl Pts',(0.00984178803684884,-0.0240341057768317,
0.0737240685946132));
#62605=CARTESIAN_POINT('Ctrl Pts',(0.00968482870614778,-0.0240966057768321,
0.0733191182514325));
#62606=CARTESIAN_POINT('Ctrl Pts',(0.00915006897976686,-0.0242216057768316,
0.0727098728765269));
#62607=CARTESIAN_POINT('Ctrl Pts',(0.00877495617636422,-0.0242841057768321,
0.0725074879130797));
#62608=CARTESIAN_POINT('Ctrl Pts',(0.00798657180708102,-0.0244091057768316,
0.0723884532858218));
#62609=CARTESIAN_POINT('Ctrl Pts',(0.00757632762613652,-0.0244716057768317,
0.0724715637712821));
#62610=CARTESIAN_POINT('Ctrl Pts',(0.00690309252231404,-0.0245966057768319,
0.072874550507322));
#62611=CARTESIAN_POINT('Ctrl Pts',(0.00664212500943859,-0.0246591057768318,
0.0731924849311315));
#62612=CARTESIAN_POINT('Ctrl Pts',(0.0063750594365665,-0.0247841057768317,
0.0739173804787947));
#62613=CARTESIAN_POINT('Ctrl Pts',(0.00636930012279967,-0.0248466057768317,
0.0743217676246966));
#62614=CARTESIAN_POINT('Ctrl Pts',(0.00660515783189783,-0.0249716057768318,
0.0750452605795038));
#62615=CARTESIAN_POINT('Ctrl Pts',(0.00684554854675824,-0.0250341057768317,
0.0753622929535182));
#62616=CARTESIAN_POINT('Ctrl Pts',(0.00746558059732679,-0.0251591057768318,
0.0757841071331952));
#62617=CARTESIAN_POINT('Ctrl Pts',(0.00784314287652831,-0.0252216057768319,
0.0758880550076066));
#62618=CARTESIAN_POINT('Ctrl Pts',(0.00858148810648805,-0.0253466057768317,
0.0758500290985359));
#62619=CARTESIAN_POINT('Ctrl Pts',(0.00894025630103604,-0.0254091057768313,
0.0757086009273785));
#62620=CARTESIAN_POINT('Ctrl Pts',(0.00950203909667648,-0.0255341057768323,
0.0752437434484126));
#62621=CARTESIAN_POINT('Ctrl Pts',(0.00970384456953965,-0.025596605776832,
0.0749218424545307));
#62622=CARTESIAN_POINT('Ctrl Pts',(0.00988070810244839,-0.0257216057768316,
0.0742244932242857));
#62623=CARTESIAN_POINT('Ctrl Pts',(0.00985569168215658,-0.0257841057768317,
0.0738508662355836));
#62624=CARTESIAN_POINT('Ctrl Pts',(0.0095959880776607,-0.0259091057768319,
0.0731899993104086));
#62625=CARTESIAN_POINT('Ctrl Pts',(0.0093622359307961,-0.0259716057768321,
0.0729041885567222));
#62626=CARTESIAN_POINT('Ctrl Pts',(0.00877642221279626,-0.0260966057768315,
0.0725190877336685));
#62627=CARTESIAN_POINT('Ctrl Pts',(0.00842584970124339,-0.0261591057768319,
0.0724203909003668));
#62628=CARTESIAN_POINT('Ctrl Pts',(0.00773369265389813,-0.0262841057768317,
0.0724380938777203));
#62629=CARTESIAN_POINT('Ctrl Pts',(0.00739357664562364,-0.0263466057768309,
0.0725541566784855));
#62630=CARTESIAN_POINT('Ctrl Pts',(0.00683896472182591,-0.0264716057768327,
0.0729545251500316));
#62631=CARTESIAN_POINT('Ctrl Pts',(0.0066254338254687,-0.0265341057768319,
0.0732377897768127));
#62632=CARTESIAN_POINT('Ctrl Pts',(0.00631271756058805,-0.0267013815257303,
0.0740865949098408));
#62633=CARTESIAN_POINT('Ctrl Pts',(0.00640039734097116,-0.0268061572746284,
0.0747218803033809));
#62634=CARTESIAN_POINT('Ctrl Pts',(0.00709490085666943,-0.0270157087724267,
0.0756461636342162));
#62635=CARTESIAN_POINT('Ctrl Pts',(0.00769343808297591,-0.0271204845213259,
0.0759180937465821));
#62636=CARTESIAN_POINT('Ctrl Pts',(0.00886901117946571,-0.027330036019121,
0.0758101160508686));
#62637=CARTESIAN_POINT('Ctrl Pts',(0.00942514191765672,-0.0274348117680204,
0.0754280191232956));
#62638=CARTESIAN_POINT('Ctrl Pts',(0.00993824128909218,-0.027644363265818,
0.0743360327809175));
#62639=CARTESIAN_POINT('Ctrl Pts',(0.00988126005128462,-0.0277491390147176,
0.0736449189018586));
#62640=CARTESIAN_POINT('Ctrl Pts',(0.00915994760067147,-0.0279586905125125,
0.072643282846725));
#62641=CARTESIAN_POINT('Ctrl Pts',(0.00850628922460295,-0.028063466261413,
0.0723566377558719));
#62642=CARTESIAN_POINT('Ctrl Pts',(0.00725482714933299,-0.0282730177592087,
0.0725352625930086));
#62643=CARTESIAN_POINT('Ctrl Pts',(0.00668635569621314,-0.0283777935081086,
0.0730024790825113));
#62644=CARTESIAN_POINT('Ctrl Pts',(0.00638644666034619,-0.0285349571314557,
0.0739272381640707));
#62645=CARTESIAN_POINT('Ctrl Pts',(0.00637529306500116,-0.0285873450059055,
0.0742662497426962));
#62646=CARTESIAN_POINT('Ctrl Pts',(0.00654082707084289,-0.0286921207548037,
0.0749016523873107));
#62647=CARTESIAN_POINT('Ctrl Pts',(0.00671748214010876,-0.0287445086292537,
0.0751968854746209));
#62648=CARTESIAN_POINT('Ctrl Pts',(0.00720892541253046,-0.0288492843781513,
0.0756455554498743));
#62649=CARTESIAN_POINT('Ctrl Pts',(0.00752301334852511,-0.0289016722526012,
0.0757979712806186));
#62650=CARTESIAN_POINT('Ctrl Pts',(0.00818946636282185,-0.0290064480014996,
0.0759028314615779));
#62651=CARTESIAN_POINT('Ctrl Pts',(0.00854060471889044,-0.0290588358759492,
0.0758547732201633));
#62652=CARTESIAN_POINT('Ctrl Pts',(0.00916084100231525,-0.0291636116248473,
0.075565804284784));
#62653=CARTESIAN_POINT('Ctrl Pts',(0.00942854510439027,-0.0292159994992974,
0.0753251761690674));
#62654=CARTESIAN_POINT('Ctrl Pts',(0.00978202913180507,-0.029320775248195,
0.0747276351526504));
#62655=CARTESIAN_POINT('Ctrl Pts',(0.00986674097407697,-0.029373163122644,
0.074371816070194));
#62656=CARTESIAN_POINT('Ctrl Pts',(0.00981369952675195,-0.0294779388715441,
0.0736690768431837));
#62657=CARTESIAN_POINT('Ctrl Pts',(0.00967567176060491,-0.0295303267459923,
0.0733237806283977));
#62658=CARTESIAN_POINT('Ctrl Pts',(0.00921778920325428,-0.0296351024948917,
0.0727737193827185));
#62659=CARTESIAN_POINT('Ctrl Pts',(0.00889870439220733,-0.0296874903693416,
0.0725705573281537));
#62660=CARTESIAN_POINT('Ctrl Pts',(0.00819375840446231,-0.0297922661182383,
0.0723920901917167));
#62661=CARTESIAN_POINT('Ctrl Pts',(0.00780958811776,-0.0298446539926894,
0.0724177047880981));
#62662=CARTESIAN_POINT('Ctrl Pts',(0.00712611907880853,-0.0299494297415862,
0.0726994025629769));
#62663=CARTESIAN_POINT('Ctrl Pts',(0.00682888960963579,-0.0300018176160353,
0.0729552009393765));
#62664=CARTESIAN_POINT('Ctrl Pts',(0.0064486506135478,-0.0301065933649361,
0.07360389947374));
#62665=CARTESIAN_POINT('Ctrl Pts',(0.00636725335643387,-0.0301589812393846,
0.0739951973945462));
#62666=CARTESIAN_POINT('Ctrl Pts',(0.00646709367460444,-0.0302637569882826,
0.0747539375372065));
#62667=CARTESIAN_POINT('Ctrl Pts',(0.00664865749162809,-0.0303161448627331,
0.0751189204946994));
#62668=CARTESIAN_POINT('Ctrl Pts',(0.00720980796629447,-0.03042092061163,
0.0756597850568809));
#62669=CARTESIAN_POINT('Ctrl Pts',(0.00758800635949914,-0.0304733084860793,
0.0758333320231676));
#62670=CARTESIAN_POINT('Ctrl Pts',(0.00837965301868817,-0.0305780842349796,
0.0758979109130133));
#62671=CARTESIAN_POINT('Ctrl Pts',(0.0087903017783351,-0.0306304721094278,
0.0757879095122608));
#62672=CARTESIAN_POINT('Ctrl Pts',(0.00945074030194221,-0.030735247858327,
0.0753188362161399));
#62673=CARTESIAN_POINT('Ctrl Pts',(0.00969742813547587,-0.0307876357327754,
0.074960862384052));
#62674=CARTESIAN_POINT('Ctrl Pts',(0.00989403626134592,-0.030892411481675,
0.0741577386296832));
#62675=CARTESIAN_POINT('Ctrl Pts',(0.00984213741241968,-0.0309447993561243,
0.0737157448994683));
#62676=CARTESIAN_POINT('Ctrl Pts',(0.00944598585501893,-0.031049575105022,
0.0729697035868178));
#62677=CARTESIAN_POINT('Ctrl Pts',(0.0091025362089969,-0.0311019629794706,
0.0726696260665349));
#62678=CARTESIAN_POINT('Ctrl Pts',(0.00828774270205792,-0.0312067387283715,
0.0723829167104463));
#62679=CARTESIAN_POINT('Ctrl Pts',(0.00782004690692066,-0.031259126602821,
0.0723989617927675));
#62680=CARTESIAN_POINT('Ctrl Pts',(0.00701384657225643,-0.0313639023517169,
0.0727620400442508));
#62681=CARTESIAN_POINT('Ctrl Pts',(0.00668038516697007,-0.0314162902261672,
0.0731084553765258));
#62682=CARTESIAN_POINT('Ctrl Pts',(0.00635465831522934,-0.0315210659750665,
0.0739540130716083));
#62683=CARTESIAN_POINT('Ctrl Pts',(0.00636598244243914,-0.0315734538495163,
0.0744486796189194));
#62684=CARTESIAN_POINT('Ctrl Pts',(0.00671098369860905,-0.0316662902261669,
0.0751967969613253));
#62685=CARTESIAN_POINT('Ctrl Pts',(0.00696811726850124,-0.0317067387283712,
0.0754772937988554));
#62686=CARTESIAN_POINT('Ctrl Pts',(0.00760906327807618,-0.0317876357327751,
0.0758329541525405));
#62687=CARTESIAN_POINT('Ctrl Pts',(0.00799152536675427,-0.0318280842349786,
0.0759066312254608));
#62688=CARTESIAN_POINT('Ctrl Pts',(0.00873342443754237,-0.0319089812393844,
0.0758027496660232));
#62689=CARTESIAN_POINT('Ctrl Pts',(0.00909066570959304,-0.0319494297415873,
0.0756247584725279));
#62690=CARTESIAN_POINT('Ctrl Pts',(0.00962495708239995,-0.0320303267459926,
0.0750753379018474));
#62691=CARTESIAN_POINT('Ctrl Pts',(0.00979975975119023,-0.0320707752481946,
0.0747050174935392));
#62692=CARTESIAN_POINT('Ctrl Pts',(0.00986603384010217,-0.0321423062648206,
0.0740141973629227));
#62693=CARTESIAN_POINT('Ctrl Pts',(0.00981302274622929,-0.0321733887792418,
0.0737035212777265));
#62694=CARTESIAN_POINT('Ctrl Pts',(0.00968430513999177,-0.0322044712936632,
0.0734247205810942));
#62695=CARTESIAN_POINT('Ctrl Pts',(0.0081456011935425,-0.0204978184012171,
0.0758667324789935));
#62696=CARTESIAN_POINT('Ctrl Pts',(0.00832936487844643,-0.0205161211862624,
0.0758661387949141));
#62697=CARTESIAN_POINT('Ctrl Pts',(0.00851181044105437,-0.0205344239713078,
0.075836824091907));
#62698=CARTESIAN_POINT('Ctrl Pts',(0.00927017203255066,-0.0206152267563535,
0.075576012429877));
#62699=CARTESIAN_POINT('Ctrl Pts',(0.0097112822413036,-0.0206777267563525,
0.0750440974548303));
#62700=CARTESIAN_POINT('Ctrl Pts',(0.00992392239817022,-0.0208027267563538,
0.0738688204965506));
#62701=CARTESIAN_POINT('Ctrl Pts',(0.00969887282490249,-0.0208652267563538,
0.0732475915762989));
#62702=CARTESIAN_POINT('Ctrl Pts',(0.00883772344357415,-0.0209902267563526,
0.0724810064826171));
#62703=CARTESIAN_POINT('Ctrl Pts',(0.00821891993500742,-0.0210527267563532,
0.0723430719052785));
#62704=CARTESIAN_POINT('Ctrl Pts',(0.00714110779247693,-0.0211777267563531,
0.072630660880558));
#62705=CARTESIAN_POINT('Ctrl Pts',(0.00669553812429927,-0.0212402267563531,
0.0730475058217461));
#62706=CARTESIAN_POINT('Ctrl Pts',(0.00632164632170585,-0.0213652267563533,
0.07406235958818));
#62707=CARTESIAN_POINT('Ctrl Pts',(0.00639399630672924,-0.0214277267563531,
0.0746466514202262));
#62708=CARTESIAN_POINT('Ctrl Pts',(0.00696595529154281,-0.0215527267563532,
0.075527773101463));
#62709=CARTESIAN_POINT('Ctrl Pts',(0.00745645937643706,-0.0216152267563529,
0.0758169501849909));
#62710=CARTESIAN_POINT('Ctrl Pts',(0.00847407362800718,-0.0217402267563534,
0.0759110617758377));
#62711=CARTESIAN_POINT('Ctrl Pts',(0.00899100183454682,-0.0218027267563532,
0.0757180231303543));
#62712=CARTESIAN_POINT('Ctrl Pts',(0.00969409180917257,-0.0219277267563531,
0.0750130725114152));
#62713=CARTESIAN_POINT('Ctrl Pts',(0.00987586082115598,-0.0219902267563532,
0.0745091594396549));
#62714=CARTESIAN_POINT('Ctrl Pts',(0.00980522878063905,-0.0221152267563531,
0.0735404818285206));
#62715=CARTESIAN_POINT('Ctrl Pts',(0.00955558274156816,-0.0221777267563529,
0.07308330524985));
#62716=CARTESIAN_POINT('Ctrl Pts',(0.00880717203323765,-0.0223027267563535,
0.0725004943671456));
#62717=CARTESIAN_POINT('Ctrl Pts',(0.00831504441399582,-0.0223652267563527,
0.072377604688286));
#62718=CARTESIAN_POINT('Ctrl Pts',(0.00739884474131507,-0.0224902267563536,
0.0725213711059004));
#62719=CARTESIAN_POINT('Ctrl Pts',(0.00698063894950555,-0.0225527267563534,
0.0727854105238122));
#62720=CARTESIAN_POINT('Ctrl Pts',(0.00645646636559797,-0.0226777267563529,
0.0735263503783403));
#62721=CARTESIAN_POINT('Ctrl Pts',(0.00635251704680801,-0.0227402267563533,
0.0739978425471124));
#62722=CARTESIAN_POINT('Ctrl Pts',(0.00650031447811829,-0.022865226756353,
0.0748744892631922));
#62723=CARTESIAN_POINT('Ctrl Pts',(0.00674993337965833,-0.0229277267563529,
0.0752748881268966));
#62724=CARTESIAN_POINT('Ctrl Pts',(0.00745066599694304,-0.0230527267563535,
0.0757930911270036));
#62725=CARTESIAN_POINT('Ctrl Pts',(0.00789740870461186,-0.0231152267563532,
0.0759091100089296));
#62726=CARTESIAN_POINT('Ctrl Pts',(0.00874674664486829,-0.0232402267563531,
0.0758106108142473));
#62727=CARTESIAN_POINT('Ctrl Pts',(0.00914532237784772,-0.0233027267563532,
0.0755976057866355));
#62728=CARTESIAN_POINT('Ctrl Pts',(0.00969700324202693,-0.0234277267563531,
0.0749649125096261));
#62729=CARTESIAN_POINT('Ctrl Pts',(0.00984830939250459,-0.0234902267563532,
0.0745487073806151));
#62730=CARTESIAN_POINT('Ctrl Pts',(0.00984178803684884,-0.0236152267563531,
0.0737240685946132));
#62731=CARTESIAN_POINT('Ctrl Pts',(0.00968482870614778,-0.0236777267563534,
0.0733191182514325));
#62732=CARTESIAN_POINT('Ctrl Pts',(0.00915006897976686,-0.0238027267563529,
0.0727098728765269));
#62733=CARTESIAN_POINT('Ctrl Pts',(0.00877495617636422,-0.0238652267563534,
0.0725074879130797));
#62734=CARTESIAN_POINT('Ctrl Pts',(0.00798657180708102,-0.0239902267563529,
0.0723884532858218));
#62735=CARTESIAN_POINT('Ctrl Pts',(0.00757632762613652,-0.024052726756353,
0.0724715637712821));
#62736=CARTESIAN_POINT('Ctrl Pts',(0.00690309252231404,-0.0241777267563532,
0.072874550507322));
#62737=CARTESIAN_POINT('Ctrl Pts',(0.00664212500943859,-0.0242402267563532,
0.0731924849311315));
#62738=CARTESIAN_POINT('Ctrl Pts',(0.0063750594365665,-0.0243652267563532,
0.0739173804787947));
#62739=CARTESIAN_POINT('Ctrl Pts',(0.00636930012279967,-0.0244277267563531,
0.0743217676246966));
#62740=CARTESIAN_POINT('Ctrl Pts',(0.00660515783189783,-0.0245527267563532,
0.0750452605795038));
#62741=CARTESIAN_POINT('Ctrl Pts',(0.00684554854675824,-0.0246152267563531,
0.0753622929535182));
#62742=CARTESIAN_POINT('Ctrl Pts',(0.00746558059732679,-0.0247402267563532,
0.0757841071331952));
#62743=CARTESIAN_POINT('Ctrl Pts',(0.00784314287652831,-0.0248027267563532,
0.0758880550076066));
#62744=CARTESIAN_POINT('Ctrl Pts',(0.00858148810648805,-0.0249277267563531,
0.0758500290985359));
#62745=CARTESIAN_POINT('Ctrl Pts',(0.00894025630103604,-0.0249902267563527,
0.0757086009273785));
#62746=CARTESIAN_POINT('Ctrl Pts',(0.00950203909667648,-0.0251152267563537,
0.0752437434484126));
#62747=CARTESIAN_POINT('Ctrl Pts',(0.00970384456953965,-0.0251777267563533,
0.0749218424545307));
#62748=CARTESIAN_POINT('Ctrl Pts',(0.00988070810244839,-0.025302726756353,
0.0742244932242857));
#62749=CARTESIAN_POINT('Ctrl Pts',(0.00985569168215658,-0.0253652267563531,
0.0738508662355836));
#62750=CARTESIAN_POINT('Ctrl Pts',(0.0095959880776607,-0.0254902267563532,
0.0731899993104086));
#62751=CARTESIAN_POINT('Ctrl Pts',(0.00936223593079611,-0.0255527267563535,
0.0729041885567222));
#62752=CARTESIAN_POINT('Ctrl Pts',(0.00877642221279626,-0.0256777267563528,
0.0725190877336685));
#62753=CARTESIAN_POINT('Ctrl Pts',(0.00842584970124339,-0.0257402267563532,
0.0724203909003668));
#62754=CARTESIAN_POINT('Ctrl Pts',(0.00773369265389813,-0.0258652267563531,
0.0724380938777203));
#62755=CARTESIAN_POINT('Ctrl Pts',(0.00739357664562364,-0.0259277267563522,
0.0725541566784855));
#62756=CARTESIAN_POINT('Ctrl Pts',(0.00683896472182591,-0.0260527267563541,
0.0729545251500316));
#62757=CARTESIAN_POINT('Ctrl Pts',(0.0066254338254687,-0.0261152267563532,
0.0732377897768127));
#62758=CARTESIAN_POINT('Ctrl Pts',(0.00631271756058805,-0.0262825025052516,
0.0740865949098408));
#62759=CARTESIAN_POINT('Ctrl Pts',(0.00640039734097116,-0.0263872782541498,
0.0747218803033809));
#62760=CARTESIAN_POINT('Ctrl Pts',(0.00709490085666943,-0.0265968297519482,
0.0756461636342162));
#62761=CARTESIAN_POINT('Ctrl Pts',(0.00769343808297591,-0.0267016055008472,
0.0759180937465821));
#62762=CARTESIAN_POINT('Ctrl Pts',(0.00886901117946571,-0.0269111569986424,
0.0758101160508686));
#62763=CARTESIAN_POINT('Ctrl Pts',(0.00942514191765672,-0.0270159327475413,
0.0754280191232956));
#62764=CARTESIAN_POINT('Ctrl Pts',(0.00993824128909218,-0.0272254842453399,
0.0743360327809175));
#62765=CARTESIAN_POINT('Ctrl Pts',(0.00988126005128462,-0.027330259994239,
0.0736449189018586));
#62766=CARTESIAN_POINT('Ctrl Pts',(0.00915994760067147,-0.0275398114920338,
0.072643282846725));
#62767=CARTESIAN_POINT('Ctrl Pts',(0.00850628922460295,-0.0276445872409343,
0.0723566377558719));
#62768=CARTESIAN_POINT('Ctrl Pts',(0.00725482714933299,-0.0278541387387302,
0.0725352625930086));
#62769=CARTESIAN_POINT('Ctrl Pts',(0.00668635569621314,-0.0279589144876299,
0.0730024790825113));
#62770=CARTESIAN_POINT('Ctrl Pts',(0.00638644666034619,-0.028116078110977,
0.0739272381640707));
#62771=CARTESIAN_POINT('Ctrl Pts',(0.00637529306500116,-0.0281684659854268,
0.0742662497426962));
#62772=CARTESIAN_POINT('Ctrl Pts',(0.00654082707084289,-0.028273241734325,
0.0749016523873107));
#62773=CARTESIAN_POINT('Ctrl Pts',(0.00671748214010876,-0.028325629608775,
0.0751968854746209));
#62774=CARTESIAN_POINT('Ctrl Pts',(0.00720892541253046,-0.0284304053576727,
0.0756455554498743));
#62775=CARTESIAN_POINT('Ctrl Pts',(0.00752301334852511,-0.0284827932321226,
0.0757979712806186));
#62776=CARTESIAN_POINT('Ctrl Pts',(0.00818946636282185,-0.0285875689810209,
0.0759028314615779));
#62777=CARTESIAN_POINT('Ctrl Pts',(0.00854060471889044,-0.0286399568554705,
0.0758547732201633));
#62778=CARTESIAN_POINT('Ctrl Pts',(0.00916084100231525,-0.0287447326043687,
0.075565804284784));
#62779=CARTESIAN_POINT('Ctrl Pts',(0.00942854510439027,-0.0287971204788187,
0.0753251761690674));
#62780=CARTESIAN_POINT('Ctrl Pts',(0.00978202913180507,-0.0289018962277164,
0.0747276351526504));
#62781=CARTESIAN_POINT('Ctrl Pts',(0.00986674097407697,-0.0289542841021654,
0.074371816070194));
#62782=CARTESIAN_POINT('Ctrl Pts',(0.00981369952675195,-0.0290590598510655,
0.0736690768431837));
#62783=CARTESIAN_POINT('Ctrl Pts',(0.00967567176060491,-0.0291114477255137,
0.0733237806283977));
#62784=CARTESIAN_POINT('Ctrl Pts',(0.00921778920325428,-0.0292162234744131,
0.0727737193827185));
#62785=CARTESIAN_POINT('Ctrl Pts',(0.00889870439220733,-0.0292686113488629,
0.0725705573281537));
#62786=CARTESIAN_POINT('Ctrl Pts',(0.00819375840446231,-0.0293733870977596,
0.0723920901917167));
#62787=CARTESIAN_POINT('Ctrl Pts',(0.00780958811776,-0.0294257749722108,
0.0724177047880981));
#62788=CARTESIAN_POINT('Ctrl Pts',(0.00712611907880853,-0.0295305507211076,
0.0726994025629769));
#62789=CARTESIAN_POINT('Ctrl Pts',(0.00682888960963579,-0.0295829385955566,
0.0729552009393765));
#62790=CARTESIAN_POINT('Ctrl Pts',(0.0064486506135478,-0.0296877143444575,
0.07360389947374));
#62791=CARTESIAN_POINT('Ctrl Pts',(0.00636725335643387,-0.0297401022189059,
0.0739951973945462));
#62792=CARTESIAN_POINT('Ctrl Pts',(0.00646709367460444,-0.029844877967804,
0.0747539375372065));
#62793=CARTESIAN_POINT('Ctrl Pts',(0.00664865749162809,-0.0298972658422544,
0.0751189204946994));
#62794=CARTESIAN_POINT('Ctrl Pts',(0.00720980796629447,-0.0300020415911513,
0.0756597850568809));
#62795=CARTESIAN_POINT('Ctrl Pts',(0.00758800635949914,-0.0300544294656007,
0.0758333320231676));
#62796=CARTESIAN_POINT('Ctrl Pts',(0.00837965301868817,-0.0301592052145009,
0.0758979109130133));
#62797=CARTESIAN_POINT('Ctrl Pts',(0.0087903017783351,-0.0302115930889491,
0.0757879095122608));
#62798=CARTESIAN_POINT('Ctrl Pts',(0.00945074030194221,-0.0303163688378483,
0.0753188362161399));
#62799=CARTESIAN_POINT('Ctrl Pts',(0.00969742813547587,-0.0303687567122968,
0.074960862384052));
#62800=CARTESIAN_POINT('Ctrl Pts',(0.00989403626134592,-0.0304735324611964,
0.0741577386296832));
#62801=CARTESIAN_POINT('Ctrl Pts',(0.00984213741241968,-0.0305259203356456,
0.0737157448994683));
#62802=CARTESIAN_POINT('Ctrl Pts',(0.00944598585501893,-0.0306306960845434,
0.0729697035868178));
#62803=CARTESIAN_POINT('Ctrl Pts',(0.0091025362089969,-0.0306830839589921,
0.0726696260665349));
#62804=CARTESIAN_POINT('Ctrl Pts',(0.00828774270205792,-0.0307878597078928,
0.0723829167104463));
#62805=CARTESIAN_POINT('Ctrl Pts',(0.00782004690692066,-0.0308402475823424,
0.0723989617927675));
#62806=CARTESIAN_POINT('Ctrl Pts',(0.00701384657225643,-0.0309450233312383,
0.0727620400442508));
#62807=CARTESIAN_POINT('Ctrl Pts',(0.00668038516697007,-0.0309974112056886,
0.0731084553765258));
#62808=CARTESIAN_POINT('Ctrl Pts',(0.00635465831522934,-0.0311021869545879,
0.0739540130716083));
#62809=CARTESIAN_POINT('Ctrl Pts',(0.00636598244243914,-0.0311545748290377,
0.0744486796189194));
#62810=CARTESIAN_POINT('Ctrl Pts',(0.00671098369860905,-0.0312474112056882,
0.0751967969613253));
#62811=CARTESIAN_POINT('Ctrl Pts',(0.00696811726850124,-0.0312878597078925,
0.0754772937988554));
#62812=CARTESIAN_POINT('Ctrl Pts',(0.00760906327807618,-0.0313687567122965,
0.0758329541525405));
#62813=CARTESIAN_POINT('Ctrl Pts',(0.00799152536675427,-0.0314092052144999,
0.0759066312254608));
#62814=CARTESIAN_POINT('Ctrl Pts',(0.00873342443754237,-0.0314901022189058,
0.0758027496660232));
#62815=CARTESIAN_POINT('Ctrl Pts',(0.00909066570959304,-0.0315305507211086,
0.0756247584725279));
#62816=CARTESIAN_POINT('Ctrl Pts',(0.00962495708239995,-0.0316114477255139,
0.0750753379018474));
#62817=CARTESIAN_POINT('Ctrl Pts',(0.00979975975119023,-0.0316518962277159,
0.0747050174935392));
#62818=CARTESIAN_POINT('Ctrl Pts',(0.00986603384010217,-0.0317234272443419,
0.0740141973629227));
#62819=CARTESIAN_POINT('Ctrl Pts',(0.00981302274622929,-0.0317545097587632,
0.0737035212777265));
#62820=CARTESIAN_POINT('Ctrl Pts',(0.00968430513999177,-0.0317855922731845,
0.0734247205810942));
#62821=CARTESIAN_POINT('Ctrl Pts',(0.00814801668780212,-0.0203072579114564,
0.07605678506462));
#62822=CARTESIAN_POINT('Ctrl Pts',(0.00835212411518636,-0.0203255606965017,
0.076056125656151));
#62823=CARTESIAN_POINT('Ctrl Pts',(0.00855476749622787,-0.0203438634815471,
0.0760235656396361));
#62824=CARTESIAN_POINT('Ctrl Pts',(0.00939708426598712,-0.0204246662665928,
0.0757338805617789));
#62825=CARTESIAN_POINT('Ctrl Pts',(0.00988702802146066,-0.0204871662665918,
0.0751430794075642));
#62826=CARTESIAN_POINT('Ctrl Pts',(0.0101232087195095,-0.0206121662665931,
0.0738376922384734));
#62827=CARTESIAN_POINT('Ctrl Pts',(0.00987324480820894,-0.020674666266593,
0.073147689549446));
#62828=CARTESIAN_POINT('Ctrl Pts',(0.0089167610235679,-0.0207996662665919,
0.0722962388864693));
#62829=CARTESIAN_POINT('Ctrl Pts',(0.00822945225385138,-0.0208621662665925,
0.0721430341238275));
#62830=CARTESIAN_POINT('Ctrl Pts',(0.00703231984039108,-0.0209871662665924,
0.0724624609241718));
#62831=CARTESIAN_POINT('Ctrl Pts',(0.00653742293657822,-0.0210496662665924,
0.0729254531013723));
#62832=CARTESIAN_POINT('Ctrl Pts',(0.00612213906812888,-0.0211746662665925,
0.0740526572687589));
#62833=CARTESIAN_POINT('Ctrl Pts',(0.0062024986305861,-0.0212371662665924,
0.0747016337122979));
#62834=CARTESIAN_POINT('Ctrl Pts',(0.00683777690670826,-0.0213621662665925,
0.0756803008502788));
#62835=CARTESIAN_POINT('Ctrl Pts',(0.00738258273676963,-0.0214246662665922,
0.0760014915719832));
#62836=CARTESIAN_POINT('Ctrl Pts',(0.00851285299155973,-0.0215496662665927,
0.0761060218805955));
#62837=CARTESIAN_POINT('Ctrl Pts',(0.00908700825207452,-0.0216121662665926,
0.0758916126988471));
#62838=CARTESIAN_POINT('Ctrl Pts',(0.009867934505352,-0.0217371662665924,
0.0751086198167669));
#62839=CARTESIAN_POINT('Ctrl Pts',(0.0100698264375556,-0.0217996662665926,
0.0745489205445409));
#62840=CARTESIAN_POINT('Ctrl Pts',(0.00999137500636933,-0.0219246662665924,
0.0734730045098974));
#62841=CARTESIAN_POINT('Ctrl Pts',(0.00971409165292503,-0.0219871662665922,
0.0729652157409598));
#62842=CARTESIAN_POINT('Ctrl Pts',(0.00888282738880219,-0.0221121662665928,
0.0723178841967402));
#62843=CARTESIAN_POINT('Ctrl Pts',(0.00833621828939995,-0.022174666266592,
0.0721813898931065));
#62844=CARTESIAN_POINT('Ctrl Pts',(0.00731858981585824,-0.0222996662665929,
0.0723410721157334));
#62845=CARTESIAN_POINT('Ctrl Pts',(0.00685408613370773,-0.0223621662665927,
0.0726343422814147));
#62846=CARTESIAN_POINT('Ctrl Pts',(0.00627188449978499,-0.0224871662665922,
0.0734573086233949));
#62847=CARTESIAN_POINT('Ctrl Pts',(0.00615642736772064,-0.0225496662665926,
0.07398099780415));
#62848=CARTESIAN_POINT('Ctrl Pts',(0.00632058686144516,-0.0226746662665923,
0.0749546945714818));
#62849=CARTESIAN_POINT('Ctrl Pts',(0.00659784007307093,-0.0227371662665921,
0.0753994199917464));
#62850=CARTESIAN_POINT('Ctrl Pts',(0.007376147995406,-0.0228621662665928,
0.075974991173125));
#62851=CARTESIAN_POINT('Ctrl Pts',(0.00787234780121979,-0.0229246662665925,
0.0761038540413805));
#62852=CARTESIAN_POINT('Ctrl Pts',(0.00881571254739481,-0.0230496662665924,
0.0759944503948627));
#62853=CARTESIAN_POINT('Ctrl Pts',(0.00925841300542465,-0.0231121662665924,
0.0757578644326881));
#62854=CARTESIAN_POINT('Ctrl Pts',(0.0098711682512917,-0.0232371662665925,
0.0750551282138252));
#62855=CARTESIAN_POINT('Ctrl Pts',(0.0100392249004471,-0.0232996662665926,
0.0745928466798487));
#62856=CARTESIAN_POINT('Ctrl Pts',(0.0100319815915929,-0.0234246662665924,
0.0736769154324963));
#62857=CARTESIAN_POINT('Ctrl Pts',(0.0098576459212449,-0.0234871662665927,
0.0732271346566689));
#62858=CARTESIAN_POINT('Ctrl Pts',(0.00926368508465529,-0.0236121662665922,
0.0725504421633576));
#62859=CARTESIAN_POINT('Ctrl Pts',(0.00884704504328137,-0.0236746662665927,
0.0723256519701696));
#62860=CARTESIAN_POINT('Ctrl Pts',(0.00797138179410088,-0.0237996662665922,
0.07219343949548));
#62861=CARTESIAN_POINT('Ctrl Pts',(0.00751572112090685,-0.0238621662665923,
0.0722857508103344));
#62862=CARTESIAN_POINT('Ctrl Pts',(0.00676795485175628,-0.0239871662665926,
0.0727333505959289));
#62863=CARTESIAN_POINT('Ctrl Pts',(0.00647809666942974,-0.0240496662665925,
0.073086482268025));
#62864=CARTESIAN_POINT('Ctrl Pts',(0.00618146533527733,-0.0241746662665925,
0.0738916281021063));
#62865=CARTESIAN_POINT('Ctrl Pts',(0.00617506843092123,-0.0242371662665925,
0.0743407833313369));
#62866=CARTESIAN_POINT('Ctrl Pts',(0.00643703700353636,-0.0243621662665925,
0.0751443712971177));
#62867=CARTESIAN_POINT('Ctrl Pts',(0.00670404041284908,-0.0244246662665925,
0.0754965010570941));
#62868=CARTESIAN_POINT('Ctrl Pts',(0.00739271373153814,-0.0245496662665925,
0.0759650125972991));
#62869=CARTESIAN_POINT('Ctrl Pts',(0.00781207442037852,-0.0246121662665926,
0.0760804681250833));
#62870=CARTESIAN_POINT('Ctrl Pts',(0.00863215889728322,-0.0247371662665924,
0.0760382325197273));
#62871=CARTESIAN_POINT('Ctrl Pts',(0.0090306448835366,-0.024799666266592,
0.0758811474014697));
#62872=CARTESIAN_POINT('Ctrl Pts',(0.0096546204052879,-0.024924666266593,
0.0753648274104897));
#62873=CARTESIAN_POINT('Ctrl Pts',(0.00987876695480732,-0.0249871662665926,
0.0750072900452153));
#62874=CARTESIAN_POINT('Ctrl Pts',(0.0100752103419703,-0.0251121662665924,
0.0742327400711651));
#62875=CARTESIAN_POINT('Ctrl Pts',(0.0100474244538565,-0.0251746662665924,
0.0738177503330937));
#62876=CARTESIAN_POINT('Ctrl Pts',(0.00975897010215047,-0.0252996662665926,
0.0730837214741746));
#62877=CARTESIAN_POINT('Ctrl Pts',(0.00949934019014137,-0.0253621662665928,
0.0727662697552228));
#62878=CARTESIAN_POINT('Ctrl Pts',(0.00884867337874248,-0.0254871662665921,
0.0723385359604954));
#62879=CARTESIAN_POINT('Ctrl Pts',(0.00845929038676506,-0.0255496662665926,
0.0722289127955772));
#62880=CARTESIAN_POINT('Ctrl Pts',(0.00769050740141413,-0.0256746662665924,
0.0722485755987396));
#62881=CARTESIAN_POINT('Ctrl Pts',(0.0073127385103659,-0.0257371662665915,
0.0723774872479133));
#62882=CARTESIAN_POINT('Ctrl Pts',(0.00669672771899448,-0.0258621662665935,
0.0728221789114253));
#62883=CARTESIAN_POINT('Ctrl Pts',(0.00645955767124918,-0.0259246662665926,
0.0731368026319471));
#62884=CARTESIAN_POINT('Ctrl Pts',(0.00611222183958379,-0.0260919420154909,
0.0740795755859367));
#62885=CARTESIAN_POINT('Ctrl Pts',(0.00620960829772417,-0.0261967177643892,
0.0747851908841829));
#62886=CARTESIAN_POINT('Ctrl Pts',(0.00698099751955323,-0.0264062692621874,
0.0758117979253375));
#62887=CARTESIAN_POINT('Ctrl Pts',(0.00764579640796796,-0.0265110450110865,
0.0761138323326925));
#62888=CARTESIAN_POINT('Ctrl Pts',(0.00895151249954563,-0.0267205965088817,
0.0759939008582095));
#62889=CARTESIAN_POINT('Ctrl Pts',(0.00956921024717631,-0.0268253722577806,
0.0755695035082156));
#62890=CARTESIAN_POINT('Ctrl Pts',(0.0101391127975682,-0.0270349237555792,
0.0743566277259409));
#62891=CARTESIAN_POINT('Ctrl Pts',(0.0100758233948543,-0.0271396995044774,
0.0735890033938645));
#62892=CARTESIAN_POINT('Ctrl Pts',(0.00927465732816471,-0.0273492510022741,
0.0724764802177239));
#62893=CARTESIAN_POINT('Ctrl Pts',(0.00854863504798854,-0.0274540267511745,
0.0721581017954751));
#62894=CARTESIAN_POINT('Ctrl Pts',(0.0071586286123545,-0.0276635782489686,
0.0723565014738116));
#62895=CARTESIAN_POINT('Ctrl Pts',(0.00652722395860935,-0.0277683539978693,
0.0728754416319487));
#62896=CARTESIAN_POINT('Ctrl Pts',(0.0061941131930515,-0.0279255176212164,
0.0739025770922874));
#62897=CARTESIAN_POINT('Ctrl Pts',(0.00618172482778142,-0.0279779054956661,
0.0742791192866981));
#62898=CARTESIAN_POINT('Ctrl Pts',(0.00636558444125528,-0.0280826812445643,
0.0749848648164158));
#62899=CARTESIAN_POINT('Ctrl Pts',(0.00656179628659944,-0.0281350691190143,
0.0753127819778567));
#62900=CARTESIAN_POINT('Ctrl Pts',(0.0071076452778826,-0.028239844867912,
0.0758111224113399));
#62901=CARTESIAN_POINT('Ctrl Pts',(0.00745650463288417,-0.0282922327423619,
0.0759804115890255));
#62902=CARTESIAN_POINT('Ctrl Pts',(0.00819673799450679,-0.0283970084912602,
0.0760968804211664));
#62903=CARTESIAN_POINT('Ctrl Pts',(0.00858674947338286,-0.0284493963657099,
0.0760435018440831));
#62904=CARTESIAN_POINT('Ctrl Pts',(0.00927564963473071,-0.0285541721146081,
0.0757225423137761));
#62905=CARTESIAN_POINT('Ctrl Pts',(0.00957299018710003,-0.028606559989058,
0.0754552752219081));
#62906=CARTESIAN_POINT('Ctrl Pts',(0.00996560701721403,-0.0287113357379557,
0.0747915828297948));
#62907=CARTESIAN_POINT('Ctrl Pts',(0.010059696968687,-0.0287637236124047,
0.074396372440036));
#62908=CARTESIAN_POINT('Ctrl Pts',(0.0100007835149004,-0.0288684993613048,
0.0736158357642392));
#62909=CARTESIAN_POINT('Ctrl Pts',(0.00984747524688978,-0.0289208872357529,
0.073232313186738));
#62910=CARTESIAN_POINT('Ctrl Pts',(0.00933890234319653,-0.0290256629846524,
0.0726213568608565));
#62911=CARTESIAN_POINT('Ctrl Pts',(0.00898449292909369,-0.0290780508591023,
0.0723957035479018));
#62912=CARTESIAN_POINT('Ctrl Pts',(0.00820150519090858,-0.0291828266079989,
0.0721974790286785));
#62913=CARTESIAN_POINT('Ctrl Pts',(0.00777480494848981,-0.0292352144824501,
0.072225929314564));
#62914=CARTESIAN_POINT('Ctrl Pts',(0.00701567178618897,-0.0293399902313469,
0.0725388127232768));
#62915=CARTESIAN_POINT('Ctrl Pts',(0.00668553723143537,-0.029392378105796,
0.0728229295147053));
#62916=CARTESIAN_POINT('Ctrl Pts',(0.00626320349708927,-0.0294971538546968,
0.0735434428689412));
#62917=CARTESIAN_POINT('Ctrl Pts',(0.00617279507523841,-0.0295495417291453,
0.0739780598173242));
#62918=CARTESIAN_POINT('Ctrl Pts',(0.00628368831566111,-0.0296543174780434,
0.0748207970461326));
#62919=CARTESIAN_POINT('Ctrl Pts',(0.00648535233659179,-0.0297067053524937,
0.0752261858068767));
#62920=CARTESIAN_POINT('Ctrl Pts',(0.00710862553564354,-0.0298114811013907,
0.0758269273212183));
#62921=CARTESIAN_POINT('Ctrl Pts',(0.00752869276012381,-0.02986386897584,
0.0760196869779353));
#62922=CARTESIAN_POINT('Ctrl Pts',(0.00840797945427604,-0.0299686447247403,
0.076091415138353));
#62923=CARTESIAN_POINT('Ctrl Pts',(0.00886408949546226,-0.0300210325991884,
0.075969235922541));
#62924=CARTESIAN_POINT('Ctrl Pts',(0.00959764252618967,-0.0301258083480876,
0.0754482333981525));
#62925=CARTESIAN_POINT('Ctrl Pts',(0.00987164018299474,-0.0301781962225362,
0.0750506297150497));
#62926=CARTESIAN_POINT('Ctrl Pts',(0.0100900140080253,-0.0302829719714357,
0.07415859534242));
#62927=CARTESIAN_POINT('Ctrl Pts',(0.0100323696451357,-0.0303353598458849,
0.0736676702543576));
#62928=CARTESIAN_POINT('Ctrl Pts',(0.00959236173346572,-0.0304401355947827,
0.0728390376922328));
#62929=CARTESIAN_POINT('Ctrl Pts',(0.00921089015096985,-0.0304925234692313,
0.0725057397900231));
#62930=CARTESIAN_POINT('Ctrl Pts',(0.00830589411414326,-0.0305972992181321,
0.0721872899879916));
#62931=CARTESIAN_POINT('Ctrl Pts',(0.00778642158836204,-0.0306496870925817,
0.0722051113571944));
#62932=CARTESIAN_POINT('Ctrl Pts',(0.00689097003953919,-0.0307544628414776,
0.0726083845495457));
#62933=CARTESIAN_POINT('Ctrl Pts',(0.00652059245595663,-0.0308068507159279,
0.0729931501375565));
#62934=CARTESIAN_POINT('Ctrl Pts',(0.00615880568740368,-0.0309116264648272,
0.0739323161427358));
#62935=CARTESIAN_POINT('Ctrl Pts',(0.00617138346343902,-0.030964014339277,
0.0744817452447779));
#62936=CARTESIAN_POINT('Ctrl Pts',(0.00655457842863585,-0.0310568507159276,
0.0753126836656081));
#62937=CARTESIAN_POINT('Ctrl Pts',(0.00684017822748756,-0.0310972992181319,
0.0756242331860024));
#62938=CARTESIAN_POINT('Ctrl Pts',(0.00755208080592647,-0.0311781962225358,
0.0760192672747625));
#62939=CARTESIAN_POINT('Ctrl Pts',(0.0079768837425508,-0.0312186447247393,
0.0761011008417093));
#62940=CARTESIAN_POINT('Ctrl Pts',(0.00880091549178614,-0.0312995417291452,
0.0759857189703642));
#62941=CARTESIAN_POINT('Ctrl Pts',(0.00919770551606028,-0.031339990231348,
0.0757880230838218));
#62942=CARTESIAN_POINT('Ctrl Pts',(0.00979114614952519,-0.0314208872357532,
0.0751777783595053));
#62943=CARTESIAN_POINT('Ctrl Pts',(0.00998530052254685,-0.0314613357379553,
0.0747664612601165));
#62944=CARTESIAN_POINT('Ctrl Pts',(0.0100589115507385,-0.0315328667545812,
0.0739991631961976));
#62945=CARTESIAN_POINT('Ctrl Pts',(0.0100000318107133,-0.0315639492690025,
0.0736540934043486));
#62946=CARTESIAN_POINT('Ctrl Pts',(0.00985706439317406,-0.0315950317834238,
0.0733444277978263));
#62947=CARTESIAN_POINT('Ctrl Pts',(0.00815067148752137,-0.0203072579114564,
0.0762656663521488));
#62948=CARTESIAN_POINT('Ctrl Pts',(0.0083771381325318,-0.0203255606965017,
0.0762649347079084));
#62949=CARTESIAN_POINT('Ctrl Pts',(0.00860198035030984,-0.0203438634815471,
0.0762288078613937));
#62950=CARTESIAN_POINT('Ctrl Pts',(0.00953656982276594,-0.0204246662665928,
0.0759073888491967));
#62951=CARTESIAN_POINT('Ctrl Pts',(0.0100801851138304,-0.0204871662665918,
0.0752518676024789));
#62952=CARTESIAN_POINT('Ctrl Pts',(0.0103422385382883,-0.0206121662665931,
0.0738034800723812));
#62953=CARTESIAN_POINT('Ctrl Pts',(0.0100648920002843,-0.020674666266593,
0.0730378901277388));
#62954=CARTESIAN_POINT('Ctrl Pts',(0.00900362893656076,-0.0207996662665919,
0.0720931661776728));
#62955=CARTESIAN_POINT('Ctrl Pts',(0.008241028020177,-0.0208621662665925,
0.0719231783970233));
#62956=CARTESIAN_POINT('Ctrl Pts',(0.00691275415584957,-0.0209871662665924,
0.0722775972279668));
#62957=CARTESIAN_POINT('Ctrl Pts',(0.00636364311727103,-0.0210496662665924,
0.0727913084945308));
#62958=CARTESIAN_POINT('Ctrl Pts',(0.00590286642913209,-0.0211746662665925,
0.0740419937307385));
#62959=CARTESIAN_POINT('Ctrl Pts',(0.00599202908596152,-0.0212371662665924,
0.0747620631556615));
#62960=CARTESIAN_POINT('Ctrl Pts',(0.00669689975963152,-0.0213621662665925,
0.0758479396774564));
#62961=CARTESIAN_POINT('Ctrl Pts',(0.00730138706368173,-0.0214246662665922,
0.0762043156608544));
#62962=CARTESIAN_POINT('Ctrl Pts',(0.00855547426588603,-0.0215496662665927,
0.0763202968801402));
#62963=CARTESIAN_POINT('Ctrl Pts',(0.00919252612250013,-0.0216121662665926,
0.0760823999614819));
#62964=CARTESIAN_POINT('Ctrl Pts',(0.0100589999732895,-0.0217371662665924,
0.075213633090309));
#62965=CARTESIAN_POINT('Ctrl Pts',(0.0102830084237745,-0.0217996662665926,
0.0745926208223076));
#62966=CARTESIAN_POINT('Ctrl Pts',(0.0101959629269755,-0.0219246662665924,
0.0733988421450626));
#62967=CARTESIAN_POINT('Ctrl Pts',(0.00988830420246689,-0.0219871662665922,
0.0728354269849725));
#62968=CARTESIAN_POINT('Ctrl Pts',(0.00896597799697031,-0.0221121662665928,
0.0721171826520367));
#62969=CARTESIAN_POINT('Ctrl Pts',(0.00835948988205837,-0.022174666266592,
0.0719657358996911));
#62970=CARTESIAN_POINT('Ctrl Pts',(0.00723038395375605,-0.0222996662665929,
0.0721429107222321));
#62971=CARTESIAN_POINT('Ctrl Pts',(0.00671499560243656,-0.0223621662665927,
0.0724683075554325));
#62972=CARTESIAN_POINT('Ctrl Pts',(0.00606901592181546,-0.0224871662665922,
0.0733814268319492));
#62973=CARTESIAN_POINT('Ctrl Pts',(0.00594091088577522,-0.0225496662665926,
0.0739624842354635));
#62974=CARTESIAN_POINT('Ctrl Pts',(0.00612305344798784,-0.0226746662665923,
0.0750428459007938));
#62975=CARTESIAN_POINT('Ctrl Pts',(0.00643067872875265,-0.0227371662665921,
0.0755362893544149));
#62976=CARTESIAN_POINT('Ctrl Pts',(0.00729424742007936,-0.0228621662665928,
0.0761749122408133));
#62977=CARTESIAN_POINT('Ctrl Pts',(0.00784480408877878,-0.0229246662665925,
0.0763178915621161));
#62978=CARTESIAN_POINT('Ctrl Pts',(0.00889151097164585,-0.0230496662665924,
0.0761965031486893));
#62979=CARTESIAN_POINT('Ctrl Pts',(0.00938270763587042,-0.0231121662665924,
0.0759340000649118));
#62980=CARTESIAN_POINT('Ctrl Pts',(0.0100625879641978,-0.0232371662665925,
0.0751542816790953));
#62981=CARTESIAN_POINT('Ctrl Pts',(0.0102490546008787,-0.0232996662665926,
0.0746413589041057));
#62982=CARTESIAN_POINT('Ctrl Pts',(0.0102410178141923,-0.0234246662665924,
0.0736250907589115));
#62983=CARTESIAN_POINT('Ctrl Pts',(0.0100475843126518,-0.0234871662665927,
0.0731260381541277));
#62984=CARTESIAN_POINT('Ctrl Pts',(0.00938855725198137,-0.0236121662665922,
0.0723752164881653));
#62985=CARTESIAN_POINT('Ctrl Pts',(0.0089262758271642,-0.0236746662665927,
0.0721258013564626));
#62986=CARTESIAN_POINT('Ctrl Pts',(0.00795468689116961,-0.0237996662665922,
0.0719791054916663));
#62987=CARTESIAN_POINT('Ctrl Pts',(0.00744911026789867,-0.0238621662665923,
0.0720815291713897));
#62988=CARTESIAN_POINT('Ctrl Pts',(0.00661942895548025,-0.0239871662665926,
0.0725781618664859));
#62989=CARTESIAN_POINT('Ctrl Pts',(0.00629781787585632,-0.0240496662665925,
0.0729699778138594));
#62990=CARTESIAN_POINT('Ctrl Pts',(0.00596869167054677,-0.0241746662665925,
0.07386332441141));
#62991=CARTESIAN_POINT('Ctrl Pts',(0.00596159400885685,-0.0242371662665925,
0.0743616829432692));
#62992=CARTESIAN_POINT('Ctrl Pts',(0.00625226027464946,-0.0243621662665925,
0.0752533010137793));
#62993=CARTESIAN_POINT('Ctrl Pts',(0.0065485129249735,-0.0244246662665925,
0.0756440052932471));
#62994=CARTESIAN_POINT('Ctrl Pts',(0.00731262787164867,-0.0245496662665925,
0.0761638405487234));
#62995=CARTESIAN_POINT('Ctrl Pts',(0.00777792798085125,-0.0246121662665926,
0.0762919438047406));
#62996=CARTESIAN_POINT('Ctrl Pts',(0.00868784969457759,-0.0247371662665924,
0.07624508144423));
#62997=CARTESIAN_POINT('Ctrl Pts',(0.00912998835433636,-0.024799666266592,
0.0760707882292855));
#62998=CARTESIAN_POINT('Ctrl Pts',(0.00982231809848441,-0.024924666266593,
0.07549790728317));
#62999=CARTESIAN_POINT('Ctrl Pts',(0.010071019077723,-0.0249871662665926,
0.0751012030151419));
#63000=CARTESIAN_POINT('Ctrl Pts',(0.0102889821151069,-0.0251121662665924,
0.0742418039415068));
#63001=CARTESIAN_POINT('Ctrl Pts',(0.0102581523851926,-0.0251746662665924,
0.0737813536046464));
#63002=CARTESIAN_POINT('Ctrl Pts',(0.00993809892066803,-0.0252996662665926,
0.0729669145852015));
#63003=CARTESIAN_POINT('Ctrl Pts',(0.00965002750714532,-0.0253621662665928,
0.0726146871985494));
#63004=CARTESIAN_POINT('Ctrl Pts',(0.00892808254078336,-0.0254871662665921,
0.07214009674052));
#63005=CARTESIAN_POINT('Ctrl Pts',(0.00849604407482765,-0.0255496662665926,
0.0720184647612599));
#63006=CARTESIAN_POINT('Ctrl Pts',(0.00764304374228332,-0.0256746662665924,
0.0720402815521564));
#63007=CARTESIAN_POINT('Ctrl Pts',(0.00722389165927775,-0.0257371662665915,
0.0721833149981475));
#63008=CARTESIAN_POINT('Ctrl Pts',(0.00654039915241529,-0.0258621662665935,
0.0726767209970879));
#63009=CARTESIAN_POINT('Ctrl Pts',(0.00627724799864211,-0.0259246662665926,
0.0730258105884879));
#63010=CARTESIAN_POINT('Ctrl Pts',(0.00589186280469173,-0.0260919420154909,
0.0740718608505132));
#63011=CARTESIAN_POINT('Ctrl Pts',(0.00599991759097347,-0.0261967177643892,
0.0748547737082654));
#63012=CARTESIAN_POINT('Ctrl Pts',(0.00685580966361203,-0.0264062692621874,
0.0759938417732247));
#63013=CARTESIAN_POINT('Ctrl Pts',(0.00759343482402584,-0.0265110450110865,
0.0763289629385248));
#63014=CARTESIAN_POINT('Ctrl Pts',(0.00904218730885863,-0.0267205965088817,
0.0761958934123178));
#63015=CARTESIAN_POINT('Ctrl Pts',(0.00972755157183108,-0.0268253722577806,
0.0757250048942655));
#63016=CARTESIAN_POINT('Ctrl Pts',(0.010359884849577,-0.0270349237555792,
0.0743792630330001));
#63017=CARTESIAN_POINT('Ctrl Pts',(0.0102896623256786,-0.0271396995044774,
0.0735275482799331));
#63018=CARTESIAN_POINT('Ctrl Pts',(0.00940073146439328,-0.0273492510022741,
0.0722931522835415));
#63019=CARTESIAN_POINT('Ctrl Pts',(0.00859517611493118,-0.0274540267511745,
0.0719398966766563));
#63020=CARTESIAN_POINT('Ctrl Pts',(0.00705289958900958,-0.0276635782489686,
0.0721600303097132));
#63021=CARTESIAN_POINT('Ctrl Pts',(0.00635232687879448,-0.0277683539978693,
0.0727358184526565));
#63022=CARTESIAN_POINT('Ctrl Pts',(0.00598272505460037,-0.0279255176212164,
0.073875472823177));
#63023=CARTESIAN_POINT('Ctrl Pts',(0.00596897958949985,-0.0279779054956661,
0.0742932638294421));
#63024=CARTESIAN_POINT('Ctrl Pts',(0.00617298034709087,-0.0280826812445643,
0.0750763211850444));
#63025=CARTESIAN_POINT('Ctrl Pts',(0.00639068647810172,-0.0281350691190143,
0.075440160464901));
#63026=CARTESIAN_POINT('Ctrl Pts',(0.00699633121784709,-0.028239844867912,
0.0759930922591544));
#63027=CARTESIAN_POINT('Ctrl Pts',(0.00738340683150901,-0.0282922327423619,
0.0761809264433306));
#63028=CARTESIAN_POINT('Ctrl Pts',(0.00820473003409823,-0.0283970084912602,
0.076310154007468));
#63029=CARTESIAN_POINT('Ctrl Pts',(0.00863746583537968,-0.0284493963657099,
0.0762509280036797));
#63030=CARTESIAN_POINT('Ctrl Pts',(0.00940183247449225,-0.0285541721146081,
0.0758948085378461));
#63031=CARTESIAN_POINT('Ctrl Pts',(0.00973174559026465,-0.028606559989058,
0.0755982633195131));
#63032=CARTESIAN_POINT('Ctrl Pts',(0.0101673721494254,-0.0287113357379557,
0.0748618658679991));
#63033=CARTESIAN_POINT('Ctrl Pts',(0.0102717693088642,-0.0287637236124047,
0.0744233616342778));
#63034=CARTESIAN_POINT('Ctrl Pts',(0.0102064021029961,-0.0288684993613048,
0.0735573200377487));
#63035=CARTESIAN_POINT('Ctrl Pts',(0.0100362994783456,-0.0289208872357529,
0.0731317839731108));
#63036=CARTESIAN_POINT('Ctrl Pts',(0.00947201428442268,-0.0290256629846524,
0.072453899629834));
#63037=CARTESIAN_POINT('Ctrl Pts',(0.00907878062310723,-0.0290780508591023,
0.0722035268267701));
#63038=CARTESIAN_POINT('Ctrl Pts',(0.00821001945932422,-0.0291828266079989,
0.0719835875408627));
#63039=CARTESIAN_POINT('Ctrl Pts',(0.00773657577545569,-0.0292352144824501,
0.0720151544508798));
#63040=CARTESIAN_POINT('Ctrl Pts',(0.00689428236856863,-0.0293399902313469,
0.0723623130857159));
#63041=CARTESIAN_POINT('Ctrl Pts',(0.00652798278812114,-0.029392378105796,
0.0726775538261953));
#63042=CARTESIAN_POINT('Ctrl Pts',(0.00605938394721744,-0.0294971538546968,
0.0734769967671513));
#63043=CARTESIAN_POINT('Ctrl Pts',(0.00595907161542407,-0.0295495417291453,
0.0739592244029917));
#63044=CARTESIAN_POINT('Ctrl Pts',(0.00608211280228693,-0.0296543174780434,
0.0748942803942386));
#63045=CARTESIAN_POINT('Ctrl Pts',(0.00630586837465766,-0.0297067053524937,
0.0753440780020337));
#63046=CARTESIAN_POINT('Ctrl Pts',(0.00699741885923872,-0.0298114811013907,
0.0760106285387534));
#63047=CARTESIAN_POINT('Ctrl Pts',(0.00746350290246076,-0.02986386897584,
0.0762245043065757));
#63048=CARTESIAN_POINT('Ctrl Pts',(0.00843911221849071,-0.0299686447247403,
0.0763040900230327));
#63049=CARTESIAN_POINT('Ctrl Pts',(0.0089451874363639,-0.0300210325991884,
0.0761685265237053));
#63050=CARTESIAN_POINT('Ctrl Pts',(0.00975909850238958,-0.0301258083480876,
0.0755904500898765));
#63051=CARTESIAN_POINT('Ctrl Pts',(0.0100631115942824,-0.0301781962225362,
0.0751492903863319));
#63052=CARTESIAN_POINT('Ctrl Pts',(0.0103054074683059,-0.0302829719714357,
0.0741595369305542));
#63053=CARTESIAN_POINT('Ctrl Pts',(0.0102414483775728,-0.0303353598458849,
0.0736148328055268));
#63054=CARTESIAN_POINT('Ctrl Pts',(0.00975323921825422,-0.0304401355947827,
0.0726954265952984));
#63055=CARTESIAN_POINT('Ctrl Pts',(0.00932997882757754,-0.0304925234692313,
0.0723256171343211));
#63056=CARTESIAN_POINT('Ctrl Pts',(0.00832584380498464,-0.0305972992181321,
0.0719722823282605));
#63057=CARTESIAN_POINT('Ctrl Pts',(0.0077494649754808,-0.0306496870925817,
0.0719920559628832));
#63058=CARTESIAN_POINT('Ctrl Pts',(0.00675592000443203,-0.0307544628414776,
0.0724395062495526));
#63059=CARTESIAN_POINT('Ctrl Pts',(0.00634496891942769,-0.0308068507159279,
0.0728664214919276));
#63060=CARTESIAN_POINT('Ctrl Pts',(0.00594354974162806,-0.0309116264648272,
0.0739084696771727));
#63061=CARTESIAN_POINT('Ctrl Pts',(0.00595750536674637,-0.030964014339277,
0.0745180867156372));
#63062=CARTESIAN_POINT('Ctrl Pts',(0.00638267793035737,-0.0310568507159276,
0.0754400513829074));
#63063=CARTESIAN_POINT('Ctrl Pts',(0.00669956413626623,-0.0310972992181319,
0.0757857300068678));
#63064=CARTESIAN_POINT('Ctrl Pts',(0.00748945302262128,-0.0311781962225358,
0.0762240386264647));
#63065=CARTESIAN_POINT('Ctrl Pts',(0.00796079155782699,-0.0312186447247393,
0.0763148367595518));
#63066=CARTESIAN_POINT('Ctrl Pts',(0.00887509295304323,-0.0312995417291452,
0.0761868152287656));
#63067=CARTESIAN_POINT('Ctrl Pts',(0.00931534986442847,-0.031339990231348,
0.075967462485304));
#63068=CARTESIAN_POINT('Ctrl Pts',(0.00997379973563606,-0.0314208872357532,
0.0752903676969252));
#63069=CARTESIAN_POINT('Ctrl Pts',(0.0101892230058022,-0.0314613357379553,
0.0748339923228011));
#63070=CARTESIAN_POINT('Ctrl Pts',(0.0102708978512695,-0.0315328667545812,
0.0739826395793677));
#63071=CARTESIAN_POINT('Ctrl Pts',(0.0102055680523813,-0.0315639492690025,
0.0735997686615574));
#63072=CARTESIAN_POINT('Ctrl Pts',(0.0100469390803206,-0.0315950317834238,
0.0732561803273014));
#63073=CARTESIAN_POINT('',(0.0102415292846688,-0.0315281082229192,0.0740373581220502));
#63074=CARTESIAN_POINT('Ctrl Pts',(0.0102415292846687,-0.0315281082229192,
0.0740373581220493));
#63075=CARTESIAN_POINT('Ctrl Pts',(0.0102443061585269,-0.0315281082229192,
0.0740372104215577));
#63076=CARTESIAN_POINT('Ctrl Pts',(0.0102470791223289,-0.0315281082229192,
0.0740374674812331));
#63077=CARTESIAN_POINT('Ctrl Pts',(0.0102549222898814,-0.0315281082229192,
0.0740392868388633));
#63078=CARTESIAN_POINT('Ctrl Pts',(0.0102596737838761,-0.0315281082229192,
0.0740416912990496));
#63079=CARTESIAN_POINT('Ctrl Pts',(0.0102714431960483,-0.0315281082229192,
0.0740498637422819));
#63080=CARTESIAN_POINT('Ctrl Pts',(0.0102781083576007,-0.0315281082229192,
0.0740571642570058));
#63081=CARTESIAN_POINT('Ctrl Pts',(0.01029611995105,-0.0315281082229192,
0.0740808578266151));
#63082=CARTESIAN_POINT('Ctrl Pts',(0.0103082953978233,-0.0315281082229192,
0.0741042852756716));
#63083=CARTESIAN_POINT('Ctrl Pts',(0.0103375938004529,-0.0315281082229192,
0.0741803459859531));
#63084=CARTESIAN_POINT('Ctrl Pts',(0.0103535661419107,-0.0315281082229192,
0.0742431662099169));
#63085=CARTESIAN_POINT('Ctrl Pts',(0.0103867339291107,-0.0315281082229192,
0.0744813090868569));
#63086=CARTESIAN_POINT('Ctrl Pts',(0.0103828904157489,-0.0315281082229192,
0.074698144384189));
#63087=CARTESIAN_POINT('Ctrl Pts',(0.0102634625434987,-0.0315281082229192,
0.075190809856021));
#63088=CARTESIAN_POINT('Ctrl Pts',(0.0101565404905841,-0.0315281082229192,
0.0754290476681851));
#63089=CARTESIAN_POINT('Ctrl Pts',(0.0098125654375786,-0.0315281082229192,
0.0759373966430771));
#63090=CARTESIAN_POINT('Ctrl Pts',(0.00958025235175371,-0.0315281082229192,
0.0761276005840903));
#63091=CARTESIAN_POINT('Ctrl Pts',(0.00916609298882152,-0.0315281082229192,
0.0764086558067814));
#63092=CARTESIAN_POINT('Ctrl Pts',(0.00889372820965532,-0.0315281082229192,
0.0765284368321801));
#63093=CARTESIAN_POINT('Ctrl Pts',(0.00822455503474282,-0.0315281082229192,
0.0766836549896214));
#63094=CARTESIAN_POINT('Ctrl Pts',(0.00789635708856245,-0.0315281082229192,
0.0766587650478001));
#63095=CARTESIAN_POINT('Ctrl Pts',(0.00745899885480862,-0.0315281082229192,
0.0765870776260973));
#63096=CARTESIAN_POINT('Ctrl Pts',(0.0071495560914034,-0.0315281082229192,
0.0765064246987785));
#63097=CARTESIAN_POINT('Ctrl Pts',(0.00655000913918567,-0.0315281082229192,
0.0761454330379778));
#63098=CARTESIAN_POINT('Ctrl Pts',(0.00630893772584743,-0.0315281082317243,
0.0759248089475972));
#63099=CARTESIAN_POINT('Ctrl Pts',(0.00611837819382198,-0.0315281082317243,
0.0756651070488126));
#63100=CARTESIAN_POINT('Ctrl Pts',(0.00599688119407085,-0.0315281082317243,
0.0754995262395158));
#63101=CARTESIAN_POINT('Ctrl Pts',(0.00584236692428051,-0.0315281082229192,
0.0752474041328658));
#63102=CARTESIAN_POINT('Ctrl Pts',(0.00567647591673654,-0.0315281082229192,
0.0746524710000351));
#63103=CARTESIAN_POINT('Ctrl Pts',(0.00564801698991816,-0.0315281082229192,
0.0743893561988201));
#63104=CARTESIAN_POINT('Ctrl Pts',(0.00567898251827618,-0.0315281082229192,
0.0738464149833142));
#63105=CARTESIAN_POINT('Ctrl Pts',(0.00574582072759108,-0.0315281082229192,
0.0735505592342265));
#63106=CARTESIAN_POINT('Ctrl Pts',(0.00600663983621015,-0.0315281082229192,
0.0730144137359113));
#63107=CARTESIAN_POINT('Ctrl Pts',(0.00617508989093895,-0.0315281082229192,
0.0727998376780962));
#63108=CARTESIAN_POINT('Ctrl Pts',(0.00651170243980347,-0.0315281082229192,
0.07250050147065));
#63109=CARTESIAN_POINT('Ctrl Pts',(0.00666205465774635,-0.0315281082229192,
0.0724117683127483));
#63110=CARTESIAN_POINT('Ctrl Pts',(0.00683725022531139,-0.0315281082229192,
0.0723411242055322));
#63111=CARTESIAN_POINT('Ctrl Pts',(0.00688753578065855,-0.0315281082229192,
0.0723272897287553));
#63112=CARTESIAN_POINT('Ctrl Pts',(0.00694306395763103,-0.0315281082229192,
0.0723209583585516));
#63113=CARTESIAN_POINT('Ctrl Pts',(0.00696094236000387,-0.0315281082229192,
0.0723202174840268));
#63114=CARTESIAN_POINT('Ctrl Pts',(0.0069840622333989,-0.0315281082229192,
0.0723240830795569));
#63115=CARTESIAN_POINT('Ctrl Pts',(0.00699153257991565,-0.0315281082229192,
0.072326114864887));
#63116=CARTESIAN_POINT('Ctrl Pts',(0.00700236736391432,-0.0315281082229192,
0.0723317082934015));
#63117=CARTESIAN_POINT('Ctrl Pts',(0.00700628093475598,-0.0315281082229192,
0.0723344806504444));
#63118=CARTESIAN_POINT('Ctrl Pts',(0.00701259234411832,-0.0315281082229192,
0.0723413281190414));
#63119=CARTESIAN_POINT('Ctrl Pts',(0.00701488997279872,-0.0315281082229192,
0.0723451142719038));
#63120=CARTESIAN_POINT('Ctrl Pts',(0.00701838111679472,-0.0315281082229192,
0.0723547226865156));
#63121=CARTESIAN_POINT('Ctrl Pts',(0.00701901723954043,-0.0315281082229192,
0.0723604498449024));
#63122=CARTESIAN_POINT('Ctrl Pts',(0.00701855552816112,-0.0315281082229192,
0.0723749667362874));
#63123=CARTESIAN_POINT('Ctrl Pts',(0.00701633056667769,-0.0315281082229192,
0.0723844150799716));
#63124=CARTESIAN_POINT('Ctrl Pts',(0.00700533444282857,-0.0315281082229192,
0.07241623739993));
#63125=CARTESIAN_POINT('Ctrl Pts',(0.006990685757266,-0.0315281082229192,
0.0724418345314411));
#63126=CARTESIAN_POINT('Ctrl Pts',(0.00689688702227869,-0.0315281082229192,
0.0725877915328833));
#63127=CARTESIAN_POINT('Ctrl Pts',(0.00673080378851581,-0.0315281082229192,
0.0727773871144422));
#63128=CARTESIAN_POINT('Ctrl Pts',(0.00645755406311322,-0.0315281082229192,
0.0732998343171583));
#63129=CARTESIAN_POINT('Ctrl Pts',(0.00639422129915112,-0.0315281082229192,
0.0735231500021576));
#63130=CARTESIAN_POINT('Ctrl Pts',(0.00632988803870339,-0.0315281082229192,
0.0739546853543993));
#63131=CARTESIAN_POINT('Ctrl Pts',(0.00633656673913058,-0.0315281082229192,
0.0741967633645283));
#63132=CARTESIAN_POINT('Ctrl Pts',(0.00643779274399072,-0.0315281082229192,
0.0746675424839583));
#63133=CARTESIAN_POINT('Ctrl Pts',(0.00652881158812033,-0.0315281082229192,
0.0748790244316244));
#63134=CARTESIAN_POINT('Ctrl Pts',(0.00678360157726101,-0.0315281082229192,
0.0752602394191017));
#63135=CARTESIAN_POINT('Ctrl Pts',(0.00694815581386843,-0.0315281082229192,
0.0754289690043338));
#63136=CARTESIAN_POINT('Ctrl Pts',(0.00737024253118045,-0.0315281082229192,
0.0757225788008902));
#63137=CARTESIAN_POINT('Ctrl Pts',(0.00760228849775194,-0.0315281082229192,
0.0758044262461883));
#63138=CARTESIAN_POINT('Ctrl Pts',(0.00799226788849764,-0.0315281082229192,
0.0758882741543255));
#63139=CARTESIAN_POINT('Ctrl Pts',(0.00824055843794205,-0.0315281082229192,
0.0759101885441291));
#63140=CARTESIAN_POINT('Ctrl Pts',(0.00877222168832291,-0.0315281082229192,
0.0758096151203664));
#63141=CARTESIAN_POINT('Ctrl Pts',(0.00901072440531448,-0.031528108222919,
0.0757123703062191));
#63142=CARTESIAN_POINT('Ctrl Pts',(0.00942936166701739,-0.031528108222919,
0.0754370419824175));
#63143=CARTESIAN_POINT('Ctrl Pts',(0.00961497183389103,-0.0315281082229192,
0.075259295977966));
#63144=CARTESIAN_POINT('Ctrl Pts',(0.00998728974756363,-0.0315281082229192,
0.0747160970557801));
#63145=CARTESIAN_POINT('Ctrl Pts',(0.0100770415748213,-0.0315281082229192,
0.0744130626439684));
#63146=CARTESIAN_POINT('Ctrl Pts',(0.0101559062218069,-0.0315281082229192,
0.0741709433951502));
#63147=CARTESIAN_POINT('Ctrl Pts',(0.0101731338183302,-0.0315281082229192,
0.0741211717490925));
#63148=CARTESIAN_POINT('Ctrl Pts',(0.0101976354678072,-0.0315281082229192,
0.0740742120961429));
#63149=CARTESIAN_POINT('Ctrl Pts',(0.010205012267356,-0.0315281082229192,
0.0740623410869319));
#63150=CARTESIAN_POINT('Ctrl Pts',(0.0102172281970335,-0.0315281082229192,
0.0740489929183199));
#63151=CARTESIAN_POINT('Ctrl Pts',(0.0102218571970461,-0.0315281082229192,
0.0740448431008829));
#63152=CARTESIAN_POINT('Ctrl Pts',(0.0102305223709339,-0.0315281082229192,
0.0740398720236682));
#63153=CARTESIAN_POINT('Ctrl Pts',(0.0102342438738187,-0.0315281082229192,
0.0740384012812181));
#63154=CARTESIAN_POINT('Ctrl Pts',(0.0102393236553668,-0.0315281082229192,
0.0740375392238714));
#63155=CARTESIAN_POINT('Ctrl Pts',(0.0102404267778191,-0.0315281082229192,
0.0740374167638213));
#63156=CARTESIAN_POINT('Ctrl Pts',(0.0102415292846687,-0.0315281082229192,
0.0740373581220493));
#63157=CARTESIAN_POINT('',(0.00600748819723868,-0.0211741814719622,0.0740583944593496));
#63158=CARTESIAN_POINT('Ctrl Pts',(0.0102415292846701,-0.0315281082229191,
0.0740373581220501));
#63159=CARTESIAN_POINT('Ctrl Pts',(0.0102474107028906,-0.0315193335619991,
0.0741426793323997));
#63160=CARTESIAN_POINT('Ctrl Pts',(0.0102454265162678,-0.0315105589010791,
0.0742481447151113));
#63161=CARTESIAN_POINT('Ctrl Pts',(0.0101892230058022,-0.0314613357379553,
0.0748339923228011));
#63162=CARTESIAN_POINT('Ctrl Pts',(0.00997379973563606,-0.0314208872357532,
0.0752903676969252));
#63163=CARTESIAN_POINT('Ctrl Pts',(0.00931534986442847,-0.031339990231348,
0.075967462485304));
#63164=CARTESIAN_POINT('Ctrl Pts',(0.00887509295304323,-0.0312995417291452,
0.0761868152287656));
#63165=CARTESIAN_POINT('Ctrl Pts',(0.00796079155782699,-0.0312186447247393,
0.0763148367595518));
#63166=CARTESIAN_POINT('Ctrl Pts',(0.00748945302262128,-0.0311781962225358,
0.0762240386264647));
#63167=CARTESIAN_POINT('Ctrl Pts',(0.00669956413626623,-0.0310972992181319,
0.0757857300068678));
#63168=CARTESIAN_POINT('Ctrl Pts',(0.00638267793035737,-0.0310568507159276,
0.0754400513829074));
#63169=CARTESIAN_POINT('Ctrl Pts',(0.00595750536674637,-0.030964014339277,
0.0745180867156372));
#63170=CARTESIAN_POINT('Ctrl Pts',(0.00594354974162806,-0.0309116264648272,
0.0739084696771727));
#63171=CARTESIAN_POINT('Ctrl Pts',(0.00634496891942769,-0.0308068507159279,
0.0728664214919276));
#63172=CARTESIAN_POINT('Ctrl Pts',(0.00675592000443203,-0.0307544628414776,
0.0724395062495526));
#63173=CARTESIAN_POINT('Ctrl Pts',(0.0077494649754808,-0.0306496870925817,
0.0719920559628832));
#63174=CARTESIAN_POINT('Ctrl Pts',(0.00832584380498464,-0.0305972992181321,
0.0719722823282605));
#63175=CARTESIAN_POINT('Ctrl Pts',(0.00932997882757754,-0.0304925234692313,
0.0723256171343211));
#63176=CARTESIAN_POINT('Ctrl Pts',(0.00975323921825422,-0.0304401355947827,
0.0726954265952984));
#63177=CARTESIAN_POINT('Ctrl Pts',(0.0102414483775728,-0.0303353598458849,
0.0736148328055268));
#63178=CARTESIAN_POINT('Ctrl Pts',(0.0103054074683059,-0.0302829719714357,
0.0741595369305542));
#63179=CARTESIAN_POINT('Ctrl Pts',(0.0100631115942824,-0.0301781962225362,
0.0751492903863319));
#63180=CARTESIAN_POINT('Ctrl Pts',(0.00975909850238958,-0.0301258083480876,
0.0755904500898765));
#63181=CARTESIAN_POINT('Ctrl Pts',(0.0089451874363639,-0.0300210325991884,
0.0761685265237053));
#63182=CARTESIAN_POINT('Ctrl Pts',(0.00843911221849071,-0.0299686447247403,
0.0763040900230327));
#63183=CARTESIAN_POINT('Ctrl Pts',(0.00746350290246076,-0.02986386897584,
0.0762245043065757));
#63184=CARTESIAN_POINT('Ctrl Pts',(0.00699741885923872,-0.0298114811013907,
0.0760106285387534));
#63185=CARTESIAN_POINT('Ctrl Pts',(0.00630586837465766,-0.0297067053524937,
0.0753440780020337));
#63186=CARTESIAN_POINT('Ctrl Pts',(0.00608211280228693,-0.0296543174780434,
0.0748942803942386));
#63187=CARTESIAN_POINT('Ctrl Pts',(0.00595907161542407,-0.0295495417291453,
0.0739592244029917));
#63188=CARTESIAN_POINT('Ctrl Pts',(0.00605938394721744,-0.0294971538546968,
0.0734769967671513));
#63189=CARTESIAN_POINT('Ctrl Pts',(0.00652798278812114,-0.029392378105796,
0.0726775538261953));
#63190=CARTESIAN_POINT('Ctrl Pts',(0.00689428236856863,-0.0293399902313469,
0.0723623130857159));
#63191=CARTESIAN_POINT('Ctrl Pts',(0.00773657577545569,-0.0292352144824501,
0.0720151544508798));
#63192=CARTESIAN_POINT('Ctrl Pts',(0.00821001945932422,-0.0291828266079989,
0.0719835875408627));
#63193=CARTESIAN_POINT('Ctrl Pts',(0.00907878062310723,-0.0290780508591023,
0.0722035268267701));
#63194=CARTESIAN_POINT('Ctrl Pts',(0.00947201428442268,-0.0290256629846524,
0.072453899629834));
#63195=CARTESIAN_POINT('Ctrl Pts',(0.0100362994783456,-0.0289208872357529,
0.0731317839731108));
#63196=CARTESIAN_POINT('Ctrl Pts',(0.0102064021029961,-0.0288684993613048,
0.0735573200377487));
#63197=CARTESIAN_POINT('Ctrl Pts',(0.0102717693088642,-0.0287637236124047,
0.0744233616342778));
#63198=CARTESIAN_POINT('Ctrl Pts',(0.0101673721494254,-0.0287113357379557,
0.0748618658679991));
#63199=CARTESIAN_POINT('Ctrl Pts',(0.00973174559026465,-0.028606559989058,
0.0755982633195131));
#63200=CARTESIAN_POINT('Ctrl Pts',(0.00940183247449225,-0.0285541721146081,
0.0758948085378461));
#63201=CARTESIAN_POINT('Ctrl Pts',(0.00863746583537968,-0.0284493963657099,
0.0762509280036797));
#63202=CARTESIAN_POINT('Ctrl Pts',(0.00820473003409823,-0.0283970084912602,
0.076310154007468));
#63203=CARTESIAN_POINT('Ctrl Pts',(0.00738340683150901,-0.0282922327423619,
0.0761809264433306));
#63204=CARTESIAN_POINT('Ctrl Pts',(0.00699633121784709,-0.028239844867912,
0.0759930922591544));
#63205=CARTESIAN_POINT('Ctrl Pts',(0.00639068647810172,-0.0281350691190143,
0.075440160464901));
#63206=CARTESIAN_POINT('Ctrl Pts',(0.00617298034709087,-0.0280826812445643,
0.0750763211850444));
#63207=CARTESIAN_POINT('Ctrl Pts',(0.00596897958949985,-0.0279779054956661,
0.0742932638294421));
#63208=CARTESIAN_POINT('Ctrl Pts',(0.00598272505460037,-0.0279255176212164,
0.073875472823177));
#63209=CARTESIAN_POINT('Ctrl Pts',(0.00635232687879448,-0.0277683539978693,
0.0727358184526565));
#63210=CARTESIAN_POINT('Ctrl Pts',(0.00705289958900958,-0.0276635782489686,
0.0721600303097132));
#63211=CARTESIAN_POINT('Ctrl Pts',(0.00859517611493118,-0.0274540267511745,
0.0719398966766563));
#63212=CARTESIAN_POINT('Ctrl Pts',(0.00940073146439328,-0.0273492510022741,
0.0722931522835415));
#63213=CARTESIAN_POINT('Ctrl Pts',(0.0102896623256786,-0.0271396995044774,
0.0735275482799331));
#63214=CARTESIAN_POINT('Ctrl Pts',(0.010359884849577,-0.0270349237555792,
0.0743792630330001));
#63215=CARTESIAN_POINT('Ctrl Pts',(0.00972755157183108,-0.0268253722577806,
0.0757250048942655));
#63216=CARTESIAN_POINT('Ctrl Pts',(0.00904218730885863,-0.0267205965088817,
0.0761958934123178));
#63217=CARTESIAN_POINT('Ctrl Pts',(0.00759343482402584,-0.0265110450110865,
0.0763289629385248));
#63218=CARTESIAN_POINT('Ctrl Pts',(0.00685580966361203,-0.0264062692621874,
0.0759938417732247));
#63219=CARTESIAN_POINT('Ctrl Pts',(0.00599991759097347,-0.0261967177643892,
0.0748547737082654));
#63220=CARTESIAN_POINT('Ctrl Pts',(0.00589186280469173,-0.0260919420154909,
0.0740718608505132));
#63221=CARTESIAN_POINT('Ctrl Pts',(0.00627724799864211,-0.0259246662665926,
0.0730258105884879));
#63222=CARTESIAN_POINT('Ctrl Pts',(0.00654039915241529,-0.0258621662665935,
0.0726767209970879));
#63223=CARTESIAN_POINT('Ctrl Pts',(0.00722389165927775,-0.0257371662665915,
0.0721833149981475));
#63224=CARTESIAN_POINT('Ctrl Pts',(0.00764304374228332,-0.0256746662665924,
0.0720402815521564));
#63225=CARTESIAN_POINT('Ctrl Pts',(0.00849604407482765,-0.0255496662665926,
0.0720184647612599));
#63226=CARTESIAN_POINT('Ctrl Pts',(0.00892808254078336,-0.0254871662665921,
0.07214009674052));
#63227=CARTESIAN_POINT('Ctrl Pts',(0.00965002750714532,-0.0253621662665928,
0.0726146871985494));
#63228=CARTESIAN_POINT('Ctrl Pts',(0.00993809892066803,-0.0252996662665926,
0.0729669145852015));
#63229=CARTESIAN_POINT('Ctrl Pts',(0.0102581523851926,-0.0251746662665924,
0.0737813536046464));
#63230=CARTESIAN_POINT('Ctrl Pts',(0.0102889821151069,-0.0251121662665924,
0.0742418039415068));
#63231=CARTESIAN_POINT('Ctrl Pts',(0.010071019077723,-0.0249871662665926,
0.0751012030151419));
#63232=CARTESIAN_POINT('Ctrl Pts',(0.00982231809848441,-0.024924666266593,
0.07549790728317));
#63233=CARTESIAN_POINT('Ctrl Pts',(0.00912998835433636,-0.024799666266592,
0.0760707882292855));
#63234=CARTESIAN_POINT('Ctrl Pts',(0.00868784969457759,-0.0247371662665924,
0.07624508144423));
#63235=CARTESIAN_POINT('Ctrl Pts',(0.00777792798085125,-0.0246121662665926,
0.0762919438047406));
#63236=CARTESIAN_POINT('Ctrl Pts',(0.00731262787164867,-0.0245496662665925,
0.0761638405487234));
#63237=CARTESIAN_POINT('Ctrl Pts',(0.0065485129249735,-0.0244246662665925,
0.0756440052932471));
#63238=CARTESIAN_POINT('Ctrl Pts',(0.00625226027464946,-0.0243621662665925,
0.0752533010137793));
#63239=CARTESIAN_POINT('Ctrl Pts',(0.00596159400885685,-0.0242371662665925,
0.0743616829432692));
#63240=CARTESIAN_POINT('Ctrl Pts',(0.00596869167054677,-0.0241746662665925,
0.07386332441141));
#63241=CARTESIAN_POINT('Ctrl Pts',(0.00629781787585632,-0.0240496662665925,
0.0729699778138594));
#63242=CARTESIAN_POINT('Ctrl Pts',(0.00661942895548025,-0.0239871662665926,
0.0725781618664859));
#63243=CARTESIAN_POINT('Ctrl Pts',(0.00744911026789867,-0.0238621662665923,
0.0720815291713897));
#63244=CARTESIAN_POINT('Ctrl Pts',(0.00795468689116961,-0.0237996662665922,
0.0719791054916663));
#63245=CARTESIAN_POINT('Ctrl Pts',(0.0089262758271642,-0.0236746662665927,
0.0721258013564626));
#63246=CARTESIAN_POINT('Ctrl Pts',(0.00938855725198137,-0.0236121662665922,
0.0723752164881653));
#63247=CARTESIAN_POINT('Ctrl Pts',(0.0100475843126518,-0.0234871662665927,
0.0731260381541277));
#63248=CARTESIAN_POINT('Ctrl Pts',(0.0102410178141923,-0.0234246662665924,
0.0736250907589115));
#63249=CARTESIAN_POINT('Ctrl Pts',(0.0102490546008787,-0.0232996662665926,
0.0746413589041057));
#63250=CARTESIAN_POINT('Ctrl Pts',(0.0100625879641978,-0.0232371662665925,
0.0751542816790953));
#63251=CARTESIAN_POINT('Ctrl Pts',(0.00938270763587042,-0.0231121662665924,
0.0759340000649118));
#63252=CARTESIAN_POINT('Ctrl Pts',(0.00889151097164585,-0.0230496662665924,
0.0761965031486893));
#63253=CARTESIAN_POINT('Ctrl Pts',(0.00784480408877878,-0.0229246662665925,
0.0763178915621161));
#63254=CARTESIAN_POINT('Ctrl Pts',(0.00729424742007936,-0.0228621662665928,
0.0761749122408133));
#63255=CARTESIAN_POINT('Ctrl Pts',(0.00643067872875265,-0.0227371662665921,
0.0755362893544149));
#63256=CARTESIAN_POINT('Ctrl Pts',(0.00612305344798784,-0.0226746662665923,
0.0750428459007938));
#63257=CARTESIAN_POINT('Ctrl Pts',(0.00594091088577522,-0.0225496662665926,
0.0739624842354635));
#63258=CARTESIAN_POINT('Ctrl Pts',(0.00606901592181546,-0.0224871662665922,
0.0733814268319492));
#63259=CARTESIAN_POINT('Ctrl Pts',(0.00671499560243656,-0.0223621662665927,
0.0724683075554325));
#63260=CARTESIAN_POINT('Ctrl Pts',(0.00723038395375605,-0.0222996662665929,
0.0721429107222321));
#63261=CARTESIAN_POINT('Ctrl Pts',(0.00835948988205837,-0.022174666266592,
0.0719657358996911));
#63262=CARTESIAN_POINT('Ctrl Pts',(0.00896597799697031,-0.0221121662665928,
0.0721171826520367));
#63263=CARTESIAN_POINT('Ctrl Pts',(0.00988830420246689,-0.0219871662665922,
0.0728354269849725));
#63264=CARTESIAN_POINT('Ctrl Pts',(0.0101959629269755,-0.0219246662665924,
0.0733988421450626));
#63265=CARTESIAN_POINT('Ctrl Pts',(0.0102830084237745,-0.0217996662665926,
0.0745926208223076));
#63266=CARTESIAN_POINT('Ctrl Pts',(0.0100589999732895,-0.0217371662665924,
0.075213633090309));
#63267=CARTESIAN_POINT('Ctrl Pts',(0.00919252612250013,-0.0216121662665926,
0.0760823999614819));
#63268=CARTESIAN_POINT('Ctrl Pts',(0.00855547426588603,-0.0215496662665927,
0.0763202968801402));
#63269=CARTESIAN_POINT('Ctrl Pts',(0.00730138706368173,-0.0214246662665922,
0.0762043156608544));
#63270=CARTESIAN_POINT('Ctrl Pts',(0.00669689975963152,-0.0213621662665925,
0.0758479396774564));
#63271=CARTESIAN_POINT('Ctrl Pts',(0.00610859628485939,-0.0212578380017156,
0.0749416387703421));
#63272=CARTESIAN_POINT('Ctrl Pts',(0.00599064760068548,-0.0212160097368389,
0.0744989393311625));
#63273=CARTESIAN_POINT('Ctrl Pts',(0.00600748819723773,-0.0211741814719621,
0.0740583944593496));
#63274=CARTESIAN_POINT('',(0.00895037744954432,-0.0211741814719619,0.0761032845693596));
#63275=CARTESIAN_POINT('Ctrl Pts',(0.00895037744954477,-0.0211741814719619,
0.0761032845693594));
#63276=CARTESIAN_POINT('Ctrl Pts',(0.00895142341614423,-0.0211741814719619,
0.0761057562390223));
#63277=CARTESIAN_POINT('Ctrl Pts',(0.00895279546040267,-0.0211741814719619,
0.0761080260384607));
#63278=CARTESIAN_POINT('Ctrl Pts',(0.0089562501401301,-0.0211741814719619,
0.0761123590771521));
#63279=CARTESIAN_POINT('Ctrl Pts',(0.00895832322888189,-0.0211741814719619,
0.0761143334593383));
#63280=CARTESIAN_POINT('Ctrl Pts',(0.00896593439949515,-0.0211741814719619,
0.0761202179010537));
#63281=CARTESIAN_POINT('Ctrl Pts',(0.00897242564316084,-0.0211741814719619,
0.076123153785668));
#63282=CARTESIAN_POINT('Ctrl Pts',(0.00899823396132728,-0.0211741814719619,
0.0761316568472288));
#63283=CARTESIAN_POINT('Ctrl Pts',(0.00902247926375369,-0.0211741814719619,
0.0761323854854028));
#63284=CARTESIAN_POINT('Ctrl Pts',(0.00909067528635312,-0.0211741814719619,
0.0761310837812301));
#63285=CARTESIAN_POINT('Ctrl Pts',(0.00916256604711786,-0.0211741814719619,
0.0761179828307763));
#63286=CARTESIAN_POINT('Ctrl Pts',(0.0094044630434647,-0.0211741814719619,
0.0760382388246817));
#63287=CARTESIAN_POINT('Ctrl Pts',(0.00960115375427539,-0.0211741814719619,
0.0759369373400467));
#63288=CARTESIAN_POINT('Ctrl Pts',(0.00999901075226726,-0.0211741814719619,
0.0756042971860892));
#63289=CARTESIAN_POINT('Ctrl Pts',(0.010168666941163,-0.0211741814719619,
0.0753988227592878));
#63290=CARTESIAN_POINT('Ctrl Pts',(0.0104152222765945,-0.0211741814719619,
0.0749673473278423));
#63291=CARTESIAN_POINT('Ctrl Pts',(0.0105190162621075,-0.0211741814719619,
0.0747132809438133));
#63292=CARTESIAN_POINT('Ctrl Pts',(0.0106108249011952,-0.0211741814719619,
0.0741008079828946));
#63293=CARTESIAN_POINT('Ctrl Pts',(0.0105931415034016,-0.0211741814719619,
0.0737885844705757));
#63294=CARTESIAN_POINT('Ctrl Pts',(0.0104463470744042,-0.0211741814719619,
0.0731922680894886));
#63295=CARTESIAN_POINT('Ctrl Pts',(0.0103180576222123,-0.0211741814719619,
0.0729082566766417));
#63296=CARTESIAN_POINT('Ctrl Pts',(0.0099644329500286,-0.0211741814719619,
0.0724044777589146));
#63297=CARTESIAN_POINT('Ctrl Pts',(0.00974294206368656,-0.0211741814719619,
0.0721926834393527));
#63298=CARTESIAN_POINT('Ctrl Pts',(0.00920576807857105,-0.0211741814719619,
0.0718531426457546));
#63299=CARTESIAN_POINT('Ctrl Pts',(0.00889561756514791,-0.0211741814719619,
0.071736241382821));
#63300=CARTESIAN_POINT('Ctrl Pts',(0.00827174092211097,-0.0211741814719619,
0.071630329583783));
#63301=CARTESIAN_POINT('Ctrl Pts',(0.00795886823722732,-0.0211741814719619,
0.0716346314104874));
#63302=CARTESIAN_POINT('Ctrl Pts',(0.00734095337665573,-0.0211741814719619,
0.0717688073312937));
#63303=CARTESIAN_POINT('Ctrl Pts',(0.00708575460295718,-0.0211741814719619,
0.071895244930667));
#63304=CARTESIAN_POINT('Ctrl Pts',(0.006653901489938,-0.0211741814719619,
0.072179942485354));
#63305=CARTESIAN_POINT('Ctrl Pts',(0.00644724510751011,-0.0211741814719619,
0.0723766081242654));
#63306=CARTESIAN_POINT('Ctrl Pts',(0.00612446840762261,-0.0211741814719619,
0.0728227795090391));
#63307=CARTESIAN_POINT('Ctrl Pts',(0.0060148726041794,-0.0211741814719619,
0.0730573587817859));
#63308=CARTESIAN_POINT('Ctrl Pts',(0.00589812726791177,-0.0211741814719619,
0.0735089027067287));
#63309=CARTESIAN_POINT('Ctrl Pts',(0.00589346761698436,-0.0211741814719619,
0.0736999278899219));
#63310=CARTESIAN_POINT('Ctrl Pts',(0.00591824566295887,-0.0211741814719619,
0.0739041184431284));
#63311=CARTESIAN_POINT('Ctrl Pts',(0.00593298868605388,-0.0211741814719619,
0.0739614758718291));
#63312=CARTESIAN_POINT('Ctrl Pts',(0.005957576476281,-0.0211741814719619,
0.0740152647149347));
#63313=CARTESIAN_POINT('Ctrl Pts',(0.00596672380209973,-0.0211741814719619,
0.0740316468526178));
#63314=CARTESIAN_POINT('Ctrl Pts',(0.0059823803419084,-0.0211741814719619,
0.0740475599562614));
#63315=CARTESIAN_POINT('Ctrl Pts',(0.00598722794163848,-0.0211741814719619,
0.0740514990739912));
#63316=CARTESIAN_POINT('Ctrl Pts',(0.00599498500208107,-0.0211741814719619,
0.0740554998710154));
#63317=CARTESIAN_POINT('Ctrl Pts',(0.00599745107590697,-0.0211741814719619,
0.0740564951510525));
#63318=CARTESIAN_POINT('Ctrl Pts',(0.00600246497103547,-0.0211741814719619,
0.0740578817256914));
#63319=CARTESIAN_POINT('Ctrl Pts',(0.00600494927171444,-0.0211741814719619,
0.0740582845598504));
#63320=CARTESIAN_POINT('Ctrl Pts',(0.00600748819723879,-0.0211741814719619,
0.0740583944593472));
#63321=CARTESIAN_POINT('Ctrl Pts',(0.00600748819723879,-0.0211741814719619,
0.0740583944593471));
#63322=CARTESIAN_POINT('Ctrl Pts',(0.00601070231456546,-0.0211741814719619,
0.074058533585081));
#63323=CARTESIAN_POINT('Ctrl Pts',(0.00601386573624221,-0.0211741814719619,
0.0740581967876821));
#63324=CARTESIAN_POINT('Ctrl Pts',(0.00602032959859923,-0.0211741814719619,
0.0740566385094979));
#63325=CARTESIAN_POINT('Ctrl Pts',(0.00602353437818118,-0.0211741814719619,
0.0740553792170983));
#63326=CARTESIAN_POINT('Ctrl Pts',(0.00603379822221034,-0.0211741814719619,
0.074050110918832));
#63327=CARTESIAN_POINT('Ctrl Pts',(0.00604038521610018,-0.0211741814719619,
0.0740445702503871));
#63328=CARTESIAN_POINT('Ctrl Pts',(0.00605963783788561,-0.0211741814719619,
0.0740249955212598));
#63329=CARTESIAN_POINT('Ctrl Pts',(0.00607311807020041,-0.0211741814719619,
0.0740046692333217));
#63330=CARTESIAN_POINT('Ctrl Pts',(0.0061160806526335,-0.0211741814719619,
0.0739272008086412));
#63331=CARTESIAN_POINT('Ctrl Pts',(0.00614780156907989,-0.0211741814719619,
0.0738518940925071));
#63332=CARTESIAN_POINT('Ctrl Pts',(0.00626308582369267,-0.0211741814719619,
0.073595816618586));
#63333=CARTESIAN_POINT('Ctrl Pts',(0.00636873577430343,-0.0211741814719619,
0.0733776720079871));
#63334=CARTESIAN_POINT('Ctrl Pts',(0.00670988430688753,-0.0211741814719619,
0.0729655110110068));
#63335=CARTESIAN_POINT('Ctrl Pts',(0.00689489702552421,-0.0211741814719619,
0.0728047622729589));
#63336=CARTESIAN_POINT('Ctrl Pts',(0.00729018071586256,-0.0211741814719619,
0.0725694044020097));
#63337=CARTESIAN_POINT('Ctrl Pts',(0.00749475094614348,-0.0211741814719619,
0.0724887144709966));
#63338=CARTESIAN_POINT('Ctrl Pts',(0.00794565217078984,-0.0211741814719619,
0.072401913681025));
#63339=CARTESIAN_POINT('Ctrl Pts',(0.00819205162095311,-0.0211741814719622,
0.0724054295806454));
#63340=CARTESIAN_POINT('Ctrl Pts',(0.0086533508659248,-0.0211741814719622,
0.0724992888967247));
#63341=CARTESIAN_POINT('Ctrl Pts',(0.0088699157664898,-0.0211741814719563,
0.072585266090591));
#63342=CARTESIAN_POINT('Ctrl Pts',(0.00924694454333932,-0.0211741814719563,
0.0728259648510416));
#63343=CARTESIAN_POINT('Ctrl Pts',(0.00941528697237473,-0.0211741814719619,
0.0729802370505302));
#63344=CARTESIAN_POINT('Ctrl Pts',(0.00969406333781521,-0.0211741814719619,
0.0733800321346033));
#63345=CARTESIAN_POINT('Ctrl Pts',(0.00979247324332182,-0.0211741814719619,
0.0736000915629057));
#63346=CARTESIAN_POINT('Ctrl Pts',(0.00988871785872756,-0.0211741814719619,
0.0739957305323329));
#63347=CARTESIAN_POINT('Ctrl Pts',(0.00992783454669963,-0.0211741814719619,
0.0742476174138145));
#63348=CARTESIAN_POINT('Ctrl Pts',(0.00984789973010626,-0.0211741814719619,
0.0747689103030387));
#63349=CARTESIAN_POINT('Ctrl Pts',(0.00977449732126798,-0.0211741814719619,
0.074980541548417));
#63350=CARTESIAN_POINT('Ctrl Pts',(0.00953289899259933,-0.0211741814719619,
0.0754403783588731));
#63351=CARTESIAN_POINT('Ctrl Pts',(0.00936282454286502,-0.0211741814719619,
0.0756352637677106));
#63352=CARTESIAN_POINT('Ctrl Pts',(0.00914639631262419,-0.0211741814719619,
0.075858559708378));
#63353=CARTESIAN_POINT('Ctrl Pts',(0.00906928299020927,-0.0211741814719619,
0.0759289651434673));
#63354=CARTESIAN_POINT('Ctrl Pts',(0.00899184880715194,-0.0211741814719619,
0.0760111053919389));
#63355=CARTESIAN_POINT('Ctrl Pts',(0.00897214521593804,-0.0211741814719619,
0.0760346209492319));
#63356=CARTESIAN_POINT('Ctrl Pts',(0.00895510134701174,-0.0211741814719619,
0.0760638173989724));
#63357=CARTESIAN_POINT('Ctrl Pts',(0.00895089982051269,-0.0211741814719619,
0.0760730008099204));
#63358=CARTESIAN_POINT('Ctrl Pts',(0.0089482497709946,-0.0211741814719619,
0.0760855423549168));
#63359=CARTESIAN_POINT('Ctrl Pts',(0.00894784735747076,-0.0211741814719619,
0.0760894012590408));
#63360=CARTESIAN_POINT('Ctrl Pts',(0.00894829061504419,-0.0211741814719619,
0.0760967100289629));
#63361=CARTESIAN_POINT('Ctrl Pts',(0.00894901845018085,-0.0211741814719619,
0.0761000731881343));
#63362=CARTESIAN_POINT('Ctrl Pts',(0.00895037744954474,-0.0211741814719619,
0.0761032845693594));
#63363=CARTESIAN_POINT('Origin',(-0.0248134380203094,-0.0211741814719619,
0.00872990597260584));
#63364=CARTESIAN_POINT('Origin',(0.000869198225586133,-0.0315281082229192,
0.0821343473622993));
#63365=CARTESIAN_POINT('',(0.,0.,0.));
#63366=CARTESIAN_POINT('Origin',(-0.0186262178068916,-0.0128741814719618,
0.0571));
#63367=CARTESIAN_POINT('',(-0.0176262178068916,-0.0128741814719618,0.05660000000001));
#63368=CARTESIAN_POINT('Origin',(-0.0186262178069016,-0.0128741814719718,
0.05660000000001));
#63369=CARTESIAN_POINT('',(-0.0171262178068916,-0.0128741814719618,0.05710000000001));
#63370=CARTESIAN_POINT('Origin',(-0.0176262178068916,-0.0128741814719618,
0.0571));
#63371=CARTESIAN_POINT('Origin',(-0.0186262178069016,-0.0128741814719718,
0.05710000000001));
#63372=CARTESIAN_POINT('Origin',(-0.0186262178068916,-0.0128741814719618,
0.0856));
#63373=CARTESIAN_POINT('',(-0.0171262178068916,-0.0128741814719618,0.08560000000001));
#63374=CARTESIAN_POINT('',(-0.0171262178068916,-0.0128741814719618,0.0856));
#63375=CARTESIAN_POINT('Origin',(-0.0186262178069016,-0.0128741814719718,
0.08560000000001));
#63376=CARTESIAN_POINT('Origin',(-0.0186262178068916,-0.0128741814719618,
0.0856));
#63377=CARTESIAN_POINT('Origin',(-0.0186262178068916,-0.0128741814719618,
0.0566));
#63378=CARTESIAN_POINT('',(0.,0.,0.));
#63379=CARTESIAN_POINT('Origin',(-0.00312621780689159,0.00227581852803817,
0.0795478161976335));
#63380=CARTESIAN_POINT('',(-0.00062621780689159,0.00227581852803817,0.05560000000001));
#63381=CARTESIAN_POINT('Origin',(-0.0031262178069016,0.00227581852804816,
0.05560000000001));
#63382=CARTESIAN_POINT('',(-0.00062621780689159,0.00227581852803817,0.0795478161976436));
#63383=CARTESIAN_POINT('',(-0.00062621780689159,0.00227581852803817,0.0795478161976335));
#63384=CARTESIAN_POINT('',(-0.00147431229815866,0.000399330267958239,0.0795478161976335));
#63385=CARTESIAN_POINT('Origin',(-0.0031262178069016,0.00227581852804816,
0.0795478161976436));
#63386=CARTESIAN_POINT('',(-0.00477812331562454,0.000399330267958239,0.0795478161976335));
#63387=CARTESIAN_POINT('Ctrl Pts',(-0.00147431229815864,0.000399330267958261,
0.0795478161976335));
#63388=CARTESIAN_POINT('Ctrl Pts',(-0.00141756753743531,0.000449283675514679,
0.0793724180142668));
#63389=CARTESIAN_POINT('Ctrl Pts',(-0.00139128264960183,0.00047581852803818,
0.0791807891325657));
#63390=CARTESIAN_POINT('Ctrl Pts',(-0.00139128264960183,0.00047581852803818,
0.079));
#63391=CARTESIAN_POINT('Ctrl Pts',(-0.00139128264960183,0.00047581852803818,
0.0788137403336619));
#63392=CARTESIAN_POINT('Ctrl Pts',(-0.00141923484858738,0.000447531815482377,
0.0786160265927576));
#63393=CARTESIAN_POINT('Ctrl Pts',(-0.00153985493559125,0.000341941867351019,
0.0782565826026003));
#63394=CARTESIAN_POINT('Ctrl Pts',(-0.00163385434425655,0.000265418371407152,
0.0780950718110287));
#63395=CARTESIAN_POINT('Ctrl Pts',(-0.00185670743308821,0.000118232327801343,
0.0778503362730228));
#63396=CARTESIAN_POINT('Ctrl Pts',(-0.00201374560920302,3.11585522271903E-5,
0.0777391784281712));
#63397=CARTESIAN_POINT('Ctrl Pts',(-0.00229857646949163,-8.77930433005222E-5,
0.0776057075686815));
#63398=CARTESIAN_POINT('Ctrl Pts',(-0.00245822273383093,-0.000139297746093857,
0.0775563101781988));
#63399=CARTESIAN_POINT('Ctrl Pts',(-0.00279192215600469,-0.000207576533398147,
0.0774937815188223));
#63400=CARTESIAN_POINT('Ctrl Pts',(-0.00296591250954424,-0.00022418147196183,
0.0774801315846429));
#63401=CARTESIAN_POINT('Ctrl Pts',(-0.00328652310423895,-0.00022418147196183,
0.0774801315846429));
#63402=CARTESIAN_POINT('Ctrl Pts',(-0.0034605134577785,-0.000207576533398146,
0.0774937815188223));
#63403=CARTESIAN_POINT('Ctrl Pts',(-0.00379421287995226,-0.000139297746093855,
0.0775563101781988));
#63404=CARTESIAN_POINT('Ctrl Pts',(-0.00395385914429156,-8.77930433005201E-5,
0.0776057075686815));
#63405=CARTESIAN_POINT('Ctrl Pts',(-0.00423869000458017,3.11585522271924E-5,
0.0777391784281712));
#63406=CARTESIAN_POINT('Ctrl Pts',(-0.00439572818069498,0.000118232327801344,
0.0778503362730228));
#63407=CARTESIAN_POINT('Ctrl Pts',(-0.00461858126952663,0.000265418371407153,
0.0780950718110287));
#63408=CARTESIAN_POINT('Ctrl Pts',(-0.00471258067819193,0.000341941867351019,
0.0782565826026003));
#63409=CARTESIAN_POINT('Ctrl Pts',(-0.0048332007651958,0.000447531815482377,
0.0786160265927576));
#63410=CARTESIAN_POINT('Ctrl Pts',(-0.00486115296418135,0.00047581852803818,
0.0788137403336619));
#63411=CARTESIAN_POINT('Ctrl Pts',(-0.00486115296418135,0.00047581852803818,
0.0791807891325657));
#63412=CARTESIAN_POINT('Ctrl Pts',(-0.00483486807634788,0.000449283675514682,
0.0793724180142668));
#63413=CARTESIAN_POINT('Ctrl Pts',(-0.00477812331562455,0.000399330267958265,
0.0795478161976335));
#63414=CARTESIAN_POINT('Origin',(-0.0031262178069016,0.00227581852804816,
0.0795478161976436));
#63415=CARTESIAN_POINT('Origin',(-0.00312621780689159,0.00227581852803817,
0.0795478161976335));
#63416=CARTESIAN_POINT('',(-0.0411262178069016,0.000399330267968239,0.0795478161976436));
#63417=CARTESIAN_POINT('Origin',(-0.00312621780689159,0.00227581852803817,
0.0556));
#63418=CARTESIAN_POINT('Origin',(-0.0411262178068916,-0.00152418147196182,
0.079));
#63419=CARTESIAN_POINT('',(0.,0.,0.));
#63420=CARTESIAN_POINT('Origin',(0.0111237821931084,0.0230268185280382,
0.07415));
#63421=CARTESIAN_POINT('',(0.0111237821931084,-0.0145741814719618,0.0759));
#63422=CARTESIAN_POINT('',(0.0111237821931084,-0.0145741814719618,0.0724));
#63423=CARTESIAN_POINT('Origin',(0.0111237821931184,-0.0145741814719718,
0.07415000000001));
#63424=CARTESIAN_POINT('',(0.0111237821931084,-0.0201741814719619,0.0724));
#63425=CARTESIAN_POINT('',(0.0111237821931184,0.0230268185280482,0.07240000000001));
#63426=CARTESIAN_POINT('',(0.0111237821931084,-0.0201741814719619,0.0759));
#63427=CARTESIAN_POINT('Origin',(0.0111237821931184,-0.0201741814719718,
0.07415000000001));
#63428=CARTESIAN_POINT('',(0.0111237821931184,0.0230268185280482,0.07590000000001));
#63429=CARTESIAN_POINT('Origin',(-0.0186262178068916,-0.0128741814719618,
0.00803151208831422));
#63430=CARTESIAN_POINT('',(-0.0211577899118759,-0.0165945500931155,0.06365));
#63431=CARTESIAN_POINT('',(-0.0144596844756917,-0.0145741814719618,0.06365));
#63432=CARTESIAN_POINT('Origin',(-0.0186262178069016,-0.0128741814719718,
0.06365000000001));
#63433=CARTESIAN_POINT('',(-0.0211577899118759,-0.0165945500931155,0.08465));
#63434=CARTESIAN_POINT('',(-0.0211577899118859,-0.0165945500931255,0.00803151208832422));
#63435=CARTESIAN_POINT('',(-0.0144596844756917,-0.0145741814719618,0.08465));
#63436=CARTESIAN_POINT('Origin',(-0.0186262178069016,-0.0128741814719718,
0.08465000000001));
#63437=CARTESIAN_POINT('',(-0.0144596844757017,-0.0145741814719718,0.00803151208832422));
#63438=CARTESIAN_POINT('Origin',(0.0220033079492963,-0.0145741814719618,
0.00803151208831422));
#63439=CARTESIAN_POINT('',(0.0021237821931084,-0.0145741814719618,0.08465));
#63440=CARTESIAN_POINT('',(0.0220033079493063,-0.0145741814719718,0.08465000000001));
#63441=CARTESIAN_POINT('',(0.0220033079492963,-0.0145741814719618,0.0812224955592779));
#63442=CARTESIAN_POINT('',(0.00212378219311841,-0.0145741814719718,0.08465000000001));
#63443=CARTESIAN_POINT('',(0.0220033079492963,-0.0145741814719618,0.067077504440722));
#63444=CARTESIAN_POINT('',(0.0220033079493063,-0.0145741814719718,0.00803151208832422));
#63445=CARTESIAN_POINT('',(0.0021237821931084,-0.0145741814719618,0.06365));
#63446=CARTESIAN_POINT('',(0.0311237821931184,-0.0145741814719718,0.06865000000001));
#63447=CARTESIAN_POINT('',(0.0220033079493063,-0.0145741814719718,0.06365000000001));
#63448=CARTESIAN_POINT('',(0.0078737821931084,-0.0145741814719618,0.0759));
#63449=CARTESIAN_POINT('',(0.00787378219311841,-0.0145741814719718,0.07590000000001));
#63450=CARTESIAN_POINT('',(0.0078737821931084,-0.0145741814719618,0.0724));
#63451=CARTESIAN_POINT('Origin',(0.0078737821931184,-0.0145741814719718,
0.07415000000001));
#63452=CARTESIAN_POINT('',(0.00787378219311841,-0.0145741814719718,0.07240000000001));
#63453=CARTESIAN_POINT('Origin',(0.0273608110672173,-0.00879017202945387,
0.00803151208831422));
#63454=CARTESIAN_POINT('',(0.0301237821931084,-0.0161741814719619,0.0798224137931034));
#63455=CARTESIAN_POINT('Origin',(0.0273608110672267,-0.00879017202946598,
0.0802987881251636));
#63456=CARTESIAN_POINT('',(0.0301237821931084,-0.0161741814719619,0.0684775862068966));
#63457=CARTESIAN_POINT('',(0.0301237821931184,-0.0161741814719718,0.00803151208832422));
#63458=CARTESIAN_POINT('Origin',(0.0273608110672274,-0.00879017202946274,
0.0680012118748562));
#63459=CARTESIAN_POINT('Origin',(0.0311237821931084,-0.0161741814719619,
0.00803151208831422));
#63460=CARTESIAN_POINT('',(0.0311237821931084,-0.0161741814719619,0.07965));
#63461=CARTESIAN_POINT('',(0.0431153304000404,-0.0161741814719718,0.0775824916884717));
#63462=CARTESIAN_POINT('',(0.0311237821931084,-0.0161741814719619,0.06865));
#63463=CARTESIAN_POINT('',(0.0311237821931184,-0.0161741814719718,0.00803151208832422));
#63464=CARTESIAN_POINT('',(0.0209740353718777,-0.0161741814719718,0.0669000436515202));
#63465=CARTESIAN_POINT('Origin',(0.0311237821931084,-0.0201741814719619,
0.00803151208831422));
#63466=CARTESIAN_POINT('',(0.0311237821931084,-0.0184241814719618,0.07965));
#63467=CARTESIAN_POINT('',(0.0311237821931184,0.0148536964671725,0.07965000000001));
#63468=CARTESIAN_POINT('',(0.0311237821931084,-0.0184241814719618,0.06865));
#63469=CARTESIAN_POINT('',(0.0311237821931184,-0.0184241814719718,0.00803151208832422));
#63470=CARTESIAN_POINT('',(0.0311237821931184,0.0148536964671725,0.06865000000001));
#63471=CARTESIAN_POINT('Origin',(-0.0158972056958719,-0.0201741814719619,
0.00803151208831422));
#63472=CARTESIAN_POINT('',(0.0293737821931084,-0.0201741814719619,0.0781759039174667));
#63473=CARTESIAN_POINT('',(0.001974024914415,-0.0201741814719619,0.0829));
#63474=CARTESIAN_POINT('',(-0.00284557577388231,-0.0201741814719718,0.0837309656359216));
#63475=CARTESIAN_POINT('',(-0.0158972056958719,-0.0201741814719619,0.0829));
#63476=CARTESIAN_POINT('',(-0.0158972056958819,-0.0201741814719718,0.08290000000001));
#63477=CARTESIAN_POINT('',(-0.0158972056958719,-0.0201741814719619,0.0654));
#63478=CARTESIAN_POINT('',(-0.0158972056958819,-0.0201741814719718,0.00803151208832422));
#63479=CARTESIAN_POINT('',(0.00197402491441486,-0.0201741814719619,0.0654));
#63480=CARTESIAN_POINT('',(0.0021237821931184,-0.0201741814719718,0.06540000000001));
#63481=CARTESIAN_POINT('',(0.0293737821931084,-0.0201741814719619,0.0701240960825334));
#63482=CARTESIAN_POINT('',(-0.024986870802045,-0.0201741814719718,0.0607515697040704));
#63483=CARTESIAN_POINT('',(0.0293737821931184,-0.0201741814719718,0.00803151208832422));
#63484=CARTESIAN_POINT('',(0.0078737821931084,-0.0201741814719619,0.0724));
#63485=CARTESIAN_POINT('',(0.0078737821931184,-0.0201741814719718,0.07240000000001));
#63486=CARTESIAN_POINT('',(0.0078737821931084,-0.0201741814719619,0.0759));
#63487=CARTESIAN_POINT('Origin',(0.0078737821931184,-0.0201741814719718,
0.07415000000001));
#63488=CARTESIAN_POINT('',(0.0078737821931184,-0.0201741814719718,0.07590000000001));
#63489=CARTESIAN_POINT('Origin',(-0.0211577899118759,-0.0165945500931155,
0.00803151208831422));
#63490=CARTESIAN_POINT('',(-0.0184689851345062,-0.0184241814719618,0.08465));
#63491=CARTESIAN_POINT('',(-0.0158972056958818,-0.0201741814719718,0.08290000000001));
#63492=CARTESIAN_POINT('',(-0.0211577899118859,-0.0165945500931255,0.08465000000001));
#63493=CARTESIAN_POINT('',(-0.0184689851345062,-0.0184241814719618,0.06365));
#63494=CARTESIAN_POINT('',(-0.0211577899118859,-0.0165945500931255,0.06365000000001));
#63495=CARTESIAN_POINT('',(-0.0250405557460001,-0.0139524727409137,0.0591782912689519));
#63496=CARTESIAN_POINT('Origin',(-0.0311262178068916,-0.0144741814719618,
0.06365));
#63497=CARTESIAN_POINT('',(0.0021237821931084,-0.0184241814719618,0.06365));
#63498=CARTESIAN_POINT('',(0.00212378219311841,0.0148536964671725,0.06365000000001));
#63499=CARTESIAN_POINT('',(-0.0158972056958819,-0.0184241814719718,0.06365000000001));
#63500=CARTESIAN_POINT('Origin',(-0.0311262178068916,-0.0144741814719618,
0.08465));
#63501=CARTESIAN_POINT('',(0.0021237821931084,-0.0184241814719618,0.08465));
#63502=CARTESIAN_POINT('',(0.0021237821931184,-0.0184241814719718,0.08465000000001));
#63503=CARTESIAN_POINT('',(0.00212378219311841,0.0148536964671725,0.08465000000001));
#63504=CARTESIAN_POINT('Origin',(0.00212378219310841,0.0148536964671625,
0.08465));
#63505=CARTESIAN_POINT('',(0.0021237821931184,-0.0184241814719718,0.08465000000001));
#63506=CARTESIAN_POINT('Origin',(0.0311237821931084,0.0148536964671625,
0.06865));
#63507=CARTESIAN_POINT('',(0.0311237821931184,-0.0184241814719718,0.06865000000001));
#63508=CARTESIAN_POINT('Origin',(0.00787378219310841,0.0230268185280382,
0.07415));
#63509=CARTESIAN_POINT('',(0.00787378219311841,0.0230268185280482,0.07590000000001));
#63510=CARTESIAN_POINT('',(0.00787378219311841,0.0230268185280482,0.07240000000001));
#63511=CARTESIAN_POINT('Origin',(0.00787378219310841,0.0230268185280382,
0.0759));
#63512=CARTESIAN_POINT('Origin',(0.00787378219310841,0.0230268185280382,
0.0724));
#63513=CARTESIAN_POINT('Origin',(-0.0311262178068916,-0.0184241814719618,
0.06365));
#63514=CARTESIAN_POINT('',(0.00200247846971871,-0.0198416853008431,0.0650675038288813));
#63515=CARTESIAN_POINT('Origin',(0.0311237821931084,-0.0184241814719618,
0.06865));
#63516=CARTESIAN_POINT('',(0.0311237821931184,-0.0184241814719718,0.06865000000001));
#63517=CARTESIAN_POINT('Origin',(0.0293737821931084,-0.0201741814719619,
0.00803151208831422));
#63518=CARTESIAN_POINT('',(0.00756730575344765,-0.0419806579116424,0.0598074230640057));
#63519=CARTESIAN_POINT('Origin',(0.0021237821931084,-0.0184241814719618,
0.08465));
#63520=CARTESIAN_POINT('',(0.00212378219311842,-0.0184241814719718,0.08465000000001));
#63521=CARTESIAN_POINT('Origin',(-0.0158972056958719,-0.0201741814719619,
0.0829));
#63522=CARTESIAN_POINT('',(0.,0.,0.));
#63523=CARTESIAN_POINT('Origin',(0.00812378219310841,-0.0355241814719619,
0.07415));
#63524=CARTESIAN_POINT('',(0.00962378219312842,-0.0201741814719718,0.07415000000001));
#63525=CARTESIAN_POINT('Origin',(0.00812378219311841,-0.0201741814719718,
0.07415000000001));
#63526=CARTESIAN_POINT('',(0.00962378219312842,-0.0315241814719718,0.07415000000001));
#63527=CARTESIAN_POINT('',(0.00962378219310841,-0.0355241814719619,0.07415));
#63528=CARTESIAN_POINT('Origin',(0.00812378219311841,-0.0315241814719718,
0.07415000000001));
#63529=CARTESIAN_POINT('Origin',(0.00812378219310841,-0.0320241814719619,
0.07415));
#63530=CARTESIAN_POINT('',(0.00800089067195264,-0.0317744765475852,0.0798989817472979));
#63531=CARTESIAN_POINT('',(0.00812378219307299,-0.031774544307656,0.0799003628356941));
#63532=CARTESIAN_POINT('Ctrl Pts',(0.00812378219303757,-0.031774544307656,
0.0799003628356941));
#63533=CARTESIAN_POINT('Ctrl Pts',(0.00811348867094932,-0.0317744296023842,
0.0799002481304222));
#63534=CARTESIAN_POINT('Ctrl Pts',(0.00810319488311751,-0.0317743418685778,
0.0799001327570061));
#63535=CARTESIAN_POINT('Ctrl Pts',(0.00806223108536668,-0.0317741013472404,
0.0798996722309655));
#63536=CARTESIAN_POINT('Ctrl Pts',(0.00803155944442365,-0.031774163538908,
0.0798993242496632));
#63537=CARTESIAN_POINT('Ctrl Pts',(0.00800089067195264,-0.0317744765475852,
0.079898981747298));
#63538=CARTESIAN_POINT('',(0.00812378219310841,-0.0315241814719669,0.0796500000000049));
#63539=CARTESIAN_POINT('',(0.00812378219310841,-0.0320241814719619,0.08015));
#63540=CARTESIAN_POINT('Origin',(0.00812378219311841,-0.0315241814719718,
0.07415000000001));
#63541=CARTESIAN_POINT('',(0.00818490370815573,-0.0317755400071256,0.0799010337471101));
#63542=CARTESIAN_POINT('Ctrl Pts',(0.00818490370815573,-0.0317755400071257,
0.0799010337471101));
#63543=CARTESIAN_POINT('Ctrl Pts',(0.00816453180595947,-0.0317751040881875,
0.0799008143144595));
#63544=CARTESIAN_POINT('Ctrl Pts',(0.0081441575200755,-0.0317747713589418,
0.0799005898869801));
#63545=CARTESIAN_POINT('Ctrl Pts',(0.00812378219303757,-0.031774544307656,
0.0799003628356941));
#63546=CARTESIAN_POINT('',(0.00836641386969367,-0.0318824481878403,0.0800032400262193));
#63547=CARTESIAN_POINT('Origin',(0.0125782760148201,-0.0332583300628553,
0.0708159433682903));
#63548=CARTESIAN_POINT('',(0.00853918443652277,-0.0317755397360895,0.0798863371607593));
#63549=CARTESIAN_POINT('Origin',(0.00345819158879964,-0.0326853491204495,
0.0717801654791084));
#63550=CARTESIAN_POINT('',(0.00872239818039313,-0.0317744765475852,0.0798690517008071));
#63551=CARTESIAN_POINT('Ctrl Pts',(0.00853918446518101,-0.0317755400678203,
0.0798863373898779));
#63552=CARTESIAN_POINT('Ctrl Pts',(0.00856971630102154,-0.0317748838920054,
0.0798834685041633));
#63553=CARTESIAN_POINT('Ctrl Pts',(0.00860025258788743,-0.0317744615155934,
0.0798805878692076));
#63554=CARTESIAN_POINT('Ctrl Pts',(0.00866132551949298,-0.0317741013465794,
0.079874820213224));
#63555=CARTESIAN_POINT('Ctrl Pts',(0.00869186305200621,-0.0317741635377597,
0.0798719331080806));
#63556=CARTESIAN_POINT('Ctrl Pts',(0.00872239818037093,-0.0317744765473203,
0.0798690517005431));
#63557=CARTESIAN_POINT('',(0.00890521740261619,-0.0317755400071256,0.0798480245711424));
#63558=CARTESIAN_POINT('Ctrl Pts',(0.00872239818039312,-0.0317744765475851,
0.079869051700807));
#63559=CARTESIAN_POINT('Ctrl Pts',(0.00875287145286697,-0.0317741635039241,
0.0798655472943847));
#63560=CARTESIAN_POINT('Ctrl Pts',(0.00878333832390794,-0.0317741013272851,
0.0798620491063663));
#63561=CARTESIAN_POINT('Ctrl Pts',(0.00884428421652555,-0.0317744615102831,
0.0798550449672046));
#63562=CARTESIAN_POINT('Ctrl Pts',(0.00887475419897025,-0.0317748838659619,
0.0798515400556039));
#63563=CARTESIAN_POINT('Ctrl Pts',(0.00890521740261618,-0.0317755400071256,
0.0798480245711423));
#63564=CARTESIAN_POINT('',(0.00909810614576694,-0.0318824481878404,0.0799266756677436));
#63565=CARTESIAN_POINT('Origin',(0.0121252829034405,-0.0332583300636472,
0.070283937281488));
#63566=CARTESIAN_POINT('',(0.00925486255046764,-0.0317755397364823,0.0797890407230367));
#63567=CARTESIAN_POINT('Origin',(0.00319796214065289,-0.0326853491204372,
0.0723836058889708));
#63568=CARTESIAN_POINT('',(0.0094344651571187,-0.0317744765475852,0.0797489287925986));
#63569=CARTESIAN_POINT('Ctrl Pts',(0.00925486260762856,-0.0317755400683138,
0.0797890409468029));
#63570=CARTESIAN_POINT('Ctrl Pts',(0.00928479412963376,-0.0317748838922174,
0.0797823680280026));
#63571=CARTESIAN_POINT('Ctrl Pts',(0.00931472858696256,-0.0317744615158803,
0.0797756828966261));
#63572=CARTESIAN_POINT('Ctrl Pts',(0.00937459705300773,-0.0317741013468556,
0.0797623062541212));
#63573=CARTESIAN_POINT('Ctrl Pts',(0.00940453194095072,-0.0317741635379398,
0.0797556145462587));
#63574=CARTESIAN_POINT('Ctrl Pts',(0.00943446515711872,-0.0317744765475852,
0.0797489287925987));
#63575=CARTESIAN_POINT('',(0.00961320739701597,-0.0317755400071255,0.0797051541438529));
#63576=CARTESIAN_POINT('Ctrl Pts',(0.00943446515711872,-0.0317744765475852,
0.0797489287925987));
#63577=CARTESIAN_POINT('Ctrl Pts',(0.00946425568272709,-0.0317741635379398,
0.0797416334984917));
#63578=CARTESIAN_POINT('Ctrl Pts',(0.00949405034927215,-0.0317741013468556,
0.0797343427978588));
#63579=CARTESIAN_POINT('Ctrl Pts',(0.00955363457623872,-0.0317744615102831,
0.079719756135239));
#63580=CARTESIAN_POINT('Ctrl Pts',(0.0095834250118687,-0.0317748838659621,
0.0797124599594862));
#63581=CARTESIAN_POINT('Ctrl Pts',(0.00961320739701597,-0.0317755400071257,
0.0797051541438529));
#63582=CARTESIAN_POINT('',(0.00981443275107406,-0.0318824481878406,0.0797590096831689));
#63583=CARTESIAN_POINT('Origin',(0.0116091837302405,-0.0332583300607984,
0.0698129013353744));
#63584=CARTESIAN_POINT('',(0.00995270285202925,-0.0317755397364837,0.0796028132440281));
#63585=CARTESIAN_POINT('Origin',(0.00301541581737871,-0.0326853491204465,
0.0730149033892818));
#63586=CARTESIAN_POINT('',(0.0101258618805387,-0.0317744765475852,0.0795405074326928));
#63587=CARTESIAN_POINT('Ctrl Pts',(0.00995270293678456,-0.0317755400683137,
0.0796028134588651));
#63588=CARTESIAN_POINT('Ctrl Pts',(0.00998156209550537,-0.0317748838923493,
0.0795924417456697));
#63589=CARTESIAN_POINT('Ctrl Pts',(0.0100104226445564,-0.0317744615158499,
0.0795820575451456));
#63590=CARTESIAN_POINT('Ctrl Pts',(0.0100681425004938,-0.0317741013467719,
0.079561282869969));
#63591=CARTESIAN_POINT('Ctrl Pts',(0.0100970026465938,-0.0317741635379696,
0.0795508920929727));
#63592=CARTESIAN_POINT('Ctrl Pts',(0.0101258618805387,-0.0317744765475852,
0.0795405074326928));
#63593=CARTESIAN_POINT('',(0.0102977082662106,-0.0317755400071256,0.0794746756172265));
#63594=CARTESIAN_POINT('Ctrl Pts',(0.0101258618805387,-0.0317744765475851,
0.0795405074326927));
#63595=CARTESIAN_POINT('Ctrl Pts',(0.0101545062686811,-0.0317741635039241,
0.0795295347289502));
#63596=CARTESIAN_POINT('Ctrl Pts',(0.0101831460029575,-0.031774101327285,
0.0795185696402207));
#63597=CARTESIAN_POINT('Ctrl Pts',(0.0102404353097176,-0.0317744615102831,
0.079496628921809));
#63598=CARTESIAN_POINT('Ctrl Pts',(0.0102690763855666,-0.0317748838659622,
0.0794856565469538));
#63599=CARTESIAN_POINT('Ctrl Pts',(0.0102977082662106,-0.0317755400071257,
0.0794746756172266));
#63600=CARTESIAN_POINT('',(0.0105040967871363,-0.0318824481878407,0.0795028862652307));
#63601=CARTESIAN_POINT('Origin',(0.0110381176980832,-0.0332583300612685,
0.0694102640075936));
#63602=CARTESIAN_POINT('',(0.0106216999825734,-0.0317755397360894,0.0793305916421598));
#63603=CARTESIAN_POINT('Origin',(0.00291343148364639,-0.0326853491206454,
0.0736641020412303));
#63604=CARTESIAN_POINT('',(0.0107856846113026,-0.0317744765475852,0.0792470745504406));
#63605=CARTESIAN_POINT('Ctrl Pts',(0.0106217000935633,-0.0317755400678203,
0.079330591844639));
#63606=CARTESIAN_POINT('Ctrl Pts',(0.0106490317714279,-0.0317748838919549,
0.0793166849026812));
#63607=CARTESIAN_POINT('Ctrl Pts',(0.0106763632593857,-0.0317744615156049,
0.0793027653996415));
#63608=CARTESIAN_POINT('Ctrl Pts',(0.0107310242162656,-0.0317741013466114,
0.0792749203246661));
#63609=CARTESIAN_POINT('Ctrl Pts',(0.0107583544827035,-0.0317741635377483,
0.0792609943461551));
#63610=CARTESIAN_POINT('Ctrl Pts',(0.0107856846111848,-0.0317744765473203,
0.0792470745502033));
#63611=CARTESIAN_POINT('',(0.010947925022592,-0.0317755400071255,0.0791602237753096));
#63612=CARTESIAN_POINT('Ctrl Pts',(0.0107856846113026,-0.0317744765475852,
0.0792470745504406));
#63613=CARTESIAN_POINT('Ctrl Pts',(0.0108127249443218,-0.0317741635379697,
0.079232599850341));
#63614=CARTESIAN_POINT('Ctrl Pts',(0.0108397704303659,-0.0317741013467719,
0.0792181285696829));
#63615=CARTESIAN_POINT('Ctrl Pts',(0.0108938551617572,-0.0317744615102529,
0.0791891821749494));
#63616=CARTESIAN_POINT('Ctrl Pts',(0.0109208951937506,-0.0317748838660943,
0.0791747066403946));
#63617=CARTESIAN_POINT('Ctrl Pts',(0.010947925022592,-0.0317755400071257,
0.0791602237753096));
#63618=CARTESIAN_POINT('',(0.0111562218401201,-0.031882448187841,0.0791623446332304));
#63619=CARTESIAN_POINT('Origin',(0.0104210908503211,-0.033258330069597,
0.0690823750888361));
#63620=CARTESIAN_POINT('',(0.0112513034569997,-0.0317755397360895,0.0789766690159622));
#63621=CARTESIAN_POINT('Origin',(0.00289361749240266,-0.0326853491202809,
0.0743209635941413));
#63622=CARTESIAN_POINT('',(0.0114035275507881,-0.0317744765475852,0.0788732577576833));
#63623=CARTESIAN_POINT('Ctrl Pts',(0.0112513035924919,-0.0317755400678203,
0.0789766692029341));
#63624=CARTESIAN_POINT('Ctrl Pts',(0.0112766767526801,-0.0317748838918833,
0.0789594463519205));
#63625=CARTESIAN_POINT('Ctrl Pts',(0.0113020481459377,-0.0317744615156214,
0.0789422110655245));
#63626=CARTESIAN_POINT('Ctrl Pts',(0.0113527909245682,-0.0317741013270863,
0.0789077328522199));
#63627=CARTESIAN_POINT('Ctrl Pts',(0.0113781547830805,-0.0317741635037164,
0.0788904950389542));
#63628=CARTESIAN_POINT('Ctrl Pts',(0.0114035275506415,-0.0317744765473203,
0.0788732577574627));
#63629=CARTESIAN_POINT('',(0.0115536033594913,-0.0317755400071255,0.0787667577114933));
#63630=CARTESIAN_POINT('Ctrl Pts',(0.0114035275507881,-0.0317744765475852,
0.0788732577576833));
#63631=CARTESIAN_POINT('Ctrl Pts',(0.0114285405028257,-0.031774163537956,
0.0788555081417705));
#63632=CARTESIAN_POINT('Ctrl Pts',(0.0114535589958953,-0.0317741013468101,
0.0788377612724408));
#63633=CARTESIAN_POINT('Ctrl Pts',(0.0115035893044095,-0.0317744615102667,
0.0788022645167903));
#63634=CARTESIAN_POINT('Ctrl Pts',(0.011528601850937,-0.0317748838660339,
0.0787845141123455));
#63635=CARTESIAN_POINT('Ctrl Pts',(0.0115536033594913,-0.0317755400071257,
0.0787667577114933));
#63636=CARTESIAN_POINT('',(0.0117605235083789,-0.0318824481878413,0.0787427553321347));
#63637=CARTESIAN_POINT('Origin',(0.00976783406872409,-0.0332583300697538,
0.0688344057025907));
#63638=CARTESIAN_POINT('',(0.0118315840528038,-0.0317755397360895,0.0785466269360707));
#63639=CARTESIAN_POINT('Origin',(0.00295628632343493,-0.0326853491203905,
0.0749751289491354));
#63640=CARTESIAN_POINT('',(0.0119696469467589,-0.0317744765475852,0.0784249523685494));
#63641=CARTESIAN_POINT('Ctrl Pts',(0.0118315842106613,-0.0317755400678203,
0.0785466271045866));
#63642=CARTESIAN_POINT('Ctrl Pts',(0.0118545986960121,-0.0317748838920054,
0.0785263599644561));
#63643=CARTESIAN_POINT('Ctrl Pts',(0.0118776098762876,-0.0317744615155934,
0.0785060807027428));
#63644=CARTESIAN_POINT('Ctrl Pts',(0.0119236287727241,-0.0317741013465795,
0.0784655168025234));
#63645=CARTESIAN_POINT('Ctrl Pts',(0.0119466371576691,-0.0317741635377597,
0.0784452315741446));
#63646=CARTESIAN_POINT('Ctrl Pts',(0.0119696469465858,-0.0317744765473203,
0.0784249523683489));
#63647=CARTESIAN_POINT('',(0.0121051913677208,-0.0317755400071256,0.0783004826206495));
#63648=CARTESIAN_POINT('Ctrl Pts',(0.0119696469467589,-0.0317744765475852,
0.0784249523685494));
#63649=CARTESIAN_POINT('Ctrl Pts',(0.0119922405024809,-0.0317741635039404,
0.0784042055051241));
#63650=CARTESIAN_POINT('Ctrl Pts',(0.0120148325343447,-0.0317741013272396,
0.0783834674352309));
#63651=CARTESIAN_POINT('Ctrl Pts',(0.0120600218711234,-0.0317744615102667,
0.0783419778674282));
#63652=CARTESIAN_POINT('Ctrl Pts',(0.0120826124706645,-0.0317748838660339,
0.0783212325268882));
#63653=CARTESIAN_POINT('Ctrl Pts',(0.0121051913677208,-0.0317755400071257,
0.0783004826206495));
#63654=CARTESIAN_POINT('',(0.0123074715936121,-0.0318824481878415,0.078250735535872));
#63655=CARTESIAN_POINT('Origin',(0.00908864960674653,-0.0332583300699432,
0.0686702664128971));
#63656=CARTESIAN_POINT('',(0.012353390398347,-0.0317755397360894,0.0780472474229795));
#63657=CARTESIAN_POINT('Origin',(0.00310044965113113,-0.0326853491203657,
0.0756162815277102));
#63658=CARTESIAN_POINT('',(0.0124751147581572,-0.0317744765475852,0.0779092284268295));
#63659=CARTESIAN_POINT('Ctrl Pts',(0.0123533905760804,-0.0317755400678203,
0.0780472475703818));
#63660=CARTESIAN_POINT('Ctrl Pts',(0.0123736834429088,-0.0317748838918832,
0.0780242557585583));
#63661=CARTESIAN_POINT('Ctrl Pts',(0.0123939715057635,-0.0317744615156213,
0.0780012523414514));
#63662=CARTESIAN_POINT('Ctrl Pts',(0.0124345457237183,-0.0317741013270862,
0.0779552381087258));
#63663=CARTESIAN_POINT('Ctrl Pts',(0.0124548258601386,-0.0317741635037164,
0.0779322341179504));
#63664=CARTESIAN_POINT('Ctrl Pts',(0.0124751147579603,-0.0317744765473203,
0.0779092284266523));
#63665=CARTESIAN_POINT('',(0.0125939901748882,-0.0317755400071256,0.0777687519394998));
#63666=CARTESIAN_POINT('Ctrl Pts',(0.0124751147581572,-0.0317744765475852,
0.0779092284268295));
#63667=CARTESIAN_POINT('Ctrl Pts',(0.0124949277333584,-0.0317741635379398,
0.0778858159783074));
#63668=CARTESIAN_POINT('Ctrl Pts',(0.0125147467586242,-0.0317741013468556,
0.0778624048120024));
#63669=CARTESIAN_POINT('Ctrl Pts',(0.0125543775856657,-0.0317744615102831,
0.0778155812241751));
#63670=CARTESIAN_POINT('Ctrl Pts',(0.012574189969852,-0.0317748838659619,
0.0777921681152774));
#63671=CARTESIAN_POINT('Ctrl Pts',(0.0125939901748881,-0.0317755400071256,
0.0777687519394998));
#63672=CARTESIAN_POINT('',(0.0127884403977845,-0.0318824481878419,0.0776940446905479));
#63673=CARTESIAN_POINT('Origin',(0.00839424863624071,-0.0332583300607026,
0.0685925458525311));
#63674=CARTESIAN_POINT('',(0.0128084932958481,-0.0317755397360895,0.0774864059899253));
#63675=CARTESIAN_POINT('Origin',(0.00332383393396606,-0.0326853491205201,
0.0762343099705962));
#63676=CARTESIAN_POINT('',(0.0129119594556425,-0.0317744765475852,0.0773342192071665));
#63677=CARTESIAN_POINT('Ctrl Pts',(0.0128084934906545,-0.0317755400678204,
0.0774864061138895));
#63678=CARTESIAN_POINT('Ctrl Pts',(0.0128257447040448,-0.0317748838918833,
0.0774610522287524));
#63679=CARTESIAN_POINT('Ctrl Pts',(0.0128429896968152,-0.0317744615156214,
0.0774356874319397));
#63680=CARTESIAN_POINT('Ctrl Pts',(0.0128774768623651,-0.0317741013270863,
0.0773849507372473));
#63681=CARTESIAN_POINT('Ctrl Pts',(0.0128947139193034,-0.0317741635037164,
0.0773595863647356));
#63682=CARTESIAN_POINT('Ctrl Pts',(0.012911959455425,-0.0317744765473203,
0.0773342192070154));
#63683=CARTESIAN_POINT('',(0.01301229113181,-0.0317755400071255,0.0771799513785266));
#63684=CARTESIAN_POINT('Ctrl Pts',(0.0129119594556425,-0.0317744765475851,
0.0773342192071665));
#63685=CARTESIAN_POINT('Ctrl Pts',(0.0129286836574135,-0.031774163503954,
0.0773085053569013));
#63686=CARTESIAN_POINT('Ctrl Pts',(0.0129454085700161,-0.0317741013272014,
0.0772828004029442));
#63687=CARTESIAN_POINT('Ctrl Pts',(0.0129788601669899,-0.0317744615102528,
0.0772313761716959));
#63688=CARTESIAN_POINT('Ctrl Pts',(0.0129955818856934,-0.0317748838660939,
0.0772056645293147));
#63689=CARTESIAN_POINT('Ctrl Pts',(0.01301229113181,-0.0317755400071256,
0.0771799513785267));
#63690=CARTESIAN_POINT('',(0.0131958447555375,-0.0318824481878423,0.0770814621433442));
#63691=CARTESIAN_POINT('Origin',(0.00769558219568638,-0.0332583300696311,
0.0686024695523869));
#63692=CARTESIAN_POINT('',(0.0131897155007483,-0.0317755397360896,0.0768729474413377));
#63693=CARTESIAN_POINT('Origin',(0.00362291626787834,-0.0326853491204316,
0.076819467600236));
#63694=CARTESIAN_POINT('',(0.0132732917373798,-0.0317744765475852,0.0767089929484456));
#63695=CARTESIAN_POINT('Ctrl Pts',(0.0131897157095554,-0.0317755400678204,
0.0768729475399086));
#63696=CARTESIAN_POINT('Ctrl Pts',(0.0132036532060474,-0.031774883891955,
0.0768456314303515));
#63697=CARTESIAN_POINT('Ctrl Pts',(0.0132175831656799,-0.031774461515605,
0.0768183052702963));
#63698=CARTESIAN_POINT('Ctrl Pts',(0.0132454393978449,-0.031774101327041,
0.0767636462572597));
#63699=CARTESIAN_POINT('Ctrl Pts',(0.0132593615358501,-0.0317741635037326,
0.0767363215158222));
#63700=CARTESIAN_POINT('Ctrl Pts',(0.0132732917371451,-0.0317744765473204,
0.076708992948323));
#63701=CARTESIAN_POINT('',(0.0133534973825149,-0.0317755400071256,0.0765433666743088));
#63702=CARTESIAN_POINT('Ctrl Pts',(0.0132732917373799,-0.0317744765475852,
0.0767089929484456));
#63703=CARTESIAN_POINT('Ctrl Pts',(0.0132866612644048,-0.0317741635039404,
0.076681385760083));
#63704=CARTESIAN_POINT('Ctrl Pts',(0.0133000326116973,-0.0317741013272397,
0.0766537873087095));
#63705=CARTESIAN_POINT('Ctrl Pts',(0.0133267752658551,-0.0317744615102666,
0.0765985759797762));
#63706=CARTESIAN_POINT('Ctrl Pts',(0.0133401426049004,-0.0317748838660336,
0.0765709712956067));
#63707=CARTESIAN_POINT('Ctrl Pts',(0.0133534973825149,-0.0317755400071256,
0.0765433666743088));
#63708=CARTESIAN_POINT('',(0.0135232596567777,-0.0318824481878426,0.0764226486869691));
#63709=CARTESIAN_POINT('Origin',(0.0070036687906888,-0.0332583300606654,
0.0686998812247189));
#63710=CARTESIAN_POINT('',(0.0134910449111451,-0.0317755397360896,0.0762165463849901));
#63711=CARTESIAN_POINT('Origin',(0.00399297994630453,-0.0326853491203843,
0.0773625261311474));
#63712=CARTESIAN_POINT('',(0.0135534131774357,-0.0317744765475852,0.0760434098422606));
#63713=CARTESIAN_POINT('Ctrl Pts',(0.0134910451306599,-0.0317755400678204,
0.0762165464566133));
#63714=CARTESIAN_POINT('Ctrl Pts',(0.0135014491094886,-0.031774883891955,
0.0761876989112398));
#63715=CARTESIAN_POINT('Ctrl Pts',(0.0135118443512286,-0.031774461515605,
0.0761588423392328));
#63716=CARTESIAN_POINT('Ctrl Pts',(0.0135326303378373,-0.0317741013270409,
0.0761011230171825));
#63717=CARTESIAN_POINT('Ctrl Pts',(0.0135430179974245,-0.0317741635037327,
0.0760722688329206));
#63718=CARTESIAN_POINT('Ctrl Pts',(0.0135534131771875,-0.0317744765473204,
0.0760434098421683));
#63719=CARTESIAN_POINT('',(0.0136122279006024,-0.0317755400071255,0.0758690371479093));
#63720=CARTESIAN_POINT('Ctrl Pts',(0.0135534131774357,-0.0317744765475851,
0.0760434098422606));
#63721=CARTESIAN_POINT('Ctrl Pts',(0.0135632161178193,-0.0317741635379696,
0.076014347858285));
#63722=CARTESIAN_POINT('Ctrl Pts',(0.0135730251553652,-0.0317741013467718,
0.0759852848394868));
#63723=CARTESIAN_POINT('Ctrl Pts',(0.0135926360570299,-0.0317744615102528,
0.0759271602795009));
#63724=CARTESIAN_POINT('Ctrl Pts',(0.0136024382067509,-0.0317748838660941,
0.0758980978933012));
#63725=CARTESIAN_POINT('Ctrl Pts',(0.0136122279006023,-0.0317755400071256,
0.0758690371479093));
#63726=CARTESIAN_POINT('',(0.0137655215729243,-0.031882448187843,0.075727994203186));
#63727=CARTESIAN_POINT('Origin',(0.0063294202056316,-0.0332583300615265,
0.068883244469716));
#63728=CARTESIAN_POINT('',(0.0137077293822312,-0.0317755397360894,0.0755275546576563));
#63729=CARTESIAN_POINT('Origin',(0.00442818884366834,-0.0326853491202104,
0.0778549212059884));
#63730=CARTESIAN_POINT('',(0.0137479060933655,-0.0317744765475852,0.075347966531792));
#63731=CARTESIAN_POINT('Ctrl Pts',(0.0137077296089918,-0.0317755400678203,
0.0755275547012022));
#63732=CARTESIAN_POINT('Ctrl Pts',(0.0137144359939304,-0.0317748838918833,
0.0754976306597627));
#63733=CARTESIAN_POINT('Ctrl Pts',(0.013721132578227,-0.0317744615156214,
0.0754676987628676));
#63734=CARTESIAN_POINT('Ctrl Pts',(0.0137345205107817,-0.0317741013270863,
0.0754078294047801));
#63735=CARTESIAN_POINT('Ctrl Pts',(0.0137412098727239,-0.0317741635037165,
0.0753779008237642));
#63736=CARTESIAN_POINT('Ctrl Pts',(0.0137479060931077,-0.0317744765473204,
0.0753479665317316));
#63737=CARTESIAN_POINT('',(0.0137844023512441,-0.0317755400071256,0.0751675973787842));
#63738=CARTESIAN_POINT('Ctrl Pts',(0.0137479060933655,-0.0317744765475852,
0.075347966531792));
#63739=CARTESIAN_POINT('Ctrl Pts',(0.0137539893027907,-0.0317741635379398,
0.075317905073158));
#63740=CARTESIAN_POINT('Ctrl Pts',(0.0137600784316405,-0.0317741013468556,
0.0752878418234986));
#63741=CARTESIAN_POINT('Ctrl Pts',(0.0137722497546434,-0.0317744615102831,
0.0752277177041611));
#63742=CARTESIAN_POINT('Ctrl Pts',(0.013778332128021,-0.0317748838659621,
0.0751976559515538));
#63743=CARTESIAN_POINT('Ctrl Pts',(0.0137844023512441,-0.0317755400071257,
0.0751675973787842));
#63744=CARTESIAN_POINT('',(0.0139188098888395,-0.0318824481878434,0.0750084538081706));
#63745=CARTESIAN_POINT('Origin',(0.00568346973988991,-0.0332583300694759,
0.0691496675676217));
#63746=CARTESIAN_POINT('',(0.0138363516704564,-0.0317755397360895,0.0748168380704599));
#63747=CARTESIAN_POINT('Origin',(0.00492167945582895,-0.032685349120183,
0.0782888874601413));
#63748=CARTESIAN_POINT('',(0.0138537032156988,-0.0317744765475852,0.0746336305734897));
#63749=CARTESIAN_POINT('Ctrl Pts',(0.0138363519008867,-0.0317755400678203,
0.0748168380852418));
#63750=CARTESIAN_POINT('Ctrl Pts',(0.0138392549267852,-0.0317748838919549,
0.0747863094742291));
#63751=CARTESIAN_POINT('Ctrl Pts',(0.013842147245254,-0.031774461515605,
0.0747557742930014));
#63752=CARTESIAN_POINT('Ctrl Pts',(0.0138479259901821,-0.0317741013270409,
0.0746946990649327));
#63753=CARTESIAN_POINT('Ctrl Pts',(0.0138508115585138,-0.0317741635037327,
0.074664168082036));
#63754=CARTESIAN_POINT('Ctrl Pts',(0.0138537032154354,-0.0317744765473203,
0.074633630573462));
#63755=CARTESIAN_POINT('',(0.0138673054405015,-0.0317755400071255,0.0744501094911124));
#63756=CARTESIAN_POINT('Ctrl Pts',(0.0138537032156987,-0.0317744765475851,
0.0746336305734897));
#63757=CARTESIAN_POINT('Ctrl Pts',(0.0138559710036869,-0.0317741635039403,
0.0746030404077552));
#63758=CARTESIAN_POINT('Ctrl Pts',(0.0138582437004173,-0.0317741013272395,
0.0745724576953827));
#63759=CARTESIAN_POINT('Ctrl Pts',(0.0138627837456575,-0.0317744615102666,
0.0745112788723768));
#63760=CARTESIAN_POINT('Ctrl Pts',(0.0138650504211692,-0.0317748838660337,
0.0744806918404243));
#63761=CARTESIAN_POINT('Ctrl Pts',(0.0138673054405015,-0.0317755400071256,
0.0744501094911124));
#63762=CARTESIAN_POINT('',(0.0139807071562112,-0.0318824481878437,0.074275375083785));
#63763=CARTESIAN_POINT('Origin',(0.00507600449970732,-0.0332583300693116,
0.0694949489328749));
#63764=CARTESIAN_POINT('',(0.0138748833255002,-0.0317755397360895,0.0740956050485428));
#63765=CARTESIAN_POINT('Origin',(0.00546566914113827,-0.0326853491204145,
0.078657580986387));
#63766=CARTESIAN_POINT('',(0.0138691360606172,-0.0317744765475852,0.0739116674721342));
#63767=CARTESIAN_POINT('Ctrl Pts',(0.0138748835559661,-0.0317755400678203,
0.0740956050343276));
#63768=CARTESIAN_POINT('Ctrl Pts',(0.0138739374410007,-0.0317748838918833,
0.074064953301563));
#63769=CARTESIAN_POINT('Ctrl Pts',(0.0138729798797259,-0.0317744615156214,
0.0740342963974567));
#63770=CARTESIAN_POINT('Ctrl Pts',(0.0138710584062604,-0.0317741013466568,
0.0739729818335607));
#63771=CARTESIAN_POINT('Ctrl Pts',(0.0138700944656008,-0.0317741635377321,
0.0739423232741826));
#63772=CARTESIAN_POINT('Ctrl Pts',(0.0138691360603524,-0.0317744765473203,
0.0739116674721398));
#63773=CARTESIAN_POINT('',(0.013859629737133,-0.0317755400071255,0.0737278886974891));
#63774=CARTESIAN_POINT('Ctrl Pts',(0.0138691360606172,-0.0317744765475852,
0.0739116674721342));
#63775=CARTESIAN_POINT('Ctrl Pts',(0.0138675521742271,-0.0317741635379696,
0.0738810376197538));
#63776=CARTESIAN_POINT('Ctrl Pts',(0.0138659735758916,-0.031774101346772,
0.0738504045607044));
#63777=CARTESIAN_POINT('Ctrl Pts',(0.0138628102534823,-0.0317744615102528,
0.0737891424571854));
#63778=CARTESIAN_POINT('Ctrl Pts',(0.0138612254838846,-0.0317748838660939,
0.0737585125218971));
#63779=CARTESIAN_POINT('Ctrl Pts',(0.013859629737133,-0.0317755400071256,
0.0737278886974891));
#63780=CARTESIAN_POINT('',(0.0139502372181573,-0.0318824481878442,0.0735403191194324));
#63781=CARTESIAN_POINT('Origin',(0.00451660453409808,-0.0332583300694264,
0.0699136432343077));
#63782=CARTESIAN_POINT('',(0.013822716680145,-0.0317755397360895,0.073375229867504));
#63783=CARTESIAN_POINT('Origin',(0.00605157885713282,-0.032685349120609,
0.0789551872677681));
#63784=CARTESIAN_POINT('',(0.0137939612429368,-0.0317744765475852,0.0731934630171163));
#63785=CARTESIAN_POINT('Ctrl Pts',(0.013822716907012,-0.0317755400678204,
0.0733752298245158));
#63786=CARTESIAN_POINT('Ctrl Pts',(0.0138179365721851,-0.0317748838919549,
0.0733449383727703));
#63787=CARTESIAN_POINT('Ctrl Pts',(0.0138131442323767,-0.031774461515605,
0.0733146432200586));
#63788=CARTESIAN_POINT('Ctrl Pts',(0.0138035526358299,-0.0317741013270409,
0.0732540496671673));
#63789=CARTESIAN_POINT('Ctrl Pts',(0.0137987548020344,-0.0317741635037326,
0.0732237602595771));
#63790=CARTESIAN_POINT('Ctrl Pts',(0.0137939612426747,-0.0317744765473203,
0.073193463017155));
#63791=CARTESIAN_POINT('',(0.0137614962915661,-0.0317755400071256,0.0730123248512634));
#63792=CARTESIAN_POINT('Ctrl Pts',(0.0137939612429368,-0.0317744765475851,
0.0731934630171163));
#63793=CARTESIAN_POINT('Ctrl Pts',(0.0137885503195655,-0.031774163503954,
0.0731632699230634));
#63794=CARTESIAN_POINT('Ctrl Pts',(0.0137831460043102,-0.0317741013272014,
0.0731330828275425));
#63795=CARTESIAN_POINT('Ctrl Pts',(0.0137723288603643,-0.0317744615102528,
0.0730726969823686));
#63796=CARTESIAN_POINT('Ctrl Pts',(0.0137669176383144,-0.031774883866094,
0.0730425071975653));
#63797=CARTESIAN_POINT('Ctrl Pts',(0.013761496291566,-0.0317755400071256,
0.0730123248512635));
#63798=CARTESIAN_POINT('',(0.0138278806038027,-0.0318824481878444,0.0728148781867722));
#63799=CARTESIAN_POINT('Origin',(0.00401409197564931,-0.0332583300606848,
0.0703991474283218));
#63800=CARTESIAN_POINT('',(0.0136806744335506,-0.0317755397360895,0.0726670732742799));
#63801=CARTESIAN_POINT('Origin',(0.00667016845759922,-0.0326853491205027,
0.0791770128756238));
#63802=CARTESIAN_POINT('',(0.01362936431444,-0.0317744765475852,0.072490343721727));
#63803=CARTESIAN_POINT('Ctrl Pts',(0.0136806746532409,-0.0317755400678203,
0.0726670732031967));
#63804=CARTESIAN_POINT('Ctrl Pts',(0.0136721354862546,-0.0317748838918833,
0.0726376197402067));
#63805=CARTESIAN_POINT('Ctrl Pts',(0.0136635839465049,-0.0317744615156214,
0.0726081641149218));
#63806=CARTESIAN_POINT('Ctrl Pts',(0.0136464745276844,-0.0317741013466568,
0.072549253711818));
#63807=CARTESIAN_POINT('Ctrl Pts',(0.013637916397321,-0.0317741635377321,
0.0725197980697543));
#63808=CARTESIAN_POINT('Ctrl Pts',(0.0136293643141849,-0.0317744765473204,
0.0724903437217983));
#63809=CARTESIAN_POINT('',(0.0135744527268592,-0.0317755400071255,0.0723147028217476));
#63810=CARTESIAN_POINT('Ctrl Pts',(0.01362936431444,-0.0317744765475851,
0.072490343721727));
#63811=CARTESIAN_POINT('Ctrl Pts',(0.0136202118588346,-0.0317741635039241,
0.0724610668749721));
#63812=CARTESIAN_POINT('Ctrl Pts',(0.0136110667109972,-0.031774101327285,
0.0724317951510505));
#63813=CARTESIAN_POINT('Ctrl Pts',(0.0135927665129182,-0.031774461510283,
0.0723732412225488));
#63814=CARTESIAN_POINT('Ctrl Pts',(0.0135836141775723,-0.0317748838659619,
0.0723439677022079));
#63815=CARTESIAN_POINT('Ctrl Pts',(0.0135744527268593,-0.0317755400071256,
0.0723147028217477));
#63816=CARTESIAN_POINT('',(0.0136155669500483,-0.0318824481878448,0.0721104929226697));
#63817=CARTESIAN_POINT('Origin',(0.00357639162872483,-0.0332583300605841,
0.0709438047849521));
#63818=CARTESIAN_POINT('',(0.0134509966767981,-0.0317755397360895,0.0719823033213779));
#63819=CARTESIAN_POINT('Origin',(0.00731168241481123,-0.0326853491200009,
0.0793195594880205));
#63820=CARTESIAN_POINT('',(0.0133779410670143,-0.0317744765475852,0.0718133981972761));
#63821=CARTESIAN_POINT('Ctrl Pts',(0.0134509968858469,-0.0317755400678204,
0.0719823032233207));
#63822=CARTESIAN_POINT('Ctrl Pts',(0.0134388335549863,-0.0317748838918833,
0.0719541522510933));
#63823=CARTESIAN_POINT('Ctrl Pts',(0.0134266576779183,-0.0317744615156214,
0.0719260006843409));
#63824=CARTESIAN_POINT('Ctrl Pts',(0.0134022984171264,-0.0317741013270863,
0.0718696961268912));
#63825=CARTESIAN_POINT('Ctrl Pts',(0.0133901186460761,-0.0317741635037165,
0.0718415514879352));
#63826=CARTESIAN_POINT('Ctrl Pts',(0.0133779410667702,-0.0317744765473203,
0.0718133981973787));
#63827=CARTESIAN_POINT('',(0.0133014488317624,-0.0317755400071256,0.0716460245250861));
#63828=CARTESIAN_POINT('Ctrl Pts',(0.0133779410670143,-0.0317744765475851,
0.0718133981972761));
#63829=CARTESIAN_POINT('Ctrl Pts',(0.0133651928047721,-0.0317741635379398,
0.0717855023455787));
#63830=CARTESIAN_POINT('Ctrl Pts',(0.0133524482787067,-0.0317741013468555,
0.0717576015655608));
#63831=CARTESIAN_POINT('Ctrl Pts',(0.013326955015208,-0.031774461510283,
0.0717018060070864));
#63832=CARTESIAN_POINT('Ctrl Pts',(0.0133142059037977,-0.0317748838659619,
0.07167391040898));
#63833=CARTESIAN_POINT('Ctrl Pts',(0.0133014488317624,-0.0317755400071256,
0.0716460245250861));
#63834=CARTESIAN_POINT('',(0.0133166445700436,-0.0318824481878451,0.0714382719035195));
#63835=CARTESIAN_POINT('Origin',(0.00321040634813816,-0.0332583300608944,
0.0715390257557646));
#63836=CARTESIAN_POINT('',(0.0131373055653141,-0.0317755397360895,0.071331719240017));
#63837=CARTESIAN_POINT('Origin',(0.00796600367088492,-0.0326853491205882,
0.0793805790579488));
#63838=CARTESIAN_POINT('',(0.0130436565954646,-0.0317744765475852,0.0711733022790721));
#63839=CARTESIAN_POINT('Ctrl Pts',(0.0131373057604247,-0.0317755400678204,
0.0713317191165323));
#63840=CARTESIAN_POINT('Ctrl Pts',(0.013121710088684,-0.0317748838918834,
0.0713053145927175));
#63841=CARTESIAN_POINT('Ctrl Pts',(0.0131061018951522,-0.0317744615156214,
0.0712789110515214));
#63842=CARTESIAN_POINT('Ctrl Pts',(0.0130748778821574,-0.0317741013270863,
0.0712261034972461));
#63843=CARTESIAN_POINT('Ctrl Pts',(0.013059266693632,-0.0317741635037165,
0.0711997073172645));
#63844=CARTESIAN_POINT('Ctrl Pts',(0.0130436565952352,-0.0317744765473204,
0.0711733022792046));
#63845=CARTESIAN_POINT('',(0.0129467900407859,-0.0317755400071255,0.0710168354174665));
#63846=CARTESIAN_POINT('Ctrl Pts',(0.0130436565954646,-0.0317744765475852,
0.0711733022790721));
#63847=CARTESIAN_POINT('Ctrl Pts',(0.0130275108253663,-0.0317741635039242,
0.0711472213414462));
#63848=CARTESIAN_POINT('Ctrl Pts',(0.0130113734074458,-0.031774101327285,
0.0711211435483423));
#63849=CARTESIAN_POINT('Ctrl Pts',(0.0129790863738693,-0.0317744615102831,
0.0710689802733736));
#63850=CARTESIAN_POINT('Ctrl Pts',(0.0129629415474981,-0.0317748838659619,
0.0710429025277493));
#63851=CARTESIAN_POINT('Ctrl Pts',(0.0129467900407859,-0.0317755400071256,
0.0710168354174665));
#63852=CARTESIAN_POINT('',(0.012935827648289,-0.0318824481878454,0.0708088164563586));
#63853=CARTESIAN_POINT('Origin',(0.00292190787764685,-0.033258330069175,
0.0721754233574242));
#63854=CARTESIAN_POINT('',(0.0127445481953167,-0.0317755397360895,0.0707255811298004));
#63855=CARTESIAN_POINT('Origin',(0.00862281318846725,-0.0326853491205626,
0.0793591092720414));
#63856=CARTESIAN_POINT('',(0.0126317827655993,-0.0317744765475852,0.0705801506621206));
#63857=CARTESIAN_POINT('Ctrl Pts',(0.012744548373412,-0.0317755400678204,
0.0707255809828356));
#63858=CARTESIAN_POINT('Ctrl Pts',(0.0127257663158992,-0.0317748838919549,
0.0707013393251905));
#63859=CARTESIAN_POINT('Ctrl Pts',(0.0127069719553852,-0.031774461515605,
0.0706771002078058));
#63860=CARTESIAN_POINT('Ctrl Pts',(0.0126693756085247,-0.0317741013270409,
0.0706286224595139));
#63861=CARTESIAN_POINT('Ctrl Pts',(0.0126505792013278,-0.0317741635037326,
0.0706043910233677));
#63862=CARTESIAN_POINT('Ctrl Pts',(0.0126317827653884,-0.0317744765473203,
0.0705801506622807));
#63863=CARTESIAN_POINT('',(0.0125160695349263,-0.0317755400071255,0.0704370581869752));
#63864=CARTESIAN_POINT('Ctrl Pts',(0.0126317827655993,-0.0317744765475851,
0.0705801506621206));
#63865=CARTESIAN_POINT('Ctrl Pts',(0.0126124975990844,-0.0317741635379696,
0.0705563015760721));
#63866=CARTESIAN_POINT('Ctrl Pts',(0.0125932148258627,-0.0317741013467719,
0.0705324467875334));
#63867=CARTESIAN_POINT('Ctrl Pts',(0.0125546466832984,-0.0317744615102529,
0.0704847440589314));
#63868=CARTESIAN_POINT('Ctrl Pts',(0.0125353607535185,-0.0317748838660941,
0.0704608954249417));
#63869=CARTESIAN_POINT('Ctrl Pts',(0.0125160695349263,-0.0317755400071257,
0.0704370581869752));
#63870=CARTESIAN_POINT('',(0.0124791218951295,-0.0318824481878456,0.0702320534696074));
#63871=CARTESIAN_POINT('Origin',(0.00271544613521357,-0.0332583300697618,
0.0728429612128157));
#63872=CARTESIAN_POINT('',(0.0122789185851526,-0.0317755397360895,0.0701734481508155));
#63873=CARTESIAN_POINT('Origin',(0.00927175268908372,-0.0326853491204069,
0.079255488721487));
#63874=CARTESIAN_POINT('',(0.012148815073757,-0.0317744765475852,0.0700432977017521));
#63875=CARTESIAN_POINT('Ctrl Pts',(0.012278918743424,-0.0317755400678203,
0.0701734479826883));
#63876=CARTESIAN_POINT('Ctrl Pts',(0.0122572465003417,-0.0317748838918833,
0.0701517514913895));
#63877=CARTESIAN_POINT('Ctrl Pts',(0.0122355623732302,-0.0317744615156213,
0.0701300590658809));
#63878=CARTESIAN_POINT('Ctrl Pts',(0.012192186615306,-0.0317741013270862,
0.0700866756542975));
#63879=CARTESIAN_POINT('Ctrl Pts',(0.012170501417954,-0.0317741635037164,
0.0700649911035623));
#63880=CARTESIAN_POINT('Ctrl Pts',(0.0121488150735677,-0.0317744765473202,
0.0700432977019375));
#63881=CARTESIAN_POINT('',(0.0120160800338609,-0.0317755400071255,0.0699158362668794));
#63882=CARTESIAN_POINT('Ctrl Pts',(0.012148815073757,-0.0317744765475851,
0.0700432977017521));
#63883=CARTESIAN_POINT('Ctrl Pts',(0.0121266928934662,-0.0317741635379696,
0.0700220537451477));
#63884=CARTESIAN_POINT('Ctrl Pts',(0.0121045723728852,-0.031774101346772,
0.0700008038310598));
#63885=CARTESIAN_POINT('Ctrl Pts',(0.0120603296144284,-0.0317744615102528,
0.0699583111227498));
#63886=CARTESIAN_POINT('Ctrl Pts',(0.0120382067335565,-0.0317748838660938,
0.0699370677103091));
#63887=CARTESIAN_POINT('Ctrl Pts',(0.012016080033861,-0.0317755400071257,
0.0699158362668794));
#63888=CARTESIAN_POINT('',(0.0119537298331154,-0.0318824481878458,0.0697170788401083));
#63889=CARTESIAN_POINT('Origin',(0.0025942770824451,-0.0332583300694133,
0.0735311118503182));
#63890=CARTESIAN_POINT('',(0.0117477599919279,-0.0317755397360895,0.0696840277699691));
#63891=CARTESIAN_POINT('Origin',(0.00990258800930164,-0.0326853491203117,
0.0790713515635572));
#63892=CARTESIAN_POINT('',(0.0116023702089484,-0.0317744765475852,0.0695712098898517));
#63893=CARTESIAN_POINT('Ctrl Pts',(0.0117477601278794,-0.0317755400678204,
0.069684027583331));
#63894=CARTESIAN_POINT('Ctrl Pts',(0.011723539485495,-0.0317748838918833,
0.0696652184276502));
#63895=CARTESIAN_POINT('Ctrl Pts',(0.0116993075623698,-0.0317744615156214,
0.069646414795164));
#63896=CARTESIAN_POINT('Ctrl Pts',(0.0116508364519961,-0.0317741013270863,
0.0696088098987382));
#63897=CARTESIAN_POINT('Ctrl Pts',(0.0116266044540401,-0.0317741635037165,
0.0695900142130668));
#63898=CARTESIAN_POINT('Ctrl Pts',(0.0116023702087839,-0.0317744765473203,
0.0695712098900593));
#63899=CARTESIAN_POINT('',(0.0114547066707008,-0.0317755400071255,0.0694613896382215));
#63900=CARTESIAN_POINT('Ctrl Pts',(0.0116023702089483,-0.0317744765475851,
0.0695712098898518));
#63901=CARTESIAN_POINT('Ctrl Pts',(0.0115777572180677,-0.0317741635039241,
0.0695529041017128));
#63902=CARTESIAN_POINT('Ctrl Pts',(0.0115531531504213,-0.031774101327285,
0.0695345981626347));
#63903=CARTESIAN_POINT('Ctrl Pts',(0.0115039308435332,-0.0317744615102831,
0.0694979836259309));
#63904=CARTESIAN_POINT('Ctrl Pts',(0.0114793199051569,-0.0317748838659621,
0.0694796804582271));
#63905=CARTESIAN_POINT('Ctrl Pts',(0.0114547066707008,-0.0317755400071257,
0.0694613896382215));
#63906=CARTESIAN_POINT('',(0.0113679372089185,-0.0318824481878459,0.0692720140253997));
#63907=CARTESIAN_POINT('Origin',(0.00256031164226087,-0.0332583300673947,
0.0742290227164587));
#63908=CARTESIAN_POINT('',(0.0111594491039563,-0.0317755397360895,0.0692650384390329));
#63909=CARTESIAN_POINT('Origin',(0.0105053704991273,-0.0326853491202493,
0.078809601752004));
#63910=CARTESIAN_POINT('',(0.0110010659331233,-0.0317744765475852,0.0691713323332258));
#63911=CARTESIAN_POINT('Ctrl Pts',(0.0111594492154439,-0.0317755400678204,
0.0692650382368272));
#63912=CARTESIAN_POINT('Ctrl Pts',(0.0111330621477567,-0.0317748838918834,
0.0692494130483858));
#63913=CARTESIAN_POINT('Ctrl Pts',(0.0111066645805211,-0.0317744615156214,
0.0692337947534391));
#63914=CARTESIAN_POINT('Ctrl Pts',(0.0110538625360635,-0.0317741013270863,
0.0692025614238513));
#63915=CARTESIAN_POINT('Ctrl Pts',(0.0110274658905872,-0.0317741635037164,
0.0691869510224353));
#63916=CARTESIAN_POINT('Ctrl Pts',(0.0110010659329861,-0.0317744765473203,
0.0691713323334524));
#63917=CARTESIAN_POINT('',(0.0108408026387313,-0.0317755400071255,0.069080885195809));
#63918=CARTESIAN_POINT('Ctrl Pts',(0.0110010659331233,-0.0317744765475851,
0.0691713323332258));
#63919=CARTESIAN_POINT('Ctrl Pts',(0.0109743526994062,-0.0317741635039241,
0.0691562557174284));
#63920=CARTESIAN_POINT('Ctrl Pts',(0.0109476482996434,-0.031774101327285,
0.0691411778335043));
#63921=CARTESIAN_POINT('Ctrl Pts',(0.0108942251070701,-0.031774461510283,
0.0691110212042464));
#63922=CARTESIAN_POINT('Ctrl Pts',(0.0108675142381039,-0.0317748838659619,
0.0690959469309762));
#63923=CARTESIAN_POINT('Ctrl Pts',(0.0108408026387313,-0.0317755400071256,
0.0690808851958091));
#63924=CARTESIAN_POINT('',(0.0107309823221581,-0.031882448187846,0.0689038779634784));
#63925=CARTESIAN_POINT('Origin',(0.00261408542943201,-0.0332583300691909,
0.0749256873615116));
#63926=CARTESIAN_POINT('',(0.0105232639353812,-0.0317755397360894,0.0689230878700478));
#63927=CARTESIAN_POINT('Origin',(0.0110705939186843,-0.0326853491202391,
0.0784743672369037));
#63928=CARTESIAN_POINT('',(0.0103543851739103,-0.0317744765475852,0.0688499713398157));
#63929=CARTESIAN_POINT('Ctrl Pts',(0.0105232640206465,-0.0317755400678203,
0.0689230876554634));
#63930=CARTESIAN_POINT('Ctrl Pts',(0.0104951266674769,-0.0317748838918833,
0.0689108928528174));
#63931=CARTESIAN_POINT('Ctrl Pts',(0.0104669797615349,-0.0317744615156213,
0.068898706205251));
#63932=CARTESIAN_POINT('Ctrl Pts',(0.0104106795027757,-0.0317741013270862,
0.0688743370107661));
#63933=CARTESIAN_POINT('Ctrl Pts',(0.0103825345006468,-0.0317741635037164,
0.0688621580789607));
#63934=CARTESIAN_POINT('Ctrl Pts',(0.0103543851738026,-0.0317744765473203,
0.0688499713400577));
#63935=CARTESIAN_POINT('',(0.0101840495712649,-0.0317755400071255,0.068780323722001));
#63936=CARTESIAN_POINT('Ctrl Pts',(0.0103543851739103,-0.0317744765475851,
0.0688499713398158));
#63937=CARTESIAN_POINT('Ctrl Pts',(0.0103259929824784,-0.0317741635039403,
0.0688383616641979));
#63938=CARTESIAN_POINT('Ctrl Pts',(0.0102976093964995,-0.0317741013272397,
0.0688267496233041));
#63939=CARTESIAN_POINT('Ctrl Pts',(0.0102408278293677,-0.0317744615102666,
0.0688035264876947));
#63940=CARTESIAN_POINT('Ctrl Pts',(0.0102124382745739,-0.0317748838660335,
0.0687919188385002));
#63941=CARTESIAN_POINT('Ctrl Pts',(0.0101840495712649,-0.0317755400071256,
0.068780323722001));
#63942=CARTESIAN_POINT('',(0.0100529103318967,-0.0318824481878461,0.0686184763799545));
#63943=CARTESIAN_POINT('Origin',(0.00275475047964434,-0.0332583300614187,
0.0756101189085328));
#63944=CARTESIAN_POINT('',(0.00984923750634952,-0.0317755397360895,0.0686635688277579));
#63945=CARTESIAN_POINT('Origin',(0.0115893443567482,-0.0326853491205606,
0.0780709348670765));
#63946=CARTESIAN_POINT('',(0.00967252647319418,-0.0317744765475852,0.0686121949644612));
#63947=CARTESIAN_POINT('Ctrl Pts',(0.00984923756404795,-0.0317755400678203,
0.068663568604179));
#63948=CARTESIAN_POINT('Ctrl Pts',(0.00981979367147625,-0.0317748838919549,
0.0686549965075861));
#63949=CARTESIAN_POINT('Ctrl Pts',(0.00979034131869444,-0.0317744615156049,
0.0686464336976297));
#63950=CARTESIAN_POINT('Ctrl Pts',(0.00973143393050001,-0.0317741013466114,
0.0686293138838769));
#63951=CARTESIAN_POINT('Ctrl Pts',(0.0097019780353993,-0.0317741635377482,
0.0686207566305228));
#63952=CARTESIAN_POINT('Ctrl Pts',(0.00967252647311763,-0.0317744765473203,
0.0686121949647148));
#63953=CARTESIAN_POINT('',(0.00949480485650097,-0.0317755400071255,0.0685644452507862));
#63954=CARTESIAN_POINT('Ctrl Pts',(0.00967252647319419,-0.0317744765475852,
0.0686121949644612));
#63955=CARTESIAN_POINT('Ctrl Pts',(0.00964290630339529,-0.031774163537956,
0.0686042361846668));
#63956=CARTESIAN_POINT('Ctrl Pts',(0.00961328471788823,-0.0317741013468101,
0.0685962713846959));
#63957=CARTESIAN_POINT('Ctrl Pts',(0.00955404347873013,-0.0317744615102666,
0.0685803488530575));
#63958=CARTESIAN_POINT('Ctrl Pts',(0.00952442295984559,-0.0317748838660336,
0.068572390888345));
#63959=CARTESIAN_POINT('Ctrl Pts',(0.00949480485650097,-0.0317755400071256,
0.0685644452507862));
#63960=CARTESIAN_POINT('',(0.00934441483848152,-0.0318824481878461,0.0684203102282909));
#63961=CARTESIAN_POINT('Origin',(0.00298008830923749,-0.0332583300645355,
0.0762715235567863));
#63962=CARTESIAN_POINT('',(0.00914799961629096,-0.0317755397360895,0.0684905740824893));
#63963=CARTESIAN_POINT('Origin',(0.0120534408096581,-0.0326853491203047,
0.0776056670125974));
#63964=CARTESIAN_POINT('',(0.00896624315000526,-0.0317744765475852,0.0684617530826412));
#63965=CARTESIAN_POINT('Ctrl Pts',(0.00914799964551254,-0.0317755400678203,
0.0684905738534419));
#63966=CARTESIAN_POINT('Ctrl Pts',(0.0091177135549392,-0.0317748838918833,
0.0684857596481305));
#63967=CARTESIAN_POINT('Ctrl Pts',(0.00908742023979814,-0.0317744615156213,
0.0684809557173699));
#63968=CARTESIAN_POINT('Ctrl Pts',(0.00902682838497098,-0.0317741013270862,
0.0684713534309399));
#63969=CARTESIAN_POINT('Ctrl Pts',(0.00899653883266233,-0.0317741635037163,
0.0684665565000764));
#63970=CARTESIAN_POINT('Ctrl Pts',(0.00896624314996109,-0.0317744765473202,
0.0684617530829025));
#63971=CARTESIAN_POINT('',(0.00878393829532611,-0.0317755400071255,0.0684366543146152));
#63972=CARTESIAN_POINT('Ctrl Pts',(0.00896624315000525,-0.0317744765475851,
0.0684617530826413));
#63973=CARTESIAN_POINT('Ctrl Pts',(0.00893585904291267,-0.0317741635379398,
0.0684575694516458));
#63974=CARTESIAN_POINT('Ctrl Pts',(0.00890547277664513,-0.0317741013468555,
0.0684533800253657));
#63975=CARTESIAN_POINT('Ctrl Pts',(0.00884470305483108,-0.031774461510283,
0.0684450079443782));
#63976=CARTESIAN_POINT('Ctrl Pts',(0.00881431870684405,-0.031774883865962,
0.0684408251662397));
#63977=CARTESIAN_POINT('Ctrl Pts',(0.00878393829532611,-0.0317755400071256,
0.0684366543146152));
#63978=CARTESIAN_POINT('',(0.00861666923907833,-0.0318824481878461,0.068312504707078));
#63979=CARTESIAN_POINT('Origin',(0.00328654529439703,-0.0332583300606616,
0.0768994704731398));
#63980=CARTESIAN_POINT('',(0.00843060920563109,-0.0317755397360895,0.0684068318647171));
#63981=CARTESIAN_POINT('Origin',(0.0124555641985925,-0.0326853491202919,
0.0770859012249049));
#63982=CARTESIAN_POINT('',(0.0082466737142653,-0.0317744765475852,0.0684010182527021));
#63983=CARTESIAN_POINT('Ctrl Pts',(0.008430609205915,-0.0317755400678204,
0.0684068316338133));
#63984=CARTESIAN_POINT('Ctrl Pts',(0.00839995855029356,-0.0317748838918834,
0.0684058512436123));
#63985=CARTESIAN_POINT('Ctrl Pts',(0.00836930201481447,-0.0317744615156214,
0.0684048819524226));
#63986=CARTESIAN_POINT('Ctrl Pts',(0.00830798445925291,-0.0317741013270863,
0.0684029495559823));
#63987=CARTESIAN_POINT('Ctrl Pts',(0.008277332534255,-0.0317741635037165,
0.0684019867378854));
#63988=CARTESIAN_POINT('Ctrl Pts',(0.00824667371425424,-0.0317744765473203,
0.0684010182529667));
#63989=CARTESIAN_POINT('',(0.00806266067806107,-0.0317755400071255,0.0683989662528899));
#63990=CARTESIAN_POINT('Ctrl Pts',(0.0082466737142653,-0.0317744765475852,
0.068401018252702));
#63991=CARTESIAN_POINT('Ctrl Pts',(0.00821600484693169,-0.0317741635379398,
0.0684006757492774));
#63992=CARTESIAN_POINT('Ctrl Pts',(0.00818533311110706,-0.0317741013468556,
0.0684003277668821));
#63993=CARTESIAN_POINT('Ctrl Pts',(0.00812399327671767,-0.0317744615102831,
0.0683996381679916));
#63994=CARTESIAN_POINT('Ctrl Pts',(0.00809332427727973,-0.031774883865962,
0.0683992965408911));
#63995=CARTESIAN_POINT('Ctrl Pts',(0.00806266067806107,-0.0317755400071256,
0.06839896625289));
#63996=CARTESIAN_POINT('',(0.00788115051652376,-0.031882448187846,0.0682967599737853));
#63997=CARTESIAN_POINT('Origin',(0.00366928835036435,-0.0332583300693303,
0.0774840566758911));
#63998=CARTESIAN_POINT('',(0.00770837994969399,-0.0317755397360895,0.0684136628392406));
#63999=CARTESIAN_POINT('Origin',(0.0127893735271636,-0.0326853484021168,
0.0765198349424559));
#64000=CARTESIAN_POINT('',(0.00752516620582388,-0.0317744765475852,0.0684309482991929));
#64001=CARTESIAN_POINT('Ctrl Pts',(0.00770837992103575,-0.0317755400678203,
0.0684136626101221));
#64002=CARTESIAN_POINT('Ctrl Pts',(0.00767784808519083,-0.0317748838920053,
0.0684165314958372));
#64003=CARTESIAN_POINT('Ctrl Pts',(0.00764731179832722,-0.0317744615155934,
0.0684194121307926));
#64004=CARTESIAN_POINT('Ctrl Pts',(0.00758623886673111,-0.0317741013465795,
0.0684251797867753));
#64005=CARTESIAN_POINT('Ctrl Pts',(0.00755570133421423,-0.0317741635377596,
0.0684280668919191));
#64006=CARTESIAN_POINT('Ctrl Pts',(0.00752516620584607,-0.0317744765473203,
0.0684309482994569));
#64007=CARTESIAN_POINT('',(0.00734234698360057,-0.0317755400071256,0.0684519754288576));
#64008=CARTESIAN_POINT('Ctrl Pts',(0.00752516620582388,-0.0317744765475852,
0.0684309482991929));
#64009=CARTESIAN_POINT('Ctrl Pts',(0.00749469293335161,-0.0317741635039242,
0.068434452705615));
#64010=CARTESIAN_POINT('Ctrl Pts',(0.0074642260623123,-0.0317741013272851,
0.0684379508936332));
#64011=CARTESIAN_POINT('Ctrl Pts',(0.00740328016968802,-0.0317744615102832,
0.0684449550327957));
#64012=CARTESIAN_POINT('Ctrl Pts',(0.00737281018723983,-0.0317748838659622,
0.0684484599443968));
#64013=CARTESIAN_POINT('Ctrl Pts',(0.00734234698360056,-0.0317755400071257,
0.0684519754288575));
#64014=CARTESIAN_POINT('',(0.00714945824045025,-0.0318824481878459,0.0683733243322622));
#64015=CARTESIAN_POINT('Origin',(0.00412228148793428,-0.0332583300609497,
0.0780160627022593));
#64016=CARTESIAN_POINT('',(0.00699270183528492,-0.0317755397360895,0.068510959277511));
#64017=CARTESIAN_POINT('Origin',(0.0130496030223191,-0.0326853484020826,
0.0759163944377061));
#64018=CARTESIAN_POINT('',(0.00681309922909792,-0.0317744765475852,0.0685510712074014));
#64019=CARTESIAN_POINT('Ctrl Pts',(0.00699270177813648,-0.0317755400678204,
0.068510959053791));
#64020=CARTESIAN_POINT('Ctrl Pts',(0.00696277025609412,-0.0317748838918833,
0.0685176319724393));
#64021=CARTESIAN_POINT('Ctrl Pts',(0.00693283579913468,-0.0317744615156214,
0.0685243171036637));
#64022=CARTESIAN_POINT('Ctrl Pts',(0.00687296733296115,-0.0317741013466568,
0.0685376937461372));
#64023=CARTESIAN_POINT('Ctrl Pts',(0.00684303244542577,-0.0317741635377321,
0.0685443854539173));
#64024=CARTESIAN_POINT('Ctrl Pts',(0.00681309922915301,-0.0317744765473203,
0.0685510712076604));
#64025=CARTESIAN_POINT('',(0.00663435698920081,-0.0317755400071256,0.0685948458561471));
#64026=CARTESIAN_POINT('Ctrl Pts',(0.00681309922909793,-0.0317744765475851,
0.0685510712074014));
#64027=CARTESIAN_POINT('Ctrl Pts',(0.00678330546761347,-0.0317741635039403,
0.0685583672939304));
#64028=CARTESIAN_POINT('Ctrl Pts',(0.00675351727781274,-0.0317741013272395,
0.0685656564087527));
#64029=CARTESIAN_POINT('Ctrl Pts',(0.00669392980840041,-0.0317744615102666,
0.0685802438651471));
#64030=CARTESIAN_POINT('Ctrl Pts',(0.00666413937109456,-0.0317748838660337,
0.068587540041312));
#64031=CARTESIAN_POINT('Ctrl Pts',(0.00663435698920084,-0.0317755400071256,
0.0685948458561471));
#64032=CARTESIAN_POINT('',(0.00643313163514339,-0.0318824481878457,0.0685409903168382));
#64033=CARTESIAN_POINT('Origin',(0.00463838065616737,-0.033258330061087,
0.0784870986645944));
#64034=CARTESIAN_POINT('',(0.00629486153379326,-0.0317755397360894,0.0686971867565749));
#64035=CARTESIAN_POINT('Origin',(0.0132321485687967,-0.0326853491204153,
0.0752850966106633));
#64036=CARTESIAN_POINT('',(0.00612170250567762,-0.0317744765475852,0.0687594925673074));
#64037=CARTESIAN_POINT('Ctrl Pts',(0.0062948614490559,-0.0317755400678203,
0.0686971865417816));
#64038=CARTESIAN_POINT('Ctrl Pts',(0.00626600228762614,-0.0317748838919548,
0.0687075582557843));
#64039=CARTESIAN_POINT('Ctrl Pts',(0.00623714174029079,-0.0317744615156049,
0.0687179424556203));
#64040=CARTESIAN_POINT('Ctrl Pts',(0.00617941875177804,-0.0317741013270409,
0.0687387182582189));
#64041=CARTESIAN_POINT('Ctrl Pts',(0.00615056487727383,-0.0317741635037326,
0.0687491067781996));
#64042=CARTESIAN_POINT('Ctrl Pts',(0.00612170250576476,-0.0317744765473203,
0.0687594925675575));
#64043=CARTESIAN_POINT('',(0.00594985612000611,-0.0317755400071255,0.0688253243827735));
#64044=CARTESIAN_POINT('Ctrl Pts',(0.00612170250567763,-0.0317744765475851,
0.0687594925673074));
#64045=CARTESIAN_POINT('Ctrl Pts',(0.00609306123154383,-0.031774163537956,
0.0687704640781778));
#64046=CARTESIAN_POINT('Ctrl Pts',(0.00606441527350702,-0.0317741013468101,
0.0687814315507554));
#64047=CARTESIAN_POINT('Ctrl Pts',(0.00600712907498679,-0.0317744615102666,
0.0688033710787701));
#64048=CARTESIAN_POINT('Ctrl Pts',(0.00597848799753159,-0.0317748838660335,
0.0688143434542423));
#64049=CARTESIAN_POINT('Ctrl Pts',(0.0059498561200061,-0.0317755400071256,
0.0688253243827735));
#64050=CARTESIAN_POINT('',(0.00574346759908138,-0.0318824481878455,0.0687971137347777));
#64051=CARTESIAN_POINT('Origin',(0.00520944668414427,-0.0332583300692591,
0.078889736052037));
#64052=CARTESIAN_POINT('',(0.00562586440364342,-0.0317755397360894,0.0689694083578402));
#64053=CARTESIAN_POINT('Origin',(0.0133341329028461,-0.0326853491203037,
0.0746358979587515));
#64054=CARTESIAN_POINT('',(0.00546187977491395,-0.0317744765475852,0.0690529254495596));
#64055=CARTESIAN_POINT('Ctrl Pts',(0.00562586429265349,-0.0317755400678202,
0.068969408155361));
#64056=CARTESIAN_POINT('Ctrl Pts',(0.00559853261180286,-0.0317748838918832,
0.0689833150988382));
#64057=CARTESIAN_POINT('Ctrl Pts',(0.00557120112538377,-0.0317744615156213,
0.068997234601096));
#64058=CARTESIAN_POINT('Ctrl Pts',(0.00551654017287186,-0.0317741013466567,
0.0690250796738461));
#64059=CARTESIAN_POINT('Ctrl Pts',(0.00548920990492778,-0.031774163537732,
0.0690390056531245));
#64060=CARTESIAN_POINT('Ctrl Pts',(0.00546187977503177,-0.0317744765473203,
0.0690529254497969));
#64061=CARTESIAN_POINT('',(0.00529963936362479,-0.0317755400071255,0.0691397762246904));
#64062=CARTESIAN_POINT('Ctrl Pts',(0.00546187977491393,-0.0317744765475852,
0.0690529254495596));
#64063=CARTESIAN_POINT('Ctrl Pts',(0.00543483650076778,-0.0317741635039242,
0.0690674017240456));
#64064=CARTESIAN_POINT('Ctrl Pts',(0.00540779688937628,-0.031774101327285,
0.0690818698602811));
#64065=CARTESIAN_POINT('Ctrl Pts',(0.00535370922709989,-0.031774461510283,
0.0691108178236381));
#64066=CARTESIAN_POINT('Ctrl Pts',(0.0053266691979104,-0.031774883865962,
0.0691252933566885));
#64067=CARTESIAN_POINT('Ctrl Pts',(0.00529963936362484,-0.0317755400071256,
0.0691397762246905));
#64068=CARTESIAN_POINT('',(0.00509134254609834,-0.0318824481878453,0.0691376553667789));
#64069=CARTESIAN_POINT('Origin',(0.00582647353396789,-0.0332583300652073,
0.0792176248812057));
#64070=CARTESIAN_POINT('',(0.00499626092921708,-0.0317755397360894,0.0693233309840378));
#64071=CARTESIAN_POINT('Origin',(0.0133539468935739,-0.0326853491203005,
0.0739790364057491));
#64072=CARTESIAN_POINT('',(0.00484403683542784,-0.0317744765475852,0.0694267422423173));
#64073=CARTESIAN_POINT('Ctrl Pts',(0.00499626079372497,-0.0317755400678203,
0.0693233307970659));
#64074=CARTESIAN_POINT('Ctrl Pts',(0.00497088763825794,-0.0317748838920054,
0.0693405536448749));
#64075=CARTESIAN_POINT('Ctrl Pts',(0.00494551624256691,-0.0317744615155934,
0.0693577889329206));
#64076=CARTESIAN_POINT('Ctrl Pts',(0.00489477621409276,-0.0317741013465794,
0.0693922652775759));
#64077=CARTESIAN_POINT('Ctrl Pts',(0.0048694068438692,-0.0317741635377597,
0.0694095068355857));
#64078=CARTESIAN_POINT('Ctrl Pts',(0.00484403683557445,-0.0317744765473203,
0.0694267422425379));
#64079=CARTESIAN_POINT('',(0.00469396102672551,-0.0317755400071256,0.0695332422885067));
#64080=CARTESIAN_POINT('Ctrl Pts',(0.00484403683542785,-0.0317744765475851,
0.0694267422423173));
#64081=CARTESIAN_POINT('Ctrl Pts',(0.00481902388447747,-0.0317741635379696,
0.0694444918574586));
#64082=CARTESIAN_POINT('Ctrl Pts',(0.00479400539256557,-0.031774101346772,
0.0694622387259671));
#64083=CARTESIAN_POINT('Ctrl Pts',(0.00474397508069731,-0.0317744615102528,
0.0694977354839971));
#64084=CARTESIAN_POINT('Ctrl Pts',(0.00471896253299177,-0.0317748838660939,
0.0695154858892795));
#64085=CARTESIAN_POINT('Ctrl Pts',(0.00469396102672552,-0.0317755400071256,
0.0695332422885067));
#64086=CARTESIAN_POINT('',(0.00448704087784028,-0.0318824481878451,0.0695572446678755));
#64087=CARTESIAN_POINT('Origin',(0.00647973031733237,-0.0332583300693583,
0.079465594297633));
#64088=CARTESIAN_POINT('',(0.00441598033341292,-0.0317755397360894,0.0697533730639295));
#64089=CARTESIAN_POINT('Origin',(0.0132912780623905,-0.0326853491205531,
0.0733248710508142));
#64090=CARTESIAN_POINT('',(0.00427791743945781,-0.0317744765475852,0.0698750476314508));
#64091=CARTESIAN_POINT('Ctrl Pts',(0.00441598017555541,-0.0317755400678203,
0.0697533728954136));
#64092=CARTESIAN_POINT('Ctrl Pts',(0.00439296568843473,-0.0317748838919549,
0.0697736400371027));
#64093=CARTESIAN_POINT('Ctrl Pts',(0.00436995450907151,-0.0317744615156049,
0.0697939192980136));
#64094=CARTESIAN_POINT('Ctrl Pts',(0.00432393561522292,-0.0317741013466114,
0.0698344831959516));
#64095=CARTESIAN_POINT('Ctrl Pts',(0.00430092722938568,-0.0317741635377482,
0.069854768425117));
#64096=CARTESIAN_POINT('Ctrl Pts',(0.0042779174396309,-0.0317744765473203,
0.0698750476316513));
#64097=CARTESIAN_POINT('',(0.00414237301849599,-0.0317755400071255,0.0699995173793506));
#64098=CARTESIAN_POINT('Ctrl Pts',(0.00427791743945776,-0.0317744765475852,
0.0698750476314508));
#64099=CARTESIAN_POINT('Ctrl Pts',(0.00425532388256617,-0.0317741635039242,
0.06989579449595));
#64100=CARTESIAN_POINT('Ctrl Pts',(0.00423273184945642,-0.0317741013272851,
0.0699165325669869));
#64101=CARTESIAN_POINT('Ctrl Pts',(0.00418754251629321,-0.0317744615102831,
0.0699580221314705));
#64102=CARTESIAN_POINT('Ctrl Pts',(0.00416495191802581,-0.031774883865962,
0.0699787674708386));
#64103=CARTESIAN_POINT('Ctrl Pts',(0.00414237301849597,-0.0317755400071257,
0.0699995173793505));
#64104=CARTESIAN_POINT('',(0.00394009279260827,-0.0318824481878447,0.0700492644641388));
#64105=CARTESIAN_POINT('Origin',(0.00715891477913272,-0.0332583300694027,
0.079629733586828));
#64106=CARTESIAN_POINT('',(0.00389417398786977,-0.0317755397360895,0.0702527525770204));
#64107=CARTESIAN_POINT('Origin',(0.0131471147347495,-0.0326853491205069,
0.0726837184722928));
#64108=CARTESIAN_POINT('',(0.00377244962806149,-0.0317744765475852,0.0703907715731684));
#64109=CARTESIAN_POINT('Ctrl Pts',(0.00389417381013636,-0.0317755400678204,
0.0702527524296181));
#64110=CARTESIAN_POINT('Ctrl Pts',(0.00387388094330818,-0.0317748838918833,
0.0702757442414414));
#64111=CARTESIAN_POINT('Ctrl Pts',(0.0038535928804539,-0.0317744615156214,
0.0702987476585478));
#64112=CARTESIAN_POINT('Ctrl Pts',(0.00381302086706254,-0.0317741013466568,
0.0703447593911317));
#64113=CARTESIAN_POINT('Ctrl Pts',(0.00379273632146808,-0.0317741635377321,
0.070367768381869));
#64114=CARTESIAN_POINT('Ctrl Pts',(0.00377244962825834,-0.0317744765473203,
0.0703907715733456));
#64115=CARTESIAN_POINT('',(0.00365357421132868,-0.0317755400071255,0.0705312480605002));
#64116=CARTESIAN_POINT('Ctrl Pts',(0.00377244962806147,-0.0317744765475851,
0.0703907715731684));
#64117=CARTESIAN_POINT('Ctrl Pts',(0.00375263449972844,-0.0317741635039242,
0.0704141865659871));
#64118=CARTESIAN_POINT('Ctrl Pts',(0.00373281978104871,-0.031774101327285,
0.0704375926437021));
#64119=CARTESIAN_POINT('Ctrl Pts',(0.00369318680055041,-0.031774461510283,
0.0704844187758258));
#64120=CARTESIAN_POINT('Ctrl Pts',(0.00367337441636236,-0.031774883865962,
0.0705078318847255));
#64121=CARTESIAN_POINT('Ctrl Pts',(0.00365357421132872,-0.0317755400071256,
0.0705312480605002));
#64122=CARTESIAN_POINT('',(0.00345912398843712,-0.0318824481878444,0.0706059553094632));
#64123=CARTESIAN_POINT('Origin',(0.00785331577631647,-0.0332583300696887,
0.0797074542031271));
#64124=CARTESIAN_POINT('',(0.00343907109036868,-0.0317755397360895,0.0708135940100747));
#64125=CARTESIAN_POINT('Origin',(0.0129237304522124,-0.0326853491203865,
0.0720656900293326));
#64126=CARTESIAN_POINT('',(0.00333560493057455,-0.0317744765475852,0.0709657807928331));
#64127=CARTESIAN_POINT('Ctrl Pts',(0.00343907089556234,-0.0317755400678203,
0.0708135938861105));
#64128=CARTESIAN_POINT('Ctrl Pts',(0.00342181968217177,-0.0317748838918833,
0.0708389477712479));
#64129=CARTESIAN_POINT('Ctrl Pts',(0.00340457468940154,-0.0317744615156214,
0.0708643125680603));
#64130=CARTESIAN_POINT('Ctrl Pts',(0.00337008752385169,-0.0317741013270863,
0.0709150492627527));
#64131=CARTESIAN_POINT('Ctrl Pts',(0.00335285046691346,-0.0317741635037165,
0.0709404136352643));
#64132=CARTESIAN_POINT('Ctrl Pts',(0.00333560493079202,-0.0317744765473204,
0.0709657807929842));
#64133=CARTESIAN_POINT('',(0.00323527325440675,-0.0317755400071256,0.0711200486214734));
#64134=CARTESIAN_POINT('Ctrl Pts',(0.00333560493057454,-0.0317744765475852,
0.0709657807928331));
#64135=CARTESIAN_POINT('Ctrl Pts',(0.0033188807272107,-0.0317741635039242,
0.0709914946455473));
#64136=CARTESIAN_POINT('Ctrl Pts',(0.00330215581291114,-0.0317741013272851,
0.0710171996021129));
#64137=CARTESIAN_POINT('Ctrl Pts',(0.00326870422085706,-0.0317744615102831,
0.0710686238257989));
#64138=CARTESIAN_POINT('Ctrl Pts',(0.00325198250388255,-0.0317748838659619,
0.0710943354655161));
#64139=CARTESIAN_POINT('Ctrl Pts',(0.00323527325440685,-0.0317755400071256,
0.0711200486214734));
#64140=CARTESIAN_POINT('',(0.00305171963068536,-0.031882448187844,0.0712185378566669));
#64141=CARTESIAN_POINT('Origin',(0.00855198215770979,-0.0332583300606185,
0.079697530396209));
#64142=CARTESIAN_POINT('',(0.00305784888546854,-0.0317755397360895,0.0714270525586625));
#64143=CARTESIAN_POINT('Origin',(0.0126246481179549,-0.0326853491205759,
0.0714805323998506));
#64144=CARTESIAN_POINT('',(0.00297427264883722,-0.0317744765475852,0.0715910070515539));
#64145=CARTESIAN_POINT('Ctrl Pts',(0.00305784867666147,-0.0317755400678203,
0.0714270524600915));
#64146=CARTESIAN_POINT('Ctrl Pts',(0.00304391117864933,-0.0317748838918833,
0.0714543685726279));
#64147=CARTESIAN_POINT('Ctrl Pts',(0.00302998121980092,-0.0317744615156213,
0.0714816947311485));
#64148=CARTESIAN_POINT('Ctrl Pts',(0.00300212650340108,-0.0317741013466568,
0.0715363507699768));
#64149=CARTESIAN_POINT('Ctrl Pts',(0.00298820133741727,-0.031774163537732,
0.0715636814523147));
#64150=CARTESIAN_POINT('Ctrl Pts',(0.00297427264907201,-0.0317744765473203,
0.0715910070516766));
#64151=CARTESIAN_POINT('',(0.00289406700370193,-0.0317755400071256,0.0717566333256912));
#64152=CARTESIAN_POINT('Ctrl Pts',(0.00297427264883726,-0.0317744765475851,
0.0715910070515539));
#64153=CARTESIAN_POINT('Ctrl Pts',(0.00296090457455914,-0.031774163537956,
0.0716186112400905));
#64154=CARTESIAN_POINT('Ctrl Pts',(0.00294753032146113,-0.03177410134681,
0.0716462156911905));
#64155=CARTESIAN_POINT('Ctrl Pts',(0.0029207891203601,-0.0317744615102666,
0.0717014240202273));
#64156=CARTESIAN_POINT('Ctrl Pts',(0.00290742178131277,-0.0317748838660337,
0.0717290287044008));
#64157=CARTESIAN_POINT('Ctrl Pts',(0.00289406700370195,-0.0317755400071256,
0.0717566333256912));
#64158=CARTESIAN_POINT('',(0.00272430472944635,-0.0318824481878437,0.0718773513130417));
#64159=CARTESIAN_POINT('Origin',(0.00924389559598285,-0.0332583300610094,
0.0796001187756036));
#64160=CARTESIAN_POINT('',(0.00275651947507167,-0.0317755397360895,0.07208345361501));
#64161=CARTESIAN_POINT('Origin',(0.0122545844395361,-0.0326853491205966,
0.0709374738690273));
#64162=CARTESIAN_POINT('',(0.00269415120878019,-0.0317744765475852,0.0722565901577418));
#64163=CARTESIAN_POINT('Ctrl Pts',(0.0027565192555569,-0.0317755400678203,
0.0720834535433868));
#64164=CARTESIAN_POINT('Ctrl Pts',(0.00274611527559222,-0.0317748838918833,
0.0721123010919102));
#64165=CARTESIAN_POINT('Ctrl Pts',(0.0027357200344381,-0.0317744615156214,
0.0721411576622954));
#64166=CARTESIAN_POINT('Ctrl Pts',(0.00271493404948892,-0.0317741013270863,
0.072198876979737));
#64167=CARTESIAN_POINT('Ctrl Pts',(0.00270454638932916,-0.0317741635037164,
0.072227731165589));
#64168=CARTESIAN_POINT('Ctrl Pts',(0.00269415120902848,-0.0317744765473203,
0.0722565901578341));
#64169=CARTESIAN_POINT('',(0.00263533648561441,-0.0317755400071256,0.0724309628520908));
#64170=CARTESIAN_POINT('Ctrl Pts',(0.0026941512087802,-0.0317744765475851,
0.0722565901577418));
#64171=CARTESIAN_POINT('Ctrl Pts',(0.00268434826746197,-0.0317741635379398,
0.0722856521444882));
#64172=CARTESIAN_POINT('Ctrl Pts',(0.00267453922892048,-0.0317741013468556,
0.0723147151662367));
#64173=CARTESIAN_POINT('Ctrl Pts',(0.00265492833014389,-0.0317744615102831,
0.0723728397176637));
#64174=CARTESIAN_POINT('Ctrl Pts',(0.00264512618143677,-0.0317748838659621,
0.072401902100848));
#64175=CARTESIAN_POINT('Ctrl Pts',(0.0026353364856144,-0.0317755400071257,
0.0724309628520908));
#64176=CARTESIAN_POINT('',(0.00248204281330085,-0.0318824481878432,0.072572005796824));
#64177=CARTESIAN_POINT('Origin',(0.00991814422157668,-0.0332583300700225,
0.0794167555683928));
#64178=CARTESIAN_POINT('',(0.00253983500398563,-0.0317755397360895,0.0727724453423437));
#64179=CARTESIAN_POINT('Origin',(0.011819375542347,-0.0326853491204354,
0.0704450787941925));
#64180=CARTESIAN_POINT('',(0.00249965829285137,-0.0317744765475852,0.0729520334682077));
#64181=CARTESIAN_POINT('Ctrl Pts',(0.00253983477722505,-0.0317755400678203,
0.0727724452987978));
#64182=CARTESIAN_POINT('Ctrl Pts',(0.0025331283922866,-0.0317748838918833,
0.0728023693402364));
#64183=CARTESIAN_POINT('Ctrl Pts',(0.00252643180798999,-0.0317744615156214,
0.0728323012371319));
#64184=CARTESIAN_POINT('Ctrl Pts',(0.00251304460285598,-0.0317741013466568,
0.0728921673422743));
#64185=CARTESIAN_POINT('Ctrl Pts',(0.00250635378587497,-0.0317741635377321,
0.0729221024289259));
#64186=CARTESIAN_POINT('Ctrl Pts',(0.00249965829310926,-0.0317744765473203,
0.0729520334682682));
#64187=CARTESIAN_POINT('',(0.00246316203497268,-0.0317755400071255,0.0731324026212159));
#64188=CARTESIAN_POINT('Ctrl Pts',(0.0024996582928514,-0.0317744765475851,
0.0729520334682077));
#64189=CARTESIAN_POINT('Ctrl Pts',(0.00249357508374126,-0.031774163537956,
0.0729820949252851));
#64190=CARTESIAN_POINT('Ctrl Pts',(0.00248748595522708,-0.0317741013468101,
0.073012158173287));
#64191=CARTESIAN_POINT('Ctrl Pts',(0.00247531463125164,-0.0317744615102666,
0.0730722822974274));
#64192=CARTESIAN_POINT('Ctrl Pts',(0.00246923225753412,-0.0317748838660336,
0.0731023440517231));
#64193=CARTESIAN_POINT('Ctrl Pts',(0.00246316203497269,-0.0317755400071256,
0.0731324026212159));
#64194=CARTESIAN_POINT('',(0.00232875449738658,-0.0318824481878429,0.0732915461918387));
#64195=CARTESIAN_POINT('Origin',(0.010564094601645,-0.0332583300617367,
0.0791503323998404));
#64196=CARTESIAN_POINT('',(0.00241121271576042,-0.0317755397360895,0.0734831619295401));
#64197=CARTESIAN_POINT('Origin',(0.0113258849301056,-0.0326853491204514,
0.0700111125401321));
#64198=CARTESIAN_POINT('',(0.002393861170518,-0.0317744765475852,0.073666369426511));
#64199=CARTESIAN_POINT('Ctrl Pts',(0.00241121248533015,-0.0317755400678203,
0.0734831619147582));
#64200=CARTESIAN_POINT('Ctrl Pts',(0.00240830945911483,-0.0317748838918833,
0.0735136905291024));
#64201=CARTESIAN_POINT('Ctrl Pts',(0.00240541714081022,-0.0317744615156214,
0.073544225708614));
#64202=CARTESIAN_POINT('Ctrl Pts',(0.0023996387103257,-0.0317741013466568,
0.0736052976133437));
#64203=CARTESIAN_POINT('Ctrl Pts',(0.00239675251364211,-0.0317741635377321,
0.0736358352346231));
#64204=CARTESIAN_POINT('Ctrl Pts',(0.00239386117078142,-0.0317744765473203,
0.0736663694265387));
#64205=CARTESIAN_POINT('',(0.0023802589457153,-0.0317755400071255,0.0738498905088876));
#64206=CARTESIAN_POINT('Ctrl Pts',(0.00239386117051799,-0.0317744765475851,
0.073666369426511));
#64207=CARTESIAN_POINT('Ctrl Pts',(0.0023915933825296,-0.0317741635039404,
0.0736969595922481));
#64208=CARTESIAN_POINT('Ctrl Pts',(0.00238932068579902,-0.0317741013272396,
0.0737275423046233));
#64209=CARTESIAN_POINT('Ctrl Pts',(0.00238478064055958,-0.0317744615102666,
0.0737887211276194));
#64210=CARTESIAN_POINT('Ctrl Pts',(0.00238251396504818,-0.0317748838660336,
0.0738193081595674));
#64211=CARTESIAN_POINT('Ctrl Pts',(0.00238025894571531,-0.0317755400071256,
0.0738498905088876));
#64212=CARTESIAN_POINT('',(0.0022668572300156,-0.0318824481878425,0.0740246249162233));
#64213=CARTESIAN_POINT('Origin',(0.0111715598869108,-0.0332583300696574,
0.0788050510671788));
#64214=CARTESIAN_POINT('',(0.00237268106071657,-0.0317755397360895,0.0742043949514572));
#64215=CARTESIAN_POINT('Origin',(0.0107818952449207,-0.0326853491204138,
0.0696424190137116));
#64216=CARTESIAN_POINT('',(0.00237842832559961,-0.0317744765475852,0.0743883325278656));
#64217=CARTESIAN_POINT('Ctrl Pts',(0.00237268083025065,-0.0317755400678204,
0.0742043949656725));
#64218=CARTESIAN_POINT('Ctrl Pts',(0.00237362694521611,-0.0317748838918833,
0.0742350466984364));
#64219=CARTESIAN_POINT('Ctrl Pts',(0.00237458450649089,-0.0317744615156214,
0.074265703602543));
#64220=CARTESIAN_POINT('Ctrl Pts',(0.00237650608436353,-0.0317741013270863,
0.0743270214980914));
#64221=CARTESIAN_POINT('Ctrl Pts',(0.00237746981646342,-0.0317741635037165,
0.0743576733943658));
#64222=CARTESIAN_POINT('Ctrl Pts',(0.00237842832586444,-0.0317744765473203,
0.07438833252786));
#64223=CARTESIAN_POINT('',(0.00238793464908376,-0.0317755400071256,0.074572111302511));
#64224=CARTESIAN_POINT('Ctrl Pts',(0.00237842832559961,-0.0317744765475852,
0.0743883325278656));
#64225=CARTESIAN_POINT('Ctrl Pts',(0.00238001238426591,-0.0317741635039242,
0.0744189657117954));
#64226=CARTESIAN_POINT('Ctrl Pts',(0.00238159063874809,-0.0317741013272851,
0.0744495921164671));
#64227=CARTESIAN_POINT('Ctrl Pts',(0.00238475413258085,-0.0317744615102831,
0.0745108575398308));
#64228=CARTESIAN_POINT('Ctrl Pts',(0.00238633890201153,-0.0317748838659621,
0.0745414874719487));
#64229=CARTESIAN_POINT('Ctrl Pts',(0.00238793464908377,-0.0317755400071257,
0.074572111302511));
#64230=CARTESIAN_POINT('',(0.00229732716806982,-0.0318824481878422,0.0747596808805746));
#64231=CARTESIAN_POINT('Origin',(0.0117309598519367,-0.0332583300698019,
0.0783863567654003));
#64232=CARTESIAN_POINT('',(0.00242484770607189,-0.0317755397360895,0.0749247701324961));
#64233=CARTESIAN_POINT('Origin',(0.0101959855290228,-0.0326853491203767,
0.0693448127321306));
#64234=CARTESIAN_POINT('',(0.0024536031432799,-0.0317744765475852,0.0751065369828829));
#64235=CARTESIAN_POINT('Ctrl Pts',(0.00242484747920488,-0.0317755400678203,
0.0749247701754843));
#64236=CARTESIAN_POINT('Ctrl Pts',(0.00242962781403169,-0.0317748838919549,
0.0749550616272295));
#64237=CARTESIAN_POINT('Ctrl Pts',(0.00243442015384011,-0.031774461515605,
0.0749853567799411));
#64238=CARTESIAN_POINT('Ctrl Pts',(0.00244401175038665,-0.031774101327041,
0.0750459503328312));
#64239=CARTESIAN_POINT('Ctrl Pts',(0.0024488095841822,-0.0317741635037326,
0.0750762397404218));
#64240=CARTESIAN_POINT('Ctrl Pts',(0.00245360314354193,-0.0317744765473203,
0.0751065369828442));
#64241=CARTESIAN_POINT('',(0.00248606809465078,-0.0317755400071256,0.0752876751487366));
#64242=CARTESIAN_POINT('Ctrl Pts',(0.0024536031432799,-0.0317744765475851,
0.0751065369828829));
#64243=CARTESIAN_POINT('Ctrl Pts',(0.00245901347869469,-0.0317741635379696,
0.0751367267961233));
#64244=CARTESIAN_POINT('Ctrl Pts',(0.00246441896965501,-0.0317741013467719,
0.075166920453516));
#64245=CARTESIAN_POINT('Ctrl Pts',(0.00247523552585244,-0.0317744615102528,
0.0752273030176307));
#64246=CARTESIAN_POINT('Ctrl Pts',(0.00248064674790228,-0.031774883866094,
0.0752574928024337));
#64247=CARTESIAN_POINT('Ctrl Pts',(0.00248606809465078,-0.0317755400071256,
0.0752876751487366));
#64248=CARTESIAN_POINT('',(0.00241968378242437,-0.0318824481878419,0.0754851218132336));
#64249=CARTESIAN_POINT('Origin',(0.0122334724704804,-0.0332583300697356,
0.0779008525869336));
#64250=CARTESIAN_POINT('',(0.00256688995266614,-0.0317755397360895,0.0756329267257202));
#64251=CARTESIAN_POINT('Origin',(0.00957739592850816,-0.0326853491203207,
0.0691229871243551));
#64252=CARTESIAN_POINT('',(0.00261820007177698,-0.0317744765475852,0.0758096562782736));
#64253=CARTESIAN_POINT('Ctrl Pts',(0.00256688973297591,-0.0317755400678204,
0.0756329267968033));
#64254=CARTESIAN_POINT('Ctrl Pts',(0.0025754288999625,-0.0317748838918833,
0.0756623802597942));
#64255=CARTESIAN_POINT('Ctrl Pts',(0.0025839804397121,-0.0317744615156214,
0.0756918358850788));
#64256=CARTESIAN_POINT('Ctrl Pts',(0.0026010907882075,-0.0317741013270863,
0.0757507494891987));
#64257=CARTESIAN_POINT('Ctrl Pts',(0.0026096470595172,-0.0317741635037165,
0.0757801987293597));
#64258=CARTESIAN_POINT('Ctrl Pts',(0.0026182000720321,-0.0317744765473204,
0.0758096562782024));
#64259=CARTESIAN_POINT('',(0.00267311165935758,-0.0317755400071256,0.0759852971782525));
#64260=CARTESIAN_POINT('Ctrl Pts',(0.002618200071777,-0.0317744765475852,
0.0758096562782736));
#64261=CARTESIAN_POINT('Ctrl Pts',(0.00262735252738243,-0.0317741635039242,
0.0758389331250288));
#64262=CARTESIAN_POINT('Ctrl Pts',(0.00263649767521997,-0.0317741013272851,
0.0758682048489508));
#64263=CARTESIAN_POINT('Ctrl Pts',(0.00265479787330016,-0.0317744615102831,
0.075926758777456));
#64264=CARTESIAN_POINT('Ctrl Pts',(0.00266395020864746,-0.0317748838659621,
0.0759560322978017));
#64265=CARTESIAN_POINT('Ctrl Pts',(0.00267311165935761,-0.0317755400071257,
0.0759852971782525));
#64266=CARTESIAN_POINT('',(0.00263199743617858,-0.0318824481878415,0.0761895070773348));
#64267=CARTESIAN_POINT('Origin',(0.0126711728188753,-0.0332583300697157,
0.0773561952226392));
#64268=CARTESIAN_POINT('',(0.00279656770941877,-0.0317755397360895,0.0763176966786222));
#64269=CARTESIAN_POINT('Origin',(0.00893588197120081,-0.0326853491203759,
0.0689804405125556));
#64270=CARTESIAN_POINT('',(0.00286962331920213,-0.0317744765475852,0.0764866018027231));
#64271=CARTESIAN_POINT('Ctrl Pts',(0.00279656750036996,-0.0317755400678203,
0.0763176967766793));
#64272=CARTESIAN_POINT('Ctrl Pts',(0.00280873083123078,-0.0317748838918833,
0.0763458477489071));
#64273=CARTESIAN_POINT('Ctrl Pts',(0.00282090670829858,-0.0317744615156214,
0.0763739993156591));
#64274=CARTESIAN_POINT('Ctrl Pts',(0.00284526596909028,-0.0317741013270863,
0.0764303038731084));
#64275=CARTESIAN_POINT('Ctrl Pts',(0.00285744574014045,-0.0317741635037164,
0.0764584485120642));
#64276=CARTESIAN_POINT('Ctrl Pts',(0.00286962331944631,-0.0317744765473203,
0.0764866018026204));
#64277=CARTESIAN_POINT('',(0.00294611555445444,-0.0317755400071255,0.0766539754749139));
#64278=CARTESIAN_POINT('Ctrl Pts',(0.00286962331920212,-0.0317744765475852,
0.0764866018027231));
#64279=CARTESIAN_POINT('Ctrl Pts',(0.0028823729661738,-0.0317741635039404,
0.0765145006844968));
#64280=CARTESIAN_POINT('Ctrl Pts',(0.00289511472089743,-0.0317741013272396,
0.0765423953996442));
#64281=CARTESIAN_POINT('Ctrl Pts',(0.00292060937168583,-0.0317744615102667,
0.076598193994396));
#64282=CARTESIAN_POINT('Ctrl Pts',(0.00293335848381762,-0.0317748838660339,
0.0766260895940772));
#64283=CARTESIAN_POINT('Ctrl Pts',(0.00294611555445441,-0.0317755400071257,
0.0766539754749139));
#64284=CARTESIAN_POINT('',(0.00293091981618271,-0.0318824481878412,0.076861728096484));
#64285=CARTESIAN_POINT('Origin',(0.0130371580999669,-0.033258330069632,
0.0767609742442826));
#64286=CARTESIAN_POINT('',(0.00311025882090281,-0.0317755397360895,0.076968280759983));
#64287=CARTESIAN_POINT('Origin',(0.00828156071521838,-0.032685349120703,
0.0689194209423546));
#64288=CARTESIAN_POINT('',(0.00320390779075248,-0.0317744765475852,0.0771266977209283));
#64289=CARTESIAN_POINT('Ctrl Pts',(0.00311025862579223,-0.0317755400678203,
0.0769682808834677));
#64290=CARTESIAN_POINT('Ctrl Pts',(0.00312585429753271,-0.0317748838918833,
0.0769946854072822));
#64291=CARTESIAN_POINT('Ctrl Pts',(0.00314146249106465,-0.0317744615156213,
0.0770210889484786));
#64292=CARTESIAN_POINT('Ctrl Pts',(0.00317268480753182,-0.0317741013466568,
0.0770738936335047));
#64293=CARTESIAN_POINT('Ctrl Pts',(0.00318829938879392,-0.0317741635377321,
0.0771002955519336));
#64294=CARTESIAN_POINT('Ctrl Pts',(0.00320390779098185,-0.0317744765473203,
0.0771266977207958));
#64295=CARTESIAN_POINT('',(0.00330077434543096,-0.0317755400071256,0.0772831645825335));
#64296=CARTESIAN_POINT('Ctrl Pts',(0.00320390779075249,-0.0317744765475851,
0.0771266977209283));
#64297=CARTESIAN_POINT('Ctrl Pts',(0.00322005180560095,-0.031774163537956,
0.0771527758232258));
#64298=CARTESIAN_POINT('Ctrl Pts',(0.0032361927313619,-0.0317741013468102,
0.0771788592831621));
#64299=CARTESIAN_POINT('Ctrl Pts',(0.00326847801320322,-0.0317744615102666,
0.0772310197280091));
#64300=CARTESIAN_POINT('Ctrl Pts',(0.00328462284048518,-0.0317748838660336,
0.0772570974751015));
#64301=CARTESIAN_POINT('Ctrl Pts',(0.00330077434543096,-0.0317755400071256,
0.0772831645825335));
#64302=CARTESIAN_POINT('',(0.00331173673793648,-0.0318824481878409,0.077491183543644));
#64303=CARTESIAN_POINT('Origin',(0.013325656508119,-0.0332583300697143,
0.0761245766423453));
#64304=CARTESIAN_POINT('',(0.00350301619090027,-0.0317755397360894,0.0775744188701997));
#64305=CARTESIAN_POINT('Origin',(0.00762475119780743,-0.0326853491204433,
0.0689408907276665));
#64306=CARTESIAN_POINT('',(0.00361578162061684,-0.0317744765475852,0.0777198493378787));
#64307=CARTESIAN_POINT('Ctrl Pts',(0.00350301601280495,-0.0317755400678203,
0.0775744190171645));
#64308=CARTESIAN_POINT('Ctrl Pts',(0.00352179807236654,-0.0317748838918833,
0.077598660677454));
#64309=CARTESIAN_POINT('Ctrl Pts',(0.00354059243182567,-0.0317744615156214,
0.0776228997934755));
#64310=CARTESIAN_POINT('Ctrl Pts',(0.00357818673292297,-0.0317741013466568,
0.0776713749039054));
#64311=CARTESIAN_POINT('Ctrl Pts',(0.00359698722635675,-0.0317741635377321,
0.0776956116093609));
#64312=CARTESIAN_POINT('Ctrl Pts',(0.00361578162082781,-0.0317744765473204,
0.0777198493377185));
#64313=CARTESIAN_POINT('',(0.00373149485129061,-0.0317755400071255,0.0778629418130248));
#64314=CARTESIAN_POINT('Ctrl Pts',(0.00361578162061688,-0.0317744765475852,
0.0777198493378787));
#64315=CARTESIAN_POINT('Ctrl Pts',(0.00363506888290464,-0.031774163503954,
0.0777437010156738));
#64316=CARTESIAN_POINT('Ctrl Pts',(0.00365434746464147,-0.0317741013272014,
0.0777675506203995));
#64317=CARTESIAN_POINT('Ctrl Pts',(0.00369291770291779,-0.0317744615102528,
0.0778152559410678));
#64318=CARTESIAN_POINT('Ctrl Pts',(0.00371220363269735,-0.031774883866094,
0.0778391045750569));
#64319=CARTESIAN_POINT('Ctrl Pts',(0.00373149485129058,-0.0317755400071256,
0.0778629418130247));
#64320=CARTESIAN_POINT('',(0.00376844249109501,-0.0318824481878408,0.0780679465303945));
#64321=CARTESIAN_POINT('Origin',(0.0135321181980821,-0.0332583300620928,
0.0754570388007481));
#64322=CARTESIAN_POINT('',(0.00396864580106426,-0.0317755397360895,0.0781265518491845));
#64323=CARTESIAN_POINT('Origin',(0.00697581169705831,-0.0326853491203594,
0.0690445112786724));
#64324=CARTESIAN_POINT('',(0.00409874931245924,-0.0317744765475852,0.0782567022982473));
#64325=CARTESIAN_POINT('Ctrl Pts',(0.00396864564279281,-0.0317755400678204,
0.0781265520173118));
#64326=CARTESIAN_POINT('Ctrl Pts',(0.00399031788587653,-0.0317748838918833,
0.078148248508612));
#64327=CARTESIAN_POINT('Ctrl Pts',(0.00401200201298715,-0.0317744615156214,
0.0781699409341198));
#64328=CARTESIAN_POINT('Ctrl Pts',(0.00405537777091025,-0.0317741013270863,
0.0782133243457021));
#64329=CARTESIAN_POINT('Ctrl Pts',(0.00407706296826219,-0.0317741635037165,
0.0782350088964372));
#64330=CARTESIAN_POINT('Ctrl Pts',(0.00409874931264841,-0.0317744765473204,
0.078256702298062));
#64331=CARTESIAN_POINT('',(0.00423148435235597,-0.0317755400071255,0.0783841637331207));
#64332=CARTESIAN_POINT('Ctrl Pts',(0.00409874931245925,-0.0317744765475851,
0.0782567022982473));
#64333=CARTESIAN_POINT('Ctrl Pts',(0.0041208738989355,-0.0317741635039241,
0.0782779485655145));
#64334=CARTESIAN_POINT('Ctrl Pts',(0.00414298961362218,-0.031774101327285,
0.0782991938641527));
#64335=CARTESIAN_POINT('Ctrl Pts',(0.00418723476963576,-0.031774461510283,
0.0783416888751821));
#64336=CARTESIAN_POINT('Ctrl Pts',(0.00420935764821783,-0.031774883865962,
0.0783629322854281));
#64337=CARTESIAN_POINT('Ctrl Pts',(0.00423148435235597,-0.0317755400071256,
0.0783841637331206));
#64338=CARTESIAN_POINT('',(0.00429383455310798,-0.0318824481878405,0.078582921159893));
#64339=CARTESIAN_POINT('Origin',(0.0136532872535296,-0.033258330061942,
0.0747688881694887));
#64340=CARTESIAN_POINT('',(0.004499804394289,-0.0317755397360895,0.0786159722300308));
#64341=CARTESIAN_POINT('Origin',(0.00634497637698724,-0.0326853491204427,
0.0692286484364096));
#64342=CARTESIAN_POINT('',(0.00464519417726763,-0.0317744765475852,0.0787287901101476));
#64343=CARTESIAN_POINT('Ctrl Pts',(0.00449980425833748,-0.0317755400678204,
0.078615972416669));
#64344=CARTESIAN_POINT('Ctrl Pts',(0.00452402489621148,-0.0317748838920056,
0.0786347815688472));
#64345=CARTESIAN_POINT('Ctrl Pts',(0.00454825682165911,-0.0317744615155934,
0.0786535852031391));
#64346=CARTESIAN_POINT('Ctrl Pts',(0.00459672793863523,-0.0317741013270089,
0.0786911901046868));
#64347=CARTESIAN_POINT('Ctrl Pts',(0.0046209599343138,-0.0317741635037441,
0.0787099857885914));
#64348=CARTESIAN_POINT('Ctrl Pts',(0.00464519417743208,-0.0317744765473204,
0.0787287901099401));
#64349=CARTESIAN_POINT('',(0.00479285771551606,-0.0317755400071256,0.0788386103617785));
#64350=CARTESIAN_POINT('Ctrl Pts',(0.0046451941772676,-0.0317744765475852,
0.0787287901101476));
#64351=CARTESIAN_POINT('Ctrl Pts',(0.00466980716687401,-0.0317741635039404,
0.0787470958973389));
#64352=CARTESIAN_POINT('Ctrl Pts',(0.00469441123316321,-0.0317741013272396,
0.0787654018354073));
#64353=CARTESIAN_POINT('Ctrl Pts',(0.00474363354398586,-0.0317744615102667,
0.0788020163750381));
#64354=CARTESIAN_POINT('Ctrl Pts',(0.00476824448374763,-0.0317748838660338,
0.0788203195437703));
#64355=CARTESIAN_POINT('Ctrl Pts',(0.00479285771551602,-0.0317755400071257,
0.0788386103617786));
#64356=CARTESIAN_POINT('',(0.00487962717730369,-0.0318824481878404,0.0790279859746015));
#64357=CARTESIAN_POINT('Origin',(0.0136872527565295,-0.0332583300699954,
0.0740709772763413));
#64358=CARTESIAN_POINT('',(0.00508811528226063,-0.0317755397360895,0.0790349615609672));
#64359=CARTESIAN_POINT('Origin',(0.00574219388719208,-0.0326853491204695,
0.0694903982482642));
#64360=CARTESIAN_POINT('',(0.00524649845309392,-0.0317744765475852,0.0791286676667744));
#64361=CARTESIAN_POINT('Ctrl Pts',(0.00508811517077312,-0.0317755400678204,
0.0790349617631729));
#64362=CARTESIAN_POINT('Ctrl Pts',(0.00511450223846017,-0.0317748838918833,
0.0790505869516141));
#64363=CARTESIAN_POINT('Ctrl Pts',(0.00514089980569581,-0.0317744615156214,
0.0790662052465609));
#64364=CARTESIAN_POINT('Ctrl Pts',(0.00519369898120271,-0.0317741013466568,
0.0790974368791144));
#64365=CARTESIAN_POINT('Ctrl Pts',(0.00522010136427528,-0.0317741635377321,
0.079113050674707));
#64366=CARTESIAN_POINT('Ctrl Pts',(0.00524649845323109,-0.0317744765473204,
0.0791286676665479));
#64367=CARTESIAN_POINT('',(0.00540676174748558,-0.0317755400071255,0.079219114804191));
#64368=CARTESIAN_POINT('Ctrl Pts',(0.00524649845309391,-0.0317744765475852,
0.0791286676667744));
#64369=CARTESIAN_POINT('Ctrl Pts',(0.00527320878412476,-0.0317741635379398,
0.079143742644332));
#64370=CARTESIAN_POINT('Ctrl Pts',(0.00529991898931921,-0.0317741013468556,
0.0791588238050543));
#64371=CARTESIAN_POINT('Ctrl Pts',(0.00535333927914465,-0.0317744615102831,
0.0791889787957524));
#64372=CARTESIAN_POINT('Ctrl Pts',(0.00538005014810841,-0.0317748838659619,
0.0792040530690213));
#64373=CARTESIAN_POINT('Ctrl Pts',(0.00540676174748559,-0.0317755400071256,
0.079219114804191));
#64374=CARTESIAN_POINT('',(0.00551658206406282,-0.0318824481878402,0.079396122036523));
#64375=CARTESIAN_POINT('Origin',(0.0136334789566357,-0.0332583300695342,
0.0733743126384046));
#64376=CARTESIAN_POINT('',(0.0057243004508357,-0.0317755397360895,0.0793769121299523));
#64377=CARTESIAN_POINT('Origin',(0.00517697046763587,-0.0326853491204486,
0.0698256327630568));
#64378=CARTESIAN_POINT('',(0.00589317921230553,-0.0317744765475852,0.0794500286601838));
#64379=CARTESIAN_POINT('Ctrl Pts',(0.0057243003655704,-0.0317755400678203,
0.0793769123445366));
#64380=CARTESIAN_POINT('Ctrl Pts',(0.00575243771566211,-0.0317748838919551,
0.0793891071458487));
#64381=CARTESIAN_POINT('Ctrl Pts',(0.00578058462318907,-0.0317744615156049,
0.0794012937941031));
#64382=CARTESIAN_POINT('Ctrl Pts',(0.00583688488645091,-0.0317741013270408,
0.0794256629905367));
#64383=CARTESIAN_POINT('Ctrl Pts',(0.00586502988702687,-0.0317741635037327,
0.0794378419216701));
#64384=CARTESIAN_POINT('Ctrl Pts',(0.00589317921241321,-0.0317744765473204,
0.0794500286599419));
#64385=CARTESIAN_POINT('',(0.00606351481495193,-0.0317755400071256,0.079519676277999));
#64386=CARTESIAN_POINT('Ctrl Pts',(0.00589317921230552,-0.0317744765475851,
0.0794500286601838));
#64387=CARTESIAN_POINT('Ctrl Pts',(0.00592156832008162,-0.0317741635379398,
0.0794616370748831));
#64388=CARTESIAN_POINT('Ctrl Pts',(0.00594995807796962,-0.0317741013468556,
0.0794732516397625));
#64389=CARTESIAN_POINT('Ctrl Pts',(0.00600673655534851,-0.0317744615102831,
0.0794964735116913));
#64390=CARTESIAN_POINT('Ctrl Pts',(0.00603512610854758,-0.031774883865962,
0.0795080811602356));
#64391=CARTESIAN_POINT('Ctrl Pts',(0.0060635148149519,-0.0317755400071257,
0.079519676277999));
#64392=CARTESIAN_POINT('',(0.00619465405432301,-0.0318824481878401,0.0796815236200473));
#64393=CARTESIAN_POINT('Origin',(0.0134928139021324,-0.0332583300607513,
0.0726898810955411));
#64394=CARTESIAN_POINT('',(0.00639832687986726,-0.0317755397360895,0.0796364311722422));
#64395=CARTESIAN_POINT('Origin',(0.00465821950616128,-0.0326853484023168,
0.0702290644721585));
#64396=CARTESIAN_POINT('',(0.00657503791302196,-0.0317744765475852,0.0796878050355386));
#64397=CARTESIAN_POINT('Ctrl Pts',(0.00639832682216884,-0.0317755400678204,
0.0796364313958211));
#64398=CARTESIAN_POINT('Ctrl Pts',(0.00642777071795408,-0.0317748838918833,
0.0796450034933495));
#64399=CARTESIAN_POINT('Ctrl Pts',(0.00645722306908044,-0.0317744615156214,
0.079653566302823));
#64400=CARTESIAN_POINT('Ctrl Pts',(0.00651613045257276,-0.0317741013466568,
0.0796706861152094));
#64401=CARTESIAN_POINT('Ctrl Pts',(0.0065455863492945,-0.0317741635377321,
0.0796792433690345));
#64402=CARTESIAN_POINT('Ctrl Pts',(0.0065750379130985,-0.0317744765473203,
0.079687805035285));
#64403=CARTESIAN_POINT('',(0.00675275952971589,-0.0317755400071255,0.0797355547492138));
#64404=CARTESIAN_POINT('Ctrl Pts',(0.00657503791302196,-0.0317744765475852,
0.0796878050355386));
#64405=CARTESIAN_POINT('Ctrl Pts',(0.00660465808435497,-0.0317741635379398,
0.0796957638157452));
#64406=CARTESIAN_POINT('Ctrl Pts',(0.00663427967149549,-0.0317741013468556,
0.0797037286161553));
#64407=CARTESIAN_POINT('Ctrl Pts',(0.00669352090591582,-0.0317744615102831,
0.0797196511465201));
#64408=CARTESIAN_POINT('Ctrl Pts',(0.00672314142313093,-0.0317748838659618,
0.0797276091107857));
#64409=CARTESIAN_POINT('Ctrl Pts',(0.00675275952971588,-0.0317755400071256,
0.0797355547492138));
#64410=CARTESIAN_POINT('',(0.0069031495477372,-0.0318824481878401,0.0798796897717117));
#64411=CARTESIAN_POINT('Origin',(0.0132674760598083,-0.0332583300604723,
0.072028476464189));
#64412=CARTESIAN_POINT('',(0.00709956476929273,-0.0317755397364821,0.079809425917849));
#64413=CARTESIAN_POINT('Origin',(0.00419412357676368,-0.0326853491206543,
0.0706943329874522));
#64414=CARTESIAN_POINT('',(0.00728132123621136,-0.0317744765475735,0.0798382469173586));
#64415=CARTESIAN_POINT('Ctrl Pts',(0.00709956474006579,-0.0317755400683136,
0.0798094261469438));
#64416=CARTESIAN_POINT('Ctrl Pts',(0.00712985083066187,-0.0317748838922172,
0.0798142403521005));
#64417=CARTESIAN_POINT('Ctrl Pts',(0.00716014414620153,-0.0317744615158801,
0.0798190442828555));
#64418=CARTESIAN_POINT('Ctrl Pts',(0.00722073270871306,-0.0317741013468555,
0.079828646047477));
#64419=CARTESIAN_POINT('Ctrl Pts',(0.0072510288455948,-0.0317741635379398,
0.0798334440220898));
#64420=CARTESIAN_POINT('Ctrl Pts',(0.0072813212362112,-0.0317744765475852,
0.0798382469173588));
#64421=CARTESIAN_POINT('',(0.0074636260908907,-0.0317755400071255,0.0798633456853848));
#64422=CARTESIAN_POINT('Ctrl Pts',(0.00728132123621146,-0.0317744765475851,
0.0798382469173587));
#64423=CARTESIAN_POINT('Ctrl Pts',(0.00731170534173171,-0.031774163537956,
0.0798424305481377));
#64424=CARTESIAN_POINT('Ctrl Pts',(0.00734209160632505,-0.0317741013468101,
0.0798466199741871));
#64425=CARTESIAN_POINT('Ctrl Pts',(0.00740286133299313,-0.0317744615102666,
0.0798549920558435));
#64426=CARTESIAN_POINT('Ctrl Pts',(0.00743324568268853,-0.0317748838660336,
0.0798591748342155));
#64427=CARTESIAN_POINT('Ctrl Pts',(0.00746362609089069,-0.0317755400071256,
0.0798633456853848));
#64428=CARTESIAN_POINT('',(0.00763089514713966,-0.0318824481878402,0.0799874952929255));
#64429=CARTESIAN_POINT('Origin',(0.0129610190916437,-0.0332583300609749,
0.0714005295268761));
#64430=CARTESIAN_POINT('',(0.00781695517999998,-0.0317755397364822,0.079893168135698));
#64431=CARTESIAN_POINT('Origin',(0.00379200018792774,-0.0326853491206267,
0.0712140987753191));
#64432=CARTESIAN_POINT('Ctrl Pts',(0.0078169551797167,-0.0317755400683137,
0.0798931683666495));
#64433=CARTESIAN_POINT('Ctrl Pts',(0.00784760582917376,-0.0317748838923494,
0.0798941487564968));
#64434=CARTESIAN_POINT('Ctrl Pts',(0.00787826236822532,-0.0317744615158499,
0.0798951180477344));
#64435=CARTESIAN_POINT('Ctrl Pts',(0.00793957660105809,-0.0317741013467719,
0.0798970503394014));
#64436=CARTESIAN_POINT('Ctrl Pts',(0.00797023518641224,-0.0317741635379696,
0.0798980133676535));
#64437=CARTESIAN_POINT('Ctrl Pts',(0.00800089067195264,-0.0317744765475852,
0.079898981747298));
#64438=CARTESIAN_POINT('Origin',(0.00812378219310841,-0.0355241814719619,
0.07415));
#64439=CARTESIAN_POINT('',(0.00808309105517532,-0.0351949306059337,0.0683208911579615));
#64440=CARTESIAN_POINT('',(0.00812378219275222,-0.0351704285080635,0.0682962470361016));
#64441=CARTESIAN_POINT('Ctrl Pts',(0.00812378219239603,-0.0351704285080635,
0.0682962470361016));
#64442=CARTESIAN_POINT('Ctrl Pts',(0.00811019485630785,-0.0351786035562758,
0.0683044220843155));
#64443=CARTESIAN_POINT('Ctrl Pts',(0.00809663611840715,-0.0351867679503489,
0.0683126337499256));
#64444=CARTESIAN_POINT('Ctrl Pts',(0.00808309105565127,-0.035194930606244,
0.0683208911584355));
#64445=CARTESIAN_POINT('',(0.00812378219310841,-0.0355241814719745,0.0686500000000126));
#64446=CARTESIAN_POINT('',(0.00812378219310841,-0.0355241814719619,0.06865));
#64447=CARTESIAN_POINT('Origin',(0.00812378219311841,-0.0355241814719719,
0.07415000000001));
#64448=CARTESIAN_POINT('',(0.00825051023896004,-0.035094370708599,0.0682215435661843));
#64449=CARTESIAN_POINT('Ctrl Pts',(0.00825051024267582,-0.035094370714152,
0.0682215435714773));
#64450=CARTESIAN_POINT('Ctrl Pts',(0.00822342491110835,-0.0351105857202016,
0.0682371832994888));
#64451=CARTESIAN_POINT('Ctrl Pts',(0.00819642805189303,-0.0351267738254377,
0.0682529789241719));
#64452=CARTESIAN_POINT('Ctrl Pts',(0.00815423794672532,-0.035152112510921,
0.0682779903654756));
#64453=CARTESIAN_POINT('Ctrl Pts',(0.00813899690518094,-0.035161274321419,
0.0682870928494552));
#64454=CARTESIAN_POINT('Ctrl Pts',(0.00812378219239603,-0.0351704285080635,
0.0682962470361016));
#64455=CARTESIAN_POINT('',(0.0084138644635775,-0.035195137125492,0.0683281780970644));
#64456=CARTESIAN_POINT('Origin',(0.00335368224046308,-0.0338370705272818,
0.0771371906830081));
#64457=CARTESIAN_POINT('',(0.00842661992254915,-0.0352722979006255,0.0684060942064975));
#64458=CARTESIAN_POINT('Origin',(0.0137020032039043,-0.0346069579033217,
0.0681231525239146));
#64459=CARTESIAN_POINT('',(0.00860741083993109,-0.0352740680168103,0.0684201085860881));
#64460=CARTESIAN_POINT('Origin',(0.00861719186418346,-0.0305802162291841,
0.06765606648571));
#64461=CARTESIAN_POINT('',(0.00878811029711487,-0.0352728165321731,0.0684371314675367));
#64462=CARTESIAN_POINT('Origin',(0.0085644044276215,-0.0288496123715138,
0.069309525093856));
#64463=CARTESIAN_POINT('',(0.00881399297514621,-0.0351949306052073,0.0683617554737295));
#64464=CARTESIAN_POINT('Ctrl Pts',(0.00878811029168475,-0.0352728165303531,
0.0684371314675542));
#64465=CARTESIAN_POINT('Ctrl Pts',(0.00879672353338646,-0.0352468764909534,
0.068412018231727));
#64466=CARTESIAN_POINT('Ctrl Pts',(0.00880535111903101,-0.0352209141752707,
0.0683868926325456));
#64467=CARTESIAN_POINT('Ctrl Pts',(0.00881399297658388,-0.035194930607398,
0.0683617554719593));
#64468=CARTESIAN_POINT('',(0.00899254353630529,-0.0350943706855873,0.0682841744236151));
#64469=CARTESIAN_POINT('Origin',(0.0123257004762265,-0.0338370705480914,
0.0778944685611667));
#64470=CARTESIAN_POINT('',(0.00914124484256304,-0.0351951371254925,0.06841044185062));
#64471=CARTESIAN_POINT('Origin',(0.00301690163542675,-0.0338370705272569,
0.076515783741189));
#64472=CARTESIAN_POINT('',(0.00914413424298837,-0.0352722979006256,0.0684893422511767));
#64473=CARTESIAN_POINT('Origin',(0.0144133815475748,-0.0346069579035747,
0.0688698124929622));
#64474=CARTESIAN_POINT('',(0.00932174310247744,-0.0352740680168102,0.0685259052334733));
#64475=CARTESIAN_POINT('Origin',(0.00942720686743619,-0.0305802162290654,
0.0677691137207357));
#64476=CARTESIAN_POINT('',(0.00949888415769095,-0.035272816532173,0.0685654415316891));
#64477=CARTESIAN_POINT('Origin',(0.00916760236170185,-0.0288496123710761,
0.0694029182935395));
#64478=CARTESIAN_POINT('',(0.00953400986011256,-0.0351949306052073,0.0684939038598372));
#64479=CARTESIAN_POINT('Ctrl Pts',(0.00949888415230144,-0.0352728165303531,
0.0685654415310259));
#64480=CARTESIAN_POINT('Ctrl Pts',(0.00951057699907121,-0.0352468764909533,
0.068541605845998));
#64481=CARTESIAN_POINT('Ctrl Pts',(0.0095222856262167,-0.0352209141752705,
0.0685177596928773));
#64482=CARTESIAN_POINT('Ctrl Pts',(0.00953400986176051,-0.0351949306073977,
0.0684939038582614));
#64483=CARTESIAN_POINT('',(0.00972087598064153,-0.0350943706855873,0.0684393128786594));
#64484=CARTESIAN_POINT('Origin',(0.0118232607428322,-0.0338370705484021,
0.0783915823134132));
#64485=CARTESIAN_POINT('',(0.00985257922776396,-0.035195137125493,0.0685832218648373));
#64486=CARTESIAN_POINT('Origin',(0.00276065961398387,-0.0338370705322628,
0.0758570669485549));
#64487=CARTESIAN_POINT('',(0.00984555700207224,-0.0352722979006258,0.068661862250068));
#64488=CARTESIAN_POINT('Origin',(0.0150255691519021,-0.0346069579032499,
0.0696997441737871));
#64489=CARTESIAN_POINT('',(0.010017182805856,-0.0352740680168101,0.0687203972149985));
#64490=CARTESIAN_POINT('Origin',(0.0102166660849917,-0.0305802162292844,
0.0679827913439425));
#64491=CARTESIAN_POINT('',(0.0101879718388395,-0.035272816532173,0.0687818234189402));
#64492=CARTESIAN_POINT('Origin',(0.00975433862813941,-0.0288496123715215,
0.069571175807738));
#64493=CARTESIAN_POINT('',(0.0102317866123413,-0.0351949306052074,0.0687152522608634));
#64494=CARTESIAN_POINT('Ctrl Pts',(0.0101879718335757,-0.035272816530353,
0.0687818234176067));
#64495=CARTESIAN_POINT('Ctrl Pts',(0.010202559882235,-0.0352468764909531,
0.0687596411863698));
#64496=CARTESIAN_POINT('Ctrl Pts',(0.010217164898837,-0.0352209141752703,
0.0687374505473897));
#64497=CARTESIAN_POINT('Ctrl Pts',(0.0102317866141735,-0.0351949306073974,
0.0687152522595068));
#64498=CARTESIAN_POINT('',(0.010424021301891,-0.0350943706855873,0.0686845122810066));
#64499=CARTESIAN_POINT('Origin',(0.0112624780227344,-0.0338370705483178,
0.0788218037795066));
#64500=CARTESIAN_POINT('',(0.0105366494509951,-0.0351951371254935,0.0688437932956783));
#64501=CARTESIAN_POINT('Origin',(0.00258899722437033,-0.0338370705329863,
0.0751714287151622));
#64502=CARTESIAN_POINT('',(0.0105198263438801,-0.0352722979006259,0.0689209334597304));
#64503=CARTESIAN_POINT('Origin',(0.0155289113492698,-0.0346069579166609,
0.0705998590110601));
#64504=CARTESIAN_POINT('',(0.0106827624505072,-0.0352740680168103,0.0690005172759302));
#64505=CARTESIAN_POINT('Origin',(0.010973119273292,-0.0305802162291668,
0.0682937295319573));
#64506=CARTESIAN_POINT('',(0.0108445060161877,-0.0352728165321731,0.069082864657668));
#64507=CARTESIAN_POINT('Origin',(0.0103153600492251,-0.0288496124320004,
0.0698116441084991));
#64508=CARTESIAN_POINT('',(0.0108963188756178,-0.0351949306052075,0.0690223098802967));
#64509=CARTESIAN_POINT('Ctrl Pts',(0.0108445060111324,-0.0352728165303531,
0.0690828646556853));
#64510=CARTESIAN_POINT('Ctrl Pts',(0.0108617591994395,-0.0352468764909531,
0.0690626857052769));
#64511=CARTESIAN_POINT('Ctrl Pts',(0.0108790302756615,-0.0352209141752702,
0.0690425005400701));
#64512=CARTESIAN_POINT('Ctrl Pts',(0.0108963188776054,-0.0351949306073972,
0.0690223098791807));
#64513=CARTESIAN_POINT('',(0.0110908904782989,-0.0350943706855873,0.0690159056896065));
#64514=CARTESIAN_POINT('Origin',(0.0106521961942472,-0.0338370705480734,
0.0791783481085643));
#64515=CARTESIAN_POINT('',(0.0111826673161923,-0.0351951371254939,0.0691880467760207));
#64516=CARTESIAN_POINT('Origin',(0.00250462165323249,-0.0338370705271412,
0.0744696819722123));
#64517=CARTESIAN_POINT('',(0.0111563086381029,-0.0352722979006261,0.0692624701724259));
#64518=CARTESIAN_POINT('Origin',(0.0159154704425166,-0.0346069579032674,
0.0715559617640655));
#64519=CARTESIAN_POINT('',(0.0113079854478385,-0.0352740680168103,0.0693618477555725));
#64520=CARTESIAN_POINT('Origin',(0.0116846367137315,-0.0305802162290746,
0.0686970246035787));
#64521=CARTESIAN_POINT('',(0.0114581327535644,-0.035272816532173,0.0694638176477042));
#64522=CARTESIAN_POINT('Origin',(0.0108418189710028,-0.0288496123714861,
0.0701205308855496));
#64523=CARTESIAN_POINT('',(0.0115171265791785,-0.0351949306052074,0.0694102342360514));
#64524=CARTESIAN_POINT('Ctrl Pts',(0.0114581327487975,-0.0352728165303531,
0.0694638176451035));
#64525=CARTESIAN_POINT('Ctrl Pts',(0.0114777789836662,-0.0352468764909529,
0.069445960209626));
#64526=CARTESIAN_POINT('Ctrl Pts',(0.0114974437443192,-0.0352209141752698,
0.0694280988503058));
#64527=CARTESIAN_POINT('Ctrl Pts',(0.01151712658129,-0.0351949306073967,
0.0694102342351935));
#64528=CARTESIAN_POINT('',(0.011710966584585,-0.0350943706855873,0.0694282668324408));
#64529=CARTESIAN_POINT('Origin',(0.0100020397743013,-0.0338370705544373,
0.0794555923382736));
#64530=CARTESIAN_POINT('',(0.0117804447357093,-0.0351951371254944,0.0696105532228325));
#64531=CARTESIAN_POINT('Origin',(0.00250886368030171,-0.0338370705332249,
0.0737628936041924));
#64532=CARTESIAN_POINT('',(0.0117449661787447,-0.0352722979006265,0.0696810861501711));
#64533=CARTESIAN_POINT('Origin',(0.0161791498534244,-0.0346069579034337,
0.0725529740133547));
#64534=CARTESIAN_POINT('',(0.0118829916576916,-0.0352740680168101,0.0697986902564126));
#64535=CARTESIAN_POINT('Origin',(0.0123399973512426,-0.0305802162291525,
0.0691863163546208));
#64536=CARTESIAN_POINT('',(0.0120191747907581,-0.0352728165321731,0.0699186745328258));
#64537=CARTESIAN_POINT('Origin',(0.0113254128382053,-0.0288496124326838,
0.0704929647860157));
#64538=CARTESIAN_POINT('',(0.0120844192146853,-0.0351949306052073,0.0698729075293024));
#64539=CARTESIAN_POINT('Ctrl Pts',(0.0120191747863548,-0.0352728165303531,
0.0699186745296482));
#64540=CARTESIAN_POINT('Ctrl Pts',(0.0120409042349252,-0.0352468764909528,
0.0699034202315265));
#64541=CARTESIAN_POINT('Ctrl Pts',(0.0120626525549864,-0.0352209141752695,
0.0698881643623993));
#64542=CARTESIAN_POINT('Ctrl Pts',(0.0120844192168873,-0.0351949306073962,
0.0698729075287162));
#64543=CARTESIAN_POINT('',(0.0122744706501375,-0.0350943706855873,0.0699150925279542));
#64544=CARTESIAN_POINT('Origin',(0.00932226209534658,-0.0338370705483705,
0.0796491642990803));
#64545=CARTESIAN_POINT('',(0.012320554402545,-0.0351951371254947,0.0701046494570542));
#64546=CARTESIAN_POINT('Origin',(0.00260165624639857,-0.0338370705282117,
0.073062210172673));
#64547=CARTESIAN_POINT('',(0.0122765154847423,-0.0352722979006269,0.0701701795689278));
#64548=CARTESIAN_POINT('Origin',(0.0163157913041077,-0.0346069579032108,
0.0735751723167505));
#64549=CARTESIAN_POINT('',(0.0123987128886455,-0.0352740680168101,0.0703041555112558));
#64550=CARTESIAN_POINT('Origin',(0.0129288657570403,-0.0305802162290188,
0.0697538883619407));
#64551=CARTESIAN_POINT('',(0.0125187841596924,-0.035272816532173,0.070440261948236));
#64552=CARTESIAN_POINT('Origin',(0.0117585150668984,-0.0288496123714419,
0.0709230723270721));
#64553=CARTESIAN_POINT('',(0.0125892502383923,-0.035194930605207,0.0704030331258278));
#64554=CARTESIAN_POINT('Ctrl Pts',(0.012518784155722,-0.035272816530353,
0.0704402619445316));
#64555=CARTESIAN_POINT('Ctrl Pts',(0.0125422541316097,-0.0352468764909525,
0.0704278513531597));
#64556=CARTESIAN_POINT('Ctrl Pts',(0.0125657430270801,-0.035220914175269,
0.070415441568395));
#64557=CARTESIAN_POINT('Ctrl Pts',(0.0125892502406501,-0.0351949306073955,
0.0704030331255223));
#64558=CARTESIAN_POINT('',(0.0127725158792218,-0.0350943706855873,0.0704687052441133));
#64559=CARTESIAN_POINT('Origin',(0.00862358367950969,-0.0338370705479122,
0.0797560111077919));
#64560=CARTESIAN_POINT('',(0.012794478464608,-0.0351951371254951,0.0706625432859136));
#64561=CARTESIAN_POINT('Origin',(0.002781536070095,-0.0338370705270207,
0.0723786818205332));
#64562=CARTESIAN_POINT('',(0.0127425737060082,-0.0352722979006273,0.0707220371333118));
#64563=CARTESIAN_POINT('Origin',(0.01632323987826,-0.0346069579035876,0.0746064359959854));
#64564=CARTESIAN_POINT('',(0.0128470159088111,-0.0352740680168102,0.0708702720310826));
#64565=CARTESIAN_POINT('Origin',(0.013441955124631,-0.0305802162290379,
0.0703907896758804));
#64566=CARTESIAN_POINT('',(0.0129490817221664,-0.0352728165321731,0.0710203541488127));
#64567=CARTESIAN_POINT('Origin',(0.0121342953984036,-0.0288496124323702,
0.0714040704362385));
#64568=CARTESIAN_POINT('',(0.0130236581634837,-0.0351949306052069,0.0709922506282884));
#64569=CARTESIAN_POINT('Ctrl Pts',(0.0129490817186916,-0.0352728165303531,
0.0710203541446399));
#64570=CARTESIAN_POINT('Ctrl Pts',(0.0129739220863566,-0.0352468764909524,
0.0710109829824574));
#64571=CARTESIAN_POINT('Ctrl Pts',(0.0129987811233229,-0.0352209141752687,
0.0710016149917742));
#64572=CARTESIAN_POINT('Ctrl Pts',(0.0130236581657616,-0.035194930607395,
0.0709922506282686));
#64573=CARTESIAN_POINT('',(0.0131972478006323,-0.0350943706857667,0.0710803741771032));
#64574=CARTESIAN_POINT('Origin',(0.00791702309657988,-0.0338370705483001,
0.0797744477714516));
#64575=CARTESIAN_POINT('',(0.0131947428563309,-0.0351951371254954,0.0712754363904597));
#64576=CARTESIAN_POINT('Origin',(0.003045666357819,-0.0338370705334225,
0.0717230882096386));
#64577=CARTESIAN_POINT('',(0.0131357908259834,-0.0352722979006277,0.0713279557198694));
#64578=CARTESIAN_POINT('Origin',(0.0162013781061114,-0.0346069579034164,
0.075630501407276));
#64579=CARTESIAN_POINT('',(0.0132208307117569,-0.0352740680168102,0.0714881118201936));
#64580=CARTESIAN_POINT('Origin',(0.0138711737281729,-0.0305802162290074,
0.0710869759822714));
#64581=CARTESIAN_POINT('',(0.0133032814285732,-0.035272816532173,0.0716498027340223));
#64582=CARTESIAN_POINT('Origin',(0.012446827528811,-0.0288496123715279,
0.0719283735020433));
#64583=CARTESIAN_POINT('',(0.0133807921174785,-0.0351949306052067,0.0716312677246893));
#64584=CARTESIAN_POINT('Ctrl Pts',(0.0133032814256488,-0.035272816530353,
0.0716498027294469));
#64585=CARTESIAN_POINT('Ctrl Pts',(0.013329100437654,-0.0352468764909521,
0.0716436187852796));
#64586=CARTESIAN_POINT('Ctrl Pts',(0.0133549375742533,-0.0352209141752683,
0.0716374403274873));
#64587=CARTESIAN_POINT('Ctrl Pts',(0.0133807921197406,-0.0351949306073944,
0.0716312677249552));
#64588=CARTESIAN_POINT('',(0.013541968139514,-0.0350943706855873,0.0717404529441539));
#64589=CARTESIAN_POINT('Origin',(0.00721372322735028,-0.0338370705482336,
0.0797041835349999));
#64590=CARTESIAN_POINT('',(0.0135150351691498,-0.0351951371254956,0.0719336630803094));
#64591=CARTESIAN_POINT('Origin',(0.00338988147407706,-0.0338370705268427,
0.0711057684529389));
#64592=CARTESIAN_POINT('',(0.0134499655757892,-0.0352722979006282,0.0719783796305319));
#64593=CARTESIAN_POINT('Origin',(0.0159521278207605,-0.0346069579033098,
0.0766312184265049));
#64594=CARTESIAN_POINT('',(0.0135142620147343,-0.0352740680168101,0.072147931176035));
#64595=CARTESIAN_POINT('Origin',(0.0142097525339431,-0.0305802162291656,
0.0718314680071569));
#64596=CARTESIAN_POINT('',(0.0135757973379538,-0.035272816532173,0.072318680923662));
#64597=CARTESIAN_POINT('Origin',(0.0126911826582227,-0.0288496123714389,
0.0724877129411867));
#64598=CARTESIAN_POINT('',(0.0136550198845806,-0.0351949306052065,0.0723100067336897));
#64599=CARTESIAN_POINT('Ctrl Pts',(0.0135757973356259,-0.035272816530353,
0.0723186809187561));
#64600=CARTESIAN_POINT('Ctrl Pts',(0.0136021878107285,-0.0352468764909519,
0.0723157817170976));
#64601=CARTESIAN_POINT('Ctrl Pts',(0.0136285955798824,-0.0352209141752679,
0.0723128902301664));
#64602=CARTESIAN_POINT('Ctrl Pts',(0.0136550198867911,-0.0351949306073937,
0.0723100067342372));
#64603=CARTESIAN_POINT('',(0.0138012404489288,-0.0350943706855873,0.0724385317071006));
#64604=CARTESIAN_POINT('Origin',(0.00652477553238292,-0.0338370705485876,
0.0795463265056502));
#64605=CARTESIAN_POINT('',(0.0137503042019585,-0.0351951371254957,0.0726268427273582));
#64606=CARTESIAN_POINT('Origin',(0.00380875312443852,-0.0338370705334268,
0.0705364580523133));
#64607=CARTESIAN_POINT('',(0.0136801432319426,-0.0352722979006287,0.0726630512916841));
#64608=CARTESIAN_POINT('Origin',(0.0155794198489981,-0.0346069579034531,
0.0775928051493414));
#64609=CARTESIAN_POINT('',(0.0137226822308082,-0.0352740680168101,0.0728393243532072));
#64610=CARTESIAN_POINT('Origin',(0.0144523519517679,-0.030580216229071,
0.072612524666635));
#64611=CARTESIAN_POINT('',(0.0137623317116241,-0.035272816532173,0.0730164401091124));
#64612=CARTESIAN_POINT('Origin',(0.0128635071531246,-0.0288496123714632,
0.0730732676405112));
#64613=CARTESIAN_POINT('',(0.013842016729087,-0.0351949306052061,0.0730177635356588));
#64614=CARTESIAN_POINT('Ctrl Pts',(0.0137623317099295,-0.035272816530353,
0.0730164401039535));
#64615=CARTESIAN_POINT('Ctrl Pts',(0.0137888774545723,-0.0352468764909517,
0.0730168713669459));
#64616=CARTESIAN_POINT('Ctrl Pts',(0.0138154393899859,-0.0352209141752674,
0.0730173124513521));
#64617=CARTESIAN_POINT('Ctrl Pts',(0.0138420167312112,-0.035194930607393,
0.0730177635364791));
#64618=CARTESIAN_POINT('',(0.0139709758501003,-0.0350943706855873,0.0731636013474081));
#64619=CARTESIAN_POINT('Origin',(0.00586104512645934,-0.0338370705482262,
0.0793033661844569));
#64620=CARTESIAN_POINT('',(0.0138968396215665,-0.0351951371254958,0.0733440434744868));
#64621=CARTESIAN_POINT('Origin',(0.00429567531282297,-0.0338370705328629,
0.070024135363444));
#64622=CARTESIAN_POINT('',(0.0138226937553044,-0.0352722979006292,0.0733711730222263));
#64623=CARTESIAN_POINT('Origin',(0.0150891320168613,-0.0346069579032025,
0.0785000967776752));
#64624=CARTESIAN_POINT('',(0.0138428044486668,-0.0352740680168103,0.0735513876682886));
#64625=CARTESIAN_POINT('Origin',(0.0145951460440602,-0.0305802162291541,
0.0734178282305441));
#64626=CARTESIAN_POINT('',(0.0138599427910812,-0.0352728165321731,0.073732076211198));
#64627=CARTESIAN_POINT('Origin',(0.0129610833543958,-0.0288496123719289,
0.073675803052224));
#64628=CARTESIAN_POINT('',(0.0139388335990533,-0.0351949306052057,0.0737433763830361));
#64629=CARTESIAN_POINT('Ctrl Pts',(0.0138599427900465,-0.0352728165303531,
0.0737320762058673));
#64630=CARTESIAN_POINT('Ctrl Pts',(0.013886225161979,-0.0352468764909514,
0.0737358311322358));
#64631=CARTESIAN_POINT('Ctrl Pts',(0.0139125223660635,-0.0352209141752669,
0.0737395978318148));
#64632=CARTESIAN_POINT('Ctrl Pts',(0.0139388336010576,-0.0351949306073923,
0.0737433763841162));
#64633=CARTESIAN_POINT('',(0.0140484975143569,-0.0350943706855873,0.0739042270837131));
#64634=CARTESIAN_POINT('Origin',(0.00523299947751265,-0.033837070554829,
0.0789791341757105));
#64635=CARTESIAN_POINT('',(0.0139523304768704,-0.0351951371254958,0.074073954637478));
#64636=CARTESIAN_POINT('Origin',(0.00484296903637281,-0.0338370705331573,
0.0695768800252357));
#64637=CARTESIAN_POINT('',(0.0138753690389657,-0.0352722979006297,0.0740915773194568));
#64638=CARTESIAN_POINT('Origin',(0.0144889964576451,-0.0346069579032552,
0.0793387847816124));
#64639=CARTESIAN_POINT('',(0.0138727342691775,-0.0352740680168102,0.0742728914574353));
#64640=CARTESIAN_POINT('Origin',(0.0146358828626028,-0.0305802162292082,
0.0742346785806469));
#64641=CARTESIAN_POINT('',(0.0138670911912921,-0.035272816532173,0.0744543032210886));
#64642=CARTESIAN_POINT('Origin',(0.0129823724269125,-0.0288496123714457,
0.0742858168330627));
#64643=CARTESIAN_POINT('',(0.0139439436346045,-0.0351949306052053,0.0744754019277582));
#64644=CARTESIAN_POINT('Ctrl Pts',(0.0138670911909336,-0.035272816530353,
0.0744543032156703));
#64645=CARTESIAN_POINT('Ctrl Pts',(0.0138926957014499,-0.0352468764909512,
0.0744613225879828));
#64646=CARTESIAN_POINT('Ctrl Pts',(0.0139183134515877,-0.0352209141752664,
0.0744683554996323));
#64647=CARTESIAN_POINT('Ctrl Pts',(0.0139439436364572,-0.0351949306073916,
0.0744754019290811));
#64648=CARTESIAN_POINT('',(0.0140325828787443,-0.0350943706855873,0.0746487288057257));
#64649=CARTESIAN_POINT('Origin',(0.0046505431174405,-0.0338370705478985,
0.078578743883373));
#64650=CARTESIAN_POINT('',(0.0139159016439338,-0.0351951371254958,0.0748050650812635));
#64651=CARTESIAN_POINT('Origin',(0.0054420031031212,-0.0338370705270375,
0.0692017454954627));
#64652=CARTESIAN_POINT('',(0.0138373383622366,-0.0352722979006302,0.0748129029772593));
#64653=CARTESIAN_POINT('Origin',(0.0137884776670116,-0.0346069579032201,
0.0800956425500761));
#64654=CARTESIAN_POINT('',(0.0138119996811912,-0.0352740680168102,0.0749924571748874));
#64655=CARTESIAN_POINT('Origin',(0.0145739199633192,-0.0305802162289763,
0.075050193498937));
#64656=CARTESIAN_POINT('',(0.0137836641777151,-0.035272816532173,0.0751717311874006));
#64657=CARTESIAN_POINT('Origin',(0.0129270386287473,-0.0288496123715092,
0.0748936887013136));
#64658=CARTESIAN_POINT('',(0.0138572662474272,-0.035194930605205,0.0752022956896942));
#64659=CARTESIAN_POINT('Ctrl Pts',(0.0137836641780386,-0.035272816530353,
0.0751717311819801));
#64660=CARTESIAN_POINT('Ctrl Pts',(0.0138081870287124,-0.035246876490951,
0.0751819043005423));
#64661=CARTESIAN_POINT('Ctrl Pts',(0.0138327213176805,-0.035220914175266,
0.0751920925110443));
#64662=CARTESIAN_POINT('Ctrl Pts',(0.0138572662490992,-0.035194930607391,
0.0752022956912388));
#64663=CARTESIAN_POINT('',(0.0139234829265729,-0.0350943706855873,0.075385365276546));
#64664=CARTESIAN_POINT('Origin',(0.00412286189794218,-0.0338370705537578,
0.0781085096178728));
#64665=CARTESIAN_POINT('',(0.0137881276272134,-0.0351951371254958,0.0755258447574009));
#64666=CARTESIAN_POINT('Origin',(0.00608333050192936,-0.033837070532533,
0.0689046479421592));
#64667=CARTESIAN_POINT('',(0.0137092014916075,-0.0352722979006308,0.0755237742591112));
#64668=CARTESIAN_POINT('Origin',(0.0129986232703443,-0.0346069579246078,
0.0807587338069652));
#64669=CARTESIAN_POINT('',(0.013661558505442,-0.03527406801681,0.0756987368394292));
#64670=CARTESIAN_POINT('Origin',(0.0144102345384795,-0.0305802162291997,
0.0758515118280225));
#64671=CARTESIAN_POINT('',(0.0136109774441913,-0.0352728165321729,0.0758730458425347));
#64672=CARTESIAN_POINT('Origin',(0.0127959546074294,-0.0288496123713882,
0.0754898321545026));
#64673=CARTESIAN_POINT('',(0.0136801683916959,-0.0351949306052046,0.0759125941199928));
#64674=CARTESIAN_POINT('Ctrl Pts',(0.0136109774451917,-0.0352728165303529,
0.0758730458371975));
#64675=CARTESIAN_POINT('Ctrl Pts',(0.0136340318960186,-0.0352468764909507,
0.0758862122658525));
#64676=CARTESIAN_POINT('Ctrl Pts',(0.0136570958034239,-0.0352209141752656,
0.0758993951010413));
#64677=CARTESIAN_POINT('Ctrl Pts',(0.0136801683931609,-0.0351949306073904,
0.0759125941217349));
#64678=CARTESIAN_POINT('',(0.0137229182292617,-0.0350943706855873,0.076102519298984));
#64679=CARTESIAN_POINT('Origin',(0.00365827753959396,-0.0338370705548003,
0.0775758473097735));
#64680=CARTESIAN_POINT('',(0.0135710234992816,-0.0351951371254955,0.0762249265398243));
#64681=CARTESIAN_POINT('Origin',(0.00675683701100066,-0.0338370705333701,
0.0686902727050293));
#64682=CARTESIAN_POINT('',(0.0134929792220735,-0.0352722979006312,0.0762129803002442));
#64683=CARTESIAN_POINT('Origin',(0.0121318897028376,-0.0346069579193411,
0.0813176016052952));
#64684=CARTESIAN_POINT('',(0.0134237832891401,-0.03527406801681,0.0763805919988452));
#64685=CARTESIAN_POINT('Origin',(0.0141474080046922,-0.0305802162291773,
0.0766259962991262));
#64686=CARTESIAN_POINT('',(0.0133517543636662,-0.0352728165321731,0.0765471870354345));
#64687=CARTESIAN_POINT('Origin',(0.0125911876422138,-0.0288496124320617,
0.0760648456574108));
#64688=CARTESIAN_POINT('',(0.0134154430063885,-0.0351949306052041,0.0765950953880969));
#64689=CARTESIAN_POINT('Ctrl Pts',(0.0133517543653276,-0.0352728165303531,
0.0765471870302647));
#64690=CARTESIAN_POINT('Ctrl Pts',(0.0133729768338461,-0.0352468764909506,
0.0765631391265675));
#64691=CARTESIAN_POINT('Ctrl Pts',(0.0133942066280911,-0.0352209141752652,
0.0765791086852571));
#64692=CARTESIAN_POINT('Ctrl Pts',(0.0134154430076234,-0.0351949306073897,
0.0765950953900088));
#64693=CARTESIAN_POINT('',(0.0134340518118987,-0.0350943706855873,0.0767888809256985));
#64694=CARTESIAN_POINT('Origin',(0.0032641168098965,-0.0338370705480144,
0.0769891573437204));
#64695=CARTESIAN_POINT('',(0.0132680131219274,-0.0351951371254952,0.076891285491214));
#64696=CARTESIAN_POINT('Origin',(0.0074519010555576,-0.0338370705327029,
0.0685620006219173));
#64697=CARTESIAN_POINT('',(0.0131920815079901,-0.0352722979006317,0.0768696519096777));
#64698=CARTESIAN_POINT('Origin',(0.0112019458402663,-0.0346069579032916,
0.0817634321243535));
#64699=CARTESIAN_POINT('',(0.0131024238894872,-0.03527406801681,0.0770272693899471));
#64700=CARTESIAN_POINT('Origin',(0.0137895852935984,-0.0305802162292673,
0.0773614328295466));
#64701=CARTESIAN_POINT('',(0.0130100830389724,-0.035272816532173,0.0771835231567753));
#64702=CARTESIAN_POINT('Origin',(0.0123159670119983,-0.0288496123715262,
0.0766096608940125));
#64703=CARTESIAN_POINT('',(0.0130672649689706,-0.0351949306052037,0.0772390360413014));
#64704=CARTESIAN_POINT('Ctrl Pts',(0.0130100830412686,-0.035272816530353,
0.0771835231518545));
#64705=CARTESIAN_POINT('Ctrl Pts',(0.0130291388364723,-0.0352468764909504,
0.0772020093417171));
#64706=CARTESIAN_POINT('Ctrl Pts',(0.0130481997110196,-0.0352209141752648,
0.0772205137744273));
#64707=CARTESIAN_POINT('Ctrl Pts',(0.0130672649699559,-0.0351949306073892,
0.0772390360433531));
#64708=CARTESIAN_POINT('',(0.0130614392704462,-0.0350943706855874,0.0774336258238241));
#64709=CARTESIAN_POINT('Origin',(0.00294659599916159,-0.0338370705541986,
0.076357692168123));
#64710=CARTESIAN_POINT('',(0.0128838751498114,-0.0351951371254949,0.077514412732843));
#64711=CARTESIAN_POINT('Origin',(0.00815756107015764,-0.0338370705324253,
0.0685218546307288));
#64712=CARTESIAN_POINT('',(0.012811253686056,-0.0352722979006321,0.0774834329838542));
#64713=CARTESIAN_POINT('Origin',(0.0102234575330089,-0.034606957902553,
0.0820891941414742));
#64714=CARTESIAN_POINT('',(0.0127025483361862,-0.03527406801681,0.0776285705239727));
#64715=CARTESIAN_POINT('Origin',(0.0133424094829901,-0.0305802162293828,
0.0780462231458248));
#64716=CARTESIAN_POINT('',(0.0125913518310046,-0.035272816532173,0.0777720188057947));
#64717=CARTESIAN_POINT('Origin',(0.0119746331291439,-0.0288496123712106,
0.0771156858121774));
#64718=CARTESIAN_POINT('',(0.0126411252550837,-0.0351949306052034,0.0778342607508339));
#64719=CARTESIAN_POINT('Ctrl Pts',(0.0125913518338994,-0.035272816530353,
0.0777720188012005));
#64720=CARTESIAN_POINT('Ctrl Pts',(0.0126079404345147,-0.0352468764909503,
0.0777927475463656));
#64721=CARTESIAN_POINT('Ctrl Pts',(0.0126245317879862,-0.0352209141752645,
0.0778134950271386));
#64722=CARTESIAN_POINT('Ctrl Pts',(0.0126411252558039,-0.0351949306073887,
0.0778342607529929));
#64723=CARTESIAN_POINT('',(0.0126109569272709,-0.0350943706855874,0.0780265859811649));
#64724=CARTESIAN_POINT('Origin',(0.00271072246036746,-0.0338370705542837,
0.0756914103695427));
#64725=CARTESIAN_POINT('',(0.0124246676682262,-0.0351951371254947,0.0780844811758725));
#64726=CARTESIAN_POINT('Origin',(0.00886268837342121,-0.0338370705330453,
0.0685704678582771));
#64727=CARTESIAN_POINT('',(0.0123565016385186,-0.0352722979006325,0.0780446438285792));
#64728=CARTESIAN_POINT('Origin',(0.00921185609345463,-0.0346069579033713,
0.0822897503235107));
#64729=CARTESIAN_POINT('',(0.0122304629055867,-0.0352740680168101,0.0781750125228384));
#64730=CARTESIAN_POINT('Origin',(0.0128129328025127,-0.0305802162293653,
0.0786695676955698));
#64731=CARTESIAN_POINT('',(0.0121021643810505,-0.035272816532173,0.0783033930545577));
#64732=CARTESIAN_POINT('Origin',(0.0115725690272512,-0.0288496123714179,
0.0775749400940305));
#64733=CARTESIAN_POINT('',(0.0121437443425793,-0.035194930605203,0.0783713824674553));
#64734=CARTESIAN_POINT('Ctrl Pts',(0.0121021643844982,-0.035272816530353,
0.0783033930503626));
#64735=CARTESIAN_POINT('Ctrl Pts',(0.0121160241783837,-0.0352468764909501,
0.0783260374461362));
#64736=CARTESIAN_POINT('Ctrl Pts',(0.0121298843552239,-0.0352209141752643,
0.0783487007748063));
#64737=CARTESIAN_POINT('Ctrl Pts',(0.0121437443430231,-0.0351949306073883,
0.0783713824696875));
#64738=CARTESIAN_POINT('',(0.0120897091580298,-0.0350943706855874,0.0785584100618229));
#64739=CARTESIAN_POINT('Origin',(0.00256021610683366,-0.0338370705542768,
0.0750008196084603));
#64740=CARTESIAN_POINT('',(0.0118976326534744,-0.0351951371254942,0.0785925005004138));
#64741=CARTESIAN_POINT('Origin',(0.00955616268257527,-0.0338370705333592,
0.0687070736356047));
#64742=CARTESIAN_POINT('',(0.0118349970768232,-0.0352722979006328,0.07854443381358));
#64743=CARTESIAN_POINT('Origin',(0.00818309507620666,-0.0346069579027949,
0.0823619377817764));
#64744=CARTESIAN_POINT('',(0.0116936126669398,-0.0352740680168101,0.078657977669793));
#64745=CARTESIAN_POINT('Origin',(0.0122095054157723,-0.0305802162292943,
0.0792216359629003));
#64746=CARTESIAN_POINT('',(0.0115502354674222,-0.035272816532173,0.0787692658137335));
#64747=CARTESIAN_POINT('Origin',(0.011116115495978,-0.0288496123715395,
0.0779801810239078));
#64748=CARTESIAN_POINT('',(0.0115829662255687,-0.0351949306052026,0.0788419304608332));
#64749=CARTESIAN_POINT('Ctrl Pts',(0.0115502354713685,-0.035272816530353,
0.0787692658100036));
#64750=CARTESIAN_POINT('Ctrl Pts',(0.0115611478812951,-0.03524687649095,
0.0787934687407373));
#64751=CARTESIAN_POINT('Ctrl Pts',(0.0115720582982357,-0.035220914175264,
0.0788176905030729));
#64752=CARTESIAN_POINT('Ctrl Pts',(0.0115829662257291,-0.0351949306073879,
0.0788419304631035));
#64753=CARTESIAN_POINT('',(0.0115059163514221,-0.0350943706855873,0.0790207108823495));
#64754=CARTESIAN_POINT('Origin',(0.00249745047290323,-0.0338370705482644,
0.0742968108926817));
#64755=CARTESIAN_POINT('',(0.0113110817625737,-0.0351951371254938,0.0790304589382426));
#64756=CARTESIAN_POINT('Origin',(0.0102270474902958,-0.0338370705270455,
0.068929517567728));
#64757=CARTESIAN_POINT('',(0.0112549644394394,-0.0352722979006331,0.0789749209522334));
#64758=CARTESIAN_POINT('Origin',(0.00715339866134947,-0.0346069579035208,
0.082304618075051));
#64759=CARTESIAN_POINT('',(0.0111004640692083,-0.03527406801681,0.0790698493159593));
#64760=CARTESIAN_POINT('Origin',(0.0115416437331749,-0.0305802162294728,
0.0796937215015325));
#64761=CARTESIAN_POINT('',(0.0109442693387939,-0.0352728165321731,0.0791622899916112));
#64762=CARTESIAN_POINT('Origin',(0.0106124710845554,-0.0288496124319553,
0.0783250177177809));
#64763=CARTESIAN_POINT('',(0.0109676347099497,-0.0351949306052022,0.0792384839080203));
#64764=CARTESIAN_POINT('Ctrl Pts',(0.0109442693431767,-0.0352728165303531,
0.0791622899884052));
#64765=CARTESIAN_POINT('Ctrl Pts',(0.010952062273921,-0.0352468764909499,
0.0791876697594232));
#64766=CARTESIAN_POINT('Ctrl Pts',(0.0109598508671691,-0.0352209141752638,
0.0792130679637629));
#64767=CARTESIAN_POINT('Ctrl Pts',(0.0109676347098241,-0.0351949306073876,
0.079238483910293));
#64768=CARTESIAN_POINT('',(0.0108687852687488,-0.0350943706855873,0.07940619768264));
#64769=CARTESIAN_POINT('Origin',(0.00252341553365714,-0.0338370705543086,
0.0735904869236782));
#64770=CARTESIAN_POINT('',(0.0106742652534621,-0.0351951371254933,0.0793914496231707));
#64771=CARTESIAN_POINT('Origin',(0.0108647625592668,-0.0338370705271384,
0.0692342916717644));
#64772=CARTESIAN_POINT('',(0.0106255511875536,-0.0352722979006333,0.0793293162052023));
#64773=CARTESIAN_POINT('Origin',(0.00613900577330561,-0.0346069579032824,
0.0821186951698965));
#64774=CARTESIAN_POINT('',(0.0104603714201079,-0.03527406801681,0.0794041319994378));
#64775=CARTESIAN_POINT('Origin',(0.0108198803322818,-0.0305802162294855,
0.0800783792403199));
#64776=CARTESIAN_POINT('',(0.0102938224430008,-0.0352728165321731,0.0794762673621242));
#64777=CARTESIAN_POINT('Origin',(0.0100695785560694,-0.028849612371461,
0.0786040118752345));
#64778=CARTESIAN_POINT('',(0.0103074539413048,-0.0351949306052018,0.0795547889242649));
#64779=CARTESIAN_POINT('Ctrl Pts',(0.0102938224477508,-0.0352728165303531,
0.0794762673594928));
#64780=CARTESIAN_POINT('Ctrl Pts',(0.0102983730001398,-0.0352468764909498,
0.079502423716645));
#64781=CARTESIAN_POINT('Ctrl Pts',(0.0103029169389272,-0.0352209141752636,
0.0795285978181342));
#64782=CARTESIAN_POINT('Ctrl Pts',(0.0103074539408953,-0.0351949306073873,
0.0795547889265041));
#64783=CARTESIAN_POINT('',(0.0101883638484256,-0.0350943706857666,0.079708791105264));
#64784=CARTESIAN_POINT('Origin',(0.00263770164532897,-0.0338370705486574,
0.0728929867578665));
#64785=CARTESIAN_POINT('',(0.00999722610290667,-0.0351951371254956,0.0796697795164551));
#64786=CARTESIAN_POINT('Origin',(0.0114592507464863,-0.0338370705486561,
0.0696165894085452));
#64787=CARTESIAN_POINT('',(0.00995668354414125,-0.0352722979006335,0.0796020305476417));
#64788=CARTESIAN_POINT('Origin',(0.00515591409378127,-0.0346069579414847,
0.0818071011663319));
#64789=CARTESIAN_POINT('',(0.00978342936308381,-0.0352740680168101,0.0796555538826207));
#64790=CARTESIAN_POINT('Origin',(0.0100555978531566,-0.0305802162293099,
0.0803695428969902));
#64791=CARTESIAN_POINT('',(0.00960915271614781,-0.035272816532173,0.0797062463145787));
#64792=CARTESIAN_POINT('Origin',(0.00949599965990695,-0.028849612371569,
0.0788127636112503));
#64793=CARTESIAN_POINT('',(0.00961283536472869,-0.0351949306052016,0.0797858571905092));
#64794=CARTESIAN_POINT('Ctrl Pts',(0.00960915272119017,-0.035272816530353,
0.0797062463125634));
#64795=CARTESIAN_POINT('Ctrl Pts',(0.00961038913029425,-0.0352468764909497,
0.0797327667544723));
#64796=CARTESIAN_POINT('Ctrl Pts',(0.0096116167539918,-0.0352209141752635,
0.0797593039718948));
#64797=CARTESIAN_POINT('Ctrl Pts',(0.00961283536404159,-0.0351949306073873,
0.0797858571926796));
#64798=CARTESIAN_POINT('',(0.00947538274148284,-0.0350943706857667,0.0799237190718858));
#64799=CARTESIAN_POINT('Origin',(0.00283850659495694,-0.0338370705540077,
0.0722153105035223));
#64800=CARTESIAN_POINT('',(0.00929064162275147,-0.035195137125491,0.079861059189403));
#64801=CARTESIAN_POINT('Origin',(0.0120011365590591,-0.0338370705323713,
0.0700703818276128));
#64802=CARTESIAN_POINT('',(0.00925890995150084,-0.0352722979006337,0.0797887631114598));
#64803=CARTESIAN_POINT('Origin',(0.00421962723954973,-0.0346069578981706,
0.0813747501428187));
#64804=CARTESIAN_POINT('',(0.00908031367876579,-0.0352740680168079,0.0798201498922159));
#64805=CARTESIAN_POINT('Origin',(0.0092608494871027,-0.0305802162292691,
0.0805626206468866));
#64806=CARTESIAN_POINT('',(0.00890105780882915,-0.0352728165321731,0.0798485999435113));
#64807=CARTESIAN_POINT('Origin',(0.00890078007252705,-0.0288496123647477,
0.0789479807675767));
#64808=CARTESIAN_POINT('',(0.00889473353011883,-0.0351949306052013,0.0799280446221614));
#64809=CARTESIAN_POINT('Ctrl Pts',(0.00890105781408429,-0.0352728165303532,
0.0798485999421439));
#64810=CARTESIAN_POINT('Ctrl Pts',(0.00889896058099329,-0.0352468764909498,
0.0798750662255982));
#64811=CARTESIAN_POINT('Ctrl Pts',(0.00889685252924194,-0.0352209141752635,
0.0799015480511828));
#64812=CARTESIAN_POINT('Ctrl Pts',(0.008894733529165,-0.0351949306073872,
0.0799280446242287));
#64813=CARTESIAN_POINT('',(0.0087410860864854,-0.0350943706857667,0.0800475920396916));
#64814=CARTESIAN_POINT('Origin',(0.00312266345952377,-0.0338370705537815,
0.0715681454234068));
#64815=CARTESIAN_POINT('',(0.00856565507233699,-0.0351951371254918,0.0799622720473137));
#64816=CARTESIAN_POINT('Origin',(0.0124818742154735,-0.0338370705274226,
0.0705885121561095));
#64817=CARTESIAN_POINT('',(0.00854323471601816,-0.0352722979006337,0.0798865690125767));
#64818=CARTESIAN_POINT('Origin',(0.00334491140344038,-0.0346069579038024,
0.0808284604609533));
#64819=CARTESIAN_POINT('',(0.00836211292151624,-0.0352740680168079,0.0798953242508273));
#64820=CARTESIAN_POINT('Origin',(0.00844816889056077,-0.0305802162291152,
0.0806545675384037));
#64821=CARTESIAN_POINT('',(0.00818070480072852,-0.0352728165321732,0.0799010832471564));
#64822=CARTESIAN_POINT('Origin',(0.00829330676799402,-0.0288496123650155,
0.0790075309130333));
#64823=CARTESIAN_POINT('',(0.0081644733313186,-0.0351949306058011,0.0799791088412712));
#64824=CARTESIAN_POINT('Ctrl Pts',(0.00818070480611361,-0.0352728165303532,
0.0799010832464584));
#64825=CARTESIAN_POINT('Ctrl Pts',(0.00817530700536458,-0.0352468764905577,
0.0799270779827507));
#64826=CARTESIAN_POINT('Ctrl Pts',(0.00816989652331777,-0.0352209141744786,
0.0799530867826816));
#64827=CARTESIAN_POINT('Ctrl Pts',(0.00816447333092876,-0.0351949306062089,
0.0799791088415971));
#64828=CARTESIAN_POINT('',(0.00799705416196017,-0.0350943707007864,0.08007845644402));
#64829=CARTESIAN_POINT('Origin',(0.00348535491286147,-0.0338373859475111,
0.0709614461967262));
#64830=CARTESIAN_POINT('',(0.00783369992265928,-0.0351951371254912,0.0799718219029567));
#64831=CARTESIAN_POINT('Origin',(0.0128938821456517,-0.0338370705272571,
0.0711628093171656));
#64832=CARTESIAN_POINT('',(0.0078209444636804,-0.0352722979006336,0.0798939057935052));
#64833=CARTESIAN_POINT('Origin',(0.0025455611822975,-0.0346069579031932,
0.0801768474759825));
#64834=CARTESIAN_POINT('',(0.00764015354630635,-0.0352740680168098,0.0798798914139134));
#64835=CARTESIAN_POINT('Origin',(0.00763037252202439,-0.0305802162295736,
0.0806439335144828));
#64836=CARTESIAN_POINT('',(0.00745945408910196,-0.035272816532173,0.0798628685324633));
#64837=CARTESIAN_POINT('Origin',(0.00768315995856749,-0.0288496123710585,
0.0789904749064774));
#64838=CARTESIAN_POINT('',(0.00743357141106809,-0.0351949306052011,0.0799382445262853));
#64839=CARTESIAN_POINT('Ctrl Pts',(0.00745945409453209,-0.035272816530353,
0.0798628685324458));
#64840=CARTESIAN_POINT('Ctrl Pts',(0.00745084085282929,-0.0352468764909498,
0.0798879817682764));
#64841=CARTESIAN_POINT('Ctrl Pts',(0.00744221326718366,-0.0352209141752637,
0.0799131073674612));
#64842=CARTESIAN_POINT('Ctrl Pts',(0.00743357140962971,-0.0351949306073875,
0.0799382445280509));
#64843=CARTESIAN_POINT('',(0.00725502085064003,-0.0350943706857667,0.0800158255764398));
#64844=CARTESIAN_POINT('Origin',(0.00392186390992144,-0.0338370705483594,
0.0704055314389981));
#64845=CARTESIAN_POINT('',(0.00710631954367321,-0.0351951371254908,0.0798895581494023));
#64846=CARTESIAN_POINT('Origin',(0.0132306627505617,-0.033837070527115,
0.0717842162590107));
#64847=CARTESIAN_POINT('',(0.00710343014324219,-0.0352722979006335,0.0798106577488273));
#64848=CARTESIAN_POINT('Origin',(0.00183418283858109,-0.0346069579033387,
0.0794301875068299));
#64849=CARTESIAN_POINT('',(0.00692582128376252,-0.03527406801681,0.0797740947665314));
#64850=CARTESIAN_POINT('Origin',(0.00682035751875458,-0.0305802162293907,
0.0805308862794182));
#64851=CARTESIAN_POINT('',(0.0067486802285259,-0.0352728165321729,0.0797345584683111));
#64852=CARTESIAN_POINT('Origin',(0.00707996202453286,-0.0288496123715112,
0.0788970817063622));
#64853=CARTESIAN_POINT('',(0.00671355452610057,-0.035194930605201,0.0798060961401762));
#64854=CARTESIAN_POINT('Ctrl Pts',(0.00674868023391541,-0.0352728165303529,
0.0797345584689743));
#64855=CARTESIAN_POINT('Ctrl Pts',(0.00673698738714423,-0.0352468764909498,
0.0797583941540052));
#64856=CARTESIAN_POINT('Ctrl Pts',(0.00672527875999732,-0.0352209141752638,
0.0797822403071289));
#64857=CARTESIAN_POINT('Ctrl Pts',(0.00671355452445208,-0.0351949306073877,
0.0798060961417479));
#64858=CARTESIAN_POINT('',(0.00652668840559494,-0.0350943706855873,0.0798606871213604));
#64859=CARTESIAN_POINT('Origin',(0.00442430365356226,-0.0338370705545198,
0.0699084177326389));
#64860=CARTESIAN_POINT('',(0.00639498515847155,-0.0351951371254902,0.0797167781351863));
#64861=CARTESIAN_POINT('Origin',(0.0134869047874854,-0.0338370705288107,
0.0724429330351057));
#64862=CARTESIAN_POINT('',(0.00640200738415908,-0.0352722979006334,0.0796381377499374));
#64863=CARTESIAN_POINT('Origin',(0.00122199523403942,-0.0346069579031278,
0.078600255826089));
#64864=CARTESIAN_POINT('',(0.00623038158038529,-0.0352740680168099,0.0795796027850097));
#64865=CARTESIAN_POINT('Origin',(0.00603089830120988,-0.0305802162294044,
0.0803172086561122));
#64866=CARTESIAN_POINT('',(0.00605959254737729,-0.035272816532173,0.0795181765810599));
#64867=CARTESIAN_POINT('Origin',(0.00649322575805522,-0.0288496123718448,
0.0787288241923079));
#64868=CARTESIAN_POINT('',(0.00601577777387097,-0.0351949306052009,0.0795847477391485));
#64869=CARTESIAN_POINT('Ctrl Pts',(0.0060595925526412,-0.035272816530353,
0.0795181765823933));
#64870=CARTESIAN_POINT('Ctrl Pts',(0.00604500450398018,-0.03524687649095,
0.0795403588136329));
#64871=CARTESIAN_POINT('Ctrl Pts',(0.00603039948737651,-0.035220914175264,
0.0795625494526157));
#64872=CARTESIAN_POINT('Ctrl Pts',(0.00601577777203827,-0.035194930607388,
0.0795847477405013));
#64873=CARTESIAN_POINT('',(0.0058235430843454,-0.0350943706855874,0.0796154877190134));
#64874=CARTESIAN_POINT('Origin',(0.00498508636730859,-0.0338370705537688,
0.0694781962621798));
#64875=CARTESIAN_POINT('',(0.0057109149352393,-0.0351951371254898,0.0794562067043462));
#64876=CARTESIAN_POINT('Origin',(0.0136585671622885,-0.0338370705331965,
0.0731285712846959));
#64877=CARTESIAN_POINT('',(0.00572773804235142,-0.0352722979006333,0.0793790665402766));
#64878=CARTESIAN_POINT('Origin',(0.000718652933226445,-0.0346069579030036,
0.0777001409526867));
#64879=CARTESIAN_POINT('',(0.00556480193573351,-0.035274068016808,0.0792994827240814));
#64880=CARTESIAN_POINT('Origin',(0.0052744451129475,-0.0305802162290773,
0.0800062704680069));
#64881=CARTESIAN_POINT('',(0.00540305837002919,-0.0352728165321732,0.0792171353423319));
#64882=CARTESIAN_POINT('Origin',(0.00593220434223688,-0.0288496124253593,
0.0784883558809479));
#64883=CARTESIAN_POINT('',(0.0053512455105937,-0.0351949306052009,0.0792776901197134));
#64884=CARTESIAN_POINT('Ctrl Pts',(0.00540305837508442,-0.0352728165303532,
0.0792171353443146));
#64885=CARTESIAN_POINT('Ctrl Pts',(0.00538580518677541,-0.0352468764909502,
0.0792373142947253));
#64886=CARTESIAN_POINT('Ctrl Pts',(0.00536853411055141,-0.0352209141752643,
0.0792574994599344));
#64887=CARTESIAN_POINT('Ctrl Pts',(0.00535124550860563,-0.0351949306073883,
0.0792776901208262));
#64888=CARTESIAN_POINT('',(0.00515667390793764,-0.0350943706855873,0.0792840943104133));
#64889=CARTESIAN_POINT('Origin',(0.00559536819040455,-0.0338370705541392,
0.0691216519384616));
#64890=CARTESIAN_POINT('',(0.00506489707003965,-0.0351951371254925,0.0791119532240087));
#64891=CARTESIAN_POINT('Origin',(0.0137429427619029,-0.0338370705482579,
0.0738303180245431));
#64892=CARTESIAN_POINT('',(0.00509125574812847,-0.0352722979006329,0.0790375298275827));
#64893=CARTESIAN_POINT('Origin',(0.000332093925861045,-0.0346069579299659,
0.0767440382573458));
#64894=CARTESIAN_POINT('',(0.00493957893840163,-0.0352740680168099,0.0789381522444425));
#64895=CARTESIAN_POINT('Origin',(0.00456292767242667,-0.0305802162293321,
0.079602975396522));
#64896=CARTESIAN_POINT('',(0.0047894316326524,-0.035272816532173,0.0788361823522959));
#64897=CARTESIAN_POINT('Origin',(0.00540574541516571,-0.02884961237144,
0.0781794691145221));
#64898=CARTESIAN_POINT('',(0.00473043780703324,-0.035194930605201,0.078889765763957));
#64899=CARTESIAN_POINT('Ctrl Pts',(0.00478943163741931,-0.035272816530353,
0.0788361823548966));
#64900=CARTESIAN_POINT('Ctrl Pts',(0.00476978540254869,-0.0352468764909502,
0.0788540397903759));
#64901=CARTESIAN_POINT('Ctrl Pts',(0.00475012064189385,-0.0352209141752646,
0.0788719011496979));
#64902=CARTESIAN_POINT('Ctrl Pts',(0.0047304378049211,-0.0351949306073888,
0.078889765764812));
#64903=CARTESIAN_POINT('',(0.00453659780165151,-0.0350943706855874,0.0788717331675791));
#64904=CARTESIAN_POINT('Origin',(0.00624552461956904,-0.0338370705480265,
0.0688444076153873));
#64905=CARTESIAN_POINT('',(0.00446711965052249,-0.035195137125489,0.078689446777193));
#64906=CARTESIAN_POINT('Origin',(0.0137387007491635,-0.0338370705274849,
0.074537106376181));
#64907=CARTESIAN_POINT('',(0.00450259820748627,-0.0352722979006326,0.0786189138498392));
#64908=CARTESIAN_POINT('Origin',(6.8414532284294E-5,-0.0346069579036642,
0.0757470259866494));
#64909=CARTESIAN_POINT('',(0.00436457272854574,-0.0352740680168099,0.0785013097436045));
#64910=CARTESIAN_POINT('Origin',(0.00390756703492207,-0.0305802162292527,
0.0791136836454428));
#64911=CARTESIAN_POINT('',(0.00422838959545862,-0.035272816532173,0.0783813254671743));
#64912=CARTESIAN_POINT('Origin',(0.00492215155327239,-0.0288496123718619,
0.0778070352087378));
#64913=CARTESIAN_POINT('',(0.00416314517152701,-0.0351949306052012,0.0784270924707041));
#64914=CARTESIAN_POINT('Ctrl Pts',(0.00422838959986201,-0.035272816530353,
0.078381325470352));
#64915=CARTESIAN_POINT('Ctrl Pts',(0.00420666015128976,-0.0352468764909504,
0.0783965797684749));
#64916=CARTESIAN_POINT('Ctrl Pts',(0.00418491183122674,-0.035220914175265,
0.0784118356376035));
#64917=CARTESIAN_POINT('Ctrl Pts',(0.00416314516932403,-0.0351949306073894,
0.0784270924712879));
#64918=CARTESIAN_POINT('',(0.00397309373609907,-0.0350943706855873,0.0783849074720655));
#64919=CARTESIAN_POINT('Origin',(0.00692530227733226,-0.0338370705548223,
0.0686508357466448));
#64920=CARTESIAN_POINT('',(0.00392700998368523,-0.0351951371254887,0.0781953505429711));
#64921=CARTESIAN_POINT('Origin',(0.0136459081016941,-0.0338370705330285,
0.0752377898391803));
#64922=CARTESIAN_POINT('',(0.00397104890148771,-0.0352722979006322,0.0781298204310839));
#64923=CARTESIAN_POINT('Origin',(-6.82269184376445E-5,-0.0346069579035453,
0.0747248276832768));
#64924=CARTESIAN_POINT('',(0.00384885149759004,-0.03527406801681,0.0779958444887646));
#64925=CARTESIAN_POINT('Origin',(0.00331869862899803,-0.0305802162295164,
0.0785461116382315));
#64926=CARTESIAN_POINT('',(0.00372878022652447,-0.035272816532173,0.077859738051764));
#64927=CARTESIAN_POINT('Origin',(0.00448904931912108,-0.0288496123714666,
0.0773769276730949));
#64928=CARTESIAN_POINT('',(0.00365831414782088,-0.0351949306052012,0.0778969668741772));
#64929=CARTESIAN_POINT('Ctrl Pts',(0.00372878023049487,-0.035272816530353,
0.0778597380554684));
#64930=CARTESIAN_POINT('Ctrl Pts',(0.0037053102546055,-0.0352468764909506,
0.0778721486468413));
#64931=CARTESIAN_POINT('Ctrl Pts',(0.00368182135913347,-0.0352209141752653,
0.0778845584316069));
#64932=CARTESIAN_POINT('Ctrl Pts',(0.00365831414556175,-0.0351949306073898,
0.0778969668744805));
#64933=CARTESIAN_POINT('',(0.00347504850701491,-0.0350943706855874,0.0778312947559066));
#64934=CARTESIAN_POINT('Origin',(0.007623980706386,-0.0338370705483359,
0.0685439888925231));
#64935=CARTESIAN_POINT('',(0.0034530859216209,-0.0351951371254883,0.0776374567141115));
#64936=CARTESIAN_POINT('Origin',(0.0134660283161429,-0.0338370705272378,
0.0759213181795987));
#64937=CARTESIAN_POINT('',(0.00350499068022065,-0.0352722979006318,0.0775779628667008));
#64938=CARTESIAN_POINT('Origin',(-7.56754917528666E-5,-0.0346069579032585,
0.0736935640038484));
#64939=CARTESIAN_POINT('',(0.00340054847742131,-0.0352740680168101,0.0774297279689394));
#64940=CARTESIAN_POINT('Origin',(0.00280560926146734,-0.0305802162293396,
0.0779092103242104));
#64941=CARTESIAN_POINT('',(0.0032984826640503,-0.0352728165321729,0.0772796458511875));
#64942=CARTESIAN_POINT('Origin',(0.00411326899362973,-0.0288496123714065,
0.0768959295603915));
#64943=CARTESIAN_POINT('',(0.00322390622273076,-0.0351949306052015,0.0773077493717152));
#64944=CARTESIAN_POINT('Ctrl Pts',(0.00329848266752508,-0.0352728165303529,
0.0772796458553603));
#64945=CARTESIAN_POINT('Ctrl Pts',(0.00327364229985878,-0.0352468764909508,
0.0772890170175433));
#64946=CARTESIAN_POINT('Ctrl Pts',(0.00324878326289108,-0.0352209141752657,
0.077298385008227));
#64947=CARTESIAN_POINT('Ctrl Pts',(0.00322390622045105,-0.0351949306073906,
0.0773077493717331));
#64948=CARTESIAN_POINT('',(0.00305031658517945,-0.0350943706855873,0.0772196258223481));
#64949=CARTESIAN_POINT('Origin',(0.00833054129011836,-0.0338370705479401,
0.0685255522280844));
#64950=CARTESIAN_POINT('',(0.00305282152989682,-0.035195137125488,0.0770245636095646));
#64951=CARTESIAN_POINT('Origin',(0.0132018980278313,-0.0338370705330224,
0.0765769117901669));
#64952=CARTESIAN_POINT('',(0.00311177356024406,-0.0352722979006314,0.0769720442801441));
#64953=CARTESIAN_POINT('Origin',(4.61862801057515E-5,-0.0346069579036435,
0.0726694985930505));
#64954=CARTESIAN_POINT('',(0.00302673367447229,-0.0352740680168101,0.0768118881798294));
#64955=CARTESIAN_POINT('Origin',(0.00237639065787438,-0.0305802162294318,
0.0772130240178286));
#64956=CARTESIAN_POINT('',(0.00294428295764374,-0.035272816532173,0.0766501972659778));
#64957=CARTESIAN_POINT('Origin',(0.00380073685025004,-0.0288496124326153,
0.0763716265010679));
#64958=CARTESIAN_POINT('',(0.00286677226873748,-0.0351949306052018,0.0766687322753135));
#64959=CARTESIAN_POINT('Ctrl Pts',(0.0029442829605681,-0.0352728165303531,
0.0766501972705532));
#64960=CARTESIAN_POINT('Ctrl Pts',(0.00291846394856184,-0.0352468764909511,
0.0766563812147208));
#64961=CARTESIAN_POINT('Ctrl Pts',(0.00289262681196146,-0.0352209141752662,
0.0766625596725133));
#64962=CARTESIAN_POINT('Ctrl Pts',(0.00286677226647317,-0.0351949306073912,
0.0766687322750457));
#64963=CARTESIAN_POINT('',(0.00270559624672265,-0.0350943706855873,0.076559547055866));
#64964=CARTESIAN_POINT('Origin',(0.00903384112997155,-0.033837070554224,
0.0685958165021795));
#64965=CARTESIAN_POINT('',(0.00273252921707685,-0.0351951371254877,0.0763663369197139));
#64966=CARTESIAN_POINT('Origin',(0.0128576828699685,-0.0338370705326189,
0.0771942315442123));
#64967=CARTESIAN_POINT('',(0.00279759881043661,-0.0352722979006309,0.0763216203694819));
#64968=CARTESIAN_POINT('Origin',(0.000295436565332532,-0.0346069579034067,
0.0716687815734711));
#64969=CARTESIAN_POINT('',(0.00273330237149167,-0.03527406801681,0.076152068823989));
#64970=CARTESIAN_POINT('Origin',(0.00203781185220466,-0.0305802162292972,
0.0764685319928733));
#64971=CARTESIAN_POINT('',(0.00267176704826306,-0.035272816532173,0.0759813190763382));
#64972=CARTESIAN_POINT('Origin',(0.00355638172827499,-0.0288496123714443,
0.0758122870587156));
#64973=CARTESIAN_POINT('',(0.00259254450163696,-0.035194930605202,0.0759899932663124));
#64974=CARTESIAN_POINT('Ctrl Pts',(0.00267176705059093,-0.035272816530353,
0.075981319081244));
#64975=CARTESIAN_POINT('Ctrl Pts',(0.00264537657548761,-0.0352468764909512,
0.0759842182829025));
#64976=CARTESIAN_POINT('Ctrl Pts',(0.00261896880633315,-0.0352209141752666,
0.0759871097698338));
#64977=CARTESIAN_POINT('Ctrl Pts',(0.00259254449942374,-0.0351949306073918,
0.075989993265763));
#64978=CARTESIAN_POINT('',(0.00244632393730788,-0.0350943706855874,0.0758614682929193));
#64979=CARTESIAN_POINT('Origin',(0.00972278885438708,-0.0338370705482382,
0.0687536734940358));
#64980=CARTESIAN_POINT('',(0.00249726018426747,-0.0351951371254876,0.0756731572726638));
#64981=CARTESIAN_POINT('Origin',(0.0124388113078349,-0.0338370705268928,
0.0777635419566633));
#64982=CARTESIAN_POINT('',(0.00256742115428162,-0.0352722979006304,0.0756369487083298));
#64983=CARTESIAN_POINT('Origin',(0.000668144537672311,-0.034606957903352,
0.0707071948512846));
#64984=CARTESIAN_POINT('',(0.0025248821554141,-0.0352740680168102,0.0754606756468147));
#64985=CARTESIAN_POINT('Origin',(0.00179521243424888,-0.0305802162295,0.0756874753334203));
#64986=CARTESIAN_POINT('',(0.00248523267459275,-0.035272816532173,0.0752835598908876));
#64987=CARTESIAN_POINT('Origin',(0.00338405722560929,-0.0288496124323458,
0.075226732360674));
#64988=CARTESIAN_POINT('',(0.00240554765713235,-0.0351949306052022,0.0752822364643431));
#64989=CARTESIAN_POINT('Ctrl Pts',(0.0024852326762874,-0.0352728165303531,
0.0752835598960465));
#64990=CARTESIAN_POINT('Ctrl Pts',(0.00245868693164429,-0.0352468764909515,
0.0752831286330541));
#64991=CARTESIAN_POINT('Ctrl Pts',(0.00243212499623051,-0.035220914175267,
0.0752826875486479));
#64992=CARTESIAN_POINT('Ctrl Pts',(0.00240554765500504,-0.0351949306073924,
0.0752822364635208));
#64993=CARTESIAN_POINT('',(0.00227658853613647,-0.0350943706855873,0.0751363986526118));
#64994=CARTESIAN_POINT('Origin',(0.010386519222081,-0.0338370705546125,
0.0689966338444921));
#64995=CARTESIAN_POINT('',(0.0023507247646591,-0.0351951371254875,0.0749559565255339));
#64996=CARTESIAN_POINT('Origin',(0.0119518891160215,-0.0338370705273412,
0.078275864650999));
#64997=CARTESIAN_POINT('',(0.00242487063091823,-0.0352722979006299,0.074928826977787));
#64998=CARTESIAN_POINT('Origin',(0.00115843236911722,-0.034606957903392,
0.0697999032221867));
#64999=CARTESIAN_POINT('',(0.00240475993755276,-0.0352740680168099,0.0747486123317347));
#65000=CARTESIAN_POINT('Origin',(0.00165241834197848,-0.0305802162295103,
0.0748821717694814));
#65001=CARTESIAN_POINT('',(0.00238762159513567,-0.0352728165321731,0.0745679237888021));
#65002=CARTESIAN_POINT('Origin',(0.00328648102428352,-0.0288496124320948,
0.0746241969480168));
#65003=CARTESIAN_POINT('',(0.00230873078716791,-0.0351949306052026,0.0745566236169663));
#65004=CARTESIAN_POINT('Ctrl Pts',(0.00238762159617038,-0.0352728165303531,
0.0745679237941327));
#65005=CARTESIAN_POINT('Ctrl Pts',(0.0023613392242382,-0.0352468764909518,
0.0745641688677643));
#65006=CARTESIAN_POINT('Ctrl Pts',(0.00233504202015395,-0.0352209141752675,
0.0745604021681853));
#65007=CARTESIAN_POINT('Ctrl Pts',(0.00230873078516012,-0.0351949306073931,
0.0745566236158839));
#65008=CARTESIAN_POINT('',(0.00219906687187978,-0.0350943706855873,0.0743957729163068));
#65009=CARTESIAN_POINT('Origin',(0.0110145649089121,-0.0338370705544943,
0.0693208658243919));
#65010=CARTESIAN_POINT('',(0.00229523390935503,-0.0351951371254875,0.0742260453625414));
#65011=CARTESIAN_POINT('Origin',(0.0114045953917401,-0.0338370705268584,
0.0787231199947708));
#65012=CARTESIAN_POINT('',(0.00237219534725549,-0.0352722979006293,0.0742084226805557));
#65013=CARTESIAN_POINT('Origin',(0.0017585679285661,-0.0346069579032107,
0.0689612152181359));
#65014=CARTESIAN_POINT('',(0.0023748301170392,-0.0352740680168101,0.0740271085425837));
#65015=CARTESIAN_POINT('Origin',(0.00161168152344718,-0.030580216229527,
0.0740653214193561));
#65016=CARTESIAN_POINT('',(0.0023804731949247,-0.035272816532173,0.0738456967789116));
#65017=CARTESIAN_POINT('Origin',(0.00326519195932053,-0.0288496123714054,
0.0740141831669405));
#65018=CARTESIAN_POINT('',(0.00230362075161854,-0.0351949306052031,0.0738245980722451));
#65019=CARTESIAN_POINT('Ctrl Pts',(0.00238047319528312,-0.035272816530353,
0.0738456967843299));
#65020=CARTESIAN_POINT('Ctrl Pts',(0.00235486868476764,-0.035246876490952,
0.0738386774120175));
#65021=CARTESIAN_POINT('Ctrl Pts',(0.0023292509346306,-0.035220914175268,
0.0738316445003683));
#65022=CARTESIAN_POINT('Ctrl Pts',(0.00230362074976191,-0.0351949306073939,
0.0738245980709196));
#65023=CARTESIAN_POINT('',(0.0022149815074924,-0.0350943706855873,0.0736512711942942));
#65024=CARTESIAN_POINT('Origin',(0.0115970212688448,-0.0338370705480172,
0.0697212561165514));
#65025=CARTESIAN_POINT('',(0.00233166274229183,-0.0351951371254875,0.0734949349187544));
#65026=CARTESIAN_POINT('Origin',(0.01080556128334,-0.0338370705272959,0.0790982545048888));
#65027=CARTESIAN_POINT('',(0.00241022602398344,-0.0352722979006288,0.0734870970227522));
#65028=CARTESIAN_POINT('Origin',(0.0024590867190163,-0.0346069579034221,
0.0682043574498562));
#65029=CARTESIAN_POINT('',(0.00243556470502341,-0.0352740680168101,0.0733075428251295));
#65030=CARTESIAN_POINT('Origin',(0.00167364442279193,-0.0305802162292074,
0.0732498065010526));
#65031=CARTESIAN_POINT('',(0.00246390020850166,-0.035272816532173,0.0731282688125995));
#65032=CARTESIAN_POINT('Origin',(0.00332052575741809,-0.028849612371474,
0.0734063112986791));
#65033=CARTESIAN_POINT('',(0.00239029813879711,-0.0351949306052035,0.0730977043103102));
#65034=CARTESIAN_POINT('Ctrl Pts',(0.00246390020817816,-0.035272816530353,
0.07312826881802));
#65035=CARTESIAN_POINT('Ctrl Pts',(0.0024393773575055,-0.0352468764909522,
0.0731180956994582));
#65036=CARTESIAN_POINT('Ctrl Pts',(0.00241484306853851,-0.0352209141752684,
0.0731079074889567));
#65037=CARTESIAN_POINT('Ctrl Pts',(0.00239029813712095,-0.0351949306073946,
0.0730977043087625));
#65038=CARTESIAN_POINT('',(0.00232408145966373,-0.0350943706855874,0.0729146347234738));
#65039=CARTESIAN_POINT('Origin',(0.0121247025115712,-0.0338370705513202,
0.0701914903750677));
#65040=CARTESIAN_POINT('',(0.00245943675901277,-0.0351951371254877,0.0727741552426159));
#65041=CARTESIAN_POINT('Origin',(0.01016423388182,-0.03383707053302,0.0793953520558185));
#65042=CARTESIAN_POINT('',(0.00253836289461168,-0.0352722979006283,0.0727762257408987));
#65043=CARTESIAN_POINT('Origin',(0.00324894114125073,-0.0346069579033883,
0.0675412660163024));
#65044=CARTESIAN_POINT('',(0.00258600588077167,-0.0352740680168102,0.0726012631605823));
#65045=CARTESIAN_POINT('Origin',(0.00183732984760715,-0.0305802162294387,
0.0724484881719455));
#65046=CARTESIAN_POINT('',(0.00263658694202549,-0.035272816532173,0.0724269541574653));
#65047=CARTESIAN_POINT('Origin',(0.00345160977874861,-0.0288496123715095,
0.0728101678454856));
#65048=CARTESIAN_POINT('',(0.00256739599452954,-0.0351949306052039,0.0723874058800131));
#65049=CARTESIAN_POINT('Ctrl Pts',(0.00263658694102517,-0.035272816530353,
0.0724269541628026));
#65050=CARTESIAN_POINT('Ctrl Pts',(0.00261353249019967,-0.0352468764909524,
0.0724137877341483));
#65051=CARTESIAN_POINT('Ctrl Pts',(0.00259046858279584,-0.0352209141752689,
0.0724006048989603));
#65052=CARTESIAN_POINT('Ctrl Pts',(0.0025673959930603,-0.0351949306073953,
0.0723874058782675));
#65053=CARTESIAN_POINT('',(0.00252464615697504,-0.0350943706855873,0.0721974807010359));
#65054=CARTESIAN_POINT('Origin',(0.0125892868464681,-0.0338370705546861,
0.0707241526903459));
#65055=CARTESIAN_POINT('',(0.00267654088694574,-0.0351951371254879,0.0720750734601912));
#65056=CARTESIAN_POINT('Origin',(0.00949072738717799,-0.0338370705310109,
0.0796097273078675));
#65057=CARTESIAN_POINT('',(0.00275458516414511,-0.0352722979006279,0.0720870196997644));
#65058=CARTESIAN_POINT('Origin',(0.00411567467158826,-0.034606957924588,
0.0669823984380814));
#65059=CARTESIAN_POINT('',(0.00282378109707297,-0.0352740680168102,0.0719194080011641));
#65060=CARTESIAN_POINT('Origin',(0.00210015638139261,-0.030580216229448,
0.0716740037008217));
#65061=CARTESIAN_POINT('',(0.00289581002255045,-0.035272816532173,0.0717528129645656));
#65062=CARTESIAN_POINT('Origin',(0.00365637675003213,-0.0288496123718428,
0.0722351543457127));
#65063=CARTESIAN_POINT('',(0.00283212137983757,-0.0351949306052042,0.0717049046119108));
#65064=CARTESIAN_POINT('Ctrl Pts',(0.00289581002088911,-0.035272816530353,
0.0717528129697354));
#65065=CARTESIAN_POINT('Ctrl Pts',(0.00287458755237228,-0.0352468764909526,
0.0717368608734338));
#65066=CARTESIAN_POINT('Ctrl Pts',(0.00285335775812898,-0.0352209141752692,
0.0717208913147453));
#65067=CARTESIAN_POINT('Ctrl Pts',(0.00283212137859842,-0.0351949306073958,
0.0717049046099949));
#65068=CARTESIAN_POINT('',(0.00281351257433806,-0.0350943706855873,0.0715111190743214));
#65069=CARTESIAN_POINT('Origin',(0.0129834475299402,-0.0338370705542504,
0.0713108426575205));
#65070=CARTESIAN_POINT('',(0.00297955126430113,-0.0351951371254881,0.0714087145088007));
#65071=CARTESIAN_POINT('Origin',(0.00879566332822816,-0.033837070532911,
0.0797379993743328));
#65072=CARTESIAN_POINT('',(0.00305548287822846,-0.0352722979006274,0.0714303480903293));
#65073=CARTESIAN_POINT('Origin',(0.00504561854555748,-0.0346069579034451,
0.066536567876592));
#65074=CARTESIAN_POINT('',(0.00314514049672617,-0.0352740680168102,0.0712727306100589));
#65075=CARTESIAN_POINT('Origin',(0.00245797909256947,-0.0305802162293691,
0.0709385671704278));
#65076=CARTESIAN_POINT('',(0.00323748134724438,-0.0352728165321731,0.0711164768432249));
#65077=CARTESIAN_POINT('Origin',(0.00393159737382974,-0.0288496123719026,
0.0716903391057524));
#65078=CARTESIAN_POINT('',(0.00318029941725562,-0.0351949306052047,0.0710609639587081));
#65079=CARTESIAN_POINT('Ctrl Pts',(0.00323748134494819,-0.0352728165303531,
0.0711164768481458));
#65080=CARTESIAN_POINT('Ctrl Pts',(0.00321842554974618,-0.0352468764909528,
0.0710979906582848));
#65081=CARTESIAN_POINT('Ctrl Pts',(0.00319936467520065,-0.0352209141752696,
0.0710794862255762));
#65082=CARTESIAN_POINT('Ctrl Pts',(0.00318029941626621,-0.0351949306073963,
0.071060963956652));
#65083=CARTESIAN_POINT('',(0.00318612511579046,-0.0350943706855874,0.0708663741761959));
#65084=CARTESIAN_POINT('Origin',(0.0133009684340317,-0.0338370705483989,
0.0719423078362993));
#65085=CARTESIAN_POINT('',(0.00336368923641856,-0.0351951371254884,0.0707855872671713));
#65086=CARTESIAN_POINT('Origin',(0.00809000333431659,-0.0338370705278078,
0.0797781454036159));
#65087=CARTESIAN_POINT('',(0.00343631070016287,-0.035272297900627,0.0708165670161512));
#65088=CARTESIAN_POINT('Origin',(0.00602410685206571,-0.0346069579033739,
0.0662108058592296));
#65089=CARTESIAN_POINT('',(0.00354501605002859,-0.0352740680168101,0.07067142947603));
#65090=CARTESIAN_POINT('Origin',(0.00290515490327304,-0.0305802162292641,
0.0702537768542104));
#65091=CARTESIAN_POINT('',(0.00365621255521218,-0.035272816532173,0.0705279811942054));
#65092=CARTESIAN_POINT('Origin',(0.00427293125686862,-0.0288496123715293,
0.071184314187666));
#65093=CARTESIAN_POINT('',(0.00360643913114228,-0.035194930605205,0.0704657392491771));
#65094=CARTESIAN_POINT('Ctrl Pts',(0.00365621255231737,-0.035272816530353,
0.0705279811987995));
#65095=CARTESIAN_POINT('Ctrl Pts',(0.00363962395170388,-0.0352468764909529,
0.0705072524536365));
#65096=CARTESIAN_POINT('Ctrl Pts',(0.00362303259823409,-0.0352209141752699,
0.0704865049728655));
#65097=CARTESIAN_POINT('Ctrl Pts',(0.00360643913041818,-0.0351949306073968,
0.0704657392470133));
#65098=CARTESIAN_POINT('',(0.00363660745896575,-0.0350943706855873,0.0702734140188551));
#65099=CARTESIAN_POINT('Origin',(0.0135368419257299,-0.0338370705541201,
0.0726085896305422));
#65100=CARTESIAN_POINT('',(0.00382289671800493,-0.0351951371254887,0.0702155188241416));
#65101=CARTESIAN_POINT('Origin',(0.00738487602467975,-0.0338370705289731,
0.0797295321728266));
#65102=CARTESIAN_POINT('',(0.00389106274770099,-0.0352722979006266,0.0702553561714247));
#65103=CARTESIAN_POINT('Origin',(0.00703570829280538,-0.0346069579035862,
0.0660102496760509));
#65104=CARTESIAN_POINT('',(0.00401710148062903,-0.0352740680168101,0.0701249874771627));
#65105=CARTESIAN_POINT('Origin',(0.00343463158368949,-0.0305802162293682,
0.069630432304418));
#65106=CARTESIAN_POINT('',(0.00414540000516627,-0.035272816532173,0.0699966069454424));
#65107=CARTESIAN_POINT('Origin',(0.00467499535910736,-0.0288496123713801,
0.0707250599061107));
#65108=CARTESIAN_POINT('',(0.0041038200436459,-0.0351949306052054,0.0699286175325576));
#65109=CARTESIAN_POINT('Ctrl Pts',(0.00414540000171849,-0.035272816530353,
0.0699966069496375));
#65110=CARTESIAN_POINT('Ctrl Pts',(0.00413154020783471,-0.035246876490953,
0.0699739625538664));
#65111=CARTESIAN_POINT('Ctrl Pts',(0.00411768003099606,-0.0352209141752702,
0.0699512992251989));
#65112=CARTESIAN_POINT('Ctrl Pts',(0.00410382004319857,-0.0351949306073972,
0.0699286175303201));
#65113=CARTESIAN_POINT('',(0.00415785522820683,-0.0350943706855873,0.0697415899381972));
#65114=CARTESIAN_POINT('Origin',(0.0136873482790303,-0.0338370705545973,
0.0732991803912815));
#65115=CARTESIAN_POINT('',(0.00434993173275813,-0.035195137125489,0.0697074994996005));
#65116=CARTESIAN_POINT('Origin',(0.00669140170371844,-0.0338370705330846,
0.0795929263638979));
#65117=CARTESIAN_POINT('',(0.00441256730939742,-0.0352722979006262,0.0697555661864226));
#65118=CARTESIAN_POINT('Origin',(0.00806446930900352,-0.0346069579035356,
0.0659380622183925));
#65119=CARTESIAN_POINT('',(0.00455395171927896,-0.0352740680168101,0.0696420223302055));
#65120=CARTESIAN_POINT('Origin',(0.00403805897045731,-0.0305802162293176,
0.0690783640371152));
#65121=CARTESIAN_POINT('',(0.00469732891879462,-0.035272816532173,0.0695307341862665));
#65122=CARTESIAN_POINT('Origin',(0.00513144889000808,-0.0288496123713709,
0.0703198189757993));
#65123=CARTESIAN_POINT('',(0.00466459816065547,-0.0351949306052058,0.0694580695391812));
#65124=CARTESIAN_POINT('Ctrl Pts',(0.00469732891484825,-0.035272816530353,
0.0695307341899964));
#65125=CARTESIAN_POINT('Ctrl Pts',(0.00468641650492311,-0.0352468764909532,
0.0695065312592657));
#65126=CARTESIAN_POINT('Ctrl Pts',(0.00467550608798394,-0.0352209141752704,
0.069482309496933));
#65127=CARTESIAN_POINT('Ctrl Pts',(0.00466459816049193,-0.0351949306073975,
0.0694580695369053));
#65128=CARTESIAN_POINT('',(0.00474164803481453,-0.0350943706855873,0.0692792891176706));
#65129=CARTESIAN_POINT('Origin',(0.013750113884078,-0.0338370705527406,
0.0740031890922119));
#65130=CARTESIAN_POINT('',(0.00493648262366037,-0.0351951371254895,0.0692695410617723));
#65131=CARTESIAN_POINT('Origin',(0.0060205168904824,-0.0338370705331194,
0.0793704823860861));
#65132=CARTESIAN_POINT('',(0.00499259994678247,-0.035272297900626,0.0693250790477682));
#65133=CARTESIAN_POINT('Origin',(0.00909416572563785,-0.0346069579029593,
0.0659953819249899));
#65134=CARTESIAN_POINT('',(0.00514710031701445,-0.0352740680168101,0.0692301506840371));
#65135=CARTESIAN_POINT('Origin',(0.00470592065312846,-0.0305802162291783,
0.0686062784986003));
#65136=CARTESIAN_POINT('',(0.00530329504742269,-0.035272816532173,0.069137710008389));
#65137=CARTESIAN_POINT('Origin',(0.00563509330511477,-0.0288496123712193,
0.0699749822889916));
#65138=CARTESIAN_POINT('',(0.00527992967627283,-0.0351949306052063,0.0690615160919956));
#65139=CARTESIAN_POINT('Ctrl Pts',(0.00530329504303985,-0.035272816530353,
0.0691377100115949));
#65140=CARTESIAN_POINT('Ctrl Pts',(0.00529550211229662,-0.0352468764909533,
0.0691123302405803));
#65141=CARTESIAN_POINT('Ctrl Pts',(0.00528771351904963,-0.0352209141752707,
0.0690869320362439));
#65142=CARTESIAN_POINT('Ctrl Pts',(0.00527992967639571,-0.035194930607398,
0.0690615160897173));
#65143=CARTESIAN_POINT('',(0.00537877911748765,-0.0350943706855873,0.0688938023173803));
#65144=CARTESIAN_POINT('Origin',(0.0137241488906242,-0.0338370705481307,
0.0747095131024691));
#65145=CARTESIAN_POINT('',(0.00557329913277311,-0.03519513712549,0.0689085503768451));
#65146=CARTESIAN_POINT('Origin',(0.00538280182741146,-0.0338370705333044,
0.0790657082803801));
#65147=CARTESIAN_POINT('',(0.00562201319866981,-0.0352722979006257,0.0689706837947988));
#65148=CARTESIAN_POINT('Origin',(0.0101085586128168,-0.0346069579030927,
0.0661813048304526));
#65149=CARTESIAN_POINT('',(0.00578719296611978,-0.0352740680168101,0.0688958680005572));
#65150=CARTESIAN_POINT('Origin',(0.00542768405399171,-0.0305802162292022,
0.0682216207597974));
#65151=CARTESIAN_POINT('',(0.0059537419432158,-0.035272816532173,0.0688237326378758));
#65152=CARTESIAN_POINT('Origin',(0.00617798583012386,-0.0288496123715834,
0.069695988124715));
#65153=CARTESIAN_POINT('',(0.00594011044491611,-0.0351949306052065,0.0687452110757515));
#65154=CARTESIAN_POINT('Ctrl Pts',(0.00595374193846581,-0.035272816530353,
0.0688237326405072));
#65155=CARTESIAN_POINT('Ctrl Pts',(0.00594919138607751,-0.0352468764909533,
0.0687975762833586));
#65156=CARTESIAN_POINT('Ctrl Pts',(0.00594464744729082,-0.0352209141752707,
0.068771402181873));
#65157=CARTESIAN_POINT('Ctrl Pts',(0.00594011044532344,-0.0351949306073981,
0.0687452110735067));
#65158=CARTESIAN_POINT('',(0.00605920053781098,-0.0350943706857667,0.068591208894756));
#65159=CARTESIAN_POINT('Origin',(0.013609862705455,-0.0338370705544637,
0.0754070132109463));
#65160=CARTESIAN_POINT('',(0.00625033828333205,-0.0351951371254905,0.0686302204835654));
#65161=CARTESIAN_POINT('Origin',(0.00478831365572456,-0.0338370705271894,
0.0786834105677195));
#65162=CARTESIAN_POINT('',(0.00629088084208389,-0.0352722979006255,0.0686979694523592));
#65163=CARTESIAN_POINT('Origin',(0.0110916503910954,-0.0346069579032766,
0.0664928988182023));
#65164=CARTESIAN_POINT('',(0.00646413502314418,-0.0352740680168103,0.0686444461173757));
#65165=CARTESIAN_POINT('Origin',(0.0061919665330451,-0.0305802162293461,
0.0679304571029579));
#65166=CARTESIAN_POINT('',(0.00663841167006886,-0.0352728165321731,0.0685937536854215));
#65167=CARTESIAN_POINT('Origin',(0.00675156472634297,-0.0288496123711304,
0.0694872363888643));
#65168=CARTESIAN_POINT('',(0.00663472902149044,-0.0351949306052067,0.0685141428095075));
#65169=CARTESIAN_POINT('Ctrl Pts',(0.00663841166502647,-0.0352728165303531,
0.0685937536874368));
#65170=CARTESIAN_POINT('Ctrl Pts',(0.00663717525592264,-0.0352468764909534,
0.0685672332455315));
#65171=CARTESIAN_POINT('Ctrl Pts',(0.00663594763222532,-0.0352209141752708,
0.0685406960281127));
#65172=CARTESIAN_POINT('Ctrl Pts',(0.00663472902217576,-0.0351949306073982,
0.0685141428073316));
#65173=CARTESIAN_POINT('',(0.00677218164542555,-0.0350943706855873,0.0683762809279056));
#65174=CARTESIAN_POINT('Origin',(0.0134090578226959,-0.0338370705483153,
0.0760846895319725));
#65175=CARTESIAN_POINT('',(0.00695692276348947,-0.035195137125491,0.0684389408106166));
#65176=CARTESIAN_POINT('Origin',(0.00424642782830705,-0.0338370705333258,
0.0782296181675427));
#65177=CARTESIAN_POINT('',(0.00698865443472587,-0.0352722979006255,0.0685112368885413));
#65178=CARTESIAN_POINT('Origin',(0.0120279371145698,-0.034606957903202,
0.0669252498662866));
#65179=CARTESIAN_POINT('',(0.00716725070746612,-0.0352740680168103,0.0684798501077816));
#65180=CARTESIAN_POINT('Origin',(0.00698671489911995,-0.0305802162291834,
0.0677373793531191));
#65181=CARTESIAN_POINT('',(0.00734650657738756,-0.035272816532173,0.0684514000564886));
#65182=CARTESIAN_POINT('Origin',(0.00734678431164021,-0.0288496123715145,
0.0693520192202523));
#65183=CARTESIAN_POINT('',(0.00735283085609856,-0.0351949306052069,0.0683719553778551));
#65184=CARTESIAN_POINT('Ctrl Pts',(0.00734650657213241,-0.035272816530353,
0.0684514000578559));
#65185=CARTESIAN_POINT('Ctrl Pts',(0.0073486038052232,-0.0352468764909534,
0.0684249337744054));
#65186=CARTESIAN_POINT('Ctrl Pts',(0.00735071185697431,-0.0352209141752708,
0.0683984519488246));
#65187=CARTESIAN_POINT('Ctrl Pts',(0.00735283085705102,-0.0351949306073981,
0.0683719553757825));
#65188=CARTESIAN_POINT('',(0.00750647830044633,-0.0350943706855873,0.0682524079601858));
#65189=CARTESIAN_POINT('Origin',(0.0131249009244661,-0.0338370705545213,
0.0767318545731042));
#65190=CARTESIAN_POINT('',(0.0076819093138999,-0.0351951371254915,0.068337727952706));
#65191=CARTESIAN_POINT('Origin',(0.00376569017080977,-0.0338370705271979,
0.0777114878440688));
#65192=CARTESIAN_POINT('',(0.00770432967021006,-0.0352722979006254,0.068413430987425));
#65193=CARTESIAN_POINT('Origin',(0.0129026529829984,-0.0346069579031808,
0.0674715395396379));
#65194=CARTESIAN_POINT('',(0.00788545146471963,-0.0352740680168103,0.0684046757491718));
#65195=CARTESIAN_POINT('Origin',(0.007799395495655,-0.0305802162292729,
0.0676454324615505));
#65196=CARTESIAN_POINT('',(0.00806685958548826,-0.035272816532173,0.0683989167528435));
#65197=CARTESIAN_POINT('Origin',(0.00795425761772123,-0.0288496123715584,
0.0692924690748105));
#65198=CARTESIAN_POINT('Ctrl Pts',(0.00806685958010319,-0.035272816530353,
0.0683989167535414));
#65199=CARTESIAN_POINT('Ctrl Pts',(0.00807225738087576,-0.0352468764904448,
0.0683729220171362));
#65200=CARTESIAN_POINT('Ctrl Pts',(0.00807766786294621,-0.0352209141742528,
0.0683469132170922));
#65201=CARTESIAN_POINT('Ctrl Pts',(0.00808309105535896,-0.0351949306058699,
0.0683208911580634));
#65202=CARTESIAN_POINT('Ctrl Pts',(0.00611239953422995,-0.0321934096636941,
0.0795381792420887));
#65203=CARTESIAN_POINT('Ctrl Pts',(0.0062088453767827,-0.0320508460844199,
0.0795741820338511));
#65204=CARTESIAN_POINT('Ctrl Pts',(0.00630618582282729,-0.0319086045662818,
0.0796075663699033));
#65205=CARTESIAN_POINT('Ctrl Pts',(0.00640420536345943,-0.0317669892867522,
0.0796382776227359));
#65206=CARTESIAN_POINT('Ctrl Pts',(0.00619157146001148,-0.0321934096636941,
0.0795657879145643));
#65207=CARTESIAN_POINT('Ctrl Pts',(0.00628851148465414,-0.0320508460844199,
0.0796003735665574));
#65208=CARTESIAN_POINT('Ctrl Pts',(0.00638630766442437,-0.0319086045662818,
0.0796323285536707));
#65209=CARTESIAN_POINT('Ctrl Pts',(0.00648474376251334,-0.0317669892867522,
0.079661601406819));
#65210=CARTESIAN_POINT('Ctrl Pts',(0.00627074338579301,-0.0321934096636941,
0.07959339658704));
#65211=CARTESIAN_POINT('Ctrl Pts',(0.00636817759252559,-0.0320508460844199,
0.0796265650992637));
#65212=CARTESIAN_POINT('Ctrl Pts',(0.00646642950602144,-0.0319086045662818,
0.0796570907374381));
#65213=CARTESIAN_POINT('Ctrl Pts',(0.00656528216156726,-0.0317669892867522,
0.0796849251909021));
#65214=CARTESIAN_POINT('Ctrl Pts',(0.00634991531157455,-0.0321934096636941,
0.0796210052595158));
#65215=CARTESIAN_POINT('Ctrl Pts',(0.00644784370039705,-0.0320508460844199,
0.07965275663197));
#65216=CARTESIAN_POINT('Ctrl Pts',(0.00654655134761852,-0.0319086045662818,
0.0796818529212054));
#65217=CARTESIAN_POINT('Ctrl Pts',(0.00664582056062116,-0.0317669892867522,
0.0797082489749852));
#65218=CARTESIAN_POINT('',(0.00634849891017779,-0.0321934096636941,0.0796205113349072));
#65219=CARTESIAN_POINT('',(0.00657475148852131,-0.0318665617511335,0.0796888291962702));
#65220=CARTESIAN_POINT('Origin',(0.0120877674127181,-0.0326371944420803,
0.0639272420168472));
#65221=CARTESIAN_POINT('Origin',(0.00362254235843933,-0.0316939261509517,
0.0902449672848619));
#65222=CARTESIAN_POINT('',(0.00623028697057217,-0.0320197221621733,0.0795806781352575));
#65223=CARTESIAN_POINT('Ctrl Pts',(0.006230440319499,-0.0320197392094662,
0.0795807815711654));
#65224=CARTESIAN_POINT('Ctrl Pts',(0.00625807389753705,-0.0319792716575961,
0.0795904154589886));
#65225=CARTESIAN_POINT('Ctrl Pts',(0.00628590671902399,-0.0319386439829625,
0.0795998825366595));
#65226=CARTESIAN_POINT('Ctrl Pts',(0.00631397072666642,-0.0318979099381557,
0.0796091847358133));
#65227=CARTESIAN_POINT('Ctrl Pts',(0.00634203417960238,-0.0318571766984883,
0.0796184867511021));
#65228=CARTESIAN_POINT('Ctrl Pts',(0.00637018561218629,-0.0318163871833556,
0.0796275783066765));
#65229=CARTESIAN_POINT('Ctrl Pts',(0.00639832711295821,-0.0317755399638303,
0.0796364314820802));
#65230=CARTESIAN_POINT('',(0.00623046951091843,-0.0321934096636184,0.0795793523635383));
#65231=CARTESIAN_POINT('Origin',(0.00549057998102661,-0.032411138515515,
0.0817649442849136));
#65232=CARTESIAN_POINT('',(0.00628948421055811,-0.0321934096636663,0.0795999318492328));
#65233=CARTESIAN_POINT('Ctrl Pts',(0.00634761694800813,-0.0321934096636618,
0.0796186849094062));
#65234=CARTESIAN_POINT('Ctrl Pts',(0.00642303437495258,-0.0320835708272592,
0.0796431796123983));
#65235=CARTESIAN_POINT('Ctrl Pts',(0.00649891497332981,-0.0319739230346488,
0.0796660993477363));
#65236=CARTESIAN_POINT('Ctrl Pts',(0.00657515940862739,-0.0318646057455573,
0.0796874222421317));
#65237=CARTESIAN_POINT('Ctrl Pts',(0.0063968930671626,-0.0321934096636618,
0.0797207291588613));
#65238=CARTESIAN_POINT('Ctrl Pts',(0.00647371776383567,-0.0320835708272592,
0.0797445443057667));
#65239=CARTESIAN_POINT('Ctrl Pts',(0.00655099075229,-0.0319739230346488,
0.0797667557558143));
#65240=CARTESIAN_POINT('Ctrl Pts',(0.0066286109860951,-0.0318646057455573,
0.0797873426786399));
#65241=CARTESIAN_POINT('Ctrl Pts',(0.00644616918631708,-0.0321934096636618,
0.0798227734083164));
#65242=CARTESIAN_POINT('Ctrl Pts',(0.00652440115271877,-0.0320835708272592,
0.0798459089991351));
#65243=CARTESIAN_POINT('Ctrl Pts',(0.00660306653125019,-0.0319739230346488,
0.0798674121638922));
#65244=CARTESIAN_POINT('Ctrl Pts',(0.00668206256356282,-0.0318646057455573,
0.0798872631151482));
#65245=CARTESIAN_POINT('Ctrl Pts',(0.00649544530547155,-0.0321934096636618,
0.0799248176577715));
#65246=CARTESIAN_POINT('Ctrl Pts',(0.00657508454160187,-0.0320835708272592,
0.0799472736925035));
#65247=CARTESIAN_POINT('Ctrl Pts',(0.00665514231021038,-0.0319739230346488,
0.0799680685719702));
#65248=CARTESIAN_POINT('Ctrl Pts',(0.00673551414103053,-0.0318646057455573,
0.0799871835516564));
#65249=CARTESIAN_POINT('',(0.00650778413467281,-0.0321763980308508,0.0799282826387235));
#65250=CARTESIAN_POINT('',(0.00649544530549579,-0.0321934096636184,0.0799248176577655));
#65251=CARTESIAN_POINT('Origin',(0.0115523914991793,-0.032638623128404,
0.0641682690361009));
#65252=CARTESIAN_POINT('Ctrl Pts',(0.00650778413552138,-0.0321763980306373,
0.0799282826356648));
#65253=CARTESIAN_POINT('Ctrl Pts',(0.00651934361022421,-0.0321259596176374,
0.0798869497196757));
#65254=CARTESIAN_POINT('Ctrl Pts',(0.00653070280202329,-0.0320749164634477,
0.0798463329500821));
#65255=CARTESIAN_POINT('Ctrl Pts',(0.00655302976147259,-0.0319716057793998,
0.0797664990161937));
#65256=CARTESIAN_POINT('Ctrl Pts',(0.00656398882969326,-0.0319193786690191,
0.079727312958225));
#65257=CARTESIAN_POINT('Ctrl Pts',(0.00657475148901346,-0.0318665617525394,
0.0796888291944782));
#65258=CARTESIAN_POINT('',(0.00642197210784679,-0.0321934096636663,0.0797726644963464));
#65259=CARTESIAN_POINT('Ctrl Pts',(0.00642018079033925,-0.0327445246967098,
0.0796432565260038));
#65260=CARTESIAN_POINT('Ctrl Pts',(0.0066273623471771,-0.032443687833936,
0.0797075089032933));
#65261=CARTESIAN_POINT('Ctrl Pts',(0.00683879507475351,-0.0321434074405927,
0.0797559729847424));
#65262=CARTESIAN_POINT('Ctrl Pts',(0.00666051466053194,-0.0327445246967098,
0.0797121015028591));
#65263=CARTESIAN_POINT('Ctrl Pts',(0.00687029274811941,-0.032443687833936,
0.0797672895400524));
#65264=CARTESIAN_POINT('Ctrl Pts',(0.00708363186683336,-0.0321434074405927,
0.0798065194509301));
#65265=CARTESIAN_POINT('',(0.00669549827496981,-0.0326943950436612,0.0797211874900408));
#65266=CARTESIAN_POINT('',(0.00692559410938842,-0.0323666188837389,0.0797751640257003));
#65267=CARTESIAN_POINT('Origin',(0.0107966333535284,-0.032639557911179,
0.063418158651594));
#65268=CARTESIAN_POINT('',(0.00692587713480487,-0.0321934096636183,0.0797738352990901));
#65269=CARTESIAN_POINT('Origin',(0.0046246570713615,-0.0321933825603155,
0.0905774351089828));
#65270=CARTESIAN_POINT('',(0.0068036198394134,-0.032193409653269,0.0797477938830148));
#65271=CARTESIAN_POINT('',(0.00686474848660418,-0.0321934096584275,0.0797608145910825));
#65272=CARTESIAN_POINT('',(0.00657475148825586,-0.0325210109756238,0.0796888291971702));
#65273=CARTESIAN_POINT('Origin',(0.0112554365552375,-0.032639312915934,
0.0635619781636827));
#65274=CARTESIAN_POINT('',(0.00657511738662487,-0.0326943950436595,0.0796875208638126));
#65275=CARTESIAN_POINT('Origin',(0.00359563216993536,-0.0326943765538142,
0.0903411861737025));
#65276=CARTESIAN_POINT('',(0.00663530783080734,-0.0326943950436703,0.0797043541769368));
#65277=CARTESIAN_POINT('Ctrl Pts',(0.00680357784751435,-0.0321934096636941,
0.0797477849389554));
#65278=CARTESIAN_POINT('Ctrl Pts',(0.00695375916615836,-0.0319797282159868,
0.0797832043113791));
#65279=CARTESIAN_POINT('Ctrl Pts',(0.00710562359026252,-0.0317669959604736,
0.0798105201877894));
#65280=CARTESIAN_POINT('Ctrl Pts',(0.00704813442386174,-0.0321934096636941,
0.0797998767133908));
#65281=CARTESIAN_POINT('Ctrl Pts',(0.00719971329733514,-0.0319797282159868,
0.0798287349496652));
#65282=CARTESIAN_POINT('Ctrl Pts',(0.0073526214655046,-0.0317669959604736,
0.0798494241930394));
#65283=CARTESIAN_POINT('Ctrl Pts',(0.00704960156178621,-0.0321934096636941,
0.0798001892211097));
#65284=CARTESIAN_POINT('Ctrl Pts',(0.00720118881943688,-0.0319797282159868,
0.0798290080959742));
#65285=CARTESIAN_POINT('Ctrl Pts',(0.00735410324921062,-0.0317669959604736,
0.0798496575850109));
#65286=CARTESIAN_POINT('',(0.00692586345786333,-0.0320197259213208,0.079775175606695));
#65287=CARTESIAN_POINT('Ctrl Pts',(0.00692602729464874,-0.0320197391311198,
0.0797752572332416));
#65288=CARTESIAN_POINT('Ctrl Pts',(0.00695465041516763,-0.0319792715672862,
0.0797813517959236));
#65289=CARTESIAN_POINT('Ctrl Pts',(0.00698345031945878,-0.0319386438886458,
0.0797872558098532));
#65290=CARTESIAN_POINT('Ctrl Pts',(0.00701245886379329,-0.0318979098685799,
0.079792967204071));
#65291=CARTESIAN_POINT('Ctrl Pts',(0.00704146683463511,-0.0318571766538168,
0.0797986784853758));
#65292=CARTESIAN_POINT('Ctrl Pts',(0.00707053584027515,-0.031816387180722,
0.0798041699052481));
#65293=CARTESIAN_POINT('Ctrl Pts',(0.00709956503935144,-0.0317755399642094,
0.0798094261960755));
#65294=CARTESIAN_POINT('Origin',(0.00652527656989749,-0.0323427478904392,
0.0816545449409095));
#65295=CARTESIAN_POINT('',(0.00704813442396921,-0.0321934096636941,0.0797998767134112));
#65296=CARTESIAN_POINT('',(0.00698700577939704,-0.0321934096636663,0.0797868560062607));
#65297=CARTESIAN_POINT('',(0.00728116543148289,-0.0318665617561286,0.0798392989017126));
#65298=CARTESIAN_POINT('Origin',(0.0107752588915392,-0.0326371944422002,
0.0635110324311407));
#65299=CARTESIAN_POINT('Origin',(0.00567527026384143,-0.0316939261508471,
0.0906822086115865));
#65300=CARTESIAN_POINT('Ctrl Pts',(0.00669450361246156,-0.0326943950436604,
0.0797194204763658));
#65301=CARTESIAN_POINT('Ctrl Pts',(0.00677126066483236,-0.0325844576448134,
0.0797391186139606));
#65302=CARTESIAN_POINT('Ctrl Pts',(0.00684843053920001,-0.0324744968375322,
0.0797572306839354));
#65303=CARTESIAN_POINT('Ctrl Pts',(0.00692591404093729,-0.0323646534831894,
0.0797737348438269));
#65304=CARTESIAN_POINT('Ctrl Pts',(0.00675008982741099,-0.0326943950436604,
0.0798181691487118));
#65305=CARTESIAN_POINT('Ctrl Pts',(0.00682820782156145,-0.0325844576448134,
0.079837101204085));
#65306=CARTESIAN_POINT('Ctrl Pts',(0.00690672289018837,-0.0324744968375322,
0.079854418991114));
#65307=CARTESIAN_POINT('Ctrl Pts',(0.0069855341291601,-0.0323646534831894,
0.07987010170879));
#65308=CARTESIAN_POINT('Ctrl Pts',(0.00680567604236041,-0.0326943950436604,
0.0799169178210579));
#65309=CARTESIAN_POINT('Ctrl Pts',(0.00688515497829054,-0.0325844576448134,
0.0799350837942094));
#65310=CARTESIAN_POINT('Ctrl Pts',(0.00696501524117674,-0.0324744968375322,
0.0799516072982926));
#65311=CARTESIAN_POINT('Ctrl Pts',(0.00704515421738291,-0.0323646534831894,
0.0799664685737531));
#65312=CARTESIAN_POINT('Ctrl Pts',(0.00686126225730983,-0.0326943950436604,
0.080015666493404));
#65313=CARTESIAN_POINT('Ctrl Pts',(0.00694210213501962,-0.0325844576448134,
0.0800330663843338));
#65314=CARTESIAN_POINT('Ctrl Pts',(0.0070233075921651,-0.0324744968375322,
0.0800487956054711));
#65315=CARTESIAN_POINT('Ctrl Pts',(0.00710477430560572,-0.0323646534831894,
0.0800628354387162));
#65316=CARTESIAN_POINT('',(0.00687379430653122,-0.0326773559991385,0.0800183498757061));
#65317=CARTESIAN_POINT('',(0.00686126225730346,-0.0326943950436594,0.0800156664933914));
#65318=CARTESIAN_POINT('Origin',(0.0102840270947223,-0.0326395669596865,
0.0637670848817632));
#65319=CARTESIAN_POINT('Ctrl Pts',(0.00687379430722387,-0.0326773559987502,
0.0800183498724243));
#65320=CARTESIAN_POINT('Ctrl Pts',(0.00688274285206967,-0.0326267922587361,
0.0799763389116804));
#65321=CARTESIAN_POINT('Ctrl Pts',(0.00689153279042086,-0.0325756109582127,
0.0799350725648748));
#65322=CARTESIAN_POINT('Ctrl Pts',(0.00690880293489446,-0.0324719985462384,
0.0798539939790238));
#65323=CARTESIAN_POINT('Ctrl Pts',(0.00691727621436546,-0.0324196091621787,
0.0798142142587047));
#65324=CARTESIAN_POINT('Ctrl Pts',(0.0069255941093985,-0.0323666188837757,
0.0797751640256525));
#65325=CARTESIAN_POINT('',(0.00677838026614664,-0.0326943950436703,0.0798684269917262));
#65326=CARTESIAN_POINT('Ctrl Pts',(0.0070470305045208,-0.0321934096636617,
0.0797981752289914));
#65327=CARTESIAN_POINT('Ctrl Pts',(0.00712492324285888,-0.0320835708272592,
0.0798130244739482));
#65328=CARTESIAN_POINT('Ctrl Pts',(0.00720307810459581,-0.0319739230346488,
0.0798262531195679));
#65329=CARTESIAN_POINT('Ctrl Pts',(0.00728139379705147,-0.0318646057455573,
0.079837851914955));
#65330=CARTESIAN_POINT('Ctrl Pts',(0.00710870760250867,-0.0321934096636617,
0.0798932388937096));
#65331=CARTESIAN_POINT('Ctrl Pts',(0.00718791134287151,-0.0320835708272592,
0.0799072375634168));
#65332=CARTESIAN_POINT('Ctrl Pts',(0.00726735884358815,-0.0319739230346488,
0.0799195889960363));
#65333=CARTESIAN_POINT('Ctrl Pts',(0.00734694724427252,-0.0318646057455573,
0.0799302851899337));
#65334=CARTESIAN_POINT('Ctrl Pts',(0.00717038470049655,-0.0321934096636617,
0.0799883025584277));
#65335=CARTESIAN_POINT('Ctrl Pts',(0.00725089944288413,-0.0320835708272592,
0.0800014506528853));
#65336=CARTESIAN_POINT('Ctrl Pts',(0.00733163958258048,-0.0319739230346488,
0.0800129248725047));
#65337=CARTESIAN_POINT('Ctrl Pts',(0.00741250069149358,-0.0318646057455573,
0.0800227184649123));
#65338=CARTESIAN_POINT('Ctrl Pts',(0.00723206179848442,-0.0321934096636617,
0.0800833662231458));
#65339=CARTESIAN_POINT('Ctrl Pts',(0.00731388754289675,-0.0320835708272592,
0.0800956637423538));
#65340=CARTESIAN_POINT('Ctrl Pts',(0.00739592032157282,-0.0319739230346488,
0.0801062607489731));
#65341=CARTESIAN_POINT('Ctrl Pts',(0.00747805413871463,-0.0318646057455573,
0.080115151739891));
#65342=CARTESIAN_POINT('',(0.00723206179850728,-0.0321934096636184,0.0800833662231361));
#65343=CARTESIAN_POINT('',(0.00714009811124825,-0.0321934096636663,0.0799416214682837));
#65344=CARTESIAN_POINT('',(0.0072447376095977,-0.0321763980308323,0.0800852574163262));
#65345=CARTESIAN_POINT('Origin',(0.0102743132755924,-0.032638623121943,
0.0638172591966035));
#65346=CARTESIAN_POINT('Ctrl Pts',(0.0072447376100568,-0.032176398030638,
0.0800852574131847));
#65347=CARTESIAN_POINT('Ctrl Pts',(0.00725102554679725,-0.0321259596179443,
0.0800428016334987));
#65348=CARTESIAN_POINT('Ctrl Pts',(0.00725720453687498,-0.0320749164640583,
0.0800010814552825));
#65349=CARTESIAN_POINT('Ctrl Pts',(0.00726934959633817,-0.0319716057814242,
0.0799190787268633));
#65350=CARTESIAN_POINT('Ctrl Pts',(0.00727531093351594,-0.0319193786724658,
0.0798788281282486));
#65351=CARTESIAN_POINT('Ctrl Pts',(0.00728116543149043,-0.0318665617561676,
0.0798392989016617));
#65352=CARTESIAN_POINT('Origin',(0.00812378219310841,-0.0315241814719618,
0.07415));
#65353=CARTESIAN_POINT('',(0.00650778413457271,-0.032210423332376,0.0799282826390797));
#65354=CARTESIAN_POINT('',(0.00652013033595527,-0.0321934096636183,0.0799317212593733));
#65355=CARTESIAN_POINT('Origin',(0.011510859167661,-0.0326387222458553,
0.064150091005772));
#65356=CARTESIAN_POINT('Origin',(0.0103707261840096,-0.0326386250403645,
0.0638377917879493));
#65357=CARTESIAN_POINT('Origin',(0.0104156615022366,-0.0326387237688314,
0.0638438037632278));
#65358=CARTESIAN_POINT('Ctrl Pts',(0.00628253620983209,-0.0325229783203769,
0.0798605002608448));
#65359=CARTESIAN_POINT('Ctrl Pts',(0.00636125533104743,-0.032413025309245,
0.0798858817964589));
#65360=CARTESIAN_POINT('Ctrl Pts',(0.00644048756263473,-0.0323031222208069,
0.0799096310763216));
#65361=CARTESIAN_POINT('Ctrl Pts',(0.00652013034027635,-0.0321934096576658,
0.0799317212605718));
#65362=CARTESIAN_POINT('Ctrl Pts',(0.00638006773521382,-0.0325229783203769,
0.0798028049942006));
#65363=CARTESIAN_POINT('Ctrl Pts',(0.00645799152844019,-0.032413025309245,
0.0798268420598701));
#65364=CARTESIAN_POINT('Ctrl Pts',(0.00653640074057769,-0.0323031222208069,
0.0798492635260847));
#65365=CARTESIAN_POINT('Ctrl Pts',(0.00661519392155494,-0.0321934096576658,
0.0798700442166176));
#65366=CARTESIAN_POINT('Ctrl Pts',(0.00647759926059556,-0.0325229783203769,
0.0797451097275563));
#65367=CARTESIAN_POINT('Ctrl Pts',(0.00655472772583294,-0.032413025309245,
0.0797678023232814));
#65368=CARTESIAN_POINT('Ctrl Pts',(0.00663231391852064,-0.0323031222208069,
0.0797888959758477));
#65369=CARTESIAN_POINT('Ctrl Pts',(0.00671025750283354,-0.0321934096576658,
0.0798083671726634));
#65370=CARTESIAN_POINT('Ctrl Pts',(0.00657513078597729,-0.0325229783203769,
0.0796874144609121));
#65371=CARTESIAN_POINT('Ctrl Pts',(0.0066514639232257,-0.032413025309245,
0.0797087625866926));
#65372=CARTESIAN_POINT('Ctrl Pts',(0.00672822709646359,-0.0323031222208069,
0.0797285284256107));
#65373=CARTESIAN_POINT('Ctrl Pts',(0.00680532108411213,-0.0321934096576658,
0.0797466901287092));
#65374=CARTESIAN_POINT('',(0.00666187508717938,-0.0321934096584275,0.0798397575712243));
#65375=CARTESIAN_POINT('Ctrl Pts',(0.00650778413550527,-0.0322104233328919,
0.0799282826357219));
#65376=CARTESIAN_POINT('Ctrl Pts',(0.00651935927351475,-0.032260942183129,
0.0798868937128506));
#65377=CARTESIAN_POINT('Ctrl Pts',(0.00653072611711976,-0.0323120888240578,
0.0798462495829169));
#65378=CARTESIAN_POINT('Ctrl Pts',(0.00655305324555121,-0.0324156524631808,
0.0797664150448035));
#65379=CARTESIAN_POINT('Ctrl Pts',(0.00656400435275298,-0.0324680267167312,
0.0797272574528198));
#65380=CARTESIAN_POINT('Ctrl Pts',(0.00657475148827184,-0.0325210109755912,
0.0796888291971297));
#65381=CARTESIAN_POINT('Origin',(0.000857015991460974,-0.0262834582511143,
0.0711337946337778));
#65382=CARTESIAN_POINT('Origin',(-4.30651632228096E-5,-0.0342770750354629,
0.0831569757493063));
#65383=CARTESIAN_POINT('Origin',(0.00812378219310841,-0.0315241814719618,
0.07415));
#65384=CARTESIAN_POINT('',(0.00687379430654047,-0.0327114338379849,0.0800183498756619));
#65385=CARTESIAN_POINT('',(0.00688633205822609,-0.0326943950436593,0.080021006486431));
#65386=CARTESIAN_POINT('Origin',(0.0102395545876542,-0.0326395654975294,
0.0637584004514019));
#65387=CARTESIAN_POINT('Origin',(0.0103823027994842,-0.0326395685578362,
0.0637880142693136));
#65388=CARTESIAN_POINT('Origin',(0.0104264524945685,-0.0326395670824504,
0.0637982142985762));
#65389=CARTESIAN_POINT('Origin',(0.00812378219310841,-0.0315241814719618,
0.07415));
#65390=CARTESIAN_POINT('',(0.00724473760954337,-0.0322104233323761,0.0800852574166919));
#65391=CARTESIAN_POINT('Origin',(0.00910588055929315,-0.0326387236910637,
0.0636378225172512));
#65392=CARTESIAN_POINT('',(0.00725741743084164,-0.0321934096636185,0.0800871215330948));
#65393=CARTESIAN_POINT('Origin',(0.0102308302744509,-0.0326387223938502,
0.063804430290524));
#65394=CARTESIAN_POINT('Origin',(0.00906054610542325,-0.032638624887444,
0.0636374902704471));
#65395=CARTESIAN_POINT('Ctrl Pts',(0.00676850500884118,-0.0332451089994433,
0.0797393960992048));
#65396=CARTESIAN_POINT('Ctrl Pts',(0.00697931253171443,-0.0329451141710254,
0.0797905112144965));
#65397=CARTESIAN_POINT('Ctrl Pts',(0.00719337137210792,-0.0326442513127493,
0.0798256022327296));
#65398=CARTESIAN_POINT('Ctrl Pts',(0.00701268781257067,-0.0332451089994433,
0.0797930128723526));
#65399=CARTESIAN_POINT('Ctrl Pts',(0.00722551752512797,-0.0329451141710254,
0.0798349184825263));
#65400=CARTESIAN_POINT('Ctrl Pts',(0.00744089911280378,-0.0326442513127493,
0.0798606738392798));
#65401=CARTESIAN_POINT('Ctrl Pts',(0.00701512964060797,-0.0332451089994433,
0.0797935490400841));
#65402=CARTESIAN_POINT('Ctrl Pts',(0.0072279795750621,-0.0329451141710254,
0.0798353625552067));
#65403=CARTESIAN_POINT('Ctrl Pts',(0.00744337439021074,-0.0326442513127493,
0.0798610245553452));
#65404=CARTESIAN_POINT('',(0.00704813442391742,-0.0331951640388616,0.0797998767134014));
#65405=CARTESIAN_POINT('',(0.00728116544438958,-0.0328677532355034,0.0798392989097624));
#65406=CARTESIAN_POINT('Origin',(0.00942570137070009,-0.0326402808280126,
0.0632053166742233));
#65407=CARTESIAN_POINT('',(0.00728136446697921,-0.0326943950436593,0.0798379550257279));
#65408=CARTESIAN_POINT('Origin',(0.0056617568152294,-0.0326944278779099,
0.0907760213917055));
#65409=CARTESIAN_POINT('',(0.00715771327076763,-0.0326943950436593,0.0798196415968991));
#65410=CARTESIAN_POINT('',(0.00721953886888343,-0.0326943950436693,0.0798287983113235));
#65411=CARTESIAN_POINT('',(0.00692559410938562,-0.0330220786163545,0.0797751640256997));
#65412=CARTESIAN_POINT('Origin',(0.00990488328926026,-0.0326396682763397,
0.06324452552734));
#65413=CARTESIAN_POINT('',(0.00692587713480482,-0.0331951640388587,0.0797738352990901));
#65414=CARTESIAN_POINT('Origin',(0.00462763753303142,-0.0331952026560205,
0.0905634351200403));
#65415=CARTESIAN_POINT('',(0.00698700577937112,-0.0331951640388701,0.0797868560062557));
#65416=CARTESIAN_POINT('Ctrl Pts',(0.00712210179944357,-0.0327445246967096,
0.0798134584300539));
#65417=CARTESIAN_POINT('Ctrl Pts',(0.00733570262603343,-0.032443687833936,
0.0798512374237038));
#65418=CARTESIAN_POINT('Ctrl Pts',(0.00755154230344066,-0.0321434074405928,
0.0798728198039668));
#65419=CARTESIAN_POINT('Ctrl Pts',(0.00736916912884946,-0.0327445246967096,
0.0798516387226174));
#65420=CARTESIAN_POINT('Ctrl Pts',(0.00758420994871405,-0.032443687833936,
0.0798800994196052));
#65421=CARTESIAN_POINT('Ctrl Pts',(0.00780078363633826,-0.0321434074405928,
0.079892281509324));
#65422=CARTESIAN_POINT('Ctrl Pts',(0.00737163980214352,-0.0327445246967096,
0.079852020525543));
#65423=CARTESIAN_POINT('Ctrl Pts',(0.00758669502194085,-0.032443687833936,
0.0798803880395643));
#65424=CARTESIAN_POINT('Ctrl Pts',(0.00780327604966724,-0.0321434074405928,
0.0798924761263776));
#65425=CARTESIAN_POINT('',(0.00728116543147845,-0.0325210109756238,0.079839298901712));
#65426=CARTESIAN_POINT('',(0.00751561932206926,-0.032193409653269,0.079869113822887));
#65427=CARTESIAN_POINT('Origin',(0.00990371151108213,-0.0326393129157963,
0.0632529675118896));
#65428=CARTESIAN_POINT('Origin',(0.00566063188032259,-0.0326943765538233,
0.0907810415460278));
#65429=CARTESIAN_POINT('',(0.00740501566319187,-0.0326943950436612,0.079856268454557));
#65430=CARTESIAN_POINT('',(0.00734319006509555,-0.0326943950436702,0.0798471117401525));
#65431=CARTESIAN_POINT('',(0.00764006217698056,-0.0323666188837389,0.0798809807141534));
#65432=CARTESIAN_POINT('Origin',(0.00943050074521163,-0.0326395579110436,
0.0631677853481666));
#65433=CARTESIAN_POINT('',(0.00764017643705447,-0.0321934096636184,0.0798796269924588));
#65434=CARTESIAN_POINT('Origin',(0.00671115127334794,-0.0321933825602894,
0.0908864564610883));
#65435=CARTESIAN_POINT('',(0.00757789787906403,-0.0321934096584275,0.0798743704077667));
#65436=CARTESIAN_POINT('Ctrl Pts',(0.00664473569757571,-0.0330240426238172,
0.0799648449217574));
#65437=CARTESIAN_POINT('Ctrl Pts',(0.00672484085150183,-0.032914277406352,
0.0799852202281985));
#65438=CARTESIAN_POINT('Ctrl Pts',(0.00680540715526839,-0.0328043479726691,
0.0800039496951787));
#65439=CARTESIAN_POINT('Ctrl Pts',(0.00688633205822612,-0.0326943950436593,
0.080021006486431));
#65440=CARTESIAN_POINT('Ctrl Pts',(0.00673845201798835,-0.0330240426238172,
0.0799011394488928));
#65441=CARTESIAN_POINT('Ctrl Pts',(0.00681767956696052,-0.032914277406352,
0.0799202237217169));
#65442=CARTESIAN_POINT('Ctrl Pts',(0.00689734113898388,-0.0328043479726691,
0.0799376796539984));
#65443=CARTESIAN_POINT('Ctrl Pts',(0.00697733529750685,-0.0326943950436593,
0.079953482072883));
#65444=CARTESIAN_POINT('Ctrl Pts',(0.00683216833840099,-0.0330240426238172,
0.0798374339760282));
#65445=CARTESIAN_POINT('Ctrl Pts',(0.00691051828241921,-0.032914277406352,
0.0798552272152352));
#65446=CARTESIAN_POINT('Ctrl Pts',(0.00698927512269936,-0.0328043479726691,
0.0798714096128182));
#65447=CARTESIAN_POINT('Ctrl Pts',(0.00706833853678758,-0.0326943950436593,
0.079885957659335));
#65448=CARTESIAN_POINT('Ctrl Pts',(0.00692588465881363,-0.0330240426238172,
0.0797737285031636));
#65449=CARTESIAN_POINT('Ctrl Pts',(0.00700335699787791,-0.032914277406352,
0.0797902307087535));
#65450=CARTESIAN_POINT('Ctrl Pts',(0.00708120910641484,-0.0328043479726691,
0.0798051395716379));
#65451=CARTESIAN_POINT('Ctrl Pts',(0.00715934177606831,-0.0326943950436593,
0.079818433245787));
#65452=CARTESIAN_POINT('',(0.00702202266450686,-0.0326943950436694,0.0799203240416751));
#65453=CARTESIAN_POINT('Ctrl Pts',(0.00687379430722661,-0.0327114338383317,
0.0800183498724113));
#65454=CARTESIAN_POINT('Ctrl Pts',(0.00688274136365943,-0.0327619876830968,
0.0799763458993577));
#65455=CARTESIAN_POINT('Ctrl Pts',(0.00689153057501085,-0.0328131562604328,
0.0799350829656163));
#65456=CARTESIAN_POINT('Ctrl Pts',(0.00690880070357794,-0.0329167375858765,
0.079854004454442));
#65457=CARTESIAN_POINT('Ctrl Pts',(0.00691727473948476,-0.032969108892062,
0.0798142211828647));
#65458=CARTESIAN_POINT('Ctrl Pts',(0.00692559410939825,-0.0330220786163187,
0.0797751640256538));
#65459=CARTESIAN_POINT('Ctrl Pts',(0.00701277044732563,-0.0325229783203769,
0.0800462405735153));
#65460=CARTESIAN_POINT('Ctrl Pts',(0.00709404999468926,-0.032413025309245,
0.0800615558461347));
#65461=CARTESIAN_POINT('Ctrl Pts',(0.00717563403050498,-0.032303122220807,
0.0800751874240448));
#65462=CARTESIAN_POINT('Ctrl Pts',(0.00725741743527886,-0.0321934096576659,
0.0800871215337423));
#65463=CARTESIAN_POINT('Ctrl Pts',(0.00710230177316844,-0.0325229783203769,
0.0799767763098309));
#65464=CARTESIAN_POINT('Ctrl Pts',(0.00718262375717627,-0.032413025309245,
0.0799908573950815));
#65465=CARTESIAN_POINT('Ctrl Pts',(0.00726322484411828,-0.032303122220807,
0.0800032747812394));
#65466=CARTESIAN_POINT('Ctrl Pts',(0.00734400122846935,-0.0321934096576659,
0.080014016205666));
#65467=CARTESIAN_POINT('Ctrl Pts',(0.00719183309901126,-0.0325229783203769,
0.0799073120461464));
#65468=CARTESIAN_POINT('Ctrl Pts',(0.00727119751966328,-0.032413025309245,
0.0799201589440282));
#65469=CARTESIAN_POINT('Ctrl Pts',(0.00735081565773157,-0.032303122220807,
0.0799313621384341));
#65470=CARTESIAN_POINT('Ctrl Pts',(0.00743058502165983,-0.0321934096576659,
0.0799409108775897));
#65471=CARTESIAN_POINT('Ctrl Pts',(0.00728136442485407,-0.0325229783203769,
0.079837847782462));
#65472=CARTESIAN_POINT('Ctrl Pts',(0.00735977128215028,-0.032413025309245,
0.0798494604929749));
#65473=CARTESIAN_POINT('Ctrl Pts',(0.00743840647134487,-0.032303122220807,
0.0798594494956288));
#65474=CARTESIAN_POINT('Ctrl Pts',(0.00751716881485032,-0.0321934096576659,
0.0798678055495134));
#65475=CARTESIAN_POINT('Ctrl Pts',(0.0072447376100483,-0.0322104233328924,
0.0800852574132425));
#65476=CARTESIAN_POINT('Ctrl Pts',(0.00725103406710004,-0.0322609421831292,
0.0800427441049149));
#65477=CARTESIAN_POINT('Ctrl Pts',(0.00725721721951797,-0.0323120888240568,
0.0800009958228221));
#65478=CARTESIAN_POINT('Ctrl Pts',(0.0072693623710612,-0.032415652463181,
0.0799189924726836));
#65479=CARTESIAN_POINT('Ctrl Pts',(0.00727531937788986,-0.0324680267167315,
0.0798787711123318));
#65480=CARTESIAN_POINT('Ctrl Pts',(0.00728116543148923,-0.0325210109755912,
0.0798392989016698));
#65481=CARTESIAN_POINT('',(0.00738651837595761,-0.0321934096584275,0.0799781176780848));
#65482=CARTESIAN_POINT('Ctrl Pts',(0.0070470305962444,-0.0331951640388604,
0.0797981753703263));
#65483=CARTESIAN_POINT('Ctrl Pts',(0.00716380300075277,-0.0330306422010619,
0.0798204365192424));
#65484=CARTESIAN_POINT('Ctrl Pts',(0.00728139570075475,-0.0328657861914644,
0.0798378523198839));
#65485=CARTESIAN_POINT('Ctrl Pts',(0.00704813442391434,-0.0331951640388604,
0.0797998767134008));
#65486=CARTESIAN_POINT('Ctrl Pts',(0.00716494200259997,-0.0330306422010619,
0.0798221150413876));
#65487=CARTESIAN_POINT('Ctrl Pts',(0.00728256890351013,-0.0328657861914644,
0.0798395065868143));
#65488=CARTESIAN_POINT('Ctrl Pts',(0.00723206179851563,-0.0331951640388604,
0.0800833662231506));
#65489=CARTESIAN_POINT('Ctrl Pts',(0.00735473034105878,-0.0330306422010619,
0.0801018019705908));
#65490=CARTESIAN_POINT('Ctrl Pts',(0.00747805603302103,-0.0328657861914644,
0.0801151519449496));
#65491=CARTESIAN_POINT('',(0.0072447376087371,-0.0331781648281939,0.0800852574177228));
#65492=CARTESIAN_POINT('',(0.00723206179850726,-0.0331951640388588,0.0800833662231361));
#65493=CARTESIAN_POINT('Origin',(0.00895854672991136,-0.0326412092321598,
0.0636520794477061));
#65494=CARTESIAN_POINT('Ctrl Pts',(0.0072447376074011,-0.033178164828644,
0.0800852574164436));
#65495=CARTESIAN_POINT('Ctrl Pts',(0.00725103492480123,-0.0331276811546784,
0.080042738216493));
#65496=CARTESIAN_POINT('Ctrl Pts',(0.00725721849869883,-0.0330765663497804,
0.0800009867766641));
#65497=CARTESIAN_POINT('Ctrl Pts',(0.00726936363266433,-0.0329730614463303,
0.0799189835691956));
#65498=CARTESIAN_POINT('Ctrl Pts',(0.00727532029166565,-0.0329207133374016,
0.079878764929847));
#65499=CARTESIAN_POINT('Ctrl Pts',(0.00728116542928284,-0.0328677532289389,
0.079839298916334));
#65500=CARTESIAN_POINT('',(0.00714009811122234,-0.0331951640388701,0.0799416214682788));
#65501=CARTESIAN_POINT('Ctrl Pts',(0.00740380737835698,-0.0326943950436604,
0.0798546400385811));
#65502=CARTESIAN_POINT('Ctrl Pts',(0.00752174670447765,-0.0325294772287039,
0.079869524999578));
#65503=CARTESIAN_POINT('Ctrl Pts',(0.00764020046178808,-0.0323646534831895,
0.0798795227037504));
#65504=CARTESIAN_POINT('Ctrl Pts',(0.00740501566318987,-0.0326943950436604,
0.0798562684545567));
#65505=CARTESIAN_POINT('Ctrl Pts',(0.00752298865563857,-0.0325294772287039,
0.0798711284351345));
#65506=CARTESIAN_POINT('Ctrl Pts',(0.00764147501804653,-0.0323646534831895,
0.0798810997887738));
#65507=CARTESIAN_POINT('Ctrl Pts',(0.00760638055272833,-0.0326943950436604,
0.0801276496671071));
#65508=CARTESIAN_POINT('Ctrl Pts',(0.00772996415638362,-0.0325294772287039,
0.080138346573553));
#65509=CARTESIAN_POINT('Ctrl Pts',(0.00785388427222964,-0.0323646534831895,
0.0801439265187721));
#65510=CARTESIAN_POINT('',(0.00760638055272024,-0.0326943950436594,0.0801276496670952));
#65511=CARTESIAN_POINT('',(0.00750569810796606,-0.0326943950436702,0.0799919590608361));
#65512=CARTESIAN_POINT('',(0.00761915009913651,-0.0326773559992498,0.080128741208886));
#65513=CARTESIAN_POINT('Origin',(0.0089656686821606,-0.0326395670106896,
0.0635782065413069));
#65514=CARTESIAN_POINT('Ctrl Pts',(0.00761915009765573,-0.0326773559997669,
0.0801287412078143));
#65515=CARTESIAN_POINT('Ctrl Pts',(0.00762276268675555,-0.0326267924002059,
0.0800859400983815));
#65516=CARTESIAN_POINT('Ctrl Pts',(0.00762631123906512,-0.0325756107621957,
0.0800438972503982));
#65517=CARTESIAN_POINT('Ctrl Pts',(0.00763328334109336,-0.0324719987229943,
0.0799612937629902));
#65518=CARTESIAN_POINT('Ctrl Pts',(0.00763670417734596,-0.0324196089019014,
0.079920765339583));
#65519=CARTESIAN_POINT('Ctrl Pts',(0.00764006217694614,-0.0323666188837573,
0.079880980714126));
#65520=CARTESIAN_POINT('Origin',(0.00812378219310841,-0.0315241814719618,
0.07415));
#65521=CARTESIAN_POINT('',(0.00724473760960414,-0.0332121607144381,0.0800852574162843));
#65522=CARTESIAN_POINT('',(0.00725741743084167,-0.0331951640388587,0.0800871215330948));
#65523=CARTESIAN_POINT('Origin',(0.00891321520677268,-0.0326413632176459,
0.0636532890694186));
#65524=CARTESIAN_POINT('Origin',(0.0103677068612828,-0.0326412105375278,
0.0638607799806587));
#65525=CARTESIAN_POINT('Origin',(0.0104107413389209,-0.032641364003851,
0.0638750845771472));
#65526=CARTESIAN_POINT('Origin',(0.00812378219310841,-0.0315241814719618,
0.07415));
#65527=CARTESIAN_POINT('',(0.00761915009998218,-0.0327114338379849,0.0801287412078418));
#65528=CARTESIAN_POINT('Origin',(0.0091108725407328,-0.0326395670427101,
0.0635912399722349));
#65529=CARTESIAN_POINT('',(0.00763192194936946,-0.0326943950436594,0.0801298054734803));
#65530=CARTESIAN_POINT('Origin',(0.00892045828662401,-0.0326395654740188,
0.0635751647114222));
#65531=CARTESIAN_POINT('Origin',(0.00906579254212087,-0.0326395685432592,
0.063586653804524));
#65532=CARTESIAN_POINT('Ctrl Pts',(0.00712211991050009,-0.0337436976235975,
0.0798134616332768));
#65533=CARTESIAN_POINT('Ctrl Pts',(0.00717305794275089,-0.0336723290703325,
0.0798224707356528));
#65534=CARTESIAN_POINT('Ctrl Pts',(0.00722414977978394,-0.033601104548885,
0.0798305621659212));
#65535=CARTESIAN_POINT('Ctrl Pts',(0.0073872758947078,-0.0333736987606856,
0.0798563964999464));
#65536=CARTESIAN_POINT('Ctrl Pts',(0.00755161571374524,-0.0331450831799191,
0.0798728271439816));
#65537=CARTESIAN_POINT('Ctrl Pts',(0.00736918736200067,-0.0337436976235975,
0.079851641135749));
#65538=CARTESIAN_POINT('Ctrl Pts',(0.00742046878648296,-0.0336723290703325,
0.079858428076022));
#65539=CARTESIAN_POINT('Ctrl Pts',(0.00747186399050261,-0.033601104548885,
0.0798642915271371));
#65540=CARTESIAN_POINT('Ctrl Pts',(0.00763595869612106,-0.0333736987606856,
0.0798830123650636));
#65541=CARTESIAN_POINT('Ctrl Pts',(0.00780085729627007,-0.0331450831799191,
0.07989228565216));
#65542=CARTESIAN_POINT('Ctrl Pts',(0.00737165803651567,-0.0337436976235975,
0.0798520229307737));
#65543=CARTESIAN_POINT('Ctrl Pts',(0.00742294289492028,-0.0336723290703325,
0.0798587876494257));
#65544=CARTESIAN_POINT('Ctrl Pts',(0.0074743411326098,-0.033601104548885,
0.0798646288207493));
#65545=CARTESIAN_POINT('Ctrl Pts',(0.00763844552413519,-0.0333736987606856,
0.0798832785237148));
#65546=CARTESIAN_POINT('Ctrl Pts',(0.00780334971209532,-0.0331450831799191,
0.0798924802372417));
#65547=CARTESIAN_POINT('',(0.0074050156632065,-0.0336938721132548,0.0798562684545589));
#65548=CARTESIAN_POINT('',(0.00764006219165131,-0.0333679870047996,0.0798809807154008));
#65549=CARTESIAN_POINT('Ctrl Pts',(0.00740501566320096,-0.0336938721132527,
0.0798562684545586));
#65550=CARTESIAN_POINT('Ctrl Pts',(0.00742728990584582,-0.0336629187933873,
0.0798590741375051));
#65551=CARTESIAN_POINT('Ctrl Pts',(0.00744957345305481,-0.0336319952301012,
0.0798617484984804));
#65552=CARTESIAN_POINT('Ctrl Pts',(0.00747186399050984,-0.0336011045488922,
0.0798642915271382));
#65553=CARTESIAN_POINT('Ctrl Pts',(0.00752779857637719,-0.0335235892595425,
0.0798706728562161));
#65554=CARTESIAN_POINT('Ctrl Pts',(0.00758387658419767,-0.0334458668665543,
0.0798762384027458));
#65555=CARTESIAN_POINT('Ctrl Pts',(0.00764006217985969,-0.0333679869962467,
0.0798809807146459));
#65556=CARTESIAN_POINT('',(0.00764017643705453,-0.0331951640388586,0.0798796269924588));
#65557=CARTESIAN_POINT('Ctrl Pts',(0.00764010643901735,-0.0333679692468943,
0.0798809851401499));
#65558=CARTESIAN_POINT('Ctrl Pts',(0.00764013865025297,-0.0333391895417487,
0.0798805330337325));
#65559=CARTESIAN_POINT('Ctrl Pts',(0.00764015955517311,-0.0333104081136032,
0.0798801939271189));
#65560=CARTESIAN_POINT('Ctrl Pts',(0.00764018169841457,-0.033253269932262,
0.0798797447215171));
#65561=CARTESIAN_POINT('Ctrl Pts',(0.00764018322692077,-0.0332249176543048,
0.0798796312789282));
#65562=CARTESIAN_POINT('Ctrl Pts',(0.00764017665659403,-0.0331960985149987,
0.0798796270408481));
#65563=CARTESIAN_POINT('Ctrl Pts',(0.00764017654790957,-0.0331956312777104,
0.0798796270018154));
#65564=CARTESIAN_POINT('Ctrl Pts',(0.00764017643705271,-0.0331951640388586,
0.0798796269924586));
#65565=CARTESIAN_POINT('',(0.0075156193285227,-0.0331951640388587,0.0798691138238489));
#65566=CARTESIAN_POINT('',(0.00757789788279861,-0.0331951640388687,0.0798743704081638));
#65567=CARTESIAN_POINT('',(0.00728116543138446,-0.0335216366567661,0.0798392989013045));
#65568=CARTESIAN_POINT('Origin',(0.0085168111349089,-0.0326434571526396,
0.0632307515618159));
#65569=CARTESIAN_POINT('',(0.00728136446697911,-0.0336938721132327,0.0798379550257279));
#65570=CARTESIAN_POINT('Origin',(0.00568141891782992,-0.0336938867896335,
0.0906406863567228));
#65571=CARTESIAN_POINT('',(0.00734319006510281,-0.0336938721132538,0.0798471117401534));
#65572=CARTESIAN_POINT('Ctrl Pts',(0.00747972886102596,-0.0332451089994432,
0.0798651833133709));
#65573=CARTESIAN_POINT('Ctrl Pts',(0.00769528052629965,-0.0329451141710253,
0.0798894741822098));
#65574=CARTESIAN_POINT('Ctrl Pts',(0.00791204951958449,-0.0326442513127494,
0.0798974598106435));
#65575=CARTESIAN_POINT('Ctrl Pts',(0.00772870617396611,-0.0332451089994432,
0.0798877730818758));
#65576=CARTESIAN_POINT('Ctrl Pts',(0.0079451098262982,-0.0329451141710253,
0.0799026736177233));
#65577=CARTESIAN_POINT('Ctrl Pts',(0.00816202106796723,-0.0326442513127494,
0.0799012314149623));
#65578=CARTESIAN_POINT('',(0.00764006217697776,-0.0330220786163545,0.0798809807141532));
#65579=CARTESIAN_POINT('',(0.0078759255272611,-0.0326943950436594,0.0798960153213506));
#65580=CARTESIAN_POINT('Origin',(0.00852402039608933,-0.0326396682764816,
0.0631072872915801));
#65581=CARTESIAN_POINT('Origin',(0.00671235452142551,-0.0331952026559979,
0.0908721933899018));
#65582=CARTESIAN_POINT('',(0.00776473354558816,-0.0331951640388616,0.0798901401610688));
#65583=CARTESIAN_POINT('',(0.00770245499133134,-0.0331951640388701,0.0798848835767737));
#65584=CARTESIAN_POINT('',(0.00800086794439122,-0.0328677532092643,0.0799000449639514));
#65585=CARTESIAN_POINT('Origin',(0.0080435778561186,-0.0326401908898621,
0.0631284489558804));
#65586=CARTESIAN_POINT('',(0.00800089697811041,-0.0326943950436593,0.0798986867390679));
#65587=CARTESIAN_POINT('Origin',(0.00776458814375024,-0.032694427913436,
0.0909534764247798));
#65588=CARTESIAN_POINT('',(0.00793841125269576,-0.0326943950436694,0.0798973510302193));
#65589=CARTESIAN_POINT('Ctrl Pts',(0.00701277233604355,-0.0335235895815171,
0.0800462409294017));
#65590=CARTESIAN_POINT('Ctrl Pts',(0.00709394570106689,-0.0334144449262748,
0.0800615361674614));
#65591=CARTESIAN_POINT('Ctrl Pts',(0.00717552831255958,-0.0333049234473147,
0.0800751719972648));
#65592=CARTESIAN_POINT('Ctrl Pts',(0.00725741743084065,-0.0331951640388587,
0.0800871215330957));
#65593=CARTESIAN_POINT('Ctrl Pts',(0.00710230374508894,-0.0335235895815171,
0.07997677655522));
#65594=CARTESIAN_POINT('Ctrl Pts',(0.0071825207962389,-0.0334144449262748,
0.079990839217163));
#65595=CARTESIAN_POINT('Ctrl Pts',(0.00726312053107448,-0.0333049234473147,
0.0800032608114941));
#65596=CARTESIAN_POINT('Ctrl Pts',(0.00734400132606785,-0.0331951640388587,
0.0800140161189775));
#65597=CARTESIAN_POINT('Ctrl Pts',(0.00719183515413433,-0.0335235895815171,
0.0799073121810384));
#65598=CARTESIAN_POINT('Ctrl Pts',(0.00727109589141091,-0.0334144449262748,
0.0799201422668647));
#65599=CARTESIAN_POINT('Ctrl Pts',(0.00735071274958938,-0.0333049234473147,
0.0799313496257235));
#65600=CARTESIAN_POINT('Ctrl Pts',(0.00743058522129505,-0.0331951640388587,
0.0799409107048593));
#65601=CARTESIAN_POINT('Ctrl Pts',(0.00728136656317972,-0.0335235895815171,
0.0798378478068567));
#65602=CARTESIAN_POINT('Ctrl Pts',(0.00735967098658292,-0.0334144449262748,
0.0798494453165664));
#65603=CARTESIAN_POINT('Ctrl Pts',(0.00743830496810428,-0.0333049234473147,
0.0798594384399528));
#65604=CARTESIAN_POINT('Ctrl Pts',(0.00751716911652226,-0.0331951640388587,
0.0798678052907411));
#65605=CARTESIAN_POINT('',(0.00738651837969219,-0.0331951640388687,0.0799781176784819));
#65606=CARTESIAN_POINT('Ctrl Pts',(0.0072447376100579,-0.0332121607145959,
0.0800852574131777));
#65607=CARTESIAN_POINT('Ctrl Pts',(0.00725102434571237,-0.0332625444109769,
0.0800428097431533));
#65608=CARTESIAN_POINT('Ctrl Pts',(0.00725720275104595,-0.033313530074687,
0.0800010935130951));
#65609=CARTESIAN_POINT('Ctrl Pts',(0.00726934780540806,-0.0334167203140549,
0.0799190908191178));
#65610=CARTESIAN_POINT('Ctrl Pts',(0.00727530975055819,-0.0334688847587227,
0.0798788361155094));
#65611=CARTESIAN_POINT('Ctrl Pts',(0.00728116543164366,-0.0335216366562291,
0.0798392989006264));
#65612=CARTESIAN_POINT('Ctrl Pts',(0.00738519173768159,-0.0330240426238172,
0.0801043668126164));
#65613=CARTESIAN_POINT('Ctrl Pts',(0.00746721894158385,-0.032914277406352,
0.0801145416157137));
#65614=CARTESIAN_POINT('Ctrl Pts',(0.00754949738064075,-0.0328043479726691,
0.0801230257598851));
#65615=CARTESIAN_POINT('Ctrl Pts',(0.00763192194936942,-0.0326943950436594,
0.0801298054734803));
#65616=CARTESIAN_POINT('Ctrl Pts',(0.00747018466400619,-0.0330240426238172,
0.0800294179069582));
#65617=CARTESIAN_POINT('Ctrl Pts',(0.00755117937371382,-0.032914277406352,
0.0800384218496908));
#65618=CARTESIAN_POINT('Ctrl Pts',(0.00763240059888571,-0.0328043479726691,
0.08004575589432));
#65619=CARTESIAN_POINT('Ctrl Pts',(0.00771374454783255,-0.0326943950436594,
0.0800514077798578));
#65620=CARTESIAN_POINT('Ctrl Pts',(0.00755517759033078,-0.0330240426238172,
0.0799544690012999));
#65621=CARTESIAN_POINT('Ctrl Pts',(0.00763513980584379,-0.032914277406352,
0.0799623020836678));
#65622=CARTESIAN_POINT('Ctrl Pts',(0.00771530381713068,-0.0328043479726691,
0.0799684860287549));
#65623=CARTESIAN_POINT('Ctrl Pts',(0.00779556714629568,-0.0326943950436594,
0.0799730100862353));
#65624=CARTESIAN_POINT('Ctrl Pts',(0.00764017051665538,-0.0330240426238172,
0.0798795200956417));
#65625=CARTESIAN_POINT('Ctrl Pts',(0.00771910023797376,-0.032914277406352,
0.0798861823176449));
#65626=CARTESIAN_POINT('Ctrl Pts',(0.00779820703537564,-0.0328043479726691,
0.0798912161631897));
#65627=CARTESIAN_POINT('Ctrl Pts',(0.00787738974475881,-0.0326943950436594,
0.0798946123926128));
#65628=CARTESIAN_POINT('Ctrl Pts',(0.00761915010025602,-0.0327114338383318,
0.0801287412045299));
#65629=CARTESIAN_POINT('Ctrl Pts',(0.00762276211271095,-0.0327619876830942,
0.0800859470818386));
#65630=CARTESIAN_POINT('Ctrl Pts',(0.00762631040159336,-0.0328131562604278,
0.0800439079383769));
#65631=CARTESIAN_POINT('Ctrl Pts',(0.00763328251806064,-0.0329167375858763,
0.079961304234419));
#65632=CARTESIAN_POINT('Ctrl Pts',(0.00763670356759461,-0.0329691088920606,
0.0799207725875));
#65633=CARTESIAN_POINT('Ctrl Pts',(0.00764006217698454,-0.0330220786163186,
0.079880980714106));
#65634=CARTESIAN_POINT('',(0.00775392373832528,-0.0326943950436694,0.0800129103974254));
#65635=CARTESIAN_POINT('Ctrl Pts',(0.00740380746807937,-0.0336938721132523,
0.079854640159517));
#65636=CARTESIAN_POINT('Ctrl Pts',(0.00743719861993812,-0.0336474569765025,
0.0798588544104961));
#65637=CARTESIAN_POINT('Ctrl Pts',(0.00747063681694241,-0.033601104548885,
0.0798626774871199));
#65638=CARTESIAN_POINT('Ctrl Pts',(0.00755529464382165,-0.0334837508592655,
0.0798723566381497));
#65639=CARTESIAN_POINT('Ctrl Pts',(0.0076402021085357,-0.0333660264659096,
0.0798795229518747));
#65640=CARTESIAN_POINT('Ctrl Pts',(0.00740501566317657,-0.0336938721132523,
0.0798562684545551));
#65641=CARTESIAN_POINT('Ctrl Pts',(0.0074384163459865,-0.0336474569765025,
0.0798604756335674));
#65642=CARTESIAN_POINT('Ctrl Pts',(0.00747186399050261,-0.033601104548885,
0.0798642915271371));
#65643=CARTESIAN_POINT('Ctrl Pts',(0.00755654573630964,-0.0334837508592655,
0.0798739524923255));
#65644=CARTESIAN_POINT('Ctrl Pts',(0.00764147657056388,-0.0333660264659096,
0.0798810999194275));
#65645=CARTESIAN_POINT('Ctrl Pts',(0.00760758874208749,-0.0336938721132523,
0.0801292779544295));
#65646=CARTESIAN_POINT('Ctrl Pts',(0.00764258744009457,-0.0336474569765025,
0.0801322994059899));
#65647=CARTESIAN_POINT('Ctrl Pts',(0.00767761910987388,-0.033601104548885,
0.080134910946569));
#65648=CARTESIAN_POINT('Ctrl Pts',(0.00776631124345654,-0.0334837508592655,
0.0801415227668837));
#65649=CARTESIAN_POINT('Ctrl Pts',(0.00785516035193512,-0.0333660264659096,
0.0801455035519669));
#65650=CARTESIAN_POINT('',(0.00761915009983477,-0.0336769361243754,0.0801287412095221));
#65651=CARTESIAN_POINT('',(0.00760638055271975,-0.0336938721132321,0.0801276496670952));
#65652=CARTESIAN_POINT('Ctrl Pts',(0.00761915009983503,-0.0336769361243751,
0.0801287412095222));
#65653=CARTESIAN_POINT('Ctrl Pts',(0.00761702148825769,-0.0336797586670475,
0.0801285615453289));
#65654=CARTESIAN_POINT('Ctrl Pts',(0.00761489305313471,-0.0336825812713744,
0.0801283807511564));
#65655=CARTESIAN_POINT('Ctrl Pts',(0.00761063654794096,-0.0336882265870973,
0.0801280169044073));
#65656=CARTESIAN_POINT('Ctrl Pts',(0.00760850847778055,-0.0336910492986195,
0.0801278338518592));
#65657=CARTESIAN_POINT('Ctrl Pts',(0.00760638055272642,-0.033693872113238,
0.0801276496671085));
#65658=CARTESIAN_POINT('Ctrl Pts',(0.00761915009983475,-0.0336769361243754,
0.0801287412095221));
#65659=CARTESIAN_POINT('Ctrl Pts',(0.00762267519166302,-0.0336279018525385,
0.0800869768983302));
#65660=CARTESIAN_POINT('Ctrl Pts',(0.00762625099640256,-0.033576782605156,
0.0800446117546109));
#65661=CARTESIAN_POINT('Ctrl Pts',(0.00763325751955493,-0.0334733172106825,
0.0799616004097819));
#65662=CARTESIAN_POINT('Ctrl Pts',(0.00763669294690799,-0.0334209631477589,
0.079920898418453));
#65663=CARTESIAN_POINT('Ctrl Pts',(0.00764006217698056,-0.0333679869844681,
0.0798809807141533));
#65664=CARTESIAN_POINT('',(0.00750569810797312,-0.0336938721132534,0.079991959060837));
#65665=CARTESIAN_POINT('Ctrl Pts',(0.00776342518707949,-0.0331951640388604,
0.0798885905798627));
#65666=CARTESIAN_POINT('Ctrl Pts',(0.00788206687599759,-0.0330306421900773,
0.0798960407304203));
#65667=CARTESIAN_POINT('Ctrl Pts',(0.00800091510898811,-0.0328657861694599,
0.0798985809287791));
#65668=CARTESIAN_POINT('Ctrl Pts',(0.00776473354558501,-0.0331951640388604,
0.0798901401610685));
#65669=CARTESIAN_POINT('Ctrl Pts',(0.00788340727110318,-0.0330306421900773,
0.0798975632621511));
#65670=CARTESIAN_POINT('Ctrl Pts',(0.00800228639533539,-0.0328657861694599,
0.0799000751100419));
#65671=CARTESIAN_POINT('Ctrl Pts',(0.00798274125483999,-0.0331951640388604,
0.0801483420587605));
#65672=CARTESIAN_POINT('Ctrl Pts',(0.0081067531394057,-0.0330306421900773,
0.0801512579899268));
#65673=CARTESIAN_POINT('Ctrl Pts',(0.00823077957518043,-0.0328657861694599,
0.0801490458875051));
#65674=CARTESIAN_POINT('',(0.00798274125482956,-0.0331951640388588,0.0801483420587467));
#65675=CARTESIAN_POINT('',(0.00787373740021886,-0.0331951640388701,0.0800192411099177));
#65676=CARTESIAN_POINT('',(0.0079955541420418,-0.0331781648281943,0.0801486296404161));
#65677=CARTESIAN_POINT('Origin',(0.00763622598507471,-0.0326412091981293,
0.0636302351063101));
#65678=CARTESIAN_POINT('Ctrl Pts',(0.00799555414055663,-0.033178164828644,
0.0801486296393133));
#65679=CARTESIAN_POINT('Ctrl Pts',(0.00799647273296179,-0.033127681151819,
0.0801056564503676));
#65680=CARTESIAN_POINT('Ctrl Pts',(0.00799737470460111,-0.0330765663440246,
0.080063459223434));
#65681=CARTESIAN_POINT('Ctrl Pts',(0.00799914634354069,-0.032973061432112,
0.0799805804403965));
#65682=CARTESIAN_POINT('Ctrl Pts',(0.00800001530045004,-0.0329207133203635,
0.0799399323678051));
#65683=CARTESIAN_POINT('Ctrl Pts',(0.00800086794435749,-0.0328677532092815,
0.0799000449639279));
#65684=CARTESIAN_POINT('Origin',(0.00812378219310841,-0.0315241814719618,
0.07415));
#65685=CARTESIAN_POINT('',(0.00761915009994875,-0.0337108120655531,0.080128741208238));
#65686=CARTESIAN_POINT('',(0.00763192194936942,-0.0336938721132327,0.0801298054734803));
#65687=CARTESIAN_POINT('Origin',(0.0101088601348352,-0.0345562507257751,
0.0639194914324974));
#65688=CARTESIAN_POINT('Ctrl Pts',(0.00763192194936625,-0.0336938721132348,
0.080129805473485));
#65689=CARTESIAN_POINT('Ctrl Pts',(0.00762979326524268,-0.0336910493096957,
0.0801296303816536));
#65690=CARTESIAN_POINT('Ctrl Pts',(0.00762766461530371,-0.0336882265926354,
0.0801294541482935));
#65691=CARTESIAN_POINT('Ctrl Pts',(0.00762340733835879,-0.033682581271277,
0.0801290993943332));
#65692=CARTESIAN_POINT('Ctrl Pts',(0.00762127871137503,-0.0336797586669988,
0.0801289208737123));
#65693=CARTESIAN_POINT('Ctrl Pts',(0.00761915009983449,-0.0336769361243751,
0.0801287412095221));
#65694=CARTESIAN_POINT('Origin',(0.00788156968309789,-0.0345562519616818,
0.0637315024488479));
#65695=CARTESIAN_POINT('Origin',(0.00812378219310841,-0.0315241814719618,
0.07415));
#65696=CARTESIAN_POINT('',(0.00799555414272147,-0.0332121607144207,0.080148629638879));
#65697=CARTESIAN_POINT('Origin',(0.0091049176852243,-0.0326413654380319,
0.0636694742416528));
#65698=CARTESIAN_POINT('',(0.00800836761556968,-0.0331951640388587,0.0801488898535752));
#65699=CARTESIAN_POINT('Origin',(0.00759140414320651,-0.0326413636678921,
0.0636371177732643));
#65700=CARTESIAN_POINT('Origin',(0.00906043161709704,-0.0326412105475495,
0.063660675157574));
#65701=CARTESIAN_POINT('Ctrl Pts',(0.00747965684771335,-0.034243627687391,
0.0798651751976138));
#65702=CARTESIAN_POINT('Ctrl Pts',(0.00769520823370105,-0.0339430054201809,
0.0798894687855002));
#65703=CARTESIAN_POINT('Ctrl Pts',(0.00791197715337794,-0.0336441434784052,
0.0798974571442634));
#65704=CARTESIAN_POINT('Ctrl Pts',(0.00772863387599453,-0.034243627687391,
0.0798877681033205));
#65705=CARTESIAN_POINT('Ctrl Pts',(0.0079450373674681,-0.0339430054201809,
0.0799026713677838));
#65706=CARTESIAN_POINT('Ctrl Pts',(0.00816194865425262,-0.0336441434784052,
0.0799012318959718));
#65707=CARTESIAN_POINT('',(0.00776473354558619,-0.034193496108874,0.0798901401610687));
#65708=CARTESIAN_POINT('',(0.00800086794805514,-0.0338664212895224,0.0799000449648617));
#65709=CARTESIAN_POINT('Origin',(0.00931760079658415,-0.0345610818075694,
0.0632275564000169));
#65710=CARTESIAN_POINT('',(0.00800089697811059,-0.0336938721132326,0.0798986867390679));
#65711=CARTESIAN_POINT('Origin',(0.00776658026320743,-0.0336938005044392,
0.0908637967520959));
#65712=CARTESIAN_POINT('',(0.00787592552726112,-0.0336938721132327,0.0798960153213506));
#65713=CARTESIAN_POINT('',(0.00793841125269586,-0.0336938721132427,0.0798973510302193));
#65714=CARTESIAN_POINT('',(0.00764006217697529,-0.0340203938281606,0.0798809807141529));
#65715=CARTESIAN_POINT('Origin',(0.00978408309822432,-0.0345589643244979,
0.0633455303789544));
#65716=CARTESIAN_POINT('',(0.00764017643705448,-0.034193496108874,0.0798796269924588));
#65717=CARTESIAN_POINT('Origin',(0.00671338119780292,-0.0341934220717617,
0.0908600308491757));
#65718=CARTESIAN_POINT('',(0.00770245499133034,-0.0341934961088841,0.0798848835767737));
#65719=CARTESIAN_POINT('Ctrl Pts',(0.00783983827644646,-0.0337436976235975,
0.0798943451195232));
#65720=CARTESIAN_POINT('Ctrl Pts',(0.00789150378703078,-0.0336723290703325,
0.0798968989541427));
#65721=CARTESIAN_POINT('Ctrl Pts',(0.00794320687478813,-0.033601104548885,
0.0798985230759225));
#65722=CARTESIAN_POINT('Ctrl Pts',(0.0081082845921927,-0.0333736987606857,
0.0799037085750454));
#65723=CARTESIAN_POINT('Ctrl Pts',(0.00827338784841755,-0.0331450831799192,
0.0798994124176215));
#65724=CARTESIAN_POINT('Ctrl Pts',(0.00808974268779718,-0.0337436976235975,
0.0799012578026096));
#65725=CARTESIAN_POINT('Ctrl Pts',(0.00814147037210082,-0.0336723290703325,
0.0799015639590792));
#65726=CARTESIAN_POINT('Ctrl Pts',(0.00819319519487387,-0.033601104548885,
0.0799009396480215));
#65727=CARTESIAN_POINT('Ctrl Pts',(0.00835834230787811,-0.0333736987606857,
0.0798989463464833));
#65728=CARTESIAN_POINT('Ctrl Pts',(0.00852310288436963,-0.0331450831799192,
0.0798874792361743));
#65729=CARTESIAN_POINT('Ctrl Pts',(0.00809224173191068,-0.0337436976235975,
0.0799013269294405));
#65730=CARTESIAN_POINT('Ctrl Pts',(0.00814397003795152,-0.0336723290703325,
0.0799016106091286));
#65731=CARTESIAN_POINT('Ctrl Pts',(0.00819569507807473,-0.033601104548885,
0.0799009638137425));
#65732=CARTESIAN_POINT('Ctrl Pts',(0.00836084288503496,-0.0333736987606857,
0.0798988987241977));
#65733=CARTESIAN_POINT('Ctrl Pts',(0.00852560003472915,-0.0331450831799192,
0.0798873599043598));
#65734=CARTESIAN_POINT('',(0.00800086794424164,-0.0335216366567656,0.07990004496356));
#65735=CARTESIAN_POINT('',(0.00823720990302466,-0.0331951640388587,0.0799002399214836));
#65736=CARTESIAN_POINT('Origin',(0.00714516726941353,-0.0326434571526036,
0.063267593509416));
#65737=CARTESIAN_POINT('Origin',(0.00776750895290892,-0.0336938867896287,
0.0908167616606058));
#65738=CARTESIAN_POINT('',(0.00812586842897576,-0.0336938721132548,0.0799013581567853));
#65739=CARTESIAN_POINT('',(0.00806338270355318,-0.0336938721132536,0.0799000224479366));
#65740=CARTESIAN_POINT('',(0.00836215880828412,-0.0333679869984219,0.079896416412814));
#65741=CARTESIAN_POINT('Ctrl Pts',(0.00812586842898595,-0.0336938721132649,
0.0799013581567863));
#65742=CARTESIAN_POINT('Ctrl Pts',(0.00814831867788204,-0.0336629187933933,
0.0799013500132285));
#65743=CARTESIAN_POINT('Ctrl Pts',(0.00817076169896996,-0.0336319952301041,
0.0799012104170416));
#65744=CARTESIAN_POINT('Ctrl Pts',(0.00819319519488396,-0.0336011045488951,
0.0799009396480218));
#65745=CARTESIAN_POINT('Ctrl Pts',(0.00824948851244248,-0.0335235892595455,
0.079900260195899));
#65746=CARTESIAN_POINT('Ctrl Pts',(0.00830582187881451,-0.033445866867327,
0.0798987534184142));
#65747=CARTESIAN_POINT('Ctrl Pts',(0.00836215880829256,-0.0333679869984152,
0.0798964164132425));
#65748=CARTESIAN_POINT('',(0.00836210249096915,-0.0331951640388588,0.0798950590454431));
#65749=CARTESIAN_POINT('Ctrl Pts',(0.00836220326593144,-0.0333679692463177,
0.0798964152568053));
#65750=CARTESIAN_POINT('Ctrl Pts',(0.00836217855921108,-0.0333391895390484,
0.0798959626782118));
#65751=CARTESIAN_POINT('Ctrl Pts',(0.00836215679795873,-0.0333104081088491,
0.0798956236254674));
#65752=CARTESIAN_POINT('Ctrl Pts',(0.00836212246616085,-0.03325326985216,
0.0798951751861306));
#65753=CARTESIAN_POINT('Ctrl Pts',(0.00836210976142365,-0.0332249172665086,
0.0798950624471958));
#65754=CARTESIAN_POINT('Ctrl Pts',(0.00836210271505692,-0.0331960985307702,
0.0798950590659285));
#65755=CARTESIAN_POINT('Ctrl Pts',(0.00836210260212061,-0.033195631261781,
0.0798950590408323));
#65756=CARTESIAN_POINT('Ctrl Pts',(0.00836210249096896,-0.0331951640388603,
0.0798950590454432));
#65757=CARTESIAN_POINT('',(0.00829965619700691,-0.0331951640388688,0.0798976494834734));
#65758=CARTESIAN_POINT('Ctrl Pts',(0.00738518997603143,-0.0340223579322397,
0.0801043665940979));
#65759=CARTESIAN_POINT('Ctrl Pts',(0.00746731622100408,-0.0339125849573575,
0.0801145537071008));
#65760=CARTESIAN_POINT('Ctrl Pts',(0.00754959560638283,-0.0338030433565231,
0.0801230338393014));
#65761=CARTESIAN_POINT('Ctrl Pts',(0.00763192194936947,-0.0336938721132327,
0.0801298054734804));
#65762=CARTESIAN_POINT('Ctrl Pts',(0.00747018306963347,-0.0340223579322397,
0.08002941758563));
#65763=CARTESIAN_POINT('Ctrl Pts',(0.00755127557230412,-0.0339125849573575,
0.0800384324222008));
#65764=CARTESIAN_POINT('Ctrl Pts',(0.00763249767838148,-0.0338030433565231,
0.080045762497778));
#65765=CARTESIAN_POINT('Ctrl Pts',(0.00771374468752323,-0.0336938721132327,
0.0800514076460144));
#65766=CARTESIAN_POINT('Ctrl Pts',(0.00755517616323551,-0.0340223579322397,
0.0799544685771621));
#65767=CARTESIAN_POINT('Ctrl Pts',(0.00763523492360417,-0.0339125849573575,
0.0799623111373008));
#65768=CARTESIAN_POINT('Ctrl Pts',(0.00771539975038013,-0.0338030433565231,
0.0799684911562546));
#65769=CARTESIAN_POINT('Ctrl Pts',(0.00779556742567699,-0.0336938721132327,
0.0799730098185483));
#65770=CARTESIAN_POINT('Ctrl Pts',(0.00764016925683755,-0.0340223579322397,
0.0798795195686942));
#65771=CARTESIAN_POINT('Ctrl Pts',(0.00771919427490421,-0.0339125849573575,
0.0798861898524009));
#65772=CARTESIAN_POINT('Ctrl Pts',(0.00779830182237878,-0.0338030433565231,
0.0798912198147312));
#65773=CARTESIAN_POINT('Ctrl Pts',(0.00787739016383075,-0.0336938721132327,
0.0798946119910823));
#65774=CARTESIAN_POINT('',(0.00775392373832528,-0.0336938721132427,0.0800129103974254));
#65775=CARTESIAN_POINT('Ctrl Pts',(0.00761915010024686,-0.0337108120662688,
0.0801287412046396));
#65776=CARTESIAN_POINT('Ctrl Pts',(0.00762276656768743,-0.0337611408994229,
0.0800858943005123));
#65777=CARTESIAN_POINT('Ctrl Pts',(0.00762631704262065,-0.0338121088781167,
0.080043829257326));
#65778=CARTESIAN_POINT('Ctrl Pts',(0.00763328924190049,-0.0339153382773235,
0.0799612245722275));
#65779=CARTESIAN_POINT('Ctrl Pts',(0.00763670801657843,-0.0339675558473111,
0.0799207198771726));
#65780=CARTESIAN_POINT('Ctrl Pts',(0.00764006217698382,-0.0340203938281305,
0.0798809807141136));
#65781=CARTESIAN_POINT('Ctrl Pts',(0.0077605279221661,-0.0335235895815172,
0.0801389937664584));
#65782=CARTESIAN_POINT('Ctrl Pts',(0.00784297821260505,-0.0334144449262748,
0.0801439946766798));
#65783=CARTESIAN_POINT('Ctrl Pts',(0.00792562654348016,-0.0333049234473147,
0.0801472979713915));
#65784=CARTESIAN_POINT('Ctrl Pts',(0.00800836761556974,-0.0331951640388588,
0.0801488898535752));
#65785=CARTESIAN_POINT('Ctrl Pts',(0.00784064715467543,-0.0335235895815172,
0.0800588558786143));
#65786=CARTESIAN_POINT('Ctrl Pts',(0.00792199418931122,-0.0334144449262748,
0.0800627537898599));
#65787=CARTESIAN_POINT('Ctrl Pts',(0.00800351520974718,-0.0333049234473147,
0.0800649756108182));
#65788=CARTESIAN_POINT('Ctrl Pts',(0.00808510623297895,-0.0331951640388588,
0.0800655090579198));
#65789=CARTESIAN_POINT('Ctrl Pts',(0.00792076638718476,-0.0335235895815172,
0.0799787179907701));
#65790=CARTESIAN_POINT('Ctrl Pts',(0.00800101016601739,-0.0334144449262748,
0.07998151290304));
#65791=CARTESIAN_POINT('Ctrl Pts',(0.0080814038760142,-0.0333049234473147,
0.079982653250245));
#65792=CARTESIAN_POINT('Ctrl Pts',(0.00816184485038816,-0.0331951640388588,
0.0799821282622644));
#65793=CARTESIAN_POINT('Ctrl Pts',(0.00800088561969408,-0.0335235895815172,
0.0798985801029259));
#65794=CARTESIAN_POINT('Ctrl Pts',(0.00808002614272356,-0.0334144449262748,
0.0799002720162201));
#65795=CARTESIAN_POINT('Ctrl Pts',(0.00815929254228122,-0.0333049234473147,
0.0799003308896717));
#65796=CARTESIAN_POINT('Ctrl Pts',(0.00823858346779737,-0.0331951640388588,
0.0798987474666089));
#65797=CARTESIAN_POINT('Ctrl Pts',(0.00799555414278324,-0.0332121607145974,
0.080148629635739));
#65798=CARTESIAN_POINT('Ctrl Pts',(0.00799647120190776,-0.0332625444109692,
0.080105728741371));
#65799=CARTESIAN_POINT('Ctrl Pts',(0.00799737245866444,-0.033313530074669,
0.080063567096736));
#65800=CARTESIAN_POINT('Ctrl Pts',(0.00799914408284852,-0.0334167203140551,
0.0799806888395441));
#65801=CARTESIAN_POINT('Ctrl Pts',(0.00800001376411097,-0.033468884758723,
0.0799400043264331));
#65802=CARTESIAN_POINT('Ctrl Pts',(0.00800086794441465,-0.0335216366562283,
0.0799000449628543));
#65803=CARTESIAN_POINT('',(0.00812278875930717,-0.0331951640388687,0.0800245648875394));
#65804=CARTESIAN_POINT('Ctrl Pts',(0.00776342512837748,-0.0341934961088741,
0.0798885905103364));
#65805=CARTESIAN_POINT('Ctrl Pts',(0.0078425568931179,-0.0340836138583034,
0.0798935596208554));
#65806=CARTESIAN_POINT('Ctrl Pts',(0.00792175351426542,-0.0339738896647349,
0.0798968888812743));
#65807=CARTESIAN_POINT('Ctrl Pts',(0.00800091334428685,-0.033864463329982,
0.0798985808253354));
#65808=CARTESIAN_POINT('Ctrl Pts',(0.00783653050386538,-0.0341934961088741,
0.0799751743598111));
#65809=CARTESIAN_POINT('Ctrl Pts',(0.00791685620861504,-0.0340836138583034,
0.0799791353904951));
#65810=CARTESIAN_POINT('Ctrl Pts',(0.00799722533680004,-0.0339738896647349,
0.0799814323486915));
#65811=CARTESIAN_POINT('Ctrl Pts',(0.00807753482879076,-0.033864463329982,
0.0799820691899589));
#65812=CARTESIAN_POINT('Ctrl Pts',(0.00790963587935328,-0.0341934961088741,
0.0800617582092858));
#65813=CARTESIAN_POINT('Ctrl Pts',(0.00799115552411218,-0.0340836138583034,
0.0800647111601349));
#65814=CARTESIAN_POINT('Ctrl Pts',(0.00807269715933465,-0.0339738896647349,
0.0800659758161088));
#65815=CARTESIAN_POINT('Ctrl Pts',(0.00815415631329468,-0.033864463329982,
0.0800655575545823));
#65816=CARTESIAN_POINT('Ctrl Pts',(0.00798274125484118,-0.0341934961088741,
0.0801483420587605));
#65817=CARTESIAN_POINT('Ctrl Pts',(0.00806545483960932,-0.0340836138583034,
0.0801502869297746));
#65818=CARTESIAN_POINT('Ctrl Pts',(0.00814816898186926,-0.0339738896647349,
0.080150519283526));
#65819=CARTESIAN_POINT('Ctrl Pts',(0.0082307777977986,-0.033864463329982,
0.0801490459192057));
#65820=CARTESIAN_POINT('',(0.00799555414272003,-0.0341764758832475,0.0801486296389534));
#65821=CARTESIAN_POINT('',(0.00798274125482951,-0.034193496108874,0.0801483420587467));
#65822=CARTESIAN_POINT('Origin',(0.008861397458876,-0.0345621026442791,
0.0636056055471864));
#65823=CARTESIAN_POINT('Ctrl Pts',(0.00799555414278307,-0.0341764758830276,
0.0801486296357497));
#65824=CARTESIAN_POINT('Ctrl Pts',(0.00799647149735682,-0.0341260048548319,
0.0801057149199867));
#65825=CARTESIAN_POINT('Ctrl Pts',(0.00799737289797397,-0.034074927129329,
0.0800635465454208));
#65826=CARTESIAN_POINT('Ctrl Pts',(0.00799914452350784,-0.033971543442925,
0.0799806682250842));
#65827=CARTESIAN_POINT('Ctrl Pts',(0.00800001405517191,-0.0339192781035257,
0.0799399907103279));
#65828=CARTESIAN_POINT('Ctrl Pts',(0.00800086794432318,-0.0338664212877424,
0.0799000449671372));
#65829=CARTESIAN_POINT('',(0.00787373740021786,-0.0341934961088841,0.0800192411099177));
#65830=CARTESIAN_POINT('Ctrl Pts',(0.00812586842894504,-0.033693872113253,
0.0799013581567852));
#65831=CARTESIAN_POINT('Ctrl Pts',(0.00815953303674479,-0.0336474569765028,
0.0799013459453546));
#65832=CARTESIAN_POINT('Ctrl Pts',(0.00819319519487387,-0.033601104548885,
0.0799009396480215));
#65833=CARTESIAN_POINT('Ctrl Pts',(0.0082784200398284,-0.0334837508592655,
0.0798999109965879));
#65834=CARTESIAN_POINT('Ctrl Pts',(0.00836357697923725,-0.0333660264659097,
0.0798963574080059));
#65835=CARTESIAN_POINT('Ctrl Pts',(0.00836106132202396,-0.033693872113253,
0.0801468257561836));
#65836=CARTESIAN_POINT('Ctrl Pts',(0.00839616273313799,-0.0336474569765028,
0.0801454368827042));
#65837=CARTESIAN_POINT('Ctrl Pts',(0.00843124548056321,-0.033601104548885,
0.0801436371980553));
#65838=CARTESIAN_POINT('Ctrl Pts',(0.00852006693100108,-0.0334837508592655,
0.0801390808102985));
#65839=CARTESIAN_POINT('Ctrl Pts',(0.00860871436238776,-0.0333660264659097,
0.0801318944596376));
#65840=CARTESIAN_POINT('',(0.00835965858108673,-0.0336938721132327,0.0801453617346741));
#65841=CARTESIAN_POINT('',(0.00824276350504124,-0.0336938721132538,0.0800233599457397));
#65842=CARTESIAN_POINT('',(0.00837246424305004,-0.0336769361243754,0.0801448442213319));
#65843=CARTESIAN_POINT('Ctrl Pts',(0.0083724642430503,-0.0336769361243751,
0.0801448442213319));
#65844=CARTESIAN_POINT('Ctrl Pts',(0.00837032989836826,-0.0336797586669794,
0.0801449327596143));
#65845=CARTESIAN_POINT('Ctrl Pts',(0.00836819558712512,-0.0336825812712383,
0.0801450201547123));
#65846=CARTESIAN_POINT('Ctrl Pts',(0.00836392704416631,-0.0336882265862871,
0.0801451926585425));
#65847=CARTESIAN_POINT('Ctrl Pts',(0.00836179281252015,-0.0336910492969991,
0.0801452777673101));
#65848=CARTESIAN_POINT('Ctrl Pts',(0.00835965858109482,-0.0336938721132384,
0.0801453617346872));
#65849=CARTESIAN_POINT('Ctrl Pts',(0.00837246424305002,-0.0336769361243754,
0.0801448442213319));
#65850=CARTESIAN_POINT('Ctrl Pts',(0.00837072712806767,-0.0336279031442069,
0.0801029685261757));
#65851=CARTESIAN_POINT('Ctrl Pts',(0.00836896502031064,-0.0335767852183815,
0.0800604903436776));
#65852=CARTESIAN_POINT('Ctrl Pts',(0.00836551221211579,-0.0334733199151731,
0.0799772553564356));
#65853=CARTESIAN_POINT('Ctrl Pts',(0.00836381919334894,-0.0334209645163069,
0.0799364426649829));
#65854=CARTESIAN_POINT('Ctrl Pts',(0.00836215879818742,-0.0333679869844682,
0.0798964164132224));
#65855=CARTESIAN_POINT('Origin',(0.00812378219310841,-0.0315241814719618,
0.07415));
#65856=CARTESIAN_POINT('',(0.00799555414271336,-0.0342105180190348,0.0801486296392591));
#65857=CARTESIAN_POINT('',(0.00800836761556967,-0.034193496108874,0.0801488898535753));
#65858=CARTESIAN_POINT('Origin',(0.0088164943374163,-0.0345621696908114,
0.0635994077056605));
#65859=CARTESIAN_POINT('Origin',(0.00783743114609163,-0.0345621044702029,
0.0635837134576787));
#65860=CARTESIAN_POINT('Origin',(0.00788255835472517,-0.0345621711986352,
0.0635794480198904));
#65861=CARTESIAN_POINT('Origin',(0.00812378219310841,-0.0315241814719618,
0.07415));
#65862=CARTESIAN_POINT('',(0.00837246424300171,-0.0337108120655824,0.0801448442200445));
#65863=CARTESIAN_POINT('Origin',(0.00657769573536795,-0.0345562518668543,
0.0638440125869785));
#65864=CARTESIAN_POINT('',(0.00838526877037957,-0.0336938721132327,0.0801442993560502));
#65865=CARTESIAN_POINT('Origin',(0.00881098448054971,-0.0345562507319043,
0.0637513655757208));
#65866=CARTESIAN_POINT('Ctrl Pts',(0.00838526877037628,-0.0336938721132354,
0.0801442993560566));
#65867=CARTESIAN_POINT('Ctrl Pts',(0.00838313492427463,-0.0336910493064383,
0.0801443924398485));
#65868=CARTESIAN_POINT('Ctrl Pts',(0.00838100097271145,-0.0336882265910066,
0.0801444843866646));
#65869=CARTESIAN_POINT('Ctrl Pts',(0.0083767328044364,-0.0336825812712758,
0.0801446660082786));
#65870=CARTESIAN_POINT('Ctrl Pts',(0.00837459858774597,-0.0336797586669982,
0.0801447556830489));
#65871=CARTESIAN_POINT('Ctrl Pts',(0.00837246424304975,-0.0336769361243751,
0.0801448442213319));
#65872=CARTESIAN_POINT('Ctrl Pts',(0.00787442585994672,-0.0346945769586966,
0.0798959832641261));
#65873=CARTESIAN_POINT('Ctrl Pts',(0.00799477778035788,-0.0345275153357699,
0.0799012061323774));
#65874=CARTESIAN_POINT('Ctrl Pts',(0.00811532508433994,-0.0343603235954687,
0.0799026453943974));
#65875=CARTESIAN_POINT('Ctrl Pts',(0.00823571118321104,-0.0341934961073027,
0.0799003020923843));
#65876=CARTESIAN_POINT('Ctrl Pts',(0.00795824004961583,-0.0346945769586966,
0.0798977748950125));
#65877=CARTESIAN_POINT('Ctrl Pts',(0.00807862949645335,-0.0345275153357699,
0.0799012422414983));
#65878=CARTESIAN_POINT('Ctrl Pts',(0.00819915912702418,-0.0343603235954687,
0.0799009243475134));
#65879=CARTESIAN_POINT('Ctrl Pts',(0.00831947248215584,-0.0341934961073027,
0.0798968274513665));
#65880=CARTESIAN_POINT('Ctrl Pts',(0.00804205423928495,-0.0346945769586966,
0.0798995665258989));
#65881=CARTESIAN_POINT('Ctrl Pts',(0.00816248121254882,-0.0345275153357699,
0.0799012783506192));
#65882=CARTESIAN_POINT('Ctrl Pts',(0.00828299316970842,-0.0343603235954687,
0.0798992033006293));
#65883=CARTESIAN_POINT('Ctrl Pts',(0.00840323378110064,-0.0341934961073027,
0.0798933528103488));
#65884=CARTESIAN_POINT('Ctrl Pts',(0.00812586842895406,-0.0346945769586966,
0.0799013581567853));
#65885=CARTESIAN_POINT('Ctrl Pts',(0.00824633292864429,-0.0345275153357699,
0.0799013144597401));
#65886=CARTESIAN_POINT('Ctrl Pts',(0.00836682721239266,-0.0343603235954687,
0.0798974822537453));
#65887=CARTESIAN_POINT('Ctrl Pts',(0.00848699508004543,-0.0341934961073027,
0.079889878169331));
#65888=CARTESIAN_POINT('',(0.00812586842896553,-0.0346945769586966,0.0799013581567853));
#65889=CARTESIAN_POINT('',(0.00836215879841123,-0.0343667727831679,0.0798964164132529));
#65890=CARTESIAN_POINT('Origin',(0.00793680313391798,-0.0345626457064672,
0.0630888181481351));
#65891=CARTESIAN_POINT('',(0.00836210249096924,-0.0341934961088739,0.0798950590454431));
#65892=CARTESIAN_POINT('Origin',(0.00882024320446819,-0.0341934771029012,
0.0909390978419296));
#65893=CARTESIAN_POINT('',(0.00823720990226415,-0.0341934961076211,0.079900239921759));
#65894=CARTESIAN_POINT('',(0.00829965619643977,-0.034193496108098,0.0798976494834846));
#65895=CARTESIAN_POINT('',(0.00800086794439598,-0.0345211942962625,0.0799000449639508));
#65896=CARTESIAN_POINT('Origin',(0.00841742866201907,-0.0345625558918781,
0.0631024169485933));
#65897=CARTESIAN_POINT('',(0.00800089697811051,-0.0346945769586885,0.0798986867390679));
#65898=CARTESIAN_POINT('Origin',(0.00776445294209699,-0.0346945685854053,
0.0909597269016649));
#65899=CARTESIAN_POINT('',(0.00806338270354802,-0.0346945769587026,0.0799000224479366));
#65900=CARTESIAN_POINT('Ctrl Pts',(0.00819853890223646,-0.034243627687391,
0.079900927549921));
#65901=CARTESIAN_POINT('Ctrl Pts',(0.00841543871042038,-0.033943005420181,
0.0798981080541562));
#65902=CARTESIAN_POINT('Ctrl Pts',(0.00863150995301438,-0.0336441434784053,
0.0798789587860116));
#65903=CARTESIAN_POINT('Ctrl Pts',(0.00820103735635621,-0.034243627687391,
0.0799008396464996));
#65904=CARTESIAN_POINT('Ctrl Pts',(0.00841793384920793,-0.033943005420181,
0.0798979259199843));
#65905=CARTESIAN_POINT('Ctrl Pts',(0.00863399468804203,-0.0336441434784053,
0.0798786829385132));
#65906=CARTESIAN_POINT('Ctrl Pts',(0.00845088276833138,-0.034243627687391,
0.079892049304359));
#65907=CARTESIAN_POINT('Ctrl Pts',(0.00866744772796387,-0.033943005420181,
0.0798797125027897));
#65908=CARTESIAN_POINT('Ctrl Pts',(0.00888246819080694,-0.0336441434784053,
0.0798510981886735));
#65909=CARTESIAN_POINT('',(0.00836215879818212,-0.0340203938281605,0.0798964164132226));
#65910=CARTESIAN_POINT('',(0.00859804663143739,-0.0336938721132327,0.0798817709516813));
#65911=CARTESIAN_POINT('Origin',(0.00841683201496112,-0.0345589643243666,
0.0632226359681015));
#65912=CARTESIAN_POINT('Origin',(0.00881882493712156,-0.0341934220717763,
0.0909050373789402));
#65913=CARTESIAN_POINT('',(0.00848699507891361,-0.0341934961088741,0.0798898781694027));
#65914=CARTESIAN_POINT('',(0.00842454878495143,-0.0341934961088841,0.079892468607433));
#65915=CARTESIAN_POINT('',(0.00872250889090621,-0.0338664212874645,0.0798701093824915));
#65916=CARTESIAN_POINT('Origin',(0.0079392327225337,-0.0345610751537147,
0.0631640572814627));
#65917=CARTESIAN_POINT('',(0.0087223674624904,-0.0336938721132328,0.0798687582284338));
#65918=CARTESIAN_POINT('Origin',(0.00986416572584789,-0.0336938005063908,
0.09077677479047));
#65919=CARTESIAN_POINT('',(0.0086602070469739,-0.0336938721132427,0.0798752645900675));
#65920=CARTESIAN_POINT('Ctrl Pts',(0.00776052615137487,-0.0345231616327895,
0.0801389936590533));
#65921=CARTESIAN_POINT('Ctrl Pts',(0.00784307599736326,-0.0344132092794018,
0.0801440006321788));
#65922=CARTESIAN_POINT('Ctrl Pts',(0.007925725149449,-0.0343032738552988,
0.0801472998685129));
#65923=CARTESIAN_POINT('Ctrl Pts',(0.00800836761624737,-0.0341934961079738,
0.0801488898535884));
#65924=CARTESIAN_POINT('Ctrl Pts',(0.00784064529399383,-0.0345231616327895,
0.0800588559085098));
#65925=CARTESIAN_POINT('Ctrl Pts',(0.00792209055391287,-0.0344132092794018,
0.08006275855205));
#65926=CARTESIAN_POINT('Ctrl Pts',(0.00800361233473437,-0.0343032738552988,
0.0800649763632687));
#65927=CARTESIAN_POINT('Ctrl Pts',(0.00808510612485482,-0.0341934961079738,
0.0800655091761332));
#65928=CARTESIAN_POINT('Ctrl Pts',(0.00792076443661279,-0.0345231616327895,
0.0799787181579662));
#65929=CARTESIAN_POINT('Ctrl Pts',(0.00800110511046248,-0.0344132092794018,
0.0799815164719211));
#65930=CARTESIAN_POINT('Ctrl Pts',(0.00808149952001974,-0.0343032738552988,
0.0799826528580245));
#65931=CARTESIAN_POINT('Ctrl Pts',(0.00816184463346228,-0.0341934961079738,
0.079982128498678));
#65932=CARTESIAN_POINT('Ctrl Pts',(0.00800088357923175,-0.0345231616327895,
0.0798985804074227));
#65933=CARTESIAN_POINT('Ctrl Pts',(0.00808011966701209,-0.0344132092794018,
0.0799002743917923));
#65934=CARTESIAN_POINT('Ctrl Pts',(0.00815938670530511,-0.0343032738552988,
0.0799003293527803));
#65935=CARTESIAN_POINT('Ctrl Pts',(0.00823858314206973,-0.0341934961079738,
0.0798987478212229));
#65936=CARTESIAN_POINT('',(0.00812278875873998,-0.034193496108098,0.0800245648875506));
#65937=CARTESIAN_POINT('Ctrl Pts',(0.00799555414278203,-0.0342105180195385,
0.0801486296357966));
#65938=CARTESIAN_POINT('Ctrl Pts',(0.00799647252560746,-0.0342610556241125,
0.0801056668174451));
#65939=CARTESIAN_POINT('Ctrl Pts',(0.00799737442852795,-0.0343122189869793,
0.0800634749446548));
#65940=CARTESIAN_POINT('Ctrl Pts',(0.00799914606515046,-0.0344158119695101,
0.0799805961055804));
#65941=CARTESIAN_POINT('Ctrl Pts',(0.00800001507423936,-0.034468199044999,
0.0799399430373854));
#65942=CARTESIAN_POINT('Ctrl Pts',(0.00800086794439187,-0.0345211942962383,
0.0799000449639186));
#65943=CARTESIAN_POINT('Ctrl Pts',(0.00813729401533547,-0.0340223579322397,
0.0801499847858721));
#65944=CARTESIAN_POINT('Ctrl Pts',(0.00822004945414989,-0.0339125849573575,
0.0801497984226033));
#65945=CARTESIAN_POINT('Ctrl Pts',(0.008302742884389,-0.0338030433565231,
0.0801478993450034));
#65946=CARTESIAN_POINT('Ctrl Pts',(0.00838526877037963,-0.0336938721132327,
0.0801442993560502));
#65947=CARTESIAN_POINT('Ctrl Pts',(0.00821222331142454,-0.0340223579322397,
0.0800649743134704));
#65948=CARTESIAN_POINT('Ctrl Pts',(0.00829380623410792,-0.0339125849573575,
0.0800637544797847));
#65949=CARTESIAN_POINT('Ctrl Pts',(0.00837530658169332,-0.0338030433565231,
0.080060846926335));
#65950=CARTESIAN_POINT('Ctrl Pts',(0.00845662045858306,-0.0336938721132327,
0.0800562646105182));
#65951=CARTESIAN_POINT('Ctrl Pts',(0.00828715260751361,-0.0340223579322397,
0.0799799638410686));
#65952=CARTESIAN_POINT('Ctrl Pts',(0.00836756301406595,-0.0339125849573575,
0.0799777105369661));
#65953=CARTESIAN_POINT('Ctrl Pts',(0.00844787027899764,-0.0338030433565231,
0.0799737945076665));
#65954=CARTESIAN_POINT('Ctrl Pts',(0.00852797214678649,-0.0336938721132327,
0.0799682298649861));
#65955=CARTESIAN_POINT('Ctrl Pts',(0.00836208190360268,-0.0340223579322397,
0.0798949533686669));
#65956=CARTESIAN_POINT('Ctrl Pts',(0.00844131979402398,-0.0339125849573575,
0.0798916665941474));
#65957=CARTESIAN_POINT('Ctrl Pts',(0.00852043397630197,-0.0338030433565231,
0.0798867420889981));
#65958=CARTESIAN_POINT('Ctrl Pts',(0.00859932383498993,-0.0336938721132327,
0.0798801951194541));
#65959=CARTESIAN_POINT('Ctrl Pts',(0.00837246424284696,-0.0337108120662689,
0.080144844216436));
#65960=CARTESIAN_POINT('Ctrl Pts',(0.00837068205231926,-0.0337611408994186,
0.0801018819093909));
#65961=CARTESIAN_POINT('Ctrl Pts',(0.00836893238281478,-0.0338121088781076,
0.0800597035691341));
#65962=CARTESIAN_POINT('Ctrl Pts',(0.00836549649192956,-0.0339153382773238,
0.079976876398362));
#65963=CARTESIAN_POINT('Ctrl Pts',(0.00836381172414221,-0.0339675558473122,
0.0799362626088399));
#65964=CARTESIAN_POINT('Ctrl Pts',(0.00836215879818578,-0.0340203938281304,
0.0798964164131825));
#65965=CARTESIAN_POINT('',(0.00849165770091848,-0.0336938721132427,0.0800130351538757));
#65966=CARTESIAN_POINT('Ctrl Pts',(0.00812446563227316,-0.0346945769586931,
0.079899894077111));
#65967=CARTESIAN_POINT('Ctrl Pts',(0.00820370207897374,-0.034584662917547,
0.0798998846589738));
#65968=CARTESIAN_POINT('Ctrl Pts',(0.00828295186469101,-0.0344746925049099,
0.0798982366620499));
#65969=CARTESIAN_POINT('Ctrl Pts',(0.00836211345418758,-0.034364806625142,
0.0798949526173048));
#65970=CARTESIAN_POINT('Ctrl Pts',(0.00820286328188074,-0.0346945769586931,
0.0799817166296364));
#65971=CARTESIAN_POINT('Ctrl Pts',(0.00828322728471282,-0.034584662917547,
0.0799806268522611));
#65972=CARTESIAN_POINT('Ctrl Pts',(0.00836358247776556,-0.0344746925049099,
0.0799778749941733));
#65973=CARTESIAN_POINT('Ctrl Pts',(0.00844382591526756,-0.034364806625142,
0.0799734650065821));
#65974=CARTESIAN_POINT('Ctrl Pts',(0.00828126093148832,-0.0346945769586931,
0.0800635391821619));
#65975=CARTESIAN_POINT('Ctrl Pts',(0.00836275249045189,-0.034584662917547,
0.0800613690455484));
#65976=CARTESIAN_POINT('Ctrl Pts',(0.0084442130908401,-0.0344746925049099,
0.0800575133262967));
#65977=CARTESIAN_POINT('Ctrl Pts',(0.00852553837634755,-0.034364806625142,
0.0800519773958594));
#65978=CARTESIAN_POINT('Ctrl Pts',(0.0083596585810959,-0.0346945769586931,
0.0801453617346874));
#65979=CARTESIAN_POINT('Ctrl Pts',(0.00844227769619097,-0.034584662917547,
0.0801421112388358));
#65980=CARTESIAN_POINT('Ctrl Pts',(0.00852484370391465,-0.0344746925049099,
0.0801371516584202));
#65981=CARTESIAN_POINT('Ctrl Pts',(0.00860725083742753,-0.034364806625142,
0.0801304897851367));
#65982=CARTESIAN_POINT('',(0.00837246424298863,-0.0346775396663494,0.0801448442197254));
#65983=CARTESIAN_POINT('',(0.00835965858108672,-0.0346945769586886,0.0801453617346741));
#65984=CARTESIAN_POINT('Origin',(0.00753182116752839,-0.0345626618000782,
0.0635645479677025));
#65985=CARTESIAN_POINT('Ctrl Pts',(0.00837246424284332,-0.0346775396659518,
0.0801448442163483));
#65986=CARTESIAN_POINT('Ctrl Pts',(0.0083706837491285,-0.0346269748529746,
0.0801019228134568));
#65987=CARTESIAN_POINT('Ctrl Pts',(0.00836893491328795,-0.0345757904818327,
0.0800597645698871));
#65988=CARTESIAN_POINT('Ctrl Pts',(0.00836549905757979,-0.0344721679344127,
0.0799769382471099));
#65989=CARTESIAN_POINT('Ctrl Pts',(0.00836381342224014,-0.0344197716859661,
0.0799363035439716));
#65990=CARTESIAN_POINT('Ctrl Pts',(0.00836215879819277,-0.0343667727831003,
0.0798964164133518));
#65991=CARTESIAN_POINT('',(0.00824276350503612,-0.0346945769587026,0.0800233599457397));
#65992=CARTESIAN_POINT('Ctrl Pts',(0.00848550275512826,-0.0341934961088741,
0.0798885047252767));
#65993=CARTESIAN_POINT('Ctrl Pts',(0.00856463333733548,-0.0340836138577592,
0.0798835168129129));
#65994=CARTESIAN_POINT('Ctrl Pts',(0.00864362273682097,-0.0339738896636479,
0.0798768938524777));
#65995=CARTESIAN_POINT('Ctrl Pts',(0.00872237042513336,-0.0338644633283559,
0.0798686510975485));
#65996=CARTESIAN_POINT('Ctrl Pts',(0.00856888350709102,-0.0341934961088741,
0.0799652433024739));
#65997=CARTESIAN_POINT('Ctrl Pts',(0.00864907226883839,-0.0340836138577592,
0.0799591056189129));
#65998=CARTESIAN_POINT('Ctrl Pts',(0.00872909554802715,-0.0339738896636479,
0.0799513115421572));
#65999=CARTESIAN_POINT('Ctrl Pts',(0.00880885159344511,-0.0338644633283559,
0.0799418779133713));
#66000=CARTESIAN_POINT('Ctrl Pts',(0.00865226425905377,-0.0341934961088741,
0.080041981879671));
#66001=CARTESIAN_POINT('Ctrl Pts',(0.0087335112003413,-0.0340836138577592,
0.0800346944249129));
#66002=CARTESIAN_POINT('Ctrl Pts',(0.00881456835923333,-0.0339738896636479,
0.0800257292318366));
#66003=CARTESIAN_POINT('Ctrl Pts',(0.00889533276175687,-0.0338644633283559,
0.0800151047291941));
#66004=CARTESIAN_POINT('Ctrl Pts',(0.00873564501101654,-0.0341934961088741,
0.0801187204568681));
#66005=CARTESIAN_POINT('Ctrl Pts',(0.00881795013184422,-0.0340836138577592,
0.0801102832309129));
#66006=CARTESIAN_POINT('Ctrl Pts',(0.00890004117043951,-0.0339738896636479,
0.080100146921516));
#66007=CARTESIAN_POINT('Ctrl Pts',(0.00898181393006862,-0.0338644633283559,
0.0800883315450169));
#66008=CARTESIAN_POINT('',(0.00873564501100223,-0.034193496108874,0.080118720456855));
#66009=CARTESIAN_POINT('',(0.00861132004496793,-0.0341934961088841,0.0800042993131389));
#66010=CARTESIAN_POINT('',(0.00874839290880158,-0.0341764758832693,0.0801173998887386));
#66011=CARTESIAN_POINT('Origin',(0.00753402011430365,-0.0345621044320822,
0.063596300007772));
#66012=CARTESIAN_POINT('Ctrl Pts',(0.00874839290846302,-0.0341764758830294,
0.0801173998855504));
#66013=CARTESIAN_POINT('Ctrl Pts',(0.00874392438930416,-0.0341260048545657,
0.0800747085898974));
#66014=CARTESIAN_POINT('Ctrl Pts',(0.00873953358334686,-0.0340749271287874,
0.0800327597498871));
#66015=CARTESIAN_POINT('Ctrl Pts',(0.00873090383116496,-0.033971543441884,
0.0799503129059302));
#66016=CARTESIAN_POINT('Ctrl Pts',(0.00872666826184563,-0.0339192781023551,
0.0799098471642289));
#66017=CARTESIAN_POINT('Ctrl Pts',(0.00872250888864519,-0.0338664212862971,
0.079870109384281));
#66018=CARTESIAN_POINT('Origin',(0.00812378219310841,-0.0315241814719618,
0.07415));
#66019=CARTESIAN_POINT('',(0.00837246424298395,-0.0347116136489624,0.0801448442196129));
#66020=CARTESIAN_POINT('',(0.00838526877038213,-0.0346945769586885,0.0801442993560471));
#66021=CARTESIAN_POINT('Origin',(0.00748666597710875,-0.0345626706594334,
0.0635682954795692));
#66022=CARTESIAN_POINT('Origin',(0.00783699278750874,-0.034562661800787,
0.0635518887600696));
#66023=CARTESIAN_POINT('Origin',(0.007882302937497,-0.0345626708902314,
0.063551884177655));
#66024=CARTESIAN_POINT('Origin',(0.00812378219310841,-0.0315241814719618,
0.07415));
#66025=CARTESIAN_POINT('',(0.00874839290883282,-0.0342105180190378,0.0801173998890376));
#66026=CARTESIAN_POINT('Origin',(0.00655961767461394,-0.0345621724972048,
0.0636930371683406));
#66027=CARTESIAN_POINT('',(0.00876113795713322,-0.034193496108874,0.0801160520974983));
#66028=CARTESIAN_POINT('Origin',(0.00748869677100344,-0.0345621724912701,
0.0635957898356987));
#66029=CARTESIAN_POINT('Origin',(0.00651538230794598,-0.0345621044227283,
0.0637029211023602));
#66030=CARTESIAN_POINT('Ctrl Pts',(0.00819861739708981,-0.0352450361874067,
0.0799009265290252));
#66031=CARTESIAN_POINT('Ctrl Pts',(0.00841551715029151,-0.0349452760959492,
0.0798981040729926));
#66032=CARTESIAN_POINT('Ctrl Pts',(0.00863158811518962,-0.0346444289841739,
0.0798789518583681));
#66033=CARTESIAN_POINT('Ctrl Pts',(0.00820111585000953,-0.0352450361874067,
0.0799008385915021));
#66034=CARTESIAN_POINT('Ctrl Pts',(0.00841801228659313,-0.0349452760959492,
0.0798979219047714));
#66035=CARTESIAN_POINT('Ctrl Pts',(0.00863407284645355,-0.0346444289841739,
0.0798786759769696));
#66036=CARTESIAN_POINT('Ctrl Pts',(0.008450961145774,-0.0352450361874067,
0.0798920448390692));
#66037=CARTESIAN_POINT('Ctrl Pts',(0.00866752592054227,-0.0349452760959492,
0.0798797050823835));
#66038=CARTESIAN_POINT('Ctrl Pts',(0.00888254597661861,-0.0346444289841739,
0.0798510878367011));
#66039=CARTESIAN_POINT('',(0.00848696272951962,-0.035195163346716,0.0798898823170016));
#66040=CARTESIAN_POINT('',(0.00872250888900978,-0.0348678972936559,0.0798701093821336));
#66041=CARTESIAN_POINT('Origin',(0.00655853854367246,-0.0345631633298701,
0.063255429313764));
#66042=CARTESIAN_POINT('',(0.00872236746249042,-0.0346945769586885,0.0798687582284338));
#66043=CARTESIAN_POINT('Origin',(0.00987283268348529,-0.0346946199326914,
0.0908599115959569));
#66044=CARTESIAN_POINT('',(0.00859804661349631,-0.0346945769330289,0.0798817709530099));
#66045=CARTESIAN_POINT('',(0.00866020703771396,-0.0346945769458128,0.0798752645908338));
#66046=CARTESIAN_POINT('',(0.00836215879816735,-0.0350221583435275,0.0798964164132232));
#66047=CARTESIAN_POINT('Origin',(0.00703135310806099,-0.0345628458714274,
0.0631648023821488));
#66048=CARTESIAN_POINT('',(0.00836210451100454,-0.035195136029876,0.0798951807167968));
#66049=CARTESIAN_POINT('Origin',(0.00881881006648593,-0.035195183836695,
0.0909046886051022));
#66050=CARTESIAN_POINT('',(0.00848699507357902,-0.0351951371328746,0.0798898781697402));
#66051=CARTESIAN_POINT('Ctrl Pts',(0.00859655477161187,-0.0346945769586965,
0.0798819271053914));
#66052=CARTESIAN_POINT('Ctrl Pts',(0.00871661227977268,-0.0345275153362944,
0.0798720246944468));
#66053=CARTESIAN_POINT('Ctrl Pts',(0.00883638941924486,-0.0343603235965185,
0.0798583440241053));
#66054=CARTESIAN_POINT('Ctrl Pts',(0.00895553254378017,-0.034193496108874,
0.0798409308207588));
#66055=CARTESIAN_POINT('Ctrl Pts',(0.00867993261225376,-0.0346945769586965,
0.0798731999053233));
#66056=CARTESIAN_POINT('Ctrl Pts',(0.00879980732571497,-0.0345275153362944,
0.0798615511121238));
#66057=CARTESIAN_POINT('Ctrl Pts',(0.00891934670109299,-0.0343603235965185,
0.0798461293565485));
#66058=CARTESIAN_POINT('Ctrl Pts',(0.00903819787187309,-0.034193496108874,
0.0798269855038953));
#66059=CARTESIAN_POINT('Ctrl Pts',(0.00876331045289566,-0.0346945769586965,
0.0798644727052552));
#66060=CARTESIAN_POINT('Ctrl Pts',(0.00888300237165726,-0.0345275153362944,
0.0798510775298008));
#66061=CARTESIAN_POINT('Ctrl Pts',(0.00900230398294112,-0.0343603235965185,
0.0798339146889917));
#66062=CARTESIAN_POINT('Ctrl Pts',(0.00912086319996601,-0.034193496108874,
0.0798130401870318));
#66063=CARTESIAN_POINT('Ctrl Pts',(0.00884668829353756,-0.0346945769586965,
0.0798557455051871));
#66064=CARTESIAN_POINT('Ctrl Pts',(0.00896619741759955,-0.0345275153362944,
0.0798406039474778));
#66065=CARTESIAN_POINT('Ctrl Pts',(0.00908526126478925,-0.0343603235965185,
0.0798217000214349));
#66066=CARTESIAN_POINT('Ctrl Pts',(0.00920352852805893,-0.034193496108874,
0.0797990948701682));
#66067=CARTESIAN_POINT('',(0.00872250888843107,-0.034521194296262,0.0798701093821982));
#66068=CARTESIAN_POINT('',(0.00895701165478282,-0.034193496108874,0.0798406813005297));
#66069=CARTESIAN_POINT('Origin',(0.00703048902793496,-0.0345625596120563,
0.0631527265340316));
#66070=CARTESIAN_POINT('Origin',(0.00987410394469407,-0.0346945685853843,
0.090872213061757));
#66071=CARTESIAN_POINT('',(0.00884668829354895,-0.0346945769586965,0.0798557455051857));
#66072=CARTESIAN_POINT('',(0.00878452787802969,-0.0346945769587025,0.0798622518668198));
#66073=CARTESIAN_POINT('',(0.00908049607825518,-0.0343667727833008,0.0798212276927166));
#66074=CARTESIAN_POINT('Origin',(0.00655194445142138,-0.0345626461565819,
0.0631994734902468));
#66075=CARTESIAN_POINT('',(0.00908027009142088,-0.034193496108874,0.079819888085349));
#66076=CARTESIAN_POINT('Origin',(0.010918983977091,-0.034193477102776,0.090719421010809));
#66077=CARTESIAN_POINT('',(0.00901864087311185,-0.034193496108884,0.0798302846929494));
#66078=CARTESIAN_POINT('Ctrl Pts',(0.00813729593822262,-0.0350241211494342,
0.0801499847815393));
#66079=CARTESIAN_POINT('Ctrl Pts',(0.00821994326849878,-0.0349144232818961,
0.0801497986352412));
#66080=CARTESIAN_POINT('Ctrl Pts',(0.00830263621940882,-0.0348045283579412,
0.0801479039981522));
#66081=CARTESIAN_POINT('Ctrl Pts',(0.00838526878148375,-0.0346945769439157,
0.0801442993555636));
#66082=CARTESIAN_POINT('Ctrl Pts',(0.00821222509612046,-0.0350241211494342,
0.0800649744109982));
#66083=CARTESIAN_POINT('Ctrl Pts',(0.00829370144339803,-0.0349144232818961,
0.0800637561462722));
#66084=CARTESIAN_POINT('Ctrl Pts',(0.00837520137579429,-0.0348045283579412,
0.080060852978038));
#66085=CARTESIAN_POINT('Ctrl Pts',(0.00845662036387449,-0.0346945769439157,
0.0800562647402515));
#66086=CARTESIAN_POINT('Ctrl Pts',(0.0082871542540183,-0.0350241211494342,
0.0799799640404571));
#66087=CARTESIAN_POINT('Ctrl Pts',(0.00836745961829727,-0.0349144232818961,
0.0799777136573032));
#66088=CARTESIAN_POINT('Ctrl Pts',(0.00844776653217976,-0.0348045283579412,
0.0799738019579238));
#66089=CARTESIAN_POINT('Ctrl Pts',(0.00852797194626523,-0.0346945769439157,
0.0799682301249394));
#66090=CARTESIAN_POINT('Ctrl Pts',(0.00836208341191614,-0.0350241211494342,
0.079894953669916));
#66091=CARTESIAN_POINT('Ctrl Pts',(0.00844121779319652,-0.0349144232818961,
0.0798916711683342));
#66092=CARTESIAN_POINT('Ctrl Pts',(0.00852033168856522,-0.0348045283579412,
0.0798867509378095));
#66093=CARTESIAN_POINT('Ctrl Pts',(0.00859932352865597,-0.0346945769439157,
0.0798801955096272));
#66094=CARTESIAN_POINT('',(0.00849165769165981,-0.0346945769458128,0.0800130351546404));
#66095=CARTESIAN_POINT('Ctrl Pts',(0.00837246424284203,-0.0347116136492819,
0.080144844216319));
#66096=CARTESIAN_POINT('Ctrl Pts',(0.00837068446168699,-0.0347621546532086,
0.0801019399907227));
#66097=CARTESIAN_POINT('Ctrl Pts',(0.00836893597389417,-0.0348133084096554,
0.0800597901373518));
#66098=CARTESIAN_POINT('Ctrl Pts',(0.00836550012579731,-0.0349168561544585,
0.0799769639980557));
#66099=CARTESIAN_POINT('Ctrl Pts',(0.00836381412832226,-0.0349692089015929,
0.0799363205651147));
#66100=CARTESIAN_POINT('Ctrl Pts',(0.00836215879818583,-0.0350221583435,
0.0798964164131859));
#66101=CARTESIAN_POINT('Ctrl Pts',(0.00851401047485387,-0.0345231616327841,
0.0801372967095463));
#66102=CARTESIAN_POINT('Ctrl Pts',(0.00859653693055541,-0.0344132092796988,
0.0801319179620799));
#66103=CARTESIAN_POINT('Ctrl Pts',(0.00867894787312256,-0.034303273855898,
0.0801248324974919));
#66104=CARTESIAN_POINT('Ctrl Pts',(0.00876113795713209,-0.034193496108874,
0.0801160520974999));
#66105=CARTESIAN_POINT('Ctrl Pts',(0.00858345393086496,-0.0345231616327841,
0.0800477492776698));
#66106=CARTESIAN_POINT('Ctrl Pts',(0.00866474610129079,-0.0344132092796988,
0.0800414133499308));
#66107=CARTESIAN_POINT('Ctrl Pts',(0.00874590302374674,-0.034303273855898,
0.0800333962846738));
#66108=CARTESIAN_POINT('Ctrl Pts',(0.00882682098992594,-0.034193496108874,
0.080023711015952));
#66109=CARTESIAN_POINT('Ctrl Pts',(0.00865289738687605,-0.0345231616327841,
0.0799582018457932));
#66110=CARTESIAN_POINT('Ctrl Pts',(0.00873295527202617,-0.0344132092796988,
0.0799509087377818));
#66111=CARTESIAN_POINT('Ctrl Pts',(0.00881285817437092,-0.034303273855898,
0.0799419600718556));
#66112=CARTESIAN_POINT('Ctrl Pts',(0.00889250402271978,-0.034193496108874,
0.0799313699344041));
#66113=CARTESIAN_POINT('Ctrl Pts',(0.00872234084288715,-0.0345231616327841,
0.0798686544139167));
#66114=CARTESIAN_POINT('Ctrl Pts',(0.00880116444276154,-0.0344132092796988,
0.0798604041256328));
#66115=CARTESIAN_POINT('Ctrl Pts',(0.00887981332499511,-0.034303273855898,
0.0798505238590375));
#66116=CARTESIAN_POINT('Ctrl Pts',(0.00895818705551363,-0.034193496108874,
0.0798390288528561));
#66117=CARTESIAN_POINT('Ctrl Pts',(0.00874839290846746,-0.0342105180195409,
0.0801173998855935));
#66118=CARTESIAN_POINT('Ctrl Pts',(0.00874391938062411,-0.0342610556241027,
0.0800746607380183));
#66119=CARTESIAN_POINT('Ctrl Pts',(0.00873952612792476,-0.0343122189869566,
0.0800326885223474));
#66120=CARTESIAN_POINT('Ctrl Pts',(0.00873089632176624,-0.03441581196951,
0.0799502411627092));
#66121=CARTESIAN_POINT('Ctrl Pts',(0.00872666329796788,-0.0344681990449968,
0.0799097997403819));
#66122=CARTESIAN_POINT('Ctrl Pts',(0.00872250888842384,-0.0345211942962374,
0.0798701093821663));
#66123=CARTESIAN_POINT('',(0.00885907480596801,-0.0341934961088839,0.079978366699024));
#66124=CARTESIAN_POINT('Ctrl Pts',(0.00848591858107241,-0.0351951371254931,
0.079888887426213));
#66125=CARTESIAN_POINT('Ctrl Pts',(0.00856495229917834,-0.0350856248738967,
0.0798839002251971));
#66126=CARTESIAN_POINT('Ctrl Pts',(0.00864394783125726,-0.0349758427086611,
0.0798772756007074));
#66127=CARTESIAN_POINT('Ctrl Pts',(0.00872280354676591,-0.0348659306906667,
0.079869016093009));
#66128=CARTESIAN_POINT('Ctrl Pts',(0.00854641813340751,-0.0351951371254931,
0.0799445675377254));
#66129=CARTESIAN_POINT('Ctrl Pts',(0.00862621865628073,-0.0350856248738967,
0.0799387471604839));
#66130=CARTESIAN_POINT('Ctrl Pts',(0.00870596440399965,-0.0349758427086611,
0.0799312728288274));
#66131=CARTESIAN_POINT('Ctrl Pts',(0.00878555272167216,-0.0348659306906667,
0.0799221481144213));
#66132=CARTESIAN_POINT('Ctrl Pts',(0.00860691768574261,-0.0351951371254931,
0.0800002476492377));
#66133=CARTESIAN_POINT('Ctrl Pts',(0.00868748501338313,-0.0350856248738967,
0.0799935940957707));
#66134=CARTESIAN_POINT('Ctrl Pts',(0.00876798097674204,-0.0349758427086611,
0.0799852700569474));
#66135=CARTESIAN_POINT('Ctrl Pts',(0.00884830189657841,-0.0348659306906667,
0.0799752801358336));
#66136=CARTESIAN_POINT('Ctrl Pts',(0.00866741723807771,-0.0351951371254931,
0.0800559277607501));
#66137=CARTESIAN_POINT('Ctrl Pts',(0.00874875137048552,-0.0350856248738967,
0.0800484410310575));
#66138=CARTESIAN_POINT('Ctrl Pts',(0.00882999754948443,-0.0349758427086611,
0.0800392672850673));
#66139=CARTESIAN_POINT('Ctrl Pts',(0.00891105107148466,-0.0348659306906667,
0.0800284121572459));
#66140=CARTESIAN_POINT('Origin',(0.00927614291461343,-0.030860918850898,
0.0851593964693888));
#66141=CARTESIAN_POINT('',(0.00856565507232487,-0.0351951371254931,0.0799622720473082));
#66142=CARTESIAN_POINT('Ctrl Pts',(0.00884511306056555,-0.0346945769586931,
0.0798544687873255));
#66143=CARTESIAN_POINT('Ctrl Pts',(0.00892372352378627,-0.0345846629175835,
0.0798445284833742));
#66144=CARTESIAN_POINT('Ctrl Pts',(0.00900214185246384,-0.034474692504983,
0.0798329608494984));
#66145=CARTESIAN_POINT('Ctrl Pts',(0.00908026762921077,-0.0343648066252516,
0.0798197811224456));
#66146=CARTESIAN_POINT('Ctrl Pts',(0.00893314760635036,-0.0346945769586931,
0.0799258203136349));
#66147=CARTESIAN_POINT('Ctrl Pts',(0.00901274132966835,-0.0345846629175835,
0.0799146668491456));
#66148=CARTESIAN_POINT('Ctrl Pts',(0.00909211799872473,-0.034474692504983,
0.0799018655141058));
#66149=CARTESIAN_POINT('Ctrl Pts',(0.00917117597472416,-0.0343648066252516,
0.0798874331310947));
#66150=CARTESIAN_POINT('Ctrl Pts',(0.00902118215213519,-0.0346945769586931,
0.0799971718399444));
#66151=CARTESIAN_POINT('Ctrl Pts',(0.00910175913555044,-0.0345846629175835,
0.079984805214917));
#66152=CARTESIAN_POINT('Ctrl Pts',(0.00918209414498561,-0.034474692504983,
0.0799707701787133));
#66153=CARTESIAN_POINT('Ctrl Pts',(0.00926208432023754,-0.0343648066252516,
0.0799550851397438));
#66154=CARTESIAN_POINT('Ctrl Pts',(0.00910921669792,-0.0346945769586931,
0.0800685233662539));
#66155=CARTESIAN_POINT('Ctrl Pts',(0.00919077694143253,-0.0345846629175835,
0.0800549435806884));
#66156=CARTESIAN_POINT('Ctrl Pts',(0.00927207029124649,-0.034474692504983,
0.0800396748433208));
#66157=CARTESIAN_POINT('Ctrl Pts',(0.00935299266575093,-0.0343648066252516,
0.0800227371483928));
#66158=CARTESIAN_POINT('',(0.009109216697909,-0.0346945769586885,0.0800685233662417));
#66159=CARTESIAN_POINT('',(0.00897795249573898,-0.0346945769587025,0.0799621344357236));
#66160=CARTESIAN_POINT('',(0.00912185652151936,-0.0346775396663496,0.0800664049570397));
#66161=CARTESIAN_POINT('Origin',(0.00620977999082163,-0.0345626617704269,
0.0637222098416));
#66162=CARTESIAN_POINT('Ctrl Pts',(0.00912185652095255,-0.0346775396659521,
0.0800664049537068));
#66163=CARTESIAN_POINT('Ctrl Pts',(0.00911471058875113,-0.03462697485299,
0.0800240451539444));
#66164=CARTESIAN_POINT('Ctrl Pts',(0.00910769171401761,-0.0345757904818634,
0.0799824385279803));
#66165=CARTESIAN_POINT('Ctrl Pts',(0.0090939020602039,-0.0344721679344743,
0.0799006959424259));
#66166=CARTESIAN_POINT('Ctrl Pts',(0.00908713683786502,-0.0344197716860438,
0.079860592922198));
#66167=CARTESIAN_POINT('Ctrl Pts',(0.0090804960779661,-0.0343667727831938,
0.0798212276929094));
#66168=CARTESIAN_POINT('Origin',(0.00812378219310841,-0.0315241814719618,
0.07415));
#66169=CARTESIAN_POINT('',(0.00912185652150067,-0.0347116136489619,0.0800664049569289));
#66170=CARTESIAN_POINT('Origin',(0.00655591106685294,-0.0345626706845752,
0.0636657179185765));
#66171=CARTESIAN_POINT('',(0.00913449179186378,-0.0346945769586886,0.0800642595569509));
#66172=CARTESIAN_POINT('Origin',(0.00616545050053386,-0.0345626706260411,
0.0637315869851469));
#66173=CARTESIAN_POINT('Origin',(0.00651095856197596,-0.0345626618561295,
0.0636714021604937));
#66174=CARTESIAN_POINT('Origin',(0.00788233303269208,-0.0351840467447537,
0.0732031905879628));
#66175=CARTESIAN_POINT('',(0.00908028734499586,-0.035195136029876,0.0798200085441095));
#66176=CARTESIAN_POINT('Origin',(0.0101570089533248,-0.0352322613584381,
0.0859412120342698));
#66177=CARTESIAN_POINT('',(0.00895731903566345,-0.0351951142564677,0.0798406090109526));
#66178=CARTESIAN_POINT('',(0.00908027014552778,-0.0351951372916786,0.0798198880762214));
#66179=CARTESIAN_POINT('Origin',(0.00838011388044975,-0.0352875103405805,
0.0739259169494507));
#66180=CARTESIAN_POINT('Ctrl Pts',(0.00891880951702706,-0.0352450361874076,
0.079846199417526));
#66181=CARTESIAN_POINT('Ctrl Pts',(0.00913364520334914,-0.0349452760959497,
0.0798162144699741));
#66182=CARTESIAN_POINT('Ctrl Pts',(0.00934561197516326,-0.0346444289841739,
0.0797701324035723));
#66183=CARTESIAN_POINT('Ctrl Pts',(0.00892127724740515,-0.0352450361874076,
0.0798457990342332));
#66184=CARTESIAN_POINT('Ctrl Pts',(0.00913609783302355,-0.0349452760959497,
0.079815721014703));
#66185=CARTESIAN_POINT('Ctrl Pts',(0.00934804253647126,-0.0346444289841739,
0.0797695472781772));
#66186=CARTESIAN_POINT('Ctrl Pts',(0.00916805028897418,-0.0352450361874076,
0.0798057607043536));
#66187=CARTESIAN_POINT('Ctrl Pts',(0.00938136080420208,-0.0349452760959497,
0.0797663754868366));
#66188=CARTESIAN_POINT('Ctrl Pts',(0.00959109867097598,-0.0346444289841739,
0.0797110347377743));
#66189=CARTESIAN_POINT('',(0.00908049607791315,-0.0350221583435275,0.0798212276927154));
#66190=CARTESIAN_POINT('',(0.00931268828447517,-0.0346945769330289,0.079777133133678));
#66191=CARTESIAN_POINT('Origin',(0.005663156899118,-0.0345628458716139,
0.0633883416159371));
#66192=CARTESIAN_POINT('Origin',(0.0109132497041071,-0.0351951838366848,
0.0906854626481361));
#66193=CARTESIAN_POINT('',(0.00920349695358097,-0.0351951633467166,0.0797991030395162));
#66194=CARTESIAN_POINT('',(0.00920352852280879,-0.0351951371328746,0.0797990948711718));
#66195=CARTESIAN_POINT('',(0.00943470755481608,-0.0348678972925388,0.0797499642584603));
#66196=CARTESIAN_POINT('Origin',(0.00520542918551106,-0.0345631633303276,
0.0635375133050744));
#66197=CARTESIAN_POINT('',(0.00943439789959453,-0.0346945769586885,0.0797486414843168));
#66198=CARTESIAN_POINT('Origin',(0.0119533318496204,-0.0346946199340818,
0.0905089382316885));
#66199=CARTESIAN_POINT('',(0.00937354309177105,-0.0346945769458128,0.0797628873091441));
#66200=CARTESIAN_POINT('Origin',(0.000623215658025582,-0.0298325076523077,
0.0739584486183963));
#66201=CARTESIAN_POINT('Origin',(0.00630463286954172,-0.033873312329463,
0.082331557296228));
#66202=CARTESIAN_POINT('Ctrl Pts',(0.00888918687231204,-0.0350241211494342,
0.0801009793880569));
#66203=CARTESIAN_POINT('Ctrl Pts',(0.00897115917338596,-0.0349144232818962,
0.080090436252429));
#66204=CARTESIAN_POINT('Ctrl Pts',(0.00905296260468609,-0.0348045283579412,
0.0800781923801888));
#66205=CARTESIAN_POINT('Ctrl Pts',(0.00913449180281645,-0.0346945769439158,
0.0800642595550811));
#66206=CARTESIAN_POINT('Ctrl Pts',(0.0089528705667935,-0.0350241211494342,
0.0800072482360308));
#66207=CARTESIAN_POINT('Ctrl Pts',(0.00903355175967953,-0.0349144232818962,
0.0799958278836228));
#66208=CARTESIAN_POINT('Ctrl Pts',(0.00911404517730361,-0.0348045283579412,
0.0799827329576747));
#66209=CARTESIAN_POINT('Ctrl Pts',(0.00919424709366599,-0.0346945769439158,
0.079967976394464));
#66210=CARTESIAN_POINT('Ctrl Pts',(0.00901655426127497,-0.0350241211494342,
0.0799135170840048));
#66211=CARTESIAN_POINT('Ctrl Pts',(0.0090959443459731,-0.0349144232818962,
0.0799012195148165));
#66212=CARTESIAN_POINT('Ctrl Pts',(0.00917512774992114,-0.0348045283579412,
0.0798872735351606));
#66213=CARTESIAN_POINT('Ctrl Pts',(0.00925400238451553,-0.0346945769439158,
0.0798716932338468));
#66214=CARTESIAN_POINT('Ctrl Pts',(0.00908023795575643,-0.0350241211494342,
0.0798197859319787));
#66215=CARTESIAN_POINT('Ctrl Pts',(0.00915833693226667,-0.0349144232818962,
0.0798066111460103));
#66216=CARTESIAN_POINT('Ctrl Pts',(0.00923621032253866,-0.0348045283579412,
0.0797918141126465));
#66217=CARTESIAN_POINT('Ctrl Pts',(0.00931375767536507,-0.0346945769439158,
0.0797754100732296));
#66218=CARTESIAN_POINT('Ctrl Pts',(0.00912185652094782,-0.0347116136492809,
0.0800664049536785));
#66219=CARTESIAN_POINT('Ctrl Pts',(0.00911471344857282,-0.0347621546531963,
0.0800240621064524));
#66220=CARTESIAN_POINT('Ctrl Pts',(0.00910769597071279,-0.0348133084096308,
0.0799824637609031));
#66221=CARTESIAN_POINT('Ctrl Pts',(0.00909390634743964,-0.0349168561544574,
0.0799007213563877));
#66222=CARTESIAN_POINT('Ctrl Pts',(0.00908713967168468,-0.0349692089015915,
0.0798606097205706));
#66223=CARTESIAN_POINT('Ctrl Pts',(0.00908049607792671,-0.0350221583435,
0.0798212276926761));
#66224=CARTESIAN_POINT('',(0.00922359003790568,-0.0346945769458128,0.0799206963454612));
#66225=CARTESIAN_POINT('Ctrl Pts',(0.00920233634567586,-0.0351951371254938,
0.0797982468602394));
#66226=CARTESIAN_POINT('Ctrl Pts',(0.00928012179748727,-0.0350856248736035,
0.0797833934333025));
#66227=CARTESIAN_POINT('Ctrl Pts',(0.00935766414079992,-0.0349758427080725,
0.0797669202804344));
#66228=CARTESIAN_POINT('Ctrl Pts',(0.00943486286483655,-0.0348659306897825,
0.0797488426595543));
#66229=CARTESIAN_POINT('Ctrl Pts',(0.00926933740939195,-0.0351951371254938,
0.0798459053129186));
#66230=CARTESIAN_POINT('Ctrl Pts',(0.00934777919481731,-0.0350856248736035,
0.079830129173476));
#66231=CARTESIAN_POINT('Ctrl Pts',(0.00942595934155043,-0.0349758427080725,
0.0798127189866814));
#66232=CARTESIAN_POINT('Ctrl Pts',(0.00950377645181123,-0.0348659306897825,
0.0797936911621062));
#66233=CARTESIAN_POINT('Ctrl Pts',(0.00933633847310804,-0.0351951371254938,
0.0798935637655978));
#66234=CARTESIAN_POINT('Ctrl Pts',(0.00941543659214735,-0.0350856248736035,
0.0798768649136495));
#66235=CARTESIAN_POINT('Ctrl Pts',(0.00949425454230094,-0.0349758427080725,
0.0798585176929283));
#66236=CARTESIAN_POINT('Ctrl Pts',(0.00957269003878591,-0.0348659306897825,
0.0798385396646581));
#66237=CARTESIAN_POINT('Ctrl Pts',(0.00940333953682413,-0.0351951371254938,
0.079941222218277));
#66238=CARTESIAN_POINT('Ctrl Pts',(0.0094830939894774,-0.0350856248736035,
0.079923600653823));
#66239=CARTESIAN_POINT('Ctrl Pts',(0.00956254974305145,-0.0349758427080725,
0.0799043163991753));
#66240=CARTESIAN_POINT('Ctrl Pts',(0.00964160362576058,-0.0348659306897825,
0.07988338816721));
#66241=CARTESIAN_POINT('',(0.0092906416227406,-0.0351951371254938,0.079861059189401));
#66242=CARTESIAN_POINT('Origin',(0.0106468975549029,-0.0308609197410635,
0.0849281543167568));
#66243=CARTESIAN_POINT('Ctrl Pts',(0.00545294195983083,-0.0321934096636941,
0.0792435987468211));
#66244=CARTESIAN_POINT('Ctrl Pts',(0.00554411495180879,-0.0320508460844048,
0.079291405515133));
#66245=CARTESIAN_POINT('Ctrl Pts',(0.00563650367258421,-0.0319086045662519,
0.0793367265985879));
#66246=CARTESIAN_POINT('Ctrl Pts',(0.00572990115924722,-0.0317669892867074,
0.0793794807900028));
#66247=CARTESIAN_POINT('Ctrl Pts',(0.00552802930713434,-0.0321934096636941,
0.0792809125901338));
#66248=CARTESIAN_POINT('Ctrl Pts',(0.0056198701991386,-0.0320508460844048,
0.0793273753306858));
#66249=CARTESIAN_POINT('Ctrl Pts',(0.00571289020496758,-0.0319086045662519,
0.0793713354546265));
#66250=CARTESIAN_POINT('Ctrl Pts',(0.00580688124369109,-0.0317669892867074,
0.0794127147970611));
#66251=CARTESIAN_POINT('Ctrl Pts',(0.00560311665443784,-0.0321934096636941,
0.0793182264334465));
#66252=CARTESIAN_POINT('Ctrl Pts',(0.00569562544646842,-0.0320508460844048,
0.0793633451462386));
#66253=CARTESIAN_POINT('Ctrl Pts',(0.00578927673735094,-0.0319086045662519,
0.0794059443106649));
#66254=CARTESIAN_POINT('Ctrl Pts',(0.00588386132813497,-0.0317669892867074,
0.0794459488041194));
#66255=CARTESIAN_POINT('Ctrl Pts',(0.00567820400174134,-0.0321934096636941,
0.0793555402767591));
#66256=CARTESIAN_POINT('Ctrl Pts',(0.00577138069379823,-0.0320508460844048,
0.0793993149617914));
#66257=CARTESIAN_POINT('Ctrl Pts',(0.00586566326973432,-0.0319086045662518,
0.0794405531667035));
#66258=CARTESIAN_POINT('Ctrl Pts',(0.00596084141257884,-0.0317669892867074,
0.0794791828111777));
#66259=CARTESIAN_POINT('',(0.00567686067426102,-0.0321934096636941,0.0793548727247266));
#66260=CARTESIAN_POINT('',(0.00589276668497216,-0.0318665617511328,0.0794510088465921));
#66261=CARTESIAN_POINT('Origin',(0.0133377615190161,-0.0326371944419888,
0.064504670602517));
#66262=CARTESIAN_POINT('Origin',(0.00164080164324394,-0.0316939261509349,
0.089553898701131));
#66263=CARTESIAN_POINT('',(0.00556457329482249,-0.0320197221621744,0.0793005377371172));
#66264=CARTESIAN_POINT('Ctrl Pts',(0.00556471247059017,-0.0320197392094667,
0.0793006595771184));
#66265=CARTESIAN_POINT('Ctrl Pts',(0.00559092070329904,-0.0319792716575964,
0.0793136809045492));
#66266=CARTESIAN_POINT('Ctrl Pts',(0.00561734751521862,-0.0319386439829625,
0.0793265617090013));
#66267=CARTESIAN_POINT('Ctrl Pts',(0.0056440243550796,-0.0318979099381557,
0.0793393079103611));
#66268=CARTESIAN_POINT('Ctrl Pts',(0.00567070066765265,-0.0318571766984881,
0.0793520538597826));
#66269=CARTESIAN_POINT('Ctrl Pts',(0.00569749064372408,-0.0318163871833553,
0.079364602035801));
#66270=CARTESIAN_POINT('Ctrl Pts',(0.00572430064325569,-0.0317755399638303,
0.0793769124665612));
#66271=CARTESIAN_POINT('',(0.0055649205590403,-0.0321934096636183,0.0792992452978757));
#66272=CARTESIAN_POINT('Origin',(0.004556373628744,-0.0324113149036198,
0.0813760325455046));
#66273=CARTESIAN_POINT('',(0.00562089061666066,-0.0321934096636663,0.0793270590113111));
#66274=CARTESIAN_POINT('Ctrl Pts',(0.00567621457844038,-0.0321934096636618,
0.0793529501619655));
#66275=CARTESIAN_POINT('Ctrl Pts',(0.00574796731611607,-0.0320835708272592,
0.0793867040268945));
#66276=CARTESIAN_POINT('Ctrl Pts',(0.00582037696876832,-0.0319739230346488,
0.0794189533940329));
#66277=CARTESIAN_POINT('Ctrl Pts',(0.00589334772661693,-0.0318646057455573,
0.0794496641126543));
#66278=CARTESIAN_POINT('Ctrl Pts',(0.00571231260492629,-0.0321934096636618,
0.0794603656973853));
#66279=CARTESIAN_POINT('Ctrl Pts',(0.0057855466865502,-0.0320835708272592,
0.0794936217423959));
#66280=CARTESIAN_POINT('Ctrl Pts',(0.00585942652155362,-0.0319739230346488,
0.0795253429220357));
#66281=CARTESIAN_POINT('Ctrl Pts',(0.00593385447102425,-0.0318646057455573,
0.0795554959057187));
#66282=CARTESIAN_POINT('Ctrl Pts',(0.0057484106314122,-0.0321934096636618,
0.0795677812328052));
#66283=CARTESIAN_POINT('Ctrl Pts',(0.00582312605698432,-0.0320835708272592,
0.0796005394578972));
#66284=CARTESIAN_POINT('Ctrl Pts',(0.00589847607433893,-0.0319739230346488,
0.0796317324500384));
#66285=CARTESIAN_POINT('Ctrl Pts',(0.00597436121543156,-0.0318646057455573,
0.0796613276987831));
#66286=CARTESIAN_POINT('Ctrl Pts',(0.00578450865789812,-0.0321934096636618,
0.079675196768225));
#66287=CARTESIAN_POINT('Ctrl Pts',(0.00586070542741844,-0.0320835708272592,
0.0797074571733986));
#66288=CARTESIAN_POINT('Ctrl Pts',(0.00593752562712424,-0.0319739230346488,
0.0797381219780412));
#66289=CARTESIAN_POINT('Ctrl Pts',(0.00601486795983887,-0.0318646057455573,
0.0797671594918474));
#66290=CARTESIAN_POINT('',(0.00579631591447991,-0.0321763980308314,0.0796801808921294));
#66291=CARTESIAN_POINT('',(0.00578450865792329,-0.0321934096636184,0.079675196768223));
#66292=CARTESIAN_POINT('Origin',(0.0127763985114372,-0.0326386231203367,
0.06467669662428));
#66293=CARTESIAN_POINT('Ctrl Pts',(0.00579631591570451,-0.0321763980306366,
0.0796801808892017));
#66294=CARTESIAN_POINT('Ctrl Pts',(0.00581296462851228,-0.0321259596176305,
0.0796406226819386));
#66295=CARTESIAN_POINT('Ctrl Pts',(0.00582932488076331,-0.032074916463434,
0.079601749871939));
#66296=CARTESIAN_POINT('Ctrl Pts',(0.005861481630547,-0.0319716057793989,
0.0795253437624975));
#66297=CARTESIAN_POINT('Ctrl Pts',(0.00587726559859713,-0.0319193786690187,
0.0794878402337576));
#66298=CARTESIAN_POINT('Ctrl Pts',(0.00589276668568432,-0.0318665617525382,
0.0794510088448763));
#66299=CARTESIAN_POINT('',(0.00573068466610216,-0.0321934096636663,0.0795150347464848));
#66300=CARTESIAN_POINT('Origin',(0.00812378219310841,-0.0315241814719618,
0.07415));
#66301=CARTESIAN_POINT('',(0.0057963159143359,-0.0322104233323592,0.0796801808924703));
#66302=CARTESIAN_POINT('',(0.00580813378883182,-0.0321934096636183,0.0796851397875583));
#66303=CARTESIAN_POINT('Origin',(0.0127374721225919,-0.0326387223296586,
0.0646534565409408));
#66304=CARTESIAN_POINT('Origin',(0.0116454707300995,-0.0326386250315982,
0.0642007234862707));
#66305=CARTESIAN_POINT('Origin',(0.0116892981152757,-0.0326387238142873,
0.0642123200058464));
#66306=CARTESIAN_POINT('Ctrl Pts',(0.00574512659303898,-0.0327445246967097,
0.0793864226850263));
#66307=CARTESIAN_POINT('Ctrl Pts',(0.00594262150320909,-0.032443687833936,
0.079476135147583));
#66308=CARTESIAN_POINT('Ctrl Pts',(0.00614631286053686,-0.0321434074405928,
0.0795507166227029));
#66309=CARTESIAN_POINT('Ctrl Pts',(0.00597493679531699,-0.0327445246967097,
0.0794848466197624));
#66310=CARTESIAN_POINT('Ctrl Pts',(0.00617614382487061,-0.032443687833936,
0.0795658916488468));
#66311=CARTESIAN_POINT('Ctrl Pts',(0.00638288388932941,-0.0321434074405928,
0.0796315507017539));
#66312=CARTESIAN_POINT('',(0.00600850577735225,-0.0326943950436612,0.0794982455707406));
#66313=CARTESIAN_POINT('',(0.00623002218363936,-0.0323666188837389,0.0795806351402517));
#66314=CARTESIAN_POINT('Origin',(0.0121206135023099,-0.0326395579113119,
0.0638377795047609));
#66315=CARTESIAN_POINT('Origin',(0.00259334537534946,-0.0321933825603034,
0.0900093432880409));
#66316=CARTESIAN_POINT('',(0.00611244010570222,-0.032193409653269,0.0795381933896475));
#66317=CARTESIAN_POINT('',(0.00617145480780626,-0.0321934096584275,0.0795587728765589));
#66318=CARTESIAN_POINT('',(0.00589276668459501,-0.0325210109756239,0.0794510088474529));
#66319=CARTESIAN_POINT('Origin',(0.0125577735393507,-0.0326393129161412,
0.0640379682458832));
#66320=CARTESIAN_POINT('',(0.00589329367539631,-0.0326943950436593,0.0794497566899203));
#66321=CARTESIAN_POINT('Origin',(0.00160204435036457,-0.0326943765538151,
0.0896459861852913));
#66322=CARTESIAN_POINT('',(0.00595089972638428,-0.0326943950436702,0.0794740011303405));
#66323=CARTESIAN_POINT('Ctrl Pts',(0.00558133952140229,-0.0325229783203769,
0.079584701947773));
#66324=CARTESIAN_POINT('Ctrl Pts',(0.00565625676890326,-0.032413025309245,
0.079619749464403));
#66325=CARTESIAN_POINT('Ctrl Pts',(0.00573188765663896,-0.032303122220807,
0.0796532419058877));
#66326=CARTESIAN_POINT('Ctrl Pts',(0.00580813379296862,-0.0321934096576658,
0.079685139789289));
#66327=CARTESIAN_POINT('Ctrl Pts',(0.00568533311590499,-0.0325229783203769,
0.0795396855669895));
#66328=CARTESIAN_POINT('Ctrl Pts',(0.0057596298135813,-0.032413025309245,
0.0795732995341935));
#66329=CARTESIAN_POINT('Ctrl Pts',(0.00583461059079949,-0.032303122220807,
0.0796053714805483));
#66330=CARTESIAN_POINT('Ctrl Pts',(0.00591017795287016,-0.0321934096576658,
0.0796358637132843));
#66331=CARTESIAN_POINT('Ctrl Pts',(0.00578932671040769,-0.0325229783203769,
0.079494669186206));
#66332=CARTESIAN_POINT('Ctrl Pts',(0.00586300285825935,-0.032413025309245,
0.079526849603984));
#66333=CARTESIAN_POINT('Ctrl Pts',(0.00593733352496002,-0.032303122220807,
0.0795575010552089));
#66334=CARTESIAN_POINT('Ctrl Pts',(0.00601222211277171,-0.0321934096576658,
0.0795865876372795));
#66335=CARTESIAN_POINT('Ctrl Pts',(0.0058933203049104,-0.0325229783203769,
0.0794496528054225));
#66336=CARTESIAN_POINT('Ctrl Pts',(0.00596637590293739,-0.032413025309245,
0.0794803996737744));
#66337=CARTESIAN_POINT('Ctrl Pts',(0.00604005645912054,-0.032303122220807,
0.0795096306298695));
#66338=CARTESIAN_POINT('Ctrl Pts',(0.00611426627267325,-0.0321934096576658,
0.0795373115612748));
#66339=CARTESIAN_POINT('',(0.00596028694676296,-0.0321934096584275,0.079611666588569));
#66340=CARTESIAN_POINT('Ctrl Pts',(0.00579631591568124,-0.0322104233328918,
0.0796801808892569));
#66341=CARTESIAN_POINT('Ctrl Pts',(0.00581298718780795,-0.0322609421831307,
0.0796405690798791));
#66342=CARTESIAN_POINT('Ctrl Pts',(0.00582935846068635,-0.0323120888240607,
0.0796016700843133));
#66343=CARTESIAN_POINT('Ctrl Pts',(0.00586151545385223,-0.0324156524631807,
0.0795252633965831));
#66344=CARTESIAN_POINT('Ctrl Pts',(0.00587728795592471,-0.0324680267167312,
0.0794877871115846));
#66345=CARTESIAN_POINT('Ctrl Pts',(0.00589276668461587,-0.0325210109755912,
0.0794510088474146));
#66346=CARTESIAN_POINT('Origin',(0.00129234738506729,-0.0262834582510987,
0.0702468110083525));
#66347=CARTESIAN_POINT('Origin',(-0.00110757709133214,-0.0342770866417274,
0.0820623878212155));
#66348=CARTESIAN_POINT('Ctrl Pts',(0.00600774042359261,-0.0326943950436604,
0.0794963678262276));
#66349=CARTESIAN_POINT('Ctrl Pts',(0.00608142339239928,-0.0325844576448134,
0.0795255308476965));
#66350=CARTESIAN_POINT('Ctrl Pts',(0.00615571471496154,-0.0324744968375322,
0.079553172048478));
#66351=CARTESIAN_POINT('Ctrl Pts',(0.00623051871641797,-0.0323646534831894,
0.0795792573259598));
#66352=CARTESIAN_POINT('Ctrl Pts',(0.00605051183421898,-0.0326943950436604,
0.0796013046358585));
#66353=CARTESIAN_POINT('Ctrl Pts',(0.00612564102893491,-0.0325844576448134,
0.0796298781871268));
#66354=CARTESIAN_POINT('Ctrl Pts',(0.00620136648854788,-0.0324744968375322,
0.079656899965667));
#66355=CARTESIAN_POINT('Ctrl Pts',(0.00627759071164313,-0.0323646534831894,
0.0796823366878515));
#66356=CARTESIAN_POINT('Ctrl Pts',(0.00609328324484535,-0.0326943950436604,
0.0797062414454894));
#66357=CARTESIAN_POINT('Ctrl Pts',(0.00616985866547053,-0.0325844576448134,
0.0797342255265571));
#66358=CARTESIAN_POINT('Ctrl Pts',(0.00624701826213421,-0.0324744968375322,
0.079760627882856));
#66359=CARTESIAN_POINT('Ctrl Pts',(0.00632466270686829,-0.0323646534831894,
0.0797854160497432));
#66360=CARTESIAN_POINT('Ctrl Pts',(0.00613605465547172,-0.0326943950436605,
0.0798111782551203));
#66361=CARTESIAN_POINT('Ctrl Pts',(0.00621407630200616,-0.0325844576448134,
0.0798385728659873));
#66362=CARTESIAN_POINT('Ctrl Pts',(0.00629267003572055,-0.0324744968375322,
0.079864355800045));
#66363=CARTESIAN_POINT('Ctrl Pts',(0.00637173470209345,-0.0323646534831894,
0.0798884954116349));
#66364=CARTESIAN_POINT('',(0.0061481515687621,-0.0326773559991203,0.0798154111604032));
#66365=CARTESIAN_POINT('',(0.00613605465546716,-0.0326943950436594,0.0798111782551076));
#66366=CARTESIAN_POINT('Origin',(0.0115683174553085,-0.0326395670534535,
0.0641197075211798));
#66367=CARTESIAN_POINT('Ctrl Pts',(0.0061481515698599,-0.0326773559987499,
0.0798154111572346));
#66368=CARTESIAN_POINT('Ctrl Pts',(0.00616229492231307,-0.0326267922587316,
0.0797748530155223));
#66369=CARTESIAN_POINT('Ctrl Pts',(0.00617618759405846,-0.0325756109582041,
0.0797350137375803));
#66370=CARTESIAN_POINT('Ctrl Pts',(0.00620348339961995,-0.032471998546238,
0.0796567390036529));
#66371=CARTESIAN_POINT('Ctrl Pts',(0.00621687558572942,-0.0324196091621781,
0.0796183349418251));
#66372=CARTESIAN_POINT('Ctrl Pts',(0.00623002218365545,-0.0323666188837756,
0.0795806351402057));
#66373=CARTESIAN_POINT('',(0.00607228021641971,-0.0326943950436703,0.0796547119129341));
#66374=CARTESIAN_POINT('Ctrl Pts',(0.00607865468745572,-0.0332451089994434,
0.0795254607696106));
#66375=CARTESIAN_POINT('Ctrl Pts',(0.00628139350736245,-0.0329451141710254,
0.0796025940154523));
#66376=CARTESIAN_POINT('Ctrl Pts',(0.00648936635907893,-0.0326442513127494,
0.0796642370171651));
#66377=CARTESIAN_POINT('Ctrl Pts',(0.00631419207329205,-0.0332451089994434,
0.07960925897886));
#66378=CARTESIAN_POINT('Ctrl Pts',(0.00652009139436912,-0.0329451141710254,
0.0796775087868542));
#66379=CARTESIAN_POINT('Ctrl Pts',(0.00673054663175123,-0.0326442513127494,
0.0797300555257605));
#66380=CARTESIAN_POINT('Ctrl Pts',(0.00631654744715042,-0.0332451089994434,
0.0796100969609525));
#66381=CARTESIAN_POINT('Ctrl Pts',(0.00652247837323919,-0.0329451141710254,
0.0796782579345683));
#66382=CARTESIAN_POINT('Ctrl Pts',(0.00673295843447796,-0.0326442513127494,
0.0797307137108465));
#66383=CARTESIAN_POINT('',(0.00634849891012766,-0.0331951640388616,0.0796205113348909));
#66384=CARTESIAN_POINT('',(0.00657475150005643,-0.0328677532355031,0.0796888292067752));
#66385=CARTESIAN_POINT('Origin',(0.0107871679007543,-0.0326402808280936,
0.0634547925117744));
#66386=CARTESIAN_POINT('Origin',(0.00359737778299924,-0.0326944278779056,
0.0903363466980259));
#66387=CARTESIAN_POINT('',(0.00645473649828102,-0.0326943950436593,0.0796538542375847));
#66388=CARTESIAN_POINT('',(0.00651492694246295,-0.0326943950436694,0.0796706875507087));
#66389=CARTESIAN_POINT('',(0.0062300221836367,-0.0330220786163545,0.0795806351402508));
#66390=CARTESIAN_POINT('Origin',(0.0112576571543798,-0.0326396682763637,
0.0635537496105579));
#66391=CARTESIAN_POINT('',(0.00623046951091848,-0.0331951640388588,0.0795793523635383));
#66392=CARTESIAN_POINT('Origin',(0.00259805675387946,-0.033195202656003,
0.0899958271549816));
#66393=CARTESIAN_POINT('',(0.00628948421053307,-0.0331951640388702,0.0795999318492247));
#66394=CARTESIAN_POINT('Ctrl Pts',(0.00634761702129453,-0.0331951640388604,
0.0796186850611225));
#66395=CARTESIAN_POINT('Ctrl Pts',(0.00646067857873859,-0.0330306422010619,
0.0796554061372785));
#66396=CARTESIAN_POINT('Ctrl Pts',(0.00657516124656832,-0.0328657861914645,
0.0796874228824649));
#66397=CARTESIAN_POINT('Ctrl Pts',(0.00634849891012466,-0.0331951640388604,
0.0796205113348899));
#66398=CARTESIAN_POINT('Ctrl Pts',(0.00646159822460796,-0.0330306422010619,
0.0796572141785598));
#66399=CARTESIAN_POINT('Ctrl Pts',(0.00657611786364599,-0.0328657861914645,
0.0796892111463014));
#66400=CARTESIAN_POINT('Ctrl Pts',(0.00649544530550182,-0.0331951640388604,
0.07992481765778));
#66401=CARTESIAN_POINT('Ctrl Pts',(0.00661483595810781,-0.033030642201062,
0.0799584824789388));
#66402=CARTESIAN_POINT('Ctrl Pts',(0.00673551599469892,-0.0328657861914645,
0.0799871839925174));
#66403=CARTESIAN_POINT('',(0.00650778413364387,-0.0331781648281935,0.0799282826400012));
#66404=CARTESIAN_POINT('',(0.00649544530549579,-0.0331951640388588,0.0799248176577655));
#66405=CARTESIAN_POINT('Origin',(0.0102677027280972,-0.0326412092317192,
0.0638394822911415));
#66406=CARTESIAN_POINT('Ctrl Pts',(0.00650778413247788,-0.033178164828644,
0.0799282826385656));
#66407=CARTESIAN_POINT('Ctrl Pts',(0.00651936086246763,-0.0331276811546791,
0.0798868879783595));
#66408=CARTESIAN_POINT('Ctrl Pts',(0.00653072851999776,-0.0330765663497815,
0.0798462407684161));
#66409=CARTESIAN_POINT('Ctrl Pts',(0.0065530556131091,-0.0329730614463311,
0.0797664063696435));
#66410=CARTESIAN_POINT('Ctrl Pts',(0.00656400603419346,-0.0329207133374058,
0.0797272514336151));
#66411=CARTESIAN_POINT('Ctrl Pts',(0.00657475148424507,-0.0328677532289387,
0.0796888292114015));
#66412=CARTESIAN_POINT('',(0.00642197210782172,-0.0331951640388701,0.0797726644963382));
#66413=CARTESIAN_POINT('Origin',(0.00812378219310841,-0.0315241814719618,
0.07415));
#66414=CARTESIAN_POINT('',(0.00614815156877667,-0.0327114338380032,0.0798154111603605));
#66415=CARTESIAN_POINT('',(0.00616025749492682,-0.0326943950436593,0.0798196182199214));
#66416=CARTESIAN_POINT('Origin',(0.011525283954854,-0.0326395656488183,
0.0641055182638404));
#66417=CARTESIAN_POINT('Origin',(0.0116631949407086,-0.0326395684957492,
0.0641527893530563));
#66418=CARTESIAN_POINT('Origin',(0.0117057178917446,-0.0326395671683965,
0.0641684423746073));
#66419=CARTESIAN_POINT('Ctrl Pts',(0.005927605104244,-0.0330240426238172,
0.0797336194528622));
#66420=CARTESIAN_POINT('Ctrl Pts',(0.00600452490206404,-0.032914277406352,
0.079763873931893));
#66421=CARTESIAN_POINT('Ctrl Pts',(0.00608210849180188,-0.0328043479726691,
0.0797925533467991));
#66422=CARTESIAN_POINT('Ctrl Pts',(0.00616025749492681,-0.0326943950436593,
0.0798196182199214));
#66423=CARTESIAN_POINT('Ctrl Pts',(0.00602856685638832,-0.0330240426238172,
0.0796821620861541));
#66424=CARTESIAN_POINT('Ctrl Pts',(0.00610477777884947,-0.032914277406352,
0.0797110257186868));
#66425=CARTESIAN_POINT('Ctrl Pts',(0.00618162338714594,-0.0328043479726691,
0.079738328248141));
#66426=CARTESIAN_POINT('Ctrl Pts',(0.00625900619957894,-0.0326943950436593,
0.0797640319867867));
#66427=CARTESIAN_POINT('Ctrl Pts',(0.00612952860853264,-0.0330240426238172,
0.079630704719446));
#66428=CARTESIAN_POINT('Ctrl Pts',(0.00620503065563489,-0.0329142774063519,
0.0796581775054807));
#66429=CARTESIAN_POINT('Ctrl Pts',(0.00628113828249001,-0.0328043479726691,
0.0796841031494829));
#66430=CARTESIAN_POINT('Ctrl Pts',(0.00635775490423107,-0.0326943950436593,
0.0797084457536519));
#66431=CARTESIAN_POINT('Ctrl Pts',(0.00623049036067695,-0.0330240426238172,
0.079579247352738));
#66432=CARTESIAN_POINT('Ctrl Pts',(0.00630528353242032,-0.0329142774063519,
0.0796053292922745));
#66433=CARTESIAN_POINT('Ctrl Pts',(0.00638065317783408,-0.0328043479726691,
0.0796298780508248));
#66434=CARTESIAN_POINT('Ctrl Pts',(0.00645650360888319,-0.0326943950436593,
0.0796528595205172));
#66435=CARTESIAN_POINT('',(0.00630749699661392,-0.0326943950436693,0.0797367362287631));
#66436=CARTESIAN_POINT('Ctrl Pts',(0.00614815156986408,-0.0327114338383317,
0.0798154111572224));
#66437=CARTESIAN_POINT('Ctrl Pts',(0.00616229256985094,-0.0327619876831005,
0.079774859761553));
#66438=CARTESIAN_POINT('Ctrl Pts',(0.00617618409255887,-0.0328131562604407,
0.0797350237786449));
#66439=CARTESIAN_POINT('Ctrl Pts',(0.00620347987297984,-0.0329167375858766,
0.0796567491168115));
#66440=CARTESIAN_POINT('Ctrl Pts',(0.00621687325465107,-0.0329691088920625,
0.0796183416265345));
#66441=CARTESIAN_POINT('Ctrl Pts',(0.00623002218365494,-0.0330220786163187,
0.0795806351402068));
#66442=CARTESIAN_POINT('Origin',(0.00812378219310841,-0.0315241814719618,
0.07415));
#66443=CARTESIAN_POINT('',(0.0065077841346841,-0.0332121607144207,0.0799282826386817));
#66444=CARTESIAN_POINT('',(0.00652013033595562,-0.033195164038859,0.0799317212593731));
#66445=CARTESIAN_POINT('Origin',(0.0102225774597537,-0.0326413637773631,
0.063835002134874));
#66446=CARTESIAN_POINT('Origin',(0.0116395938759324,-0.032641210696683,
0.0642231517663572));
#66447=CARTESIAN_POINT('Origin',(0.0116804941341952,-0.032641365556836,
0.0642427376336306));
#66448=CARTESIAN_POINT('Ctrl Pts',(0.00642019835711451,-0.0337436976235975,
0.0796432619738859));
#66449=CARTESIAN_POINT('Ctrl Pts',(0.00646960558783428,-0.0336723290703325,
0.079658584265092));
#66450=CARTESIAN_POINT('Ctrl Pts',(0.00651928042535222,-0.033601104548885,
0.0796730153971601));
#66451=CARTESIAN_POINT('Ctrl Pts',(0.0066778823415161,-0.0333736987606857,
0.0797190911432073));
#66452=CARTESIAN_POINT('Ctrl Pts',(0.00683886698624801,-0.0331450831799192,
0.0797559894676301));
#66453=CARTESIAN_POINT('Ctrl Pts',(0.00666053244746381,-0.0337436976235975,
0.0797121061821823));
#66454=CARTESIAN_POINT('Ctrl Pts',(0.00671055887342662,-0.0336723290703325,
0.0797252668721563));
#66455=CARTESIAN_POINT('Ctrl Pts',(0.00676081392562346,-0.033601104548885,
0.0797375256153175));
#66456=CARTESIAN_POINT('Ctrl Pts',(0.00692126835232302,-0.0333736987606857,
0.0797766653539112));
#66457=CARTESIAN_POINT('Ctrl Pts',(0.00708370442669944,-0.0331450831799192,
0.0798065327931359));
#66458=CARTESIAN_POINT('Ctrl Pts',(0.0066629357883673,-0.0337436976235975,
0.0797127946242653));
#66459=CARTESIAN_POINT('Ctrl Pts',(0.00671296840628254,-0.0336723290703325,
0.0797259336982269));
#66460=CARTESIAN_POINT('Ctrl Pts',(0.00676322926062617,-0.033601104548885,
0.0797381707174991));
#66461=CARTESIAN_POINT('Ctrl Pts',(0.00692370221243109,-0.0333736987606857,
0.0797772410960182));
#66462=CARTESIAN_POINT('Ctrl Pts',(0.00708615280110395,-0.0331450831799192,
0.079807038226391));
#66463=CARTESIAN_POINT('',(0.00669549827498406,-0.0336938721132548,0.0797211874900445));
#66464=CARTESIAN_POINT('',(0.00692559412378843,-0.0333679870047995,0.0797751640287754));
#66465=CARTESIAN_POINT('Ctrl Pts',(0.00669549827497859,-0.033693872113252,
0.0797211874900436));
#66466=CARTESIAN_POINT('Ctrl Pts',(0.00671724523325145,-0.0336629187933862,
0.079726762752198));
#66467=CARTESIAN_POINT('Ctrl Pts',(0.00673901788172619,-0.0336319952301,
0.0797322088940652));
#66468=CARTESIAN_POINT('Ctrl Pts',(0.00676081392563053,-0.0336011045488914,
0.0797375256153195));
#66469=CARTESIAN_POINT('Ctrl Pts',(0.00681550765797378,-0.0335235892595418,
0.0797508670882265));
#66470=CARTESIAN_POINT('Ctrl Pts',(0.00687044592600969,-0.0334458668665535,
0.0797634171868114));
#66471=CARTESIAN_POINT('Ctrl Pts',(0.00692559411218311,-0.0333679869962459,
0.0797751640265497));
#66472=CARTESIAN_POINT('Ctrl Pts',(0.00692563746768464,-0.0333679692468944,
0.0797751739643015));
#66473=CARTESIAN_POINT('Ctrl Pts',(0.0069257260888849,-0.0333391895413371,
0.07977472946001));
#66474=CARTESIAN_POINT('Ctrl Pts',(0.00692578933029035,-0.0333104081127898,
0.0797743956474309));
#66475=CARTESIAN_POINT('Ctrl Pts',(0.00692586759951753,-0.0332532697859831,
0.079773952758113));
#66476=CARTESIAN_POINT('Ctrl Pts',(0.00692588332869693,-0.0332249169284244,
0.0797738404015532));
#66477=CARTESIAN_POINT('Ctrl Pts',(0.00692587734690751,-0.0331960985446588,
0.0797738353746939));
#66478=CARTESIAN_POINT('Ctrl Pts',(0.00692587724360892,-0.0331956312477754,
0.0797738353222659));
#66479=CARTESIAN_POINT('Ctrl Pts',(0.00692587713480589,-0.0331951640388594,
0.0797738352990903));
#66480=CARTESIAN_POINT('',(0.00680361984569412,-0.0331951640388587,0.0797477938847791));
#66481=CARTESIAN_POINT('',(0.00686474849025947,-0.0331951640388687,0.0797608145919446));
#66482=CARTESIAN_POINT('',(0.00657475148821477,-0.0335216366567667,0.0796888291967531));
#66483=CARTESIAN_POINT('Origin',(0.00988225669933695,-0.0326434571528327,
0.0633661126856979));
#66484=CARTESIAN_POINT('',(0.00657511738662483,-0.0336938721132327,0.0796875208638126));
#66485=CARTESIAN_POINT('Origin',(0.00363384684509192,-0.0336938867896251,
0.0902045431394953));
#66486=CARTESIAN_POINT('',(0.00663530783081445,-0.0336938721132537,0.0797043541769385));
#66487=CARTESIAN_POINT('Ctrl Pts',(0.00628253803905408,-0.0335235895815172,
0.0798605008506432));
#66488=CARTESIAN_POINT('Ctrl Pts',(0.00636115432620475,-0.0334144449262748,
0.0798858492014999));
#66489=CARTESIAN_POINT('Ctrl Pts',(0.00644038461179668,-0.0333049234473147,
0.0799096025212135));
#66490=CARTESIAN_POINT('Ctrl Pts',(0.00652013033595572,-0.0331951640388587,
0.0799317212593731));
#66491=CARTESIAN_POINT('Ctrl Pts',(0.00638006966083075,-0.0335235895815172,
0.0798028054848014));
#66492=CARTESIAN_POINT('Ctrl Pts',(0.00645789165767889,-0.0334144449262748,
0.0798268111208623));
#66493=CARTESIAN_POINT('Ctrl Pts',(0.00653629900094778,-0.0333049234473147,
0.0798492365926033));
#66494=CARTESIAN_POINT('Ctrl Pts',(0.00661519402924983,-0.0331951640388587,
0.0798700441428444));
#66495=CARTESIAN_POINT('Ctrl Pts',(0.00647760128260742,-0.0335235895815172,
0.0797451101189596));
#66496=CARTESIAN_POINT('Ctrl Pts',(0.00655462898915302,-0.0334144449262748,
0.0797677730402246));
#66497=CARTESIAN_POINT('Ctrl Pts',(0.00663221339009887,-0.0333049234473147,
0.0797888706639931));
#66498=CARTESIAN_POINT('Ctrl Pts',(0.00671025772254394,-0.0331951640388587,
0.0798083670263157));
#66499=CARTESIAN_POINT('Ctrl Pts',(0.00657513290438409,-0.0335235895815172,
0.0796874147531178));
#66500=CARTESIAN_POINT('Ctrl Pts',(0.00665136632062716,-0.0334144449262748,
0.079708734959587));
#66501=CARTESIAN_POINT('Ctrl Pts',(0.00672812777924997,-0.0333049234473147,
0.0797285047353828));
#66502=CARTESIAN_POINT('Ctrl Pts',(0.00680532141583805,-0.0331951640388587,
0.079746689909787));
#66503=CARTESIAN_POINT('',(0.00666187509083487,-0.0331951640388689,0.0798397575720862));
#66504=CARTESIAN_POINT('Ctrl Pts',(0.00650778413552333,-0.0332121607145972,
0.0799282826356574));
#66505=CARTESIAN_POINT('Ctrl Pts',(0.00651934140213031,-0.0332625444109758,
0.0798869576150997));
#66506=CARTESIAN_POINT('Ctrl Pts',(0.00653069951889734,-0.0333135300746838,
0.0798463446894959));
#66507=CARTESIAN_POINT('Ctrl Pts',(0.00655302646867632,-0.0334167203140557,
0.0797665107901856));
#66508=CARTESIAN_POINT('Ctrl Pts',(0.00656398665427754,-0.0334688847587232,
0.0797273207368029));
#66509=CARTESIAN_POINT('Ctrl Pts',(0.00657475148855615,-0.0335216366562301,
0.0796888291961133));
#66510=CARTESIAN_POINT('Ctrl Pts',(0.00669450368631926,-0.0336938721132516,
0.0797194206075927));
#66511=CARTESIAN_POINT('Ctrl Pts',(0.00672710335326963,-0.0336474569765021,
0.079727786648979));
#66512=CARTESIAN_POINT('Ctrl Pts',(0.00675979872154734,-0.033601104548885,
0.0797357704968567));
#66513=CARTESIAN_POINT('Ctrl Pts',(0.00684257587687882,-0.0334837508592655,
0.0797559837640789));
#66514=CARTESIAN_POINT('Ctrl Pts',(0.00692591564360106,-0.0333660264659097,
0.0797737352963861));
#66515=CARTESIAN_POINT('Ctrl Pts',(0.00669549827495535,-0.0336938721132516,
0.0797211874900371));
#66516=CARTESIAN_POINT('Ctrl Pts',(0.00672810828405499,-0.0336474569765021,
0.0797295477097661));
#66517=CARTESIAN_POINT('Ctrl Pts',(0.00676081392562346,-0.033601104548885,
0.0797375256153175));
#66518=CARTESIAN_POINT('Ctrl Pts',(0.00684361709056516,-0.0334837508592655,
0.0797577238379356));
#66519=CARTESIAN_POINT('Ctrl Pts',(0.00692698240967332,-0.0333660264659097,
0.0797754595615265));
#66520=CARTESIAN_POINT('Ctrl Pts',(0.00686225684122005,-0.0336938721132516,
0.0800174333674734));
#66521=CARTESIAN_POINT('Ctrl Pts',(0.00689660087574535,-0.0336474569765021,
0.0800248174939775));
#66522=CARTESIAN_POINT('Ctrl Pts',(0.00693102899751936,-0.033601104548885,
0.0800317990742297));
#66523=CARTESIAN_POINT('Ctrl Pts',(0.00701819308631786,-0.0334837508592655,
0.08004947483026));
#66524=CARTESIAN_POINT('Ctrl Pts',(0.00710584266837151,-0.0333660264659097,
0.0800645599717287));
#66525=CARTESIAN_POINT('',(0.00687379430618294,-0.0336769361243754,0.0800183498773113));
#66526=CARTESIAN_POINT('',(0.00686126225730294,-0.033693872113232,0.0800156664933913));
#66527=CARTESIAN_POINT('Ctrl Pts',(0.00687379430618319,-0.0336769361243751,
0.0800183498773114));
#66528=CARTESIAN_POINT('Ctrl Pts',(0.00687170499727109,-0.0336797586670031,
0.080017904844059));
#66529=CARTESIAN_POINT('Ctrl Pts',(0.00686961600504582,-0.0336825812712857,
0.0800174587118532));
#66530=CARTESIAN_POINT('Ctrl Pts',(0.00686543866504512,-0.03368822658797,
0.0800165642524324));
#66531=CARTESIAN_POINT('Ctrl Pts',(0.00686335031727572,-0.0336910493003646,
0.0800161159252534));
#66532=CARTESIAN_POINT('Ctrl Pts',(0.00686126225730768,-0.0336938721132377,
0.0800156664934046));
#66533=CARTESIAN_POINT('Ctrl Pts',(0.00687379430618294,-0.0336769361243754,
0.0800183498773113));
#66534=CARTESIAN_POINT('Ctrl Pts',(0.00688252605777871,-0.0336279018525375,
0.0799773567013441));
#66535=CARTESIAN_POINT('Ctrl Pts',(0.00689138342668254,-0.0335767826051552,
0.0799357737866078));
#66536=CARTESIAN_POINT('Ctrl Pts',(0.00690873878157675,-0.0334733172106835,
0.0798542951612311));
#66537=CARTESIAN_POINT('Ctrl Pts',(0.00691724843174461,-0.033420963147761,
0.0798143446904805));
#66538=CARTESIAN_POINT('Ctrl Pts',(0.00692559410938842,-0.0333679869844681,
0.0797751640257003));
#66539=CARTESIAN_POINT('',(0.00677838026615351,-0.0336938721132534,0.0798684269917279));
#66540=CARTESIAN_POINT('Origin',(0.00812378219310841,-0.0315241814719618,
0.07415));
#66541=CARTESIAN_POINT('',(0.00687379430645763,-0.0337108120655533,0.0800183498760507));
#66542=CARTESIAN_POINT('',(0.00688633205822611,-0.0336938721132327,0.080021006486431));
#66543=CARTESIAN_POINT('Origin',(0.0113754299909055,-0.0345562507997293,
0.0642489584326503));
#66544=CARTESIAN_POINT('Ctrl Pts',(0.00688633205822346,-0.0336938721132342,
0.080021006486434));
#66545=CARTESIAN_POINT('Ctrl Pts',(0.00688424210681475,-0.0336910493131789,
0.0800205659809332));
#66546=CARTESIAN_POINT('Ctrl Pts',(0.00688215232852207,-0.0336882265943771,
0.0800201243463767));
#66547=CARTESIAN_POINT('Ctrl Pts',(0.00687797308262314,-0.033682581271242,
0.080019238811193));
#66548=CARTESIAN_POINT('Ctrl Pts',(0.00687588361507858,-0.0336797586669812,
0.0800187949105602));
#66549=CARTESIAN_POINT('Ctrl Pts',(0.00687379430618269,-0.0336769361243751,
0.0800183498773113));
#66550=CARTESIAN_POINT('Origin',(0.00918926354515599,-0.0345562519797235,
0.0637832982217835));
#66551=CARTESIAN_POINT('Ctrl Pts',(0.00676843458054931,-0.034243627687391,
0.0797393790217815));
#66552=CARTESIAN_POINT('Ctrl Pts',(0.0069792414855517,-0.0339430054201809,
0.0797904967996763));
#66553=CARTESIAN_POINT('Ctrl Pts',(0.00719329991071649,-0.0336441434784052,
0.079825590517484));
#66554=CARTESIAN_POINT('Ctrl Pts',(0.00701261670866883,-0.034243627687391,
0.0797929988717162));
#66555=CARTESIAN_POINT('Ctrl Pts',(0.00722544591964964,-0.0339430054201809,
0.0798349071688289));
#66556=CARTESIAN_POINT('Ctrl Pts',(0.0074408272098064,-0.0336441434784052,
0.0798606652406512));
#66557=CARTESIAN_POINT('',(0.00704813442391549,-0.0341934961088741,0.079799876713401));
#66558=CARTESIAN_POINT('',(0.00728116543324923,-0.0338664212863488,0.0798392989023731));
#66559=CARTESIAN_POINT('Origin',(0.0106771194136505,-0.0345610720405296,
0.0634633038873715));
#66560=CARTESIAN_POINT('Origin',(0.00567456591739579,-0.0336938005072874,
0.0906872278499356));
#66561=CARTESIAN_POINT('',(0.00715771327076761,-0.0336938721132327,0.0798196415968991));
#66562=CARTESIAN_POINT('',(0.00721953886888336,-0.0336938721132427,0.0798287983113235));
#66563=CARTESIAN_POINT('',(0.00692559410938321,-0.0340203938281605,0.0797751640256991));
#66564=CARTESIAN_POINT('Origin',(0.0111251502442658,-0.0345589643244944,
0.0636388177300196));
#66565=CARTESIAN_POINT('',(0.00692587713480481,-0.034193496108874,0.07977383529909));
#66566=CARTESIAN_POINT('Origin',(0.00463018030827809,-0.0341934220717773,
0.0905514971227124));
#66567=CARTESIAN_POINT('',(0.00698700577937015,-0.034193496108884,0.0797868560062556));
#66568=CARTESIAN_POINT('Ctrl Pts',(0.00664473397720439,-0.0340223579322397,
0.0799648444841687));
#66569=CARTESIAN_POINT('Ctrl Pts',(0.00672493584839216,-0.0339125849573575,
0.0799852444165857));
#66570=CARTESIAN_POINT('Ctrl Pts',(0.00680550359385178,-0.0338030433565231,
0.0800039700218362));
#66571=CARTESIAN_POINT('Ctrl Pts',(0.00688633205822612,-0.0336938721132327,
0.080021006486431));
#66572=CARTESIAN_POINT('Ctrl Pts',(0.00673845047646088,-0.0340223579322397,
0.0799011389302705));
#66573=CARTESIAN_POINT('Ctrl Pts',(0.00681777368190933,-0.0339125849573575,
0.0799202462677398));
#66574=CARTESIAN_POINT('Ctrl Pts',(0.00689743662534604,-0.0338030433565231,
0.0799376983726733));
#66575=CARTESIAN_POINT('Ctrl Pts',(0.00697733545287098,-0.0336938721132327,
0.0799534819576028));
#66576=CARTESIAN_POINT('Ctrl Pts',(0.00683216697571736,-0.0340223579322397,
0.0798374333763723));
#66577=CARTESIAN_POINT('Ctrl Pts',(0.0069106115154265,-0.0339125849573575,
0.079855248118894));
#66578=CARTESIAN_POINT('Ctrl Pts',(0.00698936965684029,-0.0338030433565231,
0.0798714267235104));
#66579=CARTESIAN_POINT('Ctrl Pts',(0.00706833884751585,-0.0336938721132327,
0.0798859574287746));
#66580=CARTESIAN_POINT('Ctrl Pts',(0.00692588347497385,-0.0340223579322397,
0.0797737278224742));
#66581=CARTESIAN_POINT('Ctrl Pts',(0.00700344934894367,-0.0339125849573575,
0.0797902499700482));
#66582=CARTESIAN_POINT('Ctrl Pts',(0.00708130268833455,-0.0338030433565231,
0.0798051550743475));
#66583=CARTESIAN_POINT('Ctrl Pts',(0.00715934224216072,-0.0336938721132327,
0.0798184328999464));
#66584=CARTESIAN_POINT('',(0.00702202266450686,-0.0336938721132427,0.079920324041675));
#66585=CARTESIAN_POINT('Ctrl Pts',(0.00687379430720368,-0.0337108120662689,
0.0800183498725188));
#66586=CARTESIAN_POINT('Ctrl Pts',(0.00688275239876129,-0.0337611408994256,
0.0799762940925845));
#66587=CARTESIAN_POINT('Ctrl Pts',(0.00689154702502222,-0.0338121088781224,
0.0799350057373299));
#66588=CARTESIAN_POINT('Ctrl Pts',(0.00690881735871832,-0.0339153382773237,
0.0798539262631313));
#66589=CARTESIAN_POINT('Ctrl Pts',(0.00691728575974262,-0.0339675558473116,
0.07981416944578));
#66590=CARTESIAN_POINT('Ctrl Pts',(0.00692559410939671,-0.0340203938281304,
0.0797751640256612));
#66591=CARTESIAN_POINT('Ctrl Pts',(0.00704703054551019,-0.0341934961088741,
0.0797981752921274));
#66592=CARTESIAN_POINT('Ctrl Pts',(0.00716380211997548,-0.0340287516182428,
0.0798204362841637));
#66593=CARTESIAN_POINT('Ctrl Pts',(0.00728139397905306,-0.0338644633275951,
0.0798378519968459));
#66594=CARTESIAN_POINT('Ctrl Pts',(0.00704813442391546,-0.0341934961088741,
0.079799876713401));
#66595=CARTESIAN_POINT('Ctrl Pts',(0.00716494117392518,-0.0340287516182428,
0.0798221148836209));
#66596=CARTESIAN_POINT('Ctrl Pts',(0.00728256723524739,-0.0338644633275951,
0.0798395063401556));
#66597=CARTESIAN_POINT('Ctrl Pts',(0.00723206179851671,-0.0341934961088741,
0.0800833662231507));
#66598=CARTESIAN_POINT('Ctrl Pts',(0.00735472947080411,-0.0340287516182428,
0.0801018018398009));
#66599=CARTESIAN_POINT('Ctrl Pts',(0.00747805428393412,-0.0338644633275951,
0.080115151755611));
#66600=CARTESIAN_POINT('',(0.00724473760860792,-0.0341764758832429,0.0800852574172649));
#66601=CARTESIAN_POINT('',(0.00723206179850727,-0.034193496108874,0.0800833662231361));
#66602=CARTESIAN_POINT('Origin',(0.0101771442443428,-0.0345621026889891,
0.0637811990244643));
#66603=CARTESIAN_POINT('Ctrl Pts',(0.00724473760714494,-0.0341764758837536,
0.0800852574161694));
#66604=CARTESIAN_POINT('Ctrl Pts',(0.0072510263338492,-0.0341260050040345,
0.0800427962089692));
#66605=CARTESIAN_POINT('Ctrl Pts',(0.00725720570985234,-0.0340749269147931,
0.0800010730721234));
#66606=CARTESIAN_POINT('Ctrl Pts',(0.00726935073097967,-0.0339715436305673,
0.0799190706301537));
#66607=CARTESIAN_POINT('Ctrl Pts',(0.00727531177446978,-0.0339192778236826,
0.0798788224358291));
#66608=CARTESIAN_POINT('Ctrl Pts',(0.00728116543122125,-0.0338664212854931,
0.079839298903217));
#66609=CARTESIAN_POINT('',(0.00714009811122139,-0.0341934961088841,0.0799416214682786));
#66610=CARTESIAN_POINT('Origin',(0.00812378219310841,-0.0315241814719618,
0.07415));
#66611=CARTESIAN_POINT('',(0.00724473760954819,-0.0342105180190349,0.0800852574166593));
#66612=CARTESIAN_POINT('',(0.00725741743084159,-0.034193496108874,0.0800871215330949));
#66613=CARTESIAN_POINT('Origin',(0.0101333719713516,-0.034562169737374,
0.0637694223670492));
#66614=CARTESIAN_POINT('Origin',(0.00916399607309383,-0.0345621043777391,
0.063631142614299));
#66615=CARTESIAN_POINT('Origin',(0.00920930196589667,-0.0345621711700108,
0.0636325666787368));
#66616=CARTESIAN_POINT('Ctrl Pts',(0.00715622944660961,-0.0346945769586966,
0.079819421834301));
#66617=CARTESIAN_POINT('Ctrl Pts',(0.00727497775684171,-0.0345275153362944,
0.0798396876139634));
#66618=CARTESIAN_POINT('Ctrl Pts',(0.00739439412158621,-0.0343603235965185,
0.0798562241103379));
#66619=CARTESIAN_POINT('Ctrl Pts',(0.00751412463335077,-0.034193496108874,
0.0798689876649925));
#66620=CARTESIAN_POINT('Ctrl Pts',(0.00723915818567159,-0.0346945769586966,
0.0798317040410828));
#66621=CARTESIAN_POINT('Ctrl Pts',(0.00735816375164226,-0.0345275153362944,
0.0798502328451027));
#66622=CARTESIAN_POINT('Ctrl Pts',(0.00747778281237967,-0.0343603235965185,
0.0798650238261077));
#66623=CARTESIAN_POINT('Ctrl Pts',(0.00759766093763429,-0.034193496108874,
0.0798760384970352));
#66624=CARTESIAN_POINT('Ctrl Pts',(0.0073220869247337,-0.0346945769586966,
0.0798439862478629));
#66625=CARTESIAN_POINT('Ctrl Pts',(0.0074413497464428,-0.0345275153362944,
0.0798607780762401));
#66626=CARTESIAN_POINT('Ctrl Pts',(0.00756117150317306,-0.0343603235965185,
0.0798738235418762));
#66627=CARTESIAN_POINT('Ctrl Pts',(0.00768119724191778,-0.034193496108874,
0.079883089329078));
#66628=CARTESIAN_POINT('Ctrl Pts',(0.00740501566379556,-0.0346945769586966,
0.0798562684546465));
#66629=CARTESIAN_POINT('Ctrl Pts',(0.00752453574124338,-0.0345275153362944,
0.0798713233073814));
#66630=CARTESIAN_POINT('Ctrl Pts',(0.00764456019396659,-0.0343603235965185,
0.0798826232576472));
#66631=CARTESIAN_POINT('Ctrl Pts',(0.00776473354620134,-0.034193496108874,
0.0798901401611205));
#66632=CARTESIAN_POINT('',(0.00740501566319633,-0.0346945769586966,0.0798562684545576));
#66633=CARTESIAN_POINT('',(0.0076400621771997,-0.0343667727831673,0.0798809807142107));
#66634=CARTESIAN_POINT('Origin',(0.00932461120802878,-0.0345626457063345,
0.0631526041805093));
#66635=CARTESIAN_POINT('Origin',(0.00671051934626394,-0.0341934771029274,
0.0908940004869859));
#66636=CARTESIAN_POINT('',(0.00751561932852272,-0.034193496108874,0.0798691138238489));
#66637=CARTESIAN_POINT('',(0.0075778978827986,-0.034193496108884,0.0798743704081639));
#66638=CARTESIAN_POINT('',(0.00728116543148868,-0.034521194296263,0.0798392989017116));
#66639=CARTESIAN_POINT('Origin',(0.00979974754044332,-0.0345625596120374,
0.0632263351489356));
#66640=CARTESIAN_POINT('',(0.00728136446697915,-0.0346945769586885,0.0798379550257279));
#66641=CARTESIAN_POINT('Origin',(0.00566046893509098,-0.0346945685854079,
0.0907821412878401));
#66642=CARTESIAN_POINT('',(0.00734319006509773,-0.0346945769587026,0.0798471117401527));
#66643=CARTESIAN_POINT('Ctrl Pts',(0.00701277059268193,-0.0345231616327842,
0.0800462406009045));
#66644=CARTESIAN_POINT('Ctrl Pts',(0.00709404196812263,-0.0344132092796988,
0.0800615543316371));
#66645=CARTESIAN_POINT('Ctrl Pts',(0.00717562590277485,-0.034303273855898,
0.0800751862379566));
#66646=CARTESIAN_POINT('Ctrl Pts',(0.00725741743084155,-0.034193496108874,
0.0800871215330949));
#66647=CARTESIAN_POINT('Ctrl Pts',(0.00710230189555469,-0.0345231616327842,
0.0799767763515059));
#66648=CARTESIAN_POINT('Ctrl Pts',(0.00718261580411526,-0.0344132092796988,
0.0799908560192784));
#66649=CARTESIAN_POINT('Ctrl Pts',(0.00726321679566934,-0.034303273855898,
0.080003273730757));
#66650=CARTESIAN_POINT('Ctrl Pts',(0.00734400120352891,-0.034193496108874,
0.0800140162224409));
#66651=CARTESIAN_POINT('Ctrl Pts',(0.00719183319842744,-0.0345231616327842,
0.0799073121021073));
#66652=CARTESIAN_POINT('Ctrl Pts',(0.0072711896401079,-0.0344132092796988,
0.0799201577069198));
#66653=CARTESIAN_POINT('Ctrl Pts',(0.00735080768856383,-0.034303273855898,
0.0799313612235574));
#66654=CARTESIAN_POINT('Ctrl Pts',(0.00743058497621627,-0.034193496108874,
0.0799409109117868));
#66655=CARTESIAN_POINT('Ctrl Pts',(0.00728136450130019,-0.0345231616327842,
0.0798378478527087));
#66656=CARTESIAN_POINT('Ctrl Pts',(0.00735976347610053,-0.0344132092796988,
0.079849459394561));
#66657=CARTESIAN_POINT('Ctrl Pts',(0.00743839858145832,-0.034303273855898,
0.0798594487163577));
#66658=CARTESIAN_POINT('Ctrl Pts',(0.00751716874890363,-0.034193496108874,
0.0798678056011328));
#66659=CARTESIAN_POINT('',(0.00738651837969215,-0.0341934961088839,0.0799781176784819));
#66660=CARTESIAN_POINT('Ctrl Pts',(0.00724473761004957,-0.0342105180195384,
0.0800852574132335));
#66661=CARTESIAN_POINT('Ctrl Pts',(0.00725103342009984,-0.0342610556241179,
0.0800427484734217));
#66662=CARTESIAN_POINT('Ctrl Pts',(0.00725721625509396,-0.0343122189869899,
0.0800010023345559));
#66663=CARTESIAN_POINT('Ctrl Pts',(0.00726936139472658,-0.0344158119695101,
0.0799189990648373));
#66664=CARTESIAN_POINT('Ctrl Pts',(0.00727531873191037,-0.0344681990449985,
0.079878775473947));
#66665=CARTESIAN_POINT('Ctrl Pts',(0.00728116543148774,-0.0345211942962392,
0.0798392989016795));
#66666=CARTESIAN_POINT('Ctrl Pts',(0.00740380742581461,-0.0346945769586932,
0.0798546401025433));
#66667=CARTESIAN_POINT('Ctrl Pts',(0.00748242024987177,-0.034584662917547,
0.079864561718752));
#66668=CARTESIAN_POINT('Ctrl Pts',(0.00756125167614127,-0.0344746925049099,
0.0798728593486793));
#66669=CARTESIAN_POINT('Ctrl Pts',(0.00764020065280731,-0.034364806625142,
0.0798795227775937));
#66670=CARTESIAN_POINT('Ctrl Pts',(0.00747133180145219,-0.0346945769586932,
0.0799456432907319));
#66671=CARTESIAN_POINT('Ctrl Pts',(0.00755119869544069,-0.034584662917547,
0.0799546343869138));
#66672=CARTESIAN_POINT('Ctrl Pts',(0.00763126516306773,-0.0344746925049099,
0.0799619754042279));
#66673=CARTESIAN_POINT('Ctrl Pts',(0.00771142857510226,-0.034364806625142,
0.0799676573602005));
#66674=CARTESIAN_POINT('Ctrl Pts',(0.00753885617708977,-0.0346945769586932,
0.0800366464789205));
#66675=CARTESIAN_POINT('Ctrl Pts',(0.00761997714100961,-0.034584662917547,
0.0800447070550755));
#66676=CARTESIAN_POINT('Ctrl Pts',(0.00770127864999419,-0.0344746925049099,
0.0800510914597765));
#66677=CARTESIAN_POINT('Ctrl Pts',(0.00778265649739722,-0.034364806625142,
0.0800557919428073));
#66678=CARTESIAN_POINT('Ctrl Pts',(0.00760638055272735,-0.0346945769586932,
0.0801276496671091));
#66679=CARTESIAN_POINT('Ctrl Pts',(0.00768875558657853,-0.034584662917547,
0.0801347797232373));
#66680=CARTESIAN_POINT('Ctrl Pts',(0.00777129213692066,-0.0344746925049099,
0.0801402075153251));
#66681=CARTESIAN_POINT('Ctrl Pts',(0.00785388441969217,-0.034364806625142,
0.0801439265254142));
#66682=CARTESIAN_POINT('',(0.00761915009997584,-0.0346775396663668,0.0801287412079197));
#66683=CARTESIAN_POINT('',(0.00760638055272025,-0.0346945769586886,0.0801276496670952));
#66684=CARTESIAN_POINT('Origin',(0.00886319787775422,-0.0345626617929341,
0.0635738250497379));
#66685=CARTESIAN_POINT('Ctrl Pts',(0.00761915010025431,-0.0346775396659514,
0.0801287412045515));
#66686=CARTESIAN_POINT('Ctrl Pts',(0.00762276312447797,-0.0346269748529709,
0.0800859350947044));
#66687=CARTESIAN_POINT('Ctrl Pts',(0.0076263119077185,-0.0345757904818262,
0.0800438900942244));
#66688=CARTESIAN_POINT('Ctrl Pts',(0.00763328403561633,-0.0344721679344123,
0.0799612862548403));
#66689=CARTESIAN_POINT('Ctrl Pts',(0.00763670457075407,-0.0344197716859653,
0.0799207607023451));
#66690=CARTESIAN_POINT('Ctrl Pts',(0.00764006217696968,-0.0343667727830994,
0.0798809807142818));
#66691=CARTESIAN_POINT('',(0.00750569810796829,-0.0346945769587026,0.0799919590608363));
#66692=CARTESIAN_POINT('Origin',(0.00812378219310841,-0.0315241814719618,
0.07415));
#66693=CARTESIAN_POINT('',(0.00761915009998483,-0.0347116136489593,0.0801287412078104));
#66694=CARTESIAN_POINT('',(0.00763192194936935,-0.0346945769586885,0.0801298054734804));
#66695=CARTESIAN_POINT('Origin',(0.00881792530718465,-0.0345626673615202,
0.0635718759458564));
#66696=CARTESIAN_POINT('Origin',(0.00916754804003983,-0.0345626633401097,
0.0635995098234622));
#66697=CARTESIAN_POINT('Origin',(0.00921250601583,-0.0345626690505617,0.0636051839189239));
#66698=CARTESIAN_POINT('Ctrl Pts',(0.00747724508128081,-0.0352450361874068,
0.0798649580937247));
#66699=CARTESIAN_POINT('Ctrl Pts',(0.00769278826268485,-0.0349452760959492,
0.0798893426410291));
#66700=CARTESIAN_POINT('Ctrl Pts',(0.00790955585247625,-0.034644428984174,
0.0798974223200474));
#66701=CARTESIAN_POINT('Ctrl Pts',(0.00747973485464712,-0.0352450361874068,
0.0798651839887987));
#66702=CARTESIAN_POINT('Ctrl Pts',(0.00769528655582368,-0.0349452760959492,
0.0798894746327597));
#66703=CARTESIAN_POINT('Ctrl Pts',(0.00791205556799978,-0.034644428984174,
0.07989746003346));
#66704=CARTESIAN_POINT('Ctrl Pts',(0.00772871219127743,-0.0352450361874068,
0.0798877734961964));
#66705=CARTESIAN_POINT('Ctrl Pts',(0.00794511586970579,-0.0349452760959492,
0.0799026738058181));
#66706=CARTESIAN_POINT('Ctrl Pts',(0.00816202712035146,-0.034644428984174,
0.079901231374718));
#66707=CARTESIAN_POINT('Ctrl Pts',(0.0077312268623774,-0.0352450361874068,
0.0798880016502211));
#66708=CARTESIAN_POINT('Ctrl Pts',(0.007947639145776,-0.0349452760959492,
0.079902807117466));
#66709=CARTESIAN_POINT('Ctrl Pts',(0.00816455183303021,-0.034644428984174,
0.0799012694652647));
#66710=CARTESIAN_POINT('',(0.0077647011018514,-0.0351951634053305,0.0798901405098147));
#66711=CARTESIAN_POINT('',(0.00800086794471331,-0.0348678972939192,0.0799000449641624));
#66712=CARTESIAN_POINT('Origin',(0.00793593353284433,-0.0345628965658585,
0.0631458627386298));
#66713=CARTESIAN_POINT('Origin',(0.00776473386622734,-0.0346946199326787,
0.0909473631118738));
#66714=CARTESIAN_POINT('',(0.00787592550929624,-0.0346945769330289,0.079896015320419));
#66715=CARTESIAN_POINT('',(0.00793841124341285,-0.0346945769458128,0.0798973510298189));
#66716=CARTESIAN_POINT('',(0.00764006217696069,-0.0350221583435276,0.0798809807141517));
#66717=CARTESIAN_POINT('Origin',(0.00841677757682629,-0.0345628458716598,
0.0631145062762775));
#66718=CARTESIAN_POINT('',(0.00764016319169323,-0.0351951360298762,0.0798797479575789));
#66719=CARTESIAN_POINT('Origin',(0.00671341033859371,-0.0351951838366723,
0.0908596829756913));
#66720=CARTESIAN_POINT('',(0.00776473354557716,-0.0351951371328746,0.0798901401611844));
#66721=CARTESIAN_POINT('Ctrl Pts',(0.00738519188429683,-0.0350241211494343,
0.080104366830803));
#66722=CARTESIAN_POINT('Ctrl Pts',(0.00746721084600568,-0.0349144232818962,
0.0801145406094731));
#66723=CARTESIAN_POINT('Ctrl Pts',(0.00754948919929143,-0.0348045283579412,
0.0801230250870939));
#66724=CARTESIAN_POINT('Ctrl Pts',(0.00763192196044475,-0.0346945769439158,
0.0801298054743914));
#66725=CARTESIAN_POINT('Ctrl Pts',(0.00747018482803159,-0.0350241211494343,
0.0800294179060719));
#66726=CARTESIAN_POINT('Ctrl Pts',(0.00755117139903253,-0.0349144232818962,
0.0800384209417905));
#66727=CARTESIAN_POINT('Ctrl Pts',(0.00763239254358138,-0.0348045283579412,
0.0800457553159674));
#66728=CARTESIAN_POINT('Ctrl Pts',(0.00771374457730006,-0.0346945769439158,
0.0800514077628559));
#66729=CARTESIAN_POINT('Ctrl Pts',(0.00755517777176635,-0.0350241211494343,
0.0799544689813407));
#66730=CARTESIAN_POINT('Ctrl Pts',(0.00763513195205937,-0.0349144232818962,
0.0799623012741078));
#66731=CARTESIAN_POINT('Ctrl Pts',(0.00771529588787134,-0.0348045283579412,
0.0799684855448408));
#66732=CARTESIAN_POINT('Ctrl Pts',(0.00779556719415537,-0.0346945769439158,
0.0799730100513204));
#66733=CARTESIAN_POINT('Ctrl Pts',(0.00764017071550111,-0.0350241211494343,
0.0798795200566096));
#66734=CARTESIAN_POINT('Ctrl Pts',(0.00771909250508621,-0.0349144232818962,
0.0798861816064252));
#66735=CARTESIAN_POINT('Ctrl Pts',(0.00779819923216129,-0.0348045283579412,
0.0798912157737143));
#66736=CARTESIAN_POINT('Ctrl Pts',(0.00787738981101069,-0.0346945769439158,
0.079894612339785));
#66737=CARTESIAN_POINT('',(0.00775392372904227,-0.0346945769458128,0.080012910397025));
#66738=CARTESIAN_POINT('Ctrl Pts',(0.00761915010025643,-0.034711613649279,
0.0801287412045252));
#66739=CARTESIAN_POINT('Ctrl Pts',(0.00762276167853553,-0.0347621546532138,
0.0800859522258283));
#66740=CARTESIAN_POINT('Ctrl Pts',(0.00762630975550902,-0.03481330840967,
0.0800439155930049));
#66741=CARTESIAN_POINT('Ctrl Pts',(0.00763328186796119,-0.0349168561544569,
0.0799613119366169));
#66742=CARTESIAN_POINT('Ctrl Pts',(0.00763670313795349,-0.0349692089015916,
0.0799207776777686));
#66743=CARTESIAN_POINT('Ctrl Pts',(0.00764006217698359,-0.0350221583435,
0.0798809807141169));
#66744=CARTESIAN_POINT('Ctrl Pts',(0.00776378970930018,-0.0351951371254924,
0.0798890223092295));
#66745=CARTESIAN_POINT('Ctrl Pts',(0.0078428252849622,-0.0350856248738962,
0.0798939799852341));
#66746=CARTESIAN_POINT('Ctrl Pts',(0.00792202819928413,-0.0349758427086608,
0.0798973083633598));
#66747=CARTESIAN_POINT('Ctrl Pts',(0.00800129730473024,-0.0348659306906667,
0.0798989972261563));
#66748=CARTESIAN_POINT('Ctrl Pts',(0.00781683363617358,-0.0351951371254924,
0.079951845970955));
#66749=CARTESIAN_POINT('Ctrl Pts',(0.00789673439478874,-0.0350856248738962,
0.0799560731466983));
#66750=CARTESIAN_POINT('Ctrl Pts',(0.00797678810562306,-0.0349758427086608,
0.0799586525448041));
#66751=CARTESIAN_POINT('Ctrl Pts',(0.00805689247560053,-0.0348659306906667,
0.0799595748427044));
#66752=CARTESIAN_POINT('Ctrl Pts',(0.00786987756304698,-0.0351951371254924,
0.0800146696326804));
#66753=CARTESIAN_POINT('Ctrl Pts',(0.00795064350461529,-0.0350856248738962,
0.0800181663081626));
#66754=CARTESIAN_POINT('Ctrl Pts',(0.008031548011962,-0.0349758427086608,
0.0800199967262483));
#66755=CARTESIAN_POINT('Ctrl Pts',(0.00811248764647081,-0.0348659306906667,
0.0800201524592524));
#66756=CARTESIAN_POINT('Ctrl Pts',(0.00792292148992038,-0.0351951371254924,
0.0800774932944058));
#66757=CARTESIAN_POINT('Ctrl Pts',(0.00800455261444184,-0.0350856248738962,
0.0800802594696268));
#66758=CARTESIAN_POINT('Ctrl Pts',(0.00808630791830094,-0.0349758427086608,
0.0800813409076926));
#66759=CARTESIAN_POINT('Ctrl Pts',(0.0081680828173411,-0.0348659306906667,
0.0800807300758005));
#66760=CARTESIAN_POINT('Origin',(0.00788721294704829,-0.0308609188508779,
0.0852170131853622));
#66761=CARTESIAN_POINT('',(0.00783369992264697,-0.0351951371254924,0.0799718219029499));
#66762=CARTESIAN_POINT('Origin',(0.00800290361662291,-0.035184046744755,
0.0731803948590619));
#66763=CARTESIAN_POINT('Origin',(0.00866315573714708,-0.0352322612474718,
0.0861032743007049));
#66764=CARTESIAN_POINT('',(0.00823752392040189,-0.0351951142564675,0.0799002067269712));
#66765=CARTESIAN_POINT('',(0.00836210254579337,-0.0351951372916786,0.0798950590431689));
#66766=CARTESIAN_POINT('Origin',(0.00840618459976702,-0.0352875121144073,
0.0739596041588875));
#66767=CARTESIAN_POINT('Origin',(0.000706367619496166,-0.0298325076522946,
0.0730198888008274));
#66768=CARTESIAN_POINT('Origin',(0.00529310284598232,-0.0338731063892672,
0.0820393710964081));
#66769=CARTESIAN_POINT('Ctrl Pts',(0.00483560513139321,-0.0321934096636941,
0.0788686891565478));
#66770=CARTESIAN_POINT('Ctrl Pts',(0.0049200674202468,-0.0320508460843909,
0.0789275459601164));
#66771=CARTESIAN_POINT('Ctrl Pts',(0.00500604739043419,-0.0319086045662242,
0.0789840890504166));
#66772=CARTESIAN_POINT('Ctrl Pts',(0.00509334988896869,-0.0317669892866659,
0.0790382119212771));
#66773=CARTESIAN_POINT('Ctrl Pts',(0.00490542372789669,-0.0321934096636941,
0.0789151197090981));
#66774=CARTESIAN_POINT('Ctrl Pts',(0.00499071710153061,-0.0320508460843909,
0.0789727267930371));
#66775=CARTESIAN_POINT('Ctrl Pts',(0.00507749395235713,-0.0319086045662242,
0.0790279987763921));
#66776=CARTESIAN_POINT('Ctrl Pts',(0.00516555763688526,-0.0317669892866659,
0.0790808320311662));
#66777=CARTESIAN_POINT('Ctrl Pts',(0.00497524232440018,-0.0321934096636941,
0.0789615502616486));
#66778=CARTESIAN_POINT('Ctrl Pts',(0.00506136678281444,-0.0320508460843909,
0.0790179076259579));
#66779=CARTESIAN_POINT('Ctrl Pts',(0.00514894051428005,-0.0319086045662242,
0.0790719085023677));
#66780=CARTESIAN_POINT('Ctrl Pts',(0.00523776538480183,-0.0317669892866659,
0.0791234521410554));
#66781=CARTESIAN_POINT('Ctrl Pts',(0.00504506092090366,-0.0321934096636941,
0.079007980814199));
#66782=CARTESIAN_POINT('Ctrl Pts',(0.00513201646409826,-0.0320508460843909,
0.0790630884588786));
#66783=CARTESIAN_POINT('Ctrl Pts',(0.00522038707620298,-0.0319086045662242,
0.0791158182283434));
#66784=CARTESIAN_POINT('Ctrl Pts',(0.0053099731327184,-0.0317669892866659,
0.0791660722509446));
#66785=CARTESIAN_POINT('',(0.00504381185241653,-0.0321934096636941,0.0790071501624367));
#66786=CARTESIAN_POINT('',(0.00524596632873056,-0.0318665617511322,0.0791295884207342));
#66787=CARTESIAN_POINT('Origin',(0.0145055280571824,-0.0326371944419857,
0.0652342117938775));
#66788=CARTESIAN_POINT('Origin',(-0.000238698541601191,-0.0316939261508872,
0.0886199014530148));
#66789=CARTESIAN_POINT('',(0.00493921987219606,-0.0320197221621748,0.0789391702820801));
#66790=CARTESIAN_POINT('Ctrl Pts',(0.00493934267991975,-0.0320197392094669,
0.0789393086046855));
#66791=CARTESIAN_POINT('Ctrl Pts',(0.00496371224781349,-0.0319792716575967,
0.0789555120176116));
#66792=CARTESIAN_POINT('Ctrl Pts',(0.00498831628355511,-0.0319386439829624,
0.0789716034108641));
#66793=CARTESIAN_POINT('Ctrl Pts',(0.00501318524593401,-0.0318979099381556,
0.0789875925992203));
#66794=CARTESIAN_POINT('Ctrl Pts',(0.00503805371675908,-0.031857176698488,
0.0790035814715382));
#66795=CARTESIAN_POINT('Ctrl Pts',(0.00506305974239178,-0.0318163871833551,
0.0790193883757689));
#66796=CARTESIAN_POINT('Ctrl Pts',(0.00508811543097495,-0.0317755399638303,
0.0790349619190384));
#66797=CARTESIAN_POINT('',(0.0049397263837213,-0.0321934096636185,0.0789379315578555));
#66798=CARTESIAN_POINT('Origin',(0.0036795163241933,-0.0324111462521584,
0.0808709034511289));
#66799=CARTESIAN_POINT('',(0.00499176911807891,-0.0321934096636663,0.0789725408601561));
#66800=CARTESIAN_POINT('Ctrl Pts',(0.005043411812262,-0.0321934096636618,
0.079005161782379));
#66801=CARTESIAN_POINT('Ctrl Pts',(0.0051103682771328,-0.0320835708272592,
0.0790476424906311));
#66802=CARTESIAN_POINT('Ctrl Pts',(0.00517816504058231,-0.0319739230346488,
0.0790887128977855));
#66803=CARTESIAN_POINT('Ctrl Pts',(0.0052467113285401,-0.0318646057455572,
0.0791283271142545));
#66804=CARTESIAN_POINT('Ctrl Pts',(0.00506576245863784,-0.0321934096636618,
0.0791162545966029));
#66805=CARTESIAN_POINT('Ctrl Pts',(0.00513425097999746,-0.0320835708272592,
0.0791584270720224));
#66806=CARTESIAN_POINT('Ctrl Pts',(0.00520357253241831,-0.0319739230346488,
0.0791991577193024));
#66807=CARTESIAN_POINT('Ctrl Pts',(0.00527363442433022,-0.0318646057455572,
0.0792384012332775));
#66808=CARTESIAN_POINT('Ctrl Pts',(0.00508811310501367,-0.0321934096636617,
0.0792273474108269));
#66809=CARTESIAN_POINT('Ctrl Pts',(0.00515813368286211,-0.0320835708272592,
0.0792692116534138));
#66810=CARTESIAN_POINT('Ctrl Pts',(0.00522898002425432,-0.0319739230346488,
0.0793096025408193));
#66811=CARTESIAN_POINT('Ctrl Pts',(0.00530055752012034,-0.0318646057455572,
0.0793484753523005));
#66812=CARTESIAN_POINT('Ctrl Pts',(0.0051104637513895,-0.0321934096636617,
0.0793384402250508));
#66813=CARTESIAN_POINT('Ctrl Pts',(0.00518201638572676,-0.0320835708272592,
0.0793799962348052));
#66814=CARTESIAN_POINT('Ctrl Pts',(0.00525438751609032,-0.0319739230346488,
0.0794200473623362));
#66815=CARTESIAN_POINT('Ctrl Pts',(0.00532748061591046,-0.0318646057455572,
0.0794585494713235));
#66816=CARTESIAN_POINT('',(0.00512155322786208,-0.0321763980308309,0.0793448648892966));
#66817=CARTESIAN_POINT('',(0.00511046375141491,-0.0321934096636184,0.0793384402250532));
#66818=CARTESIAN_POINT('Origin',(0.0139270308064902,-0.0326386230501741,
0.0653345240239085));
#66819=CARTESIAN_POINT('Ctrl Pts',(0.00512155322944348,-0.0321763980306358,
0.0793448648865458));
#66820=CARTESIAN_POINT('Ctrl Pts',(0.00514302862021074,-0.032125959617624,
0.0793077052445692));
#66821=CARTESIAN_POINT('Ctrl Pts',(0.00516413192196313,-0.0320749164634223,
0.0792711894416004));
#66822=CARTESIAN_POINT('Ctrl Pts',(0.0052056113309264,-0.0319716057793972,
0.0791994161265915));
#66823=CARTESIAN_POINT('Ctrl Pts',(0.00522597127620166,-0.0319193786690153,
0.0791641865801306));
#66824=CARTESIAN_POINT('Ctrl Pts',(0.00524596632965145,-0.0318665617525372,
0.0791295884191216));
#66825=CARTESIAN_POINT('',(0.00507713780192571,-0.0321934096636663,0.079172795193755));
#66826=CARTESIAN_POINT('Origin',(0.00812378219310841,-0.0315241814719618,
0.07415));
#66827=CARTESIAN_POINT('',(0.00512155322767646,-0.0322104233323594,0.0793448648896169));
#66828=CARTESIAN_POINT('',(0.00513265640034521,-0.0321934096636183,0.0793512658547612));
#66829=CARTESIAN_POINT('Origin',(0.0138913242442269,-0.0326387223796466,
0.0653065885275257));
#66830=CARTESIAN_POINT('Origin',(0.0128646762507391,-0.0326386249609679,
0.0647205611477657));
#66831=CARTESIAN_POINT('Origin',(0.0129067043389715,-0.0326387238634907,
0.0647375594113493));
#66832=CARTESIAN_POINT('Ctrl Pts',(0.00510758521549168,-0.0327445246967097,
0.0790470073302188));
#66833=CARTESIAN_POINT('Ctrl Pts',(0.00529227886628301,-0.032443687833936,
0.0791607650589165));
#66834=CARTESIAN_POINT('Ctrl Pts',(0.00548501651897787,-0.0321434074405927,
0.0792602877332916));
#66835=CARTESIAN_POINT('Ctrl Pts',(0.00532324750568314,-0.0327445246967097,
0.0791734580185892));
#66836=CARTESIAN_POINT('Ctrl Pts',(0.00551271032215167,-0.032443687833936,
0.0792790819110421));
#66837=CARTESIAN_POINT('Ctrl Pts',(0.00570959091803836,-0.0321434074405927,
0.0793701346234916));
#66838=CARTESIAN_POINT('',(0.00535487245241603,-0.0326943950436612,0.0791909586239028));
#66839=CARTESIAN_POINT('',(0.00556431598451705,-0.0323666188837389,0.0793004618945372));
#66840=CARTESIAN_POINT('Origin',(0.0133815612327477,-0.0326395579110695,
0.0644200302362526));
#66841=CARTESIAN_POINT('Origin',(0.000649251549682753,-0.0321933825603001,
0.0891911400034396));
#66842=CARTESIAN_POINT('',(0.00545298043822705,-0.032193409653269,0.0792436178677751));
#66843=CARTESIAN_POINT('',(0.00550895049813857,-0.0321934096584275,0.079271431582728));
#66844=CARTESIAN_POINT('',(0.00524596632824741,-0.0325210109756239,0.079129588421542));
#66845=CARTESIAN_POINT('Origin',(0.0137901838302527,-0.0326393129158855,
0.064673431109986));
#66846=CARTESIAN_POINT('',(0.00524664610052126,-0.0326943950436593,0.0791284121871067));
#66847=CARTESIAN_POINT('Origin',(-0.000288691790634326,-0.0326943765538279,
0.0887064052524144));
#66848=CARTESIAN_POINT('',(0.00530075927647864,-0.0326943950436702,0.0791596854055147));
#66849=CARTESIAN_POINT('Ctrl Pts',(0.00492023867268703,-0.0325229783203769,
0.0792231951384511));
#66850=CARTESIAN_POINT('Ctrl Pts',(0.00499017255672714,-0.032413025309245,
0.0792673559158233));
#66851=CARTESIAN_POINT('Ctrl Pts',(0.00506100935633197,-0.0323031222208069,
0.0793100633231205));
#66852=CARTESIAN_POINT('Ctrl Pts',(0.00513265640423252,-0.0321934096576658,
0.0793512658569968));
#66853=CARTESIAN_POINT('Ctrl Pts',(0.0050290542952026,-0.0325229783203769,
0.0791915675787449));
#66854=CARTESIAN_POINT('Ctrl Pts',(0.00509855219402381,-0.032413025309245,
0.0792342283351404));
#66855=CARTESIAN_POINT('Ctrl Pts',(0.00516892204467461,-0.0323031222208069,
0.0792754449678827));
#66856=CARTESIAN_POINT('Ctrl Pts',(0.0052400718453971,-0.0321934096576658,
0.0793151678620962));
#66857=CARTESIAN_POINT('Ctrl Pts',(0.00513786991771817,-0.0325229783203769,
0.0791599400190387));
#66858=CARTESIAN_POINT('Ctrl Pts',(0.00520693183132047,-0.032413025309245,
0.0792011007544574));
#66859=CARTESIAN_POINT('Ctrl Pts',(0.00527683473301726,-0.0323031222208069,
0.0792408266126449));
#66860=CARTESIAN_POINT('Ctrl Pts',(0.00534748728656168,-0.0321934096576658,
0.0792790698671956));
#66861=CARTESIAN_POINT('Ctrl Pts',(0.00524668554023373,-0.0325229783203769,
0.0791283124593325));
#66862=CARTESIAN_POINT('Ctrl Pts',(0.00531531146861714,-0.032413025309245,
0.0791679731737744));
#66863=CARTESIAN_POINT('Ctrl Pts',(0.0053847474213599,-0.0323031222208069,
0.0792062082574071));
#66864=CARTESIAN_POINT('Ctrl Pts',(0.00545490272772627,-0.0321934096576658,
0.0792429718722951));
#66865=CARTESIAN_POINT('',(0.00529281841879103,-0.0321934096584275,0.0792974418611707));
#66866=CARTESIAN_POINT('Ctrl Pts',(0.00512155322941316,-0.0322104233328919,
0.0793448648865983));
#66867=CARTESIAN_POINT('Ctrl Pts',(0.00514305771973737,-0.0322609421831331,
0.0793076548926103));
#66868=CARTESIAN_POINT('Ctrl Pts',(0.00516417523713712,-0.0323120888240662,
0.0792711144918086));
#66869=CARTESIAN_POINT('Ctrl Pts',(0.00520565496004409,-0.0324156524631809,
0.0791993406335716));
#66870=CARTESIAN_POINT('Ctrl Pts',(0.00522600011520745,-0.0324680267167312,
0.0791641366789603));
#66871=CARTESIAN_POINT('Ctrl Pts',(0.00524596632827296,-0.0325210109755913,
0.0791295884215067));
#66872=CARTESIAN_POINT('Origin',(0.00183541458650297,-0.0262834582510794,
0.0694213830049663));
#66873=CARTESIAN_POINT('Origin',(-0.00202648219799944,-0.0342770903299606,
0.0808430025345483));
#66874=CARTESIAN_POINT('Ctrl Pts',(0.00535434847749101,-0.0326943950436604,
0.0791889997617047));
#66875=CARTESIAN_POINT('Ctrl Pts',(0.0054237953382994,-0.0325844576448134,
0.0792271677487778));
#66876=CARTESIAN_POINT('Ctrl Pts',(0.00549403649051997,-0.0324744968375322,
0.0792639021621176));
#66877=CARTESIAN_POINT('Ctrl Pts',(0.00556498128790682,-0.0323646534831894,
0.0792991571767813));
#66878=CARTESIAN_POINT('Ctrl Pts',(0.00538363055309838,-0.0326943950436604,
0.0792984697924462));
#66879=CARTESIAN_POINT('Ctrl Pts',(0.00545458611609909,-0.0325844576448134,
0.0793362342176371));
#66880=CARTESIAN_POINT('Ctrl Pts',(0.00552632773096381,-0.0324744968375322,
0.0793725338380989));
#66881=CARTESIAN_POINT('Ctrl Pts',(0.00559876283665023,-0.0323646534831894,
0.0794073234124879));
#66882=CARTESIAN_POINT('Ctrl Pts',(0.00541291262870576,-0.0326943950436604,
0.0794079398231878));
#66883=CARTESIAN_POINT('Ctrl Pts',(0.00548537689389879,-0.0325844576448134,
0.0794453006864963));
#66884=CARTESIAN_POINT('Ctrl Pts',(0.00555861897140765,-0.0324744968375322,
0.0794811655140802));
#66885=CARTESIAN_POINT('Ctrl Pts',(0.00563254438539363,-0.0323646534831894,
0.0795154896481944));
#66886=CARTESIAN_POINT('Ctrl Pts',(0.00544219470431313,-0.0326943950436604,
0.0795174098539293));
#66887=CARTESIAN_POINT('Ctrl Pts',(0.00551616767169849,-0.0325844576448134,
0.0795543671553555));
#66888=CARTESIAN_POINT('Ctrl Pts',(0.0055909102118515,-0.0324744968375322,
0.0795897971900614));
#66889=CARTESIAN_POINT('Ctrl Pts',(0.00566632593413703,-0.0323646534831894,
0.0796236558839009));
#66890=CARTESIAN_POINT('',(0.00545366570612353,-0.0326773559991379,0.0795231255267482));
#66891=CARTESIAN_POINT('',(0.00544219470431034,-0.0326943950436594,0.0795174098539166));
#66892=CARTESIAN_POINT('Origin',(0.0127982851832748,-0.0326395670423499,
0.0646305142286374));
#66893=CARTESIAN_POINT('Ctrl Pts',(0.00545366570760913,-0.0326773559987494,
0.0795231255237429));
#66894=CARTESIAN_POINT('Ctrl Pts',(0.00547278081855304,-0.0326267922587283,
0.0794846598271862));
#66895=CARTESIAN_POINT('Ctrl Pts',(0.00549155712796076,-0.0325756109581972,
0.0794468759073205));
#66896=CARTESIAN_POINT('Ctrl Pts',(0.00552844812344945,-0.0324719985462383,
0.0793726394646285));
#66897=CARTESIAN_POINT('Ctrl Pts',(0.00554654801342227,-0.0324196091621783,
0.0793362167162885));
#66898=CARTESIAN_POINT('Ctrl Pts',(0.00556431598453872,-0.0323666188837756,
0.0793004618944936));
#66899=CARTESIAN_POINT('',(0.00539853357837318,-0.0326943950436703,0.0793541842389197));
#66900=CARTESIAN_POINT('Origin',(0.00812378219310841,-0.0315241814719618,
0.07415));
#66901=CARTESIAN_POINT('',(0.00545366570614322,-0.0327114338380033,0.0795231255267077));
#66902=CARTESIAN_POINT('',(0.00546514888907058,-0.0326943950436593,0.079528816687218));
#66903=CARTESIAN_POINT('Origin',(0.0127573694918815,-0.0326395657042319,
0.064611043345139));
#66904=CARTESIAN_POINT('Origin',(0.0128882682879769,-0.0326395684985889,
0.0646752265085024));
#66905=CARTESIAN_POINT('Origin',(0.0129284940098363,-0.032639567221667,
0.0646960856478551));
#66906=CARTESIAN_POINT('Ctrl Pts',(0.0054210572485344,-0.0332451089994434,
0.0792267512125353));
#66907=CARTESIAN_POINT('Ctrl Pts',(0.00561253005317438,-0.0329451141710254,
0.0793286861515629));
#66908=CARTESIAN_POINT('Ctrl Pts',(0.00581113706010535,-0.0326442513127493,
0.0794159089897944));
#66909=CARTESIAN_POINT('Ctrl Pts',(0.00564423465119968,-0.0332451089994434,
0.0793394093100675));
#66910=CARTESIAN_POINT('Ctrl Pts',(0.00583995642550487,-0.0329451141710254,
0.0794329269756397));
#66911=CARTESIAN_POINT('Ctrl Pts',(0.00604216630777994,-0.0326442513127493,
0.0795114364032364));
#66912=CARTESIAN_POINT('Ctrl Pts',(0.00564646642522633,-0.0332451089994434,
0.0793405358910428));
#66913=CARTESIAN_POINT('Ctrl Pts',(0.00584223068922818,-0.0329451141710254,
0.0794339693838805));
#66914=CARTESIAN_POINT('Ctrl Pts',(0.00604447660025668,-0.0326442513127493,
0.0795123916773708));
#66915=CARTESIAN_POINT('',(0.0056768606742133,-0.0331951640388616,0.0793548727247041));
#66916=CARTESIAN_POINT('',(0.00589276669509876,-0.0328677532355027,0.0794510088584609));
#66917=CARTESIAN_POINT('Origin',(0.0121066312472922,-0.0326402808281404,
0.0638729381599424));
#66918=CARTESIAN_POINT('Origin',(0.00160438252152576,-0.0326944278779215,
0.0896414035572649));
#66919=CARTESIAN_POINT('',(0.00577808157344145,-0.0326943950436593,0.0794012678091005));
#66920=CARTESIAN_POINT('',(0.00583568762442888,-0.0326943950436694,0.0794255122495204));
#66921=CARTESIAN_POINT('',(0.00556431598451448,-0.0330220786163545,0.0793004618945359));
#66922=CARTESIAN_POINT('Origin',(0.0125610079397382,-0.0326396682764704,
0.0640300828915743));
#66923=CARTESIAN_POINT('',(0.00556492055904027,-0.0331951640388588,0.0792992452978757));
#66924=CARTESIAN_POINT('Origin',(0.000655619978475284,-0.033195202656007,
0.0891783210318515));
#66925=CARTESIAN_POINT('',(0.00562089061663679,-0.0331951640388702,0.0793270590112999));
#66926=CARTESIAN_POINT('Ctrl Pts',(0.00524510953553629,-0.0330240426238172,
0.0794143369697029));
#66927=CARTESIAN_POINT('Ctrl Pts',(0.00531763090608894,-0.0329142774063519,
0.0794539934901158));
#66928=CARTESIAN_POINT('Ctrl Pts',(0.00539100824224168,-0.0328043479726691,
0.0794921705614427));
#66929=CARTESIAN_POINT('Ctrl Pts',(0.00546514888907057,-0.0326943950436593,
0.079528816687218));
#66930=CARTESIAN_POINT('Ctrl Pts',(0.00535172449226936,-0.0330240426238172,
0.0793759392225634));
#66931=CARTESIAN_POINT('Ctrl Pts',(0.00542371689644606,-0.0329142774063519,
0.0794141270180774));
#66932=CARTESIAN_POINT('Ctrl Pts',(0.00549653463986747,-0.0328043479726691,
0.079450845567505));
#66933=CARTESIAN_POINT('Ctrl Pts',(0.00557008573303214,-0.0326943950436593,
0.0794860452625987));
#66934=CARTESIAN_POINT('Ctrl Pts',(0.00545833944900243,-0.0330240426238172,
0.079337541475424));
#66935=CARTESIAN_POINT('Ctrl Pts',(0.00552980288680317,-0.0329142774063519,
0.0793742605460391));
#66936=CARTESIAN_POINT('Ctrl Pts',(0.00560206103749325,-0.0328043479726691,
0.0794095205735674));
#66937=CARTESIAN_POINT('Ctrl Pts',(0.00567502257699371,-0.0326943950436593,
0.0794432738379793));
#66938=CARTESIAN_POINT('Ctrl Pts',(0.0055649544057355,-0.0330240426238172,
0.0792991437282845));
#66939=CARTESIAN_POINT('Ctrl Pts',(0.00563588887716028,-0.0329142774063519,
0.0793343940740007));
#66940=CARTESIAN_POINT('Ctrl Pts',(0.00570758743511903,-0.0328043479726691,
0.0793681955796297));
#66941=CARTESIAN_POINT('Ctrl Pts',(0.00577995942095528,-0.0326943950436593,
0.07940050241336));
#66942=CARTESIAN_POINT('',(0.00562161523126602,-0.0326943950436693,0.0794650422481693));
#66943=CARTESIAN_POINT('Ctrl Pts',(0.00545366570761464,-0.0327114338383316,
0.0795231255237316));
#66944=CARTESIAN_POINT('Ctrl Pts',(0.0054727776391388,-0.0327619876831034,
0.0794846662251811));
#66945=CARTESIAN_POINT('Ctrl Pts',(0.00549155239559205,-0.0328131562604465,
0.0794468854303548));
#66946=CARTESIAN_POINT('Ctrl Pts',(0.00552844335710324,-0.0329167375858767,
0.0793726490560364));
#66947=CARTESIAN_POINT('Ctrl Pts',(0.0055465448629089,-0.032969108892062,
0.0793362230561256));
#66948=CARTESIAN_POINT('Ctrl Pts',(0.00556431598453815,-0.0330220786163187,
0.0793004618944946));
#66949=CARTESIAN_POINT('Ctrl Pts',(0.00567621463213379,-0.0331951640388604,
0.0793529503216706));
#66950=CARTESIAN_POINT('Ctrl Pts',(0.00578378229421297,-0.0330306422010619,
0.0794035522117594));
#66951=CARTESIAN_POINT('Ctrl Pts',(0.00589334946981015,-0.0328657861914644,
0.0794496649782933));
#66952=CARTESIAN_POINT('Ctrl Pts',(0.00567686067421046,-0.0331951640388604,
0.0793548727247027));
#66953=CARTESIAN_POINT('Ctrl Pts',(0.00578446808073979,-0.0330306422010619,
0.0794054612582857));
#66954=CARTESIAN_POINT('Ctrl Pts',(0.00589407441478735,-0.0328657861914644,
0.079451559037047));
#66955=CARTESIAN_POINT('Ctrl Pts',(0.00578450865792718,-0.0331951640388604,
0.0796751967682374));
#66956=CARTESIAN_POINT('Ctrl Pts',(0.00589873855868392,-0.0330306422010619,
0.0797235597487747));
#66957=CARTESIAN_POINT('Ctrl Pts',(0.00601486974363614,-0.0328657861914644,
0.0797671601615587));
#66958=CARTESIAN_POINT('',(0.00579631591329893,-0.0331781648281931,0.0796801808932682));
#66959=CARTESIAN_POINT('',(0.00578450865792326,-0.0331951640388588,0.079675196768223));
#66960=CARTESIAN_POINT('Origin',(0.0115430477417567,-0.0326412091917871,
0.0641894882940049));
#66961=CARTESIAN_POINT('Ctrl Pts',(0.00579631591232129,-0.033178164828644,
0.0796801808916987));
#66962=CARTESIAN_POINT('Ctrl Pts',(0.00581298948295319,-0.033127681154679,
0.079640563589756));
#66963=CARTESIAN_POINT('Ctrl Pts',(0.00582936194936585,-0.0330765663497816,
0.0796016616404801));
#66964=CARTESIAN_POINT('Ctrl Pts',(0.00586151889002797,-0.0329730614463284,
0.0795252550865608));
#66965=CARTESIAN_POINT('Ctrl Pts',(0.00587729037851306,-0.0329207133374053,
0.0794877813505832));
#66966=CARTESIAN_POINT('Ctrl Pts',(0.00589276667883221,-0.0328677532289383,
0.079451008861069));
#66967=CARTESIAN_POINT('',(0.00573068466607828,-0.0331951640388701,0.0795150347464736));
#66968=CARTESIAN_POINT('Ctrl Pts',(0.0057451433384942,-0.0337436976235975,
0.079386430291651));
#66969=CARTESIAN_POINT('Ctrl Pts',(0.00579224058614003,-0.0336723290703325,
0.0794078241300019));
#66970=CARTESIAN_POINT('Ctrl Pts',(0.0058397150222809,-0.033601104548885,
0.0794283673762962));
#66971=CARTESIAN_POINT('Ctrl Pts',(0.00599129149272274,-0.0333736987606857,
0.079493957892326));
#66972=CARTESIAN_POINT('Ctrl Pts',(0.00614638213913415,-0.0331450831799192,
0.0795507419885182));
#66973=CARTESIAN_POINT('Ctrl Pts',(0.00597495385551883,-0.0337436976235975,
0.0794848534914815));
#66974=CARTESIAN_POINT('Ctrl Pts',(0.00602293633634038,-0.0336723290703325,
0.0795041803792137));
#66975=CARTESIAN_POINT('Ctrl Pts',(0.00607125868452036,-0.033601104548885,
0.0795226410867183));
#66976=CARTESIAN_POINT('Ctrl Pts',(0.00622554237014116,-0.0333736987606857,
0.0795815824689207));
#66977=CARTESIAN_POINT('Ctrl Pts',(0.00638295420481749,-0.0331450831799192,
0.0796315730329152));
#66978=CARTESIAN_POINT('Ctrl Pts',(0.00597725196068907,-0.0337436976235975,
0.0794858377234798));
#66979=CARTESIAN_POINT('Ctrl Pts',(0.00602524329384239,-0.0336723290703325,
0.0795051439417057));
#66980=CARTESIAN_POINT('Ctrl Pts',(0.00607357412114276,-0.033601104548885,
0.0795235838238225));
#66981=CARTESIAN_POINT('Ctrl Pts',(0.00622788487891534,-0.0333736987606857,
0.0795824587146866));
#66982=CARTESIAN_POINT('Ctrl Pts',(0.00638531992547433,-0.0331450831799192,
0.0796323813433592));
#66983=CARTESIAN_POINT('',(0.00600850577736595,-0.0336938721132548,0.079498245570746));
#66984=CARTESIAN_POINT('',(0.00623002219053035,-0.0333679869945434,0.0795806351426612));
#66985=CARTESIAN_POINT('Ctrl Pts',(0.00600850577737769,-0.0336938721132649,
0.0794982455707519));
#66986=CARTESIAN_POINT('Ctrl Pts',(0.00602938248874717,-0.0336629187933932,
0.0795065024868959));
#66987=CARTESIAN_POINT('Ctrl Pts',(0.00605030087081092,-0.033631995230104,
0.0795146345207427));
#66988=CARTESIAN_POINT('Ctrl Pts',(0.00607125868453239,-0.033601104548895,
0.0795226410867234));
#66989=CARTESIAN_POINT('Ctrl Pts',(0.00612384901051982,-0.0335235892595454,
0.0795427323004617));
#66990=CARTESIAN_POINT('Ctrl Pts',(0.00617678113087338,-0.0334458668660369,
0.0795620690291126));
#66991=CARTESIAN_POINT('Ctrl Pts',(0.00623002219042159,-0.0333679869945385,
0.0795806351429525));
#66992=CARTESIAN_POINT('Ctrl Pts',(0.00623006395440777,-0.0333679692459669,
0.0795806504347048));
#66993=CARTESIAN_POINT('Ctrl Pts',(0.00623020758797247,-0.0333391895376564,
0.079580220542604));
#66994=CARTESIAN_POINT('Ctrl Pts',(0.00623031216851744,-0.0333104081064338,
0.0795798972884828));
#66995=CARTESIAN_POINT('Ctrl Pts',(0.00623044532910061,-0.0332532698692968,
0.0795794677019095));
#66996=CARTESIAN_POINT('Ctrl Pts',(0.00623047501916999,-0.0332249173570707,
0.0795793582030702));
#66997=CARTESIAN_POINT('Ctrl Pts',(0.00623046971168589,-0.0331960985270736,
0.0795793524650619));
#66998=CARTESIAN_POINT('Ctrl Pts',(0.00623046961596248,-0.0331956312655128,
0.0795793524001691));
#66999=CARTESIAN_POINT('Ctrl Pts',(0.00623046951091808,-0.0331951640388606,
0.0795793523635382));
#67000=CARTESIAN_POINT('',(0.00611244011171099,-0.0331951640388587,0.0795381933921863));
#67001=CARTESIAN_POINT('',(0.00617145481132473,-0.0331951640388687,0.0795587728778723));
#67002=CARTESIAN_POINT('',(0.00589276668460748,-0.0335216366567672,0.0794510088470328));
#67003=CARTESIAN_POINT('Origin',(0.0112199700697491,-0.0326434571526922,
0.063671542154586));
#67004=CARTESIAN_POINT('',(0.00589329367539628,-0.0336938721132328,0.0794497566899203));
#67005=CARTESIAN_POINT('Origin',(0.00165708336615458,-0.0336938867896174,
0.0895152100896136));
#67006=CARTESIAN_POINT('',(0.00595089972639112,-0.0336938721132538,0.0794740011303432));
#67007=CARTESIAN_POINT('Ctrl Pts',(0.00600812838762901,-0.0336938721132389,
0.0794973196701799));
#67008=CARTESIAN_POINT('Ctrl Pts',(0.00603942802408733,-0.0336474569764957,
0.0795097032939517));
#67009=CARTESIAN_POINT('Ctrl Pts',(0.00607087048182631,-0.033601104548885,
0.0795217196674262));
#67010=CARTESIAN_POINT('Ctrl Pts',(0.00615047555574723,-0.0334837508592656,
0.079552142362326));
#67011=CARTESIAN_POINT('Ctrl Pts',(0.00623094716051302,-0.0333660264659097,
0.0795801928344315));
#67012=CARTESIAN_POINT('Ctrl Pts',(0.00600850577734697,-0.0336938721132389,
0.0794982455707385));
#67013=CARTESIAN_POINT('Ctrl Pts',(0.00603981083340851,-0.0336474569764957,
0.079510626985523));
#67014=CARTESIAN_POINT('Ctrl Pts',(0.00607125868452036,-0.033601104548885,
0.0795226410867183));
#67015=CARTESIAN_POINT('Ctrl Pts',(0.00615087741322139,-0.0334837508592656,
0.0795530580287297));
#67016=CARTESIAN_POINT('Ctrl Pts',(0.0062313624963011,-0.0333660264659097,
0.0795811023458535));
#67017=CARTESIAN_POINT('Ctrl Pts',(0.00613681994874161,-0.0336938721132389,
0.079813055851237));
#67018=CARTESIAN_POINT('Ctrl Pts',(0.00616996769384003,-0.0336474569764957,
0.0798246862005972));
#67019=CARTESIAN_POINT('Ctrl Pts',(0.00620324931555745,-0.033601104548885,
0.0798359277168299));
#67020=CARTESIAN_POINT('Ctrl Pts',(0.00628751072982149,-0.0334837508592656,
0.0798643886513444));
#67021=CARTESIAN_POINT('Ctrl Pts',(0.00637257849918126,-0.0333660264659097,
0.0798903402475066));
#67022=CARTESIAN_POINT('',(0.00614815156821454,-0.0336769361243754,0.079815411161953));
#67023=CARTESIAN_POINT('',(0.00613605465546666,-0.033693872113232,0.0798111782551074));
#67024=CARTESIAN_POINT('Ctrl Pts',(0.00614815156821478,-0.0336769361243751,
0.0798154111619531));
#67025=CARTESIAN_POINT('Ctrl Pts',(0.00614613451157701,-0.033679758667013,
0.0798147077780765));
#67026=CARTESIAN_POINT('Ctrl Pts',(0.00614411790686429,-0.0336825812713055,
0.0798140033436034));
#67027=CARTESIAN_POINT('Ctrl Pts',(0.00614008561141594,-0.0336882265887076,
0.0798125923775529));
#67028=CARTESIAN_POINT('Ctrl Pts',(0.00613806992066078,-0.0336910493018399,
0.0798118858460027));
#67029=CARTESIAN_POINT('Ctrl Pts',(0.0061360546554696,-0.0336938721132374,
0.0798111782551204));
#67030=CARTESIAN_POINT('Ctrl Pts',(0.00614815156821451,-0.0336769361243754,
0.079815411161953));
#67031=CARTESIAN_POINT('Ctrl Pts',(0.00616195191148716,-0.0336279031428251,
0.0797758366494754));
#67032=CARTESIAN_POINT('Ctrl Pts',(0.00617595080743692,-0.0335767852155831,
0.079735692758015));
#67033=CARTESIAN_POINT('Ctrl Pts',(0.00620338130999196,-0.0334733199122754,
0.079657031760663));
#67034=CARTESIAN_POINT('Ctrl Pts',(0.00621683133435809,-0.0334209645148399,
0.0796184618391355));
#67035=CARTESIAN_POINT('Ctrl Pts',(0.00623002218363935,-0.033367986984468,
0.0795806351402516));
#67036=CARTESIAN_POINT('',(0.00607228021642631,-0.0336938721132534,0.0796547119129367));
#67037=CARTESIAN_POINT('Origin',(0.00812378219310841,-0.0315241814719618,
0.07415));
#67038=CARTESIAN_POINT('',(0.00579631591449628,-0.0332121607144398,0.0796801808920896));
#67039=CARTESIAN_POINT('',(0.00580813378883238,-0.0331951640388587,0.079685139787558));
#67040=CARTESIAN_POINT('Origin',(0.0114988399443315,-0.0326413638235096,
0.0641793877490522));
#67041=CARTESIAN_POINT('Origin',(0.0128560347686871,-0.032641210522979,
0.0647420762614981));
#67042=CARTESIAN_POINT('Origin',(0.0128941577392383,-0.0326413654357388,
0.0647666337109076));
#67043=CARTESIAN_POINT('Ctrl Pts',(0.00558134126227887,-0.0335235895815172,
0.0795847027621829));
#67044=CARTESIAN_POINT('Ctrl Pts',(0.00565616064574541,-0.0334144449262749,
0.0796197044672014));
#67045=CARTESIAN_POINT('Ctrl Pts',(0.0057317890965029,-0.0333049234473147,
0.0796532006727838));
#67046=CARTESIAN_POINT('Ctrl Pts',(0.00580813378883215,-0.0331951640388587,
0.0796851397875581));
#67047=CARTESIAN_POINT('Ctrl Pts',(0.00568533496484918,-0.0335235895815172,
0.0795396862950656));
#67048=CARTESIAN_POINT('Ctrl Pts',(0.00575953460801659,-0.0334144449262749,
0.0795732563220234));
#67049=CARTESIAN_POINT('Ctrl Pts',(0.00583451302907715,-0.0333049234473147,
0.0796053320080887));
#67050=CARTESIAN_POINT('Ctrl Pts',(0.00591017806896196,-0.0331951640388587,
0.0796358636535905));
#67051=CARTESIAN_POINT('Ctrl Pts',(0.0057893286674195,-0.0335235895815172,
0.0794946698279483));
#67052=CARTESIAN_POINT('Ctrl Pts',(0.00586290857028777,-0.0334144449262749,
0.0795268081768454));
#67053=CARTESIAN_POINT('Ctrl Pts',(0.00593723696165139,-0.0333049234473147,
0.0795574633433936));
#67054=CARTESIAN_POINT('Ctrl Pts',(0.00601222234909177,-0.0331951640388587,
0.0795865875196228));
#67055=CARTESIAN_POINT('Ctrl Pts',(0.00589332236998982,-0.0335235895815172,
0.079449653360831));
#67056=CARTESIAN_POINT('Ctrl Pts',(0.00596628253255895,-0.0334144449262749,
0.0794803600316675));
#67057=CARTESIAN_POINT('Ctrl Pts',(0.00603996089422564,-0.0333049234473147,
0.0795095946786985));
#67058=CARTESIAN_POINT('Ctrl Pts',(0.00611426662922157,-0.0331951640388587,
0.0795373113856552));
#67059=CARTESIAN_POINT('',(0.00596028695028169,-0.0331951640388687,0.0796116665898822));
#67060=CARTESIAN_POINT('Ctrl Pts',(0.00579631591570712,-0.033212160714597,
0.0796801808891952));
#67061=CARTESIAN_POINT('Ctrl Pts',(0.00581296144826987,-0.0332625444109796,
0.0796406302383598));
#67062=CARTESIAN_POINT('Ctrl Pts',(0.0058293201521852,-0.0333135300746914,
0.0796017611073038));
#67063=CARTESIAN_POINT('Ctrl Pts',(0.00586147688804284,-0.0334167203140563,
0.0795253550309514));
#67064=CARTESIAN_POINT('Ctrl Pts',(0.0058772624654211,-0.0334688847587242,
0.0794878476783467));
#67065=CARTESIAN_POINT('Ctrl Pts',(0.00589276668502568,-0.0335216366562311,
0.0794510088464411));
#67066=CARTESIAN_POINT('Origin',(0.00812378219310841,-0.0315241814719618,
0.07415));
#67067=CARTESIAN_POINT('',(0.00614815156864569,-0.0337108120655533,0.0798154111607359));
#67068=CARTESIAN_POINT('',(0.00616025749492669,-0.0336938721132327,0.0798196182199215));
#67069=CARTESIAN_POINT('Origin',(0.0125907192491432,-0.0345562507698484,
0.0647345707538487));
#67070=CARTESIAN_POINT('Ctrl Pts',(0.00616025749492479,-0.0336938721132337,
0.0798196182199231));
#67071=CARTESIAN_POINT('Ctrl Pts',(0.00615823923547568,-0.0336910493161011,
0.0798189192482954));
#67072=CARTESIAN_POINT('Ctrl Pts',(0.00615622128614975,-0.0336882265958383,
0.0798182191771287));
#67073=CARTESIAN_POINT('Ctrl Pts',(0.00615218598084661,-0.0336825812713121,
0.0798168168259064));
#67074=CARTESIAN_POINT('Ctrl Pts',(0.00615016862485449,-0.0336797586670165,
0.0798161145458304));
#67075=CARTESIAN_POINT('Ctrl Pts',(0.00614815156821449,-0.0336769361243755,
0.079815411161953));
#67076=CARTESIAN_POINT('Origin',(0.0104801540985315,-0.0345562519801551,
0.0639985831636916));
#67077=CARTESIAN_POINT('Ctrl Pts',(0.00607858695488061,-0.0342436276873911,
0.0795254349998424));
#67078=CARTESIAN_POINT('Ctrl Pts',(0.00628132482807593,-0.033943005420181,
0.0796025708098521));
#67079=CARTESIAN_POINT('Ctrl Pts',(0.00648929692949157,-0.0336441434784052,
0.0796642164378105));
#67080=CARTESIAN_POINT('Ctrl Pts',(0.00631412328481066,-0.0342436276873911,
0.0796092361769408));
#67081=CARTESIAN_POINT('Ctrl Pts',(0.00652002177150363,-0.033943005420181,
0.0796774885878225));
#67082=CARTESIAN_POINT('Ctrl Pts',(0.00673047637342439,-0.0336441434784052,
0.0797300379830996));
#67083=CARTESIAN_POINT('Ctrl Pts',(0.00631647864810996,-0.0342436276873911,
0.0796100741887117));
#67084=CARTESIAN_POINT('Ctrl Pts',(0.0065224087409379,-0.033943005420181,
0.0796782377656022));
#67085=CARTESIAN_POINT('Ctrl Pts',(0.00673288816786372,-0.0336441434784052,
0.0797306961985525));
#67086=CARTESIAN_POINT('',(0.00634849891012578,-0.0341934961088741,0.0796205113348903));
#67087=CARTESIAN_POINT('',(0.00657475148961899,-0.0338664212863112,0.079688829198174));
#67088=CARTESIAN_POINT('Origin',(0.0119963837668672,-0.0345610720404866,
0.0638675896884594));
#67089=CARTESIAN_POINT('Origin',(0.00362121447950633,-0.0336938005073021,
0.0902498586722073));
#67090=CARTESIAN_POINT('',(0.00645473649828104,-0.0336938721132327,0.0796538542375847));
#67091=CARTESIAN_POINT('',(0.00651492694246293,-0.0336938721132427,0.0796706875507087));
#67092=CARTESIAN_POINT('',(0.00623002218363433,-0.0340203938281605,0.07958063514025));
#67093=CARTESIAN_POINT('Origin',(0.0124188840229564,-0.0345589643243816,
0.0640978727049483));
#67094=CARTESIAN_POINT('',(0.00623046951091836,-0.034193496108874,0.0795793523635383));
#67095=CARTESIAN_POINT('Origin',(0.00260207576277473,-0.0341934220717541,
0.0899843020048005));
#67096=CARTESIAN_POINT('',(0.00628948421053207,-0.0341934961088841,0.0795999318492243));
#67097=CARTESIAN_POINT('Ctrl Pts',(0.00592760345228274,-0.0340223579322396,
0.0797336188031044));
#67098=CARTESIAN_POINT('Ctrl Pts',(0.00600461611826673,-0.0339125849573575,
0.079763909835815));
#67099=CARTESIAN_POINT('Ctrl Pts',(0.00608220162233248,-0.0338030433565231,
0.0797925856001345));
#67100=CARTESIAN_POINT('Ctrl Pts',(0.00616025749492674,-0.0336938721132327,
0.0798196182199215));
#67101=CARTESIAN_POINT('Ctrl Pts',(0.00602856539201688,-0.0340223579322396,
0.0796821613784168));
#67102=CARTESIAN_POINT('Ctrl Pts',(0.00610486832590783,-0.0339125849573575,
0.0797110598826587));
#67103=CARTESIAN_POINT('Ctrl Pts',(0.00618171577449755,-0.0338030433565231,
0.0797383587868282));
#67104=CARTESIAN_POINT('Ctrl Pts',(0.00625900636816637,-0.0336938721132327,
0.0797640318918879));
#67105=CARTESIAN_POINT('Ctrl Pts',(0.00612952733175102,-0.0340223579322396,
0.0796307039537292));
#67106=CARTESIAN_POINT('Ctrl Pts',(0.00620512053354894,-0.0339125849573575,
0.0796582099295023));
#67107=CARTESIAN_POINT('Ctrl Pts',(0.00628122992666263,-0.0338030433565231,
0.0796841319735219));
#67108=CARTESIAN_POINT('Ctrl Pts',(0.00635775524140601,-0.0336938721132327,
0.0797084455638543));
#67109=CARTESIAN_POINT('Ctrl Pts',(0.00623048927148517,-0.0340223579322396,
0.0795792465290416));
#67110=CARTESIAN_POINT('Ctrl Pts',(0.00630537274119004,-0.0339125849573575,
0.079605359976346));
#67111=CARTESIAN_POINT('Ctrl Pts',(0.0063807440788277,-0.0338030433565231,
0.0796299051602156));
#67112=CARTESIAN_POINT('Ctrl Pts',(0.00645650411464565,-0.0336938721132327,
0.0796528592358206));
#67113=CARTESIAN_POINT('',(0.00630749699661386,-0.0336938721132427,0.0797367362287631));
#67114=CARTESIAN_POINT('Ctrl Pts',(0.00614815156982787,-0.0337108120662688,
0.0798154111573263));
#67115=CARTESIAN_POINT('Ctrl Pts',(0.00616231001104801,-0.0337611408994286,
0.0797748097463572));
#67116=CARTESIAN_POINT('Ctrl Pts',(0.00617621009212749,-0.0338121088781288,
0.0797349492210609));
#67117=CARTESIAN_POINT('Ctrl Pts',(0.00620350619675928,-0.0339153382773237,
0.0796566736295054));
#67118=CARTESIAN_POINT('Ctrl Pts',(0.00621689067238685,-0.0339675558473111,
0.0796182916786175));
#67119=CARTESIAN_POINT('Ctrl Pts',(0.00623002218365246,-0.0340203938281304,
0.0795806351402141));
#67120=CARTESIAN_POINT('Ctrl Pts',(0.00634761698076121,-0.0341934961088741,
0.0796186849771815));
#67121=CARTESIAN_POINT('Ctrl Pts',(0.00646067773436962,-0.0340287516182427,
0.0796554057936628));
#67122=CARTESIAN_POINT('Ctrl Pts',(0.00657515957893013,-0.033864463327595,
0.0796874223461877));
#67123=CARTESIAN_POINT('Ctrl Pts',(0.00634849891012574,-0.0341934961088741,
0.0796205113348903));
#67124=CARTESIAN_POINT('Ctrl Pts',(0.00646159742224096,-0.0340287516182427,
0.0796572139181767));
#67125=CARTESIAN_POINT('Ctrl Pts',(0.00657611623945257,-0.033864463327595,
0.079689210692499));
#67126=CARTESIAN_POINT('Ctrl Pts',(0.00649544530550296,-0.0341934961088741,
0.0799248176577804));
#67127=CARTESIAN_POINT('Ctrl Pts',(0.00661483511110781,-0.0340287516182427,
0.0799584822401085));
#67128=CARTESIAN_POINT('Ctrl Pts',(0.00673551428313467,-0.033864463327595,
0.0799871835854533));
#67129=CARTESIAN_POINT('',(0.00650778413357308,-0.0341764758832424,0.0799282826395307));
#67130=CARTESIAN_POINT('',(0.00649544530549579,-0.034193496108874,0.0799248176577655));
#67131=CARTESIAN_POINT('Origin',(0.0114605081543549,-0.0345621026563146,
0.0641203147158454));
#67132=CARTESIAN_POINT('Ctrl Pts',(0.00650778413225823,-0.034176475883753,
0.079928282638261));
#67133=CARTESIAN_POINT('Ctrl Pts',(0.00651934507087322,-0.0341260050040351,
0.079886944436816));
#67134=CARTESIAN_POINT('Ctrl Pts',(0.00653070501630605,-0.0340749269147945,
0.0798463247805428));
#67135=CARTESIAN_POINT('Ctrl Pts',(0.00655303190152458,-0.0339715436305775,
0.0797664911270974));
#67136=CARTESIAN_POINT('Ctrl Pts',(0.00656399037672683,-0.0339192778237867,
0.0797273074187317));
#67137=CARTESIAN_POINT('Ctrl Pts',(0.00657475148779686,-0.0338664212855678,
0.0796888291986856));
#67138=CARTESIAN_POINT('',(0.00642197210782079,-0.0341934961088841,0.0797726644963379));
#67139=CARTESIAN_POINT('Origin',(0.00812378219310841,-0.0315241814719618,
0.07415));
#67140=CARTESIAN_POINT('',(0.00650778413458173,-0.034210518019035,0.0799282826390478));
#67141=CARTESIAN_POINT('',(0.00652013033595573,-0.034193496108874,0.079931721259373));
#67142=CARTESIAN_POINT('Origin',(0.011418557203585,-0.0345621698369096,
0.0641031448877212));
#67143=CARTESIAN_POINT('Origin',(0.010474156061617,-0.0345621043539572,
0.063844460519104));
#67144=CARTESIAN_POINT('Origin',(0.0105189261518166,-0.0345621712241411,
0.0638515515515507));
#67145=CARTESIAN_POINT('Ctrl Pts',(0.00645329191808031,-0.0346945769586966,
0.0796534502354016));
#67146=CARTESIAN_POINT('Ctrl Pts',(0.00656856388672206,-0.0345275153362944,
0.0796884393230398));
#67147=CARTESIAN_POINT('Ctrl Pts',(0.00668496604520018,-0.0343603235965185,
0.0797198122633351));
#67148=CARTESIAN_POINT('Ctrl Pts',(0.00680215274854109,-0.034193496108874,
0.0797474813857446));
#67149=CARTESIAN_POINT('Ctrl Pts',(0.00653402737037455,-0.0346945769586966,
0.0796760293202807));
#67150=CARTESIAN_POINT('Ctrl Pts',(0.00664977226698927,-0.0345275153362944,
0.079709327371546));
#67151=CARTESIAN_POINT('Ctrl Pts',(0.00676659429422632,-0.0343603235965185,
0.0797389939649302));
#67152=CARTESIAN_POINT('Ctrl Pts',(0.00688414664033257,-0.034193496108874,
0.0797649464949634));
#67153=CARTESIAN_POINT('Ctrl Pts',(0.0066147628226688,-0.0346945769586966,
0.0796986084051599));
#67154=CARTESIAN_POINT('Ctrl Pts',(0.00673098064725648,-0.0345275153362944,
0.0797302154200521));
#67155=CARTESIAN_POINT('Ctrl Pts',(0.00684822254325245,-0.0343603235965185,
0.0797581756665252));
#67156=CARTESIAN_POINT('Ctrl Pts',(0.00696614053212405,-0.034193496108874,
0.0797824116041821));
#67157=CARTESIAN_POINT('Ctrl Pts',(0.00669549827496304,-0.0346945769586966,
0.079721187490039));
#67158=CARTESIAN_POINT('Ctrl Pts',(0.00681218902752369,-0.0345275153362944,
0.0797511034685582));
#67159=CARTESIAN_POINT('Ctrl Pts',(0.00692985079227859,-0.0343603235965185,
0.0797773573681202));
#67160=CARTESIAN_POINT('Ctrl Pts',(0.00704813442391553,-0.034193496108874,
0.0797998767134009));
#67161=CARTESIAN_POINT('',(0.00669549827497416,-0.0346945769586966,0.079721187490042));
#67162=CARTESIAN_POINT('',(0.00692559410958799,-0.0343667727831515,0.0797751640257857));
#67163=CARTESIAN_POINT('Origin',(0.0106934814914887,-0.034562645706343,
0.0633898257144464));
#67164=CARTESIAN_POINT('Origin',(0.00462308388846954,-0.0341934771029066,
0.0905848402985495));
#67165=CARTESIAN_POINT('',(0.00680361984569412,-0.034193496108874,0.0797477938847791));
#67166=CARTESIAN_POINT('',(0.00686474849025947,-0.034193496108884,0.0797608145919446));
#67167=CARTESIAN_POINT('',(0.00657475148826711,-0.0345211942962637,0.07968882919717));
#67168=CARTESIAN_POINT('Origin',(0.0111556302912778,-0.0345625596120658,
0.0635225256653779));
#67169=CARTESIAN_POINT('',(0.00657511738662482,-0.0346945769586885,0.0796875208638126));
#67170=CARTESIAN_POINT('Origin',(0.00359533271229314,-0.0346945685853929,
0.0903422568304037));
#67171=CARTESIAN_POINT('',(0.00663530783080949,-0.0346945769587026,0.0797043541769372));
#67172=CARTESIAN_POINT('Ctrl Pts',(0.00628253635060995,-0.0345231616327842,
0.0798605003062357));
#67173=CARTESIAN_POINT('Ctrl Pts',(0.00636124755759006,-0.0344132092796988,
0.0798858792879077));
#67174=CARTESIAN_POINT('Ctrl Pts',(0.00644047964765093,-0.034303273855898,
0.0799096288809111));
#67175=CARTESIAN_POINT('Ctrl Pts',(0.00652013033595567,-0.034193496108874,
0.079931721259373));
#67176=CARTESIAN_POINT('Ctrl Pts',(0.00638006785141206,-0.0345231616327842,
0.0798028050508859));
#67177=CARTESIAN_POINT('Ctrl Pts',(0.00645798381052559,-0.0344132092796988,
0.0798268396981327));
#67178=CARTESIAN_POINT('Ctrl Pts',(0.00653639288725383,-0.034303273855898,
0.0798492614751472));
#67179=CARTESIAN_POINT('Ctrl Pts',(0.00661519389470903,-0.034193496108874,
0.0798700442301341));
#67180=CARTESIAN_POINT('Ctrl Pts',(0.00647759935221417,-0.0345231616327842,
0.0797451097955361));
#67181=CARTESIAN_POINT('Ctrl Pts',(0.00655472006346112,-0.0344132092796988,
0.0797678001083577));
#67182=CARTESIAN_POINT('Ctrl Pts',(0.00663230612685673,-0.034303273855898,
0.0797888940693834));
#67183=CARTESIAN_POINT('Ctrl Pts',(0.00671025745346239,-0.034193496108874,
0.0798083672008952));
#67184=CARTESIAN_POINT('Ctrl Pts',(0.00657513085301627,-0.0345231616327842,
0.0796874145401863));
#67185=CARTESIAN_POINT('Ctrl Pts',(0.00665145631639665,-0.0344132092796988,
0.0797087605185827));
#67186=CARTESIAN_POINT('Ctrl Pts',(0.00672821936645963,-0.034303273855898,
0.0797285266636195));
#67187=CARTESIAN_POINT('Ctrl Pts',(0.00680532101221575,-0.034193496108874,
0.0797466901716563));
#67188=CARTESIAN_POINT('',(0.00666187509083492,-0.0341934961088839,0.079839757572086));
#67189=CARTESIAN_POINT('Ctrl Pts',(0.00650778413550785,-0.0342105180195384,
0.0799282826357127));
#67190=CARTESIAN_POINT('Ctrl Pts',(0.00651935808409803,-0.0342610556241207,
0.0798868979658173));
#67191=CARTESIAN_POINT('Ctrl Pts',(0.00653072434416499,-0.0343122189869959,
0.0798462559224256));
#67192=CARTESIAN_POINT('Ctrl Pts',(0.0065530514506996,-0.0344158119695109,
0.0797664214626082));
#67193=CARTESIAN_POINT('Ctrl Pts',(0.00656400316521219,-0.0344681990449993,
0.079727261699079));
#67194=CARTESIAN_POINT('Ctrl Pts',(0.00657475148826946,-0.0345211942962403,
0.0796888291971384));
#67195=CARTESIAN_POINT('Ctrl Pts',(0.00669450365152847,-0.0346945769586932,
0.0797194205457717));
#67196=CARTESIAN_POINT('Ctrl Pts',(0.00680964748051673,-0.034529677707698,
0.0797489698682939));
#67197=CARTESIAN_POINT('Ctrl Pts',(0.00692591422119528,-0.034364806625142,
0.0797737349410289));
#67198=CARTESIAN_POINT('Ctrl Pts',(0.0066954982749654,-0.0346945769586932,
0.0797211874900396));
#67199=CARTESIAN_POINT('Ctrl Pts',(0.00681067863427614,-0.034529677707698,
0.079750716249426));
#67200=CARTESIAN_POINT('Ctrl Pts',(0.00692698102416918,-0.034364806625142,
0.0797754592667644));
#67201=CARTESIAN_POINT('Ctrl Pts',(0.00686126225730843,-0.0346945769586932,
0.0800156664934055));
#67202=CARTESIAN_POINT('Ctrl Pts',(0.00698253076164711,-0.034529677707698,
0.0800417681997477));
#67203=CARTESIAN_POINT('Ctrl Pts',(0.00710477445107272,-0.034364806625142,
0.0800628354637875));
#67204=CARTESIAN_POINT('',(0.00687379430557909,-0.0346775396665011,0.0800183498766304));
#67205=CARTESIAN_POINT('',(0.00686126225730344,-0.0346945769586886,0.0800156664933914));
#67206=CARTESIAN_POINT('Origin',(0.0101829135396672,-0.0345626617741161,
0.0637498947265812));
#67207=CARTESIAN_POINT('Ctrl Pts',(0.00687379430425578,-0.0346775396670097,
0.0800183498753647));
#67208=CARTESIAN_POINT('Ctrl Pts',(0.00688274382668006,-0.0346269749928203,
0.0799763342633121));
#67209=CARTESIAN_POINT('Ctrl Pts',(0.00689153426098909,-0.0345757902890825,
0.0799350653549555));
#67210=CARTESIAN_POINT('Ctrl Pts',(0.00690880436139023,-0.0344721681087976,
0.0798539869941608));
#67211=CARTESIAN_POINT('Ctrl Pts',(0.0069172772623034,-0.0344197714289672,
0.0798142093294302));
#67212=CARTESIAN_POINT('Ctrl Pts',(0.00692559410932243,-0.0343667727830727,
0.0797751640258361));
#67213=CARTESIAN_POINT('',(0.0067783802661488,-0.0346945769587026,0.0798684269917267));
#67214=CARTESIAN_POINT('Origin',(0.00812378219310841,-0.0315241814719618,
0.07415));
#67215=CARTESIAN_POINT('',(0.00687379430654705,-0.0347116136489777,0.0800183498756309));
#67216=CARTESIAN_POINT('',(0.00688633205822579,-0.034694576958689,0.0800210064864313));
#67217=CARTESIAN_POINT('Origin',(0.0101382425443413,-0.0345626675611879,
0.0637422868206545));
#67218=CARTESIAN_POINT('Origin',(0.0104816443016738,-0.0345626636336016,
0.0638135220613863));
#67219=CARTESIAN_POINT('Origin',(0.0105255369531395,-0.0345626690763649,
0.0638247862753589));
#67220=CARTESIAN_POINT('Ctrl Pts',(0.0067660446236618,-0.0352450361874069,
0.0797388559936841));
#67221=CARTESIAN_POINT('Ctrl Pts',(0.00697683178632017,-0.0349452760959493,
0.0797900639063986));
#67222=CARTESIAN_POINT('Ctrl Pts',(0.00719087731434947,-0.034644428984174,
0.0798252489912614));
#67223=CARTESIAN_POINT('Ctrl Pts',(0.00676851087054738,-0.0352450361874069,
0.0797393975205065));
#67224=CARTESIAN_POINT('Ctrl Pts',(0.006979318457225,-0.0349452760959493,
0.0797905124171933));
#67225=CARTESIAN_POINT('Ctrl Pts',(0.00719337734490327,-0.034644428984174,
0.0798256032118566));
#67226=CARTESIAN_POINT('Ctrl Pts',(0.00701269373050567,-0.0352450361874069,
0.0797930140375753));
#67227=CARTESIAN_POINT('Ctrl Pts',(0.00722552349730697,-0.0349452760959493,
0.0798349194265778));
#67228=CARTESIAN_POINT('Ctrl Pts',(0.00744090512250706,-0.034644428984174,
0.0798606745579176));
#67229=CARTESIAN_POINT('Ctrl Pts',(0.00701513555910525,-0.0352450361874069,
0.079793550202746));
#67230=CARTESIAN_POINT('Ctrl Pts',(0.00722798554770779,-0.0349452760959493,
0.0798353634966716));
#67231=CARTESIAN_POINT('Ctrl Pts',(0.00744338040028309,-0.034644428984174,
0.0798610252713782));
#67232=CARTESIAN_POINT('',(0.00704810219230022,-0.0351951634053299,0.0797998729931193));
#67233=CARTESIAN_POINT('',(0.00728116543148293,-0.0348678972925388,0.0798392989017126));
#67234=CARTESIAN_POINT('Origin',(0.00931659888056036,-0.0345628965653863,
0.0632090899675132));
#67235=CARTESIAN_POINT('Origin',(0.00566228227765515,-0.0346946199340971,
0.0907699076031147));
#67236=CARTESIAN_POINT('',(0.00715771325306242,-0.0346945769330289,0.079819641593722));
#67237=CARTESIAN_POINT('',(0.00721953885972381,-0.0346945769458128,0.0798287983097628));
#67238=CARTESIAN_POINT('',(0.00692559410936888,-0.0350221583435276,0.0797751640256961));
#67239=CARTESIAN_POINT('Origin',(0.00979758133306995,-0.0345628458716864,
0.0632382464995736));
#67240=CARTESIAN_POINT('',(0.00692584883293436,-0.0351951360298761,0.0797739536502795));
#67241=CARTESIAN_POINT('Origin',(0.00463025283431429,-0.0351951838366627,
0.0905511556451489));
#67242=CARTESIAN_POINT('',(0.00704813442389201,-0.0351951371328747,0.0797998767135148));
#67243=CARTESIAN_POINT('Ctrl Pts',(0.0066447358407554,-0.0350241211494343,
0.0799648449581764));
#67244=CARTESIAN_POINT('Ctrl Pts',(0.00672483294587503,-0.0349144232818962,
0.0799852182152474));
#67245=CARTESIAN_POINT('Ctrl Pts',(0.00680539912275446,-0.0348045283579412,
0.0800039480022977));
#67246=CARTESIAN_POINT('Ctrl Pts',(0.00688633206909981,-0.0346945769439157,
0.0800210064887231));
#67247=CARTESIAN_POINT('Ctrl Pts',(0.00673845218083138,-0.0350241211494343,
0.0799011394685713));
#67248=CARTESIAN_POINT('Ctrl Pts',(0.00681767176895197,-0.0349144232818962,
0.079920221821483));
#67249=CARTESIAN_POINT('Ctrl Pts',(0.00689733321968474,-0.0348045283579412,
0.079937678070609));
#67250=CARTESIAN_POINT('Ctrl Pts',(0.00697733532887279,-0.0346945769439157,
0.0799534820597085));
#67251=CARTESIAN_POINT('Ctrl Pts',(0.00683216852090737,-0.0350241211494343,
0.0798374339789663));
#67252=CARTESIAN_POINT('Ctrl Pts',(0.00691051059202892,-0.0349144232818962,
0.0798552254277186));
#67253=CARTESIAN_POINT('Ctrl Pts',(0.00698926731661502,-0.0348045283579412,
0.0798714081389203));
#67254=CARTESIAN_POINT('Ctrl Pts',(0.00706833858864577,-0.0346945769439157,
0.0798859576306939));
#67255=CARTESIAN_POINT('Ctrl Pts',(0.00692588486098336,-0.0350241211494343,
0.0797737284893613));
#67256=CARTESIAN_POINT('Ctrl Pts',(0.00700334941510587,-0.0349144232818962,
0.0797902290339543));
#67257=CARTESIAN_POINT('Ctrl Pts',(0.00708120141354529,-0.0348045283579412,
0.0798051382072316));
#67258=CARTESIAN_POINT('Ctrl Pts',(0.00715934184841875,-0.0346945769439157,
0.0798184332016793));
#67259=CARTESIAN_POINT('',(0.00702202265534713,-0.0346945769458131,0.0799203240401144));
#67260=CARTESIAN_POINT('Ctrl Pts',(0.00687379430722754,-0.0347116136492789,
0.0800183498724067));
#67261=CARTESIAN_POINT('Ctrl Pts',(0.00688274028816434,-0.034762154653045,
0.0799763509485115));
#67262=CARTESIAN_POINT('Ctrl Pts',(0.0068915289745913,-0.0348133084093162,
0.0799350904791837));
#67263=CARTESIAN_POINT('Ctrl Pts',(0.00690879909330109,-0.0349168561546272,
0.0798540120142869));
#67264=CARTESIAN_POINT('Ctrl Pts',(0.00691727367530838,-0.0349692089019536,
0.0798142261788806));
#67265=CARTESIAN_POINT('Ctrl Pts',(0.00692559410939604,-0.0350221583435,
0.0797751640256645));
#67266=CARTESIAN_POINT('Ctrl Pts',(0.00704733813404601,-0.0351951371254917,
0.0797986493821031));
#67267=CARTESIAN_POINT('Ctrl Pts',(0.00712512912923097,-0.035085624873602,
0.0798134737496555));
#67268=CARTESIAN_POINT('Ctrl Pts',(0.0072032903487341,-0.0349758427080718,
0.0798267026399164));
#67269=CARTESIAN_POINT('Ctrl Pts',(0.00728172272318351,-0.0348659306897824,
0.0798383132388551));
#67270=CARTESIAN_POINT('Ctrl Pts',(0.00709208990104423,-0.0351951371254917,
0.0798676258273673));
#67271=CARTESIAN_POINT('Ctrl Pts',(0.00717083081291874,-0.035085624873602,
0.0798818338910469));
#67272=CARTESIAN_POINT('Ctrl Pts',(0.00724992999223989,-0.0349758427080718,
0.0798944263402952));
#67273=CARTESIAN_POINT('Ctrl Pts',(0.00732928712096993,-0.0348659306897824,
0.0799053811053336));
#67274=CARTESIAN_POINT('Ctrl Pts',(0.00713684166804246,-0.0351951371254917,
0.0799366022726316));
#67275=CARTESIAN_POINT('Ctrl Pts',(0.0072165324966065,-0.035085624873602,
0.0799501940324382));
#67276=CARTESIAN_POINT('Ctrl Pts',(0.00729656963574569,-0.0349758427080718,
0.079962150040674));
#67277=CARTESIAN_POINT('Ctrl Pts',(0.00737685151875635,-0.0348659306897824,
0.0799724489718121));
#67278=CARTESIAN_POINT('Ctrl Pts',(0.00718159343504069,-0.0351951371254917,
0.0800055787178959));
#67279=CARTESIAN_POINT('Ctrl Pts',(0.00726223418029427,-0.035085624873602,
0.0800185541738295));
#67280=CARTESIAN_POINT('Ctrl Pts',(0.00734320927925149,-0.0349758427080718,
0.0800298737410528));
#67281=CARTESIAN_POINT('Ctrl Pts',(0.00742441591654277,-0.0348659306897824,
0.0800395168382905));
#67282=CARTESIAN_POINT('Origin',(0.00650201229109275,-0.0308609197410636,
0.0851000951589266));
#67283=CARTESIAN_POINT('',(0.00710631954366105,-0.0351951371254917,0.0798895581493945));
#67284=CARTESIAN_POINT('Origin',(0.00812538052117974,-0.0351840467441193,
0.0731728904387266));
#67285=CARTESIAN_POINT('Origin',(0.00716077028536051,-0.0352322613422822,
0.086076488883645));
#67286=CARTESIAN_POINT('',(0.00751593503015258,-0.0351951142564676,0.0798691202478984));
#67287=CARTESIAN_POINT('',(0.00764017649173142,-0.0351951372916787,0.0798796269970737));
#67288=CARTESIAN_POINT('Origin',(0.00842780899661044,-0.0352875115375133,
0.0739965727786824));
#67289=CARTESIAN_POINT('Origin',(0.000906496639794719,-0.0298325076523213,
0.0720991515120198));
#67290=CARTESIAN_POINT('Origin',(0.00432725982884279,-0.0338733733910703,
0.0816220350393757));
#67291=CARTESIAN_POINT('Ctrl Pts',(0.0042701248194806,-0.0321934096636942,
0.0784193630194674));
#67292=CARTESIAN_POINT('Ctrl Pts',(0.00434654438445685,-0.0320508460843789,
0.0784883416513423));
#67293=CARTESIAN_POINT('Ctrl Pts',(0.00442475964856207,-0.0319086045662002,
0.0785552150301777));
#67294=CARTESIAN_POINT('Ctrl Pts',(0.00450459034641189,-0.0317669892866302,
0.0786198530304804));
#67295=CARTESIAN_POINT('Ctrl Pts',(0.00433357358420958,-0.0321934096636942,
0.0784741780437055));
#67296=CARTESIAN_POINT('Ctrl Pts',(0.00441097431201675,-0.0320508460843789,
0.0785420209729062));
#67297=CARTESIAN_POINT('Ctrl Pts',(0.00449013948506295,-0.0319086045662002,
0.0786077331434814));
#67298=CARTESIAN_POINT('Ctrl Pts',(0.00457088699848174,-0.0317669892866302,
0.0786711870986076));
#67299=CARTESIAN_POINT('Ctrl Pts',(0.00439702234893855,-0.0321934096636942,
0.0785289930679436));
#67300=CARTESIAN_POINT('Ctrl Pts',(0.00447540423957666,-0.0320508460843789,
0.07859570029447));
#67301=CARTESIAN_POINT('Ctrl Pts',(0.00455551932156381,-0.0319086045662002,
0.0786602512567852));
#67302=CARTESIAN_POINT('Ctrl Pts',(0.00463718365055159,-0.0317669892866302,
0.0787225211667348));
#67303=CARTESIAN_POINT('Ctrl Pts',(0.00446047111366753,-0.0321934096636942,
0.0785838080921818));
#67304=CARTESIAN_POINT('Ctrl Pts',(0.00453983416713657,-0.0320508460843789,
0.0786493796160338));
#67305=CARTESIAN_POINT('Ctrl Pts',(0.00462089915806469,-0.0319086045662002,
0.078712769370089));
#67306=CARTESIAN_POINT('Ctrl Pts',(0.00470348030262144,-0.0317669892866302,
0.0787738552348621));
#67307=CARTESIAN_POINT('',(0.00445933600272986,-0.0321934096636942,0.0785828274405644));
#67308=CARTESIAN_POINT('',(0.00464455084779424,-0.0318665617511316,0.0787296369108196));
#67309=CARTESIAN_POINT('Origin',(0.0155726506501712,-0.0326371944419261,
0.0661043602921911));
#67310=CARTESIAN_POINT('Origin',(-0.00198631738476063,-0.0316939261508961,
0.0874577052339979));
#67311=CARTESIAN_POINT('',(0.00436408889973575,-0.0320197221621755,0.0785022747507831));
#67312=CARTESIAN_POINT('Ctrl Pts',(0.00436419340266429,-0.0320197392094673,
0.0785024273745623));
#67313=CARTESIAN_POINT('Ctrl Pts',(0.00438633998309954,-0.0319792716575971,
0.0785215573354824));
#67314=CARTESIAN_POINT('Ctrl Pts',(0.00440873322232175,-0.0319386439829625,
0.0785406055466512));
#67315=CARTESIAN_POINT('Ctrl Pts',(0.00443140210882574,-0.0318979099381557,
0.078559585562952));
#67316=CARTESIAN_POINT('Ctrl Pts',(0.00445407054726213,-0.0318571766984879,
0.0785785652040986));
#67317=CARTESIAN_POINT('Ctrl Pts',(0.00447689826249396,-0.031816387183355,
0.0785973815522193));
#67318=CARTESIAN_POINT('Ctrl Pts',(0.00449980449695246,-0.0317755399638304,
0.0786159726039175));
#67319=CARTESIAN_POINT('',(0.00436474667057906,-0.0321934096636182,0.0785011092769962));
#67320=CARTESIAN_POINT('Origin',(0.00287114878390623,-0.0324113699142621,
0.0802621419685801));
#67321=CARTESIAN_POINT('',(0.00441204133666445,-0.0321934096636662,0.0785419683587903));
#67322=CARTESIAN_POINT('Ctrl Pts',(0.0044591883271136,-0.0321934096636618,
0.0785808046011513));
#67323=CARTESIAN_POINT('Ctrl Pts',(0.00452029257573062,-0.0320835708272592,
0.0786313422065808));
#67324=CARTESIAN_POINT('Ctrl Pts',(0.00458240725451797,-0.0319739230346488,
0.0786805859488959));
#67325=CARTESIAN_POINT('Ctrl Pts',(0.00464544805667624,-0.0318646057455573,
0.0787284789233544));
#67326=CARTESIAN_POINT('Ctrl Pts',(0.00446743911033446,-0.0321934096636618,
0.0786938226941353));
#67327=CARTESIAN_POINT('Ctrl Pts',(0.00453010196653488,-0.0320835708272592,
0.0787442465148339));
#67328=CARTESIAN_POINT('Ctrl Pts',(0.0045937719940808,-0.0319739230346488,
0.0787933442831149));
#67329=CARTESIAN_POINT('Ctrl Pts',(0.00465836291054557,-0.0318646057455573,
0.0788410594337238));
#67330=CARTESIAN_POINT('Ctrl Pts',(0.00447568989355532,-0.0321934096636618,
0.0788068407871193));
#67331=CARTESIAN_POINT('Ctrl Pts',(0.00453991135733915,-0.0320835708272592,
0.078857150823087));
#67332=CARTESIAN_POINT('Ctrl Pts',(0.00460513673364362,-0.0319739230346488,
0.078906102617334));
#67333=CARTESIAN_POINT('Ctrl Pts',(0.00467127776441489,-0.0318646057455573,
0.0789536399440932));
#67334=CARTESIAN_POINT('Ctrl Pts',(0.00448394067677619,-0.0321934096636618,
0.0789198588801033));
#67335=CARTESIAN_POINT('Ctrl Pts',(0.00454972074814341,-0.0320835708272592,
0.07897005513134));
#67336=CARTESIAN_POINT('Ctrl Pts',(0.00461650147320646,-0.0319739230346488,
0.079018860951553));
#67337=CARTESIAN_POINT('Ctrl Pts',(0.00468419261828422,-0.0318646057455573,
0.0790662204544626));
#67338=CARTESIAN_POINT('',(0.00449413748547113,-0.0321763980308493,0.0789276227638977));
#67339=CARTESIAN_POINT('',(0.00448394067680125,-0.0321934096636184,0.0789198588801103));
#67340=CARTESIAN_POINT('Origin',(0.0149861426078369,-0.032638623058885,
0.0661313765646252));
#67341=CARTESIAN_POINT('Ctrl Pts',(0.00449413748738438,-0.0321763980306348,
0.0789276227613674));
#67342=CARTESIAN_POINT('Ctrl Pts',(0.00452010087637376,-0.0321259596176119,
0.0788934477144262));
#67343=CARTESIAN_POINT('Ctrl Pts',(0.00454561441595596,-0.032074916463399,
0.0788598647945113));
#67344=CARTESIAN_POINT('Ctrl Pts',(0.0045957623290327,-0.031971605779397,
0.0787938561819953));
#67345=CARTESIAN_POINT('Ctrl Pts',(0.00462037716303247,-0.0319193786690168,
0.0787614562088084));
#67346=CARTESIAN_POINT('Ctrl Pts',(0.00464455084890938,-0.0318665617525361,
0.0787296369093355));
#67347=CARTESIAN_POINT('',(0.00447163833977556,-0.0321934096636663,0.0787513431603474));
#67348=CARTESIAN_POINT('Origin',(0.00812378219310841,-0.0315241814719618,
0.07415));
#67349=CARTESIAN_POINT('',(0.0044941374852466,-0.0322104233323594,0.0789276227641925));
#67350=CARTESIAN_POINT('',(0.00450435085242233,-0.0321934096636183,0.0789353648523491));
#67351=CARTESIAN_POINT('Origin',(0.014954218876609,-0.0326387224538279,
0.0660991862359572));
#67352=CARTESIAN_POINT('Origin',(0.0140091149074795,-0.0326386249602914,
0.0653891067255413));
#67353=CARTESIAN_POINT('Origin',(0.0140486811808949,-0.0326387238743361,
0.0654112383954586));
#67354=CARTESIAN_POINT('Ctrl Pts',(0.00451761106607016,-0.0327445246967097,
0.0786303632444832));
#67355=CARTESIAN_POINT('Ctrl Pts',(0.00468659072827904,-0.032443687833936,
0.0787663722119848));
#67356=CARTESIAN_POINT('Ctrl Pts',(0.004865335088422,-0.0321434074405928,
0.0788892665535882));
#67357=CARTESIAN_POINT('Ctrl Pts',(0.00471572432102837,-0.0327445246967097,
0.0787828464835944));
#67358=CARTESIAN_POINT('Ctrl Pts',(0.00489045498261643,-0.032443687833936,
0.0789113834875353));
#67359=CARTESIAN_POINT('Ctrl Pts',(0.00507437118532303,-0.0321434074405928,
0.0790263939038594));
#67360=CARTESIAN_POINT('',(0.00474490648815703,-0.0326943950436612,0.0788041727482432));
#67361=CARTESIAN_POINT('',(0.0049389740964552,-0.0323666188837389,0.0789390627880091));
#67362=CARTESIAN_POINT('Origin',(0.0145595906482954,-0.0326395579112012,
0.065155728401725));
#67363=CARTESIAN_POINT('Origin',(-0.00117696400785318,-0.032193382560303,
0.088135729191429));
#67364=CARTESIAN_POINT('',(0.0048356409098863,-0.032193409653269,0.0788687129493481));
#67365=CARTESIAN_POINT('',(0.00488768364632547,-0.0321934096584275,0.0789033222534424));
#67366=CARTESIAN_POINT('',(0.00464455084721257,-0.0325210109756239,0.0787296369115615));
#67367=CARTESIAN_POINT('Origin',(0.0149332315833509,-0.0326393129160891,
0.065458345125981));
#67368=CARTESIAN_POINT('',(0.00464537268054427,-0.0326943950436593,0.0787285551501433));
#67369=CARTESIAN_POINT('Origin',(-0.00204675831664323,-0.0326943765538239,
0.0875372610391569));
#67370=CARTESIAN_POINT('',(0.00469513958436065,-0.0326943950436702,0.0787663639492033));
#67371=CARTESIAN_POINT('Ctrl Pts',(0.00430965961899282,-0.0325229783203769,
0.0787816810112161));
#67372=CARTESIAN_POINT('Ctrl Pts',(0.00437350724044426,-0.032413025309245,
0.078834258607491));
#67373=CARTESIAN_POINT('Ctrl Pts',(0.00443843281327257,-0.032303122220807,
0.0788855074592754));
#67374=CARTESIAN_POINT('Ctrl Pts',(0.00450435085599873,-0.0321934096576658,
0.0789353648550541));
#67375=CARTESIAN_POINT('Ctrl Pts',(0.00442158118215094,-0.0325229783203769,
0.0787639410580971));
#67376=CARTESIAN_POINT('Ctrl Pts',(0.00448518425873659,-0.032413025309245,
0.0788149758180713));
#67377=CARTESIAN_POINT('Ctrl Pts',(0.00454983340823832,-0.032303122220807,
0.0788646871262812));
#67378=CARTESIAN_POINT('Ctrl Pts',(0.00461544357275238,-0.0321934096576658,
0.0789130142282012));
#67379=CARTESIAN_POINT('Ctrl Pts',(0.00453350274530907,-0.0325229783203769,
0.078746201104978));
#67380=CARTESIAN_POINT('Ctrl Pts',(0.00459686127702891,-0.032413025309245,
0.0787956930286517));
#67381=CARTESIAN_POINT('Ctrl Pts',(0.00466123400320407,-0.0323031222208069,
0.078843866793287));
#67382=CARTESIAN_POINT('Ctrl Pts',(0.00472653628950603,-0.0321934096576658,
0.0788906636013482));
#67383=CARTESIAN_POINT('Ctrl Pts',(0.00464542430846719,-0.0325229783203769,
0.078728461151859));
#67384=CARTESIAN_POINT('Ctrl Pts',(0.00470853829532123,-0.032413025309245,
0.0787764102392321));
#67385=CARTESIAN_POINT('Ctrl Pts',(0.00477263459816983,-0.0323031222208069,
0.0788230464602929));
#67386=CARTESIAN_POINT('Ctrl Pts',(0.00483762900625968,-0.0321934096576658,
0.0788683129744954));
#67387=CARTESIAN_POINT('',(0.004669995880676,-0.0321934096584275,0.0789020389006892));
#67388=CARTESIAN_POINT('Ctrl Pts',(0.00449413748734713,-0.0322104233328918,
0.0789276227614162));
#67389=CARTESIAN_POINT('Ctrl Pts',(0.00452013605721095,-0.0322609421831359,
0.0788934014066515));
#67390=CARTESIAN_POINT('Ctrl Pts',(0.00454566678326801,-0.0323120888240719,
0.078859795864563));
#67391=CARTESIAN_POINT('Ctrl Pts',(0.00459581507590604,-0.032415652463181,
0.0787937867524388));
#67392=CARTESIAN_POINT('Ctrl Pts',(0.00462041202890994,-0.0324680267167315,
0.0787614103156084));
#67393=CARTESIAN_POINT('Ctrl Pts',(0.00464455084724232,-0.0325210109755913,
0.0787296369115297));
#67394=CARTESIAN_POINT('Origin',(0.00247765310163461,-0.0262834582511612,
0.0686705281165161));
#67395=CARTESIAN_POINT('Origin',(-0.00278525371840213,-0.034277076391757,
0.0795180575115256));
#67396=CARTESIAN_POINT('Ctrl Pts',(0.00474463215546422,-0.0326943950436604,
0.0788021636607871));
#67397=CARTESIAN_POINT('Ctrl Pts',(0.00480874768979384,-0.0325844576448134,
0.078848734681508));
#67398=CARTESIAN_POINT('Ctrl Pts',(0.00487383092674217,-0.0324744968375322,
0.0788939829837636));
#67399=CARTESIAN_POINT('Ctrl Pts',(0.00493979767822429,-0.0323646534831894,
0.0789378517429675));
#67400=CARTESIAN_POINT('Ctrl Pts',(0.00475996310022805,-0.0326943950436604,
0.0789144405048603));
#67401=CARTESIAN_POINT('Ctrl Pts',(0.00482562601989823,-0.0325844576448134,
0.078960800236429));
#67402=CARTESIAN_POINT('Ctrl Pts',(0.00489225238189191,-0.0324744968375322,
0.0790058052321134));
#67403=CARTESIAN_POINT('Ctrl Pts',(0.00495975602528217,-0.0323646534831894,
0.0790493990063364));
#67404=CARTESIAN_POINT('Ctrl Pts',(0.00477529404499188,-0.0326943950436604,
0.0790267173489334));
#67405=CARTESIAN_POINT('Ctrl Pts',(0.00484250435000262,-0.0325844576448134,
0.0790728657913501));
#67406=CARTESIAN_POINT('Ctrl Pts',(0.00491067383704165,-0.0324744968375322,
0.0791176274804633));
#67407=CARTESIAN_POINT('Ctrl Pts',(0.00497971437234006,-0.0323646534831894,
0.0791609462697054));
#67408=CARTESIAN_POINT('Ctrl Pts',(0.00479062498975571,-0.0326943950436604,
0.0791389941930066));
#67409=CARTESIAN_POINT('Ctrl Pts',(0.00485938268010701,-0.0325844576448134,
0.0791849313462711));
#67410=CARTESIAN_POINT('Ctrl Pts',(0.00492909529219139,-0.0324744968375322,
0.0792294497288132));
#67411=CARTESIAN_POINT('Ctrl Pts',(0.00499967271939794,-0.0323646534831894,
0.0792724935330743));
#67412=CARTESIAN_POINT('',(0.00480128917553514,-0.0326773559991376,0.0791461024937869));
#67413=CARTESIAN_POINT('',(0.00479062498975458,-0.0326943950436594,0.0791389941929943));
#67414=CARTESIAN_POINT('Origin',(0.0139545330167376,-0.0326395669258199,
0.0652914488846738));
#67415=CARTESIAN_POINT('Ctrl Pts',(0.00480128917738503,-0.0326773559987491,
0.0791461024909921));
#67416=CARTESIAN_POINT('Ctrl Pts',(0.0048250745901028,-0.032626792258723,
0.079110335866603));
#67417=CARTESIAN_POINT('Ctrl Pts',(0.00484843842355853,-0.0325756109581861,
0.0790752031797998));
#67418=CARTESIAN_POINT('Ctrl Pts',(0.00489434281593506,-0.0324719985462381,
0.0790061757813931));
#67419=CARTESIAN_POINT('Ctrl Pts',(0.00491686496369439,-0.0324196091621773,
0.0789723087550395));
#67420=CARTESIAN_POINT('Ctrl Pts',(0.00493897409648217,-0.0323666188837757,
0.0789390627879684));
#67421=CARTESIAN_POINT('',(0.00476776573896581,-0.0326943950436702,0.0789715834706288));
#67422=CARTESIAN_POINT('Origin',(0.00812378219310841,-0.0315241814719618,
0.07415));
#67423=CARTESIAN_POINT('',(0.0048012891755597,-0.0327114338379852,0.0791461024937492));
#67424=CARTESIAN_POINT('',(0.00481196851860964,-0.0326943950436593,0.0791531880022078));
#67425=CARTESIAN_POINT('Origin',(0.0139163806071854,-0.0326395657591289,
0.0652670033992444));
#67426=CARTESIAN_POINT('Origin',(0.0140382027957248,-0.0326395684823877,
0.0653470865582513));
#67427=CARTESIAN_POINT('Origin',(0.0140754969351185,-0.0326395672488115,
0.065372822803197));
#67428=CARTESIAN_POINT('Ctrl Pts',(0.0048060833965187,-0.0332451089994433,
0.078847978256134));
#67429=CARTESIAN_POINT('Ctrl Pts',(0.0049832705453824,-0.0329451141710254,
0.0789731073134659));
#67430=CARTESIAN_POINT('Ctrl Pts',(0.00516937955638642,-0.0326442513127493,
0.0790845344319531));
#67431=CARTESIAN_POINT('Ctrl Pts',(0.00501338117505318,-0.0332451089994433,
0.0789877195564523));
#67432=CARTESIAN_POINT('Ctrl Pts',(0.00519583875328712,-0.0329451141710254,
0.0791050302501518));
#67433=CARTESIAN_POINT('Ctrl Pts',(0.00538661430981726,-0.0326442513127493,
0.0792082642258664));
#67434=CARTESIAN_POINT('Ctrl Pts',(0.00501545415283852,-0.0332451089994433,
0.0789891169694555));
#67435=CARTESIAN_POINT('Ctrl Pts',(0.00519796443536617,-0.0329451141710254,
0.0791063494795187));
#67436=CARTESIAN_POINT('Ctrl Pts',(0.00538878665735157,-0.0326442513127493,
0.0792095015238055));
#67437=CARTESIAN_POINT('',(0.00504381185237201,-0.0331951640388616,0.0790071501624085));
#67438=CARTESIAN_POINT('',(0.0052459663372888,-0.0328677532355024,0.0791295884337797));
#67439=CARTESIAN_POINT('Origin',(0.0133632826850496,-0.0326402808283654,
0.0644531592131837));
#67440=CARTESIAN_POINT('Origin',(-0.000285797768402256,-0.032694427877906,
0.0887021517708994));
#67441=CARTESIAN_POINT('',(0.00513841974862762,-0.0326943950436593,0.0790658657503114));
#67442=CARTESIAN_POINT('',(0.00519253292458443,-0.0326943950436694,0.0790971389687191));
#67443=CARTESIAN_POINT('',(0.00493897409645284,-0.0330220786163545,0.0789390627880075));
#67444=CARTESIAN_POINT('Origin',(0.0137943810235266,-0.0326396682763673,
0.0646660133120013));
#67445=CARTESIAN_POINT('',(0.00493972638372129,-0.0331951640388587,0.0789379315578555));
#67446=CARTESIAN_POINT('Origin',(-0.00116903923235206,-0.033195202656002,
0.0881238094238224));
#67447=CARTESIAN_POINT('',(0.00499176911805666,-0.0331951640388701,0.0789725408601421));
#67448=CARTESIAN_POINT('Ctrl Pts',(0.00460801235427424,-0.0330240426238172,
0.0790120327477688));
#67449=CARTESIAN_POINT('Ctrl Pts',(0.00467499159222374,-0.0329142774063519,
0.0790604659025474));
#67450=CARTESIAN_POINT('Ctrl Pts',(0.00474300547036676,-0.0328043479726691,
0.0791075385550743));
#67451=CARTESIAN_POINT('Ctrl Pts',(0.00481196851860963,-0.0326943950436593,
0.0791531880022078));
#67452=CARTESIAN_POINT('Ctrl Pts',(0.00471859913403964,-0.0330240426238172,
0.0789873001756081));
#67453=CARTESIAN_POINT('Ctrl Pts',(0.00478523765671186,-0.0329142774063519,
0.0790342098897559));
#67454=CARTESIAN_POINT('Ctrl Pts',(0.00485287915594523,-0.0328043479726691,
0.0790797653856978));
#67455=CARTESIAN_POINT('Ctrl Pts',(0.00492143858516508,-0.0326943950436593,
0.0791239059170205));
#67456=CARTESIAN_POINT('Ctrl Pts',(0.00482918591380505,-0.0330240426238172,
0.0789625676034474));
#67457=CARTESIAN_POINT('Ctrl Pts',(0.00489548372119997,-0.0329142774063519,
0.0790079538769644));
#67458=CARTESIAN_POINT('Ctrl Pts',(0.0049627528415237,-0.0328043479726691,
0.0790519922163214));
#67459=CARTESIAN_POINT('Ctrl Pts',(0.00503090865172054,-0.0326943950436593,
0.0790946238318333));
#67460=CARTESIAN_POINT('Ctrl Pts',(0.00493977269357046,-0.0330240426238172,
0.0789378350312866));
#67461=CARTESIAN_POINT('Ctrl Pts',(0.00500572978568809,-0.0329142774063519,
0.0789816978641729));
#67462=CARTESIAN_POINT('Ctrl Pts',(0.00507262652710217,-0.0328043479726691,
0.079024219046945));
#67463=CARTESIAN_POINT('Ctrl Pts',(0.005140378718276,-0.0326943950436593,
0.079065341746646));
#67464=CARTESIAN_POINT('',(0.00497519413362863,-0.0326943950436693,0.0791095268762696));
#67465=CARTESIAN_POINT('Ctrl Pts',(0.0048012891773917,-0.0327114338383317,
0.0791461024909819));
#67466=CARTESIAN_POINT('Ctrl Pts',(0.00482507063387641,-0.0327619876831058,
0.0791103418156636));
#67467=CARTESIAN_POINT('Ctrl Pts',(0.00484843253495084,-0.0328131562604521,
0.0790752120346227));
#67468=CARTESIAN_POINT('Ctrl Pts',(0.00489433688505058,-0.0329167375858765,
0.0790061846997884));
#67469=CARTESIAN_POINT('Ctrl Pts',(0.00491686104343086,-0.0329691088920616,
0.078972314650022));
#67470=CARTESIAN_POINT('Ctrl Pts',(0.00493897409648142,-0.0330220786163187,
0.0789390627879694));
#67471=CARTESIAN_POINT('Ctrl Pts',(0.00504341184551566,-0.0331951640388604,
0.0790051619475543));
#67472=CARTESIAN_POINT('Ctrl Pts',(0.00514378920594111,-0.0330306422010619,
0.079068846629541));
#67473=CARTESIAN_POINT('Ctrl Pts',(0.00524671294949429,-0.0328657861914645,
0.0791283281915476));
#67474=CARTESIAN_POINT('Ctrl Pts',(0.00504381185236937,-0.0331951640388604,
0.0790071501624067));
#67475=CARTESIAN_POINT('Ctrl Pts',(0.00514423031786217,-0.0330306422010619,
0.0790708265745082));
#67476=CARTESIAN_POINT('Ctrl Pts',(0.00524719478955565,-0.0328657861914645,
0.0791302981747805));
#67477=CARTESIAN_POINT('Ctrl Pts',(0.00511046375141672,-0.0331951640388604,
0.0793384402250667));
#67478=CARTESIAN_POINT('Ctrl Pts',(0.00521773142655159,-0.0330306422010619,
0.0794007386518885));
#67479=CARTESIAN_POINT('Ctrl Pts',(0.00532748230170476,-0.0328657861914645,
0.0794585503593227));
#67480=CARTESIAN_POINT('',(0.00512155322654768,-0.0331781648281926,0.0793448648902783));
#67481=CARTESIAN_POINT('',(0.00511046375141491,-0.0331951640388588,0.0793384402250532));
#67482=CARTESIAN_POINT('Origin',(0.012764468923795,-0.0326412092392991,
0.0646965776852704));
#67483=CARTESIAN_POINT('Ctrl Pts',(0.00512155322577364,-0.033178164828644,
0.0793448648885998));
#67484=CARTESIAN_POINT('Ctrl Pts',(0.00514306068487822,-0.0331276811546798,
0.0793076497334389));
#67485=CARTESIAN_POINT('Ctrl Pts',(0.00516417975659762,-0.0330765663497826,
0.0792711065518096));
#67486=CARTESIAN_POINT('Ctrl Pts',(0.00520565941064976,-0.03297306144632,
0.0791993328197377));
#67487=CARTESIAN_POINT('Ctrl Pts',(0.00522600324074536,-0.0329207133373855,
0.0791641312670039));
#67488=CARTESIAN_POINT('Ctrl Pts',(0.00524596632082362,-0.032867753228938,
0.0791295884343284));
#67489=CARTESIAN_POINT('',(0.00507713780190345,-0.0331951640388701,0.0791727951937408));
#67490=CARTESIAN_POINT('Origin',(0.00812378219310841,-0.0315241814719618,
0.07415));
#67491=CARTESIAN_POINT('',(0.00512155322788321,-0.0332121607144399,0.0793448648892593));
#67492=CARTESIAN_POINT('',(0.00513265640034574,-0.0331951640388587,0.0793512658547611));
#67493=CARTESIAN_POINT('Origin',(0.0127218757545504,-0.0326413639142849,
0.0646810160177423));
#67494=CARTESIAN_POINT('Origin',(0.013997845151354,-0.0326412104312054,
0.0654093691303759));
#67495=CARTESIAN_POINT('Origin',(0.0140325894827513,-0.032641365465698,
0.0654385109720689));
#67496=CARTESIAN_POINT('Ctrl Pts',(0.00510760087554114,-0.0337436976235975,
0.0790470169756248));
#67497=CARTESIAN_POINT('Ctrl Pts',(0.00515164538838314,-0.0336723290703325,
0.0790741449675099));
#67498=CARTESIAN_POINT('Ctrl Pts',(0.00519617072292914,-0.033601104548885,
0.0791004763487643));
#67499=CARTESIAN_POINT('Ctrl Pts',(0.00533833129616268,-0.0333736987606857,
0.079184547233157));
#67500=CARTESIAN_POINT('Ctrl Pts',(0.00548508207211302,-0.0331450831799192,
0.0792603215820004));
#67501=CARTESIAN_POINT('Ctrl Pts',(0.00532326357010544,-0.0337436976235975,
0.0791734669743328));
#67502=CARTESIAN_POINT('Ctrl Pts',(0.00536844539339983,-0.0336723290703325,
0.0791986552632584));
#67503=CARTESIAN_POINT('Ctrl Pts',(0.00541407296526578,-0.033601104548885,
0.0792230267987213));
#67504=CARTESIAN_POINT('Ctrl Pts',(0.00555975276392098,-0.0333736987606857,
0.0793008402837251));
#67505=CARTESIAN_POINT('Ctrl Pts',(0.00570965788023112,-0.0331450831799192,
0.0793701655914324));
#67506=CARTESIAN_POINT('Ctrl Pts',(0.00532542019705108,-0.0337436976235975,
0.07917473147432));
#67507=CARTESIAN_POINT('Ctrl Pts',(0.00537061339345001,-0.0336723290703325,
0.0791999003662159));
#67508=CARTESIAN_POINT('Ctrl Pts',(0.00541625198768915,-0.033601104548885,
0.0792242523032209));
#67509=CARTESIAN_POINT('Ctrl Pts',(0.00556196697859858,-0.0333736987606857,
0.0793020032142308));
#67510=CARTESIAN_POINT('Ctrl Pts',(0.0057119036383123,-0.0331450831799192,
0.0793712640315267));
#67511=CARTESIAN_POINT('',(0.00535487245242893,-0.0336938721132548,0.0791909586239099));
#67512=CARTESIAN_POINT('',(0.00556431599105305,-0.0333679869945434,0.0793004618977903));
#67513=CARTESIAN_POINT('Ctrl Pts',(0.00535487245244038,-0.0336938721132648,
0.0791909586239173));
#67514=CARTESIAN_POINT('Ctrl Pts',(0.00537454967870561,-0.0336629187933932,
0.0792017669775535));
#67515=CARTESIAN_POINT('Ctrl Pts',(0.00539428389898122,-0.033631995230104,
0.0792124566563494));
#67516=CARTESIAN_POINT('Ctrl Pts',(0.00541407296527756,-0.033601104548895,
0.0792230267987281));
#67517=CARTESIAN_POINT('Ctrl Pts',(0.00546373050405251,-0.0335235892595454,
0.0792495509028554));
#67518=CARTESIAN_POINT('Ctrl Pts',(0.00551382170409883,-0.0334458668660369,
0.0792753693094286));
#67519=CARTESIAN_POINT('Ctrl Pts',(0.00556431599090787,-0.0333679869945385,
0.079300461898067));
#67520=CARTESIAN_POINT('Ctrl Pts',(0.00556435550900939,-0.0333679692459669,
0.0793004823036556));
#67521=CARTESIAN_POINT('Ctrl Pts',(0.00556455188975413,-0.0333391895374597,
0.079300073803441));
#67522=CARTESIAN_POINT('Ctrl Pts',(0.00556469616012824,-0.0333104081060613,
0.0792997662056888));
#67523=CARTESIAN_POINT('Ctrl Pts',(0.00556488211226626,-0.0332532698405432,
0.0792993566957794));
#67524=CARTESIAN_POINT('Ctrl Pts',(0.00556492529106622,-0.03322491721508,
0.0792992517812584));
#67525=CARTESIAN_POINT('Ctrl Pts',(0.00556492074556344,-0.0331960985328607,
0.0792992454237937));
#67526=CARTESIAN_POINT('Ctrl Pts',(0.00556492065866469,-0.0331956312596703,
0.0792992453473829));
#67527=CARTESIAN_POINT('Ctrl Pts',(0.0055649205590409,-0.0331951640388594,
0.0792992452978759));
#67528=CARTESIAN_POINT('',(0.00545298044386901,-0.0331951640388587,0.0792436178710481));
#67529=CARTESIAN_POINT('',(0.00550895050146465,-0.0331951640388687,0.0792714315844719));
#67530=CARTESIAN_POINT('',(0.00524596632831351,-0.0335216366567679,0.0791295884211258));
#67531=CARTESIAN_POINT('Origin',(0.0125088547087134,-0.0326434571528773,
0.0641422231621661));
#67532=CARTESIAN_POINT('',(0.00524664610052128,-0.0336938721132327,0.0791284121871067));
#67533=CARTESIAN_POINT('Origin',(-0.000217696129839952,-0.0336938867896336,
0.088583558613889));
#67534=CARTESIAN_POINT('',(0.0053007592764851,-0.0336938721132537,0.0791596854055182));
#67535=CARTESIAN_POINT('Ctrl Pts',(0.00492024029776362,-0.0335235895815172,
0.079223196164629));
#67536=CARTESIAN_POINT('Ctrl Pts',(0.00499008283117384,-0.0334144449262748,
0.079267299226012));
#67537=CARTESIAN_POINT('Ctrl Pts',(0.00506091674125023,-0.0333049234473147,
0.0793100100622914));
#67538=CARTESIAN_POINT('Ctrl Pts',(0.00513265640034556,-0.0331951640388587,
0.0793512658547612));
#67539=CARTESIAN_POINT('Ctrl Pts',(0.00502905603831519,-0.0335235895815172,
0.0791915685328141));
#67540=CARTESIAN_POINT('Ctrl Pts',(0.0050984631551044,-0.0334144449262748,
0.0792341735312899));
#67541=CARTESIAN_POINT('Ctrl Pts',(0.00516883019946658,-0.0333049234473147,
0.0792753935789491));
#67542=CARTESIAN_POINT('Ctrl Pts',(0.00524007196805507,-0.0331951640388587,
0.0793151678174233));
#67543=CARTESIAN_POINT('Ctrl Pts',(0.00513787177886675,-0.0335235895815172,
0.0791599409009992));
#67544=CARTESIAN_POINT('Ctrl Pts',(0.00520684347903495,-0.0334144449262748,
0.0792010478365679));
#67545=CARTESIAN_POINT('Ctrl Pts',(0.00527674365768294,-0.0333049234473147,
0.0792407770956068));
#67546=CARTESIAN_POINT('Ctrl Pts',(0.00534748753576459,-0.0331951640388587,
0.0792790697800854));
#67547=CARTESIAN_POINT('Ctrl Pts',(0.00524668751941831,-0.0335235895815172,
0.0791283132691844));
#67548=CARTESIAN_POINT('Ctrl Pts',(0.00531522380296551,-0.0334144449262748,
0.0791679221418459));
#67549=CARTESIAN_POINT('Ctrl Pts',(0.00538465711589929,-0.0333049234473147,
0.0792061606122645));
#67550=CARTESIAN_POINT('Ctrl Pts',(0.00545490310347411,-0.0331951640388587,
0.0792429717427476));
#67551=CARTESIAN_POINT('',(0.00529281842211738,-0.0331951640388687,0.0792974418629146));
#67552=CARTESIAN_POINT('Ctrl Pts',(0.00512155322944654,-0.033212160714597,
0.0793448648865405));
#67553=CARTESIAN_POINT('Ctrl Pts',(0.00514302451797355,-0.0332625444109832,
0.0793077123428178));
#67554=CARTESIAN_POINT('Ctrl Pts',(0.00516412582250511,-0.0333135300746992,
0.0792711999957257));
#67555=CARTESIAN_POINT('Ctrl Pts',(0.00520560521350614,-0.0334167203140571,
0.0791994267117975));
#67556=CARTESIAN_POINT('Ctrl Pts',(0.00522596723467659,-0.0334688847587259,
0.0791641935733269));
#67557=CARTESIAN_POINT('Ctrl Pts',(0.00524596632880189,-0.0335216366562323,
0.0791295884205915));
#67558=CARTESIAN_POINT('Ctrl Pts',(0.0053546140846346,-0.033693872113239,
0.0791899927248701));
#67559=CARTESIAN_POINT('Ctrl Pts',(0.00538411483450019,-0.0336474569764958,
0.0792062015847164));
#67560=CARTESIAN_POINT('Ctrl Pts',(0.00541380330812527,-0.033601104548885,
0.0792220639903966));
#67561=CARTESIAN_POINT('Ctrl Pts',(0.00548896769753591,-0.0334837508592656,
0.079262223954583));
#67562=CARTESIAN_POINT('Ctrl Pts',(0.00556528910329043,-0.0333660264659097,
0.0793001390067731));
#67563=CARTESIAN_POINT('Ctrl Pts',(0.00535487245241095,-0.033693872113239,
0.0791909586238999));
#67564=CARTESIAN_POINT('Ctrl Pts',(0.00538437885600408,-0.0336474569764958,
0.0792071659714339));
#67565=CARTESIAN_POINT('Ctrl Pts',(0.00541407296526578,-0.033601104548885,
0.0792230267987213));
#67566=CARTESIAN_POINT('Ctrl Pts',(0.00548925162281262,-0.0334837508592656,
0.0792631827667802));
#67567=CARTESIAN_POINT('Ctrl Pts',(0.00556558717202429,-0.0333660264659097,
0.0793010934018032));
#67568=CARTESIAN_POINT('Ctrl Pts',(0.00544271863782408,-0.033693872113239,
0.0795193685613193));
#67569=CARTESIAN_POINT('Ctrl Pts',(0.0054741473337589,-0.0336474569764958,
0.0795350617159796));
#67570=CARTESIAN_POINT('Ctrl Pts',(0.00550575758436879,-0.033601104548885,
0.0795503858827673));
#67571=CARTESIAN_POINT('Ctrl Pts',(0.00558578747126071,-0.0334837508592656,
0.0795891831498267));
#67572=CARTESIAN_POINT('Ctrl Pts',(0.0056669318583874,-0.0333660264659097,
0.0796255919285078));
#67573=CARTESIAN_POINT('',(0.00545366570538521,-0.0336769361243753,0.0795231255282181));
#67574=CARTESIAN_POINT('',(0.00544219470431035,-0.0336938721132327,0.0795174098539167));
#67575=CARTESIAN_POINT('Ctrl Pts',(0.00545366570538547,-0.033676936124375,
0.0795231255282182));
#67576=CARTESIAN_POINT('Ctrl Pts',(0.00545175271121779,-0.0336797586670124,
0.079522174886503));
#67577=CARTESIAN_POINT('Ctrl Pts',(0.00544984029708625,-0.0336825812713044,
0.079521223259117));
#67578=CARTESIAN_POINT('Ctrl Pts',(0.00544601663813532,-0.0336882265891408,
0.0795193180381814));
#67579=CARTESIAN_POINT('Ctrl Pts',(0.00544410539329454,-0.0336910493027062,
0.079518364444656));
#67580=CARTESIAN_POINT('Ctrl Pts',(0.00544219470431098,-0.0336938721132374,
0.0795174098539292));
#67581=CARTESIAN_POINT('Ctrl Pts',(0.00545366570538519,-0.0336769361243754,
0.079523125528218));
#67582=CARTESIAN_POINT('Ctrl Pts',(0.00547231772202003,-0.0336279018505232,
0.0794855917250323));
#67583=CARTESIAN_POINT('Ctrl Pts',(0.00549123807150779,-0.0335767826010773,
0.0794475179506085));
#67584=CARTESIAN_POINT('Ctrl Pts',(0.00552831108612262,-0.0334733172064623,
0.0793729152274124));
#67585=CARTESIAN_POINT('Ctrl Pts',(0.00554648866729878,-0.0334209631456245,
0.0793363361396069));
#67586=CARTESIAN_POINT('Ctrl Pts',(0.00556431598451702,-0.0333679869844681,
0.0793004618945372));
#67587=CARTESIAN_POINT('',(0.00539853357837964,-0.0336938721132538,0.0793541842389233));
#67588=CARTESIAN_POINT('Ctrl Pts',(0.00542099327985926,-0.0342436276873911,
0.0792267171568266));
#67589=CARTESIAN_POINT('Ctrl Pts',(0.00561246482387742,-0.0339430054201811,
0.0793286545211486));
#67590=CARTESIAN_POINT('Ctrl Pts',(0.00581107075726798,-0.0336441434784053,
0.0794158798708794));
#67591=CARTESIAN_POINT('Ctrl Pts',(0.00564416926297431,-0.0342436276873911,
0.0793393780664654));
#67592=CARTESIAN_POINT('Ctrl Pts',(0.00583988988324642,-0.0339430054201811,
0.0794328982098245));
#67593=CARTESIAN_POINT('Ctrl Pts',(0.00604209880213932,-0.0336441434784053,
0.0795114101932013));
#67594=CARTESIAN_POINT('Ctrl Pts',(0.00564640102280546,-0.0342436276873911,
0.0793405046755617));
#67595=CARTESIAN_POINT('Ctrl Pts',(0.00584216413384011,-0.0339430054201811,
0.0794339406467113));
#67596=CARTESIAN_POINT('Ctrl Pts',(0.00604440908258803,-0.0336441434784053,
0.0795123654964246));
#67597=CARTESIAN_POINT('',(0.00567686067421152,-0.034193496108874,0.0793548727247033));
#67598=CARTESIAN_POINT('',(0.0058927666861224,-0.0338664212863787,0.0794510088485209));
#67599=CARTESIAN_POINT('Origin',(0.0132545748800529,-0.0345610720405186,
0.0644340352423985));
#67600=CARTESIAN_POINT('Origin',(0.00163887119202861,-0.0336938005073097,
0.0895585850922207));
#67601=CARTESIAN_POINT('',(0.00577808157344143,-0.0336938721132327,0.0794012678091005));
#67602=CARTESIAN_POINT('',(0.00583568762442886,-0.0336938721132427,0.0794255122495204));
#67603=CARTESIAN_POINT('',(0.00556431598451228,-0.0340203938281605,0.0793004618945348));
#67604=CARTESIAN_POINT('Origin',(0.0136448814808393,-0.0345589643246379,
0.0647154557314726));
#67605=CARTESIAN_POINT('',(0.00556492055904032,-0.034193496108874,0.0792992452978757));
#67606=CARTESIAN_POINT('Origin',(0.000661051947683549,-0.0341934220717601,
0.0891673905593451));
#67607=CARTESIAN_POINT('',(0.00562089061663592,-0.0341934961088841,0.0793270590112994));
#67608=CARTESIAN_POINT('Ctrl Pts',(0.00567621460244076,-0.0341934961088741,
0.0793529502333115));
#67609=CARTESIAN_POINT('Ctrl Pts',(0.00578378149956862,-0.0340287516182428,
0.0794035517650258));
#67610=CARTESIAN_POINT('Ctrl Pts',(0.00589334788253513,-0.0338644633275951,
0.0794496642372343));
#67611=CARTESIAN_POINT('Ctrl Pts',(0.00567686067421154,-0.0341934961088741,
0.0793548727247032));
#67612=CARTESIAN_POINT('Ctrl Pts',(0.00578446731733436,-0.0340287516182428,
0.0794054608993926));
#67613=CARTESIAN_POINT('Ctrl Pts',(0.00589407286027767,-0.0338644633275951,
0.0794515583832574));
#67614=CARTESIAN_POINT('Ctrl Pts',(0.00578450865792822,-0.0341934961088741,
0.0796751967682377));
#67615=CARTESIAN_POINT('Ctrl Pts',(0.00589873774829603,-0.0340287516182428,
0.0797235594056701));
#67616=CARTESIAN_POINT('Ctrl Pts',(0.00601486809658658,-0.0338644633275951,
0.0797671595431882));
#67617=CARTESIAN_POINT('',(0.00579631591328774,-0.034176475883242,0.0796801808927925));
#67618=CARTESIAN_POINT('',(0.00578450865792329,-0.034193496108874,0.079675196768223));
#67619=CARTESIAN_POINT('Origin',(0.0126912500153698,-0.0345621026823869,
0.0646176043969201));
#67620=CARTESIAN_POINT('Ctrl Pts',(0.0057963159121418,-0.0341764758837524,
0.0796801808913685));
#67621=CARTESIAN_POINT('Ctrl Pts',(0.00581296673976368,-0.034126005004022,
0.0796406176237988));
#67622=CARTESIAN_POINT('Ctrl Pts',(0.00582932810150455,-0.034074926914769,
0.079601742044333));
#67623=CARTESIAN_POINT('Ctrl Pts',(0.00586148474250247,-0.0339715436305362,
0.0795253362037994));
#67624=CARTESIAN_POINT('Ctrl Pts',(0.00587726782772358,-0.0339192778237569,
0.0794878349318182));
#67625=CARTESIAN_POINT('Ctrl Pts',(0.00589276668396639,-0.0338664212855109,
0.0794510088488591));
#67626=CARTESIAN_POINT('',(0.00573068466607741,-0.0341934961088841,0.0795150347464732));
#67627=CARTESIAN_POINT('Origin',(0.00812378219310841,-0.0315241814719618,
0.07415));
#67628=CARTESIAN_POINT('',(0.00545366570596618,-0.0337108120655526,0.0795231255270644));
#67629=CARTESIAN_POINT('',(0.00546514888907052,-0.0336938721132327,0.079528816687218));
#67630=CARTESIAN_POINT('Origin',(0.0137355626301267,-0.0345562507985583,
0.0653686693265288));
#67631=CARTESIAN_POINT('Ctrl Pts',(0.0054651488890697,-0.0336938721132331,
0.0795288166872185));
#67632=CARTESIAN_POINT('Ctrl Pts',(0.00546323415082136,-0.0336910493194145,
0.079527870273319));
#67633=CARTESIAN_POINT('Ctrl Pts',(0.00546131985468562,-0.033688226597495,
0.0795269228057549));
#67634=CARTESIAN_POINT('Ctrl Pts',(0.00545749212905528,-0.033682581271305,
0.0795250257540697));
#67635=CARTESIAN_POINT('Ctrl Pts',(0.00545557869955279,-0.0336797586670127,
0.0795240761699332));
#67636=CARTESIAN_POINT('Ctrl Pts',(0.00545366570538492,-0.033676936124375,
0.0795231255282179));
#67637=CARTESIAN_POINT('Origin',(0.011733884582879,-0.0345562512720826,
0.0643739613533162));
#67638=CARTESIAN_POINT('Ctrl Pts',(0.0052451079780368,-0.0340223579322397,
0.0794143361180231));
#67639=CARTESIAN_POINT('Ctrl Pts',(0.00531771690306934,-0.0339125849573575,
0.0794540405433465));
#67640=CARTESIAN_POINT('Ctrl Pts',(0.00539109659599479,-0.0338030433565231,
0.0794922142328016));
#67641=CARTESIAN_POINT('Ctrl Pts',(0.00546514888906988,-0.0336938721132327,
0.0795288166872183));
#67642=CARTESIAN_POINT('Ctrl Pts',(0.00535172312814745,-0.0340223579322397,
0.0793759383368725));
#67643=CARTESIAN_POINT('Ctrl Pts',(0.0054238024476323,-0.0339125849573575,
0.0794141722612119));
#67644=CARTESIAN_POINT('Ctrl Pts',(0.00549662247120436,-0.0338030433565231,
0.0794508874445912));
#67645=CARTESIAN_POINT('Ctrl Pts',(0.00557008591218377,-0.0336938721132327,
0.0794860451895779));
#67646=CARTESIAN_POINT('Ctrl Pts',(0.0054583382782581,-0.0340223579322397,
0.0793375405557219));
#67647=CARTESIAN_POINT('Ctrl Pts',(0.00552988799219527,-0.0339125849573575,
0.0793743039790773));
#67648=CARTESIAN_POINT('Ctrl Pts',(0.00560214834641393,-0.0338030433565231,
0.0794095606563807));
#67649=CARTESIAN_POINT('Ctrl Pts',(0.00567502293529766,-0.0336938721132327,
0.0794432736919375));
#67650=CARTESIAN_POINT('Ctrl Pts',(0.00556495342836875,-0.0340223579322397,
0.0792991427745713));
#67651=CARTESIAN_POINT('Ctrl Pts',(0.00563597353675823,-0.0339125849573575,
0.0793344356969426));
#67652=CARTESIAN_POINT('Ctrl Pts',(0.0057076742216235,-0.0338030433565231,
0.0793682338681703));
#67653=CARTESIAN_POINT('Ctrl Pts',(0.00577995995841156,-0.0336938721132327,
0.0794005021942971));
#67654=CARTESIAN_POINT('',(0.00562161523126597,-0.0336938721132427,0.0794650422481692));
#67655=CARTESIAN_POINT('Ctrl Pts',(0.00545366570756543,-0.033710812066268,
0.0795231255238306));
#67656=CARTESIAN_POINT('Ctrl Pts',(0.00547280121137372,-0.0337611408994333,
0.0794846187903303));
#67657=CARTESIAN_POINT('Ctrl Pts',(0.0054915875346911,-0.0338121088781394,
0.0794468147192862));
#67658=CARTESIAN_POINT('Ctrl Pts',(0.00552847893437984,-0.0339153382773234,
0.0793725774632149));
#67659=CARTESIAN_POINT('Ctrl Pts',(0.00554656840343498,-0.0339675558473119,
0.0793361756850831));
#67660=CARTESIAN_POINT('Ctrl Pts',(0.00556431598453475,-0.0340203938281304,
0.0793004618945015));
#67661=CARTESIAN_POINT('Origin',(0.00812378219310841,-0.0315241814719618,
0.07415));
#67662=CARTESIAN_POINT('',(0.00579631591434876,-0.034210518019052,0.07968018089244));
#67663=CARTESIAN_POINT('',(0.00580813378883227,-0.034193496108874,0.0796851397875581));
#67664=CARTESIAN_POINT('Origin',(0.0126517817243141,-0.0345621697916885,
0.0645953120688972));
#67665=CARTESIAN_POINT('Origin',(0.0117472492764006,-0.0345621043445321,
0.0642203026984108));
#67666=CARTESIAN_POINT('Origin',(0.0117907777614704,-0.0345621710836054,
0.0642329490599898));
#67667=CARTESIAN_POINT('Ctrl Pts',(0.00577669901908363,-0.0346945769586965,
0.0794006859386861));
#67668=CARTESIAN_POINT('Ctrl Pts',(0.00588667673832936,-0.0345275153362944,
0.0794498465354869));
#67669=CARTESIAN_POINT('Ctrl Pts',(0.00599822895896659,-0.0343603235965185,
0.0794955611496933));
#67670=CARTESIAN_POINT('Ctrl Pts',(0.00611102374956819,-0.034193496108874,
0.0795376994812688));
#67671=CARTESIAN_POINT('Ctrl Pts',(0.005853967938694,-0.0346945769586965,
0.0794332058161165));
#67672=CARTESIAN_POINT('Ctrl Pts',(0.00596462679979276,-0.0345275153362944,
0.0794807479844593));
#67673=CARTESIAN_POINT('Ctrl Pts',(0.00607680944037584,-0.0343603235965185,
0.0795248223303149));
#67674=CARTESIAN_POINT('Ctrl Pts',(0.00619018213661502,-0.034193496108874,
0.0795653034325437));
#67675=CARTESIAN_POINT('Ctrl Pts',(0.00593123685830434,-0.0346945769586965,
0.0794657256935453));
#67676=CARTESIAN_POINT('Ctrl Pts',(0.00604257686125612,-0.0345275153362944,
0.0795116494334311));
#67677=CARTESIAN_POINT('Ctrl Pts',(0.00615538992178506,-0.0343603235965185,
0.0795540835109363));
#67678=CARTESIAN_POINT('Ctrl Pts',(0.00626934052366183,-0.034193496108874,
0.0795929073838184));
#67679=CARTESIAN_POINT('Ctrl Pts',(0.00600850577791472,-0.0346945769586965,
0.0794982455709775));
#67680=CARTESIAN_POINT('Ctrl Pts',(0.00612052692271955,-0.0345275153362944,
0.0795425508824042));
#67681=CARTESIAN_POINT('Ctrl Pts',(0.00623397040319434,-0.0343603235965185,
0.079583344691558));
#67682=CARTESIAN_POINT('Ctrl Pts',(0.00634849891070869,-0.034193496108874,
0.0796205113350935));
#67683=CARTESIAN_POINT('',(0.0060085057773564,-0.0346945769586966,0.0794982455707422));
#67684=CARTESIAN_POINT('',(0.00623002218382771,-0.0343667727831509,0.0795806351403604));
#67685=CARTESIAN_POINT('Origin',(0.0120218260819249,-0.0345626457063868,
0.0637967416251167));
#67686=CARTESIAN_POINT('Origin',(0.00259085538939692,-0.0341934771029017,
0.090016492532288));
#67687=CARTESIAN_POINT('',(0.00611244011171101,-0.034193496108874,0.0795381933921864));
#67688=CARTESIAN_POINT('',(0.00617145481132468,-0.034193496108884,0.0795587728778723));
#67689=CARTESIAN_POINT('',(0.0058927666846072,-0.0345211942962644,0.0794510088474529));
#67690=CARTESIAN_POINT('Origin',(0.0124636989864353,-0.0345625596120814,
0.063986317800692));
#67691=CARTESIAN_POINT('',(0.00589329367539629,-0.0346945769586885,0.0794497566899203));
#67692=CARTESIAN_POINT('Origin',(0.00160161318766902,-0.03469456858539,
0.0896470109187123));
#67693=CARTESIAN_POINT('',(0.00595089972638634,-0.0346945769587026,0.0794740011303412));
#67694=CARTESIAN_POINT('Ctrl Pts',(0.00558133965538096,-0.0345231616327842,
0.0795847020104502));
#67695=CARTESIAN_POINT('Ctrl Pts',(0.0056562493711466,-0.0344132092796988,
0.07961974600136));
#67696=CARTESIAN_POINT('Ctrl Pts',(0.00573188007922492,-0.034303273855898,
0.0796532387357783));
#67697=CARTESIAN_POINT('Ctrl Pts',(0.00580813378883211,-0.034193496108874,
0.0796851397875582));
#67698=CARTESIAN_POINT('Ctrl Pts',(0.00568533322408234,-0.0345231616327842,
0.0795396856377914));
#67699=CARTESIAN_POINT('Ctrl Pts',(0.00575962245252887,-0.0344132092796988,
0.0795732962237679));
#67700=CARTESIAN_POINT('Ctrl Pts',(0.00583460305645197,-0.034303273855898,
0.0796053684615008));
#67701=CARTESIAN_POINT('Ctrl Pts',(0.00591017792454178,-0.034193496108874,
0.0796358637233295));
#67702=CARTESIAN_POINT('Ctrl Pts',(0.00578932679278373,-0.0345231616327842,
0.0794946692651327));
#67703=CARTESIAN_POINT('Ctrl Pts',(0.00586299553391114,-0.0344132092796988,
0.0795268464461759));
#67704=CARTESIAN_POINT('Ctrl Pts',(0.00593732603367902,-0.034303273855898,
0.0795574981872233));
#67705=CARTESIAN_POINT('Ctrl Pts',(0.00601222206025146,-0.034193496108874,
0.0795865876591009));
#67706=CARTESIAN_POINT('Ctrl Pts',(0.00589332036148511,-0.0345231616327842,
0.079449652892474));
#67707=CARTESIAN_POINT('Ctrl Pts',(0.0059663686152934,-0.0344132092796988,
0.0794803966685838));
#67708=CARTESIAN_POINT('Ctrl Pts',(0.00604004901090607,-0.034303273855898,
0.0795096279129457));
#67709=CARTESIAN_POINT('Ctrl Pts',(0.00611426619596113,-0.034193496108874,
0.0795373115948722));
#67710=CARTESIAN_POINT('',(0.00596028695028164,-0.0341934961088839,0.0796116665898822));
#67711=CARTESIAN_POINT('Ctrl Pts',(0.00579631591568478,-0.0342105180195382,
0.0796801808892483));
#67712=CARTESIAN_POINT('Ctrl Pts',(0.00581298547473257,-0.0342610556241241,
0.0796405731502351));
#67713=CARTESIAN_POINT('Ctrl Pts',(0.00582935590716231,-0.0343122189870039,
0.0796016761516192));
#67714=CARTESIAN_POINT('Ctrl Pts',(0.00586151286878964,-0.0344158119695117,
0.0795252695388263));
#67715=CARTESIAN_POINT('Ctrl Pts',(0.00587728624555107,-0.0344681990450007,
0.0794877911755215));
#67716=CARTESIAN_POINT('Ctrl Pts',(0.00589276668461278,-0.0345211942962415,
0.0794510088474223));
#67717=CARTESIAN_POINT('Ctrl Pts',(0.00600774045365258,-0.0346945769586931,
0.0794963678999827));
#67718=CARTESIAN_POINT('Ctrl Pts',(0.00611827282701614,-0.034529677707698,
0.0795401155656829));
#67719=CARTESIAN_POINT('Ctrl Pts',(0.00623051888307191,-0.034364806625142,
0.0795792574449877));
#67720=CARTESIAN_POINT('Ctrl Pts',(0.00600850577734801,-0.0346945769586931,
0.0794982455707389));
#67721=CARTESIAN_POINT('Ctrl Pts',(0.00611907697022586,-0.034529677707698,
0.0795419774139132));
#67722=CARTESIAN_POINT('Ctrl Pts',(0.0062313611586656,-0.034364806625142,
0.0795811018797661));
#67723=CARTESIAN_POINT('Ctrl Pts',(0.00613605465547,-0.0346945769586931,
0.0798111782551212));
#67724=CARTESIAN_POINT('Ctrl Pts',(0.00625309551017338,-0.034529677707698,
0.0798522731154911));
#67725=CARTESIAN_POINT('Ctrl Pts',(0.00637173484327099,-0.034364806625142,
0.07988849545474));
#67726=CARTESIAN_POINT('',(0.00614815156770165,-0.0346775396665006,0.0798154111612007));
#67727=CARTESIAN_POINT('',(0.00613605465546712,-0.0346945769586885,0.0798111782551075));
#67728=CARTESIAN_POINT('Origin',(0.01147015549346,-0.0345626617707366,0.0640899802503613));
#67729=CARTESIAN_POINT('Ctrl Pts',(0.00614815156654657,-0.0346775396670096,
0.0798154111597802));
#67730=CARTESIAN_POINT('Ctrl Pts',(0.00616229647183186,-0.0346269749928212,
0.0797748485259631));
#67731=CARTESIAN_POINT('Ctrl Pts',(0.00617618995667073,-0.0345757902890838,
0.0797350067688319));
#67732=CARTESIAN_POINT('Ctrl Pts',(0.00620348569030341,-0.0344721681087949,
0.0796567322526532));
#67733=CARTESIAN_POINT('Ctrl Pts',(0.00621687724320778,-0.034419771428959,
0.0796183301827554));
#67734=CARTESIAN_POINT('Ctrl Pts',(0.00623002218355715,-0.0343667727830716,
0.0795806351403776));
#67735=CARTESIAN_POINT('',(0.00607228021642176,-0.0346945769587026,0.0796547119129349));
#67736=CARTESIAN_POINT('Origin',(0.00812378219310841,-0.0315241814719618,
0.07415));
#67737=CARTESIAN_POINT('',(0.00614815156878709,-0.0347116136489779,0.0798154111603306));
#67738=CARTESIAN_POINT('',(0.00616025749492668,-0.0346945769586885,0.0798196182199215));
#67739=CARTESIAN_POINT('Origin',(0.0114267900940531,-0.0345626675620375,
0.0640768340854252));
#67740=CARTESIAN_POINT('Origin',(0.0117585564508999,-0.0345626632792103,
0.0641905470644617));
#67741=CARTESIAN_POINT('Origin',(0.0118006907407996,-0.0345626691098713,
0.0642072234592839));
#67742=CARTESIAN_POINT('Ctrl Pts',(0.00607630495006719,-0.0352450361874068,
0.0795246249347493));
#67743=CARTESIAN_POINT('Ctrl Pts',(0.00627901225575353,-0.0349452760959492,
0.0796018468061226));
#67744=CARTESIAN_POINT('Ctrl Pts',(0.00648696035864053,-0.034644428984174,
0.0796635805546132));
#67745=CARTESIAN_POINT('Ctrl Pts',(0.00607866032480437,-0.0352450361874068,
0.0795254629143717));
#67746=CARTESIAN_POINT('Ctrl Pts',(0.00628139923541077,-0.0349452760959492,
0.079602595951329));
#67747=CARTESIAN_POINT('Ctrl Pts',(0.0064893721620599,-0.034644428984174,
0.0796642387371611));
#67748=CARTESIAN_POINT('Ctrl Pts',(0.00631419779852133,-0.0352450361874068,
0.0796092608766085));
#67749=CARTESIAN_POINT('Ctrl Pts',(0.00652009720113476,-0.0349452760959492,
0.0796775104719741));
#67750=CARTESIAN_POINT('Ctrl Pts',(0.00673055250399705,-0.034644428984174,
0.0797300569919472));
#67751=CARTESIAN_POINT('',(0.0063484673055885,-0.0351951633467143,0.0796205032826253));
#67752=CARTESIAN_POINT('',(0.0065747514882603,-0.0348678972925388,0.0796888291971714));
#67753=CARTESIAN_POINT('Origin',(0.010679534327633,-0.0345636767885608,
0.063445017347961));
#67754=CARTESIAN_POINT('Origin',(0.00359866410323816,-0.0346946199340881,
0.0903303466244583));
#67755=CARTESIAN_POINT('',(0.00645473648111493,-0.0346945769330289,0.0796538542322125));
#67756=CARTESIAN_POINT('',(0.00651492693357118,-0.0346945769458128,0.0796706875480123));
#67757=CARTESIAN_POINT('',(0.00623002218362052,-0.0350221583435276,0.0795806351402451));
#67758=CARTESIAN_POINT('Origin',(0.0111519882768809,-0.0345628458717012,
0.0635340715940157));
#67759=CARTESIAN_POINT('',(0.0062304265988768,-0.035195136029876,0.0795794662343274));
#67760=CARTESIAN_POINT('Origin',(0.00260219061514371,-0.0351951838366748,
0.0899839723495549));
#67761=CARTESIAN_POINT('',(0.00634849890504161,-0.0351951371328747,0.0796205113332404));
#67762=CARTESIAN_POINT('Ctrl Pts',(0.00592760524173035,-0.0350241211494343,
0.0797336195069392));
#67763=CARTESIAN_POINT('Ctrl Pts',(0.00600451731106532,-0.0349144232818962,
0.0797638709439768));
#67764=CARTESIAN_POINT('Ctrl Pts',(0.00608210073480112,-0.0348045283579412,
0.0797925506605261));
#67765=CARTESIAN_POINT('Ctrl Pts',(0.00616025750542763,-0.0346945769439157,
0.0798196182235583));
#67766=CARTESIAN_POINT('Ctrl Pts',(0.00602856701548103,-0.0350241211494343,
0.0796821621260871));
#67767=CARTESIAN_POINT('Ctrl Pts',(0.00610477028049311,-0.0349144232818962,
0.0797110228560873));
#67768=CARTESIAN_POINT('Ctrl Pts',(0.00618161572874426,-0.0348045283579412,
0.0797383256846858));
#67769=CARTESIAN_POINT('Ctrl Pts',(0.00625900623234884,-0.0346945769439157,
0.0797640319776473));
#67770=CARTESIAN_POINT('Ctrl Pts',(0.00612952878923171,-0.0350241211494343,
0.0796307047452351));
#67771=CARTESIAN_POINT('Ctrl Pts',(0.0062050232499209,-0.0349144232818962,
0.0796581747681978));
#67772=CARTESIAN_POINT('Ctrl Pts',(0.0062811307226874,-0.0348045283579412,
0.0796841007088454));
#67773=CARTESIAN_POINT('Ctrl Pts',(0.00635775495927005,-0.0346945769439157,
0.0797084457317363));
#67774=CARTESIAN_POINT('Ctrl Pts',(0.0062304905629824,-0.0350241211494343,
0.0795792473643831));
#67775=CARTESIAN_POINT('Ctrl Pts',(0.00630527621934869,-0.0349144232818962,
0.0796053266803083));
#67776=CARTESIAN_POINT('Ctrl Pts',(0.00638064571663054,-0.0348045283579412,
0.079629875733005));
#67777=CARTESIAN_POINT('Ctrl Pts',(0.00645650368619125,-0.0346945769439157,
0.0796528594858253));
#67778=CARTESIAN_POINT('',(0.00630749698772211,-0.0346945769458128,0.0797367362260666));
#67779=CARTESIAN_POINT('Ctrl Pts',(0.00614815156986566,-0.034711613649279,
0.079815411157218));
#67780=CARTESIAN_POINT('Ctrl Pts',(0.00616229087005735,-0.0347621546532189,
0.079774864635961));
#67781=CARTESIAN_POINT('Ctrl Pts',(0.00617618156314332,-0.0348133084096807,
0.0797350310321158));
#67782=CARTESIAN_POINT('Ctrl Pts',(0.00620347732784562,-0.0349168561544566,
0.079656756415358));
#67783=CARTESIAN_POINT('Ctrl Pts',(0.00621687157260909,-0.0349692089015912,
0.0796183464500372));
#67784=CARTESIAN_POINT('Ctrl Pts',(0.00623002218365135,-0.0350221583435,
0.0795806351402172));
#67785=CARTESIAN_POINT('Ctrl Pts',(0.00634786272464048,-0.035195137125491,
0.0796191938798822));
#67786=CARTESIAN_POINT('Ctrl Pts',(0.00646093487661855,-0.0350307338980939,
0.0796559099006431));
#67787=CARTESIAN_POINT('Ctrl Pts',(0.00657542792186249,-0.0348659306897824,
0.0796879211537307));
#67788=CARTESIAN_POINT('Ctrl Pts',(0.0063484989101211,-0.035195137125491,
0.0796205113348887));
#67789=CARTESIAN_POINT('Ctrl Pts',(0.00646159829965483,-0.0350307338980939,
0.079657214202914));
#67790=CARTESIAN_POINT('Ctrl Pts',(0.00657611801556334,-0.0348659306897824,
0.0796892111887473));
#67791=CARTESIAN_POINT('Ctrl Pts',(0.00645512425971208,-0.035195137125491,
0.0798413181670515));
#67792=CARTESIAN_POINT('Ctrl Pts',(0.00657278869196188,-0.0350307338980939,
0.0798758166228729));
#67793=CARTESIAN_POINT('Ctrl Pts',(0.00669177843904926,-0.0348659306897824,
0.0799054224020185));
#67794=CARTESIAN_POINT('Origin',(0.00514238959704072,-0.0308609197409829,
0.0848104887221482));
#67795=CARTESIAN_POINT('',(0.00639498515845967,-0.035195137125491,0.0797167781351773));
#67796=CARTESIAN_POINT('Origin',(0.00824783221874499,-0.0351840467441202,
0.0731807955630989));
#67797=CARTESIAN_POINT('Origin',(0.00567356812171042,-0.035232261387866,
0.0858617980372858));
#67798=CARTESIAN_POINT('',(0.00680393225277577,-0.0351951142564674,0.0797478398260794));
#67799=CARTESIAN_POINT('',(0.00692587718847221,-0.0351951372916787,0.0797738353105215));
#67800=CARTESIAN_POINT('Origin',(0.00844465116790654,-0.0352875118344055,
0.0740358531781859));
#67801=CARTESIAN_POINT('Origin',(0.00122044656463087,-0.029832507652323,
0.0712107573289516));
#67802=CARTESIAN_POINT('Origin',(0.00342050335947712,-0.0338732948498643,
0.0810873635885459));
#67803=CARTESIAN_POINT('Ctrl Pts',(0.00376541898641349,-0.0321934096636941,
0.0779027064771762));
#67804=CARTESIAN_POINT('Ctrl Pts',(0.00383259064532129,-0.032050846084365,
0.0779807191031296));
#67805=CARTESIAN_POINT('Ctrl Pts',(0.0039018077019054,-0.0319086045661724,
0.0780568681373702));
#67806=CARTESIAN_POINT('Ctrl Pts',(0.00397290762127662,-0.0317669892865887,
0.0781310018872401));
#67807=CARTESIAN_POINT('Ctrl Pts',(0.0038214972944457,-0.0321934096636941,
0.077965041507425));
#67808=CARTESIAN_POINT('Ctrl Pts',(0.00388978472071109,-0.032050846084365,
0.0780420503583689));
#67809=CARTESIAN_POINT('Ctrl Pts',(0.00396008973390662,-0.0319086045661724,
0.0781171663959826));
#67810=CARTESIAN_POINT('Ctrl Pts',(0.00403224763969298,-0.0317669892865887,
0.0781902403446855));
#67811=CARTESIAN_POINT('Ctrl Pts',(0.0038775756024779,-0.0321934096636941,
0.0780273765376737));
#67812=CARTESIAN_POINT('Ctrl Pts',(0.00394697879610091,-0.032050846084365,
0.0781033816136083));
#67813=CARTESIAN_POINT('Ctrl Pts',(0.00401837176590785,-0.0319086045661724,
0.078177464654595));
#67814=CARTESIAN_POINT('Ctrl Pts',(0.00409158765810936,-0.0317669892865887,
0.078249478802131));
#67815=CARTESIAN_POINT('Ctrl Pts',(0.00393365391051011,-0.0321934096636941,
0.0780897115679225));
#67816=CARTESIAN_POINT('Ctrl Pts',(0.00400417287149071,-0.032050846084365,
0.0781647128688477));
#67817=CARTESIAN_POINT('Ctrl Pts',(0.00407665379790908,-0.0319086045661724,
0.0782377629132073));
#67818=CARTESIAN_POINT('Ctrl Pts',(0.00415092767652572,-0.0317669892865887,
0.0783087172595763));
#67819=CARTESIAN_POINT('',(0.0039326506584995,-0.0321934096636941,0.0780885963819116));
#67820=CARTESIAN_POINT('',(0.00409800492356571,-0.0318665617511309,0.0782574617910789));
#67821=CARTESIAN_POINT('Origin',(0.0165223001385245,-0.0326371944419616,
0.0671013933342569));
#67822=CARTESIAN_POINT('Origin',(-0.00357449398580896,-0.0316939261508776,
0.0860856385078435));
#67823=CARTESIAN_POINT('',(0.00384825053644379,-0.0320197221621765,0.0779967412467433));
#67824=CARTESIAN_POINT('Ctrl Pts',(0.0038483350865036,-0.0320197392094679,
0.077996905764728));
#67825=CARTESIAN_POINT('Ctrl Pts',(0.00386790941467717,-0.0319792716575976,
0.0780186605827307));
#67826=CARTESIAN_POINT('Ctrl Pts',(0.0038877387026203,-0.0319386439829627,
0.0780403652101468));
#67827=CARTESIAN_POINT('Ctrl Pts',(0.00390785001136752,-0.0318979099381559,
0.0780620367281972));
#67828=CARTESIAN_POINT('Ctrl Pts',(0.00392796092259969,-0.0318571766984879,
0.0780837078178938));
#67829=CARTESIAN_POINT('Ctrl Pts',(0.0039482503207249,-0.0318163871833547,
0.0781052368648544));
#67830=CARTESIAN_POINT('Ctrl Pts',(0.00396864585605781,-0.0317755399638304,
0.0781265522329901));
#67831=CARTESIAN_POINT('',(0.00384904919316622,-0.0321934096636183,0.0779956674036122));
#67832=CARTESIAN_POINT('Origin',(0.00212289893016235,-0.0324157424817443,
0.0795772528035699));
#67833=CARTESIAN_POINT('',(0.00389084992584285,-0.0321934096636663,0.0780421318927719));
#67834=CARTESIAN_POINT('Ctrl Pts',(0.00393275767635423,-0.0321934096636618,
0.0780865709845288));
#67835=CARTESIAN_POINT('Ctrl Pts',(0.00398704605821487,-0.0320835708272592,
0.0781443684789084));
#67836=CARTESIAN_POINT('Ctrl Pts',(0.00404249906675006,-0.0319739230346488,
0.0782010089531512));
#67837=CARTESIAN_POINT('Ctrl Pts',(0.00409904019200004,-0.0318646057455572,
0.0782564253847822));
#67838=CARTESIAN_POINT('Ctrl Pts',(0.00392677847664008,-0.0321934096636618,
0.0781997319934329));
#67839=CARTESIAN_POINT('Ctrl Pts',(0.00398262743700604,-0.0320835708272592,
0.0782576119456364));
#67840=CARTESIAN_POINT('Ctrl Pts',(0.00403964182530797,-0.0319739230346488,
0.0783143025337832));
#67841=CARTESIAN_POINT('Ctrl Pts',(0.00409774312898821,-0.0318646057455572,
0.0783697368245971));
#67842=CARTESIAN_POINT('Ctrl Pts',(0.00392079927692593,-0.0321934096636617,
0.0783128930023369));
#67843=CARTESIAN_POINT('Ctrl Pts',(0.0039782088157972,-0.0320835708272592,
0.0783708554123644));
#67844=CARTESIAN_POINT('Ctrl Pts',(0.00403678458386588,-0.0319739230346488,
0.0784275961144152));
#67845=CARTESIAN_POINT('Ctrl Pts',(0.00409644606597639,-0.0318646057455572,
0.078483048264412));
#67846=CARTESIAN_POINT('Ctrl Pts',(0.00391482007721177,-0.0321934096636617,
0.0784260540112409));
#67847=CARTESIAN_POINT('Ctrl Pts',(0.00397379019458837,-0.0320835708272592,
0.0784840988790923));
#67848=CARTESIAN_POINT('Ctrl Pts',(0.00403392734242379,-0.0319739230346488,
0.0785408896950472));
#67849=CARTESIAN_POINT('Ctrl Pts',(0.00409514900296457,-0.0318646057455572,
0.078596359704227));
#67850=CARTESIAN_POINT('',(0.00392396340836445,-0.0321763980308298,0.0784350346734988));
#67851=CARTESIAN_POINT('',(0.00391482007723565,-0.0321934096636184,0.0784260540112524));
#67852=CARTESIAN_POINT('Origin',(0.0159370310552557,-0.0326386231710662,
0.0670546876297493));
#67853=CARTESIAN_POINT('Ctrl Pts',(0.00392396341057931,-0.0321763980306338,
0.0784350346712286));
#67854=CARTESIAN_POINT('Ctrl Pts',(0.00395400533963687,-0.0321259596176027,
0.0784043831802315));
#67855=CARTESIAN_POINT('Ctrl Pts',(0.0039835267532891,-0.0320749164633809,
0.0783742627660816));
#67856=CARTESIAN_POINT('Ctrl Pts',(0.00404155230793302,-0.0319716057793957,
0.0783150598513033));
#67857=CARTESIAN_POINT('Ctrl Pts',(0.0040700338400219,-0.0319193786690148,
0.0782860004183207));
#67858=CARTESIAN_POINT('Ctrl Pts',(0.00409800492485757,-0.0318665617525349,
0.0782574617897467));
#67859=CARTESIAN_POINT('',(0.00392373536787758,-0.0321934096636663,0.078257325196592));
#67860=CARTESIAN_POINT('Origin',(0.00812378219310841,-0.0315241814719618,
0.07415));
#67861=CARTESIAN_POINT('',(0.00392396340810453,-0.0322104233323765,0.0784350346737633));
#67862=CARTESIAN_POINT('',(0.00393312589888556,-0.0321934096636183,0.0784439957875769));
#67863=CARTESIAN_POINT('Origin',(0.0159093932547248,-0.0326387224835572,
0.067018750192623));
#67864=CARTESIAN_POINT('Origin',(0.015060738398086,-0.0326386249044207,
0.0661958168573123));
#67865=CARTESIAN_POINT('Origin',(0.0150972187277074,-0.0326387239258707,
0.0662227328979937));
#67866=CARTESIAN_POINT('Ctrl Pts',(0.00398450838954435,-0.0327445246967095,
0.078143061153943));
#67867=CARTESIAN_POINT('Ctrl Pts',(0.00413510915295419,-0.0324436878339359,
0.0782991764175831));
#67868=CARTESIAN_POINT('Ctrl Pts',(0.00429704131520911,-0.0321434074405927,
0.0784435043092344));
#67869=CARTESIAN_POINT('Ctrl Pts',(0.00416194824489146,-0.0327445246967095,
0.0783191721920251));
#67870=CARTESIAN_POINT('Ctrl Pts',(0.00431919114468679,-0.0324436878339359,
0.0784685952021174));
#67871=CARTESIAN_POINT('Ctrl Pts',(0.00448724248583043,-0.0321434074405927,
0.078605749539347));
#67872=CARTESIAN_POINT('',(0.00418822741220764,-0.0326943950436612,0.0783439877880759));
#67873=CARTESIAN_POINT('',(0.00436385853458972,-0.0323666188837389,0.0785021373004665));
#67874=CARTESIAN_POINT('Origin',(0.0156361235182012,-0.0326395579108916,
0.0660332716046196));
#67875=CARTESIAN_POINT('Origin',(-0.00285650192840184,-0.0321933825603126,
0.0868597545804409));
#67876=CARTESIAN_POINT('',(0.00427015733382251,-0.032193409653269,0.0784193911088875));
#67877=CARTESIAN_POINT('',(0.00431745200174686,-0.0321934096584275,0.0784602501927232));
#67878=CARTESIAN_POINT('',(0.00409800492289456,-0.032521010975624,0.0782574617917432));
#67879=CARTESIAN_POINT('Origin',(0.0159688902513804,-0.0326393129162593,
0.0663803317319811));
#67880=CARTESIAN_POINT('',(0.00409895585648136,-0.0326943950436592,0.0782564915633657));
#67881=CARTESIAN_POINT('Origin',(-0.00364442915373624,-0.0326943765538,
0.0861569918797376));
#67882=CARTESIAN_POINT('',(0.0041435916343545,-0.0326943950436702,0.0783002396757309));
#67883=CARTESIAN_POINT('Ctrl Pts',(0.00375923155673887,-0.0325229783203769,
0.0782671225076021));
#67884=CARTESIAN_POINT('Ctrl Pts',(0.00381598600047065,-0.032413025309245,
0.0783272877426781));
#67885=CARTESIAN_POINT('Ctrl Pts',(0.00387397643145428,-0.032303122220807,
0.0783862698139424));
#67886=CARTESIAN_POINT('Ctrl Pts',(0.00393312590209474,-0.0321934096576658,
0.0784439957907088));
#67887=CARTESIAN_POINT('Ctrl Pts',(0.0038724939906298,-0.0325229783203769,
0.0782635499307282));
#67888=CARTESIAN_POINT('Ctrl Pts',(0.0039291991864675,-0.032413025309245,
0.0783221538456299));
#67889=CARTESIAN_POINT('Ctrl Pts',(0.003987108079113,-0.032303122220807,
0.0783795758522807));
#67890=CARTESIAN_POINT('Ctrl Pts',(0.00404614389593064,-0.0321934096576658,
0.0784357450146406));
#67891=CARTESIAN_POINT('Ctrl Pts',(0.00398575642452073,-0.0325229783203769,
0.0782599773538543));
#67892=CARTESIAN_POINT('Ctrl Pts',(0.00404241237246435,-0.032413025309245,
0.0783170199485817));
#67893=CARTESIAN_POINT('Ctrl Pts',(0.00410023972677172,-0.032303122220807,
0.078372881890619));
#67894=CARTESIAN_POINT('Ctrl Pts',(0.00415916188976654,-0.0321934096576658,
0.0784274942385725));
#67895=CARTESIAN_POINT('Ctrl Pts',(0.00409901885841167,-0.0325229783203769,
0.0782564047769805));
#67896=CARTESIAN_POINT('Ctrl Pts',(0.00415562555846121,-0.032413025309245,
0.0783118860515336));
#67897=CARTESIAN_POINT('Ctrl Pts',(0.00421337137443044,-0.032303122220807,
0.0783661879289573));
#67898=CARTESIAN_POINT('Ctrl Pts',(0.00427217988360243,-0.0321934096576658,
0.0784192434625043));
#67899=CARTESIAN_POINT('',(0.00410164161590011,-0.0321934096584275,0.0784316934480136));
#67900=CARTESIAN_POINT('Ctrl Pts',(0.00392396341053566,-0.0322104233328918,
0.0784350346712731));
#67901=CARTESIAN_POINT('Ctrl Pts',(0.0039540460469616,-0.032260942183138,
0.0784043416469399));
#67902=CARTESIAN_POINT('Ctrl Pts',(0.00398358734687533,-0.0323120888240771,
0.0783742009430386));
#67903=CARTESIAN_POINT('Ctrl Pts',(0.00404161334071153,-0.0324156524631808,
0.0783149975801566));
#67904=CARTESIAN_POINT('Ctrl Pts',(0.00407007418291316,-0.0324680267167307,
0.0782859592568571));
#67905=CARTESIAN_POINT('Ctrl Pts',(0.00409800492292809,-0.0325210109755913,
0.0782574617917153));
#67906=CARTESIAN_POINT('Origin',(0.00320893444532068,-0.0262834582511651,
0.0680060877728064));
#67907=CARTESIAN_POINT('Origin',(-0.0033720415137391,-0.0342770802866463,
0.0781084632927795));
#67908=CARTESIAN_POINT('Ctrl Pts',(0.00418820704813744,-0.0326943950436604,
0.0783419601598709));
#67909=CARTESIAN_POINT('Ctrl Pts',(0.00424598011571114,-0.0325844576448134,
0.0783961997614225));
#67910=CARTESIAN_POINT('Ctrl Pts',(0.00430487903586174,-0.0324744968375322,
0.0784492483598374));
#67911=CARTESIAN_POINT('Ctrl Pts',(0.00436482740636163,-0.0323646534831894,
0.078501039027043));
#67912=CARTESIAN_POINT('Ctrl Pts',(0.00418934508390059,-0.0326943950436604,
0.0784552731443737));
#67913=CARTESIAN_POINT('Ctrl Pts',(0.00424867981677191,-0.0325844576448134,
0.0785094970616596));
#67914=CARTESIAN_POINT('Ctrl Pts',(0.00430914018836527,-0.0324744968375322,
0.0785624976769));
#67915=CARTESIAN_POINT('Ctrl Pts',(0.0043706477966784,-0.0323646534831894,
0.0786142081510959));
#67916=CARTESIAN_POINT('Ctrl Pts',(0.00419048311966374,-0.0326943950436604,
0.0785685861288765));
#67917=CARTESIAN_POINT('Ctrl Pts',(0.00425137951783268,-0.0325844576448134,
0.0786227943618967));
#67918=CARTESIAN_POINT('Ctrl Pts',(0.0043134013408688,-0.0324744968375322,
0.0786757469939626));
#67919=CARTESIAN_POINT('Ctrl Pts',(0.00437646818699518,-0.0323646534831894,
0.0787273772751487));
#67920=CARTESIAN_POINT('Ctrl Pts',(0.00419162115542689,-0.0326943950436604,
0.0786818991133793));
#67921=CARTESIAN_POINT('Ctrl Pts',(0.00425407921889344,-0.0325844576448134,
0.0787360916621338));
#67922=CARTESIAN_POINT('Ctrl Pts',(0.00431766249337233,-0.0324744968375322,
0.0787889963110252));
#67923=CARTESIAN_POINT('Ctrl Pts',(0.00438228857731196,-0.0323646534831894,
0.0788405463992016));
#67924=CARTESIAN_POINT('',(0.00420131034459516,-0.0326773559991372,0.0786902879399716));
#67925=CARTESIAN_POINT('',(0.00419162115542731,-0.0326943950436594,0.0786818991133677));
#67926=CARTESIAN_POINT('Origin',(0.0150188268209347,-0.0326395669851025,
0.0660920879965544));
#67927=CARTESIAN_POINT('Ctrl Pts',(0.00420131034678007,-0.0326773559987487,
0.0786902879374314));
#67928=CARTESIAN_POINT('Ctrl Pts',(0.00422939095110529,-0.0326267922587177,
0.0786577844462431));
#67929=CARTESIAN_POINT('Ctrl Pts',(0.00425697384699894,-0.0325756109581761,
0.0786258570559618));
#67930=CARTESIAN_POINT('Ctrl Pts',(0.00431116769657224,-0.032471998546238,
0.0785631273051464));
#67931=CARTESIAN_POINT('Ctrl Pts',(0.00433775691439304,-0.0324196091621782,
0.0785323501040173));
#67932=CARTESIAN_POINT('Ctrl Pts',(0.00436385853462161,-0.0323666188837756,
0.0785021373004296));
#67933=CARTESIAN_POINT('',(0.00418992428382747,-0.0326943950436702,0.0785129434507318));
#67934=CARTESIAN_POINT('Origin',(0.00812378219310841,-0.0315241814719618,
0.07415));
#67935=CARTESIAN_POINT('',(0.00420131034462419,-0.0327114338380035,0.0786902879399374));
#67936=CARTESIAN_POINT('',(0.00421101742817708,-0.0326943950436593,0.0786986560536431));
#67937=CARTESIAN_POINT('Origin',(0.014984038863885,-0.0326395658097383,
0.0660630537460898));
#67938=CARTESIAN_POINT('Origin',(0.0150948635439747,-0.0326395684242205,
0.0661577736041775));
#67939=CARTESIAN_POINT('Origin',(0.0151286377925338,-0.0326395672933506,
0.0661879811385929));
#67940=CARTESIAN_POINT('Ctrl Pts',(0.00424343163642233,-0.0332451089994433,
0.0783951153761972));
#67941=CARTESIAN_POINT('Ctrl Pts',(0.00440353878232574,-0.0329451141710254,
0.0785414651918511));
#67942=CARTESIAN_POINT('Ctrl Pts',(0.00457421474712319,-0.0326442513127493,
0.0786753393183718));
#67943=CARTESIAN_POINT('Ctrl Pts',(0.00443158058102485,-0.0332451089994433,
0.0785597360755183));
#67944=CARTESIAN_POINT('Ctrl Pts',(0.00459789649818397,-0.0329451141710254,
0.0786989897376274));
#67945=CARTESIAN_POINT('Ctrl Pts',(0.00477422908447897,-0.0326442513127493,
0.0788253201999939));
#67946=CARTESIAN_POINT('Ctrl Pts',(0.00443346207047087,-0.0332451089994433,
0.0785613822825115));
#67947=CARTESIAN_POINT('Ctrl Pts',(0.00459984007534255,-0.0329451141710254,
0.0787005649830851));
#67948=CARTESIAN_POINT('Ctrl Pts',(0.00477622922785252,-0.0326442513127493,
0.0788268200088102));
#67949=CARTESIAN_POINT('',(0.00445933600268922,-0.0331951640388616,0.0785828274405308));
#67950=CARTESIAN_POINT('',(0.00464455085464897,-0.032867753235502,0.0787296369248357));
#67951=CARTESIAN_POINT('Origin',(0.01453730406965,-0.0326402808282098,0.0651863052379474));
#67952=CARTESIAN_POINT('Origin',(-0.00204335396685721,-0.0326944278779124,
0.0875334038494764));
#67953=CARTESIAN_POINT('',(0.00454583887293236,-0.0326943950436593,0.078652937552044));
#67954=CARTESIAN_POINT('',(0.00459560577674832,-0.0326943950436694,0.0786907463511037));
#67955=CARTESIAN_POINT('',(0.0043638585345876,-0.0330220786163546,0.0785021373004647));
#67956=CARTESIAN_POINT('Origin',(0.0149383253770748,-0.0326396682765928,
0.0654515118674726));
#67957=CARTESIAN_POINT('',(0.00436474667057916,-0.0331951640388587,0.0785011092769963));
#67958=CARTESIAN_POINT('Origin',(-0.00284714542766966,-0.0331952026560193,
0.0868489222798781));
#67959=CARTESIAN_POINT('',(0.00441204133664418,-0.0331951640388701,0.0785419683587736));
#67960=CARTESIAN_POINT('Ctrl Pts',(0.00402636096358964,-0.0330240426238173,
0.0785330513649649));
#67961=CARTESIAN_POINT('Ctrl Pts',(0.00408674176634207,-0.032914277406352,
0.0785894973343257));
#67962=CARTESIAN_POINT('Ctrl Pts',(0.00414831956698752,-0.0328043479726691,
0.0786447232042023));
#67963=CARTESIAN_POINT('Ctrl Pts',(0.00421101742817707,-0.0326943950436593,
0.0786986560536431));
#67964=CARTESIAN_POINT('Ctrl Pts',(0.00413917554680919,-0.0330240426238173,
0.0785223740152204));
#67965=CARTESIAN_POINT('Ctrl Pts',(0.00419940925866645,-0.032914277406352,
0.0785772658537874));
#67966=CARTESIAN_POINT('Ctrl Pts',(0.0042608077668618,-0.0328043479726691,
0.078630939858859));
#67967=CARTESIAN_POINT('Ctrl Pts',(0.00432329430898262,-0.0326943950436593,
0.0786833251038636));
#67968=CARTESIAN_POINT('Ctrl Pts',(0.00425199013002873,-0.0330240426238173,
0.0785116966654759));
#67969=CARTESIAN_POINT('Ctrl Pts',(0.00431207675099082,-0.032914277406352,
0.078565034373249));
#67970=CARTESIAN_POINT('Ctrl Pts',(0.00437329596673607,-0.0328043479726691,
0.0786171565135158));
#67971=CARTESIAN_POINT('Ctrl Pts',(0.00443557118978818,-0.0326943950436593,
0.078667994154084));
#67972=CARTESIAN_POINT('Ctrl Pts',(0.00436480471324827,-0.0330240426238173,
0.0785010193157314));
#67973=CARTESIAN_POINT('Ctrl Pts',(0.0044247442433152,-0.032914277406352,
0.0785528028927107));
#67974=CARTESIAN_POINT('Ctrl Pts',(0.00448578416661034,-0.0328043479726691,
0.0786033731681725));
#67975=CARTESIAN_POINT('Ctrl Pts',(0.00454784807059373,-0.0326943950436593,
0.0786526632043045));
#67976=CARTESIAN_POINT('',(0.00437842815056471,-0.0326943950436694,0.0786757968028536));
#67977=CARTESIAN_POINT('Ctrl Pts',(0.00420131034678774,-0.0327114338383316,
0.0786902879374224));
#67978=CARTESIAN_POINT('Ctrl Pts',(0.00422938628036045,-0.0327619876829319,
0.078657789852662));
#67979=CARTESIAN_POINT('Ctrl Pts',(0.00425696689483702,-0.0328131562600878,
0.0786258651031487));
#67980=CARTESIAN_POINT('Ctrl Pts',(0.00431116069478636,-0.0329167375860513,
0.0785631354097734));
#67981=CARTESIAN_POINT('Ctrl Pts',(0.00433775228638831,-0.032969108892433,
0.0785323554609643));
#67982=CARTESIAN_POINT('Ctrl Pts',(0.00436385853462079,-0.0330220786163188,
0.0785021373004306));
#67983=CARTESIAN_POINT('Ctrl Pts',(0.00445918833940328,-0.0331951640388604,
0.0785808047691941));
#67984=CARTESIAN_POINT('Ctrl Pts',(0.00455079238723864,-0.0330306422010619,
0.0786565678976004));
#67985=CARTESIAN_POINT('Ctrl Pts',(0.00464544952982838,-0.0328657861914645,
0.0787284801953144));
#67986=CARTESIAN_POINT('Ctrl Pts',(0.00445933600268683,-0.0331951640388604,
0.0785828274405288));
#67987=CARTESIAN_POINT('Ctrl Pts',(0.00455098186795523,-0.0330306422010619,
0.0786585875160914));
#67988=CARTESIAN_POINT('Ctrl Pts',(0.00464568066606805,-0.0328657861914645,
0.0787304950352118));
#67989=CARTESIAN_POINT('Ctrl Pts',(0.00448394067680124,-0.0331951640388604,
0.0789198588801225));
#67990=CARTESIAN_POINT('Ctrl Pts',(0.00458255445099879,-0.0330306422010619,
0.0789951102698229));
#67991=CARTESIAN_POINT('Ctrl Pts',(0.00468419417948977,-0.0328657861914645,
0.0790662215467457));
#67992=CARTESIAN_POINT('',(0.00449413748404394,-0.0331781648281924,0.0789276227647071));
#67993=CARTESIAN_POINT('',(0.00448394067680124,-0.0331951640388588,0.0789198588801103));
#67994=CARTESIAN_POINT('Origin',(0.0139127037144764,-0.0326412092261607,
0.065352752982653));
#67995=CARTESIAN_POINT('Ctrl Pts',(0.00449413748348554,-0.033178164828644,
0.0789276227629457));
#67996=CARTESIAN_POINT('Ctrl Pts',(0.00452013964558557,-0.0331276811546787,
0.0788933966597935));
#67997=CARTESIAN_POINT('Ctrl Pts',(0.00454567226223526,-0.0330765663497806,
0.0788597885536142));
#67998=CARTESIAN_POINT('Ctrl Pts',(0.00459582047074767,-0.0329730614463256,
0.0787937795580319));
#67999=CARTESIAN_POINT('Ctrl Pts',(0.00462041580809327,-0.0329207133374001,
0.0787614053380697));
#68000=CARTESIAN_POINT('Ctrl Pts',(0.00464455083824491,-0.0328677532289377,
0.0787296369233164));
#68001=CARTESIAN_POINT('',(0.00447163833975523,-0.0331951640388701,0.0787513431603306));
#68002=CARTESIAN_POINT('Origin',(0.00812378219310841,-0.0315241814719618,
0.07415));
#68003=CARTESIAN_POINT('',(0.00449413748549661,-0.0332121607144209,0.0789276227638636));
#68004=CARTESIAN_POINT('',(0.00450435085242291,-0.0331951640388587,0.0789353648523489));
#68005=CARTESIAN_POINT('Origin',(0.0138723966468389,-0.0326413639619036,
0.0653319760184241));
#68006=CARTESIAN_POINT('Origin',(0.0150470180937759,-0.0326412103396109,
0.0662145069192957));
#68007=CARTESIAN_POINT('Origin',(0.0150778355420318,-0.0326413655861837,
0.0662477737448309));
#68008=CARTESIAN_POINT('Ctrl Pts',(0.00451762539374549,-0.0337436976235975,
0.0786303747765571));
#68009=CARTESIAN_POINT('Ctrl Pts',(0.00455792256350522,-0.0336723290703325,
0.0786628090973386));
#68010=CARTESIAN_POINT('Ctrl Pts',(0.00459879660533242,-0.033601104548885,
0.0786945133519412));
#68011=CARTESIAN_POINT('Ctrl Pts',(0.00472929932419518,-0.0333736987606857,
0.0787957387566284));
#68012=CARTESIAN_POINT('Ctrl Pts',(0.00486539588228306,-0.0331450831799191,
0.0788893083513764));
#68013=CARTESIAN_POINT('Ctrl Pts',(0.00471573913632553,-0.0337436976235975,
0.0787828573821255));
#68014=CARTESIAN_POINT('Ctrl Pts',(0.00475740775774911,-0.0336723290703325,
0.0788135098378812));
#68015=CARTESIAN_POINT('Ctrl Pts',(0.00479962097923611,-0.033601104548885,
0.0788434078476292));
#68016=CARTESIAN_POINT('Ctrl Pts',(0.00493439943347605,-0.0333736987606857,
0.0789388662702924));
#68017=CARTESIAN_POINT('Ctrl Pts',(0.00507443373818682,-0.0331450831799191,
0.079026433020197));
#68018=CARTESIAN_POINT('Ctrl Pts',(0.00471772027375133,-0.0337436976235975,
0.0787843822081812));
#68019=CARTESIAN_POINT('Ctrl Pts',(0.00475940260969155,-0.0336723290703325,
0.0788150168452867));
#68020=CARTESIAN_POINT('Ctrl Pts',(0.00480162922297515,-0.033601104548885,
0.0788448967925861));
#68021=CARTESIAN_POINT('Ctrl Pts',(0.00493645043456887,-0.0333736987606857,
0.0789402975454291));
#68022=CARTESIAN_POINT('Ctrl Pts',(0.00507652411674586,-0.0331450831799191,
0.0790278042668852));
#68023=CARTESIAN_POINT('',(0.00474490648816895,-0.0336938721132548,0.0788041727482519));
#68024=CARTESIAN_POINT('',(0.00493897410253327,-0.0333679869945434,0.0789390627920544));
#68025=CARTESIAN_POINT('Ctrl Pts',(0.00474490648817959,-0.0336938721132648,
0.078804172748261));
#68026=CARTESIAN_POINT('Ctrl Pts',(0.00476307390772768,-0.0336629187933932,
0.0788173620851958));
#68027=CARTESIAN_POINT('Ctrl Pts',(0.00478131274577295,-0.0336319952301039,
0.0788304408263207));
#68028=CARTESIAN_POINT('Ctrl Pts',(0.00479962097924727,-0.0336011045488949,
0.0788434078476377));
#68029=CARTESIAN_POINT('Ctrl Pts',(0.00484556260175928,-0.0335235892595453,
0.078875946541187));
#68030=CARTESIAN_POINT('Ctrl Pts',(0.00489202291335045,-0.0334458668660369,
0.0789078394539877));
#68031=CARTESIAN_POINT('Ctrl Pts',(0.00493897410235363,-0.0333679869945385,
0.0789390627923123));
#68032=CARTESIAN_POINT('Ctrl Pts',(0.00493901075134363,-0.0333679692460369,
0.0789390879899287));
#68033=CARTESIAN_POINT('Ctrl Pts',(0.00493925678222502,-0.0333391895373844,
0.0789387073238942));
#68034=CARTESIAN_POINT('Ctrl Pts',(0.00493943846720192,-0.0333104081058565,
0.0789384202335114));
#68035=CARTESIAN_POINT('Ctrl Pts',(0.00493967427870374,-0.0332532697311741,
0.0789380372579631));
#68036=CARTESIAN_POINT('Ctrl Pts',(0.00493973026308562,-0.0332249166699368,
0.0789379385812724));
#68037=CARTESIAN_POINT('Ctrl Pts',(0.00493972655318134,-0.0331960985551544,
0.0789379317062876));
#68038=CARTESIAN_POINT('Ctrl Pts',(0.00493972647635046,-0.0331956312372016,
0.0789379316194554));
#68039=CARTESIAN_POINT('Ctrl Pts',(0.00493972638372156,-0.0331951640388589,
0.0789379315578557));
#68040=CARTESIAN_POINT('',(0.00483564091507221,-0.0331951640388587,0.0788687129533036));
#68041=CARTESIAN_POINT('',(0.00488768364940674,-0.0331951640388687,0.0789033222555896));
#68042=CARTESIAN_POINT('',(0.0046445508473314,-0.0335216366567685,0.0787296369111558));
#68043=CARTESIAN_POINT('Origin',(0.013728584133644,-0.0326434571527307,
0.0647707327897084));
#68044=CARTESIAN_POINT('',(0.00464537268054423,-0.0336938721132327,0.0787285551501433));
#68045=CARTESIAN_POINT('Origin',(-0.00196092565071937,-0.0336938867896245,
0.0874242812441565));
#68046=CARTESIAN_POINT('',(0.00469513958436659,-0.0336938721132537,0.0787663639492076));
#68047=CARTESIAN_POINT('Ctrl Pts',(0.00430966110264114,-0.0335235895815172,
0.0787816822329784));
#68048=CARTESIAN_POINT('Ctrl Pts',(0.00437342532752126,-0.0334144449262748,
0.0788341911191021));
#68049=CARTESIAN_POINT('Ctrl Pts',(0.00443834760384049,-0.0333049234473147,
0.0788854430106762));
#68050=CARTESIAN_POINT('Ctrl Pts',(0.00450435085242276,-0.0331951640388587,
0.078935364852349));
#68051=CARTESIAN_POINT('Ctrl Pts',(0.00442158279194207,-0.0335235895815172,
0.0787639422231131));
#68052=CARTESIAN_POINT('Ctrl Pts',(0.00448510279065953,-0.0334144449262748,
0.07881491028683));
#68053=CARTESIAN_POINT('Ctrl Pts',(0.0045497487279985,-0.0333049234473147,
0.0788646246313078));
#68054=CARTESIAN_POINT('Ctrl Pts',(0.00461544370004225,-0.0331951640388587,
0.0789130141992537));
#68055=CARTESIAN_POINT('Ctrl Pts',(0.004533504481243,-0.0335235895815172,
0.0787462022132478));
#68056=CARTESIAN_POINT('Ctrl Pts',(0.00459678025379779,-0.0334144449262748,
0.078795629454558));
#68057=CARTESIAN_POINT('Ctrl Pts',(0.00466114985215651,-0.0333049234473147,
0.0788438062519395));
#68058=CARTESIAN_POINT('Ctrl Pts',(0.00472653654766174,-0.0331951640388587,
0.0788906635461584));
#68059=CARTESIAN_POINT('Ctrl Pts',(0.00464542617054393,-0.0335235895815172,
0.0787284622033826));
#68060=CARTESIAN_POINT('Ctrl Pts',(0.00470845771693606,-0.0334144449262748,
0.078776348622286));
#68061=CARTESIAN_POINT('Ctrl Pts',(0.00477255097631451,-0.0333049234473147,
0.0788229878725712));
#68062=CARTESIAN_POINT('Ctrl Pts',(0.00483762939528123,-0.0331951640388587,
0.0788683128930631));
#68063=CARTESIAN_POINT('',(0.00466999588375756,-0.0331951640388687,0.0789020389028363));
#68064=CARTESIAN_POINT('Ctrl Pts',(0.0044941374873876,-0.0332121607145971,
0.078927622761363));
#68065=CARTESIAN_POINT('Ctrl Pts',(0.00452009591683222,-0.033262544410985,
0.0788934542425632));
#68066=CARTESIAN_POINT('Ctrl Pts',(0.00454560704180172,-0.0333135300747026,
0.078859874500962));
#68067=CARTESIAN_POINT('Ctrl Pts',(0.00459575493317219,-0.0334167203140575,
0.0787938659170176));
#68068=CARTESIAN_POINT('Ctrl Pts',(0.00462037227689717,-0.0334688847587267,
0.0787614626403224));
#68069=CARTESIAN_POINT('Ctrl Pts',(0.00464455084788231,-0.0335216366562334,
0.0787296369106874));
#68070=CARTESIAN_POINT('Ctrl Pts',(0.00474477121693191,-0.0336938721132388,
0.0788031820835436));
#68071=CARTESIAN_POINT('Ctrl Pts',(0.00477200783575637,-0.0336474569764957,
0.0788229605560618));
#68072=CARTESIAN_POINT('Ctrl Pts',(0.00479947412030335,-0.033601104548885,
0.0788424188343343));
#68073=CARTESIAN_POINT('Ctrl Pts',(0.00486901243788165,-0.0334837508592656,
0.0788916827211816));
#68074=CARTESIAN_POINT('Ctrl Pts',(0.00493998001046396,-0.0333660264659097,
0.0789388644104339));
#68075=CARTESIAN_POINT('Ctrl Pts',(0.00474490648815247,-0.0336938721132388,
0.0788041727482399));
#68076=CARTESIAN_POINT('Ctrl Pts',(0.00477214890566613,-0.0336474569764957,
0.0788239504289708));
#68077=CARTESIAN_POINT('Ctrl Pts',(0.00479962097923612,-0.033601104548885,
0.0788434078476292));
#68078=CARTESIAN_POINT('Ctrl Pts',(0.00486917395328969,-0.0334837508592656,
0.0788926695581313));
#68079=CARTESIAN_POINT('Ctrl Pts',(0.0049401561114216,-0.0333660264659097,
0.0789398486376924));
#68080=CARTESIAN_POINT('Ctrl Pts',(0.00479089930076365,-0.0336938721132388,
0.0791410031216843));
#68081=CARTESIAN_POINT('Ctrl Pts',(0.00482011329822525,-0.0336474569764957,
0.079160511591221));
#68082=CARTESIAN_POINT('Ctrl Pts',(0.00484955366519232,-0.033601104548885,
0.0791796767372991));
#68083=CARTESIAN_POINT('Ctrl Pts',(0.00492408990558829,-0.0334837508592656,
0.0792281984808254));
#68084=CARTESIAN_POINT('Ctrl Pts',(0.00500003121502358,-0.0333660264659097,
0.079274490253836));
#68085=CARTESIAN_POINT('',(0.00480128917461756,-0.0336769361243754,0.0791461024951536));
#68086=CARTESIAN_POINT('',(0.00479062498975413,-0.033693872113232,0.0791389941929939));
#68087=CARTESIAN_POINT('Ctrl Pts',(0.00480128917461775,-0.033676936124375,
0.0791461024951537));
#68088=CARTESIAN_POINT('Ctrl Pts',(0.00479951041199867,-0.0336797586669838,
0.0791449195877995));
#68089=CARTESIAN_POINT('Ctrl Pts',(0.0047977323483792,-0.0336825812712471,
0.0791437357752447));
#68090=CARTESIAN_POINT('Ctrl Pts',(0.00479417762654158,-0.0336882265907989,
0.0791413663452849));
#68091=CARTESIAN_POINT('Ctrl Pts',(0.00479240096835471,-0.0336910493060223,
0.0791401807279334));
#68092=CARTESIAN_POINT('Ctrl Pts',(0.00479062498975387,-0.0336938721132366,
0.0791389941930052));
#68093=CARTESIAN_POINT('Ctrl Pts',(0.00480128917461751,-0.0336769361243754,
0.0791461024951536));
#68094=CARTESIAN_POINT('Ctrl Pts',(0.00482449834745087,-0.0336279018505242,
0.0791112023747748));
#68095=CARTESIAN_POINT('Ctrl Pts',(0.00484804141359443,-0.0335767826010779,
0.0790758001720155));
#68096=CARTESIAN_POINT('Ctrl Pts',(0.00489417229694787,-0.0334733172064603,
0.0790064321943725));
#68097=CARTESIAN_POINT('Ctrl Pts',(0.00491679111782316,-0.033420963145621,
0.0789724197986262));
#68098=CARTESIAN_POINT('Ctrl Pts',(0.00493897409645518,-0.033367986984468,
0.078939062788009));
#68099=CARTESIAN_POINT('',(0.00476776573897154,-0.0336938721132534,0.0789715834706329));
#68100=CARTESIAN_POINT('Origin',(0.00812378219310841,-0.0315241814719618,
0.07415));
#68101=CARTESIAN_POINT('',(0.00480128917533939,-0.0337108120655664,0.0791461024940809));
#68102=CARTESIAN_POINT('',(0.00481196851860953,-0.0336938721132327,0.0791531880022078));
#68103=CARTESIAN_POINT('Origin',(0.0147919046467725,-0.0345562508791708,
0.0661412555029351));
#68104=CARTESIAN_POINT('Ctrl Pts',(0.00481196851861003,-0.0336938721132325,
0.0791531880022075));
#68105=CARTESIAN_POINT('Ctrl Pts',(0.00481018749777614,-0.0336910493226109,
0.0791520090720634));
#68106=CARTESIAN_POINT('Ctrl Pts',(0.00480840704459998,-0.0336882265990933,
0.0791508291499735));
#68107=CARTESIAN_POINT('Ctrl Pts',(0.00480484726436342,-0.0336825812713364,
0.0791484673152215));
#68108=CARTESIAN_POINT('Ctrl Pts',(0.00480306793726456,-0.0336797586670285,
0.0791472854025262));
#68109=CARTESIAN_POINT('Ctrl Pts',(0.00480128917461733,-0.0336769361243751,
0.0791461024951534));
#68110=CARTESIAN_POINT('Origin',(0.0129306800696285,-0.0345562513805278,
0.0649035143543814));
#68111=CARTESIAN_POINT('Ctrl Pts',(0.00480602420056776,-0.034243627687391,
0.0788479364515639));
#68112=CARTESIAN_POINT('Ctrl Pts',(0.00498320979478004,-0.0339430054201809,
0.0789730677570683));
#68113=CARTESIAN_POINT('Ctrl Pts',(0.00516931742593454,-0.0336441434784052,
0.0790844972327005));
#68114=CARTESIAN_POINT('Ctrl Pts',(0.00501332021829518,-0.034243627687391,
0.0789876803638976));
#68115=CARTESIAN_POINT('Ctrl Pts',(0.00519577634104691,-0.0339430054201809,
0.0791049933712071));
#68116=CARTESIAN_POINT('Ctrl Pts',(0.00538655062146727,-0.0336441434784052,
0.0792082297618051));
#68117=CARTESIAN_POINT('Ctrl Pts',(0.00501539317847246,-0.034243627687391,
0.078989077803021));
#68118=CARTESIAN_POINT('Ctrl Pts',(0.00519790200650957,-0.0339430054201809,
0.0791063126273486));
#68119=CARTESIAN_POINT('Ctrl Pts',(0.00538872295342259,-0.0336441434784052,
0.0792094670870962));
#68120=CARTESIAN_POINT('',(0.00504381185237035,-0.0341934961088741,0.0790071501624075));
#68121=CARTESIAN_POINT('',(0.00524596632995467,-0.0338664212894231,0.0791295884229386));
#68122=CARTESIAN_POINT('Origin',(0.0144318607449391,-0.0345610818077284,
0.0651537162091521));
#68123=CARTESIAN_POINT('Origin',(-0.000241169198642399,-0.0336938005044516,
0.0886243284210318));
#68124=CARTESIAN_POINT('',(0.00513841974862763,-0.0336938721132327,0.0790658657503114));
#68125=CARTESIAN_POINT('',(0.00519253292458446,-0.0336938721132427,0.079097138968719));
#68126=CARTESIAN_POINT('',(0.00493897409645077,-0.0340203938281605,0.0789390627880061));
#68127=CARTESIAN_POINT('Origin',(0.0147838079042916,-0.0345589643245868,
0.0654818271573763));
#68128=CARTESIAN_POINT('',(0.00493972638372135,-0.034193496108874,0.0789379315578555));
#68129=CARTESIAN_POINT('Origin',(-0.00116228036178326,-0.0341934220717766,
0.088113645806421));
#68130=CARTESIAN_POINT('',(0.00499176911805584,-0.0341934961088841,0.0789725408601415));
#68131=CARTESIAN_POINT('Ctrl Pts',(0.00460801091579982,-0.0340223579322397,
0.0790120317075984));
#68132=CARTESIAN_POINT('Ctrl Pts',(0.00467507101375865,-0.0339125849573575,
0.0790605233630289));
#68133=CARTESIAN_POINT('Ctrl Pts',(0.00474308765395145,-0.0338030433565231,
0.079107592955733));
#68134=CARTESIAN_POINT('Ctrl Pts',(0.00481196851860885,-0.0336938721132327,
0.079153188002208));
#68135=CARTESIAN_POINT('Ctrl Pts',(0.00471859789168073,-0.0340223579322397,
0.0789872991259313));
#68136=CARTESIAN_POINT('Ctrl Pts',(0.0047853168628331,-0.0339125849573575,
0.0790342654985415));
#68137=CARTESIAN_POINT('Ctrl Pts',(0.00485296104611517,-0.0338030433565231,
0.0790798179407561));
#68138=CARTESIAN_POINT('Ctrl Pts',(0.00492143877205597,-0.0336938721132327,
0.0791239058670292));
#68139=CARTESIAN_POINT('Ctrl Pts',(0.00482918486756165,-0.0340223579322397,
0.0789625665442643));
#68140=CARTESIAN_POINT('Ctrl Pts',(0.00489556271190754,-0.0339125849573575,
0.0790080076340541));
#68141=CARTESIAN_POINT('Ctrl Pts',(0.00496283443827889,-0.0338030433565231,
0.0790520429257791));
#68142=CARTESIAN_POINT('Ctrl Pts',(0.00503090902550308,-0.0336938721132327,
0.0790946237318504));
#68143=CARTESIAN_POINT('Ctrl Pts',(0.00493977184344256,-0.0340223579322397,
0.0789378339625972));
#68144=CARTESIAN_POINT('Ctrl Pts',(0.00500580856098198,-0.0339125849573575,
0.0789817497695667));
#68145=CARTESIAN_POINT('Ctrl Pts',(0.00507270783044261,-0.0338030433565231,
0.0790242679108022));
#68146=CARTESIAN_POINT('Ctrl Pts',(0.0051403792789502,-0.0336938721132327,
0.0790653415966716));
#68147=CARTESIAN_POINT('',(0.00497519413362858,-0.0336938721132427,0.0791095268762696));
#68148=CARTESIAN_POINT('Ctrl Pts',(0.00480128917733045,-0.0337108120662679,
0.0791461024910741));
#68149=CARTESIAN_POINT('Ctrl Pts',(0.00482509996540099,-0.0337611408994367,
0.0791102977092344));
#68150=CARTESIAN_POINT('Ctrl Pts',(0.00484847625941539,-0.033812108878147,
0.0790751462852275));
#68151=CARTESIAN_POINT('Ctrl Pts',(0.0048943811547497,-0.0339153382773236,
0.0790061181305126));
#68152=CARTESIAN_POINT('Ctrl Pts',(0.00491689033549877,-0.0339675558473114,
0.0789722706029247));
#68153=CARTESIAN_POINT('Ctrl Pts',(0.00493897409647724,-0.0340203938281304,
0.0789390627879758));
#68154=CARTESIAN_POINT('Ctrl Pts',(0.00504341182756386,-0.0341934961088741,
0.0790051618583216));
#68155=CARTESIAN_POINT('Ctrl Pts',(0.00514378847330114,-0.0340287516194401,
0.0790688460884141));
#68156=CARTESIAN_POINT('Ctrl Pts',(0.00524671146664077,-0.033864463329982,
0.0791283272586611));
#68157=CARTESIAN_POINT('Ctrl Pts',(0.00504381185237033,-0.0341934961088741,
0.0790071501624074));
#68158=CARTESIAN_POINT('Ctrl Pts',(0.00514422960472787,-0.0340287516194401,
0.0790708261223022));
#68159=CARTESIAN_POINT('Ctrl Pts',(0.00524719332774941,-0.033864463329982,
0.0791302973304505));
#68160=CARTESIAN_POINT('Ctrl Pts',(0.00511046375141771,-0.0341934961088741,
0.0793384402250671));
#68161=CARTESIAN_POINT('Ctrl Pts',(0.00521773066477672,-0.0340287516194401,
0.0794007382094683));
#68162=CARTESIAN_POINT('Ctrl Pts',(0.00532748074355059,-0.033864463329982,
0.0794585495385583));
#68163=CARTESIAN_POINT('',(0.00512155322659617,-0.0341764758832416,0.079344864889805));
#68164=CARTESIAN_POINT('',(0.0051104637514149,-0.034193496108874,0.0793384402250532));
#68165=CARTESIAN_POINT('Origin',(0.0138499602326468,-0.0345621026920888,
0.0652652255464296));
#68166=CARTESIAN_POINT('Ctrl Pts',(0.00512155322563717,-0.0341764758837518,
0.0793448648882492));
#68167=CARTESIAN_POINT('Ctrl Pts',(0.00514303134858548,-0.0341260050044428,
0.079307700491239));
#68168=CARTESIAN_POINT('Ctrl Pts',(0.00516413609801035,-0.034074926915621,
0.0792711820800005));
#68169=CARTESIAN_POINT('Ctrl Pts',(0.00520561536501873,-0.0339715436322559,
0.0791994090187048));
#68170=CARTESIAN_POINT('Ctrl Pts',(0.00522597415170171,-0.0339192778251916,
0.0791641816003481));
#68171=CARTESIAN_POINT('Ctrl Pts',(0.00524596632672147,-0.0338664212874305,
0.0791295884241146));
#68172=CARTESIAN_POINT('',(0.00507713780190263,-0.0341934961088841,0.0791727951937404));
#68173=CARTESIAN_POINT('Ctrl Pts',(0.00513712102382444,-0.0346945769586966,
0.0790651151881108));
#68174=CARTESIAN_POINT('Ctrl Pts',(0.00524007007934417,-0.0345275153362944,
0.0791276720020953));
#68175=CARTESIAN_POINT('Ctrl Pts',(0.005345013116983,-0.0343603235965185,
0.0791870073434382));
#68176=CARTESIAN_POINT('Ctrl Pts',(0.00545163715361716,-0.034193496108874,
0.0792429503375184));
#68177=CARTESIAN_POINT('Ctrl Pts',(0.0052097048335311,-0.0346945769586966,
0.0791070630001433));
#68178=CARTESIAN_POINT('Ctrl Pts',(0.00531353250276884,-0.0345275153362944,
0.0791680995171725));
#68179=CARTESIAN_POINT('Ctrl Pts',(0.00541930656944027,-0.0343603235965185,
0.0792258865367407));
#68180=CARTESIAN_POINT('Ctrl Pts',(0.00552671166066623,-0.034193496108874,
0.0792802578000049));
#68181=CARTESIAN_POINT('Ctrl Pts',(0.00528228864323767,-0.0346945769586966,
0.0791490108121771));
#68182=CARTESIAN_POINT('Ctrl Pts',(0.00538699492619351,-0.0345275153362944,
0.0792085270322502));
#68183=CARTESIAN_POINT('Ctrl Pts',(0.00549360002189762,-0.0343603235965185,
0.079264765730044));
#68184=CARTESIAN_POINT('Ctrl Pts',(0.00560178616771541,-0.034193496108874,
0.0793175652624937));
#68185=CARTESIAN_POINT('Ctrl Pts',(0.00535487245294441,-0.0346945769586966,
0.0791909586242082));
#68186=CARTESIAN_POINT('Ctrl Pts',(0.00546045734961816,-0.0345275153362944,
0.0792489545473269));
#68187=CARTESIAN_POINT('Ctrl Pts',(0.00556789347435482,-0.0343603235965185,
0.0793036449233458));
#68188=CARTESIAN_POINT('Ctrl Pts',(0.00567686067476436,-0.034193496108874,
0.0793548727249779));
#68189=CARTESIAN_POINT('',(0.00535487245241997,-0.0346945769586966,0.0791909586239049));
#68190=CARTESIAN_POINT('',(0.00556431598469133,-0.0343667727831502,0.0793004618946675));
#68191=CARTESIAN_POINT('Origin',(0.0132886961920314,-0.0345626457065727,
0.0643669346046938));
#68192=CARTESIAN_POINT('Origin',(0.000645886075255295,-0.0341934771029131,
0.0891979212485602));
#68193=CARTESIAN_POINT('',(0.00545298044386904,-0.034193496108874,0.0792436178710481));
#68194=CARTESIAN_POINT('',(0.00550895050146468,-0.034193496108884,0.0792714315844719));
#68195=CARTESIAN_POINT('',(0.00524596632826059,-0.034521194296265,0.0791295884215426));
#68196=CARTESIAN_POINT('Origin',(0.0137033246011917,-0.0345625596120016,
0.0646103972754862));
#68197=CARTESIAN_POINT('',(0.00524664610052137,-0.0346945769586885,0.0791284121871068));
#68198=CARTESIAN_POINT('Origin',(-0.00028924817164534,-0.0346945685853917,
0.0887073677574834));
#68199=CARTESIAN_POINT('',(0.00530075927648067,-0.0346945769587026,0.0791596854055159));
#68200=CARTESIAN_POINT('Ctrl Pts',(0.00535434849807001,-0.0346945769586932,
0.0791889998386456));
#68201=CARTESIAN_POINT('Ctrl Pts',(0.00545852625425208,-0.034529677707698,
0.079246255920702));
#68202=CARTESIAN_POINT('Ctrl Pts',(0.00556498143832853,-0.034364806625142,
0.0792991573157578));
#68203=CARTESIAN_POINT('Ctrl Pts',(0.00535487245241206,-0.0346945769586932,
0.0791909586239005));
#68204=CARTESIAN_POINT('Ctrl Pts',(0.00545909070509329,-0.034529677707698,
0.0792482038735716));
#68205=CARTESIAN_POINT('Ctrl Pts',(0.0055655859033527,-0.034364806625142,
0.0793010927717408));
#68206=CARTESIAN_POINT('Ctrl Pts',(0.00544219470431115,-0.0346945769586932,
0.0795174098539296));
#68207=CARTESIAN_POINT('Ctrl Pts',(0.00555316210518375,-0.034529677707698,
0.0795728497778299));
#68208=CARTESIAN_POINT('Ctrl Pts',(0.00566632606879868,-0.034364806625142,
0.0796236559443599));
#68209=CARTESIAN_POINT('',(0.00545366570497139,-0.0346775396665004,0.0795231255274065));
#68210=CARTESIAN_POINT('',(0.00544219470431032,-0.0346945769586885,0.0795174098539166));
#68211=CARTESIAN_POINT('Origin',(0.0127046232047038,-0.0345626618182689,
0.064588718319839));
#68212=CARTESIAN_POINT('Ctrl Pts',(0.00545366570400267,-0.0346775396670097,
0.0795231255258533));
#68213=CARTESIAN_POINT('Ctrl Pts',(0.00547278291854349,-0.0346269749928203,
0.0794846555672365));
#68214=CARTESIAN_POINT('Ctrl Pts',(0.0054915603453571,-0.0345757902890819,
0.0794468692896402));
#68215=CARTESIAN_POINT('Ctrl Pts',(0.00552845124219787,-0.0344721681087867,
0.0793726330539552));
#68216=CARTESIAN_POINT('Ctrl Pts',(0.00554655025430632,-0.0344197714289421,
0.0793362122024711));
#68217=CARTESIAN_POINT('Ctrl Pts',(0.00556431598442007,-0.0343667727830705,
0.0793004618946509));
#68218=CARTESIAN_POINT('',(0.00539853357837515,-0.0346945769587026,0.0793541842389209));
#68219=CARTESIAN_POINT('Origin',(0.00812378219310841,-0.0315241814719618,
0.07415));
#68220=CARTESIAN_POINT('',(0.00512155322769303,-0.0342105180190352,0.0793448648895882));
#68221=CARTESIAN_POINT('',(0.00513265640034568,-0.0341934961088739,0.0793512658547611));
#68222=CARTESIAN_POINT('Origin',(0.0138135968724053,-0.034562169891954,
0.0652381629999228));
#68223=CARTESIAN_POINT('Origin',(0.012963198382615,-0.0345621042509321,
0.0647527421530786));
#68224=CARTESIAN_POINT('Origin',(0.0130047980182236,-0.0345621713291986,
0.0647707445053555));
#68225=CARTESIAN_POINT('Ctrl Pts',(0.00492023879775385,-0.0345231616327842,
0.0792231952174262));
#68226=CARTESIAN_POINT('Ctrl Pts',(0.00499016565133852,-0.0344132092796988,
0.0792673515529028));
#68227=CARTESIAN_POINT('Ctrl Pts',(0.0050610022359883,-0.0343032738558979,
0.0793100592283065));
#68228=CARTESIAN_POINT('Ctrl Pts',(0.00513265640034569,-0.0341934961088739,
0.0793512658547611));
#68229=CARTESIAN_POINT('Ctrl Pts',(0.00502905439365322,-0.0345231616327842,
0.0791915676625468));
#68230=CARTESIAN_POINT('Ctrl Pts',(0.00509854530592192,-0.0344132092796988,
0.079234224128234));
#68231=CARTESIAN_POINT('Ctrl Pts',(0.00516891494812477,-0.0343032738558979,
0.0792754410283371));
#68232=CARTESIAN_POINT('Ctrl Pts',(0.0052400718160332,-0.0341934961088739,
0.0793151678685117));
#68233=CARTESIAN_POINT('Ctrl Pts',(0.0051378699895526,-0.0345231616327842,
0.0791599401076674));
#68234=CARTESIAN_POINT('Ctrl Pts',(0.00520692496050531,-0.0344132092796988,
0.0792010967035653));
#68235=CARTESIAN_POINT('Ctrl Pts',(0.00527682766026125,-0.0343032738558979,
0.0792408228283676));
#68236=CARTESIAN_POINT('Ctrl Pts',(0.00534748723172071,-0.0341934961088739,
0.0792790698822624));
#68237=CARTESIAN_POINT('Ctrl Pts',(0.00524668558545197,-0.0345231616327842,
0.079128312552788));
#68238=CARTESIAN_POINT('Ctrl Pts',(0.00531530461508871,-0.0344132092796988,
0.0791679692788966));
#68239=CARTESIAN_POINT('Ctrl Pts',(0.00538474037239772,-0.0343032738558979,
0.0792062046283982));
#68240=CARTESIAN_POINT('Ctrl Pts',(0.00545490264740822,-0.0341934961088739,
0.079242971896013));
#68241=CARTESIAN_POINT('',(0.00529281842211735,-0.0341934961088839,0.0792974418629146));
#68242=CARTESIAN_POINT('Ctrl Pts',(0.00512155322941782,-0.0342105180195384,
0.0793448648865901));
#68243=CARTESIAN_POINT('Ctrl Pts',(0.0051430555100191,-0.0342610556241263,
0.0793076587161653));
#68244=CARTESIAN_POINT('Ctrl Pts',(0.0051641719433129,-0.0343122189870085,
0.0792711201912312));
#68245=CARTESIAN_POINT('Ctrl Pts',(0.00520565162553852,-0.0344158119695126,
0.0791993464033866));
#68246=CARTESIAN_POINT('Ctrl Pts',(0.00522599790897453,-0.0344681990450014,
0.0791641404964846));
#68247=CARTESIAN_POINT('Ctrl Pts',(0.00524596632826922,-0.0345211942962425,
0.0791295884215131));
#68248=CARTESIAN_POINT('Origin',(0.00812378219310841,-0.0315241814719618,
0.07415));
#68249=CARTESIAN_POINT('',(0.00545366570615726,-0.034711613648978,0.0795231255266795));
#68250=CARTESIAN_POINT('',(0.00546514888907038,-0.0346945769586885,0.0795288166872181));
#68251=CARTESIAN_POINT('Origin',(0.0126632473294917,-0.0345626675282767,
0.0645702406010984));
#68252=CARTESIAN_POINT('Origin',(0.0129781455413861,-0.0345626632992206,
0.0647246384176518));
#68253=CARTESIAN_POINT('Origin',(0.0130178575616,-0.034562669103339,0.06474646406225));
#68254=CARTESIAN_POINT('Ctrl Pts',(0.00542106257343935,-0.0352450361861256,
0.079226754047367));
#68255=CARTESIAN_POINT('Ctrl Pts',(0.00561253548933533,-0.0349452761023744,
0.0793286887878722));
#68256=CARTESIAN_POINT('Ctrl Pts',(0.0058111425924016,-0.034644428998343,
0.0794159114194262));
#68257=CARTESIAN_POINT('Ctrl Pts',(0.00564424009426933,-0.0352450361861256,
0.0793394119108128));
#68258=CARTESIAN_POINT('Ctrl Pts',(0.00583996197109809,-0.0349452761023744,
0.0794329293732153));
#68259=CARTESIAN_POINT('Ctrl Pts',(0.00604217194043589,-0.034644428998343,
0.0795114385901518));
#68260=CARTESIAN_POINT('Ctrl Pts',(0.00564647186947763,-0.0352450361861256,
0.0793405384894472));
#68261=CARTESIAN_POINT('Ctrl Pts',(0.00584223623591572,-0.0349452761023744,
0.0794339717790687));
#68262=CARTESIAN_POINT('Ctrl Pts',(0.00604448223391623,-0.034644428998343,
0.0795123938618591));
#68263=CARTESIAN_POINT('',(0.00567683038040905,-0.0351951634053288,0.0793548611056252));
#68264=CARTESIAN_POINT('',(0.00589276668460222,-0.0348678972925434,0.0794510088474559));
#68265=CARTESIAN_POINT('Origin',(0.0120010715500606,-0.034563676788786,
0.0638497500128052));
#68266=CARTESIAN_POINT('Origin',(0.00160641038181471,-0.0346946199340732,
0.0896356118820766));
#68267=CARTESIAN_POINT('',(0.00577808157344129,-0.0346945769586883,0.0794012678091004));
#68268=CARTESIAN_POINT('',(0.00583568762442879,-0.0346945769586984,0.0794255122495203));
#68269=CARTESIAN_POINT('',(0.00556431598449918,-0.0350221583435276,0.0793004618945283));
#68270=CARTESIAN_POINT('Origin',(0.0124587166940046,-0.0345629067284135,
0.0639973484499783));
#68271=CARTESIAN_POINT('',(0.00556486371357888,-0.035195136029876,0.0792993528924502));
#68272=CARTESIAN_POINT('Origin',(0.000661207092376949,-0.0351951838366793,
0.0891670778385463));
#68273=CARTESIAN_POINT('',(0.00567686067416044,-0.0351951371328747,0.0793548727248077));
#68274=CARTESIAN_POINT('Ctrl Pts',(0.00524510966521925,-0.0350241211493459,
0.079414337040617));
#68275=CARTESIAN_POINT('Ctrl Pts',(0.0053176237462245,-0.03491442328675,
0.0794539895726004));
#68276=CARTESIAN_POINT('Ctrl Pts',(0.00539100087653385,-0.0348045283677551,
0.079492166920732));
#68277=CARTESIAN_POINT('Ctrl Pts',(0.00546514888907046,-0.0346945769586885,
0.0795288166872181));
#68278=CARTESIAN_POINT('Ctrl Pts',(0.00535172464515648,-0.0350241211493459,
0.0793759392821534));
#68279=CARTESIAN_POINT('Ctrl Pts',(0.00542370981280642,-0.03491442328675,
0.0794141232365683));
#68280=CARTESIAN_POINT('Ctrl Pts',(0.00549652735663397,-0.0348045283677551,
0.0794508420611333));
#68281=CARTESIAN_POINT('Ctrl Pts',(0.00557008575680197,-0.0346945769586885,
0.0794860452529104));
#68282=CARTESIAN_POINT('Ctrl Pts',(0.00545833962509371,-0.0350241211493459,
0.0793375415236899));
#68283=CARTESIAN_POINT('Ctrl Pts',(0.00552979587938833,-0.03491442328675,
0.0793742569005361));
#68284=CARTESIAN_POINT('Ctrl Pts',(0.00560205383673409,-0.0348045283677551,
0.0794095172015345));
#68285=CARTESIAN_POINT('Ctrl Pts',(0.00567502262453347,-0.0346945769586885,
0.0794432738186027));
#68286=CARTESIAN_POINT('Ctrl Pts',(0.00556495460503094,-0.0350241211493459,
0.0792991437652263));
#68287=CARTESIAN_POINT('Ctrl Pts',(0.00563588194597025,-0.03491442328675,
0.0793343905645039));
#68288=CARTESIAN_POINT('Ctrl Pts',(0.0057075803168342,-0.0348045283677551,
0.0793681923419358));
#68289=CARTESIAN_POINT('Ctrl Pts',(0.00577995949226498,-0.0346945769586885,
0.0794005023842949));
#68290=CARTESIAN_POINT('',(0.00562161523126584,-0.0346945769586984,0.0794650422481692));
#68291=CARTESIAN_POINT('Ctrl Pts',(0.00545366570761676,-0.0347116136492789,
0.0795231255237274));
#68292=CARTESIAN_POINT('Ctrl Pts',(0.00547277534182364,-0.0347621546532227,
0.0794846708481116));
#68293=CARTESIAN_POINT('Ctrl Pts',(0.00549154897702143,-0.0348133084096884,
0.0794468923096087));
#68294=CARTESIAN_POINT('Ctrl Pts',(0.0055284399172878,-0.0349168561544569,
0.0793726559780416));
#68295=CARTESIAN_POINT('Ctrl Pts',(0.00554654258958549,-0.0349692089015918,
0.0793362276307771));
#68296=CARTESIAN_POINT('Ctrl Pts',(0.0055643159845333,-0.0350221583435,
0.0793004618945045));
#68297=CARTESIAN_POINT('Ctrl Pts',(0.00567639462613548,-0.0351951371254904,
0.0793534859230376));
#68298=CARTESIAN_POINT('Ctrl Pts',(0.00578397343281551,-0.0350307338980949,
0.0794040841254413));
#68299=CARTESIAN_POINT('Ctrl Pts',(0.00589355159233925,-0.0348659306897851,
0.0794501927438176));
#68300=CARTESIAN_POINT('Ctrl Pts',(0.00567686067420752,-0.0351951371254904,
0.0793548727247014));
#68301=CARTESIAN_POINT('Ctrl Pts',(0.00578446815214185,-0.0350307338980949,
0.0794054612918536));
#68302=CARTESIAN_POINT('Ctrl Pts',(0.00589407456018512,-0.0348659306897851,
0.0794515590981978));
#68303=CARTESIAN_POINT('Ctrl Pts',(0.00575497081680124,-0.0351951371254904,
0.079587302128884));
#68304=CARTESIAN_POINT('Ctrl Pts',(0.00586738362683585,-0.0350307338980949,
0.079636275817846));
#68305=CARTESIAN_POINT('Ctrl Pts',(0.00598172451619324,-0.0348659306897851,
0.0796805615163434));
#68306=CARTESIAN_POINT('Origin',(0.00382978524874992,-0.0308609197384744,
0.084352760014669));
#68307=CARTESIAN_POINT('',(0.00571091493522803,-0.0351951371254904,0.0794562067043364));
#68308=CARTESIAN_POINT('Origin',(0.00836832757329725,-0.03518404674412,
0.0732039856204225));
#68309=CARTESIAN_POINT('Origin',(0.00422499454032104,-0.0352322614457976,
0.0854624028434309));
#68310=CARTESIAN_POINT('',(0.00611274429739835,-0.0351951142564672,0.0795382781262157));
#68311=CARTESIAN_POINT('',(0.00623046956272987,-0.0351951372916786,0.0795793523816059));
#68312=CARTESIAN_POINT('Origin',(0.00845646098340635,-0.0352875126228133,
0.0740768915355774));
#68313=CARTESIAN_POINT('Origin',(0.00164326621622433,-0.0298325076523774,
0.0703687167587176));
#68314=CARTESIAN_POINT('Origin',(0.00258859523071002,-0.033873480203009,
0.0804430596755119));
#68315=CARTESIAN_POINT('Ctrl Pts',(0.00332944714467594,-0.0321934096636941,
0.0773268675119815));
#68316=CARTESIAN_POINT('Ctrl Pts',(0.00338631156032693,-0.0320508460843488,
0.0774126838263026));
#68317=CARTESIAN_POINT('Ctrl Pts',(0.00344543881505853,-0.0319086045661401,
0.0774969076001925));
#68318=CARTESIAN_POINT('Ctrl Pts',(0.00350668666774897,-0.0317669892865405,
0.0775793679661119));
#68319=CARTESIAN_POINT('Ctrl Pts',(0.00337727060759419,-0.0321934096636941,
0.0773957394875768));
#68320=CARTESIAN_POINT('Ctrl Pts',(0.00343536779881174,-0.0320508460843488,
0.077480699784685));
#68321=CARTESIAN_POINT('Ctrl Pts',(0.00349570390009959,-0.0319086045661401,
0.0775640350645548));
#68322=CARTESIAN_POINT('Ctrl Pts',(0.00355813422497361,-0.0317669892865405,
0.0776455765870144));
#68323=CARTESIAN_POINT('Ctrl Pts',(0.00342509407051245,-0.0321934096636941,
0.0774646114631721));
#68324=CARTESIAN_POINT('Ctrl Pts',(0.00348442403729657,-0.0320508460843488,
0.0775487157430673));
#68325=CARTESIAN_POINT('Ctrl Pts',(0.00354596898514065,-0.0319086045661401,
0.0776311625289171));
#68326=CARTESIAN_POINT('Ctrl Pts',(0.00360958178219824,-0.0317669892865405,
0.0777117852079169));
#68327=CARTESIAN_POINT('Ctrl Pts',(0.00347291753343071,-0.0321934096636941,
0.0775334834387674));
#68328=CARTESIAN_POINT('Ctrl Pts',(0.00353348027578138,-0.0320508460843488,
0.0776167317014498));
#68329=CARTESIAN_POINT('Ctrl Pts',(0.00359623407018171,-0.0319086045661401,
0.0776982899932795));
#68330=CARTESIAN_POINT('Ctrl Pts',(0.00366102933942288,-0.0317669892865405,
0.0777779938288193));
#68331=CARTESIAN_POINT('',(0.00347206196223053,-0.0321934096636941,0.0775322513055127));
#68332=CARTESIAN_POINT('',(0.00361494791176087,-0.0318665617511303,0.0777205095452145));
#68333=CARTESIAN_POINT('Origin',(0.0173394999816654,-0.0326371944420774,
0.0682095871144943));
#68334=CARTESIAN_POINT('Origin',(-0.00497818172410554,-0.0316939261509784,
0.0845253396750685));
#68335=CARTESIAN_POINT('',(0.00339983986145632,-0.0320197221621766,0.0774305423353098));
#68336=CARTESIAN_POINT('Ctrl Pts',(0.00339990312524244,-0.0320197392094684,
0.0774307161529535));
#68337=CARTESIAN_POINT('Ctrl Pts',(0.00341659650230586,-0.0319792716575983,
0.0774547527415632));
#68338=CARTESIAN_POINT('Ctrl Pts',(0.00343354911925363,-0.031938643982963,
0.0774787714902867));
#68339=CARTESIAN_POINT('Ctrl Pts',(0.00345078568289115,-0.0318979099381562,
0.0775027927373011));
#68340=CARTESIAN_POINT('Ctrl Pts',(0.00346802190583522,-0.031857176698488,
0.0775268135095177));
#68341=CARTESIAN_POINT('Ctrl Pts',(0.00348545301092505,-0.0318163871833546,
0.0775507157293868));
#68342=CARTESIAN_POINT('Ctrl Pts',(0.00350301619735661,-0.0317755399638303,
0.0775744192578713));
#68343=CARTESIAN_POINT('',(0.00340076680876396,-0.0321934096636184,0.0774295770579827));
#68344=CARTESIAN_POINT('Origin',(0.00151749285991017,-0.0324111438667224,
0.0787628845887113));
#68345=CARTESIAN_POINT('',(0.00343641438550725,-0.0321934096636663,0.0774809141817577));
#68346=CARTESIAN_POINT('Ctrl Pts',(0.00347242198582075,-0.0321934096636618,
0.0775302552918872));
#68347=CARTESIAN_POINT('Ctrl Pts',(0.00351903834071276,-0.0320835708272592,
0.0775944011742037));
#68348=CARTESIAN_POINT('Ctrl Pts',(0.00356695515192517,-0.0319739230346488,
0.07765754512626));
#68349=CARTESIAN_POINT('Ctrl Pts',(0.00361610491294562,-0.0318646057455573,
0.0777196110648324));
#68350=CARTESIAN_POINT('Ctrl Pts',(0.00345230709872301,-0.0321934096636618,
0.0776417746000015));
#68351=CARTESIAN_POINT('Ctrl Pts',(0.00350046139178699,-0.0320835708272592,
0.0777061978822878));
#68352=CARTESIAN_POINT('Ctrl Pts',(0.00354992098988267,-0.0319739230346488,
0.0777695872458599));
#68353=CARTESIAN_POINT('Ctrl Pts',(0.0036006163885113,-0.0318646057455573,
0.0778318664449979));
#68354=CARTESIAN_POINT('Ctrl Pts',(0.00343219221162527,-0.0321934096636618,
0.0777532939081159));
#68355=CARTESIAN_POINT('Ctrl Pts',(0.00348188444286121,-0.0320835708272592,
0.0778179945903719));
#68356=CARTESIAN_POINT('Ctrl Pts',(0.00353288682784016,-0.0319739230346488,
0.0778816293654599));
#68357=CARTESIAN_POINT('Ctrl Pts',(0.00358512786407699,-0.0318646057455573,
0.0779441218251635));
#68358=CARTESIAN_POINT('Ctrl Pts',(0.00341207732452753,-0.0321934096636618,
0.0778648132162302));
#68359=CARTESIAN_POINT('Ctrl Pts',(0.00346330749393543,-0.0320835708272592,
0.0779297912984559));
#68360=CARTESIAN_POINT('Ctrl Pts',(0.00351585266579766,-0.0319739230346488,
0.0779936714850599));
#68361=CARTESIAN_POINT('Ctrl Pts',(0.00356963933964267,-0.0318646057455573,
0.078056377205329));
#68362=CARTESIAN_POINT('',(0.00342002298234353,-0.0321763980308481,0.0778748690265434));
#68363=CARTESIAN_POINT('',(0.00341207732454946,-0.0321934096636184,0.0778648132162463));
#68364=CARTESIAN_POINT('Origin',(0.0167646994888026,-0.0326386230218105,
0.0680898959435203));
#68365=CARTESIAN_POINT('Ctrl Pts',(0.00342002298482514,-0.0321763980306328,
0.0778748690245691));
#68366=CARTESIAN_POINT('Ctrl Pts',(0.00345366967478655,-0.0321259596175906,
0.0778482244818392));
#68367=CARTESIAN_POINT('Ctrl Pts',(0.00348673339218307,-0.0320749164633572,
0.0778220415903783));
#68368=CARTESIAN_POINT('Ctrl Pts',(0.00355172149072844,-0.0319716057793949,
0.0777705780386704));
#68369=CARTESIAN_POINT('Ctrl Pts',(0.00358362055013076,-0.0319193786690143,
0.0777453174305103));
#68370=CARTESIAN_POINT('Ctrl Pts',(0.00361494791320901,-0.0318665617525338,
0.0777205095440551));
#68371=CARTESIAN_POINT('',(0.0034420696434,-0.0321934096636663,0.0776985322608896));
#68372=CARTESIAN_POINT('Origin',(0.00812378219310841,-0.0315241814719618,
0.07415));
#68373=CARTESIAN_POINT('',(0.00342002298205243,-0.0322104233323598,0.0778748690267733));
#68374=CARTESIAN_POINT('',(0.00342799009848551,-0.0321934096636183,0.0778849078441259));
#68375=CARTESIAN_POINT('Origin',(0.0167417837500709,-0.0326387225284402,
0.0680507782985828));
#68376=CARTESIAN_POINT('Origin',(0.0160029617252066,-0.032638624895482,
0.0671279692888624));
#68377=CARTESIAN_POINT('Origin',(0.0160357811135996,-0.0326387239005177,
0.0671592451620444));
#68378=CARTESIAN_POINT('Ctrl Pts',(0.00351668453358277,-0.0327445246967098,
0.0775927861036656));
#68379=CARTESIAN_POINT('Ctrl Pts',(0.00364653133419014,-0.032443687833936,
0.0777665456324781));
#68380=CARTESIAN_POINT('Ctrl Pts',(0.00378909753162478,-0.0321434074405927,
0.0779300309371087));
#68381=CARTESIAN_POINT('Ctrl Pts',(0.00367065265680256,-0.0327445246967098,
0.0777897475644447));
#68382=CARTESIAN_POINT('Ctrl Pts',(0.0038079279803431,-0.032443687833936,
0.0779577000905583));
#68383=CARTESIAN_POINT('Ctrl Pts',(0.00395746418988505,-0.0321434074405927,
0.0781148353428632));
#68384=CARTESIAN_POINT('',(0.0036936143861395,-0.0326943950436612,0.0778176611351237));
#68385=CARTESIAN_POINT('',(0.0038480392148886,-0.0323666188837389,0.0779965760078549));
#68386=CARTESIAN_POINT('Origin',(0.0165941822790158,-0.0326395579109043,
0.0670388204620943));
#68387=CARTESIAN_POINT('Origin',(-0.00436287349293982,-0.0321933825603008,
0.0853833401400488));
#68388=CARTESIAN_POINT('',(0.00376544772383368,-0.032193409653269,0.0779027384202294));
#68389=CARTESIAN_POINT('',(0.00380724845807768,-0.0321934096584275,0.0779492029116465));
#68390=CARTESIAN_POINT('',(0.00361494791101053,-0.0325210109756239,0.0777205095457903));
#68391=CARTESIAN_POINT('Origin',(0.016880826878996,-0.0326393129161898,
0.0674248506473343));
#68392=CARTESIAN_POINT('',(0.00361601294806189,-0.0326943950436595,0.0777196661515348));
#68393=CARTESIAN_POINT('Origin',(-0.005056508717713,-0.0326943765538189,
0.0845873647954996));
#68394=CARTESIAN_POINT('',(0.0036548136671107,-0.0326943950436703,0.0777686636433393));
#68395=CARTESIAN_POINT('Ctrl Pts',(0.00327763506527675,-0.0325229783203769,
0.0776876345225935));
#68396=CARTESIAN_POINT('Ctrl Pts',(0.00332640127980775,-0.032413025309245,
0.0777544385547724));
#68397=CARTESIAN_POINT('Ctrl Pts',(0.00337654202520829,-0.032303122220807,
0.0778202236630187));
#68398=CARTESIAN_POINT('Ctrl Pts',(0.00342799010127687,-0.0321934096576658,
0.0778849078476354));
#68399=CARTESIAN_POINT('Ctrl Pts',(0.00339045215365831,-0.0325229783203769,
0.0776982856636362));
#68400=CARTESIAN_POINT('Ctrl Pts',(0.00343936519393565,-0.032413025309245,
0.077763534514719));
#68401=CARTESIAN_POINT('Ctrl Pts',(0.0034896205718948,-0.032303122220807,
0.0778277616404636));
#68402=CARTESIAN_POINT('Ctrl Pts',(0.00354115101091851,-0.0321934096576658,
0.0778908870420193));
#68403=CARTESIAN_POINT('Ctrl Pts',(0.00350326924203986,-0.0325229783203769,
0.077708936804679));
#68404=CARTESIAN_POINT('Ctrl Pts',(0.00355232910806356,-0.032413025309245,
0.0777726304746655));
#68405=CARTESIAN_POINT('Ctrl Pts',(0.0036026991185813,-0.032303122220807,
0.0778352996179085));
#68406=CARTESIAN_POINT('Ctrl Pts',(0.00365431192056015,-0.0321934096576658,
0.0778968662364032));
#68407=CARTESIAN_POINT('Ctrl Pts',(0.00361608633042141,-0.0325229783203769,
0.0777195879457217));
#68408=CARTESIAN_POINT('Ctrl Pts',(0.00366529302219146,-0.032413025309245,
0.0777817264346121));
#68409=CARTESIAN_POINT('Ctrl Pts',(0.00371577766526781,-0.032303122220807,
0.0778428375953534));
#68410=CARTESIAN_POINT('Ctrl Pts',(0.00376747283020179,-0.0321934096576658,
0.0779028454307871));
#68411=CARTESIAN_POINT('',(0.00359671891073733,-0.0321934096584275,0.0778938231319032));
#68412=CARTESIAN_POINT('Ctrl Pts',(0.00342002298477554,-0.0322104233328918,
0.0778748690246083));
#68413=CARTESIAN_POINT('Ctrl Pts',(0.00345371526661704,-0.0322609421831403,
0.0778481883780358));
#68414=CARTESIAN_POINT('Ctrl Pts',(0.00348680125644047,-0.0323120888240814,
0.0778219878492282));
#68415=CARTESIAN_POINT('Ctrl Pts',(0.00355178984688891,-0.0324156524631808,
0.0777705239079862));
#68416=CARTESIAN_POINT('Ctrl Pts',(0.00358366573380517,-0.0324680267167304,
0.0777452816499224));
#68417=CARTESIAN_POINT('Ctrl Pts',(0.00361494791104727,-0.0325210109755912,
0.0777205095457668));
#68418=CARTESIAN_POINT('Origin',(0.00401772587397361,-0.0262834582511791,
0.067438540595134));
#68419=CARTESIAN_POINT('Origin',(-0.00377752765640774,-0.0342770824103611,
0.0766364395902537));
#68420=CARTESIAN_POINT('Ctrl Pts',(0.00369384831184546,-0.0326943950436604,
0.077815646943078));
#68421=CARTESIAN_POINT('Ctrl Pts',(0.00374436779687566,-0.0325844576448134,
0.0778766997345428));
#68422=CARTESIAN_POINT('Ctrl Pts',(0.00379615352907322,-0.0324744968375322,
0.0779367120210303));
#68423=CARTESIAN_POINT('Ctrl Pts',(0.00384913809697668,-0.0323646534831894,
0.0779956078264775));
#68424=CARTESIAN_POINT('Ctrl Pts',(0.0036807754911042,-0.0326943950436604,
0.0779282090545546));
#68425=CARTESIAN_POINT('Ctrl Pts',(0.00373284629299443,-0.0325844576448134,
0.0779894420139903));
#68426=CARTESIAN_POINT('Ctrl Pts',(0.00378618717801016,-0.0324744968375322,
0.0780496023974234));
#68427=CARTESIAN_POINT('Ctrl Pts',(0.00384072873952019,-0.0323646534831894,
0.0781086140665237));
#68428=CARTESIAN_POINT('Ctrl Pts',(0.00366770267036294,-0.0326943950436604,
0.0780407711660313));
#68429=CARTESIAN_POINT('Ctrl Pts',(0.00372132478911321,-0.0325844576448134,
0.0781021842934379));
#68430=CARTESIAN_POINT('Ctrl Pts',(0.00377622082694709,-0.0324744968375322,
0.0781624927738165));
#68431=CARTESIAN_POINT('Ctrl Pts',(0.00383231938206371,-0.0323646534831894,
0.0782216203065699));
#68432=CARTESIAN_POINT('Ctrl Pts',(0.00365462984962169,-0.0326943950436604,
0.078153333277508));
#68433=CARTESIAN_POINT('Ctrl Pts',(0.00370980328523198,-0.0325844576448134,
0.0782149265728854));
#68434=CARTESIAN_POINT('Ctrl Pts',(0.00376625447588403,-0.0324744968375322,
0.0782753831502096));
#68435=CARTESIAN_POINT('Ctrl Pts',(0.00382391002460722,-0.0323646534831894,
0.0783346265466161));
#68436=CARTESIAN_POINT('',(0.0036631912378776,-0.0326773559991367,0.0781628703331065));
#68437=CARTESIAN_POINT('',(0.00365462984962342,-0.0326943950436594,0.078153333277498));
#68438=CARTESIAN_POINT('Origin',(0.0159743814683323,-0.0326395669855557,
0.0670198053090934));
#68439=CARTESIAN_POINT('Ctrl Pts',(0.00366319124036326,-0.0326773559987476,
0.0781628703308607));
#68440=CARTESIAN_POINT('Ctrl Pts',(0.0036951241883951,-0.0326267922587068,
0.0781341425723436));
#68441=CARTESIAN_POINT('Ctrl Pts',(0.00372649114798488,-0.032575610958155,
0.0781059239925992));
#68442=CARTESIAN_POINT('Ctrl Pts',(0.0037881197853654,-0.0324719985462377,
0.0780504811750229));
#68443=CARTESIAN_POINT('Ctrl Pts',(0.0038183567453997,-0.0324196091621775,
0.0780232791739646));
#68444=CARTESIAN_POINT('Ctrl Pts',(0.00384803921492484,-0.0323666188837756,
0.0779965760078223));
#68445=CARTESIAN_POINT('',(0.00367412211789146,-0.0326943950436703,0.0779854972063209));
#68446=CARTESIAN_POINT('Origin',(0.00812378219310841,-0.0315241814719618,
0.07415));
#68447=CARTESIAN_POINT('',(0.0036631912379105,-0.0327114338379855,0.0781628703330763));
#68448=CARTESIAN_POINT('',(0.00367177297545987,-0.0326943950436593,0.0781723890818771));
#68449=CARTESIAN_POINT('Origin',(0.0159435067138025,-0.0326395658227958,
0.066986639998606));
#68450=CARTESIAN_POINT('Origin',(0.0160415858996068,-0.0326395684850483,
0.067094502901923));
#68451=CARTESIAN_POINT('Origin',(0.0160713078331,-0.032639567343421,0.067128705283839));
#68452=CARTESIAN_POINT('Ctrl Pts',(0.00374197532261405,-0.0332451089994432,
0.0778753044908689));
#68453=CARTESIAN_POINT('Ctrl Pts',(0.00388247748022288,-0.0329451141710253,
0.0780405670408267));
#68454=CARTESIAN_POINT('Ctrl Pts',(0.00403502873689203,-0.0326442513127493,
0.0781947769004333));
#68455=CARTESIAN_POINT('Ctrl Pts',(0.00390800821203346,-0.0332451089994432,
0.0780622084224248));
#68456=CARTESIAN_POINT('Ctrl Pts',(0.00405555956675183,-0.0329451141710253,
0.0782212089395058));
#68457=CARTESIAN_POINT('Ctrl Pts',(0.00421466831258984,-0.0326442513127493,
0.0783686435816667));
#68458=CARTESIAN_POINT('Ctrl Pts',(0.00390966854092765,-0.0332451089994432,
0.0780640774617403));
#68459=CARTESIAN_POINT('Ctrl Pts',(0.00405729038761712,-0.0329451141710253,
0.0782230153584925));
#68460=CARTESIAN_POINT('Ctrl Pts',(0.00421646470834681,-0.0326442513127493,
0.078370382248479));
#68461=CARTESIAN_POINT('',(0.00393265065846339,-0.0331951640388616,0.0780885963818732));
#68462=CARTESIAN_POINT('',(0.00409800492860871,-0.0328677532355016,0.0782574618058445));
#68463=CARTESIAN_POINT('Origin',(0.0156101803831019,-0.0326402808282682,
0.0660608140840406));
#68464=CARTESIAN_POINT('Origin',(-0.00364056838794087,-0.0326944278779144,
0.0861535916169325));
#68465=CARTESIAN_POINT('',(0.004009684300756,-0.0326943950436593,0.0781689953386565));
#68466=CARTESIAN_POINT('',(0.00405432007862868,-0.0326943950436692,0.0782127434510212));
#68467=CARTESIAN_POINT('',(0.0038480392148867,-0.0330220786163545,0.0779965760078528));
#68468=CARTESIAN_POINT('Origin',(0.0159748003131234,-0.0326396682764862,
0.06637419077711));
#68469=CARTESIAN_POINT('',(0.00384904919316599,-0.0331951640388587,0.077995667403612));
#68470=CARTESIAN_POINT('Origin',(-0.00435223336755533,-0.0331952026560077,
0.085373765661119));
#68471=CARTESIAN_POINT('',(0.00389084992582468,-0.0331951640388701,0.0780421318927526));
#68472=CARTESIAN_POINT('Ctrl Pts',(0.0035093283533754,-0.0330240426238172,
0.0779849466438276));
#68473=CARTESIAN_POINT('Ctrl Pts',(0.0035621584796016,-0.032914277406352,
0.0780485152411145));
#68474=CARTESIAN_POINT('Ctrl Pts',(0.00361632908404852,-0.0328043479726691,
0.0781110233833827));
#68475=CARTESIAN_POINT('Ctrl Pts',(0.00367177297545988,-0.0326943950436593,
0.0781723890818771));
#68476=CARTESIAN_POINT('Ctrl Pts',(0.00362259158667951,-0.0330240426238172,
0.0779884929046831));
#68477=CARTESIAN_POINT('Ctrl Pts',(0.00367547056610395,-0.032914277406352,
0.0780505011905842));
#68478=CARTESIAN_POINT('Ctrl Pts',(0.00372965779210934,-0.0328043479726691,
0.0781114472336624));
#68479=CARTESIAN_POINT('Ctrl Pts',(0.00378508599703424,-0.0326943950436593,
0.0781712510457416));
#68480=CARTESIAN_POINT('Ctrl Pts',(0.00373585481998362,-0.0330240426238172,
0.0779920391655386));
#68481=CARTESIAN_POINT('Ctrl Pts',(0.00378878265260629,-0.032914277406352,
0.0780524871400539));
#68482=CARTESIAN_POINT('Ctrl Pts',(0.00384298650017017,-0.0328043479726691,
0.0781118710839421));
#68483=CARTESIAN_POINT('Ctrl Pts',(0.00389839901860859,-0.0326943950436593,
0.0781701130096061));
#68484=CARTESIAN_POINT('Ctrl Pts',(0.00384911805328772,-0.0330240426238172,
0.0779955854263941));
#68485=CARTESIAN_POINT('Ctrl Pts',(0.00390209473910864,-0.032914277406352,
0.0780544730895236));
#68486=CARTESIAN_POINT('Ctrl Pts',(0.003956315208231,-0.0328043479726691,
0.0781122949342219));
#68487=CARTESIAN_POINT('Ctrl Pts',(0.00401171204018295,-0.0326943950436593,
0.0781689749734706));
#68488=CARTESIAN_POINT('',(0.00384072863811794,-0.0326943950436694,0.0781706922102768));
#68489=CARTESIAN_POINT('Ctrl Pts',(0.00366319124037136,-0.0327114338383316,
0.0781628703308533));
#68490=CARTESIAN_POINT('Ctrl Pts',(0.00369511887698221,-0.0327619876831102,
0.0781341473506367));
#68491=CARTESIAN_POINT('Ctrl Pts',(0.00372648324226078,-0.0328131562604614,
0.078105931104806));
#68492=CARTESIAN_POINT('Ctrl Pts',(0.00378811182289566,-0.0329167375858765,
0.0780504883382796));
#68493=CARTESIAN_POINT('Ctrl Pts',(0.00381835148227642,-0.0329691088920623,
0.078023283908815));
#68494=CARTESIAN_POINT('Ctrl Pts',(0.00384803921492386,-0.0330220786163187,
0.0779965760078231));
#68495=CARTESIAN_POINT('Ctrl Pts',(0.00393275766748565,-0.0331951640388604,
0.078086571152787));
#68496=CARTESIAN_POINT('Ctrl Pts',(0.00401414375217492,-0.0330306422010619,
0.0781732178978193));
#68497=CARTESIAN_POINT('Ctrl Pts',(0.00409904149411709,-0.0328657861914645,
0.0782564268313473));
#68498=CARTESIAN_POINT('Ctrl Pts',(0.00393265065846129,-0.0331951640388604,
0.078088596381871));
#68499=CARTESIAN_POINT('Ctrl Pts',(0.00401407861346341,-0.0330306422010619,
0.0781752453392462));
#68500=CARTESIAN_POINT('Ctrl Pts',(0.00409901828137901,-0.0328657861914645,
0.0782584547526827));
#68501=CARTESIAN_POINT('Ctrl Pts',(0.00391482007723423,-0.0331951640388604,
0.0784260540112631));
#68502=CARTESIAN_POINT('Ctrl Pts',(0.00400322475236632,-0.0330306422010619,
0.0785130716044733));
#68503=CARTESIAN_POINT('Ctrl Pts',(0.00409515041496016,-0.0328657861914645,
0.0785963609835681));
#68504=CARTESIAN_POINT('',(0.00392396340684694,-0.033178164828192,0.0784350346741231));
#68505=CARTESIAN_POINT('',(0.00391482007723563,-0.0331951640388588,0.0784260540112524));
#68506=CARTESIAN_POINT('Origin',(0.0149696437100718,-0.0326412091873849,
0.0661476661280231));
#68507=CARTESIAN_POINT('Ctrl Pts',(0.00392396340651288,-0.033178164828644,
0.0784350346723065));
#68508=CARTESIAN_POINT('Ctrl Pts',(0.00395405020197888,-0.0331276811546783,
0.0784043373872559));
#68509=CARTESIAN_POINT('Ctrl Pts',(0.00398359369894219,-0.0330765663497789,
0.0783741943764374));
#68510=CARTESIAN_POINT('Ctrl Pts',(0.00404161959471262,-0.0329730614463239,
0.0783149911186314));
#68511=CARTESIAN_POINT('Ctrl Pts',(0.00407007855615157,-0.0329207133373932,
0.0782859547922208));
#68512=CARTESIAN_POINT('Ctrl Pts',(0.00409800491252451,-0.0328677532289374,
0.0782574618022812));
#68513=CARTESIAN_POINT('',(0.00392373536785951,-0.0331951640388702,0.0782573251965728));
#68514=CARTESIAN_POINT('Origin',(0.00812378219310841,-0.0315241814719618,
0.07415));
#68515=CARTESIAN_POINT('',(0.00392396340839382,-0.0332121607144402,0.0784350346734683));
#68516=CARTESIAN_POINT('',(0.00393312589888615,-0.0331951640388587,0.0784439957875769));
#68517=CARTESIAN_POINT('Origin',(0.0149322586422581,-0.0326413640258274,
0.0661220012505349));
#68518=CARTESIAN_POINT('Origin',(0.0159870069992313,-0.0326412104640766,
0.0671447922847213));
#68519=CARTESIAN_POINT('Origin',(0.0160134126578002,-0.0326413654427593,
0.0671816590824428));
#68520=CARTESIAN_POINT('Ctrl Pts',(0.00398452115888946,-0.0337436976235975,
0.0781430743908167));
#68521=CARTESIAN_POINT('Ctrl Pts',(0.00402043547512745,-0.0336723290703325,
0.0781803035318806));
#68522=CARTESIAN_POINT('Ctrl Pts',(0.00405701361617926,-0.033601104548885,
0.0782168806647972));
#68523=CARTESIAN_POINT('Ctrl Pts',(0.0041738003748362,-0.0333736987606857,
0.0783336642046779));
#68524=CARTESIAN_POINT('Ctrl Pts',(0.00429709639104041,-0.0331450831799192,
0.0784435533969256));
#68525=CARTESIAN_POINT('Ctrl Pts',(0.00416196157741737,-0.0337436976235975,
0.0783191848614669));
#68526=CARTESIAN_POINT('Ctrl Pts',(0.00419945985791865,-0.0336723290703325,
0.0783548180765149));
#68527=CARTESIAN_POINT('Ctrl Pts',(0.00423759300130689,-0.033601104548885,
0.078389771051074));
#68528=CARTESIAN_POINT('Ctrl Pts',(0.00435934457439544,-0.0333736987606857,
0.0785013689750472));
#68529=CARTESIAN_POINT('Ctrl Pts',(0.00448729964286908,-0.0331450831799192,
0.0786057961871931));
#68530=CARTESIAN_POINT('Ctrl Pts',(0.00416373598160265,-0.0337436976235975,
0.0783209459661734));
#68531=CARTESIAN_POINT('Ctrl Pts',(0.00420125010174657,-0.0336723290703325,
0.0783565632219612));
#68532=CARTESIAN_POINT('Ctrl Pts',(0.00423939879515817,-0.033601104548885,
0.0783914999549368));
#68533=CARTESIAN_POINT('Ctrl Pts',(0.00436120001639104,-0.0333736987606857,
0.0785030460227508));
#68534=CARTESIAN_POINT('Ctrl Pts',(0.00448920167538737,-0.0331450831799192,
0.0786074186150958));
#68535=CARTESIAN_POINT('',(0.00418822741221839,-0.0336938721132548,0.078343987788086));
#68536=CARTESIAN_POINT('',(0.00436385854011419,-0.0333679869945434,0.0785021373052407));
#68537=CARTESIAN_POINT('Ctrl Pts',(0.00418822741222797,-0.0336938721132648,
0.0783439877880965));
#68538=CARTESIAN_POINT('Ctrl Pts',(0.00420459851399994,-0.0336629187933931,
0.0783593501046076));
#68539=CARTESIAN_POINT('Ctrl Pts',(0.0042210543324433,-0.0336319952301039,
0.0783746116485008));
#68540=CARTESIAN_POINT('Ctrl Pts',(0.00423759300131699,-0.0336011045488949,
0.0783897710510839));
#68541=CARTESIAN_POINT('Ctrl Pts',(0.00427909418073509,-0.0335235892595453,
0.0784278111794205));
#68542=CARTESIAN_POINT('Ctrl Pts',(0.00432119089700305,-0.0334458668660368,
0.0784652756281618));
#68543=CARTESIAN_POINT('Ctrl Pts',(0.00436385853990239,-0.0333679869945384,
0.0785021373054752));
#68544=CARTESIAN_POINT('Ctrl Pts',(0.00436389174180533,-0.0333679692460741,
0.078502166897738));
#68545=CARTESIAN_POINT('Ctrl Pts',(0.00436418354275695,-0.033339189537532,
0.0785018200692105));
#68546=CARTESIAN_POINT('Ctrl Pts',(0.00436439977706645,-0.0333104081060831,
0.0785015580137926));
#68547=CARTESIAN_POINT('Ctrl Pts',(0.00436468172845928,-0.0332532697777497,
0.0785012076134217));
#68548=CARTESIAN_POINT('Ctrl Pts',(0.00436474964008472,-0.0332249169019147,
0.0785011167321469));
#68549=CARTESIAN_POINT('Ctrl Pts',(0.00436474682003064,-0.0331960985456441,
0.0785011094454358));
#68550=CARTESIAN_POINT('Ctrl Pts',(0.00436474675475889,-0.0331956312467839,
0.0785011093497213));
#68551=CARTESIAN_POINT('Ctrl Pts',(0.00436474667057917,-0.0331951640388602,
0.0785011092769963));
#68552=CARTESIAN_POINT('',(0.00427015733847041,-0.0331951640388587,0.078419391113463));
#68553=CARTESIAN_POINT('',(0.00431745200453479,-0.0331951640388687,0.0784602501952397));
#68554=CARTESIAN_POINT('',(0.00409800492306439,-0.0335216366567692,0.0782574617913545));
#68555=CARTESIAN_POINT('Origin',(0.0148599224840116,-0.0326434571526649,
0.065547159063874));
#68556=CARTESIAN_POINT('',(0.00409895585648141,-0.0336938721132328,0.0782564915633658));
#68557=CARTESIAN_POINT('Origin',(-0.00354511341528025,-0.0336938867896257,
0.0860556604238307));
#68558=CARTESIAN_POINT('',(0.0041435916343599,-0.0336938721132538,0.0783002396757359));
#68559=CARTESIAN_POINT('Ctrl Pts',(0.00375923287556075,-0.0335235895815172,
0.0782671239056808));
#68560=CARTESIAN_POINT('Ctrl Pts',(0.00381591319199349,-0.0334144449262748,
0.0783272105200437));
#68561=CARTESIAN_POINT('Ctrl Pts',(0.00387389997147532,-0.0333049234473147,
0.078386195193966));
#68562=CARTESIAN_POINT('Ctrl Pts',(0.00393312589888597,-0.0331951640388587,
0.0784439957875769));
#68563=CARTESIAN_POINT('Ctrl Pts',(0.00387249544171201,-0.0335235895815172,
0.0782635512883181));
#68564=CARTESIAN_POINT('Ctrl Pts',(0.00392912657403291,-0.0334144449262748,
0.0783220786204644));
#68565=CARTESIAN_POINT('Ctrl Pts',(0.00398703189929923,-0.0333049234473147,
0.0783795032368506));
#68566=CARTESIAN_POINT('Ctrl Pts',(0.00404614402584485,-0.0331951640388587,
0.0784357450018751));
#68567=CARTESIAN_POINT('Ctrl Pts',(0.00398575800786327,-0.0335235895815172,
0.0782599786709554));
#68568=CARTESIAN_POINT('Ctrl Pts',(0.00404233995607234,-0.0334144449262748,
0.0783169467208852));
#68569=CARTESIAN_POINT('Ctrl Pts',(0.00410016382712313,-0.0333049234473147,
0.0783728112797351));
#68570=CARTESIAN_POINT('Ctrl Pts',(0.00415916215280372,-0.0331951640388587,
0.0784274942161733));
#68571=CARTESIAN_POINT('Ctrl Pts',(0.00409902057401453,-0.0335235895815172,
0.0782564060535926));
#68572=CARTESIAN_POINT('Ctrl Pts',(0.00415555333811177,-0.0334144449262748,
0.0783118148213059));
#68573=CARTESIAN_POINT('Ctrl Pts',(0.00421329575494704,-0.0333049234473147,
0.0783661193226197));
#68574=CARTESIAN_POINT('Ctrl Pts',(0.0042721802797626,-0.0331951640388587,
0.0784192434304715));
#68575=CARTESIAN_POINT('',(0.00410164161868828,-0.0331951640388687,0.0784316934505299));
#68576=CARTESIAN_POINT('Ctrl Pts',(0.00392396341058244,-0.033212160714597,
0.0784350346712254));
#68577=CARTESIAN_POINT('Ctrl Pts',(0.00395399960100596,-0.033262544410987,
0.0784043890353013));
#68578=CARTESIAN_POINT('Ctrl Pts',(0.00398351822073386,-0.0333135300747073,
0.0783742714717752));
#68579=CARTESIAN_POINT('Ctrl Pts',(0.00404154375026909,-0.0334167203140585,
0.078315068582615));
#68580=CARTESIAN_POINT('Ctrl Pts',(0.00407002818633233,-0.0334688847587279,
0.0782860061867257));
#68581=CARTESIAN_POINT('Ctrl Pts',(0.00409800492366914,-0.0335216366562345,
0.0782574617909592));
#68582=CARTESIAN_POINT('Ctrl Pts',(0.00418821737084671,-0.0336938721132389,
0.0783429879810832));
#68583=CARTESIAN_POINT('Ctrl Pts',(0.00421276032088089,-0.0336474569764957,
0.0783660241479467));
#68584=CARTESIAN_POINT('Ctrl Pts',(0.00423757125663496,-0.033601104548885,
0.0783887714301394));
#68585=CARTESIAN_POINT('Ctrl Pts',(0.00430038684157254,-0.0334837508592656,
0.0784463623187233));
#68586=CARTESIAN_POINT('Ctrl Pts',(0.00436488137996903,-0.0333660264659097,
0.0785020665616132));
#68587=CARTESIAN_POINT('Ctrl Pts',(0.00418822741220353,-0.0336938721132389,
0.078343987788072));
#68588=CARTESIAN_POINT('Ctrl Pts',(0.00421277621443978,-0.0336474569764957,
0.0783670238961601));
#68589=CARTESIAN_POINT('Ctrl Pts',(0.00423759300130689,-0.033601104548885,
0.078389771051074));
#68590=CARTESIAN_POINT('Ctrl Pts',(0.00430042339991743,-0.0334837508592656,
0.0784473616174172));
#68591=CARTESIAN_POINT('Ctrl Pts',(0.00436493273593315,-0.0333660264659097,
0.0785030650992483));
#68592=CARTESIAN_POINT('Ctrl Pts',(0.00419164151788341,-0.0336938721132389,
0.0786839265813392));
#68593=CARTESIAN_POINT('Ctrl Pts',(0.00421818009468031,-0.0336474569764957,
0.0787069427055339));
#68594=CARTESIAN_POINT('Ctrl Pts',(0.00424498628583072,-0.033601104548885,
0.0787296465851001));
#68595=CARTESIAN_POINT('Ctrl Pts',(0.0043128533986939,-0.0334837508592656,
0.0787871275882126));
#68596=CARTESIAN_POINT('Ctrl Pts',(0.00438239399062286,-0.0333660264659097,
0.0788425723066389));
#68597=CARTESIAN_POINT('',(0.00420131034351263,-0.0336769361243753,0.0786902879412135));
#68598=CARTESIAN_POINT('',(0.00419162115542691,-0.033693872113232,0.0786818991133673));
#68599=CARTESIAN_POINT('Ctrl Pts',(0.00420131034351287,-0.033676936124375,
0.0786902879412137));
#68600=CARTESIAN_POINT('Ctrl Pts',(0.00419969386454803,-0.0336797586670257,
0.0786888914233459));
#68601=CARTESIAN_POINT('Ctrl Pts',(0.00419807819252284,-0.0336825812713308,
0.0786874940950229));
#68602=CARTESIAN_POINT('Ctrl Pts',(0.00419484846833955,-0.0336882265921195,
0.0786846978233311));
#68603=CARTESIAN_POINT('Ctrl Pts',(0.00419323441613566,-0.0336910493086635,
0.0786832988799539));
#68604=CARTESIAN_POINT('Ctrl Pts',(0.00419162115542556,-0.0336938721132361,
0.0786818991133772));
#68605=CARTESIAN_POINT('Ctrl Pts',(0.00420131034351269,-0.0336769361243753,
0.0786902879412135));
#68606=CARTESIAN_POINT('Ctrl Pts',(0.00422870993497068,-0.0336279031301507,
0.0786585727270677));
#68607=CARTESIAN_POINT('Ctrl Pts',(0.00425650373818913,-0.0335767851899387,
0.0786264012101173));
#68608=CARTESIAN_POINT('Ctrl Pts',(0.00431096501853182,-0.0334733198857322,
0.0785633619063608));
#68609=CARTESIAN_POINT('Ctrl Pts',(0.00433766906313391,-0.0334209645014062,
0.0785324517924494));
#68610=CARTESIAN_POINT('Ctrl Pts',(0.00436385853458973,-0.033367986984468,
0.0785021373004666));
#68611=CARTESIAN_POINT('',(0.00418992428383265,-0.0336938721132534,0.0785129434507367));
#68612=CARTESIAN_POINT('Origin',(0.00812378219310841,-0.0315241814719618,
0.07415));
#68613=CARTESIAN_POINT('',(0.00420131034436393,-0.0337108120655529,0.0786902879402389));
#68614=CARTESIAN_POINT('',(0.00421101742817701,-0.0336938721132327,0.0786986560536431));
#68615=CARTESIAN_POINT('Origin',(0.0157430862401175,-0.0345562509322005,
0.0670401444338427));
#68616=CARTESIAN_POINT('Ctrl Pts',(0.00421101742817892,-0.0336938721132319,
0.0786986560536424));
#68617=CARTESIAN_POINT('Ctrl Pts',(0.0042093982121299,-0.0336910493257073,
0.0786972632001427));
#68618=CARTESIAN_POINT('Ctrl Pts',(0.00420777968091916,-0.0336882266006415,
0.0786958694313745));
#68619=CARTESIAN_POINT('Ctrl Pts',(0.00420454398607452,-0.0336825812712706,
0.0786930800608296));
#68620=CARTESIAN_POINT('Ctrl Pts',(0.00420292682246003,-0.0336797586669955,
0.0786916844590663));
#68621=CARTESIAN_POINT('Ctrl Pts',(0.00420131034351245,-0.033676936124375,
0.0786902879412133));
#68622=CARTESIAN_POINT('Origin',(0.0140516683263155,-0.0345562513563432,
0.0655788895999354));
#68623=CARTESIAN_POINT('Ctrl Pts',(0.00424337814675107,-0.034243627687391,
0.0783950664820488));
#68624=CARTESIAN_POINT('Ctrl Pts',(0.00440348346849126,-0.0339430054201809,
0.078541418333298));
#68625=CARTESIAN_POINT('Ctrl Pts',(0.00457415776889112,-0.0336441434784052,
0.078675294625436));
#68626=CARTESIAN_POINT('Ctrl Pts',(0.00443152501705866,-0.034243627687391,
0.0785596895521011));
#68627=CARTESIAN_POINT('Ctrl Pts',(0.00459783920024025,-0.0339430054201809,
0.0786989453271564));
#68628=CARTESIAN_POINT('Ctrl Pts',(0.00477417021782287,-0.0336441434784052,
0.0788252780254251));
#68629=CARTESIAN_POINT('Ctrl Pts',(0.00443340648576174,-0.034243627687391,
0.0785613357828016));
#68630=CARTESIAN_POINT('Ctrl Pts',(0.00459978275755775,-0.0339430054201809,
0.078700520597095));
#68631=CARTESIAN_POINT('Ctrl Pts',(0.00477617034231219,-0.0336441434784052,
0.0788267778594251));
#68632=CARTESIAN_POINT('',(0.00445933600268769,-0.0341934961088741,0.0785828274405296));
#68633=CARTESIAN_POINT('',(0.00464455084769837,-0.033866421286606,0.0787296369122528));
#68634=CARTESIAN_POINT('Origin',(0.0155096437724735,-0.0345610720405944,
0.0660152563958636));
#68635=CARTESIAN_POINT('Origin',(-0.00198935276394271,-0.0336938005073003,
0.087461764218862));
#68636=CARTESIAN_POINT('',(0.00454583887293236,-0.0336938721132327,0.078652937552044));
#68637=CARTESIAN_POINT('',(0.0045956057767483,-0.0336938721132427,0.0786907463511036));
#68638=CARTESIAN_POINT('',(0.00436385853458568,-0.0340203938281605,0.0785021373004631));
#68639=CARTESIAN_POINT('Origin',(0.0158177017432013,-0.0345589643243796,
0.0663849008475276));
#68640=CARTESIAN_POINT('',(0.00436474667057904,-0.034193496108874,0.0785011092769962));
#68641=CARTESIAN_POINT('Origin',(-0.00283916590558952,-0.0341934220717559,
0.0868396860044658));
#68642=CARTESIAN_POINT('',(0.00441204133664336,-0.0341934961088841,0.078541968358773));
#68643=CARTESIAN_POINT('Ctrl Pts',(0.00402635966682603,-0.0340223579322397,
0.078533050152708));
#68644=CARTESIAN_POINT('Ctrl Pts',(0.00408681335990656,-0.0339125849573575,
0.078589564295872));
#68645=CARTESIAN_POINT('Ctrl Pts',(0.00414839428431968,-0.0338030433565231,
0.0786447874762301));
#68646=CARTESIAN_POINT('Ctrl Pts',(0.0042110174281763,-0.0336938721132327,
0.0786986560536433));
#68647=CARTESIAN_POINT('Ctrl Pts',(0.00413917444580609,-0.0340223579322397,
0.0785223728181119));
#68648=CARTESIAN_POINT('Ctrl Pts',(0.00419948087059488,-0.0339125849573575,
0.0785773309512404));
#68649=CARTESIAN_POINT('Ctrl Pts',(0.00426088242440792,-0.0338030433565231,
0.0786310022630648));
#68650=CARTESIAN_POINT('Ctrl Pts',(0.00432329450066539,-0.0336938721132327,
0.0786833250776902));
#68651=CARTESIAN_POINT('Ctrl Pts',(0.00425198922478615,-0.0340223579322397,
0.0785116954835158));
#68652=CARTESIAN_POINT('Ctrl Pts',(0.0043121483812832,-0.0339125849573575,
0.0785650976066089));
#68653=CARTESIAN_POINT('Ctrl Pts',(0.00437337056449616,-0.0338030433565231,
0.0786172170498995));
#68654=CARTESIAN_POINT('Ctrl Pts',(0.00443557157315449,-0.0336938721132327,
0.078667994101737));
#68655=CARTESIAN_POINT('Ctrl Pts',(0.00436480400376621,-0.0340223579322397,
0.0785010181489197));
#68656=CARTESIAN_POINT('Ctrl Pts',(0.00442481589197153,-0.0339125849573575,
0.0785528642619773));
#68657=CARTESIAN_POINT('Ctrl Pts',(0.0044858587045844,-0.0338030433565231,
0.0786034318367342));
#68658=CARTESIAN_POINT('Ctrl Pts',(0.00454784864564359,-0.0336938721132327,
0.0786526631257839));
#68659=CARTESIAN_POINT('',(0.00437842815056468,-0.0336938721132427,0.0786757968028536));
#68660=CARTESIAN_POINT('Ctrl Pts',(0.00420131034671543,-0.033710812066268,
0.0786902879375062));
#68661=CARTESIAN_POINT('Ctrl Pts',(0.00422942090869603,-0.0337611408994384,
0.0786577497701273));
#68662=CARTESIAN_POINT('Ctrl Pts',(0.00425701851528578,-0.03381210887815,
0.0786258053521147));
#68663=CARTESIAN_POINT('Ctrl Pts',(0.00431121295864493,-0.0339153382773232,
0.0785630749139882));
#68664=CARTESIAN_POINT('Ctrl Pts',(0.00433778686786166,-0.0339675558473116,
0.0785323154326729));
#68665=CARTESIAN_POINT('Ctrl Pts',(0.00436385853461576,-0.0340203938281304,
0.0785021373004364));
#68666=CARTESIAN_POINT('Ctrl Pts',(0.00445918833261691,-0.0341934961088741,
0.0785808046762242));
#68667=CARTESIAN_POINT('Ctrl Pts',(0.00455079172865743,-0.0340287516182427,
0.0786565672672794));
#68668=CARTESIAN_POINT('Ctrl Pts',(0.00464544817671417,-0.0338644633275951,
0.0787284790827956));
#68669=CARTESIAN_POINT('Ctrl Pts',(0.0044593360026877,-0.0341934961088741,
0.0785828274405296));
#68670=CARTESIAN_POINT('Ctrl Pts',(0.00455098121778667,-0.0340287516182427,
0.0786585869786223));
#68671=CARTESIAN_POINT('Ctrl Pts',(0.00464567932298703,-0.0338644633275951,
0.0787304940153715));
#68672=CARTESIAN_POINT('Ctrl Pts',(0.00448394067680217,-0.0341934961088741,
0.0789198588801231));
#68673=CARTESIAN_POINT('Ctrl Pts',(0.00458255375139738,-0.0340287516182427,
0.0789951097359624));
#68674=CARTESIAN_POINT('Ctrl Pts',(0.00468419273796784,-0.0338644633275951,
0.0790662205381982));
#68675=CARTESIAN_POINT('',(0.00449413748415137,-0.0341764758832413,0.0789276227642436));
#68676=CARTESIAN_POINT('',(0.00448394067680121,-0.034193496108874,0.0789198588801102));
#68677=CARTESIAN_POINT('Origin',(0.0149183650452552,-0.0345621026722942,
0.0660529651115736));
#68678=CARTESIAN_POINT('Ctrl Pts',(0.00449413748339433,-0.0341764758837513,
0.0789276227625805));
#68679=CARTESIAN_POINT('Ctrl Pts',(0.00452010417916289,-0.0341260050040843,
0.0788934433402988));
#68680=CARTESIAN_POINT('Ctrl Pts',(0.00454561948207761,-0.0340749269148962,
0.0788598580138956));
#68681=CARTESIAN_POINT('Ctrl Pts',(0.00459576722287304,-0.0339715436307836,
0.0787938496348361));
#68682=CARTESIAN_POINT('Ctrl Pts',(0.00462038064066904,-0.0339192778237455,
0.0787614516277956));
#68683=CARTESIAN_POINT('Ctrl Pts',(0.00464455084621759,-0.0338664212855905,
0.078729636912815));
#68684=CARTESIAN_POINT('',(0.00447163833975446,-0.0341934961088841,0.0787513431603299));
#68685=CARTESIAN_POINT('Origin',(0.00812378219310841,-0.0315241814719618,
0.07415));
#68686=CARTESIAN_POINT('',(0.00449413748526666,-0.0342105180190354,0.0789276227641661));
#68687=CARTESIAN_POINT('',(0.00450435085242285,-0.0341934961088739,0.0789353648523489));
#68688=CARTESIAN_POINT('Origin',(0.0148856805237589,-0.0345621700122827,
0.0660215583807938));
#68689=CARTESIAN_POINT('Origin',(0.0141028267023117,-0.0345621042433387,
0.0654333822330383));
#68690=CARTESIAN_POINT('Origin',(0.0141418420727513,-0.0345621713716514,
0.0654564562677148));
#68691=CARTESIAN_POINT('Ctrl Pts',(0.00454464445934973,-0.0346945769586966,
0.0786520301348715));
#68692=CARTESIAN_POINT('Ctrl Pts',(0.00463894128303914,-0.0345275153362944,
0.0787269966077136));
#68693=CARTESIAN_POINT('Ctrl Pts',(0.00473562012328609,-0.0343603235965186,
0.0787990169224147));
#68694=CARTESIAN_POINT('Ctrl Pts',(0.00483439188120101,-0.034193496108874,
0.0788678823245642));
#68695=CARTESIAN_POINT('Ctrl Pts',(0.00461139846911413,-0.0346945769586966,
0.0787027443394518));
#68696=CARTESIAN_POINT('Ctrl Pts',(0.00470675752212333,-0.0345275153362944,
0.0787763126228326));
#68697=CARTESIAN_POINT('Ctrl Pts',(0.00480445489466537,-0.0343603235965186,
0.0788469009802945));
#68698=CARTESIAN_POINT('Ctrl Pts',(0.0049041985384288,-0.034193496108874,
0.0789143049372926));
#68699=CARTESIAN_POINT('Ctrl Pts',(0.00467815247887855,-0.0346945769586966,
0.0787534585440321));
#68700=CARTESIAN_POINT('Ctrl Pts',(0.0047745737612075,-0.0345275153362944,
0.0788256286379508));
#68701=CARTESIAN_POINT('Ctrl Pts',(0.00487328966604467,-0.0343603235965186,
0.0788947850381736));
#68702=CARTESIAN_POINT('Ctrl Pts',(0.00497400519565672,-0.034193496108874,
0.0789607275500208));
#68703=CARTESIAN_POINT('Ctrl Pts',(0.00474490648864292,-0.0346945769586966,
0.0788041727486125));
#68704=CARTESIAN_POINT('Ctrl Pts',(0.00484239000029171,-0.0345275153362944,
0.0788749446530705));
#68705=CARTESIAN_POINT('Ctrl Pts',(0.00494212443742393,-0.0343603235965186,
0.0789426690960541));
#68706=CARTESIAN_POINT('Ctrl Pts',(0.00504381185288439,-0.034193496108874,
0.0790071501627492));
#68707=CARTESIAN_POINT('',(0.00474490648816067,-0.0346945769586966,0.0788041727482459));
#68708=CARTESIAN_POINT('',(0.00493897409661285,-0.0343667727831496,0.0789390627881592));
#68709=CARTESIAN_POINT('Origin',(0.0144741125225068,-0.0345626457065151,
0.0650914123699995));
#68710=CARTESIAN_POINT('Origin',(-0.00118115406393903,-0.0341934771028877,
0.0881420343625942));
#68711=CARTESIAN_POINT('',(0.00483564091507222,-0.034193496108874,0.0788687129533036));
#68712=CARTESIAN_POINT('',(0.00488768364940678,-0.034193496108884,0.0789033222555896));
#68713=CARTESIAN_POINT('',(0.00464455084722664,-0.0345211942962657,0.0787296369115627));
#68714=CARTESIAN_POINT('Origin',(0.0148549574993365,-0.0345625596120213,
0.0653849219839156));
#68715=CARTESIAN_POINT('',(0.00464537268054424,-0.0346945769586886,0.0787285551501433));
#68716=CARTESIAN_POINT('Origin',(-0.00204743084295042,-0.0346945685853865,
0.0875381462982233));
#68717=CARTESIAN_POINT('',(0.00469513958436245,-0.0346945769587026,0.0787663639492045));
#68718=CARTESIAN_POINT('Ctrl Pts',(0.00430965973317534,-0.0345231616327842,
0.0787816811052434));
#68719=CARTESIAN_POINT('Ctrl Pts',(0.00437350093632571,-0.0344132092796988,
0.0788342534134986));
#68720=CARTESIAN_POINT('Ctrl Pts',(0.00443842626229129,-0.034303273855898,
0.0788855025043345));
#68721=CARTESIAN_POINT('Ctrl Pts',(0.00450435085242282,-0.0341934961088739,
0.078935364852349));
#68722=CARTESIAN_POINT('Ctrl Pts',(0.00442158126932214,-0.0345231616327842,
0.0787639411535772));
#68723=CARTESIAN_POINT('Ctrl Pts',(0.00448517795221465,-0.0344132092796988,
0.0788149707810296));
#68724=CARTESIAN_POINT('Ctrl Pts',(0.00454982686140292,-0.034303273855898,
0.0788646823283665));
#68725=CARTESIAN_POINT('Ctrl Pts',(0.00461544354281598,-0.0341934961088739,
0.0789130142308859));
#68726=CARTESIAN_POINT('Ctrl Pts',(0.00453350280546893,-0.0345231616327842,
0.0787462012019111));
#68727=CARTESIAN_POINT('Ctrl Pts',(0.00459685496810358,-0.0344132092796988,
0.0787956881485606));
#68728=CARTESIAN_POINT('Ctrl Pts',(0.00466122746051455,-0.0343032738558979,
0.0788438621523986));
#68729=CARTESIAN_POINT('Ctrl Pts',(0.00472653623320913,-0.0341934961088739,
0.0788906636094228));
#68730=CARTESIAN_POINT('Ctrl Pts',(0.00464542434161573,-0.0345231616327842,
0.0787284612502449));
#68731=CARTESIAN_POINT('Ctrl Pts',(0.00470853198399252,-0.0344132092796988,
0.0787764055160916));
#68732=CARTESIAN_POINT('Ctrl Pts',(0.00477262805962619,-0.0343032738558979,
0.0788230419764306));
#68733=CARTESIAN_POINT('Ctrl Pts',(0.00483762892360229,-0.0341934961088739,
0.0788683129879597));
#68734=CARTESIAN_POINT('',(0.00466999588375753,-0.0341934961088839,0.0789020389028363));
#68735=CARTESIAN_POINT('Ctrl Pts',(0.00449413748735283,-0.0342105180195383,
0.0789276227614087));
#68736=CARTESIAN_POINT('Ctrl Pts',(0.00452013338569833,-0.0342610556241287,
0.0788934049231057));
#68737=CARTESIAN_POINT('Ctrl Pts',(0.00454566280108907,-0.0343122189870131,
0.0788598011062189));
#68738=CARTESIAN_POINT('Ctrl Pts',(0.00459581104454471,-0.0344158119695132,
0.0787937920588325));
#68739=CARTESIAN_POINT('Ctrl Pts',(0.0046204093616113,-0.034468199045002,
0.0787614138265159));
#68740=CARTESIAN_POINT('Ctrl Pts',(0.00464455084723834,-0.0345211942962437,
0.0787296369115348));
#68741=CARTESIAN_POINT('Ctrl Pts',(0.00474463216623766,-0.0346945769586932,
0.0788021637397005));
#68742=CARTESIAN_POINT('Ctrl Pts',(0.00484081235979049,-0.034529677707698,
0.0788720252754961));
#68743=CARTESIAN_POINT('Ctrl Pts',(0.00493979781004147,-0.034364806625142,
0.078937851899701));
#68744=CARTESIAN_POINT('Ctrl Pts',(0.00474490648815338,-0.0346945769586932,
0.0788041727482405));
#68745=CARTESIAN_POINT('Ctrl Pts',(0.00484112821653624,-0.034529677707698,
0.0788740286126247));
#68746=CARTESIAN_POINT('Ctrl Pts',(0.00494015493172163,-0.034364806625142,
0.0789398478535915));
#68747=CARTESIAN_POINT('Ctrl Pts',(0.0047906249897536,-0.0346945769586932,
0.0791389941930059));
#68748=CARTESIAN_POINT('Ctrl Pts',(0.00489376891459494,-0.034529677707698,
0.0792079048597189));
#68749=CARTESIAN_POINT('Ctrl Pts',(0.00499967284542011,-0.034364806625142,
0.0792724936099335));
#68750=CARTESIAN_POINT('',(0.00480128917430954,-0.0346775396665,0.0791461024942956));
#68751=CARTESIAN_POINT('',(0.00479062498975458,-0.0346945769586886,0.0791389941929943));
#68752=CARTESIAN_POINT('Origin',(0.0138668481856376,-0.0345626618035967,
0.065238243567384));
#68753=CARTESIAN_POINT('Ctrl Pts',(0.00480128917354233,-0.0346775396670097,
0.0791461024926342));
#68754=CARTESIAN_POINT('Ctrl Pts',(0.004825077207445,-0.0346269749928202,
0.0791103319034466));
#68755=CARTESIAN_POINT('Ctrl Pts',(0.00484844244499505,-0.034575790289082,
0.079075197017556));
#68756=CARTESIAN_POINT('Ctrl Pts',(0.00489434671355866,-0.0344721681087932,
0.079006169812157));
#68757=CARTESIAN_POINT('Ctrl Pts',(0.00491686775263628,-0.0344197714289493,
0.0789723045576773));
#68758=CARTESIAN_POINT('Ctrl Pts',(0.0049389740963452,-0.0343667727830694,
0.078939062788109));
#68759=CARTESIAN_POINT('',(0.00476776573896762,-0.0346945769587026,0.0789715834706301));
#68760=CARTESIAN_POINT('Ctrl Pts',(0.00480399461433585,-0.0352450361874068,
0.0788465703505273));
#68761=CARTESIAN_POINT('Ctrl Pts',(0.00498112867174079,-0.0349452760959493,
0.0789717781936259));
#68762=CARTESIAN_POINT('Ctrl Pts',(0.00516719067698568,-0.0346444289841739,
0.0790832878724453));
#68763=CARTESIAN_POINT('Ctrl Pts',(0.00480608832337919,-0.0352450361874068,
0.0788479817354648));
#68764=CARTESIAN_POINT('Ctrl Pts',(0.00498327561204054,-0.0349452760959493,
0.0789731106130311));
#68765=CARTESIAN_POINT('Ctrl Pts',(0.00516938474931044,-0.0346444289841739,
0.0790845375410549));
#68766=CARTESIAN_POINT('Ctrl Pts',(0.00501338624846292,-0.0352450361874068,
0.078987722818386));
#68767=CARTESIAN_POINT('Ctrl Pts',(0.00519584395855024,-0.0349452760959493,
0.0791050333264142));
#68768=CARTESIAN_POINT('Ctrl Pts',(0.00538661963294988,-0.0346444289841739,
0.0792082671063583));
#68769=CARTESIAN_POINT('Ctrl Pts',(0.00501545922771376,-0.0352450361874068,
0.0789891202292151));
#68770=CARTESIAN_POINT('Ctrl Pts',(0.00519796964201533,-0.0349452760959493,
0.0791063525535481));
#68771=CARTESIAN_POINT('Ctrl Pts',(0.00538879198178627,-0.0346444289841739,
0.0792095044020113));
#68772=CARTESIAN_POINT('',(0.00504378325369919,-0.0351951634053304,0.0790071348381277));
#68773=CARTESIAN_POINT('',(0.00524596632825134,-0.0348678972925388,0.0791295884215443));
#68774=CARTESIAN_POINT('Origin',(0.0132614616026492,-0.0345636767886549,
0.0644169237729676));
#68775=CARTESIAN_POINT('Origin',(-0.000283058594760006,-0.0346946199341104,
0.0886966607326437));
#68776=CARTESIAN_POINT('',(0.00513841973333968,-0.0346945769330289,0.0790658657408367));
#68777=CARTESIAN_POINT('',(0.00519253291664268,-0.0346945769458128,0.0790971389638961));
#68778=CARTESIAN_POINT('',(0.00493897409645518,-0.0350221583435553,0.0789390627880089));
#68779=CARTESIAN_POINT('Origin',(0.013696925733086,-0.0345628459369985,
0.0646206747760047));
#68780=CARTESIAN_POINT('',(0.00493965650132374,-0.0351951360298761,0.0789380311793917));
#68781=CARTESIAN_POINT('Origin',(-0.00116208724412833,-0.0351951838366679,
0.0881133549896872));
#68782=CARTESIAN_POINT('',(0.00504381185230669,-0.0351951371328748,0.0790071501625045));
#68783=CARTESIAN_POINT('Ctrl Pts',(0.00504352329155854,-0.0351951371254922,
0.0790057158847739));
#68784=CARTESIAN_POINT('Ctrl Pts',(0.00514391217089723,-0.0350307338980945,
0.0790693983049438));
#68785=CARTESIAN_POINT('Ctrl Pts',(0.00524684733166884,-0.0348659306897824,
0.0791288771281542));
#68786=CARTESIAN_POINT('Ctrl Pts',(0.00504381185236551,-0.0351951371254922,
0.0790071501624043));
#68787=CARTESIAN_POINT('Ctrl Pts',(0.00514423038449431,-0.0350307338980945,
0.0790708266167605));
#68788=CARTESIAN_POINT('Ctrl Pts',(0.00524719492614438,-0.0348659306897824,
0.0791302982536733));
#68789=CARTESIAN_POINT('Ctrl Pts',(0.00509217494435261,-0.0351951371254922,
0.0792475365880562));
#68790=CARTESIAN_POINT('Ctrl Pts',(0.00519756331500823,-0.0350307338980945,
0.0793102131658296));
#68791=CARTESIAN_POINT('Ctrl Pts',(0.00530545212250922,-0.0348659306897824,
0.0793684803717592));
#68792=CARTESIAN_POINT('Origin',(0.0025848997906258,-0.0308609197411455,
0.0837341276772471));
#68793=CARTESIAN_POINT('',(0.00506489707002948,-0.0351951371254922,0.0791119532239969));
#68794=CARTESIAN_POINT('Origin',(0.00812378219310841,-0.0315241814719618,
0.07415));
#68795=CARTESIAN_POINT('',(0.0048012891755772,-0.0347116136489781,0.0791461024937229));
#68796=CARTESIAN_POINT('',(0.00481196851860944,-0.0346945769586885,0.0791531880022078));
#68797=CARTESIAN_POINT('Origin',(0.0138281143311945,-0.0345626675566824,
0.0652147260523571));
#68798=CARTESIAN_POINT('Origin',(0.0141211786267606,-0.0345626631941208,
0.0654073732970256));
#68799=CARTESIAN_POINT('Origin',(0.0141578417119078,-0.0345626691539936,
0.0654340041758359));
#68800=CARTESIAN_POINT('Ctrl Pts',(0.00460801247398302,-0.0350241211494502,
0.0790120328343313));
#68801=CARTESIAN_POINT('Ctrl Pts',(0.00467498498276811,-0.0349144232819069,
0.0790604611206929));
#68802=CARTESIAN_POINT('Ctrl Pts',(0.00474299862511201,-0.0348045283579466,
0.0791075340241056));
#68803=CARTESIAN_POINT('Ctrl Pts',(0.00481196852787608,-0.0346945769439158,
0.0791531880083418));
#68804=CARTESIAN_POINT('Ctrl Pts',(0.00471859927819826,-0.0350241211494502,
0.0789873002538434));
#68805=CARTESIAN_POINT('Ctrl Pts',(0.00478523110582786,-0.0349144232819069,
0.0790342052523193));
#68806=CARTESIAN_POINT('Ctrl Pts',(0.0048528723756531,-0.0348045283579466,
0.0790797609982078));
#68807=CARTESIAN_POINT('Ctrl Pts',(0.00492143861918303,-0.0346945769439158,
0.0791239059163165));
#68808=CARTESIAN_POINT('Ctrl Pts',(0.00482918608241349,-0.0350241211494502,
0.0789625676733555));
#68809=CARTESIAN_POINT('Ctrl Pts',(0.00489547722888761,-0.0349144232819069,
0.0790079493839456));
#68810=CARTESIAN_POINT('Ctrl Pts',(0.00496274612619419,-0.0348045283579466,
0.0790519879723101));
#68811=CARTESIAN_POINT('Ctrl Pts',(0.00503090871048998,-0.0346945769439158,
0.0790946238242913));
#68812=CARTESIAN_POINT('Ctrl Pts',(0.00493977288662872,-0.0350241211494502,
0.0789378350928677));
#68813=CARTESIAN_POINT('Ctrl Pts',(0.00500572335194736,-0.0349144232819069,
0.078981693515572));
#68814=CARTESIAN_POINT('Ctrl Pts',(0.00507261987673527,-0.0348045283579466,
0.0790242149464124));
#68815=CARTESIAN_POINT('Ctrl Pts',(0.00514037880179692,-0.0346945769439158,
0.079065341732266));
#68816=CARTESIAN_POINT('',(0.00497519412568671,-0.0346945769458128,0.0791095268714466));
#68817=CARTESIAN_POINT('Ctrl Pts',(0.00480128917739434,-0.0347116136492789,
0.079146102490978));
#68818=CARTESIAN_POINT('Ctrl Pts',(0.00482506777527153,-0.0347621546532295,
0.0791103461142078));
#68819=CARTESIAN_POINT('Ctrl Pts',(0.00484842828114121,-0.0348133084097021,
0.0790752184311656));
#68820=CARTESIAN_POINT('Ctrl Pts',(0.0048943326048069,-0.0349168561544683,
0.0790061911360808));
#68821=CARTESIAN_POINT('Ctrl Pts',(0.00491685821468387,-0.0349692089016065,
0.0789723189036683));
#68822=CARTESIAN_POINT('Ctrl Pts',(0.00493897409648279,-0.0350221583435177,
0.0789390627879674));
#68823=CARTESIAN_POINT('Origin',(0.0084849663280849,-0.0351840467447566,
0.0732420948397483));
#68824=CARTESIAN_POINT('Origin',(0.00283797433828648,-0.0352322613188162,
0.0848844373324612));
#68825=CARTESIAN_POINT('',(0.00545327161097464,-0.0351951142564667,0.0792437400615015));
#68826=CARTESIAN_POINT('',(0.0055649206081788,-0.0351951372916786,0.0792992453222945));
#68827=CARTESIAN_POINT('Origin',(0.00846304037582862,-0.0352875132321111,
0.0741190968493382));
#68828=CARTESIAN_POINT('Origin',(0.0021682874759184,-0.0298325076522524,
0.0695863092837193));
#68829=CARTESIAN_POINT('Origin',(0.00184281903255471,-0.033873222743243,
0.0796997796762625));
#68830=CARTESIAN_POINT('Ctrl Pts',(0.0029690848306492,-0.0321934096636942,
0.0767009274483544));
#68831=CARTESIAN_POINT('Ctrl Pts',(0.00301474521723456,-0.0320508460843402,
0.0767931940764988));
#68832=CARTESIAN_POINT('Ctrl Pts',(0.00306285019798059,-0.0319086045661229,
0.0768841643308079));
#68833=CARTESIAN_POINT('Ctrl Pts',(0.00311328006876048,-0.0317669892865148,
0.0769736508635441));
#68834=CARTESIAN_POINT('Ctrl Pts',(0.00300789924387488,-0.0321934096636942,
0.0767752502170988));
#68835=CARTESIAN_POINT('Ctrl Pts',(0.0030548899726286,-0.0320508460843402,
0.0768668220857297));
#68836=CARTESIAN_POINT('Ctrl Pts',(0.00310430562564333,-0.0319086045661229,
0.0769570623607072));
#68837=CARTESIAN_POINT('Ctrl Pts',(0.00315602380608249,-0.0317669892865148,
0.0770457854984011));
#68838=CARTESIAN_POINT('Ctrl Pts',(0.00304671365710054,-0.0321934096636942,
0.0768495729858433));
#68839=CARTESIAN_POINT('Ctrl Pts',(0.00309503472802263,-0.0320508460843402,
0.0769404500949606));
#68840=CARTESIAN_POINT('Ctrl Pts',(0.00314576105330607,-0.0319086045661229,
0.0770299603906066));
#68841=CARTESIAN_POINT('Ctrl Pts',(0.00319876754340448,-0.0317669892865148,
0.077117920133258));
#68842=CARTESIAN_POINT('Ctrl Pts',(0.00308552807032622,-0.0321934096636942,
0.0769238957545877));
#68843=CARTESIAN_POINT('Ctrl Pts',(0.00313517948341667,-0.0320508460843402,
0.0770140781041916));
#68844=CARTESIAN_POINT('Ctrl Pts',(0.00318721648096881,-0.0319086045661229,
0.0771028584205059));
#68845=CARTESIAN_POINT('Ctrl Pts',(0.00324151128072648,-0.0317669892865148,
0.0771900547681149));
#68846=CARTESIAN_POINT('',(0.00308483367280552,-0.0321934096636942,0.0769225661055668));
#68847=CARTESIAN_POINT('',(0.0032029979100201,-0.0318665617511297,0.0771272482309031));
#68848=CARTESIAN_POINT('Origin',(0.0180113624498778,-0.0326371944420234,
0.069411464754423));
#68849=CARTESIAN_POINT('Origin',(-0.00617524371148055,-0.0316939261508981,
0.0828014155067585));
#68850=CARTESIAN_POINT('',(0.00302592857898553,-0.032019722162177,0.0768126073115477));
#68851=CARTESIAN_POINT('Ctrl Pts',(0.0030259695587903,-0.032019739209469,
0.0768127876876422));
#68852=CARTESIAN_POINT('Ctrl Pts',(0.00303951872021519,-0.0319792716575989,
0.0768387269754978));
#68853=CARTESIAN_POINT('Ctrl Pts',(0.00305332731327124,-0.0319386439829633,
0.0768646810555132));
#68854=CARTESIAN_POINT('Ctrl Pts',(0.0030674173008937,-0.0318979099381565,
0.0768906732020765));
#68855=CARTESIAN_POINT('Ctrl Pts',(0.00308150701001716,-0.0318571766984882,
0.0769166648348857));
#68856=CARTESIAN_POINT('Ctrl Pts',(0.00309580492313141,-0.0318163871833546,
0.0769425632753775));
#68857=CARTESIAN_POINT('Ctrl Pts',(0.00311025877872009,-0.0317755399638303,
0.0769682811454069));
#68858=CARTESIAN_POINT('',(0.00302696919836558,-0.0321934096636183,0.0768117658230244));
#68859=CARTESIAN_POINT('Origin',(0.000990947553938459,-0.0324112197412341,
0.0778987847009924));
#68860=CARTESIAN_POINT('',(0.00305590143559555,-0.0321934096636663,0.0768671659643057));
#68861=CARTESIAN_POINT('Ctrl Pts',(0.00308544102434413,-0.0321934096636618,
0.0769206309540255));
#68862=CARTESIAN_POINT('Ctrl Pts',(0.00312365018450362,-0.0320835708272592,
0.0769901136053962));
#68863=CARTESIAN_POINT('Ctrl Pts',(0.00316327512165632,-0.0319739230346489,
0.0770587652174217));
#68864=CARTESIAN_POINT('Ctrl Pts',(0.00320425839735533,-0.0318646057455573,
0.0771265018460079));
#68865=CARTESIAN_POINT('Ctrl Pts',(0.00305150767364851,-0.0321934096636618,
0.0770287498352429));
#68866=CARTESIAN_POINT('Ctrl Pts',(0.00309120787744292,-0.0320835708272592,
0.0770987004539658));
#68867=CARTESIAN_POINT('Ctrl Pts',(0.00313233267792466,-0.0319739230346489,
0.0771677889048329));
#68868=CARTESIAN_POINT('Ctrl Pts',(0.00317482267478138,-0.0318646057455573,
0.0772359308321207));
#68869=CARTESIAN_POINT('Ctrl Pts',(0.0030175743229529,-0.0321934096636618,
0.0771368687164603));
#68870=CARTESIAN_POINT('Ctrl Pts',(0.00305876557038222,-0.0320835708272592,
0.0772072873025354));
#68871=CARTESIAN_POINT('Ctrl Pts',(0.00310139023419301,-0.0319739230346489,
0.0772768125922441));
#68872=CARTESIAN_POINT('Ctrl Pts',(0.00314538695220742,-0.0318646057455573,
0.0773453598182336));
#68873=CARTESIAN_POINT('Ctrl Pts',(0.00298364097225728,-0.0321934096636618,
0.0772449875976778));
#68874=CARTESIAN_POINT('Ctrl Pts',(0.00302632326332152,-0.0320835708272592,
0.0773158741511051));
#68875=CARTESIAN_POINT('Ctrl Pts',(0.00307044779046135,-0.0319739230346489,
0.0773858362796553));
#68876=CARTESIAN_POINT('Ctrl Pts',(0.00311595122963347,-0.0318646057455573,
0.0774547888043465));
#68877=CARTESIAN_POINT('',(0.00299026364896617,-0.0321763980308285,0.0772559599699106));
#68878=CARTESIAN_POINT('',(0.00298364097227652,-0.0321934096636184,0.0772449875976981));
#68879=CARTESIAN_POINT('Origin',(0.0174560957059853,-0.0326386229898935,
0.0692206757338883));
#68880=CARTESIAN_POINT('Ctrl Pts',(0.00299026365167526,-0.0321763980306317,
0.0772559599682634));
#68881=CARTESIAN_POINT('Ctrl Pts',(0.00302698447414228,-0.0321259596175778,
0.0772337425741577));
#68882=CARTESIAN_POINT('Ctrl Pts',(0.00306306906071051,-0.0320749164633317,
0.0772119101252265));
#68883=CARTESIAN_POINT('Ctrl Pts',(0.00313399480201706,-0.0319716057793942,
0.0771689975475394));
#68884=CARTESIAN_POINT('Ctrl Pts',(0.00316880832151041,-0.0319193786690141,
0.0771479341390824));
#68885=CARTESIAN_POINT('Ctrl Pts',(0.00320299791160168,-0.0318665617525326,
0.0771272482299349));
#68886=CARTESIAN_POINT('',(0.00303423732255102,-0.0321934096636663,0.0770837768516425));
#68887=CARTESIAN_POINT('Origin',(0.00812378219310841,-0.0315241814719618,
0.07415));
#68888=CARTESIAN_POINT('',(0.00299026364864828,-0.0322104233323768,0.0772559599701025));
#68889=CARTESIAN_POINT('',(0.00299690974454782,-0.0321934096636183,0.0772669181728473));
#68890=CARTESIAN_POINT('Origin',(0.0174382634095364,-0.0326387226163109,
0.0691789946233088));
#68891=CARTESIAN_POINT('Origin',(0.0168209260078138,-0.0326386248122561,
0.0681708631843273));
#68892=CARTESIAN_POINT('Origin',(0.0168495664139399,-0.0326387239598755,
0.0682060057493927));
#68893=CARTESIAN_POINT('Ctrl Pts',(0.00312151735985888,-0.0327445246967096,
0.0769882162599131));
#68894=CARTESIAN_POINT('Ctrl Pts',(0.00322856243605139,-0.032443687833936,
0.0771768797623295));
#68895=CARTESIAN_POINT('Ctrl Pts',(0.00334951431456717,-0.0321434074405928,
0.0773569442190236));
#68896=CARTESIAN_POINT('Ctrl Pts',(0.00324958558167206,-0.0327445246967096,
0.0772029219434933));
#68897=CARTESIAN_POINT('Ctrl Pts',(0.00336472841510119,-0.032443687833936,
0.0773867552739614));
#68898=CARTESIAN_POINT('Ctrl Pts',(0.00349339121768822,-0.0321434074405928,
0.0775613933245446));
#68899=CARTESIAN_POINT('',(0.00326886775284126,-0.0326943950436612,0.0772334932751161));
#68900=CARTESIAN_POINT('',(0.00339965091615906,-0.0323666188837389,0.0774303519137662));
#68901=CARTESIAN_POINT('Origin',(0.0174186577702613,-0.0326395579108609,
0.0681565168690591));
#68902=CARTESIAN_POINT('Origin',(-0.00567232325795304,-0.032193382560304,
0.0837297690636582));
#68903=CARTESIAN_POINT('',(0.00332947165196833,-0.0321934096532689,0.0773269028049071));
#68904=CARTESIAN_POINT('',(0.00336511922998225,-0.0321934096584275,0.0773782399311192));
#68905=CARTESIAN_POINT('',(0.00320299790920229,-0.0325210109756239,0.0771272482313813));
#68906=CARTESIAN_POINT('Origin',(0.0176546596804715,-0.0326393129161776,
0.0685754291857115));
#68907=CARTESIAN_POINT('',(0.0032041602534476,-0.0326943950436593,0.077126544972079));
#68908=CARTESIAN_POINT('Origin',(-0.00626072666954365,-0.0326943765538048,
0.0828531348999376));
#68909=CARTESIAN_POINT('',(0.00323651400315443,-0.0326943950436702,0.0771800191236075));
#68910=CARTESIAN_POINT('Ctrl Pts',(0.00287246520896839,-0.0325229783203769,
0.0770523559278832));
#68911=CARTESIAN_POINT('Ctrl Pts',(0.00291247412196393,-0.032413025309245,
0.0771247452176709));
#68912=CARTESIAN_POINT('Ctrl Pts',(0.00295397443227379,-0.032303122220807,
0.077196295892444));
#68913=CARTESIAN_POINT('Ctrl Pts',(0.0029969097468773,-0.0321934096576658,
0.077266918176679));
#68914=CARTESIAN_POINT('Ctrl Pts',(0.00298305775896316,-0.0325229783203769,
0.0770770628119856));
#68915=CARTESIAN_POINT('Ctrl Pts',(0.00302340725581576,-0.032413025309245,
0.0771479275858901));
#68916=CARTESIAN_POINT('Ctrl Pts',(0.00306521656175702,-0.032303122220807,
0.0772179469305881));
#68917=CARTESIAN_POINT('Ctrl Pts',(0.00310842895718062,-0.0321934096576658,
0.0772870330460477));
#68918=CARTESIAN_POINT('Ctrl Pts',(0.00309365030895794,-0.0325229783203769,
0.0771017696960881));
#68919=CARTESIAN_POINT('Ctrl Pts',(0.00313434038966758,-0.032413025309245,
0.0771711099541094));
#68920=CARTESIAN_POINT('Ctrl Pts',(0.00317645869124026,-0.032303122220807,
0.0772395979687324));
#68921=CARTESIAN_POINT('Ctrl Pts',(0.00321994816748395,-0.0321934096576658,
0.0773071479154165));
#68922=CARTESIAN_POINT('Ctrl Pts',(0.00320424285895271,-0.0325229783203769,
0.0771264765801905));
#68923=CARTESIAN_POINT('Ctrl Pts',(0.0032452735235194,-0.032413025309245,
0.0771942923223286));
#68924=CARTESIAN_POINT('Ctrl Pts',(0.00328770082072349,-0.032303122220807,
0.0772612490068766));
#68925=CARTESIAN_POINT('Ctrl Pts',(0.00333146737778727,-0.0321934096576658,
0.0773272627847852));
#68926=CARTESIAN_POINT('',(0.00316319069787418,-0.0321934096584275,0.0772969104885515));
#68927=CARTESIAN_POINT('Ctrl Pts',(0.00299026365162035,-0.0322104233328919,
0.0772559599682966));
#68928=CARTESIAN_POINT('Ctrl Pts',(0.00302703423146573,-0.0322609421831417,
0.0772337124692202));
#68929=CARTESIAN_POINT('Ctrl Pts',(0.00306314312537439,-0.0323120888240841,
0.0772118653134978));
#68930=CARTESIAN_POINT('Ctrl Pts',(0.00313406940354204,-0.0324156524631809,
0.0771689524109907));
#68931=CARTESIAN_POINT('Ctrl Pts',(0.00316885763339512,-0.0324680267167311,
0.077147904303651));
#68932=CARTESIAN_POINT('Ctrl Pts',(0.00320299790924169,-0.0325210109755913,
0.0771272482313627));
#68933=CARTESIAN_POINT('Origin',(0.00489127226361921,-0.0262834582511723,
0.0669768371414704));
#68934=CARTESIAN_POINT('Origin',(-0.00399534140117125,-0.0342770905168603,
0.0751251954865947));
#68935=CARTESIAN_POINT('Ctrl Pts',(0.00326935227917528,-0.0326943950436604,
0.0772315242842415));
#68936=CARTESIAN_POINT('Ctrl Pts',(0.00331182145920417,-0.0325844576448134,
0.0772984274266268));
#68937=CARTESIAN_POINT('Ctrl Pts',(0.00335567731151665,-0.0324744968375322,
0.0773644569715792));
#68938=CARTESIAN_POINT('Ctrl Pts',(0.00340086247853638,-0.0323646534831894,
0.0774295290932336));
#68939=CARTESIAN_POINT('Ctrl Pts',(0.00324227476812217,-0.0326943950436604,
0.0773415603509526));
#68940=CARTESIAN_POINT('Ctrl Pts',(0.00328626045137991,-0.0325844576448134,
0.0774088366721889));
#68941=CARTESIAN_POINT('Ctrl Pts',(0.003331640632197,-0.0324744968375322,
0.0774752080586296));
#68942=CARTESIAN_POINT('Ctrl Pts',(0.00337835599389737,-0.0323646534831894,
0.0775405902733609));
#68943=CARTESIAN_POINT('Ctrl Pts',(0.00321519725706906,-0.0326943950436604,
0.0774515964176637));
#68944=CARTESIAN_POINT('Ctrl Pts',(0.00326069944355565,-0.0325844576448134,
0.077519245917751));
#68945=CARTESIAN_POINT('Ctrl Pts',(0.00330760395287735,-0.0324744968375322,
0.0775859591456801));
#68946=CARTESIAN_POINT('Ctrl Pts',(0.00335584950925836,-0.0323646534831894,
0.0776516514534883));
#68947=CARTESIAN_POINT('Ctrl Pts',(0.00318811974601596,-0.0326943950436604,
0.0775616324843749));
#68948=CARTESIAN_POINT('Ctrl Pts',(0.00323513843573139,-0.0325844576448134,
0.0776296551633131));
#68949=CARTESIAN_POINT('Ctrl Pts',(0.0032835672735577,-0.0324744968375322,
0.0776967102327305));
#68950=CARTESIAN_POINT('Ctrl Pts',(0.00333334302461935,-0.0323646534831894,
0.0777627126336156));
#68951=CARTESIAN_POINT('',(0.00319541831515216,-0.0326773559991361,0.077572167363916));
#68952=CARTESIAN_POINT('',(0.0031881197460185,-0.0326943950436594,0.0775616324843668));
#68953=CARTESIAN_POINT('Origin',(0.0168061277761233,-0.0326395670836268,
0.0680599699871882));
#68954=CARTESIAN_POINT('Ctrl Pts',(0.00319541831789935,-0.0326773559987466,
0.0775721673619998));
#68955=CARTESIAN_POINT('Ctrl Pts',(0.00323070000797244,-0.0326267922586965,
0.0775476683900689));
#68956=CARTESIAN_POINT('Ctrl Pts',(0.00326535635556921,-0.0325756109581347,
0.0775236036447224));
#68957=CARTESIAN_POINT('Ctrl Pts',(0.00333344786032804,-0.0324719985462373,
0.0774763221267347));
#68958=CARTESIAN_POINT('Ctrl Pts',(0.00336685570765316,-0.032419609162177,
0.0774531243175539));
#68959=CARTESIAN_POINT('Ctrl Pts',(0.00339965091619911,-0.0323666188837756,
0.0774303519137384));
#68960=CARTESIAN_POINT('',(0.00322849374943987,-0.0326943950436702,0.0773975628797515));
#68961=CARTESIAN_POINT('Origin',(0.00812378219310841,-0.0315241814719618,
0.07415));
#68962=CARTESIAN_POINT('',(0.0031954183151884,-0.0327114338379857,0.0775721673638903));
#68963=CARTESIAN_POINT('',(0.00320273936760646,-0.0326943950436593,0.0775826866314311));
#68964=CARTESIAN_POINT('Origin',(0.0167796527206399,-0.0326395659357401,
0.0680231969149709));
#68965=CARTESIAN_POINT('Origin',(0.0168634398053643,-0.0326395684527436,
0.0681425016757454));
#68966=CARTESIAN_POINT('Origin',(0.0168886406309284,-0.0326395674034263,
0.068180159390258));
#68967=CARTESIAN_POINT('Ctrl Pts',(0.00330962272071791,-0.0332451089994433,
0.0772967433283306));
#68968=CARTESIAN_POINT('Ctrl Pts',(0.00342830408707474,-0.0329451141710254,
0.0774783123234561));
#68969=CARTESIAN_POINT('Ctrl Pts',(0.00356032481116817,-0.0326442513127494,
0.0776504259345422));
#68970=CARTESIAN_POINT('Ctrl Pts',(0.00345092111710486,-0.0332451089994433,
0.0775029829054696));
#68971=CARTESIAN_POINT('Ctrl Pts',(0.00357738093637565,-0.0329451141710254,
0.0776792227443859));
#68972=CARTESIAN_POINT('Ctrl Pts',(0.0037167566017878,-0.0326442513127494,
0.0778454364339609));
#68973=CARTESIAN_POINT('Ctrl Pts',(0.00345233410106873,-0.0332451089994433,
0.0775050453012409));
#68974=CARTESIAN_POINT('Ctrl Pts',(0.00357887170486866,-0.0329451141710254,
0.0776812318485952));
#68975=CARTESIAN_POINT('Ctrl Pts',(0.00371832091969399,-0.0326442513127494,
0.077847386538955));
#68976=CARTESIAN_POINT('',(0.00347206196219953,-0.0331951640388616,0.0775322513054701));
#68977=CARTESIAN_POINT('',(0.00361494791491237,-0.0328677532355012,0.0777205095604965));
#68978=CARTESIAN_POINT('Origin',(0.0165649917248435,-0.0326402808281325,
0.0670628942239344));
#68979=CARTESIAN_POINT('Origin',(-0.00505225171976446,-0.0326944278779135,
0.0845844758664123));
#68980=CARTESIAN_POINT('',(0.003538411509985,-0.0326943950436593,0.0776216711679468));
#68981=CARTESIAN_POINT('',(0.00357721222903344,-0.0326943950436694,0.0776706686597508));
#68982=CARTESIAN_POINT('',(0.00339965091615746,-0.0330220786163545,0.0774303519137639));
#68983=CARTESIAN_POINT('Origin',(0.0168874600041524,-0.0326396682766063,
0.0674194988430164));
#68984=CARTESIAN_POINT('',(0.003400766808764,-0.0331951640388587,0.0774295770579827));
#68985=CARTESIAN_POINT('Origin',(-0.00566056714797226,-0.0331952026560148,
0.0837216034790517));
#68986=CARTESIAN_POINT('',(0.00343641438549177,-0.0331951640388701,0.0774809141817364));
#68987=CARTESIAN_POINT('Ctrl Pts',(0.00306506843675485,-0.0330240426238172,
0.0773763625232311));
#68988=CARTESIAN_POINT('Ctrl Pts',(0.00310951472380506,-0.032914277406352,
0.0774460512336908));
#68989=CARTESIAN_POINT('Ctrl Pts',(0.00315542382926138,-0.0328043479726691,
0.0775148558576064));
#68990=CARTESIAN_POINT('Ctrl Pts',(0.00320273936760645,-0.0326943950436593,
0.0775826866314311));
#68991=CARTESIAN_POINT('Ctrl Pts',(0.00317699409129416,-0.0330240426238172,
0.0773940764680345));
#68992=CARTESIAN_POINT('Ctrl Pts',(0.0032216844051919,-0.032914277406352,
0.0774622232935591));
#68993=CARTESIAN_POINT('Ctrl Pts',(0.00326780578408337,-0.0328043479726691,
0.077529480219137));
#68994=CARTESIAN_POINT('Ctrl Pts',(0.00331530151590948,-0.0326943950436593,
0.0775957594564494));
#68995=CARTESIAN_POINT('Ctrl Pts',(0.00328891974583347,-0.0330240426238172,
0.0774117904128379));
#68996=CARTESIAN_POINT('Ctrl Pts',(0.00333385408657873,-0.032914277406352,
0.0774783953534273));
#68997=CARTESIAN_POINT('Ctrl Pts',(0.00338018773890536,-0.0328043479726691,
0.0775441045806676));
#68998=CARTESIAN_POINT('Ctrl Pts',(0.00342786366421251,-0.0326943950436593,
0.0776088322814676));
#68999=CARTESIAN_POINT('Ctrl Pts',(0.00340084540037278,-0.0330240426238172,
0.0774295043576413));
#69000=CARTESIAN_POINT('Ctrl Pts',(0.00344602376796557,-0.032914277406352,
0.0774945674132956));
#69001=CARTESIAN_POINT('Ctrl Pts',(0.00349256969372735,-0.0328043479726691,
0.0775587289421982));
#69002=CARTESIAN_POINT('Ctrl Pts',(0.00354042581251554,-0.0326943950436593,
0.0776219051064858));
#69003=CARTESIAN_POINT('',(0.00337057543880573,-0.0326943950436693,0.077602178899699));
#69004=CARTESIAN_POINT('Ctrl Pts',(0.00319541831790758,-0.0327114338383316,
0.077572167361994));
#69005=CARTESIAN_POINT('Ctrl Pts',(0.00323069413955649,-0.0327619876831115,
0.0775476724649914));
#69006=CARTESIAN_POINT('Ctrl Pts',(0.00326534762077641,-0.0328131562604638,
0.0775236097100055));
#69007=CARTESIAN_POINT('Ctrl Pts',(0.00333343906285031,-0.0329167375858765,
0.0774763282355452));
#69008=CARTESIAN_POINT('Ctrl Pts',(0.00336684989259642,-0.0329691088920617,
0.0774531283554249));
#69009=CARTESIAN_POINT('Ctrl Pts',(0.00339965091619805,-0.0330220786163187,
0.0774303519137392));
#69010=CARTESIAN_POINT('Ctrl Pts',(0.00347242195593373,-0.0331951640388604,
0.077530255457707));
#69011=CARTESIAN_POINT('Ctrl Pts',(0.00354230657030366,-0.0330306422010619,
0.0776264193484358));
#69012=CARTESIAN_POINT('Ctrl Pts',(0.0036161060234924,-0.0328657861914644,
0.0777196126631896));
#69013=CARTESIAN_POINT('Ctrl Pts',(0.00347206196219772,-0.0331951640388604,
0.0775322513054674));
#69014=CARTESIAN_POINT('Ctrl Pts',(0.00354198783944048,-0.0330306422010619,
0.077628422638836));
#69015=CARTESIAN_POINT('Ctrl Pts',(0.00361582882785534,-0.0328657861914644,
0.0777216216844319));
#69016=CARTESIAN_POINT('Ctrl Pts',(0.00341207732454699,-0.0331951640388604,
0.0778648132162551));
#69017=CARTESIAN_POINT('Ctrl Pts',(0.00348887870607642,-0.0330306422010619,
0.0779622246935485));
#69018=CARTESIAN_POINT('Ctrl Pts',(0.0035696405801603,-0.0328657861914644,
0.0780563786515523));
#69019=CARTESIAN_POINT('',(0.00342002298075961,-0.0331781648281916,0.0778748690269726));
#69020=CARTESIAN_POINT('',(0.00341207732454947,-0.0331951640388588,0.0778648132162463));
#69021=CARTESIAN_POINT('Origin',(0.0159186204347069,-0.0326412091816574,
0.0670687808657489));
#69022=CARTESIAN_POINT('Ctrl Pts',(0.00342002298065486,-0.033178164828644,
0.0778748690251295));
#69023=CARTESIAN_POINT('Ctrl Pts',(0.00345371992274879,-0.0331276811546788,
0.077848184672704));
#69024=CARTESIAN_POINT('Ctrl Pts',(0.00348680838142885,-0.0330765663497807,
0.0778219821305349));
#69025=CARTESIAN_POINT('Ctrl Pts',(0.00355179686141659,-0.0329730614463279,
0.0777705182812483));
#69026=CARTESIAN_POINT('Ctrl Pts',(0.0035836706321198,-0.0329207133374049,
0.0777452777686087));
#69027=CARTESIAN_POINT('Ctrl Pts',(0.0036149478994017,-0.0328677532289369,
0.0777205095549454));
#69028=CARTESIAN_POINT('',(0.0034420696433845,-0.0331951640388701,0.0776985322608681));
#69029=CARTESIAN_POINT('Origin',(0.00812378219310841,-0.0315241814719618,
0.07415));
#69030=CARTESIAN_POINT('',(0.00342002298237634,-0.0332121607144211,0.0778748690265169));
#69031=CARTESIAN_POINT('',(0.00342799009848604,-0.0331951640388587,0.077884907844126));
#69032=CARTESIAN_POINT('Origin',(0.0158847466979892,-0.0326413640993599,
0.0670386330042486));
#69033=CARTESIAN_POINT('Origin',(0.016802988518155,-0.0326412103775044,
0.0681855539297036));
#69034=CARTESIAN_POINT('Origin',(0.0168245650622733,-0.0326413655647481,
0.0682254393833421));
#69035=CARTESIAN_POINT('Ctrl Pts',(0.00351669554321774,-0.0337436976235975,
0.0775928008365862));
#69036=CARTESIAN_POINT('Ctrl Pts',(0.00354766061571275,-0.0336723290703325,
0.0776342376721385));
#69037=CARTESIAN_POINT('Ctrl Pts',(0.00357936599685407,-0.033601104548885,
0.0776751108401327));
#69038=CARTESIAN_POINT('Ctrl Pts',(0.00368059499835616,-0.0333736987606857,
0.0778056107690198));
#69039=CARTESIAN_POINT('Ctrl Pts',(0.00378914602084772,-0.0331450831799191,
0.0779300865405608));
#69040=CARTESIAN_POINT('Ctrl Pts',(0.00367066429629554,-0.0337436976235975,
0.0777897618049929));
#69041=CARTESIAN_POINT('Ctrl Pts',(0.00370340086559064,-0.0336723290703325,
0.0778298138222454));
#69042=CARTESIAN_POINT('Ctrl Pts',(0.00373685254842926,-0.033601104548885,
0.0778692705323269));
#69043=CARTESIAN_POINT('Ctrl Pts',(0.00384365714532796,-0.0333736987606857,
0.0779952479916836));
#69044=CARTESIAN_POINT('Ctrl Pts',(0.00395751504969802,-0.0331450831799191,
0.0781148887865536));
#69045=CARTESIAN_POINT('Ctrl Pts',(0.00367220398382631,-0.0337436976235975,
0.077791731414677));
#69046=CARTESIAN_POINT('Ctrl Pts',(0.00370495826808942,-0.0336723290703325,
0.0778317695837464));
#69047=CARTESIAN_POINT('Ctrl Pts',(0.00373842741394501,-0.033601104548885,
0.0778712121292489));
#69048=CARTESIAN_POINT('Ctrl Pts',(0.00384528776679768,-0.0333736987606857,
0.0779971443639103));
#69049=CARTESIAN_POINT('Ctrl Pts',(0.00395919873998652,-0.0331450831799191,
0.0781167368090136));
#69050=CARTESIAN_POINT('',(0.00369361438614891,-0.0336938721132548,0.0778176611351351));
#69051=CARTESIAN_POINT('',(0.00384803921977251,-0.0333679869945434,0.0779965760132826));
#69052=CARTESIAN_POINT('Ctrl Pts',(0.00369361438615697,-0.0336938721132648,
0.0778176611351466));
#69053=CARTESIAN_POINT('Ctrl Pts',(0.0037079309880983,-0.0336629187933931,
0.0778349541583256));
#69054=CARTESIAN_POINT('Ctrl Pts',(0.00372234426885285,-0.0336319952301039,
0.0778521578213233));
#69055=CARTESIAN_POINT('Ctrl Pts',(0.00373685254843802,-0.0336011045488949,
0.0778692705323379));
#69056=CARTESIAN_POINT('Ctrl Pts',(0.0037732587863711,-0.0335235892595452,
0.077912212179914));
#69057=CARTESIAN_POINT('Ctrl Pts',(0.00381032801695305,-0.0334458668660367,
0.077954657327859));
#69058=CARTESIAN_POINT('Ctrl Pts',(0.00384803921953166,-0.0333679869945384,
0.0779965760134899));
#69059=CARTESIAN_POINT('Ctrl Pts',(0.00384806845073468,-0.0333679692460368,
0.077996609533711));
#69060=CARTESIAN_POINT('Ctrl Pts',(0.00384840141990203,-0.0333391895371364,
0.0779963020123921));
#69061=CARTESIAN_POINT('Ctrl Pts',(0.0038486487933833,-0.0333104081053817,
0.0779960691246925));
#69062=CARTESIAN_POINT('Ctrl Pts',(0.00384897243894554,-0.0332532696655993,
0.0779957568246079));
#69063=CARTESIAN_POINT('Ctrl Pts',(0.00384905120287359,-0.0332249163443174,
0.0779956751698193));
#69064=CARTESIAN_POINT('Ctrl Pts',(0.00384904932046599,-0.0331960985684305,
0.0779956675896123));
#69065=CARTESIAN_POINT('Ctrl Pts',(0.00384904926756352,-0.0331956312238387,
0.07799566748631));
#69066=CARTESIAN_POINT('Ctrl Pts',(0.0038490491931661,-0.03319516403886,
0.077995667403612));
#69067=CARTESIAN_POINT('',(0.00376544772787017,-0.0331951640388587,0.0779027384253525));
#69068=CARTESIAN_POINT('',(0.00380724846052808,-0.0331951640388687,0.0779492029144923));
#69069=CARTESIAN_POINT('',(0.00361494791122898,-0.0335216366567698,0.0777205095454249));
#69070=CARTESIAN_POINT('Origin',(0.0158850278782498,-0.032643457152887,
0.0664592572789629));
#69071=CARTESIAN_POINT('',(0.00361601294806183,-0.0336938721132325,0.0777196661515348));
#69072=CARTESIAN_POINT('Origin',(-0.00494527546920406,-0.0336938867896149,
0.0844992804885138));
#69073=CARTESIAN_POINT('',(0.00365481366711538,-0.0336938721132536,0.0777686636433449));
#69074=CARTESIAN_POINT('Ctrl Pts',(0.00327763619847352,-0.0335235895815172,
0.0776876360749402));
#69075=CARTESIAN_POINT('Ctrl Pts',(0.00332633872400957,-0.0334144449262749,
0.0777543528157398));
#69076=CARTESIAN_POINT('Ctrl Pts',(0.00337647552050197,-0.0333049234473147,
0.0778201400484667));
#69077=CARTESIAN_POINT('Ctrl Pts',(0.00342799009848586,-0.0331951640388587,
0.0778849078441259));
#69078=CARTESIAN_POINT('Ctrl Pts',(0.00339045342314712,-0.0335235895815172,
0.0776982871923899));
#69079=CARTESIAN_POINT('Ctrl Pts',(0.00343930258228498,-0.0334144449262749,
0.0777634507819752));
#69080=CARTESIAN_POINT('Ctrl Pts',(0.00348955409390823,-0.0333049234473147,
0.0778276800497654));
#69081=CARTESIAN_POINT('Ctrl Pts',(0.00354115114140821,-0.0331951640388587,
0.0778908870456369));
#69082=CARTESIAN_POINT('Ctrl Pts',(0.00350327064782071,-0.0335235895815172,
0.0777089383098397));
#69083=CARTESIAN_POINT('Ctrl Pts',(0.00355226644056039,-0.0334144449262749,
0.0777725487482107));
#69084=CARTESIAN_POINT('Ctrl Pts',(0.00360263266731449,-0.0333049234473147,
0.0778352200510641));
#69085=CARTESIAN_POINT('Ctrl Pts',(0.00365431218433055,-0.0331951640388587,
0.0778968662471479));
#69086=CARTESIAN_POINT('Ctrl Pts',(0.00361608787249431,-0.0335235895815172,
0.0777195894272895));
#69087=CARTESIAN_POINT('Ctrl Pts',(0.0036652302988358,-0.0334144449262749,
0.0777816467144461));
#69088=CARTESIAN_POINT('Ctrl Pts',(0.00371571124072075,-0.0333049234473147,
0.0778427600523629));
#69089=CARTESIAN_POINT('Ctrl Pts',(0.00376747322725289,-0.0331951640388587,
0.0779028454486589));
#69090=CARTESIAN_POINT('',(0.0035967189131881,-0.0331951640388687,0.0778938231347492));
#69091=CARTESIAN_POINT('Ctrl Pts',(0.00342002298482788,-0.033212160714597,
0.0778748690245668));
#69092=CARTESIAN_POINT('Ctrl Pts',(0.00345366324756589,-0.0332625444109904,
0.0778482295715033));
#69093=CARTESIAN_POINT('Ctrl Pts',(0.00348672383578633,-0.0333135300747143,
0.0778220491580205));
#69094=CARTESIAN_POINT('Ctrl Pts',(0.00355171190622051,-0.033416720314059,
0.0777705856285736));
#69095=CARTESIAN_POINT('Ctrl Pts',(0.00358361421804985,-0.0334688847587291,
0.0777453224448341));
#69096=CARTESIAN_POINT('Ctrl Pts',(0.003614947911878,-0.0335216366562357,
0.0777205095451091));
#69097=CARTESIAN_POINT('Ctrl Pts',(0.00369372973300097,-0.033693872113239,
0.0778166679533916));
#69098=CARTESIAN_POINT('Ctrl Pts',(0.00371519195726162,-0.0336474569764958,
0.0778425985204879));
#69099=CARTESIAN_POINT('Ctrl Pts',(0.00373695626094463,-0.033601104548885,
0.077868276068372));
#69100=CARTESIAN_POINT('Ctrl Pts',(0.00379205847394283,-0.0334837508592656,
0.0779332857159763));
#69101=CARTESIAN_POINT('Ctrl Pts',(0.00384906286075581,-0.0333660264659097,
0.0779966340233174));
#69102=CARTESIAN_POINT('Ctrl Pts',(0.00369361438613585,-0.033693872113239,
0.0778176611351193));
#69103=CARTESIAN_POINT('Ctrl Pts',(0.00371508242381872,-0.0336474569764958,
0.0778435923773791));
#69104=CARTESIAN_POINT('Ctrl Pts',(0.00373685254842926,-0.033601104548885,
0.077869270532327));
#69105=CARTESIAN_POINT('Ctrl Pts',(0.00379196949867764,-0.0334837508592656,
0.0779342817168771));
#69106=CARTESIAN_POINT('Ctrl Pts',(0.00384898866181219,-0.0333660264659097,
0.077997631123794));
#69107=CARTESIAN_POINT('Ctrl Pts',(0.00365439594239875,-0.033693872113239,
0.0781553473103698));
#69108=CARTESIAN_POINT('Ctrl Pts',(0.00367784056932152,-0.0336474569764958,
0.0781815081111948));
#69109=CARTESIAN_POINT('Ctrl Pts',(0.00370158983500764,-0.033601104548885,
0.0782073926705059));
#69110=CARTESIAN_POINT('Ctrl Pts',(0.00376171751542633,-0.0334837508592656,
0.0782729264234479));
#69111=CARTESIAN_POINT('Ctrl Pts',(0.0038237606931727,-0.0333660264659097,
0.0783366496909593));
#69112=CARTESIAN_POINT('',(0.00366319123664695,-0.0336769361243753,0.078162870334204));
#69113=CARTESIAN_POINT('',(0.00365462984962344,-0.0336938721132327,0.078153333277498));
#69114=CARTESIAN_POINT('Ctrl Pts',(0.00366319123664715,-0.033676936124375,
0.0781628703342042));
#69115=CARTESIAN_POINT('Ctrl Pts',(0.00366176253420729,-0.0336797586670149,
0.0781612822297672));
#69116=CARTESIAN_POINT('Ctrl Pts',(0.00366033473392105,-0.0336825812713094,
0.0781596934224022));
#69117=CARTESIAN_POINT('Ctrl Pts',(0.00365748094242724,-0.0336882265929357,
0.0781565144079007));
#69118=CARTESIAN_POINT('Ctrl Pts',(0.00365605495119278,-0.0336910493102957,
0.0781549242007668));
#69119=CARTESIAN_POINT('Ctrl Pts',(0.00365462984962063,-0.033693872113236,
0.0781533332775063));
#69120=CARTESIAN_POINT('Ctrl Pts',(0.00366319123664697,-0.0336769361243754,
0.0781628703342039));
#69121=CARTESIAN_POINT('Ctrl Pts',(0.00369435055763764,-0.0336279018505218,
0.0781348385518554));
#69122=CARTESIAN_POINT('Ctrl Pts',(0.00372595814487436,-0.0335767826010767,
0.0781064034968595));
#69123=CARTESIAN_POINT('Ctrl Pts',(0.00378789085622976,-0.0334733172064618,
0.0780506871259704));
#69124=CARTESIAN_POINT('Ctrl Pts',(0.00381825760411366,-0.033420963145624,
0.0780233683641929));
#69125=CARTESIAN_POINT('Ctrl Pts',(0.00384803921488857,-0.0333679869844681,
0.077996576007855));
#69126=CARTESIAN_POINT('',(0.00367412211789618,-0.0336938721132538,0.0779854972063266));
#69127=CARTESIAN_POINT('Origin',(0.00812378219310841,-0.0315241814719618,
0.07415));
#69128=CARTESIAN_POINT('',(0.00366319123761458,-0.0337108120655385,0.0781628703333429));
#69129=CARTESIAN_POINT('',(0.00367177297545981,-0.0336938721132327,0.0781723890818771));
#69130=CARTESIAN_POINT('Origin',(0.0165741070031077,-0.0345562509814765,
0.068051159813424));
#69131=CARTESIAN_POINT('Ctrl Pts',(0.00367177297546312,-0.0336938721132315,
0.0781723890818763));
#69132=CARTESIAN_POINT('Ctrl Pts',(0.00367034109970152,-0.0336910493285698,
0.0781708042714665));
#69133=CARTESIAN_POINT('Ctrl Pts',(0.00366891001591097,-0.0336882266020728,
0.0781692186364285));
#69134=CARTESIAN_POINT('Ctrl Pts',(0.00366604943561649,-0.0336825812713202,
0.0781660457200292));
#69135=CARTESIAN_POINT('Ctrl Pts',(0.00366461993908932,-0.0336797586670204,
0.0781644584386437));
#69136=CARTESIAN_POINT('Ctrl Pts',(0.00366319123664674,-0.033676936124375,
0.0781628703342038));
#69137=CARTESIAN_POINT('Origin',(0.015079169887541,-0.0345562514173524,
0.06638943663483));
#69138=CARTESIAN_POINT('Ctrl Pts',(0.0037419283827865,-0.034243627687391,
0.0778752492782319));
#69139=CARTESIAN_POINT('Ctrl Pts',(0.00388242847548842,-0.033943005420181,
0.0780405136191053));
#69140=CARTESIAN_POINT('Ctrl Pts',(0.0040349778094604,-0.0336441434784053,
0.0781947254186484));
#69141=CARTESIAN_POINT('Ctrl Pts',(0.00390795891713605,-0.034243627687391,
0.078062155301847));
#69142=CARTESIAN_POINT('Ctrl Pts',(0.00405550828672741,-0.033943005420181,
0.078221157697888));
#69143=CARTESIAN_POINT('Ctrl Pts',(0.0042146151959899,-0.0336441434784053,
0.0783685943617086));
#69144=CARTESIAN_POINT('Ctrl Pts',(0.00390961922247955,-0.034243627687391,
0.0780640243620831));
#69145=CARTESIAN_POINT('Ctrl Pts',(0.0040572390848398,-0.033943005420181,
0.0782229641386759));
#69146=CARTESIAN_POINT('Ctrl Pts',(0.00421641156985519,-0.0336441434784053,
0.0783703330511392));
#69147=CARTESIAN_POINT('',(0.00393265065846204,-0.0341934961088741,0.0780885963818718));
#69148=CARTESIAN_POINT('',(0.00409800492354329,-0.0338664212864431,0.0782574617933473));
#69149=CARTESIAN_POINT('Origin',(0.0164709577679441,-0.0345610720405665,
0.0670050951932994));
#69150=CARTESIAN_POINT('Origin',(-0.00357801441268596,-0.0336938005072879,
0.0860892848005765));
#69151=CARTESIAN_POINT('',(0.004009684300756,-0.0336938721132327,0.0781689953386565));
#69152=CARTESIAN_POINT('',(0.00405432007862871,-0.0336938721132427,0.0782127434510211));
#69153=CARTESIAN_POINT('',(0.00384803921488506,-0.0340203938281605,0.0779965760078509));
#69154=CARTESIAN_POINT('Origin',(0.0167302578751519,-0.0345589643243195,
0.0674104347896106));
#69155=CARTESIAN_POINT('',(0.00384904919316617,-0.034193496108874,0.0779956674036122));
#69156=CARTESIAN_POINT('Origin',(-0.00434315919637213,-0.0341934220717669,
0.0853656022723086));
#69157=CARTESIAN_POINT('',(0.0038908499258241,-0.0341934961088841,0.0780421318927521));
#69158=CARTESIAN_POINT('Ctrl Pts',(0.00350932721877318,-0.0340223579322397,
0.077984945278602));
#69159=CARTESIAN_POINT('Ctrl Pts',(0.00356222111612229,-0.0339125849573575,
0.0780485906477019));
#69160=CARTESIAN_POINT('Ctrl Pts',(0.0036163951567911,-0.0338030433565231,
0.0781110965131711));
#69161=CARTESIAN_POINT('Ctrl Pts',(0.0036717729754591,-0.0336938721132327,
0.0781723890818771));
#69162=CARTESIAN_POINT('Ctrl Pts',(0.0036225906443956,-0.0340223579322397,
0.0779884915790218));
#69163=CARTESIAN_POINT('Ctrl Pts',(0.00367553345447663,-0.0339125849573575,
0.0780505747500789));
#69164=CARTESIAN_POINT('Ctrl Pts',(0.00372972403963752,-0.0338030433565231,
0.078111518502864));
#69165=CARTESIAN_POINT('Ctrl Pts',(0.00378508619048596,-0.0336938721132327,
0.0781712510437988));
#69166=CARTESIAN_POINT('Ctrl Pts',(0.00373585407001801,-0.0340223579322397,
0.0779920378794416));
#69167=CARTESIAN_POINT('Ctrl Pts',(0.00378884579283097,-0.0339125849573575,
0.0780525588524559));
#69168=CARTESIAN_POINT('Ctrl Pts',(0.00384305292248394,-0.0338030433565231,
0.0781119404925568));
#69169=CARTESIAN_POINT('Ctrl Pts',(0.00389839940551282,-0.0336938721132327,
0.0781701130057204));
#69170=CARTESIAN_POINT('Ctrl Pts',(0.00384911749564042,-0.0340223579322397,
0.0779955841798613));
#69171=CARTESIAN_POINT('Ctrl Pts',(0.00390215813118531,-0.0339125849573575,
0.078054542954833));
#69172=CARTESIAN_POINT('Ctrl Pts',(0.00395638180533036,-0.0338030433565231,
0.0781123624822497));
#69173=CARTESIAN_POINT('Ctrl Pts',(0.00401171262053968,-0.0336938721132327,
0.078168974967642));
#69174=CARTESIAN_POINT('',(0.00384072863811791,-0.0336938721132427,0.0781706922102768));
#69175=CARTESIAN_POINT('Ctrl Pts',(0.00366319124028913,-0.0337108120662679,
0.0781628703309272));
#69176=CARTESIAN_POINT('Ctrl Pts',(0.00369515825582565,-0.0337611408994407,
0.0781341119243458));
#69177=CARTESIAN_POINT('Ctrl Pts',(0.00372654194424991,-0.0338121088781551,
0.0781058782948817));
#69178=CARTESIAN_POINT('Ctrl Pts',(0.00378817125688635,-0.0339153382773233,
0.0780504348698266));
#69179=CARTESIAN_POINT('Ctrl Pts',(0.00381839080814706,-0.0339675558473107,
0.07802324853018));
#69180=CARTESIAN_POINT('Ctrl Pts',(0.00384803921491822,-0.0340203938281304,
0.0779965760078282));
#69181=CARTESIAN_POINT('Ctrl Pts',(0.003932757672405,-0.0341934961088741,
0.0780865710596998));
#69182=CARTESIAN_POINT('Ctrl Pts',(0.00401414317778697,-0.0340287516182428,
0.0781732171899265));
#69183=CARTESIAN_POINT('Ctrl Pts',(0.00409904029110814,-0.0338644633275951,
0.0782564255580111));
#69184=CARTESIAN_POINT('Ctrl Pts',(0.00393265065846206,-0.0341934961088741,
0.0780885963818717));
#69185=CARTESIAN_POINT('Ctrl Pts',(0.00401407803578436,-0.0340287516182428,
0.0781752447245274));
#69186=CARTESIAN_POINT('Ctrl Pts',(0.00409901707670845,-0.033864463327595,
0.0782584535725514));
#69187=CARTESIAN_POINT('Ctrl Pts',(0.00391482007723506,-0.0341934961088741,
0.0784260540112638));
#69188=CARTESIAN_POINT('Ctrl Pts',(0.00400322412519192,-0.0340287516182428,
0.0785130709871392));
#69189=CARTESIAN_POINT('Ctrl Pts',(0.00409514911120959,-0.033864463327595,
0.0785963598023026));
#69190=CARTESIAN_POINT('',(0.00392396340701163,-0.0341764758832409,0.0784350346736767));
#69191=CARTESIAN_POINT('',(0.00391482007723565,-0.034193496108874,0.0784260540112524));
#69192=CARTESIAN_POINT('Origin',(0.0158796153722629,-0.0345621027314363,
0.066968399723049));
#69193=CARTESIAN_POINT('Ctrl Pts',(0.00392396340646852,-0.0341764758837506,
0.0784350346719325));
#69194=CARTESIAN_POINT('Ctrl Pts',(0.00395400916461337,-0.0341260050040629,
0.0784043792545373));
#69195=CARTESIAN_POINT('Ctrl Pts',(0.00398353262931382,-0.0340749269148536,
0.0783742566738718));
#69196=CARTESIAN_POINT('Ctrl Pts',(0.00404155798382064,-0.0339715436306741,
0.07831505396907));
#69197=CARTESIAN_POINT('Ctrl Pts',(0.00407003786434501,-0.0339192778238253,
0.0782859963093393));
#69198=CARTESIAN_POINT('Ctrl Pts',(0.00409800492169441,-0.033866421285696,
0.0782574617929191));
#69199=CARTESIAN_POINT('',(0.00392373536785884,-0.0341934961088841,0.0782573251965721));
#69200=CARTESIAN_POINT('Origin',(0.00812378219310841,-0.0315241814719618,
0.07415));
#69201=CARTESIAN_POINT('',(0.00392396340812783,-0.0342105180190355,0.0784350346737397));
#69202=CARTESIAN_POINT('',(0.00393312589888613,-0.0341934961088739,0.0784439957875769));
#69203=CARTESIAN_POINT('Origin',(0.0158511247668744,-0.0345621700984072,
0.0669331443589828));
#69204=CARTESIAN_POINT('Origin',(0.015148162081767,-0.0345621041817851,
0.0662514884247236));
#69205=CARTESIAN_POINT('Origin',(0.015183977864322,-0.0345621713726151,
0.0662792703143448));
#69206=CARTESIAN_POINT('Ctrl Pts',(0.00400861303500967,-0.0346945769586966,
0.0781679453770228));
#69207=CARTESIAN_POINT('Ctrl Pts',(0.00409277050962898,-0.0345275153362944,
0.0782541392426631));
#69208=CARTESIAN_POINT('Ctrl Pts',(0.0041796604694202,-0.0343603235965185,
0.0783377087273367));
#69209=CARTESIAN_POINT('Ctrl Pts',(0.00426902225899016,-0.034193496108874,
0.0784184104890255));
#69210=CARTESIAN_POINT('Ctrl Pts',(0.00406848449422091,-0.0346945769586966,
0.0782266261808496));
#69211=CARTESIAN_POINT('Ctrl Pts',(0.00415387106177088,-0.0345275153362944,
0.0783115660148054));
#69212=CARTESIAN_POINT('Ctrl Pts',(0.00424195099425694,-0.0343603235965185,
0.0783938424895965));
#69213=CARTESIAN_POINT('Ctrl Pts',(0.00433246017371171,-0.034193496108874,
0.0784732161396614));
#69214=CARTESIAN_POINT('Ctrl Pts',(0.00412835595343221,-0.0346945769586966,
0.078285306984677));
#69215=CARTESIAN_POINT('Ctrl Pts',(0.00421497161391285,-0.0345275153362944,
0.0783689927869475));
#69216=CARTESIAN_POINT('Ctrl Pts',(0.00430424151909371,-0.0343603235965185,
0.0784499762518558));
#69217=CARTESIAN_POINT('Ctrl Pts',(0.00439589808843326,-0.034193496108874,
0.0785280217902974));
#69218=CARTESIAN_POINT('Ctrl Pts',(0.00418822741264338,-0.0346945769586966,
0.0783439877885032));
#69219=CARTESIAN_POINT('Ctrl Pts',(0.00427607216605468,-0.0345275153362944,
0.0784264195590902));
#69220=CARTESIAN_POINT('Ctrl Pts',(0.0043665320439304,-0.0343603235965185,
0.078506110014116));
#69221=CARTESIAN_POINT('Ctrl Pts',(0.00445933600315482,-0.034193496108874,
0.0785828274409331));
#69222=CARTESIAN_POINT('',(0.00418822741221091,-0.0346945769586966,0.078343987788079));
#69223=CARTESIAN_POINT('',(0.00436385853472848,-0.0343667727831489,0.0785021373006342));
#69224=CARTESIAN_POINT('Origin',(0.0155593803504305,-0.0345626457066645,
0.0659587494736872));
#69225=CARTESIAN_POINT('Origin',(-0.00286144870193541,-0.0341934771029068,
0.0868654853021026));
#69226=CARTESIAN_POINT('',(0.00427015733847042,-0.034193496108874,0.0784193911134631));
#69227=CARTESIAN_POINT('',(0.00431745200453473,-0.034193496108884,0.0784602501952396));
#69228=CARTESIAN_POINT('',(0.00409800492290952,-0.0345211942962664,0.078257461791745));
#69229=CARTESIAN_POINT('Origin',(0.015900435741368,-0.0345625596118997,
0.0662976772090484));
#69230=CARTESIAN_POINT('',(0.00409895585648141,-0.0346945769586885,0.0782564915633657));
#69231=CARTESIAN_POINT('Origin',(-0.00364520733230665,-0.0346945685853842,
0.0861577858689212));
#69232=CARTESIAN_POINT('',(0.00414359163435617,-0.0346945769587025,0.0783002396757324));
#69233=CARTESIAN_POINT('Ctrl Pts',(0.00375923165823636,-0.0345231616327841,
0.0782671226151987));
#69234=CARTESIAN_POINT('Ctrl Pts',(0.00381598039704188,-0.0344132092796987,
0.0783272817995263));
#69235=CARTESIAN_POINT('Ctrl Pts',(0.00387397055314826,-0.0343032738558979,
0.0783862640770171));
#69236=CARTESIAN_POINT('Ctrl Pts',(0.00393312589888613,-0.0341934961088739,
0.0784439957875769));
#69237=CARTESIAN_POINT('Ctrl Pts',(0.00387249406514685,-0.0345231616327841,
0.0782635500363809));
#69238=CARTESIAN_POINT('Ctrl Pts',(0.00392919356098316,-0.0344132092796987,
0.0783221480578899));
#69239=CARTESIAN_POINT('Ctrl Pts',(0.00398710218523956,-0.0343032738558979,
0.078379570271663));
#69240=CARTESIAN_POINT('Ctrl Pts',(0.00404614386589386,-0.0341934961088739,
0.0784357450135522));
#69241=CARTESIAN_POINT('Ctrl Pts',(0.00398575647205734,-0.0345231616327841,
0.0782599774575631));
#69242=CARTESIAN_POINT('Ctrl Pts',(0.00404240672492443,-0.0344132092796987,
0.0783170143162536));
#69243=CARTESIAN_POINT('Ctrl Pts',(0.00410023381733086,-0.0343032738558979,
0.0783728764663089));
#69244=CARTESIAN_POINT('Ctrl Pts',(0.00415916183290159,-0.0341934961088739,
0.0784274942395275));
#69245=CARTESIAN_POINT('Ctrl Pts',(0.00409901887896783,-0.0345231616327841,
0.0782564048787452));
#69246=CARTESIAN_POINT('Ctrl Pts',(0.00415561988886571,-0.0344132092796987,
0.0783118805746172));
#69247=CARTESIAN_POINT('Ctrl Pts',(0.00421336544942216,-0.0343032738558979,
0.0783661826609548));
#69248=CARTESIAN_POINT('Ctrl Pts',(0.00427217979990932,-0.0341934961088739,
0.0784192434655028));
#69249=CARTESIAN_POINT('',(0.00410164161868827,-0.0341934961088839,0.0784316934505299));
#69250=CARTESIAN_POINT('Ctrl Pts',(0.0039239634105423,-0.0342105180195383,
0.0784350346712663));
#69251=CARTESIAN_POINT('Ctrl Pts',(0.00395404295578628,-0.0342610556241312,
0.0784043448008363));
#69252=CARTESIAN_POINT('Ctrl Pts',(0.00398358273914332,-0.0343122189870182,
0.0783742056442631));
#69253=CARTESIAN_POINT('Ctrl Pts',(0.00404160867607172,-0.0344158119695139,
0.0783150023394436));
#69254=CARTESIAN_POINT('Ctrl Pts',(0.00407007109661467,-0.0344681990450033,
0.0782859624057777));
#69255=CARTESIAN_POINT('Ctrl Pts',(0.00409800492292408,-0.0345211942962448,
0.0782574617917192));
#69256=CARTESIAN_POINT('Ctrl Pts',(0.00418820704893545,-0.0346945769586932,
0.0783419602395123));
#69257=CARTESIAN_POINT('Ctrl Pts',(0.00427487286075145,-0.034529677707698,
0.0784233254708944));
#69258=CARTESIAN_POINT('Ctrl Pts',(0.00436482751749549,-0.034364806625142,
0.0785010391990618));
#69259=CARTESIAN_POINT('Ctrl Pts',(0.00418822741220435,-0.0346945769586932,
0.0783439877880727));
#69260=CARTESIAN_POINT('Ctrl Pts',(0.0042749351421522,-0.034529677707698,
0.0784253525984587));
#69261=CARTESIAN_POINT('Ctrl Pts',(0.00436493166380939,-0.034364806625142,
0.0785030641734747));
#69262=CARTESIAN_POINT('Ctrl Pts',(0.00419162115542487,-0.0346945769586932,
0.0786818991133777));
#69263=CARTESIAN_POINT('Ctrl Pts',(0.00428531496292501,-0.034529677707698,
0.0787631937605239));
#69264=CARTESIAN_POINT('Ctrl Pts',(0.00438228869270736,-0.034364806625142,
0.0788405464912489));
#69265=CARTESIAN_POINT('',(0.00420131034331547,-0.0346775396664996,0.0786902879403227));
#69266=CARTESIAN_POINT('',(0.00419162115542729,-0.0346945769586885,0.0786818991133677));
#69267=CARTESIAN_POINT('Origin',(0.0149385014674794,-0.0345626616892411,
0.0660283124331721));
#69268=CARTESIAN_POINT('Ctrl Pts',(0.0042013103427617,-0.0346775396670096,
0.0786902879385792));
#69269=CARTESIAN_POINT('Ctrl Pts',(0.00422939404452155,-0.0346269749928197,
0.0786577808423804));
#69270=CARTESIAN_POINT('Ctrl Pts',(0.0042569786090545,-0.034575790289081,
0.0786258514463341));
#69271=CARTESIAN_POINT('Ctrl Pts',(0.00431117231160473,-0.0344721681087947,
0.0785631218714823));
#69272=CARTESIAN_POINT('Ctrl Pts',(0.00433776020740688,-0.0344197714289613,
0.0785323462893058));
#69273=CARTESIAN_POINT('Ctrl Pts',(0.00436385853446865,-0.0343667727830683,
0.0785021373005513));
#69274=CARTESIAN_POINT('',(0.0041899242838291,-0.0346945769587026,0.0785129434507333));
#69275=CARTESIAN_POINT('Origin',(0.00812378219310841,-0.0315241814719618,
0.07415));
#69276=CARTESIAN_POINT('',(0.00420131034464479,-0.0347116136489782,0.0786902879399135));
#69277=CARTESIAN_POINT('',(0.0042110174281769,-0.0346945769586885,0.0786986560536431));
#69278=CARTESIAN_POINT('Origin',(0.014903020832005,-0.0345626676565481,
0.0660001258509192));
#69279=CARTESIAN_POINT('Origin',(0.0151696289895262,-0.0345626631767773,
0.0662279847007374));
#69280=CARTESIAN_POINT('Origin',(0.0152026653345296,-0.0345626691251745,
0.0662590006051623));
#69281=CARTESIAN_POINT('Ctrl Pts',(0.00424153578227314,-0.0352450361874068,
0.0783934567785217));
#69282=CARTESIAN_POINT('Ctrl Pts',(0.00440158038088488,-0.0349452760959493,
0.0785398781045686));
#69283=CARTESIAN_POINT('Ctrl Pts',(0.00457219936302422,-0.034644428984174,
0.0786738282490249));
#69284=CARTESIAN_POINT('Ctrl Pts',(0.0042434360883573,-0.0352450361874068,
0.078395119445592));
#69285=CARTESIAN_POINT('Ctrl Pts',(0.00440354339548659,-0.0349452760959493,
0.0785414691004188));
#69286=CARTESIAN_POINT('Ctrl Pts',(0.00457421950942565,-0.034644428984174,
0.0786753430538034));
#69287=CARTESIAN_POINT('Ctrl Pts',(0.00443158520560055,-0.0352450361874068,
0.0785597399475977));
#69288=CARTESIAN_POINT('Ctrl Pts',(0.00459790127684407,-0.0349452760959493,
0.0786989934420251));
#69289=CARTESIAN_POINT('Ctrl Pts',(0.00477423400461568,-0.034644428984174,
0.0788253237249377));
#69290=CARTESIAN_POINT('Ctrl Pts',(0.00443346669677299,-0.0352450361874068,
0.0785613861526177));
#69291=CARTESIAN_POINT('Ctrl Pts',(0.00459984485565765,-0.0349452760959493,
0.0787005686854411));
#69292=CARTESIAN_POINT('Ctrl Pts',(0.00477623414956757,-0.034644428984174,
0.078826823531649));
#69293=CARTESIAN_POINT('',(0.0044593095501685,-0.0351951634053279,0.0785828086527249));
#69294=CARTESIAN_POINT('',(0.00464455084721618,-0.0348678972925388,0.0787296369115643));
#69295=CARTESIAN_POINT('Origin',(0.0144408273820345,-0.0345636767886177,
0.0651375939594543));
#69296=CARTESIAN_POINT('Origin',(-0.00203994926337658,-0.0346946199340828,
0.0875282986026686));
#69297=CARTESIAN_POINT('',(0.0045458388589538,-0.0346945769330289,0.0786529375407269));
#69298=CARTESIAN_POINT('',(0.00459560576947358,-0.0346945769458128,0.0786907463453233));
#69299=CARTESIAN_POINT('',(0.00436385853457462,-0.0350221583435276,0.0785021373004535));
#69300=CARTESIAN_POINT('Origin',(0.0148473209008226,-0.0345628458719425,
0.0653943164018214));
#69301=CARTESIAN_POINT('',(0.00436466485333552,-0.0351951360298761,0.0785011993543997));
#69302=CARTESIAN_POINT('Origin',(-0.00283893782162353,-0.0351951838366924,
0.0868394217306688));
#69303=CARTESIAN_POINT('',(0.00445933600261231,-0.0351951371328748,0.078582827440618));
#69304=CARTESIAN_POINT('Ctrl Pts',(0.00402636107151413,-0.0350241211494343,
0.0785330514658565));
#69305=CARTESIAN_POINT('Ctrl Pts',(0.00408673580833524,-0.0349144232818962,
0.0785894917617984));
#69306=CARTESIAN_POINT('Ctrl Pts',(0.00414831334359367,-0.0348045283579412,
0.0786447178510264));
#69307=CARTESIAN_POINT('Ctrl Pts',(0.00421101743660167,-0.0346945769439157,
0.0786986560608902));
#69308=CARTESIAN_POINT('Ctrl Pts',(0.0041391756800295,-0.0350241211494343,
0.0785223741109151));
#69309=CARTESIAN_POINT('Ctrl Pts',(0.00419940334066417,-0.0349144232818962,
0.0785772604318805));
#69310=CARTESIAN_POINT('Ctrl Pts',(0.0042608015899308,-0.0348045283579412,
0.0786309346561729));
#69311=CARTESIAN_POINT('Ctrl Pts',(0.00432329434281574,-0.0346945769439157,
0.0786833251074294));
#69312=CARTESIAN_POINT('Ctrl Pts',(0.00425199028854486,-0.0350241211494343,
0.0785116967559738));
#69313=CARTESIAN_POINT('Ctrl Pts',(0.0043120708729931,-0.0349144232818962,
0.0785650291019626));
#69314=CARTESIAN_POINT('Ctrl Pts',(0.00437328983626794,-0.0348045283579412,
0.0786171514613195));
#69315=CARTESIAN_POINT('Ctrl Pts',(0.00443557124902981,-0.0346945769439157,
0.0786679941539687));
#69316=CARTESIAN_POINT('Ctrl Pts',(0.00436480489706022,-0.0350241211494343,
0.0785010194010324));
#69317=CARTESIAN_POINT('Ctrl Pts',(0.00442473840532203,-0.0349144232818962,
0.0785527977720447));
#69318=CARTESIAN_POINT('Ctrl Pts',(0.00448577808260507,-0.0348045283579412,
0.078603368266466));
#69319=CARTESIAN_POINT('Ctrl Pts',(0.00454784815524387,-0.0346945769439157,
0.0786526632005079));
#69320=CARTESIAN_POINT('',(0.00437842814328991,-0.0346945769458128,0.0786757967970733));
#69321=CARTESIAN_POINT('Ctrl Pts',(0.00420131034679082,-0.0347116136492788,
0.0786902879374189));
#69322=CARTESIAN_POINT('Ctrl Pts',(0.00422938290564181,-0.0347621546532281,
0.0786577937589219));
#69323=CARTESIAN_POINT('Ctrl Pts',(0.00425696187304804,-0.0348133084096997,
0.0786258709158915));
#69324=CARTESIAN_POINT('Ctrl Pts',(0.00431115564150317,-0.0349168561544567,
0.078563141258971));
#69325=CARTESIAN_POINT('Ctrl Pts',(0.0043377489466328,-0.0349692089015913,
0.0785323593267541));
#69326=CARTESIAN_POINT('Ctrl Pts',(0.00436385853461358,-0.0350221583435,
0.0785021373004389));
#69327=CARTESIAN_POINT('Ctrl Pts',(0.00445922947991934,-0.0351951371254893,
0.0785813683063454));
#69328=CARTESIAN_POINT('Ctrl Pts',(0.00455084523931787,-0.035030733898093,
0.0786571306344719));
#69329=CARTESIAN_POINT('Ctrl Pts',(0.00464551405235916,-0.0348659306897825,
0.0787290416459421));
#69330=CARTESIAN_POINT('Ctrl Pts',(0.00445933600268492,-0.0351951371254893,
0.0785828274405272));
#69331=CARTESIAN_POINT('Ctrl Pts',(0.00455098192876717,-0.035030733898093,
0.0786585875663624));
#69332=CARTESIAN_POINT('Ctrl Pts',(0.00464568079169184,-0.0348659306897825,
0.0787304951306015));
#69333=CARTESIAN_POINT('Ctrl Pts',(0.00447718932921445,-0.0351951371254893,
0.0788273798501157));
#69334=CARTESIAN_POINT('Ctrl Pts',(0.00457389122292753,-0.035030733898093,
0.0789027708696265));
#69335=CARTESIAN_POINT('Ctrl Pts',(0.00467362647762573,-0.0348659306897825,
0.0789741006743426));
#69336=CARTESIAN_POINT('Origin',(0.00142736582007893,-0.0308609197411502,
0.0829643479260305));
#69337=CARTESIAN_POINT('',(0.00446711965051264,-0.0351951371254893,0.0786894467771819));
#69338=CARTESIAN_POINT('Origin',(0.00859590893976371,-0.03518404674412,
0.0732945223648207));
#69339=CARTESIAN_POINT('Origin',(0.00153424433607435,-0.0352322612301065,
0.0841373491110821));
#69340=CARTESIAN_POINT('',(0.00483591447171173,-0.0351951142564667,0.0788688706731626));
#69341=CARTESIAN_POINT('',(0.00493972642941176,-0.0351951372916787,0.0789379315882405));
#69342=CARTESIAN_POINT('Origin',(0.00846414469139679,-0.0352875119101824,
0.0741619812508536));
#69343=CARTESIAN_POINT('Origin',(0.00278723044504516,-0.0298325076522633,
0.0688758739377672));
#69344=CARTESIAN_POINT('Origin',(0.00119730982211957,-0.0338734199020578,
0.0788688060512241));
#69345=CARTESIAN_POINT('Ctrl Pts',(0.00269001517329539,-0.0321934096636942,
0.0760347577350164));
#69346=CARTESIAN_POINT('Ctrl Pts',(0.00272375143924168,-0.0320508460843289,
0.0761320195771432));
#69347=CARTESIAN_POINT('Ctrl Pts',(0.00276007550171859,-0.0319086045661005,
0.0762283016566206));
#69348=CARTESIAN_POINT('Ctrl Pts',(0.00279889208139986,-0.0317669892864814,
0.0763234031000984));
#69349=CARTESIAN_POINT('Ctrl Pts',(0.0027192084103453,-0.0321934096636942,
0.0761133591824487));
#69350=CARTESIAN_POINT('Ctrl Pts',(0.00275435160477109,-0.0320508460843289,
0.076210098479534));
#69351=CARTESIAN_POINT('Ctrl Pts',(0.00279206749514457,-0.0319086045661005,
0.0763058206065784));
#69352=CARTESIAN_POINT('Ctrl Pts',(0.00283225790454788,-0.0317669892864814,
0.076400326142627));
#69353=CARTESIAN_POINT('Ctrl Pts',(0.00274840164739521,-0.0321934096636942,
0.076191960629881));
#69354=CARTESIAN_POINT('Ctrl Pts',(0.0027849517703005,-0.0320508460843289,
0.0762881773819247));
#69355=CARTESIAN_POINT('Ctrl Pts',(0.00282405948857053,-0.0319086045661005,
0.0763833395565361));
#69356=CARTESIAN_POINT('Ctrl Pts',(0.00286562372769592,-0.0317669892864814,
0.0764772491851556));
#69357=CARTESIAN_POINT('Ctrl Pts',(0.00277759488444513,-0.0321934096636942,
0.0762705620773133));
#69358=CARTESIAN_POINT('Ctrl Pts',(0.0028155519358299,-0.0320508460843289,
0.0763662562843156));
#69359=CARTESIAN_POINT('Ctrl Pts',(0.00285605148199651,-0.0319086045661005,
0.0764608585064939));
#69360=CARTESIAN_POINT('Ctrl Pts',(0.00289898955084395,-0.0317669892864814,
0.0765541722276842));
#69361=CARTESIAN_POINT('',(0.00277707261166756,-0.0321934096636942,0.0762691558818855));
#69362=CARTESIAN_POINT('',(0.0028686516159578,-0.031866561751129,0.0764870339334687));
#69363=CARTESIAN_POINT('Origin',(0.0185272918711739,-0.0326371944421996,
0.0706880719260468));
#69364=CARTESIAN_POINT('Origin',(-0.00714680149905182,-0.031693926150899,
0.0809410533642363));
#69365=CARTESIAN_POINT('',(0.00273241349331969,-0.0320197221621774,0.0761526813799176));
#69366=CARTESIAN_POINT('Ctrl Pts',(0.00273243154286703,-0.0320197392094698,
0.076152865469824));
#69367=CARTESIAN_POINT('Ctrl Pts',(0.00274262281028387,-0.0319792716575996,
0.0761802983788608));
#69368=CARTESIAN_POINT('Ctrl Pts',(0.00275306960968677,-0.0319386439829638,
0.076207778478822));
#69369=CARTESIAN_POINT('Ctrl Pts',(0.00276379081377242,-0.031897909938157,
0.0762353316132561));
#69370=CARTESIAN_POINT('Ctrl Pts',(0.00277451180594564,-0.0318571766984884,
0.0762628842030822));
#69371=CARTESIAN_POINT('Ctrl Pts',(0.00278545104045337,-0.0318163871833545,
0.0762903704303193));
#69372=CARTESIAN_POINT('Ctrl Pts',(0.00279656761926225,-0.0317755399638303,
0.07631769705572));
#69373=CARTESIAN_POINT('',(0.00273355137358275,-0.0321934096636182,0.0761519769509753));
#69374=CARTESIAN_POINT('Origin',(0.000577389415186222,-0.0324112132163665,
0.0769752261397524));
#69375=CARTESIAN_POINT('',(0.00275531199263515,-0.0321934096636662,0.0762105664164404));
#69376=CARTESIAN_POINT('Ctrl Pts',(0.00277791771285805,-0.0321934096636618,
0.0762673121109242));
#69377=CARTESIAN_POINT('Ctrl Pts',(0.00280711709700424,-0.0320835708272592,
0.07634103574843));
#69378=CARTESIAN_POINT('Ctrl Pts',(0.00283782525116754,-0.0319739230346489,
0.0764141123434925));
#69379=CARTESIAN_POINT('Ctrl Pts',(0.00286999571080509,-0.0318646057455573,
0.0764864514149958));
#69380=CARTESIAN_POINT('Ctrl Pts',(0.00273070104777598,-0.0321934096636618,
0.0763703254659009));
#69381=CARTESIAN_POINT('Ctrl Pts',(0.00276132106637121,-0.0320835708272592,
0.0764447002580166));
#69382=CARTESIAN_POINT('Ctrl Pts',(0.00279346250656865,-0.0319739230346489,
0.0765183982300369));
#69383=CARTESIAN_POINT('Ctrl Pts',(0.0028270770090207,-0.0318646057455573,
0.0765913282465753));
#69384=CARTESIAN_POINT('Ctrl Pts',(0.00268348438269391,-0.0321934096636618,
0.0764733388208775));
#69385=CARTESIAN_POINT('Ctrl Pts',(0.00271552503573818,-0.0320835708272592,
0.0765483647676032));
#69386=CARTESIAN_POINT('Ctrl Pts',(0.00274909976196975,-0.0319739230346489,
0.0766226841165813));
#69387=CARTESIAN_POINT('Ctrl Pts',(0.0027841583072363,-0.0318646057455573,
0.0766962050781548));
#69388=CARTESIAN_POINT('Ctrl Pts',(0.00263626771761184,-0.0321934096636618,
0.0765763521758541));
#69389=CARTESIAN_POINT('Ctrl Pts',(0.00266972900510516,-0.0320835708272592,
0.0766520292771898));
#69390=CARTESIAN_POINT('Ctrl Pts',(0.00270473701737086,-0.0319739230346489,
0.0767269700031256));
#69391=CARTESIAN_POINT('Ctrl Pts',(0.0027412396054519,-0.0318646057455573,
0.0768010819097342));
#69392=CARTESIAN_POINT('',(0.0026414629696454,-0.0321763980308278,0.076588068069142));
#69393=CARTESIAN_POINT('',(0.00263626771762764,-0.0321934096636185,0.0765763521758782));
#69394=CARTESIAN_POINT('Origin',(0.0180003159370518,-0.032638623175221,
0.070429194154957));
#69395=CARTESIAN_POINT('Ctrl Pts',(0.00264146297253932,-0.0321763980306305,
0.0765880680678479));
#69396=CARTESIAN_POINT('Ctrl Pts',(0.00268067881820687,-0.032125959617565,
0.0765706282039456));
#69397=CARTESIAN_POINT('Ctrl Pts',(0.00271921519846222,-0.0320749164633059,
0.0765534905083077));
#69398=CARTESIAN_POINT('Ctrl Pts',(0.00279496004121797,-0.0319716057793932,
0.076519805661622));
#69399=CARTESIAN_POINT('Ctrl Pts',(0.00283213899080369,-0.031919378669013,
0.0765032716354018));
#69400=CARTESIAN_POINT('Ctrl Pts',(0.00286865161764783,-0.0318665617525314,
0.076487033932707));
#69401=CARTESIAN_POINT('',(0.0027066701646576,-0.0321934096636664,0.0764227540288918));
#69402=CARTESIAN_POINT('Origin',(0.00812378219310841,-0.0315241814719618,
0.07415));
#69403=CARTESIAN_POINT('',(0.00264146296930577,-0.032210423332377,0.0765880680692927));
#69404=CARTESIAN_POINT('',(0.00264668323176904,-0.0321934096636183,0.0765997728400262));
#69405=CARTESIAN_POINT('Origin',(0.0179878480322056,-0.0326387226476407,
0.0703856066204022));
#69406=CARTESIAN_POINT('Origin',(0.0175017309251695,-0.0326386247673746,
0.0693080517117185));
#69407=CARTESIAN_POINT('Origin',(0.0175257409011946,-0.0326387239810024,
0.0693465066926255));
#69408=CARTESIAN_POINT('Ctrl Pts',(0.00280523889076349,-0.0327445246967095,
0.0763388860502735));
#69409=CARTESIAN_POINT('Ctrl Pts',(0.00288779407774399,-0.0324436878339359,
0.0765394781901585));
#69410=CARTESIAN_POINT('Ctrl Pts',(0.00298522415396361,-0.0321434074405927,
0.0767332820748691));
#69411=CARTESIAN_POINT('Ctrl Pts',(0.00290538749880782,-0.0327445246967095,
0.0765679499197658));
#69412=CARTESIAN_POINT('Ctrl Pts',(0.0029965819708594,-0.0324436878339359,
0.0767647648931502));
#69413=CARTESIAN_POINT('Ctrl Pts',(0.00310234227723534,-0.0321434074405927,
0.0769541515956304));
#69414=CARTESIAN_POINT('',(0.00292068602045132,-0.0326943950436612,0.0766006968841704));
#69415=CARTESIAN_POINT('',(0.00302576498972626,-0.0323666188837389,0.0768123947104103));
#69416=CARTESIAN_POINT('Origin',(0.0180965475217363,-0.0326395579112048,
0.0693687340856444));
#69417=CARTESIAN_POINT('Origin',(-0.006764200291473,-0.0321933825603,0.0819251191929099));
#69418=CARTESIAN_POINT('',(0.00296910472131925,-0.0321934096532689,0.0767009655345619));
#69419=CARTESIAN_POINT('',(0.00299803695950301,-0.0321934096584275,0.0767563656784212));
#69420=CARTESIAN_POINT('',(0.00286865161508525,-0.0325210109756238,0.0764870339338416));
#69421=CARTESIAN_POINT('Origin',(0.0182781848506571,-0.0326393129160331,
0.0698139220355885));
#69422=CARTESIAN_POINT('',(0.00286989293566145,-0.0326943950436593,0.0764864819003117));
#69423=CARTESIAN_POINT('Origin',(-0.00723809272765096,-0.0326943765538153,
0.0809816506985317));
#69424=CARTESIAN_POINT('',(0.00289528947806638,-0.0326943950436702,0.076543589392251));
#69425=CARTESIAN_POINT('Ctrl Pts',(0.00255011175848464,-0.0325229783203769,
0.0763713054464067));
#69426=CARTESIAN_POINT('Ctrl Pts',(0.00258073240548661,-0.0324130253092449,
0.0764481383714599));
#69427=CARTESIAN_POINT('Ctrl Pts',(0.00261293779602111,-0.0323031222208069,
0.0765243262158763));
#69428=CARTESIAN_POINT('Ctrl Pts',(0.00264668323359993,-0.0321934096576657,
0.0765997728441197));
#69429=CARTESIAN_POINT('Ctrl Pts',(0.00265673565951443,-0.0325229783203769,
0.0764096784312474));
#69430=CARTESIAN_POINT('Ctrl Pts',(0.00268788527727328,-0.0324130253092449,
0.0764850415481566));
#69431=CARTESIAN_POINT('Ctrl Pts',(0.0027205891534663,-0.0323031222208069,
0.0765597488649146));
#69432=CARTESIAN_POINT('Ctrl Pts',(0.00275480202000012,-0.0321934096576657,
0.0766337061649673));
#69433=CARTESIAN_POINT('Ctrl Pts',(0.00276335956054423,-0.0325229783203769,
0.076448051416088));
#69434=CARTESIAN_POINT('Ctrl Pts',(0.00279503814905994,-0.0324130253092449,
0.0765219447248533));
#69435=CARTESIAN_POINT('Ctrl Pts',(0.0028282405109115,-0.0323031222208069,
0.0765951715139529));
#69436=CARTESIAN_POINT('Ctrl Pts',(0.00286292080640031,-0.0321934096576657,
0.0766676394858149));
#69437=CARTESIAN_POINT('Ctrl Pts',(0.00286998346157403,-0.0325229783203769,
0.0764864244009287));
#69438=CARTESIAN_POINT('Ctrl Pts',(0.00290219102084661,-0.0324130253092449,
0.07655884790155));
#69439=CARTESIAN_POINT('Ctrl Pts',(0.00293589186835669,-0.0323031222208069,
0.0766305941629912));
#69440=CARTESIAN_POINT('Ctrl Pts',(0.00297103959280049,-0.0321934096576657,
0.0767015728066625));
#69441=CARTESIAN_POINT('',(0.00280789397620474,-0.0321934096584275,0.0766503691869222));
#69442=CARTESIAN_POINT('Ctrl Pts',(0.00264146297247978,-0.0322104233328919,
0.0765880680678742));
#69443=CARTESIAN_POINT('Ctrl Pts',(0.00268073195631818,-0.0322609421831417,
0.0765706045726451));
#69444=CARTESIAN_POINT('Ctrl Pts',(0.00271929429548424,-0.0323120888240844,
0.0765534553327049));
#69445=CARTESIAN_POINT('Ctrl Pts',(0.0027950397115963,-0.0324156524631806,
0.0765197702310391));
#69446=CARTESIAN_POINT('Ctrl Pts',(0.00283219165321953,-0.0324680267167308,
0.07650324821565));
#69447=CARTESIAN_POINT('Ctrl Pts',(0.00286865161512663,-0.0325210109755912,
0.076487033933828));
#69448=CARTESIAN_POINT('Origin',(0.00581579726585811,-0.0262834582511792,
0.0666282587511482));
#69449=CARTESIAN_POINT('Origin',(-0.00402200473973704,-0.0342770910835669,
0.073598576003963));
#69450=CARTESIAN_POINT('Ctrl Pts',(0.00292141350614364,-0.0326943950436604,
0.076598804146629));
#69451=CARTESIAN_POINT('Ctrl Pts',(0.00295516261683231,-0.0325844576448134,
0.0766705025374135));
#69452=CARTESIAN_POINT('Ctrl Pts',(0.00299039695627052,-0.0324744968375323,
0.076741508015463));
#69453=CARTESIAN_POINT('Ctrl Pts',(0.00302707012533032,-0.0323646534831895,
0.0768117302270937));
#69454=CARTESIAN_POINT('Ctrl Pts',(0.00288075833330346,-0.0326943950436604,
0.0767045788340702));
#69455=CARTESIAN_POINT('Ctrl Pts',(0.00291596521742796,-0.0325844576448134,
0.0767768375293324));
#69456=CARTESIAN_POINT('Ctrl Pts',(0.00295266902148612,-0.0324744968375323,
0.0768483732023684));
#69457=CARTESIAN_POINT('Ctrl Pts',(0.00299082145421641,-0.0323646534831895,
0.0769190948461468));
#69458=CARTESIAN_POINT('Ctrl Pts',(0.00284010316046328,-0.0326943950436604,
0.0768103535215114));
#69459=CARTESIAN_POINT('Ctrl Pts',(0.00287676781802361,-0.0325844576448134,
0.0768831725212512));
#69460=CARTESIAN_POINT('Ctrl Pts',(0.00291494108670172,-0.0324744968375323,
0.0769552383892738));
#69461=CARTESIAN_POINT('Ctrl Pts',(0.0029545727831025,-0.0323646534831895,
0.0770264594652));
#69462=CARTESIAN_POINT('Ctrl Pts',(0.0027994479876231,-0.0326943950436604,
0.0769161282089526));
#69463=CARTESIAN_POINT('Ctrl Pts',(0.00283757041861926,-0.0325844576448134,
0.07698950751317));
#69464=CARTESIAN_POINT('Ctrl Pts',(0.00287721315191733,-0.0324744968375323,
0.0770621035761792));
#69465=CARTESIAN_POINT('Ctrl Pts',(0.00291832411198859,-0.0323646534831895,
0.0771338240842531));
#69466=CARTESIAN_POINT('',(0.0028053686348441,-0.0326773559991174,0.0769274947710929));
#69467=CARTESIAN_POINT('',(0.00279944798762602,-0.0326943950436594,0.0769161282089466));
#69468=CARTESIAN_POINT('Origin',(0.0175009479672079,-0.0326395670470851,
0.069196178123875));
#69469=CARTESIAN_POINT('Ctrl Pts',(0.00280536863780952,-0.0326773559987453,
0.0769274947695367));
#69470=CARTESIAN_POINT('Ctrl Pts',(0.00284344265659943,-0.0326267922586819,
0.0769076109476141));
#69471=CARTESIAN_POINT('Ctrl Pts',(0.00288084184090237,-0.0325756109581063,
0.0768880795520755));
#69472=CARTESIAN_POINT('Ctrl Pts',(0.00295432236932552,-0.0324719985462371,
0.0768497049914597));
#69473=CARTESIAN_POINT('Ctrl Pts',(0.00299037424223145,-0.0324196091621781,
0.0768308772174652));
#69474=CARTESIAN_POINT('Ctrl Pts',(0.00302576498976948,-0.0323666188837757,
0.0768123947103877));
#69475=CARTESIAN_POINT('',(0.00286006700404867,-0.0326943950436703,0.0767584125465685));
#69476=CARTESIAN_POINT('Origin',(0.00812378219310841,-0.0315241814719618,
0.07415));
#69477=CARTESIAN_POINT('',(0.00280536863488315,-0.0327114338379858,0.0769274947710722));
#69478=CARTESIAN_POINT('',(0.00281131354479966,-0.0326943950436593,0.07693884866222));
#69479=CARTESIAN_POINT('Origin',(0.0174792905163763,-0.0326395659724961,
0.0691563769486344));
#69480=CARTESIAN_POINT('Origin',(0.0175474642808288,-0.0326395683304246,
0.0692852422766188));
#69481=CARTESIAN_POINT('Origin',(0.0175677465258632,-0.0326395673934692,
0.0693257614342945));
#69482=CARTESIAN_POINT('Ctrl Pts',(0.00295319228954088,-0.0332451089994432,
0.0766685561437311));
#69483=CARTESIAN_POINT('Ctrl Pts',(0.00304818118860149,-0.0329451141710253,
0.0768635681325073));
#69484=CARTESIAN_POINT('Ctrl Pts',(0.00315758933443493,-0.0326442513127493,
0.0770508711606103));
#69485=CARTESIAN_POINT('Ctrl Pts',(0.00306752783277678,-0.0332451089994432,
0.0768908788451202));
#69486=CARTESIAN_POINT('Ctrl Pts',(0.00317090176970667,-0.0329451141710253,
0.0770815785983315));
#69487=CARTESIAN_POINT('Ctrl Pts',(0.00328834631719047,-0.0326442513127493,
0.0772639500461449));
#69488=CARTESIAN_POINT('Ctrl Pts',(0.00306867118820914,-0.0332451089994432,
0.0768931020721341));
#69489=CARTESIAN_POINT('Ctrl Pts',(0.00317212897551773,-0.0329451141710253,
0.0770837587029898));
#69490=CARTESIAN_POINT('Ctrl Pts',(0.00328965388701803,-0.0326442513127493,
0.0772660808350003));
#69491=CARTESIAN_POINT('',(0.00308483367278007,-0.0331951640388616,0.0769225661055207));
#69492=CARTESIAN_POINT('',(0.00320299791123032,-0.0328677532355008,0.0771272482464603));
#69493=CARTESIAN_POINT('Origin',(0.017386680150143,-0.0326402808282017,
0.0681767422555932));
#69494=CARTESIAN_POINT('Origin',(-0.00625614153616046,-0.0326944278779117,
0.0828508016780252));
#69495=CARTESIAN_POINT('',(0.00313945275405452,-0.0326943950436593,0.0770195966690428));
#69496=CARTESIAN_POINT('',(0.00317180650376106,-0.0326943950436694,0.0770730708205709));
#69497=CARTESIAN_POINT('',(0.00302576498972491,-0.0330220786163545,0.0768123947104077));
#69498=CARTESIAN_POINT('Origin',(0.0176619112604149,-0.0326396682765736,
0.068570950932937));
#69499=CARTESIAN_POINT('',(0.00302696919836557,-0.0331951640388587,0.0768117658230245));
#69500=CARTESIAN_POINT('Origin',(-0.0067515135471169,-0.0331952026560048,
0.0819184912642713));
#69501=CARTESIAN_POINT('',(0.00305590143558282,-0.0331951640388701,0.0768671659642826));
#69502=CARTESIAN_POINT('Ctrl Pts',(0.00270058745800114,-0.0330240426238172,
0.0767168967383076));
#69503=CARTESIAN_POINT('Ctrl Pts',(0.00273594896137764,-0.0329142774063519,
0.0767916065293464));
#69504=CARTESIAN_POINT('Ctrl Pts',(0.00277287255382553,-0.0328043479726691,
0.0768656225448883));
#69505=CARTESIAN_POINT('Ctrl Pts',(0.00281131354479966,-0.0326943950436593,
0.0769388486622199));
#69506=CARTESIAN_POINT('Ctrl Pts',(0.0028094103993424,-0.0330240426238172,
0.0767484990075675));
#69507=CARTESIAN_POINT('Ctrl Pts',(0.00284520725476656,-0.0329142774063519,
0.0768217096565682));
#69508=CARTESIAN_POINT('Ctrl Pts',(0.0028825354248474,-0.0328043479726691,
0.0768942167827522));
#69509=CARTESIAN_POINT('Ctrl Pts',(0.00292134964751124,-0.0326943950436593,
0.076965926182132));
#69510=CARTESIAN_POINT('Ctrl Pts',(0.00291823334068367,-0.0330240426238172,
0.0767801012768274));
#69511=CARTESIAN_POINT('Ctrl Pts',(0.00295446554815548,-0.0329142774063519,
0.07685181278379));
#69512=CARTESIAN_POINT('Ctrl Pts',(0.00299219829586928,-0.0328043479726691,
0.0769228110206161));
#69513=CARTESIAN_POINT('Ctrl Pts',(0.00303138575022282,-0.0326943950436593,
0.076993003702044));
#69514=CARTESIAN_POINT('Ctrl Pts',(0.00302705628202493,-0.0330240426238172,
0.0768117035460873));
#69515=CARTESIAN_POINT('Ctrl Pts',(0.0030637238415444,-0.0329142774063519,
0.0768819159110119));
#69516=CARTESIAN_POINT('Ctrl Pts',(0.00310186116689115,-0.0328043479726691,
0.0769514052584801));
#69517=CARTESIAN_POINT('Ctrl Pts',(0.00314142185293441,-0.0326943950436593,
0.077020081221956));
#69518=CARTESIAN_POINT('',(0.00297538314943708,-0.0326943950436693,0.0769792226656414));
#69519=CARTESIAN_POINT('Ctrl Pts',(0.00280536863781758,-0.0327114338383317,
0.0769274947695324));
#69520=CARTESIAN_POINT('Ctrl Pts',(0.00284343632372475,-0.0327619876831131,
0.0769076142549022));
#69521=CARTESIAN_POINT('Ctrl Pts',(0.00288083241478682,-0.0328131562604672,
0.0768880844747814));
#69522=CARTESIAN_POINT('Ctrl Pts',(0.00295431287558149,-0.0329167375858766,
0.0768497099494839));
#69523=CARTESIAN_POINT('Ctrl Pts',(0.00299036796694966,-0.0329691088920619,
0.0768308804946759));
#69524=CARTESIAN_POINT('Ctrl Pts',(0.00302576498976837,-0.0330220786163186,
0.0768123947103882));
#69525=CARTESIAN_POINT('Ctrl Pts',(0.0030854409739107,-0.0331951640388604,
0.0769206311147899));
#69526=CARTESIAN_POINT('Ctrl Pts',(0.00314272199584558,-0.0330306422010619,
0.0770247955892129));
#69527=CARTESIAN_POINT('Ctrl Pts',(0.00320425929881839,-0.0328657861914645,
0.0771265035709478));
#69528=CARTESIAN_POINT('Ctrl Pts',(0.00308483367277861,-0.0331951640388604,
0.0769225661055178));
#69529=CARTESIAN_POINT('Ctrl Pts',(0.0031421546994062,-0.0330306422010619,
0.0770267431355024));
#69530=CARTESIAN_POINT('Ctrl Pts',(0.00320373249182254,-0.0328657861914645,
0.0771284620086342));
#69531=CARTESIAN_POINT('Ctrl Pts',(0.0029836409722735,-0.0331951640388604,
0.0772449875977048));
#69532=CARTESIAN_POINT('Ctrl Pts',(0.00304762785653462,-0.0330306422010619,
0.0773512567218936));
#69533=CARTESIAN_POINT('Ctrl Pts',(0.00311595227910942,-0.0328657861914645,
0.0774547903946437));
#69534=CARTESIAN_POINT('',(0.00299026364734075,-0.0331781648281913,0.0772559599701381));
#69535=CARTESIAN_POINT('',(0.00298364097227652,-0.0331951640388588,0.0772449875976981));
#69536=CARTESIAN_POINT('Origin',(0.0167446679814435,-0.0326412092246788,
0.0681015706921973));
#69537=CARTESIAN_POINT('Ctrl Pts',(0.00299026364746687,-0.033178164828644,
0.0772559599682971));
#69538=CARTESIAN_POINT('Ctrl Pts',(0.00302703931528364,-0.0331276811546775,
0.0772337093766741));
#69539=CARTESIAN_POINT('Ctrl Pts',(0.00306315091092208,-0.0330765663497785,
0.077211860532896));
#69540=CARTESIAN_POINT('Ctrl Pts',(0.0031340770679752,-0.032973061446328,
0.0771689477077748));
#69541=CARTESIAN_POINT('Ctrl Pts',(0.00316886297954141,-0.0329207133374062,
0.0771479010668649));
#69542=CARTESIAN_POINT('Ctrl Pts',(0.0032029978965378,-0.0328677532289367,
0.0771272482390092));
#69543=CARTESIAN_POINT('',(0.0030342373225383,-0.0331951640388701,0.0770837768516194));
#69544=CARTESIAN_POINT('Origin',(0.00812378219310841,-0.0315241814719618,
0.07415));
#69545=CARTESIAN_POINT('',(0.00299026364900185,-0.0332121607144214,0.0772559599698887));
#69546=CARTESIAN_POINT('',(0.00299690974454838,-0.0331951640388587,0.0772669181728474));
#69547=CARTESIAN_POINT('Origin',(0.0167148396002469,-0.0326413641344407,
0.068067415206876));
#69548=CARTESIAN_POINT('Origin',(0.0174820935607263,-0.0326412103657649,
0.0693203784622903));
#69549=CARTESIAN_POINT('Origin',(0.0174985010147094,-0.0326413655906454,
0.0693626535943588));
#69550=CARTESIAN_POINT('Ctrl Pts',(0.00312152643615495,-0.0337436976235975,
0.0769882322565332));
#69551=CARTESIAN_POINT('Ctrl Pts',(0.00314705392721609,-0.0336723290703325,
0.0770332233029239));
#69552=CARTESIAN_POINT('Ctrl Pts',(0.00317338653564643,-0.033601104548885,
0.0770777479117201));
#69553=CARTESIAN_POINT('Ctrl Pts',(0.00325746133816869,-0.0333736987606857,
0.0772199061677783));
#69554=CARTESIAN_POINT('Ctrl Pts',(0.00334955545247764,-0.0331450831799191,
0.0773570054613371));
#69555=CARTESIAN_POINT('Ctrl Pts',(0.00324959534457015,-0.0337436976235975,
0.0772029375305657));
#69556=CARTESIAN_POINT('Ctrl Pts',(0.00327705392740539,-0.0336723290703325,
0.0772467767057847));
#69557=CARTESIAN_POINT('Ctrl Pts',(0.00330529659667296,-0.033601104548885,
0.0772901148955005));
#69558=CARTESIAN_POINT('Ctrl Pts',(0.00339546984508672,-0.0333736987606857,
0.0774284851504514));
#69559=CARTESIAN_POINT('Ctrl Pts',(0.00349343497818585,-0.0331450831799191,
0.0775614527212405));
#69560=CARTESIAN_POINT('Ctrl Pts',(0.0032508760336543,-0.0337436976235975,
0.077205084583306));
#69561=CARTESIAN_POINT('Ctrl Pts',(0.00327835392740729,-0.0336723290703325,
0.0772489122398133));
#69562=CARTESIAN_POINT('Ctrl Pts',(0.00330661569728322,-0.033601104548885,
0.0772922385653383));
#69563=CARTESIAN_POINT('Ctrl Pts',(0.0033968499301559,-0.0333736987606857,
0.0774305709402782));
#69564=CARTESIAN_POINT('Ctrl Pts',(0.00349487377344293,-0.0331450831799191,
0.0775634971938395));
#69565=CARTESIAN_POINT('',(0.00326886775284914,-0.0336938721132548,0.0772334932751286));
#69566=CARTESIAN_POINT('',(0.0033996509203255,-0.0333679869945434,0.0774303519197621));
#69567=CARTESIAN_POINT('Ctrl Pts',(0.00326886775285565,-0.0336938721132647,
0.0772334932751408));
#69568=CARTESIAN_POINT('Ctrl Pts',(0.00328090407360133,-0.0336629187933931,
0.0772524442836817));
#69569=CARTESIAN_POINT('Ctrl Pts',(0.00329304751061946,-0.0336319952301039,
0.0772713187537415));
#69570=CARTESIAN_POINT('Ctrl Pts',(0.0033052965966801,-0.0336011045488949,
0.0772901148955123));
#69571=CARTESIAN_POINT('Ctrl Pts',(0.00333603374500763,-0.0335235892595453,
0.077337280846893));
#69572=CARTESIAN_POINT('Ctrl Pts',(0.0033674908859935,-0.0334458668660368,
0.0773840373087036));
#69573=CARTESIAN_POINT('Ctrl Pts',(0.00339965092005911,-0.0333679869945384,
0.0774303519199386));
#69574=CARTESIAN_POINT('Ctrl Pts',(0.00339967571956702,-0.0333679692460368,
0.077430388839483));
#69575=CARTESIAN_POINT('Ctrl Pts',(0.00340004460580707,-0.033339189537481,
0.0774301254751632));
#69576=CARTESIAN_POINT('Ctrl Pts',(0.00340031921724595,-0.0333104081060444,
0.077429925427979));
#69577=CARTESIAN_POINT('Ctrl Pts',(0.00340067945138924,-0.0332532698185305,
0.0774296561547328));
#69578=CARTESIAN_POINT('Ctrl Pts',(0.00340076783166611,-0.0332249171053087,
0.0774295850184696));
#69579=CARTESIAN_POINT('Ctrl Pts',(0.00340076691158274,-0.0331960985374019,
0.0774295772582261));
#69580=CARTESIAN_POINT('Ctrl Pts',(0.00340076687221496,-0.0331956312550877,
0.0774295771493602));
#69581=CARTESIAN_POINT('Ctrl Pts',(0.00340076680876476,-0.0331951640388587,
0.0774295770579837));
#69582=CARTESIAN_POINT('',(0.00332947165532952,-0.0331951640388587,0.0773269028104969));
#69583=CARTESIAN_POINT('',(0.00336511923205677,-0.0331951640388687,0.0773782399342498));
#69584=CARTESIAN_POINT('',(0.00320299790946593,-0.0335216366567704,0.0771272482310453));
#69585=CARTESIAN_POINT('Origin',(0.0167877337917752,-0.0326434571527087,
0.0674926431002186));
#69586=CARTESIAN_POINT('',(0.00320416025344758,-0.0336938721132327,0.077126544972079));
#69587=CARTESIAN_POINT('Origin',(-0.00613933112997888,-0.0336938867896225,
0.0827796855776315));
#69588=CARTESIAN_POINT('',(0.00323651400315836,-0.0336938721132537,0.0771800191236138));
#69589=CARTESIAN_POINT('Ctrl Pts',(0.00287246613866903,-0.0335235895815172,
0.0770523576100163));
#69590=CARTESIAN_POINT('Ctrl Pts',(0.00291242280538719,-0.0334144449262748,
0.0771246523143955));
#69591=CARTESIAN_POINT('Ctrl Pts',(0.00295391893165918,-0.0333049234473147,
0.0771962046019677));
#69592=CARTESIAN_POINT('Ctrl Pts',(0.0029969097445482,-0.0331951640388587,
0.0772669181728474));
#69593=CARTESIAN_POINT('Ctrl Pts',(0.0029830588268381,-0.0335235895815172,
0.0770770644877937));
#69594=CARTESIAN_POINT('Ctrl Pts',(0.00302335563237224,-0.0334144449262748,
0.0771478366660834));
#69595=CARTESIAN_POINT('Ctrl Pts',(0.00306516083399531,-0.0333049234473147,
0.077217857651356));
#69596=CARTESIAN_POINT('Ctrl Pts',(0.00310842908618799,-0.0331951640388587,
0.0772870330659916));
#69597=CARTESIAN_POINT('Ctrl Pts',(0.00309365151500718,-0.0335235895815172,
0.0771017713655712));
#69598=CARTESIAN_POINT('Ctrl Pts',(0.00313428845935728,-0.0334144449262748,
0.0771710210177712));
#69599=CARTESIAN_POINT('Ctrl Pts',(0.00317640273633143,-0.0333049234473147,
0.0772395107007442));
#69600=CARTESIAN_POINT('Ctrl Pts',(0.00321994842782777,-0.0331951640388587,
0.0773071479591357));
#69601=CARTESIAN_POINT('Ctrl Pts',(0.00320424420317625,-0.0335235895815172,
0.0771264782433486));
#69602=CARTESIAN_POINT('Ctrl Pts',(0.00324522128634233,-0.0334144449262748,
0.077194205369459));
#69603=CARTESIAN_POINT('Ctrl Pts',(0.00328764463866756,-0.0333049234473147,
0.0772611637501324));
#69604=CARTESIAN_POINT('Ctrl Pts',(0.00333146776946756,-0.0331951640388587,
0.0773272628522799));
#69605=CARTESIAN_POINT('',(0.00316319069994895,-0.0331951640388687,0.0772969104916822));
#69606=CARTESIAN_POINT('Ctrl Pts',(0.00299026365167755,-0.0332121607145971,
0.077255959968262));
#69607=CARTESIAN_POINT('Ctrl Pts',(0.00302697745968889,-0.0332625444109906,
0.0772337468181496));
#69608=CARTESIAN_POINT('Ctrl Pts',(0.00306305863117457,-0.0333135300747148,
0.0772119164354719));
#69609=CARTESIAN_POINT('Ctrl Pts',(0.00313398434181871,-0.0334167203140597,
0.0771690038763366));
#69610=CARTESIAN_POINT('Ctrl Pts',(0.00316880141089817,-0.033468884758729,
0.0771479383202467));
#69611=CARTESIAN_POINT('Ctrl Pts',(0.00320299791014901,-0.0335216366562368,
0.0771272482308138));
#69612=CARTESIAN_POINT('Ctrl Pts',(0.00326910666883635,-0.0336938721132388,
0.0772325223817137));
#69613=CARTESIAN_POINT('Ctrl Pts',(0.00328714969522587,-0.0336474569764957,
0.0772609384085093));
#69614=CARTESIAN_POINT('Ctrl Pts',(0.00330552413076729,-0.033601104548885,
0.0772891412718158));
#69615=CARTESIAN_POINT('Ctrl Pts',(0.00335204397701066,-0.0334837508592655,
0.0773605444374629));
#69616=CARTESIAN_POINT('Ctrl Pts',(0.00340065921900735,-0.0333660264659097,
0.0774305377686061));
#69617=CARTESIAN_POINT('Ctrl Pts',(0.00326886775283826,-0.0336938721132388,
0.0772334932751113));
#69618=CARTESIAN_POINT('Ctrl Pts',(0.00328691646218901,-0.0336474569764957,
0.0772619107003615));
#69619=CARTESIAN_POINT('Ctrl Pts',(0.00330529659667295,-0.033601104548885,
0.0772901148955005));
#69620=CARTESIAN_POINT('Ctrl Pts',(0.00335183087132848,-0.0334837508592655,
0.0773615214330415));
#69621=CARTESIAN_POINT('Ctrl Pts',(0.00340046063531764,-0.0333660264659097,
0.077431517707054));
#69622=CARTESIAN_POINT('Ctrl Pts',(0.00318763525797031,-0.0336938721132388,
0.0775636013196375));
#69623=CARTESIAN_POINT('Ctrl Pts',(0.00320761619924714,-0.0336474569764957,
0.077592494225636));
#69624=CARTESIAN_POINT('Ctrl Pts',(0.00322793399936187,-0.033601104548885,
0.0776211512497286));
#69625=CARTESIAN_POINT('Ctrl Pts',(0.00327937399789735,-0.0334837508592655,
0.0776937042460684));
#69626=CARTESIAN_POINT('Ctrl Pts',(0.00333294130348528,-0.0333660264659097,
0.0777647011086698));
#69627=CARTESIAN_POINT('',(0.00319541831379252,-0.0336769361243753,0.0775721673648515));
#69628=CARTESIAN_POINT('',(0.00318811974601819,-0.033693872113232,0.0775616324843663));
#69629=CARTESIAN_POINT('Ctrl Pts',(0.0031954183137927,-0.033676936124375,
0.0775721673648517));
#69630=CARTESIAN_POINT('Ctrl Pts',(0.00319419991937076,-0.0336797586669961,
0.0775704127192077));
#69631=CARTESIAN_POINT('Ctrl Pts',(0.00319298250808888,-0.0336825812712718,
0.0775686574892483));
#69632=CARTESIAN_POINT('Ctrl Pts',(0.00319054965489436,-0.0336882265949077,
0.0775651458660598));
#69633=CARTESIAN_POINT('Ctrl Pts',(0.0031893342129824,-0.0336910493142397,
0.0775633894728613));
#69634=CARTESIAN_POINT('Ctrl Pts',(0.00318811974601561,-0.0336938721132351,
0.077561632484373));
#69635=CARTESIAN_POINT('Ctrl Pts',(0.00319541831379256,-0.0336769361243753,
0.0775721673648515));
#69636=CARTESIAN_POINT('Ctrl Pts',(0.00322984434082938,-0.033627903142825,
0.0775482625499652));
#69637=CARTESIAN_POINT('Ctrl Pts',(0.00326476567292551,-0.0335767852155825,
0.0775240138041409));
#69638=CARTESIAN_POINT('Ctrl Pts',(0.00333319318983,-0.0334733199122762,
0.0774764989653541));
#69639=CARTESIAN_POINT('Ctrl Pts',(0.00336674531917255,-0.0334209645148413,
0.0774532009693323));
#69640=CARTESIAN_POINT('Ctrl Pts',(0.00339965091615904,-0.0333679869844681,
0.0774303519137662));
#69641=CARTESIAN_POINT('',(0.00322849374944367,-0.0336938721132534,0.0773975628797575));
#69642=CARTESIAN_POINT('Origin',(0.00812378219310841,-0.0315241814719618,
0.07415));
#69643=CARTESIAN_POINT('',(0.0031954183148614,-0.0337108120655386,0.0775721673641177));
#69644=CARTESIAN_POINT('',(0.00320273936760633,-0.0336938721132327,0.0775826866314311));
#69645=CARTESIAN_POINT('Origin',(0.0172718609241822,-0.0345562510848324,
0.0691583577627806));
#69646=CARTESIAN_POINT('Ctrl Pts',(0.00320273936761098,-0.033693872113231,
0.0775826866314307));
#69647=CARTESIAN_POINT('Ctrl Pts',(0.0032015174131691,-0.0336910493311992,
0.0775809348577371));
#69648=CARTESIAN_POINT('Ctrl Pts',(0.00320029634609684,-0.0336882266033876,
0.0775791823627307));
#69649=CARTESIAN_POINT('Ctrl Pts',(0.00319785599361853,-0.0336825812712792,
0.0775756759391047));
#69650=CARTESIAN_POINT('Ctrl Pts',(0.00319663670821591,-0.0336797586669998,
0.0775739220104976));
#69651=CARTESIAN_POINT('Ctrl Pts',(0.00319541831379236,-0.033676936124375,
0.0775721673648512));
#69652=CARTESIAN_POINT('Origin',(0.0159969813080498,-0.0345562513515122,
0.0673223721723791));
#69653=CARTESIAN_POINT('Ctrl Pts',(0.00330958307100335,-0.0342436276873909,
0.0772966826679415));
#69654=CARTESIAN_POINT('Ctrl Pts',(0.00342826216427442,-0.0339430054201809,
0.0774782531810595));
#69655=CARTESIAN_POINT('Ctrl Pts',(0.00356028073769327,-0.0336441434784051,
0.0776503684758071));
#69656=CARTESIAN_POINT('Ctrl Pts',(0.0034508788686863,-0.0342436276873909,
0.0775029240254747));
#69657=CARTESIAN_POINT('Ctrl Pts',(0.00357733648298728,-0.0339430054201809,
0.0776791654797324));
#69658=CARTESIAN_POINT('Ctrl Pts',(0.00371671007292475,-0.0336441434784051,
0.0778453809448418));
#69659=CARTESIAN_POINT('Ctrl Pts',(0.00345229182666312,-0.0342436276873909,
0.07750498643905));
#69660=CARTESIAN_POINT('Ctrl Pts',(0.00357882722617441,-0.0339430054201809,
0.0776811746027192));
#69661=CARTESIAN_POINT('Ctrl Pts',(0.00371827436627707,-0.0336441434784051,
0.0778473310695321));
#69662=CARTESIAN_POINT('',(0.00347206196219838,-0.0341934961088741,0.0775322513054685));
#69663=CARTESIAN_POINT('',(0.00361494791185617,-0.0338664212863469,0.0777205095474807));
#69664=CARTESIAN_POINT('Origin',(0.0173006318178325,-0.0345610720403646,
0.0681076134076986));
#69665=CARTESIAN_POINT('Origin',(-0.00498213160236743,-0.0336938005072949,
0.0845285157372853));
#69666=CARTESIAN_POINT('',(0.003538411509985,-0.0336938721132327,0.0776216711679468));
#69667=CARTESIAN_POINT('',(0.00357721222903342,-0.0336938721132426,0.0776706686597508));
#69668=CARTESIAN_POINT('',(0.00339965091615601,-0.0340203938281605,0.0774303519137619));
#69669=CARTESIAN_POINT('Origin',(0.0175070847443505,-0.0345589643243467,
0.0685422557012214));
#69670=CARTESIAN_POINT('',(0.00340076680876393,-0.0341934961088739,0.0774295770579827));
#69671=CARTESIAN_POINT('Origin',(-0.00565054137690369,-0.0341934220717627,
0.0837146417663959));
#69672=CARTESIAN_POINT('',(0.00343641438549115,-0.034193496108884,0.0774809141817356));
#69673=CARTESIAN_POINT('Ctrl Pts',(0.00306506748220749,-0.0340223579322396,
0.0773763610265673));
#69674=CARTESIAN_POINT('Ctrl Pts',(0.00310956741546666,-0.0339125849573574,
0.0774461338961124));
#69675=CARTESIAN_POINT('Ctrl Pts',(0.00315548021540779,-0.0338030433565231,
0.0775149366918551));
#69676=CARTESIAN_POINT('Ctrl Pts',(0.00320273936760564,-0.0336938721132327,
0.0775826866314311));
#69677=CARTESIAN_POINT('Ctrl Pts',(0.00317699332258989,-0.0340223579322396,
0.0773940750347268));
#69678=CARTESIAN_POINT('Ctrl Pts',(0.00322173757822165,-0.0339125849573574,
0.0774623041550182));
#69679=CARTESIAN_POINT('Ctrl Pts',(0.0032678625768305,-0.0338030433565231,
0.0775295592293766));
#69680=CARTESIAN_POINT('Ctrl Pts',(0.00331530170807924,-0.0336938721132327,
0.0775957594787677));
#69681=CARTESIAN_POINT('Ctrl Pts',(0.00328891916297228,-0.0340223579322396,
0.0774117890428864));
#69682=CARTESIAN_POINT('Ctrl Pts',(0.00333390774097664,-0.0339125849573574,
0.0774784744139241));
#69683=CARTESIAN_POINT('Ctrl Pts',(0.0033802449382532,-0.0338030433565231,
0.077544181766898));
#69684=CARTESIAN_POINT('Ctrl Pts',(0.00342786404855284,-0.0336938721132327,
0.0776088323261044));
#69685=CARTESIAN_POINT('Ctrl Pts',(0.00340084500335468,-0.0340223579322396,
0.0774295030510459));
#69686=CARTESIAN_POINT('Ctrl Pts',(0.00344607790373163,-0.0339125849573574,
0.0774946446728299));
#69687=CARTESIAN_POINT('Ctrl Pts',(0.00349262729967591,-0.0338030433565231,
0.0775588043044195));
#69688=CARTESIAN_POINT('Ctrl Pts',(0.00354042638902644,-0.0336938721132327,
0.0776219051734411));
#69689=CARTESIAN_POINT('',(0.00337057543880566,-0.0336938721132427,0.077602178899699));
#69690=CARTESIAN_POINT('Ctrl Pts',(0.00319541831781671,-0.033710812066268,
0.0775721673620571));
#69691=CARTESIAN_POINT('Ctrl Pts',(0.00323073764797705,-0.0337611408994413,
0.0775476422535255));
#69692=CARTESIAN_POINT('Ctrl Pts',(0.00326541247872095,-0.0338121088781569,
0.0775235646738136));
#69693=CARTESIAN_POINT('Ctrl Pts',(0.00333350472956026,-0.0339153382773232,
0.0774762826377611));
#69694=CARTESIAN_POINT('Ctrl Pts',(0.00336689334249021,-0.0339675558473112,
0.0774530981845989));
#69695=CARTESIAN_POINT('Ctrl Pts',(0.00339965091619176,-0.0340203938281304,
0.0774303519137434));
#69696=CARTESIAN_POINT('Ctrl Pts',(0.00347242197248126,-0.0341934961088741,
0.0775302553659703));
#69697=CARTESIAN_POINT('Ctrl Pts',(0.00354230608916746,-0.0340287516182428,
0.077626418574135));
#69698=CARTESIAN_POINT('Ctrl Pts',(0.00361610498956091,-0.0338644633275951,
0.0777196112491169));
#69699=CARTESIAN_POINT('Ctrl Pts',(0.00347206196219839,-0.0341934961088741,
0.0775322513054685));
#69700=CARTESIAN_POINT('Ctrl Pts',(0.0035419873433613,-0.0340287516182428,
0.0776284219565622));
#69701=CARTESIAN_POINT('Ctrl Pts',(0.00361582778059364,-0.0338644633275951,
0.077721620362621));
#69702=CARTESIAN_POINT('Ctrl Pts',(0.00341207732454776,-0.0341934961088741,
0.0778648132162559));
#69703=CARTESIAN_POINT('Ctrl Pts',(0.00348887816121998,-0.0340287516182428,
0.0779622240024765));
#69704=CARTESIAN_POINT('Ctrl Pts',(0.00356963943474203,-0.0338644633275951,
0.0780563773161981));
#69705=CARTESIAN_POINT('',(0.00342002298097895,-0.0341764758832406,0.0778748690265504));
#69706=CARTESIAN_POINT('',(0.00341207732454946,-0.034193496108874,0.0778648132162463));
#69707=CARTESIAN_POINT('Origin',(0.0167185512793139,-0.0345621025955202,
0.0679970923786799));
#69708=CARTESIAN_POINT('Ctrl Pts',(0.00342002298065817,-0.0341764758837501,
0.0778748690247524));
#69709=CARTESIAN_POINT('Ctrl Pts',(0.00345367396163459,-0.0341260050040318,
0.0778482210664868));
#69710=CARTESIAN_POINT('Ctrl Pts',(0.00348673998545543,-0.0340749269147912,
0.0778220362826484));
#69711=CARTESIAN_POINT('Ctrl Pts',(0.00355172785916549,-0.0339715436305661,
0.0777705729141452));
#69712=CARTESIAN_POINT('Ctrl Pts',(0.00358362505779547,-0.0339192778236895,
0.0777453138582455));
#69713=CARTESIAN_POINT('Ctrl Pts',(0.00361494790979576,-0.0338664212854881,
0.077720509546709));
#69714=CARTESIAN_POINT('',(0.00344206964338392,-0.0341934961088841,0.0776985322608674));
#69715=CARTESIAN_POINT('Origin',(0.00812378219310841,-0.0315241814719618,
0.07415));
#69716=CARTESIAN_POINT('',(0.00342002298207836,-0.0342105180190357,0.0778748690267528));
#69717=CARTESIAN_POINT('',(0.00342799009848599,-0.0341934961088739,0.0778849078441259));
#69718=CARTESIAN_POINT('Origin',(0.0166947039403234,-0.0345621700238114,
0.0679585443454162));
#69719=CARTESIAN_POINT('Origin',(0.0160827186936042,-0.034562104145154,
0.067194158895128));
#69720=CARTESIAN_POINT('Origin',(0.0161147699170915,-0.0345621714440594,
0.0672262105569304));
#69721=CARTESIAN_POINT('Ctrl Pts',(0.0035374802865757,-0.0346945769586966,
0.0776204952203742));
#69722=CARTESIAN_POINT('Ctrl Pts',(0.00361017119847693,-0.0345275153362944,
0.0777165571500617));
#69723=CARTESIAN_POINT('Ctrl Pts',(0.00368590197124099,-0.0343603235965186,
0.0778103578640126));
#69724=CARTESIAN_POINT('Ctrl Pts',(0.00376444450366233,-0.034193496108874,
0.0779016232702499));
#69725=CARTESIAN_POINT('Ctrl Pts',(0.00358952498655659,-0.0346945769586966,
0.0776862171921169));
#69726=CARTESIAN_POINT('Ctrl Pts',(0.00366359247146961,-0.0345275153362944,
0.0777811890247257));
#69727=CARTESIAN_POINT('Ctrl Pts',(0.00374066589074799,-0.0343603235965186,
0.0778738560676888));
#69728=CARTESIAN_POINT('Ctrl Pts',(0.00382051322206656,-0.034193496108874,
0.0779639476409435));
#69729=CARTESIAN_POINT('Ctrl Pts',(0.00364156968653757,-0.0346945769586966,
0.0777519391638623));
#69730=CARTESIAN_POINT('Ctrl Pts',(0.00371701374446233,-0.0345275153362944,
0.0778458208993921));
#69731=CARTESIAN_POINT('Ctrl Pts',(0.00379542981025503,-0.0343603235965186,
0.0779373542713669));
#69732=CARTESIAN_POINT('Ctrl Pts',(0.00387658194047087,-0.034193496108874,
0.078026272011638));
#69733=CARTESIAN_POINT('Ctrl Pts',(0.00369361438651835,-0.0346945769586966,
0.0778176611356023));
#69734=CARTESIAN_POINT('Ctrl Pts',(0.00377043501745496,-0.0345275153362944,
0.0779104527740538));
#69735=CARTESIAN_POINT('Ctrl Pts',(0.00385019372976199,-0.0343603235965186,
0.0780008524750413));
#69736=CARTESIAN_POINT('Ctrl Pts',(0.00393265065887501,-0.034193496108874,
0.0780885963823307));
#69737=CARTESIAN_POINT('',(0.00369361438614239,-0.0346945769586966,0.0778176611351273));
#69738=CARTESIAN_POINT('',(0.00384803921500643,-0.0343667727831482,0.0779965760080376));
#69739=CARTESIAN_POINT('Origin',(0.0165273843527379,-0.0345626457063339,
0.0669552674912437));
#69740=CARTESIAN_POINT('Origin',(-0.0043684998350524,-0.0341934771029004,
0.0853884053149871));
#69741=CARTESIAN_POINT('',(0.00376544772787017,-0.034193496108874,0.0779027384253525));
#69742=CARTESIAN_POINT('',(0.00380724846052817,-0.034193496108884,0.0779492029144924));
#69743=CARTESIAN_POINT('',(0.00361494791102639,-0.0345211942962673,0.0777205095457931));
#69744=CARTESIAN_POINT('Origin',(0.0168232715116394,-0.0345625596118009,
0.0673342682550502));
#69745=CARTESIAN_POINT('',(0.00361601294806193,-0.0346945769586885,0.0777196661515349));
#69746=CARTESIAN_POINT('Origin',(-0.00505738028098554,-0.0346945685853854,
0.0845880549798203));
#69747=CARTESIAN_POINT('',(0.00365481366711216,-0.0346945769587026,0.077768663643341));
#69748=CARTESIAN_POINT('Ctrl Pts',(0.00327763515248835,-0.0345231616327842,
0.0776876346420627));
#69749=CARTESIAN_POINT('Ctrl Pts',(0.003326396465438,-0.0344132092796988,
0.0777544319561883));
#69750=CARTESIAN_POINT('Ctrl Pts',(0.00337653691228175,-0.034303273855898,
0.0778202172345836));
#69751=CARTESIAN_POINT('Ctrl Pts',(0.00342799009848597,-0.034193496108874,
0.077884907844126));
#69752=CARTESIAN_POINT('Ctrl Pts',(0.00339045221434589,-0.0345231616327842,
0.0776982857777953));
#69753=CARTESIAN_POINT('Ctrl Pts',(0.00343936033820601,-0.0344132092796988,
0.077763528067557));
#69754=CARTESIAN_POINT('Ctrl Pts',(0.00348961542393308,-0.034303273855898,
0.0778277553651525));
#69755=CARTESIAN_POINT('Ctrl Pts',(0.00354115098125492,-0.034193496108874,
0.0778908870371748));
#69756=CARTESIAN_POINT('Ctrl Pts',(0.00350326927620343,-0.0345231616327842,
0.0777089369135279));
#69757=CARTESIAN_POINT('Ctrl Pts',(0.00355232421097402,-0.0344132092796988,
0.0777726241789256));
#69758=CARTESIAN_POINT('Ctrl Pts',(0.00360269393558442,-0.034303273855898,
0.0778352934957214));
#69759=CARTESIAN_POINT('Ctrl Pts',(0.00365431186402386,-0.034193496108874,
0.0778968662302236));
#69760=CARTESIAN_POINT('Ctrl Pts',(0.00361608633806097,-0.0345231616327842,
0.0777195880492606));
#69761=CARTESIAN_POINT('Ctrl Pts',(0.00366528808374204,-0.0344132092796988,
0.0777817202902942));
#69762=CARTESIAN_POINT('Ctrl Pts',(0.00371577244723576,-0.034303273855898,
0.0778428316262903));
#69763=CARTESIAN_POINT('Ctrl Pts',(0.00376747274679281,-0.034193496108874,
0.0779028454232725));
#69764=CARTESIAN_POINT('',(0.00359671891318807,-0.0341934961088839,0.0778938231347492));
#69765=CARTESIAN_POINT('Ctrl Pts',(0.00342002298478292,-0.0342105180195383,
0.0778748690246025));
#69766=CARTESIAN_POINT('Ctrl Pts',(0.00345371180452855,-0.0342610556241335,
0.0778481911196357));
#69767=CARTESIAN_POINT('Ctrl Pts',(0.00348679609582259,-0.0343122189870233,
0.07782199193588));
#69768=CARTESIAN_POINT('Ctrl Pts',(0.00355178462253462,-0.0344158119695144,
0.0777705280451103));
#69769=CARTESIAN_POINT('Ctrl Pts',(0.00358366227717941,-0.0344681990450042,
0.0777452843871966));
#69770=CARTESIAN_POINT('Ctrl Pts',(0.00361494791104364,-0.0345211942962462,
0.0777205095457699));
#69771=CARTESIAN_POINT('Ctrl Pts',(0.00369384830265547,-0.0346945769586932,
0.0778156470221916));
#69772=CARTESIAN_POINT('Ctrl Pts',(0.00376963296111065,-0.034529677707698,
0.0779072327708561));
#69773=CARTESIAN_POINT('Ctrl Pts',(0.00384913818567455,-0.034364806625142,
0.0779956080110687));
#69774=CARTESIAN_POINT('Ctrl Pts',(0.00369361438613664,-0.0346945769586932,
0.0778176611351202));
#69775=CARTESIAN_POINT('Ctrl Pts',(0.00376944068495148,-0.034529677707698,
0.0779092517198432));
#69776=CARTESIAN_POINT('Ctrl Pts',(0.00384898771417262,-0.034364806625142,
0.0779976300709476));
#69777=CARTESIAN_POINT('Ctrl Pts',(0.00365462984961993,-0.0346945769586932,
0.078153333277506));
#69778=CARTESIAN_POINT('Ctrl Pts',(0.00373739593246461,-0.034529677707698,
0.0782457298399369));
#69779=CARTESIAN_POINT('Ctrl Pts',(0.00382391012755614,-0.034364806625142,
0.0783346266524003));
#69780=CARTESIAN_POINT('',(0.0036631912365639,-0.0346775396664992,0.0781628703332946));
#69781=CARTESIAN_POINT('',(0.00365462984962341,-0.0346945769586885,0.078153333277498));
#69782=CARTESIAN_POINT('Origin',(0.0159026830614759,-0.0345626618374433,
0.0669464651399987));
#69783=CARTESIAN_POINT('Ctrl Pts',(0.00366319123623208,-0.0346775396670096,
0.0781628703314963));
#69784=CARTESIAN_POINT('Ctrl Pts',(0.0036951277090955,-0.0346269749928201,
0.0781341393846126));
#69785=CARTESIAN_POINT('Ctrl Pts',(0.00372649657555011,-0.0345757902890816,
0.0781059190240606));
#69786=CARTESIAN_POINT('Ctrl Pts',(0.00378812504502702,-0.0344721681087921,
0.0780504763626206));
#69787=CARTESIAN_POINT('Ctrl Pts',(0.0038183604905615,-0.034419771428953,
0.0780232758020536));
#69788=CARTESIAN_POINT('Ctrl Pts',(0.00384803921475855,-0.034366772783067,
0.0779965760079231));
#69789=CARTESIAN_POINT('',(0.0036741221178929,-0.0346945769587026,0.0779854972063226));
#69790=CARTESIAN_POINT('Origin',(0.00812378219310841,-0.0315241814719618,
0.07415));
#69791=CARTESIAN_POINT('',(0.00366319123793398,-0.0347116136489784,0.0781628703330552));
#69792=CARTESIAN_POINT('',(0.00367177297545972,-0.0346945769586885,0.0781723890818771));
#69793=CARTESIAN_POINT('Origin',(0.0158710147657852,-0.034562667817165,
0.0669140540721872));
#69794=CARTESIAN_POINT('Origin',(0.0161069622412668,-0.034562663129058,
0.0671735309468892));
#69795=CARTESIAN_POINT('Origin',(0.0161358505580842,-0.0345626691923073,
0.0672084428109901));
#69796=CARTESIAN_POINT('Ctrl Pts',(0.00374030229525091,-0.0352450361874067,
0.0778734213582005));
#69797=CARTESIAN_POINT('Ctrl Pts',(0.00388073343614336,-0.0349452760959492,
0.0780387470154162));
#69798=CARTESIAN_POINT('Ctrl Pts',(0.00403321863190598,-0.034644428984174,
0.0781930251517135));
#69799=CARTESIAN_POINT('Ctrl Pts',(0.00374197922941375,-0.0352450361874067,
0.0778753090861507));
#69800=CARTESIAN_POINT('Ctrl Pts',(0.00388248156713411,-0.0349452760959492,
0.0780405714967564));
#69801=CARTESIAN_POINT('Ctrl Pts',(0.00403503299346854,-0.034644428984174,
0.0781947812032845));
#69802=CARTESIAN_POINT('Ctrl Pts',(0.00390801231484276,-0.0352450361874067,
0.0780622128435846));
#69803=CARTESIAN_POINT('Ctrl Pts',(0.0040555638434466,-0.0349452760959492,
0.0782212132136182));
#69804=CARTESIAN_POINT('Ctrl Pts',(0.00421467275213715,-0.034644428984174,
0.0783686476954718));
#69805=CARTESIAN_POINT('Ctrl Pts',(0.00390967264569706,-0.0352450361874067,
0.078064081881159));
#69806=CARTESIAN_POINT('Ctrl Pts',(0.00405729466620972,-0.0349452760959492,
0.0782230196307868));
#69807=CARTESIAN_POINT('Ctrl Pts',(0.00421646914972384,-0.034644428984174,
0.0783703863603937));
#69808=CARTESIAN_POINT('',(0.00393262676926531,-0.0351951634053276,0.0780885744268352));
#69809=CARTESIAN_POINT('',(0.00409800492289777,-0.0348678972925388,0.0782574617917464));
#69810=CARTESIAN_POINT('Origin',(0.0155205695846266,-0.0345636767882058,
0.066000395172796));
#69811=CARTESIAN_POINT('Origin',(-0.00363654968017413,-0.0346946199341113,
0.0861489543183961));
#69812=CARTESIAN_POINT('',(0.0040096842883074,-0.0346945769330289,0.0781689953256754));
#69813=CARTESIAN_POINT('',(0.00405432007213583,-0.0346945769458128,0.0782127434443747));
#69814=CARTESIAN_POINT('',(0.00384803921487524,-0.0350221583435276,0.0779965760078401));
#69815=CARTESIAN_POINT('Origin',(0.0158916819271418,-0.0345628458718783,
0.0663060404294573));
#69816=CARTESIAN_POINT('',(0.00384895673138347,-0.035195136029876,0.0779957465163086));
#69817=CARTESIAN_POINT('Origin',(-0.00434289989842977,-0.0351951838366823,
0.085365368543244));
#69818=CARTESIAN_POINT('',(0.00393265065837624,-0.0351951371328748,0.0780885963819501));
#69819=CARTESIAN_POINT('Ctrl Pts',(0.00350932844780378,-0.0350241211494342,
0.0779849467574502));
#69820=CARTESIAN_POINT('Ctrl Pts',(0.00356215326699826,-0.0349144232818962,
0.078048508965792));
#69821=CARTESIAN_POINT('Ctrl Pts',(0.0036163235806588,-0.0348045283579412,
0.07811101729242));
#69822=CARTESIAN_POINT('Ctrl Pts',(0.00367177298290972,-0.0346945769439158,
0.0781723890901229));
#69823=CARTESIAN_POINT('Ctrl Pts',(0.0036225917068556,-0.0350241211494342,
0.0779884930163202));
#69824=CARTESIAN_POINT('Ctrl Pts',(0.00367546537431199,-0.0349144232818962,
0.0780504950697084));
#69825=CARTESIAN_POINT('Ctrl Pts',(0.00372965231595476,-0.0348045283579412,
0.0781114412978262));
#69826=CARTESIAN_POINT('Ctrl Pts',(0.00378508603015364,-0.0346945769439158,
0.0781712510535197));
#69827=CARTESIAN_POINT('Ctrl Pts',(0.00373585496590742,-0.0350241211494342,
0.0779920392751902));
#69828=CARTESIAN_POINT('Ctrl Pts',(0.00378877748162572,-0.0349144232818962,
0.0780524811736247));
#69829=CARTESIAN_POINT('Ctrl Pts',(0.00384298105125072,-0.0348045283579412,
0.0781118653032324));
#69830=CARTESIAN_POINT('Ctrl Pts',(0.00389839907739756,-0.0346945769439158,
0.0781701130169165));
#69831=CARTESIAN_POINT('Ctrl Pts',(0.00384911822495923,-0.0350241211494342,
0.0779955855340602));
#69832=CARTESIAN_POINT('Ctrl Pts',(0.00390208958893945,-0.0349144232818962,
0.078054467277541));
#69833=CARTESIAN_POINT('Ctrl Pts',(0.00395630978654668,-0.0348045283579412,
0.0781122893086386));
#69834=CARTESIAN_POINT('Ctrl Pts',(0.00401171212464148,-0.0346945769439158,
0.0781689749803132));
#69835=CARTESIAN_POINT('',(0.00384072863162498,-0.0346945769458128,0.0781706922036303));
#69836=CARTESIAN_POINT('Ctrl Pts',(0.00366319124037487,-0.0347116136492789,
0.0781628703308502));
#69837=CARTESIAN_POINT('Ctrl Pts',(0.00369511503917859,-0.0347621546532298,
0.0781341508032303));
#69838=CARTESIAN_POINT('Ctrl Pts',(0.00372647753133189,-0.0348133084097032,
0.0781059362425147));
#69839=CARTESIAN_POINT('Ctrl Pts',(0.00378810607647596,-0.0349168561544566,
0.0780504935079169));
#69840=CARTESIAN_POINT('Ctrl Pts',(0.00381834768455198,-0.0349692089015916,
0.0780232873253524));
#69841=CARTESIAN_POINT('Ctrl Pts',(0.00384803921491572,-0.0350221583435,
0.0779965760078304));
#69842=CARTESIAN_POINT('Ctrl Pts',(0.00393272785366326,-0.0351951371254888,
0.0780871354025537));
#69843=CARTESIAN_POINT('Ctrl Pts',(0.00401412565786805,-0.0350307338980928,
0.0781737828214646));
#69844=CARTESIAN_POINT('Ctrl Pts',(0.00409903513944573,-0.0348659306897824,
0.0782569919415866));
#69845=CARTESIAN_POINT('Ctrl Pts',(0.0039326506584598,-0.0351951371254888,
0.0780885963818693));
#69846=CARTESIAN_POINT('Ctrl Pts',(0.0040140786674953,-0.0350307338980928,
0.0781752453967426));
#69847=CARTESIAN_POINT('Ctrl Pts',(0.00409901839405667,-0.0348659306897824,
0.0782584548630651));
#69848=CARTESIAN_POINT('Ctrl Pts',(0.00391971266190752,-0.0351951371254888,
0.0783334580378068));
#69849=CARTESIAN_POINT('Ctrl Pts',(0.00400620303204808,-0.0350307338980928,
0.0784203745376411));
#69850=CARTESIAN_POINT('Ctrl Pts',(0.00409621184939875,-0.0348659306897825,
0.0785036420275136));
#69851=CARTESIAN_POINT('Origin',(0.000375438335953373,-0.0308609197411229,
0.0820555606426193));
#69852=CARTESIAN_POINT('',(0.00392700998367615,-0.0351951371254888,0.0781953505429598));
#69853=CARTESIAN_POINT('Origin',(0.00869940585763844,-0.035184046744121,
0.0733604412332708));
#69854=CARTESIAN_POINT('Origin',(0.000334508268153806,-0.0352322613438187,
0.0832326488377673));
#69855=CARTESIAN_POINT('',(0.00427040897049458,-0.0351951142564664,0.0784195818753924));
#69856=CARTESIAN_POINT('',(0.00436474671210107,-0.0351951372916787,0.0785011093128683));
#69857=CARTESIAN_POINT('Origin',(0.00845998783042524,-0.0352875122321978,
0.0742045170014701));
#69858=CARTESIAN_POINT('Origin',(0.00349033402313407,-0.0298325076522552,
0.0682486147103869));
#69859=CARTESIAN_POINT('Origin',(0.000660065224870908,-0.0338732569609108,
0.0779634230108649));
#69860=CARTESIAN_POINT('Ctrl Pts',(0.00249663926781917,-0.0321934096636942,
0.0753388642662976));
#69861=CARTESIAN_POINT('Ctrl Pts',(0.00251791937205675,-0.0320508460843224,
0.0754395874450527));
#69862=CARTESIAN_POINT('Ctrl Pts',(0.00254188966409757,-0.0319086045660874,
0.0755396629237864));
#69863=CARTESIAN_POINT('Ctrl Pts',(0.00256848079202786,-0.0317669892864618,
0.0756388794714287));
#69864=CARTESIAN_POINT('Ctrl Pts',(0.00251575093390584,-0.0321934096636942,
0.0754205048006375));
#69865=CARTESIAN_POINT('Ctrl Pts',(0.00253849236483141,-0.0320508460843224,
0.0755208858896705));
#69866=CARTESIAN_POINT('Ctrl Pts',(0.00256391369043927,-0.0319086045660874,
0.0756205802736542));
#69867=CARTESIAN_POINT('Ctrl Pts',(0.00259194250203898,-0.0317669892864618,
0.0757193777992968));
#69868=CARTESIAN_POINT('Ctrl Pts',(0.00253486259999249,-0.0321934096636942,
0.0755021453349773));
#69869=CARTESIAN_POINT('Ctrl Pts',(0.00255906535760608,-0.0320508460843224,
0.0756021843342883));
#69870=CARTESIAN_POINT('Ctrl Pts',(0.00258593771678096,-0.0319086045660874,
0.0757014976235219));
#69871=CARTESIAN_POINT('Ctrl Pts',(0.00261540421205009,-0.0317669892864618,
0.0757998761271649));
#69872=CARTESIAN_POINT('Ctrl Pts',(0.00255397426607915,-0.0321934096636942,
0.0755837858693173));
#69873=CARTESIAN_POINT('Ctrl Pts',(0.00257963835038075,-0.0320508460843224,
0.075683482778906));
#69874=CARTESIAN_POINT('Ctrl Pts',(0.00260796174312265,-0.0319086045660874,
0.0757824149733896));
#69875=CARTESIAN_POINT('Ctrl Pts',(0.0026388659220612,-0.0317669892864618,
0.075880374455033));
#69876=CARTESIAN_POINT('',(0.00255363235459846,-0.0321934096636942,0.0755823253040244));
#69877=CARTESIAN_POINT('',(0.00261718187036008,-0.0318665617511284,0.0758099632148273));
#69878=CARTESIAN_POINT('Origin',(0.0188791517298509,-0.0326371944422352,
0.0720192757713647));
#69879=CARTESIAN_POINT('Origin',(-0.00787753306643577,-0.0316939261509106,
0.0789735922318573));
#69880=CARTESIAN_POINT('',(0.00252392351269698,-0.0320197221621786,0.0754611719665832));
#69881=CARTESIAN_POINT('Ctrl Pts',(0.00252391834733507,-0.0320197392094706,
0.0754613568670933));
#69882=CARTESIAN_POINT('Ctrl Pts',(0.0025305909983687,-0.0319792716576002,
0.075489850763948));
#69883=CARTESIAN_POINT('Ctrl Pts',(0.00253751125185122,-0.0319386439829642,
0.0755184235062629));
#69884=CARTESIAN_POINT('Ctrl Pts',(0.00254469459260698,-0.0318979099381574,
0.0755471030991781));
#69885=CARTESIAN_POINT('Ctrl Pts',(0.00255187779137879,-0.0318571766984887,
0.0755757821252203));
#69886=CARTESIAN_POINT('Ctrl Pts',(0.00255928582901695,-0.0318163871833547,
0.0756044226649795));
#69887=CARTESIAN_POINT('Ctrl Pts',(0.00256688981595761,-0.0317755399638303,
0.0756329270885448));
#69888=CARTESIAN_POINT('',(0.00252514070879166,-0.0321934096636184,0.0754606157064861));
#69889=CARTESIAN_POINT('Origin',(0.000283209708318734,-0.0324111556700518,
0.0760070347756993));
#69890=CARTESIAN_POINT('',(0.00253938653170505,-0.0321934096636663,0.0755214705052652));
#69891=CARTESIAN_POINT('Ctrl Pts',(0.00255470187769009,-0.0321934096636618,
0.0755806019910128));
#69892=CARTESIAN_POINT('Ctrl Pts',(0.00257443099409214,-0.0320835708272592,
0.0756574039488498));
#69893=CARTESIAN_POINT('Ctrl Pts',(0.00259573807933072,-0.0319739230346488,
0.0757337530653914));
#69894=CARTESIAN_POINT('Ctrl Pts',(0.00261858837554064,-0.0318646057455573,
0.0758095537494409));
#69895=CARTESIAN_POINT('Ctrl Pts',(0.00249494653323593,-0.0321934096636618,
0.0756768852376034));
#69896=CARTESIAN_POINT('Ctrl Pts',(0.00251600347064723,-0.0320835708272592,
0.075754511268211));
#69897=CARTESIAN_POINT('Ctrl Pts',(0.00253865466084808,-0.0319739230346488,
0.0758316565003408));
#69898=CARTESIAN_POINT('Ctrl Pts',(0.00256286354811148,-0.0318646057455573,
0.0759082244562026));
#69899=CARTESIAN_POINT('Ctrl Pts',(0.00243519118878176,-0.0321934096636618,
0.0757731684841941));
#69900=CARTESIAN_POINT('Ctrl Pts',(0.00245757594720233,-0.0320835708272592,
0.0758516185875722));
#69901=CARTESIAN_POINT('Ctrl Pts',(0.00248157124236545,-0.0319739230346488,
0.0759295599352901));
#69902=CARTESIAN_POINT('Ctrl Pts',(0.00250713872068231,-0.0318646057455573,
0.0760068951629643));
#69903=CARTESIAN_POINT('Ctrl Pts',(0.0023754358443276,-0.0321934096636618,
0.0758694517307847));
#69904=CARTESIAN_POINT('Ctrl Pts',(0.00239914842375743,-0.0320835708272592,
0.0759487259069335));
#69905=CARTESIAN_POINT('Ctrl Pts',(0.00242448782388281,-0.0319739230346488,
0.0760274633702395));
#69906=CARTESIAN_POINT('Ctrl Pts',(0.00245141389325315,-0.0318646057455573,
0.076105565869726));
#69907=CARTESIAN_POINT('',(0.00237912173945756,-0.0321763980308272,0.075881726378492));
#69908=CARTESIAN_POINT('',(0.00237543584433933,-0.0321934096636185,0.0758694517308122));
#69909=CARTESIAN_POINT('Origin',(0.0183887770136759,-0.0326386230590182,
0.0716963916098026));
#69910=CARTESIAN_POINT('Ctrl Pts',(0.00237912174249056,-0.0321763980306293,
0.0758817263775713));
#69911=CARTESIAN_POINT('Ctrl Pts',(0.00242021415404723,-0.0321259596175519,
0.0758693390809465));
#69912=CARTESIAN_POINT('Ctrl Pts',(0.00246059458625344,-0.03207491646328,
0.075857166410302));
#69913=CARTESIAN_POINT('Ctrl Pts',(0.00253996398903856,-0.0319716057793918,
0.0758332405247676));
#69914=CARTESIAN_POINT('Ctrl Pts',(0.00257892203447221,-0.0319193786690113,
0.0758214966322547));
#69915=CARTESIAN_POINT('Ctrl Pts',(0.00261718187213179,-0.0318665617525305,
0.075809963214284));
#69916=CARTESIAN_POINT('',(0.0024645340994789,-0.0321934096636664,0.0757258885174283));
#69917=CARTESIAN_POINT('Origin',(0.00812378219310841,-0.0315241814719618,
0.07415));
#69918=CARTESIAN_POINT('',(0.00237912173910149,-0.0322104233323771,0.0758817263785991));
#69919=CARTESIAN_POINT('',(0.002382833841471,-0.0321934096636183,0.0758939931260947));
#69920=CARTESIAN_POINT('Origin',(0.0183818702993081,-0.0326387227710374,
0.0716515854926586));
#69921=CARTESIAN_POINT('Origin',(0.018034639889298,-0.0326386247628077,
0.0705216006089351));
#69922=CARTESIAN_POINT('Origin',(0.0180536409609535,-0.032638723939034,
0.070562761627751));
#69923=CARTESIAN_POINT('Ctrl Pts',(0.00257283702668973,-0.0327445246967098,
0.0756550358000437));
#69924=CARTESIAN_POINT('Ctrl Pts',(0.00262960037984349,-0.032443687833936,
0.0758643931195237));
#69925=CARTESIAN_POINT('Ctrl Pts',(0.00270197212326312,-0.0321434074405926,
0.0760688800292161));
#69926=CARTESIAN_POINT('Ctrl Pts',(0.00264348661759046,-0.0327445246967098,
0.0758948453813902));
#69927=CARTESIAN_POINT('Ctrl Pts',(0.00270929453696334,-0.032443687833936,
0.0761015381079892));
#69928=CARTESIAN_POINT('Ctrl Pts',(0.00279048444391856,-0.0321434074405926,
0.0763026867209342));
#69929=CARTESIAN_POINT('',(0.0026545602228832,-0.0326943950436612,0.0759292515393858));
#69930=CARTESIAN_POINT('',(0.00273227783999863,-0.0323666188837389,0.0761524499520336));
#69931=CARTESIAN_POINT('Origin',(0.0186171608058684,-0.0326395579111834,
0.0706563547216975));
#69932=CARTESIAN_POINT('Origin',(-0.00762128491708506,-0.0321933825603066,
0.0799978511097441));
#69933=CARTESIAN_POINT('',(0.00269003013365542,-0.0321934096532689,0.0760347980138639));
#69934=CARTESIAN_POINT('',(0.00271179075332963,-0.0321934096584274,0.0760933874820075));
#69935=CARTESIAN_POINT('',(0.00261718186944653,-0.0325210109756239,0.0758099632150888));
#69936=CARTESIAN_POINT('Origin',(0.0187415690246258,-0.0326393129157209,
0.0711207974251109));
#69937=CARTESIAN_POINT('',(0.00261848258998651,-0.0326943950436594,0.0758095711132296));
#69938=CARTESIAN_POINT('Origin',(-0.00797319251360476,-0.0326943765538147,
0.079002428014876));
#69939=CARTESIAN_POINT('',(0.00263652140644485,-0.0326943950436703,0.0758694113263177));
#69940=CARTESIAN_POINT('Ctrl Pts',(0.00231565842030428,-0.0325229783203769,
0.0756552236510969));
#69941=CARTESIAN_POINT('Ctrl Pts',(0.00233640789541759,-0.032413025309245,
0.0757352885102898));
#69942=CARTESIAN_POINT('Ctrl Pts',(0.00235881046792943,-0.0323031222208069,
0.0758149119965307));
#69943=CARTESIAN_POINT('Ctrl Pts',(0.0023828338427744,-0.0321934096576658,
0.0758939931303853));
#69944=CARTESIAN_POINT('Ctrl Pts',(0.0024166321497558,-0.0325229783203769,
0.075706657571782));
#69945=CARTESIAN_POINT('Ctrl Pts',(0.00243809064034096,-0.032413025309245,
0.0757853305103225));
#69946=CARTESIAN_POINT('Ctrl Pts',(0.00246117332712184,-0.0323031222208069,
0.0758635476201272));
#69947=CARTESIAN_POINT('Ctrl Pts',(0.00248584710742285,-0.0321934096576658,
0.0759412097539712));
#69948=CARTESIAN_POINT('Ctrl Pts',(0.00251760587920732,-0.0325229783203769,
0.075758091492467));
#69949=CARTESIAN_POINT('Ctrl Pts',(0.00253977338526434,-0.032413025309245,
0.0758353725103551));
#69950=CARTESIAN_POINT('Ctrl Pts',(0.00256353618631424,-0.0323031222208069,
0.0759121832437238));
#69951=CARTESIAN_POINT('Ctrl Pts',(0.0025888603720713,-0.0321934096576658,
0.0759884263775571));
#69952=CARTESIAN_POINT('Ctrl Pts',(0.00261857960865884,-0.0325229783203769,
0.075809525413152));
#69953=CARTESIAN_POINT('Ctrl Pts',(0.00264145613018772,-0.032413025309245,
0.0758854145103878));
#69954=CARTESIAN_POINT('Ctrl Pts',(0.00266589904550664,-0.0323031222208069,
0.0759608188673203));
#69955=CARTESIAN_POINT('Ctrl Pts',(0.00269187363671976,-0.0321934096576658,
0.0760356430011429));
#69956=CARTESIAN_POINT('',(0.00253643198727375,-0.0321934096584275,0.0759643955695672));
#69957=CARTESIAN_POINT('Ctrl Pts',(0.00237912174242734,-0.032210423332892,
0.0758817263775903));
#69958=CARTESIAN_POINT('Ctrl Pts',(0.00242026983492637,-0.032260942183143,
0.0758693222959601));
#69959=CARTESIAN_POINT('Ctrl Pts',(0.00246067746822554,-0.0323120888240864,
0.0758571414255604));
#69960=CARTESIAN_POINT('Ctrl Pts',(0.00254004747182089,-0.0324156524631809,
0.0758332153589119));
#69961=CARTESIAN_POINT('Ctrl Pts',(0.00257897721690126,-0.0324680267167309,
0.0758214799975259));
#69962=CARTESIAN_POINT('Ctrl Pts',(0.00261718186948933,-0.0325210109755912,
0.0758099632150805));
#69963=CARTESIAN_POINT('Origin',(0.00677672056911715,-0.0262834582511889,
0.0663983027135962));
#69964=CARTESIAN_POINT('Origin',(-0.00385709242765191,-0.0342770814131407,
0.0720806704906369));
#69965=CARTESIAN_POINT('Ctrl Pts',(0.0026555191950499,-0.0326943950436605,
0.0759274649047795));
#69966=CARTESIAN_POINT('Ctrl Pts',(0.00268001599276205,-0.0325844576448134,
0.0760028278175099));
#69967=CARTESIAN_POINT('Ctrl Pts',(0.00270607315274507,-0.0324744968375323,
0.076077689429851));
#69968=CARTESIAN_POINT('Ctrl Pts',(0.00273365596606139,-0.0323646534831895,
0.0761519542852319));
#69969=CARTESIAN_POINT('Ctrl Pts',(0.00260192751678469,-0.0326943950436605,
0.0760273100829432));
#69970=CARTESIAN_POINT('Ctrl Pts',(0.00262780036818173,-0.0325844576448134,
0.0761034115894416));
#69971=CARTESIAN_POINT('Ctrl Pts',(0.00265524895456519,-0.0324744968375323,
0.0761789833887758));
#69972=CARTESIAN_POINT('Ctrl Pts',(0.00268423677167008,-0.0323646534831895,
0.076253929139032));
#69973=CARTESIAN_POINT('Ctrl Pts',(0.00254833583851947,-0.0326943950436605,
0.0761271552611068));
#69974=CARTESIAN_POINT('Ctrl Pts',(0.00257558474360142,-0.0325844576448134,
0.0762039953613732));
#69975=CARTESIAN_POINT('Ctrl Pts',(0.0026044247563853,-0.0324744968375323,
0.0762802773477006));
#69976=CARTESIAN_POINT('Ctrl Pts',(0.00263481757727878,-0.0323646534831895,
0.0763559039928319));
#69977=CARTESIAN_POINT('Ctrl Pts',(0.00249474416025426,-0.0326943950436605,
0.0762270004392705));
#69978=CARTESIAN_POINT('Ctrl Pts',(0.00252336911902111,-0.0325844576448134,
0.0763045791333049));
#69979=CARTESIAN_POINT('Ctrl Pts',(0.00255360055820541,-0.0324744968375323,
0.0763815713066255));
#69980=CARTESIAN_POINT('Ctrl Pts',(0.00258539838288748,-0.0323646534831895,
0.0764578788466319));
#69981=CARTESIAN_POINT('',(0.00249919351341637,-0.0326773559991168,0.076239019426535));
#69982=CARTESIAN_POINT('',(0.00249474416025706,-0.0326943950436595,0.0762270004392665));
#69983=CARTESIAN_POINT('Origin',(0.0180478846633527,-0.0326395669977758,
0.0704105109512779));
#69984=CARTESIAN_POINT('Ctrl Pts',(0.00249919351655316,-0.0326773559987442,
0.0762390194253633));
#69985=CARTESIAN_POINT('Ctrl Pts',(0.00253945941403874,-0.0326267922586696,
0.076224064333202));
#69986=CARTESIAN_POINT('Ctrl Pts',(0.00257901162757038,-0.0325756109580818,
0.0762093743092491));
#69987=CARTESIAN_POINT('Ctrl Pts',(0.00265672234782972,-0.0324719985462368,
0.0761805118957437));
#69988=CARTESIAN_POINT('Ctrl Pts',(0.00269484968674601,-0.0324196091621767,
0.0761663510821778));
#69989=CARTESIAN_POINT('Ctrl Pts',(0.00273227784004436,-0.0323666188837757,
0.0761524499520166));
#69990=CARTESIAN_POINT('',(0.00257465219158013,-0.0326943950436703,0.0760781259893362));
#69991=CARTESIAN_POINT('Origin',(0.00812378219310841,-0.0315241814719618,
0.07415));
#69992=CARTESIAN_POINT('',(0.00249919351345739,-0.032711433837986,0.0762390194265195));
#69993=CARTESIAN_POINT('',(0.00250366852609158,-0.0326943950436593,0.0762510288836281));
#69994=CARTESIAN_POINT('Origin',(0.0180313865054977,-0.0326395661194546,
0.0703683094605398));
#69995=CARTESIAN_POINT('Origin',(0.0180828715748333,-0.0326395682947654,
0.0705047029332642));
#69996=CARTESIAN_POINT('Origin',(0.0180979155018327,-0.0326395673551978,
0.0705474446243651));
#69997=CARTESIAN_POINT('Ctrl Pts',(0.00267830514990377,-0.0332451089994434,
0.0760006498242324));
#69998=CARTESIAN_POINT('Ctrl Pts',(0.00274810354998636,-0.0329451141710254,
0.0762060293511019));
#69999=CARTESIAN_POINT('Ctrl Pts',(0.00283317368574278,-0.0326442513127492,
0.0764055679155792));
#70000=CARTESIAN_POINT('Ctrl Pts',(0.00276387470017103,-0.0332451089994434,
0.0762355494880615));
#70001=CARTESIAN_POINT('Ctrl Pts',(0.00284253248602208,-0.0329451141710254,
0.0764377017065412));
#70002=CARTESIAN_POINT('Ctrl Pts',(0.00293619374490576,-0.0326442513127492,
0.0766333548059177));
#70003=CARTESIAN_POINT('Ctrl Pts',(0.0027647303956737,-0.0332451089994434,
0.0762378984846998));
#70004=CARTESIAN_POINT('Ctrl Pts',(0.00284347677538243,-0.0329451141710254,
0.0764400184300957));
#70005=CARTESIAN_POINT('Ctrl Pts',(0.00293722394549739,-0.0326442513127492,
0.076635632674821));
#70006=CARTESIAN_POINT('',(0.00277707261164815,-0.0331951640388616,0.0762691558818365));
#70007=CARTESIAN_POINT('',(0.00286865161520751,-0.0328677532355005,0.0764870339490556));
#70008=CARTESIAN_POINT('Origin',(0.0180622871415354,-0.0326402808284701,
0.0693847921303757));
#70009=CARTESIAN_POINT('Origin',(-0.00723325094578848,-0.0326944278779115,
0.0809799113798173));
#70010=CARTESIAN_POINT('',(0.00281909985087197,-0.0326943950436593,0.0763722669164541));
#70011=CARTESIAN_POINT('',(0.00284449639327671,-0.0326943950436692,0.0764293744083929));
#70012=CARTESIAN_POINT('',(0.00273227783999764,-0.0330220786163545,0.0761524499520309));
#70013=CARTESIAN_POINT('Origin',(0.0182859405234867,-0.0326396682762467,
0.0698103879589332));
#70014=CARTESIAN_POINT('',(0.00273355137358273,-0.0331951640388588,0.0761519769509752));
#70015=CARTESIAN_POINT('Origin',(-0.00760786748069256,-0.0331952026560122,
0.0799928656019648));
#70016=CARTESIAN_POINT('',(0.00275531199262544,-0.0331951640388701,0.0762105664164158));
#70017=CARTESIAN_POINT('Ctrl Pts',(0.00242163349987949,-0.0330240426238172,
0.0760169494584312));
#70018=CARTESIAN_POINT('Ctrl Pts',(0.00244735254755011,-0.0329142774063519,
0.0760955021120148));
#70019=CARTESIAN_POINT('Ctrl Pts',(0.00247470831987959,-0.032804347972669,
0.076173562242403));
#70020=CARTESIAN_POINT('Ctrl Pts',(0.00250366852609159,-0.0326943950436592,
0.0762510288836281));
#70021=CARTESIAN_POINT('Ctrl Pts',(0.00252563752523012,-0.0330240426238172,
0.0760619416654831));
#70022=CARTESIAN_POINT('Ctrl Pts',(0.00255197638438667,-0.0329142774063519,
0.0761390615622913));
#70023=CARTESIAN_POINT('Ctrl Pts',(0.00257992265811595,-0.032804347972669,
0.0762156754083878));
#70024=CARTESIAN_POINT('Ctrl Pts',(0.00260944324813962,-0.0326943950436592,
0.0762916840697697));
#70025=CARTESIAN_POINT('Ctrl Pts',(0.00262964155058076,-0.0330240426238172,
0.0761069338725351));
#70026=CARTESIAN_POINT('Ctrl Pts',(0.00265660022122323,-0.0329142774063519,
0.0761826210125678));
#70027=CARTESIAN_POINT('Ctrl Pts',(0.0026851369963523,-0.032804347972669,
0.0762577885743726));
#70028=CARTESIAN_POINT('Ctrl Pts',(0.00271521797018765,-0.0326943950436592,
0.0763323392559112));
#70029=CARTESIAN_POINT('Ctrl Pts',(0.00273364557593139,-0.0330240426238172,
0.076151926079587));
#70030=CARTESIAN_POINT('Ctrl Pts',(0.00276122405805979,-0.0329142774063519,
0.0762261804628443));
#70031=CARTESIAN_POINT('Ctrl Pts',(0.00279035133458866,-0.032804347972669,
0.0762999017403575));
#70032=CARTESIAN_POINT('Ctrl Pts',(0.00282099269223568,-0.0326943950436592,
0.0763729944420527));
#70033=CARTESIAN_POINT('',(0.00266138418849177,-0.0326943950436693,0.0763116479000511));
#70034=CARTESIAN_POINT('Ctrl Pts',(0.00249919351656075,-0.0327114338383317,
0.0762390194253603));
#70035=CARTESIAN_POINT('Ctrl Pts',(0.00253945271657824,-0.0327619876831137,
0.0762240668206949));
#70036=CARTESIAN_POINT('Ctrl Pts',(0.0025790016587862,-0.0328131562604681,
0.076209378011739));
#70037=CARTESIAN_POINT('Ctrl Pts',(0.00265671230754119,-0.0329167375858765,
0.0761805156247909));
#70038=CARTESIAN_POINT('Ctrl Pts',(0.0026948430502022,-0.0329691088920619,
0.0761663535470457));
#70039=CARTESIAN_POINT('Ctrl Pts',(0.00273227784004319,-0.0330220786163186,
0.0761524499520169));
#70040=CARTESIAN_POINT('Ctrl Pts',(0.00277791764267319,-0.0331951640388604,
0.0762673122641001));
#70041=CARTESIAN_POINT('Ctrl Pts',(0.00282169171623913,-0.0330306422010619,
0.0763778345862308));
#70042=CARTESIAN_POINT('Ctrl Pts',(0.00286999638896757,-0.0328657861914645,
0.0764864532393173));
#70043=CARTESIAN_POINT('Ctrl Pts',(0.00277707261164708,-0.0331951640388604,
0.0762691558818335));
#70044=CARTESIAN_POINT('Ctrl Pts',(0.00282088480082764,-0.0330306422010619,
0.0763796956744389));
#70045=CARTESIAN_POINT('Ctrl Pts',(0.00286922827867427,-0.0328657861914645,
0.0764883302077133));
#70046=CARTESIAN_POINT('Ctrl Pts',(0.00263626771762459,-0.0331951640388604,
0.0765763521758829));
#70047=CARTESIAN_POINT('Ctrl Pts',(0.00268643099322868,-0.0330306422010619,
0.0766898030193965));
#70048=CARTESIAN_POINT('Ctrl Pts',(0.00274124044733536,-0.0328657861914645,
0.0768010836190257));
#70049=CARTESIAN_POINT('',(0.00264146296800414,-0.0331781648281909,0.0765880680691641));
#70050=CARTESIAN_POINT('',(0.00263626771762763,-0.0331951640388588,0.0765763521758782));
#70051=CARTESIAN_POINT('Origin',(0.0174347589091698,-0.0326412092064642,
0.0692297478366806));
#70052=CARTESIAN_POINT('Ctrl Pts',(0.00264146296835899,-0.033178164828644,
0.0765880680673543));
#70053=CARTESIAN_POINT('Ctrl Pts',(0.00268073738764738,-0.0331276811546776,
0.0765706021416561));
#70054=CARTESIAN_POINT('Ctrl Pts',(0.00271930261880876,-0.0330765663497784,
0.0765534515655876));
#70055=CARTESIAN_POINT('Ctrl Pts',(0.00279504790506716,-0.0329730614463218,
0.0765197665255157));
#70056=CARTESIAN_POINT('Ctrl Pts',(0.00283219736290148,-0.0329207133373851,
0.0765032456744304));
#70057=CARTESIAN_POINT('Ctrl Pts',(0.00286865160156484,-0.0328677532289363,
0.0764870339398219));
#70058=CARTESIAN_POINT('',(0.00270667016464789,-0.0331951640388702,0.0764227540288673));
#70059=CARTESIAN_POINT('Origin',(0.00812378219310841,-0.0315241814719618,
0.07415));
#70060=CARTESIAN_POINT('',(0.0026414629696845,-0.0332121607144215,0.0765880680691276));
#70061=CARTESIAN_POINT('',(0.00264668323176962,-0.0331951640388587,0.0765997728400264));
#70062=CARTESIAN_POINT('Origin',(0.0174094462810411,-0.0326413640761601,
0.0691921232523155));
#70063=CARTESIAN_POINT('Origin',(0.0180136125105183,-0.0326412103205533,
0.0705313689848069));
#70064=CARTESIAN_POINT('Origin',(0.0180245920194116,-0.0326413657162226,
0.0705753669552167));
#70065=CARTESIAN_POINT('Ctrl Pts',(0.00280524589058206,-0.0337436976235975,
0.076338903058317));
#70066=CARTESIAN_POINT('Ctrl Pts',(0.00282493321642591,-0.0336723290703325,
0.0763867387798682));
#70067=CARTESIAN_POINT('Ctrl Pts',(0.00284547777117999,-0.033601104548885,
0.0764342126497879));
#70068=CARTESIAN_POINT('Ctrl Pts',(0.00291107246486281,-0.0333736987606857,
0.0765857873123978));
#70069=CARTESIAN_POINT('Ctrl Pts',(0.00298525729179216,-0.0331450831799191,
0.0767333479902159));
#70070=CARTESIAN_POINT('Ctrl Pts',(0.00290539523114428,-0.0337436976235975,
0.0765679666075451));
#70071=CARTESIAN_POINT('Ctrl Pts',(0.00292714278926541,-0.0336723290703325,
0.0766149015707493));
#70072=CARTESIAN_POINT('Ctrl Pts',(0.00294973104119621,-0.033601104548885,
0.0766614377709584));
#70073=CARTESIAN_POINT('Ctrl Pts',(0.00302185085513068,-0.0333736987606857,
0.0768100186399245));
#70074=CARTESIAN_POINT('Ctrl Pts',(0.00310237824828838,-0.0331450831799191,
0.0769542160086103));
#70075=CARTESIAN_POINT('Ctrl Pts',(0.00290639672454991,-0.0337436976235975,
0.0765702572430374));
#70076=CARTESIAN_POINT('Ctrl Pts',(0.0029281648849938,-0.0336723290703325,
0.076617183198658));
#70077=CARTESIAN_POINT('Ctrl Pts',(0.00295077357389638,-0.033601104548885,
0.0766637100221701));
#70078=CARTESIAN_POINT('Ctrl Pts',(0.00302295863903336,-0.0333736987606857,
0.0768122609531998));
#70079=CARTESIAN_POINT('Ctrl Pts',(0.00310354945785334,-0.0331450831799191,
0.0769564246887942));
#70080=CARTESIAN_POINT('',(0.00292068602045762,-0.0336938721132548,0.0766006968841836));
#70081=CARTESIAN_POINT('',(0.00302576499310969,-0.0333679869945434,0.0768123947168798));
#70082=CARTESIAN_POINT('Ctrl Pts',(0.00292068602046224,-0.0336938721132647,
0.0766006968841961));
#70083=CARTESIAN_POINT('Ctrl Pts',(0.00293025224004404,-0.0336629187933931,
0.0766210070093736));
#70084=CARTESIAN_POINT('Ctrl Pts',(0.00293993432406981,-0.0336319952301038,
0.0766412546248275));
#70085=CARTESIAN_POINT('Ctrl Pts',(0.00294973104120162,-0.0336011045488948,
0.0766614377709706));
#70086=CARTESIAN_POINT('Ctrl Pts',(0.00297431435673327,-0.0335235892595452,
0.0767120841909275));
#70087=CARTESIAN_POINT('Ctrl Pts',(0.0029996633102178,-0.0334458668660368,
0.0767624145892694));
#70088=CARTESIAN_POINT('Ctrl Pts',(0.0030257649928217,-0.0333679869945383,
0.0768123947170223));
#70089=CARTESIAN_POINT('Ctrl Pts',(0.0030257849695321,-0.0333679692460369,
0.0768124344536474));
#70090=CARTESIAN_POINT('Ctrl Pts',(0.00302618395529592,-0.033339189537351,
0.0768122193997352));
#70091=CARTESIAN_POINT('Ctrl Pts',(0.00302648147390406,-0.0333104081057743,
0.0768120553479233));
#70092=CARTESIAN_POINT('Ctrl Pts',(0.00302687261701995,-0.033253269724522,
0.0768118333469244));
#70093=CARTESIAN_POINT('Ctrl Pts',(0.00302696921424088,-0.0332249166372877,
0.0768117738464262));
#70094=CARTESIAN_POINT('Ctrl Pts',(0.0030269692753617,-0.0331960985564874,
0.0768117660347441));
#70095=CARTESIAN_POINT('Ctrl Pts',(0.00302696924986029,-0.0331956312358587,
0.0768117659216277));
#70096=CARTESIAN_POINT('Ctrl Pts',(0.00302696919836504,-0.0331951640388587,
0.0768117658230233));
#70097=CARTESIAN_POINT('',(0.00296910472395193,-0.0331951640388587,0.07670096554053));
#70098=CARTESIAN_POINT('',(0.00299803696116874,-0.0331951640388687,0.0767563656817873));
#70099=CARTESIAN_POINT('',(0.00286865161539024,-0.0335216366567711,0.0764870339335403));
#70100=CARTESIAN_POINT('Origin',(0.0175538040129587,-0.0326434571528625,
0.0686310194173281));
#70101=CARTESIAN_POINT('',(0.00286989293566143,-0.0336938721132327,0.0764864819003116));
#70102=CARTESIAN_POINT('Origin',(-0.00710844836118518,-0.0336938867896263,
0.0809239963976862));
#70103=CARTESIAN_POINT('',(0.00289528947806953,-0.0336938721132538,0.0765435893922577));
#70104=CARTESIAN_POINT('Ctrl Pts',(0.00255011247002711,-0.0335235895815172,
0.0763713072317981));
#70105=CARTESIAN_POINT('Ctrl Pts',(0.0025806931374243,-0.0334144449262749,
0.0764480397690822));
#70106=CARTESIAN_POINT('Ctrl Pts',(0.00261289417477601,-0.0333049234473147,
0.0765242286891813));
#70107=CARTESIAN_POINT('Ctrl Pts',(0.00264668323176944,-0.0331951640388587,
0.0765997728400264));
#70108=CARTESIAN_POINT('Ctrl Pts',(0.00265673650893439,-0.0335235895815172,
0.0764096802276814));
#70109=CARTESIAN_POINT('Ctrl Pts',(0.00268784545616939,-0.0334144449262749,
0.0764849448751466));
#70110=CARTESIAN_POINT('Ctrl Pts',(0.00272054505478949,-0.0333049234473147,
0.0765596533051353));
#70111=CARTESIAN_POINT('Ctrl Pts',(0.00275480214549061,-0.0331951640388587,
0.0766337062009227));
#70112=CARTESIAN_POINT('Ctrl Pts',(0.00276336054784166,-0.0335235895815172,
0.0764480532235648));
#70113=CARTESIAN_POINT('Ctrl Pts',(0.00279499777491448,-0.0334144449262749,
0.0765218499812109));
#70114=CARTESIAN_POINT('Ctrl Pts',(0.00282819593480297,-0.0333049234473147,
0.0765950779210892));
#70115=CARTESIAN_POINT('Ctrl Pts',(0.00286292105921177,-0.0331951640388587,
0.076667639561819));
#70116=CARTESIAN_POINT('Ctrl Pts',(0.00286998458674894,-0.0335235895815172,
0.0764864262194482));
#70117=CARTESIAN_POINT('Ctrl Pts',(0.00290215009365957,-0.0334144449262749,
0.0765587550872753));
#70118=CARTESIAN_POINT('Ctrl Pts',(0.00293584681481645,-0.0333049234473147,
0.0766305025370432));
#70119=CARTESIAN_POINT('Ctrl Pts',(0.00297103997293294,-0.0331951640388587,
0.0767015729227154));
#70120=CARTESIAN_POINT('',(0.00280789397787078,-0.0331951640388687,0.0766503691902882));
#70121=CARTESIAN_POINT('Ctrl Pts',(0.00264146297254081,-0.0332121607145971,
0.0765880680678471));
#70122=CARTESIAN_POINT('Ctrl Pts',(0.00268067132715015,-0.0332625444110019,
0.0765706315353287));
#70123=CARTESIAN_POINT('Ctrl Pts',(0.0027192040602785,-0.0333135300747347,
0.0765534954616293));
#70124=CARTESIAN_POINT('Ctrl Pts',(0.0027949488702927,-0.0334167203140606,
0.0765198106295043));
#70125=CARTESIAN_POINT('Ctrl Pts',(0.00283213161064489,-0.0334688847587302,
0.076503274917467));
#70126=CARTESIAN_POINT('Ctrl Pts',(0.0028686516160965,-0.033521636656238,
0.0764870339333968));
#70127=CARTESIAN_POINT('Ctrl Pts',(0.00292104473773195,-0.033693872113239,
0.0765997635906665));
#70128=CARTESIAN_POINT('Ctrl Pts',(0.00293538401694588,-0.0336474569764958,
0.0766302169394442));
#70129=CARTESIAN_POINT('Ctrl Pts',(0.00295007880852096,-0.033601104548885,
0.076660500342171));
#70130=CARTESIAN_POINT('Ctrl Pts',(0.00298728264224462,-0.0334837508592656,
0.0767371709552845));
#70131=CARTESIAN_POINT('Ctrl Pts',(0.00302674204801737,-0.0333660264659097,
0.0768127054735856));
#70132=CARTESIAN_POINT('Ctrl Pts',(0.0029206860204489,-0.033693872113239,
0.0766006968841651));
#70133=CARTESIAN_POINT('Ctrl Pts',(0.00293503076253938,-0.0336474569764958,
0.076631152332634));
#70134=CARTESIAN_POINT('Ctrl Pts',(0.00294973104119621,-0.033601104548885,
0.0766614377709584));
#70135=CARTESIAN_POINT('Ctrl Pts',(0.00298694876694935,-0.0334837508592656,
0.0767381135377368));
#70136=CARTESIAN_POINT('Ctrl Pts',(0.00302642221136499,-0.0333660264659097,
0.0768136527957902));
#70137=CARTESIAN_POINT('Ctrl Pts',(0.00279872055942052,-0.033693872113239,
0.0769180207969077));
#70138=CARTESIAN_POINT('Ctrl Pts',(0.00281492270367152,-0.0336474569764958,
0.0769491901496925));
#70139=CARTESIAN_POINT('Ctrl Pts',(0.00283148861436989,-0.033601104548885,
0.0769801677001781));
#70140=CARTESIAN_POINT('Ctrl Pts',(0.00287342969151647,-0.0334837508592656,
0.0770585957358222));
#70141=CARTESIAN_POINT('Ctrl Pts',(0.00291767633653727,-0.0333660264659097,
0.0771357465305788));
#70142=CARTESIAN_POINT('',(0.00280536863337681,-0.0336769361243753,0.0769274947718516));
#70143=CARTESIAN_POINT('',(0.00279944798762601,-0.0336938721132327,0.0769161282089466));
#70144=CARTESIAN_POINT('Ctrl Pts',(0.00280536863337695,-0.033676936124375,
0.0769274947718519));
#70145=CARTESIAN_POINT('Ctrl Pts',(0.00280437976177307,-0.0336797586669909,
0.0769256012568036));
#70146=CARTESIAN_POINT('Ctrl Pts',(0.00280339193879104,-0.0336825812712615,
0.0769237072852676));
#70147=CARTESIAN_POINT('Ctrl Pts',(0.00280141839210353,-0.0336882265959168,
0.076919918434235));
#70148=CARTESIAN_POINT('Ctrl Pts',(0.00280043266840231,-0.0336910493162576,
0.0769180235547777));
#70149=CARTESIAN_POINT('Ctrl Pts',(0.00279944798762285,-0.0336938721132349,
0.0769161282089515));
#70150=CARTESIAN_POINT('Ctrl Pts',(0.00280536863337684,-0.0336769361243753,
0.0769274947718516));
#70151=CARTESIAN_POINT('Ctrl Pts',(0.0028425210803906,-0.0336279007516201,
0.0769080922326953));
#70152=CARTESIAN_POINT('Ctrl Pts',(0.00288020252032072,-0.0335767878632067,
0.0768884134316338));
#70153=CARTESIAN_POINT('Ctrl Pts',(0.00295404756158169,-0.033473319885732,
0.0768498485073897));
#70154=CARTESIAN_POINT('Ctrl Pts',(0.00299025512618674,-0.0334209645014077,
0.0768309394247733));
#70155=CARTESIAN_POINT('Ctrl Pts',(0.00302576498972625,-0.0333679869844681,
0.0768123947104102));
#70156=CARTESIAN_POINT('',(0.00286006700405182,-0.0336938721132538,0.0767584125465751));
#70157=CARTESIAN_POINT('Origin',(0.00812378219310841,-0.0315241814719618,
0.07415));
#70158=CARTESIAN_POINT('',(0.00280536863453025,-0.0337108120655389,0.0769274947712568));
#70159=CARTESIAN_POINT('',(0.00281131354479959,-0.0336938721132327,0.07693884866222));
#70160=CARTESIAN_POINT('Origin',(0.0178253440299299,-0.0345562511534441,
0.0703442768603358));
#70161=CARTESIAN_POINT('Ctrl Pts',(0.00281131354480541,-0.0336938721132305,
0.0769388486622202));
#70162=CARTESIAN_POINT('Ctrl Pts',(0.002810320782198,-0.0336910493337498,
0.076936957551993));
#70163=CARTESIAN_POINT('Ctrl Pts',(0.00280932898901947,-0.0336882266046629,
0.0769350658347944));
#70164=CARTESIAN_POINT('Ctrl Pts',(0.00280734735042096,-0.033682581271302,
0.0769312812022592));
#70165=CARTESIAN_POINT('Ctrl Pts',(0.00280635750498768,-0.0336797586670112,
0.0769293882869132));
#70166=CARTESIAN_POINT('Ctrl Pts',(0.00280536863337669,-0.033676936124375,
0.0769274947718514));
#70167=CARTESIAN_POINT('Origin',(0.0167906271279013,-0.0345562514784053,
0.0683629835414773));
#70168=CARTESIAN_POINT('Ctrl Pts',(0.00295316055523882,-0.034243627687391,
0.0766684909922402));
#70169=CARTESIAN_POINT('Ctrl Pts',(0.00304814700888272,-0.0339430054201809,
0.076863504202146));
#70170=CARTESIAN_POINT('Ctrl Pts',(0.00315755280998154,-0.0336441434784052,
0.0770508086310832));
#70171=CARTESIAN_POINT('Ctrl Pts',(0.00306749329711971,-0.034243627687391,
0.0768908151342806));
#70172=CARTESIAN_POINT('Ctrl Pts',(0.00317086484401067,-0.0339430054201809,
0.07708151621374));
#70173=CARTESIAN_POINT('Ctrl Pts',(0.00328830710985207,-0.0336441434784052,
0.0772638891629611));
#70174=CARTESIAN_POINT('Ctrl Pts',(0.00306863662453852,-0.034243627687391,
0.076893038375701));
#70175=CARTESIAN_POINT('Ctrl Pts',(0.00317209202236195,-0.0339430054201809,
0.0770836963338559));
#70176=CARTESIAN_POINT('Ctrl Pts',(0.00328961465285077,-0.0336441434784052,
0.0772660199682799));
#70177=CARTESIAN_POINT('',(0.00308483367277913,-0.034193496108874,0.0769225661055189));
#70178=CARTESIAN_POINT('',(0.0032029979098032,-0.033866421286425,0.0771272482330836));
#70179=CARTESIAN_POINT('Origin',(0.0179855814678328,-0.0345610720404878,
0.0693054236682199));
#70180=CARTESIAN_POINT('Origin',(-0.00617955990394535,-0.0336938005073058,
0.0828040724588024));
#70181=CARTESIAN_POINT('',(0.0031394527540545,-0.0336938721132327,0.0770195966690428));
#70182=CARTESIAN_POINT('',(0.00317180650376104,-0.0336938721132427,0.077073070820571));
#70183=CARTESIAN_POINT('',(0.00302576498972379,-0.0340203938281605,0.0768123947104055));
#70184=CARTESIAN_POINT('Origin',(0.018135931327103,-0.034558964324261,0.0697625140900591));
#70185=CARTESIAN_POINT('',(0.00302696919836559,-0.034193496108874,0.0768117658230245));
#70186=CARTESIAN_POINT('Origin',(-0.00674069408269382,-0.034193422071769,
0.0819128414261462));
#70187=CARTESIAN_POINT('',(0.00305590143558237,-0.034193496108884,0.0768671659642817));
#70188=CARTESIAN_POINT('Ctrl Pts',(0.00270058669856236,-0.0340223579322397,
0.0767168951338089));
#70189=CARTESIAN_POINT('Ctrl Pts',(0.00273599087720114,-0.0339125849573575,
0.0767916951439664));
#70190=CARTESIAN_POINT('Ctrl Pts',(0.00277291836413257,-0.0338030433565231,
0.0768657098087929));
#70191=CARTESIAN_POINT('Ctrl Pts',(0.00281131354479889,-0.0336938721132327,
0.0769388486622199));
#70192=CARTESIAN_POINT('Ctrl Pts',(0.00280940981634064,-0.0340223579322397,
0.0767484974892177));
#70193=CARTESIAN_POINT('Ctrl Pts',(0.00284524987388292,-0.0339125849573575,
0.0768217965447584));
#70194=CARTESIAN_POINT('Ctrl Pts',(0.00288258186715795,-0.0338030433565231,
0.0768943022879911));
#70195=CARTESIAN_POINT('Ctrl Pts',(0.00292134983536847,-0.0336938721132327,
0.0769659262283597));
#70196=CARTESIAN_POINT('Ctrl Pts',(0.00291823293411893,-0.0340223579322397,
0.0767800998446266));
#70197=CARTESIAN_POINT('Ctrl Pts',(0.00295450887056471,-0.0339125849573575,
0.0768518979455505));
#70198=CARTESIAN_POINT('Ctrl Pts',(0.00299224537018333,-0.0338030433565231,
0.0769228947671894));
#70199=CARTESIAN_POINT('Ctrl Pts',(0.00303138612593806,-0.0336938721132327,
0.0769930037944996));
#70200=CARTESIAN_POINT('Ctrl Pts',(0.00302705605189722,-0.0340223579322397,
0.0768117022000354));
#70201=CARTESIAN_POINT('Ctrl Pts',(0.00306376786724649,-0.0339125849573575,
0.0768819993463426));
#70202=CARTESIAN_POINT('Ctrl Pts',(0.00310190887320872,-0.0338030433565231,
0.0769514872463876));
#70203=CARTESIAN_POINT('Ctrl Pts',(0.00314142241650764,-0.0336938721132327,
0.0770200813606394));
#70204=CARTESIAN_POINT('',(0.00297538314943704,-0.0336938721132427,0.0769792226656414));
#70205=CARTESIAN_POINT('Ctrl Pts',(0.00280536863771951,-0.0337108120662681,
0.0769274947695836));
#70206=CARTESIAN_POINT('Ctrl Pts',(0.00284348327556921,-0.0337611408994431,
0.0769075897347138));
#70207=CARTESIAN_POINT('Ctrl Pts',(0.00288090240583828,-0.0338121088781598,
0.0768880479225696));
#70208=CARTESIAN_POINT('Ctrl Pts',(0.00295438373940751,-0.0339153382773233,
0.0768496729414733));
#70209=CARTESIAN_POINT('Ctrl Pts',(0.00299041485563483,-0.0339675558473109,
0.0768308560074719));
#70210=CARTESIAN_POINT('Ctrl Pts',(0.00302576498976157,-0.0340203938281304,
0.0768123947103918));
#70211=CARTESIAN_POINT('Ctrl Pts',(0.00308544100182471,-0.0341934961088741,
0.0769206310258527));
#70212=CARTESIAN_POINT('Ctrl Pts',(0.00314272161554826,-0.0340287516182428,
0.0770247947607176));
#70213=CARTESIAN_POINT('Ctrl Pts',(0.00320425845026947,-0.033864463327595,
0.0771265020384417));
#70214=CARTESIAN_POINT('Ctrl Pts',(0.00308483367277917,-0.0341934961088741,
0.0769225661055188));
#70215=CARTESIAN_POINT('Ctrl Pts',(0.00314215429275034,-0.0340287516182428,
0.0770267423964333));
#70216=CARTESIAN_POINT('Ctrl Pts',(0.00320373161848564,-0.033864463327595,
0.0771284605659895));
#70217=CARTESIAN_POINT('Ctrl Pts',(0.00298364097227414,-0.0341934961088741,
0.0772449875977058));
#70218=CARTESIAN_POINT('Ctrl Pts',(0.0030476274025888,-0.0340287516182428,
0.0773512559679823));
#70219=CARTESIAN_POINT('Ctrl Pts',(0.00311595131008736,-0.033864463327595,
0.0774547889262603));
#70220=CARTESIAN_POINT('',(0.00299026364761127,-0.0341764758832402,0.0772559599697467));
#70221=CARTESIAN_POINT('',(0.00298364097227651,-0.034193496108874,0.0772449875976981));
#70222=CARTESIAN_POINT('Origin',(0.0174219428488388,-0.0345621026098399,
0.0691228200665612));
#70223=CARTESIAN_POINT('Ctrl Pts',(0.00299026364751781,-0.0341764758837495,
0.0772559599679233));
#70224=CARTESIAN_POINT('Ctrl Pts',(0.00302698915521971,-0.0341260050040528,
0.0772337397230359));
#70225=CARTESIAN_POINT('Ctrl Pts',(0.00306307626717999,-0.0340749269148341,
0.0772119056857348));
#70226=CARTESIAN_POINT('Ctrl Pts',(0.00313400176244441,-0.0339715436306629,
0.0771689932616394));
#70227=CARTESIAN_POINT('Ctrl Pts',(0.0031688132413406,-0.0339192778237096,
0.0771479311599543));
#70228=CARTESIAN_POINT('Ctrl Pts',(0.0032029979078558,-0.0338664212855284,
0.0771272482321564));
#70229=CARTESIAN_POINT('',(0.00303423732253782,-0.0341934961088841,0.0770837768516186));
#70230=CARTESIAN_POINT('Origin',(0.00812378219310841,-0.0315241814719618,
0.07415));
#70231=CARTESIAN_POINT('',(0.00299026364867667,-0.0342105180190358,0.0772559599700854));
#70232=CARTESIAN_POINT('',(0.0029969097445483,-0.0341934961088739,0.0772669181728474));
#70233=CARTESIAN_POINT('Origin',(0.0174031147408198,-0.0345621700815362,
0.0690815872974236));
#70234=CARTESIAN_POINT('Origin',(0.0168917581452915,-0.0345621040926577,
0.0682465271175147));
#70235=CARTESIAN_POINT('Origin',(0.0169195395759662,-0.0345621714000146,
0.0682823430648086));
#70236=CARTESIAN_POINT('Ctrl Pts',(0.00313867625893174,-0.0346945769586966,
0.0770183132809271));
#70237=CARTESIAN_POINT('Ctrl Pts',(0.00319875422901076,-0.0345275153362943,
0.077122728320646));
#70238=CARTESIAN_POINT('Ctrl Pts',(0.00326213149522179,-0.0343603235965184,
0.0772252809705813));
#70239=CARTESIAN_POINT('Ctrl Pts',(0.0033286161078392,-0.0341934961088739,
0.0773256707113915));
#70240=CARTESIAN_POINT('Ctrl Pts',(0.00318207342367352,-0.0346945769586966,
0.0770900399458308));
#70241=CARTESIAN_POINT('Ctrl Pts',(0.00324365373746674,-0.0345275153362943,
0.0771935460145589));
#70242=CARTESIAN_POINT('Ctrl Pts',(0.003308505149674,-0.0343603235965184,
0.07729514221107));
#70243=CARTESIAN_POINT('Ctrl Pts',(0.00337643139274299,-0.0341934961088739,
0.0773945309095862));
#70244=CARTESIAN_POINT('Ctrl Pts',(0.00322547058841523,-0.0346945769586966,
0.0771617666107346));
#70245=CARTESIAN_POINT('Ctrl Pts',(0.00328855324592267,-0.0345275153362943,
0.0772643637084713));
#70246=CARTESIAN_POINT('Ctrl Pts',(0.00335487880412618,-0.0343603235965184,
0.0773650034515584));
#70247=CARTESIAN_POINT('Ctrl Pts',(0.00342424667764678,-0.0341934961088739,
0.0774633911077818));
#70248=CARTESIAN_POINT('Ctrl Pts',(0.00326886775315709,-0.0346945769586966,
0.0772334932756384));
#70249=CARTESIAN_POINT('Ctrl Pts',(0.00333345275437871,-0.0345275153362943,
0.0773351814023849));
#70250=CARTESIAN_POINT('Ctrl Pts',(0.00340125245857841,-0.0343603235965184,
0.0774348646920475));
#70251=CARTESIAN_POINT('Ctrl Pts',(0.00347206196255056,-0.0341934961088739,
0.0775322513059756));
#70252=CARTESIAN_POINT('',(0.00326886775284368,-0.0346945769586966,0.0772334932751199));
#70253=CARTESIAN_POINT('',(0.00339965091625427,-0.0343667727831474,0.0774303519139613));
#70254=CARTESIAN_POINT('Origin',(0.017362858530093,-0.0345626457066266,
0.068065250738478));
#70255=CARTESIAN_POINT('Origin',(-0.00567854003290058,-0.0341934771029006,
0.0837340891832016));
#70256=CARTESIAN_POINT('',(0.0033294716553295,-0.0341934961088739,0.0773269028104969));
#70257=CARTESIAN_POINT('',(0.00336511923205672,-0.0341934961088839,0.0773782399342499));
#70258=CARTESIAN_POINT('',(0.0032029979092189,-0.0345211942962679,0.077127248231385));
#70259=CARTESIAN_POINT('Origin',(0.0176089111386796,-0.034562559611928,
0.0684783474624671));
#70260=CARTESIAN_POINT('',(0.00320416025344759,-0.0346945769586885,0.0771265449720789));
#70261=CARTESIAN_POINT('Origin',(-0.00626167783094857,-0.0346945685853958,
0.082853710465351));
#70262=CARTESIAN_POINT('',(0.00323651400315563,-0.0346945769587025,0.0771800191236094));
#70263=CARTESIAN_POINT('Ctrl Pts',(0.00287246528051888,-0.0345231616327842,
0.0770523560573407));
#70264=CARTESIAN_POINT('Ctrl Pts',(0.00291247017257885,-0.0344132092796988,
0.077124738067718));
#70265=CARTESIAN_POINT('Ctrl Pts',(0.0029539701653608,-0.034303273855898,
0.0771962888738794));
#70266=CARTESIAN_POINT('Ctrl Pts',(0.00299690974454829,-0.0341934961088739,
0.0772669181728474));
#70267=CARTESIAN_POINT('Ctrl Pts',(0.0029830578048643,-0.0345231616327842,
0.0770770629328505));
#70268=CARTESIAN_POINT('Ctrl Pts',(0.00302340324641867,-0.0344132092796988,
0.0771479205809815));
#70269=CARTESIAN_POINT('Ctrl Pts',(0.00306521224089357,-0.034303273855898,
0.077217940059549));
#70270=CARTESIAN_POINT('Ctrl Pts',(0.00310842892835813,-0.0341934961088739,
0.0772870330375236));
#70271=CARTESIAN_POINT('Ctrl Pts',(0.00309365032920972,-0.0345231616327842,
0.0771017698083604));
#70272=CARTESIAN_POINT('Ctrl Pts',(0.00313433632025849,-0.0344132092796988,
0.0771711030942451));
#70273=CARTESIAN_POINT('Ctrl Pts',(0.00317645431642635,-0.034303273855898,
0.0772395912452187));
#70274=CARTESIAN_POINT('Ctrl Pts',(0.00321994811216796,-0.0341934961088739,
0.0773071479021997));
#70275=CARTESIAN_POINT('Ctrl Pts',(0.00320424285355514,-0.0345231616327842,
0.0771264766838702));
#70276=CARTESIAN_POINT('Ctrl Pts',(0.00324526939409831,-0.0344132092796988,
0.0771942856075086));
#70277=CARTESIAN_POINT('Ctrl Pts',(0.00328769639195912,-0.034303273855898,
0.0772612424308884));
#70278=CARTESIAN_POINT('Ctrl Pts',(0.00333146729597779,-0.0341934961088739,
0.0773272627668758));
#70279=CARTESIAN_POINT('',(0.0031631906999489,-0.0341934961088839,0.0772969104916822));
#70280=CARTESIAN_POINT('Ctrl Pts',(0.00299026365162846,-0.0342105180195383,
0.0772559599682917));
#70281=CARTESIAN_POINT('Ctrl Pts',(0.00302703045306284,-0.0342610556241344,
0.0772337147552873));
#70282=CARTESIAN_POINT('Ctrl Pts',(0.00306313749325517,-0.0343122189870244,
0.0772118687211287));
#70283=CARTESIAN_POINT('Ctrl Pts',(0.00313406370186486,-0.0344158119695154,
0.0771689558607066));
#70284=CARTESIAN_POINT('Ctrl Pts',(0.00316885386095482,-0.0344681990450055,
0.0771479065861105));
#70285=CARTESIAN_POINT('Ctrl Pts',(0.00320299790923847,-0.0345211942962474,
0.0771272482313646));
#70286=CARTESIAN_POINT('Ctrl Pts',(0.00326935226014221,-0.0346945769586932,
0.0772315243615793));
#70287=CARTESIAN_POINT('Ctrl Pts',(0.00333306059590116,-0.034529677707698,
0.0773318862655589));
#70288=CARTESIAN_POINT('Ctrl Pts',(0.00340086254339944,-0.0343648066251421,
0.0774295292874859));
#70289=CARTESIAN_POINT('Ctrl Pts',(0.00326886775283886,-0.0346945769586932,
0.0772334932751123));
#70290=CARTESIAN_POINT('Ctrl Pts',(0.00333261679449195,-0.034529677707698,
0.0773338651959376));
#70291=CARTESIAN_POINT('Ctrl Pts',(0.00340045982710713,-0.0343648066251421,
0.077431516543739));
#70292=CARTESIAN_POINT('Ctrl Pts',(0.00318811974601443,-0.0346945769586932,
0.0775616324843726));
#70293=CARTESIAN_POINT('Ctrl Pts',(0.00325865283363512,-0.034529677707698,
0.0776636738131036));
#70294=CARTESIAN_POINT('Ctrl Pts',(0.00333334311349819,-0.0343648066251421,
0.0777627127514686));
#70295=CARTESIAN_POINT('',(0.00319541831382511,-0.0346775396664988,0.0775721673639379));
#70296=CARTESIAN_POINT('',(0.00318811974601852,-0.0346945769586886,0.0775616324843668));
#70297=CARTESIAN_POINT('Origin',(0.0167441863132882,-0.0345626618330746,
0.067978222031336));
#70298=CARTESIAN_POINT('Ctrl Pts',(0.00319541831372028,-0.0346775396670096,
0.0775721673621132));
#70299=CARTESIAN_POINT('Ctrl Pts',(0.00323070390043304,-0.0346269749928193,
0.0775476656687395));
#70300=CARTESIAN_POINT('Ctrl Pts',(0.00326536236304662,-0.0345757902890807,
0.0775235993956254));
#70301=CARTESIAN_POINT('Ctrl Pts',(0.00333345368166626,-0.0344721681087968,
0.0774763180114924));
#70302=CARTESIAN_POINT('Ctrl Pts',(0.0033668598458875,-0.0344197714289659,
0.0774531214416305));
#70303=CARTESIAN_POINT('Ctrl Pts',(0.00339965091602227,-0.0343667727830658,
0.0774303519138172));
#70304=CARTESIAN_POINT('',(0.0032284937494411,-0.0346945769587026,0.0773975628797533));
#70305=CARTESIAN_POINT('Origin',(0.00812378219310841,-0.0315241814719618,
0.07415));
#70306=CARTESIAN_POINT('',(0.00319541831521432,-0.0347116136489601,0.0775721673638723));
#70307=CARTESIAN_POINT('',(0.00320273936760624,-0.0346945769586885,0.0775826866314311));
#70308=CARTESIAN_POINT('Origin',(0.0167168297805645,-0.034562667741533,
0.0679420974235828));
#70309=CARTESIAN_POINT('Origin',(0.0169183957182655,-0.0345626631704672,
0.0682291003233101));
#70310=CARTESIAN_POINT('Origin',(0.0169426807811622,-0.0345626691855843,
0.0682673575323138));
#70311=CARTESIAN_POINT('Ctrl Pts',(0.00330819890478178,-0.0352450361874069,
0.0772946653587965));
#70312=CARTESIAN_POINT('Ctrl Pts',(0.00342680190497358,-0.0349452760959493,
0.0774762880628058));
#70313=CARTESIAN_POINT('Ctrl Pts',(0.00355874853173212,-0.034644428984174,
0.0776484611325734));
#70314=CARTESIAN_POINT('Ctrl Pts',(0.00330962602076979,-0.0352450361874069,
0.0772967483770289));
#70315=CARTESIAN_POINT('Ctrl Pts',(0.00342830758328338,-0.0349452760959493,
0.0774783172564756));
#70316=CARTESIAN_POINT('Ctrl Pts',(0.00356032849489012,-0.034644428984174,
0.0776504307369548));
#70317=CARTESIAN_POINT('Ctrl Pts',(0.00345092463344402,-0.0352450361874069,
0.0775029878059855));
#70318=CARTESIAN_POINT('Ctrl Pts',(0.0035773846436591,-0.0349452760959493,
0.0776792275208075));
#70319=CARTESIAN_POINT('Ctrl Pts',(0.00371676049073153,-0.034644428984174,
0.0778454410717504));
#70320=CARTESIAN_POINT('Ctrl Pts',(0.00345233761957076,-0.0352450361874069,
0.077505050200275));
#70321=CARTESIAN_POINT('Ctrl Pts',(0.00357887541426286,-0.0349452760959493,
0.0776812366234508));
#70322=CARTESIAN_POINT('Ctrl Pts',(0.00371832481068995,-0.034644428984174,
0.0778473911750983));
#70323=CARTESIAN_POINT('',(0.00347204101307095,-0.0351951634053271,0.0775322265294441));
#70324=CARTESIAN_POINT('',(0.00361494791101335,-0.0348678972925388,0.0777205095457939));
#70325=CARTESIAN_POINT('Origin',(0.0164836600325524,-0.0345636767887041,
0.0669917205232383));
#70326=CARTESIAN_POINT('Origin',(-0.00504768341986911,-0.034694619934111,
0.0845803789055665));
#70327=CARTESIAN_POINT('',(0.00353841149926285,-0.0346945769330288,0.0776216711535067));
#70328=CARTESIAN_POINT('',(0.0035772122234248,-0.0346945769458128,0.0776706686523429));
#70329=CARTESIAN_POINT('',(0.00339965091614769,-0.0350221583435276,0.0774303519137499));
#70330=CARTESIAN_POINT('Origin',(0.0168135385341327,-0.0345628458717477,
0.067341468385268));
#70331=CARTESIAN_POINT('',(0.00340066516062048,-0.0351951360298761,0.0774296439583182));
#70332=CARTESIAN_POINT('Origin',(-0.0056502547616421,-0.0351951838366929,
0.0837144424795535));
#70333=CARTESIAN_POINT('',(0.00347206196210342,-0.0351951371328749,0.0775322513055353));
#70334=CARTESIAN_POINT('Ctrl Pts',(0.00306506851619793,-0.0350241211494343,
0.0773763626477927));
#70335=CARTESIAN_POINT('Ctrl Pts',(0.00310951033881109,-0.0349144232818962,
0.0774460443545387));
#70336=CARTESIAN_POINT('Ctrl Pts',(0.00315541913266755,-0.0348045283579412,
0.0775148491249152));
#70337=CARTESIAN_POINT('Ctrl Pts',(0.00320273937396406,-0.0346945769439157,
0.0775826866405456));
#70338=CARTESIAN_POINT('Ctrl Pts',(0.00317699419653077,-0.0350241211494343,
0.0773940765938533));
#70339=CARTESIAN_POINT('Ctrl Pts',(0.00322168002148792,-0.0349144232818962,
0.0774622165702441));
#70340=CARTESIAN_POINT('Ctrl Pts',(0.00326780109506742,-0.0348045283579412,
0.0775294736437625));
#70341=CARTESIAN_POINT('Ctrl Pts',(0.00331530154779286,-0.0346945769439157,
0.0775957594683171));
#70342=CARTESIAN_POINT('Ctrl Pts',(0.00328891987686361,-0.0350241211494343,
0.0774117905399139));
#70343=CARTESIAN_POINT('Ctrl Pts',(0.00333384970416474,-0.0349144232818962,
0.0774783887859494));
#70344=CARTESIAN_POINT('Ctrl Pts',(0.0033801830574673,-0.0348045283579412,
0.0775440981626099));
#70345=CARTESIAN_POINT('Ctrl Pts',(0.00342786372162167,-0.0346945769439157,
0.0776088322960885));
#70346=CARTESIAN_POINT('Ctrl Pts',(0.00340084555719646,-0.0350241211494343,
0.0774295044859745));
#70347=CARTESIAN_POINT('Ctrl Pts',(0.00344601938684157,-0.0349144232818962,
0.0774945610016548));
#70348=CARTESIAN_POINT('Ctrl Pts',(0.00349256501986717,-0.0348045283579412,
0.0775587226814572));
#70349=CARTESIAN_POINT('Ctrl Pts',(0.00354042589545047,-0.0346945769439157,
0.07762190512386));
#70350=CARTESIAN_POINT('',(0.00337057543319695,-0.0346945769458128,0.0776021788922911));
#70351=CARTESIAN_POINT('Ctrl Pts',(0.00319541831791141,-0.0347116136492788,
0.0775721673619913));
#70352=CARTESIAN_POINT('Ctrl Pts',(0.00323068989929081,-0.0347621546532318,
0.0775476754093557));
#70353=CARTESIAN_POINT('Ctrl Pts',(0.00326534131095514,-0.034813308409707,
0.077523614091432));
#70354=CARTESIAN_POINT('Ctrl Pts',(0.00333343271381562,-0.0349168561544567,
0.0774763326442009));
#70355=CARTESIAN_POINT('Ctrl Pts',(0.00336684569661273,-0.0349692089015914,
0.0774531312690406));
#70356=CARTESIAN_POINT('Ctrl Pts',(0.00339965091618907,-0.0350221583435,
0.0774303519137454));
#70357=CARTESIAN_POINT('Ctrl Pts',(0.00347232165795471,-0.0351951371254882,
0.0775308115215332));
#70358=CARTESIAN_POINT('Ctrl Pts',(0.00354221781496879,-0.0350307338980925,
0.0776269775496714));
#70359=CARTESIAN_POINT('Ctrl Pts',(0.00361602889183594,-0.0348659306897825,
0.0777201725209142));
#70360=CARTESIAN_POINT('Ctrl Pts',(0.0034720619621967,-0.0351951371254882,
0.077532251305466));
#70361=CARTESIAN_POINT('Ctrl Pts',(0.00354198788584025,-0.0350307338980925,
0.0776284227026511));
#70362=CARTESIAN_POINT('Ctrl Pts',(0.00361582892580994,-0.0348659306897825,
0.077721621808066));
#70363=CARTESIAN_POINT('Ctrl Pts',(0.00342853668249728,-0.0351951371254882,
0.077773560593165));
#70364=CARTESIAN_POINT('Ctrl Pts',(0.00350345152426138,-0.0350307338980925,
0.0778706318481992));
#70365=CARTESIAN_POINT('Ctrl Pts',(0.00358231441144628,-0.0348659306897825,
0.0779645238451709));
#70366=CARTESIAN_POINT('Origin',(-0.000554293137037344,-0.0308609197410472,
0.0810220979452573));
#70367=CARTESIAN_POINT('',(0.00345308592161264,-0.0351951371254882,0.0776374567141));
#70368=CARTESIAN_POINT('Origin',(0.00879382484640623,-0.0351840467441214,
0.0734388119151953));
#70369=CARTESIAN_POINT('Origin',(-0.000742447723436461,-0.0352322614715386,
0.0821847918805444));
#70370=CARTESIAN_POINT('',(0.00376567346689154,-0.0351951142564663,0.0779029592209228));
#70371=CARTESIAN_POINT('',(0.00384904922986462,-0.0351951372916786,0.0779956674444053));
#70372=CARTESIAN_POINT('Origin',(0.00845049893136249,-0.0352875121748006,
0.0742462287415656));
#70373=CARTESIAN_POINT('Origin',(0.00426650984675451,-0.0298325076522592,
0.0677144238543658));
#70374=CARTESIAN_POINT('Origin',(0.00024036384308776,-0.0338730261438308,
0.076997743730105));
#70375=CARTESIAN_POINT('Ctrl Pts',(0.00239200676776708,-0.0321934096636942,
0.0746242216979064));
#70376=CARTESIAN_POINT('Ctrl Pts',(0.00240049511033863,-0.0320508460843189,
0.0747268177485896));
#70377=CARTESIAN_POINT('Ctrl Pts',(0.0024117336061173,-0.0319086045660805,
0.0748291083764958));
#70378=CARTESIAN_POINT('Ctrl Pts',(0.00242567992432284,-0.0317669892864515,
0.0749308753240754));
#70379=CARTESIAN_POINT('Ctrl Pts',(0.00240073546049954,-0.0321934096636942,
0.0747076137991576));
#70380=CARTESIAN_POINT('Ctrl Pts',(0.00241071648197276,-0.0320508460843189,
0.0748100536103974));
#70381=CARTESIAN_POINT('Ctrl Pts',(0.00242344233332272,-0.0319086045660805,
0.0749121480113285));
#70382=CARTESIAN_POINT('Ctrl Pts',(0.00243886751601472,-0.0317669892864515,
0.0750136794305652));
#70383=CARTESIAN_POINT('Ctrl Pts',(0.00240946415323199,-0.0321934096636942,
0.0747910059004088));
#70384=CARTESIAN_POINT('Ctrl Pts',(0.00242093785360689,-0.0320508460843189,
0.0748932894722052));
#70385=CARTESIAN_POINT('Ctrl Pts',(0.00243515106052814,-0.0319086045660805,
0.0749951876461612));
#70386=CARTESIAN_POINT('Ctrl Pts',(0.0024520551077066,-0.0317669892864515,
0.0750964835370549));
#70387=CARTESIAN_POINT('Ctrl Pts',(0.00241819284596445,-0.0321934096636942,
0.07487439800166));
#70388=CARTESIAN_POINT('Ctrl Pts',(0.00243115922524102,-0.0320508460843189,
0.0749765253340131));
#70389=CARTESIAN_POINT('Ctrl Pts',(0.00244685978773356,-0.0319086045660805,
0.0750782272809939));
#70390=CARTESIAN_POINT('Ctrl Pts',(0.00246524269939848,-0.0317669892864515,
0.0751792876435447));
#70391=CARTESIAN_POINT('',(0.00241803668792887,-0.0321934096636942,0.0748729061004892));
#70392=CARTESIAN_POINT('',(0.00245255450133589,-0.0318665617511279,0.0751067138846742));
#70393=CARTESIAN_POINT('Origin',(0.019061392985984,-0.0326371944421208,
0.0733840824103799));
#70394=CARTESIAN_POINT('Origin',(-0.0083559143282543,-0.03169392615091,
0.0769300601821768));
#70395=CARTESIAN_POINT('',(0.00240374664865815,-0.032019722162179,0.0747489845880791));
#70396=CARTESIAN_POINT('Ctrl Pts',(0.00240371834984765,-0.0320197392094712,
0.0747491673832019));
#70397=CARTESIAN_POINT('Ctrl Pts',(0.00240676715280521,-0.0319792716576009,
0.0747782729020997));
#70398=CARTESIAN_POINT('Ctrl Pts',(0.00241005172383592,-0.0319386439829649,
0.0748074876775532));
#70399=CARTESIAN_POINT('Ctrl Pts',(0.0024135839156869,-0.031897909938158,
0.0748368414346369));
#70400=CARTESIAN_POINT('Ctrl Pts',(0.00241711603772156,-0.031857176698489,
0.0748661946115224));
#70401=CARTESIAN_POINT('Ctrl Pts',(0.00242087604931126,-0.0318163871833547,
0.0748955377853829));
#70402=CARTESIAN_POINT('Ctrl Pts',(0.00242484752496734,-0.0317755399638303,
0.0749247704753257));
#70403=CARTESIAN_POINT('',(0.00240502396467459,-0.0321934096636183,0.0747485852693819));
#70404=CARTESIAN_POINT('Origin',(0.000111662229081881,-0.0324112415123257,
0.075009778339421));
#70405=CARTESIAN_POINT('',(0.00241153032631172,-0.0321934096636663,0.0748107456849456));
#70406=CARTESIAN_POINT('Ctrl Pts',(0.00241931376590365,-0.0321934096636618,
0.0748713304231029));
#70407=CARTESIAN_POINT('Ctrl Pts',(0.00242926147461029,-0.0320835708272592,
0.0749499994885167));
#70408=CARTESIAN_POINT('Ctrl Pts',(0.00244083146546171,-0.0319739230346489,
0.0750284170553609));
#70409=CARTESIAN_POINT('Ctrl Pts',(0.00245400123542266,-0.0318646057455573,
0.0751064839298879));
#70410=CARTESIAN_POINT('Ctrl Pts',(0.00234796211955568,-0.0321934096636618,
0.0749593651169921));
#70411=CARTESIAN_POINT('Ctrl Pts',(0.00235912389530128,-0.0320835708272592,
0.0750390181772173));
#70412=CARTESIAN_POINT('Ctrl Pts',(0.00237192761270491,-0.0319739230346489,
0.0751183940430615));
#70413=CARTESIAN_POINT('Ctrl Pts',(0.00238634909616581,-0.0318646057455573,
0.0751973924158433));
#70414=CARTESIAN_POINT('Ctrl Pts',(0.0022766104732077,-0.0321934096636618,
0.0750473998108813));
#70415=CARTESIAN_POINT('Ctrl Pts',(0.00228898631599226,-0.0320835708272592,
0.0751280368659178));
#70416=CARTESIAN_POINT('Ctrl Pts',(0.00230302375994811,-0.0319739230346489,
0.0752083710307621));
#70417=CARTESIAN_POINT('Ctrl Pts',(0.00231869695690897,-0.0318646057455573,
0.0752883009017987));
#70418=CARTESIAN_POINT('Ctrl Pts',(0.00220525882685973,-0.0321934096636618,
0.0751354345047705));
#70419=CARTESIAN_POINT('Ctrl Pts',(0.00221884873668325,-0.0320835708272592,
0.0752170555546183));
#70420=CARTESIAN_POINT('Ctrl Pts',(0.00223411990719132,-0.0319739230346489,
0.0752983480184628));
#70421=CARTESIAN_POINT('Ctrl Pts',(0.00225104481765213,-0.0318646057455573,
0.0753792093877541));
#70422=CARTESIAN_POINT('',(0.00220737723631769,-0.0321763980308456,0.0751480743283701));
#70423=CARTESIAN_POINT('',(0.00220525882686676,-0.0321934096636184,0.0751354345048006));
#70424=CARTESIAN_POINT('Origin',(0.0186153532276283,-0.0326386231974675,
0.0730022842093011));
#70425=CARTESIAN_POINT('Ctrl Pts',(0.00220737723944192,-0.0321763980306282,
0.0751480743278375));
#70426=CARTESIAN_POINT('Ctrl Pts',(0.00224969816501251,-0.032125959617537,
0.0751409349535598));
#70427=CARTESIAN_POINT('Ctrl Pts',(0.00229128582563289,-0.0320749164632513,
0.0751339192781986));
#70428=CARTESIAN_POINT('Ctrl Pts',(0.00237302808554854,-0.0319716057793908,
0.0751201296793188));
#70429=CARTESIAN_POINT('Ctrl Pts',(0.00241315083518113,-0.0319193786690101,
0.0751133611287137));
#70430=CARTESIAN_POINT('Ctrl Pts',(0.00245255450316127,-0.0318665617525295,
0.075106713884358));
#70431=CARTESIAN_POINT('',(0.00231164775740781,-0.0321934096636663,0.0750041703026549));
#70432=CARTESIAN_POINT('Origin',(0.00812378219310841,-0.0315241814719618,
0.07415));
#70433=CARTESIAN_POINT('',(0.0022073772359508,-0.0322104233323605,0.0751480743284319));
#70434=CARTESIAN_POINT('',(0.0022095226361545,-0.0321934096636183,0.0751607095987536));
#70435=CARTESIAN_POINT('Origin',(0.0186141164605679,-0.0326387227552032,
0.0729569655886994));
#70436=CARTESIAN_POINT('Origin',(0.0184112488701724,-0.032638624733196,
0.0717923714997738));
#70437=CARTESIAN_POINT('Origin',(0.0184249411132221,-0.0326387240321869,
0.071835589278331));
#70438=CARTESIAN_POINT('Ctrl Pts',(0.00242797688386437,-0.0327445246967097,
0.0749474502361826));
#70439=CARTESIAN_POINT('Ctrl Pts',(0.00245805321120333,-0.032443687833936,
0.0751622710452652));
#70440=CARTESIAN_POINT('Ctrl Pts',(0.00250422527619636,-0.0321434074405927,
0.0753742160992186));
#70441=CARTESIAN_POINT('Ctrl Pts',(0.00246801327136899,-0.0327445246967097,
0.0751942235890301));
#70442=CARTESIAN_POINT('Ctrl Pts',(0.00250739680786285,-0.032443687833936,
0.0754075344010728));
#70443=CARTESIAN_POINT('Ctrl Pts',(0.00256273590206407,-0.0321434074405927,
0.075617272690696));
#70444=CARTESIAN_POINT('',(0.00247468732294034,-0.0326943950436612,0.0752297463349518));
#70445=CARTESIAN_POINT('',(0.00252381793464815,-0.0323666188837389,0.0754609253617077));
#70446=CARTESIAN_POINT('Origin',(0.018972287240742,-0.0326395579110082,
0.0719990722305594));
#70447=CARTESIAN_POINT('Origin',(-0.0082300605462127,-0.0321933825603015,
0.0779783584721712));
#70448=CARTESIAN_POINT('',(0.00249664906193553,-0.0321934096532689,0.0753389061025637));
#70449=CARTESIAN_POINT('',(0.00251089488512872,-0.0321934096584275,0.0753997609040791));
#70450=CARTESIAN_POINT('',(0.00245255450039553,-0.0325210109756239,0.0751067138848201));
#70451=CARTESIAN_POINT('Origin',(0.0190375043577656,-0.032639312916037,
0.0724754451495563));
#70452=CARTESIAN_POINT('',(0.00245389410775943,-0.0326943950436593,0.0751064878983125));
#70453=CARTESIAN_POINT('Origin',(-0.0084544335388826,-0.032694376553816,
0.0769466793692213));
#70454=CARTESIAN_POINT('',(0.00246429071535988,-0.0326943950436702,0.0751681171166422));
#70455=CARTESIAN_POINT('Ctrl Pts',(0.00217280266362598,-0.0325229783203769,
0.0749154035796323));
#70456=CARTESIAN_POINT('Ctrl Pts',(0.00218335373523294,-0.032413025309245,
0.0749974377023069));
#70457=CARTESIAN_POINT('Ctrl Pts',(0.00219560018777097,-0.0323031222208069,
0.0750792411204294));
#70458=CARTESIAN_POINT('Ctrl Pts',(0.0022095226369099,-0.0321934096576658,
0.0751607096031737));
#70459=CARTESIAN_POINT('Ctrl Pts',(0.00226653380546701,-0.0325229783203769,
0.0749790872925074));
#70460=CARTESIAN_POINT('Ctrl Pts',(0.00227796275566328,-0.032413025309245,
0.0750598293334414));
#70461=CARTESIAN_POINT('Ctrl Pts',(0.00229106022527254,-0.0323031222208069,
0.0751403227057466));
#70462=CARTESIAN_POINT('Ctrl Pts',(0.002305805799086,-0.0321934096576658,
0.0752204648951381));
#70463=CARTESIAN_POINT('Ctrl Pts',(0.00236026494730804,-0.0325229783203769,
0.0750427710053824));
#70464=CARTESIAN_POINT('Ctrl Pts',(0.00237257177609363,-0.032413025309245,
0.075122220964576));
#70465=CARTESIAN_POINT('Ctrl Pts',(0.00238652026277411,-0.0323031222208069,
0.0752014042910639));
#70466=CARTESIAN_POINT('Ctrl Pts',(0.0024020889612621,-0.0321934096576658,
0.0752802201871025));
#70467=CARTESIAN_POINT('Ctrl Pts',(0.00245399608914908,-0.0325229783203769,
0.0751064547182575));
#70468=CARTESIAN_POINT('Ctrl Pts',(0.00246718079652397,-0.032413025309245,
0.0751846125957105));
#70469=CARTESIAN_POINT('Ctrl Pts',(0.00248198030027568,-0.0323031222208069,
0.0752624858763811));
#70470=CARTESIAN_POINT('Ctrl Pts',(0.0024983721234382,-0.0321934096576658,
0.0753399754790668));
#70471=CARTESIAN_POINT('',(0.00235308584881014,-0.0321934096584275,0.0752498078502129));
#70472=CARTESIAN_POINT('Ctrl Pts',(0.00220737723937597,-0.0322104233328921,
0.0751480743278485));
#70473=CARTESIAN_POINT('Ctrl Pts',(0.00224975551053476,-0.0322609421831422,
0.0751409252795949));
#70474=CARTESIAN_POINT('Ctrl Pts',(0.00229137118545055,-0.0323120888240851,
0.0751339048783387));
#70475=CARTESIAN_POINT('Ctrl Pts',(0.00237311406416133,-0.0324156524631807,
0.0751201151750706));
#70476=CARTESIAN_POINT('Ctrl Pts',(0.00241320766736387,-0.0324680267167312,
0.075113351541347));
#70477=CARTESIAN_POINT('Ctrl Pts',(0.00245255450043899,-0.0325210109755913,
0.0751067138848172));
#70478=CARTESIAN_POINT('Origin',(0.00775888783888567,-0.0262834582511916,
0.0662905955728784));
#70479=CARTESIAN_POINT('Origin',(-0.00350327331151527,-0.0342770850501676,
0.0705953783460784));
#70480=CARTESIAN_POINT('Ctrl Pts',(0.00247586265801749,-0.0326943950436604,
0.0752280939795756));
#70481=CARTESIAN_POINT('Ctrl Pts',(0.00249072081361951,-0.0325844576448134,
0.0753059328960985));
#70482=CARTESIAN_POINT('Ctrl Pts',(0.00250718985716863,-0.0324744968375322,
0.0753834700303844));
#70483=CARTESIAN_POINT('Ctrl Pts',(0.00252524731729828,-0.0323646534831894,
0.0754606063283826));
#70484=CARTESIAN_POINT('Ctrl Pts',(0.00241017964710776,-0.0326943950436604,
0.0753204350303575));
#70485=CARTESIAN_POINT('Ctrl Pts',(0.00242631043545513,-0.0325844576448134,
0.0753991791818738));
#70486=CARTESIAN_POINT('Ctrl Pts',(0.00244407092355962,-0.0324744968375322,
0.0754775952950863));
#70487=CARTESIAN_POINT('Ctrl Pts',(0.00246343696984689,-0.0323646534831894,
0.0755555832125682));
#70488=CARTESIAN_POINT('Ctrl Pts',(0.00234449663619804,-0.0326943950436604,
0.0754127760811394));
#70489=CARTESIAN_POINT('Ctrl Pts',(0.00236190005729076,-0.0325844576448134,
0.0754924254676492));
#70490=CARTESIAN_POINT('Ctrl Pts',(0.0023809519899506,-0.0324744968375322,
0.0755717205597883));
#70491=CARTESIAN_POINT('Ctrl Pts',(0.00240162662239551,-0.0323646534831894,
0.0756505600967539));
#70492=CARTESIAN_POINT('Ctrl Pts',(0.00227881362528831,-0.0326943950436604,
0.0755051171319213));
#70493=CARTESIAN_POINT('Ctrl Pts',(0.00229748967912638,-0.0325844576448134,
0.0755856717534245));
#70494=CARTESIAN_POINT('Ctrl Pts',(0.00231783305634159,-0.0324744968375322,
0.0756658458244902));
#70495=CARTESIAN_POINT('Ctrl Pts',(0.00233981627494412,-0.0323646534831894,
0.0757455369809395));
#70496=CARTESIAN_POINT('',(0.0022817215154339,-0.0326773559991162,0.0755175989977011));
#70497=CARTESIAN_POINT('',(0.0022788136252905,-0.0326943950436594,0.0755051171319192));
#70498=CARTESIAN_POINT('Origin',(0.018438312426154,-0.0326395669990593,
0.0716838177891191));
#70499=CARTESIAN_POINT('Ctrl Pts',(0.00228172151869258,-0.032677355998743,
0.0755175989969323));
#70500=CARTESIAN_POINT('Ctrl Pts',(0.00232354427761802,-0.0326267922586569,
0.0755078084852715));
#70501=CARTESIAN_POINT('Ctrl Pts',(0.00236462575834461,-0.0325756109580565,
0.0754981915033596));
#70502=CARTESIAN_POINT('Ctrl Pts',(0.00244534112595734,-0.0324719985462364,
0.0754792964144627));
#70503=CARTESIAN_POINT('Ctrl Pts',(0.0024849426399717,-0.032419609162177,
0.0754700258858152));
#70504=CARTESIAN_POINT('Ctrl Pts',(0.00252381793469563,-0.0323666188837756,
0.0754609253616966));
#70505=CARTESIAN_POINT('',(0.00237675047412542,-0.0326943950436703,0.0753674317334455));
#70506=CARTESIAN_POINT('Origin',(0.00812378219310841,-0.0315241814719618,
0.07415));
#70507=CARTESIAN_POINT('',(0.00228172151547635,-0.0327114338380045,0.0755175989976911));
#70508=CARTESIAN_POINT('',(0.00228465605720561,-0.0326943950436593,0.0755300746244477));
#70509=CARTESIAN_POINT('Origin',(0.0184272333273719,-0.0326395661562076,
0.0716398814172339));
#70510=CARTESIAN_POINT('Origin',(0.0184612178671954,-0.0326395683361966,
0.0717816520510706));
#70511=CARTESIAN_POINT('Origin',(0.0184707862139934,-0.0326395674444665,
0.0718259421494922));
#70512=CARTESIAN_POINT('Ctrl Pts',(0.00248929643620834,-0.0332451089994433,
0.075303557651481));
#70513=CARTESIAN_POINT('Ctrl Pts',(0.00253280357484802,-0.0329451141710254,
0.0755160657586173));
#70514=CARTESIAN_POINT('Ctrl Pts',(0.00259219409366805,-0.0326442513127494,
0.0757246930171084));
#70515=CARTESIAN_POINT('Ctrl Pts',(0.00254475051058248,-0.0332451089994433,
0.0755473297697295));
#70516=CARTESIAN_POINT('Ctrl Pts',(0.00259745166508388,-0.0329451141710254,
0.0757577463922322));
#70517=CARTESIAN_POINT('Ctrl Pts',(0.00266585254136425,-0.0326442513127494,
0.0759635955769168));
#70518=CARTESIAN_POINT('Ctrl Pts',(0.00254530505132622,-0.0332451089994433,
0.0755497674909119));
#70519=CARTESIAN_POINT('Ctrl Pts',(0.00259809814598624,-0.0329451141710254,
0.0757601631985683));
#70520=CARTESIAN_POINT('Ctrl Pts',(0.0026665891258412,-0.0326442513127494,
0.0759659846025148));
#70521=CARTESIAN_POINT('',(0.00255363235458533,-0.0331951640388616,0.0755823253039733));
#70522=CARTESIAN_POINT('',(0.0026171818676611,-0.0328677532355001,0.0758099632301979));
#70523=CARTESIAN_POINT('Origin',(0.0185811579717228,-0.0326402808281015,
0.0706679921793711));
#70524=CARTESIAN_POINT('Origin',(-0.00796817111841373,-0.0326944278779144,
0.0790013085759663));
#70525=CARTESIAN_POINT('',(0.0025824049570902,-0.0326943950436593,0.0756898906870749));
#70526=CARTESIAN_POINT('',(0.00260044377354836,-0.0326943950436694,0.0757497309001623));
#70527=CARTESIAN_POINT('',(0.00252381793464749,-0.0330220786163545,0.0754609253617049));
#70528=CARTESIAN_POINT('Origin',(0.0187497064791712,-0.0326396682763934,
0.0711182632598278));
#70529=CARTESIAN_POINT('',(0.00252514070879168,-0.0331951640388587,0.0754606157064861));
#70530=CARTESIAN_POINT('Origin',(-0.00821612393864679,-0.0331952026560115,
0.0779750944438362));
#70531=CARTESIAN_POINT('',(0.0025393865316985,-0.0331951640388701,0.0755214705052398));
#70532=CARTESIAN_POINT('Ctrl Pts',(0.00223260583294866,-0.0330240426238172,
0.075287559270334));
#70533=CARTESIAN_POINT('Ctrl Pts',(0.00224827682016781,-0.032914277406352,
0.0753687159641902));
#70534=CARTESIAN_POINT('Ctrl Pts',(0.00226563335550769,-0.0328043479726691,
0.0754495891545376));
#70535=CARTESIAN_POINT('Ctrl Pts',(0.00228465605720559,-0.0326943950436593,
0.0755300746244477));
#70536=CARTESIAN_POINT('Ctrl Pts',(0.00233015073669985,-0.0330240426238172,
0.0753452318611957));
#70537=CARTESIAN_POINT('Ctrl Pts',(0.00234661622004579,-0.032914277406352,
0.0754250447789693));
#70538=CARTESIAN_POINT('Ctrl Pts',(0.00236473986799249,-0.0328043479726691,
0.0755045570988585));
#70539=CARTESIAN_POINT('Ctrl Pts',(0.00238450126803657,-0.0326943950436593,
0.075583666320247));
#70540=CARTESIAN_POINT('Ctrl Pts',(0.00242769564045103,-0.0330240426238172,
0.0754029044520574));
#70541=CARTESIAN_POINT('Ctrl Pts',(0.00244495561992378,-0.032914277406352,
0.0754813735937484));
#70542=CARTESIAN_POINT('Ctrl Pts',(0.00246384638047729,-0.0328043479726691,
0.0755595250431793));
#70543=CARTESIAN_POINT('Ctrl Pts',(0.00248434647886754,-0.0326943950436593,
0.0756372580160463));
#70544=CARTESIAN_POINT('Ctrl Pts',(0.00252524054420221,-0.0330240426238172,
0.075460577042919));
#70545=CARTESIAN_POINT('Ctrl Pts',(0.00254329501980176,-0.032914277406352,
0.0755377024085275));
#70546=CARTESIAN_POINT('Ctrl Pts',(0.00256295289296209,-0.0328043479726691,
0.0756144929875002));
#70547=CARTESIAN_POINT('Ctrl Pts',(0.00258419168969852,-0.0326943950436593,
0.0756908497118456));
#70548=CARTESIAN_POINT('',(0.0024335305071579,-0.0326943950436694,0.0756099826557714));
#70549=CARTESIAN_POINT('Ctrl Pts',(0.00228172151869955,-0.0327114338383318,
0.0755175989969306));
#70550=CARTESIAN_POINT('Ctrl Pts',(0.00232353732119333,-0.0327619876831142,
0.0755078101137379));
#70551=CARTESIAN_POINT('Ctrl Pts',(0.00236461540410392,-0.03281315626047,
0.0754981939272388));
#70552=CARTESIAN_POINT('Ctrl Pts',(0.00244533069746579,-0.0329167375858767,
0.0754792988557237));
#70553=CARTESIAN_POINT('Ctrl Pts',(0.00248493574682939,-0.0329691088920618,
0.0754700274994674));
#70554=CARTESIAN_POINT('Ctrl Pts',(0.00252381793469442,-0.0330220786163187,
0.0754609253616968));
#70555=CARTESIAN_POINT('Ctrl Pts',(0.00255470178886066,-0.0331951640388604,
0.0755806021341843));
#70556=CARTESIAN_POINT('Ctrl Pts',(0.00258427857076817,-0.033030642201062,
0.0756957393009799));
#70557=CARTESIAN_POINT('Ctrl Pts',(0.00261858881970751,-0.0328657861914645,
0.0758095556443734));
#70558=CARTESIAN_POINT('Ctrl Pts',(0.00255363235458461,-0.0331951640388604,
0.0755823253039703));
#70559=CARTESIAN_POINT('Ctrl Pts',(0.00258324476192266,-0.033030642201062,
0.0756974845806339));
#70560=CARTESIAN_POINT('Ctrl Pts',(0.00261759151967494,-0.0328657861914645,
0.0758113215425662));
#70561=CARTESIAN_POINT('Ctrl Pts',(0.00237543584433657,-0.0331951640388604,
0.0758694517308149));
#70562=CARTESIAN_POINT('Ctrl Pts',(0.00241098440646129,-0.033030642201062,
0.075988295106079));
#70563=CARTESIAN_POINT('Ctrl Pts',(0.00245141451426703,-0.0328657861914645,
0.0761055676710554));
#70564=CARTESIAN_POINT('',(0.00237912173782625,-0.0331781648281905,0.0758817263783082));
#70565=CARTESIAN_POINT('',(0.00237543584433932,-0.0331951640388588,0.0758694517308122));
#70566=CARTESIAN_POINT('Origin',(0.017978010182919,-0.0326412092170369,
0.0704355203308688));
#70567=CARTESIAN_POINT('Ctrl Pts',(0.00237912173840406,-0.033178164828644,
0.0758817263765579));
#70568=CARTESIAN_POINT('Ctrl Pts',(0.00242027552811085,-0.0331276811546774,
0.0758693205648664));
#70569=CARTESIAN_POINT('Ctrl Pts',(0.00246068619806179,-0.0330765663497782,
0.0758571387313375));
#70570=CARTESIAN_POINT('Ctrl Pts',(0.00254005606509915,-0.0329730614463344,
0.0758332127095248));
#70571=CARTESIAN_POINT('Ctrl Pts',(0.00257898320003413,-0.0329207133374209,
0.0758214781919652));
#70572=CARTESIAN_POINT('Ctrl Pts',(0.00261718185528346,-0.032867753228936,
0.0758099632193273));
#70573=CARTESIAN_POINT('',(0.00246453409947232,-0.0331951640388702,0.0757258885174028));
#70574=CARTESIAN_POINT('Origin',(0.00812378219310841,-0.0315241814719618,
0.07415));
#70575=CARTESIAN_POINT('',(0.00237912173949705,-0.0332121607144409,0.07588172637848));
#70576=CARTESIAN_POINT('',(0.00238283384147147,-0.0331951640388587,0.0758939931260949));
#70577=CARTESIAN_POINT('Origin',(0.0179576128667686,-0.0326413642951286,
0.0703950201715192));
#70578=CARTESIAN_POINT('Origin',(0.0183891629845607,-0.0326412102338043,
0.0717994275002161));
#70579=CARTESIAN_POINT('Origin',(0.0183945413997972,-0.0326413657341333,
0.0718444545186698));
#70580=CARTESIAN_POINT('Ctrl Pts',(0.00257284183963962,-0.0337436976235976,
0.0756550535512837));
#70581=CARTESIAN_POINT('Ctrl Pts',(0.00258637851937698,-0.0336723290703325,
0.0757049795500909));
#70582=CARTESIAN_POINT('Ctrl Pts',(0.00260081102055362,-0.033601104548885,
0.075754653989846));
#70583=CARTESIAN_POINT('Ctrl Pts',(0.00264689113789323,-0.0333736987606857,
0.075913254636032));
#70584=CARTESIAN_POINT('Ctrl Pts',(0.00270199673840641,-0.0331450831799192,
0.0760689495780717));
#70585=CARTESIAN_POINT('Ctrl Pts',(0.00264349219742188,-0.0337436976235976,
0.0758948629067002));
#70586=CARTESIAN_POINT('Ctrl Pts',(0.00265918575884595,-0.0336723290703325,
0.0759441534654821));
#70587=CARTESIAN_POINT('Ctrl Pts',(0.00267576336321349,-0.033601104548885,
0.075993153772508));
#70588=CARTESIAN_POINT('Ctrl Pts',(0.00272869237012062,-0.0333736987606857,
0.0761496020464278));
#70589=CARTESIAN_POINT('Ctrl Pts',(0.00279051205824203,-0.0331450831799192,
0.0763027551343668));
#70590=CARTESIAN_POINT('Ctrl Pts',(0.0026441987009997,-0.0337436976235976,
0.0758972610002543));
#70591=CARTESIAN_POINT('Ctrl Pts',(0.00265991383124064,-0.0336723290703325,
0.075946545204636));
#70592=CARTESIAN_POINT('Ctrl Pts',(0.00267651288664009,-0.033601104548885,
0.0759955387703346));
#70593=CARTESIAN_POINT('Ctrl Pts',(0.00272951038244289,-0.0333736987606857,
0.0761519655205318));
#70594=CARTESIAN_POINT('Ctrl Pts',(0.00279139721144039,-0.0331450831799192,
0.0763050931899297));
#70595=CARTESIAN_POINT('',(0.00265456022288775,-0.0336938721132548,0.0759292515393999));
#70596=CARTESIAN_POINT('',(0.00273227784254589,-0.0333679869945435,0.076152449958875));
#70597=CARTESIAN_POINT('Ctrl Pts',(0.00265456022289061,-0.0336938721132647,
0.075929251539412));
#70598=CARTESIAN_POINT('Ctrl Pts',(0.00266150547631112,-0.033662918793393,
0.0759506004784193));
#70599=CARTESIAN_POINT('Ctrl Pts',(0.00266857351509565,-0.0336319952301038,
0.0759719019222763));
#70600=CARTESIAN_POINT('Ctrl Pts',(0.00267576336321711,-0.0336011045488948,
0.07599315377252));
#70601=CARTESIAN_POINT('Ctrl Pts',(0.00269380515238141,-0.033523589259545,
0.0760464819367554));
#70602=CARTESIAN_POINT('Ctrl Pts',(0.00271264615022564,-0.0334458668660368,
0.0760995925311814));
#70603=CARTESIAN_POINT('Ctrl Pts',(0.0027322778422408,-0.0333679869945384,
0.0761524499589809));
#70604=CARTESIAN_POINT('Ctrl Pts',(0.00273229268110906,-0.033367969246074,
0.076152491886018));
#70605=CARTESIAN_POINT('Ctrl Pts',(0.0027327154741517,-0.0333391895375,
0.0761523285340469));
#70606=CARTESIAN_POINT('Ctrl Pts',(0.00273303120788034,-0.0333104081060346,
0.0761522030648029));
#70607=CARTESIAN_POINT('Ctrl Pts',(0.00273344709022916,-0.0332532698060263,
0.0761520318378214));
#70608=CARTESIAN_POINT('Ctrl Pts',(0.00273355038452273,-0.0332249170431269,
0.0761519849153727));
#70609=CARTESIAN_POINT('Ctrl Pts',(0.0027335514233815,-0.0331960985399096,
0.0761519771705221));
#70610=CARTESIAN_POINT('Ctrl Pts',(0.00273355141231489,-0.0331956312525604,
0.0761519770552596));
#70611=CARTESIAN_POINT('Ctrl Pts',(0.00273355137358271,-0.0331951640388588,
0.076151976950975));
#70612=CARTESIAN_POINT('',(0.00269003013551804,-0.0331951640388587,0.076034798020116));
#70613=CARTESIAN_POINT('',(0.00271179075456039,-0.0331951640388687,0.0760933874855556));
#70614=CARTESIAN_POINT('',(0.00261718186978805,-0.0335216366567717,0.0758099632148271));
#70615=CARTESIAN_POINT('Origin',(0.0181711571565241,-0.0326434571525561,
0.069856433354535));
#70616=CARTESIAN_POINT('',(0.00261848258998653,-0.0336938721132327,0.0758095711132298));
#70617=CARTESIAN_POINT('Origin',(-0.00783734462861687,-0.0336938867896231,
0.0789614764282001));
#70618=CARTESIAN_POINT('',(0.00263652140644714,-0.0336938721132538,0.0758694113263247));
#70619=CARTESIAN_POINT('Ctrl Pts',(0.00231565890246709,-0.0335235895815172,
0.0756552255115898));
#70620=CARTESIAN_POINT('Ctrl Pts',(0.00233638129515044,-0.0334144449262748,
0.0757351857638279));
#70621=CARTESIAN_POINT('Ctrl Pts',(0.00235877941398685,-0.0333049234473147,
0.075814809771671));
#70622=CARTESIAN_POINT('Ctrl Pts',(0.00238283384147129,-0.0331951640388587,
0.0758939931260949));
#70623=CARTESIAN_POINT('Ctrl Pts',(0.00241663276732491,-0.0335235895815172,
0.0757066594605111));
#70624=CARTESIAN_POINT('Ctrl Pts',(0.00243806324957928,-0.0334144449262748,
0.0757852296087002));
#70625=CARTESIAN_POINT('Ctrl Pts',(0.00246114155299237,-0.0333049234473147,
0.0758634472868355));
#70626=CARTESIAN_POINT('Ctrl Pts',(0.00248584722741736,-0.0331951640388587,
0.0759412098053713));
#70627=CARTESIAN_POINT('Ctrl Pts',(0.00251760663218272,-0.0335235895815172,
0.0757580934094324));
#70628=CARTESIAN_POINT('Ctrl Pts',(0.00253974520400812,-0.0334144449262748,
0.0758352734535725));
#70629=CARTESIAN_POINT('Ctrl Pts',(0.00256350369199788,-0.0333049234473147,
0.0759120848019999));
#70630=CARTESIAN_POINT('Ctrl Pts',(0.00258886061336342,-0.0331951640388587,
0.0759884264846476));
#70631=CARTESIAN_POINT('Ctrl Pts',(0.00261858049704053,-0.0335235895815172,
0.0758095273583538));
#70632=CARTESIAN_POINT('Ctrl Pts',(0.00264142715843697,-0.0334144449262748,
0.0758853172984448));
#70633=CARTESIAN_POINT('Ctrl Pts',(0.0026658658310034,-0.0333049234473147,
0.0759607223171644));
#70634=CARTESIAN_POINT('Ctrl Pts',(0.00269187399930949,-0.0331951640388587,
0.076035643163924));
#70635=CARTESIAN_POINT('',(0.00253643198850476,-0.0331951640388687,0.0759643955731154));
#70636=CARTESIAN_POINT('Ctrl Pts',(0.00237912174249123,-0.0332121607145971,
0.0758817263775711));
#70637=CARTESIAN_POINT('Ctrl Pts',(0.00242020630450993,-0.0332625444109943,
0.0758693414471874));
#70638=CARTESIAN_POINT('Ctrl Pts',(0.00246058291505227,-0.033313530074722,
0.0758571699285895));
#70639=CARTESIAN_POINT('Ctrl Pts',(0.00253995228355812,-0.0334167203140611,
0.0758332440533886));
#70640=CARTESIAN_POINT('Ctrl Pts',(0.00257891430115607,-0.0334688847587314,
0.0758214989634607));
#70641=CARTESIAN_POINT('Ctrl Pts',(0.00261718187050628,-0.0335216366562391,
0.075809963214774));
#70642=CARTESIAN_POINT('Ctrl Pts',(0.00265503308426364,-0.0336938721132391,
0.0759283705643767));
#70643=CARTESIAN_POINT('Ctrl Pts',(0.00266544247730287,-0.0336474569764958,
0.0759603809676342));
#70644=CARTESIAN_POINT('Ctrl Pts',(0.00267622587927018,-0.033601104548885,
0.0759922673224299));
#70645=CARTESIAN_POINT('Ctrl Pts',(0.00270352697379182,-0.0334837508592656,
0.0760729962416402));
#70646=CARTESIAN_POINT('Ctrl Pts',(0.00273320824493969,-0.0333660264659097,
0.0761528807226235));
#70647=CARTESIAN_POINT('Ctrl Pts',(0.00265456022288147,-0.0336938721132391,
0.0759292515393802));
#70648=CARTESIAN_POINT('Ctrl Pts',(0.00266497477255974,-0.0336474569764958,
0.0759612647104523));
#70649=CARTESIAN_POINT('Ctrl Pts',(0.00267576336321351,-0.033601104548885,
0.075993153772508));
#70650=CARTESIAN_POINT('Ctrl Pts',(0.00270307759429631,-0.0334837508592656,
0.076073889545878));
#70651=CARTESIAN_POINT('Ctrl Pts',(0.00273277219933971,-0.0333660264659097,
0.0761537804887477));
#70652=CARTESIAN_POINT('Ctrl Pts',(0.00249378526387214,-0.0336938721132391,
0.0762287869326754));
#70653=CARTESIAN_POINT('Ctrl Pts',(0.00250595309360374,-0.0336474569764958,
0.0762617411729333));
#70654=CARTESIAN_POINT('Ctrl Pts',(0.002518505860578,-0.033601104548885,
0.0762945507153355));
#70655=CARTESIAN_POINT('Ctrl Pts',(0.00255028658049469,-0.0334837508592656,
0.0763776169333112));
#70656=CARTESIAN_POINT('Ctrl Pts',(0.00258451476892472,-0.0333660264659097,
0.0764597049461023));
#70657=CARTESIAN_POINT('',(0.00249919351186432,-0.0336769361243754,0.0762390194271047));
#70658=CARTESIAN_POINT('',(0.00249474416025707,-0.0336938721132328,0.0762270004392665));
#70659=CARTESIAN_POINT('Ctrl Pts',(0.00249919351186441,-0.0336769361243751,
0.076239019427105));
#70660=CARTESIAN_POINT('Ctrl Pts',(0.00249844975816789,-0.0336797586670077,
0.0762370169045009));
#70661=CARTESIAN_POINT('Ctrl Pts',(0.00249770710203766,-0.0336825812712949,
0.0762350140604358));
#70662=CARTESIAN_POINT('Ctrl Pts',(0.00249622398589853,-0.0336882265975037,
0.0762310077335349));
#70663=CARTESIAN_POINT('Ctrl Pts',(0.00249548352587924,-0.0336910493194312,
0.0762290042507009));
#70664=CARTESIAN_POINT('Ctrl Pts',(0.00249474416025435,-0.0336938721132344,
0.0762270004392697));
#70665=CARTESIAN_POINT('Ctrl Pts',(0.00249919351186432,-0.0336769361243754,
0.0762390194271047));
#70666=CARTESIAN_POINT('Ctrl Pts',(0.0025384839031759,-0.0336279018505215,
0.0762244266461211));
#70667=CARTESIAN_POINT('Ctrl Pts',(0.00257833953646447,-0.0335767826010774,
0.0762096239295242));
#70668=CARTESIAN_POINT('Ctrl Pts',(0.00265643367930056,-0.0334733172064629,
0.0761806191096568));
#70669=CARTESIAN_POINT('Ctrl Pts',(0.00269472467439516,-0.0334209631456252,
0.0761663975128138));
#70670=CARTESIAN_POINT('Ctrl Pts',(0.00273227783999864,-0.0333679869844681,
0.0761524499520336));
#70671=CARTESIAN_POINT('',(0.00257465219158242,-0.0336938721132539,0.0760781259893432));
#70672=CARTESIAN_POINT('Origin',(0.00812378219310841,-0.0315241814719618,
0.07415));
#70673=CARTESIAN_POINT('',(0.00249919351308419,-0.0337108120655673,0.0762390194266585));
#70674=CARTESIAN_POINT('',(0.00250366852609151,-0.0336938721132327,0.0762510288836281));
#70675=CARTESIAN_POINT('Origin',(0.0182258276927463,-0.034556251066585,
0.0715902141959668));
#70676=CARTESIAN_POINT('Ctrl Pts',(0.00250366852609819,-0.0336938721132302,
0.0762510288836292));
#70677=CARTESIAN_POINT('Ctrl Pts',(0.00250292061121399,-0.0336910493357639,
0.076249028260651));
#70678=CARTESIAN_POINT('Ctrl Pts',(0.00250217373338578,-0.03368822660567,
0.0762470271548477));
#70679=CARTESIAN_POINT('Ctrl Pts',(0.00250068206056199,-0.0336825812712835,
0.0762430239993698));
#70680=CARTESIAN_POINT('Ctrl Pts',(0.00249993726555925,-0.033679758667002,
0.0762410219497045));
#70681=CARTESIAN_POINT('Ctrl Pts',(0.00249919351186424,-0.0336769361243751,
0.0762390194271045));
#70682=CARTESIAN_POINT('Origin',(0.0174475919152087,-0.0345562514648014,
0.0694948596281702));
#70683=CARTESIAN_POINT('Ctrl Pts',(0.00267828183148321,-0.034243627687391,
0.0760005812091178));
#70684=CARTESIAN_POINT('Ctrl Pts',(0.00274807765238379,-0.033943005420181,
0.0762059616409958));
#70685=CARTESIAN_POINT('Ctrl Pts',(0.00283314528632338,-0.0336441434784052,
0.0764055013013883));
#70686=CARTESIAN_POINT('Ctrl Pts',(0.00276384842192349,-0.034243627687391,
0.0762354819511355));
#70687=CARTESIAN_POINT('Ctrl Pts',(0.00284250367035878,-0.033943005420181,
0.0764376351858541));
#70688=CARTESIAN_POINT('Ctrl Pts',(0.00293616247741516,-0.0336441434784052,
0.0766332894888336));
#70689=CARTESIAN_POINT('Ctrl Pts',(0.00276470408782789,-0.034243627687391,
0.0762378309585557));
#70690=CARTESIAN_POINT('Ctrl Pts',(0.00284344793053853,-0.033943005420181,
0.0764399519213026));
#70691=CARTESIAN_POINT('Ctrl Pts',(0.00293719264932608,-0.0336441434784052,
0.076635567370708));
#70692=CARTESIAN_POINT('',(0.00277707261164741,-0.0341934961088741,0.0762691558818346));
#70693=CARTESIAN_POINT('',(0.00286865161518105,-0.0338664212863057,0.076487033935523));
#70694=CARTESIAN_POINT('Origin',(0.018515004651897,-0.0345610720405401,
0.0705796357915323));
#70695=CARTESIAN_POINT('Origin',(-0.00715141688422835,-0.0336938005073012,
0.0809431479026955));
#70696=CARTESIAN_POINT('',(0.00281909985087202,-0.0336938721132327,0.0763722669164541));
#70697=CARTESIAN_POINT('',(0.00284449639327672,-0.0336938721132427,0.0764293744083928));
#70698=CARTESIAN_POINT('',(0.00273227783999677,-0.0340203938281605,0.0761524499520286));
#70699=CARTESIAN_POINT('Origin',(0.0186068803369215,-0.0345589643243687,
0.0710519657530197));
#70700=CARTESIAN_POINT('',(0.00273355137358276,-0.034193496108874,0.0761519769509753));
#70701=CARTESIAN_POINT('Origin',(-0.00759642532336942,-0.0341934220717646,
0.0799886160664778));
#70702=CARTESIAN_POINT('',(0.00275531199262508,-0.034193496108884,0.0762105664164149));
#70703=CARTESIAN_POINT('Ctrl Pts',(0.00242163294752614,-0.0340223579322396,
0.0760169477714017));
#70704=CARTESIAN_POINT('Ctrl Pts',(0.00244738302649796,-0.0339125849573574,
0.0760955952813278));
#70705=CARTESIAN_POINT('Ctrl Pts',(0.00247474283189135,-0.0338030433565231,
0.0761736545597596));
#70706=CARTESIAN_POINT('Ctrl Pts',(0.00250366852609084,-0.0336938721132327,
0.0762510288836279));
#70707=CARTESIAN_POINT('Ctrl Pts',(0.00252563713712521,-0.0340223579322396,
0.0760619400860366));
#70708=CARTESIAN_POINT('Ctrl Pts',(0.00255200777746074,-0.0339125849573574,
0.0761391531069339));
#70709=CARTESIAN_POINT('Ctrl Pts',(0.00257995801756693,-0.0338030433565231,
0.0762157660601573));
#70710=CARTESIAN_POINT('Ctrl Pts',(0.00260944342872167,-0.0336938721132327,
0.0762916841391776));
#70711=CARTESIAN_POINT('Ctrl Pts',(0.00262964132672429,-0.0340223579322396,
0.0761069324006715));
#70712=CARTESIAN_POINT('Ctrl Pts',(0.00265663252842351,-0.0339125849573574,
0.0761827109325399));
#70713=CARTESIAN_POINT('Ctrl Pts',(0.00268517320324251,-0.0338030433565231,
0.076257877560555));
#70714=CARTESIAN_POINT('Ctrl Pts',(0.0027152183313525,-0.0336938721132327,
0.0763323393947272));
#70715=CARTESIAN_POINT('Ctrl Pts',(0.00273364551632336,-0.0340223579322396,
0.0761519247153065));
#70716=CARTESIAN_POINT('Ctrl Pts',(0.00276125727938629,-0.0339125849573574,
0.076226268758146));
#70717=CARTESIAN_POINT('Ctrl Pts',(0.00279038838891809,-0.0338030433565231,
0.0762999890609528));
#70718=CARTESIAN_POINT('Ctrl Pts',(0.00282099323398333,-0.0336938721132327,
0.0763729946502769));
#70719=CARTESIAN_POINT('',(0.00266138418849176,-0.0336938721132427,0.0763116479000511));
#70720=CARTESIAN_POINT('Ctrl Pts',(0.00249919351645708,-0.0337108120662681,
0.0762390194253988));
#70721=CARTESIAN_POINT('Ctrl Pts',(0.0025395023713875,-0.0337611408994432,
0.0762240483784822));
#70722=CARTESIAN_POINT('Ctrl Pts',(0.00257907567914348,-0.0338121088781598,
0.0762093505199573));
#70723=CARTESIAN_POINT('Ctrl Pts',(0.00265678725091846,-0.0339153382773232,
0.0761804877901918));
#70724=CARTESIAN_POINT('Ctrl Pts',(0.00269489263821679,-0.0339675558473112,
0.076166335129641));
#70725=CARTESIAN_POINT('Ctrl Pts',(0.00273227784003597,-0.0340203938281304,
0.0761524499520196));
#70726=CARTESIAN_POINT('Ctrl Pts',(0.00277791768151383,-0.0341934961088741,
0.0762673121793628));
#70727=CARTESIAN_POINT('Ctrl Pts',(0.00282169144277852,-0.0340287516182428,
0.0763778337166045));
#70728=CARTESIAN_POINT('Ctrl Pts',(0.0028699957391836,-0.0338644633275951,
0.0764864516125442));
#70729=CARTESIAN_POINT('Ctrl Pts',(0.00277707261164746,-0.0341934961088741,
0.0762691558818346));
#70730=CARTESIAN_POINT('Ctrl Pts',(0.00282088449000827,-0.0340287516182428,
0.0763796948902301));
#70731=CARTESIAN_POINT('Ctrl Pts',(0.00286922759303518,-0.0338644633275951,
0.0764883286669863));
#70732=CARTESIAN_POINT('Ctrl Pts',(0.00263626771762503,-0.0341934961088741,
0.0765763521758839));
#70733=CARTESIAN_POINT('Ctrl Pts',(0.00268643063735243,-0.0340287516182428,
0.0766898022145356));
#70734=CARTESIAN_POINT('Ctrl Pts',(0.00274123966999151,-0.0338644633275951,
0.0768010820407703));
#70735=CARTESIAN_POINT('',(0.00264146296832161,-0.0341764758832398,0.0765880680688096));
#70736=CARTESIAN_POINT('',(0.00263626771762762,-0.034193496108874,0.0765763521758782));
#70737=CARTESIAN_POINT('Origin',(0.0179786966131428,-0.0345621025081795,
0.0703278293545461));
#70738=CARTESIAN_POINT('Ctrl Pts',(0.00264146296845681,-0.0341764758837489,
0.0765880680669895));
#70739=CARTESIAN_POINT('Ctrl Pts',(0.0026806838197208,-0.0341260050040299,
0.0765706259619968));
#70740=CARTESIAN_POINT('Ctrl Pts',(0.00271922290453729,-0.0340749269147893,
0.0765534870070261));
#70741=CARTESIAN_POINT('Ctrl Pts',(0.00279496748398733,-0.0339715436305769,
0.0765198022818631));
#70742=CARTESIAN_POINT('Ctrl Pts',(0.00283214424516812,-0.0339192778237878,
0.0765032692964079));
#70743=CARTESIAN_POINT('Ctrl Pts',(0.00286865161362882,-0.0338664212855625,
0.0764870339344522));
#70744=CARTESIAN_POINT('',(0.00270667016464752,-0.0341934961088841,0.0764227540288665));
#70745=CARTESIAN_POINT('Origin',(0.00812378219310841,-0.0315241814719618,
0.07415));
#70746=CARTESIAN_POINT('',(0.00264146296933602,-0.0342105180190531,0.0765880680692793));
#70747=CARTESIAN_POINT('',(0.00264668323176958,-0.0341934961088739,0.0765997728400264));
#70748=CARTESIAN_POINT('Origin',(0.0179651848135109,-0.0345621701778859,
0.0702845622155633));
#70749=CARTESIAN_POINT('Origin',(0.0175625212072795,-0.0345621041234899,
0.0693919965751807));
#70750=CARTESIAN_POINT('Origin',(0.0175855946343702,-0.0345621714878735,
0.0694310119607774));
#70751=CARTESIAN_POINT('Ctrl Pts',(0.00281849032982699,-0.0346945769586965,
0.0763708963275908));
#70752=CARTESIAN_POINT('Ctrl Pts',(0.00286500789260676,-0.0345275153362944,
0.0764820177897902));
#70753=CARTESIAN_POINT('Ctrl Pts',(0.00291503215491682,-0.0343603235965185,
0.0765917050591585));
#70754=CARTESIAN_POINT('Ctrl Pts',(0.00296841034567327,-0.034193496108874,
0.0766996359283591));
#70755=CARTESIAN_POINT('Ctrl Pts',(0.00285255556015485,-0.0346945769586965,
0.0764474965133866));
#70756=CARTESIAN_POINT('Ctrl Pts',(0.00290067754449516,-0.0345275153362944,
0.0765579044656978));
#70757=CARTESIAN_POINT('Ctrl Pts',(0.0029522842041221,-0.0343603235965185,
0.0766668275830464));
#70758=CARTESIAN_POINT('Ctrl Pts',(0.00300721812151278,-0.034193496108874,
0.0767739459876756));
#70759=CARTESIAN_POINT('Ctrl Pts',(0.00288662079048272,-0.0346945769586965,
0.0765240966991827));
#70760=CARTESIAN_POINT('Ctrl Pts',(0.00293634719638359,-0.0345275153362944,
0.0766337911416053));
#70761=CARTESIAN_POINT('Ctrl Pts',(0.00298953625332745,-0.0343603235965185,
0.0767419501069332));
#70762=CARTESIAN_POINT('Ctrl Pts',(0.00304602589735237,-0.034193496108874,
0.0768482560469898));
#70763=CARTESIAN_POINT('Ctrl Pts',(0.00292068602081057,-0.0346945769586965,
0.0766006968849783));
#70764=CARTESIAN_POINT('Ctrl Pts',(0.00297201684827194,-0.0345275153362944,
0.0767096778175131));
#70765=CARTESIAN_POINT('Ctrl Pts',(0.00302678830253266,-0.0343603235965185,
0.0768170726308223));
#70766=CARTESIAN_POINT('Ctrl Pts',(0.00308483367319179,-0.034193496108874,
0.0769225661063088));
#70767=CARTESIAN_POINT('',(0.00292068602045324,-0.0346945769586966,0.0766006968841744));
#70768=CARTESIAN_POINT('',(0.00302576498982647,-0.0343667727832792,0.0768123947107075));
#70769=CARTESIAN_POINT('Origin',(0.0180526272124075,-0.0345626461567138,
0.0692711946845922));
#70770=CARTESIAN_POINT('Origin',(-0.00677090826187286,-0.0341934771027846,
0.0819286285336233));
#70771=CARTESIAN_POINT('',(0.00296910472395195,-0.034193496108874,0.07670096554053));
#70772=CARTESIAN_POINT('',(0.00299803696116878,-0.034193496108884,0.0767563656817873));
#70773=CARTESIAN_POINT('',(0.00286865161510245,-0.0345211942962685,0.0764870339338463));
#70774=CARTESIAN_POINT('Origin',(0.0182449646160614,-0.0345625596118157,
0.0697118720181048));
#70775=CARTESIAN_POINT('',(0.00286989293566145,-0.0346945769586886,0.0764864819003117));
#70776=CARTESIAN_POINT('Origin',(-0.00723910855075123,-0.0346945685853894,
0.0809821024537475));
#70777=CARTESIAN_POINT('',(0.00289528947806735,-0.0346945769587026,0.0765435893922531));
#70778=CARTESIAN_POINT('Ctrl Pts',(0.00255011181324564,-0.0345231616327842,
0.0763713055838112));
#70779=CARTESIAN_POINT('Ctrl Pts',(0.00258072938337036,-0.0344132092796988,
0.0764481307828973));
#70780=CARTESIAN_POINT('Ctrl Pts',(0.00261293444241344,-0.0343032738558979,
0.0765243187178692));
#70781=CARTESIAN_POINT('Ctrl Pts',(0.00264668323176956,-0.0341934961088739,
0.0765997728400264));
#70782=CARTESIAN_POINT('Ctrl Pts',(0.00265673568990527,-0.0345231616327842,
0.0764096785569123));
#70783=CARTESIAN_POINT('Ctrl Pts',(0.00268788217743937,-0.0344132092796988,
0.0764850340959731));
#70784=CARTESIAN_POINT('Ctrl Pts',(0.00272058572784374,-0.0343032738558979,
0.0765597415065079));
#70785=CARTESIAN_POINT('Ctrl Pts',(0.0027548019924733,-0.0341934961088739,
0.0766337061528979));
#70786=CARTESIAN_POINT('Ctrl Pts',(0.00276335956656489,-0.0345231616327842,
0.0764480515300134));
#70787=CARTESIAN_POINT('Ctrl Pts',(0.00279503497150837,-0.0344132092796988,
0.0765219374090489));
#70788=CARTESIAN_POINT('Ctrl Pts',(0.00282823701327404,-0.0343032738558979,
0.0765951642951466));
#70789=CARTESIAN_POINT('Ctrl Pts',(0.00286292075317704,-0.0341934961088739,
0.0766676394657694));
#70790=CARTESIAN_POINT('Ctrl Pts',(0.00286998344322452,-0.0345231616327842,
0.0764864245031145));
#70791=CARTESIAN_POINT('Ctrl Pts',(0.00290218776557737,-0.0344132092796988,
0.0765588407221246));
#70792=CARTESIAN_POINT('Ctrl Pts',(0.00293588829870434,-0.0343032738558979,
0.0766305870837853));
#70793=CARTESIAN_POINT('Ctrl Pts',(0.00297103951388078,-0.0341934961088739,
0.0767015727786409));
#70794=CARTESIAN_POINT('',(0.00280789397787076,-0.0341934961088839,0.0766503691902882));
#70795=CARTESIAN_POINT('Ctrl Pts',(0.00264146297248843,-0.0342105180195384,
0.0765880680678703));
#70796=CARTESIAN_POINT('Ctrl Pts',(0.00268072792119011,-0.034261055624136,
0.0765706063671259));
#70797=CARTESIAN_POINT('Ctrl Pts',(0.00271928828068896,-0.034312218987028,
0.0765534580075728));
#70798=CARTESIAN_POINT('Ctrl Pts',(0.00279503362251527,-0.0344158119695162,
0.0765197729389431));
#70799=CARTESIAN_POINT('Ctrl Pts',(0.00283218762445906,-0.0344681990450067,
0.0765032500072992));
#70800=CARTESIAN_POINT('Ctrl Pts',(0.00286865161512399,-0.0345211942962485,
0.0764870339338293));
#70801=CARTESIAN_POINT('Ctrl Pts',(0.00292141347753173,-0.0346945769586932,
0.076598804221065));
#70802=CARTESIAN_POINT('Ctrl Pts',(0.00297204077206713,-0.0345296777077528,
0.0767063595131458));
#70803=CARTESIAN_POINT('Ctrl Pts',(0.00302707016526706,-0.0343648066252516,
0.0768117304279686));
#70804=CARTESIAN_POINT('Ctrl Pts',(0.00292068602044944,-0.0346945769586932,
0.0766006968841661));
#70805=CARTESIAN_POINT('Ctrl Pts',(0.00297135244445524,-0.0345296777077528,
0.0767082672159074));
#70806=CARTESIAN_POINT('Ctrl Pts',(0.0030264215552929,-0.0343648066252516,
0.0768136515402825));
#70807=CARTESIAN_POINT('Ctrl Pts',(0.00279944798762186,-0.0346945769586932,
0.0769161282089503));
#70808=CARTESIAN_POINT('Ctrl Pts',(0.00285663573107336,-0.0345296777077528,
0.0770262050512342));
#70809=CARTESIAN_POINT('Ctrl Pts',(0.00291832418535472,-0.0343648066252516,
0.0771338242122447));
#70810=CARTESIAN_POINT('',(0.00280536863352462,-0.0346775396664985,0.0769274947709485));
#70811=CARTESIAN_POINT('',(0.002799447987626,-0.0346945769586885,0.0769161282089466));
#70812=CARTESIAN_POINT('Origin',(0.0174497406703401,-0.0345626617476886,
0.0691073113763725));
#70813=CARTESIAN_POINT('Ctrl Pts',(0.00280536863364831,-0.0346775396670096,
0.0769274947691259));
#70814=CARTESIAN_POINT('Ctrl Pts',(0.00284344685941726,-0.0346269749928347,
0.0769076087356097));
#70815=CARTESIAN_POINT('Ctrl Pts',(0.00288084833351958,-0.0345757902891115,
0.0768880760894427));
#70816=CARTESIAN_POINT('Ctrl Pts',(0.00295432866049844,-0.0344721681088523,
0.0768497016382947));
#70817=CARTESIAN_POINT('Ctrl Pts',(0.00299037870823899,-0.0344197714290315,
0.0768308748829006));
#70818=CARTESIAN_POINT('Ctrl Pts',(0.00302576498952295,-0.0343667727831574,
0.0768123947104756));
#70819=CARTESIAN_POINT('',(0.00286006700404961,-0.0346945769587026,0.0767584125465705));
#70820=CARTESIAN_POINT('Origin',(0.00812378219310841,-0.0315241814719618,
0.07415));
#70821=CARTESIAN_POINT('',(0.00280536863491102,-0.0347116136489604,0.0769274947710576));
#70822=CARTESIAN_POINT('',(0.00281131354479945,-0.0346945769586885,0.0769388486622199));
#70823=CARTESIAN_POINT('Origin',(0.0174271276195662,-0.0345626679652983,
0.0690680433225043));
#70824=CARTESIAN_POINT('Origin',(0.0175911330836941,-0.0345626630821519,
0.0693780458598815));
#70825=CARTESIAN_POINT('Origin',(0.0176104315067095,-0.03456266930565,0.069419044940195));
#70826=CARTESIAN_POINT('Ctrl Pts',(0.00295204013945966,-0.0352450361874068,
0.0766663161081523));
#70827=CARTESIAN_POINT('Ctrl Pts',(0.00304694455878776,-0.0349452760959492,
0.0768613715604168));
#70828=CARTESIAN_POINT('Ctrl Pts',(0.00315627173941708,-0.034644428984174,
0.0770487242914932));
#70829=CARTESIAN_POINT('Ctrl Pts',(0.0029531949308012,-0.0352450361874068,
0.0766685615662252));
#70830=CARTESIAN_POINT('Ctrl Pts',(0.0030481840389702,-0.0349452760959492,
0.0768635734648196));
#70831=CARTESIAN_POINT('Ctrl Pts',(0.0031575923872077,-0.034644428984174,
0.0770508763868473));
#70832=CARTESIAN_POINT('Ctrl Pts',(0.00306753070719105,-0.0352450361874068,
0.0768908841477084));
#70833=CARTESIAN_POINT('Ctrl Pts',(0.0031709048491127,-0.0349452760959492,
0.0770815838017356));
#70834=CARTESIAN_POINT('Ctrl Pts',(0.00328834959419955,-0.034644428984174,
0.0772639551347779));
#70835=CARTESIAN_POINT('Ctrl Pts',(0.00306867406495496,-0.0352450361874068,
0.0768931073735232));
#70836=CARTESIAN_POINT('Ctrl Pts',(0.00317213205721413,-0.0349452760959492,
0.0770837639051047));
#70837=CARTESIAN_POINT('Ctrl Pts',(0.00328965716626947,-0.034644428984174,
0.0772660859222573));
#70838=CARTESIAN_POINT('',(0.00308481599410115,-0.0351951634053267,0.0769225388992395));
#70839=CARTESIAN_POINT('',(0.00320299790920465,-0.0348678972925388,0.0771272482313852));
#70840=CARTESIAN_POINT('Origin',(0.0173149102123577,-0.0345636767888238,
0.0680959362170143));
#70841=CARTESIAN_POINT('Origin',(-0.00625109662106326,-0.0346946199340714,
0.0828473081894833));
#70842=CARTESIAN_POINT('',(0.00313945274522816,-0.0346945769330289,0.0770195966533715));
#70843=CARTESIAN_POINT('',(0.00317180649912508,-0.0346945769458128,0.0770730708125184));
#70844=CARTESIAN_POINT('',(0.00302576498971699,-0.0350221583435276,0.0768123947103925));
#70845=CARTESIAN_POINT('Origin',(0.0175983524926475,-0.0345628458717151,
0.0684842709518878));
#70846=CARTESIAN_POINT('',(0.00302685996691316,-0.0351951360298762,0.0768118194559413));
#70847=CARTESIAN_POINT('Origin',(-0.0067403848516491,-0.0351951838366744,
0.0819126794330099));
#70848=CARTESIAN_POINT('',(0.00308483367267652,-0.0351951371328749,0.0769225661055733));
#70849=CARTESIAN_POINT('Ctrl Pts',(0.00270058752120605,-0.0350241211494343,
0.0767168968718439));
#70850=CARTESIAN_POINT('Ctrl Pts',(0.00273594547314701,-0.0349144232818962,
0.0767915991548529));
#70851=CARTESIAN_POINT('Ctrl Pts',(0.00277286873809569,-0.0348045283579412,
0.076865615276647));
#70852=CARTESIAN_POINT('Ctrl Pts',(0.00281131354996476,-0.0346945769439158,
0.0769388486720593));
#70853=CARTESIAN_POINT('Ctrl Pts',(0.00280941048797988,-0.0350241211494343,
0.0767484991455839));
#70854=CARTESIAN_POINT('Ctrl Pts',(0.00284520374828418,-0.0349144232818962,
0.0768217024368448));
#70855=CARTESIAN_POINT('Ctrl Pts',(0.00288253159691867,-0.0348045283579412,
0.076894209671537));
#70856=CARTESIAN_POINT('Ctrl Pts',(0.00292134967765577,-0.0346945769439158,
0.0769659261979021));
#70857=CARTESIAN_POINT('Ctrl Pts',(0.00291823345475372,-0.0350241211494343,
0.0767801014193239));
#70858=CARTESIAN_POINT('Ctrl Pts',(0.00295446202342134,-0.0349144232818962,
0.0768518057188366));
#70859=CARTESIAN_POINT('Ctrl Pts',(0.00299219445574165,-0.0348045283579412,
0.0769228040664269));
#70860=CARTESIAN_POINT('Ctrl Pts',(0.00303138580534677,-0.0346945769439158,
0.0769930037237449));
#70861=CARTESIAN_POINT('Ctrl Pts',(0.00302705642152756,-0.0350241211494343,
0.0768117036930639));
#70862=CARTESIAN_POINT('Ctrl Pts',(0.00306372029855851,-0.0349144232818962,
0.0768819090008284));
#70863=CARTESIAN_POINT('Ctrl Pts',(0.00310185731456463,-0.0348045283579412,
0.0769513984613169));
#70864=CARTESIAN_POINT('Ctrl Pts',(0.00314142193303777,-0.0346945769439158,
0.0770200812495877));
#70865=CARTESIAN_POINT('',(0.00297538314480101,-0.0346945769458128,0.076979222657589));
#70866=CARTESIAN_POINT('Ctrl Pts',(0.00280536863782169,-0.0347116136492789,
0.0769274947695302));
#70867=CARTESIAN_POINT('Ctrl Pts',(0.00284343174786804,-0.0347621546532333,
0.0769076166446031));
#70868=CARTESIAN_POINT('Ctrl Pts',(0.00288082560558245,-0.034813308409711,
0.0768880880308286));
#70869=CARTESIAN_POINT('Ctrl Pts',(0.00295430602405962,-0.0349168561544566,
0.0768497135276311));
#70870=CARTESIAN_POINT('Ctrl Pts',(0.0029903634388798,-0.0349692089015919,
0.0768308828594206));
#70871=CARTESIAN_POINT('Ctrl Pts',(0.00302576498975863,-0.0350221583435,
0.0768123947103933));
#70872=CARTESIAN_POINT('Ctrl Pts',(0.00308527177353325,-0.0351951371254878,
0.0769211702232192));
#70873=CARTESIAN_POINT('Ctrl Pts',(0.00314256397920663,-0.0350307338980923,
0.0770253382648744));
#70874=CARTESIAN_POINT('Ctrl Pts',(0.0032041126065885,-0.0348659306897825,
0.0771270493468694));
#70875=CARTESIAN_POINT('Ctrl Pts',(0.00308483367277792,-0.0351951371254878,
0.0769225661055166));
#70876=CARTESIAN_POINT('Ctrl Pts',(0.003142154737442,-0.0350307338980923,
0.07702674320463));
#70877=CARTESIAN_POINT('Ctrl Pts',(0.00320373257350924,-0.0348659306897825,
0.0771284621435705));
#70878=CARTESIAN_POINT('Ctrl Pts',(0.00301140752959325,-0.0351951371254878,
0.0771565174333589));
#70879=CARTESIAN_POINT('Ctrl Pts',(0.00307356539117437,-0.0350307338980923,
0.0772622125719135));
#70880=CARTESIAN_POINT('Ctrl Pts',(0.00314003863335222,-0.0348659306897825,
0.0773652483431038));
#70881=CARTESIAN_POINT('Origin',(-0.00134716617794425,-0.0308609197410127,
0.0798802581581213));
#70882=CARTESIAN_POINT('',(0.00305282152988927,-0.0351951371254878,0.0770245636095533));
#70883=CARTESIAN_POINT('Origin',(0.0088776768623139,-0.0351840467441197,
0.0735283984580129));
#70884=CARTESIAN_POINT('Origin',(-0.00167966696799405,-0.0352322612925457,
0.0810102763570714));
#70885=CARTESIAN_POINT('',(0.00332966794130894,-0.0351951142564661,0.07732715015763));
#70886=CARTESIAN_POINT('',(0.00340076684006047,-0.0351951372916787,0.0774295771030537));
#70887=CARTESIAN_POINT('Origin',(0.00843588221042041,-0.0352875123163659,
0.074286406577489));
#70888=CARTESIAN_POINT('Origin',(0.00510351715950868,-0.0298325076522393,
0.0672817258785396));
#70889=CARTESIAN_POINT('Origin',(-5.41234501965848E-5,-0.033873131987072,
0.0759873405662144));
#70890=CARTESIAN_POINT('Ctrl Pts',(0.00237776779016926,-0.0321934096636941,
0.0739021003700527));
#70891=CARTESIAN_POINT('Ctrl Pts',(0.00237333050484116,-0.0320508460843169,
0.0740049512916559));
#70892=CARTESIAN_POINT('Ctrl Pts',(0.00237165996656505,-0.0319086045660766,
0.0741078438844261));
#70893=CARTESIAN_POINT('Ctrl Pts',(0.00237274153327594,-0.0317669892864456,
0.0742105563063861));
#70894=CARTESIAN_POINT('Ctrl Pts',(0.00237597585284884,-0.0321934096636941,
0.0739859288949626));
#70895=CARTESIAN_POINT('Ctrl Pts',(0.00237303905819812,-0.0320508460843169,
0.0740888118913904));
#70896=CARTESIAN_POINT('Ctrl Pts',(0.00237286874101169,-0.0319086045660766,
0.0741916962195769));
#70897=CARTESIAN_POINT('Ctrl Pts',(0.00237544703044969,-0.0317669892864456,
0.0742943603212735));
#70898=CARTESIAN_POINT('Ctrl Pts',(0.00237418391552844,-0.0321934096636941,
0.0740697574198723));
#70899=CARTESIAN_POINT('Ctrl Pts',(0.00237274761155508,-0.0320508460843169,
0.074172672491125));
#70900=CARTESIAN_POINT('Ctrl Pts',(0.00237407751545835,-0.0319086045660766,
0.0742755485547279));
#70901=CARTESIAN_POINT('Ctrl Pts',(0.00237815252762344,-0.0317669892864456,
0.074378164336161));
#70902=CARTESIAN_POINT('Ctrl Pts',(0.00237239197820803,-0.0321934096636941,
0.0741535859447821));
#70903=CARTESIAN_POINT('Ctrl Pts',(0.00237245616491203,-0.0320508460843169,
0.0742565330908595));
#70904=CARTESIAN_POINT('Ctrl Pts',(0.00237528628990499,-0.0319086045660766,
0.0743594008898788));
#70905=CARTESIAN_POINT('Ctrl Pts',(0.00238085802479719,-0.0317669892864456,
0.0744619683510483));
#70906=CARTESIAN_POINT('',(0.00237242403632313,-0.0321934096636941,0.0741520862359061));
#70907=CARTESIAN_POINT('',(0.00237736578083819,-0.0318665617511273,0.0743883766050468));
#70908=CARTESIAN_POINT('Origin',(0.0190711415859749,-0.0326371944419006,
0.0747609680271806));
#70909=CARTESIAN_POINT('Origin',(-0.0085744009303593,-0.0316939261509138,
0.0748426849382173));
#70910=CARTESIAN_POINT('',(0.00237377816213862,-0.0320197221621803,0.0740273508648053));
#70911=CARTESIAN_POINT('Ctrl Pts',(0.00237372717616906,-0.0320197392094719,
0.074027528671752));
#70912=CARTESIAN_POINT('Ctrl Pts',(0.00237310404960662,-0.0319792716576016,
0.0740567868012731));
#70913=CARTESIAN_POINT('Ctrl Pts',(0.00237270113853826,-0.0319386439829655,
0.0740861828754044));
#70914=CARTESIAN_POINT('Ctrl Pts',(0.00237252647670892,-0.0318979099381587,
0.0741157478703721));
#70915=CARTESIAN_POINT('Ctrl Pts',(0.0023723518183319,-0.0318571766984894,
0.0741453122809667));
#70916=CARTESIAN_POINT('Ctrl Pts',(0.00237240450624418,-0.0318163871833549,
0.0741748953295478));
#70917=CARTESIAN_POINT('Ctrl Pts',(0.00237268083807216,-0.0317755399638303,
0.0742043952688851));
#70918=CARTESIAN_POINT('',(0.00237509545404048,-0.0321934096636183,0.074027114785002));
#70919=CARTESIAN_POINT('Origin',(6.75629272769168E-5,-0.03241117574553,
0.0739988197263972));
#70920=CARTESIAN_POINT('',(0.0023737597451918,-0.0321934096636663,0.074089600510464));
#70921=CARTESIAN_POINT('Ctrl Pts',(0.00237388852889845,-0.0321934096636617,
0.0741506830435188));
#70922=CARTESIAN_POINT('Ctrl Pts',(0.00237389794860091,-0.0320835708272591,
0.0742299785583533));
#70923=CARTESIAN_POINT('Ctrl Pts',(0.00237554837939786,-0.0319739230346488,
0.0743092278836263));
#70924=CARTESIAN_POINT('Ctrl Pts',(0.00237882992797032,-0.0318646057455572,
0.0743883297873848));
#70925=CARTESIAN_POINT('Ctrl Pts',(0.00229206583874311,-0.0321934096636617,
0.0742290808249946));
#70926=CARTESIAN_POINT('Ctrl Pts',(0.00229315642495177,-0.0320835708272591,
0.0743095047384952));
#70927=CARTESIAN_POINT('Ctrl Pts',(0.00229591074728617,-0.0319739230346488,
0.0743898594332326));
#70928=CARTESIAN_POINT('Ctrl Pts',(0.00230031739153543,-0.0318646057455572,
0.0744700423714043));
#70929=CARTESIAN_POINT('Ctrl Pts',(0.00221024314858776,-0.0321934096636617,
0.0743074786064704));
#70930=CARTESIAN_POINT('Ctrl Pts',(0.00221241490130264,-0.0320835708272591,
0.0743890309186371));
#70931=CARTESIAN_POINT('Ctrl Pts',(0.00221627311517448,-0.0319739230346488,
0.074470490982839));
#70932=CARTESIAN_POINT('Ctrl Pts',(0.00222180485510055,-0.0318646057455572,
0.0745517549554239));
#70933=CARTESIAN_POINT('Ctrl Pts',(0.00212842045843242,-0.0321934096636617,
0.0743858763879462));
#70934=CARTESIAN_POINT('Ctrl Pts',(0.0021316733776535,-0.0320835708272591,
0.0744685570987791));
#70935=CARTESIAN_POINT('Ctrl Pts',(0.00213663548306279,-0.0319739230346488,
0.0745511225324453));
#70936=CARTESIAN_POINT('Ctrl Pts',(0.00214329231866566,-0.0318646057455572,
0.0746334675394434));
#70937=CARTESIAN_POINT('',(0.00212893797363555,-0.0321763980308259,0.0743986820498694));
#70938=CARTESIAN_POINT('',(0.00212842045843431,-0.0321934096636184,0.0743858763879783));
#70939=CARTESIAN_POINT('Origin',(0.018676471018924,-0.0326386230645992,
0.0743262766362804));
#70940=CARTESIAN_POINT('Ctrl Pts',(0.00212893797680168,-0.0321763980306269,
0.0743986820497332));
#70941=CARTESIAN_POINT('Ctrl Pts',(0.0021718199901083,-0.0321259596175228,
0.0743969031900029));
#70942=CARTESIAN_POINT('Ctrl Pts',(0.00221395901689214,-0.0320749164632234,
0.0743951551513188));
#70943=CARTESIAN_POINT('Ctrl Pts',(0.00229678500966819,-0.0319716057793904,
0.0743917193093));
#70944=CARTESIAN_POINT('Ctrl Pts',(0.00233743970376939,-0.0319193786690102,
0.0743900328446889));
#70945=CARTESIAN_POINT('Ctrl Pts',(0.0023773657826883,-0.0318665617525285,
0.0743883766049627));
#70946=CARTESIAN_POINT('',(0.00225042224738872,-0.0321934096636663,0.0742689813119522));
#70947=CARTESIAN_POINT('Origin',(0.00812378219310841,-0.0315241814719618,
0.07415));
#70948=CARTESIAN_POINT('',(0.00212893797326352,-0.0322104233323776,0.0743986820498849));
#70949=CARTESIAN_POINT('',(0.00212948283705857,-0.0321934096636183,0.0744114865772715));
#70950=CARTESIAN_POINT('Origin',(0.0186809237928152,-0.032638722891123,
0.0742811607215313));
#70951=CARTESIAN_POINT('Origin',(0.0186256182595173,-0.0326386247204135,
0.07310032358825));
#70952=CARTESIAN_POINT('Origin',(0.0186337858873733,-0.0326387241141357,
0.0731449165497552));
#70953=CARTESIAN_POINT('Ctrl Pts',(0.00237294299327498,-0.0327445246967096,
0.0742272884057232));
#70954=CARTESIAN_POINT('Ctrl Pts',(0.0023758579731503,-0.0324436878339359,
0.0744441848519215));
#70955=CARTESIAN_POINT('Ctrl Pts',(0.00239510219866997,-0.0321434074405927,
0.0746602455500255));
#70956=CARTESIAN_POINT('Ctrl Pts',(0.00238173477963596,-0.0327445246967096,
0.0744771337668821));
#70957=CARTESIAN_POINT('Ctrl Pts',(0.00239407283135373,-0.0324436878339359,
0.0746936986254369));
#70958=CARTESIAN_POINT('Ctrl Pts',(0.00242268838222746,-0.0321434074405927,
0.0749087188936194));
#70959=CARTESIAN_POINT('',(0.00238390402370576,-0.0326943950436612,0.0745132128858064));
#70960=CARTESIAN_POINT('',(0.00240367281091007,-0.0323666188837389,0.0747487266953189));
#70961=CARTESIAN_POINT('Origin',(0.019156326270843,-0.0326395579110921,
0.0733757111555328));
#70962=CARTESIAN_POINT('Origin',(-0.00858092611035353,-0.0321933825603038,
0.0758984911828047));
#70963=CARTESIAN_POINT('',(0.00239201124118077,-0.0321934096532689,0.0746242644318081));
#70964=CARTESIAN_POINT('',(0.00239851760275117,-0.0321934096584275,0.0746864248501227));
#70965=CARTESIAN_POINT('',(0.00237736577988581,-0.0325210109756238,0.0743883766050745));
#70966=CARTESIAN_POINT('Origin',(0.0191613237731052,-0.0326393129154959,
0.0738565016030731));
#70967=CARTESIAN_POINT('',(0.00237872314766527,-0.0326943950436593,0.0743883202978606));
#70968=CARTESIAN_POINT('Origin',(-0.00867422623493687,-0.032694376553816,
0.0748468250876423));
#70969=CARTESIAN_POINT('',(0.00238131358569552,-0.0326943950436702,0.0744507665918435));
#70970=CARTESIAN_POINT('Ctrl Pts',(0.00212379740907037,-0.0325229783203769,
0.074163512636487));
#70971=CARTESIAN_POINT('Ctrl Pts',(0.00212398368046884,-0.032413025309245,
0.0742462222955239));
#70972=CARTESIAN_POINT('Ctrl Pts',(0.00212588087916087,-0.0323031222208069,
0.0743289155567573));
#70973=CARTESIAN_POINT('Ctrl Pts',(0.00212948283725399,-0.0321934096576658,
0.0744114865817515));
#70974=CARTESIAN_POINT('Ctrl Pts',(0.00220880776720183,-0.0325229783203769,
0.0742384418113572));
#70975=CARTESIAN_POINT('Ctrl Pts',(0.0022100269356373,-0.032413025309245,
0.0743199796044664));
#70976=CARTESIAN_POINT('Ctrl Pts',(0.00221293263315515,-0.0323031222208069,
0.0744014798107064));
#70977=CARTESIAN_POINT('Ctrl Pts',(0.00221751745397346,-0.0321934096576658,
0.074482838165444));
#70978=CARTESIAN_POINT('Ctrl Pts',(0.00229381812533329,-0.0325229783203769,
0.0743133709862274));
#70979=CARTESIAN_POINT('Ctrl Pts',(0.00229607019080575,-0.032413025309245,
0.0743937369134088));
#70980=CARTESIAN_POINT('Ctrl Pts',(0.00229998438714944,-0.0323031222208069,
0.0744740440646555));
#70981=CARTESIAN_POINT('Ctrl Pts',(0.00230555207069293,-0.0321934096576658,
0.0745541897491365));
#70982=CARTESIAN_POINT('Ctrl Pts',(0.00237882848346475,-0.0325229783203769,
0.0743883001610976));
#70983=CARTESIAN_POINT('Ctrl Pts',(0.0023821134459742,-0.032413025309245,
0.0744674942223513));
#70984=CARTESIAN_POINT('Ctrl Pts',(0.00238703614114373,-0.0323031222208069,
0.0745466083186045));
#70985=CARTESIAN_POINT('Ctrl Pts',(0.00239358668741239,-0.0321934096576658,
0.074625541332829));
#70986=CARTESIAN_POINT('',(0.00226074703894315,-0.0321934096584275,0.0745178755040674));
#70987=CARTESIAN_POINT('Ctrl Pts',(0.0021289379767339,-0.0322104233328922,
0.074398682049736));
#70988=CARTESIAN_POINT('Ctrl Pts',(0.00217187809590104,-0.0322609421831419,
0.0743969007796203));
#70989=CARTESIAN_POINT('Ctrl Pts',(0.00221404550838051,-0.0323120888240847,
0.0743951515634291));
#70990=CARTESIAN_POINT('Ctrl Pts',(0.00229687212817822,-0.032415652463181,
0.0743917156953997));
#70991=CARTESIAN_POINT('Ctrl Pts',(0.00233749728942868,-0.0324680267167306,
0.0743900304558829));
#70992=CARTESIAN_POINT('Ctrl Pts',(0.00237736577992929,-0.0325210109755912,
0.0743883766050771));
#70993=CARTESIAN_POINT('Origin',(0.0087468097105921,-0.0262834582511982,
0.0663068359349611));
#70994=CARTESIAN_POINT('Origin',(-0.00296606493112828,-0.0342770791904115,
0.0691661651794213));
#70995=CARTESIAN_POINT('Ctrl Pts',(0.00238527718595703,-0.0326943950436604,
0.0745117208682917));
#70996=CARTESIAN_POINT('Ctrl Pts',(0.00239026237745925,-0.0325844576448134,
0.0745908082223948));
#70997=CARTESIAN_POINT('Ctrl Pts',(0.00239688357791956,-0.0324744968375322,
0.0746697980716994));
#70998=CARTESIAN_POINT('Ctrl Pts',(0.0024051309079293,-0.0323646534831894,
0.0747485893268164));
#70999=CARTESIAN_POINT('Ctrl Pts',(0.00230853870272208,-0.0326943950436604,
0.0745951015181593));
#71000=CARTESIAN_POINT('Ctrl Pts',(0.00231467303585146,-0.0325844576448134,
0.0746752464723846));
#71001=CARTESIAN_POINT('Ctrl Pts',(0.00232246533216997,-0.0324744968375322,
0.0747552702305265));
#71002=CARTESIAN_POINT('Ctrl Pts',(0.00233190419352096,-0.0323646534831894,
0.0748350703991877));
#71003=CARTESIAN_POINT('Ctrl Pts',(0.00223180021948713,-0.0326943950436604,
0.0746784821680268));
#71004=CARTESIAN_POINT('Ctrl Pts',(0.00223908369424368,-0.0325844576448134,
0.0747596847223744));
#71005=CARTESIAN_POINT('Ctrl Pts',(0.00224804708642038,-0.0324744968375322,
0.0748407423893536));
#71006=CARTESIAN_POINT('Ctrl Pts',(0.00225867747911263,-0.0323646534831894,
0.0749215514715591));
#71007=CARTESIAN_POINT('Ctrl Pts',(0.00215506173625218,-0.0326943950436604,
0.0747618628178944));
#71008=CARTESIAN_POINT('Ctrl Pts',(0.0021634943526359,-0.0325844576448134,
0.0748441229723642));
#71009=CARTESIAN_POINT('Ctrl Pts',(0.0021736288406708,-0.0324744968375322,
0.0749262145481808));
#71010=CARTESIAN_POINT('Ctrl Pts',(0.0021854507647043,-0.0323646534831894,
0.0750080325439304));
#71011=CARTESIAN_POINT('',(0.00215638230421628,-0.0326773559991335,0.0747746107157097));
#71012=CARTESIAN_POINT('',(0.00215506173625341,-0.0326943950436594,0.0747618628178938));
#71013=CARTESIAN_POINT('Origin',(0.0186660739182752,-0.0326395670545172,
0.0729960178679478));
#71014=CARTESIAN_POINT('Ctrl Pts',(0.00215638230754539,-0.0326773559987419,
0.074774610715356));
#71015=CARTESIAN_POINT('Ctrl Pts',(0.00219910235802171,-0.0326267922586414,
0.0747701391864154));
#71016=CARTESIAN_POINT('Ctrl Pts',(0.00224106522645314,-0.0325756109580267,
0.0747657469120963));
#71017=CARTESIAN_POINT('Ctrl Pts',(0.0023235123118499,-0.0324719985462364,
0.0747571171346427));
#71018=CARTESIAN_POINT('Ctrl Pts',(0.00236396346142973,-0.0324196091621776,
0.074752883092688));
#71019=CARTESIAN_POINT('Ctrl Pts',(0.00240367281095859,-0.0323666188837757,
0.0747487266953138));
#71020=CARTESIAN_POINT('',(0.00226948287998959,-0.0326943950436702,0.0746375378518601));
#71021=CARTESIAN_POINT('Origin',(0.00812378219310841,-0.0315241814719618,
0.07415));
#71022=CARTESIAN_POINT('',(0.00215638230425946,-0.0327114338380047,0.0747746107157052));
#71023=CARTESIAN_POINT('',(0.00215773009560762,-0.0326943950436593,0.0747873557640231));
#71024=CARTESIAN_POINT('Origin',(0.0186605887082149,-0.0326395662378234,
0.0729510394200869));
#71025=CARTESIAN_POINT('Origin',(0.0186765368098082,-0.0326395681387481,
0.0730959516853406));
#71026=CARTESIAN_POINT('Origin',(0.0186804785953922,-0.0326395674485255,
0.0731410915149567));
#71027=CARTESIAN_POINT('Ctrl Pts',(0.00238914692877785,-0.0332451089994433,
0.0745882731854638));
#71028=CARTESIAN_POINT('Ctrl Pts',(0.00240567667240838,-0.0329451141710254,
0.074804558493071));
#71029=CARTESIAN_POINT('Ctrl Pts',(0.00243845095033208,-0.0326442513127494,
0.0750189842690818));
#71030=CARTESIAN_POINT('Ctrl Pts',(0.00241361098337932,-0.0332451089994433,
0.0748370733262042));
#71031=CARTESIAN_POINT('Ctrl Pts',(0.00243952437784246,-0.0329451141710254,
0.0750524359568965));
#71032=CARTESIAN_POINT('Ctrl Pts',(0.0024815861488399,-0.0326442513127494,
0.0752652348622784));
#71033=CARTESIAN_POINT('Ctrl Pts',(0.00241385562392534,-0.0332451089994433,
0.0748395613276117));
#71034=CARTESIAN_POINT('Ctrl Pts',(0.0024398628548968,-0.0329451141710254,
0.0750549147315347));
#71035=CARTESIAN_POINT('Ctrl Pts',(0.00248201750082498,-0.0326442513127494,
0.0752676973682104));
#71036=CARTESIAN_POINT('',(0.00241803668792225,-0.0331951640388616,0.0748729061004368));
#71037=CARTESIAN_POINT('',(0.00245255449673062,-0.0328677532354998,0.0751067138995858));
#71038=CARTESIAN_POINT('Origin',(0.0189351097397747,-0.0326402808282397,
0.0720061055721766));
#71039=CARTESIAN_POINT('Origin',(-0.00844931148379163,-0.0326944278779101,
0.076946197824319));
#71040=CARTESIAN_POINT('',(0.00243310089257869,-0.0326943950436593,0.0749832294616745));
#71041=CARTESIAN_POINT('',(0.00244349750017906,-0.0326943950436693,0.0750448586800035));
#71042=CARTESIAN_POINT('',(0.00240367281090978,-0.0330220786163545,0.074748726695316));
#71043=CARTESIAN_POINT('Origin',(0.0190458952612445,-0.0326396682766514,
0.0724739508603131));
#71044=CARTESIAN_POINT('',(0.00240502396467458,-0.0331951640388587,0.0747485852693819));
#71045=CARTESIAN_POINT('Origin',(-0.00856669033432262,-0.0331952026560096,
0.0758969993447738));
#71046=CARTESIAN_POINT('',(0.00241153032630842,-0.0331951640388701,0.0748107456849194));
#71047=CARTESIAN_POINT('Ctrl Pts',(0.00213648553643562,-0.0330240426238172,
0.0745402290929985));
#71048=CARTESIAN_POINT('Ctrl Pts',(0.00214186132237346,-0.032914277406352,
0.0746227099375847));
#71049=CARTESIAN_POINT('Ctrl Pts',(0.00214894489779314,-0.0328043479726691,
0.0747051207693682));
#71050=CARTESIAN_POINT('Ctrl Pts',(0.00215773009560757,-0.0326943950436594,
0.0747873557640232));
#71051=CARTESIAN_POINT('Ctrl Pts',(0.00222603297718474,-0.0330240426238172,
0.0746096725364601));
#71052=CARTESIAN_POINT('Ctrl Pts',(0.00223236541421173,-0.032914277406352,
0.0746909197778081));
#71053=CARTESIAN_POINT('Ctrl Pts',(0.00224038061562119,-0.0328043479726691,
0.0747720766147069));
#71054=CARTESIAN_POINT('Ctrl Pts',(0.0022500711766021,-0.0326943950436594,
0.0748530387964234));
#71055=CARTESIAN_POINT('Ctrl Pts',(0.00231558041793386,-0.0330240426238172,
0.0746791159799217));
#71056=CARTESIAN_POINT('Ctrl Pts',(0.00232286950605001,-0.032914277406352,
0.0747591296180316));
#71057=CARTESIAN_POINT('Ctrl Pts',(0.00233181633344924,-0.0328043479726691,
0.0748390324600457));
#71058=CARTESIAN_POINT('Ctrl Pts',(0.00234241225759662,-0.0326943950436594,
0.0749187218288236));
#71059=CARTESIAN_POINT('Ctrl Pts',(0.00240512785868298,-0.0330240426238172,
0.0747485594233833));
#71060=CARTESIAN_POINT('Ctrl Pts',(0.00241337359788828,-0.032914277406352,
0.074827339458255));
#71061=CARTESIAN_POINT('Ctrl Pts',(0.00242325205127729,-0.0328043479726691,
0.0749059883053845));
#71062=CARTESIAN_POINT('Ctrl Pts',(0.00243475333859115,-0.0326943950436594,
0.0749844048612238));
#71063=CARTESIAN_POINT('',(0.00229541549410315,-0.0326943950436694,0.0748852926128588));
#71064=CARTESIAN_POINT('Ctrl Pts',(0.00215638230755161,-0.0327114338383319,
0.0747746107153553));
#71065=CARTESIAN_POINT('Ctrl Pts',(0.00219909525233674,-0.0327619876831146,
0.074770139930171));
#71066=CARTESIAN_POINT('Ctrl Pts',(0.00224105465004281,-0.0328131562604706,
0.0747657480191344));
#71067=CARTESIAN_POINT('Ctrl Pts',(0.00232350165961882,-0.0329167375858765,
0.074757118249617));
#71068=CARTESIAN_POINT('Ctrl Pts',(0.00236395642039812,-0.0329691088920619,
0.0747528838296762));
#71069=CARTESIAN_POINT('Ctrl Pts',(0.00240367281095737,-0.0330220786163186,
0.0747487266953138));
#71070=CARTESIAN_POINT('Ctrl Pts',(0.00241931365983049,-0.0331951640388604,
0.0748713305540121));
#71071=CARTESIAN_POINT('Ctrl Pts',(0.00243422670656056,-0.0330306422010619,
0.0749892667835727));
#71072=CARTESIAN_POINT('Ctrl Pts',(0.00245400143858907,-0.0328657861914645,
0.0751064858655472));
#71073=CARTESIAN_POINT('Ctrl Pts',(0.00241803668792191,-0.0331951640388604,
0.0748729061004337));
#71074=CARTESIAN_POINT('Ctrl Pts',(0.00243298230806411,-0.0330306422010619,
0.0749908687305697));
#71075=CARTESIAN_POINT('Ctrl Pts',(0.00245279067683453,-0.0328657861914645,
0.0751081128442673));
#71076=CARTESIAN_POINT('Ctrl Pts',(0.0022052588268649,-0.0331951640388604,
0.0751354345048016));
#71077=CARTESIAN_POINT('Ctrl Pts',(0.00222563205344984,-0.0330306422010619,
0.0752577961807944));
#71078=CARTESIAN_POINT('Ctrl Pts',(0.00225104520800275,-0.0328657861914645,
0.0753792112527129));
#71079=CARTESIAN_POINT('',(0.00220737723472213,-0.0331781648281902,0.0751480743279835));
#71080=CARTESIAN_POINT('',(0.00220525882686678,-0.0331951640388588,0.0751354345048006));
#71081=CARTESIAN_POINT('Origin',(0.0183658543510097,-0.0326412091878594,
0.0716998723397664));
#71082=CARTESIAN_POINT('Ctrl Pts',(0.00220737723551375,-0.033178164828644,
0.0751480743263201));
#71083=CARTESIAN_POINT('Ctrl Pts',(0.00224976137579082,-0.0331276811546775,
0.0751409242756966));
#71084=CARTESIAN_POINT('Ctrl Pts',(0.00229138018412607,-0.0330765663497782,
0.075133903299499));
#71085=CARTESIAN_POINT('Ctrl Pts',(0.00237312292174858,-0.0329730614463176,
0.0751201136235957));
#71086=CARTESIAN_POINT('Ctrl Pts',(0.00241321382965176,-0.0329207133373706,
0.0751133504999028));
#71087=CARTESIAN_POINT('Ctrl Pts',(0.00245255448581311,-0.0328677532289357,
0.0751067138872499));
#71088=CARTESIAN_POINT('',(0.00231164775740451,-0.0331951640388701,0.0750041703026287));
#71089=CARTESIAN_POINT('Origin',(0.00812378219310841,-0.0315241814719618,
0.07415));
#71090=CARTESIAN_POINT('',(0.00220737723635824,-0.033212160714422,0.0751480743283634));
#71091=CARTESIAN_POINT('',(0.00220952263615501,-0.0331951640388587,0.0751607095987539));
#71092=CARTESIAN_POINT('Origin',(0.0183506938193972,-0.0326413645221128,
0.0716571354312258));
#71093=CARTESIAN_POINT('Origin',(0.0186028220668772,-0.0326412102403194,
0.0731045558557979));
#71094=CARTESIAN_POINT('Origin',(0.0186025147681812,-0.0326413657479853,
0.0731499018936054));
#71095=CARTESIAN_POINT('Ctrl Pts',(0.00242797943404241,-0.0337436976235975,
0.0749474684506714));
#71096=CARTESIAN_POINT('Ctrl Pts',(0.00243515198614739,-0.0336723290703325,
0.074998697363909));
#71097=CARTESIAN_POINT('Ctrl Pts',(0.00244324482458147,-0.033601104548885,
0.0750497889779105));
#71098=CARTESIAN_POINT('Ctrl Pts',(0.00246908365460051,-0.0333736987606857,
0.0752129143807388));
#71099=CARTESIAN_POINT('Ctrl Pts',(0.00250424098045896,-0.0331450831799192,
0.0753742881847566));
#71100=CARTESIAN_POINT('Ctrl Pts',(0.002468016610698,-0.0337436976235975,
0.0751942416754861));
#71101=CARTESIAN_POINT('Ctrl Pts',(0.00247740867858648,-0.0336723290703325,
0.075245110488289));
#71102=CARTESIAN_POINT('Ctrl Pts',(0.00248771419666688,-0.033601104548885,
0.0752958021380185));
#71103=CARTESIAN_POINT('Ctrl Pts',(0.00252061767448949,-0.0333736987606857,
0.0754576505341546));
#71104=CARTESIAN_POINT('Ctrl Pts',(0.00256275472416368,-0.0331450831799192,
0.0756173440256608));
#71105=CARTESIAN_POINT('Ctrl Pts',(0.00246841698246456,-0.0337436976235975,
0.0751967094077343));
#71106=CARTESIAN_POINT('Ctrl Pts',(0.00247783124551087,-0.0336723290703325,
0.0752475746195329));
#71107=CARTESIAN_POINT('Ctrl Pts',(0.00248815889038774,-0.033601104548885,
0.0752982622696196));
#71108=CARTESIAN_POINT('Ctrl Pts',(0.00252113301468838,-0.0333736987606857,
0.0754600978956887));
#71109=CARTESIAN_POINT('Ctrl Pts',(0.00256333986160073,-0.0331450831799192,
0.0756197745840699));
#71110=CARTESIAN_POINT('',(0.00247468732294312,-0.0336938721132548,0.0752297463349663));
#71111=CARTESIAN_POINT('',(0.00252381793631918,-0.0333679869945435,0.0754609253688133));
#71112=CARTESIAN_POINT('Ctrl Pts',(0.00247468732294426,-0.0336938721132647,
0.0752297463349778));
#71113=CARTESIAN_POINT('Ctrl Pts',(0.00247890207940818,-0.033662918793393,
0.0752517974022936));
#71114=CARTESIAN_POINT('Ctrl Pts',(0.00248324460575755,-0.0336319952301038,
0.0752738167380591));
#71115=CARTESIAN_POINT('Ctrl Pts',(0.00248771419666878,-0.0336011045488948,
0.0752958021380299));
#71116=CARTESIAN_POINT('Ctrl Pts',(0.00249892992967298,-0.0335235892595452,
0.075350971029537));
#71117=CARTESIAN_POINT('Ctrl Pts',(0.00251096583808578,-0.0334458668660367,
0.0754060242342462));
#71118=CARTESIAN_POINT('Ctrl Pts',(0.0025238179360017,-0.0333679869945383,
0.0754609253688804));
#71119=CARTESIAN_POINT('Ctrl Pts',(0.00252382740301007,-0.033367969246074,
0.0754609688251143));
#71120=CARTESIAN_POINT('Ctrl Pts',(0.00252426733563364,-0.0333391895375059,
0.0754608597512404));
#71121=CARTESIAN_POINT('Ctrl Pts',(0.00252459630517395,-0.0333104081060432,
0.0754607748432893));
#71122=CARTESIAN_POINT('Ctrl Pts',(0.00252503036866947,-0.0332532697965678,
0.0754606570903441));
#71123=CARTESIAN_POINT('Ctrl Pts',(0.0025251387292648,-0.0332249169959204,
0.0754606234838277));
#71124=CARTESIAN_POINT('Ctrl Pts',(0.00252514073068577,-0.0331960985418316,
0.0754606159305638));
#71125=CARTESIAN_POINT('Ctrl Pts',(0.00252514073414812,-0.0331956312506232,
0.0754606158148028));
#71126=CARTESIAN_POINT('Ctrl Pts',(0.00252514070879179,-0.0331951640388587,
0.0754606157064865));
#71127=CARTESIAN_POINT('',(0.00249664906299847,-0.0331951640388587,0.075338906109001));
#71128=CARTESIAN_POINT('',(0.00251089488590508,-0.0331951640388687,0.0753997609077536));
#71129=CARTESIAN_POINT('',(0.00245255450076835,-0.0335216366567723,0.0751067138846023));
#71130=CARTESIAN_POINT('Origin',(0.0186300571953353,-0.0326434571528621,
0.0711495594033536));
#71131=CARTESIAN_POINT('',(0.00245389410775942,-0.0336938721132327,0.0751064878983125));
#71132=CARTESIAN_POINT('Origin',(-0.00831452423081074,-0.0336938867896226,
0.0769230771272436));
#71133=CARTESIAN_POINT('',(0.00246429071536126,-0.0336938721132538,0.0751681171166494));
#71134=CARTESIAN_POINT('Ctrl Pts',(0.0021728029088052,-0.0335235895815172,
0.0749154054858857));
#71135=CARTESIAN_POINT('Ctrl Pts',(0.00218334022226314,-0.0334144449262749,
0.0749973324321342));
#71136=CARTESIAN_POINT('Ctrl Pts',(0.00219558219087022,-0.0333049234473147,
0.0750791358095524));
#71137=CARTESIAN_POINT('Ctrl Pts',(0.00220952263615483,-0.0331951640388588,
0.0751607095987539));
#71138=CARTESIAN_POINT('Ctrl Pts',(0.00226653418144584,-0.0335235895815172,
0.0749790892437453));
#71139=CARTESIAN_POINT('Ctrl Pts',(0.00227794822721251,-0.0334144449262749,
0.075059725794486));
#71140=CARTESIAN_POINT('Ctrl Pts',(0.00229104127678745,-0.0333049234473147,
0.0751402191812586));
#71141=CARTESIAN_POINT('Ctrl Pts',(0.00230580591169218,-0.0331951640388588,
0.0752204649611722));
#71142=CARTESIAN_POINT('Ctrl Pts',(0.00236026545408649,-0.0335235895815172,
0.0750427730016049));
#71143=CARTESIAN_POINT('Ctrl Pts',(0.00237255623216187,-0.0334144449262749,
0.0751221191568377));
#71144=CARTESIAN_POINT('Ctrl Pts',(0.00238650036270467,-0.0333049234473147,
0.0752013025529648));
#71145=CARTESIAN_POINT('Ctrl Pts',(0.00240208918722953,-0.0331951640388588,
0.0752802203235906));
#71146=CARTESIAN_POINT('Ctrl Pts',(0.00245399672672714,-0.0335235895815172,
0.0751064567594644));
#71147=CARTESIAN_POINT('Ctrl Pts',(0.00246716423711124,-0.0334144449262749,
0.0751845125191895));
#71148=CARTESIAN_POINT('Ctrl Pts',(0.0024819594486219,-0.0333049234473147,
0.075262385924671));
#71149=CARTESIAN_POINT('Ctrl Pts',(0.00249837246276688,-0.0331951640388588,
0.075339975686009));
#71150=CARTESIAN_POINT('',(0.00235308584958674,-0.0331951640388687,0.0752498078538875));
#71151=CARTESIAN_POINT('Ctrl Pts',(0.00220737723944181,-0.0332121607145973,
0.0751480743278375));
#71152=CARTESIAN_POINT('Ctrl Pts',(0.00224969008078945,-0.0332625444109937,
0.0751409363173366));
#71153=CARTESIAN_POINT('Ctrl Pts',(0.00229127380548083,-0.0333135300747213,
0.075133921305958));
#71154=CARTESIAN_POINT('Ctrl Pts',(0.00237301603011546,-0.0334167203140618,
0.07512013171303));
#71155=CARTESIAN_POINT('Ctrl Pts',(0.00241314287066596,-0.0334688847587314,
0.0751133624722961));
#71156=CARTESIAN_POINT('Ctrl Pts',(0.00245255450148716,-0.03352163665624,
0.0751067138846404));
#71157=CARTESIAN_POINT('Ctrl Pts',(0.00247526687111416,-0.033693872113239,
0.0752289315719396));
#71158=CARTESIAN_POINT('Ctrl Pts',(0.00248158221563218,-0.0336474569764958,
0.0752619942064954));
#71159=CARTESIAN_POINT('Ctrl Pts',(0.002488284167301,-0.033601104548885,
0.075294980646497));
#71160=CARTESIAN_POINT('Ctrl Pts',(0.00250525196805112,-0.0334837508592656,
0.0753784947285229));
#71161=CARTESIAN_POINT('Ctrl Pts',(0.00252468701319737,-0.0333660264659098,
0.0754614693462026));
#71162=CARTESIAN_POINT('Ctrl Pts',(0.00247468732293934,-0.033693872113239,
0.0752297463349461));
#71163=CARTESIAN_POINT('Ctrl Pts',(0.00248100743653561,-0.0336474569764958,
0.0752628123617897));
#71164=CARTESIAN_POINT('Ctrl Pts',(0.00248771419666689,-0.033601104548885,
0.0752958021380185));
#71165=CARTESIAN_POINT('Ctrl Pts',(0.00250469417133847,-0.0334837508592656,
0.0753793246666048));
#71166=CARTESIAN_POINT('Ctrl Pts',(0.00252414163534938,-0.0333660264659098,
0.0754623073663972));
#71167=CARTESIAN_POINT('Ctrl Pts',(0.00227763838309537,-0.033693872113239,
0.075506769356708));
#71168=CARTESIAN_POINT('Ctrl Pts',(0.002285580004364,-0.0336474569764958,
0.0755409887763842));
#71169=CARTESIAN_POINT('Ctrl Pts',(0.00229392166298028,-0.033601104548885,
0.0755751128846199));
#71170=CARTESIAN_POINT('Ctrl Pts',(0.00231504082472912,-0.0334837508592656,
0.0756615072810482));
#71171=CARTESIAN_POINT('Ctrl Pts',(0.00233871075758991,-0.0333660264659098,
0.0757472379348749));
#71172=CARTESIAN_POINT('',(0.00228172151382143,-0.0336769361243754,0.0755175989980726));
#71173=CARTESIAN_POINT('',(0.00227881362529051,-0.0336938721132327,0.0755051171319192));
#71174=CARTESIAN_POINT('Ctrl Pts',(0.00228172151382151,-0.0336769361243751,
0.0755175989980729));
#71175=CARTESIAN_POINT('Ctrl Pts',(0.00228123460747909,-0.0336797586670031,
0.0755155190489053));
#71176=CARTESIAN_POINT('Ctrl Pts',(0.00228074883033805,-0.0336825812712857,
0.075513438918373));
#71177=CARTESIAN_POINT('Ctrl Pts',(0.00227977953466158,-0.0336882265989872,
0.0755092782977148));
#71178=CARTESIAN_POINT('Ctrl Pts',(0.00227929601612137,-0.0336910493223981,
0.0755071978075978));
#71179=CARTESIAN_POINT('Ctrl Pts',(0.00227881362528851,-0.0336938721132338,
0.0755051171319211));
#71180=CARTESIAN_POINT('Ctrl Pts',(0.00228172151382143,-0.0336769361243754,
0.0755175989980726));
#71181=CARTESIAN_POINT('Ctrl Pts',(0.00232253195311806,-0.0336279007642953,
0.0755080454656879));
#71182=CARTESIAN_POINT('Ctrl Pts',(0.0023639234699351,-0.0335767878888531,
0.0754983559057812));
#71183=CARTESIAN_POINT('Ctrl Pts',(0.00244503924067831,-0.0334733199122762,
0.0754793670843899));
#71184=CARTESIAN_POINT('Ctrl Pts',(0.00248481178595621,-0.0334209645148418,
0.0754700565181263));
#71185=CARTESIAN_POINT('Ctrl Pts',(0.00252381793464815,-0.0333679869844682,
0.0754609253617077));
#71186=CARTESIAN_POINT('',(0.00237675047412682,-0.0336938721132538,0.0753674317334528));
#71187=CARTESIAN_POINT('Origin',(0.00812378219310841,-0.0315241814719618,
0.07415));
#71188=CARTESIAN_POINT('',(0.00228172151508861,-0.033710812065583,0.0755175989977821));
#71189=CARTESIAN_POINT('',(0.00228465605720548,-0.0336938721132327,0.0755300746244476));
#71190=CARTESIAN_POINT('Origin',(0.0184669961080924,-0.034556251000384,
0.0728765208499561));
#71191=CARTESIAN_POINT('Ctrl Pts',(0.00228465605721286,-0.0336938721132298,
0.0755300746244498));
#71192=CARTESIAN_POINT('Ctrl Pts',(0.00228416478475723,-0.0336910493377706,
0.0755279960398684));
#71193=CARTESIAN_POINT('Ctrl Pts',(0.00228367460116839,-0.0336882266066734,
0.0755259171040297));
#71194=CARTESIAN_POINT('Ctrl Pts',(0.00228269641887757,-0.0336825812712869,
0.0755217585577134));
#71195=CARTESIAN_POINT('Ctrl Pts',(0.00228220842016392,-0.0336797586670037,
0.0755196789472403));
#71196=CARTESIAN_POINT('Ctrl Pts',(0.00228172151382139,-0.0336769361243751,
0.0755175989980724));
#71197=CARTESIAN_POINT('Origin',(0.0179575146465307,-0.0345562514382243,
0.0707001500671947));
#71198=CARTESIAN_POINT('Ctrl Pts',(0.00248928190141467,-0.0342436276873911,
0.0753034866548439));
#71199=CARTESIAN_POINT('Ctrl Pts',(0.00253278636778234,-0.033943005420181,
0.0755159953365952));
#71200=CARTESIAN_POINT('Ctrl Pts',(0.00259217426715855,-0.0336441434784052,
0.0757246233687993));
#71201=CARTESIAN_POINT('Ctrl Pts',(0.00254473290416811,-0.0342436276873911,
0.0755472594718143));
#71202=CARTESIAN_POINT('Ctrl Pts',(0.00259743141389354,-0.033943005420181,
0.0757576767845201));
#71203=CARTESIAN_POINT('Ctrl Pts',(0.00266582970682857,-0.0336441434784052,
0.0759635268560216));
#71204=CARTESIAN_POINT('Ctrl Pts',(0.00254528741419565,-0.0342436276873911,
0.075549697199984));
#71205=CARTESIAN_POINT('Ctrl Pts',(0.00259807786435466,-0.033943005420181,
0.0757600935989994));
#71206=CARTESIAN_POINT('Ctrl Pts',(0.00266656626122527,-0.0336441434784052,
0.0759659158908939));
#71207=CARTESIAN_POINT('',(0.00255363235458484,-0.0341934961088741,0.0755823253039714));
#71208=CARTESIAN_POINT('',(0.00261718186963272,-0.0338664212862875,0.0758099632168831));
#71209=CARTESIAN_POINT('Origin',(0.0188805520503518,-0.0345610720404299,
0.0719101546910196));
#71210=CARTESIAN_POINT('Origin',(-0.00788237466357971,-0.0336938005072939,
0.0789750915015038));
#71211=CARTESIAN_POINT('',(0.00258240495709018,-0.0336938721132327,0.0756898906870749));
#71212=CARTESIAN_POINT('',(0.00260044377354836,-0.0336938721132427,0.0757497309001623));
#71213=CARTESIAN_POINT('',(0.00252381793464694,-0.0340203938281605,0.0754609253617025));
#71214=CARTESIAN_POINT('Origin',(0.0189125046270622,-0.0345589643243083,
0.0723902752663712));
#71215=CARTESIAN_POINT('',(0.00252514070879169,-0.034193496108874,0.0754606157064862));
#71216=CARTESIAN_POINT('Origin',(-0.00820423943531576,-0.0341934220717692,
0.0779723123442933));
#71217=CARTESIAN_POINT('',(0.00253938653169827,-0.0341934961088841,0.0755214705052389));
#71218=CARTESIAN_POINT('Ctrl Pts',(0.0022326054963916,-0.0340223579322397,
0.0752875575273789));
#71219=CARTESIAN_POINT('Ctrl Pts',(0.00224829538156874,-0.0339125849573575,
0.0753688122188604));
#71220=CARTESIAN_POINT('Ctrl Pts',(0.00226565602494908,-0.0338030433565231,
0.0754496850694462));
#71221=CARTESIAN_POINT('Ctrl Pts',(0.00228465605720486,-0.0336938721132327,
0.0755300746244473));
#71222=CARTESIAN_POINT('Ctrl Pts',(0.00233015054961238,-0.0340223579322397,
0.075345230245561));
#71223=CARTESIAN_POINT('Ctrl Pts',(0.00234663589199001,-0.0339125849573575,
0.0754251395363505));
#71224=CARTESIAN_POINT('Ctrl Pts',(0.00236476358694424,-0.0338030433565231,
0.075504651467526));
#71225=CARTESIAN_POINT('Ctrl Pts',(0.00238450143849556,-0.0336938721132327,
0.0755836664117405));
#71226=CARTESIAN_POINT('Ctrl Pts',(0.00242769560283315,-0.0340223579322397,
0.0754029029637432));
#71227=CARTESIAN_POINT('Ctrl Pts',(0.00244497640241129,-0.0339125849573575,
0.0754814668538405));
#71228=CARTESIAN_POINT('Ctrl Pts',(0.00246387114893939,-0.0338030433565231,
0.0755596178656058));
#71229=CARTESIAN_POINT('Ctrl Pts',(0.00248434681978626,-0.0336938721132327,
0.0756372581990337));
#71230=CARTESIAN_POINT('Ctrl Pts',(0.00252524065605393,-0.0340223579322397,
0.0754605756819253));
#71231=CARTESIAN_POINT('Ctrl Pts',(0.00254331691283256,-0.0339125849573575,
0.0755377941713306));
#71232=CARTESIAN_POINT('Ctrl Pts',(0.00256297871093455,-0.0338030433565231,
0.0756145842636856));
#71233=CARTESIAN_POINT('Ctrl Pts',(0.00258419220107697,-0.0336938721132327,
0.0756908499863269));
#71234=CARTESIAN_POINT('',(0.00243353050715783,-0.0336938721132427,0.0756099826557713));
#71235=CARTESIAN_POINT('Ctrl Pts',(0.00228172151859185,-0.0337108120662681,
0.0755175989969558));
#71236=CARTESIAN_POINT('Ctrl Pts',(0.00232358889588207,-0.033761140899444,
0.0755077980403452));
#71237=CARTESIAN_POINT('Ctrl Pts',(0.00236469228642256,-0.0338121088781616,
0.0754981759294487));
#71238=CARTESIAN_POINT('Ctrl Pts',(0.00244540853849247,-0.0339153382773234,
0.0754792806335045));
#71239=CARTESIAN_POINT('Ctrl Pts',(0.00248498725214032,-0.0339675558473108,
0.0754700154423158));
#71240=CARTESIAN_POINT('Ctrl Pts',(0.00252381793468696,-0.0340203938281304,
0.0754609253616985));
#71241=CARTESIAN_POINT('Ctrl Pts',(0.00255470183801549,-0.0341934961088741,
0.0755806020549832));
#71242=CARTESIAN_POINT('Ctrl Pts',(0.00258427840845701,-0.0340287516182428,
0.0756957384039372));
#71243=CARTESIAN_POINT('Ctrl Pts',(0.00261858837893608,-0.0338644633275951,
0.0758095539489883));
#71244=CARTESIAN_POINT('Ctrl Pts',(0.00255363235458491,-0.0341934961088741,
0.0755823253039714));
#71245=CARTESIAN_POINT('Ctrl Pts',(0.00258324455184167,-0.0340287516182428,
0.0756974837636528));
#71246=CARTESIAN_POINT('Ctrl Pts',(0.00261759103254668,-0.0338644633275951,
0.0758113199280548));
#71247=CARTESIAN_POINT('Ctrl Pts',(0.00237543584433704,-0.0341934961088741,
0.075869451730816));
#71248=CARTESIAN_POINT('Ctrl Pts',(0.00241098415426721,-0.0340287516182428,
0.0759882942629614));
#71249=CARTESIAN_POINT('Ctrl Pts',(0.00245141394086077,-0.0338644633275951,
0.0761055660078178));
#71250=CARTESIAN_POINT('',(0.00237912173818566,-0.0341764758832395,0.0758817263779963));
#71251=CARTESIAN_POINT('',(0.00237543584433932,-0.034193496108874,0.0758694517308122));
#71252=CARTESIAN_POINT('Origin',(0.0183800328338216,-0.0345621026367731,
0.0715931167332867));
#71253=CARTESIAN_POINT('Ctrl Pts',(0.0023791217385473,-0.0341764758837485,
0.0758817263762082));
#71254=CARTESIAN_POINT('Ctrl Pts',(0.00242021939710316,-0.0341260050040296,
0.0758693374835352));
#71255=CARTESIAN_POINT('Ctrl Pts',(0.0024606026703716,-0.0340749269147885,
0.0758571639024622));
#71256=CARTESIAN_POINT('Ctrl Pts',(0.00253997179671667,-0.0339715436305742,
0.0758332381044852));
#71257=CARTESIAN_POINT('Ctrl Pts',(0.0025789275406577,-0.0339192778236512,
0.0758214949702209));
#71258=CARTESIAN_POINT('Ctrl Pts',(0.00261718186802259,-0.0338664212854278,
0.0758099632154826));
#71259=CARTESIAN_POINT('',(0.00246453409947208,-0.0341934961088841,0.0757258885174018));
#71260=CARTESIAN_POINT('Origin',(0.00812378219310841,-0.0315241814719618,
0.07415));
#71261=CARTESIAN_POINT('',(0.00237912173913322,-0.0342105180190362,0.0758817263785895));
#71262=CARTESIAN_POINT('',(0.00238283384147144,-0.0341934961088739,0.0758939931260949));
#71263=CARTESIAN_POINT('Origin',(0.0183720500414141,-0.0345621701000461,
0.0715484971096708));
#71264=CARTESIAN_POINT('Origin',(0.0180844299120316,-0.0345621040084784,
0.0706125026862545));
#71265=CARTESIAN_POINT('Origin',(0.0181024312949348,-0.0345621715591868,
0.0706541020864207));
#71266=CARTESIAN_POINT('Ctrl Pts',(0.00258197202263347,-0.0346945769586965,
0.0756884545124663));
#71267=CARTESIAN_POINT('Ctrl Pts',(0.00261419556836066,-0.0345275153362944,
0.0758045299453067));
#71268=CARTESIAN_POINT('Ctrl Pts',(0.00265007791427002,-0.0343603235965185,
0.075919622000346));
#71269=CARTESIAN_POINT('Ctrl Pts',(0.00268950787721066,-0.034193496108874,
0.0760333918636549));
#71270=CARTESIAN_POINT('Ctrl Pts',(0.00260616808954228,-0.0346945769586965,
0.0757687201886334));
#71271=CARTESIAN_POINT('Ctrl Pts',(0.00264007283199341,-0.0345275153362944,
0.0758842888251648));
#71272=CARTESIAN_POINT('Ctrl Pts',(0.00267762087119285,-0.0343603235965185,
0.0759988210807221));
#71273=CARTESIAN_POINT('Ctrl Pts',(0.00271869612221547,-0.034193496108874,
0.0761119798702332));
#71274=CARTESIAN_POINT('Ctrl Pts',(0.00263036415645107,-0.0346945769586965,
0.0758489858648032));
#71275=CARTESIAN_POINT('Ctrl Pts',(0.00266595009562619,-0.0345275153362944,
0.0759640477050237));
#71276=CARTESIAN_POINT('Ctrl Pts',(0.00270516382811572,-0.0343603235965185,
0.0760780201610976));
#71277=CARTESIAN_POINT('Ctrl Pts',(0.00274788436722025,-0.034193496108874,
0.07619056787681));
#71278=CARTESIAN_POINT('Ctrl Pts',(0.00265456022335989,-0.0346945769586965,
0.0759292515409676));
#71279=CARTESIAN_POINT('Ctrl Pts',(0.00269182735925891,-0.0345275153362944,
0.076043806584881));
#71280=CARTESIAN_POINT('Ctrl Pts',(0.00273270678503852,-0.0343603235965185,
0.0761572192414743));
#71281=CARTESIAN_POINT('Ctrl Pts',(0.00277707261222508,-0.034193496108874,
0.0762691558833898));
#71282=CARTESIAN_POINT('',(0.00265456022288458,-0.0346945769586966,0.0759292515393901));
#71283=CARTESIAN_POINT('',(0.00273227784011006,-0.0343667727836499,0.0761524499526084));
#71284=CARTESIAN_POINT('Origin',(0.018585812268892,-0.034562647418524,0.0705540814451111));
#71285=CARTESIAN_POINT('Origin',(-0.00762837865205597,-0.0341934771024016,
0.0800004955552602));
#71286=CARTESIAN_POINT('',(0.00269003013551803,-0.034193496108874,0.076034798020116));
#71287=CARTESIAN_POINT('',(0.0027117907545604,-0.034193496108884,0.0760933874855557));
#71288=CARTESIAN_POINT('',(0.00261718186946422,-0.0345211942962691,0.0758099632150947));
#71289=CARTESIAN_POINT('Origin',(0.0187214010005133,-0.0345625596118379,
0.0710153885034588));
#71290=CARTESIAN_POINT('',(0.00261848258998653,-0.0346945769586885,0.0758095711132297));
#71291=CARTESIAN_POINT('Origin',(-0.00797425693574556,-0.0346945685853909,
0.0790027489276701));
#71292=CARTESIAN_POINT('',(0.00263652140644556,-0.0346945769587026,0.0758694113263199));
#71293=CARTESIAN_POINT('Ctrl Pts',(0.00231565845741203,-0.0345231616327842,
0.0756552237942812));
#71294=CARTESIAN_POINT('Ctrl Pts',(0.00233640584823061,-0.0344132092796988,
0.0757352806027937));
#71295=CARTESIAN_POINT('Ctrl Pts',(0.00235880808051535,-0.0343032738558979,
0.075814904137329));
#71296=CARTESIAN_POINT('Ctrl Pts',(0.0023828338414714,-0.0341934961088739,
0.0758939931260949));
#71297=CARTESIAN_POINT('Ctrl Pts',(0.00241663216415694,-0.0345231616327842,
0.0757066577002648));
#71298=CARTESIAN_POINT('Ctrl Pts',(0.00243808849895635,-0.0344132092796988,
0.0757853227283894));
#71299=CARTESIAN_POINT('Ctrl Pts',(0.00246117085076418,-0.0343032738558979,
0.0758635398903994));
#71300=CARTESIAN_POINT('Ctrl Pts',(0.00248584708162573,-0.0341934961088739,
0.075941209738547));
#71301=CARTESIAN_POINT('Ctrl Pts',(0.00251760587090184,-0.0345231616327842,
0.0757580916062485));
#71302=CARTESIAN_POINT('Ctrl Pts',(0.0025397711496821,-0.0344132092796988,
0.0758353648539852));
#71303=CARTESIAN_POINT('Ctrl Pts',(0.002563533621013,-0.0343032738558979,
0.0759121756434697));
#71304=CARTESIAN_POINT('Ctrl Pts',(0.00258886032178006,-0.0341934961088739,
0.075988426350999));
#71305=CARTESIAN_POINT('Ctrl Pts',(0.00261857957764675,-0.0345231616327842,
0.0758095255122321));
#71306=CARTESIAN_POINT('Ctrl Pts',(0.00264145380040784,-0.0344132092796988,
0.075885406979581));
#71307=CARTESIAN_POINT('Ctrl Pts',(0.00266589639126183,-0.0343032738558979,
0.07596081139654));
#71308=CARTESIAN_POINT('Ctrl Pts',(0.00269187356193439,-0.0341934961088739,
0.076035642963451));
#71309=CARTESIAN_POINT('',(0.00253643198850474,-0.0341934961088839,0.0759643955731155));
#71310=CARTESIAN_POINT('Ctrl Pts',(0.00237912174243639,-0.0342105180195385,
0.0758817263775875));
#71311=CARTESIAN_POINT('Ctrl Pts',(0.00242026560670682,-0.0342610556241352,
0.0758693235705557));
#71312=CARTESIAN_POINT('Ctrl Pts',(0.00246067116560645,-0.0343122189870268,
0.0758571433254832));
#71313=CARTESIAN_POINT('Ctrl Pts',(0.00254004109136414,-0.034415811969517,
0.0758332172822989));
#71314=CARTESIAN_POINT('Ctrl Pts',(0.00257897299535572,-0.0344681990450069,
0.0758214812701097));
#71315=CARTESIAN_POINT('Ctrl Pts',(0.00261718186948729,-0.0345211942962495,
0.0758099632150811));
#71316=CARTESIAN_POINT('Ctrl Pts',(0.00265551915720157,-0.0346945769586932,
0.0759274649752898));
#71317=CARTESIAN_POINT('Ctrl Pts',(0.00269226698782536,-0.0345296777079064,
0.0760405174441954));
#71318=CARTESIAN_POINT('Ctrl Pts',(0.00273365598030741,-0.0343648066255586,
0.0761519544895733));
#71319=CARTESIAN_POINT('Ctrl Pts',(0.00265456022288184,-0.0346945769586932,
0.0759292515393815));
#71320=CARTESIAN_POINT('Ctrl Pts',(0.00269134498945405,-0.0345296777079064,
0.0760423238335756));
#71321=CARTESIAN_POINT('Ctrl Pts',(0.0027327717057206,-0.0343648066255586,
0.0761537791607048));
#71322=CARTESIAN_POINT('Ctrl Pts',(0.00249474416025337,-0.0346945769586932,
0.076227000439268));
#71323=CARTESIAN_POINT('Ctrl Pts',(0.00253768467464258,-0.0345296777079064,
0.0763433768174706));
#71324=CARTESIAN_POINT('Ctrl Pts',(0.00258539843954466,-0.0343648066255586,
0.0764578789825962));
#71325=CARTESIAN_POINT('',(0.00249919351212516,-0.0346775396664981,0.0762390194262264));
#71326=CARTESIAN_POINT('',(0.00249474416025707,-0.0346945769586886,0.0762270004392665));
#71327=CARTESIAN_POINT('Origin',(0.0180082191875373,-0.034562661794297,
0.0703159270750803));
#71328=CARTESIAN_POINT('Ctrl Pts',(0.00249919351247531,-0.0346775396670096,
0.0762390194244345));
#71329=CARTESIAN_POINT('Ctrl Pts',(0.00253946386091069,-0.0346269749928766,
0.0762240626654086));
#71330=CARTESIAN_POINT('Ctrl Pts',(0.0025790185028908,-0.0345757902891958,
0.0762093716876919));
#71331=CARTESIAN_POINT('Ctrl Pts',(0.00265672900953741,-0.0344721681090152,
0.0761805093575572));
#71332=CARTESIAN_POINT('Ctrl Pts',(0.0026948544099873,-0.0344197714292358,
0.0761663493258164));
#71333=CARTESIAN_POINT('Ctrl Pts',(0.0027322778396058,-0.0343667727834165,
0.0761524499521408));
#71334=CARTESIAN_POINT('',(0.00257465219158083,-0.0346945769587026,0.0760781259893383));
#71335=CARTESIAN_POINT('Origin',(0.00812378219310841,-0.0315241814719618,
0.07415));
#71336=CARTESIAN_POINT('',(0.002499193513487,-0.0347116136489789,0.0762390194265086));
#71337=CARTESIAN_POINT('',(0.00250366852609143,-0.0346945769586885,0.0762510288836281));
#71338=CARTESIAN_POINT('Origin',(0.0179907058082699,-0.0345626680065938,
0.0702741345734983));
#71339=CARTESIAN_POINT('Origin',(0.0181145644536158,-0.0345626631243122,
0.0706022478523321));
#71340=CARTESIAN_POINT('Origin',(0.018128572272324,-0.0345626692914332,
0.0706453424126909));
#71341=CARTESIAN_POINT('Ctrl Pts',(0.00267744283577248,-0.0352450361874069,
0.0759982830493078));
#71342=CARTESIAN_POINT('Ctrl Pts',(0.00274715197485094,-0.0349452760959493,
0.076203695108825));
#71343=CARTESIAN_POINT('Ctrl Pts',(0.00283213555440364,-0.034644428984174,
0.0764032728367221));
#71344=CARTESIAN_POINT('Ctrl Pts',(0.00267830709071825,-0.0352450361874069,
0.0760006555350061));
#71345=CARTESIAN_POINT('Ctrl Pts',(0.00274810570956311,-0.0349452760959493,
0.0762060349986132));
#71346=CARTESIAN_POINT('Ctrl Pts',(0.0028331760594223,-0.034644428984174,
0.0764055734832195));
#71347=CARTESIAN_POINT('Ctrl Pts',(0.00276387688732919,-0.0352450361874069,
0.0762355551090968));
#71348=CARTESIAN_POINT('Ctrl Pts',(0.00284253488898659,-0.0349452760959493,
0.0764377072548668));
#71349=CARTESIAN_POINT('Ctrl Pts',(0.00293619635829975,-0.034644428984174,
0.0766333602651433));
#71350=CARTESIAN_POINT('Ctrl Pts',(0.0027647325852953,-0.0352450361874069,
0.0762379041048377));
#71351=CARTESIAN_POINT('Ctrl Pts',(0.00284347918078083,-0.0349452760959493,
0.0764400239774293));
#71352=CARTESIAN_POINT('Ctrl Pts',(0.00293722656128853,-0.034644428984174,
0.0766356381329626));
#71353=CARTESIAN_POINT('',(0.00277705848222208,-0.0351951634053265,0.0762691266743592));
#71354=CARTESIAN_POINT('',(0.00286865161508712,-0.0348678972925388,0.0764870339338457));
#71355=CARTESIAN_POINT('Origin',(0.0180012108129683,-0.0345636767889768,
0.0692956281131201));
#71356=CARTESIAN_POINT('Origin',(-0.00722780739889109,-0.0346946199341087,
0.0809770789890401));
#71357=CARTESIAN_POINT('',(0.00281909984408069,-0.0346945769330289,0.076372266899799));
#71358=CARTESIAN_POINT('',(0.00284449638968655,-0.0346945769458129,0.0764293743998229));
#71359=CARTESIAN_POINT('',(0.00273227783999167,-0.0350221583435276,0.0761524499520148));
#71360=CARTESIAN_POINT('Origin',(0.0182337468182862,-0.0345628458716235,
0.0697164254497386));
#71361=CARTESIAN_POINT('',(0.00273343628146693,-0.0351951360298763,0.0761520164706515));
#71362=CARTESIAN_POINT('Origin',(-0.00759609818597462,-0.0351951838366788,
0.079988494223648));
#71363=CARTESIAN_POINT('',(0.00277707261153886,-0.0351951371328749,0.0762691558818757));
#71364=CARTESIAN_POINT('Ctrl Pts',(0.00242163354584956,-0.0350241211494342,
0.0760169495988363));
#71365=CARTESIAN_POINT('Ctrl Pts',(0.00244735001109438,-0.0349144232818962,
0.0760954943584803));
#71366=CARTESIAN_POINT('Ctrl Pts',(0.00247470544519014,-0.0348045283579412,
0.0761735545532363));
#71367=CARTESIAN_POINT('Ctrl Pts',(0.00250366852998279,-0.0346945769439158,
0.0762510288940373));
#71368=CARTESIAN_POINT('Ctrl Pts',(0.00252563759587068,-0.0350241211494342,
0.0760619418135205));
#71369=CARTESIAN_POINT('Ctrl Pts',(0.00255197381042526,-0.0349144232818962,
0.0761390539600188));
#71370=CARTESIAN_POINT('Ctrl Pts',(0.00257991975164319,-0.0348045283579412,
0.07621566787348));
#71371=CARTESIAN_POINT('Ctrl Pts',(0.00260944327606993,-0.0346945769439158,
0.0762916840891936));
#71372=CARTESIAN_POINT('Ctrl Pts',(0.00262964164589181,-0.0350241211494342,
0.0761069340282047));
#71373=CARTESIAN_POINT('Ctrl Pts',(0.00265659760975614,-0.0349144232818962,
0.0761826135615573));
#71374=CARTESIAN_POINT('Ctrl Pts',(0.00268513405809624,-0.0348045283579412,
0.0762577811937236));
#71375=CARTESIAN_POINT('Ctrl Pts',(0.00271521802215706,-0.0346945769439158,
0.0763323392843498));
#71376=CARTESIAN_POINT('Ctrl Pts',(0.00273364569591294,-0.0350241211494342,
0.076151926242889));
#71377=CARTESIAN_POINT('Ctrl Pts',(0.00276122140908702,-0.0349144232818962,
0.0762261731630958));
#71378=CARTESIAN_POINT('Ctrl Pts',(0.00279034836454929,-0.0348045283579412,
0.0762998945139673));
#71379=CARTESIAN_POINT('Ctrl Pts',(0.00282099276824419,-0.0346945769439158,
0.0763729944795061));
#71380=CARTESIAN_POINT('',(0.00266138418490153,-0.0346945769458128,0.0763116478914811));
#71381=CARTESIAN_POINT('Ctrl Pts',(0.00249919351656515,-0.0347116136492789,
0.0762390194253587));
#71382=CARTESIAN_POINT('Ctrl Pts',(0.00253944787729479,-0.0347621546532341,
0.0762240686180454));
#71383=CARTESIAN_POINT('Ctrl Pts',(0.0025789944575839,-0.0348133084097124,
0.076209380686326));
#71384=CARTESIAN_POINT('Ctrl Pts',(0.0026567050615848,-0.0349168561544564,
0.0761805183159999));
#71385=CARTESIAN_POINT('Ctrl Pts',(0.00269483826145598,-0.0349692089015912,
0.0761663553256262));
#71386=CARTESIAN_POINT('Ctrl Pts',(0.00273227784003292,-0.0350221583435,
0.0761524499520208));
#71387=CARTESIAN_POINT('Ctrl Pts',(0.00277768220828862,-0.0351951371254875,
0.0762678259150681));
#71388=CARTESIAN_POINT('Ctrl Pts',(0.00282146693031317,-0.0350307338980921,
0.0763783531779963));
#71389=CARTESIAN_POINT('Ctrl Pts',(0.00286978244958865,-0.0348659306897825,
0.0764869763262212));
#71390=CARTESIAN_POINT('Ctrl Pts',(0.0027770726116466,-0.0351951371254875,
0.0762691558818324));
#71391=CARTESIAN_POINT('Ctrl Pts',(0.00282088482989956,-0.0350307338980921,
0.0763796957477886));
#71392=CARTESIAN_POINT('Ctrl Pts',(0.00286922834280482,-0.0348659306897825,
0.0764883303518237));
#71393=CARTESIAN_POINT('Ctrl Pts',(0.00267490357911754,-0.0351951371254875,
0.0764920596976223));
#71394=CARTESIAN_POINT('Ctrl Pts',(0.00272332419390732,-0.0350307338980921,
0.0766047118442231));
#71395=CARTESIAN_POINT('Ctrl Pts',(0.00277635946833986,-0.0348659306897825,
0.0767152664539698));
#71396=CARTESIAN_POINT('Origin',(-0.00199067670531014,-0.0308609197410307,
0.0786480487766916));
#71397=CARTESIAN_POINT('',(0.00273252921706985,-0.0351951371254875,0.0763663369197028));
#71398=CARTESIAN_POINT('Origin',(0.00894963950894094,-0.0351840467441202,
0.0736277880284817));
#71399=CARTESIAN_POINT('Origin',(-0.00246205922185187,-0.0352322613882021,
0.0797274165207997));
#71400=CARTESIAN_POINT('',(0.00296926846134209,-0.035195114256466,0.0767012355384141));
#71401=CARTESIAN_POINT('',(0.00302696922376633,-0.0351951372916787,0.0768117658716625));
#71402=CARTESIAN_POINT('Origin',(0.0084163362896763,-0.0352875124680666,
0.0743244425502087));
#71403=CARTESIAN_POINT('Origin',(0.00598815585604378,-0.0298325076522621,
0.0669573446885997));
#71404=CARTESIAN_POINT('Origin',(-0.000219626886901942,-0.0338732543834639,
0.0749480502568973));
#71405=CARTESIAN_POINT('Ctrl Pts',(0.00245414689220848,-0.0321934096636941,
0.0731838885674513));
#71406=CARTESIAN_POINT('Ctrl Pts',(0.00243685395761994,-0.0320508460843085,
0.0732853723395051));
#71407=CARTESIAN_POINT('Ctrl Pts',(0.00242230073067469,-0.0319086045660596,
0.0733872442194909));
#71408=CARTESIAN_POINT('Ctrl Pts',(0.00241050048893715,-0.0317669892864203,
0.0734892822795843));
#71409=CARTESIAN_POINT('Ctrl Pts',(0.00244186258475718,-0.0321934096636941,
0.0732668314901052));
#71410=CARTESIAN_POINT('Ctrl Pts',(0.00242605428898742,-0.0320508460843085,
0.0733685351454127));
#71411=CARTESIAN_POINT('Ctrl Pts',(0.00241299048926756,-0.0319086045660596,
0.0734705868535438));
#71412=CARTESIAN_POINT('Ctrl Pts',(0.00240268122428634,-0.0317669892864203,
0.0735727645634927));
#71413=CARTESIAN_POINT('Ctrl Pts',(0.00242957827730588,-0.0321934096636941,
0.0733497744127592));
#71414=CARTESIAN_POINT('Ctrl Pts',(0.00241525462035492,-0.0320508460843085,
0.0734516979513203));
#71415=CARTESIAN_POINT('Ctrl Pts',(0.00240368024786043,-0.0319086045660596,
0.0735539294875968));
#71416=CARTESIAN_POINT('Ctrl Pts',(0.00239486195963552,-0.0317669892864203,
0.073656246847401));
#71417=CARTESIAN_POINT('Ctrl Pts',(0.00241729396985459,-0.0321934096636941,
0.073432717335413));
#71418=CARTESIAN_POINT('Ctrl Pts',(0.0024044549517224,-0.0320508460843085,
0.0735348607572279));
#71419=CARTESIAN_POINT('Ctrl Pts',(0.00239437000645331,-0.0319086045660596,
0.0736372721216497));
#71420=CARTESIAN_POINT('Ctrl Pts',(0.0023870426949847,-0.0317669892864203,
0.0737397291313093));
#71421=CARTESIAN_POINT('',(0.0024175137385447,-0.0321934096636941,0.0734312334701365));
#71422=CARTESIAN_POINT('',(0.00239280147990483,-0.0318665617511268,0.0736662799839588));
#71423=CARTESIAN_POINT('Origin',(0.0189082437893042,-0.0326371944417531,
0.0761282183133339));
#71424=CARTESIAN_POINT('Origin',(-0.00852954720918482,-0.0316939261509197,
0.0727443856010129));
#71425=CARTESIAN_POINT('',(0.0024344906740738,-0.0320197221621809,0.07330765139166));
#71426=CARTESIAN_POINT('Ctrl Pts',(0.00243441780502418,-0.0320197392094727,
0.0733078214063092));
#71427=CARTESIAN_POINT('Ctrl Pts',(0.0024301325760199,-0.0319792716576025,
0.073336770728273));
#71428=CARTESIAN_POINT('Ctrl Pts',(0.00242604853700066,-0.0319386439829662,
0.0733658845074326));
#71429=CARTESIAN_POINT('Ctrl Pts',(0.00242216977601236,-0.0318979099381593,
0.0733951944826528));
#71430=CARTESIAN_POINT('Ctrl Pts',(0.00241829109169051,-0.0318571766984898,
0.0734245038785406));
#71431=CARTESIAN_POINT('Ctrl Pts',(0.00241463562500548,-0.031816387183355,
0.0734538602594943));
#71432=CARTESIAN_POINT('Ctrl Pts',(0.00241121245508737,-0.0317755399638303,
0.0734831622165602));
#71433=CARTESIAN_POINT('',(0.00243582716738047,-0.0321934096636184,0.0733075822738708));
#71434=CARTESIAN_POINT('Origin',(0.000149372311971935,-0.0324112673258503,
0.0729902076274767));
#71435=CARTESIAN_POINT('',(0.00242667045297258,-0.0321934096636663,0.0733694078720137));
#71436=CARTESIAN_POINT('Ctrl Pts',(0.00241914254979784,-0.0321934096636617,
0.0734300248919303));
#71437=CARTESIAN_POINT('Ctrl Pts',(0.00240921353194178,-0.0320835708272592,
0.0735086963185477));
#71438=CARTESIAN_POINT('Ctrl Pts',(0.00240091837440467,-0.0319739230346488,
0.0735875275930489));
#71439=CARTESIAN_POINT('Ctrl Pts',(0.00239425994960734,-0.0318646057455573,
0.0736664170417633));
#71440=CARTESIAN_POINT('Ctrl Pts',(0.00232813920853723,-0.0321934096636617,
0.0734975493811466));
#71441=CARTESIAN_POINT('Ctrl Pts',(0.00231914140601297,-0.0320835708272592,
0.0735774758147638));
#71442=CARTESIAN_POINT('Ctrl Pts',(0.00231180289596956,-0.0319739230346488,
0.0736575420968569));
#71443=CARTESIAN_POINT('Ctrl Pts',(0.00230612520559497,-0.0318646057455573,
0.0737376450675846));
#71444=CARTESIAN_POINT('Ctrl Pts',(0.00223713586727661,-0.0321934096636617,
0.0735650738703629));
#71445=CARTESIAN_POINT('Ctrl Pts',(0.00222906928008416,-0.0320835708272592,
0.07364625531098));
#71446=CARTESIAN_POINT('Ctrl Pts',(0.00222268741753445,-0.0319739230346488,
0.0737275566006649));
#71447=CARTESIAN_POINT('Ctrl Pts',(0.0022179904615826,-0.0318646057455573,
0.0738088730934058));
#71448=CARTESIAN_POINT('Ctrl Pts',(0.002146132526016,-0.0321934096636617,
0.0736325983595793));
#71449=CARTESIAN_POINT('Ctrl Pts',(0.00213899715415534,-0.0320835708272592,
0.0737150348071961));
#71450=CARTESIAN_POINT('Ctrl Pts',(0.00213357193909934,-0.0319739230346488,
0.073797571104473));
#71451=CARTESIAN_POINT('Ctrl Pts',(0.00212985571757023,-0.0318646057455573,
0.0738801011192271));
#71452=CARTESIAN_POINT('',(0.00214504098544081,-0.0321763980308447,0.0736453679068871));
#71453=CARTESIAN_POINT('',(0.00214613252601318,-0.0321934096636184,0.0736325983596118));
#71454=CARTESIAN_POINT('Origin',(0.0185711665253974,-0.0326386231815108,
0.0756474894054743));
#71455=CARTESIAN_POINT('Ctrl Pts',(0.00214504098859838,-0.0321763980306265,
0.0736453679071493));
#71456=CARTESIAN_POINT('Ctrl Pts',(0.00218780781467109,-0.0321259596175139,
0.0736489776156494));
#71457=CARTESIAN_POINT('Ctrl Pts',(0.00222983364998933,-0.0320749164632061,
0.0736525247812591));
#71458=CARTESIAN_POINT('Ctrl Pts',(0.0023124371602503,-0.0319716057793898,
0.0736594968813775));
#71459=CARTESIAN_POINT('Ctrl Pts',(0.00235298265000875,-0.0319193786690093,
0.0736629190993149));
#71460=CARTESIAN_POINT('Ctrl Pts',(0.0023928014817504,-0.0318665617525277,
0.0736662799841081));
#71461=CARTESIAN_POINT('',(0.00228182313228894,-0.0321934096636663,0.0735319159148842));
#71462=CARTESIAN_POINT('Origin',(0.00812378219310841,-0.0315241814719618,
0.07415));
#71463=CARTESIAN_POINT('',(0.00214504098506965,-0.0322104233323609,0.0736453679068559));
#71464=CARTESIAN_POINT('',(0.00214397671962842,-0.0321934096636183,0.0736581397562614));
#71465=CARTESIAN_POINT('Origin',(0.0185812385183085,-0.0326387230348049,
0.0756032873434876));
#71466=CARTESIAN_POINT('Origin',(0.0186743673869259,-0.0326386245818049,
0.0744248298492832));
#71467=CARTESIAN_POINT('Origin',(0.0186768816158389,-0.0326387241480481,
0.074470094625862));
#71468=CARTESIAN_POINT('Ctrl Pts',(0.00240860327225173,-0.0327445246967097,
0.0735059076909357));
#71469=CARTESIAN_POINT('Ctrl Pts',(0.00238431093368944,-0.032443687833936,
0.0737214591877253));
#71470=CARTESIAN_POINT('Ctrl Pts',(0.00237632382680337,-0.0321434074405927,
0.0739382281237025));
#71471=CARTESIAN_POINT('Ctrl Pts',(0.0023860118057462,-0.0327445246967097,
0.07375488484981));
#71472=CARTESIAN_POINT('Ctrl Pts',(0.00237110979424191,-0.032443687833936,
0.073971288397688));
#71473=CARTESIAN_POINT('Ctrl Pts',(0.00237255051745677,-0.0321434074405927,
0.0741881996463537));
#71474=CARTESIAN_POINT('',(0.00238364203203967,-0.0326943950436611,0.073790951352479));
#71475=CARTESIAN_POINT('',(0.00237373722915698,-0.0323666188837389,0.0740270857512829));
#71476=CARTESIAN_POINT('Origin',(0.0191663754899599,-0.0326395579109917,
0.074764561077896));
#71477=CARTESIAN_POINT('Origin',(-0.0086683485399123,-0.0321933825603029,
0.0737910482320124));
#71478=CARTESIAN_POINT('',(0.00237776687233203,-0.0321934096532689,0.0739021433276513));
#71479=CARTESIAN_POINT('',(0.00237643116307099,-0.0321934096584275,0.0739646290558353));
#71480=CARTESIAN_POINT('',(0.00239280147895539,-0.0325210109756238,0.0736662799838677));
#71481=CARTESIAN_POINT('Origin',(0.0191110745637306,-0.0326393129159087,
0.0752421867029637));
#71482=CARTESIAN_POINT('',(0.00239415520064964,-0.0326943950436593,0.0736663942439461));
#71483=CARTESIAN_POINT('Origin',(-0.00862910428412556,-0.0326943765538171,
0.0727359819515683));
#71484=CARTESIAN_POINT('',(0.00238889861635466,-0.0326943950436702,0.0737286727982226));
#71485=CARTESIAN_POINT('Ctrl Pts',(0.00216941549877631,-0.0325229783203769,
0.0734114085909923));
#71486=CARTESIAN_POINT('Ctrl Pts',(0.00215923403235506,-0.032413025309245,
0.0734934894056602));
#71487=CARTESIAN_POINT('Ctrl Pts',(0.00215075205724437,-0.0323031222208069,
0.0735757683878763));
#71488=CARTESIAN_POINT('Ctrl Pts',(0.00214397671926085,-0.0321934096576658,
0.0736581397607305));
#71489=CARTESIAN_POINT('Ctrl Pts',(0.00224436440906771,-0.0325229783203769,
0.0734964015500094));
#71490=CARTESIAN_POINT('Ctrl Pts',(0.00223535456872785,-0.032413025309245,
0.073577449195588));
#71491=CARTESIAN_POINT('Ctrl Pts',(0.00222802266956867,-0.0323031222208069,
0.0736586709288246));
#71492=CARTESIAN_POINT('Ctrl Pts',(0.00222237443202867,-0.0321934096576658,
0.0737399623790529));
#71493=CARTESIAN_POINT('Ctrl Pts',(0.00231931331935912,-0.0325229783203769,
0.0735813945090266));
#71494=CARTESIAN_POINT('Ctrl Pts',(0.00231147510510064,-0.032413025309245,
0.0736614089855159));
#71495=CARTESIAN_POINT('Ctrl Pts',(0.00230529328189297,-0.0323031222208069,
0.0737415734697729));
#71496=CARTESIAN_POINT('Ctrl Pts',(0.00230077214479649,-0.0321934096576658,
0.0738217849973754));
#71497=CARTESIAN_POINT('Ctrl Pts',(0.00239426222965053,-0.0325229783203769,
0.0736663874680437));
#71498=CARTESIAN_POINT('Ctrl Pts',(0.00238759564147342,-0.032413025309245,
0.0737453687754437));
#71499=CARTESIAN_POINT('Ctrl Pts',(0.00238256389421727,-0.0323031222208069,
0.0738244760107211));
#71500=CARTESIAN_POINT('Ctrl Pts',(0.00237916985756431,-0.0321934096576658,
0.0739036076156978));
#71501=CARTESIAN_POINT('',(0.00226087179586497,-0.0321934096584275,0.073780141541465));
#71502=CARTESIAN_POINT('Ctrl Pts',(0.00214504098853049,-0.0322104233328923,
0.0736453679071436));
#71503=CARTESIAN_POINT('Ctrl Pts',(0.00218786576437557,-0.0322609421831417,
0.0736489825068597));
#71504=CARTESIAN_POINT('Ctrl Pts',(0.00222991990913416,-0.0323120888240843,
0.0736525320619177));
#71505=CARTESIAN_POINT('Ctrl Pts',(0.00231252404474623,-0.0324156524631811,
0.0736595042148185));
#71506=CARTESIAN_POINT('Ctrl Pts',(0.0023530400809842,-0.0324680267167309,
0.0736629239467422));
#71507=CARTESIAN_POINT('Ctrl Pts',(0.00239280147899819,-0.0325210109755912,
0.0736662799838758));
#71508=CARTESIAN_POINT('Origin',(0.0097249060661641,-0.0262834582512067,
0.0664467676796293));
#71509=CARTESIAN_POINT('Origin',(-0.00225402174624506,-0.0342771013831326,
0.0678154784922417));
#71510=CARTESIAN_POINT('Ctrl Pts',(0.00238519136587608,-0.0326943950436604,
0.0737896432028331));
#71511=CARTESIAN_POINT('Ctrl Pts',(0.0023802249738305,-0.0325844576448134,
0.0738687317396979));
#71512=CARTESIAN_POINT('Ctrl Pts',(0.00237689391091544,-0.0324744968375322,
0.0739479285869114));
#71513=CARTESIAN_POINT('Ctrl Pts',(0.00237520104548429,-0.0323646534831895,
0.0740271322139863));
#71514=CARTESIAN_POINT('Ctrl Pts',(0.00229860762203796,-0.0326943950436604,
0.0738627484891289));
#71515=CARTESIAN_POINT('Ctrl Pts',(0.00229464875785145,-0.0325844576448134,
0.073943030312259));
#71516=CARTESIAN_POINT('Ctrl Pts',(0.00229234997321614,-0.0324744968375322,
0.0740233996928605));
#71517=CARTESIAN_POINT('Ctrl Pts',(0.00229171279314884,-0.0323646534831895,
0.0741037536163709));
#71518=CARTESIAN_POINT('Ctrl Pts',(0.00221202387819984,-0.0326943950436604,
0.0739358537754246));
#71519=CARTESIAN_POINT('Ctrl Pts',(0.00220907254187239,-0.0325844576448134,
0.0740173288848201));
#71520=CARTESIAN_POINT('Ctrl Pts',(0.00220780603551685,-0.0324744968375322,
0.0740988707988096));
#71521=CARTESIAN_POINT('Ctrl Pts',(0.00220822454081339,-0.0323646534831895,
0.0741803750187554));
#71522=CARTESIAN_POINT('Ctrl Pts',(0.00212544013436172,-0.0326943950436604,
0.0740089590617204));
#71523=CARTESIAN_POINT('Ctrl Pts',(0.00212349632589333,-0.0325844576448134,
0.0740916274573811));
#71524=CARTESIAN_POINT('Ctrl Pts',(0.00212326209781756,-0.0324744968375322,
0.0741743419047587));
#71525=CARTESIAN_POINT('Ctrl Pts',(0.00212473628847795,-0.0323646534831895,
0.07425699642114));
#71526=CARTESIAN_POINT('',(0.00212515255399853,-0.0326773559991329,0.0740217719496073));
#71527=CARTESIAN_POINT('',(0.00212544013436172,-0.0326943950436594,0.0740089590617211));
#71528=CARTESIAN_POINT('Origin',(0.0187275769404676,-0.0326395670532496,
0.0743264168673391));
#71529=CARTESIAN_POINT('Ctrl Pts',(0.00212515255734552,-0.0326773559987408,
0.0740217719496743));
#71530=CARTESIAN_POINT('Ctrl Pts',(0.00216809617865336,-0.0326267922586304,
0.0740226899221395));
#71531=CARTESIAN_POINT('Ctrl Pts',(0.00221027865528394,-0.032575610958006,
0.0740235916242056));
#71532=CARTESIAN_POINT('Ctrl Pts',(0.00229315721868346,-0.0324719985462361,
0.0740253632549352));
#71533=CARTESIAN_POINT('Ctrl Pts',(0.00233382006503627,-0.0324196091621767,
0.0740262324730443));
#71534=CARTESIAN_POINT('Ctrl Pts',(0.00237373722920576,-0.0323666188837757,
0.0740270857512839));
#71535=CARTESIAN_POINT('',(0.0022545410832107,-0.0326943950436702,0.0738999552071101));
#71536=CARTESIAN_POINT('Origin',(0.00812378219310841,-0.0315241814719618,
0.07415));
#71537=CARTESIAN_POINT('',(0.00212515255404165,-0.0327114338379866,0.0740217719496084));
#71538=CARTESIAN_POINT('',(0.00212489233953398,-0.0326943950436593,0.074034585422462));
#71539=CARTESIAN_POINT('Origin',(0.0187277723063497,-0.0326395662664893,
0.0742811056495937));
#71540=CARTESIAN_POINT('Origin',(0.0187254324157374,-0.032639568123537,
0.0744268740492791));
#71541=CARTESIAN_POINT('Origin',(0.0187236855789967,-0.0326395675150339,
0.0744721518653795));
#71542=CARTESIAN_POINT('Ctrl Pts',(0.00237943604517094,-0.0332451089994432,
0.0738660768895002));
#71543=CARTESIAN_POINT('Ctrl Pts',(0.00236872770986089,-0.0329451141710252,
0.0740827284490749));
#71544=CARTESIAN_POINT('Ctrl Pts',(0.00237436887694699,-0.0326442513127493,
0.0742995711200258));
#71545=CARTESIAN_POINT('Ctrl Pts',(0.00237252426724457,-0.0332451089994432,
0.0741159813258873));
#71546=CARTESIAN_POINT('Ctrl Pts',(0.00237124123195885,-0.0329451141710252,
0.0743328935674314));
#71547=CARTESIAN_POINT('Ctrl Pts',(0.00238630055841826,-0.0326442513127493,
0.0745492862276531));
#71548=CARTESIAN_POINT('Ctrl Pts',(0.0023724551494653,-0.0332451089994432,
0.0741184803702511));
#71549=CARTESIAN_POINT('Ctrl Pts',(0.00237126636717983,-0.0329451141710252,
0.0743353952186149));
#71550=CARTESIAN_POINT('Ctrl Pts',(0.00238641987523298,-0.0326442513127493,
0.0745517833787293));
#71551=CARTESIAN_POINT('',(0.00237242403632311,-0.0331951640388616,0.0741520862358533));
#71552=CARTESIAN_POINT('',(0.00237736577183239,-0.0328677532463079,0.0743883766242067));
#71553=CARTESIAN_POINT('Origin',(0.0191185650576716,-0.0326403163409216,
0.0733780785999388));
#71554=CARTESIAN_POINT('Origin',(-0.00866908174770781,-0.0326944278639077,
0.0748471381129464));
#71555=CARTESIAN_POINT('',(0.00237354227162478,-0.0326943950436593,0.0742634277099163));
#71556=CARTESIAN_POINT('',(0.00237613270965503,-0.0326943950436693,0.0743258740038985));
#71557=CARTESIAN_POINT('',(0.00237373722915705,-0.0330220786163545,0.07402708575128));
#71558=CARTESIAN_POINT('Origin',(0.0191698357957509,-0.0326396682760288,
0.0738560707557115));
#71559=CARTESIAN_POINT('',(0.00237509545404048,-0.0331951640388586,0.074027114785002));
#71560=CARTESIAN_POINT('Origin',(-0.00865403804678937,-0.0331952026560058,
0.0737913527080536));
#71561=CARTESIAN_POINT('',(0.0023737597451918,-0.0331951640388701,0.0740896005104377));
#71562=CARTESIAN_POINT('Ctrl Pts',(0.00213478848483599,-0.0330240426238172,
0.073786744769755));
#71563=CARTESIAN_POINT('Ctrl Pts',(0.00212978429013694,-0.0329142774063519,
0.0738692489928803));
#71564=CARTESIAN_POINT('Ctrl Pts',(0.00212648319342054,-0.0328043479726691,
0.0739518977980528));
#71565=CARTESIAN_POINT('Ctrl Pts',(0.00212489233953394,-0.0326943950436593,
0.0740345854224621));
#71566=CARTESIAN_POINT('Ctrl Pts',(0.00221492624594939,-0.0330240426238172,
0.0738668639012297));
#71567=CARTESIAN_POINT('Ctrl Pts',(0.0022110257703427,-0.0329142774063519,
0.0739482641486212));
#71568=CARTESIAN_POINT('Ctrl Pts',(0.00220880612070064,-0.0328043479726691,
0.074029785610731));
#71569=CARTESIAN_POINT('Ctrl Pts',(0.00220827301668285,-0.0326943950436593,
0.0741113239308051));
#71570=CARTESIAN_POINT('Ctrl Pts',(0.00229506400706279,-0.0330240426238172,
0.0739469830327043));
#71571=CARTESIAN_POINT('Ctrl Pts',(0.00229226725054845,-0.0329142774063519,
0.074027279304362));
#71572=CARTESIAN_POINT('Ctrl Pts',(0.00229112904798074,-0.0328043479726691,
0.0741076734234092));
#71573=CARTESIAN_POINT('Ctrl Pts',(0.00229165369383175,-0.0326943950436593,
0.0741880624391481));
#71574=CARTESIAN_POINT('Ctrl Pts',(0.0023752017681762,-0.0330240426238172,
0.0740271021641789));
#71575=CARTESIAN_POINT('Ctrl Pts',(0.0023735087307542,-0.0329142774063519,
0.0741062944601029));
#71576=CARTESIAN_POINT('Ctrl Pts',(0.00237345197526084,-0.0328043479726691,
0.0741855612360874));
#71577=CARTESIAN_POINT('Ctrl Pts',(0.00237503437098066,-0.0326943950436593,
0.0742648009474911));
#71578=CARTESIAN_POINT('',(0.00224921730558938,-0.0326943950436693,0.0741490065661991));
#71579=CARTESIAN_POINT('Ctrl Pts',(0.0021251525573509,-0.0327114338383319,
0.0740217719496745));
#71580=CARTESIAN_POINT('Ctrl Pts',(0.00216808903577093,-0.032761987683113,
0.0740226897694516));
#71581=CARTESIAN_POINT('Ctrl Pts',(0.00221026802350364,-0.032813156260467,
0.0740235913969382));
#71582=CARTESIAN_POINT('Ctrl Pts',(0.00229314651070481,-0.0329167375858765,
0.074025363026039));
#71583=CARTESIAN_POINT('Ctrl Pts',(0.00233381298715526,-0.0329691088920615,
0.0740262323217458));
#71584=CARTESIAN_POINT('Ctrl Pts',(0.00237373722920451,-0.0330220786163187,
0.0740270857512838));
#71585=CARTESIAN_POINT('Ctrl Pts',(0.00237388840724671,-0.0331951640388604,
0.0741506831601087));
#71586=CARTESIAN_POINT('Ctrl Pts',(0.00237390253114358,-0.0330306422053993,
0.0742695585245084));
#71587=CARTESIAN_POINT('Ctrl Pts',(0.00237882988666516,-0.0328657862001532,
0.0743883317269922));
#71588=CARTESIAN_POINT('Ctrl Pts',(0.00237242403632318,-0.0331951640388604,
0.0741520862358502));
#71589=CARTESIAN_POINT('Ctrl Pts',(0.00237246716791067,-0.0330306422053993,
0.0742709918751792));
#71590=CARTESIAN_POINT('Ctrl Pts',(0.00237742475763063,-0.0328657862001532,
0.0743897941278041));
#71591=CARTESIAN_POINT('Ctrl Pts',(0.00212842045843366,-0.0331951640388604,
0.0743858763879778));
#71592=CARTESIAN_POINT('Ctrl Pts',(0.00213329705139667,-0.0330306422053993,
0.074509826644706));
#71593=CARTESIAN_POINT('Ctrl Pts',(0.00214329247167014,-0.0328657862001532,
0.0746334694321039));
#71594=CARTESIAN_POINT('',(0.0021289379721009,-0.0331781648281899,0.0743986820492859));
#71595=CARTESIAN_POINT('',(0.00212842045843432,-0.0331951640388588,0.0743858763879783));
#71596=CARTESIAN_POINT('Origin',(0.0185921750515698,-0.0326412092571505,
0.073002864439015));
#71597=CARTESIAN_POINT('Ctrl Pts',(0.00212893797309369,-0.033178164828644,
0.0743986820477356));
#71598=CARTESIAN_POINT('Ctrl Pts',(0.00217188403951269,-0.0331276811561084,
0.0743969005188));
#71599=CARTESIAN_POINT('Ctrl Pts',(0.00221405463159051,-0.0330765663526748,
0.0743951511249712));
#71600=CARTESIAN_POINT('Ctrl Pts',(0.00229688110570806,-0.0329730614522356,
0.0743917152665022));
#71601=CARTESIAN_POINT('Ctrl Pts',(0.00233750352844884,-0.0329207133441171,
0.074390030195206));
#71602=CARTESIAN_POINT('Ctrl Pts',(0.00237736575892228,-0.0328677532371618,
0.0743883766059144));
#71603=CARTESIAN_POINT('',(0.00225042224738872,-0.0331951640388701,0.0742689813119258));
#71604=CARTESIAN_POINT('Origin',(0.00812378219310841,-0.0315241814719618,
0.07415));
#71605=CARTESIAN_POINT('',(0.00212893797367636,-0.0332121607144414,0.0743986820498679));
#71606=CARTESIAN_POINT('',(0.00212948283705904,-0.0331951640388587,0.0744114865772719));
#71607=CARTESIAN_POINT('Origin',(0.0185824901785092,-0.0326413645154682,
0.072958564314666));
#71608=CARTESIAN_POINT('Origin',(0.0186512205433514,-0.0326412102439409,
0.0744261714448057));
#71609=CARTESIAN_POINT('Origin',(0.0186452323088342,-0.0326413658176302,
0.0744711213127881));
#71610=CARTESIAN_POINT('Ctrl Pts',(0.00237294324046329,-0.0337436976235975,
0.0742273067962073));
#71611=CARTESIAN_POINT('Ctrl Pts',(0.00237363854950455,-0.0336723290703325,
0.0742790307133109));
#71612=CARTESIAN_POINT('Ctrl Pts',(0.00237526409629952,-0.033601104548885,
0.0743307337562853));
#71613=CARTESIAN_POINT('Ctrl Pts',(0.00238045414521322,-0.0333736987606857,
0.0744958113307069));
#71614=CARTESIAN_POINT('Ctrl Pts',(0.00239510874438618,-0.0331450831799192,
0.0746603190354133));
#71615=CARTESIAN_POINT('Ctrl Pts',(0.00238173582579931,-0.0337436976235975,
0.0744771521292499));
#71616=CARTESIAN_POINT('Ctrl Pts',(0.00238467828163104,-0.0336723290703325,
0.0745287969645084));
#71617=CARTESIAN_POINT('Ctrl Pts',(0.00238854918924797,-0.033601104548885,
0.0745803805193434));
#71618=CARTESIAN_POINT('Ctrl Pts',(0.00240090823048522,-0.0333736987606857,
0.0747450765918053));
#71619=CARTESIAN_POINT('Ctrl Pts',(0.00242269811526736,-0.0331450831799192,
0.0749087920251213));
#71620=CARTESIAN_POINT('Ctrl Pts',(0.00238182375165267,-0.0337436976235975,
0.0744796505825803));
#71621=CARTESIAN_POINT('Ctrl Pts',(0.00238478867895231,-0.0336723290703325,
0.0745312946270204));
#71622=CARTESIAN_POINT('Ctrl Pts',(0.00238868204017745,-0.033601104548885,
0.074582876986974));
#71623=CARTESIAN_POINT('Ctrl Pts',(0.00240111277133794,-0.0333736987606857,
0.0747475692444162));
#71624=CARTESIAN_POINT('Ctrl Pts',(0.00242297400897617,-0.0331450831799192,
0.0749112767550183));
#71625=CARTESIAN_POINT('',(0.0023839040237067,-0.0336938721132548,0.0745132128858211));
#71626=CARTESIAN_POINT('',(0.00240367281197103,-0.0333679869984219,0.0747487267053694));
#71627=CARTESIAN_POINT('Ctrl Pts',(0.00238390402370562,-0.0336938721132476,
0.0745132128858081));
#71628=CARTESIAN_POINT('Ctrl Pts',(0.00238532181398584,-0.0336629187933822,
0.0745356183229366));
#71629=CARTESIAN_POINT('Ctrl Pts',(0.00238687034366562,-0.033631995230096,
0.0745580082925362));
#71630=CARTESIAN_POINT('Ctrl Pts',(0.00238854918924793,-0.033601104548887,
0.0745803805193432));
#71631=CARTESIAN_POINT('Ctrl Pts',(0.00239276198728257,-0.0335235892595373,
0.074636520091747));
#71632=CARTESIAN_POINT('Ctrl Pts',(0.00239780299271234,-0.033445866865335,
0.0746926476830146));
#71633=CARTESIAN_POINT('Ctrl Pts',(0.00240367281094795,-0.0333679869925471,
0.0747487266973178));
#71634=CARTESIAN_POINT('Ctrl Pts',(0.00240367675719604,-0.0333679692464398,
0.0747487710027038));
#71635=CARTESIAN_POINT('Ctrl Pts',(0.00240412689138218,-0.033339189539121,
0.0747487179270901));
#71636=CARTESIAN_POINT('Ctrl Pts',(0.00240446390868399,-0.0333104081088676,
0.0747486749194812));
#71637=CARTESIAN_POINT('Ctrl Pts',(0.00240490930745797,-0.0332532698468693,
0.0747486124976845));
#71638=CARTESIAN_POINT('Ctrl Pts',(0.00240502102613422,-0.0332249172402823,
0.0747485927389032));
#71639=CARTESIAN_POINT('Ctrl Pts',(0.00240502395830143,-0.0331960985318751,
0.0747485854943265));
#71640=CARTESIAN_POINT('Ctrl Pts',(0.00240502397625562,-0.0331956312606631,
0.0747485853800244));
#71641=CARTESIAN_POINT('Ctrl Pts',(0.00240502396467461,-0.0331951640388587,
0.0747485852693819));
#71642=CARTESIAN_POINT('',(0.00239201124142713,-0.0331951640388587,0.074624264438329));
#71643=CARTESIAN_POINT('',(0.00239851760306085,-0.0331951640388687,0.0746864248538654));
#71644=CARTESIAN_POINT('',(0.00237736578028421,-0.0335216366567729,0.0743883766049044));
#71645=CARTESIAN_POINT('Origin',(0.0189232670005926,-0.0326434571526242,
0.0724900041920831));
#71646=CARTESIAN_POINT('',(0.00237872314766524,-0.0336938721132325,0.0743883202978607));
#71647=CARTESIAN_POINT('Origin',(-0.00853246199787757,-0.0336938867896247,
0.074840944499333));
#71648=CARTESIAN_POINT('',(0.00238131358569597,-0.0336938721132536,0.0744507665918509));
#71649=CARTESIAN_POINT('Ctrl Pts',(0.00212379741339946,-0.0335235895815171,
0.0741635145584381));
#71650=CARTESIAN_POINT('Ctrl Pts',(0.00212398346790408,-0.0334144449262748,
0.0742461161618138));
#71651=CARTESIAN_POINT('Ctrl Pts',(0.00212587622312389,-0.0333049234473147,
0.0743288088206783));
#71652=CARTESIAN_POINT('Ctrl Pts',(0.0021294828370589,-0.0331951640388587,
0.0744114865772718));
#71653=CARTESIAN_POINT('Ctrl Pts',(0.00220880789566106,-0.0335235895815171,
0.0742384437943317));
#71654=CARTESIAN_POINT('Ctrl Pts',(0.00221002549861985,-0.0334144449262748,
0.0743198750610488));
#71655=CARTESIAN_POINT('Ctrl Pts',(0.00221292680914344,-0.0333049234473147,
0.0744013747276649));
#71656=CARTESIAN_POINT('Ctrl Pts',(0.00221751755741549,-0.0331951640388587,
0.0744828382450707));
#71657=CARTESIAN_POINT('Ctrl Pts',(0.00229381837792267,-0.0335235895815171,
0.0743133730302253));
#71658=CARTESIAN_POINT('Ctrl Pts',(0.00229606752933562,-0.0334144449262748,
0.0743936339602838));
#71659=CARTESIAN_POINT('Ctrl Pts',(0.00229997739516298,-0.0333049234473147,
0.0744739406346515));
#71660=CARTESIAN_POINT('Ctrl Pts',(0.00230555227777208,-0.0331951640388587,
0.0745541899128695));
#71661=CARTESIAN_POINT('Ctrl Pts',(0.00237882886018428,-0.0335235895815171,
0.0743883022661188));
#71662=CARTESIAN_POINT('Ctrl Pts',(0.00238210956005139,-0.0334144449262748,
0.0744673928595188));
#71663=CARTESIAN_POINT('Ctrl Pts',(0.00238702798118253,-0.0333049234473147,
0.0745465065416382));
#71664=CARTESIAN_POINT('Ctrl Pts',(0.00239358699812867,-0.0331951640388587,
0.0746255415806684));
#71665=CARTESIAN_POINT('',(0.00226074703925309,-0.0331951640388687,0.0745178755078105));
#71666=CARTESIAN_POINT('Ctrl Pts',(0.00212893797680065,-0.0332121607145973,
0.0743986820497332));
#71667=CARTESIAN_POINT('Ctrl Pts',(0.00217181179869377,-0.0332625444109943,
0.0743969035298045));
#71668=CARTESIAN_POINT('Ctrl Pts',(0.00221394683735506,-0.0333135300747218,
0.0743951556565651));
#71669=CARTESIAN_POINT('Ctrl Pts',(0.00229677279440457,-0.0334167203140626,
0.0743917198160283));
#71670=CARTESIAN_POINT('Ctrl Pts',(0.0023374316336624,-0.0334688847587328,
0.0743900331794583));
#71671=CARTESIAN_POINT('Ctrl Pts',(0.00237736578099208,-0.033521636656241,
0.074388376605033));
#71672=CARTESIAN_POINT('Ctrl Pts',(0.00238527708192473,-0.0336938721132474,
0.0745117209813181));
#71673=CARTESIAN_POINT('Ctrl Pts',(0.00238739435486032,-0.0336474569765,
0.0745453103559748));
#71674=CARTESIAN_POINT('Ctrl Pts',(0.00238990468875923,-0.033601104548885,
0.074578872643713));
#71675=CARTESIAN_POINT('Ctrl Pts',(0.00239626027702875,-0.0334837508592656,
0.074663844639805));
#71676=CARTESIAN_POINT('Ctrl Pts',(0.00240513097081255,-0.0333660264659097,
0.0747485909932007));
#71677=CARTESIAN_POINT('Ctrl Pts',(0.00238390402370508,-0.0336938721132474,
0.0745132128857947));
#71678=CARTESIAN_POINT('Ctrl Pts',(0.00238603002925264,-0.0336474569765,
0.0745468102974167));
#71679=CARTESIAN_POINT('Ctrl Pts',(0.00238854918924798,-0.033601104548885,
0.0745803805193434));
#71680=CARTESIAN_POINT('Ctrl Pts',(0.00239492712316441,-0.0334837508592656,
0.0746653726029762));
#71681=CARTESIAN_POINT('Ctrl Pts',(0.00240382074801805,-0.0333660264659097,
0.0747501383729442));
#71682=CARTESIAN_POINT('Ctrl Pts',(0.00215368868249986,-0.0336938721132474,
0.0747633547175056));
#71683=CARTESIAN_POINT('Ctrl Pts',(0.00215727885119442,-0.0336474569765,
0.0747982996559134));
#71684=CARTESIAN_POINT('Ctrl Pts',(0.00216127784851377,-0.033601104548885,
0.0748332001724142));
#71685=CARTESIAN_POINT('Ctrl Pts',(0.00217140239029833,-0.0334837508592656,
0.0749215602560544));
#71686=CARTESIAN_POINT('Ctrl Pts',(0.00218414077860928,-0.0333660264659097,
0.0750095815272931));
#71687=CARTESIAN_POINT('',(0.00215638230256883,-0.0336769361243754,0.0747746107158768));
#71688=CARTESIAN_POINT('',(0.00215506173625341,-0.0336938721132327,0.0747618628178939));
#71689=CARTESIAN_POINT('Ctrl Pts',(0.00215638230256886,-0.0336769361243751,
0.0747746107158772));
#71690=CARTESIAN_POINT('Ctrl Pts',(0.00215615992238297,-0.033679758667006,
0.0747724861421816));
#71691=CARTESIAN_POINT('Ctrl Pts',(0.00215593868522542,-0.0336825812712914,
0.0747703615300778));
#71692=CARTESIAN_POINT('Ctrl Pts',(0.00215549849665084,-0.0336882266005929,
0.0747661122309904));
#71693=CARTESIAN_POINT('Ctrl Pts',(0.00215527954523117,-0.0336910493256095,
0.0747639875440074));
#71694=CARTESIAN_POINT('Ctrl Pts',(0.00215506173625251,-0.0336938721132332,
0.0747618628178946));
#71695=CARTESIAN_POINT('Ctrl Pts',(0.00215638230256887,-0.0336769361243754,
0.0747746107158769));
#71696=CARTESIAN_POINT('Ctrl Pts',(0.0021980683132912,-0.0336279007656795,
0.0747702474203919));
#71697=CARTESIAN_POINT('Ctrl Pts',(0.00224034786837482,-0.0335767878916504,
0.0747658219983228));
#71698=CARTESIAN_POINT('Ctrl Pts',(0.00232320394749111,-0.0334733199151693,
0.0747571494112931));
#71699=CARTESIAN_POINT('Ctrl Pts',(0.00236382979889138,-0.0334209645163038,
0.0747528970832124));
#71700=CARTESIAN_POINT('Ctrl Pts',(0.00240367281091008,-0.0333679869844681,
0.0747487266953188));
#71701=CARTESIAN_POINT('',(0.00226948287999006,-0.0336938721132538,0.0746375378518675));
#71702=CARTESIAN_POINT('Origin',(0.00812378219310841,-0.0315241814719618,
0.07415));
#71703=CARTESIAN_POINT('',(0.00215638230386339,-0.0337108120655394,0.0747746107157469));
#71704=CARTESIAN_POINT('',(0.00215773009560755,-0.0336938721132327,0.0747873557640231));
#71705=CARTESIAN_POINT('Origin',(0.0185450458257195,-0.0345562511617489,
0.0741829112955836));
#71706=CARTESIAN_POINT('Ctrl Pts',(0.00215773009561513,-0.0336938721132297,
0.0747873557640264));
#71707=CARTESIAN_POINT('Ctrl Pts',(0.0021575032128262,-0.0336910493391369,
0.0747852319979679));
#71708=CARTESIAN_POINT('Ctrl Pts',(0.00215727745417631,-0.0336882266073566,
0.0747831080183507));
#71709=CARTESIAN_POINT('Ctrl Pts',(0.00215682818914659,-0.0336825812712765,
0.0747788596641427));
#71710=CARTESIAN_POINT('Ctrl Pts',(0.00215660468275411,-0.0336797586669985,
0.0747767352895666));
#71711=CARTESIAN_POINT('Ctrl Pts',(0.0021563823025688,-0.033676936124375,
0.0747746107158766));
#71712=CARTESIAN_POINT('Origin',(0.0183123534849744,-0.0345562514305373,
0.0719598466703149));
#71713=CARTESIAN_POINT('Ctrl Pts',(0.00238914140683346,-0.034243627687391,
0.0745882009269639));
#71714=CARTESIAN_POINT('Ctrl Pts',(0.00240566842724529,-0.033943005420181,
0.0748044864697307));
#71715=CARTESIAN_POINT('Ctrl Pts',(0.00243844000940833,-0.0336441434784052,
0.0750189126850498));
#71716=CARTESIAN_POINT('Ctrl Pts',(0.00241360232646182,-0.034243627687391,
0.0748370013759405));
#71717=CARTESIAN_POINT('Ctrl Pts',(0.00243951301049845,-0.033943005420181,
0.0750523643599149));
#71718=CARTESIAN_POINT('Ctrl Pts',(0.00248157210737336,-0.0336441434784052,
0.075265163821342));
#71719=CARTESIAN_POINT('Ctrl Pts',(0.0024138469356581,-0.034243627687391,
0.0748394893804303));
#71720=CARTESIAN_POINT('Ctrl Pts',(0.00243985145633099,-0.033943005420181,
0.0750548431388167));
#71721=CARTESIAN_POINT('Ctrl Pts',(0.00248200342835301,-0.0336441434784052,
0.0752676263327049));
#71722=CARTESIAN_POINT('',(0.00241803668792201,-0.0341934961088741,0.0748729061004349));
#71723=CARTESIAN_POINT('',(0.0024525545003163,-0.0338664212873141,0.0751067138871893));
#71724=CARTESIAN_POINT('Origin',(0.0190764587066775,-0.0345610751535256,
0.0732760016444799));
#71725=CARTESIAN_POINT('Origin',(-0.00836090388560083,-0.0336938005063928,
0.0769309530129564));
#71726=CARTESIAN_POINT('',(0.0024331008925787,-0.0336938721132327,0.0749832294616745));
#71727=CARTESIAN_POINT('',(0.00244349750017906,-0.0336938721132427,0.0750448586800035));
#71728=CARTESIAN_POINT('',(0.00240367281090953,-0.0340203938281605,0.0747487266953136));
#71729=CARTESIAN_POINT('Origin',(0.0190479843192207,-0.0345589643246074,
0.0737563366905984));
#71730=CARTESIAN_POINT('',(0.00240502396467459,-0.0341934961088739,0.074748585269382));
#71731=CARTESIAN_POINT('Origin',(-0.00855455086234155,-0.0341934220717637,
0.0758957286238388));
#71732=CARTESIAN_POINT('',(0.0024115303263083,-0.0341934961088841,0.0748107456849185));
#71733=CARTESIAN_POINT('Ctrl Pts',(0.00213648542098265,-0.0340223579322397,
0.0745402273216054));
#71734=CARTESIAN_POINT('Ctrl Pts',(0.00214186767350316,-0.0339125849573575,
0.0746228077596185));
#71735=CARTESIAN_POINT('Ctrl Pts',(0.0021489553671536,-0.0338030433565231,
0.0747052187691935));
#71736=CARTESIAN_POINT('Ctrl Pts',(0.00215773009560691,-0.0336938721132327,
0.0747873557640227));
#71737=CARTESIAN_POINT('Ctrl Pts',(0.00222603299406526,-0.0340223579322397,
0.074609670910117));
#71738=CARTESIAN_POINT('Ctrl Pts',(0.00223237305478783,-0.0339125849573575,
0.0746910162535475));
#71739=CARTESIAN_POINT('Ctrl Pts',(0.00224039232001169,-0.0338030433565231,
0.0747721732120223));
#71740=CARTESIAN_POINT('Ctrl Pts',(0.00225007133424981,-0.0336938721132327,
0.0748530389085596));
#71741=CARTESIAN_POINT('Ctrl Pts',(0.00231558056714786,-0.0340223579322397,
0.0746791144986287));
#71742=CARTESIAN_POINT('Ctrl Pts',(0.0023228784360725,-0.0339125849573575,
0.0747592247474764));
#71743=CARTESIAN_POINT('Ctrl Pts',(0.00233182927286978,-0.0338030433565231,
0.0748391276548511));
#71744=CARTESIAN_POINT('Ctrl Pts',(0.00234241257289271,-0.0336938721132327,
0.0749187220530965));
#71745=CARTESIAN_POINT('Ctrl Pts',(0.00240512814023047,-0.0340223579322397,
0.0747485580871403));
#71746=CARTESIAN_POINT('Ctrl Pts',(0.00241338381735716,-0.0339125849573575,
0.0748274332414054));
#71747=CARTESIAN_POINT('Ctrl Pts',(0.00242326622572788,-0.0338030433565231,
0.0749060820976799));
#71748=CARTESIAN_POINT('Ctrl Pts',(0.00243475381153561,-0.0336938721132327,
0.0749844051976334));
#71749=CARTESIAN_POINT('',(0.00229541549410313,-0.0336938721132427,0.0748852926128588));
#71750=CARTESIAN_POINT('Ctrl Pts',(0.00215638230744163,-0.0337108120662682,
0.0747746107153668));
#71751=CARTESIAN_POINT('Ctrl Pts',(0.00219914793354054,-0.0337611408994438,
0.0747701344160031));
#71752=CARTESIAN_POINT('Ctrl Pts',(0.00224113318184206,-0.0338121088781615,
0.0747657397991719));
#71753=CARTESIAN_POINT('Ctrl Pts',(0.00232358117069541,-0.0339153382773233,
0.0747571099271531));
#71754=CARTESIAN_POINT('Ctrl Pts',(0.00236400903073593,-0.0339675558473108,
0.074752878322926));
#71755=CARTESIAN_POINT('Ctrl Pts',(0.00240367281094967,-0.0340203938281304,
0.0747487266953146));
#71756=CARTESIAN_POINT('Ctrl Pts',(0.00241931371808394,-0.0341934961088741,
0.0748713304821396));
#71757=CARTESIAN_POINT('Ctrl Pts',(0.00243422665749493,-0.0340287516186244,
0.0749892658735396));
#71758=CARTESIAN_POINT('Ctrl Pts',(0.0024540012132723,-0.0338644633283559,
0.0751064841283056));
#71759=CARTESIAN_POINT('Ctrl Pts',(0.00241803668792207,-0.0341934961088741,
0.0748729061004349));
#71760=CARTESIAN_POINT('Ctrl Pts',(0.00243298220199995,-0.0340287516186244,
0.0749908678934274));
#71761=CARTESIAN_POINT('Ctrl Pts',(0.00245279039580763,-0.0338644633283559,
0.0751081111808905));
#71762=CARTESIAN_POINT('Ctrl Pts',(0.00220525882686514,-0.0341934961088741,
0.0751354345048027));
#71763=CARTESIAN_POINT('Ctrl Pts',(0.00222563190886776,-0.0340287516186244,
0.0752577953124335));
#71764=CARTESIAN_POINT('Ctrl Pts',(0.00225104484745915,-0.0338644633283559,
0.0753792095301615));
#71765=CARTESIAN_POINT('',(0.00220737723511777,-0.0341764758832392,0.0751480743277191));
#71766=CARTESIAN_POINT('',(0.00220525882686678,-0.034193496108874,0.0751354345048007));
#71767=CARTESIAN_POINT('Origin',(0.0186196216528808,-0.0345621026454919,
0.0728987275951916));
#71768=CARTESIAN_POINT('Ctrl Pts',(0.00220737723570005,-0.034176475883748,
0.075148074325991));
#71769=CARTESIAN_POINT('Ctrl Pts',(0.00224970356681359,-0.0341260050041583,
0.0751409340258941));
#71770=CARTESIAN_POINT('Ctrl Pts',(0.00229129416008601,-0.0340749269150491,
0.0751339178033822));
#71771=CARTESIAN_POINT('Ctrl Pts',(0.00237303613459714,-0.0339715436310937,
0.075120128256751));
#71772=CARTESIAN_POINT('Ctrl Pts',(0.0024131565058429,-0.033919277824191,
0.0751133601699633));
#71773=CARTESIAN_POINT('Ctrl Pts',(0.00245255449839893,-0.0338664212861448,
0.0751067138851224));
#71774=CARTESIAN_POINT('',(0.00231164775740439,-0.0341934961088841,0.0750041703026279));
#71775=CARTESIAN_POINT('Origin',(0.00812378219310841,-0.0315241814719618,
0.07415));
#71776=CARTESIAN_POINT('',(0.00220737723598346,-0.0342105180190534,0.0751480743284265));
#71777=CARTESIAN_POINT('',(0.00220952263615493,-0.0341934961088739,0.0751607095987538));
#71778=CARTESIAN_POINT('Origin',(0.0186172940355559,-0.0345621701730135,
0.072853459403901));
#71779=CARTESIAN_POINT('Origin',(0.0184492530654878,-0.0345621040853264,
0.0718887970165648));
#71780=CARTESIAN_POINT('Origin',(0.0184618988578972,-0.0345621714960468,
0.0719323247288287));
#71781=CARTESIAN_POINT('Ctrl Pts',(0.0024328513723479,-0.0346945769586966,
0.0749817503506608));
#71782=CARTESIAN_POINT('Ctrl Pts',(0.00245027271645716,-0.0345275153362945,
0.0751009491752261));
#71783=CARTESIAN_POINT('Ctrl Pts',(0.00247144725993594,-0.0343603235965186,
0.0752196309454758));
#71784=CARTESIAN_POINT('Ctrl Pts',(0.00249630716099106,-0.034193496108874,
0.0753374455841857));
#71785=CARTESIAN_POINT('Ctrl Pts',(0.00244679668926106,-0.0346945769586966,
0.0750644156790485));
#71786=CARTESIAN_POINT('Ctrl Pts',(0.00246594949177079,-0.0345275153362945,
0.0751833224133676));
#71787=CARTESIAN_POINT('Ctrl Pts',(0.00248884675552448,-0.0343603235965186,
0.0753016575650486));
#71788=CARTESIAN_POINT('Ctrl Pts',(0.00251541555892339,-0.034193496108874,
0.0754190721577369));
#71789=CARTESIAN_POINT('Ctrl Pts',(0.00246074200617428,-0.0346945769586966,
0.0751470810074338));
#71790=CARTESIAN_POINT('Ctrl Pts',(0.00248162626708448,-0.0345275153362945,
0.0752656956515077));
#71791=CARTESIAN_POINT('Ctrl Pts',(0.00250624625111307,-0.0343603235965186,
0.075383684184621));
#71792=CARTESIAN_POINT('Ctrl Pts',(0.00253452395685577,-0.034193496108874,
0.0755006987312884));
#71793=CARTESIAN_POINT('Ctrl Pts',(0.00247468732308737,-0.0346945769586966,
0.0752297463358237));
#71794=CARTESIAN_POINT('Ctrl Pts',(0.00249730304239805,-0.0345275153362945,
0.0753480688896505));
#71795=CARTESIAN_POINT('Ctrl Pts',(0.00252364574670156,-0.0343603235965186,
0.0754657108041943));
#71796=CARTESIAN_POINT('Ctrl Pts',(0.00255363235478807,-0.034193496108874,
0.0755823253048392));
#71797=CARTESIAN_POINT('',(0.00247468732294121,-0.0346945769586966,0.0752297463349562));
#71798=CARTESIAN_POINT('',(0.00252381793467388,-0.0343667727832779,0.0754609253620189));
#71799=CARTESIAN_POINT('Origin',(0.018954003831437,-0.0345626461565567,
0.0718936746724204));
#71800=CARTESIAN_POINT('Origin',(-0.00823743066395237,-0.0341934771027668,
0.0779800887105191));
#71801=CARTESIAN_POINT('',(0.00249664906299847,-0.034193496108874,0.075338906109001));
#71802=CARTESIAN_POINT('',(0.00251089488590508,-0.034193496108884,0.0753997609077536));
#71803=CARTESIAN_POINT('',(0.00245255450041352,-0.0345211942962698,0.0751067138848273));
#71804=CARTESIAN_POINT('Origin',(0.0190307066060976,-0.0345625596119866,
0.0723683396847151));
#71805=CARTESIAN_POINT('',(0.00245389410775944,-0.0346945769586885,0.0751064878983125));
#71806=CARTESIAN_POINT('Origin',(-0.00845552983703033,-0.0346945685853896,
0.0769468640561198));
#71807=CARTESIAN_POINT('',(0.00246429071536032,-0.0346945769587026,0.0751681171166444));
#71808=CARTESIAN_POINT('Ctrl Pts',(0.00217280268249536,-0.0345231616327841,
0.0749154037263385));
#71809=CARTESIAN_POINT('Ctrl Pts',(0.00218335269526068,-0.0344132092796988,
0.0749974296005833));
#71810=CARTESIAN_POINT('Ctrl Pts',(0.00219559880420149,-0.0343032738558979,
0.0750792330239777));
#71811=CARTESIAN_POINT('Ctrl Pts',(0.0022095226361549,-0.0341934961088739,
0.0751607095987539));
#71812=CARTESIAN_POINT('Ctrl Pts',(0.0022665338036514,-0.0345231616327841,
0.0749790874217822));
#71813=CARTESIAN_POINT('Ctrl Pts',(0.00227796160649894,-0.0344132092796988,
0.0750598213444847));
#71814=CARTESIAN_POINT('Ctrl Pts',(0.00229105873723346,-0.0343032738558979,
0.0751403147266002));
#71815=CARTESIAN_POINT('Ctrl Pts',(0.00230580577542545,-0.0341934961088739,
0.0752204648766023));
#71816=CARTESIAN_POINT('Ctrl Pts',(0.00236026492480743,-0.0345231616327841,
0.0750427711172259));
#71817=CARTESIAN_POINT('Ctrl Pts',(0.0023725705177372,-0.0344132092796988,
0.0751222130883861));
#71818=CARTESIAN_POINT('Ctrl Pts',(0.00238651867026543,-0.0343032738558979,
0.0752013964292226));
#71819=CARTESIAN_POINT('Ctrl Pts',(0.002402088914696,-0.0341934961088739,
0.0752802201544507));
#71820=CARTESIAN_POINT('Ctrl Pts',(0.00245399604596347,-0.0345231616327841,
0.0751064548126695));
#71821=CARTESIAN_POINT('Ctrl Pts',(0.00246717942897545,-0.0344132092796988,
0.0751846048322875));
#71822=CARTESIAN_POINT('Ctrl Pts',(0.0024819786032974,-0.0343032738558979,
0.075262478131845));
#71823=CARTESIAN_POINT('Ctrl Pts',(0.00249837205396655,-0.0341934961088739,
0.0753399754322991));
#71824=CARTESIAN_POINT('',(0.0023530858495867,-0.0341934961088839,0.0752498078538874));
#71825=CARTESIAN_POINT('Ctrl Pts',(0.00220737723938524,-0.0342105180195385,
0.075148074327847));
#71826=CARTESIAN_POINT('Ctrl Pts',(0.00224975115590851,-0.0342610556241365,
0.0751409260142033));
#71827=CARTESIAN_POINT('Ctrl Pts',(0.00229136469440918,-0.0343122189870295,
0.075133905973352));
#71828=CARTESIAN_POINT('Ctrl Pts',(0.00237310749295284,-0.0344158119695179,
0.0751201162836077));
#71829=CARTESIAN_POINT('Ctrl Pts',(0.00241320331961001,-0.034468199045008,
0.0751133522747961));
#71830=CARTESIAN_POINT('Ctrl Pts',(0.00245255450043772,-0.0345211942962506,
0.0751067138848174));
#71831=CARTESIAN_POINT('Ctrl Pts',(0.00247586261179299,-0.0346945769586932,
0.0752280940445576));
#71832=CARTESIAN_POINT('Ctrl Pts',(0.00249815144332193,-0.0345296777077528,
0.0753448607855227));
#71833=CARTESIAN_POINT('Ctrl Pts',(0.00252524730602475,-0.0343648066252516,
0.0754606065328785));
#71834=CARTESIAN_POINT('Ctrl Pts',(0.00247468732293958,-0.0346945769586932,
0.0752297463349473));
#71835=CARTESIAN_POINT('Ctrl Pts',(0.0024970103144032,-0.0345296777077528,
0.0753465373741779));
#71836=CARTESIAN_POINT('Ctrl Pts',(0.00252414131212109,-0.0343648066252516,
0.0754623059871751));
#71837=CARTESIAN_POINT('Ctrl Pts',(0.00227881362528771,-0.0346945769586932,
0.0755051171319187));
#71838=CARTESIAN_POINT('Ctrl Pts',(0.0023068297131307,-0.0345296777077528,
0.0756259577212511));
#71839=CARTESIAN_POINT('Ctrl Pts',(0.00233981631417512,-0.0343648066252516,
0.0757455371231554));
#71840=CARTESIAN_POINT('',(0.0022817215141913,-0.0346775396664978,0.0755175989972332));
#71841=CARTESIAN_POINT('',(0.00227881362529054,-0.0346945769586886,0.0755051171319192));
#71842=CARTESIAN_POINT('Origin',(0.0184108143037993,-0.0345626619277667,
0.0715850084953972));
#71843=CARTESIAN_POINT('Ctrl Pts',(0.00228172151476219,-0.0346775396670097,
0.0755175989955));
#71844=CARTESIAN_POINT('Ctrl Pts',(0.00232354889847931,-0.0346269749928344,
0.0755078073879644));
#71845=CARTESIAN_POINT('Ctrl Pts',(0.00236463290806837,-0.0345757902891101,
0.0754981897641689));
#71846=CARTESIAN_POINT('Ctrl Pts',(0.00244534805337453,-0.0344721681088584,
0.075479294731196));
#71847=CARTESIAN_POINT('Ctrl Pts',(0.00248494754623924,-0.0344197714290507,
0.0754700247352496));
#71848=CARTESIAN_POINT('Ctrl Pts',(0.00252381793443664,-0.0343667727831552,
0.07546092536172));
#71849=CARTESIAN_POINT('',(0.00237675047412587,-0.0346945769587026,0.0753674317334477));
#71850=CARTESIAN_POINT('Origin',(0.00812378219310841,-0.0315241814719618,
0.07415));
#71851=CARTESIAN_POINT('',(0.00228172151550705,-0.0347116136489607,0.0755175989976839));
#71852=CARTESIAN_POINT('',(0.00228465605720542,-0.0346945769586885,0.0755300746244476));
#71853=CARTESIAN_POINT('Origin',(0.0183986768196557,-0.0345626681602985,
0.0715413506044575));
#71854=CARTESIAN_POINT('Origin',(0.0184804353446439,-0.0345626630729688,
0.0718824000672343));
#71855=CARTESIAN_POINT('Origin',(0.0184889314692112,-0.0345626693828237,
0.0719269102778483));
#71856=CARTESIAN_POINT('Ctrl Pts',(0.00248873755723595,-0.0352450361874068,
0.0753011014626653));
#71857=CARTESIAN_POINT('Ctrl Pts',(0.00253215206129927,-0.0349452760959493,
0.0755136306585492));
#71858=CARTESIAN_POINT('Ctrl Pts',(0.00259145179795907,-0.034644428984174,
0.075722285923276));
#71859=CARTESIAN_POINT('Ctrl Pts',(0.00248929764596918,-0.0352450361874068,
0.0753035635604722));
#71860=CARTESIAN_POINT('Ctrl Pts',(0.00253280500957504,-0.0349452760959493,
0.075516071632263));
#71861=CARTESIAN_POINT('Ctrl Pts',(0.00259219575082006,-0.034644428984174,
0.0757246988383471));
#71862=CARTESIAN_POINT('Ctrl Pts',(0.00254475197599172,-0.0352450361874068,
0.0755473356205648));
#71863=CARTESIAN_POINT('Ctrl Pts',(0.00259745335371073,-0.0349452760959493,
0.0757577521979789));
#71864=CARTESIAN_POINT('Ctrl Pts',(0.00266585444992848,-0.034644428984174,
0.07596360132064));
#71865=CARTESIAN_POINT('Ctrl Pts',(0.00254530651929195,-0.0352450361874068,
0.0755497733411657));
#71866=CARTESIAN_POINT('Ctrl Pts',(0.00259809983715208,-0.0349452760959493,
0.075760169003636));
#71867=CARTESIAN_POINT('Ctrl Pts',(0.00266659103691956,-0.034644428984174,
0.0759659903454629));
#71868=CARTESIAN_POINT('',(0.00255362199724152,-0.0351951634053262,0.0755822945559194));
#71869=CARTESIAN_POINT('',(0.00261718186944784,-0.0348678972925388,0.0758099632150931));
#71870=CARTESIAN_POINT('Origin',(0.0185317384632803,-0.0345636767885976,
0.070571876353144));
#71871=CARTESIAN_POINT('Origin',(-0.00796241552129287,-0.0346946199341063,
0.0789991807159483));
#71872=CARTESIAN_POINT('',(0.00258240495244123,-0.0346945769330289,0.0756898906696988));
#71873=CARTESIAN_POINT('',(0.0026004437710606,-0.0346945769458128,0.0757497308912099));
#71874=CARTESIAN_POINT('',(0.00252381793464359,-0.0350221583435275,0.0754609253616882));
#71875=CARTESIAN_POINT('Origin',(0.0187097009618073,-0.0345628458715169,
0.0710185000669408));
#71876=CARTESIAN_POINT('',(0.00252502157108339,-0.035195136029876,0.0754606404896734));
#71877=CARTESIAN_POINT('Origin',(-0.00820389956172542,-0.03519518383668,
0.0779722326526504));
#71878=CARTESIAN_POINT('',(0.00255363235447195,-0.035195137132875,0.0755823253039986));
#71879=CARTESIAN_POINT('Ctrl Pts',(0.00223260586095877,-0.0350241211494342,
0.0752875594153934));
#71880=CARTESIAN_POINT('Ctrl Pts',(0.00224827527548829,-0.0349144232818961,
0.0753687079538924));
#71881=CARTESIAN_POINT('Ctrl Pts',(0.0022656314671941,-0.0348045283579412,
0.0754495811657081));
#71882=CARTESIAN_POINT('Ctrl Pts',(0.00228465605976146,-0.0346945769439158,
0.0755300746352625));
#71883=CARTESIAN_POINT('Ctrl Pts',(0.00233015078822936,-0.0350241211494342,
0.0753452320169192));
#71884=CARTESIAN_POINT('Ctrl Pts',(0.00234661461919822,-0.0349144232818961,
0.0754250369140401));
#71885=CARTESIAN_POINT('Ctrl Pts',(0.00236473792881249,-0.0348045283579412,
0.075504549259088));
#71886=CARTESIAN_POINT('Ctrl Pts',(0.00238450129331217,-0.0346945769439158,
0.0755836663430184));
#71887=CARTESIAN_POINT('Ctrl Pts',(0.00242769571549996,-0.0350241211494342,
0.0754029046184451));
#71888=CARTESIAN_POINT('Ctrl Pts',(0.00244495396290814,-0.0349144232818961,
0.0754813658741877));
#71889=CARTESIAN_POINT('Ctrl Pts',(0.00246384439043087,-0.0348045283579412,
0.0755595173524679));
#71890=CARTESIAN_POINT('Ctrl Pts',(0.00248434652686288,-0.0346945769439158,
0.0756372580507742));
#71891=CARTESIAN_POINT('Ctrl Pts',(0.00252524064277055,-0.0350241211494342,
0.0754605772199709));
#71892=CARTESIAN_POINT('Ctrl Pts',(0.00254329330661806,-0.0349144232818961,
0.0755376948343354));
#71893=CARTESIAN_POINT('Ctrl Pts',(0.00256295085204925,-0.0348045283579412,
0.0756144854458478));
#71894=CARTESIAN_POINT('Ctrl Pts',(0.00258419176041358,-0.0346945769439158,
0.07569084975853));
#71895=CARTESIAN_POINT('',(0.00243353050467004,-0.0346945769458128,0.0756099826468189));
#71896=CARTESIAN_POINT('Ctrl Pts',(0.0022817215187041,-0.034711613649279,
0.0755175989969295));
#71897=CARTESIAN_POINT('Ctrl Pts',(0.00232353229480107,-0.0347621546532343,
0.0755078112903928));
#71898=CARTESIAN_POINT('Ctrl Pts',(0.00236460792446927,-0.0348133084097125,
0.0754981956781862));
#71899=CARTESIAN_POINT('Ctrl Pts',(0.00244532317134808,-0.0349168561544567,
0.0754793006175525));
#71900=CARTESIAN_POINT('Ctrl Pts',(0.00248493077292884,-0.0349692089015914,
0.0754700286638342));
#71901=CARTESIAN_POINT('Ctrl Pts',(0.00252381793468374,-0.0350221583434999,
0.0754609253616993));
#71902=CARTESIAN_POINT('Ctrl Pts',(0.00255440383340984,-0.0351951371254872,
0.0755810822271085));
#71903=CARTESIAN_POINT('Ctrl Pts',(0.00258399056056355,-0.035030733898092,
0.0756962256303476));
#71904=CARTESIAN_POINT('Ctrl Pts',(0.00261831100713141,-0.0348659306897825,
0.0758100477928667));
#71905=CARTESIAN_POINT('Ctrl Pts',(0.00255363235458435,-0.0351951371254872,
0.0755823253039693));
#71906=CARTESIAN_POINT('Ctrl Pts',(0.00258324478157223,-0.035030733898092,
0.075697484657049));
#71907=CARTESIAN_POINT('Ctrl Pts',(0.00261759156523801,-0.0348659306897825,
0.0758113216935779));
#71908=CARTESIAN_POINT('Ctrl Pts',(0.00242433169938697,-0.0351951371254872,
0.0757906662813757));
#71909=CARTESIAN_POINT('Ctrl Pts',(0.00245825144536512,-0.035030733898092,
0.0759084988443757));
#71910=CARTESIAN_POINT('Ctrl Pts',(0.00249701235409287,-0.0348659306897825,
0.076024828780441));
#71911=CARTESIAN_POINT('Origin',(-0.00247467617372032,-0.0308609197410693,
0.0773449024790721));
#71912=CARTESIAN_POINT('',(0.00249726018426095,-0.0351951371254872,0.0756731572726532));
#71913=CARTESIAN_POINT('Origin',(0.0090085778923309,-0.03518404674412,0.0737354131937099));
#71914=CARTESIAN_POINT('Origin',(-0.00307767051212848,-0.0352322613345126,
0.0783566974641126));
#71915=CARTESIAN_POINT('',(0.00269015874208231,-0.0351951142564657,0.0760350864107232));
#71916=CARTESIAN_POINT('',(0.00273355139268732,-0.0351951372916788,0.0761519770024135));
#71917=CARTESIAN_POINT('Origin',(0.00839212773806127,-0.035287512144001,
0.0743597447775152));
#71918=CARTESIAN_POINT('Origin',(0.00690647465570691,-0.0298325076522345,
0.066746395969514));
#71919=CARTESIAN_POINT('Origin',(-0.000254157257254604,-0.033873118223129,
0.0738958328557447));
#71920=CARTESIAN_POINT('Ctrl Pts',(0.00261993952981883,-0.0321934096636942,
0.0724809129192682));
#71921=CARTESIAN_POINT('Ctrl Pts',(0.00259006366587907,-0.0320508460843096,
0.0725794290820573));
#71922=CARTESIAN_POINT('Ctrl Pts',(0.00256285726334741,-0.0319086045660617,
0.0726786736688491));
#71923=CARTESIAN_POINT('Ctrl Pts',(0.00253836131002253,-0.0317669892864235,
0.0727784281659069));
#71924=CARTESIAN_POINT('Ctrl Pts',(0.00259735658310347,-0.0321934096636942,
0.0725616621802282));
#71925=CARTESIAN_POINT('Ctrl Pts',(0.00256892609248277,-0.0320508460843096,
0.0726605825670096));
#71926=CARTESIAN_POINT('Ctrl Pts',(0.002543174834155,-0.0319086045660617,
0.0727601922386784));
#71927=CARTESIAN_POINT('Ctrl Pts',(0.00252014059802141,-0.0317669892864235,
0.0728602721533488));
#71928=CARTESIAN_POINT('Ctrl Pts',(0.0025747736363881,-0.0321934096636942,
0.0726424114411881));
#71929=CARTESIAN_POINT('Ctrl Pts',(0.00254778851908645,-0.0320508460843096,
0.0727417360519618));
#71930=CARTESIAN_POINT('Ctrl Pts',(0.00252349240496258,-0.0319086045660617,
0.0728417108085077));
#71931=CARTESIAN_POINT('Ctrl Pts',(0.00250191988602029,-0.0317669892864235,
0.0729421161407907));
#71932=CARTESIAN_POINT('Ctrl Pts',(0.00255219068967273,-0.0321934096636942,
0.0727231607021481));
#71933=CARTESIAN_POINT('Ctrl Pts',(0.00252665094569015,-0.0320508460843096,
0.0728228895369141));
#71934=CARTESIAN_POINT('Ctrl Pts',(0.00250380997577015,-0.0319086045660617,
0.0729232293783371));
#71935=CARTESIAN_POINT('Ctrl Pts',(0.00248369917401917,-0.0317669892864235,
0.0730239601282326));
#71936=CARTESIAN_POINT('',(0.00255259470305427,-0.0321934096636942,0.0727217160819132));
#71937=CARTESIAN_POINT('',(0.00249861816834072,-0.0318665617511265,0.0729518119164843));
#71938=CARTESIAN_POINT('Origin',(0.0185752685902041,-0.0326371944423118,
0.0774642709158772));
#71939=CARTESIAN_POINT('Origin',(-0.00822206054077306,-0.0316939261509366,
0.0706682537005622));
#71940=CARTESIAN_POINT('',(0.0025849267118823,-0.0320197221621813,0.0726012362592632));
#71941=CARTESIAN_POINT('Ctrl Pts',(0.00258483310894102,-0.0320197392094734,
0.0726013958003824));
#71942=CARTESIAN_POINT('Ctrl Pts',(0.00257695335811615,-0.0319792716576031,
0.0726295797666881));
#71943=CARTESIAN_POINT('Ctrl Pts',(0.00256925259888108,-0.0319386439829669,
0.0726579521091869));
#71944=CARTESIAN_POINT('Ctrl Pts',(0.00256173090911167,-0.03189790993816,
0.0726865448288411));
#71945=CARTESIAN_POINT('Ctrl Pts',(0.00255420936801374,-0.0318571766984903,
0.0727151369833401));
#71946=CARTESIAN_POINT('Ctrl Pts',(0.00254690339562464,-0.0318163871833552,
0.072743803729002));
#71947=CARTESIAN_POINT('Ctrl Pts',(0.00253983470939491,-0.0317755399638303,
0.0727724455944296));
#71948=CARTESIAN_POINT('',(0.00258626132929582,-0.0321934096636184,0.0726013351935164));
#71949=CARTESIAN_POINT('Origin',(0.00035674042977136,-0.0324113908119595,
0.0719996587770169));
#71950=CARTESIAN_POINT('',(0.00256942801618504,-0.0321934096636663,0.0726615256377248));
#71951=CARTESIAN_POINT('Ctrl Pts',(0.00255436214565888,-0.0321934096636618,
0.0727207211778884));
#71952=CARTESIAN_POINT('Ctrl Pts',(0.00253465127678719,-0.0320835708272592,
0.0727975278208948));
#71953=CARTESIAN_POINT('Ctrl Pts',(0.00251654135050567,-0.0319739230346489,
0.0728746978283338));
#71954=CARTESIAN_POINT('Ctrl Pts',(0.00250004795967516,-0.0318646057455573,
0.0729521306882717));
#71955=CARTESIAN_POINT('Ctrl Pts',(0.0024556133303472,-0.0321934096636618,
0.0727763074733133));
#71956=CARTESIAN_POINT('Ctrl Pts',(0.00243666903981085,-0.0320835708272592,
0.0728544759394432));
#71957=CARTESIAN_POINT('Ctrl Pts',(0.00241935343007684,-0.0319739230346489,
0.0729329911157941));
#71958=CARTESIAN_POINT('Ctrl Pts',(0.00240368094564729,-0.0318646057455573,
0.0730117508473781));
#71959=CARTESIAN_POINT('Ctrl Pts',(0.00235686451503552,-0.0321934096636618,
0.0728318937687382));
#71960=CARTESIAN_POINT('Ctrl Pts',(0.00233868680283451,-0.0320835708272592,
0.0729114240579916));
#71961=CARTESIAN_POINT('Ctrl Pts',(0.002322165509648,-0.0319739230346489,
0.0729912844032544));
#71962=CARTESIAN_POINT('Ctrl Pts',(0.00230731393161943,-0.0318646057455573,
0.0730713710064846));
#71963=CARTESIAN_POINT('Ctrl Pts',(0.00225811569972384,-0.0321934096636618,
0.0728874800641631));
#71964=CARTESIAN_POINT('Ctrl Pts',(0.00224070456585816,-0.0320835708272592,
0.07296837217654));
#71965=CARTESIAN_POINT('Ctrl Pts',(0.00222497758921917,-0.0319739230346489,
0.0730495776907147));
#71966=CARTESIAN_POINT('Ctrl Pts',(0.00221094691759156,-0.0318646057455573,
0.073130991165591));
#71967=CARTESIAN_POINT('',(0.00225543231761759,-0.0321763980308446,0.0729000121134659));
#71968=CARTESIAN_POINT('',(0.00225811569971697,-0.0321934096636185,0.072887480064195));
#71969=CARTESIAN_POINT('Origin',(0.018301100644114,-0.032638623085492,0.0769450855961415));
#71970=CARTESIAN_POINT('Ctrl Pts',(0.00225543232071656,-0.0321763980306266,
0.0729000121141224));
#71971=CARTESIAN_POINT('Ctrl Pts',(0.002297409501156,-0.0321259596175108,
0.0729089534635944));
#71972=CARTESIAN_POINT('Ctrl Pts',(0.00233865937247787,-0.0320749164631984,
0.0729177398925782));
#71973=CARTESIAN_POINT('Ctrl Pts',(0.00241973769352951,-0.0319716057793896,
0.0729350099806482));
#71974=CARTESIAN_POINT('Ctrl Pts',(0.00245953455235092,-0.031919378669009,
0.0729434869107129));
#71975=CARTESIAN_POINT('Ctrl Pts',(0.00249861817015242,-0.0318665617525271,
0.0729518119168646));
#71976=CARTESIAN_POINT('',(0.00240535520139562,-0.0321934096636664,0.0728045980730641));
#71977=CARTESIAN_POINT('Origin',(0.00812378219310841,-0.0315241814719618,
0.07415));
#71978=CARTESIAN_POINT('',(0.00225543231725343,-0.032210423332378,0.0729000121133884));
#71979=CARTESIAN_POINT('',(0.00225277570667768,-0.0321934096636183,0.0729125498651181));
#71980=CARTESIAN_POINT('Origin',(0.0183166330047819,-0.0326387230361829,
0.0769024945259561));
#71981=CARTESIAN_POINT('Origin',(0.018556727463541,-0.0326386245551484,
0.0757450017082887));
#71982=CARTESIAN_POINT('Origin',(0.0185535487766797,-0.0326387242491453,
0.0757902245208387));
#71983=CARTESIAN_POINT('Ctrl Pts',(0.00253439533689285,-0.0327445246967097,
0.0727946846966241));
#71984=CARTESIAN_POINT('Ctrl Pts',(0.00248327878458362,-0.032443687833936,
0.0730054918681366));
#71985=CARTESIAN_POINT('Ctrl Pts',(0.00244818630673866,-0.0321434074405927,
0.073219550466375));
#71986=CARTESIAN_POINT('Ctrl Pts',(0.00248077689844309,-0.0327445246967097,
0.0730388671346867));
#71987=CARTESIAN_POINT('Ctrl Pts',(0.00243886983734017,-0.032443687833936,
0.0732516965586647));
#71988=CARTESIAN_POINT('Ctrl Pts',(0.00241311301183042,-0.0321434074405927,
0.0734670779678456));
#71989=CARTESIAN_POINT('',(0.00247390547970712,-0.0326943950436612,0.0730743522308083));
#71990=CARTESIAN_POINT('',(0.00243448329139577,-0.0323666188837389,0.0733073832383745));
#71991=CARTESIAN_POINT('Origin',(0.0190022764167063,-0.0326395579111547,
0.0761437190053379));
#71992=CARTESIAN_POINT('Origin',(-0.00849094901744373,-0.0321933825603011,
0.071689266830627));
#71993=CARTESIAN_POINT('',(0.00245414059759521,-0.0321934096532688,0.0731839310712801));
#71994=CARTESIAN_POINT('',(0.00244498388243575,-0.0321934096584275,0.0732457566720727));
#71995=CARTESIAN_POINT('',(0.00249861816740909,-0.0325210109756238,0.0729518119162755));
#71996=CARTESIAN_POINT('Origin',(0.0188875491908828,-0.0326393129156696,
0.0766106473652476));
#71997=CARTESIAN_POINT('',(0.00249994689401835,-0.0326943950436593,0.0729520949416965));
#71998=CARTESIAN_POINT('Origin',(-0.00831977921037526,-0.0326943765538164,
0.0706474379779526));
#71999=CARTESIAN_POINT('',(0.00248692618687274,-0.0326943950436702,0.0730132235862623));
#72000=CARTESIAN_POINT('Ctrl Pts',(0.00230893750821803,-0.0325229783203769,
0.0726709525732306));
#72001=CARTESIAN_POINT('Ctrl Pts',(0.00228854887178465,-0.032413025309245,
0.0727511100800496));
#72002=CARTESIAN_POINT('Ctrl Pts',(0.00226982148868562,-0.0323031222208069,
0.0728316771945477));
#72003=CARTESIAN_POINT('Ctrl Pts',(0.00225277570575284,-0.0321934096576658,
0.0729125498695059));
#72004=CARTESIAN_POINT('Ctrl Pts',(0.0023726429815818,-0.0325229783203769,
0.0727646689266587));
#72005=CARTESIAN_POINT('Ctrl Pts',(0.00235354622303098,-0.032413025309245,
0.0728439482549205));
#72006=CARTESIAN_POINT('Ctrl Pts',(0.00233609235562436,-0.0323031222208069,
0.0729236105999009));
#72007=CARTESIAN_POINT('Ctrl Pts',(0.00232030013580616,-0.0321934096576658,
0.0730035531308888));
#72008=CARTESIAN_POINT('Ctrl Pts',(0.00243634845494557,-0.0325229783203769,
0.0728583852800867));
#72009=CARTESIAN_POINT('Ctrl Pts',(0.00241854357427731,-0.032413025309245,
0.0729367864297913));
#72010=CARTESIAN_POINT('Ctrl Pts',(0.00240236322256311,-0.0323031222208069,
0.0730155440052541));
#72011=CARTESIAN_POINT('Ctrl Pts',(0.00238782456585947,-0.0321934096576658,
0.0730945563922718));
#72012=CARTESIAN_POINT('Ctrl Pts',(0.00250005392830934,-0.0325229783203769,
0.0729521016335148));
#72013=CARTESIAN_POINT('Ctrl Pts',(0.00248354092552364,-0.032413025309245,
0.0730296246046622));
#72014=CARTESIAN_POINT('Ctrl Pts',(0.00246863408950186,-0.0323031222208069,
0.0731074774106072));
#72015=CARTESIAN_POINT('Ctrl Pts',(0.00245534899591279,-0.0321934096576658,
0.0731855596536547));
#72016=CARTESIAN_POINT('',(0.00235345815208435,-0.0321934096584274,0.0730482404676965));
#72017=CARTESIAN_POINT('Ctrl Pts',(0.00225543232065011,-0.0322104233328924,
0.0729000121141082));
#72018=CARTESIAN_POINT('Ctrl Pts',(0.00229746638087521,-0.0322609421831408,
0.072908965579259));
#72019=CARTESIAN_POINT('Ctrl Pts',(0.00233874403892756,-0.0323120888240825,
0.0729177579269624));
#72020=CARTESIAN_POINT('Ctrl Pts',(0.00241982297379117,-0.0324156524631811,
0.0729350281457774));
#72021=CARTESIAN_POINT('Ctrl Pts',(0.00245959092292148,-0.0324680267167303,
0.0729434989179262));
#72022=CARTESIAN_POINT('Ctrl Pts',(0.00249861816745052,-0.0325210109755912,
0.0729518119162889));
#72023=CARTESIAN_POINT('Origin',(0.0106777517417982,-0.0262834582512102,
0.0667081839996702));
#72024=CARTESIAN_POINT('Origin',(-0.00137820958750585,-0.0342770679433053,
0.0665648411243571));
#72025=CARTESIAN_POINT('Ctrl Pts',(0.00247560655120864,-0.0326943950436604,
0.0730732485793327));
#72026=CARTESIAN_POINT('Ctrl Pts',(0.0024607668985846,-0.0325844576448134,
0.0731510910254874));
#72027=CARTESIAN_POINT('Ctrl Pts',(0.00244753610514621,-0.0324744968375322,
0.0732292458890192));
#72028=CARTESIAN_POINT('Ctrl Pts',(0.00243592974177329,-0.0323646534831894,
0.0733076127995393));
#72029=CARTESIAN_POINT('Ctrl Pts',(0.0023805430241299,-0.0326943950436604,
0.0731349255880212));
#72030=CARTESIAN_POINT('Ctrl Pts',(0.00236655339628062,-0.0325844576448134,
0.0732140781877471));
#72031=CARTESIAN_POINT('Ctrl Pts',(0.00235419978389844,-0.0324744968375322,
0.0732935257176657));
#72032=CARTESIAN_POINT('Ctrl Pts',(0.00234349661112315,-0.0323646534831894,
0.0733731661666505));
#72033=CARTESIAN_POINT('Ctrl Pts',(0.00228547949705116,-0.0326943950436604,
0.0731966025967096));
#72034=CARTESIAN_POINT('Ctrl Pts',(0.00227233989397664,-0.0325844576448134,
0.0732770653500068));
#72035=CARTESIAN_POINT('Ctrl Pts',(0.00226086346265067,-0.0324744968375322,
0.0733578055463122));
#72036=CARTESIAN_POINT('Ctrl Pts',(0.002251063480473,-0.0323646534831894,
0.0734387195337618));
#72037=CARTESIAN_POINT('Ctrl Pts',(0.00219041596997242,-0.0326943950436604,
0.0732582796053981));
#72038=CARTESIAN_POINT('Ctrl Pts',(0.00217812639167266,-0.0325844576448134,
0.0733400525122664));
#72039=CARTESIAN_POINT('Ctrl Pts',(0.00216752714140291,-0.0324744968375322,
0.0734220853749587));
#72040=CARTESIAN_POINT('Ctrl Pts',(0.00215863034982285,-0.0323646534831894,
0.073504272900873));
#72041=CARTESIAN_POINT('',(0.00218852477659689,-0.0326773559991149,0.0732709554164597));
#72042=CARTESIAN_POINT('',(0.00219041596997239,-0.0326943950436586,0.0732582796053982));
#72043=CARTESIAN_POINT('Origin',(0.0186218521183369,-0.0326395662072158,
0.0756540325384767));
#72044=CARTESIAN_POINT('Ctrl Pts',(0.00218852477990817,-0.0326773559987408,
0.0732709554169462));
#72045=CARTESIAN_POINT('Ctrl Pts',(0.00223101472548232,-0.0326267922586254,
0.0732772484138444));
#72046=CARTESIAN_POINT('Ctrl Pts',(0.00227275156745392,-0.0325756109579953,
0.0732834298719168));
#72047=CARTESIAN_POINT('Ctrl Pts',(0.00235475456441007,-0.0324719985462359,
0.0732955749711518));
#72048=CARTESIAN_POINT('Ctrl Pts',(0.00239498783015737,-0.0324196091621769,
0.0733015337412356));
#72049=CARTESIAN_POINT('Ctrl Pts',(0.002434483291444,-0.0323666188837756,
0.0733073832383817));
#72050=CARTESIAN_POINT('',(0.00233216072484976,-0.0326943950436699,0.0731663159181133));
#72051=CARTESIAN_POINT('Origin',(0.00812378219310841,-0.0315241814719618,
0.07415));
#72052=CARTESIAN_POINT('',(0.00218852477663969,-0.032711433838005,0.0732709554164661));
#72053=CARTESIAN_POINT('',(0.0021866606600143,-0.0326943950436593,0.0732836352377341));
#72054=CARTESIAN_POINT('Origin',(0.0186277245646419,-0.0326395663828417,
0.0756091043363607));
#72055=CARTESIAN_POINT('Origin',(0.0186071336100769,-0.0326395680916905,
0.0757534299451567));
#72056=CARTESIAN_POINT('Origin',(0.0185997258295675,-0.0326395677069748,
0.0757981315088539));
#72057=CARTESIAN_POINT('Ctrl Pts',(0.002460316931823,-0.0332451089994433,
0.0731483582305965));
#72058=CARTESIAN_POINT('Ctrl Pts',(0.00242253939441707,-0.0329451141710254,
0.0733619593176228));
#72059=CARTESIAN_POINT('Ctrl Pts',(0.00240095848609075,-0.0326442513127493,
0.0735777991450574));
#72060=CARTESIAN_POINT('Ctrl Pts',(0.00242213832423559,-0.0332451089994433,
0.0733954258203826));
#72061=CARTESIAN_POINT('Ctrl Pts',(0.00239367909343392,-0.0329451141710254,
0.0736104668371525));
#72062=CARTESIAN_POINT('Ctrl Pts',(0.00238149848078103,-0.0326442513127493,
0.0738270406106954));
#72063=CARTESIAN_POINT('Ctrl Pts',(0.00242175653815972,-0.0332451089994433,
0.0733978964962804));
#72064=CARTESIAN_POINT('Ctrl Pts',(0.00239339049042408,-0.0329451141710254,
0.0736129519123477));
#72065=CARTESIAN_POINT('Ctrl Pts',(0.00238130388072793,-0.0326442513127493,
0.0738295330253518));
#72066=CARTESIAN_POINT('',(0.00241751373855127,-0.0331951640388616,0.0734312334700842));
#72067=CARTESIAN_POINT('',(0.00239280147173386,-0.0328677532354992,0.0736662799972576));
#72068=CARTESIAN_POINT('Origin',(0.0191286168676268,-0.0326402808281847,
0.0747621277855758));
#72069=CARTESIAN_POINT('Origin',(-0.00862402338789303,-0.0326944278779084,
0.0727367892861736));
#72070=CARTESIAN_POINT('',(0.00240466836925949,-0.0326943950436593,0.0735418371354143));
#72071=CARTESIAN_POINT('',(0.00239941178496456,-0.0326943950436693,0.0736041156896901));
#72072=CARTESIAN_POINT('',(0.00243448329139616,-0.0330220786163545,0.0733073832383717));
#72073=CARTESIAN_POINT('Origin',(0.019119573466244,-0.0326396682762752,
0.0752428260920572));
#72074=CARTESIAN_POINT('',(0.00243582716738045,-0.0331951640388587,0.0733075822738707));
#72075=CARTESIAN_POINT('Origin',(-0.00847678952003185,-0.033195202656004,
0.0716913624358378));
#72076=CARTESIAN_POINT('',(0.00242667045297585,-0.0331951640388701,0.0733694078719874));
#72077=CARTESIAN_POINT('Ctrl Pts',(0.00222754144166722,-0.0330240426238171,
0.0730389891984906));
#72078=CARTESIAN_POINT('Ctrl Pts',(0.00221223618547105,-0.0329142774063519,
0.0731202156592707));
#72079=CARTESIAN_POINT('Ctrl Pts',(0.00219860247688576,-0.0328043479726691,
0.0732017990168026));
#72080=CARTESIAN_POINT('Ctrl Pts',(0.00218666066001426,-0.0326943950436593,
0.0732836352377341));
#72081=CARTESIAN_POINT('Ctrl Pts',(0.00229700570278015,-0.0330240426238171,
0.0731285204914141));
#72082=CARTESIAN_POINT('Ctrl Pts',(0.00228293382737012,-0.0329142774063519,
0.0732087900143216));
#72083=CARTESIAN_POINT('Ctrl Pts',(0.00227051433187736,-0.0328043479726691,
0.0732893904594863));
#72084=CARTESIAN_POINT('Ctrl Pts',(0.00225976597022969,-0.0326943950436593,
0.073370219009902));
#72085=CARTESIAN_POINT('Ctrl Pts',(0.00236646996389308,-0.0330240426238171,
0.0732180517843375));
#72086=CARTESIAN_POINT('Ctrl Pts',(0.00235363146926918,-0.0329142774063519,
0.0732973643693725));
#72087=CARTESIAN_POINT('Ctrl Pts',(0.00234242618686896,-0.0328043479726691,
0.0733769819021701));
#72088=CARTESIAN_POINT('Ctrl Pts',(0.00233287128044513,-0.0326943950436593,
0.0734568027820699));
#72089=CARTESIAN_POINT('Ctrl Pts',(0.00243593422500602,-0.0330240426238171,
0.073307583077261));
#72090=CARTESIAN_POINT('Ctrl Pts',(0.00242432911116825,-0.0329142774063519,
0.0733859387244234));
#72091=CARTESIAN_POINT('Ctrl Pts',(0.00241433804186056,-0.0328043479726691,
0.0734645733448538));
#72092=CARTESIAN_POINT('Ctrl Pts',(0.00240597659066056,-0.0326943950436593,
0.0735433865542377));
#72093=CARTESIAN_POINT('',(0.0022956645146469,-0.0326943950436693,0.0734127361865842));
#72094=CARTESIAN_POINT('Ctrl Pts',(0.0021885247799137,-0.0327114338383321,
0.0732709554169469));
#72095=CARTESIAN_POINT('Ctrl Pts',(0.00223100765805619,-0.0327619876831129,
0.0732772473671192));
#72096=CARTESIAN_POINT('Ctrl Pts',(0.00227274104798354,-0.0328131562604663,
0.0732834283139248));
#72097=CARTESIAN_POINT('Ctrl Pts',(0.00235474396955514,-0.0329167375858764,
0.0732955734019949));
#72098=CARTESIAN_POINT('Ctrl Pts',(0.00239498082705073,-0.0329691088920619,
0.0733015327040366));
#72099=CARTESIAN_POINT('Ctrl Pts',(0.0024344832914428,-0.0330220786163187,
0.0733073832383814));
#72100=CARTESIAN_POINT('Ctrl Pts',(0.00241914241450137,-0.0331951640388604,
0.0734300249923475));
#72101=CARTESIAN_POINT('Ctrl Pts',(0.00240425739282318,-0.0330306422010619,
0.0735479647622954));
#72102=CARTESIAN_POINT('Ctrl Pts',(0.00239425966501202,-0.0328657861914644,
0.0736664189671357));
#72103=CARTESIAN_POINT('Ctrl Pts',(0.00241751373855174,-0.0331951640388604,
0.0734312334700811));
#72104=CARTESIAN_POINT('Ctrl Pts',(0.00240265370137588,-0.0330306422010619,
0.0735492069118601));
#72105=CARTESIAN_POINT('Ctrl Pts',(0.00239268232841017,-0.0328657861914644,
0.0736676937271233));
#72106=CARTESIAN_POINT('Ctrl Pts',(0.0021461325260133,-0.0331951640388604,
0.0736325983596107));
#72107=CARTESIAN_POINT('Ctrl Pts',(0.00213543557882531,-0.0330306422010619,
0.0737561824339654));
#72108=CARTESIAN_POINT('Ctrl Pts',(0.00212985563186088,-0.0328657861914644,
0.0738801030226711));
#72109=CARTESIAN_POINT('',(0.00214504098399125,-0.0331781648281896,0.0736453679061157));
#72110=CARTESIAN_POINT('',(0.00214613252601325,-0.033195164038858,0.0736325983596112));
#72111=CARTESIAN_POINT('Origin',(0.0186534028072523,-0.0326412086709817,
0.0743239466882793));
#72112=CARTESIAN_POINT('Ctrl Pts',(0.00214504098516957,-0.033178164828644,
0.0736453679047027));
#72113=CARTESIAN_POINT('Ctrl Pts',(0.00218787169502291,-0.0331276811546784,
0.0736489829931305));
#72114=CARTESIAN_POINT('Ctrl Pts',(0.00222992901774062,-0.0330765663497797,
0.0736525327705596));
#72115=CARTESIAN_POINT('Ctrl Pts',(0.00231253300989468,-0.0329730614463142,
0.0736595049148786));
#72116=CARTESIAN_POINT('Ctrl Pts',(0.00235304630866117,-0.0329207133373816,
0.0736629244705147));
#72117=CARTESIAN_POINT('Ctrl Pts',(0.00239280146422714,-0.0328677532289352,
0.0736662799825947));
#72118=CARTESIAN_POINT('',(0.00228182313229225,-0.0331951640388698,0.0735319159148577));
#72119=CARTESIAN_POINT('Origin',(0.00812378219310841,-0.0315241814719618,
0.07415));
#72120=CARTESIAN_POINT('',(0.00214504098548132,-0.0332121607144223,0.0736453679068907));
#72121=CARTESIAN_POINT('',(0.00214397671962883,-0.0331951640388587,0.0736581397562618));
#72122=CARTESIAN_POINT('Origin',(0.018649346519188,-0.0326413645333489,
0.0742787828462342));
#72123=CARTESIAN_POINT('Origin',(0.018533594970632,-0.0326412101255305,
0.0757434317878519));
#72124=CARTESIAN_POINT('Origin',(0.018522020263712,-0.0326413657463797,
0.0757872766267247));
#72125=CARTESIAN_POINT('Ctrl Pts',(0.00240860121255209,-0.0337436976235975,
0.0735059259673862));
#72126=CARTESIAN_POINT('Ctrl Pts',(0.00240280831309068,-0.0336723290703325,
0.0735573291712847));
#72127=CARTESIAN_POINT('Ctrl Pts',(0.00239794093240255,-0.033601104548885,
0.0736088282553585));
#72128=CARTESIAN_POINT('Ctrl Pts',(0.00238240035003915,-0.0333736987606856,
0.0737732546294123));
#72129=CARTESIAN_POINT('Ctrl Pts',(0.00237632111074342,-0.0331450831799191,
0.073938301850032));
#72130=CARTESIAN_POINT('Ctrl Pts',(0.00238601054224536,-0.0337436976235975,
0.0737549031985041));
#72131=CARTESIAN_POINT('Ctrl Pts',(0.00238245698173415,-0.0336723290703325,
0.073806509586315));
#72132=CARTESIAN_POINT('Ctrl Pts',(0.00237983223236211,-0.033601104548885,
0.0738581715427814));
#72133=CARTESIAN_POINT('Ctrl Pts',(0.00237145192755075,-0.0333736987606856,
0.0740231179361216));
#72134=CARTESIAN_POINT('Ctrl Pts',(0.00237255100794119,-0.0331450831799191,
0.0741882734210653));
#72135=CARTESIAN_POINT('Ctrl Pts',(0.00238578463554229,-0.0337436976235975,
0.0737573929708152));
#72136=CARTESIAN_POINT('Ctrl Pts',(0.00238225346842058,-0.0336723290703325,
0.0738090013904653));
#72137=CARTESIAN_POINT('Ctrl Pts',(0.0023796511453617,-0.033601104548885,
0.0738606649756556));
#72138=CARTESIAN_POINT('Ctrl Pts',(0.00237134244332586,-0.0333736987606856,
0.0740256165691887));
#72139=CARTESIAN_POINT('Ctrl Pts',(0.00237251330691316,-0.0331450831799191,
0.0741907731367756));
#72140=CARTESIAN_POINT('',(0.00238364203203872,-0.0336938721132548,0.0737909513524937));
#72141=CARTESIAN_POINT('',(0.00237373722885253,-0.0333679870047995,0.0740270857660023));
#72142=CARTESIAN_POINT('Ctrl Pts',(0.00238364203203947,-0.0336938721132476,
0.0737909513524793));
#72143=CARTESIAN_POINT('Ctrl Pts',(0.00238224049673511,-0.0336629187933822,
0.0738133578122843));
#72144=CARTESIAN_POINT('Ctrl Pts',(0.00238097060850649,-0.033631995230096,
0.0738357653125182));
#72145=CARTESIAN_POINT('Ctrl Pts',(0.00237983223236218,-0.0336011045488869,
0.07385817154278));
#72146=CARTESIAN_POINT('Ctrl Pts',(0.00237697565708572,-0.033523589259537,
0.0739143964414873));
#72147=CARTESIAN_POINT('Ctrl Pts',(0.00237494226013591,-0.033445866866549,
0.0739707132557272));
#72148=CARTESIAN_POINT('Ctrl Pts',(0.0023737372288467,-0.0333679869962413,
0.0740270857541789));
#72149=CARTESIAN_POINT('Ctrl Pts',(0.002373735591128,-0.0333679692470414,
0.0740271302038922));
#72150=CARTESIAN_POINT('Ctrl Pts',(0.00237418882798317,-0.033339189541522,
0.0740271339635706));
#72151=CARTESIAN_POINT('Ctrl Pts',(0.0023745285780814,-0.0333104081130171,
0.0740271335345558));
#72152=CARTESIAN_POINT('Ctrl Pts',(0.00237497828857451,-0.0332532698153858,
0.0740271274282393));
#72153=CARTESIAN_POINT('Ctrl Pts',(0.00237509160253743,-0.0332249170742957,
0.0740271218262043));
#72154=CARTESIAN_POINT('Ctrl Pts',(0.00237509541952204,-0.0331960985387042,
0.0740271150074511));
#72155=CARTESIAN_POINT('Ctrl Pts',(0.00237509545166307,-0.0331956312537763,
0.0740271148962221));
#72156=CARTESIAN_POINT('Ctrl Pts',(0.00237509545404053,-0.0331951640388589,
0.0740271147850021));
#72157=CARTESIAN_POINT('',(0.00237776687175779,-0.0331951640388587,0.0739021433341527));
#72158=CARTESIAN_POINT('',(0.00237643116290913,-0.0331951640388687,0.0739646290595873));
#72159=CARTESIAN_POINT('',(0.00239280147937305,-0.0335216366567733,0.073666279983748));
#72160=CARTESIAN_POINT('Origin',(0.0190461624799162,-0.032643457152522,
0.0738566281064757));
#72161=CARTESIAN_POINT('',(0.00239415520064963,-0.0336938721132326,0.073666394243946));
#72162=CARTESIAN_POINT('Origin',(-0.008487720796425,-0.0336938867896233,
0.0727479146722203));
#72163=CARTESIAN_POINT('',(0.00238889861635418,-0.0336938721132537,0.0737286727982298));
#72164=CARTESIAN_POINT('Ctrl Pts',(0.00216941526218682,-0.0335235895815171,
0.0734114104983307));
#72165=CARTESIAN_POINT('Ctrl Pts',(0.00215924712354743,-0.0334144449262748,
0.0734933840822045));
#72166=CARTESIAN_POINT('Ctrl Pts',(0.00215076081549949,-0.0333049234473147,
0.0735756619098868));
#72167=CARTESIAN_POINT('Ctrl Pts',(0.00214397671962867,-0.0331951640388587,
0.0736581397562617));
#72168=CARTESIAN_POINT('Ctrl Pts',(0.00224436428798135,-0.0335235895815171,
0.0734964035334477));
#72169=CARTESIAN_POINT('Ctrl Pts',(0.00223536624580623,-0.0334144449262748,
0.0735773452964204));
#72170=CARTESIAN_POINT('Ctrl Pts',(0.00222803006187835,-0.0333049234473147,
0.073658565944452));
#72171=CARTESIAN_POINT('Ctrl Pts',(0.00222237452467511,-0.0331951640388587,
0.0737399624710165));
#72172=CARTESIAN_POINT('Ctrl Pts',(0.00231931331377588,-0.0335235895815171,
0.0735813965685646));
#72173=CARTESIAN_POINT('Ctrl Pts',(0.00231148536806503,-0.0334144449262748,
0.0736613065106362));
#72174=CARTESIAN_POINT('Ctrl Pts',(0.00230529930825722,-0.0333049234473147,
0.0737414699790171));
#72175=CARTESIAN_POINT('Ctrl Pts',(0.00230077232972155,-0.0331951640388587,
0.0738217851857713));
#72176=CARTESIAN_POINT('Ctrl Pts',(0.00239426233957041,-0.0335235895815171,
0.0736663896036816));
#72177=CARTESIAN_POINT('Ctrl Pts',(0.00238760449032383,-0.0334144449262748,
0.0737452677248521));
#72178=CARTESIAN_POINT('Ctrl Pts',(0.00238256855463608,-0.0333049234473147,
0.0738243740135823));
#72179=CARTESIAN_POINT('Ctrl Pts',(0.00237917013476799,-0.0331951640388587,
0.0739036079005261));
#72180=CARTESIAN_POINT('',(0.00226087179570331,-0.0331951640388687,0.0737801415452172));
#72181=CARTESIAN_POINT('Ctrl Pts',(0.00214504098859704,-0.0332121607145974,
0.0736453679071492));
#72182=CARTESIAN_POINT('Ctrl Pts',(0.00218779964525095,-0.0332625444109927,
0.0736489769261144));
#72183=CARTESIAN_POINT('Ctrl Pts',(0.00222982150315124,-0.0333135300747189,
0.0736525237560192));
#72184=CARTESIAN_POINT('Ctrl Pts',(0.00231242497779767,-0.0334167203140631,
0.0736594958531316));
#72185=CARTESIAN_POINT('Ctrl Pts',(0.00235297460157892,-0.0334688847587333,
0.0736629184199919));
#72186=CARTESIAN_POINT('Ctrl Pts',(0.00239280148005874,-0.0335216366562418,
0.0736662799839652));
#72187=CARTESIAN_POINT('Ctrl Pts',(0.00238519125082585,-0.0336938721132474,
0.0737896432999643));
#72188=CARTESIAN_POINT('Ctrl Pts',(0.00238308196348132,-0.0336474569765,
0.0738232331770189));
#72189=CARTESIAN_POINT('Ctrl Pts',(0.00238136603258792,-0.033601104548885,
0.0738568454443452));
#72190=CARTESIAN_POINT('Ctrl Pts',(0.00237702169008348,-0.0334837508592655,
0.0739419439772629));
#72191=CARTESIAN_POINT('Ctrl Pts',(0.00237520090126284,-0.0333660264659097,
0.0740271338730523));
#72192=CARTESIAN_POINT('Ctrl Pts',(0.00238364203204049,-0.0336938721132474,
0.0737909513524672));
#72193=CARTESIAN_POINT('Ctrl Pts',(0.00238154040116131,-0.0336474569765,
0.0738245502976135));
#72194=CARTESIAN_POINT('Ctrl Pts',(0.00237983223236211,-0.033601104548885,
0.0738581715427814));
#72195=CARTESIAN_POINT('Ctrl Pts',(0.00237550754169554,-0.0334837508592655,
0.0739432928055301));
#72196=CARTESIAN_POINT('Ctrl Pts',(0.00237370706961516,-0.0333660264659097,
0.0740285048388446));
#72197=CARTESIAN_POINT('Ctrl Pts',(0.00212389092293176,-0.0336938721132474,
0.0740102671080028));
#72198=CARTESIAN_POINT('Ctrl Pts',(0.00212307301994653,-0.0336474569765,
0.0740453864625853));
#72199=CARTESIAN_POINT('Ctrl Pts',(0.00212266628939154,-0.033601104548885,
0.0740805129853544));
#72200=CARTESIAN_POINT('Ctrl Pts',(0.00212163654113961,-0.0334837508592655,
0.0741694452649036));
#72201=CARTESIAN_POINT('Ctrl Pts',(0.00212324249290732,-0.0333660264659097,
0.0742583690055255));
#72202=CARTESIAN_POINT('',(0.00212515255234191,-0.0336769361243753,0.0740217719495674));
#72203=CARTESIAN_POINT('',(0.00212544013436168,-0.0336938721132327,0.0740089590617211));
#72204=CARTESIAN_POINT('Ctrl Pts',(0.00212515255234192,-0.033676936124375,
0.0740217719495677));
#72205=CARTESIAN_POINT('Ctrl Pts',(0.00212519820538143,-0.033679758667006,
0.0740196362571424));
#72206=CARTESIAN_POINT('Ctrl Pts',(0.00212524499724999,-0.0336825812712915,
0.0740175006698712));
#72207=CARTESIAN_POINT('Ctrl Pts',(0.00212534085811385,-0.0336882266020684,
0.0740132297064027));
#72208=CARTESIAN_POINT('Ctrl Pts',(0.00212538992711016,-0.0336910493285604,
0.0740110943302047));
#72209=CARTESIAN_POINT('Ctrl Pts',(0.00212544013436201,-0.0336938721132326,
0.074008959061721));
#72210=CARTESIAN_POINT('Ctrl Pts',(0.00212515255234196,-0.0336769361243753,
0.0740217719495674));
#72211=CARTESIAN_POINT('Ctrl Pts',(0.00216705673264463,-0.0336279007536338,
0.0740226677027089));
#72212=CARTESIAN_POINT('Ctrl Pts',(0.00220955756321641,-0.0335767878672832,
0.0740235762099796));
#72213=CARTESIAN_POINT('Ctrl Pts',(0.00229284726020332,-0.0334733198899511,
0.0740253566291929));
#72214=CARTESIAN_POINT('Ctrl Pts',(0.0023336857126357,-0.0334209645035433,
0.0740262296010973));
#72215=CARTESIAN_POINT('Ctrl Pts',(0.00237373722915698,-0.0333679869844681,
0.0740270857512829));
#72216=CARTESIAN_POINT('',(0.0022545410832102,-0.0336938721132538,0.0738999552071174));
#72217=CARTESIAN_POINT('Origin',(0.00812378219310841,-0.0315241814719618,
0.07415));
#72218=CARTESIAN_POINT('',(0.00212515255364349,-0.0337108120655397,0.0740217719496001));
#72219=CARTESIAN_POINT('',(0.00212489233953393,-0.0336938721132327,0.074034585422462));
#72220=CARTESIAN_POINT('Origin',(0.0184587460170713,-0.0345562512088088,
0.0754887825082202));
#72221=CARTESIAN_POINT('Ctrl Pts',(0.00212489233954153,-0.0336938721132294,
0.0740345854224665));
#72222=CARTESIAN_POINT('Ctrl Pts',(0.00212493342423983,-0.0336910493404263,
0.0740324499679598));
#72223=CARTESIAN_POINT('Ctrl Pts',(0.00212497565100609,-0.0336882266080013,
0.0740303144410065));
#72224=CARTESIAN_POINT('Ctrl Pts',(0.00212506238854535,-0.0336825812712813,
0.0740260432780174));
#72225=CARTESIAN_POINT('Ctrl Pts',(0.0021251068993025,-0.0336797586670009,
0.0740239076419885));
#72226=CARTESIAN_POINT('Ctrl Pts',(0.00212515255234193,-0.033676936124375,
0.0740217719495671));
#72227=CARTESIAN_POINT('Origin',(0.0185065124361043,-0.0345562516912807,
0.0732540829213579));
#72228=CARTESIAN_POINT('Ctrl Pts',(0.00237943962316015,-0.034243627687391,
0.073866004508697));
#72229=CARTESIAN_POINT('Ctrl Pts',(0.00236872855663149,-0.0339430054201809,
0.074082655960267));
#72230=CARTESIAN_POINT('Ctrl Pts',(0.00237436699415386,-0.0336441434784051,
0.074299498729194));
#72231=CARTESIAN_POINT('Ctrl Pts',(0.00237252469634862,-0.034243627687391,
0.0741159088579732));
#72232=CARTESIAN_POINT('Ctrl Pts',(0.00237123892773092,-0.0339430054201809,
0.0743328211103074));
#72233=CARTESIAN_POINT('Ctrl Pts',(0.00238629553146314,-0.0336441434784051,
0.0745492139870331));
#72234=CARTESIAN_POINT('Ctrl Pts',(0.00237245554708051,-0.034243627687391,
0.0741184079014659));
#72235=CARTESIAN_POINT('Ctrl Pts',(0.00237126403144192,-0.0339430054201809,
0.0743353227618078));
#72236=CARTESIAN_POINT('Ctrl Pts',(0.00238641481683623,-0.0336441434784051,
0.0745517111396116));
#72237=CARTESIAN_POINT('',(0.00237242403632307,-0.0341934961088741,0.0741520862358514));
#72238=CARTESIAN_POINT('',(0.0023773657793568,-0.0338664212891033,0.0743883766089048));
#72239=CARTESIAN_POINT('Origin',(0.0190996333364463,-0.0345610818075015,
0.0746556369668814));
#72240=CARTESIAN_POINT('Origin',(-0.00857946260158768,-0.0336938005044531,
0.0748429706856536));
#72241=CARTESIAN_POINT('',(0.00237354227162478,-0.0336938721132327,0.0742634277099163));
#72242=CARTESIAN_POINT('',(0.00237613270965501,-0.0336938721132426,0.0743258740038986));
#72243=CARTESIAN_POINT('',(0.00237373722915707,-0.0340203938281605,0.0740270857512775));
#72244=CARTESIAN_POINT('Origin',(0.0190111828180154,-0.0345589643243929,
0.0751286064196521));
#72245=CARTESIAN_POINT('',(0.00237509545404047,-0.0341934961088739,0.074027114785002));
#72246=CARTESIAN_POINT('Origin',(-0.00864183503513343,-0.0341934220717644,
0.0737916134911796));
#72247=CARTESIAN_POINT('',(0.00237375974519177,-0.034193496108884,0.0740896005104367));
#72248=CARTESIAN_POINT('Ctrl Pts',(0.00213478859230788,-0.0340223579322396,
0.0737867429978597));
#72249=CARTESIAN_POINT('Ctrl Pts',(0.00212977833083434,-0.0339125849573575,
0.0738693468395658));
#72250=CARTESIAN_POINT('Ctrl Pts',(0.00212648129759202,-0.0338030433565231,
0.073951996337279));
#72251=CARTESIAN_POINT('Ctrl Pts',(0.0021248923395334,-0.0336938721132327,
0.0740345854224616));
#72252=CARTESIAN_POINT('Ctrl Pts',(0.00221492646653166,-0.0340223579322397,
0.0738668622898264));
#72253=CARTESIAN_POINT('Ctrl Pts',(0.00221102125905422,-0.0339125849573575,
0.0739483608212386));
#72254=CARTESIAN_POINT('Ctrl Pts',(0.00220880562594467,-0.0338030433565231,
0.0740298829132967));
#72255=CARTESIAN_POINT('Ctrl Pts',(0.00220827315903309,-0.0336938721132327,
0.0741113240618156));
#72256=CARTESIAN_POINT('Ctrl Pts',(0.00229506434075544,-0.0340223579322397,
0.0739469815817931));
#72257=CARTESIAN_POINT('Ctrl Pts',(0.00229226418727411,-0.0339125849573575,
0.0740273748029114));
#72258=CARTESIAN_POINT('Ctrl Pts',(0.00229112995429731,-0.0338030433565231,
0.0741077694893144));
#72259=CARTESIAN_POINT('Ctrl Pts',(0.00229165397853278,-0.0336938721132327,
0.0741880627011696));
#72260=CARTESIAN_POINT('Ctrl Pts',(0.00237520221497922,-0.0340223579322397,
0.0740271008737598));
#72261=CARTESIAN_POINT('Ctrl Pts',(0.00237350711549399,-0.0339125849573575,
0.0741063887845841));
#72262=CARTESIAN_POINT('Ctrl Pts',(0.00237345428264996,-0.0338030433565231,
0.0741856560653321));
#72263=CARTESIAN_POINT('Ctrl Pts',(0.00237503479803247,-0.0336938721132327,
0.0742648013405236));
#72264=CARTESIAN_POINT('',(0.00224921730558935,-0.0336938721132427,0.0741490065661992));
#72265=CARTESIAN_POINT('Ctrl Pts',(0.00212515255724037,-0.0337108120662684,
0.074021771949672));
#72266=CARTESIAN_POINT('Ctrl Pts',(0.00216814199267721,-0.0337611408994435,
0.0740226909014702));
#72267=CARTESIAN_POINT('Ctrl Pts',(0.0022103469662926,-0.0338121088781604,
0.0740235930844369));
#72268=CARTESIAN_POINT('Ctrl Pts',(0.00229322643789414,-0.0339153382773233,
0.0740253647345805));
#72269=CARTESIAN_POINT('Ctrl Pts',(0.00233386587282454,-0.0339675558473115,
0.0740262334522417));
#72270=CARTESIAN_POINT('Ctrl Pts',(0.0023737372291968,-0.0340203938281304,
0.0740270857512837));
#72271=CARTESIAN_POINT('Ctrl Pts',(0.00237388847297717,-0.0341934961088741,
0.0741506830971307));
#72272=CARTESIAN_POINT('Ctrl Pts',(0.00237390259547209,-0.03402875161944,
0.074269557619096));
#72273=CARTESIAN_POINT('Ctrl Pts',(0.0023788298800418,-0.0338644633299819,
0.074388329981364));
#72274=CARTESIAN_POINT('Ctrl Pts',(0.00237242403632317,-0.0341934961088741,
0.0741520862358513));
#72275=CARTESIAN_POINT('Ctrl Pts',(0.00237246716760552,-0.03402875161944,
0.0742709910338906));
#72276=CARTESIAN_POINT('Ctrl Pts',(0.0023774246875083,-0.0338644633299819,
0.074389792447407));
#72277=CARTESIAN_POINT('Ctrl Pts',(0.00212842045843375,-0.0341934961088741,
0.0743858763879789));
#72278=CARTESIAN_POINT('Ctrl Pts',(0.00213329701689356,-0.03402875161944,
0.0745098257677254));
#72279=CARTESIAN_POINT('Ctrl Pts',(0.00214329233029034,-0.0338644633299819,
0.0746334676832399));
#72280=CARTESIAN_POINT('',(0.00212893797252645,-0.0341764758832388,0.0743986820490732));
#72281=CARTESIAN_POINT('',(0.00212842045843431,-0.034193496108874,0.0743858763879783));
#72282=CARTESIAN_POINT('Origin',(0.0186936848809415,-0.034562102674501,
0.0742240717872174));
#72283=CARTESIAN_POINT('Ctrl Pts',(0.00212893797332019,-0.0341764758837474,
0.0743986820474324));
#72284=CARTESIAN_POINT('Ctrl Pts',(0.00217182546541595,-0.0341260050043394,
0.0743969029466841));
#72285=CARTESIAN_POINT('Ctrl Pts',(0.00221396747014351,-0.0340749269154166,
0.0743951547327292));
#72286=CARTESIAN_POINT('Ctrl Pts',(0.00229679317293366,-0.0339715436318644,
0.074391718906788));
#72287=CARTESIAN_POINT('Ctrl Pts',(0.00233744544902731,-0.033919277825295,
0.0743900326042564));
#72288=CARTESIAN_POINT('Ctrl Pts',(0.00237736577692892,-0.0338664212873869,
0.0743883766051632));
#72289=CARTESIAN_POINT('',(0.00225042224738869,-0.0341934961088841,0.0742689813119249));
#72290=CARTESIAN_POINT('Origin',(0.00812378219310841,-0.0315241814719618,
0.07415));
#72291=CARTESIAN_POINT('',(0.00212893797329664,-0.0342105180190537,0.0743986820498836));
#72292=CARTESIAN_POINT('',(0.00212948283705898,-0.0341934961088739,0.0744114865772719));
#72293=CARTESIAN_POINT('Origin',(0.0186970490369613,-0.034562170373609,
0.0741788690574407));
#72294=CARTESIAN_POINT('Origin',(0.0186512375102797,-0.0345621039704051,
0.0732007520833079));
#72295=CARTESIAN_POINT('Origin',(0.0186583280135043,-0.0345621716132366,
0.0732455212001824));
#72296=CARTESIAN_POINT('Ctrl Pts',(0.00237348010070173,-0.0346945769586966,
0.0742619289889591));
#72297=CARTESIAN_POINT('Ctrl Pts',(0.0023758244981894,-0.0345275153362944,
0.0743823713685799));
#72298=CARTESIAN_POINT('Ctrl Pts',(0.00238195730403783,-0.0343603235965185,
0.0745027711716261));
#72299=CARTESIAN_POINT('Ctrl Pts',(0.00239185508771714,-0.034193496108874,
0.0746227725785056));
#72300=CARTESIAN_POINT('Ctrl Pts',(0.00237695474171148,-0.0346945769586966,
0.0743456902881114));
#72301=CARTESIAN_POINT('Ctrl Pts',(0.00238105355314609,-0.0345275153362944,
0.0744660598899851));
#72302=CARTESIAN_POINT('Ctrl Pts',(0.0023889389379296,-0.0343603235965185,
0.0745863317217564));
#72303=CARTESIAN_POINT('Ctrl Pts',(0.00240058228780687,-0.034193496108874,
0.0747061504193534));
#72304=CARTESIAN_POINT('Ctrl Pts',(0.00238042938272128,-0.0346945769586966,
0.074429451587263));
#72305=CARTESIAN_POINT('Ctrl Pts',(0.00238628260810281,-0.0345275153362944,
0.0745497484113905));
#72306=CARTESIAN_POINT('Ctrl Pts',(0.0023959205718214,-0.0343603235965185,
0.0746698922718872));
#72307=CARTESIAN_POINT('Ctrl Pts',(0.00240930948789662,-0.034193496108874,
0.0747895282602017));
#72308=CARTESIAN_POINT('Ctrl Pts',(0.00238390402373097,-0.0346945769586966,
0.0745132128864162));
#72309=CARTESIAN_POINT('Ctrl Pts',(0.00239151166305946,-0.0345275153362944,
0.0746334369327957));
#72310=CARTESIAN_POINT('Ctrl Pts',(0.00240290220571316,-0.0343603235965185,
0.074753452822017));
#72311=CARTESIAN_POINT('Ctrl Pts',(0.00241803668798633,-0.034193496108874,
0.0748729061010489));
#72312=CARTESIAN_POINT('',(0.00238390402370603,-0.0346945769586966,0.0745132128858109));
#72313=CARTESIAN_POINT('',(0.00240367281090493,-0.0343667727831449,0.074748726695533));
#72314=CARTESIAN_POINT('Origin',(0.0191513968172488,-0.0345626457061575,
0.0732688525457317));
#72315=CARTESIAN_POINT('Origin',(-0.00858845504753611,-0.0341934771029168,
0.0758992828933265));
#72316=CARTESIAN_POINT('',(0.00239201124142713,-0.034193496108874,0.074624264438329));
#72317=CARTESIAN_POINT('',(0.00239851760306086,-0.0341934961088839,0.0746864248538655));
#72318=CARTESIAN_POINT('',(0.00237736577990387,-0.0345211942962703,0.0743883766050832));
#72319=CARTESIAN_POINT('Origin',(0.0191680034977935,-0.0345625596118732,
0.0737493887132169));
#72320=CARTESIAN_POINT('',(0.00237872314766526,-0.0346945769586885,0.0743883202978607));
#72321=CARTESIAN_POINT('Origin',(-0.00867533702907217,-0.0346945685853894,
0.0748468710747448));
#72322=CARTESIAN_POINT('',(0.00238131358569564,-0.0346945769587026,0.0744507665918459));
#72323=CARTESIAN_POINT('Ctrl Pts',(0.00212379740940387,-0.0345231616327842,
0.0741635127844013));
#72324=CARTESIAN_POINT('Ctrl Pts',(0.00212398366411236,-0.0344132092796988,
0.0742462141273418));
#72325=CARTESIAN_POINT('Ctrl Pts',(0.00212588052125579,-0.0343032738558979,
0.0743289073507414));
#72326=CARTESIAN_POINT('Ctrl Pts',(0.00212948283705895,-0.0341934961088739,
0.0744114865772719));
#72327=CARTESIAN_POINT('Ctrl Pts',(0.00220880774919815,-0.0345231616327842,
0.0742384419393851));
#72328=CARTESIAN_POINT('Ctrl Pts',(0.00221002679681628,-0.0344132092796988,
0.0743199715344765));
#72329=CARTESIAN_POINT('Ctrl Pts',(0.00221293215690198,-0.0343032738558979,
0.0744014717079772));
#72330=CARTESIAN_POINT('Ctrl Pts',(0.00221751743282267,-0.0341934961088739,
0.0744828381440889));
#72331=CARTESIAN_POINT('Ctrl Pts',(0.00229381808899242,-0.0345231616327842,
0.0743133710943689));
#72332=CARTESIAN_POINT('Ctrl Pts',(0.00229606992952019,-0.0344132092796988,
0.0743937289416112));
#72333=CARTESIAN_POINT('Ctrl Pts',(0.00229998379254817,-0.0343032738558979,
0.0744740360652129));
#72334=CARTESIAN_POINT('Ctrl Pts',(0.00230555202858638,-0.0341934961088739,
0.074554189710906));
#72335=CARTESIAN_POINT('Ctrl Pts',(0.00237882842878669,-0.0345231616327842,
0.0743883002493527));
#72336=CARTESIAN_POINT('Ctrl Pts',(0.00238211306222411,-0.0344132092796988,
0.0744674863487459));
#72337=CARTESIAN_POINT('Ctrl Pts',(0.00238703542819436,-0.0343032738558979,
0.0745466004224487));
#72338=CARTESIAN_POINT('Ctrl Pts',(0.00239358662435009,-0.0341934961088739,
0.074625541277723));
#72339=CARTESIAN_POINT('',(0.00226074703925305,-0.0341934961088839,0.0745178755078104));
#72340=CARTESIAN_POINT('Ctrl Pts',(0.00212893797674334,-0.0342105180195387,
0.0743986820497355));
#72341=CARTESIAN_POINT('Ctrl Pts',(0.00217187368354173,-0.0342610556241366,
0.0743969009626567));
#72342=CARTESIAN_POINT('Ctrl Pts',(0.00221403893128144,-0.0343122189870292,
0.0743951518362646));
#72343=CARTESIAN_POINT('Ctrl Pts',(0.00229686546984916,-0.0344158119695183,
0.0743917159716049));
#72344=CARTESIAN_POINT('Ctrl Pts',(0.00233749288403387,-0.0344681990450091,
0.0743900306386304));
#72345=CARTESIAN_POINT('Ctrl Pts',(0.00237736577992857,-0.0345211942962515,
0.0743883766050772));
#72346=CARTESIAN_POINT('Ctrl Pts',(0.00238527713202041,-0.0346945769586933,
0.0745117209268942));
#72347=CARTESIAN_POINT('Ctrl Pts',(0.00239275545623842,-0.034529677707698,
0.0746303604585962));
#72348=CARTESIAN_POINT('Ctrl Pts',(0.00240513087118744,-0.0343648066251421,
0.074748589528289));
#72349=CARTESIAN_POINT('Ctrl Pts',(0.00238390402370555,-0.0346945769586933,
0.0745132128858019));
#72350=CARTESIAN_POINT('Ctrl Pts',(0.00239141319311831,-0.034529677707698,
0.0746318808055468));
#72351=CARTESIAN_POINT('Ctrl Pts',(0.00240382060020912,-0.0343648066251421,
0.074750136964165));
#72352=CARTESIAN_POINT('Ctrl Pts',(0.00215506173625195,-0.0346945769586933,
0.0747618628178917));
#72353=CARTESIAN_POINT('Ctrl Pts',(0.00216771156707162,-0.034529677707698,
0.0748852618900061));
#72354=CARTESIAN_POINT('Ctrl Pts',(0.00218545078581339,-0.0343648066251421,
0.0750080326900234));
#72355=CARTESIAN_POINT('',(0.00215638230304205,-0.0346775396664975,0.0747746107150898));
#72356=CARTESIAN_POINT('',(0.00215506173625342,-0.0346945769586887,0.0747618628178938));
#72357=CARTESIAN_POINT('Origin',(0.0186511766211248,-0.0345626618038484,
0.0728945410564125));
#72358=CARTESIAN_POINT('Ctrl Pts',(0.00215638230382469,-0.0346775396670097,
0.0747746107134425));
#72359=CARTESIAN_POINT('Ctrl Pts',(0.00219910707997535,-0.0346269749928188,
0.0747701386769084));
#72360=CARTESIAN_POINT('Ctrl Pts',(0.00224107253777998,-0.0345757902890782,
0.0747657460827174));
#72361=CARTESIAN_POINT('Ctrl Pts',(0.0023235193956571,-0.0344721681088003,
0.0747571163328799));
#72362=CARTESIAN_POINT('Ctrl Pts',(0.00236396847327309,-0.0344197714289742,
0.0747528825661073));
#72363=CARTESIAN_POINT('Ctrl Pts',(0.00240367281076893,-0.0343667727830615,
0.0747487266952973));
#72364=CARTESIAN_POINT('',(0.00226948287998973,-0.0346945769587026,0.0746375378518624));
#72365=CARTESIAN_POINT('Origin',(0.00812378219310841,-0.0315241814719618,
0.07415));
#72366=CARTESIAN_POINT('',(0.00215638230429078,-0.0347116136489792,0.0747746107157019));
#72367=CARTESIAN_POINT('',(0.00215773009560744,-0.0346945769586885,0.074787355764023));
#72368=CARTESIAN_POINT('Origin',(0.018644606527977,-0.0345626681934436,
0.0728497064115708));
#72369=CARTESIAN_POINT('Origin',(0.0186829756296675,-0.0345626630859793,
0.0731983135855367));
#72370=CARTESIAN_POINT('Origin',(0.0186858261559396,-0.0345626693552011,
0.0732435377202918));
#72371=CARTESIAN_POINT('Ctrl Pts',(0.00238890029881963,-0.0352450361874068,
0.0745857663183217));
#72372=CARTESIAN_POINT('Ctrl Pts',(0.00240533549520417,-0.0349452760959493,
0.0748020609381946));
#72373=CARTESIAN_POINT('Ctrl Pts',(0.00243801619670002,-0.0346444289841739,
0.0750165031215818));
#72374=CARTESIAN_POINT('Ctrl Pts',(0.0023891473884064,-0.0352450361874068,
0.074588279199484));
#72375=CARTESIAN_POINT('Ctrl Pts',(0.00240567735965917,-0.0349452760959493,
0.0748045645002203));
#72376=CARTESIAN_POINT('Ctrl Pts',(0.00243845186482231,-0.0346444289841739,
0.0750189902521146));
#72377=CARTESIAN_POINT('Ctrl Pts',(0.00241361170392928,-0.0352450361874068,
0.0748370793145684));
#72378=CARTESIAN_POINT('Ctrl Pts',(0.00243952532550101,-0.0349452760959493,
0.075052441928504));
#72379=CARTESIAN_POINT('Ctrl Pts',(0.00248158732247518,-0.0346444289841739,
0.0752652407999173));
#72380=CARTESIAN_POINT('Ctrl Pts',(0.00241385634708451,-0.0352450361874068,
0.0748395673157192));
#72381=CARTESIAN_POINT('Ctrl Pts',(0.00243986380515942,-0.0349452760959493,
0.075054920702787));
#72382=CARTESIAN_POINT('Ctrl Pts',(0.00248201867705171,-0.0346444289841739,
0.0752677033053952));
#72383=CARTESIAN_POINT('',(0.00241803026600223,-0.0351951634053262,0.0748728742967211));
#72384=CARTESIAN_POINT('',(0.00245255450039629,-0.0348678972925388,0.0751067138848245));
#72385=CARTESIAN_POINT('Origin',(0.0188981264262113,-0.0345636767886491,
0.0719045537410315));
#72386=CARTESIAN_POINT('Origin',(-0.0084433345167475,-0.0346946199341098,
0.076944808478318));
#72387=CARTESIAN_POINT('',(0.00243310089014555,-0.0346945769330288,0.0749832294438517));
#72388=CARTESIAN_POINT('',(0.00244349749883294,-0.0346945769458128,0.07504485867081));
#72389=CARTESIAN_POINT('',(0.00240367281090796,-0.0350221583435275,0.0747487266952989));
#72390=CARTESIAN_POINT('Origin',(0.0190187088434312,-0.0345628458713957,
0.0723699603085454));
#72391=CARTESIAN_POINT('',(0.00240490266024603,-0.035195136029876,0.0747485949252347));
#72392=CARTESIAN_POINT('Origin',(-0.00855420375129167,-0.0351951838366786,
0.0758956914862782));
#72393=CARTESIAN_POINT('',(0.00241803668780661,-0.035195137132875,0.0748729061004478));
#72394=CARTESIAN_POINT('Ctrl Pts',(0.00213648554604413,-0.0350241211494342,
0.0745402292404247));
#72395=CARTESIAN_POINT('Ctrl Pts',(0.00214186079383076,-0.0349144232818961,
0.0746227017968508));
#72396=CARTESIAN_POINT('Ctrl Pts',(0.00214894402563534,-0.0348045283579411,
0.0747051126068645));
#72397=CARTESIAN_POINT('Ctrl Pts',(0.00215773009678787,-0.0346945769439157,
0.074787355775073));
#72398=CARTESIAN_POINT('Ctrl Pts',(0.0022260330087906,-0.0350241211494342,
0.0746096726974142));
#72399=CARTESIAN_POINT('Ctrl Pts',(0.00223236481172434,-0.0349144232818961,
0.0746909117742568));
#72400=CARTESIAN_POINT('Ctrl Pts',(0.002240379674316,-0.0348045283579411,
0.0747720685937117));
#72401=CARTESIAN_POINT('Ctrl Pts',(0.0022500711988244,-0.0346945769439157,
0.074853038822183));
#72402=CARTESIAN_POINT('Ctrl Pts',(0.00231558047153708,-0.0350241211494342,
0.0746791161544036));
#72403=CARTESIAN_POINT('Ctrl Pts',(0.00232286882961792,-0.0349144232818961,
0.0747591217516629));
#72404=CARTESIAN_POINT('Ctrl Pts',(0.00233181532299665,-0.0348045283579411,
0.0748390245805589));
#72405=CARTESIAN_POINT('Ctrl Pts',(0.00234241230086092,-0.0346945769439157,
0.074918721869293));
#72406=CARTESIAN_POINT('Ctrl Pts',(0.00240512793428355,-0.0350241211494342,
0.0747485596113931));
#72407=CARTESIAN_POINT('Ctrl Pts',(0.00241337284751149,-0.0349144232818961,
0.0748273317290688));
#72408=CARTESIAN_POINT('Ctrl Pts',(0.00242325097167731,-0.0348045283579411,
0.074905980567406));
#72409=CARTESIAN_POINT('Ctrl Pts',(0.00243475340289745,-0.0346945769439157,
0.074984404916403));
#72410=CARTESIAN_POINT('',(0.00229541549275694,-0.0346945769458128,0.0748852926036652));
#72411=CARTESIAN_POINT('Ctrl Pts',(0.00215638230755627,-0.034711613649279,
0.0747746107153548));
#72412=CARTESIAN_POINT('Ctrl Pts',(0.00219909011810518,-0.0347621546532347,
0.0747701404675735));
#72413=CARTESIAN_POINT('Ctrl Pts',(0.00224104700993601,-0.0348133084097138,
0.0747657488188281));
#72414=CARTESIAN_POINT('Ctrl Pts',(0.00232349397203097,-0.0349168561544564,
0.0747571190542807));
#72415=CARTESIAN_POINT('Ctrl Pts',(0.00236395133978478,-0.034969208901592,
0.0747528843614666));
#72416=CARTESIAN_POINT('Ctrl Pts',(0.00240367281094638,-0.0350221583434999,
0.074748726695315));
#72417=CARTESIAN_POINT('Ctrl Pts',(0.00241895788224886,-0.0351951371254872,
0.0748717695175402));
#72418=CARTESIAN_POINT('Ctrl Pts',(0.00243388001417029,-0.035030733898092,
0.0749897131808378));
#72419=CARTESIAN_POINT('Ctrl Pts',(0.00245366413408612,-0.0348659306897825,
0.0751069393141541));
#72420=CARTESIAN_POINT('Ctrl Pts',(0.00241803668792182,-0.0351951371254872,
0.0748729061004327));
#72421=CARTESIAN_POINT('Ctrl Pts',(0.00243298231798144,-0.035030733898092,
0.0749908688088451));
#72422=CARTESIAN_POINT('Ctrl Pts',(0.00245279070311158,-0.0348659306897825,
0.0751081129997988));
#72423=CARTESIAN_POINT('Ctrl Pts',(0.00226364355862915,-0.0351951371254872,
0.0750633985777853));
#72424=CARTESIAN_POINT('Ctrl Pts',(0.00228252750113895,-0.035030733898092,
0.0751845532672762));
#72425=CARTESIAN_POINT('Ctrl Pts',(0.00230640276147664,-0.0348659306897825,
0.0753048239370764));
#72426=CARTESIAN_POINT('Origin',(-0.00279153162246081,-0.0308609197411044,
0.0759913706608974));
#72427=CARTESIAN_POINT('',(0.0023507247646528,-0.0351951371254872,0.0749559565255237));
#72428=CARTESIAN_POINT('Origin',(0.00905356251905436,-0.0351840467441192,
0.0738495766405217));
#72429=CARTESIAN_POINT('Origin',(-0.00351662015186023,-0.0352322614047276,
0.0769196211525918));
#72430=CARTESIAN_POINT('',(0.00249674051053438,-0.0351951142564656,0.0753392083442391));
#72431=CARTESIAN_POINT('',(0.00252514072129866,-0.0351951372916786,0.0754606157599132));
#72432=CARTESIAN_POINT('Origin',(0.00836370110251291,-0.035287511944211,
0.0743917270355528));
#72433=CARTESIAN_POINT('Origin',(0.00784399112240425,-0.0298325076522344,
0.0666522065087368));
#72434=CARTESIAN_POINT('Origin',(-0.000155814137235747,-0.0338733336719971,
0.0728482042036773));
#72435=CARTESIAN_POINT('Ctrl Pts',(0.00287253105406548,-0.0321934096636942,
0.0718042597714128));
#72436=CARTESIAN_POINT('Ctrl Pts',(0.00283054342099563,-0.0320508460843093,
0.0718982546661998));
#72437=CARTESIAN_POINT('Ctrl Pts',(0.00279111290409766,-0.0319086045660614,
0.071993306813379));
#72438=CARTESIAN_POINT('Ctrl Pts',(0.00275430755500245,-0.0317669892864229,
0.0720892045593931));
#72439=CARTESIAN_POINT('Ctrl Pts',(0.00284000561464614,-0.0321934096636942,
0.0718815419065962));
#72440=CARTESIAN_POINT('Ctrl Pts',(0.00279940129499496,-0.0320508460843093,
0.0719761189912605));
#72441=CARTESIAN_POINT('Ctrl Pts',(0.00276136869078604,-0.0319086045660614,
0.0720717157224417));
#72442=CARTESIAN_POINT('Ctrl Pts',(0.00272597274716384,-0.0317669892864229,
0.0721681195217954));
#72443=CARTESIAN_POINT('Ctrl Pts',(0.00280748017522678,-0.0321934096636942,
0.0719588240417795));
#72444=CARTESIAN_POINT('Ctrl Pts',(0.00276825916899429,-0.0320508460843093,
0.072053983316321));
#72445=CARTESIAN_POINT('Ctrl Pts',(0.00273162447747442,-0.0319086045660614,
0.0721501246315045));
#72446=CARTESIAN_POINT('Ctrl Pts',(0.00269763793932524,-0.0317669892864229,
0.0722470344841978));
#72447=CARTESIAN_POINT('Ctrl Pts',(0.00277495473580743,-0.0321934096636942,
0.0720361061769628));
#72448=CARTESIAN_POINT('Ctrl Pts',(0.00273711704299362,-0.0320508460843093,
0.0721318476413816));
#72449=CARTESIAN_POINT('Ctrl Pts',(0.0027018802641628,-0.0319086045660614,
0.0722285335405672));
#72450=CARTESIAN_POINT('Ctrl Pts',(0.00266930313148663,-0.0317669892864229,
0.0723259494466002));
#72451=CARTESIAN_POINT('',(0.00277553662234814,-0.0321934096636942,0.0720347235842935));
#72452=CARTESIAN_POINT('',(0.00269314705375743,-0.0318665617511262,0.0722562399908496));
#72453=CARTESIAN_POINT('Origin',(0.0180774672077036,-0.0326371944420532,
0.0787480554851963));
#72454=CARTESIAN_POINT('Origin',(-0.00765679016673187,-0.0316939261509361,
0.0686470309856634));
#72455=CARTESIAN_POINT('',(0.00282271380938108,-0.0320197221621828,0.0719192460562448));
#72456=CARTESIAN_POINT('Ctrl Pts',(0.00282260094872311,-0.0320197392094742,
0.0719193926077748));
#72457=CARTESIAN_POINT('Ctrl Pts',(0.00281125094445531,-0.0319792716576039,
0.0719463667404374));
#72458=CARTESIAN_POINT('Ctrl Pts',(0.00280005491057772,-0.0319386439829676,
0.0719735501974854));
#72459=CARTESIAN_POINT('Ctrl Pts',(0.00278900891356809,-0.0318979099381608,
0.0720009747373043));
#72460=CARTESIAN_POINT('Ctrl Pts',(0.00277796313489029,-0.0318571766984908,
0.072028398735058));
#72461=CARTESIAN_POINT('Ctrl Pts',(0.00276712187634602,-0.0318163871833554,
0.0720559237537243));
#72462=CARTESIAN_POINT('Ctrl Pts',(0.00275651915120915,-0.0317755399638303,
0.072083453828186));
#72463=CARTESIAN_POINT('',(0.00282402550318807,-0.0321934096636183,0.071919511482288));
#72464=CARTESIAN_POINT('Origin',(0.000689099354915879,-0.0324111540182647,
0.0710438044112699));
#72465=CARTESIAN_POINT('',(0.00279978106277811,-0.0321934096636662,0.0719771175333007));
#72466=CARTESIAN_POINT('Ctrl Pts',(0.00277741482267836,-0.0321934096636618,
0.0720339580446808));
#72467=CARTESIAN_POINT('Ctrl Pts',(0.00274823295496786,-0.0320835708272592,
0.0721076886174341));
#72468=CARTESIAN_POINT('Ctrl Pts',(0.00272059386429774,-0.0319739230346489,
0.0721819803406944));
#72469=CARTESIAN_POINT('Ctrl Pts',(0.00269452561806012,-0.0318646057455573,
0.0722567354493983));
#72470=CARTESIAN_POINT('Ctrl Pts',(0.0026724778611228,-0.0321934096636618,
0.0720767295172299));
#72471=CARTESIAN_POINT('Ctrl Pts',(0.00264388584535289,-0.0320835708272592,
0.072151907252466));
#72472=CARTESIAN_POINT('Ctrl Pts',(0.00261686621343762,-0.0319739230346489,
0.072227633091841));
#72473=CARTESIAN_POINT('Ctrl Pts',(0.00259144609939487,-0.0318646057455573,
0.0723038074962655));
#72474=CARTESIAN_POINT('Ctrl Pts',(0.00256754089956724,-0.0321934096636618,
0.0721195009897789));
#72475=CARTESIAN_POINT('Ctrl Pts',(0.00253953873573791,-0.0320835708272592,
0.072196125887498));
#72476=CARTESIAN_POINT('Ctrl Pts',(0.00251313856257751,-0.0319739230346489,
0.0722732858429875));
#72477=CARTESIAN_POINT('Ctrl Pts',(0.00248836658072962,-0.0318646057455573,
0.0723508795431327));
#72478=CARTESIAN_POINT('Ctrl Pts',(0.00246260393801168,-0.0321934096636618,
0.0721622724623279));
#72479=CARTESIAN_POINT('Ctrl Pts',(0.00243519162612294,-0.0320835708272592,
0.07224034452253));
#72480=CARTESIAN_POINT('Ctrl Pts',(0.0024094109117174,-0.0319739230346489,
0.0723189385941341));
#72481=CARTESIAN_POINT('Ctrl Pts',(0.00238528706206437,-0.0318646057455573,
0.0723979515899999));
#72482=CARTESIAN_POINT('',(0.00245837103291331,-0.0321763980308256,0.0721743693757221));
#72483=CARTESIAN_POINT('',(0.00246260393800085,-0.0321934096636184,0.0721622724623588));
#72484=CARTESIAN_POINT('Origin',(0.0178705323178745,-0.0326386231243202,
0.0781986017914123));
#72485=CARTESIAN_POINT('Ctrl Pts',(0.00245837103590465,-0.0321763980306268,
0.0721743693767623));
#72486=CARTESIAN_POINT('Ctrl Pts',(0.0024988965654995,-0.0321259596175073,
0.0721885013567844));
#72487=CARTESIAN_POINT('Ctrl Pts',(0.00253871993771195,-0.0320749164631912,
0.072202388481909));
#72488=CARTESIAN_POINT('Ctrl Pts',(0.00261699441599857,-0.0319716057793887,
0.0722296841983239));
#72489=CARTESIAN_POINT('Ctrl Pts',(0.0026554150236457,-0.0319193786690081,
0.0722430821542649));
#72490=CARTESIAN_POINT('Ctrl Pts',(0.00269314705550645,-0.0318665617525265,
0.072256239991455));
#72491=CARTESIAN_POINT('',(0.0026190702801845,-0.0321934096636663,0.0720984980233362));
#72492=CARTESIAN_POINT('Origin',(0.00812378219310841,-0.0315241814719618,
0.07415));
#72493=CARTESIAN_POINT('',(0.00245837103256181,-0.0322104233323781,0.0721743693755995));
#72494=CARTESIAN_POINT('',(0.00245416397318719,-0.0321934096636183,0.0721864753018188));
#72495=CARTESIAN_POINT('Origin',(0.017891280271871,-0.0326387229794279,
0.0781582931490726));
#72496=CARTESIAN_POINT('Origin',(0.0182745539159592,-0.0326386246414647,
0.0770400193105253));
#72497=CARTESIAN_POINT('Origin',(0.0182657321622171,-0.0326387241409828,
0.0770844873325173));
#72498=CARTESIAN_POINT('Ctrl Pts',(0.00274833537119431,-0.0327445246967096,
0.072104835834273));
#72499=CARTESIAN_POINT('Ctrl Pts',(0.00267120074370361,-0.032443687833936,
0.0723075741254835));
#72500=CARTESIAN_POINT('Ctrl Pts',(0.00260955632423863,-0.0321434074405927,
0.0725155465540164));
#72501=CARTESIAN_POINT('Ctrl Pts',(0.00266453555560477,-0.0327445246967096,
0.0723403726486082));
#72502=CARTESIAN_POINT('Ctrl Pts',(0.0025962843442909,-0.032443687833936,
0.0725462715015319));
#72503=CARTESIAN_POINT('Ctrl Pts',(0.00254373617058122,-0.0321434074405927,
0.0727567263777426));
#72504=CARTESIAN_POINT('',(0.00265327085821773,-0.0326943950436612,0.0723747167170185));
#72505=CARTESIAN_POINT('',(0.00258495299593697,-0.0323666188837389,0.0726009692951519));
#72506=CARTESIAN_POINT('Origin',(0.0186666169906941,-0.0326395579111819,
0.0774914347928655));
#72507=CARTESIAN_POINT('Origin',(-0.00805152535827163,-0.0321933825603026,
0.0696262928316853));
#72508=CARTESIAN_POINT('',(0.0026199279576995,-0.0321934096532688,0.0724809542990163));
#72509=CARTESIAN_POINT('',(0.00260309464350963,-0.0321934096584275,0.0725411447457605));
#72510=CARTESIAN_POINT('',(0.00269314705285821,-0.0325210109756238,0.0722562399905266));
#72511=CARTESIAN_POINT('Origin',(0.018494272782392,-0.0326393129154779,
0.0779403021487711));
#72512=CARTESIAN_POINT('',(0.0026944298295701,-0.0326943950436593,0.07225668731781));
#72513=CARTESIAN_POINT('Origin',(-0.00775112945723936,-0.0326943765538138,
0.068614132187655));
#72514=CARTESIAN_POINT('',(0.00267385034390392,-0.0326943950436702,0.0723157020174243));
#72515=CARTESIAN_POINT('Ctrl Pts',(0.00254016309196034,-0.0325229783203769,
0.0719538220169292));
#72516=CARTESIAN_POINT('Ctrl Pts',(0.00250988882649095,-0.032413025309245,
0.0720307920841329));
#72517=CARTESIAN_POINT('Ctrl Pts',(0.00248121137742225,-0.0323031222208069,
0.072108376739389));
#72518=CARTESIAN_POINT('Ctrl Pts',(0.00245416397171971,-0.0321934096576658,
0.0721864753060561));
#72519=CARTESIAN_POINT('Ctrl Pts',(0.00259162045502572,-0.0325229783203769,
0.0720547838018912));
#72520=CARTESIAN_POINT('Ctrl Pts',(0.00256273794555414,-0.032413025309245,
0.0721310445304703));
#72521=CARTESIAN_POINT('Ctrl Pts',(0.00253543736781553,-0.0323031222208069,
0.0722078911644263));
#72522=CARTESIAN_POINT('Ctrl Pts',(0.00250975021845946,-0.0321934096576658,
0.0722852240347048));
#72523=CARTESIAN_POINT('Ctrl Pts',(0.0026430778180911,-0.0325229783203769,
0.0721557455868532));
#72524=CARTESIAN_POINT('Ctrl Pts',(0.00261558706461734,-0.032413025309245,
0.0722312969768077));
#72525=CARTESIAN_POINT('Ctrl Pts',(0.00258966335820881,-0.0323031222208069,
0.0723074055894637));
#72526=CARTESIAN_POINT('Ctrl Pts',(0.0025653364651992,-0.0321934096576658,
0.0723839727633535));
#72527=CARTESIAN_POINT('Ctrl Pts',(0.00269453518115648,-0.0325229783203769,
0.0722567073718152));
#72528=CARTESIAN_POINT('Ctrl Pts',(0.00266843618368053,-0.032413025309245,
0.0723315494231452));
#72529=CARTESIAN_POINT('Ctrl Pts',(0.00264388934860209,-0.0323031222208069,
0.072406920014501));
#72530=CARTESIAN_POINT('Ctrl Pts',(0.00262092271193895,-0.0321934096576658,
0.0724827214920023));
#72531=CARTESIAN_POINT('',(0.00253704596545532,-0.0321934096584274,0.0723337147999117));
#72532=CARTESIAN_POINT('Ctrl Pts',(0.00245837103584071,-0.0322104233328925,
0.0721743693767398));
#72533=CARTESIAN_POINT('Ctrl Pts',(0.00249895147820631,-0.03226094218314,
0.0721885205058314));
#72534=CARTESIAN_POINT('Ctrl Pts',(0.00253880167622704,-0.0323120888240809,
0.0722024169856044));
#72535=CARTESIAN_POINT('Ctrl Pts',(0.00261707674710496,-0.0324156524631811,
0.0722297129086665));
#72536=CARTESIAN_POINT('Ctrl Pts',(0.00265546944481441,-0.0324680267167308,
0.0722431011319038));
#72537=CARTESIAN_POINT('Ctrl Pts',(0.00269314705289765,-0.0325210109755911,
0.0722562399905452));
#72538=CARTESIAN_POINT('Origin',(0.0115903197919812,-0.0262834582512137,
0.0670869622035607));
#72539=CARTESIAN_POINT('Origin',(-0.000352622835556759,-0.0342770775805864,
0.0654337076718416));
#72540=CARTESIAN_POINT('Ctrl Pts',(0.00265509684047048,-0.0326943950436604,
0.0723738349689563));
#72541=CARTESIAN_POINT('Ctrl Pts',(0.00263061795745464,-0.0325844576448134,
0.0724492037025243));
#72542=CARTESIAN_POINT('Ctrl Pts',(0.00260769609100913,-0.0324744968375322,
0.0725250840334893));
#72543=CARTESIAN_POINT('Ctrl Pts',(0.00258635926897814,-0.0323646534831894,
0.0726013783344614));
#72544=CARTESIAN_POINT('Ctrl Pts',(0.00255305273876136,-0.0326943950436604,
0.0724231110167664));
#72545=CARTESIAN_POINT('Ctrl Pts',(0.0025292529720375,-0.0325844576448134,
0.072499886109307));
#72546=CARTESIAN_POINT('Ctrl Pts',(0.00250703935575539,-0.0324744968375322,
0.0725771588535364));
#72547=CARTESIAN_POINT('Ctrl Pts',(0.00248643898570054,-0.0323646534831894,
0.0726548298505402));
#72548=CARTESIAN_POINT('Ctrl Pts',(0.00245100863705224,-0.0326943950436604,
0.0724723870645765));
#72549=CARTESIAN_POINT('Ctrl Pts',(0.00242788798662036,-0.0325844576448134,
0.0725505685160898));
#72550=CARTESIAN_POINT('Ctrl Pts',(0.00240638262050166,-0.0324744968375322,
0.0726292336735836));
#72551=CARTESIAN_POINT('Ctrl Pts',(0.00238651870242293,-0.0323646534831894,
0.0727082813666191));
#72552=CARTESIAN_POINT('Ctrl Pts',(0.00234896453534312,-0.0326943950436604,
0.0725216631123867));
#72553=CARTESIAN_POINT('Ctrl Pts',(0.00232652300120322,-0.0325844576448134,
0.0726012509228725));
#72554=CARTESIAN_POINT('Ctrl Pts',(0.00230572588524793,-0.0324744968375322,
0.0726813084936307));
#72555=CARTESIAN_POINT('Ctrl Pts',(0.00228659841914533,-0.0323646534831894,
0.072761732882698));
#72556=CARTESIAN_POINT('',(0.00234549955420468,-0.0326773559991329,0.0725340019415104));
#72557=CARTESIAN_POINT('',(0.00234896453534291,-0.0326943950436594,0.0725216631123874));
#72558=CARTESIAN_POINT('Origin',(0.018350566223493,-0.0326395671359021,
0.0769579310642256));
#72559=CARTESIAN_POINT('Ctrl Pts',(0.00234549955742792,-0.032677355998741,
0.0725340019424086));
#72560=CARTESIAN_POINT('Ctrl Pts',(0.00238686573544265,-0.0326267922586223,
0.0725455707194201));
#72561=CARTESIAN_POINT('Ctrl Pts',(0.00242749872782376,-0.0325756109579881,
0.0725569344482132));
#72562=CARTESIAN_POINT('Ctrl Pts',(0.00250733292209098,-0.0324719985462362,
0.072579261480482));
#72563=CARTESIAN_POINT('Ctrl Pts',(0.00254650210459833,-0.032419609162177,
0.072590215829177));
#72564=CARTESIAN_POINT('Ctrl Pts',(0.00258495299598395,-0.0323666188837757,
0.0726009692951651));
#72565=CARTESIAN_POINT('',(0.00250111769679032,-0.0326943950436703,0.0724481899147129));
#72566=CARTESIAN_POINT('Origin',(0.00812378219310841,-0.0315241814719618,
0.07415));
#72567=CARTESIAN_POINT('',(0.00234549955424635,-0.032711433837987,0.0725340019415222));
#72568=CARTESIAN_POINT('',(0.00234206093373601,-0.0326943950436593,0.0725463481428483));
#72569=CARTESIAN_POINT('Origin',(0.0183620233690585,-0.0326395665175228,
0.0769140920533534));
#72570=CARTESIAN_POINT('Origin',(0.0183235060544162,-0.0326395680346485,
0.0770546987928396));
#72571=CARTESIAN_POINT('Origin',(0.0183105541251864,-0.0326395676274512,
0.0770981194695469));
#72572=CARTESIAN_POINT('Ctrl Pts',(0.00263051404883578,-0.0332451089994434,
0.0724464360607481));
#72573=CARTESIAN_POINT('Ctrl Pts',(0.00256626308366603,-0.0329451141710254,
0.0726536180584844));
#72574=CARTESIAN_POINT('Ctrl Pts',(0.00251780044374341,-0.0326442513127493,
0.0728650511193878));
#72575=CARTESIAN_POINT('Ctrl Pts',(0.00256167071103577,-0.0332451089994434,
0.0726867704004512));
#72576=CARTESIAN_POINT('Ctrl Pts',(0.00250648410378859,-0.0329451141710254,
0.0728965488671531));
#72577=CARTESIAN_POINT('Ctrl Pts',(0.00246725564756127,-0.0326442513127493,
0.0731098882562337));
#72578=CARTESIAN_POINT('Ctrl Pts',(0.00256098227765777,-0.0332451089994434,
0.0726891737438483));
#72579=CARTESIAN_POINT('Ctrl Pts',(0.00250588631398981,-0.0329451141710254,
0.0728989781752398));
#72580=CARTESIAN_POINT('Ctrl Pts',(0.00246675019959945,-0.0326442513127493,
0.0731123366276022));
#72581=CARTESIAN_POINT('',(0.00255259470306739,-0.0331951640388616,0.0727217160818621));
#72582=CARTESIAN_POINT('',(0.00249861815856648,-0.032867753235499,0.0729518119286545));
#72583=CARTESIAN_POINT('Origin',(0.0189651205048505,-0.0326402808279159,
0.0761365724894495));
#72584=CARTESIAN_POINT('Origin',(-0.0083148397757615,-0.0326944278779092,
0.0706488767437466));
#72585=CARTESIAN_POINT('',(0.00252598830832928,-0.0326943950436593,0.0728298376525857));
#72586=CARTESIAN_POINT('',(0.00251296760118381,-0.0326943950436693,0.0728909662971511));
#72587=CARTESIAN_POINT('',(0.00258495299593777,-0.0330220786163545,0.0726009692951491));
#72588=CARTESIAN_POINT('Origin',(0.0188959009399299,-0.0326396682764628,
0.07661234690804));
#72589=CARTESIAN_POINT('',(0.00258626132929582,-0.0331951640388588,0.0726013351935165));
#72590=CARTESIAN_POINT('Origin',(-0.00803773995683232,-0.0331952026560128,
0.0696301458319343));
#72591=CARTESIAN_POINT('',(0.0025694280161916,-0.0331951640388701,0.0726615256376993));
#72592=CARTESIAN_POINT('Ctrl Pts',(0.0024132816373922,-0.0330240426238172,
0.0723087549312516));
#72593=CARTESIAN_POINT('Ctrl Pts',(0.00238791669273204,-0.032914277406352,
0.0723874226398777));
#72594=CARTESIAN_POINT('Ctrl Pts',(0.00236416538400663,-0.0328043479726691,
0.0724666539314852));
#72595=CARTESIAN_POINT('Ctrl Pts',(0.00234206093373597,-0.0326943950436593,
0.0725463481428483));
#72596=CARTESIAN_POINT('Ctrl Pts',(0.00247097690561098,-0.0330240426238172,
0.0724062864236511));
#72597=CARTESIAN_POINT('Ctrl Pts',(0.00244695555227895,-0.032914277406352,
0.0724841593237477));
#72598=CARTESIAN_POINT('Ctrl Pts',(0.00242453207379845,-0.0328043479726691,
0.0725625676347988));
#72599=CARTESIAN_POINT('Ctrl Pts',(0.00240373796260485,-0.0326943950436593,
0.0726414117010313));
#72600=CARTESIAN_POINT('Ctrl Pts',(0.00252867217382976,-0.0330240426238172,
0.0725038179160505));
#72601=CARTESIAN_POINT('Ctrl Pts',(0.00250599441182586,-0.032914277406352,
0.0725808960076177));
#72602=CARTESIAN_POINT('Ctrl Pts',(0.00248489876359028,-0.0328043479726691,
0.0726584813381124));
#72603=CARTESIAN_POINT('Ctrl Pts',(0.00246541499147372,-0.0326943950436593,
0.0727364752592143));
#72604=CARTESIAN_POINT('Ctrl Pts',(0.00258636744204854,-0.0330240426238172,
0.07260134940845));
#72605=CARTESIAN_POINT('Ctrl Pts',(0.00256503327137277,-0.032914277406352,
0.0726776326914877));
#72606=CARTESIAN_POINT('Ctrl Pts',(0.0025452654533821,-0.0328043479726691,
0.072754395041426));
#72607=CARTESIAN_POINT('Ctrl Pts',(0.0025270920203426,-0.0326943950436593,
0.0728315388173973));
#72608=CARTESIAN_POINT('',(0.00243402462104264,-0.0326943950436693,0.072688092897727));
#72609=CARTESIAN_POINT('Ctrl Pts',(0.00234549955743356,-0.0327114338383322,
0.0725340019424101));
#72610=CARTESIAN_POINT('Ctrl Pts',(0.00238685885493013,-0.0327619876831102,
0.0725455687951641));
#72611=CARTESIAN_POINT('Ctrl Pts',(0.00242748848656163,-0.0328131562604616,
0.0725569315840646));
#72612=CARTESIAN_POINT('Ctrl Pts',(0.0025073226074475,-0.0329167375858765,
0.0725792585958111));
#72613=CARTESIAN_POINT('Ctrl Pts',(0.00254649528670868,-0.0329691088920617,
0.0725902139224345));
#72614=CARTESIAN_POINT('Ctrl Pts',(0.00258495299598281,-0.0330220786163186,
0.0726009692951646));
#72615=CARTESIAN_POINT('Ctrl Pts',(0.00255436199884358,-0.0331951640388604,
0.0727207212605565));
#72616=CARTESIAN_POINT('Ctrl Pts',(0.00252481257727386,-0.0330306422010619,
0.0728358654522929));
#72617=CARTESIAN_POINT('Ctrl Pts',(0.00250004743601074,-0.0328657861914645,
0.0729521325627926));
#72618=CARTESIAN_POINT('Ctrl Pts',(0.00255259470306825,-0.0331951640388604,
0.072721716081859));
#72619=CARTESIAN_POINT('Ctrl Pts',(0.00252306584879114,-0.0330306422010619,
0.0728368968113025));
#72620=CARTESIAN_POINT('Ctrl Pts',(0.00249832276738788,-0.0328657861914645,
0.0729531995782202));
#72621=CARTESIAN_POINT('Ctrl Pts',(0.00225811569971723,-0.0331951640388604,
0.0728874800641939));
#72622=CARTESIAN_POINT('Ctrl Pts',(0.00223201390949691,-0.0330306422010619,
0.0730087489582292));
#72623=CARTESIAN_POINT('Ctrl Pts',(0.00221094659399328,-0.0328657861914645,
0.0731309930432835));
#72624=CARTESIAN_POINT('',(0.00225543231627635,-0.0331781648281893,0.072900012112519));
#72625=CARTESIAN_POINT('',(0.00225811569971698,-0.0331951640388588,0.072887480064195));
#72626=CARTESIAN_POINT('Origin',(0.0185485722983833,-0.0326412091073963,
0.0756422870574227));
#72627=CARTESIAN_POINT('Ctrl Pts',(0.00225543231762155,-0.033178164828644,
0.0729000121112653));
#72628=CARTESIAN_POINT('Ctrl Pts',(0.00229747220381256,-0.0331276811546783,
0.0729089668050028));
#72629=CARTESIAN_POINT('Ctrl Pts',(0.00233875298689534,-0.0330765663497793,
0.072917759771628));
#72630=CARTESIAN_POINT('Ctrl Pts',(0.00241983178050239,-0.0329730614463187,
0.0729350299639476));
#72631=CARTESIAN_POINT('Ctrl Pts',(0.00245959703584213,-0.0329207133373865,
0.072943500218103));
#72632=CARTESIAN_POINT('Ctrl Pts',(0.00249861815295666,-0.032867753228935,
0.0729518119131668));
#72633=CARTESIAN_POINT('',(0.00240535520140218,-0.0331951640388701,0.0728045980730385));
#72634=CARTESIAN_POINT('Origin',(0.00812378219310841,-0.0315241814719618,
0.07415));
#72635=CARTESIAN_POINT('',(0.00225543231765757,-0.0332121607144417,0.0729000121134746));
#72636=CARTESIAN_POINT('',(0.00225277570667803,-0.0331951640388587,0.0729125498651186));
#72637=CARTESIAN_POINT('Origin',(0.0185502083173675,-0.0326413646593987,
0.0755969704929008));
#72638=CARTESIAN_POINT('Origin',(0.0182518005157393,-0.0326412102062352,
0.0770355624861156));
#72639=CARTESIAN_POINT('Origin',(0.0182348218801358,-0.0326413658608145,
0.0770776108576931));
#72640=CARTESIAN_POINT('Ctrl Pts',(0.00253439100278785,-0.0337436976235975,
0.0727947025708106));
#72641=CARTESIAN_POINT('Ctrl Pts',(0.00252220125230878,-0.0336723290703325,
0.0728449744022718));
#72642=CARTESIAN_POINT('Ctrl Pts',(0.00251091770563862,-0.033601104548885,
0.072895457356125));
#72643=CARTESIAN_POINT('Ctrl Pts',(0.00247489157626549,-0.0333736987606857,
0.0730566394276685));
#72644=CARTESIAN_POINT('Ctrl Pts',(0.00244817437173634,-0.0331450831799191,
0.0732196232709377));
#72645=CARTESIAN_POINT('Ctrl Pts',(0.00248077334520411,-0.0337436976235975,
0.0730388851803373));
#72646=CARTESIAN_POINT('Ctrl Pts',(0.00247077981012201,-0.0336723290703325,
0.0730896392571367));
#72647=CARTESIAN_POINT('Ctrl Pts',(0.00246170079762656,-0.033601104548885,
0.0731405648753196));
#72648=CARTESIAN_POINT('Ctrl Pts',(0.00243271330917961,-0.0333736987606857,
0.0733031602863809));
#72649=CARTESIAN_POINT('Ctrl Pts',(0.00241310425202402,-0.0331450831799191,
0.0734671512222955));
#72650=CARTESIAN_POINT('Ctrl Pts',(0.00248023716862828,-0.0337436976235975,
0.0730413270064326));
#72651=CARTESIAN_POINT('Ctrl Pts',(0.00247026559570014,-0.0336723290703325,
0.0730920859056854));
#72652=CARTESIAN_POINT('Ctrl Pts',(0.00246120862854643,-0.033601104548885,
0.0731430159505116));
#72653=CARTESIAN_POINT('Ctrl Pts',(0.00243229152650876,-0.0333736987606857,
0.073305625494968));
#72654=CARTESIAN_POINT('Ctrl Pts',(0.0024127535508269,-0.0331450831799191,
0.0734696265018091));
#72655=CARTESIAN_POINT('',(0.0024739054797044,-0.0336938721132548,0.0730743522308228));
#72656=CARTESIAN_POINT('',(0.00243448329033809,-0.0333679869945434,0.0733073832455932));
#72657=CARTESIAN_POINT('Ctrl Pts',(0.002473905479702,-0.0336938721132646,
0.0730743522308302));
#72658=CARTESIAN_POINT('Ctrl Pts',(0.00246970672186403,-0.0336629187933929,
0.0730964063500471));
#72659=CARTESIAN_POINT('Ctrl Pts',(0.00246563844262391,-0.0336319952301037,
0.0731184780012467));
#72660=CARTESIAN_POINT('Ctrl Pts',(0.00246170079762486,-0.0336011045488947,
0.0731405648753273));
#72661=CARTESIAN_POINT('Ctrl Pts',(0.00245181989893595,-0.0335235892595451,
0.0731959884000984));
#72662=CARTESIAN_POINT('Ctrl Pts',(0.00244274416720702,-0.0334458668660366,
0.0732516062887103));
#72663=CARTESIAN_POINT('Ctrl Pts',(0.00243448329001444,-0.0333679869945382,
0.0733073832455381));
#72664=CARTESIAN_POINT('Ctrl Pts',(0.00243447609490957,-0.0333679692460365,
0.0733074271351641));
#72665=CARTESIAN_POINT('Ctrl Pts',(0.0024349252866878,-0.0333391895375683,
0.0733074876708405));
#72666=CARTESIAN_POINT('Ctrl Pts',(0.00243526241153149,-0.0333104081062018,
0.0733075298271899));
#72667=CARTESIAN_POINT('Ctrl Pts',(0.00243570934097129,-0.0332532698406287,
0.0733075801326614));
#72668=CARTESIAN_POINT('Ctrl Pts',(0.00243582246359359,-0.0332249172150636,
0.0733075887777692));
#72669=CARTESIAN_POINT('Ctrl Pts',(0.00243582710526423,-0.0331960985328845,
0.0733075824901749));
#72670=CARTESIAN_POINT('Ctrl Pts',(0.00243582715108201,-0.0331956312596458,
0.073307582383917));
#72671=CARTESIAN_POINT('Ctrl Pts',(0.00243582716738049,-0.0331951640388591,
0.0733075822738707));
#72672=CARTESIAN_POINT('',(0.00245414059620932,-0.0331951640388587,0.0731839310776592));
#72673=CARTESIAN_POINT('',(0.00244498388180488,-0.0331951640388687,0.073245756675775));
#72674=CARTESIAN_POINT('',(0.0024986181678396,-0.0335216366567738,0.0729518119162085));
#72675=CARTESIAN_POINT('Origin',(0.0189968054966534,-0.0326434571528791,
0.0752278786714746));
#72676=CARTESIAN_POINT('',(0.00249994689401839,-0.0336938721132328,0.0729520949416964));
#72677=CARTESIAN_POINT('Origin',(-0.00818100638126998,-0.033693886789632,
0.0706769977807942));
#72678=CARTESIAN_POINT('',(0.0024869261868714,-0.0336938721132538,0.0730132235862696));
#72679=CARTESIAN_POINT('Ctrl Pts',(0.00230893703444126,-0.0335235895815172,
0.0726709544358767));
#72680=CARTESIAN_POINT('Ctrl Pts',(0.00228857506027835,-0.0334144449262748,
0.0727510072278623));
#72681=CARTESIAN_POINT('Ctrl Pts',(0.00226984352311004,-0.0333049234473147,
0.0728315726538694));
#72682=CARTESIAN_POINT('Ctrl Pts',(0.00225277570667789,-0.0331951640388587,
0.0729125498651184));
#72683=CARTESIAN_POINT('Ctrl Pts',(0.00237264261285953,-0.0335235895815172,
0.0727646708792808));
#72684=CARTESIAN_POINT('Ctrl Pts',(0.00235357083005078,-0.0334144449262748,
0.0728438466385548));
#72685=CARTESIAN_POINT('Ctrl Pts',(0.0023361128476744,-0.0333049234473147,
0.0729235073698635));
#72686=CARTESIAN_POINT('Ctrl Pts',(0.002320300216196,-0.0331951640388587,
0.0730035532337389));
#72687=CARTESIAN_POINT('Ctrl Pts',(0.0024363481912778,-0.0335235895815172,
0.072858387322685));
#72688=CARTESIAN_POINT('Ctrl Pts',(0.0024185665998232,-0.0334144449262748,
0.0729366860492473));
#72689=CARTESIAN_POINT('Ctrl Pts',(0.00240238217223875,-0.0333049234473147,
0.0730154420858577));
#72690=CARTESIAN_POINT('Ctrl Pts',(0.0023878247257141,-0.0331951640388587,
0.0730945566023593));
#72691=CARTESIAN_POINT('Ctrl Pts',(0.00250005376969607,-0.0335235895815172,
0.0729521037660892));
#72692=CARTESIAN_POINT('Ctrl Pts',(0.00248356236959563,-0.0334144449262748,
0.0730295254599398));
#72693=CARTESIAN_POINT('Ctrl Pts',(0.00246865149680311,-0.0333049234473147,
0.0731073768018518));
#72694=CARTESIAN_POINT('Ctrl Pts',(0.00245534923523221,-0.0331951640388587,
0.0731855599709798));
#72695=CARTESIAN_POINT('',(0.00235345815145367,-0.0331951640388687,0.0730482404713989));
#72696=CARTESIAN_POINT('Ctrl Pts',(0.00225543232071546,-0.0332121607145975,
0.0729000121141221));
#72697=CARTESIAN_POINT('Ctrl Pts',(0.00229740148257267,-0.0332625444109919,
0.0729089517555959));
#72698=CARTESIAN_POINT('Ctrl Pts',(0.00233864744991015,-0.0333135300747167,
0.0729177373530184));
#72699=CARTESIAN_POINT('Ctrl Pts',(0.00241972573601266,-0.0334167203140634,
0.072935007433644));
#72700=CARTESIAN_POINT('Ctrl Pts',(0.00245952665252752,-0.0334688847587342,
0.0729434852280108));
#72701=CARTESIAN_POINT('Ctrl Pts',(0.00249861816849204,-0.0335216366562426,
0.0729518119165108));
#72702=CARTESIAN_POINT('Ctrl Pts',(0.00247474426424094,-0.0336938721132388,
0.0730738080292304));
#72703=CARTESIAN_POINT('Ctrl Pts',(0.00246844495551768,-0.0336474569764957,
0.0731068737227775));
#72704=CARTESIAN_POINT('Ctrl Pts',(0.00246253315411867,-0.033601104548885,
0.0731400108920043));
#72705=CARTESIAN_POINT('Ctrl Pts',(0.00244756583218471,-0.0334837508592656,
0.0732239065857737));
#72706=CARTESIAN_POINT('Ctrl Pts',(0.00243509108614637,-0.0333660264659097,
0.0733082089515187));
#72707=CARTESIAN_POINT('Ctrl Pts',(0.00247390547970826,-0.0336938721132388,
0.0730743522308028));
#72708=CARTESIAN_POINT('Ctrl Pts',(0.00246760935637739,-0.0336474569764957,
0.0731074228340341));
#72709=CARTESIAN_POINT('Ctrl Pts',(0.00246170079762656,-0.033601104548885,
0.0731405648753196));
#72710=CARTESIAN_POINT('Ctrl Pts',(0.00244674168533225,-0.0334837508592656,
0.0732244729040216));
#72711=CARTESIAN_POINT('Ctrl Pts',(0.00243427551083811,-0.0333660264659097,
0.073308787356014));
#72712=CARTESIAN_POINT('Ctrl Pts',(0.00218871503290588,-0.0336938721132388,
0.0732593831696475));
#72713=CARTESIAN_POINT('Ctrl Pts',(0.00218350195705983,-0.0336474569764957,
0.0732941230872002));
#72714=CARTESIAN_POINT('Ctrl Pts',(0.00217869591301452,-0.033601104548885,
0.0733289216499863));
#72715=CARTESIAN_POINT('Ctrl Pts',(0.0021665281144706,-0.0334837508592656,
0.0734170236102697));
#72716=CARTESIAN_POINT('Ctrl Pts',(0.00215697630287576,-0.0333660264659097,
0.073505447439764));
#72717=CARTESIAN_POINT('',(0.00218852477495756,-0.0336769361243753,0.073270955416213));
#72718=CARTESIAN_POINT('',(0.00219041596997241,-0.033693872113232,0.0732582796053983));
#72719=CARTESIAN_POINT('Ctrl Pts',(0.00218852477495752,-0.033676936124375,
0.0732709554162133));
#72720=CARTESIAN_POINT('Ctrl Pts',(0.00218883774124687,-0.0336797586670072,
0.0732688422862028));
#72721=CARTESIAN_POINT('Ctrl Pts',(0.00218915182420595,-0.0336825812712939,
0.0732667294032504));
#72722=CARTESIAN_POINT('Ctrl Pts',(0.00218978222305854,-0.0336882266040259,
0.0732625041306933));
#72723=CARTESIAN_POINT('Ctrl Pts',(0.0021900985389585,-0.0336910493324753,
0.0732603917410849));
#72724=CARTESIAN_POINT('Ctrl Pts',(0.00219041596997441,-0.0336938721132317,
0.0732582796053982));
#72725=CARTESIAN_POINT('Ctrl Pts',(0.00218852477495759,-0.0336769361243753,
0.073270955416213));
#72726=CARTESIAN_POINT('Ctrl Pts',(0.00222998626234548,-0.0336279007516223,
0.0732770960927425));
#72727=CARTESIAN_POINT('Ctrl Pts',(0.00227203809666917,-0.0335767878632079,
0.073283324202931));
#72728=CARTESIAN_POINT('Ctrl Pts',(0.0023544478837272,-0.0334733198857318,
0.0732955295500391));
#72729=CARTESIAN_POINT('Ctrl Pts',(0.00239485489871443,-0.0334209645014067,
0.0733015140533508));
#72730=CARTESIAN_POINT('Ctrl Pts',(0.00243448329139574,-0.0333679869844681,
0.0733073832383745));
#72731=CARTESIAN_POINT('',(0.00233216072484841,-0.0336938721132534,0.0731663159181205));
#72732=CARTESIAN_POINT('Origin',(0.00812378219310841,-0.0315241814719618,
0.07415));
#72733=CARTESIAN_POINT('',(0.00218852477624567,-0.0337108120655398,0.073270955416408));
#72734=CARTESIAN_POINT('',(0.00218666066001425,-0.0336938721132327,0.073283635237734));
#72735=CARTESIAN_POINT('Origin',(0.0182094577056769,-0.0345562511818623,
0.076773540193245));
#72736=CARTESIAN_POINT('Ctrl Pts',(0.0021866606600214,-0.0336938721132293,
0.0732836352377395));
#72737=CARTESIAN_POINT('Ctrl Pts',(0.00218696906411422,-0.0336910493409645,
0.0732815217716105));
#72738=CARTESIAN_POINT('Ctrl Pts',(0.00218727861043721,-0.0336882266082704,
0.0732794083761406));
#72739=CARTESIAN_POINT('Ctrl Pts',(0.00218789998272394,-0.0336825812712746,
0.0732751817634371));
#72740=CARTESIAN_POINT('Ctrl Pts',(0.00218821180866932,-0.0336797586669975,
0.0732730685462159));
#72741=CARTESIAN_POINT('Ctrl Pts',(0.0021885247749576,-0.033676936124375,
0.0732709554162127));
#72742=CARTESIAN_POINT('Origin',(0.0185369295380939,-0.034556251520342,
0.0745624488552952));
#72743=CARTESIAN_POINT('Ctrl Pts',(0.00246032955331888,-0.034243627687391,
0.0731482868689784));
#72744=CARTESIAN_POINT('Ctrl Pts',(0.00242254931976735,-0.0339430054201809,
0.0733618875065393));
#72745=CARTESIAN_POINT('Ctrl Pts',(0.00240096569112108,-0.0336441434784052,
0.0735777270890724));
#72746=CARTESIAN_POINT('Ctrl Pts',(0.00242214783259408,-0.034243627687391,
0.0733953539776808));
#72747=CARTESIAN_POINT('Ctrl Pts',(0.00239368588866121,-0.0339430054201809,
0.0736103946625782));
#72748=CARTESIAN_POINT('Ctrl Pts',(0.00238150254761548,-0.0336441434784052,
0.0738269683096698));
#72749=CARTESIAN_POINT('Ctrl Pts',(0.00242176601538683,-0.034243627687391,
0.0733978246487678));
#72750=CARTESIAN_POINT('Ctrl Pts',(0.00239339725435015,-0.0339430054201809,
0.0736128797341386));
#72751=CARTESIAN_POINT('Ctrl Pts',(0.00238130791618042,-0.0336441434784052,
0.0738294607218758));
#72752=CARTESIAN_POINT('',(0.00241751373855154,-0.0341934961088741,0.0734312334700822));
#72753=CARTESIAN_POINT('',(0.00239280147842421,-0.0338664212863773,0.0736662799856491));
#72754=CARTESIAN_POINT('Origin',(0.0189497159229241,-0.0345610720406939,
0.0760272755920783));
#72755=CARTESIAN_POINT('Origin',(-0.00853460080732833,-0.033693800507303,
0.0727439981907874));
#72756=CARTESIAN_POINT('',(0.00240466836925947,-0.0336938721132327,0.0735418371354143));
#72757=CARTESIAN_POINT('',(0.00239941178496455,-0.0336938721132427,0.0736041156896902));
#72758=CARTESIAN_POINT('',(0.00243448329139656,-0.0340203938281605,0.0733073832383692));
#72759=CARTESIAN_POINT('Origin',(0.018802680505642,-0.0345589643240237,
0.0764854429407088));
#72760=CARTESIAN_POINT('',(0.00243582716738048,-0.0341934961088739,0.0733075822738707));
#72761=CARTESIAN_POINT('Origin',(-0.0084647153816561,-0.0341934220717687,
0.0716931503575934));
#72762=CARTESIAN_POINT('',(0.002426670452976,-0.0341934961088841,0.0733694078719864));
#72763=CARTESIAN_POINT('Ctrl Pts',(0.00222754177036901,-0.0340223579322397,
0.073038987454037));
#72764=CARTESIAN_POINT('Ctrl Pts',(0.00221221800971782,-0.0339125849573575,
0.0731203119875072));
#72765=CARTESIAN_POINT('Ctrl Pts',(0.00219858824576653,-0.0338030433565231,
0.0732018965414073));
#72766=CARTESIAN_POINT('Ctrl Pts',(0.00218666066001375,-0.0336938721132326,
0.0732836352377335));
#72767=CARTESIAN_POINT('Ctrl Pts',(0.00229700612358545,-0.0340223579322397,
0.0731285189203635));
#72768=CARTESIAN_POINT('Ctrl Pts',(0.00228291723536276,-0.0339125849573575,
0.0732088853592322));
#72769=CARTESIAN_POINT('Ctrl Pts',(0.00227050164577749,-0.0338030433565231,
0.0732894869327829));
#72770=CARTESIAN_POINT('Ctrl Pts',(0.00225976609503748,-0.0336938721132326,
0.0733702191577206));
#72771=CARTESIAN_POINT('Ctrl Pts',(0.00236647047680189,-0.0340223579322397,
0.0732180503866899));
#72772=CARTESIAN_POINT('Ctrl Pts',(0.00235361646100771,-0.0339125849573575,
0.0732974587309572));
#72773=CARTESIAN_POINT('Ctrl Pts',(0.00234241504578844,-0.0338030433565231,
0.0733770773241585));
#72774=CARTESIAN_POINT('Ctrl Pts',(0.00233287153006121,-0.0336938721132326,
0.0734568030777077));
#72775=CARTESIAN_POINT('Ctrl Pts',(0.00243593483001833,-0.0340223579322397,
0.0733075818530164));
#72776=CARTESIAN_POINT('Ctrl Pts',(0.00242431568665266,-0.0339125849573575,
0.0733860321026821));
#72777=CARTESIAN_POINT('Ctrl Pts',(0.0024143284457994,-0.0338030433565231,
0.0734646677155342));
#72778=CARTESIAN_POINT('Ctrl Pts',(0.00240597696508495,-0.0336938721132326,
0.0735433869976948));
#72779=CARTESIAN_POINT('',(0.00229566451464686,-0.0336938721132427,0.0734127361865842));
#72780=CARTESIAN_POINT('Ctrl Pts',(0.0021885247798043,-0.0337108120662684,
0.0732709554169307));
#72781=CARTESIAN_POINT('Ctrl Pts',(0.00223106005550166,-0.033761140899443,
0.0732772551274719));
#72782=CARTESIAN_POINT('Ctrl Pts',(0.0022728191567851,-0.0338121088781593,
0.073283439882272));
#72783=CARTESIAN_POINT('Ctrl Pts',(0.00235482305235754,-0.033915338277323,
0.0732955851145971));
#72784=CARTESIAN_POINT('Ctrl Pts',(0.00239503315401185,-0.0339675558473116,
0.0733015404539501));
#72785=CARTESIAN_POINT('Ctrl Pts',(0.0024344832914352,-0.0340203938281304,
0.0733073832383803));
#72786=CARTESIAN_POINT('Ctrl Pts',(0.0024191424893604,-0.0341934961088741,
0.0734300249368031));
#72787=CARTESIAN_POINT('Ctrl Pts',(0.00240425757213368,-0.0340287516182428,
0.0735479638684953));
#72788=CARTESIAN_POINT('Ctrl Pts',(0.00239425987930614,-0.0338644633275951,
0.0736664172285476));
#72789=CARTESIAN_POINT('Ctrl Pts',(0.00241751373855163,-0.0341934961088741,
0.0734312334700822));
#72790=CARTESIAN_POINT('Ctrl Pts',(0.00240265380679836,-0.0340287516182428,
0.0735492060749143));
#72791=CARTESIAN_POINT('Ctrl Pts',(0.00239268246983108,-0.0338644633275951,
0.0736676920466647));
#72792=CARTESIAN_POINT('Ctrl Pts',(0.00214613252601321,-0.0341934961088741,
0.0736325983596118));
#72793=CARTESIAN_POINT('Ctrl Pts',(0.00213543565471333,-0.0340287516182428,
0.0737561815572157));
#72794=CARTESIAN_POINT('Ctrl Pts',(0.00212985571099966,-0.0338644633275951,
0.0738801012651471));
#72795=CARTESIAN_POINT('',(0.00214504098444017,-0.0341764758832386,0.0736453679059581));
#72796=CARTESIAN_POINT('',(0.00214613252601315,-0.034193496108874,0.0736325983596118));
#72797=CARTESIAN_POINT('Origin',(0.0186010544269866,-0.0345621026495323,
0.075548247761691));
#72798=CARTESIAN_POINT('Ctrl Pts',(0.00214504098543265,-0.034176475883747,
0.0736453679044303));
#72799=CARTESIAN_POINT('Ctrl Pts',(0.00218781327756581,-0.0341260050040171,
0.0736489780605097));
#72800=CARTESIAN_POINT('Ctrl Pts',(0.00222984208957002,-0.0340749269147647,
0.0736525254254876));
#72801=CARTESIAN_POINT('Ctrl Pts',(0.00231244531064647,-0.0339715436305273,
0.0736594975052568));
#72802=CARTESIAN_POINT('Ctrl Pts',(0.00235298838128689,-0.0339192778237525,
0.0736629195809504));
#72803=CARTESIAN_POINT('Ctrl Pts',(0.00239280147742893,-0.0338664212855041,
0.0736662799837048));
#72804=CARTESIAN_POINT('',(0.00228182313229235,-0.0341934961088841,0.0735319159148571));
#72805=CARTESIAN_POINT('Origin',(0.00812378219310841,-0.0315241814719618,
0.07415));
#72806=CARTESIAN_POINT('',(0.00214504098510271,-0.0342105180190538,0.0736453679068587));
#72807=CARTESIAN_POINT('',(0.0021439767196288,-0.0341934961088739,0.0736581397562618));
#72808=CARTESIAN_POINT('Origin',(0.0186100572327185,-0.0345621703323684,
0.0755038230687897));
#72809=CARTESIAN_POINT('Origin',(0.0186871976013945,-0.0345621039636221,
0.0745276772041862));
#72810=CARTESIAN_POINT('Origin',(0.0186886212027649,-0.034562171586023,
0.074572982011659));
#72811=CARTESIAN_POINT('Ctrl Pts',(0.00240479452811651,-0.0346945769586966,
0.0735403424402366));
#72812=CARTESIAN_POINT('Ctrl Pts',(0.00239202500643369,-0.0345275153362944,
0.0736601289266377));
#72813=CARTESIAN_POINT('Ctrl Pts',(0.00238301935663994,-0.0343603235965185,
0.073780347985663));
#72814=CARTESIAN_POINT('Ctrl Pts',(0.00237779892898214,-0.0341934961088739,
0.0739006436668402));
#72815=CARTESIAN_POINT('Ctrl Pts',(0.00239774369607375,-0.0346945769586966,
0.0736238787445202));
#72816=CARTESIAN_POINT('Ctrl Pts',(0.00238672387573027,-0.0345275153362944,
0.0737438129134213));
#72817=CARTESIAN_POINT('Ctrl Pts',(0.00237947302431693,-0.0343603235965185,
0.0738641246666484));
#72818=CARTESIAN_POINT('Ctrl Pts',(0.00237600729809141,-0.0341934961088739,
0.0739844578567164));
#72819=CARTESIAN_POINT('Ctrl Pts',(0.00239069286403098,-0.0346945769586966,
0.0737074150488039));
#72820=CARTESIAN_POINT('Ctrl Pts',(0.00238142274502685,-0.0345275153362944,
0.073827496900205));
#72821=CARTESIAN_POINT('Ctrl Pts',(0.00237592669199397,-0.0343603235965185,
0.0739479013476339));
#72822=CARTESIAN_POINT('Ctrl Pts',(0.0023742156672008,-0.0341934961088739,
0.074068272046593));
#72823=CARTESIAN_POINT('Ctrl Pts',(0.00238364203198824,-0.0346945769586966,
0.0737909513530872));
#72824=CARTESIAN_POINT('Ctrl Pts',(0.00237612161432341,-0.0345275153362944,
0.0739111808869886));
#72825=CARTESIAN_POINT('Ctrl Pts',(0.0023723803596709,-0.0343603235965185,
0.0740316780286192));
#72826=CARTESIAN_POINT('Ctrl Pts',(0.00237242403630996,-0.0341934961088739,
0.0741520862364687));
#72827=CARTESIAN_POINT('',(0.00238364203203939,-0.0346945769586966,0.0737909513524835));
#72828=CARTESIAN_POINT('',(0.00237373722912618,-0.0343667727831445,0.0740270857514938));
#72829=CARTESIAN_POINT('Origin',(0.0191748778417514,-0.0345626457064276,
0.0746579272563131));
#72830=CARTESIAN_POINT('Origin',(-0.00867591732885543,-0.0341934771028958,
0.0737908895859129));
#72831=CARTESIAN_POINT('',(0.00237776687175778,-0.034193496108874,0.0739021433341527));
#72832=CARTESIAN_POINT('',(0.00237643116290913,-0.0341934961088839,0.0739646290595874));
#72833=CARTESIAN_POINT('',(0.00239280147897343,-0.0345211942962709,0.0736662799838778));
#72834=CARTESIAN_POINT('Origin',(0.0191311264218782,-0.0345625596119205,
0.0751367556212441));
#72835=CARTESIAN_POINT('',(0.00239415520064965,-0.0346945769586885,0.073666394243946));
#72836=CARTESIAN_POINT('Origin',(-0.00863021209177555,-0.0346945685853906,
0.0727358884589146));
#72837=CARTESIAN_POINT('',(0.00238889861635452,-0.0346945769587025,0.0737286727982248));
#72838=CARTESIAN_POINT('Ctrl Pts',(0.00216941548056856,-0.0345231616327842,
0.073411408737782));
#72839=CARTESIAN_POINT('Ctrl Pts',(0.0021592350398722,-0.0344132092796988,
0.0734934812998365));
#72840=CARTESIAN_POINT('Ctrl Pts',(0.00215075273064796,-0.0343032738558979,
0.0735757602017098));
#72841=CARTESIAN_POINT('Ctrl Pts',(0.00214397671962875,-0.0341934961088739,
0.0736581397562618));
#72842=CARTESIAN_POINT('Ctrl Pts',(0.00224436437515982,-0.0345231616327842,
0.0734964016747713));
#72843=CARTESIAN_POINT('Ctrl Pts',(0.00223535544243938,-0.0344132092796988,
0.0735774411718335));
#72844=CARTESIAN_POINT('Ctrl Pts',(0.00222802321261212,-0.0343032738558979,
0.0736586628302974));
#72845=CARTESIAN_POINT('Ctrl Pts',(0.00222237441372113,-0.0341934961088739,
0.0737399623552154));
#72846=CARTESIAN_POINT('Ctrl Pts',(0.00231931326975108,-0.0345231616327842,
0.0735813946117606));
#72847=CARTESIAN_POINT('Ctrl Pts',(0.00231147584500655,-0.0344132092796988,
0.0736614010438304));
#72848=CARTESIAN_POINT('Ctrl Pts',(0.00230529369457628,-0.0343032738558979,
0.073741565458885));
#72849=CARTESIAN_POINT('Ctrl Pts',(0.00230077210781351,-0.0341934961088739,
0.0738217849541689));
#72850=CARTESIAN_POINT('Ctrl Pts',(0.00239426216434234,-0.0345231616327842,
0.0736663875487499));
#72851=CARTESIAN_POINT('Ctrl Pts',(0.00238759624757372,-0.0344132092796988,
0.0737453609158274));
#72852=CARTESIAN_POINT('Ctrl Pts',(0.00238256417654045,-0.0343032738558979,
0.0738244680874726));
#72853=CARTESIAN_POINT('Ctrl Pts',(0.00237916980190589,-0.0341934961088739,
0.0739036075531224));
#72854=CARTESIAN_POINT('',(0.00226087179570329,-0.0341934961088839,0.0737801415452172));
#72855=CARTESIAN_POINT('Ctrl Pts',(0.00214504098853992,-0.0342105180195387,
0.0736453679071444));
#72856=CARTESIAN_POINT('Ctrl Pts',(0.00218786136386767,-0.0342610556241353,
0.0736489821354375));
#72857=CARTESIAN_POINT('Ctrl Pts',(0.00222991334970009,-0.0343122189870262,
0.0736525315082725));
#72858=CARTESIAN_POINT('Ctrl Pts',(0.00231251740430272,-0.0344158119695188,
0.0736595036543358));
#72859=CARTESIAN_POINT('Ctrl Pts',(0.00235303568742227,-0.0344681990450085,
0.0736629235759062));
#72860=CARTESIAN_POINT('Ctrl Pts',(0.00239280147899817,-0.0345211942962524,
0.0736662799838758));
#72861=CARTESIAN_POINT('Ctrl Pts',(0.00238519130502,-0.0346945769586932,
0.0737896432542134));
#72862=CARTESIAN_POINT('Ctrl Pts',(0.00237774118428112,-0.034529677707698,
0.073908284560328));
#72863=CARTESIAN_POINT('Ctrl Pts',(0.00237520098378099,-0.034364806625142,
0.0740271324092652));
#72864=CARTESIAN_POINT('Ctrl Pts',(0.00238364203204002,-0.0346945769586932,
0.0737909513524745));
#72865=CARTESIAN_POINT('Ctrl Pts',(0.0023762189553071,-0.034529677707698,
0.0739096246887117));
#72866=CARTESIAN_POINT('Ctrl Pts',(0.00237370709953858,-0.0343648066251421,
0.0740285034226486));
#72867=CARTESIAN_POINT('Ctrl Pts',(0.0021254401343527,-0.0346945769586932,
0.0740089590617254));
#72868=CARTESIAN_POINT('Ctrl Pts',(0.00212252421275124,-0.034529677707698,
0.0741329705394995));
#72869=CARTESIAN_POINT('Ctrl Pts',(0.00212473629110149,-0.0343648066251421,
0.0742569965687347));
#72870=CARTESIAN_POINT('',(0.00212515255291101,-0.0346775396664972,0.0740217719488452));
#72871=CARTESIAN_POINT('',(0.00212544013436173,-0.0346945769586886,0.0740089590617211));
#72872=CARTESIAN_POINT('Origin',(0.0187255156885455,-0.0345626617235455,
0.0742238730028019));
#72873=CARTESIAN_POINT('Ctrl Pts',(0.00212515255389289,-0.0346775396670097,
0.0740217719473096));
#72874=CARTESIAN_POINT('Ctrl Pts',(0.00216810092722141,-0.0346269749928192,
0.0740226900084676));
#72875=CARTESIAN_POINT('Ctrl Pts',(0.00221028601288986,-0.0345757902890794,
0.0740235917177184));
#72876=CARTESIAN_POINT('Ctrl Pts',(0.00229316434710726,-0.0344721681088162,
0.0740253633473307));
#72877=CARTESIAN_POINT('Ctrl Pts',(0.00233382510333092,-0.0344197714290091,
0.0740262325787656));
#72878=CARTESIAN_POINT('Ctrl Pts',(0.00237373722902026,-0.0343667727830607,
0.0740270857512437));
#72879=CARTESIAN_POINT('',(0.00225454108321056,-0.0346945769587026,0.0738999552071123));
#72880=CARTESIAN_POINT('Origin',(0.00812378219310841,-0.0315241814719618,
0.07415));
#72881=CARTESIAN_POINT('',(0.00212515255407319,-0.0347116136489611,0.0740217719496091));
#72882=CARTESIAN_POINT('',(0.00212489233953384,-0.0346945769586885,0.0740345854224619));
#72883=CARTESIAN_POINT('Origin',(0.0187246164869726,-0.0345626683317801,
0.0741785687284629));
#72884=CARTESIAN_POINT('Origin',(0.0187189911031968,-0.0345626630395094,
0.0745292358347301));
#72885=CARTESIAN_POINT('Origin',(0.0187161510230357,-0.0345626693449426,
0.0745744605800943));
#72886=CARTESIAN_POINT('Ctrl Pts',(0.0023795055537286,-0.0352450361874067,
0.0738635588788241));
#72887=CARTESIAN_POINT('Ctrl Pts',(0.00236870224956947,-0.0349452760959492,
0.0740802078273224));
#72888=CARTESIAN_POINT('Ctrl Pts',(0.00237424852171626,-0.034644428984174,
0.0742970550480364));
#72889=CARTESIAN_POINT('Ctrl Pts',(0.00237943574741855,-0.0352450361874067,
0.0738660829137049));
#72890=CARTESIAN_POINT('Ctrl Pts',(0.00236872763879703,-0.0349452760959492,
0.0740827344949913));
#72891=CARTESIAN_POINT('Ctrl Pts',(0.0023743690343533,-0.034644428984174,
0.0742995771704966));
#72892=CARTESIAN_POINT('Ctrl Pts',(0.0023725242315717,-0.0352450361874067,
0.0741159873573403));
#72893=CARTESIAN_POINT('Ctrl Pts',(0.00237124142370388,-0.0349452760959492,
0.0743328996107243));
#72894=CARTESIAN_POINT('Ctrl Pts',(0.00238630097861556,-0.034644428984174,
0.0745492922655673));
#72895=CARTESIAN_POINT('Ctrl Pts',(0.00237245511641323,-0.0352450361874067,
0.0741184864017767));
#72896=CARTESIAN_POINT('Ctrl Pts',(0.00237126656155295,-0.0349452760959492,
0.0743354012618816));
#72897=CARTESIAN_POINT('Ctrl Pts',(0.00238642029805818,-0.034644428984174,
0.074551789416518));
#72898=CARTESIAN_POINT('',(0.00237242165110434,-0.0351951634053262,0.0741520538780395));
#72899=CARTESIAN_POINT('',(0.00237736577994594,-0.0348678972935461,0.0743883766056446));
#72900=CARTESIAN_POINT('Origin',(0.0190945965440124,-0.0345636767883521,
0.0732726431573248));
#72901=CARTESIAN_POINT('Origin',(-0.00866297998397881,-0.0346946199326802,
0.0748463754880312));
#72902=CARTESIAN_POINT('',(0.00237354227144593,-0.0346945769330288,0.0742634276919279));
#72903=CARTESIAN_POINT('',(0.00237613270947176,-0.0346945769458128,0.0743258739946087));
#72904=CARTESIAN_POINT('',(0.00237373722915741,-0.0350221583435276,0.0740270857512628));
#72905=CARTESIAN_POINT('Origin',(0.0191558972229172,-0.0345628458717777,
0.0737494928402475));
#72906=CARTESIAN_POINT('',(0.00237497389593432,-0.035195136029876,0.0740271091612433));
#72907=CARTESIAN_POINT('Origin',(-0.00864148601942892,-0.0351951838366824,
0.0737916207221787));
#72908=CARTESIAN_POINT('',(0.00237242403620701,-0.035195137132875,0.0741520862358497));
#72909=CARTESIAN_POINT('Ctrl Pts',(0.00213478847589137,-0.0350241211494343,
0.073786744917223));
#72910=CARTESIAN_POINT('Ctrl Pts',(0.0021297847860665,-0.0349144232818962,
0.0738692408500946));
#72911=CARTESIAN_POINT('Ctrl Pts',(0.00212648335117296,-0.0348045283579412,
0.0739518895906026));
#72912=CARTESIAN_POINT('Ctrl Pts',(0.00212489233932004,-0.0346945769439157,
0.0740345854335728));
#72913=CARTESIAN_POINT('Ctrl Pts',(0.00221492625713316,-0.0350241211494343,
0.0738668640648758));
#72914=CARTESIAN_POINT('Ctrl Pts',(0.00221102617571708,-0.0349144232818962,
0.0739482561326685));
#72915=CARTESIAN_POINT('Ctrl Pts',(0.0022088061921152,-0.0348045283579412,
0.0740297775350068));
#72916=CARTESIAN_POINT('Ctrl Pts',(0.00220827303550138,-0.0346945769439157,
0.0741113239591468));
#72917=CARTESIAN_POINT('Ctrl Pts',(0.00229506403837495,-0.0350241211494343,
0.0739469832125286));
#72918=CARTESIAN_POINT('Ctrl Pts',(0.00229226756536765,-0.0349144232818962,
0.0740272714152425));
#72919=CARTESIAN_POINT('Ctrl Pts',(0.00229112903305743,-0.0348045283579412,
0.0741076654794111));
#72920=CARTESIAN_POINT('Ctrl Pts',(0.00229165373168272,-0.0346945769439157,
0.0741880624847209));
#72921=CARTESIAN_POINT('Ctrl Pts',(0.00237520181961674,-0.0350241211494343,
0.0740271023601814));
#72922=CARTESIAN_POINT('Ctrl Pts',(0.00237350895501823,-0.0349144232818962,
0.0741062866978165));
#72923=CARTESIAN_POINT('Ctrl Pts',(0.00237345187399967,-0.0348045283579412,
0.0741855534238153));
#72924=CARTESIAN_POINT('Ctrl Pts',(0.00237503442786406,-0.0346945769439157,
0.0742648010102949));
#72925=CARTESIAN_POINT('',(0.00224921730540605,-0.0346945769458128,0.0741490065569093));
#72926=CARTESIAN_POINT('Ctrl Pts',(0.0021251525573556,-0.0347116136492792,
0.0740217719496746));
#72927=CARTESIAN_POINT('Ctrl Pts',(0.00216808387467062,-0.034762154653234,
0.0740226896591267));
#72928=CARTESIAN_POINT('Ctrl Pts',(0.00221026034341442,-0.0348133084097118,
0.0740235912327669));
#72929=CARTESIAN_POINT('Ctrl Pts',(0.00229313878288501,-0.0349168561544567,
0.0740253628608474));
#72930=CARTESIAN_POINT('Ctrl Pts',(0.00233380787995237,-0.0349692089015909,
0.0740262322125731));
#72931=CARTESIAN_POINT('Ctrl Pts',(0.00237373722919349,-0.0350221583435001,
0.0740270857512836));
#72932=CARTESIAN_POINT('Ctrl Pts',(0.00237348041836607,-0.0351951371254872,
0.0741510740715169));
#72933=CARTESIAN_POINT('Ctrl Pts',(0.00237350262412072,-0.0350307338985332,
0.0742699579525277));
#72934=CARTESIAN_POINT('Ctrl Pts',(0.00237843840996862,-0.0348659306906667,
0.0743887393301731));
#72935=CARTESIAN_POINT('Ctrl Pts',(0.00237242403632317,-0.0351951371254872,
0.0741520862358493));
#72936=CARTESIAN_POINT('Ctrl Pts',(0.00237246716794029,-0.0350307338985332,
0.0742709919568959));
#72937=CARTESIAN_POINT('Ctrl Pts',(0.00237742476444186,-0.0348659306906667,
0.0743897942910266));
#72938=CARTESIAN_POINT('Ctrl Pts',(0.00219537330481443,-0.0351951371254872,
0.0743217260329856));
#72939=CARTESIAN_POINT('Ctrl Pts',(0.00219892363279228,-0.0350307338985332,
0.0744442921668109));
#72940=CARTESIAN_POINT('Ctrl Pts',(0.00220753671758532,-0.0348659306906667,
0.0745666068297094));
#72941=CARTESIAN_POINT('Origin',(-0.00293624707561006,-0.0308609188508701,
0.0746088010768252));
#72942=CARTESIAN_POINT('',(0.00229523390934874,-0.0351951371254872,0.0742260453625317));
#72943=CARTESIAN_POINT('Origin',(0.00908388395447356,-0.0351840467441202,
0.0739684779432064));
#72944=CARTESIAN_POINT('Origin',(-0.00377189715848901,-0.0352322613739614,
0.0754388458336736));
#72945=CARTESIAN_POINT('',(0.00239206408775232,-0.0351951142564655,0.0746245757517679));
#72946=CARTESIAN_POINT('',(0.00240502397038673,-0.0351951372916786,0.0747485853239551));
#72947=CARTESIAN_POINT('Origin',(0.00833153237709209,-0.0352875121341927,
0.0744198901674271));
#72948=CARTESIAN_POINT('Origin',(0.00878592006143388,-0.0298325076522275,
0.066676261730273));
#72949=CARTESIAN_POINT('Origin',(7.23359568405449E-5,-0.0338731629816332,
0.0718204020753387));
#72950=CARTESIAN_POINT('Ctrl Pts',(0.00320793794572019,-0.0321934096636941,
0.0711646003482395));
#72951=CARTESIAN_POINT('Ctrl Pts',(0.00315450071357742,-0.0320508460843131,
0.0712525916193816));
#72952=CARTESIAN_POINT('Ctrl Pts',(0.00310346792512061,-0.0319086045660688,
0.0713419522978032));
#72953=CARTESIAN_POINT('Ctrl Pts',(0.00305493362259791,-0.0317669892864341,
0.0714324809280297));
#72954=CARTESIAN_POINT('Ctrl Pts',(0.00316598295920628,-0.0321934096636941,
0.0712371965722084));
#72955=CARTESIAN_POINT('Ctrl Pts',(0.0031138451649028,-0.0320508460843131,
0.0713259388176304));
#72956=CARTESIAN_POINT('Ctrl Pts',(0.00306413101170198,-0.0319086045660688,
0.0714160149907642));
#72957=CARTESIAN_POINT('Ctrl Pts',(0.00301693157576772,-0.0317669892864341,
0.0715072223292938));
#72958=CARTESIAN_POINT('Ctrl Pts',(0.00312402797269236,-0.0321934096636941,
0.0713097927961771));
#72959=CARTESIAN_POINT('Ctrl Pts',(0.00307318961622818,-0.0320508460843131,
0.0713992860158791));
#72960=CARTESIAN_POINT('Ctrl Pts',(0.00302479409828335,-0.0319086045660688,
0.071490077683725));
#72961=CARTESIAN_POINT('Ctrl Pts',(0.00297892952893754,-0.0317669892864341,
0.0715819637305579));
#72962=CARTESIAN_POINT('Ctrl Pts',(0.00308207298617844,-0.0321934096636941,
0.0713823890201459));
#72963=CARTESIAN_POINT('Ctrl Pts',(0.00303253406755356,-0.0320508460843131,
0.0714726332141279));
#72964=CARTESIAN_POINT('Ctrl Pts',(0.00298545718486472,-0.0319086045660688,
0.0715641403766859));
#72965=CARTESIAN_POINT('Ctrl Pts',(0.00294092748210736,-0.0317669892864341,
0.0716567051318221));
#72966=CARTESIAN_POINT('',(0.00308282356917989,-0.0321934096636941,0.0713810902593544));
#72967=CARTESIAN_POINT('',(0.00297332029942594,-0.0318665617511259,0.0715905337918369));
#72968=CARTESIAN_POINT('Origin',(0.0174226902661654,-0.0326371944421278,
0.0799593259731346));
#72969=CARTESIAN_POINT('Origin',(-0.00684265072727457,-0.0316939261509315,
0.0667125933533414));
#72970=CARTESIAN_POINT('',(0.00314410192199668,-0.0320197221621831,0.071272436175507));
#72971=CARTESIAN_POINT('Ctrl Pts',(0.00314397158350144,-0.0320197392094748,
0.0712725674262431));
#72972=CARTESIAN_POINT('Ctrl Pts',(0.00312933032213814,-0.0319792716576045,
0.0712979063270771));
#72973=CARTESIAN_POINT('Ctrl Pts',(0.00311481558176056,-0.0319386439829683,
0.0713234721993179));
#72974=CARTESIAN_POINT('Ctrl Pts',(0.00310041947948218,-0.0318979099381615,
0.0713492960579256));
#72975=CARTESIAN_POINT('Ctrl Pts',(0.00308602366175272,-0.0318571766984912,
0.071375119406107));
#72976=CARTESIAN_POINT('Ctrl Pts',(0.00307181809017675,-0.0318163871833557,
0.0714010686117907));
#72977=CARTESIAN_POINT('Ctrl Pts',(0.00305784853744171,-0.0317755399638303,
0.0714270527295668));
#72978=CARTESIAN_POINT('',(0.00314537000600163,-0.0321934096636183,0.0712728639074129));
#72979=CARTESIAN_POINT('Origin',(0.00113569280887835,-0.0324113643887189,
0.0701357262204479));
#72980=CARTESIAN_POINT('',(0.00311409678760076,-0.0321934096636663,0.0713269770833937));
#72981=CARTESIAN_POINT('Ctrl Pts',(0.00308478290689466,-0.0321934096636618,
0.071380566157171));
#72982=CARTESIAN_POINT('Ctrl Pts',(0.00304659025583153,-0.0320835708272592,
0.0714500578844942));
#72983=CARTESIAN_POINT('Ctrl Pts',(0.00300985788574346,-0.0319739230346488,
0.0715202996987203));
#72984=CARTESIAN_POINT('Ctrl Pts',(0.00297462589591431,-0.0318646057455572,
0.0715911981234695));
#72985=CARTESIAN_POINT('Ctrl Pts',(0.00297531271766522,-0.0321934096636618,
0.0714098482751716));
#72986=CARTESIAN_POINT('Ctrl Pts',(0.00293752388983048,-0.0320835708272592,
0.0714808496817204));
#72987=CARTESIAN_POINT('Ctrl Pts',(0.00290122635147,-0.0319739230346488,
0.0715525919423959));
#72988=CARTESIAN_POINT('Ctrl Pts',(0.00286645949819773,-0.0318646057455572,
0.0716249797037988));
#72989=CARTESIAN_POINT('Ctrl Pts',(0.00286584252843579,-0.0321934096636618,
0.0714391303931721));
#72990=CARTESIAN_POINT('Ctrl Pts',(0.00282845752382942,-0.0320835708272592,
0.0715116414789465));
#72991=CARTESIAN_POINT('Ctrl Pts',(0.00279259481719655,-0.0319739230346488,
0.0715848841860716));
#72992=CARTESIAN_POINT('Ctrl Pts',(0.00275829310048115,-0.0318646057455572,
0.0716587612841281));
#72993=CARTESIAN_POINT('Ctrl Pts',(0.00275637233920636,-0.0321934096636618,
0.0714684125111727));
#72994=CARTESIAN_POINT('Ctrl Pts',(0.00271939115782836,-0.0320835708272592,
0.0715424332761726));
#72995=CARTESIAN_POINT('Ctrl Pts',(0.00268396328292309,-0.0319739230346488,
0.0716171764297472));
#72996=CARTESIAN_POINT('Ctrl Pts',(0.00265012670276457,-0.0318646057455572,
0.0716925428644575));
#72997=CARTESIAN_POINT('',(0.00275065666655781,-0.0321763980308258,0.0714798835131076));
#72998=CARTESIAN_POINT('',(0.00275637233919176,-0.0321934096636184,0.0714684125112019));
#72999=CARTESIAN_POINT('Origin',(0.0172862519340763,-0.032638623111625,
0.0793882690510444));
#73000=CARTESIAN_POINT('Ctrl Pts',(0.00275065666939444,-0.0321763980306269,
0.0714798835145151));
#73001=CARTESIAN_POINT('Ctrl Pts',(0.00278909143633438,-0.0321259596175033,
0.0714989832553213));
#73002=CARTESIAN_POINT('Ctrl Pts',(0.00282686027106803,-0.0320749164631834,
0.0715177520683285));
#73003=CARTESIAN_POINT('Ctrl Pts',(0.0029010964713076,-0.0319716057793887,
0.0715546429433331));
#73004=CARTESIAN_POINT('Ctrl Pts',(0.00293753491184741,-0.0319193786690067,
0.0715727506313821));
#73005=CARTESIAN_POINT('Ctrl Pts',(0.00297332030108458,-0.031866561752526,
0.0715905337926576));
#73006=CARTESIAN_POINT('',(0.00291959795419583,-0.0321934096636663,0.0714247513852882));
#73007=CARTESIAN_POINT('Origin',(0.00812378219310841,-0.0315241814719618,
0.07415));
#73008=CARTESIAN_POINT('',(0.00275065666622462,-0.0322104233323614,0.0714798835129422));
#73009=CARTESIAN_POINT('',(0.00274496550589061,-0.0321934096636183,0.0714913666959626));
#73010=CARTESIAN_POINT('Origin',(0.0173118880729296,-0.0326387230595964,
0.0793508786892778));
#73011=CARTESIAN_POINT('Origin',(0.0178322963308996,-0.0326386244950934,
0.0782894597796565));
#73012=CARTESIAN_POINT('Origin',(0.0178179710295711,-0.0326387241904305,
0.0783324713134188));
#73013=CARTESIAN_POINT('Ctrl Pts',(0.00304704941301366,-0.0327445246967097,
0.0714472404325372));
#73014=CARTESIAN_POINT('Ctrl Pts',(0.00294511316949499,-0.032443687833936,
0.0716387125394833));
#73015=CARTESIAN_POINT('Ctrl Pts',(0.00285788897772951,-0.0321434074405927,
0.0718373189488763));
#73016=CARTESIAN_POINT('Ctrl Pts',(0.00293438979343578,-0.0327445246967097,
0.07167041706688));
#73017=CARTESIAN_POINT('Ctrl Pts',(0.00284087079428464,-0.032443687833936,
0.0718661382008406));
#73018=CARTESIAN_POINT('Ctrl Pts',(0.00276235998846516,-0.0321434074405927,
0.0720683475449638));
#73019=CARTESIAN_POINT('',(0.00291890946840458,-0.0326943950436612,0.0717030784811042));
#73020=CARTESIAN_POINT('',(0.00282277334565379,-0.0323666188837389,0.0719189844914907));
#73021=CARTESIAN_POINT('Origin',(0.0181646907621997,-0.0326395579109636,
0.0787864541573588));
#73022=CARTESIAN_POINT('Origin',(-0.00735700719535952,-0.0321933825603006,
0.0676346595754701));
#73023=CARTESIAN_POINT('',(0.00287251438693947,-0.0321934096532689,0.0718042993744971));
#73024=CARTESIAN_POINT('',(0.00284826994513973,-0.0321934096584275,0.0718619054278915));
#73025=CARTESIAN_POINT('',(0.00297332029857321,-0.0325210109756239,0.0715905337914046));
#73026=CARTESIAN_POINT('Origin',(0.0179374475416283,-0.0326393129159266,
0.0792101816038873));
#73027=CARTESIAN_POINT('',(0.00297453689523271,-0.0326943950436593,0.0715911383659319));
#73028=CARTESIAN_POINT('Origin',(-0.00693212286675309,-0.0326943765538135,
0.0666681302351314));
#73029=CARTESIAN_POINT('',(0.00294672318182864,-0.0326943950436702,0.0716471084235281));
#73030=CARTESIAN_POINT('Ctrl Pts',(0.00285944568442008,-0.0325229783203769,
0.0712713264993541));
#73031=CARTESIAN_POINT('Ctrl Pts',(0.00281976323316612,-0.032413025309245,
0.071343895263003));
#73032=CARTESIAN_POINT('Ctrl Pts',(0.00278158797863065,-0.032303122220807,
0.0714172739026568));
#73033=CARTESIAN_POINT('Ctrl Pts',(0.00274496550390364,-0.0321934096576658,
0.0714913666999825));
#73034=CARTESIAN_POINT('Ctrl Pts',(0.00289784342383241,-0.0325229783203769,
0.0713779414881895));
#73035=CARTESIAN_POINT('Ctrl Pts',(0.00285963065786802,-0.032413025309245,
0.0714499809398402));
#73036=CARTESIAN_POINT('Ctrl Pts',(0.00282291391621693,-0.032303122220807,
0.0715227999454484));
#73037=CARTESIAN_POINT('Ctrl Pts',(0.00278773693901311,-0.0321934096576658,
0.0715963035694566));
#73038=CARTESIAN_POINT('Ctrl Pts',(0.00293624116324473,-0.0325229783203769,
0.0714845564770249));
#73039=CARTESIAN_POINT('Ctrl Pts',(0.00289949808256992,-0.032413025309245,
0.0715560666166775));
#73040=CARTESIAN_POINT('Ctrl Pts',(0.00286423985380321,-0.032303122220807,
0.0716283259882399));
#73041=CARTESIAN_POINT('Ctrl Pts',(0.00283050837412259,-0.0321934096576658,
0.0717012404389307));
#73042=CARTESIAN_POINT('Ctrl Pts',(0.00297463890265705,-0.0325229783203769,
0.0715911714658602));
#73043=CARTESIAN_POINT('Ctrl Pts',(0.00293936550727183,-0.032413025309245,
0.0716621522935148));
#73044=CARTESIAN_POINT('Ctrl Pts',(0.0029055657913895,-0.032303122220807,
0.0717338520310315));
#73045=CARTESIAN_POINT('Ctrl Pts',(0.00287327980923206,-0.0321934096576658,
0.0718061773084048));
#73046=CARTESIAN_POINT('',(0.00280873994649101,-0.0321934096584275,0.0716478330347288));
#73047=CARTESIAN_POINT('Ctrl Pts',(0.00275065666933405,-0.0322104233328926,
0.071479883514485));
#73048=CARTESIAN_POINT('Ctrl Pts',(0.00278914351602082,-0.0322609421831371,
0.0714990091357568));
#73049=CARTESIAN_POINT('Ctrl Pts',(0.00282693779257923,-0.0323120888240734,
0.0715177905918107));
#73050=CARTESIAN_POINT('Ctrl Pts',(0.0029011745548487,-0.0324156524631814,
0.07155468174611));
#73051=CARTESIAN_POINT('Ctrl Pts',(0.00293758652535974,-0.0324680267167317,
0.0715727762801575));
#73052=CARTESIAN_POINT('Ctrl Pts',(0.00297332029861009,-0.0325210109755912,
0.0715905337914279));
#73053=CARTESIAN_POINT('Origin',(0.0124482184734131,-0.0262834582512208,
0.0675771287327571));
#73054=CARTESIAN_POINT('Origin',(0.000806663783453315,-0.0342770697900545,
0.0644400878420418));
#73055=CARTESIAN_POINT('Ctrl Pts',(0.00292083156457773,-0.0326943950436604,
0.071702432542149));
#73056=CARTESIAN_POINT('Ctrl Pts',(0.00288709949777823,-0.0325844576448134,
0.0717741389531789));
#73057=CARTESIAN_POINT('Ctrl Pts',(0.00285484804985231,-0.0324744968375323,
0.0718465480734288));
#73058=CARTESIAN_POINT('Ctrl Pts',(0.00282411726359269,-0.0323646534831895,
0.0719195665581506));
#73059=CARTESIAN_POINT('Ctrl Pts',(0.00281341618468038,-0.0326943950436604,
0.0717385305163707));
#73060=CARTESIAN_POINT('Ctrl Pts',(0.00278018161562046,-0.0325844576448134,
0.0718117173126535));
#73061=CARTESIAN_POINT('Ctrl Pts',(0.00274845831743698,-0.0324744968375323,
0.0718855966338565));
#73062=CARTESIAN_POINT('Ctrl Pts',(0.0027182856302444,-0.0323646534831895,
0.0719600732608581));
#73063=CARTESIAN_POINT('Ctrl Pts',(0.00270600080478302,-0.0326943950436604,
0.0717746284905924));
#73064=CARTESIAN_POINT('Ctrl Pts',(0.00267326373346269,-0.0325844576448134,
0.0718492956721281));
#73065=CARTESIAN_POINT('Ctrl Pts',(0.00264206858502164,-0.0324744968375323,
0.0719246451942843));
#73066=CARTESIAN_POINT('Ctrl Pts',(0.0026124539968961,-0.0323646534831895,
0.0720005799635657));
#73067=CARTESIAN_POINT('Ctrl Pts',(0.00259858542488566,-0.0326943950436604,
0.0718107264648142));
#73068=CARTESIAN_POINT('Ctrl Pts',(0.00256634585130493,-0.0325844576448134,
0.0718868740316027));
#73069=CARTESIAN_POINT('Ctrl Pts',(0.00253567885260631,-0.0324744968375323,
0.0719636937547119));
#73070=CARTESIAN_POINT('Ctrl Pts',(0.0025066223635478,-0.0323646534831895,
0.0720410866662732));
#73071=CARTESIAN_POINT('',(0.00259360130080664,-0.032677355999133,0.0718225337212939));
#73072=CARTESIAN_POINT('',(0.00259858542488537,-0.0326943950436594,0.0718107264648148));
#73073=CARTESIAN_POINT('Origin',(0.0179179980259199,-0.0326395670272396,
0.0782175454982723));
#73074=CARTESIAN_POINT('Ctrl Pts',(0.00259360130389114,-0.0326773559987412,
0.0718225337225895));
#73075=CARTESIAN_POINT('Ctrl Pts',(0.00263319134500798,-0.0326267922586193,
0.0718391958331907));
#73076=CARTESIAN_POINT('Ctrl Pts',(0.00267207968123486,-0.032575610957982,
0.0718555626199136));
#73077=CARTESIAN_POINT('Ctrl Pts',(0.00274848603988036,-0.0324719985462361,
0.0718877194745789));
#73078=CARTESIAN_POINT('Ctrl Pts',(0.00278597341774083,-0.0324196091621768,
0.0719034966452622));
#73079=CARTESIAN_POINT('Ctrl Pts',(0.00282277334569873,-0.0323666188837757,
0.0719189844915097));
#73080=CARTESIAN_POINT('',(0.00275874744665497,-0.0326943950436703,0.0717569024729695));
#73081=CARTESIAN_POINT('Origin',(0.00812378219310841,-0.0315241814719618,
0.07415));
#73082=CARTESIAN_POINT('',(0.00259360130084671,-0.0327114338380053,0.0718225337213109));
#73083=CARTESIAN_POINT('',(0.00258864240555084,-0.0326943950436593,0.071834351595725));
#73084=CARTESIAN_POINT('Origin',(0.0179348591208374,-0.0326395665215589,
0.078175488213683));
#73085=CARTESIAN_POINT('Origin',(0.0178790229887526,-0.0326395681402186,
0.0783101586361176));
#73086=CARTESIAN_POINT('Origin',(0.0178607309245503,-0.0326395676290809,
0.0783516136817013));
#73087=CARTESIAN_POINT('Ctrl Pts',(0.00288734328600302,-0.0332451089994434,
0.0717713801118816));
#73088=CARTESIAN_POINT('Ctrl Pts',(0.00279763216917186,-0.0329451141710254,
0.071968875636459));
#73089=CARTESIAN_POINT('Ctrl Pts',(0.00272305208243469,-0.0326442513127493,
0.0721725675051566));
#73090=CARTESIAN_POINT('Ctrl Pts',(0.00278892091855253,-0.0332451089994434,
0.0720011909853959));
#73091=CARTESIAN_POINT('Ctrl Pts',(0.00270787726062302,-0.0329451141710254,
0.0722023985702943));
#73092=CARTESIAN_POINT('Ctrl Pts',(0.00264221961700992,-0.0326442513127493,
0.0724091390853039));
#73093=CARTESIAN_POINT('',(0.00277553662236751,-0.0331951640388616,0.0720347235842445));
#73094=CARTESIAN_POINT('',(0.0026931470528567,-0.0328677532092642,0.0722562399905309));
#73095=CARTESIAN_POINT('Origin',(0.0186306846361962,-0.0326401908901966,
0.0774795677200636));
#73096=CARTESIAN_POINT('Origin',(-0.00774627647633802,-0.0326944279134284,
0.0686158263327017));
#73097=CARTESIAN_POINT('',(0.00273558880092205,-0.0326943950436593,0.0721386579186026));
#73098=CARTESIAN_POINT('',(0.00271500931525608,-0.0326943950436693,0.0721976726182163));
#73099=CARTESIAN_POINT('',(0.00282277334565488,-0.0330220786163545,0.0719189844914881));
#73100=CARTESIAN_POINT('Origin',(0.0185023456661935,-0.0326396682763639,
0.0779430350420078));
#73101=CARTESIAN_POINT('',(0.0028240255031881,-0.0331951640388588,0.0719195114822879));
#73102=CARTESIAN_POINT('Origin',(-0.00734381359202158,-0.033195202656006,
0.0676402104103637));
#73103=CARTESIAN_POINT('',(0.0027997810627878,-0.0331951640388701,0.0719771175332762));
#73104=CARTESIAN_POINT('Ctrl Pts',(0.00268907983816847,-0.0330240426238172,
0.0716075581986534));
#73105=CARTESIAN_POINT('Ctrl Pts',(0.00265405522537389,-0.0329142774063519,
0.0716824265183666));
#73106=CARTESIAN_POINT('Ctrl Pts',(0.0026205608888353,-0.0328043479726691,
0.0717580562192506));
#73107=CARTESIAN_POINT('Ctrl Pts',(0.00258864240555083,-0.0326943950436593,
0.0718343515957249));
#73108=CARTESIAN_POINT('Ctrl Pts',(0.00273409622464781,-0.0330240426238172,
0.0717115517606312));
#73109=CARTESIAN_POINT('Ctrl Pts',(0.00270050422448549,-0.0329142774063519,
0.0717857999357634));
#73110=CARTESIAN_POINT('Ctrl Pts',(0.00266843039466803,-0.0328043479726691,
0.0718607795667967));
#73111=CARTESIAN_POINT('Ctrl Pts',(0.00263791846948381,-0.0326943950436593,
0.0719363957308223));
#73112=CARTESIAN_POINT('Ctrl Pts',(0.00277911261112714,-0.0330240426238172,
0.071815545322609));
#73113=CARTESIAN_POINT('Ctrl Pts',(0.00274695322359709,-0.0329142774063519,
0.0718891733531601));
#73114=CARTESIAN_POINT('Ctrl Pts',(0.00271629990050076,-0.0328043479726691,
0.0719635029143427));
#73115=CARTESIAN_POINT('Ctrl Pts',(0.0026871945334168,-0.0326943950436593,
0.0720384398659197));
#73116=CARTESIAN_POINT('Ctrl Pts',(0.00282412899760648,-0.0330240426238172,
0.0719195388845869));
#73117=CARTESIAN_POINT('Ctrl Pts',(0.00279340222270869,-0.0329142774063519,
0.0719925467705569));
#73118=CARTESIAN_POINT('Ctrl Pts',(0.00276416940633348,-0.0328043479726691,
0.0720662262618888));
#73119=CARTESIAN_POINT('Ctrl Pts',(0.00273647059734978,-0.0326943950436593,
0.072140484001017));
#73120=CARTESIAN_POINT('',(0.00266211560324645,-0.0326943950436693,0.0719865047571738));
#73121=CARTESIAN_POINT('Ctrl Pts',(0.00259360130389673,-0.0327114338383323,
0.0718225337225918));
#73122=CARTESIAN_POINT('Ctrl Pts',(0.00263318475991938,-0.0327619876831079,
0.0718391930617494));
#73123=CARTESIAN_POINT('Ctrl Pts',(0.00267206987969294,-0.0328131562604566,
0.0718555584947757));
#73124=CARTESIAN_POINT('Ctrl Pts',(0.00274847616811621,-0.0329167375858769,
0.0718877153198868));
#73125=CARTESIAN_POINT('Ctrl Pts',(0.0027859668925906,-0.032969108892062,
0.0719034938990468));
#73126=CARTESIAN_POINT('Ctrl Pts',(0.00282277334569761,-0.0330220786163187,
0.0719189844915091));
#73127=CARTESIAN_POINT('Ctrl Pts',(0.00277741466668486,-0.0331951640388604,
0.0720339581082862));
#73128=CARTESIAN_POINT('Ctrl Pts',(0.00274827046695098,-0.0330855618127442,
0.072107593513923));
#73129=CARTESIAN_POINT('Ctrl Pts',(0.00272062717571139,-0.0329757224171941,
0.0721818843631614));
#73130=CARTESIAN_POINT('Ctrl Pts',(0.00269452485838531,-0.0328657861694599,
0.0722567372584769));
#73131=CARTESIAN_POINT('Ctrl Pts',(0.00267247775712366,-0.0331951640388604,
0.0720767295596433));
#73132=CARTESIAN_POINT('Ctrl Pts',(0.00264392264767487,-0.0330855618127442,
0.072151810259092));
#73133=CARTESIAN_POINT('Ctrl Pts',(0.00261689874314343,-0.0329757224171941,
0.0722275352685439));
#73134=CARTESIAN_POINT('Ctrl Pts',(0.00259144540587207,-0.0328657861694599,
0.0723038093150394));
#73135=CARTESIAN_POINT('Ctrl Pts',(0.00256754084756247,-0.0331951640388604,
0.0721195010110005));
#73136=CARTESIAN_POINT('Ctrl Pts',(0.00253957482839877,-0.0330855618127442,
0.072196027004261));
#73137=CARTESIAN_POINT('Ctrl Pts',(0.00251317031057548,-0.0329757224171941,
0.0722731861739263));
#73138=CARTESIAN_POINT('Ctrl Pts',(0.00248836595335883,-0.0328657861694599,
0.0723508813716019));
#73139=CARTESIAN_POINT('Ctrl Pts',(0.00246260393800127,-0.0331951640388604,
0.0721622724623576));
#73140=CARTESIAN_POINT('Ctrl Pts',(0.00243522700912267,-0.0330855618127442,
0.07224024374943));
#73141=CARTESIAN_POINT('Ctrl Pts',(0.00240944187800752,-0.0329757224171941,
0.0723188370793087));
#73142=CARTESIAN_POINT('Ctrl Pts',(0.00238528650084559,-0.0328657861694599,
0.0723979534281644));
#73143=CARTESIAN_POINT('',(0.00245837103251906,-0.0331781648278993,0.0721743693755846));
#73144=CARTESIAN_POINT('',(0.00246260393800087,-0.0331951640388588,0.0721622724623588));
#73145=CARTESIAN_POINT('Origin',(0.0182793365849877,-0.0326412091099719,
0.0769370925964116));
#73146=CARTESIAN_POINT('Ctrl Pts',(0.00245837103582962,-0.0331781648273345,
0.0721743693767361));
#73147=CARTESIAN_POINT('Ctrl Pts',(0.00249895721972424,-0.0331276810207545,
0.0721885225080019));
#73148=CARTESIAN_POINT('Ctrl Pts',(0.00253881023828218,-0.0330765665169234,
0.0722024199713469));
#73149=CARTESIAN_POINT('Ctrl Pts',(0.00261708542752709,-0.0329730612715178,
0.0722297159356858));
#73150=CARTESIAN_POINT('Ctrl Pts',(0.0026554751898153,-0.0329207135598908,
0.0722431031352889));
#73151=CARTESIAN_POINT('Ctrl Pts',(0.00269314705289973,-0.0328677532092986,
0.072256239990546));
#73152=CARTESIAN_POINT('',(0.00261907028019419,-0.0331951640388702,0.0720984980233116));
#73153=CARTESIAN_POINT('Origin',(0.00812378219310841,-0.0315241814719618,
0.07415));
#73154=CARTESIAN_POINT('',(0.00245837103295193,-0.0332121607144419,0.0721743693757357));
#73155=CARTESIAN_POINT('',(0.00245416397318748,-0.0331951640388587,0.0721864753018193));
#73156=CARTESIAN_POINT('Origin',(0.0182866392920863,-0.0326413646240691,
0.0768923383319838));
#73157=CARTESIAN_POINT('Origin',(0.0178102809754642,-0.0326412100744096,
0.0782821863608264));
#73158=CARTESIAN_POINT('Origin',(0.0177881662202434,-0.0326413658440793,
0.0783217750389539));
#73159=CARTESIAN_POINT('Ctrl Pts',(0.00274832883103548,-0.0337436976235975,
0.0721048530243088));
#73160=CARTESIAN_POINT('Ctrl Pts',(0.00272993446918561,-0.0336723290703325,
0.0721532006665195));
#73161=CARTESIAN_POINT('Ctrl Pts',(0.00271241270480488,-0.033601104548885,
0.0722018713438128));
#73162=CARTESIAN_POINT('Ctrl Pts',(0.00265646918200321,-0.0333736987606857,
0.0723572671752923));
#73163=CARTESIAN_POINT('Ctrl Pts',(0.00260953535851614,-0.0331450831799192,
0.072515617288641));
#73164=CARTESIAN_POINT('Ctrl Pts',(0.00266452976866446,-0.0337436976235975,
0.0723403901066244));
#73165=CARTESIAN_POINT('Ctrl Pts',(0.00264825386302956,-0.0336723290703325,
0.0723894914503022));
#73166=CARTESIAN_POINT('Ctrl Pts',(0.00263286376886128,-0.033601104548885,
0.0724388776027813));
#73167=CARTESIAN_POINT('Ctrl Pts',(0.00258372624678785,-0.0333736987606857,
0.0725965578048016));
#73168=CARTESIAN_POINT('Ctrl Pts',(0.00254371829863148,-0.0331450831799192,
0.0727567979566642));
#73169=CARTESIAN_POINT('Ctrl Pts',(0.00266369177804075,-0.0337436976235975,
0.0723427454774475));
#73170=CARTESIAN_POINT('Ctrl Pts',(0.002647437056968,-0.0336723290703325,
0.07239185435814));
#73171=CARTESIAN_POINT('Ctrl Pts',(0.00263206827950185,-0.033601104548885,
0.072441247665371));
#73172=CARTESIAN_POINT('Ctrl Pts',(0.0025829988174357,-0.0333736987606857,
0.0725989507110966));
#73173=CARTESIAN_POINT('Ctrl Pts',(0.00254306012803263,-0.0331450831799192,
0.0727592097633445));
#73174=CARTESIAN_POINT('',(0.00265327085821316,-0.0336938721132548,0.0723747167170325));
#73175=CARTESIAN_POINT('',(0.00258495299398426,-0.0333679869945434,0.0726009693021799));
#73176=CARTESIAN_POINT('Ctrl Pts',(0.00265327085821043,-0.0336938721132646,
0.0723747167170381));
#73177=CARTESIAN_POINT('Ctrl Pts',(0.00264634109475723,-0.0336629187933929,
0.072396070689041));
#73178=CARTESIAN_POINT('Ctrl Pts',(0.0026395385836991,-0.0336319952301037,
0.0724174584080862));
#73179=CARTESIAN_POINT('Ctrl Pts',(0.00263286376885911,-0.0336011045488947,
0.0724388776027873));
#73180=CARTESIAN_POINT('Ctrl Pts',(0.00261611437443248,-0.0335235892595451,
0.0724926256915283));
#73181=CARTESIAN_POINT('Ctrl Pts',(0.00260013943773531,-0.0334458668660366,
0.0725466675256716));
#73182=CARTESIAN_POINT('Ctrl Pts',(0.00258495299366919,-0.0333679869945382,
0.0726009693020844));
#73183=CARTESIAN_POINT('Ctrl Pts',(0.0025849403544701,-0.0333679692460736,
0.0726010119438432));
#73184=CARTESIAN_POINT('Ctrl Pts',(0.0025853784171049,-0.0333391895375831,
0.0726011283008377));
#73185=CARTESIAN_POINT('Ctrl Pts',(0.00258570760002757,-0.0333104081062015,
0.0726012123777164));
#73186=CARTESIAN_POINT('Ctrl Pts',(0.00258614470042685,-0.0332532698303069,
0.0726013183016452));
#73187=CARTESIAN_POINT('Ctrl Pts',(0.00258625584754641,-0.0332249171635303,
0.0726013410562512));
#73188=CARTESIAN_POINT('Ctrl Pts',(0.00258626124055257,-0.033196098535,
0.0726013354003529));
#73189=CARTESIAN_POINT('Ctrl Pts',(0.0025862612993336,-0.0331956312575113,
0.0726013353006517));
#73190=CARTESIAN_POINT('Ctrl Pts',(0.00258626132929588,-0.0331951640388587,
0.0726013351935164));
#73191=CARTESIAN_POINT('',(0.00261992795552372,-0.0331951640388587,0.0724809543051726));
#73192=CARTESIAN_POINT('',(0.00260309464241977,-0.0331951640388687,0.0725411447493546));
#73193=CARTESIAN_POINT('',(0.00269314705329479,-0.0335216366567741,0.0722562399905133));
#73194=CARTESIAN_POINT('Origin',(0.0187759744413429,-0.0326434571526037,
0.0765821304451633));
#73195=CARTESIAN_POINT('',(0.00269442982957012,-0.0336938721132328,0.0722566873178099));
#73196=CARTESIAN_POINT('Origin',(-0.00761715546663589,-0.033693886789626,
0.0686608510278571));
#73197=CARTESIAN_POINT('',(0.00267385034390164,-0.0336938721132538,0.0723157020174312));
#73198=CARTESIAN_POINT('Ctrl Pts',(0.00254016238846795,-0.0335235895815171,
0.0719538238055078));
#73199=CARTESIAN_POINT('Ctrl Pts',(0.00250992769927774,-0.0334144449262748,
0.0720306933252545));
#73200=CARTESIAN_POINT('Ctrl Pts',(0.00248124634051988,-0.0333049234473147,
0.0721082757846909));
#73201=CARTESIAN_POINT('Ctrl Pts',(0.00245416397318736,-0.0331951640388587,
0.0721864753018191));
#73202=CARTESIAN_POINT('Ctrl Pts',(0.00259161984448248,-0.0335235895815171,
0.0720547856929032));
#73203=CARTESIAN_POINT('Ctrl Pts',(0.00256277509444792,-0.0334144449262748,
0.0721309467994575));
#73204=CARTESIAN_POINT('Ctrl Pts',(0.00253547063643401,-0.0333049234473147,
0.0722077913167236));
#73205=CARTESIAN_POINT('Ctrl Pts',(0.00250975028532488,-0.0331951640388587,
0.0722852241468193));
#73206=CARTESIAN_POINT('Ctrl Pts',(0.002643077300497,-0.0335235895815171,
0.0721557475802987));
#73207=CARTESIAN_POINT('Ctrl Pts',(0.0026156224896181,-0.0334144449262748,
0.0722312002736604));
#73208=CARTESIAN_POINT('Ctrl Pts',(0.00258969493234813,-0.0333049234473147,
0.0723073068487562));
#73209=CARTESIAN_POINT('Ctrl Pts',(0.0025653365974624,-0.0331951640388587,
0.0723839729918196));
#73210=CARTESIAN_POINT('Ctrl Pts',(0.00269453475651152,-0.0335235895815171,
0.0722567094676941));
#73211=CARTESIAN_POINT('Ctrl Pts',(0.00266846988478829,-0.0334144449262748,
0.0723314537478634));
#73212=CARTESIAN_POINT('Ctrl Pts',(0.00264391922826226,-0.0333049234473147,
0.0724068223807889));
#73213=CARTESIAN_POINT('Ctrl Pts',(0.00262092290959992,-0.0331951640388587,
0.0724827218368198));
#73214=CARTESIAN_POINT('',(0.0025370459643656,-0.0331951640388687,0.0723337148035059));
#73215=CARTESIAN_POINT('Ctrl Pts',(0.0024583710359038,-0.0332121607145976,
0.0721743693767619));
#73216=CARTESIAN_POINT('Ctrl Pts',(0.00249888882421,-0.0332625444109904,
0.0721884986572576));
#73217=CARTESIAN_POINT('Ctrl Pts',(0.00253870842744081,-0.0333135300747139,
0.0722023844680778));
#73218=CARTESIAN_POINT('Ctrl Pts',(0.00261698287199452,-0.0334167203140642,
0.0722296801727295));
#73219=CARTESIAN_POINT('Ctrl Pts',(0.00265540739701302,-0.0334688847587347,
0.072243079494721));
#73220=CARTESIAN_POINT('Ctrl Pts',(0.0026931470539036,-0.0335216366562431,
0.0722562399908959));
#73221=CARTESIAN_POINT('Ctrl Pts',(0.00265417123522845,-0.0336938721132389,
0.0723742819342105));
#73222=CARTESIAN_POINT('Ctrl Pts',(0.00264377736814366,-0.0336474569764957,
0.0724062973821562));
#73223=CARTESIAN_POINT('Ctrl Pts',(0.00263375899449409,-0.033601104548885,
0.0724384323097205));
#73224=CARTESIAN_POINT('Ctrl Pts',(0.00260839477578187,-0.0334837508592655,
0.0725197905580304));
#73225=CARTESIAN_POINT('Ctrl Pts',(0.00258545250874611,-0.0333660264659097,
0.0726018646741827));
#73226=CARTESIAN_POINT('Ctrl Pts',(0.00265327085821957,-0.0336938721132389,
0.0723747167170131));
#73227=CARTESIAN_POINT('Ctrl Pts',(0.0026428795360628,-0.0336474569764957,
0.0724067374351643));
#73228=CARTESIAN_POINT('Ctrl Pts',(0.00263286376886128,-0.033601104548885,
0.0724388776027813));
#73229=CARTESIAN_POINT('Ctrl Pts',(0.00260750614907625,-0.0334837508592655,
0.0725202491176999));
#73230=CARTESIAN_POINT('Ctrl Pts',(0.00258457087118706,-0.0333660264659097,
0.0726023362990952));
#73231=CARTESIAN_POINT('Ctrl Pts',(0.00234713869739755,-0.0336938721132389,
0.0725225447907597));
#73232=CARTESIAN_POINT('Ctrl Pts',(0.00233761266201098,-0.0336474569764957,
0.0725563574020336));
#73233=CARTESIAN_POINT('Ctrl Pts',(0.00232848309866109,-0.033601104548885,
0.0725902792107175));
#73234=CARTESIAN_POINT('Ctrl Pts',(0.00230536914327736,-0.0334837508592655,
0.0726761614311924));
#73235=CARTESIAN_POINT('Ctrl Pts',(0.00228481020609527,-0.0333660264659097,
0.0727626908529466));
#73236=CARTESIAN_POINT('',(0.00234549955260835,-0.0336769361243754,0.0725340019410606));
#73237=CARTESIAN_POINT('',(0.00234896453534305,-0.033693872113232,0.0725216631123868));
#73238=CARTESIAN_POINT('Ctrl Pts',(0.00234549955260829,-0.0336769361243751,
0.0725340019410609));
#73239=CARTESIAN_POINT('Ctrl Pts',(0.00234607489648189,-0.0336797586670061,
0.0725319446987896));
#73240=CARTESIAN_POINT('Ctrl Pts',(0.00234665131725535,-0.0336825812712917,
0.0725298878415841));
#73241=CARTESIAN_POINT('Ctrl Pts',(0.00234780631258848,-0.0336882266054485,
0.0725257748954517));
#73242=CARTESIAN_POINT('Ctrl Pts',(0.0023483848871579,-0.0336910493353204,
0.0725237188065247));
#73243=CARTESIAN_POINT('Ctrl Pts',(0.00234896453534645,-0.0336938721132312,
0.0725216631123867));
#73244=CARTESIAN_POINT('Ctrl Pts',(0.00234549955260836,-0.0336769361243754,
0.0725340019410606));
#73245=CARTESIAN_POINT('Ctrl Pts',(0.00238586447293965,-0.0336279007516211,
0.0725452906988046));
#73246=CARTESIAN_POINT('Ctrl Pts',(0.00242680412680003,-0.0335767878632072,
0.072556740190857));
#73247=CARTESIAN_POINT('Ctrl Pts',(0.00250703435245218,-0.0334733198857316,
0.0725791779802468));
#73248=CARTESIAN_POINT('Ctrl Pts',(0.00254637268890566,-0.0334209645014069,
0.0725901796358093));
#73249=CARTESIAN_POINT('Ctrl Pts',(0.00258495299593697,-0.0333679869844681,
0.0726009692951519));
#73250=CARTESIAN_POINT('',(0.00250111769678811,-0.0336938721132534,0.0724481899147197));
#73251=CARTESIAN_POINT('Origin',(0.00812378219310841,-0.0315241814719618,
0.07415));
#73252=CARTESIAN_POINT('',(0.00234549955386281,-0.0337108120655682,0.0725340019414152));
#73253=CARTESIAN_POINT('',(0.00234206093373597,-0.0336938721132327,0.0725463481428482));
#73254=CARTESIAN_POINT('Origin',(0.0178011120907627,-0.0345562513279639,
0.0780169232437248));
#73255=CARTESIAN_POINT('Ctrl Pts',(0.00234206093374247,-0.0336938721132293,
0.0725463481428547));
#73256=CARTESIAN_POINT('Ctrl Pts',(0.00234263179342879,-0.0336910493414198,
0.0725442899956516));
#73257=CARTESIAN_POINT('Ctrl Pts',(0.00234320377762032,-0.0336882266084981,
0.0725422320612115));
#73258=CARTESIAN_POINT('Ctrl Pts',(0.00234434998528453,-0.0336825812712737,
0.072538116655043));
#73259=CARTESIAN_POINT('Ctrl Pts',(0.00234492420873666,-0.0336797586669971,
0.0725360591833251));
#73260=CARTESIAN_POINT('Ctrl Pts',(0.00234549955260843,-0.0336769361243751,
0.0725340019410604));
#73261=CARTESIAN_POINT('Origin',(0.0184031252217066,-0.0345562515972652,
0.0758643098980786));
#73262=CARTESIAN_POINT('Ctrl Pts',(0.00263053551478968,-0.0342436276873911,
0.0724463668437305));
#73263=CARTESIAN_POINT('Ctrl Pts',(0.00256628193106721,-0.0339430054201811,
0.072653548057629));
#73264=CARTESIAN_POINT('Ctrl Pts',(0.00251781662296948,-0.0336441434784053,
0.0728649805346154));
#73265=CARTESIAN_POINT('Ctrl Pts',(0.00256168914869608,-0.0342436276873911,
0.0726867003159638));
#73266=CARTESIAN_POINT('Ctrl Pts',(0.00250649989130621,-0.0339430054201811,
0.0728964781133647));
#73267=CARTESIAN_POINT('Ctrl Pts',(0.0024672687440488,-0.0336441434784053,
0.0731098170350327));
#73268=CARTESIAN_POINT('Ctrl Pts',(0.00256100068503515,-0.0342436276873911,
0.0726891036506861));
#73269=CARTESIAN_POINT('Ctrl Pts',(0.0025059020709086,-0.0339430054201811,
0.0728989074139221));
#73270=CARTESIAN_POINT('Ctrl Pts',(0.00246676326525959,-0.0336441434784053,
0.0731122654000369));
#73271=CARTESIAN_POINT('',(0.00255259470306785,-0.0341934961088741,0.0727217160818602));
#73272=CARTESIAN_POINT('',(0.00249861816545665,-0.033866421289281,0.0729518119189903));
#73273=CARTESIAN_POINT('Origin',(0.0186290599892738,-0.0345610818076339,
0.0773693346343042));
#73274=CARTESIAN_POINT('Origin',(-0.00822703412941682,-0.0336938005044306,
0.0706672710820475));
#73275=CARTESIAN_POINT('',(0.0025259883083293,-0.0336938721132327,0.0728298376525857));
#73276=CARTESIAN_POINT('',(0.00251296760118384,-0.0336938721132427,0.0728909662971511));
#73277=CARTESIAN_POINT('',(0.00258495299593841,-0.0340203938281605,0.0726009692951467));
#73278=CARTESIAN_POINT('Origin',(0.0184257655862531,-0.0345589643247985,
0.0778054481328131));
#73279=CARTESIAN_POINT('',(0.0025862613292958,-0.0341934961088741,0.0726013351935164));
#73280=CARTESIAN_POINT('Origin',(-0.00802598527630373,-0.0341934220717649,
0.0696334335361931));
#73281=CARTESIAN_POINT('',(0.00256942801619183,-0.0341934961088841,0.0726615256376983));
#73282=CARTESIAN_POINT('Ctrl Pts',(0.00241328218214011,-0.0340223579322397,
0.0723087532417509));
#73283=CARTESIAN_POINT('Ctrl Pts',(0.00238788658717071,-0.0339125849573575,
0.0723875159305114));
#73284=CARTESIAN_POINT('Ctrl Pts',(0.00236413904203001,-0.0338030433565231,
0.0724667489034471));
#73285=CARTESIAN_POINT('Ctrl Pts',(0.00234206093373559,-0.0336938721132327,
0.0725463481428476));
#73286=CARTESIAN_POINT('Ctrl Pts',(0.00247097752000295,-0.0340223579322397,
0.0724062849177297));
#73287=CARTESIAN_POINT('Ctrl Pts',(0.00244692714121859,-0.0339125849573575,
0.0724842518373053));
#73288=CARTESIAN_POINT('Ctrl Pts',(0.00242450739642207,-0.0338030433565231,
0.0725626617573847));
#73289=CARTESIAN_POINT('Ctrl Pts',(0.00240373806790193,-0.0336938721132327,
0.0726414118633269));
#73290=CARTESIAN_POINT('Ctrl Pts',(0.0025286728578658,-0.0340223579322397,
0.0725038165937084));
#73291=CARTESIAN_POINT('Ctrl Pts',(0.00250596769526647,-0.0339125849573575,
0.0725809877440991));
#73292=CARTESIAN_POINT('Ctrl Pts',(0.00248487575081414,-0.0338030433565231,
0.0726585746113223));
#73293=CARTESIAN_POINT('Ctrl Pts',(0.00246541520206826,-0.0336938721132327,
0.0727364755838062));
#73294=CARTESIAN_POINT('Ctrl Pts',(0.00258636819572864,-0.0340223579322397,
0.0726013482696872));
#73295=CARTESIAN_POINT('Ctrl Pts',(0.00256500824931436,-0.0339125849573575,
0.072677723650893));
#73296=CARTESIAN_POINT('Ctrl Pts',(0.0025452441052062,-0.0338030433565231,
0.0727544874652599));
#73297=CARTESIAN_POINT('Ctrl Pts',(0.0025270923362346,-0.0336938721132327,
0.0728315393042854));
#73298=CARTESIAN_POINT('',(0.00243402462104263,-0.0336938721132427,0.072688092897727));
#73299=CARTESIAN_POINT('Ctrl Pts',(0.00234549955732709,-0.0337108120662685,
0.0725340019423802));
#73300=CARTESIAN_POINT('Ctrl Pts',(0.00238690986657648,-0.033761140899441,
0.0725455830614654));
#73301=CARTESIAN_POINT('Ctrl Pts',(0.00242756452955417,-0.0338121088781553,
0.0725569528508209));
#73302=CARTESIAN_POINT('Ctrl Pts',(0.00250739959868047,-0.0339153382773236,
0.0725792801277594));
#73303=CARTESIAN_POINT('Ctrl Pts',(0.00254654622973458,-0.0339675558473117,
0.072590228169545));
#73304=CARTESIAN_POINT('Ctrl Pts',(0.00258495299597539,-0.0340203938281304,
0.0726009692951626));
#73305=CARTESIAN_POINT('Ctrl Pts',(0.00255436207816171,-0.0341934961088741,
0.0727207212159088));
#73306=CARTESIAN_POINT('Ctrl Pts',(0.00252481286551814,-0.0340287516194401,
0.0728358645882933));
#73307=CARTESIAN_POINT('Ctrl Pts',(0.00250004786501172,-0.033864463329982,
0.0729521308642372));
#73308=CARTESIAN_POINT('Ctrl Pts',(0.00255259470306794,-0.0341934961088741,
0.0727217160818602));
#73309=CARTESIAN_POINT('Ctrl Pts',(0.00252306605849399,-0.0340287516194401,
0.0728368959933322));
#73310=CARTESIAN_POINT('Ctrl Pts',(0.00249832311867037,-0.033864463329982,
0.0729531979270476));
#73311=CARTESIAN_POINT('Ctrl Pts',(0.002258115699717,-0.0341934961088741,
0.0728874800641951));
#73312=CARTESIAN_POINT('Ctrl Pts',(0.00223201409486208,-0.0340287516194401,
0.073008748097023));
#73313=CARTESIAN_POINT('Ctrl Pts',(0.00221094689309027,-0.033864463329982,
0.0731309913077608));
#73314=CARTESIAN_POINT('',(0.00225543231674149,-0.0341764758832383,0.0729000121124188));
#73315=CARTESIAN_POINT('',(0.00225811569971695,-0.034193496108874,0.072887480064195));
#73316=CARTESIAN_POINT('Origin',(0.018343191126596,-0.0345621026071988,
0.0768503725182579));
#73317=CARTESIAN_POINT('Ctrl Pts',(0.00225543231791702,-0.0341764758837467,
0.0729000121110281));
#73318=CARTESIAN_POINT('Ctrl Pts',(0.00229741486488263,-0.0341260050044177,
0.0729089545895575));
#73319=CARTESIAN_POINT('Ctrl Pts',(0.00233866766410551,-0.034074926915576,
0.0729177415893458));
#73320=CARTESIAN_POINT('Ctrl Pts',(0.00241974570017303,-0.0339715436321982,
0.0729350116208483));
#73321=CARTESIAN_POINT('Ctrl Pts',(0.00245954017661583,-0.0339192778256753,
0.07294348810656));
#73322=CARTESIAN_POINT('Ctrl Pts',(0.00249861816420593,-0.0338664212878159,
0.0729518119155586));
#73323=CARTESIAN_POINT('',(0.0024053552014024,-0.0341934961088841,0.0728045980730376));
#73324=CARTESIAN_POINT('Origin',(0.00812378219310841,-0.0315241814719618,
0.07415));
#73325=CARTESIAN_POINT('',(0.0022554323172859,-0.034210518019037,0.0729000121133953));
#73326=CARTESIAN_POINT('',(0.00225277570667799,-0.0341934961088739,0.0729125498651185));
#73327=CARTESIAN_POINT('Origin',(0.0183576906715232,-0.0345621703957348,
0.0768074265873306));
#73328=CARTESIAN_POINT('Origin',(0.0185565663266295,-0.0345621038964406,
0.0758486461905739));
#73329=CARTESIAN_POINT('Origin',(0.0185523004742703,-0.0345621716491088,
0.0758937719971404));
#73330=CARTESIAN_POINT('Ctrl Pts',(0.00252630080736586,-0.0346945769586966,
0.0728283705554236));
#73331=CARTESIAN_POINT('Ctrl Pts',(0.00249861874949764,-0.0345275153362944,
0.0729456120441572));
#73332=CARTESIAN_POINT('Ctrl Pts',(0.00247461666853867,-0.0343603235965185,
0.0730637544327854));
#73333=CARTESIAN_POINT('Ctrl Pts',(0.00245436035880645,-0.034193496108874,
0.073182447253507));
#73334=CARTESIAN_POINT('Ctrl Pts',(0.00250883569810389,-0.0346945769586966,
0.0729103644474174));
#73335=CARTESIAN_POINT('Ctrl Pts',(0.00248287103513205,-0.0345275153362944,
0.0730279717498572));
#73336=CARTESIAN_POINT('Ctrl Pts',(0.00246059829778009,-0.0343603235965185,
0.073146426036321));
#73337=CARTESIAN_POINT('Ctrl Pts',(0.0024420781520247,-0.034193496108874,
0.073265375992569));
#73338=CARTESIAN_POINT('Ctrl Pts',(0.00249137058884199,-0.0346945769586966,
0.0729923583394103));
#73339=CARTESIAN_POINT('Ctrl Pts',(0.00246712332076652,-0.0345275153362944,
0.0731103314555584));
#73340=CARTESIAN_POINT('Ctrl Pts',(0.00244657992702156,-0.0343603235965185,
0.0732290976398585));
#73341=CARTESIAN_POINT('Ctrl Pts',(0.00242979594524296,-0.034193496108874,
0.0733483047316324));
#73342=CARTESIAN_POINT('Ctrl Pts',(0.00247390547957996,-0.0346945769586966,
0.0730743522314051));
#73343=CARTESIAN_POINT('Ctrl Pts',(0.00245137560640087,-0.0345275153362944,
0.0731926911612572));
#73344=CARTESIAN_POINT('Ctrl Pts',(0.00243256155626293,-0.0343603235965185,
0.0733117692433922));
#73345=CARTESIAN_POINT('Ctrl Pts',(0.00241751373846119,-0.034193496108874,
0.0734312334706929));
#73346=CARTESIAN_POINT('',(0.00247390547970629,-0.0346945769586966,0.0730743522308127));
#73347=CARTESIAN_POINT('',(0.00243448329133996,-0.034366772783144,0.0733073832385791));
#73348=CARTESIAN_POINT('Origin',(0.0190240764866805,-0.0345626457061231,
0.0760389916498902));
#73349=CARTESIAN_POINT('Origin',(-0.0084984381877856,-0.0341934771028977,
0.0716881604615297));
#73350=CARTESIAN_POINT('',(0.00245414059620934,-0.0341934961088739,0.0731839310776592));
#73351=CARTESIAN_POINT('',(0.00244498388180492,-0.0341934961088839,0.073245756675775));
#73352=CARTESIAN_POINT('',(0.00249861816742679,-0.0345211942962711,0.072951811916287));
#73353=CARTESIAN_POINT('Origin',(0.0189206569525864,-0.0345625596115329,
0.0765085608031198));
#73354=CARTESIAN_POINT('',(0.00249994689401839,-0.0346945769586885,0.0729520949416963));
#73355=CARTESIAN_POINT('Origin',(-0.00832086656064614,-0.0346945685853893,
0.0706472063572769));
#73356=CARTESIAN_POINT('',(0.00248692618687234,-0.0346945769587026,0.0730132235862645));
#73357=CARTESIAN_POINT('Ctrl Pts',(0.00230893747175623,-0.0345231616327841,
0.0726709527165808));
#73358=CARTESIAN_POINT('Ctrl Pts',(0.00228855088728632,-0.0344132092796988,
0.0727511021644182));
#73359=CARTESIAN_POINT('Ctrl Pts',(0.00226982318277795,-0.0343032738558979,
0.0728316691573314));
#73360=CARTESIAN_POINT('Ctrl Pts',(0.00225277570667794,-0.0341934961088739,
0.0729125498651185));
#73361=CARTESIAN_POINT('Ctrl Pts',(0.00237264293230449,-0.0345231616327841,
0.072764669046187));
#73362=CARTESIAN_POINT('Ctrl Pts',(0.00235354809549615,-0.0344132092796988,
0.0728439404039408));
#73363=CARTESIAN_POINT('Ctrl Pts',(0.00233609390940038,-0.0343032738558979,
0.0729236026332944));
#73364=CARTESIAN_POINT('Ctrl Pts',(0.00232030012063065,-0.0341934961088739,
0.0730035531049446));
#73365=CARTESIAN_POINT('Ctrl Pts',(0.00243634839285275,-0.0345231616327841,
0.0728583853757931));
#73366=CARTESIAN_POINT('Ctrl Pts',(0.00241854530370599,-0.0344132092796988,
0.0729367786434633));
#73367=CARTESIAN_POINT('Ctrl Pts',(0.00240236463602281,-0.0343032738558979,
0.0730155361092575));
#73368=CARTESIAN_POINT('Ctrl Pts',(0.00238782453458337,-0.0341934961088739,
0.0730945563447708));
#73369=CARTESIAN_POINT('Ctrl Pts',(0.002500053853401,-0.0345231616327841,
0.0729521017053992));
#73370=CARTESIAN_POINT('Ctrl Pts',(0.00248354251191583,-0.0344132092796988,
0.0730296168829859));
#73371=CARTESIAN_POINT('Ctrl Pts',(0.00246863536264524,-0.0343032738558979,
0.0731074695852204));
#73372=CARTESIAN_POINT('Ctrl Pts',(0.00245534894853608,-0.0341934961088739,
0.073185559584597));
#73373=CARTESIAN_POINT('',(0.00235345815145366,-0.0341934961088839,0.0730482404713988));
#73374=CARTESIAN_POINT('Ctrl Pts',(0.00225543232065939,-0.0342105180195389,
0.0729000121141101));
#73375=CARTESIAN_POINT('Ctrl Pts',(0.00229746206161806,-0.0342610556241343,
0.0729089646592356));
#73376=CARTESIAN_POINT('Ctrl Pts',(0.00233873760060634,-0.0343122189870239,
0.0729177565555677));
#73377=CARTESIAN_POINT('Ctrl Pts',(0.00241981645595705,-0.0344158119695192,
0.0729350267574461));
#73378=CARTESIAN_POINT('Ctrl Pts',(0.00245958661048381,-0.03446819904501,
0.0729434979993555));
#73379=CARTESIAN_POINT('Ctrl Pts',(0.00249861816745104,-0.0345211942962529,
0.072951811916289));
#73380=CARTESIAN_POINT('Ctrl Pts',(0.0024756064843927,-0.0346945769586932,
0.0730732486226806));
#73381=CARTESIAN_POINT('Ctrl Pts',(0.00245334541155146,-0.034529677707698,
0.0731900206589373));
#73382=CARTESIAN_POINT('Ctrl Pts',(0.00243592965608153,-0.0343648066251421,
0.073307612985545));
#73383=CARTESIAN_POINT('Ctrl Pts',(0.00247390547970809,-0.0346945769586932,
0.0730743522308038));
#73384=CARTESIAN_POINT('Ctrl Pts',(0.00245166722318391,-0.034529677707698,
0.0731911594341289));
#73385=CARTESIAN_POINT('Ctrl Pts',(0.00243427571802203,-0.0343648066251421,
0.0733087859547356));
#73386=CARTESIAN_POINT('Ctrl Pts',(0.00219041596997284,-0.0346945769586932,
0.0732582796053955));
#73387=CARTESIAN_POINT('Ctrl Pts',(0.0021719802817755,-0.034529677707698,
0.0733809477537435));
#73388=CARTESIAN_POINT('Ctrl Pts',(0.0021586303339369,-0.0343648066251421,
0.0735042730476258));
#73389=CARTESIAN_POINT('',(0.00218852477561365,-0.0346775396664969,0.0732709554155673));
#73390=CARTESIAN_POINT('',(0.00219041596997232,-0.0346945769586887,0.0732582796053988));
#73391=CARTESIAN_POINT('Origin',(0.0186326590362704,-0.0345626618789612,
0.0755520402302187));
#73392=CARTESIAN_POINT('Ctrl Pts',(0.00218852477677931,-0.0346775396670097,
0.0732709554141674));
#73393=CARTESIAN_POINT('Ctrl Pts',(0.00223101942578306,-0.0346269749928186,
0.0732772490946446));
#73394=CARTESIAN_POINT('Ctrl Pts',(0.00227275885531511,-0.0345757902890784,
0.0732834308868437));
#73395=CARTESIAN_POINT('Ctrl Pts',(0.00235476162507108,-0.0344721681087817,
0.0732955759562511));
#73396=CARTESIAN_POINT('Ctrl Pts',(0.00239499281551225,-0.034419771428957,
0.073301534477595));
#73397=CARTESIAN_POINT('Ctrl Pts',(0.00243448329126564,-0.0343667727830599,
0.0733073832383186));
#73398=CARTESIAN_POINT('',(0.00233216072484931,-0.0346945769587026,0.0731663159181158));
#73399=CARTESIAN_POINT('Origin',(0.00812378219310841,-0.0315241814719618,
0.07415));
#73400=CARTESIAN_POINT('',(0.00218852477667093,-0.0347116136489613,0.0732709554164708));
#73401=CARTESIAN_POINT('',(0.00218666066001419,-0.0346945769586885,0.0732836352377339));
#73402=CARTESIAN_POINT('Origin',(0.0186374449334779,-0.0345626683579165,
0.0755069803020974));
#73403=CARTESIAN_POINT('Origin',(0.0185879136793979,-0.0345626628398701,
0.0758541774810751));
#73404=CARTESIAN_POINT('Origin',(0.0185794279522539,-0.0345626695130172,
0.07589868918301));
#73405=CARTESIAN_POINT('Ctrl Pts',(0.00246070148270513,-0.0352450361874068,
0.0731458687869191));
#73406=CARTESIAN_POINT('Ctrl Pts',(0.00242283005256249,-0.0349452760959492,
0.073359455380705));
#73407=CARTESIAN_POINT('Ctrl Pts',(0.00240115442733529,-0.034644428984174,
0.073575287828537));
#73408=CARTESIAN_POINT('Ctrl Pts',(0.00246031588138545,-0.0352450361874068,
0.0731483641699803));
#73409=CARTESIAN_POINT('Ctrl Pts',(0.00242253856615933,-0.0349452760959492,
0.0733619653069586));
#73410=CARTESIAN_POINT('Ctrl Pts',(0.00240095788393081,-0.034644428984174,
0.0735778051675469));
#73411=CARTESIAN_POINT('Ctrl Pts',(0.00242213753290251,-0.0352450361874068,
0.0733954317998048));
#73412=CARTESIAN_POINT('Ctrl Pts',(0.00239367852624155,-0.0349452760959492,
0.0736104728568243));
#73413=CARTESIAN_POINT('Ctrl Pts',(0.00238149814091364,-0.034644428984174,
0.0738270466536636));
#73414=CARTESIAN_POINT('Ctrl Pts',(0.00242175574941768,-0.0352450361874068,
0.0733979024761031));
#73415=CARTESIAN_POINT('Ctrl Pts',(0.00239338992584237,-0.0349452760959492,
0.0736129579323229));
#73416=CARTESIAN_POINT('Ctrl Pts',(0.00238130354348347,-0.034644428984174,
0.0738295390685247));
#73417=CARTESIAN_POINT('',(0.00241751542765013,-0.0351951634053263,0.0734312010684742));
#73418=CARTESIAN_POINT('',(0.0023928014789834,-0.0348678972934074,0.0736662799844453));
#73419=CARTESIAN_POINT('Origin',(0.0191180503661572,-0.0345636767881002,
0.0746545690151686));
#73420=CARTESIAN_POINT('Origin',(-0.00861789031430973,-0.0346946199326795,
0.0727369448443345));
#73421=CARTESIAN_POINT('',(0.00240466837133796,-0.0346945769330289,0.0735418371175442));
#73422=CARTESIAN_POINT('',(0.00239941178594709,-0.0346945769458128,0.0736041156804507));
#73423=CARTESIAN_POINT('',(0.00243448329139868,-0.0350221583435276,0.0733073832383547));
#73424=CARTESIAN_POINT('Origin',(0.0191191025579792,-0.0345628458719109,
0.0751353416087238));
#73425=CARTESIAN_POINT('',(0.0024357072726396,-0.035195136029876,0.0733075614591906));
#73426=CARTESIAN_POINT('Origin',(-0.0084643700309076,-0.0351951838366836,
0.0716932013219096));
#73427=CARTESIAN_POINT('',(0.00241751373843655,-0.035195137132875,0.073431233470066));
#73428=CARTESIAN_POINT('Ctrl Pts',(0.00222754141431054,-0.0350241211494343,
0.0730389893436746));
#73429=CARTESIAN_POINT('Ctrl Pts',(0.00221223769805176,-0.0349144232818962,
0.0731202076428497));
#73430=CARTESIAN_POINT('Ctrl Pts',(0.00219860366206057,-0.0348045283579413,
0.0732017908938422));
#73431=CARTESIAN_POINT('Ctrl Pts',(0.00218666065840955,-0.0346945769439158,
0.0732836352487303));
#73432=CARTESIAN_POINT('Ctrl Pts',(0.00229700569336549,-0.0350241211494343,
0.0731285206551714));
#73433=CARTESIAN_POINT('Ctrl Pts',(0.00228293523421331,-0.0349144232818962,
0.073208782112384));
#73434=CARTESIAN_POINT('Ctrl Pts',(0.00227051541488546,-0.0348045283579413,
0.0732893824563923));
#73435=CARTESIAN_POINT('Ctrl Pts',(0.00225976598534772,-0.0346945769439158,
0.0733702190403788));
#73436=CARTESIAN_POINT('Ctrl Pts',(0.00236646997242043,-0.0350241211494343,
0.0732180519666682));
#73437=CARTESIAN_POINT('Ctrl Pts',(0.00235363277037486,-0.0349144232818962,
0.0732973565819183));
#73438=CARTESIAN_POINT('Ctrl Pts',(0.00234242716771034,-0.0348045283579413,
0.0733769740189424));
#73439=CARTESIAN_POINT('Ctrl Pts',(0.00233287131228588,-0.0346945769439158,
0.0734568028320273));
#73440=CARTESIAN_POINT('Ctrl Pts',(0.00243593425147538,-0.0350241211494343,
0.073307583278165));
#73441=CARTESIAN_POINT('Ctrl Pts',(0.0024243303065364,-0.0349144232818962,
0.0733859310514526));
#73442=CARTESIAN_POINT('Ctrl Pts',(0.00241433892053522,-0.0348045283579413,
0.0734645655814925));
#73443=CARTESIAN_POINT('Ctrl Pts',(0.00240597663922405,-0.0346945769439158,
0.0735433866236757));
#73444=CARTESIAN_POINT('',(0.00229566451562936,-0.0346945769458128,0.0734127361773446));
#73445=CARTESIAN_POINT('Ctrl Pts',(0.0021885247799184,-0.0347116136492793,
0.0732709554169476));
#73446=CARTESIAN_POINT('Ctrl Pts',(0.00223100255147917,-0.0347621546532328,
0.0732772466108068));
#73447=CARTESIAN_POINT('Ctrl Pts',(0.00227273344902875,-0.0348133084097092,
0.0732834271884774));
#73448=CARTESIAN_POINT('Ctrl Pts',(0.00235473632337568,-0.0349168561544568,
0.0732955722695532));
#73449=CARTESIAN_POINT('Ctrl Pts',(0.00239497577380308,-0.0349692089015917,
0.0733015319556226));
#73450=CARTESIAN_POINT('Ctrl Pts',(0.00243448329143193,-0.0350221583435,
0.0733073832383798));
#73451=CARTESIAN_POINT('Ctrl Pts',(0.00241868864853549,-0.0351951371254872,
0.0734303616867431));
#73452=CARTESIAN_POINT('Ctrl Pts',(0.00240381057796537,-0.0350307338985332,
0.0735483109159624));
#73453=CARTESIAN_POINT('Ctrl Pts',(0.00239382018952007,-0.0348659306906665,
0.0736667742849673));
#73454=CARTESIAN_POINT('Ctrl Pts',(0.00241751373855187,-0.0351951371254872,
0.0734312334700801));
#73455=CARTESIAN_POINT('Ctrl Pts',(0.00240265369155523,-0.0350307338985332,
0.073549206989826));
#73456=CARTESIAN_POINT('Ctrl Pts',(0.00239268231523604,-0.0348659306906665,
0.0736676938836678));
#73457=CARTESIAN_POINT('Ctrl Pts',(0.00222059760062791,-0.0351951371254872,
0.0735773452660617));
#73458=CARTESIAN_POINT('Ctrl Pts',(0.00220875832333139,-0.0350307338985332,
0.0736993899033987));
#73459=CARTESIAN_POINT('Ctrl Pts',(0.00220197339916482,-0.0348659306906665,
0.0738218195844148));
#73460=CARTESIAN_POINT('Origin',(-0.00290653846384609,-0.030860918850895,
0.073218994061773));
#73461=CARTESIAN_POINT('',(0.00233166274228548,-0.0351951371254872,0.0734949349187452));
#73462=CARTESIAN_POINT('Origin',(0.00909906401176292,-0.0351840467441185,
0.0740902419571476));
#73463=CARTESIAN_POINT('Origin',(-0.00383964241854335,-0.0352322613866184,
0.0739377587820059));
#73464=CARTESIAN_POINT('',(0.00237778028345409,-0.0351951142564653,0.0739024588161934));
#73465=CARTESIAN_POINT('',(0.00237509545286777,-0.0351951372916786,0.0740271148398609));
#73466=CARTESIAN_POINT('Origin',(0.00829604622235164,-0.0352875119212674,
0.0744437979227203));
#73467=CARTESIAN_POINT('Origin',(0.00971740669074562,-0.0298325076522173,
0.0668181822689157));
#73468=CARTESIAN_POINT('Origin',(0.000427998268266064,-0.0338732996266689,
0.0708299719531315));
#73469=CARTESIAN_POINT('Ctrl Pts',(0.00362087063773921,-0.0321934096636942,
0.0705720224609657));
#73470=CARTESIAN_POINT('Ctrl Pts',(0.00355682654359785,-0.0320508460843192,
0.0706526224335524));
#73471=CARTESIAN_POINT('Ctrl Pts',(0.00349499630114318,-0.0319086045660808,
0.0707348823719354));
#73472=CARTESIAN_POINT('Ctrl Pts',(0.00343549846013825,-0.031766989286452,
0.0708186141957953));
#73473=CARTESIAN_POINT('Ctrl Pts',(0.00357014775933072,-0.0321934096636942,
0.0706387878879011));
#73474=CARTESIAN_POINT('Ctrl Pts',(0.00350729873453828,-0.0320508460843192,
0.0707202957758575));
#73475=CARTESIAN_POINT('Ctrl Pts',(0.00344668705424083,-0.0319086045660808,
0.0708034308358836));
#73476=CARTESIAN_POINT('Ctrl Pts',(0.00338842848929625,-0.031766989286452,
0.0708880033193749));
#73477=CARTESIAN_POINT('Ctrl Pts',(0.00351942488092221,-0.0321934096636942,
0.0707055533148366));
#73478=CARTESIAN_POINT('Ctrl Pts',(0.0034577709254787,-0.0320508460843192,
0.0707879691181626));
#73479=CARTESIAN_POINT('Ctrl Pts',(0.00339837780733849,-0.0319086045660808,
0.0708719792998318));
#73480=CARTESIAN_POINT('Ctrl Pts',(0.00334135851845424,-0.031766989286452,
0.0709573924429544));
#73481=CARTESIAN_POINT('Ctrl Pts',(0.00346870200251372,-0.0321934096636942,
0.070772318741772));
#73482=CARTESIAN_POINT('Ctrl Pts',(0.00340824311641913,-0.0320508460843192,
0.0708556424604677));
#73483=CARTESIAN_POINT('Ctrl Pts',(0.00335006856043615,-0.0319086045660808,
0.0709405277637799));
#73484=CARTESIAN_POINT('Ctrl Pts',(0.00329428854761224,-0.031766989286452,
0.0710267815665341));
#73485=CARTESIAN_POINT('',(0.00346960944483376,-0.0321934096636942,0.0707711242950919));
#73486=CARTESIAN_POINT('',(0.00333471940589462,-0.0318665617511257,0.0709651919038781));
#73487=CARTESIAN_POINT('Origin',(0.0166212639895788,-0.0326371944420649,
0.0810789799200326));
#73488=CARTESIAN_POINT('Origin',(-0.00579248170359597,-0.0316939261509038,
0.0648954480805042));
#73489=CARTESIAN_POINT('',(0.00354402256720402,-0.0320197221621841,0.0706710071952549));
#73490=CARTESIAN_POINT('Ctrl Pts',(0.00354387680638793,-0.0320197392094754,
0.0706711210752944));
#73491=CARTESIAN_POINT('Ctrl Pts',(0.00352617518936717,-0.0319792716576052,
0.0706944251346968));
#73492=CARTESIAN_POINT('Ctrl Pts',(0.00350857064861603,-0.0319386439829691,
0.0707179702330528));
#73493=CARTESIAN_POINT('Ctrl Pts',(0.00349105147620165,-0.0318979099381623,
0.0707417861527729));
#73494=CARTESIAN_POINT('Ctrl Pts',(0.00347353265006574,-0.0318571766984918,
0.0707656016017551));
#73495=CARTESIAN_POINT('Ctrl Pts',(0.00345618679580781,-0.0318163871833561,
0.0707895657599812));
#73496=CARTESIAN_POINT('Ctrl Pts',(0.00343907072366616,-0.0317755399638303,
0.0708135941360121));
#73497=CARTESIAN_POINT('',(0.00354522704296514,-0.0321934096636184,0.0706715904874358));
#73498=CARTESIAN_POINT('Origin',(0.00174950357711688,-0.0324018949057924,
0.0693329757938452));
#73499=CARTESIAN_POINT('',(0.00350741824390944,-0.0321934096636663,0.0707213573912738));
#73500=CARTESIAN_POINT('Ctrl Pts',(0.00347161902000672,-0.0321934096636618,
0.070770849895742));
#73501=CARTESIAN_POINT('Ctrl Pts',(0.00342501790651343,-0.0320835708272592,
0.070835006851583));
#73502=CARTESIAN_POINT('Ctrl Pts',(0.00337977154842656,-0.0319739230346488,
0.0709000910014041));
#73503=CARTESIAN_POINT('Ctrl Pts',(0.00333593144453206,-0.0318646057455572,
0.0709660146316876));
#73504=CARTESIAN_POINT('Ctrl Pts',(0.0033593420133819,-0.0321934096636618,
0.070786180862701));
#73505=CARTESIAN_POINT('Ctrl Pts',(0.00331295232587124,-0.0320835708272592,
0.070851886205967));
#73506=CARTESIAN_POINT('Ctrl Pts',(0.00326794931492861,-0.0319739230346488,
0.0709185134696356));
#73507=CARTESIAN_POINT('Ctrl Pts',(0.00322438401647163,-0.0318646057455572,
0.0709859729897772));
#73508=CARTESIAN_POINT('Ctrl Pts',(0.00324706500675709,-0.0321934096636618,
0.07080151182966));
#73509=CARTESIAN_POINT('Ctrl Pts',(0.00320088674522905,-0.0320835708272592,
0.0708687655603509));
#73510=CARTESIAN_POINT('Ctrl Pts',(0.00315612708143066,-0.0319739230346488,
0.0709369359378671));
#73511=CARTESIAN_POINT('Ctrl Pts',(0.00311283658841121,-0.0318646057455572,
0.0710059313478667));
#73512=CARTESIAN_POINT('Ctrl Pts',(0.00313478800013228,-0.0321934096636618,
0.070816842796619));
#73513=CARTESIAN_POINT('Ctrl Pts',(0.00308882116458686,-0.0320835708272592,
0.0708856449147348));
#73514=CARTESIAN_POINT('Ctrl Pts',(0.00304430484793271,-0.0319739230346488,
0.0709553584060986));
#73515=CARTESIAN_POINT('Ctrl Pts',(0.00300128916035079,-0.0318646057455572,
0.0710258897059563));
#73516=CARTESIAN_POINT('',(0.00312767969950581,-0.0321763980308448,0.0708275069825419));
#73517=CARTESIAN_POINT('',(0.00313478800011415,-0.0321934096636184,0.0708168427966462));
#73518=CARTESIAN_POINT('Origin',(0.016557473997587,-0.032638623064701,0.0804953256685402));
#73519=CARTESIAN_POINT('Ctrl Pts',(0.0031276797021428,-0.0321763980306271,
0.0708275069842942));
#73520=CARTESIAN_POINT('Ctrl Pts',(0.00316341756719317,-0.032125959617499,
0.0708512732715633));
#73521=CARTESIAN_POINT('Ctrl Pts',(0.00319853622736263,-0.0320749164631742,
0.0708746277770612));
#73522=CARTESIAN_POINT('Ctrl Pts',(0.00326756340033043,-0.0319716057793889,
0.070920532019517));
#73523=CARTESIAN_POINT('Ctrl Pts',(0.00330144501778713,-0.0319193786690074,
0.0709430638706159));
#73524=CARTESIAN_POINT('Ctrl Pts',(0.00333471940743654,-0.0318665617525257,
0.070965191904901));
#73525=CARTESIAN_POINT('',(0.00330219872248395,-0.0321934096636663,0.0707939835458791));
#73526=CARTESIAN_POINT('Origin',(0.00812378219310841,-0.0315241814719618,
0.07415));
#73527=CARTESIAN_POINT('',(0.00312767969919601,-0.0322104233323785,0.070827506982336));
#73528=CARTESIAN_POINT('',(0.00312059419090078,-0.0321934096636183,0.0708381863255016));
#73529=CARTESIAN_POINT('Origin',(0.0165875939923736,-0.0326387231199789,
0.0804614432059535));
#73530=CARTESIAN_POINT('Origin',(0.0172369298668578,-0.0326386244598137,
0.0794736183952894));
#73531=CARTESIAN_POINT('Origin',(0.01721732674277,-0.032638724241897,0.0795144951905481));
#73532=CARTESIAN_POINT('Ctrl Pts',(0.00342582656346833,-0.0327445246967098,
0.0708322691637306));
#73533=CARTESIAN_POINT('Ctrl Pts',(0.00330069629937572,-0.032443687833936,
0.0710094554569059));
#73534=CARTESIAN_POINT('Ctrl Pts',(0.00318926791291908,-0.0321434074405927,
0.071195563705441));
#73535=CARTESIAN_POINT('Ctrl Pts',(0.00328608384940243,-0.0327445246967098,
0.0710395659892381));
#73536=CARTESIAN_POINT('Ctrl Pts',(0.00316877191289618,-0.032443687833936,
0.0712220227650352));
#73537=CARTESIAN_POINT('Ctrl Pts',(0.00306553663727474,-0.0321434074405927,
0.0714127976149198));
#73538=CARTESIAN_POINT('',(0.00326663203070031,-0.0326943950436612,0.071070029659263));
#73539=CARTESIAN_POINT('',(0.00314419377156412,-0.0323666188837389,0.0712721841351429));
#73540=CARTESIAN_POINT('Origin',(0.0175044134070871,-0.0326395579110853,
0.0800083538704801));
#73541=CARTESIAN_POINT('Origin',(-0.00641834808919296,-0.0321933825603042,
0.065745777979453));
#73542=CARTESIAN_POINT('',(0.00320791644643815,-0.0321934096532688,0.0711646375500956));
#73543=CARTESIAN_POINT('',(0.00317664322635874,-0.0321934096584274,0.071218750728266));
#73544=CARTESIAN_POINT('',(0.00333471940510188,-0.0325210109756239,0.070965191903343));
#73545=CARTESIAN_POINT('Origin',(0.017225854936219,-0.0326393129159402,
0.0804002589717525));
#73546=CARTESIAN_POINT('',(0.00333585063525292,-0.0326943950436595,0.0709659441906129));
#73547=CARTESIAN_POINT('Origin',(-0.00587567575929243,-0.0326943765538164,
0.0648401219455952));
#73548=CARTESIAN_POINT('',(0.00330124133298662,-0.0326943950436703,0.071017986924948));
#73549=CARTESIAN_POINT('Ctrl Pts',(0.00326175000838405,-0.0325229783203769,
0.0706342293825203));
#73550=CARTESIAN_POINT('Ctrl Pts',(0.00321328518730691,-0.032413025309245,
0.0707012523898611));
#73551=CARTESIAN_POINT('Ctrl Pts',(0.00316621417387347,-0.0323031222208069,
0.0707692677889311));
#73552=CARTESIAN_POINT('Ctrl Pts',(0.00312059418842563,-0.0321934096576658,
0.0708381863292408));
#73553=CARTESIAN_POINT('Ctrl Pts',(0.00328648256885509,-0.0325229783203769,
0.0707448161931664));
#73554=CARTESIAN_POINT('Ctrl Pts',(0.00323954218454434,-0.032413025309245,
0.070811498262702));
#73555=CARTESIAN_POINT('Ctrl Pts',(0.00319398832393011,-0.0323031222208069,
0.0708791412407439));
#73556=CARTESIAN_POINT('Ctrl Pts',(0.00314987628082275,-0.0321934096576658,
0.0709476564224224));
#73557=CARTESIAN_POINT('Ctrl Pts',(0.00331121512932613,-0.0325229783203769,
0.0708554030038125));
#73558=CARTESIAN_POINT('Ctrl Pts',(0.00326579918178176,-0.032413025309245,
0.0709217441355429));
#73559=CARTESIAN_POINT('Ctrl Pts',(0.00322176247398675,-0.0323031222208069,
0.0709890146925567));
#73560=CARTESIAN_POINT('Ctrl Pts',(0.00317915837321986,-0.0321934096576658,
0.071057126515604));
#73561=CARTESIAN_POINT('Ctrl Pts',(0.00333594768979717,-0.0325229783203769,
0.0709659898144587));
#73562=CARTESIAN_POINT('Ctrl Pts',(0.00329205617901919,-0.032413025309245,
0.0710319900083838));
#73563=CARTESIAN_POINT('Ctrl Pts',(0.00324953662404339,-0.0323031222208069,
0.0710988881443695));
#73564=CARTESIAN_POINT('Ctrl Pts',(0.00320844046561698,-0.0321934096576658,
0.0711665966087856));
#73565=CARTESIAN_POINT('',(0.00316425531880832,-0.0321934096584275,0.0710014119373104));
#73566=CARTESIAN_POINT('Ctrl Pts',(0.00312767970208687,-0.0322104233328928,
0.0708275069842569));
#73567=CARTESIAN_POINT('Ctrl Pts',(0.00316346599253226,-0.0322609421831346,
0.0708513054752362));
#73568=CARTESIAN_POINT('Ctrl Pts',(0.00319860830931172,-0.0323120888240686,
0.0708746757127897));
#73569=CARTESIAN_POINT('Ctrl Pts',(0.00326763600488211,-0.0324156524631813,
0.0709205803027851));
#73570=CARTESIAN_POINT('Ctrl Pts',(0.0033014930096676,-0.0324680267167311,
0.0709430957860314));
#73571=CARTESIAN_POINT('Ctrl Pts',(0.00333471940513553,-0.0325210109755913,
0.0709651919033707));
#73572=CARTESIAN_POINT('Origin',(0.0132379182114124,-0.0262834582512268,
0.0681709533682772));
#73573=CARTESIAN_POINT('Origin',(0.00208133209419324,-0.0342770788205475,
0.0635995452934657));
#73574=CARTESIAN_POINT('Ctrl Pts',(0.00326861992818894,-0.0326943950436604,
0.071069629716258));
#73575=CARTESIAN_POINT('Ctrl Pts',(0.00322616665244976,-0.0325844576448134,
0.0711365429518124));
#73576=CARTESIAN_POINT('Ctrl Pts',(0.00318509424764331,-0.0324744968375322,
0.0712043389262659));
#73577=CARTESIAN_POINT('Ctrl Pts',(0.00314545414001204,-0.0323646534831894,
0.0712729300496142));
#73578=CARTESIAN_POINT('Ctrl Pts',(0.00315752727481116,-0.0326943950436604,
0.0710919803302739));
#73579=CARTESIAN_POINT('Ctrl Pts',(0.00311538203242263,-0.0325844576448134,
0.0711604246308018));
#73580=CARTESIAN_POINT('Ctrl Pts',(0.0030746493477007,-0.0324744968375322,
0.0712297454079498));
#73581=CARTESIAN_POINT('Ctrl Pts',(0.00303538018467171,-0.0323646534831894,
0.0712998531240512));
#73582=CARTESIAN_POINT('Ctrl Pts',(0.00304643462143338,-0.0326943950436604,
0.0711143309442899));
#73583=CARTESIAN_POINT('Ctrl Pts',(0.00300459741239551,-0.0325844576448134,
0.0711843063097911));
#73584=CARTESIAN_POINT('Ctrl Pts',(0.0029642044477581,-0.0324744968375322,
0.0712551518896336));
#73585=CARTESIAN_POINT('Ctrl Pts',(0.00292530622933137,-0.0323646534831894,
0.0713267761984882));
#73586=CARTESIAN_POINT('Ctrl Pts',(0.0029353419680556,-0.0326943950436604,
0.0711366815583059));
#73587=CARTESIAN_POINT('Ctrl Pts',(0.00289381279236838,-0.0325844576448134,
0.0712081879887805));
#73588=CARTESIAN_POINT('Ctrl Pts',(0.00285375954781549,-0.0324744968375322,
0.0712805583713175));
#73589=CARTESIAN_POINT('Ctrl Pts',(0.00281523227399103,-0.0323646534831894,
0.0713536992729253));
#73590=CARTESIAN_POINT('',(0.00292891730365027,-0.032677355999133,0.0711477710346538));
#73591=CARTESIAN_POINT('',(0.00293534196805522,-0.0326943950436594,0.0711366815583065));
#73592=CARTESIAN_POINT('Origin',(0.0173309690388185,-0.0326395670637737,
0.0794130124607109));
#73593=CARTESIAN_POINT('Ctrl Pts',(0.00292891730654715,-0.0326773559987413,
0.0711477710363262));
#73594=CARTESIAN_POINT('Ctrl Pts',(0.00296610685216895,-0.0326267922586144,
0.0711692637090808));
#73595=CARTESIAN_POINT('Ctrl Pts',(0.00300263723995047,-0.0325756109579706,
0.0711903754397316));
#73596=CARTESIAN_POINT('Ctrl Pts',(0.00307441078905216,-0.0324719985462362,
0.0712318549839823));
#73597=CARTESIAN_POINT('Ctrl Pts',(0.0031096251639229,-0.0324196091621772,
0.0712522061612474));
#73598=CARTESIAN_POINT('Ctrl Pts',(0.00314419377160632,-0.0323666188837756,
0.0712721841351673));
#73599=CARTESIAN_POINT('',(0.00310098699938777,-0.0326943950436702,0.0711033556087947));
#73600=CARTESIAN_POINT('Origin',(0.00812378219310841,-0.0315241814719618,
0.07415));
#73601=CARTESIAN_POINT('',(0.00292891730368791,-0.0327114338379873,0.0711477710346757));
#73602=CARTESIAN_POINT('',(0.00292251633834769,-0.0326943950436593,0.0711588742072384));
#73603=CARTESIAN_POINT('Origin',(0.0173529681295403,-0.0326395666107975,
0.0793734000170662));
#73604=CARTESIAN_POINT('Origin',(0.0172806936696031,-0.0326395680226932,
0.0795000104820588));
#73605=CARTESIAN_POINT('Origin',(0.0172573503043656,-0.0326395676472844,
0.0795388459199229));
#73606=CARTESIAN_POINT('Ctrl Pts',(0.00322675429283235,-0.0332451089994435,
0.071133836419569));
#73607=CARTESIAN_POINT('Ctrl Pts',(0.003112997822243,-0.0329451141710254,
0.0713185308485872));
#73608=CARTESIAN_POINT('Ctrl Pts',(0.00301347646121109,-0.0326442513127493,
0.0715112691826301));
#73609=CARTESIAN_POINT('Ctrl Pts',(0.00310030507526074,-0.0332451089994435,
0.0713494995721371));
#73610=CARTESIAN_POINT('Ctrl Pts',(0.00299468247354755,-0.0329451141710254,
0.0715389631114226));
#73611=CARTESIAN_POINT('Ctrl Pts',(0.00290363110281041,-0.0326442513127493,
0.0717358443309388));
#73612=CARTESIAN_POINT('Ctrl Pts',(0.00309904058308502,-0.0332451089994435,
0.0713516562036627));
#73613=CARTESIAN_POINT('Ctrl Pts',(0.0029934993200606,-0.0329451141710254,
0.071541167434051));
#73614=CARTESIAN_POINT('Ctrl Pts',(0.0029025326492264,-0.0326442513127493,
0.0717380900824218));
#73615=CARTESIAN_POINT('',(0.0030828235692053,-0.0331951640388616,0.0713810902593082));
#73616=CARTESIAN_POINT('',(0.00297332028693037,-0.0328677532354987,0.071590533801195));
#73617=CARTESIAN_POINT('Origin',(0.0181304794375318,-0.0326402808280178,
0.0787702918631664));
#73618=CARTESIAN_POINT('Origin',(-0.00692769621469471,-0.0326944278779092,
0.0666707517731004));
#73619=CARTESIAN_POINT('',(0.00303016432206029,-0.0326943950436593,0.0714791982507606));
#73620=CARTESIAN_POINT('',(0.00300235060865649,-0.0326943950436694,0.0715351683083562));
#73621=CARTESIAN_POINT('',(0.00314419377156557,-0.0330220786163545,0.0712721841351405));
#73622=CARTESIAN_POINT('Origin',(0.0179451142460192,-0.0326396682765936,
0.0792139047477438));
#73623=CARTESIAN_POINT('',(0.00314537000600169,-0.033195164038859,0.0712728639074128));
#73624=CARTESIAN_POINT('Origin',(-0.00640595420462623,-0.0331952026560018,
0.0657529386041598));
#73625=CARTESIAN_POINT('',(0.0031140967876135,-0.0331951640388702,0.0713269770833705));
#73626=CARTESIAN_POINT('Ctrl Pts',(0.00305058654161593,-0.0330240426238172,
0.0709464572920434));
#73627=CARTESIAN_POINT('Ctrl Pts',(0.0030064546197534,-0.0329142774063519,
0.0710163455047177));
#73628=CARTESIAN_POINT('Ctrl Pts',(0.00296374548109739,-0.0328043479726691,
0.0710871808893163));
#73629=CARTESIAN_POINT('Ctrl Pts',(0.00292251633834767,-0.0326943950436593,
0.0711588742072383));
#73630=CARTESIAN_POINT('Ctrl Pts',(0.00308221411104959,-0.0330240426238172,
0.0710552728830045));
#73631=CARTESIAN_POINT('Ctrl Pts',(0.00303958122996644,-0.0329142774063519,
0.0711247253950967));
#73632=CARTESIAN_POINT('Ctrl Pts',(0.00299836287226821,-0.0328043479726691,
0.0711950938725401));
#73633=CARTESIAN_POINT('Ctrl Pts',(0.00295861432438048,-0.0326943950436593,
0.0712662896222814));
#73634=CARTESIAN_POINT('Ctrl Pts',(0.00311384168048324,-0.0330240426238172,
0.0711640884739656));
#73635=CARTESIAN_POINT('Ctrl Pts',(0.00307270784017947,-0.0329142774063519,
0.0712331052854756));
#73636=CARTESIAN_POINT('Ctrl Pts',(0.00303298026343902,-0.0328043479726691,
0.071303006855764));
#73637=CARTESIAN_POINT('Ctrl Pts',(0.00299471231041328,-0.0326943950436593,
0.0713737050373245));
#73638=CARTESIAN_POINT('Ctrl Pts',(0.00314546924991689,-0.0330240426238172,
0.0712729040649268));
#73639=CARTESIAN_POINT('Ctrl Pts',(0.00310583445039251,-0.0329142774063519,
0.0713414851758545));
#73640=CARTESIAN_POINT('Ctrl Pts',(0.00306759765460984,-0.0328043479726691,
0.0714109198389878));
#73641=CARTESIAN_POINT('Ctrl Pts',(0.00303081029644609,-0.0326943950436593,
0.0714811204523675));
#73642=CARTESIAN_POINT('',(0.00297634033021399,-0.0326943950436693,0.0713190362290095));
#73643=CARTESIAN_POINT('Ctrl Pts',(0.00292891730655267,-0.0327114338383325,
0.0711477710363293));
#73644=CARTESIAN_POINT('Ctrl Pts',(0.00296610066635426,-0.0327619876831058,
0.0711692601341597));
#73645=CARTESIAN_POINT('Ctrl Pts',(0.0030026280327023,-0.0328131562604518,
0.0711903701186562));
#73646=CARTESIAN_POINT('Ctrl Pts',(0.00307440151585102,-0.032916737585877,
0.0712318496247912));
#73647=CARTESIAN_POINT('Ctrl Pts',(0.00310961903441792,-0.0329691088920623,
0.0712522026188688));
#73648=CARTESIAN_POINT('Ctrl Pts',(0.00314419377160533,-0.0330220786163187,
0.0712721841351665));
#73649=CARTESIAN_POINT('Ctrl Pts',(0.00308478274413301,-0.0331951640388604,
0.0713805662007306));
#73650=CARTESIAN_POINT('Ctrl Pts',(0.00302752647592885,-0.0330306422010619,
0.0714847442836322));
#73651=CARTESIAN_POINT('Ctrl Pts',(0.00297462492252726,-0.0328657861914645,
0.071591199808869));
#73652=CARTESIAN_POINT('Ctrl Pts',(0.00308282356920689,-0.0331951640388604,
0.0713810902593056));
#73653=CARTESIAN_POINT('Ctrl Pts',(0.00302557813557777,-0.0330306422010619,
0.0714853088468927));
#73654=CARTESIAN_POINT('Ctrl Pts',(0.0029726890815944,-0.0328657861914645,
0.0715918043943996));
#73655=CARTESIAN_POINT('Ctrl Pts',(0.00275637233919229,-0.0331951640388604,
0.0714684125112009));
#73656=CARTESIAN_POINT('Ctrl Pts',(0.00270093223713529,-0.0330306422010619,
0.0715793802686675));
#73657=CARTESIAN_POINT('Ctrl Pts',(0.00265012592236956,-0.0328657861914645,
0.0716925446026832));
#73658=CARTESIAN_POINT('',(0.00275065666549445,-0.033178164828189,0.071479883511857));
#73659=CARTESIAN_POINT('',(0.00275637233919176,-0.0331951640388588,0.0714684125112019));
#73660=CARTESIAN_POINT('Origin',(0.0178499416008269,-0.0326412092185282,
0.0781879441317988));
#73661=CARTESIAN_POINT('Ctrl Pts',(0.00275065666710743,-0.033178164828644,
0.0714798835109781));
#73662=CARTESIAN_POINT('Ctrl Pts',(0.00278914885119287,-0.033127681154678,
0.0714990117710988));
#73663=CARTESIAN_POINT('Ctrl Pts',(0.00282694600068731,-0.0330765663497788,
0.0715177946037952));
#73664=CARTESIAN_POINT('Ctrl Pts',(0.00290118263271588,-0.0329730614463246,
0.0715546856972969));
#73665=CARTESIAN_POINT('Ctrl Pts',(0.00293759212287904,-0.0329207133374027,
0.0715727790597024));
#73666=CARTESIAN_POINT('Ctrl Pts',(0.00297332028534813,-0.0328677532289348,
0.0715905337847994));
#73667=CARTESIAN_POINT('',(0.00291959795420853,-0.0331951640388701,0.0714247513852651));
#73668=CARTESIAN_POINT('Origin',(0.00812378219310841,-0.0315241814719618,
0.07415));
#73669=CARTESIAN_POINT('',(0.00275065666659455,-0.033212160714442,0.0714798835131262));
#73670=CARTESIAN_POINT('',(0.00274496550589083,-0.0331951640388587,0.0714913666959631));
#73671=CARTESIAN_POINT('Origin',(0.0178627958923643,-0.0326413646727927,
0.0781444579374741));
#73672=CARTESIAN_POINT('Origin',(0.0172159996961188,-0.0326412100651403,
0.079463643032878));
#73673=CARTESIAN_POINT('Origin',(0.0171890976271707,-0.0326413658901262,
0.0795001477874614));
#73674=CARTESIAN_POINT('Ctrl Pts',(0.00304704076994315,-0.0337436976235975,
0.0714472566673252));
#73675=CARTESIAN_POINT('Ctrl Pts',(0.00302273188679711,-0.0336723290703325,
0.0714929176490864));
#73676=CARTESIAN_POINT('Ctrl Pts',(0.00299924823339709,-0.033601104548885,
0.0715390084841644));
#73677=CARTESIAN_POINT('Ctrl Pts',(0.00292426957994049,-0.0333736987606857,
0.0716861673904885));
#73678=CARTESIAN_POINT('Ctrl Pts',(0.00285785931192881,-0.0331450831799192,
0.0718373864980354));
#73679=CARTESIAN_POINT('Ctrl Pts',(0.00293438186405758,-0.0337436976235975,
0.0716704336619386));
#73680=CARTESIAN_POINT('Ctrl Pts',(0.0029120802686245,-0.0336723290703325,
0.0717171079149733));
#73681=CARTESIAN_POINT('Ctrl Pts',(0.00289062180376203,-0.033601104548885,
0.0717641757526222));
#73682=CARTESIAN_POINT('Ctrl Pts',(0.00282210917613855,-0.0333736987606857,
0.0719144540346219));
#73683=CARTESIAN_POINT('Ctrl Pts',(0.00276233328622339,-0.0331450831799192,
0.0720684163195151));
#73684=CARTESIAN_POINT('Ctrl Pts',(0.00293325527499873,-0.0337436976235975,
0.0716726654318848));
#73685=CARTESIAN_POINT('Ctrl Pts',(0.00291097375244277,-0.0336723290703325,
0.0717193498176322));
#73686=CARTESIAN_POINT('Ctrl Pts',(0.00288953553946568,-0.033601104548885,
0.0717664274253068));
#73687=CARTESIAN_POINT('Ctrl Pts',(0.00282108757210053,-0.0333736987606857,
0.0719167369010632));
#73688=CARTESIAN_POINT('Ctrl Pts',(0.00276137802596633,-0.0331450831799192,
0.0720707266177299));
#73689=CARTESIAN_POINT('',(0.00291890946839834,-0.0336938721132548,0.0717030784811175));
#73690=CARTESIAN_POINT('',(0.00282277333995648,-0.0333679870047996,0.0719189845050616));
#73691=CARTESIAN_POINT('Ctrl Pts',(0.002918909468406,-0.0336938721132481,
0.071703078481101));
#73692=CARTESIAN_POINT('Ctrl Pts',(0.0029093579858429,-0.0336629187933826,
0.0717233955410027));
#73693=CARTESIAN_POINT('Ctrl Pts',(0.00289992852262783,-0.0336319952300965,
0.0717437620307916));
#73694=CARTESIAN_POINT('Ctrl Pts',(0.00289062180376428,-0.0336011045488875,
0.0717641757526174));
#73695=CARTESIAN_POINT('Ctrl Pts',(0.00286726806155567,-0.0335235892595377,
0.071815400765861));
#73696=CARTESIAN_POINT('Ctrl Pts',(0.00284464585483451,-0.0334458668665494,
0.0718670142721589));
#73697=CARTESIAN_POINT('Ctrl Pts',(0.00282277334430087,-0.0333679869962417,
0.0719189844940655));
#73698=CARTESIAN_POINT('Ctrl Pts',(0.00282275545855579,-0.0333679692470412,
0.0719190252194836));
#73699=CARTESIAN_POINT('Ctrl Pts',(0.00282317548349692,-0.0333391895414745,
0.0719191955627592));
#73700=CARTESIAN_POINT('Ctrl Pts',(0.00282349153308067,-0.0333104081129247,
0.0719193202342241));
#73701=CARTESIAN_POINT('Ctrl Pts',(0.00282391191135071,-0.0332532697957439,
0.0719194801062434));
#73702=CARTESIAN_POINT('Ctrl Pts',(0.00282401933036336,-0.0332249169766573,
0.0719195166106337));
#73703=CARTESIAN_POINT('Ctrl Pts',(0.00282402538918768,-0.0331960985427074,
0.0719195116764479));
#73704=CARTESIAN_POINT('Ctrl Pts',(0.00282402546003503,-0.0331956312497407,
0.071919511584822));
#73705=CARTESIAN_POINT('Ctrl Pts',(0.00282402550318796,-0.0331951640388588,
0.0719195114822884));
#73706=CARTESIAN_POINT('',(0.00287251438400792,-0.0331951640388587,0.071804299380333));
#73707=CARTESIAN_POINT('',(0.00284826994360801,-0.0331951640388687,0.0718619054313205));
#73708=CARTESIAN_POINT('',(0.0029733202990091,-0.0335216366567745,0.0715905337914453));
#73709=CARTESIAN_POINT('Origin',(0.0183871519506845,-0.032643457152678,
0.0778980260693054));
#73710=CARTESIAN_POINT('',(0.00297453689523276,-0.0336938721132329,0.0715911383659318));
#73711=CARTESIAN_POINT('Origin',(-0.0068050609203762,-0.0336938867896239,
0.0667312724711584));
#73712=CARTESIAN_POINT('',(0.00294672318182555,-0.0336938721132539,0.0716471084235347));
#73713=CARTESIAN_POINT('Ctrl Pts',(0.00285944476230661,-0.0335235895815172,
0.0712713281856582));
#73714=CARTESIAN_POINT('Ctrl Pts',(0.00281981417719894,-0.0334144449262748,
0.0713438021549198));
#73715=CARTESIAN_POINT('Ctrl Pts',(0.00278163531901257,-0.0333049234473147,
0.0714171781260547));
#73716=CARTESIAN_POINT('Ctrl Pts',(0.00274496550589072,-0.0331951640388587,
0.071491366695963));
#73717=CARTESIAN_POINT('Ctrl Pts',(0.00289784258109682,-0.0335235895815172,
0.0713779432877689));
#73718=CARTESIAN_POINT('Ctrl Pts',(0.00285967976277552,-0.0334144449262748,
0.0714498886354565));
#73719=CARTESIAN_POINT('Ctrl Pts',(0.00282295943673785,-0.0333049234473147,
0.071522705054738));
#73720=CARTESIAN_POINT('Ctrl Pts',(0.00278773699129957,-0.0331951640388587,
0.0715963036890676));
#73721=CARTESIAN_POINT('Ctrl Pts',(0.00293624039988703,-0.0335235895815172,
0.0714845583898797));
#73722=CARTESIAN_POINT('Ctrl Pts',(0.00289954534835211,-0.0334144449262748,
0.0715559751159933));
#73723=CARTESIAN_POINT('Ctrl Pts',(0.00286428355446313,-0.0333049234473147,
0.0716282319834214));
#73724=CARTESIAN_POINT('Ctrl Pts',(0.00283050847670842,-0.0331951640388587,
0.0717012406821722));
#73725=CARTESIAN_POINT('Ctrl Pts',(0.00297463821867724,-0.0335235895815172,
0.0715911734919904));
#73726=CARTESIAN_POINT('Ctrl Pts',(0.00293941093392869,-0.0334144449262748,
0.07166206159653));
#73727=CARTESIAN_POINT('Ctrl Pts',(0.00290560767218842,-0.0333049234473147,
0.0717337589121048));
#73728=CARTESIAN_POINT('Ctrl Pts',(0.00287327996211727,-0.0331951640388587,
0.0718061776752768));
#73729=CARTESIAN_POINT('',(0.00280873994495937,-0.0331951640388687,0.071647833038158));
#73730=CARTESIAN_POINT('Ctrl Pts',(0.00275065666939384,-0.0332121607145978,
0.0714798835145147));
#73731=CARTESIAN_POINT('Ctrl Pts',(0.00278908409442409,-0.0332625444109897,
0.0714989796068384));
#73732=CARTESIAN_POINT('Ctrl Pts',(0.002826849354618,-0.0333135300747116,
0.0715177466435245));
#73733=CARTESIAN_POINT('Ctrl Pts',(0.00290108552287232,-0.0334167203140644,
0.0715546375026344));
#73734=CARTESIAN_POINT('Ctrl Pts',(0.00293752767868182,-0.0334688847587355,
0.0715727470369388));
#73735=CARTESIAN_POINT('Ctrl Pts',(0.00297332029956439,-0.0335216366562437,
0.0715905337919021));
#73736=CARTESIAN_POINT('Ctrl Pts',(0.00292083142185517,-0.033693872113248,
0.0717024325901044));
#73737=CARTESIAN_POINT('Ctrl Pts',(0.00290650499761469,-0.0336474569765003,
0.0717328871874937));
#73738=CARTESIAN_POINT('Ctrl Pts',(0.00289253606454429,-0.033601104548885,
0.0717635074069987));
#73739=CARTESIAN_POINT('Ctrl Pts',(0.00285716993767254,-0.0334837508592655,
0.0718410307627479));
#73740=CARTESIAN_POINT('Ctrl Pts',(0.00282411651876059,-0.0333660264659096,
0.0719195680476179));
#73741=CARTESIAN_POINT('Ctrl Pts',(0.00291890946840991,-0.033693872113248,
0.0717030784810931));
#73742=CARTESIAN_POINT('Ctrl Pts',(0.00290458682478371,-0.0336474569765003,
0.0717335443283136));
#73743=CARTESIAN_POINT('Ctrl Pts',(0.00289062180376203,-0.033601104548885,
0.0717641757526222));
#73744=CARTESIAN_POINT('Ctrl Pts',(0.00285526558129819,-0.0334837508592655,
0.0718417274763579));
#73745=CARTESIAN_POINT('Ctrl Pts',(0.00282222290304712,-0.0333660264659096,
0.0719202928232692));
#73746=CARTESIAN_POINT('Ctrl Pts',(0.00259666348057398,-0.033693872113248,
0.0718113723527249));
#73747=CARTESIAN_POINT('Ctrl Pts',(0.00258297471691422,-0.0336474569765003,
0.071843724412645));
#73748=CARTESIAN_POINT('Ctrl Pts',(0.00256966561292629,-0.033601104548885,
0.0718762345000432));
#73749=CARTESIAN_POINT('Ctrl Pts',(0.00253597002158697,-0.0334837508592655,
0.0719585425667899));
#73750=CARTESIAN_POINT('Ctrl Pts',(0.00250472818553856,-0.0333660264659096,
0.0720418129601336));
#73751=CARTESIAN_POINT('',(0.00259360129927857,-0.0336769361243753,0.0718225337206482));
#73752=CARTESIAN_POINT('',(0.00259858542488537,-0.0336938721132327,0.0718107264648148));
#73753=CARTESIAN_POINT('Ctrl Pts',(0.00259360129927847,-0.033676936124375,
0.0718225337206485));
#73754=CARTESIAN_POINT('Ctrl Pts',(0.00259442994721403,-0.0336797586669862,
0.071820564810069));
#73755=CARTESIAN_POINT('Ctrl Pts',(0.00259525961529622,-0.0336825812712519,
0.0718185964164901));
#73756=CARTESIAN_POINT('Ctrl Pts',(0.0025969209922326,-0.0336882266062521,
0.0718146606608783));
#73757=CARTESIAN_POINT('Ctrl Pts',(0.00259775270108091,-0.0336910493369274,
0.0718126932988885));
#73758=CARTESIAN_POINT('Ctrl Pts',(0.00259858542488982,-0.0336938721132311,
0.0718107264648143));
#73759=CARTESIAN_POINT('Ctrl Pts',(0.00259360129927861,-0.0336769361243753,
0.0718225337206483));
#73760=CARTESIAN_POINT('Ctrl Pts',(0.00263223409018507,-0.033627899461326,
0.0718387929569804));
#73761=CARTESIAN_POINT('Ctrl Pts',(0.00267141690363832,-0.0335767852527761,
0.0718552836792171));
#73762=CARTESIAN_POINT('Ctrl Pts',(0.00274820223265939,-0.0334733171841367,
0.0718876000297085));
#73763=CARTESIAN_POINT('Ctrl Pts',(0.00278585051157554,-0.0334209631343279,
0.07190344491821));
#73764=CARTESIAN_POINT('Ctrl Pts',(0.00282277334565376,-0.0333679869844681,
0.0719189844914907));
#73765=CARTESIAN_POINT('',(0.00275874744665185,-0.0336938721132538,0.0717569024729762));
#73766=CARTESIAN_POINT('Origin',(0.00812378219310841,-0.0315241814719618,
0.07415));
#73767=CARTESIAN_POINT('',(0.00259360130047952,-0.033710812065584,0.0718225337211568));
#73768=CARTESIAN_POINT('',(0.00258864240555081,-0.0336938721132327,0.0718343515957249));
#73769=CARTESIAN_POINT('Origin',(0.0172401493584967,-0.0345562513266994,
0.0791993224028963));
#73770=CARTESIAN_POINT('Ctrl Pts',(0.00258864240555639,-0.0336938721132293,
0.071834351595732));
#73771=CARTESIAN_POINT('Ctrl Pts',(0.00258946671812912,-0.0336910493412779,
0.0718323812252257));
#73772=CARTESIAN_POINT('Ctrl Pts',(0.00259029211961167,-0.0336882266084272,
0.0718304112068913));
#73773=CARTESIAN_POINT('Ctrl Pts',(0.00259194508622508,-0.0336825812712832,
0.0718264719098986));
#73774=CARTESIAN_POINT('Ctrl Pts',(0.00259277265133854,-0.0336797586670018,
0.0718245026312384));
#73775=CARTESIAN_POINT('Ctrl Pts',(0.0025936012992787,-0.033676936124375,
0.071822533720648));
#73776=CARTESIAN_POINT('Origin',(0.0181072094118419,-0.0345562516517652,
0.0771391352255455));
#73777=CARTESIAN_POINT('Ctrl Pts',(0.00288737325788412,-0.0342436276873911,
0.0717713141310582));
#73778=CARTESIAN_POINT('Ctrl Pts',(0.00279765964138925,-0.0339430054201811,
0.071968808549787));
#73779=CARTESIAN_POINT('Ctrl Pts',(0.00272307698070054,-0.0336441434784053,
0.072172499504761));
#73780=CARTESIAN_POINT('Ctrl Pts',(0.00278894799474185,-0.0342436276873911,
0.0720011237643971));
#73781=CARTESIAN_POINT('Ctrl Pts',(0.00270790179145247,-0.0339430054201811,
0.0722023303531213));
#73782=CARTESIAN_POINT('Ctrl Pts',(0.00264224153661118,-0.0336441434784053,
0.0724090700671285));
#73783=CARTESIAN_POINT('Ctrl Pts',(0.00278796374211043,-0.0342436276873911,
0.0720034218607305));
#73784=CARTESIAN_POINT('Ctrl Pts',(0.0027070042129531,-0.0339430054201811,
0.0722046655711546));
#73785=CARTESIAN_POINT('Ctrl Pts',(0.00264143318217029,-0.0336441434784053,
0.0724114357727522));
#73786=CARTESIAN_POINT('',(0.00277553662236825,-0.0341934961088741,0.0720347235842427));
#73787=CARTESIAN_POINT('',(0.00269314705195942,-0.0338664212862887,0.0722562399920861));
#73788=CARTESIAN_POINT('Origin',(0.0181427398522205,-0.034561072040627,
0.0786605977649371));
#73789=CARTESIAN_POINT('Origin',(-0.00766158860517668,-0.0336938005073027,
0.0686453988303866));
#73790=CARTESIAN_POINT('',(0.00273558880092204,-0.0336938721132327,0.0721386579186026));
#73791=CARTESIAN_POINT('',(0.00271500931525608,-0.0336938721132427,0.0721976726182162));
#73792=CARTESIAN_POINT('',(0.00282277334565588,-0.0340203938281605,0.0719189844914858));
#73793=CARTESIAN_POINT('Origin',(0.017886382235818,-0.0345589643246135,
0.0790678047230892));
#73794=CARTESIAN_POINT('',(0.00282402550318816,-0.0341934961088741,0.0719195114822878));
#73795=CARTESIAN_POINT('Origin',(-0.00733256363980539,-0.0341934220717646,
0.0676449453940501));
#73796=CARTESIAN_POINT('',(0.00279978106278821,-0.0341934961088841,0.0719771175332752));
#73797=CARTESIAN_POINT('Ctrl Pts',(0.00268908059037142,-0.0340223579322397,
0.0716075565907498));
#73798=CARTESIAN_POINT('Ctrl Pts',(0.00265401366478708,-0.0339125849573575,
0.0716825153001484));
#73799=CARTESIAN_POINT('Ctrl Pts',(0.0026205228514299,-0.0338030433565231,
0.0717581471408051));
#73800=CARTESIAN_POINT('Ctrl Pts',(0.00258864240555047,-0.0336938721132327,
0.0718343515957243));
#73801=CARTESIAN_POINT('Ctrl Pts',(0.00273409702293709,-0.0340223579322397,
0.0717115503435881));
#73802=CARTESIAN_POINT('Ctrl Pts',(0.00270046444243147,-0.0339125849573575,
0.0717858881589738));
#73803=CARTESIAN_POINT('Ctrl Pts',(0.00266839411519205,-0.0338030433565231,
0.0718608698543025));
#73804=CARTESIAN_POINT('Ctrl Pts',(0.00263791855360951,-0.0336938721132327,
0.0719363959050354));
#73805=CARTESIAN_POINT('Ctrl Pts',(0.00277911345550275,-0.0340223579322397,
0.0718155440964263));
#73806=CARTESIAN_POINT('Ctrl Pts',(0.00274691522007587,-0.0339125849573575,
0.0718892610177992));
#73807=CARTESIAN_POINT('Ctrl Pts',(0.00271626537895419,-0.0338030433565231,
0.0719635925677999));
#73808=CARTESIAN_POINT('Ctrl Pts',(0.00268719470166855,-0.0336938721132327,
0.0720384402143466));
#73809=CARTESIAN_POINT('Ctrl Pts',(0.00282412988806841,-0.0340223579322397,
0.0719195378492646));
#73810=CARTESIAN_POINT('Ctrl Pts',(0.00279336599772027,-0.0339125849573575,
0.0719926338766246));
#73811=CARTESIAN_POINT('Ctrl Pts',(0.00276413664271634,-0.0338030433565231,
0.0720663152812973));
#73812=CARTESIAN_POINT('Ctrl Pts',(0.00273647084972759,-0.0336938721132327,
0.0721404845236578));
#73813=CARTESIAN_POINT('',(0.00266211560324642,-0.0336938721132427,0.0719865047571738));
#73814=CARTESIAN_POINT('Ctrl Pts',(0.0025936013037948,-0.0337108120662688,
0.0718225337225488));
#73815=CARTESIAN_POINT('Ctrl Pts',(0.0026332335812827,-0.0337611408994398,
0.0718392136090115));
#73816=CARTESIAN_POINT('Ctrl Pts',(0.00267214265763427,-0.033812108878153,
0.0718555891245521));
#73817=CARTESIAN_POINT('Ctrl Pts',(0.00274854985358115,-0.0339153382773235,
0.0718877463316092));
#73818=CARTESIAN_POINT('Ctrl Pts',(0.00278601564827816,-0.0339675558473108,
0.0719035144186683));
#73819=CARTESIAN_POINT('Ctrl Pts',(0.00282277334569056,-0.0340203938281304,
0.0719189844915061));
#73820=CARTESIAN_POINT('Ctrl Pts',(0.00277741475298016,-0.0341934961088741,
0.0720339580731138));
#73821=CARTESIAN_POINT('Ctrl Pts',(0.00273366725318469,-0.0340287516182428,
0.0721444900080067));
#73822=CARTESIAN_POINT('Ctrl Pts',(0.0026945255035161,-0.0338644633275951,
0.0722567356128313));
#73823=CARTESIAN_POINT('Ctrl Pts',(0.00277553662236835,-0.0341934961088741,
0.0720347235842427));
#73824=CARTESIAN_POINT('Ctrl Pts',(0.00273180494891239,-0.0340287516182428,
0.0721452943480065));
#73825=CARTESIAN_POINT('Ctrl Pts',(0.0026926806168867,-0.0338644633275951,
0.0722575780944087));
#73826=CARTESIAN_POINT('Ctrl Pts',(0.00246260393800087,-0.0341934961088741,
0.0721622724623588));
#73827=CARTESIAN_POINT('Ctrl Pts',(0.00242150923711545,-0.0340287516182428,
0.0722793128628397));
#73828=CARTESIAN_POINT('Ctrl Pts',(0.00238528701941142,-0.0338644633275951,
0.0723979517297015));
#73829=CARTESIAN_POINT('',(0.00245837103217539,-0.0341764758832382,0.0721743693745735));
#73830=CARTESIAN_POINT('',(0.00246260393800085,-0.034193496108874,0.0721622724623588));
#73831=CARTESIAN_POINT('Origin',(0.0179241615674465,-0.034562102639047,
0.0781099108692202));
#73832=CARTESIAN_POINT('Ctrl Pts',(0.00245837103351531,-0.0341764758837464,
0.0721743693733416));
#73833=CARTESIAN_POINT('Ctrl Pts',(0.00249890174612151,-0.0341260050040274,
0.0721885031462305));
#73834=CARTESIAN_POINT('Ctrl Pts',(0.00253872795190624,-0.0340749269147865,
0.0722023912047264));
#73835=CARTESIAN_POINT('Ctrl Pts',(0.00261700215513479,-0.0339715436305901,
0.0722296868295073));
#73836=CARTESIAN_POINT('Ctrl Pts',(0.0026554204551241,-0.0339192778237013,
0.0722430840460927));
#73837=CARTESIAN_POINT('Ctrl Pts',(0.00269314705147574,-0.0338664212854263,
0.0722562399900086));
#73838=CARTESIAN_POINT('',(0.00261907028019455,-0.0341934961088841,0.0720984980233107));
#73839=CARTESIAN_POINT('Origin',(0.00812378219310841,-0.0315241814719618,
0.07415));
#73840=CARTESIAN_POINT('',(0.00245837103259312,-0.0342105180190372,0.0721743693756105));
#73841=CARTESIAN_POINT('',(0.00245416397318747,-0.0341934961088739,0.0721864753018193));
#73842=CARTESIAN_POINT('Origin',(0.0179439291967614,-0.0345621704431894,
0.0780691208298281));
#73843=CARTESIAN_POINT('Origin',(0.0182614037932373,-0.0345621038666668,
0.0771428264373991));
#73844=CARTESIAN_POINT('Origin',(0.0182515158399669,-0.0345621716292033,
0.0771870617550893));
#73845=CARTESIAN_POINT('Ctrl Pts',(0.00273608271184164,-0.0346945769586965,
0.0721372415564544));
#73846=CARTESIAN_POINT('Ctrl Pts',(0.00269392468037706,-0.0345275153362944,
0.0722500890792067));
#73847=CARTESIAN_POINT('Ctrl Pts',(0.00265530469540775,-0.0343603235965186,
0.0723642916213943));
#73848=CARTESIAN_POINT('Ctrl Pts',(0.00262033195770613,-0.034193496108874,
0.0724795097249739));
#73849=CARTESIAN_POINT('Ctrl Pts',(0.00270847876056665,-0.0346945769586965,
0.0722163999435012));
#73850=CARTESIAN_POINT('Ctrl Pts',(0.00266797873321206,-0.0345275153362944,
0.072329825642065));
#73851=CARTESIAN_POINT('Ctrl Pts',(0.00263103536429461,-0.0343603235965186,
0.0724445543669067));
#73852=CARTESIAN_POINT('Ctrl Pts',(0.00259775287277131,-0.034193496108874,
0.0725602451774675));
#73853=CARTESIAN_POINT('Ctrl Pts',(0.00268087480929167,-0.0346945769586965,
0.0722955583305481));
#73854=CARTESIAN_POINT('Ctrl Pts',(0.00264203278604706,-0.0345275153362944,
0.0724095622049234));
#73855=CARTESIAN_POINT('Ctrl Pts',(0.00260676603318147,-0.0343603235965186,
0.0725248171124188));
#73856=CARTESIAN_POINT('Ctrl Pts',(0.00257517378783649,-0.034193496108874,
0.0726409806299595));
#73857=CARTESIAN_POINT('Ctrl Pts',(0.00265327085801668,-0.0346945769586965,
0.0723747167175948));
#73858=CARTESIAN_POINT('Ctrl Pts',(0.00261608683888205,-0.0345275153362944,
0.0724892987677815));
#73859=CARTESIAN_POINT('Ctrl Pts',(0.00258249670206834,-0.0343603235965186,
0.0726050798579316));
#73860=CARTESIAN_POINT('Ctrl Pts',(0.00255259470290167,-0.034193496108874,
0.0727217160824547));
#73861=CARTESIAN_POINT('',(0.00265327085821636,-0.0346945769586966,0.0723747167170228));
#73862=CARTESIAN_POINT('',(0.00258495299585706,-0.0343667727831436,0.0726009692953471));
#73863=CARTESIAN_POINT('Origin',(0.0187013709783458,-0.0345626457062745,
0.0773902655172281));
#73864=CARTESIAN_POINT('Origin',(-0.00805881704567561,-0.0341934771029153,
0.0696242573967093));
#73865=CARTESIAN_POINT('',(0.0026199279555237,-0.034193496108874,0.0724809543051726));
#73866=CARTESIAN_POINT('',(0.00260309464241975,-0.0341934961088841,0.0725411447493545));
#73867=CARTESIAN_POINT('',(0.00269314705287547,-0.0345211942962717,0.0722562399905395));
#73868=CARTESIAN_POINT('Origin',(0.018539914317741,-0.0345625596119444,
0.0778431700731569));
#73869=CARTESIAN_POINT('',(0.00269442982957011,-0.0346945769586887,0.0722566873178099));
#73870=CARTESIAN_POINT('Origin',(-0.00775217934461158,-0.0346945685853861,
0.0686137665159061));
#73871=CARTESIAN_POINT('',(0.00267385034390324,-0.0346945769587026,0.0723157020174264));
#73872=CARTESIAN_POINT('Ctrl Pts',(0.00254016303781951,-0.0345231616327842,
0.0719538221545793));
#73873=CARTESIAN_POINT('Ctrl Pts',(0.00250989181819146,-0.0344132092796988,
0.072030784483528));
#73874=CARTESIAN_POINT('Ctrl Pts',(0.00248121406548646,-0.034303273855898,
0.0721083689778747));
#73875=CARTESIAN_POINT('Ctrl Pts',(0.0024541639731874,-0.0341934961088739,
0.0721864753018193));
#73876=CARTESIAN_POINT('Ctrl Pts',(0.00259162039115611,-0.0345231616327842,
0.072054783914301));
#73877=CARTESIAN_POINT('Ctrl Pts',(0.00256274078724304,-0.0344132092796988,
0.07213103697608));
#73878=CARTESIAN_POINT('Ctrl Pts',(0.0025354399078201,-0.034303273855898,
0.0722078834553787));
#73879=CARTESIAN_POINT('Ctrl Pts',(0.00250975020665528,-0.0341934961088739,
0.0722852240070632));
#73880=CARTESIAN_POINT('Ctrl Pts',(0.00264307774449271,-0.0345231616327842,
0.0721557456740226));
#73881=CARTESIAN_POINT('Ctrl Pts',(0.00261558975629461,-0.0344132092796988,
0.0722312894686321));
#73882=CARTESIAN_POINT('Ctrl Pts',(0.00258966575015374,-0.034303273855898,
0.0723073979328828));
#73883=CARTESIAN_POINT('Ctrl Pts',(0.00256533644012315,-0.0341934961088739,
0.0723839727123072));
#73884=CARTESIAN_POINT('Ctrl Pts',(0.00269453509782931,-0.0345231616327842,
0.0722567074337443));
#73885=CARTESIAN_POINT('Ctrl Pts',(0.00266843872534619,-0.0344132092796988,
0.0723315419611842));
#73886=CARTESIAN_POINT('Ctrl Pts',(0.00264389159248737,-0.034303273855898,
0.0724069124103868));
#73887=CARTESIAN_POINT('Ctrl Pts',(0.00262092267359103,-0.0341934961088739,
0.0724827214175512));
#73888=CARTESIAN_POINT('',(0.00253704596436558,-0.0341934961088839,0.0723337148035059));
#73889=CARTESIAN_POINT('Ctrl Pts',(0.00245837103584969,-0.0342105180195391,
0.072174369376743));
#73890=CARTESIAN_POINT('Ctrl Pts',(0.00249894730831671,-0.0342610556241328,
0.072188519051716));
#73891=CARTESIAN_POINT('Ctrl Pts',(0.00253879546055414,-0.0343122189870209,
0.0722024148180876));
#73892=CARTESIAN_POINT('Ctrl Pts',(0.0026170704546704,-0.03441581196952,
0.0722297107143816));
#73893=CARTESIAN_POINT('Ctrl Pts',(0.00265546528150917,-0.0344681990450108,
0.0722430996800844));
#73894=CARTESIAN_POINT('Ctrl Pts',(0.00269314705289859,-0.0345211942962537,
0.0722562399905454));
#73895=CARTESIAN_POINT('Ctrl Pts',(0.00265509676874847,-0.0346945769586931,
0.072373835003588));
#73896=CARTESIAN_POINT('Ctrl Pts',(0.0026183758142217,-0.034529677707698,
0.072486896205219));
#73897=CARTESIAN_POINT('Ctrl Pts',(0.0025863591606494,-0.0343648066251421,
0.0726013785082602));
#73898=CARTESIAN_POINT('Ctrl Pts',(0.00265327085821918,-0.0346945769586931,
0.0723747167170142));
#73899=CARTESIAN_POINT('Ctrl Pts',(0.00261656813249361,-0.034529677707698,
0.0724878156680534));
#73900=CARTESIAN_POINT('Ctrl Pts',(0.00258457125236397,-0.0343648066251421,
0.0726023349348334));
#73901=CARTESIAN_POINT('Ctrl Pts',(0.00234896453534388,-0.0346945769586931,
0.072521663112384));
#73902=CARTESIAN_POINT('Ctrl Pts',(0.00231529982236665,-0.034529677707698,
0.0726410533813284));
#73903=CARTESIAN_POINT('Ctrl Pts',(0.00228659838499166,-0.0343648066251421,
0.0727617330263024));
#73904=CARTESIAN_POINT('',(0.00234549955334111,-0.0346775396664966,0.0725340019405017));
#73905=CARTESIAN_POINT('',(0.00234896453534292,-0.0346945769586885,0.0725216631123873));
#73906=CARTESIAN_POINT('Origin',(0.0183740712136008,-0.0345626618126048,
0.0768580961612871));
#73907=CARTESIAN_POINT('Ctrl Pts',(0.00234549955467211,-0.0346775396670096,
0.0725340019392594));
#73908=CARTESIAN_POINT('Ctrl Pts',(0.00238687031335062,-0.0346269749928187,
0.072545571983955));
#73909=CARTESIAN_POINT('Ctrl Pts',(0.00242750583100824,-0.0345757902890786,
0.0725569363685466));
#73910=CARTESIAN_POINT('Ctrl Pts',(0.00250733980358265,-0.0344721681088186,
0.0725792633427411));
#73911=CARTESIAN_POINT('Ctrl Pts',(0.0025465069583118,-0.0344197714290122,
0.0725902171845494));
#73912=CARTESIAN_POINT('Ctrl Pts',(0.00258495299581539,-0.0343667727830592,
0.0726009692950803));
#73913=CARTESIAN_POINT('',(0.00250111769678964,-0.0346945769587026,0.0724481899147151));
#73914=CARTESIAN_POINT('Origin',(0.00812378219310841,-0.0315241814719618,
0.07415));
#73915=CARTESIAN_POINT('',(0.0023454995542768,-0.0347116136489615,0.0725340019415307));
#73916=CARTESIAN_POINT('',(0.00234206093373591,-0.0346945769586885,0.0725463481428481));
#73917=CARTESIAN_POINT('Origin',(0.018384466689097,-0.034562668345578,0.0768139913977689));
#73918=CARTESIAN_POINT('Origin',(0.0182918108157433,-0.0345626629385285,
0.0771522428356373));
#73919=CARTESIAN_POINT('Origin',(0.0182778130545486,-0.0345626694088764,
0.0771953402433519));
#73920=CARTESIAN_POINT('Ctrl Pts',(0.0026312075774452,-0.0352450361874068,
0.0724440144440831));
#73921=CARTESIAN_POINT('Ctrl Pts',(0.0025668652763957,-0.0349452760959493,
0.0726511702949823));
#73922=CARTESIAN_POINT('Ctrl Pts',(0.00251830959135272,-0.034644428984174,
0.072862584163298));
#73923=CARTESIAN_POINT('Ctrl Pts',(0.00263051226227906,-0.0352450361874068,
0.0724464418216433));
#73924=CARTESIAN_POINT('Ctrl Pts',(0.0025662615112765,-0.0349452760959493,
0.0726536238967844));
#73925=CARTESIAN_POINT('Ctrl Pts',(0.00251779909151362,-0.034644428984174,
0.0728650570189173));
#73926=CARTESIAN_POINT('Ctrl Pts',(0.00256166917652225,-0.0352450361874068,
0.0726867762335436));
#73927=CARTESIAN_POINT('Ctrl Pts',(0.00250648278660377,-0.0349452760959493,
0.07289655476827));
#73928=CARTESIAN_POINT('Ctrl Pts',(0.0024672545529891,-0.034644428984174,
0.0731098942089546));
#73929=CARTESIAN_POINT('Ctrl Pts',(0.00256098074566468,-0.0352450361874068,
0.0726891795776626));
#73930=CARTESIAN_POINT('Ctrl Pts',(0.00250588499935705,-0.0349452760959493,
0.0728989840769848));
#73931=CARTESIAN_POINT('Ctrl Pts',(0.00246674910760385,-0.034644428984174,
0.073112342580855));
#73932=CARTESIAN_POINT('',(0.00255260043984588,-0.0351951634053264,0.0727216841474485));
#73933=CARTESIAN_POINT('',(0.00249861816740813,-0.0348678972925388,0.07295181191628));
#73934=CARTESIAN_POINT('Origin',(0.018968118011654,-0.0345636767880447,
0.076028537518523));
#73935=CARTESIAN_POINT('Origin',(-0.00830877103174432,-0.0346946199341129,
0.070649785006046));
#73936=CARTESIAN_POINT('',(0.00252598831263244,-0.0346945769330288,0.0728298376351159));
#73937=CARTESIAN_POINT('',(0.00251296760331662,-0.0346945769458128,0.0728909662881075));
#73938=CARTESIAN_POINT('',(0.00258495299594239,-0.0350221583435276,0.0726009692951326));
#73939=CARTESIAN_POINT('Origin',(0.0189089051229494,-0.0345628458717638,
0.0765056509510742));
#73940=CARTESIAN_POINT('',(0.00258614498873088,-0.035195136029876,0.0726012995161749));
#73941=CARTESIAN_POINT('Origin',(-0.0080256490247682,-0.0351951838366814,
0.0696335273409525));
#73942=CARTESIAN_POINT('',(0.00255259470295588,-0.035195137132875,0.0727217160818296));
#73943=CARTESIAN_POINT('Ctrl Pts',(0.00241328159205483,-0.0350241211494343,
0.0723087550718622));
#73944=CARTESIAN_POINT('Ctrl Pts',(0.00238791919810954,-0.0349144232818962,
0.0723874148762453));
#73945=CARTESIAN_POINT('Ctrl Pts',(0.00236416757791286,-0.0348045283579412,
0.0724666460211186));
#73946=CARTESIAN_POINT('Ctrl Pts',(0.00234206093076571,-0.0346945769439157,
0.0725463481535567));
#73947=CARTESIAN_POINT('Ctrl Pts',(0.00247097687574631,-0.0350241211494343,
0.0724062865849373));
#73948=CARTESIAN_POINT('Ctrl Pts',(0.00244695793840415,-0.0349144232818962,
0.0724841516604435));
#73949=CARTESIAN_POINT('Ctrl Pts',(0.00242453415132036,-0.0348045283579412,
0.0725625598305485));
#73950=CARTESIAN_POINT('Ctrl Pts',(0.0024037379737839,-0.0346945769439157,
0.0726414117331626));
#73951=CARTESIAN_POINT('Ctrl Pts',(0.00252867215943778,-0.0350241211494343,
0.0725038180980124));
#73952=CARTESIAN_POINT('Ctrl Pts',(0.00250599667869876,-0.0349144232818962,
0.0725808884446417));
#73953=CARTESIAN_POINT('Ctrl Pts',(0.00248490072472786,-0.0348045283579412,
0.0726584736399783));
#73954=CARTESIAN_POINT('Ctrl Pts',(0.0024654150168021,-0.0346945769439157,
0.0727364753127685));
#73955=CARTESIAN_POINT('Ctrl Pts',(0.00258636744312925,-0.0350241211494343,
0.0726013496110874));
#73956=CARTESIAN_POINT('Ctrl Pts',(0.00256503541899336,-0.0349144232818962,
0.0726776252288399));
#73957=CARTESIAN_POINT('Ctrl Pts',(0.00254526729813537,-0.0348045283579412,
0.0727543874494082));
#73958=CARTESIAN_POINT('Ctrl Pts',(0.00252709205982029,-0.0346945769439157,
0.0728315388923744));
#73959=CARTESIAN_POINT('',(0.00243402462317538,-0.0346945769458128,0.0726880928886834));
#73960=CARTESIAN_POINT('Ctrl Pts',(0.00234549955743811,-0.0347116136492794,
0.0725340019424112));
#73961=CARTESIAN_POINT('Ctrl Pts',(0.00238685388341253,-0.034762154653232,
0.0725455674047919));
#73962=CARTESIAN_POINT('Ctrl Pts',(0.00242748108858528,-0.0348133084097077,
0.0725569295150907));
#73963=CARTESIAN_POINT('Ctrl Pts',(0.00250731516349295,-0.0349168561544568,
0.0725792565139786));
#73964=CARTESIAN_POINT('Ctrl Pts',(0.00254649036710825,-0.0349692089015911,
0.072590212546582));
#73965=CARTESIAN_POINT('Ctrl Pts',(0.00258495299597225,-0.0350221583435,
0.0726009692951616));
#73966=CARTESIAN_POINT('Ctrl Pts',(0.00255386961196152,-0.0351951371254874,
0.0727209984280599));
#73967=CARTESIAN_POINT('Ctrl Pts',(0.00252432590104789,-0.0350307338980917,
0.0728361528759925));
#73968=CARTESIAN_POINT('Ctrl Pts',(0.00249956689264955,-0.0348659306897818,
0.0729524299985762));
#73969=CARTESIAN_POINT('Ctrl Pts',(0.00255259470306853,-0.0351951371254874,
0.072721716081858));
#73970=CARTESIAN_POINT('Ctrl Pts',(0.0025230658291969,-0.0350307338980917,
0.0728368968877321));
#73971=CARTESIAN_POINT('Ctrl Pts',(0.00249832273456456,-0.0348659306897818,
0.0729531997325036));
#73972=CARTESIAN_POINT('Ctrl Pts',(0.00233891864385632,-0.0351951371254874,
0.0728419956063795));
#73973=CARTESIAN_POINT('Ctrl Pts',(0.00231187647368822,-0.0350307338980917,
0.0729615940307128));
#73974=CARTESIAN_POINT('Ctrl Pts',(0.00228980054282336,-0.0348659306897818,
0.0730822079409672));
#73975=CARTESIAN_POINT('Origin',(-0.00270287367950345,-0.0308609197411111,
0.0718438681262935));
#73976=CARTESIAN_POINT('',(0.00245943675900611,-0.0351951371254874,0.0727741552426069));
#73977=CARTESIAN_POINT('Origin',(0.00909886329211686,-0.0351840467441176,
0.0742129483911409));
#73978=CARTESIAN_POINT('Origin',(-0.00371869835454763,-0.0352322613820738,
0.072440018805345));
#73979=CARTESIAN_POINT('',(0.00245411436176611,-0.0351951142564653,0.0731842457529613));
#73980=CARTESIAN_POINT('',(0.00243582715934136,-0.0351951372916786,0.0733075823281499));
#73981=CARTESIAN_POINT('Origin',(0.00825783852632709,-0.035287511665086,
0.0744630656346189));
#73982=CARTESIAN_POINT('Origin',(0.0106237609097371,-0.0298325076522142,
0.0670757299530051));
#73983=CARTESIAN_POINT('Origin',(0.000904856559393061,-0.0338733559830917,
0.0698917526735384));
#73984=CARTESIAN_POINT('Ctrl Pts',(0.00410481693489538,-0.0321934096636942,
0.0700358714168625));
#73985=CARTESIAN_POINT('Ctrl Pts',(0.00403117599237873,-0.0320508460843247,
0.0701078089811792));
#73986=CARTESIAN_POINT('Ctrl Pts',(0.00395952339578597,-0.0319086045660919,
0.0701816708911563));
#73987=CARTESIAN_POINT('Ctrl Pts',(0.00389000033279445,-0.0317669892864685,
0.0702572854077693));
#73988=CARTESIAN_POINT('Ctrl Pts',(0.00404612609468526,-0.0321934096636942,
0.0700957531160981));
#73989=CARTESIAN_POINT('Ctrl Pts',(0.00397355700606964,-0.0320508460843247,
0.0701687412185063));
#73990=CARTESIAN_POINT('Ctrl Pts',(0.0039030036810822,-0.0319086045660919,
0.0702436240758665));
#73991=CARTESIAN_POINT('Ctrl Pts',(0.00383460475949915,-0.0317669892864685,
0.0703202279457344));
#73992=CARTESIAN_POINT('Ctrl Pts',(0.00398743525447512,-0.0321934096636942,
0.0701556348153335));
#73993=CARTESIAN_POINT('Ctrl Pts',(0.00391593801976054,-0.0320508460843247,
0.0702296734558335));
#73994=CARTESIAN_POINT('Ctrl Pts',(0.00384648396637842,-0.0319086045660919,
0.0703055772605765));
#73995=CARTESIAN_POINT('Ctrl Pts',(0.00377920918620383,-0.0317669892864685,
0.0703831704836995));
#73996=CARTESIAN_POINT('Ctrl Pts',(0.00392874441426499,-0.0321934096636942,
0.0702155165145691));
#73997=CARTESIAN_POINT('Ctrl Pts',(0.00385831903345145,-0.0320508460843247,
0.0702906056931606));
#73998=CARTESIAN_POINT('Ctrl Pts',(0.00378996425167463,-0.0319086045660919,
0.0703675304452866));
#73999=CARTESIAN_POINT('Ctrl Pts',(0.00372381361290853,-0.0317669892864685,
0.0704461130216646));
#74000=CARTESIAN_POINT('',(0.00392979440499592,-0.0321934096636942,0.0702144452191382));
#74001=CARTESIAN_POINT('',(0.00377164489336527,-0.0318665617511256,0.0703900763421073));
#74002=CARTESIAN_POINT('Origin',(0.0156858273485652,-0.0326371944421723,
0.0820893597144095));
#74003=CARTESIAN_POINT('Origin',(-0.00452284489056498,-0.0316939261509002,
0.063224252635214));
#74004=CARTESIAN_POINT('',(0.00401616875752808,-0.0320197221621845,0.0701244440097831));
#74005=CARTESIAN_POINT('Ctrl Pts',(0.00401600987312598,-0.0320197392094761,
0.0701245387231699));
#74006=CARTESIAN_POINT('Ctrl Pts',(0.00399552706552251,-0.0319792716576057,
0.0701454404222029));
#74007=CARTESIAN_POINT('Ctrl Pts',(0.00397511035852195,-0.0319386439829698,
0.0701665934264079));
#74008=CARTESIAN_POINT('Ctrl Pts',(0.00395474440378606,-0.031897909938163,
0.0701880258159594));
#74009=CARTESIAN_POINT('Ctrl Pts',(0.00393437885159715,-0.0318571766984924,
0.0702094577818851));
#74010=CARTESIAN_POINT('Ctrl Pts',(0.00391416626914079,-0.0318163871833565,
0.0702310589635628));
#74011=CARTESIAN_POINT('Ctrl Pts',(0.00389417360827464,-0.0317755399638303,
0.0702527526560048));
#74012=CARTESIAN_POINT('',(0.00401729062974265,-0.0321934096636183,0.070125173663373));
#74013=CARTESIAN_POINT('Origin',(0.00239233619437014,-0.0324040108403075,
0.068561306614717));
#74014=CARTESIAN_POINT('',(0.00397354251737928,-0.0321934096636663,0.0701698094412656));
#74015=CARTESIAN_POINT('Ctrl Pts',(0.00393182252542624,-0.0321934096636618,
0.0702144248500637));
#74016=CARTESIAN_POINT('Ctrl Pts',(0.00387754787690073,-0.0320835708272592,
0.0702722352409033));
#74017=CARTESIAN_POINT('Ctrl Pts',(0.00382450109291094,-0.0319739230346488,
0.0703311353103973));
#74018=CARTESIAN_POINT('Ctrl Pts',(0.00377274425957832,-0.0318646057455573,
0.0703910444911847));
#74019=CARTESIAN_POINT('Ctrl Pts',(0.00381850937687154,-0.0321934096636618,
0.0702155628874739));
#74020=CARTESIAN_POINT('Ctrl Pts',(0.00376425042276885,-0.0320835708272592,
0.0702749359549432));
#74021=CARTESIAN_POINT('Ctrl Pts',(0.00371125166361012,-0.0319739230346488,
0.0703353974698556));
#74022=CARTESIAN_POINT('Ctrl Pts',(0.00365957497074976,-0.0318646057455573,
0.0703968648718049));
#74023=CARTESIAN_POINT('Ctrl Pts',(0.00370519622831685,-0.0321934096636618,
0.0702167009248841));
#74024=CARTESIAN_POINT('Ctrl Pts',(0.00365095296863698,-0.0320835708272592,
0.070277636668983));
#74025=CARTESIAN_POINT('Ctrl Pts',(0.0035980022343093,-0.0319739230346488,
0.0703396596293139));
#74026=CARTESIAN_POINT('Ctrl Pts',(0.0035464056819212,-0.0318646057455573,
0.070402685252425));
#74027=CARTESIAN_POINT('Ctrl Pts',(0.00359188307976215,-0.0321934096636618,
0.0702178389622942));
#74028=CARTESIAN_POINT('Ctrl Pts',(0.0035376555145051,-0.0320835708272592,
0.0702803373830229));
#74029=CARTESIAN_POINT('Ctrl Pts',(0.00348475280500847,-0.0319739230346488,
0.0703439217887722));
#74030=CARTESIAN_POINT('Ctrl Pts',(0.00343323639309263,-0.0318646057455573,
0.0704085056330452));
#74031=CARTESIAN_POINT('',(0.00358349425330485,-0.0321763980308449,0.0702275281516227));
#74032=CARTESIAN_POINT('',(0.00359188307974073,-0.0321934096636184,0.0702178389623189));
#74033=CARTESIAN_POINT('Origin',(0.0156956915595299,-0.0326386231130585,
0.0815023127650536));
#74034=CARTESIAN_POINT('Ctrl Pts',(0.00358349425570071,-0.0321763980306272,
0.0702275281536921));
#74035=CARTESIAN_POINT('Ctrl Pts',(0.00361597161137929,-0.0321259596174965,
0.0702555861788765));
#74036=CARTESIAN_POINT('Ctrl Pts',(0.00364788625473379,-0.0320749164631678,
0.0702831580623622));
#74037=CARTESIAN_POINT('Ctrl Pts',(0.00371061580068031,-0.0319716057793885,
0.070337351734944));
#74038=CARTESIAN_POINT('Ctrl Pts',(0.00374140626170689,-0.0319193786690071,
0.0703639524083413));
#74039=CARTESIAN_POINT('Ctrl Pts',(0.00377164489476594,-0.0318665617525255,
0.0703900763433163));
#74040=CARTESIAN_POINT('',(0.00376083874237832,-0.0321934096636663,0.0702161420907385));
#74041=CARTESIAN_POINT('Origin',(0.00812378219310841,-0.0315241814719618,
0.07415));
#74042=CARTESIAN_POINT('',(0.00358349425302338,-0.0322104233323617,0.0702275281513797));
#74043=CARTESIAN_POINT('',(0.00357512613946538,-0.0321934096636183,0.0702372352350691));
#74044=CARTESIAN_POINT('Origin',(0.0157298205001204,-0.0326387232157297,
0.0814724724679504));
#74045=CARTESIAN_POINT('Origin',(0.0164978436301158,-0.0326386244487335,
0.0805738203269208));
#74046=CARTESIAN_POINT('Origin',(0.0164732718154305,-0.0326387242180456,
0.0806119178557787));
#74047=CARTESIAN_POINT('Ctrl Pts',(0.00387869328062491,-0.0327445246967096,
0.0702696204921284));
#74048=CARTESIAN_POINT('Ctrl Pts',(0.0037323423749724,-0.032443687833936,
0.0704297266378436));
#74049=CARTESIAN_POINT('Ctrl Pts',(0.00359846708604318,-0.0321434074405928,
0.0706004016872655));
#74050=CARTESIAN_POINT('Ctrl Pts',(0.00371407129815008,-0.0327445246967096,
0.0704577683140293));
#74051=CARTESIAN_POINT('Ctrl Pts',(0.00357481650360626,-0.032443687833936,
0.070624083279314));
#74052=CARTESIAN_POINT('Ctrl Pts',(0.00344848484014925,-0.0321434074405928,
0.0708004150016139));
#74053=CARTESIAN_POINT('',(0.00369095475257805,-0.0326943950436612,0.0704855538095802));
#74054=CARTESIAN_POINT('',(0.00354414528154417,-0.0323666188837389,0.0706707686541077));
#74055=CARTESIAN_POINT('Origin',(0.0166961978936742,-0.0326395579112711,
0.0811378638432646));
#74056=CARTESIAN_POINT('Origin',(-0.00525035045722684,-0.0321933825603105,
0.0639894352154793));
#74057=CARTESIAN_POINT('',(0.00362084464535784,-0.0321934096532689,0.0705720566748985));
#74058=CARTESIAN_POINT('',(0.00358303584436114,-0.0321934096584275,0.0706218235806995));
#74059=CARTESIAN_POINT('',(0.00377164489264482,-0.0325210109756239,0.0703900763414779));
#74060=CARTESIAN_POINT('Origin',(0.0163707172064862,-0.0326393129158769,
0.081491766021844));
#74061=CARTESIAN_POINT('',(0.00377267291611207,-0.0326943950436593,0.0703909644774707));
#74062=CARTESIAN_POINT('Origin',(-0.00459844862906292,-0.0326943765538128,
0.063158935663208));
#74063=CARTESIAN_POINT('',(0.00373181383435506,-0.0326943950436702,0.0704382591435355));
#74064=CARTESIAN_POINT('Ctrl Pts',(0.00374073148433831,-0.0325229783203769,
0.0700525780685438));
#74065=CARTESIAN_POINT('Ctrl Pts',(0.00368424861261789,-0.032413025309245,
0.0701129983267132));
#74066=CARTESIAN_POINT('Ctrl Pts',(0.00362902417828721,-0.032303122220807,
0.0701745778417256));
#74067=CARTESIAN_POINT('Ctrl Pts',(0.00357512613654111,-0.0321934096576658,
0.0702372352384686));
#74068=CARTESIAN_POINT('Ctrl Pts',(0.00375140881861494,-0.0325229783203769,
0.0701653926809355));
#74069=CARTESIAN_POINT('Ctrl Pts',(0.00369648109385924,-0.032413025309245,
0.0702256657522854));
#74070=CARTESIAN_POINT('Ctrl Pts',(0.00364280852587634,-0.032303122220807,
0.0702870659325893));
#74071=CARTESIAN_POINT('Ctrl Pts',(0.0035904570901365,-0.0321934096576658,
0.070349512146594));
#74072=CARTESIAN_POINT('Ctrl Pts',(0.00376208615289156,-0.0325229783203769,
0.0702782072933271));
#74073=CARTESIAN_POINT('Ctrl Pts',(0.00370871357510059,-0.032413025309245,
0.0703383331778576));
#74074=CARTESIAN_POINT('Ctrl Pts',(0.00365659287346548,-0.032303122220807,
0.070399554023453));
#74075=CARTESIAN_POINT('Ctrl Pts',(0.00360578804373189,-0.0321934096576658,
0.0704617890547194));
#74076=CARTESIAN_POINT('Ctrl Pts',(0.00377276348716819,-0.0325229783203769,
0.0703910219057188));
#74077=CARTESIAN_POINT('Ctrl Pts',(0.00372094605634195,-0.032413025309245,
0.0704510006034297));
#74078=CARTESIAN_POINT('Ctrl Pts',(0.00367037722105461,-0.032303122220807,
0.0705120421143167));
#74079=CARTESIAN_POINT('Ctrl Pts',(0.00362111899732728,-0.0321934096576658,
0.0705740659628447));
#74080=CARTESIAN_POINT('',(0.00359798539261125,-0.0321934096584275,0.0704046459545161));
#74081=CARTESIAN_POINT('Ctrl Pts',(0.00358349425565004,-0.0322104233328929,
0.0702275281536483));
#74082=CARTESIAN_POINT('Ctrl Pts',(0.00361601561867657,-0.0322609421831325,
0.0702556241979155));
#74083=CARTESIAN_POINT('Ctrl Pts',(0.00364795176034818,-0.0323120888240634,
0.0702832146543609));
#74084=CARTESIAN_POINT('Ctrl Pts',(0.00371068178122496,-0.0324156524631812,
0.0703374087372471));
#74085=CARTESIAN_POINT('Ctrl Pts',(0.00374144987509459,-0.032468026716731,
0.0703639900870716));
#74086=CARTESIAN_POINT('Ctrl Pts',(0.00377164489267473,-0.0325210109755913,
0.0703900763415096));
#74087=CARTESIAN_POINT('Origin',(0.0139469649693696,-0.0262834582512307,
0.0688590711408863));
#74088=CARTESIAN_POINT('Origin',(0.00345130090604331,-0.0342770954208307,
0.0629253641850408));
#74089=CARTESIAN_POINT('Ctrl Pts',(0.00369297710105128,-0.0326943950436604,
0.0704854061698654));
#74090=CARTESIAN_POINT('Ctrl Pts',(0.00364247212989119,-0.0325844576448134,
0.0705464709682477));
#74091=CARTESIAN_POINT('Ctrl Pts',(0.00359322650456347,-0.0324744968375322,
0.0706085846138884));
#74092=CARTESIAN_POINT('Ctrl Pts',(0.00354530222373777,-0.0323646534831894,
0.0706716666528736));
#74093=CARTESIAN_POINT('Ctrl Pts',(0.00357995917170039,-0.0326943950436604,
0.070493656941141));
#74094=CARTESIAN_POINT('Ctrl Pts',(0.00352956791163207,-0.0325844576448134,
0.070556279338408));
#74095=CARTESIAN_POINT('Ctrl Pts',(0.00348046821914228,-0.0324744968375322,
0.0706199483414351));
#74096=CARTESIAN_POINT('Ctrl Pts',(0.00343272187843611,-0.0323646534831894,
0.0706845815060732));
#74097=CARTESIAN_POINT('Ctrl Pts',(0.00346694124234949,-0.0326943950436604,
0.0705019077124166));
#74098=CARTESIAN_POINT('Ctrl Pts',(0.00341666369337294,-0.0325844576448134,
0.0705660877085682));
#74099=CARTESIAN_POINT('Ctrl Pts',(0.0033677099337211,-0.0324744968375322,
0.0706313120689818));
#74100=CARTESIAN_POINT('Ctrl Pts',(0.00332014153313445,-0.0323646534831894,
0.0706974963592727));
#74101=CARTESIAN_POINT('Ctrl Pts',(0.0033539233129986,-0.0326943950436604,
0.0705101584836922));
#74102=CARTESIAN_POINT('Ctrl Pts',(0.00330375947511382,-0.0325844576448134,
0.0705758960787284));
#74103=CARTESIAN_POINT('Ctrl Pts',(0.00325495164829991,-0.0324744968375322,
0.0706426757965286));
#74104=CARTESIAN_POINT('Ctrl Pts',(0.0032075611878328,-0.0323646534831894,
0.0707104112124722));
#74105=CARTESIAN_POINT('',(0.0033461594290625,-0.0326773559991151,0.0705203552922419));
#74106=CARTESIAN_POINT('',(0.00335392331299816,-0.0326943950436594,0.0705101584836928));
#74107=CARTESIAN_POINT('Origin',(0.0165987371531689,-0.0326395670956439,
0.0805254785140288));
#74108=CARTESIAN_POINT('Ctrl Pts',(0.00334615943172621,-0.0326773559987414,
0.0705203552942646));
#74109=CARTESIAN_POINT('Ctrl Pts',(0.00338036198050024,-0.0326267922586118,
0.070546339576884));
#74110=CARTESIAN_POINT('Ctrl Pts',(0.00341395831379564,-0.032575610957966,
0.0705718633068576));
#74111=CARTESIAN_POINT('Ctrl Pts',(0.00347996714161408,-0.0324719985462366,
0.0706220113835035));
#74112=CARTESIAN_POINT('Ctrl Pts',(0.00351235316176784,-0.032419609162177,
0.0706466156171281));
#74113=CARTESIAN_POINT('Ctrl Pts',(0.00354414528158299,-0.0323666188837756,
0.0706707686541372));
#74114=CARTESIAN_POINT('',(0.0035224390327981,-0.0326943950436703,0.0704978561466466));
#74115=CARTESIAN_POINT('Origin',(0.00812378219310841,-0.0315241814719618,
0.07415));
#74116=CARTESIAN_POINT('',(0.0033461594290972,-0.0327114338379875,0.0705203552922685));
#74117=CARTESIAN_POINT('',(0.00333841734075972,-0.0326943950436593,0.0705305686593156));
#74118=CARTESIAN_POINT('Origin',(0.0166255274977898,-0.0326395666325422,
0.0804889356024141));
#74119=CARTESIAN_POINT('Origin',(0.0165379545151668,-0.0326395680308184,
0.0806054893179686));
#74120=CARTESIAN_POINT('Origin',(0.0165099277966083,-0.0326395676864378,
0.0806410927357026));
#74121=CARTESIAN_POINT('Ctrl Pts',(0.00364339435499156,-0.0332451089994433,
0.070543859428689));
#74122=CARTESIAN_POINT('Ctrl Pts',(0.00350738653814015,-0.0329451141710254,
0.070712840020671));
#74123=CARTESIAN_POINT('Ctrl Pts',(0.00338449341412824,-0.0326442513127494,
0.0708915852213949));
#74124=CARTESIAN_POINT('Ctrl Pts',(0.00349091246699706,-0.0332451089994433,
0.0707419737235636));
#74125=CARTESIAN_POINT('Ctrl Pts',(0.00336237665302521,-0.0329451141710254,
0.0709167052640417));
#74126=CARTESIAN_POINT('Ctrl Pts',(0.00324736748967208,-0.0326442513127494,
0.0711006222536213));
#74127=CARTESIAN_POINT('Ctrl Pts',(0.00348938764811711,-0.0332451089994433,
0.0707439548665123));
#74128=CARTESIAN_POINT('Ctrl Pts',(0.00336092655417406,-0.0329451141710254,
0.0709187439164753));
#74129=CARTESIAN_POINT('Ctrl Pts',(0.00324599623042752,-0.0326442513127494,
0.0711027126239436));
#74130=CARTESIAN_POINT('',(0.00346960944486475,-0.0331951640388616,0.0707711242950492));
#74131=CARTESIAN_POINT('',(0.00333471939232407,-0.0328677532354985,0.0709651919115967));
#74132=CARTESIAN_POINT('Origin',(0.0174724975217998,-0.0326402808279898,
0.079988031204783));
#74133=CARTESIAN_POINT('Origin',(-0.0058716122919306,-0.0326944278779021,
0.0648432771865053));
#74134=CARTESIAN_POINT('',(0.00340506923980481,-0.0326943950436593,0.0708618587219638));
#74135=CARTESIAN_POINT('',(0.00337045993753886,-0.0326943950436694,0.0709139014562983));
#74136=CARTESIAN_POINT('',(0.00354414528154591,-0.0330220786163545,0.0706707686541055));
#74137=CARTESIAN_POINT('Origin',(0.0172329945527583,-0.0326396682765297,
0.0804049136502552));
#74138=CARTESIAN_POINT('',(0.0035452270429651,-0.0331951640388587,0.0706715904874359));
#74139=CARTESIAN_POINT('Origin',(-0.00523895195084356,-0.0331952026560205,
0.0639980929800267));
#74140=CARTESIAN_POINT('',(0.00350741824392492,-0.0331951640388701,0.0707213573912525));
#74141=CARTESIAN_POINT('Ctrl Pts',(0.0034921005710676,-0.0330240426238172,
0.0703358781676416));
#74142=CARTESIAN_POINT('Ctrl Pts',(0.00343955732690801,-0.032914277406352,
0.070399684094414));
#74143=CARTESIAN_POINT('Ctrl Pts',(0.0033883069347644,-0.0328043479726691,
0.070464608046397));
#74144=CARTESIAN_POINT('Ctrl Pts',(0.00333841734075968,-0.0326943950436593,
0.0705305686593156));
#74145=CARTESIAN_POINT('Ctrl Pts',(0.0035098405377922,-0.0330240426238172,
0.0704477997007132));
#74146=CARTESIAN_POINT('Ctrl Pts',(0.00345883912179054,-0.032914277406352,
0.0705113612421608));
#74147=CARTESIAN_POINT('Ctrl Pts',(0.0034091262743351,-0.0328043479726691,
0.0705760088130891));
#74148=CARTESIAN_POINT('Ctrl Pts',(0.00336076796208867,-0.0326943950436593,
0.0706416613490422));
#74149=CARTESIAN_POINT('Ctrl Pts',(0.0035275805045168,-0.0330240426238172,
0.0705597212337848));
#74150=CARTESIAN_POINT('Ctrl Pts',(0.00347812091667307,-0.032914277406352,
0.0706230383899076));
#74151=CARTESIAN_POINT('Ctrl Pts',(0.0034299456139058,-0.0328043479726691,
0.0706874095797811));
#74152=CARTESIAN_POINT('Ctrl Pts',(0.00338311858341766,-0.0326943950436593,
0.0707527540387689));
#74153=CARTESIAN_POINT('Ctrl Pts',(0.0035453204712414,-0.0330240426238172,
0.0706716427668565));
#74154=CARTESIAN_POINT('Ctrl Pts',(0.00349740271155559,-0.032914277406352,
0.0707347155376544));
#74155=CARTESIAN_POINT('Ctrl Pts',(0.0034507649534765,-0.0328043479726691,
0.0707988103464731));
#74156=CARTESIAN_POINT('Ctrl Pts',(0.00340546920474664,-0.0326943950436593,
0.0708638467284955));
#74157=CARTESIAN_POINT('',(0.00337174329029227,-0.0326943950436693,0.0706962136906497));
#74158=CARTESIAN_POINT('Ctrl Pts',(0.00334615943173144,-0.0327114338383327,
0.0705203552942685));
#74159=CARTESIAN_POINT('Ctrl Pts',(0.00338035629151675,-0.0327619876831051,
0.0705463352548623));
#74160=CARTESIAN_POINT('Ctrl Pts',(0.00341394984605243,-0.0328131562604493,
0.070571856873763));
#74161=CARTESIAN_POINT('Ctrl Pts',(0.00347995861321972,-0.0329167375858768,
0.0706220049043311));
#74162=CARTESIAN_POINT('Ctrl Pts',(0.00351234752457318,-0.0329691088920619,
0.0706466113344513));
#74163=CARTESIAN_POINT('Ctrl Pts',(0.00354414528158209,-0.0330220786163187,
0.0706707686541364));
#74164=CARTESIAN_POINT('Ctrl Pts',(0.00347161885306906,-0.0331951640388604,
0.0707708499185587));
#74165=CARTESIAN_POINT('Ctrl Pts',(0.00340175709164472,-0.0330306422010619,
0.0708670304129244));
#74166=CARTESIAN_POINT('Ctrl Pts',(0.00333593026758393,-0.0328657861914645,
0.0709660161817996));
#74167=CARTESIAN_POINT('Ctrl Pts',(0.00346960944486666,-0.0331951640388604,
0.0707711242950467));
#74168=CARTESIAN_POINT('Ctrl Pts',(0.00339975335600029,-0.0330306422010619,
0.0708673463326386));
#74169=CARTESIAN_POINT('Ctrl Pts',(0.00333393391667554,-0.0328657861914645,
0.0709663733747889));
#74170=CARTESIAN_POINT('Ctrl Pts',(0.00313478800011482,-0.0331951640388604,
0.0708168427966452));
#74171=CARTESIAN_POINT('Ctrl Pts',(0.00306587711195702,-0.0330306422010619,
0.0709199870529398));
#74172=CARTESIAN_POINT('Ctrl Pts',(0.00300128816825202,-0.0328657861914645,
0.0710258913326662));
#74173=CARTESIAN_POINT('',(0.00312767969860762,-0.0331781648281888,0.0708275069811679));
#74174=CARTESIAN_POINT('',(0.00313478800011414,-0.0331951640388588,0.0708168427966462));
#74175=CARTESIAN_POINT('Origin',(0.0172671593927324,-0.0326412091979399,
0.0793751147514508));
#74176=CARTESIAN_POINT('Ctrl Pts',(0.00312767970031722,-0.033178164828644,
0.0708275069804985));
#74177=CARTESIAN_POINT('Ctrl Pts',(0.00316347095534084,-0.0331276811546778,
0.0708513087584733));
#74178=CARTESIAN_POINT('Ctrl Pts',(0.00319861594986478,-0.0330765663497786,
0.0708746807218895));
#74179=CARTESIAN_POINT('Ctrl Pts',(0.00326764352385894,-0.0329730614462931,
0.0709205852352549));
#74180=CARTESIAN_POINT('Ctrl Pts',(0.00330149821473158,-0.0329207133373202,
0.0709430992452487));
#74181=CARTESIAN_POINT('Ctrl Pts',(0.00333471939280908,-0.0328677532289346,
0.0709651918951324));
#74182=CARTESIAN_POINT('',(0.00330219872249944,-0.0331951640388701,0.0707939835458577));
#74183=CARTESIAN_POINT('Origin',(0.00812378219310841,-0.0315241814719618,
0.07415));
#74184=CARTESIAN_POINT('',(0.00312767969954,-0.0332121607144422,0.0708275069825649));
#74185=CARTESIAN_POINT('',(0.00312059419090093,-0.0331951640388587,0.0708381863255022));
#74186=CARTESIAN_POINT('Origin',(0.0172853622406674,-0.0326413648569167,
0.0793335826227612));
#74187=CARTESIAN_POINT('Origin',(0.0164783289049674,-0.0326412101666988,
0.0805613003101866));
#74188=CARTESIAN_POINT('Origin',(0.0164470635230991,-0.0326413658922313,
0.0805941455259154));
#74189=CARTESIAN_POINT('Ctrl Pts',(0.00342581595379246,-0.0337436976235975,
0.0708322841872385));
#74190=CARTESIAN_POINT('Ctrl Pts',(0.0033959759149589,-0.0336723290703325,
0.0708745384075912));
#74191=CARTESIAN_POINT('Ctrl Pts',(0.00336690072378216,-0.033601104548885,
0.0709173225204514));
#74192=CARTESIAN_POINT('Ctrl Pts',(0.00327406939782573,-0.0333736987606858,
0.0710539237177589));
#74193=CARTESIAN_POINT('Ctrl Pts',(0.00318923001488756,-0.0331450831799193,
0.071195627003844));
#74194=CARTESIAN_POINT('Ctrl Pts',(0.00328607390263732,-0.0337436976235975,
0.0710395814596252));
#74195=CARTESIAN_POINT('Ctrl Pts',(0.00325809832688837,-0.0336723290703325,
0.0710830925411644));
#74196=CARTESIAN_POINT('Ctrl Pts',(0.00323090990414125,-0.033601104548885,
0.0711270997760665));
#74197=CARTESIAN_POINT('Ctrl Pts',(0.00314410265603281,-0.0333736987606858,
0.0712676061597666));
#74198=CARTESIAN_POINT('Ctrl Pts',(0.00306550152585123,-0.0331450831799193,
0.0714128625004848));
#74199=CARTESIAN_POINT('Ctrl Pts',(0.00328467648212577,-0.0337436976235975,
0.0710416544323491));
#74200=CARTESIAN_POINT('Ctrl Pts',(0.00325671955100766,-0.0336723290703325,
0.0710851780825002));
#74201=CARTESIAN_POINT('Ctrl Pts',(0.00322954999594483,-0.033601104548885,
0.0711291975486227));
#74202=CARTESIAN_POINT('Ctrl Pts',(0.00314280298861488,-0.0333736987606858,
0.0712697429841868));
#74203=CARTESIAN_POINT('Ctrl Pts',(0.00306426424096087,-0.0331450831799193,
0.0714150348554512));
#74204=CARTESIAN_POINT('',(0.00326663203069243,-0.0336938721132548,0.0710700296592754));
#74205=CARTESIAN_POINT('',(0.00314419376792775,-0.0333679869945434,0.0712721841414624));
#74206=CARTESIAN_POINT('Ctrl Pts',(0.00326663203069023,-0.0336938721132646,
0.0710700296592773));
#74207=CARTESIAN_POINT('Ctrl Pts',(0.00325460946161088,-0.0336629187933929,
0.0710889893948913));
#74208=CARTESIAN_POINT('Ctrl Pts',(0.00324270175451054,-0.0336319952301037,
0.0711080134637059));
#74209=CARTESIAN_POINT('Ctrl Pts',(0.00323090990413955,-0.0336011045488947,
0.0711270997760688));
#74210=CARTESIAN_POINT('Ctrl Pts',(0.0032013201166146,-0.0335235892595451,
0.071174993864756));
#74211=CARTESIAN_POINT('Ctrl Pts',(0.00317240740429413,-0.0334458668660366,
0.0712233650700992));
#74212=CARTESIAN_POINT('Ctrl Pts',(0.00314419376764526,-0.0333679869945382,
0.0712721841412908));
#74213=CARTESIAN_POINT('Ctrl Pts',(0.00314417092095408,-0.0333679692460735,
0.071272222300142));
#74214=CARTESIAN_POINT('Ctrl Pts',(0.00314456628424068,-0.033339189537642,
0.0712724439433076));
#74215=CARTESIAN_POINT('Ctrl Pts',(0.00314486421620311,-0.0333104081062908,
0.0712726072432279));
#74216=CARTESIAN_POINT('Ctrl Pts',(0.00314526124204551,-0.0332532698353254,
0.0712728185417925));
#74217=CARTESIAN_POINT('Ctrl Pts',(0.00314536323838122,-0.0332249171884949,
0.0712728682228483));
#74218=CARTESIAN_POINT('Ctrl Pts',(0.00314536986861459,-0.0331960985339516,
0.071272864085671));
#74219=CARTESIAN_POINT('Ctrl Pts',(0.00314536995033752,-0.0331956312585707,
0.0712728640037306));
#74220=CARTESIAN_POINT('Ctrl Pts',(0.00314537000600209,-0.0331951640388598,
0.0712728639074122));
#74221=CARTESIAN_POINT('',(0.00320791644279702,-0.0331951640388587,0.0711646375555192));
#74222=CARTESIAN_POINT('',(0.00317664322440935,-0.0331951640388689,0.071218750731476));
#74223=CARTESIAN_POINT('',(0.00333471940553021,-0.0335216366567748,0.0709651919034373));
#74224=CARTESIAN_POINT('Origin',(0.0178364699876207,-0.0326434571528789,
0.0791548130834105));
#74225=CARTESIAN_POINT('',(0.00333585063525283,-0.0336938721132327,0.070965944190613));
#74226=CARTESIAN_POINT('Origin',(-0.00575752938773102,-0.0336938867896278,
0.0649186911191892));
#74227=CARTESIAN_POINT('',(0.00330124133298263,-0.0336938721132538,0.0710179869249542));
#74228=CARTESIAN_POINT('Ctrl Pts',(0.00326174888219176,-0.0335235895815171,
0.070634230939956));
#74229=CARTESIAN_POINT('Ctrl Pts',(0.00321334739916796,-0.0334144449262748,
0.0707011664009435));
#74230=CARTESIAN_POINT('Ctrl Pts',(0.00316627314495361,-0.0333049234473147,
0.0707691787008793));
#74231=CARTESIAN_POINT('Ctrl Pts',(0.00312059419090086,-0.0331951640388587,
0.070838186325502));
#74232=CARTESIAN_POINT('Ctrl Pts',(0.00328648150721761,-0.0335235895815171,
0.070744817872933));
#74233=CARTESIAN_POINT('Ctrl Pts',(0.00323960247105187,-0.0334144449262748,
0.0708114128406429));
#74234=CARTESIAN_POINT('Ctrl Pts',(0.00319404537846771,-0.0333049234473147,
0.0708790528035093));
#74235=CARTESIAN_POINT('Ctrl Pts',(0.00314987631770572,-0.0331951640388587,
0.0709476565476434));
#74236=CARTESIAN_POINT('Ctrl Pts',(0.00331121413224346,-0.0335235895815172,
0.0708554048059099));
#74237=CARTESIAN_POINT('Ctrl Pts',(0.00326585754293578,-0.0334144449262748,
0.0709216592803423));
#74238=CARTESIAN_POINT('Ctrl Pts',(0.00322181761198181,-0.0333049234473147,
0.0709889269061394));
#74239=CARTESIAN_POINT('Ctrl Pts',(0.00317915844451057,-0.0331951640388587,
0.0710571267697849));
#74240=CARTESIAN_POINT('Ctrl Pts',(0.00333594675726931,-0.0335235895815172,
0.0709659917388869));
#74241=CARTESIAN_POINT('Ctrl Pts',(0.00329211261481969,-0.0334144449262748,
0.0710319057200417));
#74242=CARTESIAN_POINT('Ctrl Pts',(0.00324958984549591,-0.0333049234473147,
0.0710988010087694));
#74243=CARTESIAN_POINT('Ctrl Pts',(0.00320844057131542,-0.0331951640388587,
0.0711665969919264));
#74244=CARTESIAN_POINT('',(0.00316425531685898,-0.0331951640388687,0.0710014119405206));
#74245=CARTESIAN_POINT('Ctrl Pts',(0.00312767970214249,-0.0332121607145979,
0.0708275069842939));
#74246=CARTESIAN_POINT('Ctrl Pts',(0.00316341074044679,-0.0332625444109863,
0.0708512687316609));
#74247=CARTESIAN_POINT('Ctrl Pts',(0.00319852607688945,-0.0333135300747045,
0.0708746210268322));
#74248=CARTESIAN_POINT('Ctrl Pts',(0.00326755322012772,-0.0334167203140649,
0.0709205252495173));
#74249=CARTESIAN_POINT('Ctrl Pts',(0.00330143829216079,-0.0334688847587354,
0.0709430593979601));
#74250=CARTESIAN_POINT('Ctrl Pts',(0.00333471940602311,-0.033521636656244,
0.0709651919039611));
#74251=CARTESIAN_POINT('Ctrl Pts',(0.00326761224679909,-0.033693872113239,
0.0710698324506134));
#74252=CARTESIAN_POINT('Ctrl Pts',(0.00324958300402455,-0.0336474569764958,
0.0710982572247573));
#74253=CARTESIAN_POINT('Ctrl Pts',(0.00323188774449564,-0.033601104548885,
0.0711268911062677));
#74254=CARTESIAN_POINT('Ctrl Pts',(0.00318708741576369,-0.0334837508592656,
0.07119938551091));
#74255=CARTESIAN_POINT('Ctrl Pts',(0.00314445491954967,-0.0333660264659097,
0.0712731756079792));
#74256=CARTESIAN_POINT('Ctrl Pts',(0.00326663203070348,-0.033693872113239,
0.0710700296592581));
#74257=CARTESIAN_POINT('Ctrl Pts',(0.00324860394225659,-0.0336474569764958,
0.071098460170932));
#74258=CARTESIAN_POINT('Ctrl Pts',(0.00323090990414125,-0.033601104548885,
0.0711270997760665));
#74259=CARTESIAN_POINT('Ctrl Pts',(0.00318611266774766,-0.0334837508592656,
0.0711996086716091));
#74260=CARTESIAN_POINT('Ctrl Pts',(0.00314348369190948,-0.0333660264659097,
0.0712734131615827));
#74261=CARTESIAN_POINT('Ctrl Pts',(0.00293335422767099,-0.033693872113239,
0.0711370814696989));
#74262=CARTESIAN_POINT('Ctrl Pts',(0.00291571861572076,-0.0336474569764958,
0.0711674627669472));
#74263=CARTESIAN_POINT('Ctrl Pts',(0.00289843986361754,-0.033601104548885,
0.0711980484295541));
#74264=CARTESIAN_POINT('Ctrl Pts',(0.0028546940359264,-0.0334837508592655,
0.0712754842951902));
#74265=CARTESIAN_POINT('Ctrl Pts',(0.00281326200342863,-0.0333660264659097,
0.0713541824362755));
#74266=CARTESIAN_POINT('',(0.00292891730221443,-0.0336769361243753,0.0711477710338222));
#74267=CARTESIAN_POINT('',(0.00293534196805525,-0.0336938721132327,0.0711366815583065));
#74268=CARTESIAN_POINT('Ctrl Pts',(0.00292891730221426,-0.033676936124375,
0.0711477710338225));
#74269=CARTESIAN_POINT('Ctrl Pts',(0.0029299861859421,-0.0336797586669841,
0.0711459215058175));
#74270=CARTESIAN_POINT('Ctrl Pts',(0.00293105601697502,-0.0336825812712478,
0.0711440726185949));
#74271=CARTESIAN_POINT('Ctrl Pts',(0.0029331975748887,-0.033688226607443,
0.0711403761225528));
#74272=CARTESIAN_POINT('Ctrl Pts',(0.00293426930175874,-0.0336910493393091,
0.0711385285137804));
#74273=CARTESIAN_POINT('Ctrl Pts',(0.00293534196806087,-0.0336938721132307,
0.0711366815583066));
#74274=CARTESIAN_POINT('Ctrl Pts',(0.00292891730221448,-0.0336769361243754,
0.0711477710338222));
#74275=CARTESIAN_POINT('Ctrl Pts',(0.0029652049241925,-0.0336279031301482,
0.0711687424646687));
#74276=CARTESIAN_POINT('Ctrl Pts',(0.0030020146345147,-0.0335767851899347,
0.0711900156220816));
#74277=CARTESIAN_POINT('Ctrl Pts',(0.00307414236519179,-0.0334733198857316,
0.0712316998558108));
#74278=CARTESIAN_POINT('Ctrl Pts',(0.00310950881498663,-0.0334209645014074,
0.0712521389205869));
#74279=CARTESIAN_POINT('Ctrl Pts',(0.0031441937715641,-0.0333679869844682,
0.0712721841351429));
#74280=CARTESIAN_POINT('',(0.00310098699938384,-0.0336938721132538,0.071103355608801));
#74281=CARTESIAN_POINT('Origin',(0.00812378219310841,-0.0315241814719618,
0.07415));
#74282=CARTESIAN_POINT('',(0.00292891730334296,-0.0337108120655685,0.0711477710344767));
#74283=CARTESIAN_POINT('',(0.00292251633834766,-0.0336938721132327,0.0711588742072383));
#74284=CARTESIAN_POINT('Origin',(0.0165354160029626,-0.0345562514102215,
0.0803020907901988));
#74285=CARTESIAN_POINT('Ctrl Pts',(0.00292251633835219,-0.0336938721132294,
0.0711588742072459));
#74286=CARTESIAN_POINT('Ctrl Pts',(0.00292358110397635,-0.0336910493410251,
0.0711570226872939));
#74287=CARTESIAN_POINT('Ctrl Pts',(0.00292464690564218,-0.0336882266083007,
0.0711551716534623));
#74288=CARTESIAN_POINT('Ctrl Pts',(0.00292678056290971,-0.0336825812712639,
0.0711514705907239));
#74289=CARTESIAN_POINT('Ctrl Pts',(0.0029278484184837,-0.0336797586669922,
0.0711496205618321));
#74290=CARTESIAN_POINT('Ctrl Pts',(0.00292891730221458,-0.033676936124375,
0.0711477710338219));
#74291=CARTESIAN_POINT('Origin',(0.0176538489882102,-0.0345562515768689,
0.078366820253175));
#74292=CARTESIAN_POINT('Ctrl Pts',(0.00322679229796606,-0.0342436276873911,
0.0711337747154972));
#74293=CARTESIAN_POINT('Ctrl Pts',(0.00311303348602325,-0.0339430054201811,
0.0713184677340956));
#74294=CARTESIAN_POINT('Ctrl Pts',(0.00301350968585616,-0.0336441434784053,
0.0715112048390181));
#74295=CARTESIAN_POINT('Ctrl Pts',(0.00310034036297127,-0.0342436276873911,
0.0713494362747424));
#74296=CARTESIAN_POINT('Ctrl Pts',(0.00299471536082295,-0.0339430054201811,
0.0715388985066906));
#74297=CARTESIAN_POINT('Ctrl Pts',(0.00290366149984018,-0.0336441434784053,
0.0717357786042467));
#74298=CARTESIAN_POINT('Ctrl Pts',(0.00309907584362133,-0.0342436276873911,
0.0713515928903348));
#74299=CARTESIAN_POINT('Ctrl Pts',(0.00299353217957095,-0.0339430054201811,
0.0715411028144165));
#74300=CARTESIAN_POINT('Ctrl Pts',(0.00290256301798002,-0.0336441434784053,
0.071738024341899));
#74301=CARTESIAN_POINT('',(0.00308282356920625,-0.0341934961088741,0.0713810902593065));
#74302=CARTESIAN_POINT('',(0.0029733202979627,-0.0338664212863039,0.0715905337923547));
#74303=CARTESIAN_POINT('Origin',(0.0174984095754237,-0.0345610720405512,
0.0798807387145763));
#74304=CARTESIAN_POINT('Origin',(-0.00684720665499033,-0.0336938005073043,
0.0667103724431221));
#74305=CARTESIAN_POINT('',(0.00303016432206031,-0.0336938721132327,0.0714791982507606));
#74306=CARTESIAN_POINT('',(0.00300235060865654,-0.0336938721132428,0.0715351683083563));
#74307=CARTESIAN_POINT('',(0.00314419377156682,-0.0340203938281605,0.0712721841351383));
#74308=CARTESIAN_POINT('Origin',(0.0171930368507349,-0.0345589643244692,
0.0802526045951889));
#74309=CARTESIAN_POINT('',(0.00314537000600162,-0.034193496108874,0.0712728639074129));
#74310=CARTESIAN_POINT('Origin',(-0.0063953862268463,-0.0341934220717719,
0.0657590459209844));
#74311=CARTESIAN_POINT('',(0.00311409678761393,-0.0341934961088841,0.0713269770833697));
#74312=CARTESIAN_POINT('Ctrl Pts',(0.00305058748941132,-0.0340223579322397,
0.0709464557910948));
#74313=CARTESIAN_POINT('Ctrl Pts',(0.00300640225957646,-0.0339125849573575,
0.071016428377506));
#74314=CARTESIAN_POINT('Ctrl Pts',(0.00296369634813591,-0.0338030433565231,
0.0710872663265762));
#74315=CARTESIAN_POINT('Ctrl Pts',(0.00292251633834744,-0.0336938721132327,
0.0711588742072376));
#74316=CARTESIAN_POINT('Ctrl Pts',(0.00308221508064672,-0.0340223579322397,
0.0710552715771874));
#74317=CARTESIAN_POINT('Ctrl Pts',(0.00303953070430557,-0.0339125849573575,
0.0711248079366273));
#74318=CARTESIAN_POINT('Ctrl Pts',(0.00299831556284169,-0.0338030433565231,
0.071195178901078));
#74319=CARTESIAN_POINT('Ctrl Pts',(0.00295861438600814,-0.0336938721132327,
0.0712662898056645));
#74320=CARTESIAN_POINT('Ctrl Pts',(0.00311384267188213,-0.0340223579322397,
0.0711640873632801));
#74321=CARTESIAN_POINT('Ctrl Pts',(0.00307265914903468,-0.0339125849573575,
0.0712331874957486));
#74322=CARTESIAN_POINT('Ctrl Pts',(0.00303293477754747,-0.0338030433565231,
0.0713030914755798));
#74323=CARTESIAN_POINT('Ctrl Pts',(0.00299471243366884,-0.0336938721132327,
0.0713737054040914));
#74324=CARTESIAN_POINT('Ctrl Pts',(0.00314547026311753,-0.0340223579322397,
0.0712729031493728));
#74325=CARTESIAN_POINT('Ctrl Pts',(0.00310578759376378,-0.0339125849573575,
0.0713415670548699));
#74326=CARTESIAN_POINT('Ctrl Pts',(0.00306755399225326,-0.0338030433565231,
0.0714110040500815));
#74327=CARTESIAN_POINT('Ctrl Pts',(0.00303081048132955,-0.0336938721132327,
0.0714811210025183));
#74328=CARTESIAN_POINT('',(0.00297634033021399,-0.0336938721132427,0.0713190362290094));
#74329=CARTESIAN_POINT('Ctrl Pts',(0.00292891730645694,-0.0337108120662688,
0.071147771036274));
#74330=CARTESIAN_POINT('Ctrl Pts',(0.00296614652749129,-0.033761140899437,
0.0711692866383397));
#74331=CARTESIAN_POINT('Ctrl Pts',(0.00300269639783767,-0.0338121088781463,
0.0711904096284017));
#74332=CARTESIAN_POINT('Ctrl Pts',(0.00307447073348461,-0.0339153382773235,
0.0712318896272146));
#74333=CARTESIAN_POINT('Ctrl Pts',(0.00310966483386169,-0.0339675558473108,
0.0712522290873949));
#74334=CARTESIAN_POINT('Ctrl Pts',(0.00314419377159869,-0.0340203938281304,
0.0712721841351628));
#74335=CARTESIAN_POINT('Ctrl Pts',(0.00308478283418244,-0.0341934961088741,
0.0713805661766441));
#74336=CARTESIAN_POINT('Ctrl Pts',(0.00302752697167734,-0.0340287516182428,
0.0714847435186065));
#74337=CARTESIAN_POINT('Ctrl Pts',(0.00297462576178992,-0.0338644633275951,
0.0715911982712576));
#74338=CARTESIAN_POINT('Ctrl Pts',(0.00308282356920633,-0.0341934961088741,
0.0713810902593065));
#74339=CARTESIAN_POINT('Ctrl Pts',(0.0030255785416974,-0.0340287516182428,
0.0714853081075287));
#74340=CARTESIAN_POINT('Ctrl Pts',(0.00297268983170229,-0.0338644633275951,
0.0715918028840092));
#74341=CARTESIAN_POINT('Ctrl Pts',(0.00275637233919177,-0.0341934961088741,
0.071468412511202));
#74342=CARTESIAN_POINT('Ctrl Pts',(0.00270093263044727,-0.0340287516182428,
0.0715793794814226));
#74343=CARTESIAN_POINT('Ctrl Pts',(0.00265012664293871,-0.0338644633275951,
0.0716925429977116));
#74344=CARTESIAN_POINT('',(0.0027506566659699,-0.034176475883238,0.0714798835118756));
#74345=CARTESIAN_POINT('',(0.00275637233919176,-0.034193496108874,0.0714684125112019));
#74346=CARTESIAN_POINT('Origin',(0.0173505741629366,-0.034562102665955,
0.0793069990404853));
#74347=CARTESIAN_POINT('Ctrl Pts',(0.00275065666745294,-0.0341764758837462,
0.071479883510822));
#74348=CARTESIAN_POINT('Ctrl Pts',(0.00278909635182647,-0.0341260050040262,
0.0714989856799601));
#74349=CARTESIAN_POINT('Ctrl Pts',(0.00282686788080487,-0.0340749269147838,
0.0715177557741188));
#74350=CARTESIAN_POINT('Ctrl Pts',(0.00290110381968543,-0.0339715436305319,
0.0715546465237605));
#74351=CARTESIAN_POINT('Ctrl Pts',(0.0029375400635527,-0.0339192778234585,
0.0715727531891187));
#74352=CARTESIAN_POINT('Ctrl Pts',(0.00297332029732877,-0.0338664212853344,
0.0715905337907483));
#74353=CARTESIAN_POINT('',(0.00291959795420901,-0.0341934961088841,0.0714247513852643));
#74354=CARTESIAN_POINT('Origin',(0.00812378219310841,-0.0315241814719618,
0.07415));
#74355=CARTESIAN_POINT('',(0.00275065666625436,-0.0342105180190544,0.071479883512957));
#74356=CARTESIAN_POINT('',(0.00274496550589082,-0.0341934961088739,0.0714913666959631));
#74357=CARTESIAN_POINT('Origin',(0.0173752979548923,-0.0345621706502888,
0.0792690082965156));
#74358=CARTESIAN_POINT('Origin',(0.0178063648150556,-0.0345621037473414,
0.0783898080859335));
#74359=CARTESIAN_POINT('Origin',(0.0177910107596772,-0.0345621716267852,
0.0784324551737312));
#74360=CARTESIAN_POINT('Ctrl Pts',(0.0030308318555927,-0.0346945769586965,
0.0714778549605037));
#74361=CARTESIAN_POINT('Ctrl Pts',(0.00297486270787194,-0.0345275153362944,
0.071584528844429));
#74362=CARTESIAN_POINT('Ctrl Pts',(0.0029222338791257,-0.0343603235965185,
0.0716929904978644));
#74363=CARTESIAN_POINT('Ctrl Pts',(0.00287309625441993,-0.034193496108874,
0.0718029168259806));
#74364=CARTESIAN_POINT('Ctrl Pts',(0.00299352439310611,-0.0346945769586965,
0.0715529294675527));
#74365=CARTESIAN_POINT('Ctrl Pts',(0.00293912771099369,-0.0345275153362944,
0.0716603847712169));
#74366=CARTESIAN_POINT('Ctrl Pts',(0.00288809632950747,-0.0343603235965185,
0.0717695785939104));
#74367=CARTESIAN_POINT('Ctrl Pts',(0.00284057637698957,-0.034193496108874,
0.071880185745591));
#74368=CARTESIAN_POINT('Ctrl Pts',(0.00295621693061952,-0.0346945769586965,
0.0716280039746005));
#74369=CARTESIAN_POINT('Ctrl Pts',(0.00290339271411542,-0.0345275153362944,
0.0717362406980053));
#74370=CARTESIAN_POINT('Ctrl Pts',(0.0028539587798892,-0.0343603235965185,
0.0718461666899566));
#74371=CARTESIAN_POINT('Ctrl Pts',(0.00280805649955915,-0.034193496108874,
0.0719574546651999));
#74372=CARTESIAN_POINT('Ctrl Pts',(0.00291890946813294,-0.0346945769586965,
0.0717030784816508));
#74373=CARTESIAN_POINT('Ctrl Pts',(0.00286765771723718,-0.0345275153362944,
0.0718120966247927));
#74374=CARTESIAN_POINT('Ctrl Pts',(0.00281982123027101,-0.0343603235965185,
0.0719227547860021));
#74375=CARTESIAN_POINT('Ctrl Pts',(0.00277553662212886,-0.034193496108874,
0.0720347235848117));
#74376=CARTESIAN_POINT('',(0.0029189094684027,-0.0346945769586966,0.0717030784811083));
#74377=CARTESIAN_POINT('',(0.00282277334555112,-0.0343667727831433,0.0719189844916737));
#74378=CARTESIAN_POINT('Origin',(0.0182118505758894,-0.034562645706894,
0.078690438462228));
#74379=CARTESIAN_POINT('Origin',(-0.0073639863885442,-0.0341934771029151,
0.0676317265628182));
#74380=CARTESIAN_POINT('',(0.00287251438400795,-0.034193496108874,0.071804299380333));
#74381=CARTESIAN_POINT('',(0.00284826994360806,-0.0341934961088841,0.0718619054313204));
#74382=CARTESIAN_POINT('',(0.00297332029858978,-0.034521194296272,0.0715905337914187));
#74383=CARTESIAN_POINT('Origin',(0.0179949030575089,-0.0345625596118343,
0.0791195358443171));
#74384=CARTESIAN_POINT('',(0.00297453689523274,-0.0346945769586886,0.0715911383659319));
#74385=CARTESIAN_POINT('Origin',(-0.00693311847756907,-0.0346945685853897,
0.0666676355251271));
#74386=CARTESIAN_POINT('',(0.00294672318182772,-0.0346945769587026,0.0716471084235301));
#74387=CARTESIAN_POINT('Ctrl Pts',(0.00285944561345406,-0.0345231616327842,
0.0712713266291331));
#74388=CARTESIAN_POINT('Ctrl Pts',(0.00281976715388458,-0.0344132092796988,
0.0713438880972906));
#74389=CARTESIAN_POINT('Ctrl Pts',(0.00278159161827437,-0.0343032738558979,
0.0714172665392481));
#74390=CARTESIAN_POINT('Ctrl Pts',(0.00274496550589077,-0.0341934961088739,
0.0714913666959631));
#74391=CARTESIAN_POINT('Ctrl Pts',(0.00289784334637777,-0.0345231616327842,
0.0713779415917079));
#74392=CARTESIAN_POINT('Ctrl Pts',(0.00285963442396553,-0.0344132092796988,
0.0714499738011767));
#74393=CARTESIAN_POINT('Ctrl Pts',(0.00282291740239268,-0.0343032738558979,
0.0715227926155359));
#74394=CARTESIAN_POINT('Ctrl Pts',(0.00278773693076643,-0.0341934961088739,
0.0715963035405536));
#74395=CARTESIAN_POINT('Ctrl Pts',(0.00293624107930148,-0.0345231616327842,
0.0714845565542826));
#74396=CARTESIAN_POINT('Ctrl Pts',(0.00289950169404647,-0.0344132092796988,
0.0715560595050627));
#74397=CARTESIAN_POINT('Ctrl Pts',(0.002864243186511,-0.0343032738558979,
0.0716283186918237));
#74398=CARTESIAN_POINT('Ctrl Pts',(0.00283050835564208,-0.0341934961088739,
0.071701240385144));
#74399=CARTESIAN_POINT('Ctrl Pts',(0.00297463881222519,-0.0345231616327842,
0.0715911715168574));
#74400=CARTESIAN_POINT('Ctrl Pts',(0.00293936896412741,-0.0344132092796988,
0.0716621452089488));
#74401=CARTESIAN_POINT('Ctrl Pts',(0.00290556897062931,-0.0343032738558979,
0.0717338447681115));
#74402=CARTESIAN_POINT('Ctrl Pts',(0.00287327978051774,-0.0341934961088739,
0.0718061772297345));
#74403=CARTESIAN_POINT('',(0.00280873994495938,-0.0341934961088839,0.0716478330381581));
#74404=CARTESIAN_POINT('Ctrl Pts',(0.00275065666934253,-0.0342105180195392,
0.0714798835144891));
#74405=CARTESIAN_POINT('Ctrl Pts',(0.00278913956126267,-0.034261055624132,
0.0714990071704826));
#74406=CARTESIAN_POINT('Ctrl Pts',(0.00282693189758478,-0.0343122189870191,
0.0715177876623571));
#74407=CARTESIAN_POINT('Ctrl Pts',(0.00290116858704878,-0.0344158119695203,
0.0715546787804765));
#74408=CARTESIAN_POINT('Ctrl Pts',(0.00293758257684465,-0.0344681990450117,
0.0715727743179857));
#74409=CARTESIAN_POINT('Ctrl Pts',(0.0029733202986113,-0.0345211942962542,
0.0715905337914284));
#74410=CARTESIAN_POINT('Ctrl Pts',(0.00292083148908078,-0.0346945769586932,
0.0717024325675185));
#74411=CARTESIAN_POINT('Ctrl Pts',(0.00287022976425739,-0.034529677707698,
0.0718099998918345));
#74412=CARTESIAN_POINT('Ctrl Pts',(0.00282411713433537,-0.034364806625142,
0.0719195667170019));
#74413=CARTESIAN_POINT('Ctrl Pts',(0.00291890946840661,-0.0346945769586932,
0.0717030784811002));
#74414=CARTESIAN_POINT('Ctrl Pts',(0.00286832109738949,-0.034529677707698,
0.0718106855418335));
#74415=CARTESIAN_POINT('Ctrl Pts',(0.00282222345220572,-0.034364806625142,
0.0719202915175391));
#74416=CARTESIAN_POINT('Ctrl Pts',(0.00259858542488672,-0.0346945769586932,
0.0718107264648117));
#74417=CARTESIAN_POINT('Ctrl Pts',(0.00255022259976356,-0.034529677707698,
0.0719249559984909));
#74418=CARTESIAN_POINT('Ctrl Pts',(0.00250662231166498,-0.034364806625142,
0.0720410868044649));
#74419=CARTESIAN_POINT('',(0.00259360130007642,-0.0346775396664965,0.071822533720185));
#74420=CARTESIAN_POINT('',(0.00259858542488539,-0.0346945769586885,0.0718107264648148));
#74421=CARTESIAN_POINT('Origin',(0.0179538301029704,-0.0345626618414984,
0.0781214438937064));
#74422=CARTESIAN_POINT('Ctrl Pts',(0.00259360130155185,-0.0346775396670097,
0.07182253371912));
#74423=CARTESIAN_POINT('Ctrl Pts',(0.00263319572832671,-0.0346269749928193,
0.0718391976615173));
#74424=CARTESIAN_POINT('Ctrl Pts',(0.00267208648772173,-0.0345757902890796,
0.0718555654153675));
#74425=CARTESIAN_POINT('Ctrl Pts',(0.00274849263373398,-0.0344721681087812,
0.0718877221846446));
#74426=CARTESIAN_POINT('Ctrl Pts',(0.00278597806337797,-0.0344197714289114,
0.071903498598308));
#74427=CARTESIAN_POINT('Ctrl Pts',(0.0028227733455425,-0.0343667727830586,
0.0719189844914046));
#74428=CARTESIAN_POINT('',(0.00275874744665404,-0.0346945769587026,0.0717569024729716));
#74429=CARTESIAN_POINT('Origin',(0.00812378219310841,-0.0315241814719618,
0.07415));
#74430=CARTESIAN_POINT('',(0.00259360130087575,-0.03471161364898,0.0718225337213232));
#74431=CARTESIAN_POINT('',(0.00258864240555078,-0.0346945769586885,0.0718343515957248));
#74432=CARTESIAN_POINT('Origin',(0.0179696711837717,-0.0345626685633996,
0.0780789899898139));
#74433=CARTESIAN_POINT('Origin',(0.0178353519249934,-0.0345626628434408,
0.0784029612363081));
#74434=CARTESIAN_POINT('Origin',(0.0178160631121034,-0.0345626694948275,
0.0784439642081316));
#74435=CARTESIAN_POINT('Ctrl Pts',(0.00288833485497925,-0.0352450361874068,
0.0717690645125704));
#74436=CARTESIAN_POINT('Ctrl Pts',(0.00279853639954668,-0.0349452760959493,
0.0719665226490653));
#74437=CARTESIAN_POINT('Ctrl Pts',(0.00272386640684683,-0.0346444289841741,
0.0721701838148685));
#74438=CARTESIAN_POINT('Ctrl Pts',(0.00288734079150217,-0.0352450361874068,
0.0717713856034353));
#74439=CARTESIAN_POINT('Ctrl Pts',(0.00279762987744806,-0.0349452760959493,
0.0719688812316495));
#74440=CARTESIAN_POINT('Ctrl Pts',(0.00272305000146052,-0.0346444289841741,
0.0721725731886873));
#74441=CARTESIAN_POINT('Ctrl Pts',(0.00278891866505875,-0.0352450361874068,
0.072001196580167));
#74442=CARTESIAN_POINT('Ctrl Pts',(0.00270787521421854,-0.0349452760959493,
0.0722024042597919));
#74443=CARTESIAN_POINT('Ctrl Pts',(0.00264221778499502,-0.0346444289841741,
0.0724091448538994));
#74444=CARTESIAN_POINT('Ctrl Pts',(0.00278793444379431,-0.0352450361874068,
0.0720034946899342));
#74445=CARTESIAN_POINT('Ctrl Pts',(0.00270697766758624,-0.0349452760959493,
0.0722047394900734));
#74446=CARTESIAN_POINT('Ctrl Pts',(0.00264140946283037,-0.0346444289841741,
0.0724115105705516));
#74447=CARTESIAN_POINT('',(0.00277554631635331,-0.0351951634053266,0.072034692620652));
#74448=CARTESIAN_POINT('',(0.00269314705285671,-0.0348678972925388,0.072256239990531));
#74449=CARTESIAN_POINT('Origin',(0.0186471640029153,-0.0345636767884868,
0.0773728803636752));
#74450=CARTESIAN_POINT('Origin',(-0.00774050194262602,-0.0346946199341123,
0.0686178395383498));
#74451=CARTESIAN_POINT('',(0.00273558880738216,-0.0346945769330288,0.0721386579018089));
#74452=CARTESIAN_POINT('',(0.0027150093185055,-0.0346945769458129,0.0721976726095114));
#74453=CARTESIAN_POINT('',(0.00282277334566154,-0.0350221583435276,0.0719189844914724));
#74454=CARTESIAN_POINT('Origin',(0.018528619856001,-0.0345628458719578,
0.0778388102710214));
#74455=CARTESIAN_POINT('',(0.00282391455155809,-0.035195136029876,0.0719194615049381));
#74456=CARTESIAN_POINT('Origin',(-0.00733224189768627,-0.0351951838366883,
0.0676450808400573));
#74457=CARTESIAN_POINT('',(0.00277553662226091,-0.035195137132875,0.0720347235841983));
#74458=CARTESIAN_POINT('Ctrl Pts',(0.0026890797755654,-0.0350241211494343,
0.0716075583324728));
#74459=CARTESIAN_POINT('Ctrl Pts',(0.00265405868403688,-0.0349144232818962,
0.0716824191299597));
#74460=CARTESIAN_POINT('Ctrl Pts',(0.00262056405687373,-0.0348045283579412,
0.071758048646229));
#74461=CARTESIAN_POINT('Ctrl Pts',(0.00258864240126185,-0.0346945769439158,
0.0718343516059767));
#74462=CARTESIAN_POINT('Ctrl Pts',(0.0027340961748041,-0.0350241211494343,
0.0717115519169025));
#74463=CARTESIAN_POINT('Ctrl Pts',(0.00270050755226207,-0.0349144232818962,
0.0717857926319474));
#74464=CARTESIAN_POINT('Ctrl Pts',(0.00266843343393998,-0.0348045283579412,
0.0718607720844678));
#74465=CARTESIAN_POINT('Ctrl Pts',(0.0026379184765476,-0.0346945769439158,
0.0719363957641014));
#74466=CARTESIAN_POINT('Ctrl Pts',(0.0027791125740428,-0.0350241211494343,
0.0718155455013322));
#74467=CARTESIAN_POINT('Ctrl Pts',(0.00274695642048726,-0.0349144232818962,
0.071889166133935));
#74468=CARTESIAN_POINT('Ctrl Pts',(0.00271630281100623,-0.0348045283579412,
0.0719634955227065));
#74469=CARTESIAN_POINT('Ctrl Pts',(0.00268719455183335,-0.0346945769439158,
0.0720384399222262));
#74470=CARTESIAN_POINT('Ctrl Pts',(0.0028241289732815,-0.0350241211494343,
0.0719195390857619));
#74471=CARTESIAN_POINT('Ctrl Pts',(0.00279340528871245,-0.0349144232818962,
0.0719925396359226));
#74472=CARTESIAN_POINT('Ctrl Pts',(0.00276417218807248,-0.0348045283579412,
0.0720662189609453));
#74473=CARTESIAN_POINT('Ctrl Pts',(0.0027364706271191,-0.0346945769439158,
0.0721404840803509));
#74474=CARTESIAN_POINT('',(0.00266211560649583,-0.0346945769458128,0.0719865047484688));
#74475=CARTESIAN_POINT('Ctrl Pts',(0.00259360130390104,-0.0347116136492796,
0.0718225337225936));
#74476=CARTESIAN_POINT('Ctrl Pts',(0.00263318000186453,-0.034762154653231,
0.0718391910592448));
#74477=CARTESIAN_POINT('Ctrl Pts',(0.00267206279936505,-0.0348133084097055,
0.0718555555149049));
#74478=CARTESIAN_POINT('Ctrl Pts',(0.00274846904378221,-0.0349168561544571,
0.0718877123214953));
#74479=CARTESIAN_POINT('Ctrl Pts',(0.00278596218422295,-0.0349692089015917,
0.071903491917454));
#74480=CARTESIAN_POINT('Ctrl Pts',(0.00282277334568756,-0.0350221583435,
0.0719189844915049));
#74481=CARTESIAN_POINT('Ctrl Pts',(0.00277689142409584,-0.0351951371254876,
0.0720341713778109));
#74482=CARTESIAN_POINT('Ctrl Pts',(0.00273314799484822,-0.0350307338980915,
0.0721447149897066));
#74483=CARTESIAN_POINT('Ctrl Pts',(0.00269401083086319,-0.0348659306897811,
0.0722569721058663));
#74484=CARTESIAN_POINT('Ctrl Pts',(0.0027755366223692,-0.0351951371254876,
0.0720347235842403));
#74485=CARTESIAN_POINT('Ctrl Pts',(0.00273180460964304,-0.0350307338980915,
0.0721452952058117));
#74486=CARTESIAN_POINT('Ctrl Pts',(0.00269268001009425,-0.0348659306897811,
0.0722575798358558));
#74487=CARTESIAN_POINT('Ctrl Pts',(0.00254847044096598,-0.0351951371254876,
0.0721272739573489));
#74488=CARTESIAN_POINT('Ctrl Pts',(0.00250665184913576,-0.0350307338980915,
0.0722425400297545));
#74489=CARTESIAN_POINT('Ctrl Pts',(0.00246963306219441,-0.0348659306897811,
0.0723594360155021));
#74490=CARTESIAN_POINT('Origin',(-0.0023284672996302,-0.030860919741036,
0.070505112876027));
#74491=CARTESIAN_POINT('',(0.00267654088693848,-0.0351951371254876,0.0720750734601824));
#74492=CARTESIAN_POINT('Origin',(0.00908328496106734,-0.0351840467441164,
0.0743346620914201));
#74493=CARTESIAN_POINT('Origin',(-0.00341101805982505,-0.0352322613913528,
0.0709692410551445));
#74494=CARTESIAN_POINT('',(0.00261986248867378,-0.0351951142564652,0.0724812632111186));
#74495=CARTESIAN_POINT('',(0.00258626131451716,-0.0351951372916786,0.07260133524636));
#74496=CARTESIAN_POINT('Origin',(0.00821759083541753,-0.0352875121537596,
0.0744774156840959));
#74497=CARTESIAN_POINT('Origin',(0.0114906889709513,-0.029832507652212,
0.0674448431017022));
#74498=CARTESIAN_POINT('Origin',(0.00149551904094535,-0.0338734032822288,
0.0690206808999644));
#74499=CARTESIAN_POINT('Ctrl Pts',(0.00465214471498694,-0.0321934096636941,
0.069564602638177));
#74500=CARTESIAN_POINT('Ctrl Pts',(0.00457006828575119,-0.0320508460843319,
0.0696267432958608));
#74501=CARTESIAN_POINT('Ctrl Pts',(0.00448972333927352,-0.0319086045661065,
0.0696910423309887));
#74502=CARTESIAN_POINT('Ctrl Pts',(0.00441127147453155,-0.0317669892864902,
0.0697573470542575));
#74503=CARTESIAN_POINT('Ctrl Pts',(0.00458641150258548,-0.0321934096636941,
0.0696166562395441));
#74504=CARTESIAN_POINT('Ctrl Pts',(0.00450526680802655,-0.0320508460843319,
0.0696799734904281));
#74505=CARTESIAN_POINT('Ctrl Pts',(0.00442588450643241,-0.0319086045661065,
0.0697454231977286));
#74506=CARTESIAN_POINT('Ctrl Pts',(0.0043484239200655,-0.0317669892864902,
0.0698128503651842));
#74507=CARTESIAN_POINT('Ctrl Pts',(0.00452067829018401,-0.0321934096636941,
0.0696687098409112));
#74508=CARTESIAN_POINT('Ctrl Pts',(0.00444046533030192,-0.0320508460843319,
0.0697332036849953));
#74509=CARTESIAN_POINT('Ctrl Pts',(0.00436204567359129,-0.0319086045661065,
0.0697998040644686));
#74510=CARTESIAN_POINT('Ctrl Pts',(0.00428557636559944,-0.0317669892864902,
0.069868353676111));
#74511=CARTESIAN_POINT('Ctrl Pts',(0.00445494507778255,-0.0321934096636941,
0.0697207634422783));
#74512=CARTESIAN_POINT('Ctrl Pts',(0.00437566385257729,-0.0320508460843319,
0.0697864338795626));
#74513=CARTESIAN_POINT('Ctrl Pts',(0.00429820684075017,-0.0319086045661065,
0.0698541849312086));
#74514=CARTESIAN_POINT('Ctrl Pts',(0.00422272881113338,-0.0317669892864902,
0.0699238569870377));
#74515=CARTESIAN_POINT('',(0.00445612105794349,-0.0321934096636941,0.0697198321930652));
#74516=CARTESIAN_POINT('',(0.0042772061858937,-0.0318665617511257,0.0698742570224911));
#74517=CARTESIAN_POINT('Origin',(0.0146311327386297,-0.0326371944421084,
0.0829745310635062));
#74518=CARTESIAN_POINT('Origin',(-0.00305376322288012,-0.0316939261508759,
0.0617253627574423));
#74519=CARTESIAN_POINT('',(0.00455309446550072,-0.0320197221621846,0.0696413662470279));
#74520=CARTESIAN_POINT('Ctrl Pts',(0.00455292496321436,-0.0320197392094765,
0.0696414403000754));
#74521=CARTESIAN_POINT('Ctrl Pts',(0.00452998399114003,-0.0319792716576063,
0.069659610006459));
#74522=CARTESIAN_POINT('Ctrl Pts',(0.00450707710155583,-0.0319386439829706,
0.0696780373210006));
#74523=CARTESIAN_POINT('Ctrl Pts',(0.00448418554777068,-0.0318979099381638,
0.0696967481787971));
#74524=CARTESIAN_POINT('Ctrl Pts',(0.0044612944464526,-0.031857176698493,
0.0697154586667608));
#74525=CARTESIAN_POINT('Ctrl Pts',(0.00443853390029749,-0.0318163871833569,
0.0697343562083512));
#74526=CARTESIAN_POINT('Ctrl Pts',(0.00441597994691168,-0.0317755399638302,
0.0697533730947152));
#74527=CARTESIAN_POINT('',(0.00455411604157367,-0.0321934096636183,0.0696422307549535));
#74528=CARTESIAN_POINT('Origin',(0.0031040652733624,-0.0324113879591786,
0.0678450009147852));
#74529=CARTESIAN_POINT('',(0.00450511854976857,-0.0321934096636662,0.0696810314740193));
#74530=CARTESIAN_POINT('Ctrl Pts',(0.00445813573896037,-0.0321934096636618,
0.0697200661754986));
#74531=CARTESIAN_POINT('Ctrl Pts',(0.00439704349903201,-0.0320835708272592,
0.069770618296939));
#74532=CARTESIAN_POINT('Ctrl Pts',(0.00433703286861146,-0.0319739230346488,
0.0698224053968247));
#74533=CARTESIAN_POINT('Ctrl Pts',(0.00427817554202042,-0.0318646057455573,
0.0698753553245471));
#74534=CARTESIAN_POINT('Ctrl Pts',(0.00434557346451849,-0.0321934096636618,
0.0697069933358301));
#74535=CARTESIAN_POINT('Ctrl Pts',(0.00428430093994273,-0.0320835708272592,
0.069759097778761));
#74536=CARTESIAN_POINT('Ctrl Pts',(0.00422414225465977,-0.0319739230346488,
0.0698124400307091));
#74537=CARTESIAN_POINT('Ctrl Pts',(0.00416516913971261,-0.0318646057455573,
0.0698669459368185));
#74538=CARTESIAN_POINT('Ctrl Pts',(0.00423301119007662,-0.0321934096636618,
0.0696939204961617));
#74539=CARTESIAN_POINT('Ctrl Pts',(0.00417155838085345,-0.0320835708272592,
0.069747577260583));
#74540=CARTESIAN_POINT('Ctrl Pts',(0.00411125164070808,-0.0319739230346488,
0.0698024746645934));
#74541=CARTESIAN_POINT('Ctrl Pts',(0.0040521627374048,-0.0318646057455573,
0.0698585365490899));
#74542=CARTESIAN_POINT('Ctrl Pts',(0.00412044891563474,-0.0321934096636618,
0.0696808476564932));
#74543=CARTESIAN_POINT('Ctrl Pts',(0.00405881582176417,-0.0320835708272592,
0.0697360567424051));
#74544=CARTESIAN_POINT('Ctrl Pts',(0.00399836102675639,-0.0319739230346488,
0.0697925092984778));
#74545=CARTESIAN_POINT('Ctrl Pts',(0.00393915633509698,-0.0318646057455573,
0.0698501271613613));
#74546=CARTESIAN_POINT('',(0.00411091186015112,-0.032176398030845,0.0696894090449235));
#74547=CARTESIAN_POINT('',(0.00412044891561043,-0.0321934096636184,0.069680847656515));
#74548=CARTESIAN_POINT('Origin',(0.0147144957395131,-0.0326386230867408,
0.0823933495046793));
#74549=CARTESIAN_POINT('Ctrl Pts',(0.00411091186226809,-0.0321763980306273,
0.0696894090472774));
#74550=CARTESIAN_POINT('Ctrl Pts',(0.00413961652127484,-0.0321259596174931,
0.0697213163185597));
#74551=CARTESIAN_POINT('Ctrl Pts',(0.00416782383482309,-0.0320749164631609,
0.0697526707549605));
#74552=CARTESIAN_POINT('Ctrl Pts',(0.00422326647133633,-0.0319716057793885,
0.0698142991910765));
#74553=CARTESIAN_POINT('Ctrl Pts',(0.00425048019196887,-0.0319193786690077,
0.0698445491782618));
#74554=CARTESIAN_POINT('Ctrl Pts',(0.00427720618713083,-0.0318665617525256,
0.069874257023867));
#74555=CARTESIAN_POINT('',(0.00428828498678695,-0.0321934096636663,0.0697003399248001));
#74556=CARTESIAN_POINT('Origin',(0.00812378219310841,-0.0315241814719618,
0.07415));
#74557=CARTESIAN_POINT('',(0.00411091185990249,-0.0322104233323619,0.0696894090446472));
#74558=CARTESIAN_POINT('',(0.00410139311123134,-0.0321934096636183,0.0696979907823519));
#74559=CARTESIAN_POINT('Origin',(0.0147520956102168,-0.0326387231234825,
0.0823680219401029));
#74560=CARTESIAN_POINT('Origin',(0.0156266935458865,-0.0326386244938891,
0.0815727147650413));
#74561=CARTESIAN_POINT('Origin',(0.0155975407542225,-0.0326387243547428,
0.0816074322076005));
#74562=CARTESIAN_POINT('Ctrl Pts',(0.0043985075858247,-0.0327445246967097,
0.0697681677233916));
#74563=CARTESIAN_POINT('Ctrl Pts',(0.00423324407982012,-0.032443687833936,
0.0699086687520859));
#74564=CARTESIAN_POINT('Ctrl Pts',(0.00407903318169789,-0.0321434074405927,
0.0700612189549092));
#74565=CARTESIAN_POINT('Ctrl Pts',(0.00421160252194496,-0.0327445246967097,
0.0699341993381404));
#74566=CARTESIAN_POINT('Ctrl Pts',(0.00405260100066022,-0.032443687833936,
0.0700817496065585));
#74567=CARTESIAN_POINT('Ctrl Pts',(0.00390516527516717,-0.0321434074405927,
0.0702408573446777));
#74568=CARTESIAN_POINT('',(0.00418518581123572,-0.0326943950436612,0.0699588684653545));
#74569=CARTESIAN_POINT('',(0.00401632040136206,-0.0323666188837389,0.0701242227297893));
#74570=CARTESIAN_POINT('Origin',(0.0157527902649768,-0.0326395579109763,
0.0821571710290731));
#74571=CARTESIAN_POINT('Origin',(-0.00387143505510243,-0.0321933825603063,
0.0623933310808583));
#74572=CARTESIAN_POINT('',(0.00410478685933017,-0.0321934096532688,0.070035902103298));
#74573=CARTESIAN_POINT('',(0.00406103874479378,-0.0321934096584274,0.0700805378828959));
#74574=CARTESIAN_POINT('',(0.00427720618525688,-0.0325210109756239,0.0698742570217772));
#74575=CARTESIAN_POINT('Origin',(0.0153855203852089,-0.0326393129158089,
0.0824674890361115));
#74576=CARTESIAN_POINT('',(0.00427811478949626,-0.0326943950436593,0.0698752670000577));
#74577=CARTESIAN_POINT('Origin',(-0.00312058435812075,-0.0326943765538058,
0.0616510851198891));
#74578=CARTESIAN_POINT('',(0.00423165030037599,-0.0326943950436702,0.069917067732716));
#74579=CARTESIAN_POINT('Ctrl Pts',(0.00428883628827747,-0.0325229783203769,
0.0695355455461076));
#74580=CARTESIAN_POINT('Ctrl Pts',(0.00422522613454202,-0.032413025309245,
0.0695884101915409));
#74581=CARTESIAN_POINT('Ctrl Pts',(0.00416271920163296,-0.032303122220807,
0.069642582676758));
#74582=CARTESIAN_POINT('Ctrl Pts',(0.00410139310790405,-0.0321934096576658,
0.0696979907853581));
#74583=CARTESIAN_POINT('Ctrl Pts',(0.00428529000841981,-0.0325229783203769,
0.0696488088064151));
#74584=CARTESIAN_POINT('Ctrl Pts',(0.00422324118625079,-0.032413025309245,
0.0697017223372388));
#74585=CARTESIAN_POINT('Ctrl Pts',(0.00416229635935874,-0.032303122220807,
0.0697559114022826));
#74586=CARTESIAN_POINT('Ctrl Pts',(0.00410253114440126,-0.0321934096576658,
0.0698113038345151));
#74587=CARTESIAN_POINT('Ctrl Pts',(0.00428174372856215,-0.0325229783203769,
0.0697620720667227));
#74588=CARTESIAN_POINT('Ctrl Pts',(0.00422125623795956,-0.032413025309245,
0.0698150344829366));
#74589=CARTESIAN_POINT('Ctrl Pts',(0.00416187351708452,-0.032303122220807,
0.0698692401278072));
#74590=CARTESIAN_POINT('Ctrl Pts',(0.00410366918089846,-0.0321934096576658,
0.0699246168836721));
#74591=CARTESIAN_POINT('Ctrl Pts',(0.00427819744870449,-0.0325229783203769,
0.0698753353270303));
#74592=CARTESIAN_POINT('Ctrl Pts',(0.00421927128966834,-0.032413025309245,
0.0699283466286345));
#74593=CARTESIAN_POINT('Ctrl Pts',(0.0041614506748103,-0.032303122220807,
0.0699825688533318));
#74594=CARTESIAN_POINT('Ctrl Pts',(0.00410480721739566,-0.0321934096576658,
0.0700379299328292));
#74595=CARTESIAN_POINT('',(0.00410308998553813,-0.0321934096584275,0.0698669464423854));
#74596=CARTESIAN_POINT('Ctrl Pts',(0.00411091186222349,-0.0322104233328931,
0.0696894090472278));
#74597=CARTESIAN_POINT('Ctrl Pts',(0.00413965541650832,-0.0322609421831288,
0.0697213595533796));
#74598=CARTESIAN_POINT('Ctrl Pts',(0.00416788173104027,-0.0323120888240559,
0.0697527351107362));
#74599=CARTESIAN_POINT('Ctrl Pts',(0.00422332478732175,-0.0324156524631813,
0.0698143640134545));
#74600=CARTESIAN_POINT('Ctrl Pts',(0.00425051873905522,-0.032468026716731,
0.0698445920260914));
#74601=CARTESIAN_POINT('Ctrl Pts',(0.00427720618528259,-0.0325210109755912,
0.0698742570218124));
#74602=CARTESIAN_POINT('Origin',(0.0145641766563385,-0.0262834582512374,
0.0696306300222498));
#74603=CARTESIAN_POINT('Origin',(0.00489496422593971,-0.0342770941894682,
0.0624282604882694));
#74604=CARTESIAN_POINT('Ctrl Pts',(0.00418721071705005,-0.0326943950436604,
0.0699589754572965));
#74605=CARTESIAN_POINT('Ctrl Pts',(0.00412945054403444,-0.0325844576448134,
0.0700132287901579));
#74606=CARTESIAN_POINT('Ctrl Pts',(0.00407280833111478,-0.0324744968375322,
0.0700686805376889));
#74607=CARTESIAN_POINT('Ctrl Pts',(0.00401735567163183,-0.0323646534831895,
0.070125258650873));
#74608=CARTESIAN_POINT('Ctrl Pts',(0.00407404987198554,-0.0326943950436604,
0.0699529962662399));
#74609=CARTESIAN_POINT('Ctrl Pts',(0.00401620729451098,-0.0325844576448134,
0.0700088091676323));
#74610=CARTESIAN_POINT('Ctrl Pts',(0.00395951492573464,-0.0324744968375322,
0.0700658222983268));
#74611=CARTESIAN_POINT('Ctrl Pts',(0.00390404439566649,-0.0323646534831895,
0.0701239616078851));
#74612=CARTESIAN_POINT('Ctrl Pts',(0.00396088902692103,-0.0326943950436604,
0.0699470170751833));
#74613=CARTESIAN_POINT('Ctrl Pts',(0.00390296404498751,-0.0325844576448134,
0.0700043895451067));
#74614=CARTESIAN_POINT('Ctrl Pts',(0.00384622152035449,-0.0324744968375322,
0.0700629640589646));
#74615=CARTESIAN_POINT('Ctrl Pts',(0.00379073311970116,-0.0323646534831895,
0.0701226645648972));
#74616=CARTESIAN_POINT('Ctrl Pts',(0.00384772818185653,-0.0326943950436604,
0.0699410378841267));
#74617=CARTESIAN_POINT('Ctrl Pts',(0.00378972079546405,-0.0325844576448134,
0.0699999699225811));
#74618=CARTESIAN_POINT('Ctrl Pts',(0.00373292811497434,-0.0324744968375322,
0.0700601058196024));
#74619=CARTESIAN_POINT('Ctrl Pts',(0.00367742184373582,-0.0323646534831895,
0.0701213675219093));
#74620=CARTESIAN_POINT('',(0.00383874751947724,-0.0326773559991152,0.069950181215116));
#74621=CARTESIAN_POINT('',(0.003847728181856,-0.0326943950436594,0.0699410378841272));
#74622=CARTESIAN_POINT('Origin',(0.0157328504357829,-0.0326395670218336,
0.0815373995020848));
#74623=CARTESIAN_POINT('Ctrl Pts',(0.00383874752186574,-0.0326773559987415,
0.0699501812174572));
#74624=CARTESIAN_POINT('Ctrl Pts',(0.00386942367916692,-0.0326267922586078,
0.0699802473222834));
#74625=CARTESIAN_POINT('Ctrl Pts',(0.00389955612373196,-0.0325756109579571,
0.0700097805271131));
#74626=CARTESIAN_POINT('Ctrl Pts',(0.00395875923161915,-0.0324719985462364,
0.0700678062710256));
#74627=CARTESIAN_POINT('Ctrl Pts',(0.00398780615017079,-0.0324196091621775,
0.0700962755375468));
#74628=CARTESIAN_POINT('Ctrl Pts',(0.00401632040139686,-0.0323666188837757,
0.0701242227298235));
#74629=CARTESIAN_POINT('',(0.00401645699655587,-0.0326943950436702,0.0699499531747509));
#74630=CARTESIAN_POINT('Origin',(0.00812378219310841,-0.0315241814719618,
0.07415));
#74631=CARTESIAN_POINT('',(0.00383874751950847,-0.0327114338379877,0.0699501812151468));
#74632=CARTESIAN_POINT('',(0.00382978640553166,-0.0326943950436593,0.0699593437057789));
#74633=CARTESIAN_POINT('Origin',(0.0157640093170233,-0.0326395666891383,
0.0815045024555703));
#74634=CARTESIAN_POINT('Origin',(0.0156625188665274,-0.0326395680025381,
0.0816091612983061));
#74635=CARTESIAN_POINT('Origin',(0.0156302508924236,-0.0326395677096589,
0.081640971233586));
#74636=CARTESIAN_POINT('Ctrl Pts',(0.00413069280981186,-0.0332451089994432,
0.0700107534288225));
#74637=CARTESIAN_POINT('Ctrl Pts',(0.00397457857121719,-0.0329451141710253,
0.0701613552588885));
#74638=CARTESIAN_POINT('Ctrl Pts',(0.00383025178220369,-0.0326442513127493,
0.0703232884077009));
#74639=CARTESIAN_POINT('Ctrl Pts',(0.00395458298185639,-0.0332451089994432,
0.0701881944852257));
#74640=CARTESIAN_POINT('Ctrl Pts',(0.00380516104219571,-0.0329451141710253,
0.0703454384061234));
#74641=CARTESIAN_POINT('Ctrl Pts',(0.00366800784943576,-0.0326442513127493,
0.0705134906849743));
#74642=CARTESIAN_POINT('Ctrl Pts',(0.00395282188357683,-0.0332451089994432,
0.0701899688957897));
#74643=CARTESIAN_POINT('Ctrl Pts',(0.00380346686690549,-0.0329451141710253,
0.0703472792375957));
#74644=CARTESIAN_POINT('Ctrl Pts',(0.00366638541010808,-0.0326442513127493,
0.070515392707747));
#74645=CARTESIAN_POINT('',(0.00392979440503199,-0.0331951640388616,0.0702144452190998));
#74646=CARTESIAN_POINT('',(0.00377164487893352,-0.0328677532354985,0.0703900763480648));
#74647=CARTESIAN_POINT('Origin',(0.0166670807805257,-0.0326402808279353,
0.0811137013066832));
#74648=CARTESIAN_POINT('Origin',(-0.00459481279605483,-0.0326944278779134,
0.0631625754702518));
#74649=CARTESIAN_POINT('',(0.00385439107964536,-0.0326943950436593,0.070296375145362));
#74650=CARTESIAN_POINT('',(0.00381353199788872,-0.0326943950436693,0.0703436698114264));
#74651=CARTESIAN_POINT('',(0.00401632040136406,-0.0330220786163545,0.0701242227297873));
#74652=CARTESIAN_POINT('Origin',(0.0163772171391324,-0.0326396682765136,
0.0814972788281632));
#74653=CARTESIAN_POINT('',(0.00401729062974261,-0.0331951640388587,0.070125173663373));
#74654=CARTESIAN_POINT('Origin',(-0.0038612114645624,-0.0331952026559987,
0.0624033491204828));
#74655=CARTESIAN_POINT('',(0.00397354251739729,-0.0331951640388701,0.0701698094412464));
#74656=CARTESIAN_POINT('Ctrl Pts',(0.00400665898653133,-0.0330240426238172,
0.0697854500229821));
#74657=CARTESIAN_POINT('Ctrl Pts',(0.0039465330584229,-0.032914277406352,
0.0698421674062715));
#74658=CARTESIAN_POINT('Ctrl Pts',(0.0038875496620913,-0.0328043479726691,
0.0699001560361325));
#74659=CARTESIAN_POINT('Ctrl Pts',(0.00382978640553166,-0.0326943950436593,
0.0699593437057788));
#74660=CARTESIAN_POINT('Ctrl Pts',(0.00401023158067429,-0.0330240426238172,
0.069898712428729));
#74661=CARTESIAN_POINT('Ctrl Pts',(0.00395166595255125,-0.032914277406352,
0.0699553805960535));
#74662=CARTESIAN_POINT('Ctrl Pts',(0.00389424261664,-0.0328043479726691,
0.0700132877296544));
#74663=CARTESIAN_POINT('Ctrl Pts',(0.00383803717950686,-0.0326943950436593,
0.0700723616721085));
#74664=CARTESIAN_POINT('Ctrl Pts',(0.00401380417481726,-0.0330240426238172,
0.0700119748344759));
#74665=CARTESIAN_POINT('Ctrl Pts',(0.00395679884667959,-0.032914277406352,
0.0700685937858354));
#74666=CARTESIAN_POINT('Ctrl Pts',(0.00390093557118869,-0.0328043479726691,
0.0701264194231762));
#74667=CARTESIAN_POINT('Ctrl Pts',(0.00384628795348206,-0.0326943950436593,
0.0701853796384381));
#74668=CARTESIAN_POINT('Ctrl Pts',(0.00401737676896022,-0.0330240426238172,
0.0701252372402228));
#74669=CARTESIAN_POINT('Ctrl Pts',(0.00396193174080793,-0.032914277406352,
0.0701818069756174));
#74670=CARTESIAN_POINT('Ctrl Pts',(0.00390762852573739,-0.0328043479726691,
0.0702395511166981));
#74671=CARTESIAN_POINT('Ctrl Pts',(0.00385453872745727,-0.0326943950436593,
0.0702983976047677));
#74672=CARTESIAN_POINT('',(0.00384208874259851,-0.0326943950436694,0.0701278594255804));
#74673=CARTESIAN_POINT('Ctrl Pts',(0.00383874752187065,-0.0327114338383328,
0.0699501812174619));
#74674=CARTESIAN_POINT('Ctrl Pts',(0.00386941857673141,-0.032761987683102,
0.0699802423213192));
#74675=CARTESIAN_POINT('Ctrl Pts',(0.00389954852903165,-0.0328131562604436,
0.0700097730834474));
#74676=CARTESIAN_POINT('Ctrl Pts',(0.00395875158252924,-0.0329167375858768,
0.0700677987740519));
#74677=CARTESIAN_POINT('Ctrl Pts',(0.00398780109418897,-0.0329691088920616,
0.0700962705821124));
#74678=CARTESIAN_POINT('Ctrl Pts',(0.00401632040139609,-0.0330220786163187,
0.0701242227298225));
#74679=CARTESIAN_POINT('Ctrl Pts',(0.00393182235694514,-0.0331951640388604,
0.0702144248517776));
#74680=CARTESIAN_POINT('Ctrl Pts',(0.00385045686401168,-0.0330306422010619,
0.0703010909337557));
#74681=CARTESIAN_POINT('Ctrl Pts',(0.00377274289763015,-0.0328657861914645,
0.0703910458815629));
#74682=CARTESIAN_POINT('Ctrl Pts',(0.00392979440503419,-0.0331951640388604,
0.0702144452190975));
#74683=CARTESIAN_POINT('Ctrl Pts',(0.003848429333182,-0.0330306422010619,
0.0703011532276811));
#74684=CARTESIAN_POINT('Ctrl Pts',(0.00377071752039264,-0.0328657861914645,
0.0703911500488642));
#74685=CARTESIAN_POINT('Ctrl Pts',(0.00359188307974148,-0.0331951640388604,
0.070217838962318));
#74686=CARTESIAN_POINT('Ctrl Pts',(0.00351058817135452,-0.0330306422010619,
0.0703115330709035));
#74687=CARTESIAN_POINT('Ctrl Pts',(0.00343323520493602,-0.0328657861914645,
0.0704085071225851));
#74688=CARTESIAN_POINT('',(0.00358349425258602,-0.0331781648281888,0.0702275281501469));
#74689=CARTESIAN_POINT('',(0.00359188307974073,-0.0331951640388588,0.0702178389623189));
#74690=CARTESIAN_POINT('Origin',(0.0165401803771366,-0.0326412093141841,
0.0804798821977587));
#74691=CARTESIAN_POINT('Ctrl Pts',(0.00358349425436534,-0.033178164828644,
0.0702275281496977));
#74692=CARTESIAN_POINT('Ctrl Pts',(0.0036160201308545,-0.0331276811546779,
0.0702556280772692));
#74693=CARTESIAN_POINT('Ctrl Pts',(0.00364795871284956,-0.0330765663497788,
0.0702832205815802));
#74694=CARTESIAN_POINT('Ctrl Pts',(0.00371068862268351,-0.0329730614463369,
0.0703374145731777));
#74695=CARTESIAN_POINT('Ctrl Pts',(0.00374145460550374,-0.0329207133374194,
0.0703639941713307));
#74696=CARTESIAN_POINT('Ctrl Pts',(0.00377164488147798,-0.0328677532289346,
0.0703900763317915));
#74697=CARTESIAN_POINT('',(0.00376083874239636,-0.0331951640388701,0.0702161420907193));
#74698=CARTESIAN_POINT('Origin',(0.00812378219310841,-0.0315241814719618,
0.07415));
#74699=CARTESIAN_POINT('',(0.00358349425333596,-0.0332121607144232,0.0702275281516499));
#74700=CARTESIAN_POINT('',(0.00357512613946546,-0.0331951640388587,0.0702372352350697));
#74701=CARTESIAN_POINT('Origin',(0.0165634452037064,-0.0326413648504218,
0.08044095890546));
#74702=CARTESIAN_POINT('Origin',(0.0156089014564926,-0.0326412100340455,
0.0815578475744207));
#74703=CARTESIAN_POINT('Origin',(0.0155737662735942,-0.0326413659626031,
0.0815865150718522));
#74704=CARTESIAN_POINT('Ctrl Pts',(0.00387868087166481,-0.0337436976235975,
0.0702696340674263));
#74705=CARTESIAN_POINT('Ctrl Pts',(0.0038437802723817,-0.0336723290703325,
0.0703078151520742));
#74706=CARTESIAN_POINT('Ctrl Pts',(0.00380957207656177,-0.033601104548885,
0.0703466178116988));
#74707=CARTESIAN_POINT('Ctrl Pts',(0.00370035208357056,-0.0333736987606857,
0.0704705070175065));
#74708=CARTESIAN_POINT('Ctrl Pts',(0.00359842155345539,-0.0331450831799191,
0.0706004597366589));
#74709=CARTESIAN_POINT('Ctrl Pts',(0.00371405949086468,-0.0337436976235975,
0.0704577824157674));
#74710=CARTESIAN_POINT('Ctrl Pts',(0.00368085112634121,-0.0336723290703325,
0.0704974441300632));
#74711=CARTESIAN_POINT('Ctrl Pts',(0.00364836152337774,-0.033601104548885,
0.0705376967418353));
#74712=CARTESIAN_POINT('Ctrl Pts',(0.00354462865694311,-0.0333736987606857,
0.0706662153576305));
#74713=CARTESIAN_POINT('Ctrl Pts',(0.00344844187327208,-0.0331450831799191,
0.0708004749749087));
#74714=CARTESIAN_POINT('Ctrl Pts',(0.00371241327705668,-0.0337436976235975,
0.0704596638992509));
#74715=CARTESIAN_POINT('Ctrl Pts',(0.00367922183488081,-0.0336723290703325,
0.0704993404198431));
#74716=CARTESIAN_POINT('Ctrl Pts',(0.0036467494178459,-0.033601104548885,
0.0705396075311367));
#74717=CARTESIAN_POINT('Ctrl Pts',(0.00354307142267684,-0.0333736987606857,
0.0706681724410318));
#74718=CARTESIAN_POINT('Ctrl Pts',(0.00344694207647024,-0.0331450831799191,
0.0708024751272912));
#74719=CARTESIAN_POINT('',(0.00369095475256867,-0.0336938721132548,0.0704855538095916));
#74720=CARTESIAN_POINT('',(0.00354414527714575,-0.0333679869945434,0.0706707686599204));
#74721=CARTESIAN_POINT('Ctrl Pts',(0.0036909547525674,-0.0336938721132646,
0.0704855538095919));
#74722=CARTESIAN_POINT('Ctrl Pts',(0.00367665070006428,-0.0336629187933929,
0.070502857214569));
#74723=CARTESIAN_POINT('Ctrl Pts',(0.00366245254073096,-0.0336319952301037,
0.0705202388414836));
#74724=CARTESIAN_POINT('Ctrl Pts',(0.00364836152337687,-0.0336011045488947,
0.0705376967418361));
#74725=CARTESIAN_POINT('Ctrl Pts',(0.00361300233916066,-0.0335235892595451,
0.0705815045875778));
#74726=CARTESIAN_POINT('Ctrl Pts',(0.00357825509263566,-0.0334458668660366,
0.0706258706477928));
#74727=CARTESIAN_POINT('Ctrl Pts',(0.00354414527688669,-0.0333679869945382,
0.0706707686597147));
#74728=CARTESIAN_POINT('Ctrl Pts',(0.00354411782777536,-0.0333679692460734,
0.0706708036542234));
#74729=CARTESIAN_POINT('Ctrl Pts',(0.00354448229424894,-0.03333918953762,
0.0706710731018273));
#74730=CARTESIAN_POINT('Ctrl Pts',(0.00354475741002288,-0.0333104081062542,
0.0706712724548537));
#74731=CARTESIAN_POINT('Ctrl Pts',(0.0035451248223397,-0.0332532698548129,
0.0706715318477102));
#74732=CARTESIAN_POINT('Ctrl Pts',(0.00354521978741927,-0.0332249172858275,
0.0706715939211706));
#74733=CARTESIAN_POINT('Ctrl Pts',(0.0035452268843479,-0.0331960985300325,
0.0706715906470329));
#74734=CARTESIAN_POINT('Ctrl Pts',(0.00354522697566713,-0.0331956312625235,
0.0706715905760188));
#74735=CARTESIAN_POINT('Ctrl Pts',(0.00354522704296523,-0.033195164038859,
0.0706715904874357));
#74736=CARTESIAN_POINT('',(0.00362084464106437,-0.0331951640388587,0.0705720566798239));
#74737=CARTESIAN_POINT('',(0.00358303584202474,-0.0331951640388687,0.0706218235836399));
#74738=CARTESIAN_POINT('',(0.00377164489305891,-0.0335216366567749,0.0703900763416243));
#74739=CARTESIAN_POINT('Origin',(0.0171326131364008,-0.0326434571527407,
0.0803326712051912));
#74740=CARTESIAN_POINT('',(0.00377267291611205,-0.0336938721132326,0.0703909644774707));
#74741=CARTESIAN_POINT('Origin',(-0.00449108115158622,-0.033693886789624,
0.0632516928999231));
#74742=CARTESIAN_POINT('',(0.00373181383435036,-0.0336938721132537,0.0704382591435412));
#74743=CARTESIAN_POINT('Ctrl Pts',(0.00374073017182796,-0.0335235895815172,
0.0700525794725493));
#74744=CARTESIAN_POINT('Ctrl Pts',(0.00368432111118894,-0.0334144449262748,
0.0701129208130575));
#74745=CARTESIAN_POINT('Ctrl Pts',(0.00362909385005637,-0.0333049234473147,
0.0701744968471957));
#74746=CARTESIAN_POINT('Ctrl Pts',(0.00357512613946542,-0.0331951640388587,
0.0702372352350695));
#74747=CARTESIAN_POINT('Ctrl Pts',(0.00375140755481824,-0.0335235895815172,
0.070165394214398));
#74748=CARTESIAN_POINT('Ctrl Pts',(0.00369655161121256,-0.0334144449262748,
0.0702255885597076));
#74749=CARTESIAN_POINT('Ctrl Pts',(0.00364287621464645,-0.0333049234473147,
0.0702869853435383));
#74750=CARTESIAN_POINT('Ctrl Pts',(0.00359045711103427,-0.0331951640388587,
0.0703495122754503));
#74751=CARTESIAN_POINT('Ctrl Pts',(0.00376208493780853,-0.0335235895815172,
0.0702782089562468));
#74752=CARTESIAN_POINT('Ctrl Pts',(0.00370878211123618,-0.0334144449262748,
0.0703382563063576));
#74753=CARTESIAN_POINT('Ctrl Pts',(0.00365665857923653,-0.0333049234473147,
0.070399473839881));
#74754=CARTESIAN_POINT('Ctrl Pts',(0.00360578808260313,-0.0331951640388587,
0.0704617893158311));
#74755=CARTESIAN_POINT('Ctrl Pts',(0.00377276232079881,-0.0335235895815172,
0.0703910236980955));
#74756=CARTESIAN_POINT('Ctrl Pts',(0.0037210126112598,-0.0334144449262748,
0.0704509240530077));
#74757=CARTESIAN_POINT('Ctrl Pts',(0.00367044094382661,-0.0333049234473147,
0.0705119623362236));
#74758=CARTESIAN_POINT('Ctrl Pts',(0.00362111905417199,-0.0331951640388587,
0.0705740663562119));
#74759=CARTESIAN_POINT('',(0.00359798539027491,-0.0331951640388687,0.0704046459574569));
#74760=CARTESIAN_POINT('Ctrl Pts',(0.00358349425570064,-0.0332121607145981,
0.070227528153692));
#74761=CARTESIAN_POINT('Ctrl Pts',(0.00361596540746101,-0.0332625444109836,
0.0702555808191513));
#74762=CARTESIAN_POINT('Ctrl Pts',(0.00364787703032069,-0.0333135300746987,
0.0702831500931627));
#74763=CARTESIAN_POINT('Ctrl Pts',(0.00371060654925751,-0.0334167203140654,
0.0703373437424101));
#74764=CARTESIAN_POINT('Ctrl Pts',(0.0037414001496865,-0.0334688847587355,
0.0703639471280091));
#74765=CARTESIAN_POINT('Ctrl Pts',(0.00377164489348147,-0.0335216366562442,
0.0703900763422066));
#74766=CARTESIAN_POINT('Ctrl Pts',(0.00369195195617788,-0.033693872113239,
0.0704854810096331));
#74767=CARTESIAN_POINT('Ctrl Pts',(0.00367050231051092,-0.0336474569764958,
0.070511421982647));
#74768=CARTESIAN_POINT('Ctrl Pts',(0.0036493578064295,-0.033601104548885,
0.0705376122733537));
#74769=CARTESIAN_POINT('Ctrl Pts',(0.00359582478352168,-0.0334837508592656,
0.0706039200678976));
#74770=CARTESIAN_POINT('Ctrl Pts',(0.0035442801058033,-0.0333660264659097,
0.070671785039406));
#74771=CARTESIAN_POINT('Ctrl Pts',(0.00369095475258184,-0.0336938721132391,
0.0704855538095758));
#74772=CARTESIAN_POINT('Ctrl Pts',(0.0036695055330371,-0.0336474569764958,
0.0705115006195533));
#74773=CARTESIAN_POINT('Ctrl Pts',(0.00364836152337774,-0.033601104548885,
0.0705376967418353));
#74774=CARTESIAN_POINT('Ctrl Pts',(0.00359482975223288,-0.0334837508592656,
0.0706040193005872));
#74775=CARTESIAN_POINT('Ctrl Pts',(0.00354328676322187,-0.0333660264659097,
0.0706718989927277));
#74776=CARTESIAN_POINT('Ctrl Pts',(0.0033519011243526,-0.0336938721132391,
0.0705103061117345));
#74777=CARTESIAN_POINT('Ctrl Pts',(0.00333059678824609,-0.0336474569764958,
0.070538237515108));
#74778=CARTESIAN_POINT('Ctrl Pts',(0.00330962088426888,-0.033601104548885,
0.0705664163987568));
#74779=CARTESIAN_POINT('Ctrl Pts',(0.00325651471806131,-0.0334837508592656,
0.0706377588534238));
#74780=CARTESIAN_POINT('Ctrl Pts',(0.0032055458970172,-0.0333660264659097,
0.0707106436255546));
#74781=CARTESIAN_POINT('',(0.00334615942774154,-0.0336769361243753,0.0705203552912374));
#74782=CARTESIAN_POINT('',(0.00335392331299817,-0.0336938721132327,0.0705101584836928));
#74783=CARTESIAN_POINT('Ctrl Pts',(0.00334615942774136,-0.033676936124375,
0.0705203552912377));
#74784=CARTESIAN_POINT('Ctrl Pts',(0.0033474516903319,-0.0336797586669944,
0.0705186543139611));
#74785=CARTESIAN_POINT('Ctrl Pts',(0.00334874481244644,-0.0336825812712685,
0.070516954091143));
#74786=CARTESIAN_POINT('Ctrl Pts',(0.00335133277778879,-0.0336882266084466,
0.0705135551508626));
#74787=CARTESIAN_POINT('Ctrl Pts',(0.00335262762101661,-0.0336910493413165,
0.0705118564334281));
#74788=CARTESIAN_POINT('Ctrl Pts',(0.00335392331300474,-0.0336938721132303,
0.0705101584836938));
#74789=CARTESIAN_POINT('Ctrl Pts',(0.00334615942774159,-0.0336769361243753,
0.0705203552912374));
#74790=CARTESIAN_POINT('Ctrl Pts',(0.00337953499220296,-0.033627899459312,
0.0705457112992143));
#74791=CARTESIAN_POINT('Ctrl Pts',(0.00341338573099195,-0.0335767852487023,
0.0705714283055508));
#74792=CARTESIAN_POINT('Ctrl Pts',(0.00347972195807058,-0.0334733171799194,
0.0706218251132185));
#74793=CARTESIAN_POINT('Ctrl Pts',(0.00351224698220595,-0.0334209631321932,
0.0706465349506327));
#74794=CARTESIAN_POINT('Ctrl Pts',(0.00354414528154423,-0.033367986984468,
0.0706707686541077));
#74795=CARTESIAN_POINT('',(0.00352243903279342,-0.0336938721132538,0.0704978561466522));
#74796=CARTESIAN_POINT('Origin',(0.00812378219310841,-0.0315241814719618,
0.07415));
#74797=CARTESIAN_POINT('',(0.00334615942877989,-0.0337108120655687,0.0705203552920277));
#74798=CARTESIAN_POINT('',(0.0033384173407597,-0.0336938721132327,0.0705305686593155));
#74799=CARTESIAN_POINT('Origin',(0.0156980260465387,-0.0345562514985363,
0.0813078369163719));
#74800=CARTESIAN_POINT('Ctrl Pts',(0.00333841734076304,-0.0336938721132296,
0.0705305686593232));
#74801=CARTESIAN_POINT('Ctrl Pts',(0.00333970576774112,-0.0336910493402228,
0.0705288651891934));
#74802=CARTESIAN_POINT('Ctrl Pts',(0.00334099516111529,-0.0336882266078996,
0.0705271623319283));
#74803=CARTESIAN_POINT('Ctrl Pts',(0.00334357585981417,-0.03368258127131,
0.0705237578716093));
#74804=CARTESIAN_POINT('Ctrl Pts',(0.00334486716514167,-0.0336797586670152,
0.0705220562685262));
#74805=CARTESIAN_POINT('Ctrl Pts',(0.00334615942774173,-0.033676936124375,
0.0705203552912372));
#74806=CARTESIAN_POINT('Origin',(0.0170501938751676,-0.0345562516464922,
0.0795280033588314));
#74807=CARTESIAN_POINT('Ctrl Pts',(0.00364343979401434,-0.034243627687391,
0.0705438029744785));
#74808=CARTESIAN_POINT('Ctrl Pts',(0.00350742983104413,-0.0339430054201809,
0.0707127818737128));
#74809=CARTESIAN_POINT('Ctrl Pts',(0.00338453444117993,-0.0336441434784052,
0.0708915255493037));
#74810=CARTESIAN_POINT('Ctrl Pts',(0.00349095540972062,-0.034243627687391,
0.0707419153480107));
#74811=CARTESIAN_POINT('Ctrl Pts',(0.00336241737809453,-0.0339430054201809,
0.0709166452906058));
#74812=CARTESIAN_POINT('Ctrl Pts',(0.00324740588475092,-0.0336441434784052,
0.0711005608549621));
#74813=CARTESIAN_POINT('Ctrl Pts',(0.00348943056587769,-0.034243627687391,
0.0707438964717461));
#74814=CARTESIAN_POINT('Ctrl Pts',(0.00336096725356504,-0.0339430054201809,
0.0709186839247747));
#74815=CARTESIAN_POINT('Ctrl Pts',(0.00324603459918663,-0.0336441434784052,
0.0711026512080186));
#74816=CARTESIAN_POINT('',(0.00346960944486587,-0.0341934961088741,0.0707711242950476));
#74817=CARTESIAN_POINT('',(0.00333471940384579,-0.0338664212862863,0.0709651919046286));
#74818=CARTESIAN_POINT('Origin',(0.0167062358242239,-0.0345610720407109,
0.0810105024913875));
#74819=CARTESIAN_POINT('Origin',(-0.00579672281994097,-0.0336938005072901,
0.0648926728744124));
#74820=CARTESIAN_POINT('',(0.00340506923980481,-0.0336938721132327,0.0708618587219638));
#74821=CARTESIAN_POINT('',(0.00337045993753882,-0.0336938721132427,0.0709139014562984));
#74822=CARTESIAN_POINT('',(0.00354414528154742,-0.0340203938281605,0.0706707686541035));
#74823=CARTESIAN_POINT('Origin',(0.0163566639023995,-0.0345589643241676,
0.081341162747349));
#74824=CARTESIAN_POINT('',(0.00354522704296507,-0.0341934961088739,0.0706715904874359));
#74825=CARTESIAN_POINT('Origin',(-0.00522923290532131,-0.0341934220717675,
0.0640054768600253));
#74826=CARTESIAN_POINT('',(0.00350741824392547,-0.0341934961088841,0.0707213573912518));
#74827=CARTESIAN_POINT('Ctrl Pts',(0.00349210169950806,-0.0340223579322397,
0.0703358767973186));
#74828=CARTESIAN_POINT('Ctrl Pts',(0.00343949499289216,-0.0339125849573575,
0.0703997597512552));
#74829=CARTESIAN_POINT('Ctrl Pts',(0.00338824748110293,-0.0338030433565231,
0.0704646866519656));
#74830=CARTESIAN_POINT('Ctrl Pts',(0.00333841734075952,-0.0336938721132327,
0.0705305686593148));
#74831=CARTESIAN_POINT('Ctrl Pts',(0.00350984166340604,-0.0340223579322397,
0.0704477985267156));
#74832=CARTESIAN_POINT('Ctrl Pts',(0.00345877864934265,-0.0339125849573575,
0.0705114368002823));
#74833=CARTESIAN_POINT('Ctrl Pts',(0.00340906868105594,-0.0338030433565231,
0.070576087241708));
#74834=CARTESIAN_POINT('Ctrl Pts',(0.00336076800024638,-0.0336938721132327,
0.0706416615387033));
#74835=CARTESIAN_POINT('Ctrl Pts',(0.00352758162730401,-0.0340223579322397,
0.0705597202561127));
#74836=CARTESIAN_POINT('Ctrl Pts',(0.00347806230579314,-0.0339125849573575,
0.0706231138493094));
#74837=CARTESIAN_POINT('Ctrl Pts',(0.00342988988100896,-0.0338030433565231,
0.0706874878314505));
#74838=CARTESIAN_POINT('Ctrl Pts',(0.00338311865973323,-0.0336938721132327,
0.0707527544180917));
#74839=CARTESIAN_POINT('Ctrl Pts',(0.00354532159120199,-0.0340223579322397,
0.0706716419855097));
#74840=CARTESIAN_POINT('Ctrl Pts',(0.00349734596224362,-0.0339125849573575,
0.0707347908983365));
#74841=CARTESIAN_POINT('Ctrl Pts',(0.00345071108096197,-0.0338030433565231,
0.0707988884211929));
#74842=CARTESIAN_POINT('Ctrl Pts',(0.00340546931922008,-0.0336938721132327,
0.0708638472974802));
#74843=CARTESIAN_POINT('',(0.00337174329029226,-0.0336938721132427,0.0706962136906497));
#74844=CARTESIAN_POINT('Ctrl Pts',(0.00334615943164338,-0.033710812066269,
0.0705203552942016));
#74845=CARTESIAN_POINT('Ctrl Pts',(0.00338039846916955,-0.0337611408994349,
0.0705463672979728));
#74846=CARTESIAN_POINT('Ctrl Pts',(0.00341401272022329,-0.0338121088781425,
0.0705719046403851));
#74847=CARTESIAN_POINT('Ctrl Pts',(0.00348002227141877,-0.0339153382773237,
0.0706220532665934));
#74848=CARTESIAN_POINT('Ctrl Pts',(0.00351238964548876,-0.0339675558473105,
0.0706466433344575));
#74849=CARTESIAN_POINT('Ctrl Pts',(0.00354414528157595,-0.0340203938281304,
0.0706707686541318));
#74850=CARTESIAN_POINT('Ctrl Pts',(0.00347161894542728,-0.0341934961088741,
0.0707708499059484));
#74851=CARTESIAN_POINT('Ctrl Pts',(0.00340175767936725,-0.0340287516182428,
0.0708670297160649));
#74852=CARTESIAN_POINT('Ctrl Pts',(0.00333593129294256,-0.0338644633275951,
0.0709660147615001));
#74853=CARTESIAN_POINT('Ctrl Pts',(0.00346960944486598,-0.0341934961088741,
0.0707711242950476));
#74854=CARTESIAN_POINT('Ctrl Pts',(0.0033997538515844,-0.0340287516182428,
0.0708673456500051));
#74855=CARTESIAN_POINT('Ctrl Pts',(0.00333393485017068,-0.0338644633275951,
0.0709663719703218));
#74856=CARTESIAN_POINT('Ctrl Pts',(0.00313478800011416,-0.0341934961088741,
0.0708168427966462));
#74857=CARTESIAN_POINT('Ctrl Pts',(0.00306587760083556,-0.0340287516182428,
0.0709199863211976));
#74858=CARTESIAN_POINT('Ctrl Pts',(0.00300128908429549,-0.0338644633275951,
0.0710258898306616));
#74859=CARTESIAN_POINT('',(0.00312767969907691,-0.0341764758832379,0.070827506981246));
#74860=CARTESIAN_POINT('',(0.00313478800011417,-0.034193496108874,0.0708168427966462));
#74861=CARTESIAN_POINT('Origin',(0.0166314748765275,-0.0345621026256374,
0.0804227582310192));
#74862=CARTESIAN_POINT('Ctrl Pts',(0.0031276797006797,-0.034176475883746,
0.0708275069803871));
#74863=CARTESIAN_POINT('Ctrl Pts',(0.0031634221400341,-0.0341260050040264,
0.0708512762931555));
#74864=CARTESIAN_POINT('Ctrl Pts',(0.00319854331262926,-0.0340749269147844,
0.0708746324073788));
#74865=CARTESIAN_POINT('Ctrl Pts',(0.00326757024200344,-0.0339715436305533,
0.0709205364926982));
#74866=CARTESIAN_POINT('Ctrl Pts',(0.00330144980820865,-0.0339192778236031,
0.070943067053803));
#74867=CARTESIAN_POINT('Ctrl Pts',(0.0033347194038929,-0.0338664212854243,
0.0709651919024983));
#74868=CARTESIAN_POINT('',(0.00330219872250002,-0.0341934961088841,0.070793983545857));
#74869=CARTESIAN_POINT('Origin',(0.00812378219310841,-0.0315241814719618,
0.07415));
#74870=CARTESIAN_POINT('',(0.00312767969922361,-0.0342105180190374,0.0708275069823544));
#74871=CARTESIAN_POINT('',(0.00312059419090093,-0.0341934961088739,0.0708381863255021));
#74872=CARTESIAN_POINT('Origin',(0.0166607652514386,-0.0345621705449535,
0.0803881656872907));
#74873=CARTESIAN_POINT('Origin',(0.017198625998726,-0.0345621038351193,
0.0795699252462993));
#74874=CARTESIAN_POINT('Origin',(0.0171780478231302,-0.0345621716956665,
0.0796103116433129));
#74875=CARTESIAN_POINT('Ctrl Pts',(0.00340589986854741,-0.0346945769586965,
0.070860609688088));
#74876=CARTESIAN_POINT('Ctrl Pts',(0.00333700227146439,-0.0345275153362944,
0.0709594276223129));
#74877=CARTESIAN_POINT('Ctrl Pts',(0.0032711945870095,-0.0343603235965185,
0.0710604378819296));
#74878=CARTESIAN_POINT('Ctrl Pts',(0.00320866700499458,-0.034193496108874,
0.0711633388307211));
#74879=CARTESIAN_POINT('Ctrl Pts',(0.00335947725581904,-0.0346945769586965,
0.0709304163453157));
#74880=CARTESIAN_POINT('Ctrl Pts',(0.00329204178712072,-0.0345275153362944,
0.0710302066197508));
#74881=CARTESIAN_POINT('Ctrl Pts',(0.00322772718843645,-0.0343603235965185,
0.0711321434884827));
#74882=CARTESIAN_POINT('Ctrl Pts',(0.00316671919296221,-0.034193496108874,
0.0712359226404277));
#74883=CARTESIAN_POINT('Ctrl Pts',(0.00331305464309072,-0.0346945769586965,
0.0710002230025449));
#74884=CARTESIAN_POINT('Ctrl Pts',(0.00324708130277711,-0.0345275153362944,
0.0711009856171904));
#74885=CARTESIAN_POINT('Ctrl Pts',(0.00318425978986348,-0.0343603235965185,
0.0712038490950376));
#74886=CARTESIAN_POINT('Ctrl Pts',(0.00312477138092993,-0.034193496108874,
0.0713085064501362));
#74887=CARTESIAN_POINT('Ctrl Pts',(0.00326663203036231,-0.0346945769586965,
0.0710700296597711));
#74888=CARTESIAN_POINT('Ctrl Pts',(0.00320212081843338,-0.0345275153362944,
0.0711717646146266));
#74889=CARTESIAN_POINT('Ctrl Pts',(0.00314079239129035,-0.0343603235965185,
0.0712755547015891));
#74890=CARTESIAN_POINT('Ctrl Pts',(0.00308282356889745,-0.034193496108874,
0.071381090259841));
#74891=CARTESIAN_POINT('',(0.00326663203069789,-0.0346945769586966,0.0710700296592668));
#74892=CARTESIAN_POINT('',(0.00314419377144035,-0.034366772783143,0.0712721841353108));
#74893=CARTESIAN_POINT('Origin',(0.0175632353100188,-0.0345626457064379,
0.0799190059793397));
#74894=CARTESIAN_POINT('Origin',(-0.00642490442479576,-0.034193477102909,
0.0657419929855118));
#74895=CARTESIAN_POINT('',(0.00320791644279703,-0.034193496108874,0.0711646375555192));
#74896=CARTESIAN_POINT('',(0.00317664322440932,-0.0341934961088841,0.0712187507314761));
#74897=CARTESIAN_POINT('',(0.00333471940511753,-0.0345211942962721,0.0709651919033584));
#74898=CARTESIAN_POINT('Origin',(0.0172942183244265,-0.034562559611922,
0.0803175290668221));
#74899=CARTESIAN_POINT('',(0.00333585063525286,-0.0346945769586885,0.0709659441906129));
#74900=CARTESIAN_POINT('Origin',(-0.0058766013599473,-0.0346945685853852,
0.064839506119231));
#74901=CARTESIAN_POINT('',(0.00330124133298537,-0.0346945769587026,0.0710179869249498));
#74902=CARTESIAN_POINT('Ctrl Pts',(0.00326174992171197,-0.0345231616327842,
0.0706342295023815));
#74903=CARTESIAN_POINT('Ctrl Pts',(0.00321328997521123,-0.0344132092796988,
0.0707012457720489));
#74904=CARTESIAN_POINT('Ctrl Pts',(0.00316621870769734,-0.034303273855898,
0.0707692609397534));
#74905=CARTESIAN_POINT('Ctrl Pts',(0.00312059419090085,-0.0341934961088739,
0.0708381863255021));
#74906=CARTESIAN_POINT('Ctrl Pts',(0.00328648247903689,-0.0345231616327842,
0.0707448162861609));
#74907=CARTESIAN_POINT('Ctrl Pts',(0.00323954681565681,-0.0344132092796988,
0.0708114916523462));
#74908=CARTESIAN_POINT('Ctrl Pts',(0.00319399270129795,-0.034303273855898,
0.0708791344055637));
#74909=CARTESIAN_POINT('Ctrl Pts',(0.0031498762762636,-0.0341934961088739,
0.0709476563927137));
#74910=CARTESIAN_POINT('Ctrl Pts',(0.00331121503636181,-0.0345231616327842,
0.0708554030699402));
#74911=CARTESIAN_POINT('Ctrl Pts',(0.00326580365610239,-0.0344132092796988,
0.0709217375326434));
#74912=CARTESIAN_POINT('Ctrl Pts',(0.00322176669489857,-0.034303273855898,
0.0709890078713739));
#74913=CARTESIAN_POINT('Ctrl Pts',(0.00317915836162634,-0.0341934961088739,
0.0710571264599253));
#74914=CARTESIAN_POINT('Ctrl Pts',(0.00333594759368673,-0.0345231616327842,
0.0709659898537196));
#74915=CARTESIAN_POINT('Ctrl Pts',(0.00329206049654798,-0.0344132092796988,
0.0710319834129407));
#74916=CARTESIAN_POINT('Ctrl Pts',(0.00324954068849918,-0.034303273855898,
0.0710988813371842));
#74917=CARTESIAN_POINT('Ctrl Pts',(0.00320844044698908,-0.0341934961088739,
0.0711665965271368));
#74918=CARTESIAN_POINT('',(0.00316425531685898,-0.0341934961088839,0.0710014119405207));
#74919=CARTESIAN_POINT('Ctrl Pts',(0.00312767970209473,-0.0342105180195393,
0.0708275069842621));
#74920=CARTESIAN_POINT('Ctrl Pts',(0.00316346231527264,-0.0342610556241295,
0.0708513030297961));
#74921=CARTESIAN_POINT('Ctrl Pts',(0.00319860282795846,-0.0343122189870136,
0.0708746720675967));
#74922=CARTESIAN_POINT('Ctrl Pts',(0.00326763045583263,-0.0344158119695204,
0.070920576612573));
#74923=CARTESIAN_POINT('Ctrl Pts',(0.0033014893382135,-0.0344681990450117,
0.0709430933444522));
#74924=CARTESIAN_POINT('Ctrl Pts',(0.0033347194051368,-0.0345211942962544,
0.0709651919033716));
#74925=CARTESIAN_POINT('Ctrl Pts',(0.00326861985010767,-0.0346945769586932,
0.0710696297319652));
#74926=CARTESIAN_POINT('Ctrl Pts',(0.00320493537441614,-0.034529677707698,
0.071170006778004));
#74927=CARTESIAN_POINT('Ctrl Pts',(0.00314545399186463,-0.0343648066251421,
0.0712729301910127));
#74928=CARTESIAN_POINT('Ctrl Pts',(0.00326663203070282,-0.0346945769586932,
0.0710700296592592));
#74929=CARTESIAN_POINT('Ctrl Pts',(0.00320295582322511,-0.034529677707698,
0.0711704478020577));
#74930=CARTESIAN_POINT('Ctrl Pts',(0.00314348440038918,-0.0343648066251421,
0.0712734119349765));
#74931=CARTESIAN_POINT('Ctrl Pts',(0.00293534196805695,-0.0346945769586932,
0.0711366815583036));
#74932=CARTESIAN_POINT('Ctrl Pts',(0.00287304374143061,-0.034529677707698,
0.0712439488887339));
#74933=CARTESIAN_POINT('Ctrl Pts',(0.00281523220519733,-0.0343648066251421,
0.0713536994035245));
#74934=CARTESIAN_POINT('',(0.00292891730306486,-0.0346775396664965,0.0711477710334621));
#74935=CARTESIAN_POINT('',(0.00293534196805525,-0.0346945769586886,0.0711366815583065));
#74936=CARTESIAN_POINT('Origin',(0.0173785634158705,-0.0345626618297238,
0.07932215959235));
#74937=CARTESIAN_POINT('Ctrl Pts',(0.00292891730466133,-0.0346775396670097,
0.0711477710325909));
#74938=CARTESIAN_POINT('Ctrl Pts',(0.00296611097177062,-0.0346269749928187,
0.0711692660723642));
#74939=CARTESIAN_POINT('Ctrl Pts',(0.00300264364239575,-0.0345757902890786,
0.0711903790662173));
#74940=CARTESIAN_POINT('Ctrl Pts',(0.00307441699124798,-0.0344721681087842,
0.0712318584991063));
#74941=CARTESIAN_POINT('Ctrl Pts',(0.0031096295281245,-0.0344197714289452,
0.0712522086811331));
#74942=CARTESIAN_POINT('Ctrl Pts',(0.00314419377146478,-0.0343667727830583,
0.0712721841350437));
#74943=CARTESIAN_POINT('',(0.00310098699938657,-0.0346945769587026,0.0711033556087966));
#74944=CARTESIAN_POINT('Origin',(0.00812378219310841,-0.0315241814719618,
0.07415));
#74945=CARTESIAN_POINT('',(0.0029289173037152,-0.0347116136489618,0.0711477710346915));
#74946=CARTESIAN_POINT('',(0.00292251633834764,-0.0346945769586885,0.0711588742072382));
#74947=CARTESIAN_POINT('Origin',(0.0173996004797876,-0.0345626684329631,
0.0792820256874896));
#74948=CARTESIAN_POINT('Origin',(0.0172257359434592,-0.0345626628847385,
0.0795866077582412));
#74949=CARTESIAN_POINT('Origin',(0.0172014601357675,-0.0345626695489208,
0.0796248698269157));
#74950=CARTESIAN_POINT('Ctrl Pts',(0.00322802826454031,-0.0352450361874068,
0.0711316633559964));
#74951=CARTESIAN_POINT('Ctrl Pts',(0.00311418983000982,-0.0349452760959493,
0.0713163097453188));
#74952=CARTESIAN_POINT('Ctrl Pts',(0.00301458312004364,-0.034644428984174,
0.0715090063503637));
#74953=CARTESIAN_POINT('Ctrl Pts',(0.00322675112972715,-0.0352450361874068,
0.0711338415551767));
#74954=CARTESIAN_POINT('Ctrl Pts',(0.0031129948473268,-0.0349452760959493,
0.0713185361124289));
#74955=CARTESIAN_POINT('Ctrl Pts',(0.00301347368431078,-0.034644428984174,
0.0715112745605292));
#74956=CARTESIAN_POINT('Ctrl Pts',(0.00310030213832565,-0.0352450361874068,
0.0713495048403541));
#74957=CARTESIAN_POINT('Ctrl Pts',(0.00299467973019645,-0.0349452760959493,
0.0715389684995745));
#74958=CARTESIAN_POINT('Ctrl Pts',(0.00290362856224478,-0.034644428984174,
0.0717358498244349));
#74959=CARTESIAN_POINT('Ctrl Pts',(0.00309903764841163,-0.0352450361874068,
0.071351661473206));
#74960=CARTESIAN_POINT('Ctrl Pts',(0.00299349657902514,-0.0349452760959493,
0.0715411728234459));
#74961=CARTESIAN_POINT('Ctrl Pts',(0.00290253011102412,-0.034644428984174,
0.0717380955770739));
#74962=CARTESIAN_POINT('',(0.00308283706751842,-0.0351951634053268,0.0713810607548514));
#74963=CARTESIAN_POINT('',(0.00297332029856974,-0.0348678972925434,0.0715905337914116));
#74964=CARTESIAN_POINT('Origin',(0.0181602499772387,-0.0345636767877706,
0.0786663964587444));
#74965=CARTESIAN_POINT('Origin',(-0.00692204325513113,-0.0346946199340719,
0.0666731392099248));
#74966=CARTESIAN_POINT('',(0.00303016433057554,-0.0346945769330288,0.0714791982349079));
#74967=CARTESIAN_POINT('',(0.00300235061297133,-0.0346945769458129,0.0715351683001273));
#74968=CARTESIAN_POINT('',(0.00314419377157413,-0.0350221583435276,0.0712721841351256));
#74969=CARTESIAN_POINT('Origin',(0.0179842440841164,-0.0345628458719571,
0.0791137948493126));
#74970=CARTESIAN_POINT('',(0.00314526619307874,-0.0351951360298761,0.0712728004182273));
#74971=CARTESIAN_POINT('Origin',(-0.00639508383650517,-0.0351951838366808,
0.0657592203489523));
#74972=CARTESIAN_POINT('',(0.00308282356910537,-0.0351951371328751,0.071381090259249));
#74973=CARTESIAN_POINT('Ctrl Pts',(0.00305058646273447,-0.0350241211494343,
0.0709464574169615));
#74974=CARTESIAN_POINT('Ctrl Pts',(0.00300645897715671,-0.0349144232818962,
0.0710163386080562));
#74975=CARTESIAN_POINT('Ctrl Pts',(0.00296374957330617,-0.0348045283579412,
0.0710871737730708));
#74976=CARTESIAN_POINT('Ctrl Pts',(0.00292251633280762,-0.0346945769439157,
0.0711588742168717));
#74977=CARTESIAN_POINT('Ctrl Pts',(0.00308221404201289,-0.0350241211494343,
0.0710552730317966));
#74978=CARTESIAN_POINT('Ctrl Pts',(0.00303958544691334,-0.0349144232818962,
0.0711247185659545));
#74979=CARTESIAN_POINT('Ctrl Pts',(0.00299836682535904,-0.0348045283579412,
0.0711950868301334));
#74980=CARTESIAN_POINT('Ctrl Pts',(0.00295861432721755,-0.0346945769439157,
0.0712662896561834));
#74981=CARTESIAN_POINT('Ctrl Pts',(0.00311384162129132,-0.0350241211494343,
0.0711640886466316));
#74982=CARTESIAN_POINT('Ctrl Pts',(0.00307271191666998,-0.0349144232818962,
0.0712330985238528));
#74983=CARTESIAN_POINT('Ctrl Pts',(0.0030329840774119,-0.0348045283579412,
0.0713029998871961));
#74984=CARTESIAN_POINT('Ctrl Pts',(0.00299471232162748,-0.0346945769439157,
0.0713737050954951));
#74985=CARTESIAN_POINT('Ctrl Pts',(0.00314546920056974,-0.0350241211494343,
0.0712729042614667));
#74986=CARTESIAN_POINT('Ctrl Pts',(0.00310583838642662,-0.0349144232818962,
0.0713414784817511));
#74987=CARTESIAN_POINT('Ctrl Pts',(0.00306760132946477,-0.0348045283579412,
0.0714109129442587));
#74988=CARTESIAN_POINT('Ctrl Pts',(0.00303081031603742,-0.0346945769439157,
0.0714811205348068));
#74989=CARTESIAN_POINT('',(0.00297634033452877,-0.0346945769458128,0.0713190362207805));
#74990=CARTESIAN_POINT('Ctrl Pts',(0.00292891730655676,-0.0347116136492798,
0.0711477710363316));
#74991=CARTESIAN_POINT('Ctrl Pts',(0.00296609619679808,-0.0347621546532283,
0.0711692575511029));
#74992=CARTESIAN_POINT('Ctrl Pts',(0.00300262138168077,-0.0348133084096993,
0.0711903662748816));
#74993=CARTESIAN_POINT('Ctrl Pts',(0.00307439482349242,-0.034916856154457,
0.0712318457571271));
#74994=CARTESIAN_POINT('Ctrl Pts',(0.00310961461153599,-0.0349692089015911,
0.0712522000627862));
#74995=CARTESIAN_POINT('Ctrl Pts',(0.00314419377159582,-0.0350221583435,
0.0712721841351612));
#74996=CARTESIAN_POINT('Ctrl Pts',(0.00308423689773535,-0.0351951371254879,
0.0713807122088686));
#74997=CARTESIAN_POINT('Ctrl Pts',(0.00302698361016444,-0.0350307338980929,
0.0714849016459314));
#74998=CARTESIAN_POINT('Ctrl Pts',(0.00297408550704852,-0.0348659306897834,
0.0715913683938852));
#74999=CARTESIAN_POINT('Ctrl Pts',(0.00308282356920761,-0.0351951371254879,
0.0713810902593042));
#75000=CARTESIAN_POINT('Ctrl Pts',(0.00302557809759226,-0.0350307338980929,
0.0714853089160476));
#75001=CARTESIAN_POINT('Ctrl Pts',(0.00297268901143414,-0.0348659306897834,
0.071591804535672));
#75002=CARTESIAN_POINT('Ctrl Pts',(0.00284594823493688,-0.0351951371254879,
0.071444451906329));
#75003=CARTESIAN_POINT('Ctrl Pts',(0.0027900127256193,-0.0350307338980929,
0.0715535678119876));
#75004=CARTESIAN_POINT('Ctrl Pts',(0.0027386348909858,-0.0348659306897834,
0.0716649023537017));
#75005=CARTESIAN_POINT('Origin',(-0.00178922270627967,-0.0308609197384417,
0.0692238396757387));
#75006=CARTESIAN_POINT('',(0.00297955126429345,-0.0351951371254879,0.071408714508792));
#75007=CARTESIAN_POINT('Origin',(0.00905257469815753,-0.0351840467441159,
0.0744534635602127));
#75008=CARTESIAN_POINT('Origin',(-0.00292136006055052,-0.0352322614082497,
0.0695486482211981));
#75009=CARTESIAN_POINT('',(0.00287241071720265,-0.0351951142564652,0.0718045976452916));
#75010=CARTESIAN_POINT('',(0.00282402548190293,-0.0351951372916786,0.0719195115328626));
#75011=CARTESIAN_POINT('Origin',(0.00817580825674042,-0.0352875120661354,
0.0744865877874527));
#75012=CARTESIAN_POINT('Origin',(0.0123045189010117,-0.0298325076521961,
0.0679197005801442));
#75013=CARTESIAN_POINT('Origin',(0.00219055981987634,-0.0338732045131652,
0.0682298561825369));
#75014=CARTESIAN_POINT('Ctrl Pts',(0.00525422229196418,-0.0321934096636942,
0.0691656483150708));
#75015=CARTESIAN_POINT('Ctrl Pts',(0.00516500477033232,-0.0320508460843443,
0.0692170120708283));
#75016=CARTESIAN_POINT('Ctrl Pts',(0.00507723456177527,-0.0319086045661309,
0.0692707341969115));
#75017=CARTESIAN_POINT('Ctrl Pts',(0.00499109112805847,-0.0317669892865267,
0.0693266834617408));
#75018=CARTESIAN_POINT('Ctrl Pts',(0.0051824833593981,-0.0321934096636942,
0.0692090529021806));
#75019=CARTESIAN_POINT('Ctrl Pts',(0.00509404275920641,-0.0320508460843443,
0.0692617007506693));
#75020=CARTESIAN_POINT('Ctrl Pts',(0.0050070833873262,-0.0319086045661309,
0.0693166851269273));
#75021=CARTESIAN_POINT('Ctrl Pts',(0.00492178273589887,-0.0317669892865267,
0.0693738722252596));
#75022=CARTESIAN_POINT('Ctrl Pts',(0.00511074442683202,-0.0321934096636942,
0.0692524574892904));
#75023=CARTESIAN_POINT('Ctrl Pts',(0.00502308074808051,-0.0320508460843443,
0.0693063894305101));
#75024=CARTESIAN_POINT('Ctrl Pts',(0.00493693221287711,-0.0319086045661309,
0.0693626360569431));
#75025=CARTESIAN_POINT('Ctrl Pts',(0.00485247434373929,-0.0317669892865268,
0.0694210609887785));
#75026=CARTESIAN_POINT('Ctrl Pts',(0.00503900549426594,-0.0321934096636942,
0.0692958620764002));
#75027=CARTESIAN_POINT('Ctrl Pts',(0.0049521187369546,-0.0320508460843443,
0.0693510781103512));
#75028=CARTESIAN_POINT('Ctrl Pts',(0.00486678103842803,-0.0319086045661309,
0.069408586986959));
#75029=CARTESIAN_POINT('Ctrl Pts',(0.0047831659515797,-0.0317669892865268,
0.0694682497522974));
#75030=CARTESIAN_POINT('',(0.00504028891794717,-0.0321934096636942,0.0692950855597615));
#75031=CARTESIAN_POINT('',(0.00484343027988913,-0.0318665617511257,0.0694258687238353));
#75032=CARTESIAN_POINT('Origin',(0.0134738133231417,-0.0326371944421483,
0.0837205342863425));
#75033=CARTESIAN_POINT('Origin',(-0.00140840499145849,-0.0316939261509243,
0.0604224168376222));
#75034=CARTESIAN_POINT('',(0.00514633205196241,-0.0320197221621856,0.0692293923318842));
#75035=CARTESIAN_POINT('Ctrl Pts',(0.00514615460494484,-0.032019739209477,
0.0692294445567315));
#75036=CARTESIAN_POINT('Ctrl Pts',(0.00512111726123343,-0.0319792716576067,
0.0692445957233421));
#75037=CARTESIAN_POINT('Ctrl Pts',(0.00509608144439834,-0.0319386439829713,
0.069260006738462));
#75038=CARTESIAN_POINT('Ctrl Pts',(0.00507102530504198,-0.0318979099381645,
0.0692757009830988));
#75039=CARTESIAN_POINT('Ctrl Pts',(0.0050459696609371,-0.0318571766984935,
0.0692913949175282));
#75040=CARTESIAN_POINT('Ctrl Pts',(0.00502102009849267,-0.0318163871833572,
0.0693072907935115));
#75041=CARTESIAN_POINT('Ctrl Pts',(0.00499626054190498,-0.0317755399638303,
0.0693233309661393));
#75042=CARTESIAN_POINT('',(0.00514723722102942,-0.0321934096636183,0.0692303780603392));
#75043=CARTESIAN_POINT('Origin',(0.00393412247364323,-0.0324113231919104,
0.067265984065929));
#75044=CARTESIAN_POINT('',(0.00509376306949829,-0.0321934096636663,0.0692627318100604));
#75045=CARTESIAN_POINT('Ctrl Pts',(0.00504225838682757,-0.0321934096636618,
0.0692955702036599));
#75046=CARTESIAN_POINT('Ctrl Pts',(0.00497531201661472,-0.0320835708272592,
0.0693380668185477));
#75047=CARTESIAN_POINT('Ctrl Pts',(0.00490928394325373,-0.0319739230346488,
0.069381924235324));
#75048=CARTESIAN_POINT('Ctrl Pts',(0.00484425433860424,-0.0318646057455572,
0.0694270798579903));
#75049=CARTESIAN_POINT('Ctrl Pts',(0.00493222216080788,-0.0321934096636618,
0.0692684926534038));
#75050=CARTESIAN_POINT('Ctrl Pts',(0.00486490237007399,-0.0320835708272592,
0.0693125067536056));
#75051=CARTESIAN_POINT('Ctrl Pts',(0.00479853249707075,-0.0319739230346488,
0.069357888503411));
#75052=CARTESIAN_POINT('Ctrl Pts',(0.00473319300128829,-0.0318646057455572,
0.069404573322981));
#75053=CARTESIAN_POINT('Ctrl Pts',(0.00482218593478819,-0.0321934096636618,
0.0692414151031477));
#75054=CARTESIAN_POINT('Ctrl Pts',(0.00475449272353326,-0.0320835708272592,
0.0692869466886635));
#75055=CARTESIAN_POINT('Ctrl Pts',(0.00468778105088776,-0.0319739230346488,
0.0693338527714981));
#75056=CARTESIAN_POINT('Ctrl Pts',(0.00462213166397235,-0.0318646057455572,
0.0693820667879717));
#75057=CARTESIAN_POINT('Ctrl Pts',(0.00471214970876851,-0.0321934096636618,
0.0692143375528915));
#75058=CARTESIAN_POINT('Ctrl Pts',(0.00464408307699253,-0.0320835708272592,
0.0692613866237214));
#75059=CARTESIAN_POINT('Ctrl Pts',(0.00457702960470477,-0.0319739230346488,
0.0693098170395851));
#75060=CARTESIAN_POINT('Ctrl Pts',(0.0045110703266564,-0.0318646057455572,
0.0693595602529624));
#75061=CARTESIAN_POINT('',(0.00470161482932084,-0.0321763980308261,0.0692216361222138));
#75062=CARTESIAN_POINT('',(0.00471214970874164,-0.0321934096636185,0.0692143375529101));
#75063=CARTESIAN_POINT('Origin',(0.01362936035573,-0.0326386230750649,0.0831543836591411));
#75064=CARTESIAN_POINT('Ctrl Pts',(0.0047016148311254,-0.0321763980306274,
0.069221636124815));
#75065=CARTESIAN_POINT('Ctrl Pts',(0.00472609410383957,-0.0321259596174904,
0.0692568894454666));
#75066=CARTESIAN_POINT('Ctrl Pts',(0.00475014924139586,-0.0320749164631554,
0.0692915319565902));
#75067=CARTESIAN_POINT('Ctrl Pts',(0.00479743060497968,-0.0319716057793888,
0.0693596232389876));
#75068=CARTESIAN_POINT('Ctrl Pts',(0.00482063840858775,-0.0319193786690074,
0.0693930454795933));
#75069=CARTESIAN_POINT('Ctrl Pts',(0.00484343028094309,-0.0318665617525257,
0.0694258687253562));
#75070=CARTESIAN_POINT('',(0.00487621931335441,-0.0321934096636664,0.0692547115563458));
#75071=CARTESIAN_POINT('Origin',(0.00812378219310841,-0.0315241814719618,
0.07415));
#75072=CARTESIAN_POINT('',(0.00470161482910887,-0.032210423332379,0.0692216361219087));
#75073=CARTESIAN_POINT('',(0.00469109556167723,-0.0321934096636183,0.0692289571744985));
#75074=CARTESIAN_POINT('Origin',(0.0136698375773385,-0.0326387233381217,
0.0831339680613262));
#75075=CARTESIAN_POINT('Origin',(0.014637217912418,-0.0326386244463913,
0.0824545485597093));
#75076=CARTESIAN_POINT('Origin',(0.0146039435917886,-0.0326387242889573,
0.0824853382453447));
#75077=CARTESIAN_POINT('Ctrl Pts',(0.00497707169695243,-0.0327445246967096,
0.0693358190672367));
#75078=CARTESIAN_POINT('Ctrl Pts',(0.00479550189480918,-0.0324436878339359,
0.0694544991937564));
#75079=CARTESIAN_POINT('Ctrl Pts',(0.00462338738547849,-0.0321434074405927,
0.0695865187421534));
#75080=CARTESIAN_POINT('Ctrl Pts',(0.00477083115617685,-0.0327445246967096,
0.0694771160570865));
#75081=CARTESIAN_POINT('Ctrl Pts',(0.0045945904571248,-0.0324436878339359,
0.0696035746727626));
#75082=CARTESIAN_POINT('Ctrl Pts',(0.00442837581906062,-0.0321434074405927,
0.0697429492026246));
#75083=CARTESIAN_POINT('',(0.00474153088763896,-0.0326943950436612,0.0694982797690907));
#75084=CARTESIAN_POINT('',(0.00455327264731455,-0.0323666188837389,0.0696411657179049));
#75085=CARTESIAN_POINT('Origin',(0.0146890686202625,-0.0326395579112807,
0.0830502003442997));
#75086=CARTESIAN_POINT('Origin',(-0.00230334794594286,-0.0321933825602924,
0.0609826366339883));
#75087=CARTESIAN_POINT('',(0.00465211103054775,-0.0321934096532689,0.0695646293131717));
#75088=CARTESIAN_POINT('',(0.00460311353637187,-0.0321934096584275,0.0696034300336581));
#75089=CARTESIAN_POINT('',(0.0048434302793459,-0.0325210109756239,0.0694258687230481));
#75090=CARTESIAN_POINT('Origin',(0.0142858016141189,-0.0326393129159858,
0.0833120402794587));
#75091=CARTESIAN_POINT('',(0.00484420513512571,-0.0326943950436593,0.0694269846156556));
#75092=CARTESIAN_POINT('Origin',(-0.0014653897014078,-0.0326943765538158,
0.0603403499416489));
#75093=CARTESIAN_POINT('',(0.00479286801139234,-0.0326943950436702,0.0694626321923832));
#75094=CARTESIAN_POINT('Ctrl Pts',(0.00489742048002139,-0.0325229783203769,
0.0690912857269507));
#75095=CARTESIAN_POINT('Ctrl Pts',(0.00482768621439418,-0.032413025309245,
0.0691357610526098));
#75096=CARTESIAN_POINT('Ctrl Pts',(0.00475888255457854,-0.0323031222208069,
0.0691816721755787));
#75097=CARTESIAN_POINT('Ctrl Pts',(0.00469109555799938,-0.0321934096576658,
0.069228957177064));
#75098=CARTESIAN_POINT('Ctrl Pts',(0.00487970651298126,-0.0325229783203769,
0.0692032114058989));
#75099=CARTESIAN_POINT('Ctrl Pts',(0.0048115151403907,-0.032413025309245,
0.0692479309182062));
#75100=CARTESIAN_POINT('Ctrl Pts',(0.00474425919091624,-0.0323031222208069,
0.0692940542740633));
#75101=CARTESIAN_POINT('Ctrl Pts',(0.00467802272988302,-0.0321934096576658,
0.0693415193527775));
#75102=CARTESIAN_POINT('Ctrl Pts',(0.00486199254594113,-0.0325229783203769,
0.0693151370848471));
#75103=CARTESIAN_POINT('Ctrl Pts',(0.00479534406638722,-0.032413025309245,
0.0693601007838027));
#75104=CARTESIAN_POINT('Ctrl Pts',(0.00472963582725395,-0.0323031222208069,
0.0694064363725479));
#75105=CARTESIAN_POINT('Ctrl Pts',(0.00466494990176666,-0.0321934096576658,
0.0694540815284909));
#75106=CARTESIAN_POINT('Ctrl Pts',(0.004844278578901,-0.0325229783203769,
0.0694270627637952));
#75107=CARTESIAN_POINT('Ctrl Pts',(0.00477917299238373,-0.032413025309245,
0.0694722706493991));
#75108=CARTESIAN_POINT('Ctrl Pts',(0.00471501246359166,-0.0323031222208069,
0.0695188184710325));
#75109=CARTESIAN_POINT('Ctrl Pts',(0.0046518770736503,-0.0321934096576658,
0.0695666437042044));
#75110=CARTESIAN_POINT('',(0.00467160329642365,-0.0321934096584275,0.0693967932434306));
#75111=CARTESIAN_POINT('Ctrl Pts',(0.00470161483108758,-0.0322104233328934,
0.0692216361247604));
#75112=CARTESIAN_POINT('Ctrl Pts',(0.00472612727361019,-0.0322609421831263,
0.0692569372142288));
#75113=CARTESIAN_POINT('Ctrl Pts',(0.00475019861516221,-0.0323120888240518,
0.0692916030612151));
#75114=CARTESIAN_POINT('Ctrl Pts',(0.00479748033672828,-0.0324156524631818,
0.0693596948591533));
#75115=CARTESIAN_POINT('Ctrl Pts',(0.00482067128146181,-0.0324680267167314,
0.069393092820786));
#75116=CARTESIAN_POINT('Ctrl Pts',(0.00484343027936698,-0.0325210109755913,
0.0694258687230862));
#75117=CARTESIAN_POINT('Origin',(0.0150798194753273,-0.0262834582512383,
0.0704734620679012));
#75118=CARTESIAN_POINT('Origin',(0.00638952005960307,-0.0342770595364488,
0.0621161235546925));
#75119=CARTESIAN_POINT('Ctrl Pts',(0.00474352641682006,-0.0326943950436604,
0.0694986397053626));
#75120=CARTESIAN_POINT('Ctrl Pts',(0.00467942195438166,-0.0325844576448134,
0.0695452259652344));
#75121=CARTESIAN_POINT('Ctrl Pts',(0.00461627643540422,-0.0324744968375322,
0.0695931413074722));
#75122=CARTESIAN_POINT('Ctrl Pts',(0.00455416991882988,-0.0323646534831895,
0.0696423232242119));
#75123=CARTESIAN_POINT('Ctrl Pts',(0.00463200727016761,-0.0326943950436604,
0.0694785248473886));
#75124=CARTESIAN_POINT('Ctrl Pts',(0.00456762558728707,-0.0325844576448134,
0.0695266480501104));
#75125=CARTESIAN_POINT('Ctrl Pts',(0.00450423461474615,-0.0324744968375322,
0.0695761061773433));
#75126=CARTESIAN_POINT('Ctrl Pts',(0.0044419146987117,-0.0323646534831895,
0.0696268347401793));
#75127=CARTESIAN_POINT('Ctrl Pts',(0.00452048812351516,-0.0326943950436604,
0.0694584099894146));
#75128=CARTESIAN_POINT('Ctrl Pts',(0.00445582922019247,-0.0325844576448134,
0.0695080701349864));
#75129=CARTESIAN_POINT('Ctrl Pts',(0.00439219279408808,-0.0324744968375322,
0.0695590710472144));
#75130=CARTESIAN_POINT('Ctrl Pts',(0.00432965947859353,-0.0323646534831895,
0.0696113462561468));
#75131=CARTESIAN_POINT('Ctrl Pts',(0.00440896897686272,-0.0326943950436604,
0.0694382951314406));
#75132=CARTESIAN_POINT('Ctrl Pts',(0.00434403285309788,-0.0325844576448134,
0.0694894922198624));
#75133=CARTESIAN_POINT('Ctrl Pts',(0.00428015097343002,-0.0324744968375322,
0.0695420359170855));
#75134=CARTESIAN_POINT('Ctrl Pts',(0.00421740425847536,-0.0323646534831895,
0.0695958577721142));
#75135=CARTESIAN_POINT('',(0.00439891316645083,-0.0326773559991153,0.0694462407890779));
#75136=CARTESIAN_POINT('',(0.00440896897686215,-0.0326943950436594,0.069438295131441));
#75137=CARTESIAN_POINT('Origin',(0.0147469639985691,-0.0326395670261279,
0.0824328167942656));
#75138=CARTESIAN_POINT('Ctrl Pts',(0.00439891316852646,-0.0326773559987416,
0.0694462407917005));
#75139=CARTESIAN_POINT('Ctrl Pts',(0.00442557915302754,-0.0326267922586054,
0.0694799145582994));
#75140=CARTESIAN_POINT('Ctrl Pts',(0.00445177250220936,-0.0325756109579523,
0.0695129914817018));
#75141=CARTESIAN_POINT('Ctrl Pts',(0.00450323622179075,-0.0324719985462366,
0.0695779797922375));
#75142=CARTESIAN_POINT('Ctrl Pts',(0.00452848595148346,-0.0324196091621776,
0.0696098651143161));
#75143=CARTESIAN_POINT('Ctrl Pts',(0.00455327264734479,-0.0323666188837757,
0.0696411657179432));
#75144=CARTESIAN_POINT('',(0.00457524993226056,-0.0326943950436703,0.0694682874502759));
#75145=CARTESIAN_POINT('Origin',(0.00812378219310841,-0.0315241814719618,
0.07415));
#75146=CARTESIAN_POINT('',(0.00439891316647808,-0.032711433838006,0.0694462407891124));
#75147=CARTESIAN_POINT('',(0.0043888743489824,-0.0326943950436593,0.0694542079053788));
#75148=CARTESIAN_POINT('Origin',(0.0147820001238029,-0.0326395667286811,
0.0824040842777885));
#75149=CARTESIAN_POINT('Origin',(0.0146681926336194,-0.032639567897862,
0.0824951977524825));
#75150=CARTESIAN_POINT('Origin',(0.0146321924657103,-0.0326395677254717,
0.0825227126084884));
#75151=CARTESIAN_POINT('Ctrl Pts',(0.00468096466956283,-0.0332451089994433,
0.0695429258200494));
#75152=CARTESIAN_POINT('Ctrl Pts',(0.00450720602402564,-0.0329451141710254,
0.0696727738073743));
#75153=CARTESIAN_POINT('Ctrl Pts',(0.00434372168968992,-0.0326442513127493,
0.0698153411217842));
#75154=CARTESIAN_POINT('Ctrl Pts',(0.00448400425883616,-0.0332451089994433,
0.0696968952865237));
#75155=CARTESIAN_POINT('Ctrl Pts',(0.00431605266673542,-0.0329451141710254,
0.0698341717572756));
#75156=CARTESIAN_POINT('Ctrl Pts',(0.00415891843234981,-0.0326442513127493,
0.0699837090405706));
#75157=CARTESIAN_POINT('Ctrl Pts',(0.00448203465472889,-0.0332451089994433,
0.0696984349811885));
#75158=CARTESIAN_POINT('Ctrl Pts',(0.00431414113316252,-0.0329451141710254,
0.0698357857367745));
#75159=CARTESIAN_POINT('Ctrl Pts',(0.0041570703997764,-0.0326442513127493,
0.0699853927197585));
#75160=CARTESIAN_POINT('',(0.0044561210579841,-0.0331951640388616,0.0697198321930316));
#75161=CARTESIAN_POINT('',(0.00427720617082845,-0.0328677532354985,0.0698742570265934));
#75162=CARTESIAN_POINT('Origin',(0.0157269311170673,-0.0326402808279943,
0.0821295496793115));
#75163=CARTESIAN_POINT('Origin',(-0.0031174335433749,-0.0326944278779242,
0.0616551520620115));
#75164=CARTESIAN_POINT('',(0.00437104376775591,-0.0326943950436593,0.0697916655347617));
#75165=CARTESIAN_POINT('',(0.00432457927863608,-0.0326943950436693,0.0698334662674197));
#75166=CARTESIAN_POINT('',(0.00455327264731677,-0.0330220786163545,0.0696411657179031));
#75167=CARTESIAN_POINT('Origin',(0.0153912781259877,-0.0326396682765248,
0.0824737730299198));
#75168=CARTESIAN_POINT('',(0.00455411604157358,-0.0331951640388587,0.0696422307549535));
#75169=CARTESIAN_POINT('Origin',(-0.00229446032951578,-0.0331952026560113,
0.0609938568475875));
#75170=CARTESIAN_POINT('',(0.00450511854978884,-0.0331951640388701,0.0696810314740025));
#75171=CARTESIAN_POINT('Ctrl Pts',(0.00458614689441293,-0.0330240426238172,
0.069303853438716));
#75172=CARTESIAN_POINT('Ctrl Pts',(0.00451938650415942,-0.0329142774063519,
0.0693525878115066));
#75173=CARTESIAN_POINT('Ctrl Pts',(0.00445360030703494,-0.0328043479726691,
0.0694027266039119));
#75174=CARTESIAN_POINT('Ctrl Pts',(0.0043888743489824,-0.0326943950436593,
0.0694542079053788));
#75175=CARTESIAN_POINT('Ctrl Pts',(0.00457549577403047,-0.0330240426238172,
0.0694166705013398));
#75176=CARTESIAN_POINT('Ctrl Pts',(0.00451028954872694,-0.0329142774063519,
0.0694655516036906));
#75177=CARTESIAN_POINT('Ctrl Pts',(0.00444606132467023,-0.0328043479726691,
0.0695158050698752));
#75178=CARTESIAN_POINT('Ctrl Pts',(0.00438289515596947,-0.0326943950436593,
0.0695673687874687));
#75179=CARTESIAN_POINT('Ctrl Pts',(0.00456484465364802,-0.0330240426238172,
0.0695294875639636));
#75180=CARTESIAN_POINT('Ctrl Pts',(0.00450119259329447,-0.0329142774063519,
0.0695785153958745));
#75181=CARTESIAN_POINT('Ctrl Pts',(0.00443852234230552,-0.0328043479726691,
0.0696288835358384));
#75182=CARTESIAN_POINT('Ctrl Pts',(0.00437691596295654,-0.0326943950436593,
0.0696805296695587));
#75183=CARTESIAN_POINT('Ctrl Pts',(0.00455419353326556,-0.0330240426238172,
0.0696423046265874));
#75184=CARTESIAN_POINT('Ctrl Pts',(0.00449209563786199,-0.0329142774063519,
0.0696914791880584));
#75185=CARTESIAN_POINT('Ctrl Pts',(0.00443098335994081,-0.0328043479726691,
0.0697419620018017));
#75186=CARTESIAN_POINT('Ctrl Pts',(0.0043709367699436,-0.0326943950436593,
0.0697936905516486));
#75187=CARTESIAN_POINT('',(0.00437995905837915,-0.0326943950436693,0.0696229367200802));
#75188=CARTESIAN_POINT('Ctrl Pts',(0.00439891316853094,-0.0327114338383331,
0.069446240791706));
#75189=CARTESIAN_POINT('Ctrl Pts',(0.00442557471761049,-0.0327619876830991,
0.0694799089572611));
#75190=CARTESIAN_POINT('Ctrl Pts',(0.00445176590032874,-0.0328131562604373,
0.0695129831448564));
#75191=CARTESIAN_POINT('Ctrl Pts',(0.00450322957263624,-0.0329167375858768,
0.0695779713956947));
#75192=CARTESIAN_POINT('Ctrl Pts',(0.00452848155645018,-0.0329691088920615,
0.0696098595642743));
#75193=CARTESIAN_POINT('Ctrl Pts',(0.00455327264734411,-0.0330220786163186,
0.0696411657179421));
#75194=CARTESIAN_POINT('Ctrl Pts',(0.00445813557159303,-0.0331951640388604,
0.0697200661560827));
#75195=CARTESIAN_POINT('Ctrl Pts',(0.00436654952957937,-0.0330306422010619,
0.0697958510497885));
#75196=CARTESIAN_POINT('Ctrl Pts',(0.00427817401655101,-0.0328657861914645,
0.0698753565332643));
#75197=CARTESIAN_POINT('Ctrl Pts',(0.00445612105798658,-0.0331951640388604,
0.0697198321930296));
#75198=CARTESIAN_POINT('Ctrl Pts',(0.0043645301789368,-0.0330306422010619,
0.0697956587355127));
#75199=CARTESIAN_POINT('Ctrl Pts',(0.0042761515543933,-0.0328657861914645,
0.0698752060320969));
#75200=CARTESIAN_POINT('Ctrl Pts',(0.00412044891561131,-0.0331951640388604,
0.0696808476565142));
#75201=CARTESIAN_POINT('Ctrl Pts',(0.00402805205626363,-0.0330306422010619,
0.069763614005328));
#75202=CARTESIAN_POINT('Ctrl Pts',(0.00393915496962046,-0.0328657861914645,
0.0698501284902403));
#75203=CARTESIAN_POINT('',(0.00411091185962303,-0.0331781648281887,0.0696894090433693));
#75204=CARTESIAN_POINT('',(0.00412044891561044,-0.0331951640388588,0.069680847656515));
#75205=CARTESIAN_POINT('Origin',(0.015680470248199,-0.0326412091686146,
0.0814848236176645));
#75206=CARTESIAN_POINT('Ctrl Pts',(0.00411091186144395,-0.033178164828644,
0.0696894090431472));
#75207=CARTESIAN_POINT('Ctrl Pts',(0.00413965940689649,-0.033127681154678,
0.0697213639676716));
#75208=CARTESIAN_POINT('Ctrl Pts',(0.00416788788584545,-0.0330765663497789,
0.0697527418626016));
#75209=CARTESIAN_POINT('Ctrl Pts',(0.00422333084341036,-0.0329730614463125,
0.0698143706608437));
#75210=CARTESIAN_POINT('Ctrl Pts',(0.00425052292029112,-0.032920713337378,
0.0698445966710455));
#75211=CARTESIAN_POINT('Ctrl Pts',(0.00427720617539217,-0.0328677532289346,
0.0698742570107675));
#75212=CARTESIAN_POINT('',(0.00428828498680727,-0.0331951640388702,0.0697003399247833));
#75213=CARTESIAN_POINT('Origin',(0.00812378219310841,-0.0315241814719618,
0.07415));
#75214=CARTESIAN_POINT('',(0.00411091186017873,-0.0332121607144234,0.0696894090449544));
#75215=CARTESIAN_POINT('',(0.00410139311123134,-0.0331951640388587,0.0696979907823525));
#75216=CARTESIAN_POINT('Origin',(0.0157084293955862,-0.0326413649983711,
0.0814491230060563));
#75217=CARTESIAN_POINT('Origin',(0.0146214296216661,-0.0326412100335714,
0.0824375687480616));
#75218=CARTESIAN_POINT('Origin',(0.0145829785968182,-0.0326413660078431,
0.0824616066048647));
#75219=CARTESIAN_POINT('Ctrl Pts',(0.00439849357327689,-0.0337436976235975,
0.0697681796363892));
#75220=CARTESIAN_POINT('Ctrl Pts',(0.00435908281684353,-0.0336723290703325,
0.0698016854468189));
#75221=CARTESIAN_POINT('Ctrl Pts',(0.00432028110006349,-0.033601104548885,
0.0698358947120861));
#75222=CARTESIAN_POINT('Ctrl Pts',(0.00419639490457184,-0.0333736987606857,
0.0699451181196106));
#75223=CARTESIAN_POINT('Ctrl Pts',(0.00407898073262994,-0.0331450831799191,
0.0700612708398194));
#75224=CARTESIAN_POINT('Ctrl Pts',(0.00421158904034702,-0.0337436976235975,
0.0699342118488369));
#75225=CARTESIAN_POINT('Ctrl Pts',(0.00417367160279528,-0.0336723290703325,
0.069969398706962));
#75226=CARTESIAN_POINT('Ctrl Pts',(0.00413639320006255,-0.033601104548885,
0.0700052618878707));
#75227=CARTESIAN_POINT('Ctrl Pts',(0.00401737064457243,-0.0333736987606857,
0.0701197659204165));
#75228=CARTESIAN_POINT('Ctrl Pts',(0.00390511513044965,-0.0331450831799191,
0.0702409114598875));
#75229=CARTESIAN_POINT('Ctrl Pts',(0.00420971999501772,-0.0337436976235975,
0.0699358721709613));
#75230=CARTESIAN_POINT('Ctrl Pts',(0.0041718174906548,-0.0336723290703325,
0.0699710758395633));
#75231=CARTESIAN_POINT('Ctrl Pts',(0.00413455432106253,-0.033601104548885,
0.0700069555596285));
#75232=CARTESIAN_POINT('Ctrl Pts',(0.00401558040197243,-0.0333736987606857,
0.0701215123984247));
#75233=CARTESIAN_POINT('Ctrl Pts',(0.00390337647442785,-0.0331450831799191,
0.0702427078660882));
#75234=CARTESIAN_POINT('',(0.00418518581122499,-0.0336938721132548,0.0699588684653646));
#75235=CARTESIAN_POINT('',(0.00401632039107351,-0.0333679870047996,0.0701242227403068));
#75236=CARTESIAN_POINT('Ctrl Pts',(0.00418518581124073,-0.0336938721132494,
0.0699588684653497));
#75237=CARTESIAN_POINT('Ctrl Pts',(0.00416882585876012,-0.0336629187933839,
0.0699742426546625));
#75238=CARTESIAN_POINT('Ctrl Pts',(0.00415256116064488,-0.0336319952300977,
0.0699897077210402));
#75239=CARTESIAN_POINT('Ctrl Pts',(0.00413639320006895,-0.0336011045488887,
0.0700052618878647));
#75240=CARTESIAN_POINT('Ctrl Pts',(0.00409582225461918,-0.0335235892595388,
0.0700442926147639));
#75241=CARTESIAN_POINT('Ctrl Pts',(0.00405578845983254,-0.0334458668665506,
0.0700839538495439));
#75242=CARTESIAN_POINT('Ctrl Pts',(0.00401632039915872,-0.033367986996243,
0.0701242227316827));
#75243=CARTESIAN_POINT('Ctrl Pts',(0.00401628877738654,-0.033367969247041,
0.0701242540130376));
#75244=CARTESIAN_POINT('Ctrl Pts',(0.00401661659916247,-0.0333391895417412,
0.0701245670156927));
#75245=CARTESIAN_POINT('Ctrl Pts',(0.00401686455999755,-0.0333104081134104,
0.0701247992779087));
#75246=CARTESIAN_POINT('Ctrl Pts',(0.00401719656448682,-0.0332532698872406,
0.0701251026742335));
#75247=CARTESIAN_POINT('Ctrl Pts',(0.00401728300028147,-0.0332249174314659,
0.070125176161426));
#75248=CARTESIAN_POINT('Ctrl Pts',(0.00401729045242689,-0.033196098524122,
0.070125173801778));
#75249=CARTESIAN_POINT('Ctrl Pts',(0.00401729055187332,-0.0331956312684894,
0.0701251737428223));
#75250=CARTESIAN_POINT('Ctrl Pts',(0.00401729062974416,-0.0331951640388587,
0.0701251736633715));
#75251=CARTESIAN_POINT('',(0.00410478685445198,-0.0331951640388587,0.0700359021076475));
#75252=CARTESIAN_POINT('',(0.00406103874210729,-0.0331951640388687,0.0700805378855203));
#75253=CARTESIAN_POINT('',(0.00427720618565027,-0.0335216366567749,0.0698742570219735));
#75254=CARTESIAN_POINT('Origin',(0.0162866816396492,-0.0326434571525472,
0.081413024908701));
#75255=CARTESIAN_POINT('',(0.00427811478949624,-0.0336938721132326,0.0698752670000577));
#75256=CARTESIAN_POINT('Origin',(-0.00302568927549291,-0.0336938867896202,
0.0617565678363322));
#75257=CARTESIAN_POINT('',(0.00423165030037061,-0.0336938721132537,0.0699170677327212));
#75258=CARTESIAN_POINT('Ctrl Pts',(0.00428883481014811,-0.0335235895815172,
0.069535546774541));
#75259=CARTESIAN_POINT('Ctrl Pts',(0.00422530777647728,-0.0334144449262749,
0.069588342375584));
#75260=CARTESIAN_POINT('Ctrl Pts',(0.00416279847532571,-0.0333049234473147,
0.0696425110530825));
#75261=CARTESIAN_POINT('Ctrl Pts',(0.00410139311123132,-0.0331951640388587,
0.0696979907823524));
#75262=CARTESIAN_POINT('Ctrl Pts',(0.00428528856239471,-0.0335235895815172,
0.0696488101693902));
#75263=CARTESIAN_POINT('Ctrl Pts',(0.00422332082234909,-0.0334144449262749,
0.0697016545915155));
#75264=CARTESIAN_POINT('Ctrl Pts',(0.004162373614869,-0.0333049234473147,
0.0697558399323529));
#75265=CARTESIAN_POINT('Ctrl Pts',(0.00410253114898426,-0.0331951640388587,
0.0698113039649746));
#75266=CARTESIAN_POINT('Ctrl Pts',(0.00428174231464131,-0.0335235895815172,
0.0697620735642394));
#75267=CARTESIAN_POINT('Ctrl Pts',(0.00422133386822089,-0.0334144449262749,
0.069814966807447));
#75268=CARTESIAN_POINT('Ctrl Pts',(0.00416194875441229,-0.0333049234473147,
0.0698691688116234));
#75269=CARTESIAN_POINT('Ctrl Pts',(0.0041036691867372,-0.0331951640388587,
0.0699246171475968));
#75270=CARTESIAN_POINT('Ctrl Pts',(0.00427819606688791,-0.0335235895815172,
0.0698753369590886));
#75271=CARTESIAN_POINT('Ctrl Pts',(0.0042193469140927,-0.0334144449262749,
0.0699282790233785));
#75272=CARTESIAN_POINT('Ctrl Pts',(0.00416152389395558,-0.0333049234473147,
0.0699824976908938));
#75273=CARTESIAN_POINT('Ctrl Pts',(0.00410480722449014,-0.0331951640388587,
0.070037930330219));
#75274=CARTESIAN_POINT('',(0.00410308998285166,-0.0331951640388687,0.06986694644501));
#75275=CARTESIAN_POINT('Ctrl Pts',(0.00411091186226826,-0.0332121607145984,
0.0696894090472775));
#75276=CARTESIAN_POINT('Ctrl Pts',(0.00413961103802514,-0.033262544410982,
0.0697213102235373));
#75277=CARTESIAN_POINT('Ctrl Pts',(0.00416781568194698,-0.0333135300746948,
0.0697526616924685));
#75278=CARTESIAN_POINT('Ctrl Pts',(0.00422325829459368,-0.0334167203140651,
0.0698142901020552));
#75279=CARTESIAN_POINT('Ctrl Pts',(0.00425047478994511,-0.0334688847587358,
0.0698445431735279));
#75280=CARTESIAN_POINT('Ctrl Pts',(0.00427720618599561,-0.0335216366562442,
0.069874257022605));
#75281=CARTESIAN_POINT('Ctrl Pts',(0.00418721056670061,-0.0336938721132493,
0.0699589754493442));
#75282=CARTESIAN_POINT('Ctrl Pts',(0.00416267910927351,-0.0336474569765009,
0.0699820175093691));
#75283=CARTESIAN_POINT('Ctrl Pts',(0.00413841906916301,-0.033601104548885,
0.0700053451622198));
#75284=CARTESIAN_POINT('Ctrl Pts',(0.00407699822534293,-0.0334837508592656,
0.0700644054158677));
#75285=CARTESIAN_POINT('Ctrl Pts',(0.00401735443079853,-0.0333660264659097,
0.0701252597615537));
#75286=CARTESIAN_POINT('Ctrl Pts',(0.00418518581124541,-0.0336938721132493,
0.0699588684653455));
#75287=CARTESIAN_POINT('Ctrl Pts',(0.00416065372760546,-0.0336474569765009,
0.0699819223769358));
#75288=CARTESIAN_POINT('Ctrl Pts',(0.00413639320006256,-0.033601104548885,
0.0700052618878707));
#75289=CARTESIAN_POINT('Ctrl Pts',(0.00407497112217571,-0.0334837508592656,
0.0700643521634612));
#75290=CARTESIAN_POINT('Ctrl Pts',(0.00401532698371886,-0.0333660264659097,
0.0701252365544743));
#75291=CARTESIAN_POINT('Ctrl Pts',(0.00384570343603074,-0.0336938721132493,
0.0699409309006279));
#75292=CARTESIAN_POINT('Ctrl Pts',(0.00382106635787218,-0.0336474569765009,
0.0699659719152129));
#75293=CARTESIAN_POINT('Ctrl Pts',(0.00379672410455441,-0.033601104548885,
0.0699912996220781));
#75294=CARTESIAN_POINT('Ctrl Pts',(0.00373509511579557,-0.0334837508592656,
0.0700554235526489));
#75295=CARTESIAN_POINT('Ctrl Pts',(0.00367539331496028,-0.0333660264659097,
0.0701213455194301));
#75296=CARTESIAN_POINT('',(0.003838747518292,-0.0336769361243754,0.0699501812139545));
#75297=CARTESIAN_POINT('',(0.00384772818185602,-0.0336938721132328,0.0699410378841272));
#75298=CARTESIAN_POINT('Ctrl Pts',(0.00383874751829182,-0.033676936124375,
0.0699501812139546));
#75299=CARTESIAN_POINT('Ctrl Pts',(0.00384024277999362,-0.0336797586670049,
0.0699486556128355));
#75300=CARTESIAN_POINT('Ctrl Pts',(0.00384173879988311,-0.0336825812712892,
0.0699471308679525));
#75301=CARTESIAN_POINT('Ctrl Pts',(0.00384473235897705,-0.033688226609326,
0.0699440830869327));
#75302=CARTESIAN_POINT('Ctrl Pts',(0.00384622989819641,-0.033691049343075,
0.0699425600508077));
#75303=CARTESIAN_POINT('Ctrl Pts',(0.00384772818186329,-0.03369387211323,
0.0699410378841292));
#75304=CARTESIAN_POINT('Ctrl Pts',(0.003838747518292,-0.0336769361243754,
0.0699501812139545));
#75305=CARTESIAN_POINT('Ctrl Pts',(0.00386867971389577,-0.0336279031321641,
0.0699795181521461));
#75306=CARTESIAN_POINT('Ctrl Pts',(0.00389904255917442,-0.0335767851940115,
0.0700092771757418));
#75307=CARTESIAN_POINT('Ctrl Pts',(0.00395853781724498,-0.0334733198899499,
0.0700675892598876));
#75308=CARTESIAN_POINT('Ctrl Pts',(0.00398771017746988,-0.0334209645035421,
0.0700961814734416));
#75309=CARTESIAN_POINT('Ctrl Pts',(0.00401632040136205,-0.0333679869844681,
0.0701242227297893));
#75310=CARTESIAN_POINT('',(0.0040164569965505,-0.0336938721132538,0.0699499531747559));
#75311=CARTESIAN_POINT('Origin',(0.00812378219310841,-0.0315241814719618,
0.07415));
#75312=CARTESIAN_POINT('',(0.00383874751922387,-0.0337108120655845,0.0699501812148682));
#75313=CARTESIAN_POINT('',(0.00382978640553166,-0.0336938721132327,0.0699593437057788));
#75314=CARTESIAN_POINT('Origin',(0.0147411860276537,-0.0345562514810309,
0.0822006996781526));
#75315=CARTESIAN_POINT('Ctrl Pts',(0.00382978640553377,-0.0336938721132299,
0.0699593437057861));
#75316=CARTESIAN_POINT('Ctrl Pts',(0.00383127817504152,-0.0336910493388199,
0.0699578151499866));
#75317=CARTESIAN_POINT('Ctrl Pts',(0.00383277082540093,-0.0336882266071981,
0.0699562873244816));
#75318=CARTESIAN_POINT('Ctrl Pts',(0.00383575786619216,-0.033682581271266,
0.0699532331570176));
#75319=CARTESIAN_POINT('Ctrl Pts',(0.00383725225659651,-0.0336797586669932,
0.0699517068150672));
#75320=CARTESIAN_POINT('Ctrl Pts',(0.00383874751829216,-0.0336769361243751,
0.0699501812139543));
#75321=CARTESIAN_POINT('Origin',(0.0163057639141442,-0.0345562517080938,
0.0806043721342636));
#75322=CARTESIAN_POINT('Ctrl Pts',(0.00413074496612322,-0.034243627687391,
0.0700107031147898));
#75323=CARTESIAN_POINT('Ctrl Pts',(0.00397462881049004,-0.0339430054201809,
0.0701613029964762));
#75324=CARTESIAN_POINT('Ctrl Pts',(0.00383029996464101,-0.0336441434784052,
0.0703232343481949));
#75325=CARTESIAN_POINT('Ctrl Pts',(0.00395463290236064,-0.034243627687391,
0.0701881419521319));
#75326=CARTESIAN_POINT('Ctrl Pts',(0.00380520896280041,-0.0339430054201809,
0.0703453840098006));
#75327=CARTESIAN_POINT('Ctrl Pts',(0.0036680536370505,-0.0336441434784052,
0.0705134345826412));
#75328=CARTESIAN_POINT('Ctrl Pts',(0.00395287178172302,-0.034243627687391,
0.0701899163405053));
#75329=CARTESIAN_POINT('Ctrl Pts',(0.00380351476432351,-0.0339430054201809,
0.0703472248199339));
#75330=CARTESIAN_POINT('Ctrl Pts',(0.00366643117377459,-0.0336441434784052,
0.0705153365849856));
#75331=CARTESIAN_POINT('',(0.00392979440503335,-0.0341934961088741,0.0702144452190983));
#75332=CARTESIAN_POINT('',(0.00377164489123366,-0.0338664212864733,0.070390076342541));
#75333=CARTESIAN_POINT('Origin',(0.0157787116534421,-0.0345610720404402,
0.0820320720457151));
#75334=CARTESIAN_POINT('Origin',(-0.0045267054850951,-0.0336938005073093,
0.0632209686267812));
#75335=CARTESIAN_POINT('',(0.00385439107964538,-0.0336938721132327,0.070296375145362));
#75336=CARTESIAN_POINT('',(0.00381353199788871,-0.0336938721132427,0.0703436698114264));
#75337=CARTESIAN_POINT('',(0.00401632040136582,-0.0340203938281605,0.0701242227297855));
#75338=CARTESIAN_POINT('Origin',(0.015390453490231,-0.0345589643244941,
0.0823163119673952));
#75339=CARTESIAN_POINT('',(0.00401729062974263,-0.0341934961088739,0.070125173663373));
#75340=CARTESIAN_POINT('Origin',(-0.0038524944108664,-0.0341934220717632,
0.0624118928000223));
#75341=CARTESIAN_POINT('',(0.003973542517398,-0.034193496108884,0.0701698094412456));
#75342=CARTESIAN_POINT('Ctrl Pts',(0.00400666027782073,-0.0340223579322397,
0.0697854488048955));
#75343=CARTESIAN_POINT('Ctrl Pts',(0.00394646173361285,-0.0339125849573575,
0.0698422346540121));
#75344=CARTESIAN_POINT('Ctrl Pts',(0.00388748082534962,-0.0338030433565231,
0.069900226570353));
#75345=CARTESIAN_POINT('Ctrl Pts',(0.00382978640553159,-0.0336938721132327,
0.0699593437057781));
#75346=CARTESIAN_POINT('Ctrl Pts',(0.00401023284455326,-0.0340223579322397,
0.0698987114050655));
#75347=CARTESIAN_POINT('Ctrl Pts',(0.00395159648700299,-0.0339125849573575,
0.0699554479791692));
#75348=CARTESIAN_POINT('Ctrl Pts',(0.00389417564778862,-0.0338030433565231,
0.0700133583214883));
#75349=CARTESIAN_POINT('Ctrl Pts',(0.00383803719359283,-0.0336938721132327,
0.0700723618650565));
#75350=CARTESIAN_POINT('Ctrl Pts',(0.00401380541128579,-0.0340223579322397,
0.0700119740052354));
#75351=CARTESIAN_POINT('Ctrl Pts',(0.00395673124039312,-0.0339125849573575,
0.0700686613043262));
#75352=CARTESIAN_POINT('Ctrl Pts',(0.00390087047022762,-0.0338030433565231,
0.0701264900726237));
#75353=CARTESIAN_POINT('Ctrl Pts',(0.00384628798165408,-0.0336938721132327,
0.0701853800243348));
#75354=CARTESIAN_POINT('Ctrl Pts',(0.00401737797801833,-0.0340223579322397,
0.0701252366054053));
#75355=CARTESIAN_POINT('Ctrl Pts',(0.00396186599378326,-0.0339125849573575,
0.0701818746294833));
#75356=CARTESIAN_POINT('Ctrl Pts',(0.00390756529266662,-0.0338030433565231,
0.070239621823759));
#75357=CARTESIAN_POINT('Ctrl Pts',(0.00385453876971533,-0.0336938721132327,
0.0702983981836132));
#75358=CARTESIAN_POINT('',(0.00384208874259852,-0.0336938721132427,0.0701278594255804));
#75359=CARTESIAN_POINT('Ctrl Pts',(0.00383874752179171,-0.0337108120662692,
0.0699501812173845));
#75360=CARTESIAN_POINT('Ctrl Pts',(0.0038694564057343,-0.0337611408994321,
0.069980279398022));
#75361=CARTESIAN_POINT('Ctrl Pts',(0.00389960492067525,-0.0338121088781361,
0.0700098283536383));
#75362=CARTESIAN_POINT('Ctrl Pts',(0.00395880867736566,-0.0339153382773237,
0.0700678547334513));
#75363=CARTESIAN_POINT('Ctrl Pts',(0.0039878388723051,-0.0339675558473117,
0.0700963076089405));
#75364=CARTESIAN_POINT('Ctrl Pts',(0.0040163204013906,-0.0340203938281304,
0.0701242227298172));
#75365=CARTESIAN_POINT('Ctrl Pts',(0.00393182245015566,-0.0341934961088741,
0.0702144248508423));
#75366=CARTESIAN_POINT('Ctrl Pts',(0.00385045753443956,-0.0340287516182428,
0.0703010903160523));
#75367=CARTESIAN_POINT('Ctrl Pts',(0.00377274409291432,-0.0338644633275951,
0.0703910446009745));
#75368=CARTESIAN_POINT('Ctrl Pts',(0.00392979440503345,-0.0341934961088741,
0.0702144452190984));
#75369=CARTESIAN_POINT('Ctrl Pts',(0.003848429910415,-0.0340287516182428,
0.0703011526125435));
#75370=CARTESIAN_POINT('Ctrl Pts',(0.00377071862255335,-0.0338644633275951,
0.0703911487724697));
#75371=CARTESIAN_POINT('Ctrl Pts',(0.00359188307974076,-0.0341934961088741,
0.0702178389623189));
#75372=CARTESIAN_POINT('Ctrl Pts',(0.00351058874808976,-0.0340287516182428,
0.0703115324062039));
#75373=CARTESIAN_POINT('Ctrl Pts',(0.00343323630200735,-0.0338644633275951,
0.0704085057472349));
#75374=CARTESIAN_POINT('',(0.00358349425304188,-0.0341764758832377,0.0702275281502832));
#75375=CARTESIAN_POINT('',(0.00359188307974075,-0.034193496108874,0.0702178389623189));
#75376=CARTESIAN_POINT('Origin',(0.0157782040706306,-0.0345621026475542,
0.0814395923005888));
#75377=CARTESIAN_POINT('Ctrl Pts',(0.00358349425473896,-0.0341764758837459,
0.0702275281496326));
#75378=CARTESIAN_POINT('Ctrl Pts',(0.00361597576944247,-0.0341260050040449,
0.0702555897497597));
#75379=CARTESIAN_POINT('Ctrl Pts',(0.00364789270377078,-0.0340749269148221,
0.070283163544164));
#75380=CARTESIAN_POINT('Ctrl Pts',(0.00371062202772195,-0.0339715436306273,
0.0703373570303035));
#75381=CARTESIAN_POINT('Ctrl Pts',(0.00374141061532904,-0.0339192778237161,
0.0703639561667697));
#75382=CARTESIAN_POINT('Ctrl Pts',(0.00377164489147254,-0.0338664212855619,
0.0703900763404203));
#75383=CARTESIAN_POINT('',(0.00376083874239706,-0.0341934961088841,0.0702161420907186));
#75384=CARTESIAN_POINT('Origin',(0.00812378219310841,-0.0315241814719618,
0.07415));
#75385=CARTESIAN_POINT('',(0.0035834942530485,-0.0342105180190376,0.0702275281514014));
#75386=CARTESIAN_POINT('',(0.00357512613946545,-0.0341934961088739,0.0702372352350696));
#75387=CARTESIAN_POINT('Origin',(0.0158115988130717,-0.0345621706866152,
0.0814089435689751));
#75388=CARTESIAN_POINT('Origin',(0.0164477712777528,-0.0345621037838267,
0.0806645670300262));
#75389=CARTESIAN_POINT('Origin',(0.0164222936593224,-0.034562171692472,
0.0807020557971328));
#75390=CARTESIAN_POINT('Ctrl Pts',(0.00385537170408677,-0.0346945769586966,
0.0702952400658775));
#75391=CARTESIAN_POINT('Ctrl Pts',(0.00377463221390489,-0.0345275153362944,
0.0703846436325484));
#75392=CARTESIAN_POINT('Ctrl Pts',(0.00369668350023679,-0.0343603235965185,
0.0704766095062116));
#75393=CARTESIAN_POINT('Ctrl Pts',(0.00362175205823326,-0.0341934961088739,
0.070570862266246));
#75394=CARTESIAN_POINT('Ctrl Pts',(0.00380056605345085,-0.0346945769586966,
0.070358677980599));
#75395=CARTESIAN_POINT('Ctrl Pts',(0.00372115529579197,-0.0345275153362944,
0.0704492294735654));
#75396=CARTESIAN_POINT('Ctrl Pts',(0.00364457175955056,-0.0343603235965185,
0.0705423017830219));
#75397=CARTESIAN_POINT('Ctrl Pts',(0.00357103785365299,-0.0341934961088739,
0.0706376162760104));
#75398=CARTESIAN_POINT('Ctrl Pts',(0.00374576040281499,-0.0346945769586966,
0.0704221158953208));
#75399=CARTESIAN_POINT('Ctrl Pts',(0.00366767837767903,-0.0345275153362944,
0.0705138153145834));
#75400=CARTESIAN_POINT('Ctrl Pts',(0.00359246001886427,-0.0343603235965185,
0.0706079940598334));
#75401=CARTESIAN_POINT('Ctrl Pts',(0.00352032364907269,-0.0341934961088739,
0.0707043702857762));
#75402=CARTESIAN_POINT('Ctrl Pts',(0.00369095475217901,-0.0346945769586966,
0.0704855538100419));
#75403=CARTESIAN_POINT('Ctrl Pts',(0.00361420145956612,-0.0345275153362944,
0.0705784011555995));
#75404=CARTESIAN_POINT('Ctrl Pts',(0.00354034827817808,-0.0343603235965185,
0.0706736863366425));
#75405=CARTESIAN_POINT('Ctrl Pts',(0.00346960944449247,-0.0341934961088739,
0.0707711242955393));
#75406=CARTESIAN_POINT('',(0.0036909547525752,-0.0346945769586966,0.0704855538095837));
#75407=CARTESIAN_POINT('',(0.00354414528140131,-0.0343667727831428,0.070670768654258));
#75408=CARTESIAN_POINT('Origin',(0.016765754229002,-0.0345626457063744,
0.0810565928262449));
#75409=CARTESIAN_POINT('Origin',(-0.00525638033940051,-0.034193477102889,
0.0639848578490789));
#75410=CARTESIAN_POINT('',(0.00362084464106437,-0.034193496108874,0.0705720566798239));
#75411=CARTESIAN_POINT('',(0.00358303584202472,-0.0341934961088839,0.0706218235836399));
#75412=CARTESIAN_POINT('',(0.00377164489265938,-0.0345211942962721,0.0703900763414942));
#75413=CARTESIAN_POINT('Origin',(0.0164489103351654,-0.0345625596120514,
0.08141825667154));
#75414=CARTESIAN_POINT('',(0.00377267291611208,-0.0346945769586885,0.0703909644774707));
#75415=CARTESIAN_POINT('Origin',(-0.00459928980844164,-0.0346945685853842,
0.0631582087556491));
#75416=CARTESIAN_POINT('',(0.00373181383435364,-0.0346945769587026,0.0704382591435372));
#75417=CARTESIAN_POINT('Ctrl Pts',(0.00374073138332709,-0.0345231616327842,
0.0700525781765969));
#75418=CARTESIAN_POINT('Ctrl Pts',(0.00368425419219998,-0.0344132092796988,
0.0701129923611679));
#75419=CARTESIAN_POINT('Ctrl Pts',(0.00362902953479011,-0.0343032738558979,
0.0701745716147944));
#75420=CARTESIAN_POINT('Ctrl Pts',(0.00357512613946539,-0.0341934961088739,
0.0702372352350696));
#75421=CARTESIAN_POINT('Ctrl Pts',(0.0037514087178497,-0.0345231616327842,
0.0701653927619394));
#75422=CARTESIAN_POINT('Ctrl Pts',(0.0036964865169513,-0.0344132092796988,
0.0702256597744864));
#75423=CARTESIAN_POINT('Ctrl Pts',(0.00364281372540257,-0.0343032738558979,
0.0702870596999361));
#75424=CARTESIAN_POINT('Ctrl Pts',(0.00359045708933678,-0.0341934961088739,
0.070349512116548));
#75425=CARTESIAN_POINT('Ctrl Pts',(0.00376208605237231,-0.0345231616327842,
0.0702782073472817));
#75426=CARTESIAN_POINT('Ctrl Pts',(0.00370871884170262,-0.0344132092796988,
0.0703383271878048));
#75427=CARTESIAN_POINT('Ctrl Pts',(0.00365659791601503,-0.0343032738558979,
0.0703995477850777));
#75428=CARTESIAN_POINT('Ctrl Pts',(0.00360578803920817,-0.0341934961088739,
0.0704617889980265));
#75429=CARTESIAN_POINT('Ctrl Pts',(0.00377276338689492,-0.0345231616327842,
0.0703910219326241));
#75430=CARTESIAN_POINT('Ctrl Pts',(0.00372095116645394,-0.0344132092796988,
0.0704509946011233));
#75431=CARTESIAN_POINT('Ctrl Pts',(0.00367038210662749,-0.0343032738558979,
0.0705120358702194));
#75432=CARTESIAN_POINT('Ctrl Pts',(0.00362111898907955,-0.0341934961088739,
0.0705740658795049));
#75433=CARTESIAN_POINT('',(0.00359798539027491,-0.0341934961088839,0.0704046459574568));
#75434=CARTESIAN_POINT('Ctrl Pts',(0.00358349425565724,-0.0342105180195395,
0.0702275281536545));
#75435=CARTESIAN_POINT('Ctrl Pts',(0.00361601227690777,-0.0342610556241267,
0.0702556213108751));
#75436=CARTESIAN_POINT('Ctrl Pts',(0.00364794677908014,-0.0343122189870072,
0.0702832103509149));
#75437=CARTESIAN_POINT('Ctrl Pts',(0.00371067673843757,-0.0344158119695202,
0.070337404380653));
#75438=CARTESIAN_POINT('Ctrl Pts',(0.00374144653860155,-0.0344681990450108,
0.0703639872045892));
#75439=CARTESIAN_POINT('Ctrl Pts',(0.00377164489267596,-0.0345211942962546,
0.0703900763415107));
#75440=CARTESIAN_POINT('Ctrl Pts',(0.00369297702161709,-0.0346945769586932,
0.0704854061756626));
#75441=CARTESIAN_POINT('Ctrl Pts',(0.00361721413728232,-0.034529677707698,
0.0705770099374461));
#75442=CARTESIAN_POINT('Ctrl Pts',(0.00354530205903659,-0.0343648066251421,
0.0706716667745894));
#75443=CARTESIAN_POINT('Ctrl Pts',(0.00369095475258102,-0.0346945769586932,
0.0704855538095767));
#75444=CARTESIAN_POINT('Ctrl Pts',(0.00361519492047297,-0.034529677707698,
0.0705771993803416));
#75445=CARTESIAN_POINT('Ctrl Pts',(0.00354328761984949,-0.0343648066251421,
0.0706718978645897));
#75446=CARTESIAN_POINT('Ctrl Pts',(0.00335392331300024,-0.0346945769586932,
0.0705101584836901));
#75447=CARTESIAN_POINT('Ctrl Pts',(0.00327867216511978,-0.034529677707698,
0.0706087719409925));
#75448=CARTESIAN_POINT('Ctrl Pts',(0.00320756110321309,-0.0343648066251421,
0.0707104113334196));
#75449=CARTESIAN_POINT('',(0.00334615942863117,-0.0346775396664963,0.0705203552909863));
#75450=CARTESIAN_POINT('',(0.00335392331299816,-0.0346945769586886,0.0705101584836928));
#75451=CARTESIAN_POINT('Origin',(0.016657343190845,-0.0345626618351403,
0.0804413072159766));
#75452=CARTESIAN_POINT('Ctrl Pts',(0.00334615943032344,-0.0346775396670097,
0.0705203552903225));
#75453=CARTESIAN_POINT('Ctrl Pts',(0.00338036577141767,-0.0346269749928192,
0.0705463424378536));
#75454=CARTESIAN_POINT('Ctrl Pts',(0.00341396421123299,-0.0345757902890796,
0.070571867707184));
#75455=CARTESIAN_POINT('Ctrl Pts',(0.00347997285435171,-0.0344721681087691,
0.0706220156482585));
#75456=CARTESIAN_POINT('Ctrl Pts',(0.00351235717575486,-0.0344197714289052,
0.0706466186641413));
#75457=CARTESIAN_POINT('Ctrl Pts',(0.00354414528145819,-0.034366772783058,
0.0706707686539969));
#75458=CARTESIAN_POINT('',(0.00352243903279668,-0.0346945769587026,0.0704978561466482));
#75459=CARTESIAN_POINT('Origin',(0.00812378219310841,-0.0315241814719618,
0.07415));
#75460=CARTESIAN_POINT('',(0.00334615942912236,-0.034711613648962,0.0705203552922876));
#75461=CARTESIAN_POINT('',(0.00333841734075968,-0.0346945769586885,0.0705305686593154));
#75462=CARTESIAN_POINT('Origin',(0.0166832442648657,-0.0345626685577737,
0.0804041264557915));
#75463=CARTESIAN_POINT('Origin',(0.0164725764164216,-0.0345626627644068,
0.0806845157712007));
#75464=CARTESIAN_POINT('Origin',(0.0164436967321114,-0.0345626695232125,
0.0807194335678264));
#75465=CARTESIAN_POINT('Ctrl Pts',(0.00364493063813646,-0.0352450361874068,
0.0705418631713652));
#75466=CARTESIAN_POINT('Ctrl Pts',(0.00350884752462439,-0.0349452760959492,
0.070710785829653));
#75467=CARTESIAN_POINT('Ctrl Pts',(0.00338587495471023,-0.034644428984174,
0.0708894789333667));
#75468=CARTESIAN_POINT('Ctrl Pts',(0.00364339057316616,-0.0352450361874068,
0.0705438641273586));
#75469=CARTESIAN_POINT('Ctrl Pts',(0.00350738292694774,-0.0349452760959492,
0.0707128448701498));
#75470=CARTESIAN_POINT('Ctrl Pts',(0.00338448998509506,-0.034644428984174,
0.0708915902088497));
#75471=CARTESIAN_POINT('Ctrl Pts',(0.00349090889293795,-0.0352450361874068,
0.0707419785821436));
#75472=CARTESIAN_POINT('Ctrl Pts',(0.00336237325599172,-0.0349452760959492,
0.0709167102658732));
#75473=CARTESIAN_POINT('Ctrl Pts',(0.00324736428062184,-0.034644428984174,
0.0711006273853824));
#75474=CARTESIAN_POINT('Ctrl Pts',(0.00348938407613567,-0.0352450361874068,
0.0707439597266914));
#75475=CARTESIAN_POINT('Ctrl Pts',(0.00336092315928216,-0.0349452760959492,
0.0709187489198304));
#75476=CARTESIAN_POINT('Ctrl Pts',(0.00324599302357711,-0.034644428984174,
0.0711027177571476));
#75477=CARTESIAN_POINT('',(0.00346962653462896,-0.0351951634053271,0.0707710967150308));
#75478=CARTESIAN_POINT('',(0.00333471940509753,-0.0348678972925434,0.0709651919033495));
#75479=CARTESIAN_POINT('Origin',(0.017515054857925,-0.0345636767888727,
0.0798886862858971));
#75480=CARTESIAN_POINT('Origin',(-0.00586630416223851,-0.0346946199341124,
0.0648463558596404));
#75481=CARTESIAN_POINT('',(0.0034050692502411,-0.0346945769330288,0.0708618587073022));
#75482=CARTESIAN_POINT('',(0.00337045994285098,-0.0346945769458128,0.070913901448675));
#75483=CARTESIAN_POINT('',(0.00354414528155627,-0.0350221583435276,0.0706707686540918));
#75484=CARTESIAN_POINT('Origin',(0.0172843629381708,-0.0345628458716402,
0.0803104974173432));
#75485=CARTESIAN_POINT('',(0.00354513200593994,-0.035195136029876,0.0706715144876764));
#75486=CARTESIAN_POINT('Origin',(-0.00522895466634155,-0.0351951838366816,
0.0640056876872522));
#75487=CARTESIAN_POINT('',(0.00346960944477295,-0.035195137132875,0.070771124294978));
#75488=CARTESIAN_POINT('Ctrl Pts',(0.00349210047715177,-0.0350241211494343,
0.0703358782816882));
#75489=CARTESIAN_POINT('Ctrl Pts',(0.00343956251433281,-0.0349144232818962,
0.070399677798262));
#75490=CARTESIAN_POINT('Ctrl Pts',(0.00338831188660698,-0.0348045283579412,
0.0704646014991549));
#75491=CARTESIAN_POINT('Ctrl Pts',(0.00333841733405596,-0.0346945769439157,
0.0705305686681786));
#75492=CARTESIAN_POINT('Ctrl Pts',(0.00350984045065131,-0.0350241211494343,
0.0704477998396794));
#75493=CARTESIAN_POINT('Ctrl Pts',(0.00345884416140406,-0.0349144232818962,
0.0705113549953919));
#75494=CARTESIAN_POINT('Ctrl Pts',(0.00340913107890226,-0.0348045283579412,
0.0705760023216674));
#75495=CARTESIAN_POINT('Ctrl Pts',(0.00336076796065435,-0.0346945769439157,
0.0706416613830324));
#75496=CARTESIAN_POINT('Ctrl Pts',(0.00352758042415085,-0.0350241211494343,
0.0705597213976706));
#75497=CARTESIAN_POINT('Ctrl Pts',(0.0034781258084753,-0.0349144232818962,
0.0706230321925219));
#75498=CARTESIAN_POINT('Ctrl Pts',(0.00342995027119753,-0.0348045283579412,
0.0706874031441799));
#75499=CARTESIAN_POINT('Ctrl Pts',(0.00338311858725274,-0.0346945769439157,
0.0707527540978863));
#75500=CARTESIAN_POINT('Ctrl Pts',(0.00354532039765039,-0.0350241211494343,
0.0706716429556618));
#75501=CARTESIAN_POINT('Ctrl Pts',(0.00349740745554654,-0.0349144232818962,
0.0707347093896518));
#75502=CARTESIAN_POINT('Ctrl Pts',(0.00345076946349281,-0.0348045283579412,
0.0707988039666924));
#75503=CARTESIAN_POINT('Ctrl Pts',(0.00340546921385113,-0.0346945769439157,
0.0708638468127401));
#75504=CARTESIAN_POINT('',(0.0033717432956044,-0.0346945769458128,0.0706962136830263));
#75505=CARTESIAN_POINT('Ctrl Pts',(0.00334615943173523,-0.0347116136492799,
0.0705203552942714));
#75506=CARTESIAN_POINT('Ctrl Pts',(0.00338035218094575,-0.0347621546532253,
0.0705463321319886));
#75507=CARTESIAN_POINT('Ctrl Pts',(0.00341394372922662,-0.0348133084096931,
0.0705718522267019));
#75508=CARTESIAN_POINT('Ctrl Pts',(0.00347995245837948,-0.0349168561544571,
0.0706220002283899));
#75509=CARTESIAN_POINT('Ctrl Pts',(0.00351234345693012,-0.0349692089015923,
0.0706466082441908));
#75510=CARTESIAN_POINT('Ctrl Pts',(0.00354414528157333,-0.0350221583435,
0.0706707686541298));
#75511=CARTESIAN_POINT('Ctrl Pts',(0.00347105901116135,-0.0351951371254883,
0.0707709263626847));
#75512=CARTESIAN_POINT('Ctrl Pts',(0.00340119878381317,-0.0350307338980928,
0.0708671184952531));
#75513=CARTESIAN_POINT('Ctrl Pts',(0.00333537397625194,-0.034865930689783,
0.0709661158307866));
#75514=CARTESIAN_POINT('Ctrl Pts',(0.0034696094448677,-0.0351951371254883,
0.0707711242950452));
#75515=CARTESIAN_POINT('Ctrl Pts',(0.00339975330964688,-0.0350307338980928,
0.0708673463964872));
#75516=CARTESIAN_POINT('Ctrl Pts',(0.0033339338293622,-0.034865930689783,
0.0709663735061541));
#75517=CARTESIAN_POINT('Ctrl Pts',(0.00322666062325334,-0.0351951371254883,
0.0708042979649621));
#75518=CARTESIAN_POINT('Ctrl Pts',(0.00315749033284418,-0.0350307338980928,
0.0709055428808597));
#75519=CARTESIAN_POINT('Ctrl Pts',(0.003092563709662,-0.034865930689783,
0.0710095601663106));
#75520=CARTESIAN_POINT('Origin',(-0.0010936440991894,-0.0308609197384602,
0.068020254962796));
#75521=CARTESIAN_POINT('',(0.00336368923641043,-0.0351951371254883,0.0707855872671623));
#75522=CARTESIAN_POINT('Origin',(0.00900721682260279,-0.0351840467441148,
0.0745674792273879));
#75523=CARTESIAN_POINT('Origin',(-0.00225761982641391,-0.0352322614444702,
0.0682005758416904));
#75524=CARTESIAN_POINT('',(0.00320777621092359,-0.0351951142564653,0.0711649204756739));
#75525=CARTESIAN_POINT('',(0.00314536997854559,-0.0351951372916787,0.071272863954921));
#75526=CARTESIAN_POINT('Origin',(0.00813327152284308,-0.0352875127175844,
0.0744904946253621));
#75527=CARTESIAN_POINT('Origin',(0.01305241611569,-0.0298325076522079,0.0684928136022584));
#75528=CARTESIAN_POINT('Origin',(0.00297934781069869,-0.0338732790727179,
0.067533109811178));
#75529=CARTESIAN_POINT('Ctrl Pts',(0.00590155454277438,-0.0321934096636941,
0.0688453001955434));
#75530=CARTESIAN_POINT('Ctrl Pts',(0.00580660294236103,-0.0320508460843585,
0.0688850770122644));
#75531=CARTESIAN_POINT('Ctrl Pts',(0.00571279166034753,-0.0319086045661596,
0.068927374999284));
#75532=CARTESIAN_POINT('Ctrl Pts',(0.00562031519106785,-0.0317669892865695,
0.0689720864523457));
#75533=CARTESIAN_POINT('Ctrl Pts',(0.00582494125586505,-0.0321934096636941,
0.0688793712521285));
#75534=CARTESIAN_POINT('Ctrl Pts',(0.00573059951114002,-0.0320508460843585,
0.0689205194102022));
#75535=CARTESIAN_POINT('Ctrl Pts',(0.00563743447021791,-0.0319086045661596,
0.0689641713189593));
#75536=CARTESIAN_POINT('Ctrl Pts',(0.00554563899596201,-0.0317669892865695,
0.0690102164734667));
#75537=CARTESIAN_POINT('Ctrl Pts',(0.00574832796895574,-0.0321934096636941,
0.0689134423087136));
#75538=CARTESIAN_POINT('Ctrl Pts',(0.00565459607991902,-0.0320508460843585,
0.0689559618081398));
#75539=CARTESIAN_POINT('Ctrl Pts',(0.00556207728008829,-0.0319086045661596,
0.0690009676386347));
#75540=CARTESIAN_POINT('Ctrl Pts',(0.00547096280085618,-0.0317669892865695,
0.0690483464945876));
#75541=CARTESIAN_POINT('Ctrl Pts',(0.00567171468204641,-0.0321934096636941,
0.0689475133652987));
#75542=CARTESIAN_POINT('Ctrl Pts',(0.00557859264869801,-0.0320508460843585,
0.0689914042060775));
#75543=CARTESIAN_POINT('Ctrl Pts',(0.00548672008995868,-0.0319086045661596,
0.0690377639583101));
#75544=CARTESIAN_POINT('Ctrl Pts',(0.00539628660575034,-0.0317669892865695,
0.0690864765157086));
#75545=CARTESIAN_POINT('',(0.00567308530888974,-0.0321934096636941,0.0689469038273657));
#75546=CARTESIAN_POINT('',(0.00546138748314337,-0.0318665617511259,0.069051982797464));
#75547=CARTESIAN_POINT('Origin',(0.0122321207203587,-0.0326371944422025,
0.0843156044656728));
#75548=CARTESIAN_POINT('Origin',(0.000387281604560991,-0.0316939261509096,
0.0593359630523767));
#75549=CARTESIAN_POINT('',(0.00578652580579316,-0.0320197221621852,0.0688950193390954));
#75550=CARTESIAN_POINT('Ctrl Pts',(0.00578634321248903,-0.0320197392094773,
0.0688950489121256));
#75551=CARTESIAN_POINT('Ctrl Pts',(0.00575960435100756,-0.031979271657607,
0.0689069425960148));
#75552=CARTESIAN_POINT('Ctrl Pts',(0.00573283443670875,-0.0319386439829719,
0.0689190942707985));
#75553=CARTESIAN_POINT('Ctrl Pts',(0.00570600886206676,-0.031897909938165,
0.0689315243946623));
#75554=CARTESIAN_POINT('Ctrl Pts',(0.00567918381765027,-0.0318571766984939,
0.0689439542728364));
#75555=CARTESIAN_POINT('Ctrl Pts',(0.00565243870842038,-0.0318163871833576,
0.0689565977957526));
#75556=CARTESIAN_POINT('Ctrl Pts',(0.00562586402162872,-0.0317755399638302,
0.0689694082915398));
#75557=CARTESIAN_POINT('',(0.0057873002927968,-0.0321934096636183,0.068896110742553));
#75558=CARTESIAN_POINT('Origin',(0.00482998040805077,-0.032411314875615,
0.0667952183655116));
#75559=CARTESIAN_POINT('',(0.00573019280085328,-0.0321934096636663,0.0689215072849694));
#75560=CARTESIAN_POINT('Ctrl Pts',(0.0056749785059328,-0.0321934096636618,
0.0689476314896054));
#75561=CARTESIAN_POINT('Ctrl Pts',(0.00560323378968558,-0.0320835708272592,
0.0689814024009375));
#75562=CARTESIAN_POINT('Ctrl Pts',(0.00553222957554433,-0.0319739230346488,
0.0690166384769426));
#75563=CARTESIAN_POINT('Ctrl Pts',(0.00546205324854853,-0.0318646057455572,
0.0690532876634087));
#75564=CARTESIAN_POINT('Ctrl Pts',(0.00556920366535213,-0.0321934096636618,
0.0689069762579045));
#75565=CARTESIAN_POINT('Ctrl Pts',(0.00549689828177492,-0.0320835708272592,
0.0689422058867243));
#75566=CARTESIAN_POINT('Ctrl Pts',(0.00542536391359611,-0.0319739230346488,
0.0689789114370829));
#75567=CARTESIAN_POINT('Ctrl Pts',(0.0053546884798588,-0.0318646057455572,
0.0690170389226206));
#75568=CARTESIAN_POINT('Ctrl Pts',(0.00546342882477146,-0.0321934096636618,
0.0688663210262035));
#75569=CARTESIAN_POINT('Ctrl Pts',(0.00539056277386426,-0.0320835708272592,
0.068903009372511));
#75570=CARTESIAN_POINT('Ctrl Pts',(0.00531849825164789,-0.0319739230346488,
0.0689411843972231));
#75571=CARTESIAN_POINT('Ctrl Pts',(0.00524732371116907,-0.0318646057455572,
0.0689807901818324));
#75572=CARTESIAN_POINT('Ctrl Pts',(0.00535765398419079,-0.0321934096636618,
0.0688256657945026));
#75573=CARTESIAN_POINT('Ctrl Pts',(0.0052842272659536,-0.0320835708272592,
0.0688638128582977));
#75574=CARTESIAN_POINT('Ctrl Pts',(0.00521163258969967,-0.0319739230346488,
0.0689034573573634));
#75575=CARTESIAN_POINT('Ctrl Pts',(0.00513995894247935,-0.0318646057455572,
0.0689445414410442));
#75576=CARTESIAN_POINT('',(0.00534628742212121,-0.0321763980308452,0.0688315864419187));
#75577=CARTESIAN_POINT('',(0.00535765398416181,-0.0321934096636184,0.0688256657945176));
#75578=CARTESIAN_POINT('Origin',(0.0124573985862644,-0.032638623105711,
0.0837734131738772));
#75579=CARTESIAN_POINT('Ctrl Pts',(0.0053462874235849,-0.0321763980306276,
0.0688315864447262));
#75580=CARTESIAN_POINT('Ctrl Pts',(0.00536615525725229,-0.0321259596174872,
0.0688696298488218));
#75581=CARTESIAN_POINT('Ctrl Pts',(0.00538567885492711,-0.0320749164631493,
0.0689070141015737));
#75582=CARTESIAN_POINT('Ctrl Pts',(0.005424053290234,-0.0319716057793892,
0.0689804943900522));
#75583=CARTESIAN_POINT('Ctrl Pts',(0.00544288917589063,-0.0319193786690081,
0.0690165617953779));
#75584=CARTESIAN_POINT('Ctrl Pts',(0.00546138748399746,-0.031866561752526,
0.0690519827991057));
#75585=CARTESIAN_POINT('',(0.00551536964653578,-0.0321934096636663,0.0688862848109516));
#75586=CARTESIAN_POINT('Origin',(0.00812378219310841,-0.0315241814719618,
0.07415));
#75587=CARTESIAN_POINT('',(0.00534628742194917,-0.0322104233323791,0.0688315864415895));
#75588=CARTESIAN_POINT('',(0.00533493353088838,-0.0321934096636183,0.0688375313516916));
#75589=CARTESIAN_POINT('Origin',(0.0125001154882419,-0.0326387233587389,
0.0837582318680157));
#75590=CARTESIAN_POINT('Origin',(0.0135450215143358,-0.0326386243771962,
0.0832054147042603));
#75591=CARTESIAN_POINT('Origin',(0.0135081509368146,-0.0326387244007988,
0.0832317913507903));
#75592=CARTESIAN_POINT('Ctrl Pts',(0.0056052613123584,-0.0327445246967097,
0.0689793929202437));
#75593=CARTESIAN_POINT('Ctrl Pts',(0.00541024867832073,-0.032443687833936,
0.0690743804880976));
#75594=CARTESIAN_POINT('Ctrl Pts',(0.00522294490640992,-0.0321434074405927,
0.0691837873549253));
#75595=CARTESIAN_POINT('Ctrl Pts',(0.00538293783121712,-0.0327445246967097,
0.0690937269472576));
#75596=CARTESIAN_POINT('Ctrl Pts',(0.00519223737550286,-0.032443687833936,
0.0691970995822799));
#75597=CARTESIAN_POINT('Ctrl Pts',(0.00500986512900158,-0.0321434074405927,
0.0693145428842906));
#75598=CARTESIAN_POINT('',(0.00535121608758842,-0.0326943950436612,0.0691110514796713));
#75599=CARTESIAN_POINT('',(0.00514653396172323,-0.0323666188837389,0.0692292157160962));
#75600=CARTESIAN_POINT('Origin',(0.0135218084878484,-0.0326395579110189,
0.0838028681836174));
#75601=CARTESIAN_POINT('Origin',(-0.000570818722665324,-0.0321933825603095,
0.0597795993160227));
#75602=CARTESIAN_POINT('',(0.00525418552987477,-0.0321934096532689,0.0691656705579445));
#75603=CARTESIAN_POINT('',(0.00520071137581225,-0.0321934096584275,0.0691980243087788));
#75604=CARTESIAN_POINT('',(0.00546138748270218,-0.0325210109756239,0.0690519827966157));
#75605=CARTESIAN_POINT('Origin',(0.0130889041165304,-0.0326393129159009,
0.0840121006749662));
#75606=CARTESIAN_POINT('',(0.00546201637008394,-0.0326943950436593,0.0690531870052572));
#75607=CARTESIAN_POINT('Origin',(0.000341031935603809,-0.0326943765538163,
0.0592474012077398));
#75608=CARTESIAN_POINT('',(0.00540661622884618,-0.0326943950436702,0.0690821192424742));
#75609=CARTESIAN_POINT('Ctrl Pts',(0.00555688632331576,-0.0325229783203769,
0.0687268048538092));
#75610=CARTESIAN_POINT('Ctrl Pts',(0.00548212769682297,-0.032413025309245,
0.06876218945724));
#75611=CARTESIAN_POINT('Ctrl Pts',(0.00540811238491736,-0.0323031222208069,
0.0687991151721256));
#75612=CARTESIAN_POINT('Ctrl Pts',(0.00533493352691798,-0.0321934096576658,
0.0688375313537759));
#75613=CARTESIAN_POINT('Ctrl Pts',(0.0055252840289352,-0.0325229783203769,
0.0688356278165799));
#75614=CARTESIAN_POINT('Ctrl Pts',(0.00545202552460439,-0.032413025309245,
0.0688714480569477));
#75615=CARTESIAN_POINT('Ctrl Pts',(0.00537951911904752,-0.0323031222208069,
0.0689087783107434));
#75616=CARTESIAN_POINT('Ctrl Pts',(0.00530785600049679,-0.0321934096576658,
0.0689475674832935));
#75617=CARTESIAN_POINT('Ctrl Pts',(0.00549368173455463,-0.0325229783203769,
0.0689444507793506));
#75618=CARTESIAN_POINT('Ctrl Pts',(0.00542192335238582,-0.032413025309245,
0.0689807066566553));
#75619=CARTESIAN_POINT('Ctrl Pts',(0.00535092585317768,-0.032303122220807,
0.0690184414493611));
#75620=CARTESIAN_POINT('Ctrl Pts',(0.00528077847407559,-0.0321934096576658,
0.0690576036128112));
#75621=CARTESIAN_POINT('Ctrl Pts',(0.00546207944017407,-0.0325229783203769,
0.0690532737421213));
#75622=CARTESIAN_POINT('Ctrl Pts',(0.00539182118016725,-0.032413025309245,
0.0690899652563629));
#75623=CARTESIAN_POINT('Ctrl Pts',(0.00532233258730784,-0.032303122220807,
0.0691281045879789));
#75624=CARTESIAN_POINT('Ctrl Pts',(0.0052537009476544,-0.0321934096576658,
0.0691676397423288));
#75625=CARTESIAN_POINT('',(0.00529455953074173,-0.0321934096584275,0.069001600954455));
#75626=CARTESIAN_POINT('Ctrl Pts',(0.00534628742355425,-0.0322104233328935,
0.0688315864446675));
#75627=CARTESIAN_POINT('Ctrl Pts',(0.00536618217845319,-0.0322609421831227,
0.0688696813981825));
#75628=CARTESIAN_POINT('Ctrl Pts',(0.00538571892758863,-0.0323120888240435,
0.068907090833681));
#75629=CARTESIAN_POINT('Ctrl Pts',(0.00542409365344589,-0.0324156524631814,
0.0689805716785123));
#75630=CARTESIAN_POINT('Ctrl Pts',(0.00544291585612749,-0.0324680267167309,
0.0690166128833349));
#75631=CARTESIAN_POINT('Ctrl Pts',(0.0054613874827183,-0.0325210109755912,
0.0690519827966562));
#75632=CARTESIAN_POINT('Origin',(0.0154857614310304,-0.0262834582512449,
0.0713742753129969));
#75633=CARTESIAN_POINT('Origin',(0.00791146188208468,-0.034277077895491,
0.0619935970171797));
#75634=CARTESIAN_POINT('Ctrl Pts',(0.00535315076944912,-0.0326943950436604,
0.0691116586838633));
#75635=CARTESIAN_POINT('Ctrl Pts',(0.0052837129832547,-0.0325844576448134,
0.069149843177598));
#75636=CARTESIAN_POINT('Ctrl Pts',(0.00521506000077505,-0.0324744968375322,
0.069189466460972));
#75637=CARTESIAN_POINT('Ctrl Pts',(0.00514727908397632,-0.0323646534831894,
0.0692304765530607));
#75638=CARTESIAN_POINT('Ctrl Pts',(0.00524503204476973,-0.0326943950436604,
0.0690777253822981));
#75639=CARTESIAN_POINT('Ctrl Pts',(0.00517512659408197,-0.0325844576448134,
0.069117399954695));
#75640=CARTESIAN_POINT('Ctrl Pts',(0.00510603673128137,-0.0324744968375322,
0.0691585230942548));
#75641=CARTESIAN_POINT('Ctrl Pts',(0.00503785025158459,-0.0323646534831894,
0.069201040890629));
#75642=CARTESIAN_POINT('Ctrl Pts',(0.00513691332009035,-0.0326943950436604,
0.0690437920807329));
#75643=CARTESIAN_POINT('Ctrl Pts',(0.00506654020490923,-0.0325844576448134,
0.069084956731792));
#75644=CARTESIAN_POINT('Ctrl Pts',(0.00499701346178769,-0.0324744968375322,
0.0691275797275376));
#75645=CARTESIAN_POINT('Ctrl Pts',(0.00492842141919285,-0.0323646534831894,
0.0691716052281974));
#75646=CARTESIAN_POINT('Ctrl Pts',(0.00502879459541097,-0.0326943950436604,
0.0690098587791677));
#75647=CARTESIAN_POINT('Ctrl Pts',(0.0049579538157365,-0.0325844576448134,
0.069052513508889));
#75648=CARTESIAN_POINT('Ctrl Pts',(0.00488799019229401,-0.0324744968375322,
0.0690966363608204));
#75649=CARTESIAN_POINT('Ctrl Pts',(0.00481899258680112,-0.0323646534831894,
0.0691421695657657));
#75650=CARTESIAN_POINT('',(0.00501782222310387,-0.0326773559991334,0.0690164814556856));
#75651=CARTESIAN_POINT('',(0.00502879459541033,-0.0326943950436594,0.0690098587791681));
#75652=CARTESIAN_POINT('Origin',(0.0136566259742715,-0.0326395670209633,
0.0831976090128865));
#75653=CARTESIAN_POINT('Ctrl Pts',(0.00501782222483375,-0.0326773559987417,
0.0690164814585482));
#75654=CARTESIAN_POINT('Ctrl Pts',(0.00504005749802945,-0.0326267922586026,
0.0690532318315055));
#75655=CARTESIAN_POINT('Ctrl Pts',(0.00506189866706431,-0.0325756109579462,
0.0690893308306403));
#75656=CARTESIAN_POINT('Ctrl Pts',(0.00510481138473952,-0.0324719985462365,
0.0691602568033186));
#75657=CARTESIAN_POINT('Ctrl Pts',(0.00512586572225259,-0.0324196091621774,
0.069195055330378));
#75658=CARTESIAN_POINT('Ctrl Pts',(0.00514653396174843,-0.0323666188837756,
0.069229215716138));
#75659=CARTESIAN_POINT('',(0.00519000534150938,-0.0326943950436702,0.0690604551294297));
#75660=CARTESIAN_POINT('Origin',(0.00812378219310841,-0.0315241814719618,
0.07415));
#75661=CARTESIAN_POINT('',(0.00501782222312663,-0.0327114338379879,0.0690164814557234));
#75662=CARTESIAN_POINT('',(0.00500686402026083,-0.0326943950436593,0.069023127551441));
#75663=CARTESIAN_POINT('Origin',(0.0136949868758667,-0.0326395667777739,
0.083173494238871));
#75664=CARTESIAN_POINT('Origin',(0.0135706575092932,-0.0326395679847929,
0.0832496254823012));
#75665=CARTESIAN_POINT('Origin',(0.0135314925742125,-0.0326395677859133,
0.0832724112383833));
#75666=CARTESIAN_POINT('Ctrl Pts',(0.00528553181829957,-0.0332451089994433,
0.0691477545232268));
#75667=CARTESIAN_POINT('Ctrl Pts',(0.00509686904345838,-0.0329451141710254,
0.069254800887483));
#75668=CARTESIAN_POINT('Ctrl Pts',(0.00491680540941372,-0.0326442513127493,
0.0693757539957767));
#75669=CARTESIAN_POINT('Ctrl Pts',(0.00507082700813731,-0.0332451089994433,
0.0692758242093091));
#75670=CARTESIAN_POINT('Ctrl Pts',(0.00488699446053337,-0.0329451141710254,
0.0693909682979662));
#75671=CARTESIAN_POINT('Ctrl Pts',(0.00471235728526579,-0.0326442513127493,
0.0695196322934187));
#75672=CARTESIAN_POINT('',(0.00504028891799165,-0.0331951640388616,0.0692950855597332));
#75673=CARTESIAN_POINT('',(0.00484343027934221,-0.0328677532092642,0.0694258687230506));
#75674=CARTESIAN_POINT('Origin',(0.014666974025928,-0.0326401908899162,
0.0830194791727825));
#75675=CARTESIAN_POINT('Origin',(-0.00146245926292119,-0.0326944279134284,
0.0603445729840615));
#75676=CARTESIAN_POINT('',(0.00494687938261152,-0.0326943950436593,0.0693556894622211));
#75677=CARTESIAN_POINT('',(0.00489554225887862,-0.0326943950436693,0.0693913370389483));
#75678=CARTESIAN_POINT('',(0.00514653396172563,-0.0330220786163545,0.0692292157160947));
#75679=CARTESIAN_POINT('Origin',(0.0142907263605349,-0.032639668276516,
0.0833189963584933));
#75680=CARTESIAN_POINT('',(0.00514723722102947,-0.0331951640388587,0.0692303780603392));
#75681=CARTESIAN_POINT('Origin',(-0.000563407297126675,-0.0331952026560132,
0.0597918448727092));
#75682=CARTESIAN_POINT('',(0.00509376306952056,-0.0331951640388701,0.0692627318100462));
#75683=CARTESIAN_POINT('Ctrl Pts',(0.00522142542423587,-0.0330240426238172,
0.0688986834806688));
#75684=CARTESIAN_POINT('Ctrl Pts',(0.00514908342307229,-0.032914277406352,
0.0689386662727892));
#75685=CARTESIAN_POINT('Ctrl Pts',(0.00507753191278236,-0.0328043479726691,
0.0689801645090312));
#75686=CARTESIAN_POINT('Ctrl Pts',(0.00500686402026084,-0.0326943950436593,
0.069023127551441));
#75687=CARTESIAN_POINT('Ctrl Pts',(0.00519671856385909,-0.0330240426238172,
0.0690092760076984));
#75688=CARTESIAN_POINT('Ctrl Pts',(0.00512590008250043,-0.032914277406352,
0.0690495991608912));
#75689=CARTESIAN_POINT('Ctrl Pts',(0.00505587988775971,-0.0328043479726691,
0.0690914064324779));
#75690=CARTESIAN_POINT('Ctrl Pts',(0.00498674915570538,-0.0326943950436593,
0.0691346467345818));
#75691=CARTESIAN_POINT('Ctrl Pts',(0.00517201170348231,-0.0330240426238172,
0.069119868534728));
#75692=CARTESIAN_POINT('Ctrl Pts',(0.00510271674192856,-0.032914277406352,
0.0691605320489933));
#75693=CARTESIAN_POINT('Ctrl Pts',(0.00503422786273706,-0.0328043479726691,
0.0692026483559246));
#75694=CARTESIAN_POINT('Ctrl Pts',(0.00496663429114993,-0.0326943950436593,
0.0692461659177226));
#75695=CARTESIAN_POINT('Ctrl Pts',(0.00514730484310553,-0.0330240426238172,
0.0692304610617576));
#75696=CARTESIAN_POINT('Ctrl Pts',(0.00507953340135669,-0.032914277406352,
0.0692714649370953));
#75697=CARTESIAN_POINT('Ctrl Pts',(0.0050125758377144,-0.0328043479726691,
0.0693138902793714));
#75698=CARTESIAN_POINT('Ctrl Pts',(0.00494651942659447,-0.0326943950436593,
0.0693576851008633));
#75699=CARTESIAN_POINT('',(0.00497687170144618,-0.0326943950436694,0.0691894085068411));
#75700=CARTESIAN_POINT('Ctrl Pts',(0.00501782222483762,-0.0327114338383332,
0.0690164814585545));
#75701=CARTESIAN_POINT('Ctrl Pts',(0.00504005379958046,-0.0327619876830956,
0.0690532257187232));
#75702=CARTESIAN_POINT('Ctrl Pts',(0.00506189316211955,-0.0328131562604296,
0.0690893217320889));
#75703=CARTESIAN_POINT('Ctrl Pts',(0.00510480584038152,-0.0329167375858771,
0.0691602476396251));
#75704=CARTESIAN_POINT('Ctrl Pts',(0.00512586205748005,-0.0329691088920615,
0.069195049273256));
#75705=CARTESIAN_POINT('Ctrl Pts',(0.00514653396174787,-0.0330220786163186,
0.0692292157161368));
#75706=CARTESIAN_POINT('Ctrl Pts',(0.00504225822323976,-0.0331951640388604,
0.069295570163427));
#75707=CARTESIAN_POINT('Ctrl Pts',(0.00497539826488769,-0.0330855618127442,
0.0693380119271814));
#75708=CARTESIAN_POINT('Ctrl Pts',(0.00490936730693175,-0.0329757224171941,
0.0693818661678264));
#75709=CARTESIAN_POINT('Ctrl Pts',(0.00484425266066457,-0.0328657861694599,
0.0694270808750398));
#75710=CARTESIAN_POINT('Ctrl Pts',(0.00493222205174072,-0.0331951640388604,
0.0692684926265878));
#75711=CARTESIAN_POINT('Ctrl Pts',(0.00486498915505268,-0.0330855618127442,
0.0693124499161797));
#75712=CARTESIAN_POINT('Ctrl Pts',(0.00479861631324684,-0.0329757224171941,
0.0693578284831826));
#75713=CARTESIAN_POINT('Ctrl Pts',(0.00473319137116802,-0.0328657861694599,
0.0694045743867574));
#75714=CARTESIAN_POINT('Ctrl Pts',(0.00482218588024168,-0.0331951640388604,
0.0692414150897486));
#75715=CARTESIAN_POINT('Ctrl Pts',(0.00475458004521767,-0.0330855618127442,
0.069286887905178));
#75716=CARTESIAN_POINT('Ctrl Pts',(0.00468786531956193,-0.0329757224171941,
0.0693337907985387));
#75717=CARTESIAN_POINT('Ctrl Pts',(0.00462213008167146,-0.0328657861694599,
0.069382067898475));
#75718=CARTESIAN_POINT('Ctrl Pts',(0.00471214970874264,-0.0331951640388604,
0.0692143375529094));
#75719=CARTESIAN_POINT('Ctrl Pts',(0.00464417093538266,-0.0330855618127442,
0.0692613258941764));
#75720=CARTESIAN_POINT('Ctrl Pts',(0.00457711432587703,-0.0329757224171941,
0.0693097531138949));
#75721=CARTESIAN_POINT('Ctrl Pts',(0.00451106879217491,-0.0328657861694599,
0.0693595614101926));
#75722=CARTESIAN_POINT('',(0.00470161482908265,-0.0331781648279162,0.0692216361218709));
#75723=CARTESIAN_POINT('',(0.00471214970874164,-0.0331951640388588,0.0692143375529101));
#75724=CARTESIAN_POINT('Origin',(0.0147015863296263,-0.0326412091934606,
0.0823740905285352));
#75725=CARTESIAN_POINT('Ctrl Pts',(0.00470161483108013,-0.0331781648273352,
0.0692216361247498));
#75726=CARTESIAN_POINT('Ctrl Pts',(0.00472613074176301,-0.0331276810207405,
0.0692569422088178));
#75727=CARTESIAN_POINT('Ctrl Pts',(0.00475020378706199,-0.0330765665168933,
0.0692916105094203));
#75728=CARTESIAN_POINT('Ctrl Pts',(0.0047974855800995,-0.0329730612715184,
0.0693597024102866));
#75729=CARTESIAN_POINT('Ctrl Pts',(0.00482067475170455,-0.0329207135598913,
0.0693930978183848));
#75730=CARTESIAN_POINT('Ctrl Pts',(0.0048434302793682,-0.0328677532092986,
0.0694258687230881));
#75731=CARTESIAN_POINT('',(0.00487621931337665,-0.0331951640388701,0.0692547115563316));
#75732=CARTESIAN_POINT('Origin',(0.00812378219310841,-0.0315241814719618,
0.07415));
#75733=CARTESIAN_POINT('',(0.00470161482934441,-0.0332121607144427,0.069221636122248));
#75734=CARTESIAN_POINT('',(0.00469109556167718,-0.0331951640388587,0.069228957174499));
#75735=CARTESIAN_POINT('Origin',(0.014733799291535,-0.0326413651105875,
0.082342175563266));
#75736=CARTESIAN_POINT('Origin',(0.0135314857625357,-0.0326412100173772,
0.0831865897364757));
#75737=CARTESIAN_POINT('Origin',(0.0134903253941661,-0.0326413661000901,
0.0832056188927701));
#75738=CARTESIAN_POINT('Ctrl Pts',(0.00497705630180331,-0.0337436976235975,
0.0693358291300589));
#75739=CARTESIAN_POINT('Ctrl Pts',(0.0049337569193915,-0.0336723290703325,
0.0693641312596247));
#75740=CARTESIAN_POINT('Ctrl Pts',(0.00489097360790398,-0.033601104548885,
0.0693932076299855));
#75741=CARTESIAN_POINT('Ctrl Pts',(0.00475437496922083,-0.0333736987606857,
0.0694860427208433));
#75742=CARTESIAN_POINT('Ctrl Pts',(0.00462332884708358,-0.0331450831799191,
0.0695865636443243));
#75743=CARTESIAN_POINT('Ctrl Pts',(0.00477081621287937,-0.0337436976235975,
0.06947712677944));
#75744=CARTESIAN_POINT('Ctrl Pts',(0.00472878768294034,-0.0336723290703325,
0.0695072838636221));
#75745=CARTESIAN_POINT('Ctrl Pts',(0.00468730838311847,-0.033601104548885,
0.069538192029881));
#75746=CARTESIAN_POINT('Ctrl Pts',(0.00455487319537358,-0.0333736987606857,
0.0696368756821829));
#75747=CARTESIAN_POINT('Ctrl Pts',(0.00442831928731498,-0.0331450831799191,
0.0697429966063202));
#75748=CARTESIAN_POINT('Ctrl Pts',(0.00476875381199013,-0.0337436976235975,
0.0694785397559338));
#75749=CARTESIAN_POINT('Ctrl Pts',(0.00472673799057583,-0.0336723290703325,
0.0695087153896621));
#75750=CARTESIAN_POINT('Ctrl Pts',(0.00468527173087061,-0.033601104548885,
0.06953964187388));
#75751=CARTESIAN_POINT('Ctrl Pts',(0.00455287817763511,-0.0333736987606857,
0.0696383840117963));
#75752=CARTESIAN_POINT('Ctrl Pts',(0.0044263691917173,-0.0331450831799191,
0.0697445609359402));
#75753=CARTESIAN_POINT('',(0.00474153088762703,-0.0336938721132548,0.0694982797690993));
#75754=CARTESIAN_POINT('',(0.00455327264161155,-0.0333679869945434,0.069641165722439));
#75755=CARTESIAN_POINT('Ctrl Pts',(0.00474153088762864,-0.0336938721132646,
0.0694982797690973));
#75756=CARTESIAN_POINT('Ctrl Pts',(0.00472337304140678,-0.0336629187933929,
0.0695114822825854));
#75757=CARTESIAN_POINT('Ctrl Pts',(0.00470529830852139,-0.0336319952301037,
0.0695247868950853));
#75758=CARTESIAN_POINT('Ctrl Pts',(0.00468730838312026,-0.0336011045488947,
0.0695381920298795));
#75759=CARTESIAN_POINT('Ctrl Pts',(0.00464216550448278,-0.0335235892595451,
0.0695718301000573));
#75760=CARTESIAN_POINT('Ctrl Pts',(0.00459747651609426,-0.0334458668660366,
0.0696061610300895));
#75761=CARTESIAN_POINT('Ctrl Pts',(0.00455327264141187,-0.0333679869945382,
0.0696411657221753));
#75762=CARTESIAN_POINT('Ctrl Pts',(0.0045532373518823,-0.0333679692460362,
0.0696411927909531));
#75763=CARTESIAN_POINT('Ctrl Pts',(0.00455352335907653,-0.0333391895375493,
0.0696415444124923));
#75764=CARTESIAN_POINT('Ctrl Pts',(0.00455374025450246,-0.0333104081061546,
0.0696418059209864));
#75765=CARTESIAN_POINT('Ctrl Pts',(0.00455403161565926,-0.033253269824495,
0.0696421485364477));
#75766=CARTESIAN_POINT('Ctrl Pts',(0.00455410816086979,-0.0332249171348981,
0.0696422322757971));
#75767=CARTESIAN_POINT('Ctrl Pts',(0.0045541158481945,-0.0331960985361085,
0.0696422308701326));
#75768=CARTESIAN_POINT('Ctrl Pts',(0.00455411595436276,-0.0331956312563914,
0.0696422308240151));
#75769=CARTESIAN_POINT('Ctrl Pts',(0.00455411604157513,-0.0331951640388587,
0.0696422307549524));
#75770=CARTESIAN_POINT('',(0.00465211102516163,-0.0331951640388587,0.0695646293168766));
#75771=CARTESIAN_POINT('',(0.00460311353337761,-0.0331951640388687,0.069603430035925));
#75772=CARTESIAN_POINT('',(0.00484343027971246,-0.0335216366567749,0.0694258687232914));
#75773=CARTESIAN_POINT('Origin',(0.0153120163414045,-0.0326434571528763,
0.0823788363706307));
#75774=CARTESIAN_POINT('',(0.0048442051351257,-0.0336938721132327,0.0694269846156556));
#75775=CARTESIAN_POINT('Origin',(-0.00138446321486033,-0.0336938867896402,
0.060456894283551));
#75776=CARTESIAN_POINT('',(0.00479286801138636,-0.0336938721132538,0.0694626321923875));
#75777=CARTESIAN_POINT('Ctrl Pts',(0.00489741885958399,-0.0335235895815172,
0.0690912867604388));
#75778=CARTESIAN_POINT('Ctrl Pts',(0.00482777571215158,-0.0334144449262748,
0.0691357040038496));
#75779=CARTESIAN_POINT('Ctrl Pts',(0.00475897018000144,-0.0333049234473147,
0.0691816110523054));
#75780=CARTESIAN_POINT('Ctrl Pts',(0.00469109556167717,-0.0331951640388587,
0.0692289571744989));
#75781=CARTESIAN_POINT('Ctrl Pts',(0.00487970490753242,-0.0335235895815172,
0.0692032125768915));
#75782=CARTESIAN_POINT('Ctrl Pts',(0.00481160263932514,-0.0334144449262748,
0.0692478736877279));
#75783=CARTESIAN_POINT('Ctrl Pts',(0.00474434479480116,-0.0333049234473147,
0.0692939930503782));
#75784=CARTESIAN_POINT('Ctrl Pts',(0.00467802271807902,-0.0331951640388587,
0.0693415194827825));
#75785=CARTESIAN_POINT('Ctrl Pts',(0.00486199095548085,-0.0335235895815172,
0.0693151383933442));
#75786=CARTESIAN_POINT('Ctrl Pts',(0.0047954295664987,-0.0334144449262748,
0.0693600433716061));
#75787=CARTESIAN_POINT('Ctrl Pts',(0.00472971940960087,-0.0333049234473147,
0.069406375048451));
#75788=CARTESIAN_POINT('Ctrl Pts',(0.00466494987448086,-0.0331951640388587,
0.0694540817910662));
#75789=CARTESIAN_POINT('Ctrl Pts',(0.00484427700342929,-0.0335235895815172,
0.0694270642097969));
#75790=CARTESIAN_POINT('Ctrl Pts',(0.00477925649367226,-0.0334144449262748,
0.0694722130554844));
#75791=CARTESIAN_POINT('Ctrl Pts',(0.00471509402440059,-0.0333049234473147,
0.0695187570465238));
#75792=CARTESIAN_POINT('Ctrl Pts',(0.00465187703088271,-0.0331951640388587,
0.0695666440993499));
#75793=CARTESIAN_POINT('',(0.0046716032934294,-0.0331951640388687,0.0693967932456978));
#75794=CARTESIAN_POINT('Ctrl Pts',(0.00470161483112568,-0.0332121607145986,
0.0692216361248153));
#75795=CARTESIAN_POINT('Ctrl Pts',(0.00472608942773211,-0.0332625444109771,
0.0692568827112666));
#75796=CARTESIAN_POINT('Ctrl Pts',(0.00475014228863203,-0.033313530074685,
0.0692915219437223));
#75797=CARTESIAN_POINT('Ctrl Pts',(0.0047974236318699,-0.0334167203140656,
0.0693596131968189));
#75798=CARTESIAN_POINT('Ctrl Pts',(0.00482063380175359,-0.0334688847587368,
0.0693930388451559));
#75799=CARTESIAN_POINT('Ctrl Pts',(0.00484343027997499,-0.0335216366562442,
0.0694258687239619));
#75800=CARTESIAN_POINT('Ctrl Pts',(0.00474251486686462,-0.0336938721132391,
0.0694984572507384));
#75801=CARTESIAN_POINT('Ctrl Pts',(0.00471528784360763,-0.0336474569764958,
0.0695182489304224));
#75802=CARTESIAN_POINT('Ctrl Pts',(0.00468829437256328,-0.033601104548885,
0.0695383579806518));
#75803=CARTESIAN_POINT('Ctrl Pts',(0.00461995311006718,-0.0334837508592656,
0.0695892694724721));
#75804=CARTESIAN_POINT('Ctrl Pts',(0.00455315047107649,-0.0333660264659097,
0.0696421837010198));
#75805=CARTESIAN_POINT('Ctrl Pts',(0.00474153088764373,-0.0336938721132391,
0.0694982797690873));
#75806=CARTESIAN_POINT('Ctrl Pts',(0.00471430282552774,-0.0336474569764958,
0.0695180772083282));
#75807=CARTESIAN_POINT('Ctrl Pts',(0.00468730838311847,-0.033601104548885,
0.069538192029881));
#75808=CARTESIAN_POINT('Ctrl Pts',(0.0046189646613497,-0.0334837508592656,
0.0695891181333652));
#75809=CARTESIAN_POINT('Ctrl Pts',(0.00455215999714016,-0.0333660264659097,
0.0696420470400339));
#75810=CARTESIAN_POINT('Ctrl Pts',(0.00440697360539036,-0.0336938721132391,
0.0694379352236103));
#75811=CARTESIAN_POINT('Ctrl Pts',(0.00437939232662525,-0.0336474569764958,
0.0694596909376421));
#75812=CARTESIAN_POINT('Ctrl Pts',(0.00435206761584843,-0.033601104548885,
0.0694817680346504));
#75813=CARTESIAN_POINT('Ctrl Pts',(0.00428288773050648,-0.0334837508592656,
0.0695376621684326));
#75814=CARTESIAN_POINT('Ctrl Pts',(0.00421539448294333,-0.0333660264659097,
0.0695955817010667));
#75815=CARTESIAN_POINT('',(0.00439891316541995,-0.0336769361243754,0.0694462407877776));
#75816=CARTESIAN_POINT('',(0.00440896897686215,-0.0336938721132327,0.069438295131441));
#75817=CARTESIAN_POINT('Ctrl Pts',(0.00439891316541972,-0.0336769361243751,
0.0694462407877777));
#75818=CARTESIAN_POINT('Ctrl Pts',(0.00440058784506195,-0.0336797586670119,
0.06944491462246));
#75819=CARTESIAN_POINT('Ctrl Pts',(0.00440226316959848,-0.0336825812713033,
0.0694435894016527));
#75820=CARTESIAN_POINT('Ctrl Pts',(0.0044056151122592,-0.033688226610054,
0.0694409408454027));
#75821=CARTESIAN_POINT('Ctrl Pts',(0.00440729173041062,-0.0336910493445311,
0.0694396175099648));
#75822=CARTESIAN_POINT('Ctrl Pts',(0.00440896897686973,-0.0336938721132297,
0.0694382951314443));
#75823=CARTESIAN_POINT('Ctrl Pts',(0.00439891316541994,-0.0336769361243754,
0.0694462407877776));
#75824=CARTESIAN_POINT('Ctrl Pts',(0.00442493244446343,-0.0336279031301501,
0.0694790978956615));
#75825=CARTESIAN_POINT('Ctrl Pts',(0.00445132607601624,-0.0335767851899374,
0.069512427735351));
#75826=CARTESIAN_POINT('Ctrl Pts',(0.00450304375408568,-0.0334733198857323,
0.0695777367442975));
#75827=CARTESIAN_POINT('Ctrl Pts',(0.00452840252591669,-0.0334209645014072,
0.0696097597646312));
#75828=CARTESIAN_POINT('Ctrl Pts',(0.00455327264731456,-0.0333679869844681,
0.0696411657179049));
#75829=CARTESIAN_POINT('',(0.00457524993225459,-0.0336938721132538,0.0694682874502802));
#75830=CARTESIAN_POINT('Origin',(0.00812378219310841,-0.0315241814719618,
0.07415));
#75831=CARTESIAN_POINT('',(0.00439891316623064,-0.0337108120655408,0.0694462407888005));
#75832=CARTESIAN_POINT('',(0.00438887434898242,-0.0336938721132327,0.0694542079053787));
#75833=CARTESIAN_POINT('Origin',(0.0136799853731458,-0.0345562515490529,
0.0829665979872995));
#75834=CARTESIAN_POINT('Ctrl Pts',(0.00438887434898348,-0.0336938721132302,
0.0694542079053855));
#75835=CARTESIAN_POINT('Ctrl Pts',(0.00439054593505895,-0.0336910493375117,
0.0694528783703849));
#75836=CARTESIAN_POINT('Ctrl Pts',(0.00439221830234833,-0.0336882266065441,
0.0694515496712456));
#75837=CARTESIAN_POINT('Ctrl Pts',(0.00439556457770277,-0.0336825812713071,
0.0694488939626126));
#75838=CARTESIAN_POINT('Ctrl Pts',(0.00439723848577676,-0.0336797586670138,
0.0694475669530962));
#75839=CARTESIAN_POINT('Ctrl Pts',(0.00439891316542014,-0.0336769361243751,
0.0694462407877774));
#75840=CARTESIAN_POINT('Origin',(0.0154322992487056,-0.0345562517336882,
0.0815789516969124));
#75841=CARTESIAN_POINT('Ctrl Pts',(0.00468102272062642,-0.034243627687391,
0.0695428824396771));
#75842=CARTESIAN_POINT('Ctrl Pts',(0.00450726241736391,-0.0339430054201809,
0.0696727282537171));
#75843=CARTESIAN_POINT('Ctrl Pts',(0.00434377626764699,-0.0336441434784052,
0.0698152935274142));
#75844=CARTESIAN_POINT('Ctrl Pts',(0.00448406036984477,-0.034243627687391,
0.0696968494243672));
#75845=CARTESIAN_POINT('Ctrl Pts',(0.00431610702713881,-0.0339430054201809,
0.0698341237959283));
#75846=CARTESIAN_POINT('Ctrl Pts',(0.00415897089040231,-0.0336441434784052,
0.0699836591193309));
#75847=CARTESIAN_POINT('Ctrl Pts',(0.00448209074633695,-0.034243627687391,
0.0696983890942141));
#75848=CARTESIAN_POINT('Ctrl Pts',(0.00431419547323655,-0.0339430054201809,
0.0698357377513504));
#75849=CARTESIAN_POINT('Ctrl Pts',(0.00415712283662986,-0.0336441434784052,
0.06998534277525));
#75850=CARTESIAN_POINT('',(0.00445612105798559,-0.0341934961088741,0.0697198321930303));
#75851=CARTESIAN_POINT('',(0.0042772061819807,-0.0338664212894524,0.0698742570236255));
#75852=CARTESIAN_POINT('Origin',(0.0147304530405027,-0.0345610818077101,
0.0829293437895861));
#75853=CARTESIAN_POINT('Origin',(-0.00305720950804172,-0.0336938005044372,
0.0617216445300011));
#75854=CARTESIAN_POINT('',(0.00437104376775592,-0.0336938721132327,0.0697916655347617));
#75855=CARTESIAN_POINT('',(0.00432457927863607,-0.0336938721132426,0.0698334662674197));
#75856=CARTESIAN_POINT('',(0.00455327264731872,-0.0340203938281605,0.0696411657179016));
#75857=CARTESIAN_POINT('Origin',(0.0143096433318419,-0.0345589643242961,
0.0831626735693432));
#75858=CARTESIAN_POINT('',(0.00455411604157358,-0.034193496108874,0.0696422307549535));
#75859=CARTESIAN_POINT('Origin',(-0.00228688298184838,-0.0341934220717671,
0.0610034258243513));
#75860=CARTESIAN_POINT('',(0.00450511854978958,-0.034193496108884,0.0696810314740019));
#75861=CARTESIAN_POINT('Ctrl Pts',(0.00458614832818682,-0.0340223579322397,
0.069303852392076));
#75862=CARTESIAN_POINT('Ctrl Pts',(0.00451930731339,-0.0339125849573575,
0.0693526455896097));
#75863=CARTESIAN_POINT('Ctrl Pts',(0.0044535231728096,-0.0338030433565231,
0.0694027879544177));
#75864=CARTESIAN_POINT('Ctrl Pts',(0.00438887434898245,-0.0336938721132327,
0.069454207905378));
#75865=CARTESIAN_POINT('Ctrl Pts',(0.0045754971562424,-0.0340223579322397,
0.0694166696441543));
#75866=CARTESIAN_POINT('Ctrl Pts',(0.00451021218559149,-0.0339125849573575,
0.0694656097491285));
#75867=CARTESIAN_POINT('Ctrl Pts',(0.00444598603638544,-0.0338030433565231,
0.0695158667116488));
#75868=CARTESIAN_POINT('Ctrl Pts',(0.0043828951457616,-0.0336938721132327,
0.0695673689806607));
#75869=CARTESIAN_POINT('Ctrl Pts',(0.00456484598429799,-0.0340223579322397,
0.0695294868962326));
#75870=CARTESIAN_POINT('Ctrl Pts',(0.00450111705779298,-0.0339125849573575,
0.0695785739086474));
#75871=CARTESIAN_POINT('Ctrl Pts',(0.00443844889996129,-0.0338030433565231,
0.06962894546888));
#75872=CARTESIAN_POINT('Ctrl Pts',(0.00437691594254075,-0.0336938721132327,
0.0696805300559434));
#75873=CARTESIAN_POINT('Ctrl Pts',(0.00455419481235357,-0.0340223579322397,
0.0696423041483109));
#75874=CARTESIAN_POINT('Ctrl Pts',(0.00449202192999447,-0.0339125849573575,
0.0696915380681663));
#75875=CARTESIAN_POINT('Ctrl Pts',(0.00443091176353713,-0.0338030433565231,
0.0697420242261112));
#75876=CARTESIAN_POINT('Ctrl Pts',(0.00437093673931991,-0.0336938721132327,
0.0697936911312261));
#75877=CARTESIAN_POINT('',(0.00437995905837917,-0.0336938721132427,0.0696229367200802));
#75878=CARTESIAN_POINT('Ctrl Pts',(0.00439891316846227,-0.0337108120662694,
0.0694462407916194));
#75879=CARTESIAN_POINT('Ctrl Pts',(0.00442560760137709,-0.0337611408994287,
0.0694799504828339));
#75880=CARTESIAN_POINT('Ctrl Pts',(0.00445181492011522,-0.033812108878129,
0.0695130450469718));
#75881=CARTESIAN_POINT('Ctrl Pts',(0.00450327920369031,-0.0339153382773236,
0.0695780340697179));
#75882=CARTESIAN_POINT('Ctrl Pts',(0.0045285143959822,-0.033967555847311,
0.0696099010339878));
#75883=CARTESIAN_POINT('Ctrl Pts',(0.00455327264733931,-0.0340203938281304,
0.0696411657179362));
#75884=CARTESIAN_POINT('Ctrl Pts',(0.00445813566200616,-0.0341934961088741,
0.0697200661665839));
#75885=CARTESIAN_POINT('Ctrl Pts',(0.00436655027062025,-0.03402875161944,
0.0697958505202239));
#75886=CARTESIAN_POINT('Ctrl Pts',(0.00427817536200608,-0.033864463329982,
0.0698753554112645));
#75887=CARTESIAN_POINT('Ctrl Pts',(0.00445612105798569,-0.0341934961088741,
0.0697198321930303));
#75888=CARTESIAN_POINT('Ctrl Pts',(0.00436453082938092,-0.03402875161944,
0.069795658197021));
#75889=CARTESIAN_POINT('Ctrl Pts',(0.00427615280912178,-0.033864463329982,
0.0698752049027488));
#75890=CARTESIAN_POINT('Ctrl Pts',(0.00412044891561043,-0.0341934961088741,
0.069680847656515));
#75891=CARTESIAN_POINT('Ctrl Pts',(0.00402805271243154,-0.03402875161944,
0.0697636134175524));
#75892=CARTESIAN_POINT('Ctrl Pts',(0.00393915623170969,-0.033864463329982,
0.0698501272619776));
#75893=CARTESIAN_POINT('',(0.00411091186005815,-0.0341764758832377,0.0696894090435617));
#75894=CARTESIAN_POINT('',(0.00412044891561043,-0.034193496108874,0.069680847656515));
#75895=CARTESIAN_POINT('Origin',(0.0148042182940886,-0.0345621027386101,
0.0823414650918333));
#75896=CARTESIAN_POINT('Ctrl Pts',(0.00411091186182281,-0.0341764758837459,
0.0696894090431294));
#75897=CARTESIAN_POINT('Ctrl Pts',(0.00413962019877557,-0.0341260050044363,
0.0697213203821793));
#75898=CARTESIAN_POINT('Ctrl Pts',(0.00416782954551442,-0.0340749269156142,
0.0697526770013249));
#75899=CARTESIAN_POINT('Ctrl Pts',(0.00422327198472234,-0.0339715436322714,
0.0698143052241697));
#75900=CARTESIAN_POINT('Ctrl Pts',(0.00425048403929732,-0.0339192778254715,
0.0698445534516979));
#75901=CARTESIAN_POINT('Ctrl Pts',(0.00427720618315993,-0.0338664212876715,
0.0698742570193955));
#75902=CARTESIAN_POINT('',(0.00428828498680801,-0.0341934961088841,0.0697003399247827));
#75903=CARTESIAN_POINT('Origin',(0.00812378219310841,-0.0315241814719618,
0.07415));
#75904=CARTESIAN_POINT('',(0.00411091185992463,-0.0342105180190378,0.0696894090446719));
#75905=CARTESIAN_POINT('',(0.00410139311123135,-0.0341934961088739,0.0696979907823524));
#75906=CARTESIAN_POINT('Origin',(0.0148411909658773,-0.0345621707841575,
0.082315243466159));
#75907=CARTESIAN_POINT('Origin',(0.0155656421348607,-0.0345621036641094,
0.0816564701496351));
#75908=CARTESIAN_POINT('Origin',(0.0155356672756884,-0.0345621718092742,
0.0816904701435844));
#75909=CARTESIAN_POINT('Ctrl Pts',(0.00437215892286278,-0.0346945769586965,
0.0697906623105502));
#75910=CARTESIAN_POINT('Ctrl Pts',(0.00428085084957366,-0.0345275153362944,
0.0698692415620135));
#75911=CARTESIAN_POINT('Ctrl Pts',(0.00419199040447123,-0.0343603235965185,
0.0699507126929578));
#75912=CARTESIAN_POINT('Ctrl Pts',(0.00410583681608137,-0.034193496108874,
0.0700348308419054));
#75913=CARTESIAN_POINT('Ctrl Pts',(0.00430983455216918,-0.0346945769586965,
0.0698467310289543));
#75914=CARTESIAN_POINT('Ctrl Pts',(0.00421970086063573,-0.0345275153362944,
0.0699266156893151));
#75915=CARTESIAN_POINT('Ctrl Pts',(0.00413205615495252,-0.0343603235965185,
0.0700093556335772));
#75916=CARTESIAN_POINT('Ctrl Pts',(0.00404715601225469,-0.034193496108874,
0.0700947023011167));
#75917=CARTESIAN_POINT('Ctrl Pts',(0.00424751018147558,-0.0346945769586965,
0.0699027997473563));
#75918=CARTESIAN_POINT('Ctrl Pts',(0.00415855087169777,-0.0345275153362944,
0.0699839898166162));
#75919=CARTESIAN_POINT('Ctrl Pts',(0.00407212190543375,-0.0343603235965185,
0.0700679985741978));
#75920=CARTESIAN_POINT('Ctrl Pts',(0.00398847520842793,-0.034193496108874,
0.0701545737603309));
#75921=CARTESIAN_POINT('Ctrl Pts',(0.004185185810782,-0.0346945769586965,
0.0699588684657625));
#75922=CARTESIAN_POINT('Ctrl Pts',(0.00409740088275988,-0.0345275153362944,
0.0700413639439183));
#75923=CARTESIAN_POINT('Ctrl Pts',(0.0040121876559151,-0.0343603235965185,
0.0701266415148161));
#75924=CARTESIAN_POINT('Ctrl Pts',(0.00392979440460133,-0.034193496108874,
0.0702144452195393));
#75925=CARTESIAN_POINT('',(0.00418518581123245,-0.0346945769586966,0.0699588684653575));
#75926=CARTESIAN_POINT('',(0.00401632040120248,-0.0343667727831428,0.0701242227299197));
#75927=CARTESIAN_POINT('Origin',(0.0158319840860491,-0.0345626457065531,
0.082085258578487));
#75928=CARTESIAN_POINT('Origin',(-0.00387684372025463,-0.0341934771028963,
0.0623880340926365));
#75929=CARTESIAN_POINT('',(0.00410478685445196,-0.034193496108874,0.0700359021076476));
#75930=CARTESIAN_POINT('',(0.0040610387421073,-0.034193496108884,0.0700805378855203));
#75931=CARTESIAN_POINT('',(0.00427720618527019,-0.034521194296272,0.0698742570217944));
#75932=CARTESIAN_POINT('Origin',(0.0154723101030635,-0.0345625596116798,
0.0824043595268634));
#75933=CARTESIAN_POINT('',(0.00427811478949626,-0.0346945769586885,0.0698752670000577));
#75934=CARTESIAN_POINT('Origin',(-0.00312132793923013,-0.0346945685853823,
0.0616502586418894));
#75935=CARTESIAN_POINT('',(0.00423165030037435,-0.0346945769587026,0.0699170677327176));
#75936=CARTESIAN_POINT('Ctrl Pts',(0.00428883617452006,-0.0345231616327841,
0.0695355456406487));
#75937=CARTESIAN_POINT('Ctrl Pts',(0.0042252324178085,-0.0344132092796988,
0.0695884049723428));
#75938=CARTESIAN_POINT('Ctrl Pts',(0.00416272529633964,-0.0343032738558979,
0.069642577170276));
#75939=CARTESIAN_POINT('Ctrl Pts',(0.00410139311123132,-0.034193496108874,
0.0696979907823524));
#75940=CARTESIAN_POINT('Ctrl Pts',(0.00428528989829662,-0.0345231616327841,
0.0696488088741512));
#75941=CARTESIAN_POINT('Ctrl Pts',(0.00422324731579701,-0.0344132092796988,
0.0697017170862703));
#75942=CARTESIAN_POINT('Ctrl Pts',(0.00416230229904373,-0.0343032738558979,
0.0697559058704493));
#75943=CARTESIAN_POINT('Ctrl Pts',(0.00410253114737363,-0.034193496108874,
0.0698113038046059));
#75944=CARTESIAN_POINT('Ctrl Pts',(0.00428174362207317,-0.0345231616327841,
0.0697620721076537));
#75945=CARTESIAN_POINT('Ctrl Pts',(0.00422126221378552,-0.0344132092796988,
0.0698150292001977));
#75946=CARTESIAN_POINT('Ctrl Pts',(0.00416187930174781,-0.0343032738558979,
0.0698692345706226));
#75947=CARTESIAN_POINT('Ctrl Pts',(0.00410366918351593,-0.034193496108874,
0.0699246168268594));
#75948=CARTESIAN_POINT('Ctrl Pts',(0.00427819734584973,-0.0345231616327841,
0.0698753353411561));
#75949=CARTESIAN_POINT('Ctrl Pts',(0.00421927711177403,-0.0344132092796988,
0.0699283413141251));
#75950=CARTESIAN_POINT('Ctrl Pts',(0.0041614563044519,-0.0343032738558979,
0.0699825632707959));
#75951=CARTESIAN_POINT('Ctrl Pts',(0.00410480721965824,-0.034193496108874,
0.0700379298491129));
#75952=CARTESIAN_POINT('',(0.00410308998285166,-0.0341934961088839,0.06986694644501));
#75953=CARTESIAN_POINT('Ctrl Pts',(0.00411091186222982,-0.0342105180195396,
0.0696894090472348));
#75954=CARTESIAN_POINT('Ctrl Pts',(0.00413965246293281,-0.0342610556241236,
0.0697213562702702));
#75955=CARTESIAN_POINT('Ctrl Pts',(0.00416787732841666,-0.0343122189870013,
0.0697527302169068));
#75956=CARTESIAN_POINT('Ctrl Pts',(0.00422332033032435,-0.0344158119695205,
0.0698143590591847));
#75957=CARTESIAN_POINT('Ctrl Pts',(0.00425051986541438,-0.0344682069747753,
0.0698445932781199));
#75958=CARTESIAN_POINT('Ctrl Pts',(0.00427721020851433,-0.034521202284613,
0.0698742614939208));
#75959=CARTESIAN_POINT('Ctrl Pts',(0.00418721063751565,-0.0346945769586932,
0.0699589754530923));
#75960=CARTESIAN_POINT('Ctrl Pts',(0.00410056417048217,-0.034529677707698,
0.0700403612845754));
#75961=CARTESIAN_POINT('Ctrl Pts',(0.00401735549297437,-0.034364806625142,
0.0701252587509863));
#75962=CARTESIAN_POINT('Ctrl Pts',(0.00418518581123912,-0.0346945769586932,
0.0699588684653514));
#75963=CARTESIAN_POINT('Ctrl Pts',(0.00409853713230981,-0.034529677707698,
0.0700402961586851));
#75964=CARTESIAN_POINT('Ctrl Pts',(0.00401532797498495,-0.034364806625142,
0.0701252355425959));
#75965=CARTESIAN_POINT('Ctrl Pts',(0.00384772818185842,-0.0346945769586932,
0.0699410378841248));
#75966=CARTESIAN_POINT('Ctrl Pts',(0.00376071086827876,-0.034529677707698,
0.0700294422751687));
#75967=CARTESIAN_POINT('Ctrl Pts',(0.00367742174462465,-0.034364806625142,
0.0701213676312973));
#75968=CARTESIAN_POINT('',(0.00383874751920677,-0.0346775396664962,0.0699501812138163));
#75969=CARTESIAN_POINT('',(0.00384772818185601,-0.0346945769586886,0.0699410378841272));
#75970=CARTESIAN_POINT('Origin',(0.0158015436411093,-0.0345626618350802,
0.0814612371772208));
#75971=CARTESIAN_POINT('Ctrl Pts',(0.00383874752096816,-0.0346775396670097,
0.0699501812133703));
#75972=CARTESIAN_POINT('Ctrl Pts',(0.00386942708161475,-0.0346269749928192,
0.0699802506358189));
#75973=CARTESIAN_POINT('Ctrl Pts',(0.00389956142315404,-0.0345757902890796,
0.0700097856318815));
#75974=CARTESIAN_POINT('Ctrl Pts',(0.00395876436476409,-0.0344721681088223,
0.0700678112181175));
#75975=CARTESIAN_POINT('Ctrl Pts',(0.0039878097505526,-0.0344197714290205,
0.0700962790635588));
#75976=CARTESIAN_POINT('Ctrl Pts',(0.00401632040129074,-0.0343667727830579,
0.0701242227296687));
#75977=CARTESIAN_POINT('',(0.00401645699655423,-0.0346945769587026,0.0699499531747524));
#75978=CARTESIAN_POINT('Origin',(0.00812378219310841,-0.0315241814719618,
0.07415));
#75979=CARTESIAN_POINT('',(0.00383874751953099,-0.0347116136489621,0.0699501812151688));
#75980=CARTESIAN_POINT('',(0.00382978640553166,-0.0346945769586885,0.0699593437057787));
#75981=CARTESIAN_POINT('Origin',(0.0158319003503651,-0.0345626685753207,
0.0814275957869821));
#75982=CARTESIAN_POINT('Origin',(0.0155877516718174,-0.0345626627740259,
0.0816793705041721));
#75983=CARTESIAN_POINT('Origin',(0.0155547234227488,-0.0345626695951028,
0.0817103933327597));
#75984=CARTESIAN_POINT('Ctrl Pts',(0.0041324671762908,-0.0352450361874068,
0.070008965459918));
#75985=CARTESIAN_POINT('Ctrl Pts',(0.00397628549578934,-0.0349452760959493,
0.0701595003759405));
#75986=CARTESIAN_POINT('Ctrl Pts',(0.00383188641681499,-0.034644428984174,
0.0703213718813314));
#75987=CARTESIAN_POINT('Ctrl Pts',(0.00413068846890791,-0.0352450361874068,
0.0700107576164531));
#75988=CARTESIAN_POINT('Ctrl Pts',(0.00397457438069932,-0.0349452760959493,
0.0701613596175253));
#75989=CARTESIAN_POINT('Ctrl Pts',(0.00383024775511567,-0.034644428984174,
0.0703232929260563));
#75990=CARTESIAN_POINT('Ctrl Pts',(0.00395457882703833,-0.0352450361874068,
0.070188198857546));
#75991=CARTESIAN_POINT('Ctrl Pts',(0.00380515704505319,-0.0349452760959493,
0.0703454429427528));
#75992=CARTESIAN_POINT('Ctrl Pts',(0.0036680040225097,-0.034644428984174,
0.0705134953740692));
#75993=CARTESIAN_POINT('Ctrl Pts',(0.00395281773061963,-0.0352450361874068,
0.0701899732699569));
#75994=CARTESIAN_POINT('Ctrl Pts',(0.00380346287169672,-0.0349452760959493,
0.0703472837760051));
#75995=CARTESIAN_POINT('Ctrl Pts',(0.00366638158518364,-0.034644428984174,
0.0705153973985493));
#75996=CARTESIAN_POINT('',(0.00392981481673165,-0.0351951634053275,0.0702144199984733));
#75997=CARTESIAN_POINT('',(0.00377164489264186,-0.0348678972925388,0.0703900763414813));
#75998=CARTESIAN_POINT('Origin',(0.0167217537595203,-0.0345636767885282,
0.0810204736003928));
#75999=CARTESIAN_POINT('Origin',(-0.00458993218393289,-0.034694619934112,
0.0631662949218706));
#76000=CARTESIAN_POINT('',(0.00385439109183824,-0.0346945769330288,0.0702963751321229));
#76001=CARTESIAN_POINT('',(0.00381353200411445,-0.0346945769458128,0.0703436698045289));
#76002=CARTESIAN_POINT('',(0.00401632040137605,-0.0350221583435276,0.0701242227297751));
#76003=CARTESIAN_POINT('Origin',(0.0164400139611837,-0.0345628458716476,
0.0814100452612684));
#76004=CARTESIAN_POINT('',(0.00401720586740456,-0.035195136029876,0.0701250863516008));
#76005=CARTESIAN_POINT('Origin',(-0.00385224485374814,-0.0351951838366788,
0.0624121369015669));
#76006=CARTESIAN_POINT('',(0.00392979440494988,-0.0351951371328751,0.0702144452190176));
#76007=CARTESIAN_POINT('Ctrl Pts',(0.00400665887906221,-0.0350241211494343,
0.0697854501243585));
#76008=CARTESIAN_POINT('Ctrl Pts',(0.00394653899406037,-0.0349144232818962,
0.0698421618099233));
#76009=CARTESIAN_POINT('Ctrl Pts',(0.00388755539547412,-0.0348045283579412,
0.0699001501611477));
#76010=CARTESIAN_POINT('Ctrl Pts',(0.00382978639776993,-0.0346945769439158,
0.0699593437137317));
#76011=CARTESIAN_POINT('Ctrl Pts',(0.00401023147680345,-0.0350241211494343,
0.0698987125556777));
#76012=CARTESIAN_POINT('Ctrl Pts',(0.00395167173535362,-0.0349144232818962,
0.0699553750301733));
#76013=CARTESIAN_POINT('Ctrl Pts',(0.00389424819691255,-0.0348045283579412,
0.0700132818915915));
#76014=CARTESIAN_POINT('Ctrl Pts',(0.00383803717382372,-0.0346945769439158,
0.070072361705651));
#76015=CARTESIAN_POINT('Ctrl Pts',(0.00401380407454468,-0.0350241211494343,
0.0700119749869968));
#76016=CARTESIAN_POINT('Ctrl Pts',(0.00395680447664688,-0.0349144232818962,
0.0700685882504234));
#76017=CARTESIAN_POINT('Ctrl Pts',(0.00390094099835097,-0.0348045283579412,
0.0701264136220353));
#76018=CARTESIAN_POINT('Ctrl Pts',(0.00384628794987751,-0.0346945769439158,
0.0701853796975702));
#76019=CARTESIAN_POINT('Ctrl Pts',(0.00401737667228592,-0.0350241211494343,
0.070125237418316));
#76020=CARTESIAN_POINT('Ctrl Pts',(0.00396193721794013,-0.0349144232818962,
0.0701818014706735));
#76021=CARTESIAN_POINT('Ctrl Pts',(0.00390763379978939,-0.0348045283579412,
0.070239545352479));
#76022=CARTESIAN_POINT('Ctrl Pts',(0.00385453872593129,-0.0346945769439158,
0.0702983976894894));
#76023=CARTESIAN_POINT('',(0.00384208874882424,-0.0346945769458128,0.0701278594186829));
#76024=CARTESIAN_POINT('Ctrl Pts',(0.00383874752187396,-0.03471161364928,
0.0699501812174652));
#76025=CARTESIAN_POINT('Ctrl Pts',(0.00386941488997327,-0.0347621546532222,
0.0699802387078791));
#76026=CARTESIAN_POINT('Ctrl Pts',(0.00389954304286951,-0.0348133084096866,
0.0700097677063879));
#76027=CARTESIAN_POINT('Ctrl Pts',(0.00395874606227251,-0.034916856154457,
0.0700677933635758));
#76028=CARTESIAN_POINT('Ctrl Pts',(0.00398779744593243,-0.0349692089015913,
0.0700962670064083));
#76029=CARTESIAN_POINT('Ctrl Pts',(0.00401632040138823,-0.0350221583435,
0.070124222729815));
#76030=CARTESIAN_POINT('Ctrl Pts',(0.00393125734856887,-0.0351951371254888,
0.070214430526322));
#76031=CARTESIAN_POINT('Ctrl Pts',(0.00384989191896045,-0.0350307338980916,
0.0703011083470038));
#76032=CARTESIAN_POINT('Ctrl Pts',(0.00377217850349031,-0.0348659306897799,
0.070391075022998));
#76033=CARTESIAN_POINT('Ctrl Pts',(0.00392979440503568,-0.0351951371254888,
0.0702144452190959));
#76034=CARTESIAN_POINT('Ctrl Pts',(0.00384842927919115,-0.0350307338980916,
0.0703011532852173));
#76035=CARTESIAN_POINT('Ctrl Pts',(0.00377071741730197,-0.0348659306897799,
0.0703911501682518));
#76036=CARTESIAN_POINT('Ctrl Pts',(0.00368460354412518,-0.0351951371254888,
0.0702169077433135));
#76037=CARTESIAN_POINT('Ctrl Pts',(0.0036032893294238,-0.0350307338980916,
0.0703086849766463));
#76038=CARTESIAN_POINT('Ctrl Pts',(0.00352583784932513,-0.0348659306897799,
0.070403744591106));
#76039=CARTESIAN_POINT('Origin',(-0.000252701167597929,-0.0308609197411073,
0.0669133399892798));
#76040=CARTESIAN_POINT('',(0.00382289671799627,-0.0351951371254888,0.0702155188241323));
#76041=CARTESIAN_POINT('Origin',(0.00894792665521693,-0.0351840467441147,
0.0746749109977826));
#76042=CARTESIAN_POINT('Origin',(-0.0014300780706032,-0.0352322613594373,
0.066946369667333));
#76043=CARTESIAN_POINT('',(0.00362067005566337,-0.0351951142564653,0.0705723197933546));
#76044=CARTESIAN_POINT('',(0.00354522700977118,-0.0351951372916786,0.0706715905311282));
#76045=CARTESIAN_POINT('Origin',(0.00809048848650377,-0.0352875122426966,
0.0744889700069903));
#76046=CARTESIAN_POINT('Origin',(0.0137225858292214,-0.0298325076521994,
0.0691551438332945));
#76047=CARTESIAN_POINT('Origin',(0.00384922868754202,-0.0338732835503703,
0.0669405297094214));
#76048=CARTESIAN_POINT('Ctrl Pts',(0.00658393265112485,-0.0321934096636942,
0.0686086103608062));
#76049=CARTESIAN_POINT('Ctrl Pts',(0.00648474441538785,-0.0320508460843686,
0.0686361729343328));
#76050=CARTESIAN_POINT('Ctrl Pts',(0.00638637151987351,-0.0319086045661796,
0.068666379717769));
#76051=CARTESIAN_POINT('Ctrl Pts',(0.00628902042419258,-0.0317669892865994,
0.0686991482327426));
#76052=CARTESIAN_POINT('Ctrl Pts',(0.00650365324717335,-0.0321934096636942,
0.0686328105659513));
#76053=CARTESIAN_POINT('Ctrl Pts',(0.00640489818358434,-0.0320508460843686,
0.0686618101025796));
#76054=CARTESIAN_POINT('Ctrl Pts',(0.00630699674196796,-0.0319086045661796,
0.0686934411271617));
#76055=CARTESIAN_POINT('Ctrl Pts',(0.00621015411434681,-0.0317669892865994,
0.068727618178255));
#76056=CARTESIAN_POINT('Ctrl Pts',(0.00642337384322185,-0.0321934096636942,
0.0686570107710964));
#76057=CARTESIAN_POINT('Ctrl Pts',(0.00632505195178082,-0.0320508460843686,
0.0686874472708264));
#76058=CARTESIAN_POINT('Ctrl Pts',(0.0062276219640624,-0.0319086045661796,
0.0687205025365546));
#76059=CARTESIAN_POINT('Ctrl Pts',(0.00613128780450104,-0.0317669892865994,
0.0687560881237672));
#76060=CARTESIAN_POINT('Ctrl Pts',(0.00634309443927034,-0.0321934096636942,
0.0686812109762414));
#76061=CARTESIAN_POINT('Ctrl Pts',(0.0062452057199773,-0.0320508460843686,
0.0687130844390733));
#76062=CARTESIAN_POINT('Ctrl Pts',(0.00614824718615683,-0.0319086045661796,
0.0687475639459472));
#76063=CARTESIAN_POINT('Ctrl Pts',(0.00605242149465527,-0.0317669892865994,
0.0687845580692796));
#76064=CARTESIAN_POINT('',(0.00634453065367179,-0.0321934096636942,0.0686807780297913));
#76065=CARTESIAN_POINT('',(0.00612133224141135,-0.0318665617511261,0.0687584956477846));
#76066=CARTESIAN_POINT('Origin',(0.0109256371654381,-0.0326371944421567,
0.0847503569909728));
#76067=CARTESIAN_POINT('Origin',(0.00230497730286294,-0.0316939261509612,
0.058483135554525));
#76068=CARTESIAN_POINT('',(0.00646357948906075,-0.0320197221621857,0.0686435205305022));
#76069=CARTESIAN_POINT('Ctrl Pts',(0.00646339462907598,-0.0320197392094775,
0.068643526985331));
#76070=CARTESIAN_POINT('Ctrl Pts',(0.00643537593764299,-0.0319792716576073,
0.0686519756159989));
#76071=CARTESIAN_POINT('Ctrl Pts',(0.00640729410342048,-0.0319386439829724,
0.0686606763112761));
#76072=CARTESIAN_POINT('Ctrl Pts',(0.00637912214882976,-0.0318979099381656,
0.0686696462838884));
#76073=CARTESIAN_POINT('Ctrl Pts',(0.00635095075107656,-0.0318571766984944,
0.0686786160792031));
#76074=CARTESIAN_POINT('Ctrl Pts',(0.00632283188141053,-0.0318163871833579,
0.0686878078531429));
#76075=CARTESIAN_POINT('Ctrl Pts',(0.00629486116310049,-0.0317755399638302,
0.0686971866429181));
#76076=CARTESIAN_POINT('',(0.00646421107987872,-0.0321934096636183,0.0686447003968781));
#76077=CARTESIAN_POINT('Origin',(0.00577732083413186,-0.032411512718906,
0.0664390070771916));
#76078=CARTESIAN_POINT('',(0.00640437086678525,-0.0321934096636663,0.0686627392133447));
#76079=CARTESIAN_POINT('Ctrl Pts',(0.00634631772202925,-0.0321934096636618,
0.0686817372347041));
#76080=CARTESIAN_POINT('Ctrl Pts',(0.00627090611678108,-0.0320835708272592,
0.0687062498550351));
#76081=CARTESIAN_POINT('Ctrl Pts',(0.00619604554073242,-0.0319739230346489,
0.0687323088963013));
#76082=CARTESIAN_POINT('Ctrl Pts',(0.00612182921398835,-0.0318646057455573,
0.0687598736670035));
#76083=CARTESIAN_POINT('Ctrl Pts',(0.00624647239931037,-0.0321934096636618,
0.0686281454788485));
#76084=CARTESIAN_POINT('Ctrl Pts',(0.00617032172198197,-0.0320835708272592,
0.0686540350439947));
#76085=CARTESIAN_POINT('Ctrl Pts',(0.00609475099834633,-0.0319739230346489,
0.0686814855264505));
#76086=CARTESIAN_POINT('Ctrl Pts',(0.00601985422046366,-0.0318646057455573,
0.0687104543847327));
#76087=CARTESIAN_POINT('Ctrl Pts',(0.00614662707659148,-0.0321934096636618,
0.0685745537229929));
#76088=CARTESIAN_POINT('Ctrl Pts',(0.00606973732718286,-0.0320835708272592,
0.0686018202329543));
#76089=CARTESIAN_POINT('Ctrl Pts',(0.00599345645596023,-0.0319739230346489,
0.0686306621565996));
#76090=CARTESIAN_POINT('Ctrl Pts',(0.00591787922693896,-0.0318646057455573,
0.0686610351024619));
#76091=CARTESIAN_POINT('Ctrl Pts',(0.00604678175387259,-0.0321934096636618,
0.0685209619671374));
#76092=CARTESIAN_POINT('Ctrl Pts',(0.00596915293238375,-0.0320835708272592,
0.0685496054219139));
#76093=CARTESIAN_POINT('Ctrl Pts',(0.00589216191357413,-0.0319739230346489,
0.0685798387867487));
#76094=CARTESIAN_POINT('Ctrl Pts',(0.00581590423341427,-0.0318646057455573,
0.0686116158201911));
#76095=CARTESIAN_POINT('',(0.00603476276665501,-0.0321763980308453,0.0685254113205008));
#76096=CARTESIAN_POINT('',(0.00604678175384193,-0.0321934096636184,0.0685209619671487));
#76097=CARTESIAN_POINT('Origin',(0.0112170931696844,-0.032638623146326,
0.0842406758194546));
#76098=CARTESIAN_POINT('Ctrl Pts',(0.00603476276775469,-0.0321763980306276,
0.0685254113234703));
#76099=CARTESIAN_POINT('Ctrl Pts',(0.00604970583476894,-0.0321259596174849,
0.0685656448438009));
#76100=CARTESIAN_POINT('Ctrl Pts',(0.00606438999376357,-0.0320749164631446,
0.0686051812661828));
#76101=CARTESIAN_POINT('Ctrl Pts',(0.00609325231302661,-0.0319716057793892,
0.0686828917326989));
#76102=CARTESIAN_POINT('Ctrl Pts',(0.00610741922756306,-0.0319193786690082,
0.0687210354982171));
#76103=CARTESIAN_POINT('Ctrl Pts',(0.00612133224205194,-0.0318665617525264,
0.068758495649521));
#76104=CARTESIAN_POINT('',(0.00619565620376686,-0.0321934096636664,0.06860086999848));
#76105=CARTESIAN_POINT('Origin',(0.00812378219310841,-0.0315241814719618,
0.07415));
#76106=CARTESIAN_POINT('',(0.00603476276652569,-0.0322104233323623,0.0685254113201528));
#76107=CARTESIAN_POINT('',(0.00602275330948016,-0.0321934096636183,0.0685298863329836));
#76108=CARTESIAN_POINT('Origin',(0.011261375913722,-0.0326387234006215,
0.0842309679557854));
#76109=CARTESIAN_POINT('Origin',(0.0123673288377802,-0.0326386243116258,
0.0838134712769871));
#76110=CARTESIAN_POINT('Origin',(0.0123274431598962,-0.0326387243621781,
0.0838350188156792));
#76111=CARTESIAN_POINT('Ctrl Pts',(0.00627316950654523,-0.0327445246967097,
0.0687045103356693));
#76112=CARTESIAN_POINT('Ctrl Pts',(0.00606778950634687,-0.032443687833936,
0.0687743073341694));
#76113=CARTESIAN_POINT('Ctrl Pts',(0.00586825036422881,-0.0321434074405927,
0.0688593761077817));
#76114=CARTESIAN_POINT('Ctrl Pts',(0.00603826925914547,-0.0327445246967097,
0.0687900782839417));
#76115=CARTESIAN_POINT('Ctrl Pts',(0.00583611650687456,-0.032443687833936,
0.0688687346901042));
#76116=CARTESIAN_POINT('Ctrl Pts',(0.00564046277120741,-0.0321434074405927,
0.0689623946132334));
#76117=CARTESIAN_POINT('',(0.00600462631127269,-0.0326943950436611,0.0688032904185394));
#76118=CARTESIAN_POINT('',(0.0057867482592627,-0.0323666188837389,0.0688948694219787));
#76119=CARTESIAN_POINT('Origin',(0.0122694182553645,-0.0326395579111418,
0.0844033045251258));
#76120=CARTESIAN_POINT('Origin',(0.00129882962827823,-0.0321933825602991,
0.0588031917507565));
#76121=CARTESIAN_POINT('',(0.00590151528279517,-0.0321934096532688,0.0688453176555126));
#76122=CARTESIAN_POINT('',(0.00584440778819952,-0.0321934096584275,0.0688707141987171));
#76123=CARTESIAN_POINT('',(0.00612133224107911,-0.0325210109756238,0.0687584956468886));
#76124=CARTESIAN_POINT('Origin',(0.0118137036797941,-0.0326393129158326,
0.0845566298508461));
#76125=CARTESIAN_POINT('',(0.00612180524213315,-0.0326943950436593,0.0687597691804743));
#76126=CARTESIAN_POINT('Origin',(0.00227019204011562,-0.0326943765538122,
0.0583894754321644));
#76127=CARTESIAN_POINT('',(0.00606321577671292,-0.0326943950436702,0.0687815297995169));
#76128=CARTESIAN_POINT('Ctrl Pts',(0.006256833647866,-0.0325229783203769,
0.068447851007783));
#76129=CARTESIAN_POINT('Ctrl Pts',(0.00617822964870606,-0.032413025309245,
0.0684735868526517));
#76130=CARTESIAN_POINT('Ctrl Pts',(0.00610016995039386,-0.0323031222208069,
0.0685009448188719));
#76131=CARTESIAN_POINT('Ctrl Pts',(0.00602275330527986,-0.0321934096576658,
0.0685298863345538));
#76132=CARTESIAN_POINT('Ctrl Pts',(0.00621184141320569,-0.0325229783203769,
0.0685518550512456));
#76133=CARTESIAN_POINT('Ctrl Pts',(0.00613467110751046,-0.032413025309245,
0.0685782111130852));
#76134=CARTESIAN_POINT('Ctrl Pts',(0.00605805771520003,-0.0323031222208069,
0.0686061595444171));
#76135=CARTESIAN_POINT('Ctrl Pts',(0.00598209810932082,-0.0321934096576658,
0.0686356610823807));
#76136=CARTESIAN_POINT('Ctrl Pts',(0.00616684917854538,-0.0325229783203769,
0.0686558590947081));
#76137=CARTESIAN_POINT('Ctrl Pts',(0.00609111256631486,-0.032413025309245,
0.0686828353735186));
#76138=CARTESIAN_POINT('Ctrl Pts',(0.00601594548000621,-0.0323031222208069,
0.0687113742699624));
#76139=CARTESIAN_POINT('Ctrl Pts',(0.00594144291336179,-0.0321934096576658,
0.0687414358302075));
#76140=CARTESIAN_POINT('Ctrl Pts',(0.00612185694388507,-0.0325229783203769,
0.0687598631381707));
#76141=CARTESIAN_POINT('Ctrl Pts',(0.00604755402511927,-0.032413025309245,
0.0687874596339521));
#76142=CARTESIAN_POINT('Ctrl Pts',(0.00597383324481239,-0.0323031222208069,
0.0688165889955077));
#76143=CARTESIAN_POINT('Ctrl Pts',(0.00590078771740276,-0.0321934096576658,
0.0688472105780344));
#76144=CARTESIAN_POINT('',(0.00596213429654121,-0.0321934096584274,0.0686876019939325));
#76145=CARTESIAN_POINT('Ctrl Pts',(0.00603476276773177,-0.0322104233328937,
0.0685254113234084));
#76146=CARTESIAN_POINT('Ctrl Pts',(0.00604972608283879,-0.0322609421831202,
0.0685656993607969));
#76147=CARTESIAN_POINT('Ctrl Pts',(0.00606442013335418,-0.0323120888240375,
0.0686052624156628));
#76148=CARTESIAN_POINT('Ctrl Pts',(0.00609328267115004,-0.0324156524631816,
0.0686829734705684));
#76149=CARTESIAN_POINT('Ctrl Pts',(0.00610743929439966,-0.0324680267167313,
0.068721089527251));
#76150=CARTESIAN_POINT('Ctrl Pts',(0.00612133224109001,-0.0325210109755912,
0.0687584956469308));
#76151=CARTESIAN_POINT('Origin',(0.0157756005763264,-0.0262834582512467,
0.0723188633945439));
#76152=CARTESIAN_POINT('Origin',(0.00943677067931257,-0.0342770989687757,
0.0620627815514928));
#76153=CARTESIAN_POINT('Ctrl Pts',(0.0060064696347242,-0.0326943950436604,
0.0688041353146785));
#76154=CARTESIAN_POINT('Ctrl Pts',(0.00593279360014221,-0.0325844576448134,
0.0688333158499997));
#76155=CARTESIAN_POINT('Ctrl Pts',(0.00585971585270536,-0.0324744968375322,
0.0688640221916614));
#76156=CARTESIAN_POINT('Ctrl Pts',(0.00578732948123054,-0.0323646534831894,
0.0688962137054484));
#76157=CARTESIAN_POINT('Ctrl Pts',(0.0059034564288931,-0.0326943950436604,
0.0687569187179587));
#76158=CARTESIAN_POINT('Ctrl Pts',(0.00582912966111497,-0.0325844576448134,
0.0687875189683235));
#76159=CARTESIAN_POINT('Ctrl Pts',(0.00575543049646335,-0.0324744968375322,
0.0688196585837337));
#76160=CARTESIAN_POINT('Ctrl Pts',(0.0056824527946217,-0.0323646534831894,
0.0688532950825982));
#76161=CARTESIAN_POINT('Ctrl Pts',(0.00580044322306199,-0.0326943950436604,
0.0687097021212388));
#76162=CARTESIAN_POINT('Ctrl Pts',(0.00572546572208774,-0.0325844576448134,
0.0687417220866473));
#76163=CARTESIAN_POINT('Ctrl Pts',(0.00565114514022135,-0.0324744968375322,
0.068775294975806));
#76164=CARTESIAN_POINT('Ctrl Pts',(0.00557757610801285,-0.0323646534831894,
0.068810376459748));
#76165=CARTESIAN_POINT('Ctrl Pts',(0.00569743001723089,-0.0326943950436604,
0.0686624855245189));
#76166=CARTESIAN_POINT('Ctrl Pts',(0.0056218017830605,-0.0325844576448134,
0.0686959252049712));
#76167=CARTESIAN_POINT('Ctrl Pts',(0.00554685978397934,-0.0324744968375322,
0.0687309313678783));
#76168=CARTESIAN_POINT('Ctrl Pts',(0.00547269942140401,-0.0323646534831894,
0.0687674578368979));
#76169=CARTESIAN_POINT('',(0.00568571412389441,-0.0326773559991155,0.0686676807763526));
#76170=CARTESIAN_POINT('',(0.00569743001723023,-0.0326943950436594,0.0686624855245192));
#76171=CARTESIAN_POINT('Origin',(0.0124790316359852,-0.0326395670859815,
0.0838197150605463));
#76172=CARTESIAN_POINT('Ctrl Pts',(0.0056857141252513,-0.0326773559987418,
0.0686676807794101));
#76173=CARTESIAN_POINT('Ctrl Pts',(0.00570316802359972,-0.0326267922586007,
0.0687069281833901));
#76174=CARTESIAN_POINT('Ctrl Pts',(0.00572031256420384,-0.0325756109579419,
0.068745479955476));
#76175=CARTESIAN_POINT('Ctrl Pts',(0.00575399752078182,-0.0324719985462368,
0.0688212250453391));
#76176=CARTESIAN_POINT('Ctrl Pts',(0.00577052442663532,-0.0324196091621779,
0.0688583879838198));
#76177=CARTESIAN_POINT('Ctrl Pts',(0.00578674825928252,-0.0323666188837756,
0.0688948694220232));
#76178=CARTESIAN_POINT('',(0.00585102816426146,-0.0326943950436702,0.0687328879715393));
#76179=CARTESIAN_POINT('Origin',(0.00812378219310841,-0.0315241814719618,
0.07415));
#76180=CARTESIAN_POINT('',(0.00568571412391236,-0.0327114338379881,0.0686676807763931));
#76181=CARTESIAN_POINT('',(0.00567400935308163,-0.0326943950436593,0.0686729010386623));
#76182=CARTESIAN_POINT('Origin',(0.0125201122070344,-0.0326395669401792,
0.0838005981465262));
#76183=CARTESIAN_POINT('Origin',(0.0123872216574439,-0.0326395679064938,
0.0838605466837996));
#76184=CARTESIAN_POINT('Origin',(0.0123455098264391,-0.0326395678140561,
0.0838782439513655));
#76185=CARTESIAN_POINT('Ctrl Pts',(0.00593485987093565,-0.0332451089994433,
0.0688314716257697));
#76186=CARTESIAN_POINT('Ctrl Pts',(0.00573426829145138,-0.0329451141710254,
0.0689140281818464));
#76187=CARTESIAN_POINT('Ctrl Pts',(0.00554046506877148,-0.0326442513127493,
0.0690114595812519));
#76188=CARTESIAN_POINT('Ctrl Pts',(0.00570579668445249,-0.0332451089994433,
0.068931621796005));
#76189=CARTESIAN_POINT('Ctrl Pts',(0.00550898233043731,-0.0329451141710254,
0.0690228176115056));
#76190=CARTESIAN_POINT('Ctrl Pts',(0.00531959634686495,-0.0326442513127493,
0.0691285792110471));
#76191=CARTESIAN_POINT('Ctrl Pts',(0.00570350605258766,-0.0332451089994433,
0.0689326232977073));
#76192=CARTESIAN_POINT('Ctrl Pts',(0.00550672947082717,-0.0329451141710254,
0.0690239055058022));
#76193=CARTESIAN_POINT('Ctrl Pts',(0.00531738765964588,-0.0326442513127493,
0.0691297504073451));
#76194=CARTESIAN_POINT('',(0.00567308530893743,-0.0331951640388616,0.0689469038273432));
#76195=CARTESIAN_POINT('',(0.00546138746752985,-0.0328677532354987,0.0690519827976921));
#76196=CARTESIAN_POINT('Origin',(0.0135036309031346,-0.0326402808279522,
0.0837696837008342));
#76197=CARTESIAN_POINT('Origin',(0.00034307225992035,-0.0326944278779019,
0.0592521240019454));
#76198=CARTESIAN_POINT('',(0.00557281665257838,-0.0326943950436593,0.0689953225308435));
#76199=CARTESIAN_POINT('',(0.00551741651134116,-0.0326943950436694,0.0690242547680603));
#76200=CARTESIAN_POINT('',(0.00578674825926528,-0.0330220786163545,0.0688948694219775));
#76201=CARTESIAN_POINT('Origin',(0.0130929182019664,-0.032639668276383,
0.0840196191375121));
#76202=CARTESIAN_POINT('',(0.00578730029279678,-0.0331951640388587,0.068896110742553));
#76203=CARTESIAN_POINT('Origin',(0.00130464766631461,-0.0331952026560022,
0.0588162697243794));
#76204=CARTESIAN_POINT('',(0.0057301928008771,-0.0331951640388701,0.0689215072849581));
#76205=CARTESIAN_POINT('Ctrl Pts',(0.00590247585408771,-0.0330240426238172,
0.0685763299211161));
#76206=CARTESIAN_POINT('Ctrl Pts',(0.00582569311858744,-0.0329142774063519,
0.06860693058005));
#76207=CARTESIAN_POINT('Ctrl Pts',(0.00574950470519212,-0.0328043479726691,
0.0686391338081532));
#76208=CARTESIAN_POINT('Ctrl Pts',(0.00567400935308162,-0.0326943950436593,
0.0686729010386623));
#76209=CARTESIAN_POINT('Ctrl Pts',(0.00586410289566394,-0.0330240426238172,
0.0686829538023354));
#76210=CARTESIAN_POINT('Ctrl Pts',(0.00578878900800608,-0.0329142774063519,
0.0687140830861565));
#76211=CARTESIAN_POINT('Ctrl Pts',(0.00571408110288044,-0.0328043479726691,
0.0687467848374978));
#76212=CARTESIAN_POINT('Ctrl Pts',(0.00564007604041373,-0.0326943950436593,
0.0687810197987173));
#76213=CARTESIAN_POINT('Ctrl Pts',(0.00582572993724016,-0.0330240426238172,
0.0687895776835547));
#76214=CARTESIAN_POINT('Ctrl Pts',(0.00575188489742471,-0.0329142774063519,
0.068821235592263));
#76215=CARTESIAN_POINT('Ctrl Pts',(0.00567865750056877,-0.0328043479726691,
0.0688544358668425));
#76216=CARTESIAN_POINT('Ctrl Pts',(0.00560614272774585,-0.0326943950436593,
0.0688891385587724));
#76217=CARTESIAN_POINT('Ctrl Pts',(0.00578735697881639,-0.0330240426238172,
0.068896201564774));
#76218=CARTESIAN_POINT('Ctrl Pts',(0.00571498078684335,-0.0329142774063519,
0.0689283880983696));
#76219=CARTESIAN_POINT('Ctrl Pts',(0.00564323389825709,-0.0328043479726691,
0.0689620868961871));
#76220=CARTESIAN_POINT('Ctrl Pts',(0.00557220941507797,-0.0326943950436593,
0.0689972573188274));
#76221=CARTESIAN_POINT('',(0.00562341300284001,-0.0326943950436694,0.0688341117847629));
#76222=CARTESIAN_POINT('Ctrl Pts',(0.00568571412525445,-0.0327114338383335,
0.068667680779417));
#76223=CARTESIAN_POINT('Ctrl Pts',(0.00570316512044694,-0.0327619876830919,
0.068706921655266));
#76224=CARTESIAN_POINT('Ctrl Pts',(0.00572030824301397,-0.0328131562604212,
0.0687454702387077));
#76225=CARTESIAN_POINT('Ctrl Pts',(0.00575399316865828,-0.0329167375858774,
0.0688212152590123));
#76226=CARTESIAN_POINT('Ctrl Pts',(0.00577052154991993,-0.0329691088920632,
0.0688583815151439));
#76227=CARTESIAN_POINT('Ctrl Pts',(0.00578674825928208,-0.0330220786163186,
0.0688948694220221));
#76228=CARTESIAN_POINT('Ctrl Pts',(0.00567497834865205,-0.0331951640388604,
0.0689476314291769));
#76229=CARTESIAN_POINT('Ctrl Pts',(0.00556742271389869,-0.033030642201062,
0.068998258878634));
#76230=CARTESIAN_POINT('Ctrl Pts',(0.00546205147040875,-0.0328657861914645,
0.0690532884547829));
#76231=CARTESIAN_POINT('Ctrl Pts',(0.00567308530894032,-0.0331951640388604,
0.0689469038273419));
#76232=CARTESIAN_POINT('Ctrl Pts',(0.00556551463148551,-0.033030642201062,
0.0689975704141814));
#76233=CARTESIAN_POINT('Ctrl Pts',(0.00546012997573719,-0.0328657861914645,
0.0690526397160007));
#76234=CARTESIAN_POINT('Ctrl Pts',(0.00535765398416284,-0.0331951640388604,
0.0688256657945171));
#76235=CARTESIAN_POINT('Ctrl Pts',(0.00524757678810997,-0.033030642201062,
0.0688828537217605));
#76236=CARTESIAN_POINT('Ctrl Pts',(0.00513995728942306,-0.0328657861914645,
0.0689445423885937));
#76237=CARTESIAN_POINT('',(0.00534628742199613,-0.0331781648281888,0.0688315864402821));
#76238=CARTESIAN_POINT('',(0.00535765398416181,-0.0331951640388588,0.0688256657945176));
#76239=CARTESIAN_POINT('Origin',(0.0136189663352319,-0.0326412092601028,
0.0831336584167454));
#76240=CARTESIAN_POINT('Ctrl Pts',(0.00534628742381383,-0.033178164828644,
0.0688315864405209));
#76241=CARTESIAN_POINT('Ctrl Pts',(0.00536618494568857,-0.0331276811546781,
0.0688696866661652));
#76242=CARTESIAN_POINT('Ctrl Pts',(0.00538572320991325,-0.033076566349779,
0.0689070989040707));
#76243=CARTESIAN_POINT('Ctrl Pts',(0.00542409786612605,-0.0329730614463308,
0.0689805796231364));
#76244=CARTESIAN_POINT('Ctrl Pts',(0.00544291875083521,-0.032920713337418,
0.0690166184221636));
#76245=CARTESIAN_POINT('Ctrl Pts',(0.00546138747588533,-0.0328677532289347,
0.0690519827834986));
#76246=CARTESIAN_POINT('',(0.00551536964655962,-0.0331951640388701,0.0688862848109404));
#76247=CARTESIAN_POINT('Origin',(0.00812378219310841,-0.0315241814719618,
0.07415));
#76248=CARTESIAN_POINT('',(0.00534628742214034,-0.0332121607144428,0.0688315864419558));
#76249=CARTESIAN_POINT('',(0.00533493353088822,-0.0331951640388587,0.0688375313516922));
#76250=CARTESIAN_POINT('Origin',(0.0136549253353356,-0.0326413651674531,
0.0831060325170448));
#76251=CARTESIAN_POINT('Origin',(0.0123562593090519,-0.0326412099775407,
0.0837930984558483));
#76252=CARTESIAN_POINT('Origin',(0.01231303860202,-0.0326413661134083,0.0838068188101578));
#76253=CARTESIAN_POINT('Ctrl Pts',(0.00557414628843926,-0.0336938721132646,
0.0689946281401935));
#76254=CARTESIAN_POINT('Ctrl Pts',(0.00546622319260924,-0.0335278710435224,
0.069048002485935));
#76255=CARTESIAN_POINT('Ctrl Pts',(0.00536001186947911,-0.0333620469224384,
0.0691047424949314));
#76256=CARTESIAN_POINT('Ctrl Pts',(0.00525546893502409,-0.0331951640388587,
0.0691648940520025));
#76257=CARTESIAN_POINT('Ctrl Pts',(0.00549983622149611,-0.0336938721132646,
0.0690334359200156));
#76258=CARTESIAN_POINT('Ctrl Pts',(0.00539272553180373,-0.0335278710435224,
0.0690883658805011));
#76259=CARTESIAN_POINT('Ctrl Pts',(0.00528737511268256,-0.0333620469224384,
0.0691466354801345));
#76260=CARTESIAN_POINT('Ctrl Pts',(0.00518374226268052,-0.0331951640388587,
0.0692082912212457));
#76261=CARTESIAN_POINT('Ctrl Pts',(0.00542552615455296,-0.0336938721132646,
0.0690722436998376));
#76262=CARTESIAN_POINT('Ctrl Pts',(0.00531922787099822,-0.0335278710435224,
0.0691287292750671));
#76263=CARTESIAN_POINT('Ctrl Pts',(0.005214738355886,-0.0333620469224384,
0.0691885284653376));
#76264=CARTESIAN_POINT('Ctrl Pts',(0.00511201559033694,-0.0331951640388587,
0.069251688390489));
#76265=CARTESIAN_POINT('Ctrl Pts',(0.00535121608760981,-0.0336938721132646,
0.0691110514796596));
#76266=CARTESIAN_POINT('Ctrl Pts',(0.00524573021019271,-0.0335278710435224,
0.0691690926696332));
#76267=CARTESIAN_POINT('Ctrl Pts',(0.00514210159908944,-0.0333620469224384,
0.0692304214505407));
#76268=CARTESIAN_POINT('Ctrl Pts',(0.00504028891799337,-0.0331951640388587,
0.0692950855597323));
#76269=CARTESIAN_POINT('',(0.00535121608757554,-0.0336938721132548,0.0691110514796784));
#76270=CARTESIAN_POINT('',(0.00514653394508866,-0.0333679846208662,0.069229215691045));
#76271=CARTESIAN_POINT('Ctrl Pts',(0.00535121608758644,-0.033693872113239,
0.0691110514796663));
#76272=CARTESIAN_POINT('Ctrl Pts',(0.00533154670769848,-0.0336629187933851,
0.0691218741058165));
#76273=CARTESIAN_POINT('Ctrl Pts',(0.00531194698936719,-0.033631995230099,
0.0691328084427585));
#76274=CARTESIAN_POINT('Ctrl Pts',(0.00524341592934891,-0.0335235892595403,
0.069171568059534));
#76275=CARTESIAN_POINT('Ctrl Pts',(0.00519477652140877,-0.0334458668645711,
0.0692000272619926));
#76276=CARTESIAN_POINT('Ctrl Pts',(0.00514653395765004,-0.0333679869902153,
0.0692292157118869));
#76277=CARTESIAN_POINT('Ctrl Pts',(0.00514653356476184,-0.0333679128829488,
0.0692292150600056));
#76278=CARTESIAN_POINT('Ctrl Pts',(0.0051467682263833,-0.0333391359256866,
0.0692296029078199));
#76279=CARTESIAN_POINT('Ctrl Pts',(0.00514694409275441,-0.0333103578181726,
0.0692298935790735));
#76280=CARTESIAN_POINT('Ctrl Pts',(0.00514706131756792,-0.0332815781851601,
0.0692300873277904));
#76281=CARTESIAN_POINT('Ctrl Pts',(0.00514717864297711,-0.0332527738550986,
0.0692302812427714));
#76282=CARTESIAN_POINT('Ctrl Pts',(0.00514723722102821,-0.0332239691713941,
0.06923037806034));
#76283=CARTESIAN_POINT('Ctrl Pts',(0.00514723722102868,-0.0331951640388599,
0.0692303780603397));
#76284=CARTESIAN_POINT('',(0.00525418552406561,-0.0331951640388587,0.0691656705609461));
#76285=CARTESIAN_POINT('',(0.00520071137255754,-0.0331951640388687,0.0691980243106526));
#76286=CARTESIAN_POINT('',(0.00546138748282756,-0.0335216366559765,0.0690519827968478));
#76287=CARTESIAN_POINT('Origin',(0.0142239882975866,-0.0326434571528019,
0.0832148741677039));
#76288=CARTESIAN_POINT('',(0.00546201637008394,-0.0336938721132327,0.0690531870052572));
#76289=CARTESIAN_POINT('Origin',(0.000406713303217545,-0.0336938867896339,
0.0593731693981297));
#76290=CARTESIAN_POINT('',(0.00540661622883974,-0.0336938721132538,0.0690821192424778));
#76291=CARTESIAN_POINT('Ctrl Pts',(0.00555688458612558,-0.0335235895815172,
0.0687268056760533));
#76292=CARTESIAN_POINT('Ctrl Pts',(0.00548222363896938,-0.0334144449262748,
0.0687621440753697));
#76293=CARTESIAN_POINT('Ctrl Pts',(0.0054082069801651,-0.0333049234473147,
0.0687990655132052));
#76294=CARTESIAN_POINT('Ctrl Pts',(0.00533493353088825,-0.0331951640388587,
0.0688375313516921));
#76295=CARTESIAN_POINT('Ctrl Pts',(0.0055252822893815,-0.0335235895815172,
0.0688356287771228));
#76296=CARTESIAN_POINT('Ctrl Pts',(0.0054521195064645,-0.0334144449262748,
0.0688714022442731));
#76297=CARTESIAN_POINT('Ctrl Pts',(0.00537961172128263,-0.0333049234473147,
0.0689087282988371));
#76298=CARTESIAN_POINT('Ctrl Pts',(0.00530785597249189,-0.0331951640388587,
0.0689475676107942));
#76299=CARTESIAN_POINT('Ctrl Pts',(0.00549367999263743,-0.0335235895815172,
0.0689444518781923));
#76300=CARTESIAN_POINT('Ctrl Pts',(0.00542201537395962,-0.0334144449262748,
0.0689806604131765));
#76301=CARTESIAN_POINT('Ctrl Pts',(0.00535101646240017,-0.0333049234473147,
0.0690183910844689));
#76302=CARTESIAN_POINT('Ctrl Pts',(0.00528077841409552,-0.0331951640388587,
0.0690576038698963));
#76303=CARTESIAN_POINT('Ctrl Pts',(0.00546207769589335,-0.0335235895815172,
0.0690532749792618));
#76304=CARTESIAN_POINT('Ctrl Pts',(0.00539191124145473,-0.0334144449262748,
0.0690899185820799));
#76305=CARTESIAN_POINT('Ctrl Pts',(0.0053224212035177,-0.0333049234473147,
0.0691280538701008));
#76306=CARTESIAN_POINT('Ctrl Pts',(0.00525370085569916,-0.0331951640388587,
0.0691676401289984));
#76307=CARTESIAN_POINT('',(0.00529455952748692,-0.0331951640388687,0.0690016009563292));
#76308=CARTESIAN_POINT('Ctrl Pts',(0.00534628742358526,-0.0332121607145988,
0.0688315864447267));
#76309=CARTESIAN_POINT('Ctrl Pts',(0.00536615146201264,-0.0332625444109202,
0.0688696225816059));
#76310=CARTESIAN_POINT('Ctrl Pts',(0.00538567321188656,-0.0333135300745695,
0.068907003296159));
#76311=CARTESIAN_POINT('Ctrl Pts',(0.00542404666424387,-0.0334167177151536,
0.068980481702462));
#76312=CARTESIAN_POINT('Ctrl Pts',(0.00544288636915261,-0.0334688874167339,
0.0690165564209686));
#76313=CARTESIAN_POINT('Ctrl Pts',(0.00546138748300939,-0.0335216366556671,
0.0690519827972136));
#76314=CARTESIAN_POINT('Ctrl Pts',(0.00535121608759359,-0.033693872113239,
0.0691110514796686));
#76315=CARTESIAN_POINT('Ctrl Pts',(0.00532172144980367,-0.0336474569764958,
0.0691272802291192));
#76316=CARTESIAN_POINT('Ctrl Pts',(0.00529241881100787,-0.033601104548885,
0.0691438531385406));
#76317=CARTESIAN_POINT('Ctrl Pts',(0.00521823126667602,-0.0334837508592656,
0.0691858119348449));
#76318=CARTESIAN_POINT('Ctrl Pts',(0.00514531962617555,-0.0333660264659097,
0.0692299506366928));
#76319=CARTESIAN_POINT('Ctrl Pts',(0.00502686006645084,-0.033693872113239,
0.0690092516229594));
#76320=CARTESIAN_POINT('Ctrl Pts',(0.00499676956031882,-0.0336474569764958,
0.0690273789358345));
#76321=CARTESIAN_POINT('Ctrl Pts',(0.00496689331909221,-0.033601104548885,
0.0690458572539809));
#76322=CARTESIAN_POINT('Ctrl Pts',(0.00489125354528501,-0.0334837508592655,
0.0690926401070958));
#76323=CARTESIAN_POINT('Ctrl Pts',(0.00481703325982658,-0.0333660264659097,
0.0691416437799547));
#76324=CARTESIAN_POINT('',(0.00501782222224344,-0.0336769361243753,0.069016481454267));
#76325=CARTESIAN_POINT('',(0.00502879459541034,-0.0336938721132327,0.0690098587791681));
#76326=CARTESIAN_POINT('Ctrl Pts',(0.00501782222224317,-0.033676936124375,
0.0690164814542672));
#76327=CARTESIAN_POINT('Ctrl Pts',(0.005019649909106,-0.0336797586669845,
0.0690153756391845));
#76328=CARTESIAN_POINT('Ctrl Pts',(0.00502147811739939,-0.0336825812712485,
0.0690142708419912));
#76329=CARTESIAN_POINT('Ctrl Pts',(0.00502513558148546,-0.0336882266105785,
0.0690120632799841));
#76330=CARTESIAN_POINT('Ctrl Pts',(0.00502696483725222,-0.03369104934558,
0.0690109605152117));
#76331=CARTESIAN_POINT('Ctrl Pts',(0.00502879459541793,-0.0336938721132295,
0.0690098587791725));
#76332=CARTESIAN_POINT('Ctrl Pts',(0.00501782222224345,-0.0336769361243754,
0.0690164814542671));
#76333=CARTESIAN_POINT('Ctrl Pts',(0.00503951824392448,-0.0336279031301476,
0.0690523405544207));
#76334=CARTESIAN_POINT('Ctrl Pts',(0.00506152641722645,-0.0335767851899352,
0.0690887155775568));
#76335=CARTESIAN_POINT('Ctrl Pts',(0.00510465089668413,-0.0334733198857318,
0.0691599915492846));
#76336=CARTESIAN_POINT('Ctrl Pts',(0.00512579615833764,-0.0334209645014078,
0.0691949403554103));
#76337=CARTESIAN_POINT('Ctrl Pts',(0.00514653396172319,-0.0333679869844681,
0.0692292157160962));
#76338=CARTESIAN_POINT('',(0.00519000534150295,-0.0336938721132538,0.0690604551294333));
#76339=CARTESIAN_POINT('Origin',(0.00812378219310841,-0.0315241814719618,
0.07415));
#76340=CARTESIAN_POINT('',(0.00501782222292022,-0.0337108120655555,0.0690164814553829));
#76341=CARTESIAN_POINT('',(0.00500686402026081,-0.0336938721132327,0.069023127551441));
#76342=CARTESIAN_POINT('Origin',(0.0125311601701808,-0.0345562516250795,
0.083593453341771));
#76343=CARTESIAN_POINT('Ctrl Pts',(0.00500686402026099,-0.0336938721132306,
0.0690231275514468));
#76344=CARTESIAN_POINT('Ctrl Pts',(0.0050086890615784,-0.0336910493355375,
0.0690220180047386));
#76345=CARTESIAN_POINT('Ctrl Pts',(0.00501051477127385,-0.0336882266055569,
0.0690209093863788));
#76346=CARTESIAN_POINT('Ctrl Pts',(0.00501416750820236,-0.0336825812712406,
0.0690186940186733));
#76347=CARTESIAN_POINT('Ctrl Pts',(0.00501599453538342,-0.0336797586669805,
0.069017587269348));
#76348=CARTESIAN_POINT('Ctrl Pts',(0.0050178222222437,-0.033676936124375,
0.0690164814542668));
#76349=CARTESIAN_POINT('Origin',(0.0144435748101146,-0.0345562517443326,
0.082436372141593));
#76350=CARTESIAN_POINT('Ctrl Pts',(0.00528559484861555,-0.034243627687391,
0.0691477187606492));
#76351=CARTESIAN_POINT('Ctrl Pts',(0.00509693070150552,-0.033943005420181,
0.0692547627609895));
#76352=CARTESIAN_POINT('Ctrl Pts',(0.00491686552216361,-0.0336441434784052,
0.0693757136171344));
#76353=CARTESIAN_POINT('Ctrl Pts',(0.00507088842474626,-0.034243627687391,
0.0692757857413635));
#76354=CARTESIAN_POINT('Ctrl Pts',(0.0048870544034395,-0.033943005420181,
0.0693909275279737));
#76355=CARTESIAN_POINT('Ctrl Pts',(0.00471241558646132,-0.0336441434784052,
0.0695195893405603));
#76356=CARTESIAN_POINT('Ctrl Pts',(0.00506874136050757,-0.034243627687391,
0.0692770664111706));
#76357=CARTESIAN_POINT('Ctrl Pts',(0.00488495564045884,-0.033943005420181,
0.0693922891756435));
#76358=CARTESIAN_POINT('Ctrl Pts',(0.0047103710871043,-0.0336441434784052,
0.0695210280977945));
#76359=CARTESIAN_POINT('',(0.00504028891799333,-0.0341934961088741,0.0692950855597322));
#76360=CARTESIAN_POINT('',(0.00484343027595112,-0.03386642128919,0.069425868724495));
#76361=CARTESIAN_POINT('Origin',(0.0135780139220781,-0.034561081807594,
0.0836881514620321));
#76362=CARTESIAN_POINT('Origin',(-0.00141135814116461,-0.0336938005044317,
0.0604182960296151));
#76363=CARTESIAN_POINT('',(0.00494687938261151,-0.0336938721132327,0.0693556894622211));
#76364=CARTESIAN_POINT('',(0.00489554225887861,-0.0336938721132427,0.0693913370389483));
#76365=CARTESIAN_POINT('',(0.00514653396172778,-0.0340203938281605,0.0692292157160934));
#76366=CARTESIAN_POINT('Origin',(0.01313127844728,-0.0345589643244171,0.0838668999249553));
#76367=CARTESIAN_POINT('',(0.00514723722102949,-0.034193496108874,0.0692303780603392));
#76368=CARTESIAN_POINT('Origin',(-0.000557089076279621,-0.0341934220717597,
0.0598022881300443));
#76369=CARTESIAN_POINT('',(0.00509376306952142,-0.0341934961088841,0.0692627318100457));
#76370=CARTESIAN_POINT('Ctrl Pts',(0.00522142697788282,-0.0340223579322396,
0.0688986826219814));
#76371=CARTESIAN_POINT('Ctrl Pts',(0.00514899761522924,-0.0339125849573574,
0.0689387136700595));
#76372=CARTESIAN_POINT('Ctrl Pts',(0.00507744769752613,-0.0338030433565231,
0.068980215708288));
#76373=CARTESIAN_POINT('Ctrl Pts',(0.00500686402026092,-0.0336938721132326,
0.0690231275514403));
#76374=CARTESIAN_POINT('Ctrl Pts',(0.00519672004260572,-0.0340223579322396,
0.0690092753305091));
#76375=CARTESIAN_POINT('Ctrl Pts',(0.00512581604184064,-0.0339125849573574,
0.0690496471516631));
#76376=CARTESIAN_POINT('Ctrl Pts',(0.00505579746738269,-0.0338030433565231,
0.0690914581520635));
#76377=CARTESIAN_POINT('Ctrl Pts',(0.00498674912136458,-0.0336938721132326,
0.069134646924971));
#76378=CARTESIAN_POINT('Ctrl Pts',(0.00517201310732862,-0.0340223579322397,
0.0691198680390369));
#76379=CARTESIAN_POINT('Ctrl Pts',(0.00510263446845203,-0.0339125849573575,
0.0691605806332668));
#76380=CARTESIAN_POINT('Ctrl Pts',(0.00503414723723926,-0.0338030433565231,
0.0692027005958391));
#76381=CARTESIAN_POINT('Ctrl Pts',(0.00496663422246824,-0.0336938721132327,
0.0692461662985017));
#76382=CARTESIAN_POINT('Ctrl Pts',(0.00514730617205152,-0.0340223579322397,
0.0692304607475647));
#76383=CARTESIAN_POINT('Ctrl Pts',(0.00507945289506342,-0.0339125849573575,
0.0692715141148704));
#76384=CARTESIAN_POINT('Ctrl Pts',(0.00501249700709583,-0.0338030433565231,
0.0693139430396147));
#76385=CARTESIAN_POINT('Ctrl Pts',(0.00494651932357189,-0.0336938721132327,
0.0693576856720325));
#76386=CARTESIAN_POINT('',(0.00497687170144616,-0.0336938721132427,0.0691894085068411));
#76387=CARTESIAN_POINT('Ctrl Pts',(0.00501782222478039,-0.0337108120662696,
0.0690164814584599));
#76388=CARTESIAN_POINT('Ctrl Pts',(0.00504008121951515,-0.0337611408994269,
0.0690532710382845));
#76389=CARTESIAN_POINT('Ctrl Pts',(0.00506193403697947,-0.0338121088781246,
0.0690893892898982));
#76390=CARTESIAN_POINT('Ctrl Pts',(0.0051048472249419,-0.0339153382773238,
0.0691603160398654));
#76391=CARTESIAN_POINT('Ctrl Pts',(0.0051258894405293,-0.0339675558473111,
0.0691950945318533));
#76392=CARTESIAN_POINT('Ctrl Pts',(0.0051465339617439,-0.0340203938281304,
0.0692292157161303));
#76393=CARTESIAN_POINT('Ctrl Pts',(0.00504225831159741,-0.0341934961088741,
0.0692955701851708));
#76394=CARTESIAN_POINT('Ctrl Pts',(0.00494189680028251,-0.03402875161944,
0.0693592782632969));
#76395=CARTESIAN_POINT('Ctrl Pts',(0.00484425414914076,-0.033864463329982,
0.0694270799214622));
#76396=CARTESIAN_POINT('Ctrl Pts',(0.00504028891799343,-0.0341934961088741,
0.0692950855597323));
#76397=CARTESIAN_POINT('Ctrl Pts',(0.00493991738742946,-0.03402875161944,
0.0693588343535194));
#76398=CARTESIAN_POINT('Ctrl Pts',(0.00484226640840904,-0.033864463329982,
0.069426677106658));
#76399=CARTESIAN_POINT('Ctrl Pts',(0.00471214970874164,-0.0341934961088741,
0.0692143375529102));
#76400=CARTESIAN_POINT('Ctrl Pts',(0.00461010877676299,-0.03402875161944,
0.0692848703662873));
#76401=CARTESIAN_POINT('Ctrl Pts',(0.00451107021147381,-0.033864463329982,
0.0693595603398275));
#76402=CARTESIAN_POINT('',(0.00470161482939921,-0.0341764758832377,0.0692216361208511));
#76403=CARTESIAN_POINT('',(0.00471214970874166,-0.034193496108874,0.0692143375529101));
#76404=CARTESIAN_POINT('Origin',(0.0137248784044839,-0.0345621026793295,
0.0831141536822559));
#76405=CARTESIAN_POINT('Ctrl Pts',(0.00470161483120347,-0.034176475883746,
0.069221636120644));
#76406=CARTESIAN_POINT('Ctrl Pts',(0.0047260972430818,-0.0341260050043381,
0.0692568939380233));
#76407=CARTESIAN_POINT('Ctrl Pts',(0.00475015412427072,-0.0340749269154154,
0.0692915388695708));
#76408=CARTESIAN_POINT('Ctrl Pts',(0.00479743531893986,-0.0339715436318372,
0.0693596299158009));
#76409=CARTESIAN_POINT('Ctrl Pts',(0.00482064169003878,-0.0339192778253278,
0.0693930502016218));
#76410=CARTESIAN_POINT('Ctrl Pts',(0.00484343027765033,-0.0338664212874711,
0.0694258687205468));
#76411=CARTESIAN_POINT('',(0.0048762193133775,-0.0341934961088841,0.0692547115563312));
#76412=CARTESIAN_POINT('Origin',(0.00812378219310841,-0.0315241814719618,
0.07415));
#76413=CARTESIAN_POINT('',(0.00470161482912772,-0.034210518019055,0.0692216361219359));
#76414=CARTESIAN_POINT('',(0.00469109556167716,-0.0341934961088739,0.069228957174499));
#76415=CARTESIAN_POINT('Origin',(0.0137648456250437,-0.034562170836886,
0.0830927724808212));
#76416=CARTESIAN_POINT('Origin',(0.014566150630993,-0.034562103658163,0.0825299917182353));
#76417=CARTESIAN_POINT('Origin',(0.0145321507033199,-0.0345621718255471,
0.0825599665698366));
#76418=CARTESIAN_POINT('Ctrl Pts',(0.00494811148172171,-0.0346945769586965,
0.0693548339147276));
#76419=CARTESIAN_POINT('Ctrl Pts',(0.00484767480818592,-0.0345275153362944,
0.0694213496092468));
#76420=CARTESIAN_POINT('Ctrl Pts',(0.00474930401395107,-0.0343603235965185,
0.0694910411490686));
#76421=CARTESIAN_POINT('Ctrl Pts',(0.00465328697272945,-0.034193496108874,
0.0695636980934709));
#76422=CARTESIAN_POINT('Ctrl Pts',(0.004879251283527,-0.0346945769586965,
0.0694026491996313));
#76423=CARTESIAN_POINT('Ctrl Pts',(0.00477981612027772,-0.0345275153362944,
0.0694706071985718));
#76424=CARTESIAN_POINT('Ctrl Pts',(0.00468249245451773,-0.0343603235965185,
0.0695417099192921));
#76425=CARTESIAN_POINT('Ctrl Pts',(0.00458756500098687,-0.034193496108874,
0.0696157427934518));
#76426=CARTESIAN_POINT('Ctrl Pts',(0.00481039108533224,-0.0346945769586965,
0.0694504644845362));
#76427=CARTESIAN_POINT('Ctrl Pts',(0.00471195743236938,-0.0345275153362944,
0.0695198647878973));
#76428=CARTESIAN_POINT('Ctrl Pts',(0.00461568089508422,-0.0343603235965185,
0.0695923786895156));
#76429=CARTESIAN_POINT('Ctrl Pts',(0.00452184302924412,-0.034193496108874,
0.0696677874934326));
#76430=CARTESIAN_POINT('Ctrl Pts',(0.00474153088713759,-0.0346945769586965,
0.0694982797694387));
#76431=CARTESIAN_POINT('Ctrl Pts',(0.00464409874446132,-0.0345275153362944,
0.0695691223772218));
#76432=CARTESIAN_POINT('Ctrl Pts',(0.00454886933565105,-0.0343603235965185,
0.0696430474597389));
#76433=CARTESIAN_POINT('Ctrl Pts',(0.00445612105750169,-0.034193496108874,
0.0697198321934136));
#76434=CARTESIAN_POINT('',(0.00474153088763531,-0.0346945769586966,0.0694982797690933));
#76435=CARTESIAN_POINT('',(0.00455327264714076,-0.0343667727831427,0.0696411657180134));
#76436=CARTESIAN_POINT('Origin',(0.0147766509948415,-0.0345626457065548,
0.0829887805624754));
#76437=CARTESIAN_POINT('Origin',(-0.00230804983714372,-0.0341934771028877,
0.0609767033420708));
#76438=CARTESIAN_POINT('',(0.0046521110251616,-0.034193496108874,0.0695646293168766));
#76439=CARTESIAN_POINT('',(0.00460311353337759,-0.034193496108884,0.0696034300359251));
#76440=CARTESIAN_POINT('',(0.00484343027935788,-0.0345211942962721,0.069425868723066));
#76441=CARTESIAN_POINT('Origin',(0.0143798191940824,-0.0345625596120614,
0.0832602862009375));
#76442=CARTESIAN_POINT('',(0.00484420513512573,-0.0346945769586885,0.0694269846156556));
#76443=CARTESIAN_POINT('Origin',(-0.00146602387291882,-0.0346945685853955,
0.0603394368119114));
#76444=CARTESIAN_POINT('',(0.00479286801139052,-0.0346945769587026,0.0694626321923844));
#76445=CARTESIAN_POINT('Ctrl Pts',(0.00489742035531189,-0.0345231616327842,
0.0690912858064888));
#76446=CARTESIAN_POINT('Ctrl Pts',(0.00482769310225423,-0.0344132092796988,
0.0691357566620687));
#76447=CARTESIAN_POINT('Ctrl Pts',(0.00475888929137185,-0.0343032738558979,
0.0691816674763862));
#76448=CARTESIAN_POINT('Ctrl Pts',(0.00469109556167711,-0.0341934961088739,
0.069228957174499));
#76449=CARTESIAN_POINT('Ctrl Pts',(0.00487970639523689,-0.0345231616327842,
0.0692032114592987));
#76450=CARTESIAN_POINT('Ctrl Pts',(0.0048115218797245,-0.0344132092796988,
0.069247926476879));
#76451=CARTESIAN_POINT('Ctrl Pts',(0.00474426577708761,-0.0343032738558979,
0.0692940495302901));
#76452=CARTESIAN_POINT('Ctrl Pts',(0.00467802273658055,-0.0341934961088739,
0.0693415193234766));
#76453=CARTESIAN_POINT('Ctrl Pts',(0.00486199243516188,-0.0345231616327842,
0.0693151371121086));
#76454=CARTESIAN_POINT('Ctrl Pts',(0.00479535065719477,-0.0344132092796988,
0.0693600962916893));
#76455=CARTESIAN_POINT('Ctrl Pts',(0.00472964226280337,-0.0343032738558979,
0.0694064315841939));
#76456=CARTESIAN_POINT('Ctrl Pts',(0.004664949911484,-0.0341934961088739,
0.0694540814724543));
#76457=CARTESIAN_POINT('Ctrl Pts',(0.00484427847508689,-0.0345231616327842,
0.0694270627649186));
#76458=CARTESIAN_POINT('Ctrl Pts',(0.00477917943466504,-0.0344132092796988,
0.0694722661064996));
#76459=CARTESIAN_POINT('Ctrl Pts',(0.00471501874851913,-0.0343032738558979,
0.0695188136380977));
#76460=CARTESIAN_POINT('Ctrl Pts',(0.00465187708638745,-0.0341934961088739,
0.0695666436214319));
#76461=CARTESIAN_POINT('',(0.00467160329342937,-0.0341934961088839,0.0693967932456977));
#76462=CARTESIAN_POINT('Ctrl Pts',(0.00470161483109297,-0.0342105180195399,
0.0692216361247682));
#76463=CARTESIAN_POINT('Ctrl Pts',(0.00472612475480663,-0.0342610556241199,
0.0692569335868257));
#76464=CARTESIAN_POINT('Ctrl Pts',(0.00475019486061234,-0.0343122189869934,
0.0692915976541774));
#76465=CARTESIAN_POINT('Ctrl Pts',(0.00479747653581031,-0.0344158119695211,
0.0693596893853396));
#76466=CARTESIAN_POINT('Ctrl Pts',(0.00482066876663529,-0.0344681990450118,
0.0693930891991104));
#76467=CARTESIAN_POINT('Ctrl Pts',(0.00484343027936789,-0.0345211942962545,
0.0694258687230875));
#76468=CARTESIAN_POINT('Ctrl Pts',(0.0047435263384397,-0.0346945769586932,
0.0694986396912232));
#76469=CARTESIAN_POINT('Ctrl Pts',(0.00464736275525272,-0.034529677707698,
0.0695685240892262));
#76470=CARTESIAN_POINT('Ctrl Pts',(0.0045541697290336,-0.0343648066251421,
0.0696423233011442));
#76471=CARTESIAN_POINT('Ctrl Pts',(0.00474153088764269,-0.0346945769586932,
0.0694982797690881));
#76472=CARTESIAN_POINT('Ctrl Pts',(0.00464535986332024,-0.034529677707698,
0.0695682054216243));
#76473=CARTESIAN_POINT('Ctrl Pts',(0.00455216110741178,-0.0343648066251421,
0.069642046160373));
#76474=CARTESIAN_POINT('Ctrl Pts',(0.00440896897686485,-0.0346945769586932,
0.0694382951314389));
#76475=CARTESIAN_POINT('Ctrl Pts',(0.00431155781260277,-0.034529677707698,
0.0695150962661672));
#76476=CARTESIAN_POINT('Ctrl Pts',(0.00421740414643578,-0.0343648066251421,
0.0695958578682178));
#76477=CARTESIAN_POINT('',(0.00439891316634542,-0.0346775396664962,0.0694462407877545));
#76478=CARTESIAN_POINT('',(0.00440896897686213,-0.0346945769586886,0.0694382951314411));
#76479=CARTESIAN_POINT('Origin',(0.014824661290163,-0.0345626618061633,
0.0823658646068263));
#76480=CARTESIAN_POINT('Ctrl Pts',(0.00439891316814823,-0.0346775396670097,
0.0694462407875334));
#76481=CARTESIAN_POINT('Ctrl Pts',(0.00442558211322793,-0.0346269749930482,
0.0694799182719924));
#76482=CARTESIAN_POINT('Ctrl Pts',(0.00445177711982146,-0.0345757902895592,
0.0695129972101099));
#76483=CARTESIAN_POINT('Ctrl Pts',(0.00450323940186589,-0.0344721707114263,
0.069577983711416));
#76484=CARTESIAN_POINT('Ctrl Pts',(0.00452849032766865,-0.0344197687642437,
0.0696098706373707));
#76485=CARTESIAN_POINT('Ctrl Pts',(0.00455327264725885,-0.0343667727830579,
0.0696411657177762));
#76486=CARTESIAN_POINT('',(0.00457524993225872,-0.0346945769587026,0.0694682874502772));
#76487=CARTESIAN_POINT('Origin',(0.00812378219310841,-0.0315241814719618,
0.07415));
#76488=CARTESIAN_POINT('',(0.00439891316649769,-0.0347116136489807,0.0694462407891372));
#76489=CARTESIAN_POINT('',(0.00438887434898241,-0.0346945769586885,0.0694542079053786));
#76490=CARTESIAN_POINT('Origin',(0.0148589946893147,-0.0345626686843321,
0.0823362930815001));
#76491=CARTESIAN_POINT('Origin',(0.0145852157278249,-0.0345626627999594,
0.0825554825893273));
#76492=CARTESIAN_POINT('Origin',(0.0145485596705449,-0.0345626696657839,
0.0825821210917095));
#76493=CARTESIAN_POINT('Ctrl Pts',(0.00468294913655636,-0.0352450361874068,
0.0695413743369022));
#76494=CARTESIAN_POINT('Ctrl Pts',(0.00450913196746544,-0.0349452760959492,
0.0696711474851085));
#76495=CARTESIAN_POINT('Ctrl Pts',(0.00434558363916616,-0.034644428984174,
0.0698136445818391));
#76496=CARTESIAN_POINT('Ctrl Pts',(0.00468095983803887,-0.0352450361874068,
0.0695429294305999));
#76497=CARTESIAN_POINT('Ctrl Pts',(0.00450720132026919,-0.0349452760959492,
0.0696727776064309));
#76498=CARTESIAN_POINT('Ctrl Pts',(0.00434371712805659,-0.034644428984174,
0.0698153450997831));
#76499=CARTESIAN_POINT('Ctrl Pts',(0.004483999588783,-0.0352450361874068,
0.0696968991036301));
#76500=CARTESIAN_POINT('Ctrl Pts',(0.0043160481325211,-0.0349452760959492,
0.0698341757571574));
#76501=CARTESIAN_POINT('Ctrl Pts',(0.00415891404790077,-0.034644428984174,
0.0699837132130496));
#76502=CARTESIAN_POINT('Ctrl Pts',(0.00448202998629044,-0.0352450361874068,
0.0696984388003605));
#76503=CARTESIAN_POINT('Ctrl Pts',(0.00431413660064362,-0.0349452760959492,
0.0698357897386648));
#76504=CARTESIAN_POINT('Ctrl Pts',(0.00415706601709922,-0.034644428984174,
0.0699853968941822));
#76505=CARTESIAN_POINT('',(0.00445614446971457,-0.035195163405328,0.0697198097295415));
#76506=CARTESIAN_POINT('',(0.0042772061852535,-0.0348678972925388,0.0698742570217802));
#76507=CARTESIAN_POINT('Origin',(0.0157928575127484,-0.034563676789046,
0.0820439094430579));
#76508=CARTESIAN_POINT('Origin',(-0.00311305772362403,-0.0346946199341114,
0.0616594540075098));
#76509=CARTESIAN_POINT('',(0.00437104378151317,-0.0346945769330288,0.0697916655231541));
#76510=CARTESIAN_POINT('',(0.00432457928567719,-0.0346945769458128,0.069833466261357));
#76511=CARTESIAN_POINT('',(0.00455327264733022,-0.0350221583435276,0.0696411657178925));
#76512=CARTESIAN_POINT('Origin',(0.0154645130411218,-0.0345628458717289,
0.0823950978543954));
#76513=CARTESIAN_POINT('',(0.00455404289067444,-0.035195136029876,0.0696421335081262));
#76514=CARTESIAN_POINT('Origin',(-0.00228666599125885,-0.0351951838366893,
0.0610036992822474));
#76515=CARTESIAN_POINT('',(0.00445612105791295,-0.035195137132875,0.0697198321929397));
#76516=CARTESIAN_POINT('Ctrl Pts',(0.00458614677508542,-0.0350241211494343,
0.0693038535258235));
#76517=CARTESIAN_POINT('Ctrl Pts',(0.00451939309440105,-0.0349144232818962,
0.0693525830032198));
#76518=CARTESIAN_POINT('Ctrl Pts',(0.00445360673153917,-0.0348045283579412,
0.0694027214938365));
#76519=CARTESIAN_POINT('Ctrl Pts',(0.00438887434028513,-0.0346945769439157,
0.0694542079122961));
#76520=CARTESIAN_POINT('Ctrl Pts',(0.0045754956550678,-0.0350241211494343,
0.069416670614269));
#76521=CARTESIAN_POINT('Ctrl Pts',(0.00451029598351996,-0.0349144232818962,
0.0694655468064763));
#76522=CARTESIAN_POINT('Ctrl Pts',(0.00444606759264397,-0.0348045283579412,
0.0695157999772407));
#76523=CARTESIAN_POINT('Ctrl Pts',(0.00438289514612716,-0.0346945769439157,
0.0695673688200344));
#76524=CARTESIAN_POINT('Ctrl Pts',(0.00456484453505019,-0.0350241211494343,
0.0695294877027144));
#76525=CARTESIAN_POINT('Ctrl Pts',(0.00450119887263888,-0.0349144232818962,
0.0695785106097329));
#76526=CARTESIAN_POINT('Ctrl Pts',(0.00443852845374877,-0.0348045283579412,
0.069628878460645));
#76527=CARTESIAN_POINT('Ctrl Pts',(0.0043769159519692,-0.0346945769439157,
0.0696805297277726));
#76528=CARTESIAN_POINT('Ctrl Pts',(0.00455419341503258,-0.0350241211494343,
0.0696423047911598));
#76529=CARTESIAN_POINT('Ctrl Pts',(0.00449210176175779,-0.0349144232818962,
0.0696914744129894));
#76530=CARTESIAN_POINT('Ctrl Pts',(0.00443098931485357,-0.0348045283579412,
0.0697419569440492));
#76531=CARTESIAN_POINT('Ctrl Pts',(0.00437093675781124,-0.0346945769439157,
0.0697936906355109));
#76532=CARTESIAN_POINT('',(0.00437995906542026,-0.0346945769458128,0.0696229367140174));
#76533=CARTESIAN_POINT('Ctrl Pts',(0.00439891316853388,-0.0347116136492803,
0.0694462407917096));
#76534=CARTESIAN_POINT('Ctrl Pts',(0.00442557151280757,-0.0347621546532191,
0.0694799049102405));
#76535=CARTESIAN_POINT('Ctrl Pts',(0.00445176113135062,-0.0348133084096798,
0.0695129771225977));
#76536=CARTESIAN_POINT('Ctrl Pts',(0.00450322477402094,-0.0349168561544572,
0.0695779653360103));
#76537=CARTESIAN_POINT('Ctrl Pts',(0.00452847838511639,-0.0349692089015925,
0.0696098555595186));
#76538=CARTESIAN_POINT('Ctrl Pts',(0.00455327264733732,-0.0350221583435,
0.0696411657179335));
#76539=CARTESIAN_POINT('Ctrl Pts',(0.00445757430726783,-0.0351951371254893,
0.0697200009715545));
#76540=CARTESIAN_POINT('Ctrl Pts',(0.00436598685682996,-0.0350307338980916,
0.0697957975193377));
#76541=CARTESIAN_POINT('Ctrl Pts',(0.00427761042043704,-0.0348659306897796,
0.0698753147075681));
#76542=CARTESIAN_POINT('Ctrl Pts',(0.00445612105798853,-0.0351951371254893,
0.069719832193028));
#76543=CARTESIAN_POINT('Ctrl Pts',(0.00436453011816052,-0.0350307338980916,
0.0697956587858282));
#76544=CARTESIAN_POINT('Ctrl Pts',(0.0042761514371521,-0.0348659306897796,
0.0698752061376226));
#76545=CARTESIAN_POINT('Ctrl Pts',(0.00421255496412829,-0.0351951371254893,
0.0696915447360682));
#76546=CARTESIAN_POINT('Ctrl Pts',(0.00412037919887578,-0.0350307338980916,
0.0697724069050406));
#76547=CARTESIAN_POINT('Ctrl Pts',(0.00403162431796947,-0.0348659306897796,
0.0698570097016025));
#76548=CARTESIAN_POINT('Origin',(0.000720343904793222,-0.0308609197410131,
0.0659205514694643));
#76549=CARTESIAN_POINT('',(0.0043499317327492,-0.0351951371254893,0.0697074994995907));
#76550=CARTESIAN_POINT('Origin',(0.00887563923730569,-0.0351840467441134,
0.0747740646081582));
#76551=CARTESIAN_POINT('Origin',(-0.000451870359554896,-0.035232261333163,
0.0658057740145225));
#76552=CARTESIAN_POINT('',(0.00410458066883951,-0.0351951142564652,0.0700361412650968));
#76553=CARTESIAN_POINT('',(0.00401729059133434,-0.0351951372916786,0.0701251737025606));
#76554=CARTESIAN_POINT('Origin',(0.00804826481983064,-0.0352875123221079,
0.0744821219329415));
#76555=CARTESIAN_POINT('Origin',(0.0143044590648397,-0.0298325076521956,
0.0698962459298664));
#76556=CARTESIAN_POINT('Origin',(0.00478655016906604,-0.0338732271129292,
0.0664614842499923));
#76557=CARTESIAN_POINT('Ctrl Pts',(0.00729059510661384,-0.0321934096636941,
0.0684593115509448));
#76558=CARTESIAN_POINT('Ctrl Pts',(0.00718873449328596,-0.0320508460843821,
0.0684742252030288));
#76559=CARTESIAN_POINT('Ctrl Pts',(0.00708735138360126,-0.0319086045662065,
0.0684918644038634));
#76560=CARTESIAN_POINT('Ctrl Pts',(0.00698666094645583,-0.0317669892866397,
0.0685121732016937));
#76561=CARTESIAN_POINT('Ctrl Pts',(0.00720791563977711,-0.0321934096636941,
0.0684732592529581));
#76562=CARTESIAN_POINT('Ctrl Pts',(0.00710630468367337,-0.0320508460843821,
0.0684896528281265));
#76563=CARTESIAN_POINT('Ctrl Pts',(0.0070052108055836,-0.0319086045662065,
0.0685087641283815));
#76564=CARTESIAN_POINT('Ctrl Pts',(0.00690484829068893,-0.0317669892866397,
0.0685305340835495));
#76565=CARTESIAN_POINT('Ctrl Pts',(0.00712523617294039,-0.0321934096636941,
0.0684872069549715));
#76566=CARTESIAN_POINT('Ctrl Pts',(0.00702387487406078,-0.0320508460843821,
0.0685050804532242));
#76567=CARTESIAN_POINT('Ctrl Pts',(0.00692307022756595,-0.0319086045662065,
0.0685256638528998));
#76568=CARTESIAN_POINT('Ctrl Pts',(0.00682303563492204,-0.0317669892866397,
0.0685488949654052));
#76569=CARTESIAN_POINT('Ctrl Pts',(0.00704255670610367,-0.0321934096636941,
0.0685011546569848));
#76570=CARTESIAN_POINT('Ctrl Pts',(0.00694144506444819,-0.0320508460843821,
0.0685205080783219));
#76571=CARTESIAN_POINT('Ctrl Pts',(0.00684092964954828,-0.0319086045662065,
0.068542563577418));
#76572=CARTESIAN_POINT('Ctrl Pts',(0.00674122297915514,-0.0317669892866397,
0.0685672558472609));
#76573=CARTESIAN_POINT('',(0.00704403585810413,-0.0321934096636941,0.068500905129842));
#76574=CARTESIAN_POINT('',(0.00681285683162341,-0.0318665617511264,0.0685500357424682));
#76575=CARTESIAN_POINT('Origin',(0.00957496668345433,-0.0326371944421322,
0.0850179355532371));
#76576=CARTESIAN_POINT('Origin',(0.00431443910331527,-0.0316939261509309,
0.0578773838241723));
#76577=CARTESIAN_POINT('',(0.00716681556072824,-0.0320197221621859,0.0684788621925544));
#76578=CARTESIAN_POINT('Ctrl Pts',(0.00716663134941515,-0.0320197392094778,
0.0684788454273853));
#76579=CARTESIAN_POINT('Ctrl Pts',(0.00713777469953208,-0.0319792716576075,
0.0684837157648794));
#76580=CARTESIAN_POINT('Ctrl Pts',(0.00710882381268693,-0.0319386439829729,
0.0684888282654879));
#76581=CARTESIAN_POINT('Ctrl Pts',(0.00707974976670056,-0.0318979099381661,
0.0684941966250222));
#76582=CARTESIAN_POINT('Ctrl Pts',(0.00705067629538211,-0.0318571766984948,
0.0684995648784473));
#76583=CARTESIAN_POINT('Ctrl Pts',(0.00702162711665199,-0.0318163871833584,
0.0685051599436445));
#76584=CARTESIAN_POINT('Ctrl Pts',(0.0069927014817602,-0.0317755399638303,
0.0685109591182903));
#76585=CARTESIAN_POINT('',(0.0071672942947959,-0.0321934096636183,0.068480111914651));
#76586=CARTESIAN_POINT('Origin',(0.00676376797449013,-0.0324103422814711,
0.0662141487655565));
#76587=CARTESIAN_POINT('',(0.00710566507646001,-0.0321934096636663,0.0684905085222565));
#76588=CARTESIAN_POINT('Ctrl Pts',(0.00704568861464045,-0.0321934096636618,
0.0685020807501934));
#76589=CARTESIAN_POINT('Ctrl Pts',(0.0069677994064548,-0.0320835708272592,
0.0685169485008574));
#76590=CARTESIAN_POINT('Ctrl Pts',(0.00689026306450258,-0.0319739230346488,
0.0685334195407371));
#76591=CARTESIAN_POINT('Ctrl Pts',(0.00681317717381767,-0.0318646057455572,
0.068551465182775));
#76592=CARTESIAN_POINT('Ctrl Pts',(0.0069533474301673,-0.0321934096636618,
0.0684363976441872));
#76593=CARTESIAN_POINT('Ctrl Pts',(0.0068745524007594,-0.0320835708272592,
0.0684525388517516));
#76594=CARTESIAN_POINT('Ctrl Pts',(0.00679613711712243,-0.0319739230346488,
0.0684703013557981));
#76595=CARTESIAN_POINT('Ctrl Pts',(0.00671820016202277,-0.0318646057455572,
0.0684896547306246));
#76596=CARTESIAN_POINT('Ctrl Pts',(0.00686100624569415,-0.0321934096636618,
0.068370714538181));
#76597=CARTESIAN_POINT('Ctrl Pts',(0.00678130539506401,-0.0320835708272592,
0.0683881292026458));
#76598=CARTESIAN_POINT('Ctrl Pts',(0.00670201116974227,-0.0319739230346488,
0.068407183170859));
#76599=CARTESIAN_POINT('Ctrl Pts',(0.00662322315022787,-0.0318646057455572,
0.0684278442784741));
#76600=CARTESIAN_POINT('Ctrl Pts',(0.006768665061221,-0.0321934096636618,
0.0683050314321747));
#76601=CARTESIAN_POINT('Ctrl Pts',(0.00668805838936861,-0.0320835708272592,
0.06832371955354));
#76602=CARTESIAN_POINT('Ctrl Pts',(0.00660788522236212,-0.0319739230346488,
0.06834406498592));
#76603=CARTESIAN_POINT('Ctrl Pts',(0.00652824613843297,-0.0318646057455572,
0.0683660338263237));
#76604=CARTESIAN_POINT('',(0.00675618319546388,-0.0321763980308454,0.0683079393225251));
#76605=CARTESIAN_POINT('',(0.00676866506118924,-0.0321934096636184,0.0683050314321821));
#76606=CARTESIAN_POINT('Origin',(0.00992800456953099,-0.0326386231073049,
0.0845488027386375));
#76607=CARTESIAN_POINT('Ctrl Pts',(0.00675618319618208,-0.0321763980306277,
0.0683079393256096));
#76608=CARTESIAN_POINT('Ctrl Pts',(0.00676596583544919,-0.0321259596174836,
0.0683497284555247));
#76609=CARTESIAN_POINT('Ctrl Pts',(0.00677557897780387,-0.0320749164631413,
0.0683907935345376));
#76610=CARTESIAN_POINT('Ctrl Pts',(0.00679447400500781,-0.03197160577939,
0.0684715086386123));
#76611=CARTESIAN_POINT('Ctrl Pts',(0.00680374852771889,-0.0319193786690096,
0.0685111272143545));
#76612=CARTESIAN_POINT('Ctrl Pts',(0.00681285683204034,-0.0318665617525269,
0.0685500357442718));
#76613=CARTESIAN_POINT('',(0.00690635045965669,-0.0321934096636663,0.0684029682810221));
#76614=CARTESIAN_POINT('Origin',(0.00812378219310841,-0.0315241814719618,
0.07415));
#76615=CARTESIAN_POINT('',(0.00675618319537921,-0.0322104233323793,0.0683079393221637));
#76616=CARTESIAN_POINT('',(0.00674370756866053,-0.0321934096636183,0.0683108738640975));
#76617=CARTESIAN_POINT('Origin',(0.00997315455773778,-0.0326387235070079,
0.0845447211264128));
#76618=CARTESIAN_POINT('Origin',(0.0111227131009451,-0.0326386242831274,
0.084269129501095));
#76619=CARTESIAN_POINT('Origin',(0.0110804413412371,-0.0326387243911324,
0.084285507925658));
#76620=CARTESIAN_POINT('Ctrl Pts',(0.00697026296830151,-0.0327445246967097,
0.0685155063760795));
#76621=CARTESIAN_POINT('Ctrl Pts',(0.00675775456723365,-0.032443687833936,
0.0685590120648648));
#76622=CARTESIAN_POINT('Ctrl Pts',(0.00654912690637849,-0.0321434074405927,
0.0686184011598839));
#76623=CARTESIAN_POINT('Ctrl Pts',(0.00672649047186738,-0.0327445246967097,
0.06857095878795));
#76624=CARTESIAN_POINT('Ctrl Pts',(0.00651607349270334,-0.032443687833936,
0.0686236585067403));
#76625=CARTESIAN_POINT('Ctrl Pts',(0.00631022384415969,-0.0321434074405927,
0.0686920579780508));
#76626=CARTESIAN_POINT('',(0.00669145688913583,-0.0326943950436612,0.0685798501614767));
#76627=CARTESIAN_POINT('',(0.00646381897801533,-0.0323666188837389,0.0686433996763394));
#76628=CARTESIAN_POINT('Origin',(0.0109516488654873,-0.0326395579113589,
0.0848420401288825));
#76629=CARTESIAN_POINT('Origin',(0.0032761114381671,-0.032193382560307,
0.0580688125701116));
#76630=CARTESIAN_POINT('',(0.00658389151240922,-0.0321934096532689,0.0686086227625171));
#76631=CARTESIAN_POINT('',(0.00652405129658461,-0.0321934096584275,0.0686266615794344));
#76632=CARTESIAN_POINT('',(0.00681285683140512,-0.0325210109756239,0.0685500357415387));
#76633=CARTESIAN_POINT('Origin',(0.0104803109773102,-0.0326393129157746,
0.0849370402584136));
#76634=CARTESIAN_POINT('',(0.00681316648662225,-0.0326943950436593,0.0685513585156833));
#76635=CARTESIAN_POINT('Origin',(0.00429166690332564,-0.0326943765538226,
0.0577801024812186));
#76636=CARTESIAN_POINT('',(0.00675231168788904,-0.0326943950436702,0.0685656043385901));
#76637=CARTESIAN_POINT('Ctrl Pts',(0.00698622386623576,-0.0325229783203769,
0.0682588234576625));
#76638=CARTESIAN_POINT('Ctrl Pts',(0.00690501412643116,-0.032413025309245,
0.0682745046743217));
#76639=CARTESIAN_POINT('Ctrl Pts',(0.00682414108978533,-0.032303122220807,
0.0682918634404063));
#76640=CARTESIAN_POINT('Ctrl Pts',(0.0067437075642966,-0.0321934096576658,
0.0683108738651289));
#76641=CARTESIAN_POINT('Ctrl Pts',(0.00692855124571332,-0.0325229783203769,
0.0683563683759227));
#76642=CARTESIAN_POINT('Ctrl Pts',(0.00684868616047378,-0.032413025309245,
0.0683728446083945));
#76643=CARTESIAN_POINT('Ctrl Pts',(0.00676917402037314,-0.032303122220807,
0.0683909704538051));
#76644=CARTESIAN_POINT('Ctrl Pts',(0.00669011585552622,-0.0321934096576658,
0.068410719100305));
#76645=CARTESIAN_POINT('Ctrl Pts',(0.00687087862519088,-0.0325229783203769,
0.0684539132941828));
#76646=CARTESIAN_POINT('Ctrl Pts',(0.00679235819451639,-0.032413025309245,
0.0684711845424674));
#76647=CARTESIAN_POINT('Ctrl Pts',(0.00671420695096094,-0.032303122220807,
0.0684900774672039));
#76648=CARTESIAN_POINT('Ctrl Pts',(0.00663652414675584,-0.0321934096576658,
0.0685105643354812));
#76649=CARTESIAN_POINT('Ctrl Pts',(0.00681320600466844,-0.0325229783203769,
0.068551458212443));
#76650=CARTESIAN_POINT('Ctrl Pts',(0.006736030228559,-0.032413025309245,
0.0685695244765402));
#76651=CARTESIAN_POINT('Ctrl Pts',(0.00665923988154875,-0.032303122220807,
0.0685891844806027));
#76652=CARTESIAN_POINT('Ctrl Pts',(0.00658293243798545,-0.0321934096576658,
0.0686104095706573));
#76653=CARTESIAN_POINT('',(0.00666379954097551,-0.0321934096584275,0.0684597483130441));
#76654=CARTESIAN_POINT('Ctrl Pts',(0.0067561831961672,-0.0322104233328939,
0.0683079393255456));
#76655=CARTESIAN_POINT('Ctrl Pts',(0.00676597909106434,-0.0322609421831152,
0.0683497850803887));
#76656=CARTESIAN_POINT('Ctrl Pts',(0.0067755987090056,-0.0323120888240273,
0.0683908778216115));
#76657=CARTESIAN_POINT('Ctrl Pts',(0.00679449387927703,-0.0324156524631819,
0.068471593536837));
#76658=CARTESIAN_POINT('Ctrl Pts',(0.00680376166468919,-0.0324680267167316,
0.0685111833323961));
#76659=CARTESIAN_POINT('Ctrl Pts',(0.00681285683141068,-0.0325210109755913,
0.0685500357415819));
#76660=CARTESIAN_POINT('Origin',(0.0159447659747408,-0.0262834582512507,
0.0732923295942242));
#76661=CARTESIAN_POINT('Origin',(0.0109413105581775,-0.0342770797690015,
0.0623227055287267));
#76662=CARTESIAN_POINT('Ctrl Pts',(0.00669317978386622,-0.0326943950436604,
0.068580919425046));
#76663=CARTESIAN_POINT('Ctrl Pts',(0.00661642741597393,-0.0325844576448134,
0.0686006358074801));
#76664=CARTESIAN_POINT('Ctrl Pts',(0.00654007738331149,-0.0324744968375322,
0.0686219409500783));
#76665=CARTESIAN_POINT('Ctrl Pts',(0.00646422713348024,-0.0323646534831894,
0.0686448062061611));
#76666=CARTESIAN_POINT('Ctrl Pts',(0.00659689667667646,-0.0326943950436604,
0.0685211641671075));
#76667=CARTESIAN_POINT('Ctrl Pts',(0.00651932076933648,-0.0325844576448134,
0.0685422075112125));
#76668=CARTESIAN_POINT('Ctrl Pts',(0.00644217458268614,-0.0324744968375322,
0.0685648567415387));
#76669=CARTESIAN_POINT('Ctrl Pts',(0.00636555656065241,-0.0323646534831894,
0.0685890814752131));
#76670=CARTESIAN_POINT('Ctrl Pts',(0.00650061356948669,-0.0326943950436604,
0.0684614089091691));
#76671=CARTESIAN_POINT('Ctrl Pts',(0.00642221412269904,-0.0325844576448134,
0.0684837792149449));
#76672=CARTESIAN_POINT('Ctrl Pts',(0.00634427178206078,-0.0324744968375322,
0.0685077725329991));
#76673=CARTESIAN_POINT('Ctrl Pts',(0.00626688598782457,-0.0323646534831894,
0.068533356744265));
#76674=CARTESIAN_POINT('Ctrl Pts',(0.00640433046229693,-0.0326943950436604,
0.0684016536512307));
#76675=CARTESIAN_POINT('Ctrl Pts',(0.00632510747606159,-0.0325844576448134,
0.0684253509186773));
#76676=CARTESIAN_POINT('Ctrl Pts',(0.00624636898143543,-0.0324744968375322,
0.0684506883244595));
#76677=CARTESIAN_POINT('Ctrl Pts',(0.00616821541499673,-0.0323646534831894,
0.068477632013317));
#76678=CARTESIAN_POINT('',(0.0063920558145679,-0.0326773559991157,0.0684053395461553));
#76679=CARTESIAN_POINT('',(0.00640433046229621,-0.0326943950436594,0.0684016536512309));
#76680=CARTESIAN_POINT('Origin',(0.0112327526299647,-0.0326395670494284,
0.0842893241052763));
#76681=CARTESIAN_POINT('Ctrl Pts',(0.00639205581553023,-0.0326773559987419,
0.0684053395493593));
#76682=CARTESIAN_POINT('Ctrl Pts',(0.0064044530806279,-0.0326267922585978,
0.068446465029357));
#76683=CARTESIAN_POINT('Ctrl Pts',(0.00641663061315396,-0.0325756109579362,
0.0684868615899192));
#76684=CARTESIAN_POINT('Ctrl Pts',(0.00644055657674764,-0.0324719985462367,
0.0685662312516508));
#76685=CARTESIAN_POINT('Ctrl Pts',(0.00645229541176373,-0.0324196091621771,
0.0686051725198134));
#76686=CARTESIAN_POINT('Ctrl Pts',(0.00646381897802939,-0.0323666188837756,
0.0686433996763861));
#76687=CARTESIAN_POINT('',(0.00654789367572602,-0.0326943950436703,0.0684907519063639));
#76688=CARTESIAN_POINT('Origin',(0.00812378219310841,-0.0315241814719618,
0.07415));
#76689=CARTESIAN_POINT('',(0.00639205581458065,-0.0327114338379882,0.0684053395461977));
#76690=CARTESIAN_POINT('',(0.00637978906701307,-0.0326943950436593,0.0684090516483641));
#76691=CARTESIAN_POINT('Origin',(0.0112759051401613,-0.0326395669585225,
0.0842755065717678));
#76692=CARTESIAN_POINT('Origin',(0.0111365488380453,-0.0326395678495505,
0.0843183266738395));
#76693=CARTESIAN_POINT('Origin',(0.011092948081802,-0.0326395679003803,
0.0843306565853654));
#76694=CARTESIAN_POINT('Ctrl Pts',(0.00661870853619124,-0.0332451089994433,
0.0685990650979088));
#76695=CARTESIAN_POINT('Ctrl Pts',(0.00640935160109997,-0.0329451141710254,
0.0686558298795999));
#76696=CARTESIAN_POINT('Ctrl Pts',(0.0062048651823789,-0.0326442513127493,
0.0687282030187462));
#76697=CARTESIAN_POINT('Ctrl Pts',(0.00637889943667374,-0.0332451089994433,
0.0686697163242861));
#76698=CARTESIAN_POINT('Ctrl Pts',(0.00617220715618131,-0.0329451141710254,
0.0687355256541421));
#76699=CARTESIAN_POINT('Ctrl Pts',(0.00597105909439879,-0.0326442513127493,
0.0688167169341688));
#76700=CARTESIAN_POINT('',(0.00634453065372195,-0.0331951640388616,0.068680778029775));
#76701=CARTESIAN_POINT('',(0.00612133224107488,-0.0328677532092642,0.0687584956468902));
#76702=CARTESIAN_POINT('Origin',(0.0122556578473816,-0.032640190890057,
0.0843680538129557));
#76703=CARTESIAN_POINT('Origin',(0.00227198026462762,-0.0326944279134336,
0.0583942945404394));
#76704=CARTESIAN_POINT('',(0.00623898417299244,-0.0326943950436593,0.0687162479424096));
#76705=CARTESIAN_POINT('',(0.00618039470757279,-0.0326943950436693,0.068738008561452));
#76706=CARTESIAN_POINT('',(0.00646381897801807,-0.0330220786163545,0.0686433996763386));
#76707=CARTESIAN_POINT('Origin',(0.011816743799778,-0.0326396682763674,
0.0845645921266418));
#76708=CARTESIAN_POINT('',(0.0064642110798787,-0.0331951640388587,0.0686447003968781));
#76709=CARTESIAN_POINT('Origin',(0.00328024443866656,-0.0331952026560115,
0.0580825166274355));
#76710=CARTESIAN_POINT('',(0.00640437086681032,-0.0331951640388701,0.0686627392133366));
#76711=CARTESIAN_POINT('Ctrl Pts',(0.00661855761185007,-0.0330240426238172,
0.0683418764682563));
#76712=CARTESIAN_POINT('Ctrl Pts',(0.00653854505161971,-0.0329142774063519,
0.0683626124033324));
#76713=CARTESIAN_POINT('Ctrl Pts',(0.006458921271911,-0.032804347972669,
0.0683850127591524));
#76714=CARTESIAN_POINT('Ctrl Pts',(0.00637978906701304,-0.0326943950436592,
0.0684090516483641));
#76715=CARTESIAN_POINT('Ctrl Pts',(0.00656712371985652,-0.0330240426238172,
0.0684428501813645));
#76716=CARTESIAN_POINT('Ctrl Pts',(0.00648850217089816,-0.0329142774063519,
0.0684642946684124));
#76717=CARTESIAN_POINT('Ctrl Pts',(0.00641028474367978,-0.032804347972669,
0.0684873751733547));
#76718=CARTESIAN_POINT('Ctrl Pts',(0.00633257245484427,-0.0326943950436592,
0.0685120648879004));
#76719=CARTESIAN_POINT('Ctrl Pts',(0.00651568982786298,-0.0330240426238172,
0.0685438238944727));
#76720=CARTESIAN_POINT('Ctrl Pts',(0.0064384592901766,-0.0329142774063519,
0.0685659769334924));
#76721=CARTESIAN_POINT('Ctrl Pts',(0.00636164821544856,-0.032804347972669,
0.0685897375875569));
#76722=CARTESIAN_POINT('Ctrl Pts',(0.0062853558426755,-0.0326943950436592,
0.0686150781274367));
#76723=CARTESIAN_POINT('Ctrl Pts',(0.00646425593586943,-0.0330240426238172,
0.0686447976075808));
#76724=CARTESIAN_POINT('Ctrl Pts',(0.00638841640945504,-0.0329142774063519,
0.0686676591985724));
#76725=CARTESIAN_POINT('Ctrl Pts',(0.00631301168721734,-0.032804347972669,
0.0686921000017591));
#76726=CARTESIAN_POINT('Ctrl Pts',(0.00623813923050673,-0.0326943950436592,
0.068718091366973));
#76727=CARTESIAN_POINT('',(0.00630938662001275,-0.0326943950436693,0.0685626497953969));
#76728=CARTESIAN_POINT('Ctrl Pts',(0.0063920558155326,-0.0327114338383336,
0.0684053395493668));
#76729=CARTESIAN_POINT('Ctrl Pts',(0.00640445101855673,-0.0327619876830886,
0.0684464581888426));
#76730=CARTESIAN_POINT('Ctrl Pts',(0.00641662754386919,-0.0328131562604148,
0.0684868514081724));
#76731=CARTESIAN_POINT('Ctrl Pts',(0.00644055348549382,-0.0329167375858771,
0.0685662209970261));
#76732=CARTESIAN_POINT('Ctrl Pts',(0.00645229336847186,-0.0329691088920623,
0.0686051657415956));
#76733=CARTESIAN_POINT('Ctrl Pts',(0.00646381897802911,-0.0330220786163187,
0.0686433996763849));
#76734=CARTESIAN_POINT('Ctrl Pts',(0.00634631757358637,-0.0331951640388604,
0.0686817371550525));
#76735=CARTESIAN_POINT('Ctrl Pts',(0.00627100330633363,-0.0330855618127442,
0.0687062181372552));
#76736=CARTESIAN_POINT('Ctrl Pts',(0.00619614072618659,-0.032975722417194,
0.0687322733848046));
#76737=CARTESIAN_POINT('Ctrl Pts',(0.00612182733583426,-0.0328657861694598,
0.0687598742348139));
#76738=CARTESIAN_POINT('Ctrl Pts',(0.00624647230033861,-0.0331951640388604,
0.0686281454257511));
#76739=CARTESIAN_POINT('Ctrl Pts',(0.00617041991534398,-0.0330855618127442,
0.0686540015747676));
#76740=CARTESIAN_POINT('Ctrl Pts',(0.00609484710770694,-0.032975722417194,
0.0686814482361032));
#76741=CARTESIAN_POINT('Ctrl Pts',(0.00601985237700612,-0.0328657861694598,
0.0687104550096942));
#76742=CARTESIAN_POINT('Ctrl Pts',(0.00614662702709085,-0.0331951640388604,
0.0685745536964497));
#76743=CARTESIAN_POINT('Ctrl Pts',(0.00606983652435434,-0.0330855618127442,
0.0686017850122799));
#76744=CARTESIAN_POINT('Ctrl Pts',(0.0059935534892273,-0.032975722417194,
0.0686306230874018));
#76745=CARTESIAN_POINT('Ctrl Pts',(0.00591787741817799,-0.0328657861694598,
0.0686610357845745));
#76746=CARTESIAN_POINT('Ctrl Pts',(0.00604678175384308,-0.0331951640388604,
0.0685209619671483));
#76747=CARTESIAN_POINT('Ctrl Pts',(0.00596925313336469,-0.0330855618127442,
0.0685495684497923));
#76748=CARTESIAN_POINT('Ctrl Pts',(0.00589225987074765,-0.032975722417194,
0.0685797979387003));
#76749=CARTESIAN_POINT('Ctrl Pts',(0.00581590245934985,-0.0328657861694598,
0.0686116165594547));
#76750=CARTESIAN_POINT('',(0.00603476276650962,-0.0331781648279164,0.0685254113201094));
#76751=CARTESIAN_POINT('',(0.00604678175384198,-0.0331951640388587,0.0685209619671487));
#76752=CARTESIAN_POINT('Origin',(0.0124496843299243,-0.0326412092132826,
0.083751548933787));
#76753=CARTESIAN_POINT('Ctrl Pts',(0.00603476276772703,-0.0331781648273353,
0.0685254113233959));
#76754=CARTESIAN_POINT('Ctrl Pts',(0.00604972819993293,-0.0331276810207345,
0.0685657050609758));
#76755=CARTESIAN_POINT('Ctrl Pts',(0.00606442329048319,-0.0330765665168813,
0.0686052709160877));
#76756=CARTESIAN_POINT('Ctrl Pts',(0.00609328587190068,-0.0329730612715184,
0.0686829820884425));
#76757=CARTESIAN_POINT('Ctrl Pts',(0.00610744141276619,-0.0329207135598909,
0.0687210952308556));
#76758=CARTESIAN_POINT('Ctrl Pts',(0.00612133224109073,-0.0328677532092985,
0.0687584956469329));
#76759=CARTESIAN_POINT('',(0.00619565620379196,-0.0331951640388701,0.0686008699984719));
#76760=CARTESIAN_POINT('Origin',(0.00812378219310841,-0.0315241814719618,
0.07415));
#76761=CARTESIAN_POINT('',(0.00603476276666942,-0.0332121607144237,0.0685254113205401));
#76762=CARTESIAN_POINT('',(0.00602275330947992,-0.0331951640388587,0.0685298863329841));
#76763=CARTESIAN_POINT('Origin',(0.012488821924199,-0.0326413652568557,
0.0837286474373116));
#76764=CARTESIAN_POINT('Origin',(0.011114284309464,-0.0326412100054318,
0.0842475298356103));
#76765=CARTESIAN_POINT('Origin',(0.0110696848207288,-0.0326413661676127,
0.084255724981764));
#76766=CARTESIAN_POINT('Ctrl Pts',(0.0062731520925408,-0.0337436976235975,
0.0687045162537317));
#76767=CARTESIAN_POINT('Ctrl Pts',(0.00622417458644122,-0.0336723290703325,
0.0687211611013268));
#76768=CARTESIAN_POINT('Ctrl Pts',(0.00617550439209288,-0.033601104548885,
0.0687386842071387));
#76769=CARTESIAN_POINT('Ctrl Pts',(0.00602011010256092,-0.0333736987606857,
0.0687946320128644));
#76770=CARTESIAN_POINT('Ctrl Pts',(0.0058681824982094,-0.0331450831799192,
0.0688594050413615));
#76771=CARTESIAN_POINT('Ctrl Pts',(0.00603825211877815,-0.0337436976235975,
0.0687900849531859));
#76772=CARTESIAN_POINT('Ctrl Pts',(0.00599004423052975,-0.0336723290703325,
0.0688088425267451));
#76773=CARTESIAN_POINT('Ctrl Pts',(0.00594218153080748,-0.033601104548885,
0.0688284641737325));
#76774=CARTESIAN_POINT('Ctrl Pts',(0.00578936541166089,-0.0333736987606857,
0.0688911122057338));
#76775=CARTESIAN_POINT('Ctrl Pts',(0.00564039622669078,-0.0331450831799192,
0.0689624264687813));
#76776=CARTESIAN_POINT('Ctrl Pts',(0.00603590311904052,-0.0337436976235975,
0.0687909406401804));
#76777=CARTESIAN_POINT('Ctrl Pts',(0.00598770292697063,-0.0336723290703325,
0.0688097193409994));
#76778=CARTESIAN_POINT('Ctrl Pts',(0.00593984830219463,-0.033601104548885,
0.0688293619733985));
#76779=CARTESIAN_POINT('Ctrl Pts',(0.0057870579647519,-0.0333736987606857,
0.0688920770076626));
#76780=CARTESIAN_POINT('Ctrl Pts',(0.0056381183639756,-0.0331450831799192,
0.0689634566830555));
#76781=CARTESIAN_POINT('',(0.00600462631125898,-0.0336938721132548,0.0688032904185449));
#76782=CARTESIAN_POINT('',(0.00578674824582927,-0.0333679870047996,0.0688948694279671));
#76783=CARTESIAN_POINT('Ctrl Pts',(0.00600462631128152,-0.0336938721132513,
0.0688032904185359));
#76784=CARTESIAN_POINT('Ctrl Pts',(0.00598375559559105,-0.0336629187933857,
0.0688115624780597));
#76785=CARTESIAN_POINT('Ctrl Pts',(0.00596293999109099,-0.0336319952300996,
0.0688199540984121));
#76786=CARTESIAN_POINT('Ctrl Pts',(0.00594218153081813,-0.0336011045488905,
0.0688284641737283));
#76787=CARTESIAN_POINT('Ctrl Pts',(0.00589009145084816,-0.0335235892595407,
0.0688498188646805));
#76788=CARTESIAN_POINT('Ctrl Pts',(0.00583826869550219,-0.0334458668665523,
0.0688719575253822));
#76789=CARTESIAN_POINT('Ctrl Pts',(0.00578674825651963,-0.0333679869962447,
0.0688948694229269));
#76790=CARTESIAN_POINT('Ctrl Pts',(0.00578670733990235,-0.0333679692470408,
0.0688948868668454));
#76791=CARTESIAN_POINT('Ctrl Pts',(0.00578689691692108,-0.0333391895417259,
0.0688952985685979));
#76792=CARTESIAN_POINT('Ctrl Pts',(0.00578704196364883,-0.0333104081133762,
0.0688956058010175));
#76793=CARTESIAN_POINT('Ctrl Pts',(0.00578723896601389,-0.0332532698772281,
0.0688960101108606));
#76794=CARTESIAN_POINT('Ctrl Pts',(0.0057872922798601,-0.033224917381766,
0.0688961102564426));
#76795=CARTESIAN_POINT('Ctrl Pts',(0.00578730007695781,-0.0331960985261731,
0.0688961108059752));
#76796=CARTESIAN_POINT('Ctrl Pts',(0.00578730019114828,-0.0331956312664165,
0.0688961107877576));
#76797=CARTESIAN_POINT('Ctrl Pts',(0.0057873002927981,-0.0331951640388587,
0.0688961107425525));
#76798=CARTESIAN_POINT('',(0.00590151527665438,-0.0331951640388587,0.0688453176577636));
#76799=CARTESIAN_POINT('',(0.00584440778473558,-0.0331951640388687,0.0688707142001683));
#76800=CARTESIAN_POINT('',(0.00612133224137555,-0.0335216366567747,0.0687584956472138));
#76801=CARTESIAN_POINT('Origin',(0.0130397563591545,-0.0326434571527544,
0.0839079534837288));
#76802=CARTESIAN_POINT('',(0.00612180524213312,-0.0336938721132327,0.0687597691804743));
#76803=CARTESIAN_POINT('Origin',(0.00231959251784929,-0.0336938867896205,
0.0585224839769945));
#76804=CARTESIAN_POINT('',(0.00606321577670605,-0.0336938721132538,0.0687815297995196));
#76805=CARTESIAN_POINT('Ctrl Pts',(0.00625683182131963,-0.0335235895815172,
0.0684478516058156));
#76806=CARTESIAN_POINT('Ctrl Pts',(0.00617833052217658,-0.0334144449262749,
0.0684735538533703));
#76807=CARTESIAN_POINT('Ctrl Pts',(0.0061002700236429,-0.0333049234473147,
0.068500907407455));
#76808=CARTESIAN_POINT('Ctrl Pts',(0.00602275330948,-0.0331951640388587,
0.0685298863329839));
#76809=CARTESIAN_POINT('Ctrl Pts',(0.00621183956698099,-0.0335235895815172,
0.0685518557861903));
#76810=CARTESIAN_POINT('Ctrl Pts',(0.00613477009014618,-0.0334144449262749,
0.0685781774407076));
#76811=CARTESIAN_POINT('Ctrl Pts',(0.0060581558553928,-0.0333049234473147,
0.0686061215330071));
#76812=CARTESIAN_POINT('Ctrl Pts',(0.00598209806555667,-0.0331951640388587,
0.0686356612053659));
#76813=CARTESIAN_POINT('Ctrl Pts',(0.00616684731264234,-0.0335235895815172,
0.0686558599665651));
#76814=CARTESIAN_POINT('Ctrl Pts',(0.00609120965811578,-0.0334144449262749,
0.0686828010280449));
#76815=CARTESIAN_POINT('Ctrl Pts',(0.00601604168714269,-0.0333049234473147,
0.0687113356585592));
#76816=CARTESIAN_POINT('Ctrl Pts',(0.00594144282163335,-0.0331951640388587,
0.0687414360777479));
#76817=CARTESIAN_POINT('Ctrl Pts',(0.0061218550583037,-0.0335235895815172,
0.0687598641469398));
#76818=CARTESIAN_POINT('Ctrl Pts',(0.00604764922608538,-0.0334144449262749,
0.0687874246153822));
#76819=CARTESIAN_POINT('Ctrl Pts',(0.00597392751889259,-0.0333049234473147,
0.0688165497841113));
#76820=CARTESIAN_POINT('Ctrl Pts',(0.00590078757771002,-0.0331951640388587,
0.0688472109501299));
#76821=CARTESIAN_POINT('',(0.00596213429307715,-0.0331951640388687,0.0686876019953839));
#76822=CARTESIAN_POINT('Ctrl Pts',(0.00603476276775504,-0.0332121607145989,
0.068525411323471));
#76823=CARTESIAN_POINT('Ctrl Pts',(0.00604970298029355,-0.0332625444109694,
0.0685656371582569));
#76824=CARTESIAN_POINT('Ctrl Pts',(0.00606438574952495,-0.0333135300746684,
0.0686051698387849));
#76825=CARTESIAN_POINT('Ctrl Pts',(0.00609324805637579,-0.0334167203140655,
0.0686828802718817));
#76826=CARTESIAN_POINT('Ctrl Pts',(0.00610741641537851,-0.0334688847587357,
0.0687210279265394));
#76827=CARTESIAN_POINT('Ctrl Pts',(0.00612133224146106,-0.0335216366562436,
0.0687584956479298));
#76828=CARTESIAN_POINT('Ctrl Pts',(0.00600646949786311,-0.0336938721132512,
0.0688041352519375));
#76829=CARTESIAN_POINT('Ctrl Pts',(0.00597517837754259,-0.0336474569765019,
0.0688165285857433));
#76830=CARTESIAN_POINT('Ctrl Pts',(0.00594403448092964,-0.033601104548885,
0.0688292873724213));
#76831=CARTESIAN_POINT('Ctrl Pts',(0.00586518529514674,-0.0334837508592655,
0.0688615896868568));
#76832=CARTESIAN_POINT('Ctrl Pts',(0.00578732791866564,-0.0333660264659096,
0.0688962142813527));
#76833=CARTESIAN_POINT('Ctrl Pts',(0.0060046263112863,-0.0336938721132512,
0.0688032904185342));
#76834=CARTESIAN_POINT('Ctrl Pts',(0.00597333024587553,-0.0336474569765019,
0.0688156945411226));
#76835=CARTESIAN_POINT('Ctrl Pts',(0.00594218153080748,-0.033601104548885,
0.0688284641737325));
#76836=CARTESIAN_POINT('Ctrl Pts',(0.00586332014580413,-0.0334837508592655,
0.0688607939475741));
#76837=CARTESIAN_POINT('Ctrl Pts',(0.0057854513891387,-0.0333660264659097,
0.068895446350906));
#76838=CARTESIAN_POINT('Ctrl Pts',(0.00569558683942607,-0.0336938721132512,
0.0686616406951254));
#76839=CARTESIAN_POINT('Ctrl Pts',(0.00566346165117972,-0.0336474569765019,
0.068675853728293));
#76840=CARTESIAN_POINT('Ctrl Pts',(0.00563150504567037,-0.033601104548885,
0.0686904418534641));
#76841=CARTESIAN_POINT('Ctrl Pts',(0.00555059826781557,-0.0334837508592655,
0.0687273756323722));
#76842=CARTESIAN_POINT('Ctrl Pts',(0.0054708214427003,-0.0333660264659097,
0.068766690628262));
#76843=CARTESIAN_POINT('',(0.00568571412321803,-0.0336769361243754,0.068667680774838));
#76844=CARTESIAN_POINT('',(0.0056974300172302,-0.0336938721132327,0.0686624855245192));
#76845=CARTESIAN_POINT('Ctrl Pts',(0.00568571412321775,-0.0336769361243751,
0.0686676807748381));
#76846=CARTESIAN_POINT('Ctrl Pts',(0.00568766599362715,-0.0336797586670183,
0.0686668127493317));
#76847=CARTESIAN_POINT('Ctrl Pts',(0.00568961825378007,-0.033682581271316,
0.0686659457990411));
#76848=CARTESIAN_POINT('Ctrl Pts',(0.00569352355871244,-0.033688226610875,
0.0686642140460501));
#76849=CARTESIAN_POINT('Ctrl Pts',(0.00569547660353143,-0.033691049346173,
0.0686633492433572));
#76850=CARTESIAN_POINT('Ctrl Pts',(0.0056974300172374,-0.0336938721132294,
0.0686624855245247));
#76851=CARTESIAN_POINT('Ctrl Pts',(0.00568571412321801,-0.0336769361243754,
0.068667680774838));
#76852=CARTESIAN_POINT('Ctrl Pts',(0.00570274472761296,-0.0336279031321627,
0.0687059763462553));
#76853=CARTESIAN_POINT('Ctrl Pts',(0.00572002035994807,-0.0335767851940105,
0.0687448228954735));
#76854=CARTESIAN_POINT('Ctrl Pts',(0.0057538715420316,-0.0334733198899491,
0.0688209417654192));
#76855=CARTESIAN_POINT('Ctrl Pts',(0.0057704698207817,-0.0334209645035413,
0.0688582651953198));
#76856=CARTESIAN_POINT('Ctrl Pts',(0.00578674825926269,-0.0333679869844681,
0.0688948694219787));
#76857=CARTESIAN_POINT('',(0.00585102816425459,-0.0336938721132538,0.0687328879715421));
#76858=CARTESIAN_POINT('Origin',(0.00812378219310841,-0.0315241814719618,
0.07415));
#76859=CARTESIAN_POINT('',(0.00568571412375028,-0.0337108120655693,0.0686676807760293));
#76860=CARTESIAN_POINT('',(0.00567400935308169,-0.0336938721132327,0.0686729010386622));
#76861=CARTESIAN_POINT('Origin',(0.0113128278435283,-0.0345562516955559,
0.0840713794002105));
#76862=CARTESIAN_POINT('Ctrl Pts',(0.00567400935308121,-0.033693872113231,
0.0686729010386669));
#76863=CARTESIAN_POINT('Ctrl Pts',(0.0056759590678808,-0.0336910493335091,
0.0686720289787689));
#76864=CARTESIAN_POINT('Ctrl Pts',(0.00567790932733335,-0.0336882266045427,
0.0686711579246108));
#76865=CARTESIAN_POINT('Ctrl Pts',(0.00568181091981302,-0.0336825812712757,
0.0686694178353954));
#76866=CARTESIAN_POINT('Ctrl Pts',(0.00568376225282281,-0.0336797586669981,
0.0686685488003381));
#76867=CARTESIAN_POINT('Ctrl Pts',(0.00568571412321826,-0.0336769361243751,
0.0686676807748379));
#76868=CARTESIAN_POINT('Origin',(0.0133551836121441,-0.0345562518084255,
0.0831631116134414));
#76869=CARTESIAN_POINT('Ctrl Pts',(0.00593492688647828,-0.0342436276873911,
0.0688314440449839));
#76870=CARTESIAN_POINT('Ctrl Pts',(0.00573433424182315,-0.033943005420181,
0.0689139980837942));
#76871=CARTESIAN_POINT('Ctrl Pts',(0.00554052976830017,-0.0336441434784052,
0.0690114270551327));
#76872=CARTESIAN_POINT('Ctrl Pts',(0.00570586243808517,-0.0342436276873911,
0.0689315913289329));
#76873=CARTESIAN_POINT('Ctrl Pts',(0.00550904691051073,-0.033943005420181,
0.069022784675835));
#76874=CARTESIAN_POINT('Ctrl Pts',(0.00531965957175876,-0.0336441434784052,
0.0691285439039623));
#76875=CARTESIAN_POINT('',(0.0056730853089392,-0.0341934961088741,0.0689469038273424));
#76876=CARTESIAN_POINT('',(0.0054613874790652,-0.0338664212895199,0.0690519827975974));
#76877=CARTESIAN_POINT('Origin',(0.0123395583110997,-0.0345610818075423,
0.0842965367884047));
#76878=CARTESIAN_POINT('Origin',(0.000384867417876509,-0.0336938005044518,
0.0593315050317913));
#76879=CARTESIAN_POINT('',(0.00557281665257841,-0.0336938721132327,0.0689953225308435));
#76880=CARTESIAN_POINT('',(0.00551741651134117,-0.0336938721132427,0.0690242547680603));
#76881=CARTESIAN_POINT('',(0.00578674825926758,-0.0340203938281605,0.0688948694219765));
#76882=CARTESIAN_POINT('Origin',(0.0118739423558916,-0.0345589643244194,
0.0844178849644761));
#76883=CARTESIAN_POINT('',(0.00578730029279683,-0.034193496108874,0.068896110742553));
#76884=CARTESIAN_POINT('Origin',(0.00130960736199823,-0.0341934220717618,
0.0588274224331425));
#76885=CARTESIAN_POINT('',(0.00573019280087801,-0.0341934961088841,0.0689215072849577));
#76886=CARTESIAN_POINT('Ctrl Pts',(0.00590247750310578,-0.0340223579322397,
0.0685763292639232));
#76887=CARTESIAN_POINT('Ctrl Pts',(0.00582560204691174,-0.0339125849573575,
0.0686069668490042));
#76888=CARTESIAN_POINT('Ctrl Pts',(0.00574941473702995,-0.0338030433565231,
0.0686391740487182));
#76889=CARTESIAN_POINT('Ctrl Pts',(0.00567400935308184,-0.0336938721132327,
0.0686729010386616));
#76890=CARTESIAN_POINT('Ctrl Pts',(0.00586410444762454,-0.0340223579322397,
0.068682953315822));
#76891=CARTESIAN_POINT('Ctrl Pts',(0.00578869961519338,-0.0339125849573575,
0.0687141201654192));
#76892=CARTESIAN_POINT('Ctrl Pts',(0.00571399285022984,-0.0338030433565231,
0.0687468258192468));
#76893=CARTESIAN_POINT('Ctrl Pts',(0.00564007598248167,-0.0336938721132327,
0.0687810199833012));
#76894=CARTESIAN_POINT('Ctrl Pts',(0.0058257313921433,-0.0340223579322397,
0.0687895773677208));
#76895=CARTESIAN_POINT('Ctrl Pts',(0.00575179718347503,-0.0339125849573575,
0.0688212734818342));
#76896=CARTESIAN_POINT('Ctrl Pts',(0.00567857096342973,-0.0338030433565231,
0.0688544775897753));
#76897=CARTESIAN_POINT('Ctrl Pts',(0.00560614261188149,-0.0336938721132327,
0.0688891389279408));
#76898=CARTESIAN_POINT('Ctrl Pts',(0.00578735833666206,-0.0340223579322397,
0.0688962014196196));
#76899=CARTESIAN_POINT('Ctrl Pts',(0.00571489475175667,-0.0339125849573575,
0.0689284267982492));
#76900=CARTESIAN_POINT('Ctrl Pts',(0.00564314907662961,-0.0338030433565231,
0.0689621293603038));
#76901=CARTESIAN_POINT('Ctrl Pts',(0.00557220924128132,-0.0336938721132327,
0.0689972578725805));
#76902=CARTESIAN_POINT('',(0.00562341300284005,-0.0336938721132427,0.0688341117847629));
#76903=CARTESIAN_POINT('Ctrl Pts',(0.00568571412520953,-0.0337108120662699,
0.0686676807793159));
#76904=CARTESIAN_POINT('Ctrl Pts',(0.00570318664412029,-0.0337611408994238,
0.0687069700540986));
#76905=CARTESIAN_POINT('Ctrl Pts',(0.00572034032832543,-0.0338121088781185,
0.0687455423867835));
#76906=CARTESIAN_POINT('Ctrl Pts',(0.00575402565406572,-0.0339153382773242,
0.068821288306757));
#76907=CARTESIAN_POINT('Ctrl Pts',(0.0057705430446389,-0.0339675558473115,
0.0688584298488686));
#76908=CARTESIAN_POINT('Ctrl Pts',(0.00578674825927892,-0.0340203938281304,
0.0688948694220151));
#76909=CARTESIAN_POINT('Ctrl Pts',(0.00567497843361324,-0.0341934961088741,
0.0689476314618332));
#76910=CARTESIAN_POINT('Ctrl Pts',(0.00560324085231802,-0.0340836138583034,
0.0689813990154933));
#76911=CARTESIAN_POINT('Ctrl Pts',(0.0055322364407307,-0.0339738896647348,
0.0690166348255629));
#76912=CARTESIAN_POINT('Ctrl Pts',(0.00546205305262393,-0.033864463329982,
0.069053287702634));
#76913=CARTESIAN_POINT('Ctrl Pts',(0.00556920361712944,-0.0341934961088741,
0.0689069762393947));
#76914=CARTESIAN_POINT('Ctrl Pts',(0.00549690542439284,-0.0340836138583034,
0.0689422023651342));
#76915=CARTESIAN_POINT('Ctrl Pts',(0.00542537085244468,-0.0339738896647348,
0.0689789076481103));
#76916=CARTESIAN_POINT('Ctrl Pts',(0.00535468830752193,-0.033864463329982,
0.0690170389726853));
#76917=CARTESIAN_POINT('Ctrl Pts',(0.00546342880064564,-0.0341934961088741,
0.0688663210169561));
#76918=CARTESIAN_POINT('Ctrl Pts',(0.00539056999646766,-0.0340836138583034,
0.0689030057147751));
#76919=CARTESIAN_POINT('Ctrl Pts',(0.00531850526415866,-0.0339738896647348,
0.0689411804706578));
#76920=CARTESIAN_POINT('Ctrl Pts',(0.00524732356241992,-0.033864463329982,
0.0689807902427367));
#76921=CARTESIAN_POINT('Ctrl Pts',(0.00535765398416183,-0.0341934961088741,
0.0688256657945176));
#76922=CARTESIAN_POINT('Ctrl Pts',(0.00528423456854248,-0.0340836138583034,
0.068863809064416));
#76923=CARTESIAN_POINT('Ctrl Pts',(0.00521163967587265,-0.0339738896647348,
0.0689034532932052));
#76924=CARTESIAN_POINT('Ctrl Pts',(0.00513995881731792,-0.033864463329982,
0.0689445415127881));
#76925=CARTESIAN_POINT('',(0.00534628742210696,-0.03417647588326,0.0688315864418915));
#76926=CARTESIAN_POINT('',(0.00535765398416182,-0.034193496108874,0.0688256657945176));
#76927=CARTESIAN_POINT('Origin',(0.0125572058492587,-0.0345621026014781,
0.0837454721759852));
#76928=CARTESIAN_POINT('Ctrl Pts',(0.00534628742358402,-0.0341764758830167,
0.0688315864447245));
#76929=CARTESIAN_POINT('Ctrl Pts',(0.005366157861692,-0.0341260048546759,
0.0688696348358654));
#76930=CARTESIAN_POINT('Ctrl Pts',(0.00538568272774161,-0.0340749271290188,
0.0689070215173464));
#76931=CARTESIAN_POINT('Ctrl Pts',(0.00542405717566493,-0.0339715434429171,
0.0689805018299831));
#76932=CARTESIAN_POINT('Ctrl Pts',(0.00544289174144717,-0.0339192781035154,
0.069016566707967));
#76933=CARTESIAN_POINT('Ctrl Pts',(0.0054613874812267,-0.033866421287732,
0.0690519827938002));
#76934=CARTESIAN_POINT('',(0.00551536964656051,-0.0341934961088841,0.06888628481094));
#76935=CARTESIAN_POINT('Origin',(0.00812378219310841,-0.0315241814719618,
0.07415));
#76936=CARTESIAN_POINT('',(0.00534628742196449,-0.034210518019038,0.0688315864416189));
#76937=CARTESIAN_POINT('',(0.00533493353088824,-0.0341934961088739,0.0688375313516922));
#76938=CARTESIAN_POINT('Origin',(0.0125995375225319,-0.0345621708608686,
0.0837292687609065));
#76939=CARTESIAN_POINT('Origin',(0.0134650591095609,-0.0345621036373532,
0.0832713557882409));
#76940=CARTESIAN_POINT('Origin',(0.0134275703865789,-0.0345621717810568,
0.0832968329301066));
#76941=CARTESIAN_POINT('Ctrl Pts',(0.00557414626475439,-0.0346945769586966,
0.0689946281525624));
#76942=CARTESIAN_POINT('Ctrl Pts',(0.00546616493731153,-0.0345275153362944,
0.0690480312979003));
#76943=CARTESIAN_POINT('Ctrl Pts',(0.00535983516013318,-0.0343603235965185,
0.069104844169385));
#76944=CARTESIAN_POINT('Ctrl Pts',(0.00525546891217763,-0.034193496108874,
0.0691648940658255));
#76945=CARTESIAN_POINT('Ctrl Pts',(0.00549983620543779,-0.0346945769586966,
0.0690334359284018));
#76946=CARTESIAN_POINT('Ctrl Pts',(0.00539266772239766,-0.0345275153362944,
0.0690883955276842));
#76947=CARTESIAN_POINT('Ctrl Pts',(0.00528719994890919,-0.0343603235965185,
0.0691467396924839));
#76948=CARTESIAN_POINT('Ctrl Pts',(0.00518374224719534,-0.034193496108874,
0.0692082912306149));
#76949=CARTESIAN_POINT('Ctrl Pts',(0.0054255261461213,-0.0346945769586966,
0.0690722437042413));
#76950=CARTESIAN_POINT('Ctrl Pts',(0.00531917050748389,-0.0345275153362944,
0.0691287597574667));
#76951=CARTESIAN_POINT('Ctrl Pts',(0.00521456473768522,-0.0343603235965185,
0.0691886352155814));
#76952=CARTESIAN_POINT('Ctrl Pts',(0.00511201558221298,-0.034193496108874,
0.0692516883954046));
#76953=CARTESIAN_POINT('Ctrl Pts',(0.00535121608680457,-0.0346945769586966,
0.0691110514800807));
#76954=CARTESIAN_POINT('Ctrl Pts',(0.00524567329256993,-0.0345275153362944,
0.0691691239872521));
#76955=CARTESIAN_POINT('Ctrl Pts',(0.00514192952646121,-0.0343603235965185,
0.0692305307386816));
#76956=CARTESIAN_POINT('Ctrl Pts',(0.00504028891723077,-0.034193496108874,
0.0692950855601937));
#76957=CARTESIAN_POINT('',(0.00535121608758449,-0.0346945769586966,0.0691110514796735));
#76958=CARTESIAN_POINT('',(0.00514653396144725,-0.0343667727832754,0.0692292157162159));
#76959=CARTESIAN_POINT('Origin',(0.0136163976382128,-0.0345626461564186,
0.0837529099911741));
#76960=CARTESIAN_POINT('Origin',(-0.000574742401596686,-0.0341934771027763,
0.059773124973944));
#76961=CARTESIAN_POINT('',(0.00525418552406562,-0.0341934961088739,0.0691656705609461));
#76962=CARTESIAN_POINT('',(0.00520071137255756,-0.0341934961088839,0.0691980243106526));
#76963=CARTESIAN_POINT('',(0.00546138748271273,-0.034521194296272,0.0690519827966342));
#76964=CARTESIAN_POINT('Origin',(0.0131886668458207,-0.034562559611912,
0.0839725382199522));
#76965=CARTESIAN_POINT('',(0.00546201637008398,-0.0346945769586886,0.0690531870052571));
#76966=CARTESIAN_POINT('Origin',(0.000340517204970014,-0.0346945685853854,
0.0592464157979725));
#76967=CARTESIAN_POINT('',(0.00540661622884424,-0.0346945769587026,0.0690821192424753));
#76968=CARTESIAN_POINT('Ctrl Pts',(0.00555688618962087,-0.0345231616327842,
0.0687268049170898));
#76969=CARTESIAN_POINT('Ctrl Pts',(0.0054821350806509,-0.0344132092796988,
0.0687621859645974));
#76970=CARTESIAN_POINT('Ctrl Pts',(0.00540811965755405,-0.0343032738558979,
0.0687991113543318));
#76971=CARTESIAN_POINT('Ctrl Pts',(0.0053349335308882,-0.0341934961088739,
0.0688375313516922));
#76972=CARTESIAN_POINT('Ctrl Pts',(0.0055252839054265,-0.0345231616327842,
0.0688356278548013));
#76973=CARTESIAN_POINT('Ctrl Pts',(0.00545203276744245,-0.0344132092796988,
0.0688714444953041));
#76974=CARTESIAN_POINT('Ctrl Pts',(0.00537952624783742,-0.0343032738558979,
0.0689087744298423));
#76975=CARTESIAN_POINT('Ctrl Pts',(0.00530785601081389,-0.0341934961088739,
0.0689475674550632));
#76976=CARTESIAN_POINT('Ctrl Pts',(0.00549368162123214,-0.0345231616327842,
0.0689444507925129));
#76977=CARTESIAN_POINT('Ctrl Pts',(0.005421930454234,-0.0344132092796988,
0.0689807030260108));
#76978=CARTESIAN_POINT('Ctrl Pts',(0.00535093283812078,-0.0343032738558979,
0.0690184375053529));
#76979=CARTESIAN_POINT('Ctrl Pts',(0.00528077849073958,-0.0341934961088739,
0.0690576035584343));
#76980=CARTESIAN_POINT('Ctrl Pts',(0.00546207933703777,-0.0345231616327842,
0.0690532737302244));
#76981=CARTESIAN_POINT('Ctrl Pts',(0.00539182814102554,-0.0344132092796988,
0.0690899615567174));
#76982=CARTESIAN_POINT('Ctrl Pts',(0.00532233942840415,-0.0343032738558979,
0.0691281005808634));
#76983=CARTESIAN_POINT('Ctrl Pts',(0.00525370097066527,-0.0341934961088739,
0.0691676396618053));
#76984=CARTESIAN_POINT('',(0.00529455952748693,-0.0341934961088839,0.0690016009563292));
#76985=CARTESIAN_POINT('Ctrl Pts',(0.00534628742355866,-0.03421051801954,
0.0688315864446759));
#76986=CARTESIAN_POINT('Ctrl Pts',(0.00536618013406737,-0.0342610556239182,
0.0688696774835435));
#76987=CARTESIAN_POINT('Ctrl Pts',(0.00538571588016893,-0.0343122189865703,
0.0689070849984284));
#76988=CARTESIAN_POINT('Ctrl Pts',(0.00542408960451617,-0.0344158093671077,
0.0689805639255444));
#76989=CARTESIAN_POINT('Ctrl Pts',(0.00544291474401996,-0.0344682017099466,
0.0690166107538446));
#76990=CARTESIAN_POINT('Ctrl Pts',(0.00546138748271902,-0.0345211942962543,
0.0690519827966574));
#76991=CARTESIAN_POINT('Ctrl Pts',(0.00535315069336335,-0.0346945769586932,
0.0691116586599817));
#76992=CARTESIAN_POINT('Ctrl Pts',(0.00524898655120909,-0.0345296777077528,
0.0691689395057838));
#76993=CARTESIAN_POINT('Ctrl Pts',(0.00514727888600538,-0.0343648066252516,
0.0692304766055316));
#76994=CARTESIAN_POINT('Ctrl Pts',(0.00535121608759247,-0.0346945769586932,
0.0691110514796692));
#76995=CARTESIAN_POINT('Ctrl Pts',(0.00524703939241488,-0.0345296777077528,
0.0691683723220768));
#76996=CARTESIAN_POINT('Ctrl Pts',(0.0051453208380107,-0.0343648066252516,
0.0692299499030813));
#76997=CARTESIAN_POINT('Ctrl Pts',(0.00502879459541324,-0.0346945769586932,
0.0690098587791664));
#76998=CARTESIAN_POINT('Ctrl Pts',(0.00492252581275511,-0.0345296777077528,
0.0690738454577844));
#76999=CARTESIAN_POINT('Ctrl Pts',(0.00481899246366886,-0.0343648066252516,
0.0691421696470237));
#77000=CARTESIAN_POINT('',(0.00501782222316508,-0.0346775396664962,0.0690164814543596));
#77001=CARTESIAN_POINT('',(0.00502879459541034,-0.0346945769586886,0.0690098587791681));
#77002=CARTESIAN_POINT('Origin',(0.0137421018776223,-0.0345626618292509,
0.0831409227960663));
#77003=CARTESIAN_POINT('Ctrl Pts',(0.00501782222498079,-0.0346775396670097,
0.0690164814543668));
#77004=CARTESIAN_POINT('Ctrl Pts',(0.00504005996953166,-0.0346269749928338,
0.0690532358870802));
#77005=CARTESIAN_POINT('Ctrl Pts',(0.005061902530474,-0.0345757902891088,
0.0690893370929175));
#77006=CARTESIAN_POINT('Ctrl Pts',(0.00510481512632278,-0.0344721681088299,
0.0691602628715452));
#77007=CARTESIAN_POINT('Ctrl Pts',(0.00512586833264621,-0.0344197714289979,
0.0691950596410056));
#77008=CARTESIAN_POINT('Ctrl Pts',(0.0051465339616478,-0.034366772783151,
0.0692292157159015));
#77009=CARTESIAN_POINT('',(0.00519000534150742,-0.0346945769587026,0.0690604551294308));
#77010=CARTESIAN_POINT('Origin',(0.00812378219310841,-0.0315241814719618,
0.07415));
#77011=CARTESIAN_POINT('',(0.00501782222314295,-0.0347116136489808,0.0690164814557504));
#77012=CARTESIAN_POINT('',(0.00500686402026083,-0.0346945769586885,0.0690231275514409));
#77013=CARTESIAN_POINT('Origin',(0.0137798706785429,-0.0345626688067305,
0.0831158875518691));
#77014=CARTESIAN_POINT('Origin',(0.0134807789049568,-0.0345626626943302,
0.0832990351857672));
#77015=CARTESIAN_POINT('Origin',(0.0134410735156174,-0.0345626697525361,
0.0833208694376766));
#77016=CARTESIAN_POINT('Ctrl Pts',(0.00528769508957777,-0.0352450361874068,
0.0691464639936529));
#77017=CARTESIAN_POINT('Ctrl Pts',(0.00509898363248728,-0.0349452760959493,
0.069253428773973));
#77018=CARTESIAN_POINT('Ctrl Pts',(0.00491886530969939,-0.034644428984174,
0.0693743041977043));
#77019=CARTESIAN_POINT('Ctrl Pts',(0.00528552657235165,-0.0352450361874068,
0.0691477574997566));
#77020=CARTESIAN_POINT('Ctrl Pts',(0.0050968639006444,-0.0349452760959493,
0.0692548040670459));
#77021=CARTESIAN_POINT('Ctrl Pts',(0.00491680038517477,-0.034644428984174,
0.0693757573706836));
#77022=CARTESIAN_POINT('Ctrl Pts',(0.00507082189649861,-0.0352450361874068,
0.0692758274110036));
#77023=CARTESIAN_POINT('Ctrl Pts',(0.00488698946075453,-0.0349452760959493,
0.0693909716980202));
#77024=CARTESIAN_POINT('Ctrl Pts',(0.00471235241243916,-0.034644428984174,
0.0695196358834792));
#77025=CARTESIAN_POINT('Ctrl Pts',(0.00506867484974007,-0.0352450361874068,
0.069277108110116));
#77026=CARTESIAN_POINT('Ctrl Pts',(0.00488489071635562,-0.0349452760959493,
0.0693923333743298));
#77027=CARTESIAN_POINT('Ctrl Pts',(0.00471030793271181,-0.034644428984174,
0.0695210746686072));
#77028=CARTESIAN_POINT('',(0.00504031496053605,-0.0351951634053284,0.0692950662076422));
#77029=CARTESIAN_POINT('',(0.00484343027934216,-0.0348678972925388,0.0694258687230507));
#77030=CARTESIAN_POINT('Origin',(0.0147430153683402,-0.0345636767881302,
0.0829428536169149));
#77031=CARTESIAN_POINT('Origin',(-0.00145897125933837,-0.0346946199341064,
0.0603495961363917));
#77032=CARTESIAN_POINT('',(0.00494687939771636,-0.0346945769330288,0.0693556894524282));
#77033=CARTESIAN_POINT('',(0.00489554226662406,-0.0346945769458128,0.0693913370338159));
#77034=CARTESIAN_POINT('',(0.00514653396174029,-0.0350221583435276,0.0692292157160859));
#77035=CARTESIAN_POINT('Origin',(0.0143732444102733,-0.0345628458718996,
0.0832501203288295));
#77036=CARTESIAN_POINT('',(0.00514717683520144,-0.0351951360298761,0.0692302724120965));
#77037=CARTESIAN_POINT('Origin',(-0.000556908188897693,-0.0351951838366778,
0.0598025866993451));
#77038=CARTESIAN_POINT('',(0.00504028891793258,-0.0351951371328751,0.0692950855596333));
#77039=CARTESIAN_POINT('Ctrl Pts',(0.00522142529493176,-0.0350241211494343,
0.068898683552134));
#77040=CARTESIAN_POINT('Ctrl Pts',(0.00514909056398597,-0.0349144232818962,
0.0689386623283936));
#77041=CARTESIAN_POINT('Ctrl Pts',(0.00507753892708967,-0.0348045283579412,
0.0689801602444542));
#77042=CARTESIAN_POINT('Ctrl Pts',(0.00500686401076511,-0.0346945769439157,
0.0690231275572138));
#77043=CARTESIAN_POINT('Ctrl Pts',(0.00519671843168066,-0.0350241211494343,
0.0690092761048272));
#77044=CARTESIAN_POINT('Ctrl Pts',(0.00512590706780351,-0.0349144232818962,
0.069049595207998));
#77045=CARTESIAN_POINT('Ctrl Pts',(0.0050558867445849,-0.0348045283579412,
0.0690914021655859));
#77046=CARTESIAN_POINT('Ctrl Pts',(0.00498674914185908,-0.0346945769439157,
0.0691346467656571));
#77047=CARTESIAN_POINT('Ctrl Pts',(0.00517201156842956,-0.0350241211494342,
0.0691198686575205));
#77048=CARTESIAN_POINT('Ctrl Pts',(0.00510272357162104,-0.0349144232818962,
0.0691605280876023));
#77049=CARTESIAN_POINT('Ctrl Pts',(0.00503423456208013,-0.0348045283579412,
0.0692026440867175));
#77050=CARTESIAN_POINT('Ctrl Pts',(0.00496663427295305,-0.0346945769439157,
0.0692461659741004));
#77051=CARTESIAN_POINT('Ctrl Pts',(0.00514730470517846,-0.0350241211494342,
0.0692304612102137));
#77052=CARTESIAN_POINT('Ctrl Pts',(0.00507954007543858,-0.0349144232818962,
0.0692714609672067));
#77053=CARTESIAN_POINT('Ctrl Pts',(0.00501258237957536,-0.0348045283579412,
0.0693138860078492));
#77054=CARTESIAN_POINT('Ctrl Pts',(0.00494651940404702,-0.0346945769439157,
0.0693576851825436));
#77055=CARTESIAN_POINT('',(0.00497687170919161,-0.0346945769458128,0.0691894085017085));
#77056=CARTESIAN_POINT('Ctrl Pts',(0.00501782222484005,-0.0347116136492805,
0.0690164814585585));
#77057=CARTESIAN_POINT('Ctrl Pts',(0.00504005112727424,-0.034762154653215,
0.069053221301946));
#77058=CARTESIAN_POINT('Ctrl Pts',(0.0050618891855351,-0.0348133084096714,
0.0690893151596056));
#77059=CARTESIAN_POINT('Ctrl Pts',(0.0051048018390844,-0.034916856154457,
0.0691602410262969));
#77060=CARTESIAN_POINT('Ctrl Pts',(0.00512585941308189,-0.0349692089015918,
0.069195044902605));
#77061=CARTESIAN_POINT('Ctrl Pts',(0.00514653396174227,-0.0350221583435,
0.0692292157161274));
#77062=CARTESIAN_POINT('Ctrl Pts',(0.00504170955441301,-0.0351951371254899,
0.0692954351478188));
#77063=CARTESIAN_POINT('Ctrl Pts',(0.00494134447195073,-0.0350307338980918,
0.0693591550658663));
#77064=CARTESIAN_POINT('Ctrl Pts',(0.00484369876383043,-0.0348659306897793,
0.069426968732773));
#77065=CARTESIAN_POINT('Ctrl Pts',(0.00504028891799687,-0.0351951371254899,
0.06929508555973));
#77066=CARTESIAN_POINT('Ctrl Pts',(0.0049399166080202,-0.0350307338980918,
0.0693588348485441));
#77067=CARTESIAN_POINT('Ctrl Pts',(0.00484226489248684,-0.0348659306897793,
0.0694266781598411));
#77068=CARTESIAN_POINT('Ctrl Pts',(0.00480218877398651,-0.0351951371254899,
0.0692364942316872));
#77069=CARTESIAN_POINT('Ctrl Pts',(0.00470060512506399,-0.0350307338980918,
0.0693051660915897));
#77070=CARTESIAN_POINT('Ctrl Pts',(0.00460194656084147,-0.0348659306897793,
0.0693779778336128));
#77071=CARTESIAN_POINT('Origin',(0.00181014562194367,-0.0308609197410754,
0.0650575462689631));
#77072=CARTESIAN_POINT('',(0.00493648262365106,-0.0351951371254899,0.0692695410617617));
#77073=CARTESIAN_POINT('Origin',(0.00879149458470891,-0.0351840467441126,
0.0748633763469272));
#77074=CARTESIAN_POINT('Origin',(0.000661576364853088,-0.0352322614578571,
0.0647967767776562));
#77075=CARTESIAN_POINT('',(0.00465187649100793,-0.0351951142564654,0.0695648407465883));
#77076=CARTESIAN_POINT('',(0.00455411599855671,-0.0351951372916786,0.0696422307890182));
#77077=CARTESIAN_POINT('Origin',(0.0080072158301023,-0.0352875118963586,
0.0744700109874943));
#77078=CARTESIAN_POINT('Origin',(0.0147888593340341,-0.0298325076521914,
0.0707044322691962));
#77079=CARTESIAN_POINT('Origin',(0.00577656859764103,-0.0338731362290147,
0.0661036106639049));
#77080=CARTESIAN_POINT('Ctrl Pts',(0.00801039742017867,-0.0321934096636942,
0.0683997582973775));
#77081=CARTESIAN_POINT('Ctrl Pts',(0.0079074708319817,-0.0320508460843967,
0.0684017878308188));
#77082=CARTESIAN_POINT('Ctrl Pts',(0.00780467638033086,-0.0319086045662354,
0.06840658126832));
#77083=CARTESIAN_POINT('Ctrl Pts',(0.00770223455006554,-0.0317669892866828,
0.0684141100671357));
#77084=CARTESIAN_POINT('Ctrl Pts',(0.00792662179503905,-0.0321934096636942,
0.0684032335326665));
#77085=CARTESIAN_POINT('Ctrl Pts',(0.00782375741189882,-0.0320508460843967,
0.0684067626099037));
#77086=CARTESIAN_POINT('Ctrl Pts',(0.00772106540818489,-0.0319086045662354,
0.0684130527892125));
#77087=CARTESIAN_POINT('Ctrl Pts',(0.00761876578283156,-0.0317669892866828,
0.0684220723232597));
#77088=CARTESIAN_POINT('Ctrl Pts',(0.00784284616989943,-0.0321934096636942,
0.0684067087679555));
#77089=CARTESIAN_POINT('Ctrl Pts',(0.00774004399181596,-0.0320508460843967,
0.0684117373889885));
#77090=CARTESIAN_POINT('Ctrl Pts',(0.00763745443603893,-0.0319086045662354,
0.0684195243101051));
#77091=CARTESIAN_POINT('Ctrl Pts',(0.00753529701559759,-0.0317669892866828,
0.0684300345793837));
#77092=CARTESIAN_POINT('Ctrl Pts',(0.0077590705447598,-0.0321934096636942,
0.0684101840032445));
#77093=CARTESIAN_POINT('Ctrl Pts',(0.00765633057173309,-0.0320508460843967,
0.0684167121680733));
#77094=CARTESIAN_POINT('Ctrl Pts',(0.00755384346389296,-0.0319086045662354,
0.0684259958309976));
#77095=CARTESIAN_POINT('Ctrl Pts',(0.00745182824836361,-0.0317669892866828,
0.0684379968355076));
#77096=CARTESIAN_POINT('',(0.00776056930724865,-0.0321934096636942,0.0684101218306007));
#77097=CARTESIAN_POINT('',(0.00752505549789501,-0.0318665617511268,0.0684298906187498));
#77098=CARTESIAN_POINT('Origin',(0.00820141015539198,-0.0326371944420527,
0.0851141202804744));
#77099=CARTESIAN_POINT('Origin',(0.00638397650341509,-0.0316939261509635,
0.0575282609788763));
#77100=CARTESIAN_POINT('',(0.00788514356785206,-0.0320197221621866,0.0684036410856033));
#77101=CARTESIAN_POINT('Ctrl Pts',(0.00788496291033336,-0.0320197392094778,
0.0684036013648333));
#77102=CARTESIAN_POINT('Ctrl Pts',(0.00785572338860702,-0.0319792716576076,
0.0684048166010218));
#77103=CARTESIAN_POINT('Ctrl Pts',(0.00782636002191936,-0.0319386439829735,
0.0684062602797732));
#77104=CARTESIAN_POINT('Ctrl Pts',(0.00779684239961052,-0.0318979099381666,
0.0684079423639928));
#77105=CARTESIAN_POINT('Ctrl Pts',(0.00776732536073717,-0.0318571766984953,
0.0684096244149649));
#77106=CARTESIAN_POINT('Ctrl Pts',(0.0077378039958447,-0.0318163871833588,
0.0684115345338993));
#77107=CARTESIAN_POINT('Ctrl Pts',(0.00770837961891253,-0.0317755399638303,
0.068413662636967));
#77108=CARTESIAN_POINT('',(0.00788546189524767,-0.0321934096636183,0.0684049409545569));
#77109=CARTESIAN_POINT('Origin',(0.00776873771683435,-0.0324113708469043,
0.0660987583219195));
#77110=CARTESIAN_POINT('',(0.00782301560125816,-0.0321934096636663,0.0684075313925888));
#77111=CARTESIAN_POINT('Ctrl Pts',(0.007762061687006,-0.0321934096636618,
0.0684114953261555));
#77112=CARTESIAN_POINT('Ctrl Pts',(0.00768292323522471,-0.0320835708272592,
0.0684164837338431));
#77113=CARTESIAN_POINT('Ctrl Pts',(0.00760393392179947,-0.0319739230346488,
0.0684231070141982));
#77114=CARTESIAN_POINT('Ctrl Pts',(0.00752519415771869,-0.0318646057455573,
0.0684313489370169));
#77115=CARTESIAN_POINT('Ctrl Pts',(0.00767868091641969,-0.0321934096636618,
0.0683347567318175));
#77116=CARTESIAN_POINT('Ctrl Pts',(0.00759848417961592,-0.0320835708272592,
0.0683408950253147));
#77117=CARTESIAN_POINT('Ctrl Pts',(0.00751846099184358,-0.0319739230346488,
0.0683486894256524));
#77118=CARTESIAN_POINT('Ctrl Pts',(0.00743871297186613,-0.0318646057455573,
0.068358122102741));
#77119=CARTESIAN_POINT('Ctrl Pts',(0.00759530014583338,-0.0321934096636618,
0.0682580181374796));
#77120=CARTESIAN_POINT('Ctrl Pts',(0.00751404512400712,-0.0320835708272592,
0.0682653063167864));
#77121=CARTESIAN_POINT('Ctrl Pts',(0.00743298806188769,-0.0319739230346488,
0.0682742718371066));
#77122=CARTESIAN_POINT('Ctrl Pts',(0.00735223178601357,-0.0318646057455573,
0.0682848952684651));
#77123=CARTESIAN_POINT('Ctrl Pts',(0.00751191937524706,-0.0321934096636618,
0.0681812795431417));
#77124=CARTESIAN_POINT('Ctrl Pts',(0.00742960606839833,-0.0320835708272592,
0.068189717608258));
#77125=CARTESIAN_POINT('Ctrl Pts',(0.0073475151319318,-0.0319739230346488,
0.0681998542485608));
#77126=CARTESIAN_POINT('Ctrl Pts',(0.00726575060016101,-0.0318646057455573,
0.0682116684341893));
#77127=CARTESIAN_POINT('',(0.00749917147742976,-0.0321763980308455,0.0681826001113111));
#77128=CARTESIAN_POINT('',(0.0075119193752146,-0.0321934096636184,0.068181279543145));
#77129=CARTESIAN_POINT('Origin',(0.00861046215821728,-0.0326386231061021,
0.0846929340187781));
#77130=CARTESIAN_POINT('Ctrl Pts',(0.00749917147775506,-0.0321763980306277,
0.0681826001144621));
#77131=CARTESIAN_POINT('Ctrl Pts',(0.00750363941120969,-0.0321259596174824,
0.0682252858144191));
#77132=CARTESIAN_POINT('Ctrl Pts',(0.00750802993192638,-0.0320749164631392,
0.0682672319292351));
#77133=CARTESIAN_POINT('Ctrl Pts',(0.00751665968120572,-0.0319716057793906,
0.0683496787454615));
#77134=CARTESIAN_POINT('Ctrl Pts',(0.00752089554732806,-0.03191937866901,
0.0683901473228217));
#77135=CARTESIAN_POINT('Ctrl Pts',(0.00752505549808159,-0.0318665617525276,
0.0684298906205918));
#77136=CARTESIAN_POINT('',(0.00763624434124162,-0.0321934096636663,0.0682957006868829));
#77137=CARTESIAN_POINT('Origin',(0.00812378219310841,-0.0315241814719618,
0.07415));
#77138=CARTESIAN_POINT('',(0.00749917147739109,-0.0322104233323794,0.068182600110942));
#77139=CARTESIAN_POINT('',(0.00748642642908507,-0.0321934096636183,0.0681839479024995));
#77140=CARTESIAN_POINT('Origin',(0.00865576766829494,-0.0326387235197539,
0.0846945433864166));
#77141=CARTESIAN_POINT('Origin',(0.00983080235707136,-0.0326386242537259,
0.0845652026842633));
#77142=CARTESIAN_POINT('Origin',(0.00978681119076951,-0.0326387243745439,
0.0845761540139851));
#77143=CARTESIAN_POINT('Ctrl Pts',(0.00768554811731203,-0.0327445246967097,
0.0684153617468221));
#77144=CARTESIAN_POINT('Ctrl Pts',(0.0074692626998059,-0.032443687833936,
0.0684318900151914));
#77145=CARTESIAN_POINT('Ctrl Pts',(0.00725483670305344,-0.0321434074405927,
0.0684646628301117));
#77146=CARTESIAN_POINT('Ctrl Pts',(0.00743674780973492,-0.0327445246967097,
0.0684398241046301));
#77147=CARTESIAN_POINT('Ctrl Pts',(0.00722138500513619,-0.032443687833936,
0.0684657360300016));
#77148=CARTESIAN_POINT('Ctrl Pts',(0.00700858581564219,-0.0321434074405927,
0.0685077963489708));
#77149=CARTESIAN_POINT('',(0.0074008760926723,-0.0326943950436611,0.0684442544948138));
#77150=CARTESIAN_POINT('',(0.00716706830828393,-0.0323666188837389,0.0684787723072879));
#77151=CARTESIAN_POINT('Origin',(0.00958928232954848,-0.0326395579112405,
0.0851121558730604));
#77152=CARTESIAN_POINT('Origin',(0.00532984421989297,-0.0321933825603065,
0.057588043245766));
#77153=CARTESIAN_POINT('',(0.00729055273794418,-0.0321934096532689,0.0684593186988152));
#77154=CARTESIAN_POINT('',(0.00722892351684091,-0.0321934096584275,0.0684697153065266));
#77155=CARTESIAN_POINT('',(0.00752505549779406,-0.0325210109756239,0.0684298906178012));
#77156=CARTESIAN_POINT('Origin',(0.00910975440756268,-0.0326393129158705,
0.0851473325956557));
#77157=CARTESIAN_POINT('',(0.00752519692372645,-0.0326943950436593,0.0684312417715662));
#77158=CARTESIAN_POINT('Origin',(0.00637357625577623,-0.032694376553807,
0.0574288926357137));
#77159=CARTESIAN_POINT('',(0.00746303650820937,-0.0326943950436702,0.0684377481331999));
#77160=CARTESIAN_POINT('Ctrl Pts',(0.0077335540589646,-0.0325229783203769,
0.0681627032808331));
#77161=CARTESIAN_POINT('Ctrl Pts',(0.00765101930462442,-0.032413025309245,
0.0681680825671286));
#77162=CARTESIAN_POINT('Ctrl Pts',(0.00756860834574407,-0.032303122220807,
0.0681751683749668));
#77163=CARTESIAN_POINT('Ctrl Pts',(0.00748642642462623,-0.0321934096576658,
0.0681839479029759));
#77164=CARTESIAN_POINT('Ctrl Pts',(0.00766411058425769,-0.0325229783203769,
0.0682522507322593));
#77165=CARTESIAN_POINT('Ctrl Pts',(0.00758281023957715,-0.032413025309245,
0.068258587295335));
#77166=CARTESIAN_POINT('Ctrl Pts',(0.00750165330563394,-0.032303122220807,
0.0682666046994141));
#77167=CARTESIAN_POINT('Ctrl Pts',(0.007420743376306,-0.0321934096576658,
0.0682762890064978));
#77168=CARTESIAN_POINT('Ctrl Pts',(0.00759466710955079,-0.0325229783203769,
0.0683417981836855));
#77169=CARTESIAN_POINT('Ctrl Pts',(0.00751460117452988,-0.032413025309245,
0.0683490920235413));
#77170=CARTESIAN_POINT('Ctrl Pts',(0.00743469826552381,-0.032303122220807,
0.0683580410238614));
#77171=CARTESIAN_POINT('Ctrl Pts',(0.00735506032798578,-0.0321934096576658,
0.0683686301100198));
#77172=CARTESIAN_POINT('Ctrl Pts',(0.00752522363484389,-0.0325229783203769,
0.0684313456351116));
#77173=CARTESIAN_POINT('Ctrl Pts',(0.00744639210948262,-0.032413025309245,
0.0684395967517477));
#77174=CARTESIAN_POINT('Ctrl Pts',(0.00736774322541367,-0.032303122220807,
0.0684494773483087));
#77175=CARTESIAN_POINT('Ctrl Pts',(0.00728937727966555,-0.0321934096576658,
0.0684609712135418));
#77176=CARTESIAN_POINT('',(0.00738848958398549,-0.0321934096584275,0.0683216333004508));
#77177=CARTESIAN_POINT('Ctrl Pts',(0.00749917147774838,-0.0322104233328942,
0.0681826001143968));
#77178=CARTESIAN_POINT('Ctrl Pts',(0.00750364546532274,-0.0322609421831134,
0.0682253436541457));
#77179=CARTESIAN_POINT('Ctrl Pts',(0.00750803894356958,-0.0323120888240227,
0.0682673180246502));
#77180=CARTESIAN_POINT('Ctrl Pts',(0.00751666875819141,-0.0324156524631819,
0.0683497654651452));
#77181=CARTESIAN_POINT('Ctrl Pts',(0.00752090154725391,-0.0324680267167318,
0.0683902046448552));
#77182=CARTESIAN_POINT('Ctrl Pts',(0.00752505549779413,-0.0325210109755912,
0.0684298906178448));
#77183=CARTESIAN_POINT('Origin',(0.0159905897868985,-0.0262834582512493,
0.0742793217685553));
#77184=CARTESIAN_POINT('Origin',(0.0124014873473407,-0.0342770978491508,
0.0627690532049329));
#77185=CARTESIAN_POINT('Ctrl Pts',(0.00740245138760245,-0.0326943950436603,
0.068445531262888));
#77186=CARTESIAN_POINT('Ctrl Pts',(0.00732383311709117,-0.0325844576448133,
0.0684554725533059));
#77187=CARTESIAN_POINT('Ctrl Pts',(0.00724541488482755,-0.0324744968375322,
0.068467040502015));
#77188=CARTESIAN_POINT('Ctrl Pts',(0.00716729696039047,-0.0323646534831894,
0.068480218901646));
#77189=CARTESIAN_POINT('Ctrl Pts',(0.00731441682117113,-0.0326943950436603,
0.0683741797198448));
#77190=CARTESIAN_POINT('Ctrl Pts',(0.00723481519266967,-0.0325844576448133,
0.0683853342915824));
#77191=CARTESIAN_POINT('Ctrl Pts',(0.00715543862546899,-0.0324744968375322,
0.0683981359449325));
#77192=CARTESIAN_POINT('Ctrl Pts',(0.00707638859522006,-0.0323646534831894,
0.0684125668748955));
#77193=CARTESIAN_POINT('Ctrl Pts',(0.00722638225473981,-0.0326943950436603,
0.0683028281768015));
#77194=CARTESIAN_POINT('Ctrl Pts',(0.00714579726824817,-0.0325844576448133,
0.0683151960298589));
#77195=CARTESIAN_POINT('Ctrl Pts',(0.00706546236611043,-0.0324744968375322,
0.0683292313878501));
#77196=CARTESIAN_POINT('Ctrl Pts',(0.00698548023004965,-0.0323646534831894,
0.068344914848145));
#77197=CARTESIAN_POINT('Ctrl Pts',(0.00713834768830848,-0.0326943950436603,
0.0682314766337582));
#77198=CARTESIAN_POINT('Ctrl Pts',(0.00705677934382667,-0.0325844576448133,
0.0682450577681354));
#77199=CARTESIAN_POINT('Ctrl Pts',(0.00697548610675187,-0.0324744968375322,
0.0682603268307676));
#77200=CARTESIAN_POINT('Ctrl Pts',(0.00689457186487923,-0.0323646534831894,
0.0682772628213945));
#77201=CARTESIAN_POINT('',(0.00712570786471424,-0.0326773559991336,0.0682335950430089));
#77202=CARTESIAN_POINT('',(0.0071383476883078,-0.0326943950436594,0.0682314766337583));
#77203=CARTESIAN_POINT('Origin',(0.00993744315770636,-0.0326395670738684,
0.0845990298098265));
#77204=CARTESIAN_POINT('Ctrl Pts',(0.00712570786526682,-0.0326773559987419,
0.068233595046309));
#77205=CARTESIAN_POINT('Ctrl Pts',(0.00713285298483651,-0.0326267922585964,
0.0682759500289366));
#77206=CARTESIAN_POINT('Ctrl Pts',(0.00713987146232143,-0.0325756109579333,
0.0683175543000823));
#77207=CARTESIAN_POINT('Ctrl Pts',(0.0071536611061937,-0.0324719985462369,
0.0683992968267055));
#77208=CARTESIAN_POINT('Ctrl Pts',(0.00716042674193148,-0.0324196091621777,
0.068439402297488));
#77209=CARTESIAN_POINT('Ctrl Pts',(0.0071670683082921,-0.0323666188837756,
0.0684787723073359));
#77210=CARTESIAN_POINT('',(0.00726961189050005,-0.0326943950436702,0.0683378655642961));
#77211=CARTESIAN_POINT('Origin',(0.00812378219310841,-0.0315241814719618,
0.07415));
#77212=CARTESIAN_POINT('',(0.00712570786472155,-0.0327114338379883,0.0682335950430528));
#77213=CARTESIAN_POINT('',(0.00711307259435397,-0.0326943950436593,0.0682357404430475));
#77214=CARTESIAN_POINT('Origin',(0.0099819871076458,-0.0326395670367085,
0.0845907295957668));
#77215=CARTESIAN_POINT('Origin',(0.00983836293701956,-0.0326395678116252,
0.084615746030193));
#77216=CARTESIAN_POINT('Origin',(0.00979356073219717,-0.0326395679143015,
0.0846225142356918));
#77217=CARTESIAN_POINT('Ctrl Pts',(0.00732629311210369,-0.0332451089994433,
0.0684542001294218));
#77218=CARTESIAN_POINT('Ctrl Pts',(0.00711147250533561,-0.0329451141710254,
0.0684842779222104));
#77219=CARTESIAN_POINT('Ctrl Pts',(0.00689952776355092,-0.0326442513127493,
0.0685304514334594));
#77220=CARTESIAN_POINT('Ctrl Pts',(0.00707952003230626,-0.0332451089994433,
0.0684942381998959));
#77221=CARTESIAN_POINT('Ctrl Pts',(0.006866209486072,-0.0329451141710254,
0.0685336231916627));
#77222=CARTESIAN_POINT('Ctrl Pts',(0.00665647157117369,-0.0326442513127493,
0.0685889637171875));
#77223=CARTESIAN_POINT('Ctrl Pts',(0.00707705230150829,-0.0332451089994433,
0.0684946385806006));
#77224=CARTESIAN_POINT('Ctrl Pts',(0.00686375685587936,-0.0329451141710254,
0.0685341166443573));
#77225=CARTESIAN_POINT('Ctrl Pts',(0.00665404100924992,-0.0326442513127493,
0.0685895488400247));
#77226=CARTESIAN_POINT('',(0.00704403585815591,-0.0331951640388616,0.0685009051298321));
#77227=CARTESIAN_POINT('',(0.00681285681644229,-0.032867753235499,0.0685500357388078));
#77228=CARTESIAN_POINT('Origin',(0.0109422950086399,-0.0326402808281317,
0.0848053776164348));
#77229=CARTESIAN_POINT('Origin',(0.00429246866519795,-0.0326944278779127,
0.0577851842994068));
#77230=CARTESIAN_POINT('',(0.00693487608410739,-0.0326943950436593,0.0685228668698901));
#77231=CARTESIAN_POINT('',(0.00687402128537481,-0.0326943950436693,0.0685371126927966));
#77232=CARTESIAN_POINT('',(0.00716706830828674,-0.0330220786163545,0.0684787723072874));
#77233=CARTESIAN_POINT('Origin',(0.0104823291870166,-0.0326396682763501,
0.0849453207766407));
#77234=CARTESIAN_POINT('',(0.00716729429479589,-0.0331951640388587,0.068480111914651));
#77235=CARTESIAN_POINT('Origin',(0.00533222690299956,-0.0331952026559981,
0.0576021572729662));
#77236=CARTESIAN_POINT('',(0.0071056650764859,-0.0331951640388701,0.0684905085222516));
#77237=CARTESIAN_POINT('Ctrl Pts',(0.00735837766043643,-0.0330240426238172,
0.068199020593097));
#77238=CARTESIAN_POINT('Ctrl Pts',(0.00727639712134802,-0.032914277406352,
0.068209564786232));
#77239=CARTESIAN_POINT('Ctrl Pts',(0.00719459368989688,-0.0328043479726691,
0.0682218090027762));
#77240=CARTESIAN_POINT('Ctrl Pts',(0.007113072594354,-0.0326943950436593,
0.0682357404430475));
#77241=CARTESIAN_POINT('Ctrl Pts',(0.00729469397807497,-0.0330240426238172,
0.0682927517223196));
#77242=CARTESIAN_POINT('Ctrl Pts',(0.00721400467660942,-0.032914277406352,
0.0683041732202231));
#77243=CARTESIAN_POINT('Ctrl Pts',(0.00713351126285038,-0.0328043479726691,
0.0683172684854157));
#77244=CARTESIAN_POINT('Ctrl Pts',(0.00705331731686408,-0.0326943950436593,
0.0683320235817404));
#77245=CARTESIAN_POINT('Ctrl Pts',(0.00723101029571351,-0.0330240426238172,
0.0683864828515421));
#77246=CARTESIAN_POINT('Ctrl Pts',(0.00715161223187082,-0.0329142774063519,
0.0683987816542143));
#77247=CARTESIAN_POINT('Ctrl Pts',(0.00707242883580387,-0.0328043479726691,
0.0684127279680553));
#77248=CARTESIAN_POINT('Ctrl Pts',(0.00699356203937417,-0.0326943950436593,
0.0684283067204333));
#77249=CARTESIAN_POINT('Ctrl Pts',(0.00716732661335206,-0.0330240426238172,
0.0684802139807647));
#77250=CARTESIAN_POINT('Ctrl Pts',(0.00708921978713222,-0.0329142774063519,
0.0684933900882054));
#77251=CARTESIAN_POINT('Ctrl Pts',(0.00701134640875737,-0.0328043479726691,
0.0685081874506948));
#77252=CARTESIAN_POINT('Ctrl Pts',(0.00693380676188425,-0.0326943950436593,
0.0685245898591262));
#77253=CARTESIAN_POINT('',(0.00702397433924068,-0.0326943950436693,0.0683793036564788));
#77254=CARTESIAN_POINT('Ctrl Pts',(0.00712570786526824,-0.0327114338383338,
0.0682335950463169));
#77255=CARTESIAN_POINT('Ctrl Pts',(0.00713285179636839,-0.0327619876830847,
0.0682759429839112));
#77256=CARTESIAN_POINT('Ctrl Pts',(0.00713986969334866,-0.0328131562604072,
0.0683175438139299));
#77257=CARTESIAN_POINT('Ctrl Pts',(0.00715365932456068,-0.0329167375858778,
0.0683992862655054));
#77258=CARTESIAN_POINT('Ctrl Pts',(0.00716042556428761,-0.0329691088920624,
0.0684393953166267));
#77259=CARTESIAN_POINT('Ctrl Pts',(0.00716706830829191,-0.0330220786163187,
0.0684787723073348));
#77260=CARTESIAN_POINT('Ctrl Pts',(0.00704568847732885,-0.0331951640388604,
0.0685020806525492));
#77261=CARTESIAN_POINT('Ctrl Pts',(0.00692892136592929,-0.0330306422010619,
0.0685243695489135));
#77262=CARTESIAN_POINT('Ctrl Pts',(0.00681317525473458,-0.0328657861914645,
0.0685514655070815));
#77263=CARTESIAN_POINT('Ctrl Pts',(0.007044035858159,-0.0331951640388604,
0.0685009051298316));
#77264=CARTESIAN_POINT('Ctrl Pts',(0.00692724444358094,-0.0330306422010619,
0.0685232281930377));
#77265=CARTESIAN_POINT('Ctrl Pts',(0.00681147546212611,-0.0328657861914645,
0.068550359293328));
#77266=CARTESIAN_POINT('Ctrl Pts',(0.0067686650611903,-0.0331951640388604,
0.0683050314321819));
#77267=CARTESIAN_POINT('Ctrl Pts',(0.00664782408349586,-0.0330306422010619,
0.0683330476100639));
#77268=CARTESIAN_POINT('Ctrl Pts',(0.00652824430166454,-0.0328657861914645,
0.0683660343330059));
#77269=CARTESIAN_POINT('',(0.00675618319574967,-0.0331781648281891,0.0683079393209088));
#77270=CARTESIAN_POINT('',(0.00676866506118923,-0.0331951640388588,0.0683050314321821));
#77271=CARTESIAN_POINT('Origin',(0.0112121800492513,-0.0326412092471448,
0.0842180170307076));
#77272=CARTESIAN_POINT('Ctrl Pts',(0.00675618319744972,-0.033178164828644,
0.0683079393215935));
#77273=CARTESIAN_POINT('Ctrl Pts',(0.00676598046126932,-0.0331276811546782,
0.0683497908710576));
#77274=CARTESIAN_POINT('Ctrl Pts',(0.00677560084977164,-0.0330765663497795,
0.0683908867034381));
#77275=CARTESIAN_POINT('Ctrl Pts',(0.00679449598386189,-0.0329730614463221,
0.0684716022795236));
#77276=CARTESIAN_POINT('Ctrl Pts',(0.00680376309100563,-0.0329207133374056,
0.0685111894171055));
#77277=CARTESIAN_POINT('Ctrl Pts',(0.00681285682806447,-0.032867753228935,
0.0685500357271382));
#77278=CARTESIAN_POINT('',(0.00690635045968257,-0.0331951640388701,0.0684029682810171));
#77279=CARTESIAN_POINT('Origin',(0.00812378219310841,-0.0315241814719618,
0.07415));
#77280=CARTESIAN_POINT('',(0.00675618319547328,-0.033212160714443,0.068307939322566));
#77281=CARTESIAN_POINT('',(0.00674370756866027,-0.0331951640388587,0.0683108738640981));
#77282=CARTESIAN_POINT('Origin',(0.0112538793822697,-0.0326413652941119,
0.0842002015163731));
#77283=CARTESIAN_POINT('Origin',(0.00982514711364439,-0.0326412099009382,
0.0845427171574036));
#77284=CARTESIAN_POINT('Origin',(0.00977987220206338,-0.0326413661470917,
0.0845452574844475));
#77285=CARTESIAN_POINT('Ctrl Pts',(0.0069702449498819,-0.0337436976235975,
0.0685155100649225));
#77286=CARTESIAN_POINT('Ctrl Pts',(0.00691956749347552,-0.0336723290703325,
0.0685258851537115));
#77287=CARTESIAN_POINT('Ctrl Pts',(0.00686908485063321,-0.033601104548885,
0.0685371700917642));
#77288=CARTESIAN_POINT('Ctrl Pts',(0.0067079037720858,-0.0333736987606857,
0.0685732006635465));
#77289=CARTESIAN_POINT('Ctrl Pts',(0.00654905594916388,-0.0331450831799191,
0.068618421359446));
#77290=CARTESIAN_POINT('Ctrl Pts',(0.00672647263077907,-0.0337436976235975,
0.0685709632563478));
#77291=CARTESIAN_POINT('Ctrl Pts',(0.00667629392878052,-0.0336723290703325,
0.0685835308703194));
#77292=CARTESIAN_POINT('Ctrl Pts',(0.00662634939627669,-0.033601104548885,
0.0685969990078362));
#77293=CARTESIAN_POINT('Ctrl Pts',(0.00646688639744637,-0.0333736987606857,
0.0686400001030398));
#77294=CARTESIAN_POINT('Ctrl Pts',(0.00631015383180769,-0.0331450831799191,
0.0686920812421688));
#77295=CARTESIAN_POINT('Ctrl Pts',(0.00672403490758804,-0.0337436976235975,
0.0685715177882619));
#77296=CARTESIAN_POINT('Ctrl Pts',(0.00667386119313358,-0.0336723290703325,
0.0685841073274855));
#77297=CARTESIAN_POINT('Ctrl Pts',(0.00662392204173313,-0.033601104548885,
0.0685975972969969));
#77298=CARTESIAN_POINT('Ctrl Pts',(0.00646447622369998,-0.0333736987606857,
0.0686406680974347));
#77299=CARTESIAN_POINT('Ctrl Pts',(0.00630776481063412,-0.0331450831799191,
0.0686928178409961));
#77300=CARTESIAN_POINT('',(0.0066914568891216,-0.0336938721132548,0.0685798501614804));
#77301=CARTESIAN_POINT('',(0.00646381896393862,-0.0333679870047995,0.0686433996805959));
#77302=CARTESIAN_POINT('Ctrl Pts',(0.00669145688914577,-0.0336938721132519,
0.0685798501614743));
#77303=CARTESIAN_POINT('Ctrl Pts',(0.00666971398131391,-0.0336629187933865,
0.0685854411990537));
#77304=CARTESIAN_POINT('Ctrl Pts',(0.00664801076515907,-0.0336319952301003,
0.0685911577619526));
#77305=CARTESIAN_POINT('Ctrl Pts',(0.00662634939628842,-0.0336011045488913,
0.0685969990078332));
#77306=CARTESIAN_POINT('Ctrl Pts',(0.00657199360968862,-0.0335235892595416,
0.0686116566925097));
#77307=CARTESIAN_POINT('Ctrl Pts',(0.0065178047823149,-0.033445866866553,
0.0686271256697595));
#77308=CARTESIAN_POINT('Ctrl Pts',(0.00646381897517569,-0.0333679869962453,
0.0686433996769363));
#77309=CARTESIAN_POINT('Ctrl Pts',(0.00646377619489206,-0.0333679692470407,
0.0686434118550933));
#77310=CARTESIAN_POINT('Ctrl Pts',(0.00646391267711552,-0.0333391895417761,
0.0686438440707583));
#77311=CARTESIAN_POINT('Ctrl Pts',(0.00646401807368413,-0.0333104081135165,
0.0686441670597292));
#77312=CARTESIAN_POINT('Ctrl Pts',(0.0064641628490814,-0.0332532699115172,
0.0686445928721591));
#77313=CARTESIAN_POINT('Ctrl Pts',(0.00646420318974104,-0.0332249175515492,
0.068644698910686));
#77314=CARTESIAN_POINT('Ctrl Pts',(0.00646421085788016,-0.0331960985192758,
0.0686447004327229));
#77315=CARTESIAN_POINT('Ctrl Pts',(0.0064642109733624,-0.0331956312733899,
0.0686447004289874));
#77316=CARTESIAN_POINT('Ctrl Pts',(0.00646421107987799,-0.0331951640388603,
0.0686447003968783));
#77317=CARTESIAN_POINT('',(0.00658389150603356,-0.0331951640388587,0.0686086227639818));
#77318=CARTESIAN_POINT('',(0.00652405129296613,-0.0331951640388687,0.0686266615804399));
#77319=CARTESIAN_POINT('',(0.00681285683165936,-0.0335216366567744,0.0685500357418976));
#77320=CARTESIAN_POINT('Origin',(0.0117779965714527,-0.0326434571527492,
0.0844471440443612));
#77321=CARTESIAN_POINT('',(0.00681316648662222,-0.0336938721132326,0.0685513585156833));
#77322=CARTESIAN_POINT('Origin',(0.00432400742965567,-0.0336938867896239,
0.0579182537421924));
#77323=CARTESIAN_POINT('',(0.00675231168788191,-0.0336938721132537,0.0685656043385918));
#77324=CARTESIAN_POINT('Ctrl Pts',(0.00698622197913881,-0.0335235895815172,
0.0682588238220527));
#77325=CARTESIAN_POINT('Ctrl Pts',(0.00690511834039081,-0.0334144449262748,
0.0682744845780479));
#77326=CARTESIAN_POINT('Ctrl Pts',(0.00682424506282069,-0.0333049234473147,
0.0682918388664937));
#77327=CARTESIAN_POINT('Ctrl Pts',(0.00674370756866033,-0.0331951640388587,
0.0683108738640979));
#77328=CARTESIAN_POINT('Ctrl Pts',(0.00692854932193361,-0.0335235895815172,
0.0683563688736789));
#77329=CARTESIAN_POINT('Ctrl Pts',(0.00684878858286978,-0.0334144449262748,
0.0683728236073476));
#77330=CARTESIAN_POINT('Ctrl Pts',(0.00676927615079407,-0.0333049234473147,
0.0683909450423542));
#77331=CARTESIAN_POINT('Ctrl Pts',(0.00669011579669301,-0.0331951640388587,
0.0684107192168355));
#77332=CARTESIAN_POINT('Ctrl Pts',(0.00687087666472841,-0.0335235895815172,
0.0684539139253052));
#77333=CARTESIAN_POINT('Ctrl Pts',(0.00679245882534875,-0.0334144449262748,
0.0684711626366474));
#77334=CARTESIAN_POINT('Ctrl Pts',(0.00671430723876745,-0.0333049234473147,
0.0684900512182147));
#77335=CARTESIAN_POINT('Ctrl Pts',(0.00663652402472568,-0.0331951640388587,
0.068510564569573));
#77336=CARTESIAN_POINT('Ctrl Pts',(0.00681320400752322,-0.0335235895815172,
0.0685514589769314));
#77337=CARTESIAN_POINT('Ctrl Pts',(0.00673612906782772,-0.0334144449262748,
0.0685695016659471));
#77338=CARTESIAN_POINT('Ctrl Pts',(0.00665933832674083,-0.0333049234473147,
0.0685891573940752));
#77339=CARTESIAN_POINT('Ctrl Pts',(0.00658293225275836,-0.0331951640388587,
0.0686104099223105));
#77340=CARTESIAN_POINT('',(0.00666379953735691,-0.0331951640388687,0.0684597483140499));
#77341=CARTESIAN_POINT('Ctrl Pts',(0.00675618319618243,-0.0332121607145991,
0.0683079393256107));
#77342=CARTESIAN_POINT('Ctrl Pts',(0.00676596396673557,-0.0332625444109669,
0.0683497204728199));
#77343=CARTESIAN_POINT('Ctrl Pts',(0.00677557619926364,-0.0333135300746636,
0.0683907816652977));
#77344=CARTESIAN_POINT('Ctrl Pts',(0.00679447121834327,-0.0334167203140648,
0.0684714967346675));
#77345=CARTESIAN_POINT('Ctrl Pts',(0.00680374668669211,-0.0334688847587346,
0.0685111193499218));
#77346=CARTESIAN_POINT('Ctrl Pts',(0.00681285683165345,-0.0335216366562431,
0.0685500357426192));
#77347=CARTESIAN_POINT('Ctrl Pts',(0.00669317965594853,-0.0336938721132518,
0.0685809193456466));
#77348=CARTESIAN_POINT('Ctrl Pts',(0.00666058197885721,-0.0336474569765022,
0.068589293137022));
#77349=CARTESIAN_POINT('Ctrl Pts',(0.00662808456118034,-0.033601104548885,
0.068598047951588));
#77350=CARTESIAN_POINT('Ctrl Pts',(0.00654580857125863,-0.0334837508592655,
0.068620213129208));
#77351=CARTESIAN_POINT('Ctrl Pts',(0.00646422551105693,-0.0333660264659096,
0.0686448065816831));
#77352=CARTESIAN_POINT('Ctrl Pts',(0.0066914568891505,-0.0336938721132518,
0.068579850161473));
#77353=CARTESIAN_POINT('Ctrl Pts',(0.00665885295376941,-0.0336474569765022,
0.0685882340367742));
#77354=CARTESIAN_POINT('Ctrl Pts',(0.00662634939627669,-0.033601104548885,
0.0685969990078362));
#77355=CARTESIAN_POINT('Ctrl Pts',(0.00654405786175287,-0.0334837508592655,
0.0686191898993688));
#77356=CARTESIAN_POINT('Ctrl Pts',(0.00646246002573164,-0.0333660264659096,
0.0686438095150837));
#77357=CARTESIAN_POINT('Ctrl Pts',(0.00640260770369985,-0.0336938721132518,
0.0684005844721348));
#77358=CARTESIAN_POINT('Ctrl Pts',(0.00636895446675226,-0.0336474569765022,
0.068410659077569));
#77359=CARTESIAN_POINT('Ctrl Pts',(0.00633542147172276,-0.033601104548885,
0.0684211269463137));
#77360=CARTESIAN_POINT('Ctrl Pts',(0.00625052363803872,-0.0334837508592655,
0.0684476291832578));
#77361=CARTESIAN_POINT('Ctrl Pts',(0.00616644840145523,-0.0333660264659096,
0.0684766354812069));
#77362=CARTESIAN_POINT('',(0.00639205581408608,-0.0336769361243753,0.0684053395445685));
#77363=CARTESIAN_POINT('',(0.00640433046229623,-0.0336938721132327,0.0684016536512309));
#77364=CARTESIAN_POINT('Ctrl Pts',(0.00639205581408579,-0.033676936124375,
0.0684053395445686));
#77365=CARTESIAN_POINT('Ctrl Pts',(0.00639410108586206,-0.0336797586670244,
0.0684047229979311));
#77366=CARTESIAN_POINT('Ctrl Pts',(0.00639614660954832,-0.0336825812713284,
0.0684041075668789));
#77367=CARTESIAN_POINT('Ctrl Pts',(0.00640023816625122,-0.033688226610976,
0.0684028789337534));
#77368=CARTESIAN_POINT('Ctrl Pts',(0.0064022841993198,-0.0336910493463751,
0.0684022657316887));
#77369=CARTESIAN_POINT('Ctrl Pts',(0.00640433046230283,-0.0336938721132293,
0.0684016536512373));
#77370=CARTESIAN_POINT('Ctrl Pts',(0.00639205581408608,-0.0336769361243753,
0.0684053395445686));
#77371=CARTESIAN_POINT('Ctrl Pts',(0.00640415332488983,-0.0336278994613247,
0.0684454706488616));
#77372=CARTESIAN_POINT('Ctrl Pts',(0.00641642307030404,-0.0335767852527761,
0.0684861731074774));
#77373=CARTESIAN_POINT('Ctrl Pts',(0.00644046770507109,-0.0334733171841366,
0.0685659364374034));
#77374=CARTESIAN_POINT('Ctrl Pts',(0.00645225692480437,-0.0334209631343272,
0.0686050448469222));
#77375=CARTESIAN_POINT('Ctrl Pts',(0.00646381897801536,-0.0333679869844681,
0.0686433996763394));
#77376=CARTESIAN_POINT('',(0.00654789367571891,-0.0336938721132538,0.0684907519063656));
#77377=CARTESIAN_POINT('Origin',(0.00812378219310841,-0.0315241814719618,
0.07415));
#77378=CARTESIAN_POINT('',(0.0063920558144654,-0.033710812065585,0.0684053395458166));
#77379=CARTESIAN_POINT('',(0.00637978906701309,-0.0336938721132327,0.068409051648364));
#77380=CARTESIAN_POINT('Origin',(0.0100442027223466,-0.0345562517227294,
0.0843928399467902));
#77381=CARTESIAN_POINT('Ctrl Pts',(0.00637978906701234,-0.0336938721132314,
0.0684090516483674));
#77382=CARTESIAN_POINT('Ctrl Pts',(0.00638183270751947,-0.0336910493311555,
0.0684084308284648));
#77383=CARTESIAN_POINT('Ctrl Pts',(0.00638387675977588,-0.0336882266033658,
0.0684078110754133));
#77384=CARTESIAN_POINT('Ctrl Pts',(0.00638796567720988,-0.0336825812712471,
0.0684065737067743));
#77385=CARTESIAN_POINT('Ctrl Pts',(0.00639001054233957,-0.0336797586669837,
0.068405956091197));
#77386=CARTESIAN_POINT('Ctrl Pts',(0.00639205581408636,-0.033676936124375,
0.0684053395445684));
#77387=CARTESIAN_POINT('Origin',(0.0121842899637513,-0.0345562518086802,
0.0837477087828097));
#77388=CARTESIAN_POINT('Ctrl Pts',(0.00661877848008525,-0.034243627687391,
0.0685990461338805));
#77389=CARTESIAN_POINT('Ctrl Pts',(0.0064094208037195,-0.033943005420181,
0.0686558082846532));
#77390=CARTESIAN_POINT('Ctrl Pts',(0.00620493344833617,-0.0336441434784053,
0.0687281788581062));
#77391=CARTESIAN_POINT('Ctrl Pts',(0.00637896849035594,-0.034243627687391,
0.0686696943385713));
#77392=CARTESIAN_POINT('Ctrl Pts',(0.00617227535495563,-0.033943005420181,
0.0687355010722084));
#77393=CARTESIAN_POINT('Ctrl Pts',(0.00597112624589656,-0.0336441434784053,
0.0688166898296711));
#77394=CARTESIAN_POINT('Ctrl Pts',(0.00637657039045866,-0.034243627687391,
0.0686704008206182));
#77395=CARTESIAN_POINT('Ctrl Pts',(0.00616990390046798,-0.033943005420181,
0.0687362980000839));
#77396=CARTESIAN_POINT('Ctrl Pts',(0.00596878817387217,-0.0336441434784053,
0.0688175749393868));
#77397=CARTESIAN_POINT('',(0.00634453065372381,-0.034193496108874,0.0686807780297744));
#77398=CARTESIAN_POINT('',(0.0061213322399811,-0.0338664212864867,0.0687584956471367));
#77399=CARTESIAN_POINT('Origin',(0.0110346308465843,-0.0345610720405585,
0.0847449027782907));
#77400=CARTESIAN_POINT('Origin',(0.00230317710792826,-0.033693800507297,
0.05847839760108));
#77401=CARTESIAN_POINT('',(0.00623898417299239,-0.0336938721132327,0.0687162479424096));
#77402=CARTESIAN_POINT('',(0.00618039470757276,-0.0336938721132427,0.0687380085614519));
#77403=CARTESIAN_POINT('',(0.00646381897802044,-0.0340203938281605,0.0686433996763379));
#77404=CARTESIAN_POINT('Origin',(0.0105574639983245,-0.0345589643244318,
0.0848069393239999));
#77405=CARTESIAN_POINT('',(0.00646421107987864,-0.034193496108874,0.0686447003968781));
#77406=CARTESIAN_POINT('Origin',(0.00328376725328437,-0.0341934220717591,
0.0580942029998901));
#77407=CARTESIAN_POINT('',(0.00640437086681123,-0.0341934961088841,0.0686627392133364));
#77408=CARTESIAN_POINT('Ctrl Pts',(0.00661855933023323,-0.0340223579322397,
0.0683418760229223));
#77409=CARTESIAN_POINT('Ctrl Pts',(0.00653845015236607,-0.0339125849573575,
0.0683626369719874));
#77410=CARTESIAN_POINT('Ctrl Pts',(0.00645882696969454,-0.0338030433565231,
0.0683850414064078));
#77411=CARTESIAN_POINT('Ctrl Pts',(0.00637978906701337,-0.0336938721132327,
0.0684090516483634));
#77412=CARTESIAN_POINT('Ctrl Pts',(0.00656712532055574,-0.0340223579322397,
0.0684428498931996));
#77413=CARTESIAN_POINT('Ctrl Pts',(0.00648840883571061,-0.0339125849573575,
0.0684643202514037));
#77414=CARTESIAN_POINT('Ctrl Pts',(0.0064101920505526,-0.0338030433565231,
0.0684874047709601));
#77415=CARTESIAN_POINT('Ctrl Pts',(0.00633257237423454,-0.0336938721132327,
0.0685120650637679));
#77416=CARTESIAN_POINT('Ctrl Pts',(0.00651569131087825,-0.0340223579322397,
0.0685438237634769));
#77417=CARTESIAN_POINT('Ctrl Pts',(0.00643836751905516,-0.0339125849573575,
0.06856600353082));
#77418=CARTESIAN_POINT('Ctrl Pts',(0.00636155713141065,-0.0338030433565231,
0.0685897681355124));
#77419=CARTESIAN_POINT('Ctrl Pts',(0.00628535568145572,-0.0336938721132327,
0.0686150784791725));
#77420=CARTESIAN_POINT('Ctrl Pts',(0.00646425730120076,-0.0340223579322397,
0.0686447976337542));
#77421=CARTESIAN_POINT('Ctrl Pts',(0.0063883262023997,-0.0339125849573575,
0.0686676868102363));
#77422=CARTESIAN_POINT('Ctrl Pts',(0.00631292221226871,-0.0338030433565231,
0.0686921315000647));
#77423=CARTESIAN_POINT('Ctrl Pts',(0.00623813898867689,-0.0336938721132327,
0.068718091894577));
#77424=CARTESIAN_POINT('',(0.00630938662001274,-0.0336938721132427,0.0685626497953968));
#77425=CARTESIAN_POINT('Ctrl Pts',(0.00639205581550063,-0.03371081206627,
0.068405339549261));
#77426=CARTESIAN_POINT('Ctrl Pts',(0.00640446630652668,-0.0337611408994182,
0.0684465089036657));
#77427=CARTESIAN_POINT('Ctrl Pts',(0.00641665033362538,-0.0338121088781064,
0.0684869270086906));
#77428=CARTESIAN_POINT('Ctrl Pts',(0.00644057655943417,-0.0339153382773244,
0.068566297540269));
#77429=CARTESIAN_POINT('Ctrl Pts',(0.00645231039752609,-0.0339675637691194,
0.068605222232122));
#77430=CARTESIAN_POINT('Ctrl Pts',(0.00646382071677454,-0.0340204018098272,
0.0686434054443299));
#77431=CARTESIAN_POINT('Ctrl Pts',(0.00634631765569402,-0.0341934961088741,
0.0686817371991245));
#77432=CARTESIAN_POINT('Ctrl Pts',(0.00623326563024816,-0.0340287516182428,
0.0687184848781279));
#77433=CARTESIAN_POINT('Ctrl Pts',(0.00612182901504797,-0.0338644633275951,
0.0687598736829219));
#77434=CARTESIAN_POINT('Ctrl Pts',(0.00634453065372386,-0.0341934961088741,
0.0686807780297745));
#77435=CARTESIAN_POINT('Ctrl Pts',(0.00623145879820733,-0.0340287516182428,
0.0687175626536358));
#77436=CARTESIAN_POINT('Ctrl Pts',(0.0061200038968399,-0.0338644633275951,
0.0687589891913109));
#77437=CARTESIAN_POINT('Ctrl Pts',(0.00604678175384191,-0.0341934961088741,
0.0685209619671487));
#77438=CARTESIAN_POINT('Ctrl Pts',(0.00593040582713559,-0.0340287516182428,
0.068563902314945));
#77439=CARTESIAN_POINT('Ctrl Pts',(0.00581590409858431,-0.0338644633275951,
0.0686116158763756));
#77440=CARTESIAN_POINT('',(0.00603476276706981,-0.0341764758832379,0.0685254113192004));
#77441=CARTESIAN_POINT('',(0.00604678175384194,-0.034193496108874,0.0685209619671487));
#77442=CARTESIAN_POINT('Origin',(0.0113196153181899,-0.0345621026496214,
0.0842254642322378));
#77443=CARTESIAN_POINT('Ctrl Pts',(0.00603476276886755,-0.0341764758837464,
0.0685254113194495));
#77444=CARTESIAN_POINT('Ctrl Pts',(0.00604970775821637,-0.0341260050040501,
0.0685656499761387));
#77445=CARTESIAN_POINT('Ctrl Pts',(0.00606439300421029,-0.034074926914832,
0.0686051891767446));
#77446=CARTESIAN_POINT('Ctrl Pts',(0.00609325521875247,-0.0339715436306764,
0.0686828993729217));
#77447=CARTESIAN_POINT('Ctrl Pts',(0.00610742123204215,-0.0339192778236902,
0.068721040889147));
#77448=CARTESIAN_POINT('Ctrl Pts',(0.0061213322405873,-0.0338664212854632,
0.0687584956454671));
#77449=CARTESIAN_POINT('',(0.00619565620379288,-0.0341934961088841,0.0686008699984716));
#77450=CARTESIAN_POINT('Origin',(0.00812378219310841,-0.0315241814719618,
0.07415));
#77451=CARTESIAN_POINT('',(0.00603476276653722,-0.0342105180190382,0.0685254113201839));
#77452=CARTESIAN_POINT('',(0.00602275330947995,-0.0341934961088739,0.0685298863329841));
#77453=CARTESIAN_POINT('Origin',(0.0113636440338325,-0.0345621709122607,
0.0842146942021983));
#77454=CARTESIAN_POINT('Origin',(0.012279732518218,-0.0345621036048912,
0.0838688707717797));
#77455=CARTESIAN_POINT('Origin',(0.0122393463298125,-0.0345621718614647,
0.0838894481597944));
#77456=CARTESIAN_POINT('Ctrl Pts',(0.00624039032944951,-0.0346945769586966,
0.0687157256841039));
#77457=CARTESIAN_POINT('Ctrl Pts',(0.00612656727813833,-0.0345275153362944,
0.0687551740807572));
#77458=CARTESIAN_POINT('Ctrl Pts',(0.00601395540212098,-0.0343603235965185,
0.0687982123109832));
#77459=CARTESIAN_POINT('Ctrl Pts',(0.00590288586550722,-0.0341934961088739,
0.0688447081367231));
#77460=CARTESIAN_POINT('Ctrl Pts',(0.00616180232339275,-0.0346945769586966,
0.0687449139289149));
#77461=CARTESIAN_POINT('Ctrl Pts',(0.00604859063155547,-0.0345275153362944,
0.06878600838282));
#77462=CARTESIAN_POINT('Ctrl Pts',(0.00593664204012637,-0.0343603235965185,
0.0688306738693598));
#77463=CARTESIAN_POINT('Ctrl Pts',(0.00582628567998455,-0.0341934961088739,
0.0688787733669295));
#77464=CARTESIAN_POINT('Ctrl Pts',(0.00608321431733598,-0.0346945769586966,
0.0687741021737259));
#77465=CARTESIAN_POINT('Ctrl Pts',(0.0059706139849726,-0.0345275153362944,
0.0688168426848828));
#77466=CARTESIAN_POINT('Ctrl Pts',(0.00585932867813176,-0.0343603235965185,
0.0688631354277364));
#77467=CARTESIAN_POINT('Ctrl Pts',(0.00574968549446188,-0.0341934961088739,
0.068912838597136));
#77468=CARTESIAN_POINT('Ctrl Pts',(0.00600462631127922,-0.0346945769586966,
0.068803290418537));
#77469=CARTESIAN_POINT('Ctrl Pts',(0.00589263733838974,-0.0345275153362944,
0.0688476769869456));
#77470=CARTESIAN_POINT('Ctrl Pts',(0.00578201531613716,-0.0343603235965185,
0.068895596986113));
#77471=CARTESIAN_POINT('Ctrl Pts',(0.00567308530893922,-0.0341934961088739,
0.0689469038273425));
#77472=CARTESIAN_POINT('',(0.00600462631126852,-0.0346945769586966,0.0688032904185411));
#77473=CARTESIAN_POINT('',(0.0057867482589667,-0.0343667727832908,0.0688948694220707));
#77474=CARTESIAN_POINT('Origin',(0.0123695229635273,-0.0345626461566603,
0.084365595431727));
#77475=CARTESIAN_POINT('Origin',(0.00129574829283271,-0.0341934771027846,
0.0587962767159609));
#77476=CARTESIAN_POINT('',(0.00590151527665439,-0.0341934961088739,0.0688453176577636));
#77477=CARTESIAN_POINT('',(0.00584440778473561,-0.034193496108884,0.0688707142001683));
#77478=CARTESIAN_POINT('',(0.00612133224108813,-0.0345211942962717,0.0687584956469073));
#77479=CARTESIAN_POINT('Origin',(0.011917638240633,-0.0345625596118878,
0.0845298829433527));
#77480=CARTESIAN_POINT('',(0.00612180524213312,-0.0346945769586885,0.0687597691804744));
#77481=CARTESIAN_POINT('Origin',(0.00226980493413639,-0.0346945685853964,
0.0583884332561724));
#77482=CARTESIAN_POINT('',(0.00606321577671083,-0.0346945769587026,0.0687815297995178));
#77483=CARTESIAN_POINT('Ctrl Pts',(0.00625683350729417,-0.0345231616327842,
0.0684478510538082));
#77484=CARTESIAN_POINT('Ctrl Pts',(0.00617823741205449,-0.0344132092796988,
0.0684735843129886));
#77485=CARTESIAN_POINT('Ctrl Pts',(0.00610017764418005,-0.0343032738558979,
0.0685009419426854));
#77486=CARTESIAN_POINT('Ctrl Pts',(0.00602275330947989,-0.0341934961088739,
0.0685298863329841));
#77487=CARTESIAN_POINT('Ctrl Pts',(0.00621184128588049,-0.0345231616327842,
0.0685518550736859));
#77488=CARTESIAN_POINT('Ctrl Pts',(0.00613467873962887,-0.0344132092796988,
0.0685782084872945));
#77489=CARTESIAN_POINT('Ctrl Pts',(0.00605806527418315,-0.0343032738558979,
0.0686061565875924));
#77490=CARTESIAN_POINT('Ctrl Pts',(0.00598209812309473,-0.0341934961088739,
0.068635661055666));
#77491=CARTESIAN_POINT('Ctrl Pts',(0.00616684906446681,-0.0345231616327842,
0.0686558590935636));
#77492=CARTESIAN_POINT('Ctrl Pts',(0.00609112006720326,-0.0344132092796988,
0.0686828326616004));
#77493=CARTESIAN_POINT('Ctrl Pts',(0.00601595290418624,-0.0343032738558979,
0.0687113712324993));
#77494=CARTESIAN_POINT('Ctrl Pts',(0.00594144293670958,-0.0341934961088739,
0.068741435778348));
#77495=CARTESIAN_POINT('Ctrl Pts',(0.00612185684305314,-0.0345231616327842,
0.0687598631134413));
#77496=CARTESIAN_POINT('Ctrl Pts',(0.00604756139477765,-0.0344132092796988,
0.0687874568359063));
#77497=CARTESIAN_POINT('Ctrl Pts',(0.00597384053418934,-0.0343032738558979,
0.0688165858774063));
#77498=CARTESIAN_POINT('Ctrl Pts',(0.00590078775032442,-0.0341934961088739,
0.0688472105010299));
#77499=CARTESIAN_POINT('',(0.00596213429307717,-0.0341934961088839,0.0686876019953838));
#77500=CARTESIAN_POINT('Ctrl Pts',(0.0060347627677351,-0.0342105180195403,
0.0685254113234173));
#77501=CARTESIAN_POINT('Ctrl Pts',(0.00604972454526662,-0.0342610556241142,
0.0685656952209547));
#77502=CARTESIAN_POINT('Ctrl Pts',(0.00606441784143634,-0.0343122189869805,
0.0686052562447796));
#77503=CARTESIAN_POINT('Ctrl Pts',(0.00609328035092692,-0.0344158119695204,
0.0686829672234745));
#77504=CARTESIAN_POINT('Ctrl Pts',(0.00610743775925481,-0.0344681990450104,
0.0687210853939441));
#77505=CARTESIAN_POINT('Ctrl Pts',(0.00612133224109043,-0.0345211942962538,
0.0687584956469318));
#77506=CARTESIAN_POINT('Ctrl Pts',(0.00600646956223161,-0.0346945769586932,
0.0688041352814491));
#77507=CARTESIAN_POINT('Ctrl Pts',(0.0059328008443355,-0.0345846629175836,
0.0688333129197011));
#77508=CARTESIAN_POINT('Ctrl Pts',(0.00585972292521789,-0.0344746925049831,
0.0688640189803979));
#77509=CARTESIAN_POINT('Ctrl Pts',(0.00578732927824432,-0.0343648066252516,
0.0688962137326933));
#77510=CARTESIAN_POINT('Ctrl Pts',(0.00590345638056552,-0.0346945769586932,
0.0687569186958054));
#77511=CARTESIAN_POINT('Ctrl Pts',(0.00582913699425355,-0.0345846629175836,
0.0687875159077689));
#77512=CARTESIAN_POINT('Ctrl Pts',(0.0057554376517857,-0.0344746925049831,
0.0688196552401995));
#77513=CARTESIAN_POINT('Ctrl Pts',(0.00568245261518233,-0.0343648066252516,
0.0688532951224898));
#77514=CARTESIAN_POINT('Ctrl Pts',(0.00580044319889943,-0.0346945769586932,
0.0687097021101616));
#77515=CARTESIAN_POINT('Ctrl Pts',(0.00572547314417161,-0.0345846629175836,
0.0687417188958366));
#77516=CARTESIAN_POINT('Ctrl Pts',(0.0056511523783535,-0.0344746925049831,
0.068775291500001));
#77517=CARTESIAN_POINT('Ctrl Pts',(0.00557757595212033,-0.0343648066252516,
0.0688103765122862));
#77518=CARTESIAN_POINT('Ctrl Pts',(0.00569743001723334,-0.0346945769586932,
0.0686624855245178));
#77519=CARTESIAN_POINT('Ctrl Pts',(0.00562180929408966,-0.0345846629175836,
0.0686959218839044));
#77520=CARTESIAN_POINT('Ctrl Pts',(0.00554686710492131,-0.0344746925049831,
0.0687309277598026));
#77521=CARTESIAN_POINT('Ctrl Pts',(0.00547269928905834,-0.0343648066252516,
0.0687674579020826));
#77522=CARTESIAN_POINT('',(0.00568571412388135,-0.0346775396663606,0.0686676807763232));
#77523=CARTESIAN_POINT('',(0.00569743001723021,-0.0346945769586886,0.0686624855245192));
#77524=CARTESIAN_POINT('Origin',(0.0125709383820059,-0.0345626618064187,
0.0837741889178235));
#77525=CARTESIAN_POINT('Ctrl Pts',(0.00568571412524865,-0.0346775396659408,
0.0686676807794041));
#77526=CARTESIAN_POINT('Ctrl Pts',(0.00570317000872294,-0.0346269748528332,
0.0687069326472027));
#77527=CARTESIAN_POINT('Ctrl Pts',(0.00572031551976361,-0.0345757904815517,
0.068745486601444));
#77528=CARTESIAN_POINT('Ctrl Pts',(0.00575400050052634,-0.0344721679344607,
0.0688212317456897));
#77529=CARTESIAN_POINT('Ctrl Pts',(0.00577052639654102,-0.0344197716860284,
0.068858392413414));
#77530=CARTESIAN_POINT('Ctrl Pts',(0.00578674825918659,-0.034366772783177,
0.0688948694218075));
#77531=CARTESIAN_POINT('',(0.00585102816425936,-0.0346945769587026,0.0687328879715402));
#77532=CARTESIAN_POINT('Origin',(0.00812378219310841,-0.0315241814719618,
0.07415));
#77533=CARTESIAN_POINT('',(0.00568571412392511,-0.0347116136489625,0.0686676807764219));
#77534=CARTESIAN_POINT('',(0.0056740093530817,-0.0346945769586885,0.0686729010386621));
#77535=CARTESIAN_POINT('Origin',(0.0126115469653707,-0.034562668844092,
0.0837540846355363));
#77536=CARTESIAN_POINT('Origin',(0.0122918590496367,-0.0345626626357112,
0.0838983018354193));
#77537=CARTESIAN_POINT('Origin',(0.0122497303169883,-0.0345626697496677,
0.0839149876111518));
#77538=CARTESIAN_POINT('Ctrl Pts',(0.00593716783041815,-0.0352450361874068,
0.0688304624021912));
#77539=CARTESIAN_POINT('Ctrl Pts',(0.00573653817773724,-0.0349452760959493,
0.0689129319161419));
#77540=CARTESIAN_POINT('Ctrl Pts',(0.00554269043400859,-0.034644428984174,
0.0690102793892341));
#77541=CARTESIAN_POINT('Ctrl Pts',(0.00593485429329546,-0.0352450361874068,
0.0688314739213368));
#77542=CARTESIAN_POINT('Ctrl Pts',(0.00573426279068515,-0.0349452760959493,
0.0689140306917719));
#77543=CARTESIAN_POINT('Ctrl Pts',(0.00554045966116219,-0.034644428984174,
0.0690114622998426));
#77544=CARTESIAN_POINT('Ctrl Pts',(0.00570579121184181,-0.0352450361874068,
0.0689316243317951));
#77545=CARTESIAN_POINT('Ctrl Pts',(0.00550897694394346,-0.0349452760959493,
0.0690228203581108));
#77546=CARTESIAN_POINT('Ctrl Pts',(0.00531959106250815,-0.034644428984174,
0.0691285821620719));
#77547=CARTESIAN_POINT('Ctrl Pts',(0.00570350058102728,-0.0352450361874068,
0.0689326258358997));
#77548=CARTESIAN_POINT('Ctrl Pts',(0.00550672408547605,-0.0349452760959493,
0.0690239082547742));
#77549=CARTESIAN_POINT('Ctrl Pts',(0.00531738237652162,-0.034644428984174,
0.0691297533606941));
#77550=CARTESIAN_POINT('',(0.00567311357158921,-0.035195163405329,0.0689468878918456));
#77551=CARTESIAN_POINT('',(0.00546138748269816,-0.0348678972925388,0.0690519827966178));
#77552=CARTESIAN_POINT('Origin',(0.0135887839607815,-0.0345636767887483,
0.0837031292376524));
#77553=CARTESIAN_POINT('Origin',(0.000346240795818812,-0.0346946199341177,
0.0592573789986556));
#77554=CARTESIAN_POINT('',(0.00557281666879287,-0.0346945769330288,0.0689953225230199));
#77555=CARTESIAN_POINT('',(0.00551741651966883,-0.0346945769458128,0.0690242547639391));
#77556=CARTESIAN_POINT('',(0.00578674825928095,-0.0350221583435276,0.0688948694219706));
#77557=CARTESIAN_POINT('Origin',(0.01318341802763,-0.0345628458718028,0.0839616284697936));
#77558=CARTESIAN_POINT('',(0.00578725362435978,-0.035195136029876,0.0688959983590295));
#77559=CARTESIAN_POINT('Origin',(0.00130974932011656,-0.0351951838366708,
0.0588277413573055));
#77560=CARTESIAN_POINT('',(0.00567308530889138,-0.035195137132875,0.0689469038272366));
#77561=CARTESIAN_POINT('Ctrl Pts',(0.00590247571684632,-0.0350241211494343,
0.0685763299758115));
#77562=CARTESIAN_POINT('Ctrl Pts',(0.0058257006975568,-0.0349144232818962,
0.0686069275617508));
#77563=CARTESIAN_POINT('Ctrl Pts',(0.00574951219868282,-0.0348045283579412,
0.0686391304563295));
#77564=CARTESIAN_POINT('Ctrl Pts',(0.00567400934293733,-0.0346945769439158,
0.0686729010431994));
#77565=CARTESIAN_POINT('Ctrl Pts',(0.00586410275235436,-0.0350241211494343,
0.0686829538821318));
#77566=CARTESIAN_POINT('Ctrl Pts',(0.0057887964336569,-0.0349144232818962,
0.0687140800399236));
#77567=CARTESIAN_POINT('Ctrl Pts',(0.00571408844042096,-0.0348045283579412,
0.0687467814636396));
#77568=CARTESIAN_POINT('Ctrl Pts',(0.00564007602278193,-0.0346945769439158,
0.0687810198278122));
#77569=CARTESIAN_POINT('Ctrl Pts',(0.0058257297878624,-0.0350241211494343,
0.0687895777884522));
#77570=CARTESIAN_POINT('Ctrl Pts',(0.005751892169757,-0.0349144232818962,
0.0688212325180963));
#77571=CARTESIAN_POINT('Ctrl Pts',(0.00567866468215911,-0.0348045283579412,
0.0688544324709497));
#77572=CARTESIAN_POINT('Ctrl Pts',(0.00560614270262652,-0.0346945769439158,
0.068889138612425));
#77573=CARTESIAN_POINT('Ctrl Pts',(0.00578735682337044,-0.0350241211494343,
0.0688962016947726));
#77574=CARTESIAN_POINT('Ctrl Pts',(0.0057149879058571,-0.0349144232818962,
0.068928384996269));
#77575=CARTESIAN_POINT('Ctrl Pts',(0.00564324092389725,-0.0348045283579412,
0.0689620834782598));
#77576=CARTESIAN_POINT('Ctrl Pts',(0.00557220938247111,-0.0346945769439158,
0.0689972573970378));
#77577=CARTESIAN_POINT('',(0.00562341301116769,-0.0346945769458128,0.0688341117806416));
#77578=CARTESIAN_POINT('Ctrl Pts',(0.00568571412525632,-0.0347116136492807,
0.0686676807794213));
#77579=CARTESIAN_POINT('Ctrl Pts',(0.00570316302278226,-0.034762154653213,
0.0687069169383889));
#77580=CARTESIAN_POINT('Ctrl Pts',(0.00572030512153781,-0.0348133084096664,
0.0687454632196547));
#77581=CARTESIAN_POINT('Ctrl Pts',(0.00575399002778241,-0.0349168561544574,
0.0688212081963366));
#77582=CARTESIAN_POINT('Ctrl Pts',(0.00577051947416102,-0.0349692089015921,
0.0688583768475247));
#77583=CARTESIAN_POINT('Ctrl Pts',(0.00578674825927763,-0.0350221583435,
0.0688948694220121));
#77584=CARTESIAN_POINT('Ctrl Pts',(0.00567445092821152,-0.0351951371254906,
0.0689474287117786));
#77585=CARTESIAN_POINT('Ctrl Pts',(0.00556689103103042,-0.0350307338980921,
0.0689980670989182));
#77586=CARTESIAN_POINT('Ctrl Pts',(0.00546151598233047,-0.0348659306897792,
0.0690531077824641));
#77587=CARTESIAN_POINT('Ctrl Pts',(0.00567308530894344,-0.0351951371254906,
0.0689469038273406));
#77588=CARTESIAN_POINT('Ctrl Pts',(0.00556551456010591,-0.0350307338980921,
0.0689975704478017));
#77589=CARTESIAN_POINT('Ctrl Pts',(0.00546012983593585,-0.0348659306897792,
0.0690526397890546));
#77590=CARTESIAN_POINT('Ctrl Pts',(0.00544420609628805,-0.0351951371254906,
0.0688589326484588));
#77591=CARTESIAN_POINT('Ctrl Pts',(0.00533481659852212,-0.0350307338980921,
0.068914331203038));
#77592=CARTESIAN_POINT('Ctrl Pts',(0.00522781025547691,-0.0348659306897792,
0.0689742036058547));
#77593=CARTESIAN_POINT('Origin',(0.00299951715930774,-0.0308609197411333,
0.0643379344954456));
#77594=CARTESIAN_POINT('',(0.00557329913276375,-0.0351951371254906,0.0689085503768337));
#77595=CARTESIAN_POINT('Origin',(0.00869681970877851,-0.0351840467441122,
0.0749414377145248));
#77596=CARTESIAN_POINT('Origin',(0.00189259307280093,-0.0352322614929444,
0.0639351132346021));
#77597=CARTESIAN_POINT('',(0.00525392634011456,-0.0351951142564654,0.0691658509285475));
#77598=CARTESIAN_POINT('',(0.00514723717408231,-0.0351951372916787,0.0692303780887438));
#77599=CARTESIAN_POINT('Origin',(0.00796802316457458,-0.0352875118755706,
0.0744528703542965));
#77600=CARTESIAN_POINT('Origin',(0.0151681473551898,-0.0298325076521879,
0.0715669572699247));
#77601=CARTESIAN_POINT('Origin',(0.00680340913363432,-0.0338732635903356,
0.0658731868073005));
#77602=CARTESIAN_POINT('Ctrl Pts',(0.00873198787934537,-0.0321934096636942,
0.0684308897904884));
#77603=CARTESIAN_POINT('Ctrl Pts',(0.00862961853006105,-0.0320508460844117,
0.068420003198335));
#77604=CARTESIAN_POINT('Ctrl Pts',(0.00852703386635374,-0.0319086045662657,
0.0684118752771323));
#77605=CARTESIAN_POINT('Ctrl Pts',(0.0084244562118284,-0.031766989286728,
0.0684065053432813));
#77606=CARTESIAN_POINT('Ctrl Pts',(0.00864843728755645,-0.0321934096636942,
0.0684238377525166));
#77607=CARTESIAN_POINT('Ctrl Pts',(0.00854594171015065,-0.0320508460844117,
0.068414446676169));
#77608=CARTESIAN_POINT('Ctrl Pts',(0.00844327109505708,-0.0319086045662657,
0.0684078165346489));
#77609=CARTESIAN_POINT('Ctrl Pts',(0.00834064768544859,-0.031766989286728,
0.068403943404138));
#77610=CARTESIAN_POINT('Ctrl Pts',(0.00856488669576753,-0.0321934096636942,
0.0684167857145446));
#77611=CARTESIAN_POINT('Ctrl Pts',(0.00846226489024025,-0.0320508460844117,
0.068408890154003));
#77612=CARTESIAN_POINT('Ctrl Pts',(0.00835950832376042,-0.0319086045662657,
0.0684037577921656));
#77613=CARTESIAN_POINT('Ctrl Pts',(0.00825683915906878,-0.031766989286728,
0.0684013814649947));
#77614=CARTESIAN_POINT('Ctrl Pts',(0.00848133610397861,-0.0321934096636942,
0.0684097336765728));
#77615=CARTESIAN_POINT('Ctrl Pts',(0.00837858807032984,-0.0320508460844117,
0.068403333631837));
#77616=CARTESIAN_POINT('Ctrl Pts',(0.00827574555246378,-0.0319086045662657,
0.0683996990496821));
#77617=CARTESIAN_POINT('Ctrl Pts',(0.00817303063268897,-0.031766989286728,
0.0683988195258514));
#77618=CARTESIAN_POINT('',(0.00848283084057609,-0.0321934096636942,0.0684098598389279));
#77619=CARTESIAN_POINT('',(0.00824669644181227,-0.0318665617511272,0.0683999550370014));
#77620=CARTESIAN_POINT('Origin',(0.00682662938771915,-0.0326371944421028,
0.0850373942807947));
#77621=CARTESIAN_POINT('Origin',(0.00848095171668544,-0.0316939261509279,
0.0574412728810131));
#77622=CARTESIAN_POINT('',(0.00860723504865228,-0.032019722162187,0.0684190434914406));
#77623=CARTESIAN_POINT('Ctrl Pts',(0.00860706079400472,-0.0320197392094779,
0.0684189814414899));
#77624=CARTESIAN_POINT('Ctrl Pts',(0.00857789952515948,-0.0319792716576076,
0.0684165224113723));
#77625=CARTESIAN_POINT('Ctrl Pts',(0.00854858675646262,-0.0319386439829738,
0.0684142745005901));
#77626=CARTESIAN_POINT('Ctrl Pts',(0.00851909106836822,-0.031897909938167,
0.0684122437820222));
#77627=CARTESIAN_POINT('Ctrl Pts',(0.00848959596327579,-0.0318571766984958,
0.0684102131035927));
#77628=CARTESIAN_POINT('Ctrl Pts',(0.0084600679817806,-0.0318163871833592,
0.0684084081525476));
#77629=CARTESIAN_POINT('Ctrl Pts',(0.00843060890280958,-0.0317755399638303,
0.0684068316225805));
#77630=CARTESIAN_POINT('',(0.0086073879491624,-0.0321934096636184,0.0684203730075413));
#77631=CARTESIAN_POINT('Origin',(0.00878062777302303,-0.0324113749715919,
0.0661177156651816));
#77632=CARTESIAN_POINT('',(0.00854510939487925,-0.0321934096636663,0.0684151164232446));
#77633=CARTESIAN_POINT('Ctrl Pts',(0.00848413930783408,-0.0321934096636618,
0.0684114095488407));
#77634=CARTESIAN_POINT('Ctrl Pts',(0.00840499967311677,-0.0320835708272592,
0.0684064399433827));
#77635=CARTESIAN_POINT('Ctrl Pts',(0.00832580309687715,-0.0319739230346488,
0.0684031110111253));
#77636=CARTESIAN_POINT('Ctrl Pts',(0.00824665123251692,-0.0318646057455573,
0.0684014192346785));
#77637=CARTESIAN_POINT('Ctrl Pts',(0.00841103391569604,-0.0321934096636618,
0.0683248256796451));
#77638=CARTESIAN_POINT('Ctrl Pts',(0.008330700221943,-0.0320835708272592,
0.0683208642545198));
#77639=CARTESIAN_POINT('Ctrl Pts',(0.00825033114351001,-0.0319739230346488,
0.068318567628799));
#77640=CARTESIAN_POINT('Ctrl Pts',(0.00817002973256898,-0.0318646057455573,
0.0683179308491973));
#77641=CARTESIAN_POINT('Ctrl Pts',(0.00833792852355801,-0.0321934096636618,
0.0682382418104496));
#77642=CARTESIAN_POINT('Ctrl Pts',(0.00825640077076924,-0.0320835708272592,
0.0682352885656568));
#77643=CARTESIAN_POINT('Ctrl Pts',(0.00817485919014287,-0.0319739230346488,
0.0682340242464728));
#77644=CARTESIAN_POINT('Ctrl Pts',(0.00809340823262104,-0.0318646057455573,
0.0682344424637161));
#77645=CARTESIAN_POINT('Ctrl Pts',(0.00826482313141997,-0.0321934096636618,
0.0681516579412541));
#77646=CARTESIAN_POINT('Ctrl Pts',(0.00818210131959548,-0.0320835708272592,
0.0681497128767939));
#77647=CARTESIAN_POINT('Ctrl Pts',(0.00809938723677573,-0.0319739230346488,
0.0681494808641465));
#77648=CARTESIAN_POINT('Ctrl Pts',(0.00801678673267309,-0.0318646057455573,
0.0681509540782349));
#77649=CARTESIAN_POINT('',(0.00825201024350632,-0.0321763980308456,0.0681513703610936));
#77650=CARTESIAN_POINT('',(0.00826482313138734,-0.0321934096636185,0.0681516579412533));
#77651=CARTESIAN_POINT('Origin',(0.00728524449179297,-0.0326386231366924,
0.0846707968808568));
#77652=CARTESIAN_POINT('Ctrl Pts',(0.00825201024343353,-0.0321763980306277,
0.0681513703642613));
#77653=CARTESIAN_POINT('Ctrl Pts',(0.00825109300909574,-0.0321259596174814,
0.0681942794552726));
#77654=CARTESIAN_POINT('Ctrl Pts',(0.00825019166703981,-0.0320749164631369,
0.068236445090604));
#77655=CARTESIAN_POINT('Ctrl Pts',(0.00824842004209381,-0.031971605779391,
0.0683193233834387));
#77656=CARTESIAN_POINT('Ctrl Pts',(0.00824755044948827,-0.0319193786690104,
0.0683600037487772));
#77657=CARTESIAN_POINT('Ctrl Pts',(0.00824669644176559,-0.0318665617525284,
0.0683999550388528));
#77658=CARTESIAN_POINT('',(0.00837382698599171,-0.0321934096636664,0.0682807588901006));
#77659=CARTESIAN_POINT('Origin',(0.00812378219310841,-0.0315241814719618,
0.07415));
#77660=CARTESIAN_POINT('',(0.00825201024351424,-0.0322104233323795,0.0681513703607228));
#77661=CARTESIAN_POINT('',(0.00823919677064607,-0.0321934096636183,0.0681511101464259));
#77662=CARTESIAN_POINT('Origin',(0.00732999092986969,-0.0326387236409409,
0.084678071674358));
#77663=CARTESIAN_POINT('Origin',(0.00851197086234812,-0.0326386241790837,
0.0846970221127516));
#77664=CARTESIAN_POINT('Origin',(0.00846695424061251,-0.0326387244629747,
0.0847023730764388));
#77665=CARTESIAN_POINT('Ctrl Pts',(0.00840774447948624,-0.0327445246967098,
0.0684056557885242));
#77666=CARTESIAN_POINT('Ctrl Pts',(0.00819109299577849,-0.032443687833936,
0.0683949459758117));
#77667=CARTESIAN_POINT('Ctrl Pts',(0.00797425028918936,-0.0321434074405927,
0.0684005856637645));
#77668=CARTESIAN_POINT('Ctrl Pts',(0.0081578400902427,-0.0327445246967098,
0.068398742306274));
#77669=CARTESIAN_POINT('Ctrl Pts',(0.00794092786028926,-0.032443687833936,
0.0683974577916846));
#77670=CARTESIAN_POINT('Ctrl Pts',(0.00772453510018328,-0.0321434074405927,
0.0684125156419567));
#77671=CARTESIAN_POINT('',(0.00812169595725582,-0.0326943950436612,0.0683986418432147));
#77672=CARTESIAN_POINT('',(0.0078854055880294,-0.0323666188837389,0.0684035835867776));
#77673=CARTESIAN_POINT('Origin',(0.00820380398097328,-0.0326395579111606,
0.0852093918711237));
#77674=CARTESIAN_POINT('Origin',(0.0074276388939793,-0.0321933825602993,
0.0573684659390598));
#77675=CARTESIAN_POINT('',(0.00801035448973432,-0.0321934096532689,0.0683997600786812));
#77676=CARTESIAN_POINT('',(0.00794790819298478,-0.0321934096584275,0.0684023505164726));
#77677=CARTESIAN_POINT('',(0.00824669644183017,-0.0325210109756238,0.0683999550360487));
#77678=CARTESIAN_POINT('Origin',(0.00772364846753187,-0.0326393129157461,
0.0851841904293704));
#77679=CARTESIAN_POINT('',(0.00824666740810641,-0.0326943950436594,0.0684013132609321));
#77680=CARTESIAN_POINT('Origin',(0.00848308765021364,-0.032694376553819,
0.0573413845913037));
#77681=CARTESIAN_POINT('',(0.00818418168269111,-0.0326943950436703,0.0683999775520834));
#77682=CARTESIAN_POINT('Ctrl Pts',(0.00848703838247985,-0.0325229783203769,
0.0681610063499027));
#77683=CARTESIAN_POINT('Ctrl Pts',(0.0084044802359839,-0.032413025309245,
0.0681559988712761));
#77684=CARTESIAN_POINT('Ctrl Pts',(0.00832183102492051,-0.0323031222208069,
0.0681526999734455));
#77685=CARTESIAN_POINT('Ctrl Pts',(0.00823919676616269,-0.0321934096576658,
0.0681511101463396));
#77686=CARTESIAN_POINT('Ctrl Pts',(0.00840691921866812,-0.0325229783203769,
0.0682411441176928));
#77687=CARTESIAN_POINT('Ctrl Pts',(0.00832546576954866,-0.032413025309245,
0.0682372410799873));
#77688=CARTESIAN_POINT('Ctrl Pts',(0.00824394393509196,-0.0323031222208069,
0.0682350236034833));
#77689=CARTESIAN_POINT('Ctrl Pts',(0.00816245823920177,-0.0321934096576658,
0.068234490843843));
#77690=CARTESIAN_POINT('Ctrl Pts',(0.00832680005485639,-0.0325229783203769,
0.068321281885483));
#77691=CARTESIAN_POINT('Ctrl Pts',(0.00824645130311342,-0.032413025309245,
0.0683184832886985));
#77692=CARTESIAN_POINT('Ctrl Pts',(0.00816605684526341,-0.0323031222208069,
0.0683173472335212));
#77693=CARTESIAN_POINT('Ctrl Pts',(0.00808571971224084,-0.0321934096576658,
0.0683178715413464));
#77694=CARTESIAN_POINT('Ctrl Pts',(0.00824668089104465,-0.0325229783203769,
0.0684014196532732));
#77695=CARTESIAN_POINT('Ctrl Pts',(0.00816743683667817,-0.032413025309245,
0.0683997254974097));
#77696=CARTESIAN_POINT('Ctrl Pts',(0.00808816975543486,-0.0323031222208069,
0.068399670863559));
#77697=CARTESIAN_POINT('Ctrl Pts',(0.00800898118527992,-0.0321934096576658,
0.0684012522388497));
#77698=CARTESIAN_POINT('',(0.00812477563068398,-0.0321934096584275,0.0682754351124071));
#77699=CARTESIAN_POINT('Ctrl Pts',(0.00825201024343501,-0.0322104233328944,
0.068151370364196));
#77700=CARTESIAN_POINT('Ctrl Pts',(0.00825109176623048,-0.0322609421831085,
0.0681943375976923));
#77701=CARTESIAN_POINT('Ctrl Pts',(0.008250189817007,-0.0323120888240131,
0.06823653163658));
#77702=CARTESIAN_POINT('Ctrl Pts',(0.00824841817864644,-0.032415652463182,
0.0683194105569602));
#77703=CARTESIAN_POINT('Ctrl Pts',(0.00824754921774712,-0.0324680267167319,
0.0683600613707999));
#77704=CARTESIAN_POINT('Ctrl Pts',(0.00824669644182473,-0.0325210109755912,
0.0683999550360919));
#77705=CARTESIAN_POINT('Origin',(0.0159123493438964,-0.0262834582512498,
0.0752642744613413));
#77706=CARTESIAN_POINT('Origin',(0.0137941110260438,-0.0342770758373598,
0.0633949811933364));
#77707=CARTESIAN_POINT('Ctrl Pts',(0.00812309880904369,-0.0326943950436605,
0.0684001059803989));
#77708=CARTESIAN_POINT('Ctrl Pts',(0.00804385449300363,-0.0325844576448134,
0.068400115398712));
#77709=CARTESIAN_POINT('Ctrl Pts',(0.00796460476350637,-0.0324744968375322,
0.0684017637200703));
#77710=CARTESIAN_POINT('Ctrl Pts',(0.00788545113079718,-0.0323646534831894,
0.068405047432015));
#77711=CARTESIAN_POINT('Ctrl Pts',(0.00804470114107275,-0.0326943950436605,
0.0683182834087079));
#77712=CARTESIAN_POINT('Ctrl Pts',(0.00796432915664294,-0.0325844576448134,
0.0683193732938186));
#77713=CARTESIAN_POINT('Ctrl Pts',(0.00788397402477391,-0.0324744968375322,
0.0683221254804718));
#77714=CARTESIAN_POINT('Ctrl Pts',(0.00780373865250897,-0.0323646534831894,
0.0683265350223373));
#77715=CARTESIAN_POINT('Ctrl Pts',(0.0079663034731018,-0.0326943950436605,
0.0682364608370169));
#77716=CARTESIAN_POINT('Ctrl Pts',(0.00788480382028225,-0.0325844576448134,
0.0682386311889251));
#77717=CARTESIAN_POINT('Ctrl Pts',(0.00780334328604146,-0.0324744968375322,
0.0682424872408734));
#77718=CARTESIAN_POINT('Ctrl Pts',(0.00772202617422075,-0.0323646534831894,
0.0682480226126596));
#77719=CARTESIAN_POINT('Ctrl Pts',(0.00788790580513086,-0.0326943950436605,
0.0681546382653259));
#77720=CARTESIAN_POINT('Ctrl Pts',(0.00780527848392157,-0.0325844576448134,
0.0681578890840317));
#77721=CARTESIAN_POINT('Ctrl Pts',(0.007722712547309,-0.0324744968375322,
0.0681628490012749));
#77722=CARTESIAN_POINT('Ctrl Pts',(0.00764031369593254,-0.0323646534831894,
0.0681695102029818));
#77723=CARTESIAN_POINT('',(0.00787510014324013,-0.0326773559991159,0.0681551557803234));
#77724=CARTESIAN_POINT('',(0.00788790580513014,-0.0326943950436595,0.0681546382653259));
#77725=CARTESIAN_POINT('Origin',(0.00861353130803579,-0.0326395669917778,
0.084743947908737));
#77726=CARTESIAN_POINT('Ctrl Pts',(0.00787510014337409,-0.032677355998742,
0.0681551557836675));
#77727=CARTESIAN_POINT('Ctrl Pts',(0.00787688043461156,-0.0326267922585957,
0.0681980723055467));
#77728=CARTESIAN_POINT('Ctrl Pts',(0.00787862917147246,-0.0325756109579314,
0.0682402281630666));
#77729=CARTESIAN_POINT('Ctrl Pts',(0.00788206502470259,-0.0324719985462369,
0.0683230544261068));
#77730=CARTESIAN_POINT('Ctrl Pts',(0.00788375076304503,-0.0324196091621773,
0.0683636916122777));
#77731=CARTESIAN_POINT('Ctrl Pts',(0.00788540558803144,-0.0323666188837756,
0.0684035835868263));
#77732=CARTESIAN_POINT('',(0.00800480088120298,-0.0326943950436704,0.0682766400542803));
#77733=CARTESIAN_POINT('Origin',(0.00812378219310841,-0.0315241814719618,
0.07415));
#77734=CARTESIAN_POINT('',(0.00787510014324197,-0.0327114338379884,0.0681551557803679));
#77735=CARTESIAN_POINT('',(0.00786229561583587,-0.0326943950436593,0.0681557006439515));
#77736=CARTESIAN_POINT('Origin',(0.00865876418508889,-0.0326395670442531,
0.0847412958988538));
#77737=CARTESIAN_POINT('Origin',(0.0085131371617776,-0.0326395678070698,
0.0847481145319865));
#77738=CARTESIAN_POINT('Origin',(0.00846784000449152,-0.0326395679529206,
0.0847492139789644));
#77739=CARTESIAN_POINT('Ctrl Pts',(0.00804645456722067,-0.0332451089994434,
0.0683991613273998));
#77740=CARTESIAN_POINT('Ctrl Pts',(0.00782955813807205,-0.0329451141710254,
0.0684020777865259));
#77741=CARTESIAN_POINT('Ctrl Pts',(0.00761349756841127,-0.0326442513127493,
0.0684213234860225));
#77742=CARTESIAN_POINT('Ctrl Pts',(0.00779660926602679,-0.0332451089994434,
0.0684079548176817));
#77743=CARTESIAN_POINT('Ctrl Pts',(0.00758004448879027,-0.0329451141710254,
0.0684202943465118));
#77744=CARTESIAN_POINT('Ctrl Pts',(0.00736502441298541,-0.0326442513127493,
0.0684489113643881));
#77745=CARTESIAN_POINT('Ctrl Pts',(0.00779411081301486,-0.0332451089994434,
0.0684080427525845));
#77746=CARTESIAN_POINT('Ctrl Pts',(0.00757754935229745,-0.0329451141710254,
0.0684204765121117));
#77747=CARTESIAN_POINT('Ctrl Pts',(0.00736253968143116,-0.0326442513127493,
0.0684491872431718));
#77748=CARTESIAN_POINT('',(0.0077605693073013,-0.0331951640388616,0.0684101218305974));
#77749=CARTESIAN_POINT('',(0.00752505548329177,-0.0328677532354991,0.0684298906132163));
#77750=CARTESIAN_POINT('Origin',(0.00958459726176004,-0.0326402808280928,
0.0850746101061591));
#77751=CARTESIAN_POINT('Origin',(0.00637373518186439,-0.0326944278779095,
0.05743403482466));
#77752=CARTESIAN_POINT('',(0.00764951775477939,-0.0326943950436593,0.0684182290483187));
#77753=CARTESIAN_POINT('',(0.00758735733926293,-0.0326943950436694,0.0684247354099524));
#77754=CARTESIAN_POINT('',(0.0078854055880323,-0.0330220786163545,0.0684035835867775));
#77755=CARTESIAN_POINT('Origin',(0.00911071887922066,-0.0326396682763578,
0.0851558007694508));
#77756=CARTESIAN_POINT('',(0.00788546189524771,-0.0331951640388588,0.0684049409545569));
#77757=CARTESIAN_POINT('Origin',(0.0074282336680204,-0.0331952026560223,
0.0573827673067081));
#77758=CARTESIAN_POINT('',(0.00782301560128451,-0.0331951640388702,0.0684075313925871));
#77759=CARTESIAN_POINT('Ctrl Pts',(0.00811026859573352,-0.0330240426238172,
0.0681500152181272));
#77760=CARTESIAN_POINT('Ctrl Pts',(0.00802761295986126,-0.032914277406352,
0.0681502013810968));
#77761=CARTESIAN_POINT('Ctrl Pts',(0.00794491996564863,-0.0328043479726691,
0.068152096359756));
#77762=CARTESIAN_POINT('Ctrl Pts',(0.00786229561583584,-0.0326943950436593,
0.0681557006439515));
#77763=CARTESIAN_POINT('Ctrl Pts',(0.00803533945271779,-0.0330240426238172,
0.0682350255675641));
#77764=CARTESIAN_POINT('Ctrl Pts',(0.00795385491723059,-0.032914277406352,
0.0682362439524786));
#77765=CARTESIAN_POINT('Ctrl Pts',(0.00787235494615025,-0.0328043479726691,
0.0682391474577668));
#77766=CARTESIAN_POINT('Ctrl Pts',(0.00779094404944688,-0.0326943950436593,
0.0682437352391871));
#77767=CARTESIAN_POINT('Ctrl Pts',(0.00796041030970206,-0.0330240426238172,
0.068320035917001));
#77768=CARTESIAN_POINT('Ctrl Pts',(0.00788009687459993,-0.032914277406352,
0.0683222865238605));
#77769=CARTESIAN_POINT('Ctrl Pts',(0.00779978992665187,-0.0328043479726691,
0.0683261985557777));
#77770=CARTESIAN_POINT('Ctrl Pts',(0.00771959248305792,-0.0326943950436593,
0.0683317698344226));
#77771=CARTESIAN_POINT('Ctrl Pts',(0.00788548116668633,-0.0330240426238172,
0.0684050462664379));
#77772=CARTESIAN_POINT('Ctrl Pts',(0.00780633883196926,-0.032914277406352,
0.0684083290952423));
#77773=CARTESIAN_POINT('Ctrl Pts',(0.00772722490715349,-0.0328043479726691,
0.0684132496537885));
#77774=CARTESIAN_POINT('Ctrl Pts',(0.00764824091666895,-0.0326943950436593,
0.0684198044296582));
#77775=CARTESIAN_POINT('',(0.00775590668531764,-0.0326943950436693,0.0682869648461451));
#77776=CARTESIAN_POINT('Ctrl Pts',(0.00787510014337457,-0.0327114338383341,
0.0681551557836757));
#77777=CARTESIAN_POINT('Ctrl Pts',(0.00787688013849059,-0.0327619876830805,
0.0681980651671147));
#77778=CARTESIAN_POINT('Ctrl Pts',(0.00787862873071166,-0.0328131562603977,
0.0682402175378805));
#77779=CARTESIAN_POINT('Ctrl Pts',(0.0078820645807877,-0.0329167375858776,
0.0683230437248869));
#77780=CARTESIAN_POINT('Ctrl Pts',(0.00788375046962117,-0.0329691088920625,
0.0683636845388643));
#77781=CARTESIAN_POINT('Ctrl Pts',(0.00788540558803146,-0.0330220786163187,
0.0684035835868251));
#77782=CARTESIAN_POINT('Ctrl Pts',(0.00776206156301519,-0.0331951640388604,
0.0684114952120716));
#77783=CARTESIAN_POINT('Ctrl Pts',(0.0076434216557117,-0.0330306422010619,
0.068418973554185));
#77784=CARTESIAN_POINT('Ctrl Pts',(0.00752519221312171,-0.0328657861914644,
0.0684313490182411));
#77785=CARTESIAN_POINT('Ctrl Pts',(0.00776056930730447,-0.0331951640388604,
0.0684101218305973));
#77786=CARTESIAN_POINT('Ctrl Pts',(0.00764190100621953,-0.0330306422010619,
0.0684176310241408));
#77787=CARTESIAN_POINT('Ctrl Pts',(0.00752364446923242,-0.0328657861914644,
0.0684300384868095));
#77788=CARTESIAN_POINT('Ctrl Pts',(0.0075119193752158,-0.0331951640388604,
0.0681812795431449));
#77789=CARTESIAN_POINT('Ctrl Pts',(0.00738851990655781,-0.0330306422010619,
0.0681939294146148));
#77790=CARTESIAN_POINT('Ctrl Pts',(0.00726574871437195,-0.0328657861914644,
0.0682116687066678));
#77791=CARTESIAN_POINT('',(0.00749917147791584,-0.0331781648281892,0.0681826001097433));
#77792=CARTESIAN_POINT('',(0.00751191937521466,-0.0331951640388588,0.068181279543145));
#77793=CARTESIAN_POINT('Origin',(0.00992597004207064,-0.0326412092057475,
0.0845257066684922));
#77794=CARTESIAN_POINT('Ctrl Pts',(0.00749917147951614,-0.033178164828644,
0.0681826001106365));
#77795=CARTESIAN_POINT('Ctrl Pts',(0.0075036460989602,-0.0331276811546782,
0.0682253495708871));
#77796=CARTESIAN_POINT('Ctrl Pts',(0.00750803995426746,-0.0330765663497791,
0.068267327104754));
#77797=CARTESIAN_POINT('Ctrl Pts',(0.00751666975043236,-0.032973061446316,
0.0683497744026723));
#77798=CARTESIAN_POINT('Ctrl Pts',(0.0075209021997093,-0.0329207133373781,
0.0683902108603701));
#77799=CARTESIAN_POINT('Ctrl Pts',(0.00752505549628465,-0.0328677532289351,
0.0684298906030954));
#77800=CARTESIAN_POINT('',(0.00763624434126798,-0.0331951640388702,0.0682957006868812));
#77801=CARTESIAN_POINT('Origin',(0.00812378219310841,-0.0315241814719618,
0.07415));
#77802=CARTESIAN_POINT('',(0.007499171477434,-0.033212160714424,0.068182600111353));
#77803=CARTESIAN_POINT('',(0.00748642642908472,-0.0331951640388587,0.0681839479025));
#77804=CARTESIAN_POINT('Origin',(0.00996957324839171,-0.0326413653794834,
0.0845132577386242));
#77805=CARTESIAN_POINT('Origin',(0.00850917857750277,-0.0326412099826809,
0.0846740047827594));
#77806=CARTESIAN_POINT('Origin',(0.00846394233505875,-0.0326413662553115,
0.0846708507653181));
#77807=CARTESIAN_POINT('Ctrl Pts',(0.00768552977863837,-0.0337436976235975,
0.0684153631482707));
#77808=CARTESIAN_POINT('Ctrl Pts',(0.00763395158568592,-0.0336723290703325,
0.0684193048569054));
#77809=CARTESIAN_POINT('Ctrl Pts',(0.00758245263578412,-0.033601104548885,
0.0684241736569848));
#77810=CARTESIAN_POINT('Ctrl Pts',(0.00741802669011486,-0.0333736987606857,
0.068439718771183));
#77811=CARTESIAN_POINT('Ctrl Pts',(0.00725476377368111,-0.0331450831799191,
0.0684646739770972));
#77812=CARTESIAN_POINT('Ctrl Pts',(0.00743672954929019,-0.0337436976235975,
0.0684398263017117));
#77813=CARTESIAN_POINT('Ctrl Pts',(0.00738537138164728,-0.0336723290703325,
0.068446005757316));
#77814=CARTESIAN_POINT('Ctrl Pts',(0.00733413267147486,-0.033601104548885,
0.0684531079847882));
#77815=CARTESIAN_POINT('Ctrl Pts',(0.00717053761971092,-0.0333736987606857,
0.068475783990235));
#77816=CARTESIAN_POINT('Ctrl Pts',(0.00700851343959128,-0.0331450831799191,
0.0685078106547699));
#77817=CARTESIAN_POINT('Ctrl Pts',(0.00743424154699671,-0.0337436976235975,
0.0684400709332462));
#77818=CARTESIAN_POINT('Ctrl Pts',(0.0073828855796069,-0.0336723290703325,
0.0684462727663201));
#77819=CARTESIAN_POINT('Ctrl Pts',(0.00733164947183177,-0.033601104548885,
0.0684533973280662));
#77820=CARTESIAN_POINT('Ctrl Pts',(0.00716806272900688,-0.0333736987606857,
0.0684761446424256));
#77821=CARTESIAN_POINT('Ctrl Pts',(0.00700605093625038,-0.0331450831799191,
0.0685082420215466));
#77822=CARTESIAN_POINT('',(0.00740087609265772,-0.0336938721132548,0.0684442544948156));
#77823=CARTESIAN_POINT('',(0.00716706829378607,-0.0333679870047996,0.0684787723097453));
#77824=CARTESIAN_POINT('Ctrl Pts',(0.00740087609268289,-0.0336938721132527,
0.0684442544948124));
#77825=CARTESIAN_POINT('Ctrl Pts',(0.00737860389135478,-0.0336629187933872,
0.0684470763364449));
#77826=CARTESIAN_POINT('Ctrl Pts',(0.00735635533622876,-0.033631995230101,
0.0684500276882784));
#77827=CARTESIAN_POINT('Ctrl Pts',(0.00733413267148733,-0.033601104548892,
0.0684531079847866));
#77828=CARTESIAN_POINT('Ctrl Pts',(0.00727836840148316,-0.0335235892595422,
0.0684608375027439));
#77829=CARTESIAN_POINT('Ctrl Pts',(0.00722266809226004,-0.0334458668665538,
0.0684693928415299));
#77830=CARTESIAN_POINT('Ctrl Pts',(0.0071670683053924,-0.0333679869962462,
0.068478772307524));
#77831=CARTESIAN_POINT('Ctrl Pts',(0.00716702433611697,-0.0333679692470407,
0.0684787790278612));
#77832=CARTESIAN_POINT('Ctrl Pts',(0.00716710557115595,-0.0333391895416172,
0.0684792249411365));
#77833=CARTESIAN_POINT('Ctrl Pts',(0.00716716965538581,-0.0333104081131861,
0.0684795585929379));
#77834=CARTESIAN_POINT('Ctrl Pts',(0.00716725992084898,-0.0332532698396013,
0.0684799991934275));
#77835=CARTESIAN_POINT('Ctrl Pts',(0.00716728665582308,-0.0332249171946172,
0.068480109450876));
#77836=CARTESIAN_POINT('Ctrl Pts',(0.00716729406987529,-0.0331960985338305,
0.0684801119224179));
#77837=CARTESIAN_POINT('Ctrl Pts',(0.00716729418510157,-0.033195631258691,
0.0684801119331561));
#77838=CARTESIAN_POINT('Ctrl Pts',(0.00716729429479814,-0.0331951640388587,
0.0684801119146507));
#77839=CARTESIAN_POINT('',(0.00729055273143395,-0.0331951640388587,0.0684593186994703));
#77840=CARTESIAN_POINT('',(0.00722892351312492,-0.0331951640388687,0.0684697153070706));
#77841=CARTESIAN_POINT('',(0.00752505549800226,-0.033521636656774,0.068429890618188));
#77842=CARTESIAN_POINT('Origin',(0.0104586076404711,-0.0326434571524804,
0.0848239424923361));
#77843=CARTESIAN_POINT('',(0.00752519692372646,-0.0336938721132327,0.0684312417715662));
#77844=CARTESIAN_POINT('Origin',(0.00638834720438303,-0.0336938867896287,
0.0575700078327438));
#77845=CARTESIAN_POINT('',(0.00746303650820209,-0.0336938721132538,0.0684377481332009));
#77846=CARTESIAN_POINT('Ctrl Pts',(0.00773355214107778,-0.0335235895815172,
0.0681627034058339));
#77847=CARTESIAN_POINT('Ctrl Pts',(0.00765112521555684,-0.0334144449262748,
0.0681680756907924));
#77848=CARTESIAN_POINT('Ctrl Pts',(0.00756871457884892,-0.0333049234473147,
0.0681751570261036));
#77849=CARTESIAN_POINT('Ctrl Pts',(0.00748642642908477,-0.0331951640388587,
0.0681839479024999));
#77850=CARTESIAN_POINT('Ctrl Pts',(0.00766410861326214,-0.0335235895815172,
0.0682522509849771));
#77851=CARTESIAN_POINT('Ctrl Pts',(0.00758291448647106,-0.0334144449262748,
0.0682585792968177));
#77852=CARTESIAN_POINT('Ctrl Pts',(0.00750175781562528,-0.0333049234473147,
0.068266592288676));
#77853=CARTESIAN_POINT('Ctrl Pts',(0.00742074330333155,-0.0331951640388587,
0.0682762891147356));
#77854=CARTESIAN_POINT('Ctrl Pts',(0.00759466508544649,-0.0335235895815172,
0.0683417985641202));
#77855=CARTESIAN_POINT('Ctrl Pts',(0.00751470375738527,-0.0334144449262748,
0.0683490829028429));
#77856=CARTESIAN_POINT('Ctrl Pts',(0.00743480105240163,-0.0333049234473147,
0.0683580275512484));
#77857=CARTESIAN_POINT('Ctrl Pts',(0.00735506017757833,-0.0331951640388587,
0.0683686303269713));
#77858=CARTESIAN_POINT('Ctrl Pts',(0.00752522155763084,-0.0335235895815172,
0.0684313461432633));
#77859=CARTESIAN_POINT('Ctrl Pts',(0.00744649302829949,-0.0334144449262748,
0.0684395865088681));
#77860=CARTESIAN_POINT('Ctrl Pts',(0.00736784428917799,-0.0333049234473147,
0.0684494628138208));
#77861=CARTESIAN_POINT('Ctrl Pts',(0.00728937705182512,-0.0331951640388587,
0.068460971539207));
#77862=CARTESIAN_POINT('',(0.00738848958026934,-0.0331951640388687,0.0683216333009952));
#77863=CARTESIAN_POINT('Ctrl Pts',(0.00749917147775533,-0.0332121607145994,
0.0681826001144633));
#77864=CARTESIAN_POINT('Ctrl Pts',(0.00750363855772909,-0.0332625444109625,
0.0682252776604436));
#77865=CARTESIAN_POINT('Ctrl Pts',(0.007508028662905,-0.0333135300746545,
0.0682672198053353));
#77866=CARTESIAN_POINT('Ctrl Pts',(0.00751665840847482,-0.0334167203140651,
0.0683496665861217));
#77867=CARTESIAN_POINT('Ctrl Pts',(0.00752089470649319,-0.0334688847587347,
0.0683901392896609));
#77868=CARTESIAN_POINT('Ctrl Pts',(0.00752505549790497,-0.0335216366562424,
0.0684298906189037));
#77869=CARTESIAN_POINT('Ctrl Pts',(0.00740245127064529,-0.0336938721132526,
0.0684455311680823));
#77870=CARTESIAN_POINT('Ctrl Pts',(0.00736906112162373,-0.0336474569765026,
0.068449753357335));
#77871=CARTESIAN_POINT('Ctrl Pts',(0.00733572268657267,-0.033601104548885,
0.0684543661311333));
#77872=CARTESIAN_POINT('Ctrl Pts',(0.0072513174340225,-0.0334837508592655,
0.0684660446138457));
#77873=CARTESIAN_POINT('Ctrl Pts',(0.00716729530369496,-0.0333660264659096,
0.0684802190708632));
#77874=CARTESIAN_POINT('Ctrl Pts',(0.00740087609268784,-0.0336938721132526,
0.0684442544948119));
#77875=CARTESIAN_POINT('Ctrl Pts',(0.00736747847087398,-0.0336474569765026,
0.0684484859041039));
#77876=CARTESIAN_POINT('Ctrl Pts',(0.00733413267147486,-0.033601104548885,
0.0684531079847882));
#77877=CARTESIAN_POINT('Ctrl Pts',(0.00724970877408859,-0.0334837508592655,
0.0684648100303961));
#77878=CARTESIAN_POINT('Ctrl Pts',(0.00716566870532982,-0.0333660264659096,
0.0684790085924473));
#77879=CARTESIAN_POINT('Ctrl Pts',(0.00713677251785141,-0.0336938721132526,
0.0682301999665531));
#77880=CARTESIAN_POINT('Ctrl Pts',(0.00710212196385264,-0.0336474569765026,
0.0682359772617078));
#77881=CARTESIAN_POINT('Ctrl Pts',(0.00706754141466618,-0.033601104548885,
0.0682421597894828));
#77882=CARTESIAN_POINT('Ctrl Pts',(0.00697999141470561,-0.0334837508592655,
0.0682578125283545));
#77883=CARTESIAN_POINT('Ctrl Pts',(0.00689294368335894,-0.0333660264659096,
0.0682760526817168));
#77884=CARTESIAN_POINT('',(0.00712570786443446,-0.0336769361243754,0.068233595041375));
#77885=CARTESIAN_POINT('',(0.00713834768830781,-0.0336938721132328,0.0682314766337583));
#77886=CARTESIAN_POINT('Ctrl Pts',(0.00712570786443419,-0.0336769361243751,
0.0682335950413751));
#77887=CARTESIAN_POINT('Ctrl Pts',(0.00712781428237837,-0.033679758666975,
0.0682332396969235));
#77888=CARTESIAN_POINT('Ctrl Pts',(0.00712992081042633,-0.0336825812712295,
0.0682328854908329));
#77889=CARTESIAN_POINT('Ctrl Pts',(0.00713413409255186,-0.0336882266108864,
0.0682321793538773));
#77890=CARTESIAN_POINT('Ctrl Pts',(0.00713624084656904,-0.0336910493461957,
0.0682318274230456));
#77891=CARTESIAN_POINT('Ctrl Pts',(0.00713834768831345,-0.0336938721132294,
0.0682314766337654));
#77892=CARTESIAN_POINT('Ctrl Pts',(0.00712570786443447,-0.0336769361243754,
0.0682335950413751));
#77893=CARTESIAN_POINT('Ctrl Pts',(0.0071326800361329,-0.033627900766312,
0.068274924820154));
#77894=CARTESIAN_POINT('Ctrl Pts',(0.00713975148078475,-0.0335767878929294,
0.0683168430711277));
#77895=CARTESIAN_POINT('Ctrl Pts',(0.00715360953070402,-0.0334733199164922,
0.0683989910964836));
#77896=CARTESIAN_POINT('Ctrl Pts',(0.00716040438618989,-0.0334209645169725,
0.0684392697766759));
#77897=CARTESIAN_POINT('Ctrl Pts',(0.00716706830828396,-0.0333679869844681,
0.0684787723072879));
#77898=CARTESIAN_POINT('',(0.00726961189049276,-0.0336938721132538,0.068337865564297));
#77899=CARTESIAN_POINT('Origin',(0.00812378219310841,-0.0315241814719618,
0.07415));
#77900=CARTESIAN_POINT('',(0.00712570786465501,-0.0337108120655413,0.0682335950426601));
#77901=CARTESIAN_POINT('',(0.00711307259435403,-0.0336938721132327,0.0682357404430475));
#77902=CARTESIAN_POINT('Origin',(0.00874529130525542,-0.0345562517440147,
0.0845527643280791));
#77903=CARTESIAN_POINT('Ctrl Pts',(0.00711307259435331,-0.033693872113232,
0.0682357404430494));
#77904=CARTESIAN_POINT('Ctrl Pts',(0.00711517793149364,-0.0336910493284972,
0.0682353806542312));
#77905=CARTESIAN_POINT('Ctrl Pts',(0.00711728354044955,-0.0336882266020367,
0.0682350219759683));
#77906=CARTESIAN_POINT('Ctrl Pts',(0.00712149529799299,-0.0336825812712153,
0.0682343068417588));
#77907=CARTESIAN_POINT('Ctrl Pts',(0.00712360144649586,-0.0336797586669679,
0.0682339503858257));
#77908=CARTESIAN_POINT('Ctrl Pts',(0.00712570786443473,-0.0336769361243751,
0.068233595041375));
#77909=CARTESIAN_POINT('Origin',(0.0109493597483956,-0.0345562517879156,
0.0841809445835711));
#77910=CARTESIAN_POINT('Ctrl Pts',(0.00732636488129234,-0.034243627687391,
0.0684541900812249));
#77911=CARTESIAN_POINT('Ctrl Pts',(0.00711154386883641,-0.0339430054201809,
0.0684842651709342));
#77912=CARTESIAN_POINT('Ctrl Pts',(0.00689959851934188,-0.0336441434784052,
0.0685304360193264));
#77913=CARTESIAN_POINT('Ctrl Pts',(0.00707959129702041,-0.034243627687391,
0.0684942250422663));
#77914=CARTESIAN_POINT('Ctrl Pts',(0.00686628022801189,-0.0339430054201809,
0.0685336073511379));
#77915=CARTESIAN_POINT('Ctrl Pts',(0.00665654159025616,-0.0336441434784052,
0.0685889452427313));
#77916=CARTESIAN_POINT('Ctrl Pts',(0.00707712356117769,-0.034243627687391,
0.0684946253918768));
#77917=CARTESIAN_POINT('Ctrl Pts',(0.00686382759160364,-0.0339430054201809,
0.06853410077294));
#77918=CARTESIAN_POINT('Ctrl Pts',(0.00665411102096531,-0.0336441434784052,
0.0685895303349653));
#77919=CARTESIAN_POINT('',(0.00704403585815788,-0.0341934961088741,0.0685009051298317));
#77920=CARTESIAN_POINT('',(0.00681285682892965,-0.0338664212873204,0.0685500357415913));
#77921=CARTESIAN_POINT('Origin',(0.00968378016107057,-0.0345610751536084,
0.0850261850981422));
#77922=CARTESIAN_POINT('Origin',(0.00431323542083257,-0.0336938005063867,
0.0578724600114735));
#77923=CARTESIAN_POINT('',(0.00693487608410741,-0.0336938721132327,0.0685228668698901));
#77924=CARTESIAN_POINT('',(0.00687402128537482,-0.0336938721132427,0.0685371126927967));
#77925=CARTESIAN_POINT('',(0.00716706830828924,-0.0340203938281605,0.068478772307287));
#77926=CARTESIAN_POINT('Origin',(0.00920260502512305,-0.0345589643243972,
0.0850279273847569));
#77927=CARTESIAN_POINT('',(0.00716729429479592,-0.034193496108874,0.068480111914651));
#77928=CARTESIAN_POINT('Origin',(0.00533425715374061,-0.0341934220717661,
0.057614193034139));
#77929=CARTESIAN_POINT('',(0.00710566507648691,-0.0341934961088841,0.0684905085222514));
#77930=CARTESIAN_POINT('Ctrl Pts',(0.00735837942108477,-0.0340223579322397,
0.0681990203666452));
#77931=CARTESIAN_POINT('Ctrl Pts',(0.00727629989113435,-0.0339125849573575,
0.0682095772671256));
#77932=CARTESIAN_POINT('Ctrl Pts',(0.0071944965408284,-0.0338030433565231,
0.0682218256049378));
#77933=CARTESIAN_POINT('Ctrl Pts',(0.00711307259435439,-0.0336938721132327,
0.0682357404430468));
#77934=CARTESIAN_POINT('Ctrl Pts',(0.00729469560226883,-0.0340223579322397,
0.0682927516370478));
#77935=CARTESIAN_POINT('Ctrl Pts',(0.00721390887099868,-0.0339125849573575,
0.0683041869034841));
#77936=CARTESIAN_POINT('Ctrl Pts',(0.00713341559107257,-0.0338030433565231,
0.0683172862321059));
#77937=CARTESIAN_POINT('Ctrl Pts',(0.00705331721484792,-0.0336938721132327,
0.0683320237461181));
#77938=CARTESIAN_POINT('Ctrl Pts',(0.00723101178345289,-0.0340223579322397,
0.0683864829074505));
#77939=CARTESIAN_POINT('Ctrl Pts',(0.00715151785086301,-0.0339125849573575,
0.0683987965398426));
#77940=CARTESIAN_POINT('Ctrl Pts',(0.00707233464131675,-0.0338030433565231,
0.068412746859274));
#77941=CARTESIAN_POINT('Ctrl Pts',(0.00699356183534144,-0.0336938721132327,
0.0684283070491894));
#77942=CARTESIAN_POINT('Ctrl Pts',(0.00716732796463695,-0.0340223579322397,
0.0684802141778531));
#77943=CARTESIAN_POINT('Ctrl Pts',(0.00708912683072734,-0.0339125849573575,
0.0684934061762011));
#77944=CARTESIAN_POINT('Ctrl Pts',(0.00701125369156093,-0.0338030433565231,
0.0685082074864422));
#77945=CARTESIAN_POINT('Ctrl Pts',(0.00693380645583497,-0.0336938721132327,
0.0685245903522606));
#77946=CARTESIAN_POINT('',(0.00702397433924072,-0.0336938721132427,0.0683793036564788));
#77947=CARTESIAN_POINT('Ctrl Pts',(0.00712570786524982,-0.0337108120662702,
0.0682335950462078));
#77948=CARTESIAN_POINT('Ctrl Pts',(0.00713286060753573,-0.0337611408994164,
0.0682759952149251));
#77949=CARTESIAN_POINT('Ctrl Pts',(0.00713988282814399,-0.0338121088781025,
0.0683176216746322));
#77950=CARTESIAN_POINT('Ctrl Pts',(0.00715367262314392,-0.0339153382773243,
0.068399365097113));
#77951=CARTESIAN_POINT('Ctrl Pts',(0.00716043436360203,-0.0339675558473115,
0.0684394474773785));
#77952=CARTESIAN_POINT('Ctrl Pts',(0.00716706830829067,-0.0340203938281304,
0.0684787723073271));
#77953=CARTESIAN_POINT('Ctrl Pts',(0.00704568855271773,-0.0341934961088741,
0.0685020807061749));
#77954=CARTESIAN_POINT('Ctrl Pts',(0.0069289222710861,-0.0340287516186244,
0.0685243694428034));
#77955=CARTESIAN_POINT('Ctrl Pts',(0.00681317697440068,-0.0338644633283558,
0.0685514651731272));
#77956=CARTESIAN_POINT('Ctrl Pts',(0.00704403585815796,-0.0341934961088741,
0.0685009051298318));
#77957=CARTESIAN_POINT('Ctrl Pts',(0.00692724527241162,-0.0340287516186244,
0.0685232280346182));
#77958=CARTESIAN_POINT('Ctrl Pts',(0.00681147710457479,-0.0338644633283559,
0.0685503589084114));
#77959=CARTESIAN_POINT('Ctrl Pts',(0.00676866506118924,-0.0341934961088741,
0.0683050314321821));
#77960=CARTESIAN_POINT('Ctrl Pts',(0.006647824941065,-0.0340287516186244,
0.0683330474112423));
#77961=CARTESIAN_POINT('Ctrl Pts',(0.00652824599817819,-0.0338644633283559,
0.0683660338650138));
#77962=CARTESIAN_POINT('',(0.00675618319603834,-0.034176475883238,0.068307939321287));
#77963=CARTESIAN_POINT('',(0.00676866506118928,-0.034193496108874,0.0683050314321821));
#77964=CARTESIAN_POINT('Origin',(0.0100316246976099,-0.0345621026625278,
0.084546560318849));
#77965=CARTESIAN_POINT('Ctrl Pts',(0.00675618319779017,-0.0341764758837466,
0.0683079393217599));
#77966=CARTESIAN_POINT('Ctrl Pts',(0.00676596710045816,-0.0341260050041473,
0.0683497337883827));
#77967=CARTESIAN_POINT('Ctrl Pts',(0.00677558097301842,-0.0340749269150289,
0.0683908017598703));
#77968=CARTESIAN_POINT('Ctrl Pts',(0.0067944759301737,-0.0339715436310858,
0.0684715165824595));
#77969=CARTESIAN_POINT('Ctrl Pts',(0.00680374984062147,-0.0339192778243037,
0.0685111328135425));
#77970=CARTESIAN_POINT('Ctrl Pts',(0.00681285683097385,-0.0338664212861684,
0.0685500357395477));
#77971=CARTESIAN_POINT('',(0.00690635045968359,-0.0341934961088841,0.0684029682810169));
#77972=CARTESIAN_POINT('Origin',(0.00812378219310841,-0.0315241814719618,
0.07415));
#77973=CARTESIAN_POINT('',(0.00675618319538678,-0.0342105180190554,0.068307939322196));
#77974=CARTESIAN_POINT('',(0.00674370756866026,-0.0341934961088739,0.068310873864098));
#77975=CARTESIAN_POINT('Origin',(0.0100766559208261,-0.03456217101078,0.0845413933107676));
#77976=CARTESIAN_POINT('Origin',(0.0110288640294853,-0.0345621035739969,
0.0843131131097792));
#77977=CARTESIAN_POINT('Origin',(0.0109862174074218,-0.0345621718861817,
0.0843284667798951));
#77978=CARTESIAN_POINT('Ctrl Pts',(0.00693633660892827,-0.0346945769586966,
0.0685225249678815));
#77979=CARTESIAN_POINT('Ctrl Pts',(0.00681846689126245,-0.0345275153362944,
0.0685473964910694));
#77980=CARTESIAN_POINT('Ctrl Pts',(0.00670134887296188,-0.0343603235965185,
0.0685759813414362));
#77981=CARTESIAN_POINT('Ctrl Pts',(0.00658532768063191,-0.0341934961088739,
0.068608189829528));
#77982=CARTESIAN_POINT('Ctrl Pts',(0.00685471003537714,-0.0346945769586966,
0.0685416333658137));
#77983=CARTESIAN_POINT('Ctrl Pts',(0.00673724055075659,-0.0345275153362944,
0.0685682145902662));
#77984=CARTESIAN_POINT('Ctrl Pts',(0.00662057663755315,-0.0343603235965185,
0.0685984969971529));
#77985=CARTESIAN_POINT('Ctrl Pts',(0.00650506200471142,-0.0341934961088739,
0.0686323858963626));
#77986=CARTESIAN_POINT('Ctrl Pts',(0.00677308346182602,-0.0346945769586966,
0.0685607417637437));
#77987=CARTESIAN_POINT('Ctrl Pts',(0.00665601421025059,-0.0345275153362944,
0.0685890326894601));
#77988=CARTESIAN_POINT('Ctrl Pts',(0.0065398044021443,-0.0343603235965185,
0.0686210126528679));
#77989=CARTESIAN_POINT('Ctrl Pts',(0.00642479632879096,-0.0341934961088739,
0.0686565819631985));
#77990=CARTESIAN_POINT('Ctrl Pts',(0.00669145688827487,-0.0346945769586966,
0.0685798501616782));
#77991=CARTESIAN_POINT('Ctrl Pts',(0.00657478786974487,-0.0345275153362944,
0.0686098507886597));
#77992=CARTESIAN_POINT('Ctrl Pts',(0.00645903216673571,-0.0343603235965185,
0.0686435283085863));
#77993=CARTESIAN_POINT('Ctrl Pts',(0.00634453065287045,-0.0341934961088739,
0.0686807780300318));
#77994=CARTESIAN_POINT('',(0.00669145688913151,-0.0346945769586966,0.0685798501614778));
#77995=CARTESIAN_POINT('',(0.00646381897772016,-0.034366772783276,0.068643399676385));
#77996=CARTESIAN_POINT('Origin',(0.0110556904213785,-0.0345626461564986,
0.0848171748300519));
#77997=CARTESIAN_POINT('Origin',(0.00327392128255998,-0.0341934771027958,
0.0580615658089922));
#77998=CARTESIAN_POINT('',(0.00658389150603352,-0.0341934961088739,0.0686086227639818));
#77999=CARTESIAN_POINT('',(0.00652405129296608,-0.034193496108884,0.06862666158044));
#78000=CARTESIAN_POINT('',(0.00681285683141268,-0.0345211942962713,0.0685500357415574));
#78001=CARTESIAN_POINT('Origin',(0.0105867782592795,-0.0345625596118762,
0.0849235307122997));
#78002=CARTESIAN_POINT('',(0.00681316648662224,-0.0346945769586886,0.0685513585156833));
#78003=CARTESIAN_POINT('Origin',(0.0042914133953859,-0.0346945685853918,
0.0577790200246689));
#78004=CARTESIAN_POINT('',(0.00675231168788688,-0.0346945769587026,0.0685656043385906));
#78005=CARTESIAN_POINT('Ctrl Pts',(0.00698622372100385,-0.0345231616327842,
0.0682588234857065));
#78006=CARTESIAN_POINT('Ctrl Pts',(0.00690502214686742,-0.0344132092796988,
0.0682745031276902));
#78007=CARTESIAN_POINT('Ctrl Pts',(0.00682414908338544,-0.0343032738558979,
0.0682918615511867));
#78008=CARTESIAN_POINT('Ctrl Pts',(0.00674370756866024,-0.0341934961088739,
0.068310873864098));
#78009=CARTESIAN_POINT('Ctrl Pts',(0.0069285511165796,-0.0345231616327842,
0.0683563683822279));
#78010=CARTESIAN_POINT('Ctrl Pts',(0.00684869406150948,-0.0344132092796988,
0.0683728429598671));
#78011=CARTESIAN_POINT('Ctrl Pts',(0.00676918189033981,-0.0343032738558979,
0.0683909684676876));
#78012=CARTESIAN_POINT('Ctrl Pts',(0.00669011587253975,-0.0341934961088739,
0.0684107190755274));
#78013=CARTESIAN_POINT('Ctrl Pts',(0.00687087851215535,-0.0345231616327842,
0.0684539132787493));
#78014=CARTESIAN_POINT('Ctrl Pts',(0.00679236597615154,-0.0344132092796988,
0.068471182792044));
#78015=CARTESIAN_POINT('Ctrl Pts',(0.00671421469729419,-0.0343032738558979,
0.0684900753841886));
#78016=CARTESIAN_POINT('Ctrl Pts',(0.00663652417641926,-0.0341934961088739,
0.0685105642869568));
#78017=CARTESIAN_POINT('Ctrl Pts',(0.00681320590773109,-0.0345231616327842,
0.0685514581752708));
#78018=CARTESIAN_POINT('Ctrl Pts',(0.00673603789079361,-0.0344132092796988,
0.0685695226242208));
#78019=CARTESIAN_POINT('Ctrl Pts',(0.00665924750424856,-0.0343032738558979,
0.0685891823006895));
#78020=CARTESIAN_POINT('Ctrl Pts',(0.00658293248029878,-0.0341934961088739,
0.0686104094983862));
#78021=CARTESIAN_POINT('',(0.00666379953735689,-0.0341934961088839,0.0684597483140499));
#78022=CARTESIAN_POINT('Ctrl Pts',(0.00675618319616943,-0.0342105180195406,
0.0683079393255548));
#78023=CARTESIAN_POINT('Ctrl Pts',(0.00676597808447636,-0.0342610556241096,
0.0683497807804818));
#78024=CARTESIAN_POINT('Ctrl Pts',(0.00677559720857732,-0.0343122189869719,
0.0683908714121353));
#78025=CARTESIAN_POINT('Ctrl Pts',(0.00679449236031797,-0.0344158119695203,
0.0684715870482019));
#78026=CARTESIAN_POINT('Ctrl Pts',(0.00680376065969012,-0.0344681990450108,
0.0685111790392771));
#78027=CARTESIAN_POINT('Ctrl Pts',(0.00681285683141085,-0.0345211942962532,
0.0685500357415825));
#78028=CARTESIAN_POINT('Ctrl Pts',(0.00669317971611005,-0.0346945769586932,
0.068580919382993));
#78029=CARTESIAN_POINT('Ctrl Pts',(0.00657804291494672,-0.0345296777077528,
0.0686104960769332));
#78030=CARTESIAN_POINT('Ctrl Pts',(0.00646422692867993,-0.0343648066252516,
0.0686448062077502));
#78031=CARTESIAN_POINT('Ctrl Pts',(0.00669145688914032,-0.0346945769586932,
0.0685798501614757));
#78032=CARTESIAN_POINT('Ctrl Pts',(0.00657629798257868,-0.0345296777077528,
0.0686094624736444));
#78033=CARTESIAN_POINT('Ctrl Pts',(0.0064624613819365,-0.0343648066252516,
0.0686438091058911));
#78034=CARTESIAN_POINT('Ctrl Pts',(0.00640433046229951,-0.0346945769586932,
0.06840165365123));
#78035=CARTESIAN_POINT('Ctrl Pts',(0.00628548746897756,-0.0345296777077528,
0.0684372020991076));
#78036=CARTESIAN_POINT('Ctrl Pts',(0.00616821527552477,-0.0343648066252516,
0.0684776320614004));
#78037=CARTESIAN_POINT('',(0.00639205581495692,-0.0346775396664964,0.0684053395448861));
#78038=CARTESIAN_POINT('',(0.00640433046229623,-0.0346945769586887,0.0684016536512309));
#78039=CARTESIAN_POINT('Origin',(0.0113296404334329,-0.0345626618229783,
0.0842556756019206));
#78040=CARTESIAN_POINT('Ctrl Pts',(0.00639205581671261,-0.0346775396670097,
0.068405339545346));
#78041=CARTESIAN_POINT('Ctrl Pts',(0.0064044544659018,-0.0346269749928334,
0.0684464695721525));
#78042=CARTESIAN_POINT('Ctrl Pts',(0.00641663279782036,-0.0345757902891081,
0.0684868686162392));
#78043=CARTESIAN_POINT('Ctrl Pts',(0.00644055869167247,-0.0344721681088438,
0.0685662380597165));
#78044=CARTESIAN_POINT('Ctrl Pts',(0.00645229686813701,-0.0344197714290001,
0.0686051773441915));
#78045=CARTESIAN_POINT('Ctrl Pts',(0.0064638189779905,-0.0343667727831519,
0.0686433996761315));
#78046=CARTESIAN_POINT('',(0.00654789367572387,-0.0346945769587026,0.0684907519063644));
#78047=CARTESIAN_POINT('Origin',(0.00812378219310841,-0.0315241814719618,
0.07415));
#78048=CARTESIAN_POINT('',(0.00639205581458973,-0.0347116136489626,0.0684053395462279));
#78049=CARTESIAN_POINT('',(0.00637978906701314,-0.0346945769586885,0.0684090516483639));
#78050=CARTESIAN_POINT('Origin',(0.0113724486185158,-0.0345626688543831,
0.0842408196828196));
#78051=CARTESIAN_POINT('Origin',(0.0110372063907197,-0.0345626626523952,
0.0843438322450094));
#78052=CARTESIAN_POINT('Origin',(0.010993318521225,-0.0345626697901873,
0.0843551060349324));
#78053=CARTESIAN_POINT('Ctrl Pts',(0.00662110080507579,-0.0352450361874068,
0.0685983601615324));
#78054=CARTESIAN_POINT('Ctrl Pts',(0.0064117172727439,-0.0349452760959493,
0.0686550347200684));
#78055=CARTESIAN_POINT('Ctrl Pts',(0.0062071975366287,-0.0346444289841739,
0.0687273198965322));
#78056=CARTESIAN_POINT('Ctrl Pts',(0.00661870271482155,-0.0352450361874068,
0.0685990666763112));
#78057=CARTESIAN_POINT('Ctrl Pts',(0.00640934582913179,-0.0349452760959493,
0.0686558316803052));
#78058=CARTESIAN_POINT('Ctrl Pts',(0.00620485947668039,-0.0346444289841739,
0.0687282050381468));
#78059=CARTESIAN_POINT('Ctrl Pts',(0.00637889368574284,-0.0352450361874068,
0.0686697181552573));
#78060=CARTESIAN_POINT('Ctrl Pts',(0.00617220146430665,-0.0349452760959493,
0.0687355277051972));
#78061=CARTESIAN_POINT('Ctrl Pts',(0.00597105347828606,-0.0346444289841739,
0.0688167192009672));
#78062=CARTESIAN_POINT('',(0.00634456095533437,-0.0351951633467146,0.0686807659675127));
#78063=CARTESIAN_POINT('',(0.00612133224107484,-0.0348678972925388,0.0687584956468902));
#78064=CARTESIAN_POINT('Origin',(0.0123492203897781,-0.0345631633298062,
0.0843130374478586));
#78065=CARTESIAN_POINT('Origin',(0.00227410942706091,-0.0346946199341028,
0.0584000273317687));
#78066=CARTESIAN_POINT('',(0.00623898419006084,-0.0346945769330288,0.0687162479366787));
#78067=CARTESIAN_POINT('',(0.00618039471635125,-0.0346945769458128,0.068738008558407));
#78068=CARTESIAN_POINT('',(0.00646381897803458,-0.0350221583435275,0.0686433996763336));
#78069=CARTESIAN_POINT('Origin',(0.0119137981656891,-0.0345628458714449,
0.0845184013684698));
#78070=CARTESIAN_POINT('',(0.00646417886482151,-0.035195136029876,0.0686445830504279));
#78071=CARTESIAN_POINT('Origin',(0.00328386838325173,-0.035195183836688,
0.0580945371203709));
#78072=CARTESIAN_POINT('',(0.00634453065880707,-0.035195137132875,0.0686807780281208));
#78073=CARTESIAN_POINT('Ctrl Pts',(0.00661855746883567,-0.0350241211494342,
0.0683418765053196));
#78074=CARTESIAN_POINT('Ctrl Pts',(0.00653855294911979,-0.0349144232818961,
0.0683626103587302));
#78075=CARTESIAN_POINT('Ctrl Pts',(0.00645892912640817,-0.0348045283579412,
0.0683850103729423));
#78076=CARTESIAN_POINT('Ctrl Pts',(0.00637978905638008,-0.0346945769439157,
0.068409051651594));
#78077=CARTESIAN_POINT('Ctrl Pts',(0.00656712356767582,-0.0350241211494342,
0.0684428502425703));
#78078=CARTESIAN_POINT('Ctrl Pts',(0.00648850991978973,-0.0349144232818961,
0.0684642925768807));
#78079=CARTESIAN_POINT('Ctrl Pts',(0.00641029244621817,-0.0348045283579412,
0.0684873727457379));
#78080=CARTESIAN_POINT('Ctrl Pts',(0.00633257243370495,-0.0346945769439157,
0.0685120649145559));
#78081=CARTESIAN_POINT('Ctrl Pts',(0.00651568966651597,-0.0350241211494342,
0.068543823979821));
#78082=CARTESIAN_POINT('Ctrl Pts',(0.00643846689045967,-0.0349144232818961,
0.0685659747950312));
#78083=CARTESIAN_POINT('Ctrl Pts',(0.00636165576602818,-0.0348045283579412,
0.0685897351185336));
#78084=CARTESIAN_POINT('Ctrl Pts',(0.00628535581102983,-0.0346945769439157,
0.0686150781775178));
#78085=CARTESIAN_POINT('Ctrl Pts',(0.00646425576535612,-0.0350241211494342,
0.0686447977170718));
#78086=CARTESIAN_POINT('Ctrl Pts',(0.0063884238611296,-0.0349144232818961,
0.0686676570131817));
#78087=CARTESIAN_POINT('Ctrl Pts',(0.00631301908583818,-0.0348045283579412,
0.0686920974913292));
#78088=CARTESIAN_POINT('Ctrl Pts',(0.0062381391883547,-0.0346945769439157,
0.0687180914404797));
#78089=CARTESIAN_POINT('',(0.00630938662879126,-0.0346945769458128,0.0685626497923518));
#78090=CARTESIAN_POINT('Ctrl Pts',(0.00639205581553391,-0.0347116136492808,
0.0684053395493713));
#78091=CARTESIAN_POINT('Ctrl Pts',(0.0064044495286139,-0.0347621546532085,
0.0684464532462514));
#78092=CARTESIAN_POINT('Ctrl Pts',(0.00641662532672676,-0.0348133084096574,
0.0684868440532401));
#78093=CARTESIAN_POINT('Ctrl Pts',(0.00644055125457274,-0.0349168561544573,
0.0685662135963857));
#78094=CARTESIAN_POINT('Ctrl Pts',(0.00645229189408879,-0.0349692089015913,
0.0686051608506207));
#78095=CARTESIAN_POINT('Ctrl Pts',(0.00646381897802599,-0.0350221583434999,
0.0686433996763744));
#78096=CARTESIAN_POINT('Ctrl Pts',(0.00634581971921704,-0.0351951371254913,
0.068681469932819));
#78097=CARTESIAN_POINT('Ctrl Pts',(0.00627050925695388,-0.0350856248736006,
0.068705955338248));
#78098=CARTESIAN_POINT('Ctrl Pts',(0.00619564299169479,-0.0349758427080694,
0.068732017228011));
#78099=CARTESIAN_POINT('Ctrl Pts',(0.0061213187293352,-0.034865930689779,
0.0687596278671616));
#78100=CARTESIAN_POINT('Ctrl Pts',(0.00627337379092395,-0.0351951371254913,
0.0686425847412442));
#78101=CARTESIAN_POINT('Ctrl Pts',(0.00619752781697544,-0.0350856248736006,
0.0686680678437292));
#78102=CARTESIAN_POINT('Ctrl Pts',(0.00612214621905836,-0.0349758427080694,
0.0686951393165914));
#78103=CARTESIAN_POINT('Ctrl Pts',(0.00604732753873635,-0.034865930689779,
0.0687237701711421));
#78104=CARTESIAN_POINT('Ctrl Pts',(0.00620092786263085,-0.0351951371254913,
0.0686036995496694));
#78105=CARTESIAN_POINT('Ctrl Pts',(0.00612454637699699,-0.0350856248736006,
0.0686301803492104));
#78106=CARTESIAN_POINT('Ctrl Pts',(0.00604864944642193,-0.0349758427080694,
0.0686582614051718));
#78107=CARTESIAN_POINT('Ctrl Pts',(0.00597333634813751,-0.034865930689779,
0.0686879124751227));
#78108=CARTESIAN_POINT('Ctrl Pts',(0.00612848193433776,-0.0351951371254913,
0.0685648143580946));
#78109=CARTESIAN_POINT('Ctrl Pts',(0.00605156493701854,-0.0350856248736006,
0.0685922928546916));
#78110=CARTESIAN_POINT('Ctrl Pts',(0.0059751526737855,-0.0349758427080694,
0.0686213834937522));
#78111=CARTESIAN_POINT('Ctrl Pts',(0.00589934515753867,-0.034865930689779,
0.0686520547791032));
#78112=CARTESIAN_POINT('Origin',(0.00426970141720928,-0.0308609197410927,
0.0637730648563144));
#78113=CARTESIAN_POINT('',(0.00625033828332303,-0.0351951371254913,0.0686302204835531));
#78114=CARTESIAN_POINT('Origin',(0.00859310768890597,-0.0351840467441098,
0.0750070176365937));
#78115=CARTESIAN_POINT('Origin',(0.00322208857129343,-0.0352322615287784,
0.0632348972788652));
#78116=CARTESIAN_POINT('',(0.00590123553039178,-0.0351951142564656,0.0688454641187499));
#78117=CARTESIAN_POINT('',(0.00578730024265978,-0.0351951372916786,0.0688961107648497));
#78118=CARTESIAN_POINT('Origin',(0.00793123669642114,-0.0352875104107299,
0.0744308068679663));
#78119=CARTESIAN_POINT('Origin',(0.0154363415296375,-0.0298325076521851,
0.0724702183975427));
#78120=CARTESIAN_POINT('Origin',(0.00785119176127153,-0.0338732556787189,
0.0657729478221477));
#78121=CARTESIAN_POINT('Ctrl Pts',(0.0094439865715157,-0.0321934096636941,
0.068552215068034));
#78122=CARTESIAN_POINT('Ctrl Pts',(0.00934378888693288,-0.0320508460844246,
0.0685285840383499));
#78123=CARTESIAN_POINT('Ctrl Pts',(0.00924303183259509,-0.0319086045662913,
0.0685076629406188));
#78124=CARTESIAN_POINT('Ctrl Pts',(0.00914193606469694,-0.0317669892867664,
0.0684894789611682));
#78125=CARTESIAN_POINT('Ctrl Pts',(0.00936197865582068,-0.0321934096636941,
0.0685347469716528));
#78126=CARTESIAN_POINT('Ctrl Pts',(0.00926146830063105,-0.0320508460844246,
0.0685125838446069));
#78127=CARTESIAN_POINT('Ctrl Pts',(0.00916043825108861,-0.0319086045662913,
0.068493137943553));
#78128=CARTESIAN_POINT('Ctrl Pts',(0.00905910948969717,-0.0317669892867664,
0.0684764332300684));
#78129=CARTESIAN_POINT('Ctrl Pts',(0.00927997074012567,-0.0321934096636941,
0.0685172788752715));
#78130=CARTESIAN_POINT('Ctrl Pts',(0.00917914771432923,-0.0320508460844246,
0.0684965836508641));
#78131=CARTESIAN_POINT('Ctrl Pts',(0.00907784466958213,-0.0319086045662913,
0.0684786129464871));
#78132=CARTESIAN_POINT('Ctrl Pts',(0.00897628291469741,-0.0317669892867664,
0.0684633874989687));
#78133=CARTESIAN_POINT('Ctrl Pts',(0.00919796282443065,-0.0321934096636941,
0.0684998107788903));
#78134=CARTESIAN_POINT('Ctrl Pts',(0.00909682712802741,-0.0320508460844246,
0.0684805834571211));
#78135=CARTESIAN_POINT('Ctrl Pts',(0.00899525108807564,-0.0319086045662913,
0.0684640879494213));
#78136=CARTESIAN_POINT('Ctrl Pts',(0.00889345633969765,-0.0317669892867663,
0.0684503417678689));
#78137=CARTESIAN_POINT('',(0.00919942996224764,-0.0321934096636941,0.0685001232865888));
#78138=CARTESIAN_POINT('',(0.00896639895460232,-0.0318665617511278,0.06846070109923));
#78139=CARTESIAN_POINT('Origin',(0.00547230549469594,-0.032637194442216,
0.0847889675687293));
#78140=CARTESIAN_POINT('Origin',(0.0105722941342516,-0.0316939261508945,
0.0576177913948755));
#78141=CARTESIAN_POINT('',(0.00932170218911971,-0.0320197221621871,0.0685248265049253));
#78142=CARTESIAN_POINT('Ctrl Pts',(0.0093215370854431,-0.0320197392094776,
0.0685247431043587));
#78143=CARTESIAN_POINT('Ctrl Pts',(0.0092929139601089,-0.0319792716576074,
0.0685186485883089));
#78144=CARTESIAN_POINT('Ctrl Pts',(0.00926411406927588,-0.031938643982974,
0.0685127445388893));
#78145=CARTESIAN_POINT('Ctrl Pts',(0.00923510548001692,-0.0318979099381672,
0.0685070330431788));
#78146=CARTESIAN_POINT('Ctrl Pts',(0.00920609746413207,-0.0318571766984959,
0.0685013216603598));
#78147=CARTESIAN_POINT('Ctrl Pts',(0.00917702853994146,-0.0318163871833594,
0.0684958301044913));
#78148=CARTESIAN_POINT('Ctrl Pts',(0.00914799934620503,-0.0317755399638303,
0.0684905738043085));
#78149=CARTESIAN_POINT('',(0.00932168725141204,-0.0321934096636183,0.06852616470091));
#78150=CARTESIAN_POINT('Origin',(0.00978186381970738,-0.0324111717947839,
0.0662648353462695));
#78151=CARTESIAN_POINT('',(0.00926055860683984,-0.0321934096636663,0.0685131439937594));
#78152=CARTESIAN_POINT('Ctrl Pts',(0.00920053388169604,-0.0321934096636617,
0.0685018247710085));
#78153=CARTESIAN_POINT('Ctrl Pts',(0.00912264114335793,-0.0320835708272592,
0.0684869755260517));
#78154=CARTESIAN_POINT('Ctrl Pts',(0.009044486281621,-0.0319739230346488,
0.068473746880432));
#78155=CARTESIAN_POINT('Ctrl Pts',(0.00896617058916533,-0.0318646057455573,
0.0684621480850449));
#78156=CARTESIAN_POINT('Ctrl Pts',(0.00913885678371131,-0.0321934096636617,
0.0684067611062953));
#78157=CARTESIAN_POINT('Ctrl Pts',(0.00905965304334853,-0.0320835708272592,
0.068392762436588));
#78158=CARTESIAN_POINT('Ctrl Pts',(0.00898020554263194,-0.0319739230346488,
0.0683804110039684));
#78159=CARTESIAN_POINT('Ctrl Pts',(0.00890061714194762,-0.0318646057455573,
0.068369714810071));
#78160=CARTESIAN_POINT('Ctrl Pts',(0.00907717968572658,-0.0321934096636617,
0.068311697441582));
#78161=CARTESIAN_POINT('Ctrl Pts',(0.00899666494333912,-0.0320835708272592,
0.0682985493471242));
#78162=CARTESIAN_POINT('Ctrl Pts',(0.00891592480364289,-0.0319739230346488,
0.0682870751275048));
#78163=CARTESIAN_POINT('Ctrl Pts',(0.00883506369472991,-0.0318646057455573,
0.0682772815350971));
#78164=CARTESIAN_POINT('Ctrl Pts',(0.00901550258774186,-0.0321934096636617,
0.0682166337768687));
#78165=CARTESIAN_POINT('Ctrl Pts',(0.00893367684332971,-0.0320835708272592,
0.0682043362576605));
#78166=CARTESIAN_POINT('Ctrl Pts',(0.00885164406465383,-0.0319739230346488,
0.0681937392510411));
#78167=CARTESIAN_POINT('Ctrl Pts',(0.0087695102475122,-0.0318646057455573,
0.0681848482601232));
#78168=CARTESIAN_POINT('',(0.00900282677662865,-0.0321763980308457,0.0682147425836894));
#78169=CARTESIAN_POINT('',(0.00901550258770958,-0.0321934096636184,0.0682166337768639));
#78170=CARTESIAN_POINT('Origin',(0.00597325106342534,-0.0326386231399442,
0.0844827409580259));
#78171=CARTESIAN_POINT('Ctrl Pts',(0.00900282677615878,-0.0321763980306278,
0.0682147425868238));
#78172=CARTESIAN_POINT('Ctrl Pts',(0.00899653883936201,-0.0321259596174822,
0.0682571983668901));
#78173=CARTESIAN_POINT('Ctrl Pts',(0.00899035984923604,-0.032074916463138,
0.0682989185454781));
#78174=CARTESIAN_POINT('Ctrl Pts',(0.00897821478964855,-0.0319716057793914,
0.0683809212747366));
#78175=CARTESIAN_POINT('Ctrl Pts',(0.00897225345231002,-0.0319193786690108,
0.0684211718743905));
#78176=CARTESIAN_POINT('Ctrl Pts',(0.00896639895432312,-0.0318665617525293,
0.0684607011010613));
#78177=CARTESIAN_POINT('',(0.00910746627498862,-0.0321934096636663,0.0683583785317363));
#78178=CARTESIAN_POINT('Origin',(0.00812378219310841,-0.0315241814719618,
0.07415));
#78179=CARTESIAN_POINT('',(0.00900282677668285,-0.0322104233323627,0.0682147425833225));
#78180=CARTESIAN_POINT('',(0.00899014695537404,-0.0321934096636183,0.0682128784669062));
#78181=CARTESIAN_POINT('Origin',(0.00601673289315573,-0.0326387236839092,
0.0844955662196018));
#78182=CARTESIAN_POINT('Origin',(0.00718701739197183,-0.0326386240897199,
0.0846625085056469));
#78183=CARTESIAN_POINT('Origin',(0.00714168519673485,-0.0326387244881,0.0846621754870935));
#78184=CARTESIAN_POINT('Ctrl Pts',(0.00912546258677331,-0.0327445246967097,
0.0684865415699463));
#78185=CARTESIAN_POINT('Ctrl Pts',(0.00891186176018342,-0.032443687833936,
0.0684487625762962));
#78186=CARTESIAN_POINT('Ctrl Pts',(0.00869602208277616,-0.0321434074405928,
0.0684271801960333));
#78187=CARTESIAN_POINT('Ctrl Pts',(0.0088783952573674,-0.0327445246967097,
0.0684483612773827));
#78188=CARTESIAN_POINT('Ctrl Pts',(0.00866335443750278,-0.032443687833936,
0.0684199005803948));
#78189=CARTESIAN_POINT('Ctrl Pts',(0.00844678074987853,-0.0321434074405928,
0.068407718490676));
#78190=CARTESIAN_POINT('',(0.00884254872302497,-0.0326943950436612,0.068443731545443));
#78191=CARTESIAN_POINT('',(0.00860750220923627,-0.0323666188837389,0.0684190192858466));
#78192=CARTESIAN_POINT('Origin',(0.00681706364081476,-0.0326395579111504,
0.0851322146524214));
#78193=CARTESIAN_POINT('Origin',(0.00953641204844979,-0.0321933825603182,
0.057413543452628));
#78194=CARTESIAN_POINT('',(0.00873194506416534,-0.0321934096532689,0.0684308861771334));
#78195=CARTESIAN_POINT('',(0.00866966650717283,-0.0321934096584275,0.0684256295922533));
#78196=CARTESIAN_POINT('',(0.00896639895473841,-0.0325210109756238,0.068460701098288));
#78197=CARTESIAN_POINT('Origin',(0.00634385287505525,-0.0326393129158472,
0.0850470324884165));
#78198=CARTESIAN_POINT('',(0.00896619991923769,-0.0326943950436593,0.0684620449742721));
#78199=CARTESIAN_POINT('Origin',(0.01058693251845,-0.0326943765538216,0.0575189584561217));
#78200=CARTESIAN_POINT('',(0.00890437432114132,-0.0326943950436702,0.0684528882598675));
#78201=CARTESIAN_POINT('Ctrl Pts',(0.00923479393888999,-0.0325229783203769,
0.0682537594264856));
#78202=CARTESIAN_POINT('Ctrl Pts',(0.00915351439152637,-0.032413025309245,
0.0682384441538662));
#78203=CARTESIAN_POINT('Ctrl Pts',(0.00907193035571066,-0.032303122220807,
0.0682248125759562));
#78204=CARTESIAN_POINT('Ctrl Pts',(0.00899014695093679,-0.0321934096576658,
0.0682128784662587));
#78205=CARTESIAN_POINT('Ctrl Pts',(0.0091452626130476,-0.0325229783203769,
0.0683232236901697));
#78206=CARTESIAN_POINT('Ctrl Pts',(0.00906494062903978,-0.032413025309245,
0.0683091426049192));
#78207=CARTESIAN_POINT('Ctrl Pts',(0.00898433954209778,-0.032303122220807,
0.0682967252187612));
#78208=CARTESIAN_POINT('Ctrl Pts',(0.00890356315774672,-0.0321934096576658,
0.0682859837943346));
#78209=CARTESIAN_POINT('Ctrl Pts',(0.00905573128720521,-0.0325229783203769,
0.0683926879538539));
#78210=CARTESIAN_POINT('Ctrl Pts',(0.00897636686655319,-0.032413025309245,
0.0683798410559721));
#78211=CARTESIAN_POINT('Ctrl Pts',(0.0088967487284849,-0.032303122220807,
0.0683686378615661));
#78212=CARTESIAN_POINT('Ctrl Pts',(0.00881697936455664,-0.0321934096576658,
0.0683590891224106));
#78213=CARTESIAN_POINT('Ctrl Pts',(0.00896619996136282,-0.0325229783203769,
0.068462152217538));
#78214=CARTESIAN_POINT('Ctrl Pts',(0.0088877931040666,-0.032413025309245,
0.0684505395070251));
#78215=CARTESIAN_POINT('Ctrl Pts',(0.00880915791487202,-0.032303122220807,
0.0684405505043711));
#78216=CARTESIAN_POINT('Ctrl Pts',(0.00873039557136657,-0.0321934096576658,
0.0684321944504865));
#78217=CARTESIAN_POINT('',(0.00886104601027864,-0.0321934096584275,0.0683218823219358));
#78218=CARTESIAN_POINT('Ctrl Pts',(0.00900282677616828,-0.0322104233328946,
0.0682147425867594));
#78219=CARTESIAN_POINT('Ctrl Pts',(0.00899653031911972,-0.0322609421831059,
0.0682572558950655));
#78220=CARTESIAN_POINT('Ctrl Pts',(0.00899034716670475,-0.0323120888240066,
0.0682990041771383));
#78221=CARTESIAN_POINT('Ctrl Pts',(0.00897820201515553,-0.0324156524631819,
0.0683810075273171));
#78222=CARTESIAN_POINT('Ctrl Pts',(0.00897224500832695,-0.0324680267167319,
0.0684212288876685));
#78223=CARTESIAN_POINT('Ctrl Pts',(0.00896639895472762,-0.0325210109755912,
0.0684607010983302));
#78224=CARTESIAN_POINT('Origin',(0.0157112785443541,-0.0262834582511764,
0.0762316543803413));
#78225=CARTESIAN_POINT('Origin',(0.0150973441873914,-0.0342770700395395,
0.0641904785327736));
#78226=CARTESIAN_POINT('Ctrl Pts',(0.00884375700785978,-0.0326943950436604,
0.0684453599614188));
#78227=CARTESIAN_POINT('Ctrl Pts',(0.0087651363764932,-0.0325844576448134,
0.0684354373590949));
#78228=CARTESIAN_POINT('Ctrl Pts',(0.00868630496533801,-0.0324744968375323,
0.06842714005809));
#78229=CARTESIAN_POINT('Ctrl Pts',(0.00860736392442869,-0.0323646534831895,
0.0684204772962495));
#78230=CARTESIAN_POINT('Ctrl Pts',(0.00877623261640564,-0.0326943950436604,
0.0683543567519142));
#78231=CARTESIAN_POINT('Ctrl Pts',(0.00869635779025389,-0.0325844576448134,
0.0683453647622587));
#78232=CARTESIAN_POINT('Ctrl Pts',(0.00861629134214797,-0.0324744968375323,
0.0683380240785876));
#78233=CARTESIAN_POINT('Ctrl Pts',(0.00853613598761797,-0.0323646534831895,
0.0683323426912462));
#78234=CARTESIAN_POINT('Ctrl Pts',(0.00870870822495149,-0.0326943950436604,
0.0682633535424095));
#78235=CARTESIAN_POINT('Ctrl Pts',(0.00862757920401458,-0.0325844576448134,
0.0682552921654225));
#78236=CARTESIAN_POINT('Ctrl Pts',(0.00854627771895792,-0.0324744968375323,
0.0682489080990851));
#78237=CARTESIAN_POINT('Ctrl Pts',(0.00846490805080725,-0.0323646534831895,
0.0682442080862429));
#78238=CARTESIAN_POINT('Ctrl Pts',(0.00864118383349735,-0.0326943950436604,
0.0681723503329048));
#78239=CARTESIAN_POINT('Ctrl Pts',(0.00855880061777527,-0.0325844576448134,
0.0681652195685863));
#78240=CARTESIAN_POINT('Ctrl Pts',(0.00847626409576787,-0.0324744968375323,
0.0681597921195827));
#78241=CARTESIAN_POINT('Ctrl Pts',(0.00839368011399654,-0.0323646534831895,
0.0681560734812396));
#78242=CARTESIAN_POINT('',(0.00862841428624813,-0.032677355999116,0.0681712587921285));
#78243=CARTESIAN_POINT('',(0.00864118383349658,-0.0326943950436595,0.0681723503329048));
#78244=CARTESIAN_POINT('Origin',(0.00728189562577048,-0.0326395670678001,
0.0847217934799203));
#78245=CARTESIAN_POINT('Ctrl Pts',(0.00862841428596128,-0.032677355998742,
0.0681712587954638));
#78246=CARTESIAN_POINT('Ctrl Pts',(0.00862480167261006,-0.032626792258595,
0.0682140600374077));
#78247=CARTESIAN_POINT('Ctrl Pts',(0.00862125309022181,-0.0325756109579303,
0.0682561026582453));
#78248=CARTESIAN_POINT('Ctrl Pts',(0.00861428096735214,-0.0324719985462367,
0.0683387064380571));
#78249=CARTESIAN_POINT('Ctrl Pts',(0.00861086022319848,-0.032419609162177,
0.0683792344669148));
#78250=CARTESIAN_POINT('Ctrl Pts',(0.00860750220923214,-0.0323666188837756,
0.0684190192858952));
#78251=CARTESIAN_POINT('',(0.00874186627827078,-0.0326943950436703,0.0683080409391839));
#78252=CARTESIAN_POINT('Origin',(0.00812378219310841,-0.0315241814719618,
0.07415));
#78253=CARTESIAN_POINT('',(0.00862841428624429,-0.0327114338379885,0.068171258792173));
#78254=CARTESIAN_POINT('',(0.00861564243684584,-0.0326943950436593,0.0681701945265212));
#78255=CARTESIAN_POINT('Origin',(0.00732710419379926,-0.0326395671577066,
0.0847248312028982));
#78256=CARTESIAN_POINT('Origin',(0.00718177098644518,-0.0326395677642361,
0.0847133440405204));
#78257=CARTESIAN_POINT('Origin',(0.00713669334567575,-0.0326395680194222,
0.0847087577456239));
#78258=CARTESIAN_POINT('Ctrl Pts',(0.00876783552519102,-0.0332451089994433,
0.0684348166866291));
#78259=CARTESIAN_POINT('Ctrl Pts',(0.00855228385991727,-0.0329451141710254,
0.0684105258177901));
#78260=CARTESIAN_POINT('Ctrl Pts',(0.00833551486663236,-0.0326442513127494,
0.0684025401893565));
#78261=CARTESIAN_POINT('Ctrl Pts',(0.00851885821225085,-0.0332451089994433,
0.0684122269181242));
#78262=CARTESIAN_POINT('Ctrl Pts',(0.0083024545599187,-0.0329451141710254,
0.0683973263822767));
#78263=CARTESIAN_POINT('Ctrl Pts',(0.0080855433182496,-0.0326442513127494,
0.0683987685850377));
#78264=CARTESIAN_POINT('Ctrl Pts',(0.00851636843912145,-0.0332451089994433,
0.0684120010204392));
#78265=CARTESIAN_POINT('Ctrl Pts',(0.00829995626691872,-0.0329451141710254,
0.0683971943879216));
#78266=CARTESIAN_POINT('Ctrl Pts',(0.00808304360276577,-0.0326442513127494,
0.0683987308689945));
#78267=CARTESIAN_POINT('',(0.00848283084062868,-0.0331951640388616,0.0684098598389312));
#78268=CARTESIAN_POINT('',(0.00824669642355681,-0.0328677532457581,0.0683999550269371));
#78269=CARTESIAN_POINT('Origin',(0.00820381225447208,-0.0326403163409033,
0.0851715565180648));
#78270=CARTESIAN_POINT('Origin',(0.00848245237122557,-0.0326944278639109,
0.0573464992760607));
#78271=CARTESIAN_POINT('',(0.00837163885895575,-0.0326943950436593,0.0684039846786494));
#78272=CARTESIAN_POINT('',(0.00830915313354108,-0.0326943950436694,0.0684026489698008));
#78273=CARTESIAN_POINT('',(0.00860750220923909,-0.0330220786163545,0.0684190192858468));
#78274=CARTESIAN_POINT('Origin',(0.00772354399028894,-0.0326396682763611,
0.0851927127086911));
#78275=CARTESIAN_POINT('',(0.00860738794916238,-0.0331951640388587,0.0684203730075413));
#78276=CARTESIAN_POINT('Origin',(0.00953520974333515,-0.0331952026559975,
0.0574278065989809));
#78277=CARTESIAN_POINT('',(0.00854510939490553,-0.0331951640388701,0.0684151164232462));
#78278=CARTESIAN_POINT('Ctrl Pts',(0.00886237264853371,-0.0330240426238172,
0.0681956331873849));
#78279=CARTESIAN_POINT('Ctrl Pts',(0.00878034544463144,-0.0329142774063519,
0.0681854583842876));
#78280=CARTESIAN_POINT('Ctrl Pts',(0.00869806700557452,-0.0328043479726691,
0.0681769742401163));
#78281=CARTESIAN_POINT('Ctrl Pts',(0.00861564243684584,-0.0326943950436593,
0.0681701945265212));
#78282=CARTESIAN_POINT('Ctrl Pts',(0.00877737972220961,-0.0330240426238172,
0.0682705820930427));
#78283=CARTESIAN_POINT('Ctrl Pts',(0.00869638501250196,-0.0329142774063519,
0.0682615781503101));
#78284=CARTESIAN_POINT('Ctrl Pts',(0.00861516378733005,-0.0328043479726691,
0.068254244105681));
#78285=CARTESIAN_POINT('Ctrl Pts',(0.00853381983838319,-0.0326943950436593,
0.0682485922201432));
#78286=CARTESIAN_POINT('Ctrl Pts',(0.00869238679588551,-0.0330240426238172,
0.0683455309987005));
#78287=CARTESIAN_POINT('Ctrl Pts',(0.00861242458037248,-0.0329142774063519,
0.0683376979163326));
#78288=CARTESIAN_POINT('Ctrl Pts',(0.00853226056908557,-0.0328043479726691,
0.0683315139712456));
#78289=CARTESIAN_POINT('Ctrl Pts',(0.00845199723992054,-0.0326943950436593,
0.0683269899137652));
#78290=CARTESIAN_POINT('Ctrl Pts',(0.00860739386956141,-0.0330240426238172,
0.0684204799043583));
#78291=CARTESIAN_POINT('Ctrl Pts',(0.00852846414824299,-0.0329142774063519,
0.0684138176823551));
#78292=CARTESIAN_POINT('Ctrl Pts',(0.00844935735084109,-0.0328043479726691,
0.0684087838368103));
#78293=CARTESIAN_POINT('Ctrl Pts',(0.00837017464145789,-0.0326943950436593,
0.0684053876073873));
#78294=CARTESIAN_POINT('',(0.0084936406479108,-0.0326943950436694,0.0682870896025953));
#78295=CARTESIAN_POINT('Ctrl Pts',(0.00862841428596059,-0.0327114338383342,
0.0681712587954722));
#78296=CARTESIAN_POINT('Ctrl Pts',(0.008624802273507,-0.0327619876830778,
0.0682140529181476));
#78297=CARTESIAN_POINT('Ctrl Pts',(0.00862125398462585,-0.0328131562603919,
0.0682560920615946));
#78298=CARTESIAN_POINT('Ctrl Pts',(0.0086142818681561,-0.0329167375858774,
0.0683386957655818));
#78299=CARTESIAN_POINT('Ctrl Pts',(0.0086108608186221,-0.0329691088920621,
0.0683792274125011));
#78300=CARTESIAN_POINT('Ctrl Pts',(0.0086075022092323,-0.0330220786163186,
0.068419019285894));
#78301=CARTESIAN_POINT('Ctrl Pts',(0.00848413919911251,-0.0331951640388604,
0.068411409420108));
#78302=CARTESIAN_POINT('Ctrl Pts',(0.00836549752124305,-0.0330306422053994,
0.0684039592702446));
#78303=CARTESIAN_POINT('Ctrl Pts',(0.00824664929933022,-0.0328657862001532,
0.0684014190716655));
#78304=CARTESIAN_POINT('Ctrl Pts',(0.00848283084063181,-0.0331951640388604,
0.0684098598389315));
#78305=CARTESIAN_POINT('Ctrl Pts',(0.00836415712616587,-0.0330306422053994,
0.0684024367385402));
#78306=CARTESIAN_POINT('Ctrl Pts',(0.0082452780130147,-0.0328657862001532,
0.0683999248904258));
#78307=CARTESIAN_POINT('Ctrl Pts',(0.00826482313138845,-0.0331951640388604,
0.0681516579412534));
#78308=CARTESIAN_POINT('Ctrl Pts',(0.00814081125837241,-0.0330306422053994,
0.0681487420103583));
#78309=CARTESIAN_POINT('Ctrl Pts',(0.00801678483414019,-0.0328657862001532,
0.0681509541120963));
#78310=CARTESIAN_POINT('',(0.00825201024418503,-0.0331781648281895,0.0681513703595991));
#78311=CARTESIAN_POINT('',(0.00826482313138731,-0.0331951640388588,0.0681516579412533));
#78312=CARTESIAN_POINT('Origin',(0.00861133834247988,-0.0326412092360721,
0.0846697652686003));
#78313=CARTESIAN_POINT('Ctrl Pts',(0.00825201024566016,-0.033178164828644,
0.0681513703606867));
#78314=CARTESIAN_POINT('Ctrl Pts',(0.00825109165333182,-0.0331276811560401,
0.0681943435460393));
#78315=CARTESIAN_POINT('Ctrl Pts',(0.00825018968174488,-0.0330765663525361,
0.0682365407694903));
#78316=CARTESIAN_POINT('Ctrl Pts',(0.00824841804298898,-0.0329730614519476,
0.068319419543932));
#78317=CARTESIAN_POINT('Ctrl Pts',(0.00824754908615228,-0.0329207133437511,
0.0683600676141577));
#78318=CARTESIAN_POINT('Ctrl Pts',(0.00824669644230155,-0.0328677532367531,
0.0683999550153815));
#78319=CARTESIAN_POINT('',(0.00837382698601799,-0.0331951640388701,0.0682807588901023));
#78320=CARTESIAN_POINT('Origin',(0.00812378219310841,-0.0315241814719618,
0.07415));
#78321=CARTESIAN_POINT('',(0.00825201024350532,-0.033212160714424,0.0681513703611358));
#78322=CARTESIAN_POINT('',(0.00823919677064574,-0.0331951640388587,0.0681511101464263));
#78323=CARTESIAN_POINT('Origin',(0.00865615796368383,-0.0326413654336508,
0.0846628791406934));
#78324=CARTESIAN_POINT('Origin',(0.0071871319098763,-0.0326412098688358,
0.0846393229117763));
#78325=CARTESIAN_POINT('Origin',(0.00714264784117156,-0.0326413662714906,
0.0846305242971188));
#78326=CARTESIAN_POINT('Ctrl Pts',(0.00840772610977036,-0.0337436976235975,
0.0684056548804768));
#78327=CARTESIAN_POINT('Ctrl Pts',(0.00835606059918607,-0.0336723290703325,
0.0684031010458575));
#78328=CARTESIAN_POINT('Ctrl Pts',(0.00830435751142873,-0.033601104548885,
0.0684014769240775));
#78329=CARTESIAN_POINT('Ctrl Pts',(0.00813927979402415,-0.0333736987606857,
0.0683962914249547));
#78330=CARTESIAN_POINT('Ctrl Pts',(0.00797417653779931,-0.0331450831799192,
0.0684005875823786));
#78331=CARTESIAN_POINT('Ctrl Pts',(0.00815782169841966,-0.0337436976235975,
0.0683987421973904));
#78332=CARTESIAN_POINT('Ctrl Pts',(0.00810609401411603,-0.0336723290703325,
0.0683984360409208));
#78333=CARTESIAN_POINT('Ctrl Pts',(0.008054369191343,-0.033601104548885,
0.0683990603519785));
#78334=CARTESIAN_POINT('Ctrl Pts',(0.00788922207833876,-0.0333736987606857,
0.0684010536535167));
#78335=CARTESIAN_POINT('Ctrl Pts',(0.00772446150184724,-0.0331450831799192,
0.0684125207638257));
#78336=CARTESIAN_POINT('Ctrl Pts',(0.00815532265430615,-0.0337436976235975,
0.0683986730705595));
#78337=CARTESIAN_POINT('Ctrl Pts',(0.00810359434826533,-0.0336723290703325,
0.0683983893908714));
#78338=CARTESIAN_POINT('Ctrl Pts',(0.00805186930814214,-0.033601104548885,
0.0683990361862575));
#78339=CARTESIAN_POINT('Ctrl Pts',(0.0078867215011819,-0.0333736987606857,
0.0684011012758023));
#78340=CARTESIAN_POINT('Ctrl Pts',(0.00772196435148772,-0.0331450831799192,
0.0684126400956403));
#78341=CARTESIAN_POINT('',(0.00812169595724109,-0.0336938721132548,0.0683986418432147));
#78342=CARTESIAN_POINT('',(0.00788540557795273,-0.0333679869984219,0.068403583587206));
#78343=CARTESIAN_POINT('Ctrl Pts',(0.00812169595725132,-0.0336938721132646,
0.0683986418432142));
#78344=CARTESIAN_POINT('Ctrl Pts',(0.00809924570835516,-0.033662918793393,
0.0683986499867719));
#78345=CARTESIAN_POINT('Ctrl Pts',(0.00807680268726717,-0.0336319952301037,
0.0683987895829587));
#78346=CARTESIAN_POINT('Ctrl Pts',(0.0080543691913531,-0.0336011045488947,
0.0683990603519784));
#78347=CARTESIAN_POINT('Ctrl Pts',(0.00799807587379437,-0.0335235892595451,
0.068399739804101));
#78348=CARTESIAN_POINT('Ctrl Pts',(0.00794174250742213,-0.0334458668673266,
0.0684012465815856));
#78349=CARTESIAN_POINT('Ctrl Pts',(0.00788540557794386,-0.0333679869984148,
0.0684035835867571));
#78350=CARTESIAN_POINT('Ctrl Pts',(0.00788536112028597,-0.0333679692463166,
0.0684035847431947));
#78351=CARTESIAN_POINT('Ctrl Pts',(0.00788538582701036,-0.0333391895391197,
0.0684040373217868));
#78352=CARTESIAN_POINT('Ctrl Pts',(0.00788540758825821,-0.0333104081089681,
0.0684043763745313));
#78353=CARTESIAN_POINT('Ctrl Pts',(0.00788544192004787,-0.0332532698661692,
0.0684048248137598));
#78354=CARTESIAN_POINT('Ctrl Pts',(0.00788545462428967,-0.0332249173360562,
0.0684049375528162));
#78355=CARTESIAN_POINT('Ctrl Pts',(0.00788546167119418,-0.0331960985279258,
0.0684049409340705));
#78356=CARTESIAN_POINT('Ctrl Pts',(0.00788546178409538,-0.0331956312646462,
0.0684049409591678));
#78357=CARTESIAN_POINT('Ctrl Pts',(0.00788546189524772,-0.0331951640388588,
0.0684049409545569));
#78358=CARTESIAN_POINT('',(0.00801035448319217,-0.0331951640388587,0.0683997600785164));
#78359=CARTESIAN_POINT('',(0.00794790818922994,-0.0331951640388687,0.0684023505165466));
#78360=CARTESIAN_POINT('',(0.00824669644198909,-0.0335216366567736,0.0683999550364575));
#78361=CARTESIAN_POINT('Origin',(0.00910239711679951,-0.0326434571526194,
0.0850324064906018));
#78362=CARTESIAN_POINT('',(0.00824666740810635,-0.0336938721132327,0.0684013132609321));
#78363=CARTESIAN_POINT('Origin',(0.00848005542000744,-0.0336938867896227,
0.0574832383406437));
#78364=CARTESIAN_POINT('',(0.00818418168268372,-0.0336938721132538,0.0683999775520834));
#78365=CARTESIAN_POINT('Ctrl Pts',(0.00848703646404946,-0.0335235895815171,
0.0681610062335428));
#78366=CARTESIAN_POINT('Ctrl Pts',(0.00840458617361054,-0.0334144449262748,
0.0681560053233215));
#78367=CARTESIAN_POINT('Ctrl Pts',(0.00832193784273545,-0.0333049234473147,
0.0681527020286099));
#78368=CARTESIAN_POINT('Ctrl Pts',(0.00823919677064589,-0.0331951640388587,
0.0681511101464262));
#78369=CARTESIAN_POINT('Ctrl Pts',(0.00840691723154057,-0.0335235895815171,
0.0682411441213866));
#78370=CARTESIAN_POINT('Ctrl Pts',(0.00832557019690479,-0.0334144449262748,
0.068237246210141));
#78371=CARTESIAN_POINT('Ctrl Pts',(0.00824404917646885,-0.0333049234473147,
0.0682350243891827));
#78372=CARTESIAN_POINT('Ctrl Pts',(0.00816245815323709,-0.0331951640388587,
0.0682344909420812));
#78373=CARTESIAN_POINT('Ctrl Pts',(0.00832679799903168,-0.0335235895815171,
0.0683212820092303));
#78374=CARTESIAN_POINT('Ctrl Pts',(0.00824655422019905,-0.0334144449262748,
0.0683184870969605));
#78375=CARTESIAN_POINT('Ctrl Pts',(0.00816616051020225,-0.0333049234473147,
0.0683173467497555));
#78376=CARTESIAN_POINT('Ctrl Pts',(0.00808571953582829,-0.0331951640388587,
0.0683178717377361));
#78377=CARTESIAN_POINT('Ctrl Pts',(0.00824667876652278,-0.0335235895815171,
0.0684014198970741));
#78378=CARTESIAN_POINT('Ctrl Pts',(0.00816753824349331,-0.0334144449262748,
0.06839972798378));
#78379=CARTESIAN_POINT('Ctrl Pts',(0.00808827184393565,-0.0333049234473147,
0.0683996691103284));
#78380=CARTESIAN_POINT('Ctrl Pts',(0.0080089809184195,-0.0331951640388587,
0.0684012525333911));
#78381=CARTESIAN_POINT('',(0.00812477562692895,-0.0331951640388687,0.0682754351124813));
#78382=CARTESIAN_POINT('Ctrl Pts',(0.00825201024343362,-0.0332121607145995,
0.0681513703642628));
#78383=CARTESIAN_POINT('Ctrl Pts',(0.00825109318430936,-0.033262544410958,
0.0681942712586196));
#78384=CARTESIAN_POINT('Ctrl Pts',(0.00825019192755287,-0.0333135300746445,
0.0682364329032445));
#78385=CARTESIAN_POINT('Ctrl Pts',(0.00824842030336822,-0.0334167203140643,
0.0683193111604632));
#78386=CARTESIAN_POINT('Ctrl Pts',(0.00824755062210575,-0.0334688847587333,
0.068359995673575));
#78387=CARTESIAN_POINT('Ctrl Pts',(0.00824669644180204,-0.0335216366562416,
0.0683999550371558));
#78388=CARTESIAN_POINT('Ctrl Pts',(0.00812309870278496,-0.0336938721132533,
0.0684001058694834));
#78389=CARTESIAN_POINT('Ctrl Pts',(0.0080894426644167,-0.0336474569765029,
0.068400109870179));
#78390=CARTESIAN_POINT('Ctrl Pts',(0.00805578897901491,-0.033601104548885,
0.0684005078570237));
#78391=CARTESIAN_POINT('Ctrl Pts',(0.00797058558505805,-0.0334837508592655,
0.0684015154682114));
#78392=CARTESIAN_POINT('Ctrl Pts',(0.00788544946376104,-0.0333660264659096,
0.0684050473901492));
#78393=CARTESIAN_POINT('Ctrl Pts',(0.00812169595727198,-0.0336938721132533,
0.0683986418432148));
#78394=CARTESIAN_POINT('Ctrl Pts',(0.00808803134947216,-0.0336474569765029,
0.0683986540546454));
#78395=CARTESIAN_POINT('Ctrl Pts',(0.008054369191343,-0.033601104548885,
0.0683990603519785));
#78396=CARTESIAN_POINT('Ctrl Pts',(0.00796914434638846,-0.0334837508592655,
0.0684000890034121));
#78397=CARTESIAN_POINT('Ctrl Pts',(0.00788398740697958,-0.0333660264659096,
0.068403642591994));
#78398=CARTESIAN_POINT('Ctrl Pts',(0.00788650306420541,-0.0336938721132533,
0.0681531742438294));
#78399=CARTESIAN_POINT('Ctrl Pts',(0.00785140165309137,-0.0336474569765029,
0.0681545631173086));
#78400=CARTESIAN_POINT('Ctrl Pts',(0.00781631890566614,-0.033601104548885,
0.0681563628019574));
#78401=CARTESIAN_POINT('Ctrl Pts',(0.00772749745522845,-0.0334837508592655,
0.068160919189714));
#78402=CARTESIAN_POINT('Ctrl Pts',(0.00763885002384193,-0.0333660264659096,
0.0681681055403747));
#78403=CARTESIAN_POINT('',(0.00787510014316679,-0.0336769361243754,0.0681551557786681));
#78404=CARTESIAN_POINT('',(0.00788790580513013,-0.0336938721132327,0.0681546382653259));
#78405=CARTESIAN_POINT('Ctrl Pts',(0.00787510014316647,-0.0336769361243751,
0.0681551557786681));
#78406=CARTESIAN_POINT('Ctrl Pts',(0.00787723448785643,-0.0336797586669899,
0.0681550672403853));
#78407=CARTESIAN_POINT('Ctrl Pts',(0.00787936879910747,-0.0336825812712593,
0.068154979845287));
#78408=CARTESIAN_POINT('Ctrl Pts',(0.00788363736050296,-0.0336882266106913,
0.0681548073407118));
#78409=CARTESIAN_POINT('Ctrl Pts',(0.00788577161061702,-0.0336910493458056,
0.0681547222312585));
#78410=CARTESIAN_POINT('Ctrl Pts',(0.00788790580513471,-0.0336938721132295,
0.0681546382653335));
#78411=CARTESIAN_POINT('Ctrl Pts',(0.00787510014316678,-0.0336769361243754,
0.0681551557786681));
#78412=CARTESIAN_POINT('Ctrl Pts',(0.00787683730438134,-0.0336279018392284,
0.0681970325883166));
#78413=CARTESIAN_POINT('Ctrl Pts',(0.00787859945683888,-0.0335767825782273,
0.0682395118483854));
#78414=CARTESIAN_POINT('Ctrl Pts',(0.007882052262458,-0.0334733171828138,
0.0683227467735353));
#78415=CARTESIAN_POINT('Ctrl Pts',(0.00788374523620226,-0.0334209631336572,
0.068363558379654));
#78416=CARTESIAN_POINT('Ctrl Pts',(0.00788540558802949,-0.0333679869844681,
0.0684035835867776));
#78417=CARTESIAN_POINT('',(0.00800480088119561,-0.0336938721132538,0.0682766400542803));
#78418=CARTESIAN_POINT('Origin',(0.00812378219310841,-0.0315241814719618,
0.07415));
#78419=CARTESIAN_POINT('',(0.00787510014322512,-0.0337108120655559,0.06815515577997));
#78420=CARTESIAN_POINT('',(0.00786229561583594,-0.0336938721132327,0.0681557006439514));
#78421=CARTESIAN_POINT('Origin',(0.0074365782648503,-0.0345562518650087,
0.0845486310755648));
#78422=CARTESIAN_POINT('Ctrl Pts',(0.00786229561583568,-0.0336938721132325,
0.068155700643952));
#78423=CARTESIAN_POINT('Ctrl Pts',(0.00786442944729637,-0.0336910493258036,
0.0681556075607988));
#78424=CARTESIAN_POINT('Ctrl Pts',(0.00786656340618438,-0.0336882266006898,
0.0681555156136469));
#78425=CARTESIAN_POINT('Ctrl Pts',(0.00787083158178454,-0.0336825812712704,
0.0681553339917212));
#78426=CARTESIAN_POINT('Ctrl Pts',(0.00787296579847292,-0.0336797586669955,
0.068155244316951));
#78427=CARTESIAN_POINT('Ctrl Pts',(0.00787510014316708,-0.0336769361243751,
0.068155155778668));
#78428=CARTESIAN_POINT('Origin',(0.00966986852248645,-0.0345562518009696,
0.0844559863629194));
#78429=CARTESIAN_POINT('Ctrl Pts',(0.00804652702986067,-0.034243627687391,
0.0683991603535004));
#78430=CARTESIAN_POINT('Ctrl Pts',(0.00782963053700891,-0.033943005420181,
0.0684020740800157));
#78431=CARTESIAN_POINT('Ctrl Pts',(0.00761356969817478,-0.0336441434784052,
0.0684213170614867));
#78432=CARTESIAN_POINT('Ctrl Pts',(0.0077966816178855,-0.034243627687391,
0.0684079506956411));
#78433=CARTESIAN_POINT('Ctrl Pts',(0.00758011665825297,-0.033943005420181,
0.0684202874972104));
#78434=CARTESIAN_POINT('Ctrl Pts',(0.00736509619540987,-0.0336441434784052,
0.0684489018113266));
#78435=CARTESIAN_POINT('Ctrl Pts',(0.00779418316376575,-0.034243627687391,
0.0684080385990625));
#78436=CARTESIAN_POINT('Ctrl Pts',(0.00757762151946541,-0.033943005420181,
0.0684204696313823));
#78437=CARTESIAN_POINT('Ctrl Pts',(0.00736261146038223,-0.0336441434784052,
0.0684491776588249));
#78438=CARTESIAN_POINT('',(0.00776056930730323,-0.0341934961088741,0.0684101218305973));
#78439=CARTESIAN_POINT('',(0.00752505549616061,-0.0338664212871963,0.0684298906172921));
#78440=CARTESIAN_POINT('Origin',(0.00830833166368909,-0.0345610751537998,
0.0851359427198085));
#78441=CARTESIAN_POINT('Origin',(0.00638339852864064,-0.0336938005063805,
0.0575232252220561));
#78442=CARTESIAN_POINT('',(0.00764951775477944,-0.0336938721132327,0.0684182290483187));
#78443=CARTESIAN_POINT('',(0.00758735733926295,-0.0336938721132427,0.0684247354099524));
#78444=CARTESIAN_POINT('',(0.00788540558803474,-0.0340203938281605,0.0684035835867774));
#78445=CARTESIAN_POINT('Origin',(0.00783073237135354,-0.0345589643243248,
0.0850773640322105));
#78446=CARTESIAN_POINT('',(0.00788546189524766,-0.034193496108874,0.0684049409545569));
#78447=CARTESIAN_POINT('Origin',(0.00742873964645005,-0.0341934220717729,
0.0573949626134628));
#78448=CARTESIAN_POINT('',(0.00782301560128544,-0.0341934961088841,0.068407531392587));
#78449=CARTESIAN_POINT('Ctrl Pts',(0.0081102703708805,-0.0340223579322396,
0.0681500152141289));
#78450=CARTESIAN_POINT('Ctrl Pts',(0.0080275149320661,-0.0339125849573575,
0.0681502015773978));
#78451=CARTESIAN_POINT('Ctrl Pts',(0.007944821501827,-0.0338030433565231,
0.0681521006549977));
#78452=CARTESIAN_POINT('Ctrl Pts',(0.00786229561583637,-0.0336938721132327,
0.0681557006439509));
#78453=CARTESIAN_POINT('Ctrl Pts',(0.00803534107479174,-0.0340223579322397,
0.0682350256865303));
#78454=CARTESIAN_POINT('Ctrl Pts',(0.00795375815210837,-0.0339125849573575,
0.068236245520216));
#78455=CARTESIAN_POINT('Ctrl Pts',(0.00787225780452297,-0.0338030433565231,
0.0682391530736658));
#78456=CARTESIAN_POINT('Ctrl Pts',(0.00779094392763323,-0.0336938721132327,
0.0682437353894825));
#78457=CARTESIAN_POINT('Ctrl Pts',(0.00796041177870297,-0.0340223579322397,
0.0683200361589317));
#78458=CARTESIAN_POINT('Ctrl Pts',(0.00788000137215064,-0.0339125849573575,
0.0683222894630343));
#78459=CARTESIAN_POINT('Ctrl Pts',(0.00779969410721894,-0.0338030433565231,
0.0683262054923338));
#78460=CARTESIAN_POINT('Ctrl Pts',(0.00771959223943009,-0.0336938721132327,
0.0683317701350142));
#78461=CARTESIAN_POINT('Ctrl Pts',(0.00788548248261421,-0.0340223579322397,
0.0684050466313331));
#78462=CARTESIAN_POINT('Ctrl Pts',(0.00780624459219291,-0.0339125849573575,
0.0684083334058526));
#78463=CARTESIAN_POINT('Ctrl Pts',(0.00772713040991491,-0.0338030433565231,
0.0684132579110019));
#78464=CARTESIAN_POINT('Ctrl Pts',(0.00764824055122694,-0.0336938721132327,
0.0684198048805459));
#78465=CARTESIAN_POINT('',(0.00775590668531769,-0.0336938721132427,0.0682869648461451));
#78466=CARTESIAN_POINT('Ctrl Pts',(0.00787510014336996,-0.0337108120662704,
0.0681551557835653));
#78467=CARTESIAN_POINT('Ctrl Pts',(0.00787688233389737,-0.0337611408994119,
0.0681981180906034));
#78468=CARTESIAN_POINT('Ctrl Pts',(0.00787863200340158,-0.0338121088780922,
0.0682402964308537));
#78469=CARTESIAN_POINT('Ctrl Pts',(0.00788206789428731,-0.0339153382773239,
0.0683231236016381));
#78470=CARTESIAN_POINT('Ctrl Pts',(0.00788375266207461,-0.033967555847311,
0.0683637373911592));
#78471=CARTESIAN_POINT('Ctrl Pts',(0.0078854055880311,-0.0340203938281304,
0.0684035835868175));
#78472=CARTESIAN_POINT('Ctrl Pts',(0.00776206163108845,-0.0341934961088741,
0.0684114952747232));
#78473=CARTESIAN_POINT('Ctrl Pts',(0.00764342256703021,-0.0340287516186244,
0.0684189735623579));
#78474=CARTESIAN_POINT('Ctrl Pts',(0.00752519396108338,-0.0338644633283559,
0.0684313489024514));
#78475=CARTESIAN_POINT('Ctrl Pts',(0.00776056930730329,-0.0341934961088741,
0.0684101218305973));
#78476=CARTESIAN_POINT('Ctrl Pts',(0.00764190184836983,-0.0340287516186244,
0.0684176309708505));
#78477=CARTESIAN_POINT('Ctrl Pts',(0.00752364614697278,-0.0338644633283559,
0.0684300383107814));
#78478=CARTESIAN_POINT('Ctrl Pts',(0.00751191937521459,-0.0341934961088741,
0.0681812795431451));
#78479=CARTESIAN_POINT('Ctrl Pts',(0.00738852078228368,-0.0340287516186244,
0.0681939293248429));
#78480=CARTESIAN_POINT('Ctrl Pts',(0.00726575045616308,-0.0338644633283559,
0.0682116684549956));
#78481=CARTESIAN_POINT('',(0.00749917147815481,-0.0341764758832383,0.0681826001101547));
#78482=CARTESIAN_POINT('',(0.00751191937521463,-0.034193496108874,0.068181279543145));
#78483=CARTESIAN_POINT('Origin',(0.00871354627553403,-0.0345621026663571,
0.084703696538433));
#78484=CARTESIAN_POINT('Ctrl Pts',(0.00749917147983292,-0.034176475883747,
0.0681826001108439));
#78485=CARTESIAN_POINT('Ctrl Pts',(0.00750363999786195,-0.0341260050041165,
0.0682252912637987));
#78486=CARTESIAN_POINT('Ctrl Pts',(0.00750803088050584,-0.0340749269149653,
0.0682672403398259));
#78487=CARTESIAN_POINT('Ctrl Pts',(0.00751666059557544,-0.0339715436309371,
0.0683496868680737));
#78488=CARTESIAN_POINT('Ctrl Pts',(0.00752089614811635,-0.0339192778242717,
0.0683901530424331));
#78489=CARTESIAN_POINT('Ctrl Pts',(0.00752505549761581,-0.0338664212861681,
0.0684298906157721));
#78490=CARTESIAN_POINT('',(0.00763624434126893,-0.0341934961088841,0.0682957006868812));
#78491=CARTESIAN_POINT('Origin',(0.00812378219310841,-0.0315241814719618,
0.07415));
#78492=CARTESIAN_POINT('',(0.0074991714773945,-0.0342105180190384,0.0681826001109751));
#78493=CARTESIAN_POINT('',(0.00748642642908479,-0.0341934961088739,0.0681839479025));
#78494=CARTESIAN_POINT('Origin',(0.00875886989547323,-0.0345621710737136,
0.0847042138250342));
#78495=CARTESIAN_POINT('Origin',(0.00973218070959005,-0.034562103557307,
0.0845970769388304));
#78496=CARTESIAN_POINT('Origin',(0.00968794611505139,-0.0345621719168675,
0.0846069645717558));
#78497=CARTESIAN_POINT('Ctrl Pts',(0.00765100961461013,-0.0346945769586965,
0.0684180728946081));
#78498=CARTESIAN_POINT('Ctrl Pts',(0.00753095210644929,-0.0345275153362944,
0.0684279753055526));
#78499=CARTESIAN_POINT('Ctrl Pts',(0.00741117496697709,-0.0343603235965185,
0.0684416559758941));
#78500=CARTESIAN_POINT('Ctrl Pts',(0.00729203184244175,-0.034193496108874,
0.0684590691792403));
#78501=CARTESIAN_POINT('Ctrl Pts',(0.00756763177367103,-0.0346945769586965,
0.0684268000947073));
#78502=CARTESIAN_POINT('Ctrl Pts',(0.00744775706021046,-0.0345275153362944,
0.0684384488879129));
#78503=CARTESIAN_POINT('Ctrl Pts',(0.00732821768483326,-0.0343603235965185,
0.0684538706434943));
#78504=CARTESIAN_POINT('Ctrl Pts',(0.00720936651405417,-0.034193496108874,
0.0684730144961536));
#78505=CARTESIAN_POINT('Ctrl Pts',(0.00748425393273184,-0.0346945769586965,
0.0684355272948049));
#78506=CARTESIAN_POINT('Ctrl Pts',(0.0073645620139717,-0.0345275153362944,
0.0684489224702714));
#78507=CARTESIAN_POINT('Ctrl Pts',(0.00724526040268954,-0.0343603235965185,
0.0684660853110933));
#78508=CARTESIAN_POINT('Ctrl Pts',(0.00712670118566658,-0.034193496108874,
0.0684869598130667));
#78509=CARTESIAN_POINT('Ctrl Pts',(0.00740087609179284,-0.0346945769586965,
0.0684442544949057));
#78510=CARTESIAN_POINT('Ctrl Pts',(0.00728136696773278,-0.0345275153362944,
0.0684593960526336));
#78511=CARTESIAN_POINT('Ctrl Pts',(0.0071623031205456,-0.0343603235965185,
0.068478299978695));
#78512=CARTESIAN_POINT('Ctrl Pts',(0.00704403585727901,-0.034193496108874,
0.0685009051299801));
#78513=CARTESIAN_POINT('',(0.00740087609266788,-0.0346945769586966,0.0684442544948143));
#78514=CARTESIAN_POINT('',(0.00716706830798636,-0.0343667727832763,0.0684787723072952));
#78515=CARTESIAN_POINT('Origin',(0.00969561993458519,-0.0345626461566601,
0.0851005265089994));
#78516=CARTESIAN_POINT('Origin',(0.00532857933020388,-0.034193477102778,
0.0575805791713511));
#78517=CARTESIAN_POINT('',(0.007290552731434,-0.034193496108874,0.0684593186994703));
#78518=CARTESIAN_POINT('',(0.00722892351312495,-0.0341934961088839,0.0684697153070706));
#78519=CARTESIAN_POINT('',(0.00752505549780014,-0.0345211942962709,0.0684298906178197));
#78520=CARTESIAN_POINT('Origin',(0.00921707535829783,-0.0345625596120209,
0.0851472734654589));
#78521=CARTESIAN_POINT('',(0.00752519692372647,-0.0346945769586885,0.0684312417715662));
#78522=CARTESIAN_POINT('Origin',(0.00637346058295795,-0.0346945685853895,
0.057427786922971));
#78523=CARTESIAN_POINT('',(0.00746303650820717,-0.0346945769587026,0.0684377481332003));
#78524=CARTESIAN_POINT('Ctrl Pts',(0.00773355391136304,-0.0345231616327841,
0.0681627032904536));
#78525=CARTESIAN_POINT('Ctrl Pts',(0.00765102745566147,-0.0344132092796988,
0.06816808203792));
#78526=CARTESIAN_POINT('Ctrl Pts',(0.0075686165130943,-0.0343032738558979,
0.068175167502508));
#78527=CARTESIAN_POINT('Ctrl Pts',(0.00748642642908473,-0.0341934961088739,
0.0681839479025));
#78528=CARTESIAN_POINT('Ctrl Pts',(0.00766411045535195,-0.0345231616327841,
0.0682522507223301));
#78529=CARTESIAN_POINT('Ctrl Pts',(0.00758281828492609,-0.0344132092796988,
0.068258586650069));
#78530=CARTESIAN_POINT('Ctrl Pts',(0.00750166136247011,-0.0343032738558979,
0.0682666037153261));
#78531=CARTESIAN_POINT('Ctrl Pts',(0.00742074339629089,-0.0341934961088739,
0.0682762889840479));
#78532=CARTESIAN_POINT('Ctrl Pts',(0.00759466699934085,-0.0345231616327841,
0.0683417981542066));
#78533=CARTESIAN_POINT('Ctrl Pts',(0.00751460911419072,-0.0344132092796988,
0.0683490912622181));
#78534=CARTESIAN_POINT('Ctrl Pts',(0.00743470621184593,-0.0343032738558979,
0.0683580399281443));
#78535=CARTESIAN_POINT('Ctrl Pts',(0.00735506036349704,-0.0341934961088739,
0.0683686300655959));
#78536=CARTESIAN_POINT('Ctrl Pts',(0.00752522354332976,-0.0345231616327841,
0.0684313455860831));
#78537=CARTESIAN_POINT('Ctrl Pts',(0.00744639994345534,-0.0344132092796988,
0.0684395958743671));
#78538=CARTESIAN_POINT('Ctrl Pts',(0.00736775106122175,-0.0343032738558979,
0.0684494761409624));
#78539=CARTESIAN_POINT('Ctrl Pts',(0.0072893773307032,-0.0341934961088739,
0.0684609711471438));
#78540=CARTESIAN_POINT('',(0.00738848958026939,-0.0341934961088839,0.0683216333009951));
#78541=CARTESIAN_POINT('Ctrl Pts',(0.00749917147774936,-0.0342105180195407,
0.0681826001144063));
#78542=CARTESIAN_POINT('Ctrl Pts',(0.00750364500559306,-0.0342610556241064,
0.0682253392619848));
#78543=CARTESIAN_POINT('Ctrl Pts',(0.00750803825829279,-0.034312218986965,
0.0682673114776594));
#78544=CARTESIAN_POINT('Ctrl Pts',(0.00751666806445142,-0.03441581196952,
0.0683497588372985));
#78545=CARTESIAN_POINT('Ctrl Pts',(0.00752090108824999,-0.0344681990450097,
0.0683902002596279));
#78546=CARTESIAN_POINT('Ctrl Pts',(0.00752505549779421,-0.0345211942962525,
0.0684298906178449));
#78547=CARTESIAN_POINT('Ctrl Pts',(0.00740245132565116,-0.0346945769586932,
0.0684455312126745));
#78548=CARTESIAN_POINT('Ctrl Pts',(0.00728451546986506,-0.0345296777077528,
0.0684604442179569));
#78549=CARTESIAN_POINT('Ctrl Pts',(0.00716729675700591,-0.0343648066252516,
0.0684802188775543));
#78550=CARTESIAN_POINT('Ctrl Pts',(0.00740087609267687,-0.0346945769586932,
0.0684442544948132));
#78551=CARTESIAN_POINT('Ctrl Pts',(0.00728291384165238,-0.0345296777077528,
0.0684592000669228));
#78552=CARTESIAN_POINT('Ctrl Pts',(0.00716567010212613,-0.0343648066252516,
0.0684790083564589));
#78553=CARTESIAN_POINT('Ctrl Pts',(0.00713834768831118,-0.0346945769586932,
0.0682314766337577));
#78554=CARTESIAN_POINT('Ctrl Pts',(0.00701598640556762,-0.0345296777077528,
0.0682518497948666));
#78555=CARTESIAN_POINT('Ctrl Pts',(0.00689457172048071,-0.0343648066252516,
0.0682772628516183));
#78556=CARTESIAN_POINT('',(0.00712570786525928,-0.0346775396664966,0.0682335950417985));
#78557=CARTESIAN_POINT('',(0.00713834768830782,-0.0346945769586886,0.0682314766337583));
#78558=CARTESIAN_POINT('Origin',(0.0100377842878865,-0.034562661826208,
0.0845777899648913));
#78559=CARTESIAN_POINT('Ctrl Pts',(0.00712570786694295,-0.0346775396670097,
0.0682335950424754));
#78560=CARTESIAN_POINT('Ctrl Pts',(0.00713285378982359,-0.0346269749928344,
0.0682759547095296));
#78561=CARTESIAN_POINT('Ctrl Pts',(0.00713987274912904,-0.0345757902891101,
0.0683175615448052));
#78562=CARTESIAN_POINT('Ctrl Pts',(0.00715366235116246,-0.0344721681088617,
0.068399303846144));
#78563=CARTESIAN_POINT('Ctrl Pts',(0.00716042758215949,-0.0344197714290521,
0.0684394072663182));
#78564=CARTESIAN_POINT('Ctrl Pts',(0.00716706830828532,-0.0343667727831525,
0.068478772307078));
#78565=CARTESIAN_POINT('',(0.00726961189049784,-0.0346945769587026,0.0683378655642963));
#78566=CARTESIAN_POINT('Origin',(0.00812378219310841,-0.0315241814719618,
0.07415));
#78567=CARTESIAN_POINT('',(0.0071257078647268,-0.0347116136489812,0.0682335950430839));
#78568=CARTESIAN_POINT('',(0.00711307259435407,-0.0346945769586886,0.0682357404430474));
#78569=CARTESIAN_POINT('Origin',(0.0100821166646013,-0.0345626689394674,
0.0845684159877676));
#78570=CARTESIAN_POINT('Origin',(0.00973660713539254,-0.0345626626257731,
0.0846285994614035));
#78571=CARTESIAN_POINT('Origin',(0.00969165239065285,-0.0345626697747338,
0.0846342838689481));
#78572=CARTESIAN_POINT('Ctrl Pts',(0.00732877954649289,-0.0352450361874068,
0.0684537965786412));
#78573=CARTESIAN_POINT('Ctrl Pts',(0.00711394370916413,-0.0349452760959493,
0.0684837805954732));
#78574=CARTESIAN_POINT('Ctrl Pts',(0.0069019767166667,-0.034644428984174,
0.0685298617451737));
#78575=CARTESIAN_POINT('Ctrl Pts',(0.00732628713881102,-0.0352450361874068,
0.0684542009657669));
#78576=CARTESIAN_POINT('Ctrl Pts',(0.00711146655319298,-0.0349452760959493,
0.068484278985297));
#78577=CARTESIAN_POINT('Ctrl Pts',(0.00689952184974562,-0.034644428984174,
0.0685304527218228));
#78578=CARTESIAN_POINT('Ctrl Pts',(0.0070795141010024,-0.0352450361874068,
0.0684942392950365));
#78579=CARTESIAN_POINT('Ctrl Pts',(0.00686620358575187,-0.0349452760959493,
0.0685336245124117));
#78580=CARTESIAN_POINT('Ctrl Pts',(0.00665646571894468,-0.034644428984174,
0.0685889652613342));
#78581=CARTESIAN_POINT('Ctrl Pts',(0.00707704637062432,-0.0352450361874068,
0.0684946396783292));
#78582=CARTESIAN_POINT('Ctrl Pts',(0.00686375095607746,-0.0349452760959493,
0.0685341179676828));
#78583=CARTESIAN_POINT('Ctrl Pts',(0.00665403515763668,-0.034644428984174,
0.0685895503867294));
#78584=CARTESIAN_POINT('',(0.00704406719588301,-0.0351951634053301,0.0685008967236133));
#78585=CARTESIAN_POINT('',(0.00681285683139752,-0.0348678972925434,0.0685500357415405));
#78586=CARTESIAN_POINT('Origin',(0.0110413242494258,-0.0345636767881713,
0.0847620907885232));
#78587=CARTESIAN_POINT('Origin',(0.00429423075620386,-0.0346946199341032,
0.0577910621877315));
#78588=CARTESIAN_POINT('',(0.00693487610176077,-0.0346945769330288,0.0685228668663425));
#78589=CARTESIAN_POINT('',(0.00687402129446573,-0.0346945769458128,0.068537112690876));
#78590=CARTESIAN_POINT('',(0.0071670683083037,-0.0350221583435276,0.0684787723072845));
#78591=CARTESIAN_POINT('Origin',(0.0105844074873605,-0.0345628458714861,
0.0849116583843685));
#78592=CARTESIAN_POINT('',(0.00716727704116918,-0.035195136029876,0.0684799914558962));
#78593=CARTESIAN_POINT('Origin',(0.0053343155728567,-0.0351951838366754,
0.0576145372036346));
#78594=CARTESIAN_POINT('',(0.0070440358581378,-0.035195137132875,0.0685009051297173));
#78595=CARTESIAN_POINT('Ctrl Pts',(0.00735837751390443,-0.0350241211494342,
0.0681990206119436));
#78596=CARTESIAN_POINT('Ctrl Pts',(0.00727640521283051,-0.0349144232818962,
0.0682095637475715));
#78597=CARTESIAN_POINT('Ctrl Pts',(0.00719460178153038,-0.0348045283579412,
0.0682218076198117));
#78598=CARTESIAN_POINT('Ctrl Pts',(0.00711307258340003,-0.0346945769439158,
0.0682357404449193));
#78599=CARTESIAN_POINT('Ctrl Pts',(0.00729469381942308,-0.0350241211494342,
0.0682927517639695));
#78600=CARTESIAN_POINT('Ctrl Pts',(0.00721401262653705,-0.0349144232818962,
0.0683041721163775));
#78601=CARTESIAN_POINT('Ctrl Pts',(0.00713351920891297,-0.0348045283579412,
0.0683172670423256));
#78602=CARTESIAN_POINT('Ctrl Pts',(0.0070533172925506,-0.0346945769439158,
0.0683320236055363));
#78603=CARTESIAN_POINT('Ctrl Pts',(0.00723101012494173,-0.0350241211494342,
0.0683864829159954));
#78604=CARTESIAN_POINT('Ctrl Pts',(0.0071516200402436,-0.0349144232818962,
0.0683987804851836));
#78605=CARTESIAN_POINT('Ctrl Pts',(0.00707243663629556,-0.0348045283579412,
0.0684127264648395));
#78606=CARTESIAN_POINT('Ctrl Pts',(0.00699356200170117,-0.0346945769439158,
0.0684283067661533));
#78607=CARTESIAN_POINT('Ctrl Pts',(0.00716732643046039,-0.0350241211494342,
0.0684802140680213));
#78608=CARTESIAN_POINT('Ctrl Pts',(0.00708922745395014,-0.0349144232818962,
0.0684933888539896));
#78609=CARTESIAN_POINT('Ctrl Pts',(0.00701135406367814,-0.0348045283579412,
0.0685081858873534));
#78610=CARTESIAN_POINT('Ctrl Pts',(0.00693380671085173,-0.0346945769439158,
0.0685245899267703));
#78611=CARTESIAN_POINT('',(0.00702397434833165,-0.0346945769458128,0.068379303654558));
#78612=CARTESIAN_POINT('Ctrl Pts',(0.00712570786526901,-0.0347116136492811,
0.0682335950463216));
#78613=CARTESIAN_POINT('Ctrl Pts',(0.00713285093764519,-0.0347621546532048,
0.0682759378935546));
#78614=CARTESIAN_POINT('Ctrl Pts',(0.00713986841550647,-0.0348133084096492,
0.0683175362391114));
#78615=CARTESIAN_POINT('Ctrl Pts',(0.00715365803877717,-0.0349168561544575,
0.0683992786436124));
#78616=CARTESIAN_POINT('Ctrl Pts',(0.00716042471453214,-0.0349692089015917,
0.0684393902794295));
#78617=CARTESIAN_POINT('Ctrl Pts',(0.00716706830829008,-0.0350221583435,
0.068478772307324));
#78618=CARTESIAN_POINT('Ctrl Pts',(0.00704522804053917,-0.0351951371254919,
0.0685017531397606));
#78619=CARTESIAN_POINT('Ctrl Pts',(0.00692845408053324,-0.035030733898094,
0.0685240515701573));
#78620=CARTESIAN_POINT('Ctrl Pts',(0.00681270152137923,-0.0348659306897816,
0.0685511573404456));
#78621=CARTESIAN_POINT('Ctrl Pts',(0.00704403585816338,-0.035195137125492,
0.0685009051298308));
#78622=CARTESIAN_POINT('Ctrl Pts',(0.00692724436608421,-0.035030733898094,
0.0685232282078501));
#78623=CARTESIAN_POINT('Ctrl Pts',(0.00681147530855085,-0.0348659306897816,
0.0685503593293192));
#78624=CARTESIAN_POINT('Ctrl Pts',(0.0068442248494029,-0.035195137125492,
0.0683587777817316));
#78625=CARTESIAN_POINT('Ctrl Pts',(0.00672449496357548,-0.035030733898094,
0.0683852318269914));
#78626=CARTESIAN_POINT('Ctrl Pts',(0.00660596076046755,-0.0348659306897816,
0.068416611832798));
#78627=CARTESIAN_POINT('Origin',(0.00560066682560257,-0.0308609197383906,
0.0633718456812268));
#78628=CARTESIAN_POINT('',(0.00695692276348074,-0.035195137125492,0.0684389408106035));
#78629=CARTESIAN_POINT('Origin',(0.00848199412557994,-0.0351840467441107,
0.0750590818785555));
#78630=CARTESIAN_POINT('Origin',(0.00462868883488077,-0.0352322614588957,
0.0627063745744573));
#78631=CARTESIAN_POINT('',(0.00658359560922478,-0.0351951142564657,0.0686087330085759));
#78632=CARTESIAN_POINT('',(0.00646421102734251,-0.0351951372916786,0.0686447004127151));
#78633=CARTESIAN_POINT('Origin',(0.00789759517336728,-0.0352875118894279,
0.0744046163418812));
#78634=CARTESIAN_POINT('Origin',(0.0155892122750297,-0.0298325076521865,
0.073399970684482));
#78635=CARTESIAN_POINT('Origin',(0.00890344754906864,-0.0338731501726093,
0.0658046183588913));
#78636=CARTESIAN_POINT('Ctrl Pts',(0.0101351648519866,-0.0321934096636942,
0.0687618207579114));
#78637=CARTESIAN_POINT('Ctrl Pts',(0.0100387190094497,-0.0320508460844432,
0.0687258179661549));
#78638=CARTESIAN_POINT('Ctrl Pts',(0.0099413785634212,-0.0319086045663286,
0.0686924336301076));
#78639=CARTESIAN_POINT('Ctrl Pts',(0.00984335902280536,-0.031766989286822,
0.0686617223772792));
#78640=CARTESIAN_POINT('Ctrl Pts',(0.0100559929262052,-0.0321934096636942,
0.0687342120854356));
#78641=CARTESIAN_POINT('Ctrl Pts',(0.00995905290157842,-0.0320508460844432,
0.0686996264334484));
#78642=CARTESIAN_POINT('Ctrl Pts',(0.00986125672182438,-0.0319086045663286,
0.0686676714463398));
#78643=CARTESIAN_POINT('Ctrl Pts',(0.00976282062375176,-0.031766989286822,
0.0686383985931954));
#78644=CARTESIAN_POINT('Ctrl Pts',(0.00997682100042376,-0.0321934096636942,
0.06870660341296));
#78645=CARTESIAN_POINT('Ctrl Pts',(0.00987938679370717,-0.0320508460844432,
0.0686734349007418));
#78646=CARTESIAN_POINT('Ctrl Pts',(0.00978113488022756,-0.0319086045663286,
0.068642909262572));
#78647=CARTESIAN_POINT('Ctrl Pts',(0.00968228222469816,-0.031766989286822,
0.0686150748091116));
#78648=CARTESIAN_POINT('Ctrl Pts',(0.00989764907464233,-0.0321934096636942,
0.0686789947404844));
#78649=CARTESIAN_POINT('Ctrl Pts',(0.00979972068583591,-0.0320508460844432,
0.0686472433680353));
#78650=CARTESIAN_POINT('Ctrl Pts',(0.00970101303863074,-0.0319086045663286,
0.0686181470788042));
#78651=CARTESIAN_POINT('Ctrl Pts',(0.00960174382564456,-0.031766989286822,
0.0685917510250278));
#78652=CARTESIAN_POINT('',(0.00989906547603906,-0.0321934096636942,0.0686794886650928));
#78653=CARTESIAN_POINT('',(0.00967281289770884,-0.0318665617511283,0.0686111708037462));
#78654=CARTESIAN_POINT('Origin',(0.00415979697328217,-0.0326371944421585,
0.0843727579835789));
#78655=CARTESIAN_POINT('Origin',(0.0126250220541809,-0.0316939261509442,
0.0580550327220509));
#78656=CARTESIAN_POINT('',(0.0100172774156477,-0.032019722162186,0.0687193218647438));
#78657=CARTESIAN_POINT('Ctrl Pts',(0.0100171240667253,-0.0320197392094775,
0.0687192184288374));
#78658=CARTESIAN_POINT('Ctrl Pts',(0.00998949048868716,-0.0319792716576073,
0.0687095845410141));
#78659=CARTESIAN_POINT('Ctrl Pts',(0.00996165766720061,-0.0319386439829743,
0.0687001174633433));
#78660=CARTESIAN_POINT('Ctrl Pts',(0.00993359365955867,-0.0318979099381674,
0.0686908152641895));
#78661=CARTESIAN_POINT('Ctrl Pts',(0.00990553020662064,-0.0318571766984962,
0.0686815132488999));
#78662=CARTESIAN_POINT('Ctrl Pts',(0.00987737877403414,-0.0318163871833598,
0.0686724216933247));
#78663=CARTESIAN_POINT('Ctrl Pts',(0.00984923727325862,-0.0317755399638303,
0.0686635685179199));
#78664=CARTESIAN_POINT('',(0.0100170948752984,-0.0321934096636184,0.0687206476364617));
#78665=CARTESIAN_POINT('Origin',(0.0107576046418906,-0.0324114026571386,
0.0665332235056358));
#78666=CARTESIAN_POINT('',(0.00995808017567875,-0.0321934096636663,0.0687000681507873));
#78667=CARTESIAN_POINT('Ctrl Pts',(0.00989994743820871,-0.0321934096636618,
0.0686813150905937));
#78668=CARTESIAN_POINT('Ctrl Pts',(0.00982453001126425,-0.0320835708272592,
0.0686568203876015));
#78669=CARTESIAN_POINT('Ctrl Pts',(0.00974864941288699,-0.0319739230346488,
0.0686339006522635));
#78670=CARTESIAN_POINT('Ctrl Pts',(0.0096724049775894,-0.0318646057455573,
0.0686125777578681));
#78671=CARTESIAN_POINT('Ctrl Pts',(0.00985067131905665,-0.0321934096636618,
0.0685792708411436));
#78672=CARTESIAN_POINT('Ctrl Pts',(0.00977384662238364,-0.0320835708272592,
0.0685554556942381));
#78673=CARTESIAN_POINT('Ctrl Pts',(0.00969657363392936,-0.0319739230346488,
0.0685332442441905));
#78674=CARTESIAN_POINT('Ctrl Pts',(0.00961895340012431,-0.0318646057455573,
0.0685126573213648));
#78675=CARTESIAN_POINT('Ctrl Pts',(0.00980139519990459,-0.0321934096636618,
0.0684772265916935));
#78676=CARTESIAN_POINT('Ctrl Pts',(0.00972316323350302,-0.0320835708272592,
0.0684540910008747));
#78677=CARTESIAN_POINT('Ctrl Pts',(0.00964449785497172,-0.0319739230346488,
0.0684325878361175));
#78678=CARTESIAN_POINT('Ctrl Pts',(0.00956550182265921,-0.0318646057455573,
0.0684127368848614));
#78679=CARTESIAN_POINT('Ctrl Pts',(0.00975211908075253,-0.0321934096636618,
0.0683751823422434));
#78680=CARTESIAN_POINT('Ctrl Pts',(0.00967247984462241,-0.0320835708272592,
0.0683527263075112));
#78681=CARTESIAN_POINT('Ctrl Pts',(0.00959242207601408,-0.0319739230346488,
0.0683319314280444));
#78682=CARTESIAN_POINT('Ctrl Pts',(0.00951205024519412,-0.0318646057455573,
0.0683128164483581));
#78683=CARTESIAN_POINT('',(0.00973978025155323,-0.0321763980308458,0.0683717173612915));
#78684=CARTESIAN_POINT('',(0.00975211908072106,-0.0321934096636184,0.0683751823422345));
#78685=CARTESIAN_POINT('Origin',(0.00469517298259082,-0.0326386230618203,
0.0841317309506976));
#78686=CARTESIAN_POINT('Ctrl Pts',(0.00973978025069336,-0.0321763980306277,
0.0683717173643431));
#78687=CARTESIAN_POINT('Ctrl Pts',(0.00972822077595706,-0.0321259596174817,
0.0684130502804517));
#78688=CARTESIAN_POINT('Ctrl Pts',(0.00971686158412674,-0.0320749164631385,
0.0684536670501569));
#78689=CARTESIAN_POINT('Ctrl Pts',(0.00969453462474263,-0.031971605779392,
0.0685335009838122));
#78690=CARTESIAN_POINT('Ctrl Pts',(0.00968357555652206,-0.0319193786690118,
0.0685726870417803));
#78691=CARTESIAN_POINT('Ctrl Pts',(0.00967281289720152,-0.0318665617525302,
0.0686111708055284));
#78692=CARTESIAN_POINT('',(0.00982559227839006,-0.0321934096636663,0.0685273355036737));
#78693=CARTESIAN_POINT('Origin',(0.00812378219310841,-0.0315241814719618,
0.07415));
#78694=CARTESIAN_POINT('',(0.00973978025165294,-0.0322104233323627,0.0683717173609343));
#78695=CARTESIAN_POINT('',(0.00972743405025982,-0.0321934096636183,0.0683682787406278));
#78696=CARTESIAN_POINT('Origin',(0.00473670438611051,-0.0326387237043649,
0.0841499047667895));
#78697=CARTESIAN_POINT('Origin',(0.00587683744484425,-0.0326386241300037,
0.0844622064349481));
#78698=CARTESIAN_POINT('Origin',(0.00583190441155826,-0.0326387244927525,
0.0844561943596892));
#78699=CARTESIAN_POINT('Ctrl Pts',(0.00982738359587753,-0.0327445246967097,
0.0686567434739962));
#78700=CARTESIAN_POINT('Ctrl Pts',(0.00962020203903971,-0.032443687833936,
0.0685924910967068));
#78701=CARTESIAN_POINT('Ctrl Pts',(0.00940876931146334,-0.0321434074405927,
0.0685440270152576));
#78702=CARTESIAN_POINT('Ctrl Pts',(0.00958704972568487,-0.0327445246967097,
0.0685878984971409));
#78703=CARTESIAN_POINT('Ctrl Pts',(0.00937727163809743,-0.032443687833936,
0.0685327104599476));
#78704=CARTESIAN_POINT('Ctrl Pts',(0.00916393251938352,-0.0321434074405927,
0.06849348054907));
#78705=CARTESIAN_POINT('',(0.00955206611124706,-0.0326943950436612,0.0685788125099592));
#78706=CARTESIAN_POINT('',(0.00932197027682842,-0.0323666188837389,0.0685248359742998));
#78707=CARTESIAN_POINT('Origin',(0.00545093103263963,-0.0326395579112774,
0.0848818413481453));
#78708=CARTESIAN_POINT('Origin',(0.0116229071770842,-0.0321933825602941,
0.0577225648590064));
#78709=CARTESIAN_POINT('',(0.00944394454682107,-0.0321934096532688,0.0685522061170054));
#78710=CARTESIAN_POINT('',(0.00938281589963273,-0.0321934096584275,0.0685391854089375));
#78711=CARTESIAN_POINT('',(0.00967281289796098,-0.0325210109756238,0.0686111708028298));
#78712=CARTESIAN_POINT('Origin',(0.0049921278315033,-0.0326393129156624,
0.0847380218359002));
#78713=CARTESIAN_POINT('',(0.00967244699959204,-0.0326943950436593,0.0686124791361874));
#78714=CARTESIAN_POINT('Origin',(0.0126519322500182,-0.0326943765538051,
0.0579588138369248));
#78715=CARTESIAN_POINT('',(0.00961225655542955,-0.0326943950436702,0.0685956458230833));
#78716=CARTESIAN_POINT('Ctrl Pts',(0.00996502817638299,-0.0325229783203769,
0.0684394997391562));
#78717=CARTESIAN_POINT('Ctrl Pts',(0.00988630905516765,-0.032413025309245,
0.0684141182035422));
#78718=CARTESIAN_POINT('Ctrl Pts',(0.00980707682358036,-0.0323031222208069,
0.0683903689236795));
#78719=CARTESIAN_POINT('Ctrl Pts',(0.00972743404593875,-0.0321934096576658,
0.0683682787394293));
#78720=CARTESIAN_POINT('Ctrl Pts',(0.00986749665100188,-0.0325229783203769,
0.0684971950058001));
#78721=CARTESIAN_POINT('Ctrl Pts',(0.00978957285777552,-0.032413025309245,
0.0684731579401305));
#78722=CARTESIAN_POINT('Ctrl Pts',(0.00971116364563802,-0.0323031222208069,
0.0684507364739161));
#78723=CARTESIAN_POINT('Ctrl Pts',(0.00963237046466076,-0.0321934096576658,
0.0684299557833831));
#78724=CARTESIAN_POINT('Ctrl Pts',(0.00976996512562077,-0.0325229783203769,
0.068554890272444));
#78725=CARTESIAN_POINT('Ctrl Pts',(0.00969283666038338,-0.032413025309245,
0.0685321976767189));
#78726=CARTESIAN_POINT('Ctrl Pts',(0.00961525046769568,-0.0323031222208069,
0.0685111040241527));
#78727=CARTESIAN_POINT('Ctrl Pts',(0.00953730688338278,-0.0321934096576658,
0.0684916328273369));
#78728=CARTESIAN_POINT('Ctrl Pts',(0.00967243360023966,-0.0325229783203769,
0.0686125855390879));
#78729=CARTESIAN_POINT('Ctrl Pts',(0.00959610046299125,-0.032413025309245,
0.0685912374133073));
#78730=CARTESIAN_POINT('Ctrl Pts',(0.00951933728975334,-0.0323031222208069,
0.0685714715743892));
#78731=CARTESIAN_POINT('Ctrl Pts',(0.00944224330210479,-0.0321934096576658,
0.0685533098712907));
#78732=CARTESIAN_POINT('',(0.00958568929905662,-0.0321934096584275,0.0684602424287965));
#78733=CARTESIAN_POINT('Ctrl Pts',(0.00973978025071093,-0.0322104233328948,
0.0683717173642805));
#78734=CARTESIAN_POINT('Ctrl Pts',(0.00972820511270824,-0.0322609421831021,
0.0684131062871274));
#78735=CARTESIAN_POINT('Ctrl Pts',(0.00971683826910974,-0.032312088823999,
0.0684537504170378));
#78736=CARTESIAN_POINT('Ctrl Pts',(0.00969451114066534,-0.0324156524631821,
0.0685335849551975));
#78737=CARTESIAN_POINT('Ctrl Pts',(0.0096835600334637,-0.0324680267167318,
0.0685727425471806));
#78738=CARTESIAN_POINT('Ctrl Pts',(0.009672812897945,-0.0325210109755912,
0.0686111708028703));
#78739=CARTESIAN_POINT('Origin',(0.015390548394678,-0.0262834582511949,
0.0771662053661228));
#78740=CARTESIAN_POINT('Origin',(0.0162906581482553,-0.0342770845939972,
0.0651430105617909));
#78741=CARTESIAN_POINT('Ctrl Pts',(0.00955306077375524,-0.0326943950436604,
0.0685805795236342));
#78742=CARTESIAN_POINT('Ctrl Pts',(0.00947630372138444,-0.0325844576448134,
0.0685608813860393));
#78743=CARTESIAN_POINT('Ctrl Pts',(0.00939913384701679,-0.0324744968375322,
0.0685427693160645));
#78744=CARTESIAN_POINT('Ctrl Pts',(0.0093216503452795,-0.0323646534831894,
0.068526265156173));
#78745=CARTESIAN_POINT('Ctrl Pts',(0.0094974745588082,-0.0326943950436604,
0.0684818308512924));
#78746=CARTESIAN_POINT('Ctrl Pts',(0.00941935656465779,-0.0325844576448134,
0.0684628987959191));
#78747=CARTESIAN_POINT('Ctrl Pts',(0.00934084149603092,-0.0324744968375322,
0.0684455810088901));
#78748=CARTESIAN_POINT('Ctrl Pts',(0.00926203025705925,-0.0323646534831894,
0.0684298982912141));
#78749=CARTESIAN_POINT('Ctrl Pts',(0.00944188834386116,-0.0326943950436604,
0.0683830821789505));
#78750=CARTESIAN_POINT('Ctrl Pts',(0.00936240940793115,-0.0325844576448134,
0.0683649162057989));
#78751=CARTESIAN_POINT('Ctrl Pts',(0.00928254914504506,-0.0324744968375322,
0.0683483927017157));
#78752=CARTESIAN_POINT('Ctrl Pts',(0.009202410168839,-0.0323646534831894,
0.0683335314262551));
#78753=CARTESIAN_POINT('Ctrl Pts',(0.00938630212891412,-0.0326943950436604,
0.0682843335066087));
#78754=CARTESIAN_POINT('Ctrl Pts',(0.0093054622512045,-0.0325844576448134,
0.0682669336156788));
#78755=CARTESIAN_POINT('Ctrl Pts',(0.00922425679405919,-0.0324744968375322,
0.0682512043945413));
#78756=CARTESIAN_POINT('Ctrl Pts',(0.00914279008061875,-0.0323646534831894,
0.0682371645612962));
#78757=CARTESIAN_POINT('',(0.00937377007969489,-0.032677355999134,0.0682816501243087));
#78758=CARTESIAN_POINT('',(0.00938630212891341,-0.0326943950436594,0.0682843335066086));
#78759=CARTESIAN_POINT('Origin',(0.00596353707384605,-0.0326395670796928,
0.084532915372086));
#78760=CARTESIAN_POINT('Ctrl Pts',(0.00937377007899148,-0.032677355998742,
0.0682816501275826));
#78761=CARTESIAN_POINT('Ctrl Pts',(0.00936482153412216,-0.0326267922585947,
0.0683236610884369));
#78762=CARTESIAN_POINT('Ctrl Pts',(0.00935603159574872,-0.0325756109579294,
0.0683649274353469));
#78763=CARTESIAN_POINT('Ctrl Pts',(0.00933876145132211,-0.032471998546237,
0.0684460060209773));
#78764=CARTESIAN_POINT('Ctrl Pts',(0.00933028817185125,-0.0324196091621783,
0.0684857857412956));
#78765=CARTESIAN_POINT('Ctrl Pts',(0.00932197027681829,-0.0323666188837756,
0.0685248359743474));
#78766=CARTESIAN_POINT('',(0.00946918412009023,-0.0326943950436702,0.0684315730082939));
#78767=CARTESIAN_POINT('Origin',(0.00812378219310841,-0.0315241814719618,
0.07415));
#78768=CARTESIAN_POINT('',(0.00937377007968546,-0.0327114338379885,0.0682816501243525));
#78769=CARTESIAN_POINT('',(0.00936123232798897,-0.0326943950436593,0.0682789935135703));
#78770=CARTESIAN_POINT('Origin',(0.0060080083695752,-0.0326395672210718,
0.0845415952384133));
#78771=CARTESIAN_POINT('Origin',(0.00586526092940993,-0.0326395677385031,
0.0845119835878526));
#78772=CARTESIAN_POINT('Origin',(0.00582111352953083,-0.0326395679977111,
0.0845017838739028));
#78773=CARTESIAN_POINT('Ctrl Pts',(0.00947905937737567,-0.0332451089994433,
0.0685606039007953));
#78774=CARTESIAN_POINT('Ctrl Pts',(0.00926825185450242,-0.0329451141710254,
0.0685094887855036));
#78775=CARTESIAN_POINT('Ctrl Pts',(0.00905419301410892,-0.0326442513127493,
0.0684743977672704));
#78776=CARTESIAN_POINT('Ctrl Pts',(0.00923487657364615,-0.0332451089994433,
0.0685069871276474));
#78777=CARTESIAN_POINT('Ctrl Pts',(0.00902204686108887,-0.0329451141710254,
0.0684650815174738));
#78778=CARTESIAN_POINT('Ctrl Pts',(0.00880666527341307,-0.0326442513127493,
0.0684393261607204));
#78779=CARTESIAN_POINT('Ctrl Pts',(0.00923243474560885,-0.0332451089994433,
0.0685064509599159));
#78780=CARTESIAN_POINT('Ctrl Pts',(0.00901958481115473,-0.0329451141710254,
0.0684646374447935));
#78781=CARTESIAN_POINT('Ctrl Pts',(0.00880418999600611,-0.0326442513127493,
0.0684389754446548));
#78782=CARTESIAN_POINT('',(0.00919942996229942,-0.0331951640388616,0.0685001232865986));
#78783=CARTESIAN_POINT('',(0.00896639894183233,-0.0328677532354997,0.0684607010902404));
#78784=CARTESIAN_POINT('Origin',(0.00682186301550851,-0.0326402808281147,
0.0850946833251804));
#78785=CARTESIAN_POINT('Origin',(0.0105858075905475,-0.0326944278779061,
0.0575239786106484));
#78786=CARTESIAN_POINT('',(0.00908985111544921,-0.0326943950436593,0.0684803584031009));
#78787=CARTESIAN_POINT('',(0.00902802551735345,-0.0326943950436694,0.0684712016886965));
#78788=CARTESIAN_POINT('',(0.00932197027683122,-0.0330220786163545,0.0685248359743003));
#78789=CARTESIAN_POINT('Origin',(0.00634268109692061,-0.0326396682763936,
0.085055474472575));
#78790=CARTESIAN_POINT('',(0.00932168725141204,-0.0331951640388587,0.06852616470091));
#78791=CARTESIAN_POINT('Origin',(0.0116199269105786,-0.0331952026560299,
0.057736564890264));
#78792=CARTESIAN_POINT('',(0.00926055860686573,-0.0331951640388701,0.0685131439937643));
#78793=CARTESIAN_POINT('Ctrl Pts',(0.00960282868863939,-0.0330240426238172,
0.0683351550782438));
#78794=CARTESIAN_POINT('Ctrl Pts',(0.00952272353471329,-0.032914277406352,
0.0683147797718027));
#78795=CARTESIAN_POINT('Ctrl Pts',(0.00944215723094673,-0.0328043479726691,
0.0682960503048226));
#78796=CARTESIAN_POINT('Ctrl Pts',(0.00936123232798902,-0.0326943950436593,
0.0682789935135703));
#78797=CARTESIAN_POINT('Ctrl Pts',(0.00950911236822733,-0.0330240426238172,
0.068398860551108));
#78798=CARTESIAN_POINT('Ctrl Pts',(0.00942988481925516,-0.032914277406352,
0.068379776278284));
#78799=CARTESIAN_POINT('Ctrl Pts',(0.00935022324723181,-0.0328043479726691,
0.0683623203460024));
#78800=CARTESIAN_POINT('Ctrl Pts',(0.00927022908870884,-0.0326943950436593,
0.0683465179271179));
#78801=CARTESIAN_POINT('Ctrl Pts',(0.00941539604781526,-0.0330240426238172,
0.0684625660239722));
#78802=CARTESIAN_POINT('Ctrl Pts',(0.00933704610379704,-0.032914277406352,
0.0684447727847653));
#78803=CARTESIAN_POINT('Ctrl Pts',(0.00925828926351689,-0.0328043479726691,
0.0684285903871823));
#78804=CARTESIAN_POINT('Ctrl Pts',(0.00917922584942867,-0.0326943950436593,
0.0684140423406654));
#78805=CARTESIAN_POINT('Ctrl Pts',(0.0093216797274032,-0.0330240426238172,
0.0685262714968365));
#78806=CARTESIAN_POINT('Ctrl Pts',(0.00924420738833892,-0.032914277406352,
0.0685097692912466));
#78807=CARTESIAN_POINT('Ctrl Pts',(0.00916635527980197,-0.0328043479726691,
0.0684948604283621));
#78808=CARTESIAN_POINT('Ctrl Pts',(0.0090882226101485,-0.0326943950436593,
0.068481566754213));
#78809=CARTESIAN_POINT('',(0.00922554172172909,-0.0326943950436694,0.0683796759583456));
#78810=CARTESIAN_POINT('Ctrl Pts',(0.00937377007898977,-0.0327114338383345,
0.068281650127591));
#78811=CARTESIAN_POINT('Ctrl Pts',(0.00936482302256169,-0.032761987683073,
0.0683236541006224));
#78812=CARTESIAN_POINT('Ctrl Pts',(0.00935603381121453,-0.0328131562603818,
0.0683649170343438));
#78813=CARTESIAN_POINT('Ctrl Pts',(0.00933876368263874,-0.0329167375858778,
0.068445995545559));
#78814=CARTESIAN_POINT('Ctrl Pts',(0.00933028964673212,-0.0329691088920621,
0.0684857788171354));
#78815=CARTESIAN_POINT('Ctrl Pts',(0.00932197027681863,-0.0330220786163186,
0.0685248359743463));
#78816=CARTESIAN_POINT('Ctrl Pts',(0.00920053378997214,-0.0331951640388604,
0.0685018246296733));
#78817=CARTESIAN_POINT('Ctrl Pts',(0.00908376138546374,-0.033030642201062,
0.068479563480757));
#78818=CARTESIAN_POINT('Ctrl Pts',(0.00896616868546174,-0.0328657861914645,
0.0684621476801156));
#78819=CARTESIAN_POINT('Ctrl Pts',(0.00919942996230253,-0.0331951640388604,
0.0685001232865992));
#78820=CARTESIAN_POINT('Ctrl Pts',(0.00908262238361688,-0.033030642201062,
0.0684778849586123));
#78821=CARTESIAN_POINT('Ctrl Pts',(0.00896499548270671,-0.0328657861914645,
0.0684604934131856));
#78822=CARTESIAN_POINT('Ctrl Pts',(0.00901550258771073,-0.0331951640388604,
0.0682166337768641));
#78823=CARTESIAN_POINT('Ctrl Pts',(0.00889283404516787,-0.033030642201062,
0.0681981980294236));
#78824=CARTESIAN_POINT('Ctrl Pts',(0.00876950835320592,-0.0328657861914645,
0.0681848480550647));
#78825=CARTESIAN_POINT('',(0.00900282677748922,-0.0331781648281898,0.0682147425822916));
#78826=CARTESIAN_POINT('',(0.00901550258770959,-0.0331951640388588,0.0682166337768639));
#78827=CARTESIAN_POINT('Origin',(0.00728901762487964,-0.0326412092428282,
0.0846479206670505));
#78828=CARTESIAN_POINT('Ctrl Pts',(0.00900282677881569,-0.033178164828644,
0.0682147425835564));
#78829=CARTESIAN_POINT('Ctrl Pts',(0.00899652946141545,-0.0331276811546773,
0.068257261783508));
#78830=CARTESIAN_POINT('Ctrl Pts',(0.00899034588751766,-0.0330765663497778,
0.068299013223338));
#78831=CARTESIAN_POINT('Ctrl Pts',(0.00897820075354882,-0.032973061446299,
0.0683810164308291));
#78832=CARTESIAN_POINT('Ctrl Pts',(0.00897224409454443,-0.0329207133373404,
0.0684212350701986));
#78833=CARTESIAN_POINT('Ctrl Pts',(0.00896639895693368,-0.0328677532289356,
0.0684607010836685));
#78834=CARTESIAN_POINT('',(0.00910746627501451,-0.0331951640388702,0.0683583785317412));
#78835=CARTESIAN_POINT('Origin',(0.00812378219310841,-0.0315241814719618,
0.07415));
#78836=CARTESIAN_POINT('',(0.00900282677662223,-0.0332121607144241,0.0682147425837313));
#78837=CARTESIAN_POINT('',(0.00899014695537356,-0.0331951640388587,0.0682128784669066));
#78838=CARTESIAN_POINT('Origin',(0.00733434671698646,-0.032641365580181,
0.0846467061318248));
#78839=CARTESIAN_POINT('Origin',(0.00587985698336055,-0.0326412098755649,
0.084439217681164));
#78840=CARTESIAN_POINT('Origin',(0.00583682644230013,-0.0326413663090767,
0.0844249134056763));
#78841=CARTESIAN_POINT('Ctrl Pts',(0.00912544447571675,-0.0337436976235975,
0.068486538366723));
#78842=CARTESIAN_POINT('Ctrl Pts',(0.00907450644346596,-0.0336723290703325,
0.0684775292643472));
#78843=CARTESIAN_POINT('Ctrl Pts',(0.00902341460643292,-0.033601104548885,
0.0684694378340787));
#78844=CARTESIAN_POINT('Ctrl Pts',(0.00886028849150909,-0.0333736987606857,
0.0684436035000535));
#78845=CARTESIAN_POINT('Ctrl Pts',(0.00869594867247166,-0.0331450831799191,
0.0684271728560183));
#78846=CARTESIAN_POINT('Ctrl Pts',(0.00887837702421617,-0.0337436976235975,
0.068448358864251));
#78847=CARTESIAN_POINT('Ctrl Pts',(0.00882709559973389,-0.0336723290703325,
0.068441571923978));
#78848=CARTESIAN_POINT('Ctrl Pts',(0.00877570039571424,-0.033601104548885,
0.0684357084728629));
#78849=CARTESIAN_POINT('Ctrl Pts',(0.00861160569009581,-0.0333736987606857,
0.0684169876349365));
#78850=CARTESIAN_POINT('Ctrl Pts',(0.00844670708994683,-0.0331450831799191,
0.06840771434784));
#78851=CARTESIAN_POINT('Ctrl Pts',(0.00887590634970116,-0.0337436976235975,
0.0684479770692262));
#78852=CARTESIAN_POINT('Ctrl Pts',(0.00882462149129657,-0.0336723290703325,
0.0684412123505743));
#78853=CARTESIAN_POINT('Ctrl Pts',(0.00877322325360705,-0.033601104548885,
0.0684353711792508));
#78854=CARTESIAN_POINT('Ctrl Pts',(0.00860911886208168,-0.0333736987606857,
0.0684167214762853));
#78855=CARTESIAN_POINT('Ctrl Pts',(0.00844421467412158,-0.0331450831799191,
0.0684075197627583));
#78856=CARTESIAN_POINT('',(0.00884254872301036,-0.0336938721132548,0.0684437315454411));
#78857=CARTESIAN_POINT('',(0.00860750220198468,-0.0333679869945434,0.0684190192852437));
#78858=CARTESIAN_POINT('Ctrl Pts',(0.0088425487230217,-0.0336938721132647,
0.068443731545442));
#78859=CARTESIAN_POINT('Ctrl Pts',(0.00882027448038528,-0.033662918793393,
0.0684409258624969));
#78860=CARTESIAN_POINT('Ctrl Pts',(0.00879799093318047,-0.0336319952301038,
0.0684382515015221));
#78861=CARTESIAN_POINT('Ctrl Pts',(0.00877570039572543,-0.0336011045488948,
0.0684357084728643));
#78862=CARTESIAN_POINT('Ctrl Pts',(0.00871976580985809,-0.0335235892595452,
0.0684293271437862));
#78863=CARTESIAN_POINT('Ctrl Pts',(0.0086636878005343,-0.0334458668660367,
0.0684237615970615));
#78864=CARTESIAN_POINT('Ctrl Pts',(0.00860750220201912,-0.0333679869945383,
0.0684190192849199));
#78865=CARTESIAN_POINT('Ctrl Pts',(0.00860745794719471,-0.0333679692459108,
0.0684190148598652));
#78866=CARTESIAN_POINT('Ctrl Pts',(0.00860742573596226,-0.0333391895377652,
0.0684194669663275));
#78867=CARTESIAN_POINT('Ctrl Pts',(0.00860740483103624,-0.0333104081066984,
0.0684198060729485));
#78868=CARTESIAN_POINT('Ctrl Pts',(0.00860738268779856,-0.0332532699288407,
0.0684202552784963));
#78869=CARTESIAN_POINT('Ctrl Pts',(0.00860738115929402,-0.0332249176525949,
0.0684203687210718));
#78870=CARTESIAN_POINT('Ctrl Pts',(0.00860738772962057,-0.0331960985150662,
0.0684203729591516));
#78871=CARTESIAN_POINT('Ctrl Pts',(0.00860738783830507,-0.0331956312776463,
0.0684203729981844));
#78872=CARTESIAN_POINT('Ctrl Pts',(0.00860738794916192,-0.0331951640388598,
0.0684203730075412));
#78873=CARTESIAN_POINT('',(0.00873194505769415,-0.0331951640388587,0.0684308861761511));
#78874=CARTESIAN_POINT('',(0.00866966650343826,-0.0331951640388687,0.0684256295918562));
#78875=CARTESIAN_POINT('',(0.0089663989548458,-0.0335216366567732,0.0684607010987125));
#78876=CARTESIAN_POINT('Origin',(0.00773075325147134,-0.0326434571526403,
0.0850692484370686));
#78877=CARTESIAN_POINT('',(0.00896619991923771,-0.0336938721132327,0.0684620449742721));
#78878=CARTESIAN_POINT('Origin',(0.0105661453900854,-0.0336938867896312,
0.0576593136321265));
#78879=CARTESIAN_POINT('',(0.00890437432113403,-0.0336938721132538,0.0684528882598666));
#78880=CARTESIAN_POINT('Ctrl Pts',(0.00923479205017076,-0.0335235895815172,
0.0682537590706003));
#78881=CARTESIAN_POINT('Ctrl Pts',(0.00915361868514744,-0.0334144449262748,
0.0682384638325407));
#78882=CARTESIAN_POINT('Ctrl Pts',(0.00907203607365478,-0.0333049234473147,
0.0682248280027372));
#78883=CARTESIAN_POINT('Ctrl Pts',(0.00899014695537373,-0.0331951640388587,
0.0682128784669064));
#78884=CARTESIAN_POINT('Ctrl Pts',(0.00914526064112622,-0.0335235895815172,
0.0683232234447813));
#78885=CARTESIAN_POINT('Ctrl Pts',(0.00906504358997627,-0.0334144449262748,
0.0683091607828383));
#78886=CARTESIAN_POINT('Ctrl Pts',(0.0089844438551407,-0.0333049234473147,
0.0682967391885072));
#78887=CARTESIAN_POINT('Ctrl Pts',(0.00890356306014734,-0.0331951640388587,
0.0682859838810239));
#78888=CARTESIAN_POINT('Ctrl Pts',(0.00905572923208167,-0.0335235895815172,
0.0683926878189622));
#78889=CARTESIAN_POINT('Ctrl Pts',(0.00897646849480509,-0.0334144449262748,
0.0683798577331359));
#78890=CARTESIAN_POINT('Ctrl Pts',(0.00889685163662663,-0.0333049234473147,
0.0683686503742772));
#78891=CARTESIAN_POINT('Ctrl Pts',(0.00881697916492096,-0.0331951640388587,
0.0683590892951414));
#78892=CARTESIAN_POINT('Ctrl Pts',(0.00896619782303712,-0.0335235895815172,
0.0684621521931432));
#78893=CARTESIAN_POINT('Ctrl Pts',(0.00888789339963391,-0.0334144449262748,
0.0684505546834335));
#78894=CARTESIAN_POINT('Ctrl Pts',(0.00880925941811255,-0.0333049234473147,
0.0684405615600472));
#78895=CARTESIAN_POINT('Ctrl Pts',(0.00873039526969457,-0.0331951640388587,
0.0684321947092588));
#78896=CARTESIAN_POINT('',(0.00886104600654386,-0.0331951640388687,0.0683218823215388));
#78897=CARTESIAN_POINT('Ctrl Pts',(0.00900282677615849,-0.0332121607145997,
0.0682147425868254));
#78898=CARTESIAN_POINT('Ctrl Pts',(0.00899654004050732,-0.0332625444109542,
0.0682571902568275));
#78899=CARTESIAN_POINT('Ctrl Pts',(0.00899036163517683,-0.0333135300746364,
0.0682989064868647));
#78900=CARTESIAN_POINT('Ctrl Pts',(0.00897821658080767,-0.0334167203140643,
0.0683809091808895));
#78901=CARTESIAN_POINT('Ctrl Pts',(0.00897225463565744,-0.0334688847587331,
0.0684211638844984));
#78902=CARTESIAN_POINT('Ctrl Pts',(0.00896639895457182,-0.0335216366562408,
0.0684607010993822));
#78903=CARTESIAN_POINT('Ctrl Pts',(0.00884314451846207,-0.0336938721132389,
0.0684445345041274));
#78904=CARTESIAN_POINT('Ctrl Pts',(0.00880974853564058,-0.0336474569764957,
0.0684403238377273));
#78905=CARTESIAN_POINT('Ctrl Pts',(0.0087763055499666,-0.033601104548885,
0.0684365044019894));
#78906=CARTESIAN_POINT('Ctrl Pts',(0.0086916355992645,-0.0334837508592656,
0.0684268344688444));
#78907=CARTESIAN_POINT('Ctrl Pts',(0.0086067162891965,-0.0333660264659097,
0.0684196777282104));
#78908=CARTESIAN_POINT('Ctrl Pts',(0.00884254872303063,-0.0336938721132389,
0.0684437315454438));
#78909=CARTESIAN_POINT('Ctrl Pts',(0.00880914804022551,-0.0336474569764957,
0.0684395243664322));
#78910=CARTESIAN_POINT('Ctrl Pts',(0.00877570039571424,-0.033601104548885,
0.0684357084728629));
#78911=CARTESIAN_POINT('Ctrl Pts',(0.00869101864990724,-0.0334837508592656,
0.0684260475076745));
#78912=CARTESIAN_POINT('Ctrl Pts',(0.00860608781565303,-0.0333660264659097,
0.0684189000805725));
#78913=CARTESIAN_POINT('Ctrl Pts',(0.00863997564415778,-0.0336938721132389,
0.0681707220456216));
#78914=CARTESIAN_POINT('Ctrl Pts',(0.00860497694615604,-0.0336474569764957,
0.0681677005940614));
#78915=CARTESIAN_POINT('Ctrl Pts',(0.00856994527638209,-0.033601104548885,
0.0681650890534824));
#78916=CARTESIAN_POINT('Ctrl Pts',(0.00848125314280023,-0.0334837508592656,
0.0681584772331672));
#78917=CARTESIAN_POINT('Ctrl Pts',(0.00839240403432243,-0.0333660264659097,
0.0681544964480833));
#78918=CARTESIAN_POINT('',(0.00862841428638208,-0.0336769361243754,0.0681712587904779));
#78919=CARTESIAN_POINT('',(0.00864118383349715,-0.033693872113232,0.0681723503329048));
#78920=CARTESIAN_POINT('Ctrl Pts',(0.00862841428638182,-0.0336769361243751,
0.0681712587904778));
#78921=CARTESIAN_POINT('Ctrl Pts',(0.00863054289791591,-0.0336797586669902,
0.0681714384546674));
#78922=CARTESIAN_POINT('Ctrl Pts',(0.00863267133299573,-0.0336825812712599,
0.0681716192488361));
#78923=CARTESIAN_POINT('Ctrl Pts',(0.00863692785609007,-0.033688226610724,
0.0681719830971155));
#78924=CARTESIAN_POINT('Ctrl Pts',(0.00863905594407222,-0.0336910493458711,
0.0681721661512459));
#78925=CARTESIAN_POINT('Ctrl Pts',(0.0086411838335001,-0.0336938721132293,
0.0681723503329129));
#78926=CARTESIAN_POINT('Ctrl Pts',(0.00862841428638209,-0.0336769361243754,
0.0681712587904779));
#78927=CARTESIAN_POINT('Ctrl Pts',(0.00862488911540854,-0.0336279007516212,
0.068213024039362));
#78928=CARTESIAN_POINT('Ctrl Pts',(0.00862131375149712,-0.0335767878632074,
0.0682553839602703));
#78929=CARTESIAN_POINT('Ctrl Pts',(0.00861430704219723,-0.0334733198857322,
0.0683383975105235));
#78930=CARTESIAN_POINT('Ctrl Pts',(0.0086108715253995,-0.0334209645014077,
0.0683791005615683));
#78931=CARTESIAN_POINT('Ctrl Pts',(0.00860750220923624,-0.0333679869844681,
0.0684190192858466));
#78932=CARTESIAN_POINT('',(0.00874186627826375,-0.0336938721132534,0.068308040939183));
#78933=CARTESIAN_POINT('Origin',(0.00812378219310841,-0.0315241814719618,
0.07415));
#78934=CARTESIAN_POINT('',(0.00862841428627746,-0.033710812065556,0.0681712587917762));
#78935=CARTESIAN_POINT('',(0.00861564243684592,-0.0336938721132327,0.0681701945265211));
#78936=CARTESIAN_POINT('Origin',(0.00613870297800496,-0.0345562519032924,
0.0843805051160357));
#78937=CARTESIAN_POINT('Ctrl Pts',(0.00861564243684644,-0.0336938721132331,
0.0681701945265203));
#78938=CARTESIAN_POINT('Ctrl Pts',(0.00861777111120703,-0.0336910493226405,
0.0681703696175487));
#78939=CARTESIAN_POINT('Ctrl Pts',(0.00861989976603181,-0.0336882265991082,
0.0681705458512997));
#78940=CARTESIAN_POINT('Ctrl Pts',(0.00862415704786373,-0.0336825812712695,
0.0681709006056672));
#78941=CARTESIAN_POINT('Ctrl Pts',(0.00862628567484466,-0.033679758666995,
0.068171079126288));
#78942=CARTESIAN_POINT('Ctrl Pts',(0.00862841428638236,-0.0336769361243751,
0.0681712587904779));
#78943=CARTESIAN_POINT('Origin',(0.008365994683725,-0.0345562518554779,
0.0845684961448049));
#78944=CARTESIAN_POINT('Ctrl Pts',(0.00876790753850355,-0.0342436276873911,
0.0684348248023863));
#78945=CARTESIAN_POINT('Ctrl Pts',(0.00855235615251585,-0.033943005420181,
0.0684105312144997));
#78946=CARTESIAN_POINT('Ctrl Pts',(0.00833558723283896,-0.0336441434784052,
0.0684025428557366));
#78947=CARTESIAN_POINT('Ctrl Pts',(0.00851893051022238,-0.0342436276873911,
0.0684122318966795));
#78948=CARTESIAN_POINT('Ctrl Pts',(0.00830252701874881,-0.033943005420181,
0.0683973286322161));
#78949=CARTESIAN_POINT('Ctrl Pts',(0.0080856157319643,-0.0336441434784052,
0.0683987681040282));
#78950=CARTESIAN_POINT('Ctrl Pts',(0.00851644073993956,-0.0342436276873911,
0.0684120059676224));
#78951=CARTESIAN_POINT('Ctrl Pts',(0.00830002872741114,-0.033943005420181,
0.0683971966063933));
#78952=CARTESIAN_POINT('Ctrl Pts',(0.00808311601695554,-0.0336441434784052,
0.0683987303565111));
#78953=CARTESIAN_POINT('',(0.00848283084063066,-0.0341934961088741,0.0684098598389313));
#78954=CARTESIAN_POINT('',(0.00824669644070164,-0.0338664212863613,0.0683999550358944));
#78955=CARTESIAN_POINT('Origin',(0.00692997697895972,-0.034561072040625,
0.0850724463328746));
#78956=CARTESIAN_POINT('Origin',(0.00848102226634798,-0.0336938005072915,
0.0574362049537827));
#78957=CARTESIAN_POINT('',(0.00837163885895573,-0.0336938721132327,0.0684039846786494));
#78958=CARTESIAN_POINT('',(0.00830915313354104,-0.0336938721132427,0.0684026489698008));
#78959=CARTESIAN_POINT('',(0.00860750220924159,-0.0340203938281605,0.0684190192858471));
#78960=CARTESIAN_POINT('Origin',(0.00646348128806438,-0.0345589643244434,
0.0849544696214529));
#78961=CARTESIAN_POINT('',(0.00860738794916238,-0.034193496108874,0.0684203730075413));
#78962=CARTESIAN_POINT('Origin',(0.00953418318736831,-0.0341934220717554,
0.0574399691515785));
#78963=CARTESIAN_POINT('',(0.00854510939490652,-0.0341934961088841,0.0684151164232464));
#78964=CARTESIAN_POINT('Ctrl Pts',(0.00886237441018436,-0.0340223579322396,
0.0681956334059029));
#78965=CARTESIAN_POINT('Ctrl Pts',(0.00878024816521174,-0.0339125849573574,
0.0681854462929001));
#78966=CARTESIAN_POINT('Ctrl Pts',(0.00869796877983302,-0.0338030433565231,
0.0681769661606995));
#78967=CARTESIAN_POINT('Ctrl Pts',(0.00861564243684641,-0.0336938721132327,
0.0681701945265206));
#78968=CARTESIAN_POINT('Ctrl Pts',(0.00877738131658268,-0.0340223579322397,
0.0682705824143705));
#78969=CARTESIAN_POINT('Ctrl Pts',(0.00869628881391204,-0.0339125849573575,
0.0682615675777997));
#78970=CARTESIAN_POINT('Ctrl Pts',(0.00861506670783471,-0.0338030433565231,
0.0682542375022226));
#78971=CARTESIAN_POINT('Ctrl Pts',(0.00853381969869298,-0.0336938721132327,
0.0682485923539863));
#78972=CARTESIAN_POINT('Ctrl Pts',(0.00869238822298099,-0.0340223579322397,
0.0683455314228382));
#78973=CARTESIAN_POINT('Ctrl Pts',(0.00861232946261234,-0.0339125849573575,
0.0683376888626994));
#78974=CARTESIAN_POINT('Ctrl Pts',(0.0085321646358364,-0.0338030433565231,
0.0683315088437457));
#78975=CARTESIAN_POINT('Ctrl Pts',(0.00845199696053956,-0.0336938721132327,
0.0683269901814519));
#78976=CARTESIAN_POINT('Ctrl Pts',(0.0086073951293793,-0.0340223579322397,
0.0684204804313058));
#78977=CARTESIAN_POINT('Ctrl Pts',(0.00852837011131264,-0.0339125849573575,
0.0684138101475991));
#78978=CARTESIAN_POINT('Ctrl Pts',(0.00844926256383809,-0.0338030433565231,
0.0684087801852688));
#78979=CARTESIAN_POINT('Ctrl Pts',(0.00837017422238613,-0.0336938721132327,
0.0684053880089176));
#78980=CARTESIAN_POINT('',(0.00849364064791083,-0.0336938721132427,0.0682870896025953));
#78981=CARTESIAN_POINT('Ctrl Pts',(0.00862841428596992,-0.0337108120662706,
0.068171258795362));
#78982=CARTESIAN_POINT('Ctrl Pts',(0.0086247978185304,-0.0337611408994095,
0.0682141056994763));
#78983=CARTESIAN_POINT('Ctrl Pts',(0.00862124734359817,-0.0338121088780875,
0.0682561707426506));
#78984=CARTESIAN_POINT('Ctrl Pts',(0.00861427514431629,-0.0339153382773245,
0.0683387754277732));
#78985=CARTESIAN_POINT('Ctrl Pts',(0.00861085636963837,-0.0339675558473123,
0.0683792801228283));
#78986=CARTESIAN_POINT('Ctrl Pts',(0.00860750220923303,-0.0340203938281304,
0.0684190192858864));
#78987=CARTESIAN_POINT('Ctrl Pts',(0.00848413925925491,-0.0341934961088741,
0.06841140949134));
#78988=CARTESIAN_POINT('Ctrl Pts',(0.00836549842141796,-0.0340287516182428,
0.068403959392891));
#78989=CARTESIAN_POINT('Ctrl Pts',(0.00824665104168689,-0.0338644633275951,
0.0684014191762442));
#78990=CARTESIAN_POINT('Ctrl Pts',(0.00848283084063074,-0.0341934961088741,
0.0684098598389314));
#78991=CARTESIAN_POINT('Ctrl Pts',(0.00836415796495106,-0.0340287516182428,
0.0684024367910067));
#78992=CARTESIAN_POINT('Ctrl Pts',(0.0082452796927717,-0.033864463327595,
0.0683999249259183));
#78993=CARTESIAN_POINT('Ctrl Pts',(0.00826482313138735,-0.0341934961088741,
0.0681516579412533));
#78994=CARTESIAN_POINT('Ctrl Pts',(0.0081408121348877,-0.0340287516182428,
0.0681487420309681));
#78995=CARTESIAN_POINT('Ctrl Pts',(0.00801678658662852,-0.033864463327595,
0.0681509540808397));
#78996=CARTESIAN_POINT('',(0.00825201024437053,-0.0341764758832384,0.0681513703600372));
#78997=CARTESIAN_POINT('',(0.00826482313138735,-0.034193496108874,0.0681516579412533));
#78998=CARTESIAN_POINT('Origin',(0.00738616690623692,-0.0345621026576131,
0.0846943946009223));
#78999=CARTESIAN_POINT('Ctrl Pts',(0.0082520102459485,-0.0341764758837473,
0.0681513703609318));
#79000=CARTESIAN_POINT('Ctrl Pts',(0.0082510929081322,-0.0341260050040342,
0.0681942849352783));
#79001=CARTESIAN_POINT('Ctrl Pts',(0.00825019155400999,-0.0340749269147992,
0.0682364535538986));
#79002=CARTESIAN_POINT('Ctrl Pts',(0.00824841993121393,-0.0339715436305663,
0.0683193315568962));
#79003=CARTESIAN_POINT('Ctrl Pts',(0.00824755032866946,-0.0339192778235215,
0.0683600094991655));
#79004=CARTESIAN_POINT('Ctrl Pts',(0.00824669644189481,-0.0338664212853738,
0.0683999550346134));
#79005=CARTESIAN_POINT('',(0.00837382698601901,-0.0341934961088841,0.0682807588901023));
#79006=CARTESIAN_POINT('Origin',(0.00812378219310841,-0.0315241814719618,
0.07415));
#79007=CARTESIAN_POINT('',(0.00825201024351351,-0.0342105180190385,0.0681513703607559));
#79008=CARTESIAN_POINT('',(0.00823919677064574,-0.0341934961088739,0.0681511101464263));
#79009=CARTESIAN_POINT('Origin',(0.00743106824044017,-0.0345621711153071,
0.0847005881547815));
#79010=CARTESIAN_POINT('Origin',(0.00841013196553991,-0.0345621034777229,
0.0847162844815517));
#79011=CARTESIAN_POINT('Origin',(0.00836500708698931,-0.0345621719574124,
0.0847205499687025));
#79012=CARTESIAN_POINT('Ctrl Pts',(0.00837313852628012,-0.0346945769586966,
0.0684040167358742));
#79013=CARTESIAN_POINT('Ctrl Pts',(0.00825278660624681,-0.0345275153362944,
0.0683987938676391));
#79014=CARTESIAN_POINT('Ctrl Pts',(0.00813223930264381,-0.0343603235965185,
0.0683973546056114));
#79015=CARTESIAN_POINT('Ctrl Pts',(0.00801185320414964,-0.034193496108874,
0.0683996979075932));
#79016=CARTESIAN_POINT('Ctrl Pts',(0.00828932433605479,-0.0346945769586966,
0.0684022251049759));
#79017=CARTESIAN_POINT('Ctrl Pts',(0.00816893488959499,-0.0345275153362944,
0.0683987577585124));
#79018=CARTESIAN_POINT('Ctrl Pts',(0.00804840525940311,-0.0343603235965185,
0.0683990756524959));
#79019=CARTESIAN_POINT('Ctrl Pts',(0.00792809190464829,-0.034193496108874,
0.0684031725486176));
#79020=CARTESIAN_POINT('Ctrl Pts',(0.00820551014582946,-0.0346945769586966,
0.0684004334740784));
#79021=CARTESIAN_POINT('Ctrl Pts',(0.00808508317294308,-0.0345275153362944,
0.0683987216493865));
#79022=CARTESIAN_POINT('Ctrl Pts',(0.00796457121616235,-0.0343603235965185,
0.0684007966993806));
#79023=CARTESIAN_POINT('Ctrl Pts',(0.00784433060514703,-0.034193496108874,
0.0684066471896415));
#79024=CARTESIAN_POINT('Ctrl Pts',(0.00812169595560415,-0.0346945769586966,
0.0683986418431793));
#79025=CARTESIAN_POINT('Ctrl Pts',(0.00800123145629136,-0.0345275153362944,
0.0683986855402592));
#79026=CARTESIAN_POINT('Ctrl Pts',(0.00788073717292172,-0.0343603235965185,
0.0684025177462647));
#79027=CARTESIAN_POINT('Ctrl Pts',(0.0077605693056456,-0.034193496108874,
0.0684101218306662));
#79028=CARTESIAN_POINT('',(0.00812169595725133,-0.0346945769586966,0.0683986418432147));
#79029=CARTESIAN_POINT('',(0.0078854055874641,-0.0343667727836481,0.0684035835867093));
#79030=CARTESIAN_POINT('Origin',(0.00831075887806156,-0.0345626474182898,
0.0852111818206586));
#79031=CARTESIAN_POINT('Origin',(0.00742731571724248,-0.0341934771023922,
0.0573609022276176));
#79032=CARTESIAN_POINT('',(0.00801035448319213,-0.034193496108874,0.0683997600785164));
#79033=CARTESIAN_POINT('',(0.0079479081892299,-0.0341934961088839,0.0684023505165466));
#79034=CARTESIAN_POINT('',(0.00824669644183473,-0.0345211942962704,0.0683999550360667));
#79035=CARTESIAN_POINT('Origin',(0.00783013057141495,-0.0345625596119596,
0.0851975826479658));
#79036=CARTESIAN_POINT('',(0.00824666740810637,-0.0346945769586885,0.0684013132609321));
#79037=CARTESIAN_POINT('Origin',(0.00848311153581144,-0.034694568585393,
0.0573402731026649));
#79038=CARTESIAN_POINT('',(0.00818418168268885,-0.0346945769587026,0.0683999775520834));
#79039=CARTESIAN_POINT('Ctrl Pts',(0.00848703823483649,-0.0345231616327842,
0.0681610063409479));
#79040=CARTESIAN_POINT('Ctrl Pts',(0.00840448838907507,-0.0344132092796988,
0.0681559993678363));
#79041=CARTESIAN_POINT('Ctrl Pts',(0.00832183923721686,-0.0343032738558979,
0.0681527001315066));
#79042=CARTESIAN_POINT('Ctrl Pts',(0.0082391967706457,-0.0341934961088739,
0.0681511101464262));
#79043=CARTESIAN_POINT('Ctrl Pts',(0.00840691909202334,-0.0345231616327842,
0.0682411440916858));
#79044=CARTESIAN_POINT('Ctrl Pts',(0.00832547383233092,-0.0344132092796988,
0.0682372414481591));
#79045=CARTESIAN_POINT('Ctrl Pts',(0.00824395205173651,-0.0343032738558979,
0.0682350236369445));
#79046=CARTESIAN_POINT('Ctrl Pts',(0.00816245826184278,-0.0341934961088739,
0.0682344908240748));
#79047=CARTESIAN_POINT('Ctrl Pts',(0.00832679994921019,-0.0345231616327842,
0.0683212818424236));
#79048=CARTESIAN_POINT('Ctrl Pts',(0.00824645927558676,-0.0344132092796988,
0.0683184835284819));
#79049=CARTESIAN_POINT('Ctrl Pts',(0.00816606486625616,-0.0343032738558979,
0.0683173471423824));
#79050=CARTESIAN_POINT('Ctrl Pts',(0.00808571975303985,-0.0341934961088739,
0.0683178715017235));
#79051=CARTESIAN_POINT('Ctrl Pts',(0.00824668080639703,-0.0345231616327842,
0.0684014195931615));
#79052=CARTESIAN_POINT('Ctrl Pts',(0.0081674447188426,-0.0344132092796988,
0.0683997256088047));
#79053=CARTESIAN_POINT('Ctrl Pts',(0.00808817768077582,-0.0343032738558979,
0.0683996706478203));
#79054=CARTESIAN_POINT('Ctrl Pts',(0.00800898124423693,-0.0341934961088739,
0.0684012521793721));
#79055=CARTESIAN_POINT('',(0.00812477562692893,-0.0341934961088839,0.0682754351124813));
#79056=CARTESIAN_POINT('Ctrl Pts',(0.0082520102434348,-0.0342105180195408,
0.0681513703642054));
#79057=CARTESIAN_POINT('Ctrl Pts',(0.0082510918606096,-0.0342610556241025,
0.0681943331825463));
#79058=CARTESIAN_POINT('Ctrl Pts',(0.00825018995768933,-0.034312218986956,
0.0682365250553266));
#79059=CARTESIAN_POINT('Ctrl Pts',(0.00824841832106623,-0.0344158119695194,
0.0683194038944269));
#79060=CARTESIAN_POINT('Ctrl Pts',(0.0082475493119773,-0.0344681990450092,
0.0683600569626224));
#79061=CARTESIAN_POINT('Ctrl Pts',(0.00824669644182474,-0.0345211942962516,
0.0683999550360913));
#79062=CARTESIAN_POINT('Ctrl Pts',(0.00812309875368016,-0.0346945769586932,
0.068400105922614));
#79063=CARTESIAN_POINT('Ctrl Pts',(0.008004223762275,-0.0345296777079064,
0.0684001200522406));
#79064=CARTESIAN_POINT('Ctrl Pts',(0.00788545093205472,-0.0343648066255586,
0.0684050473824189));
#79065=CARTESIAN_POINT('Ctrl Pts',(0.00812169595726038,-0.0346945769586932,
0.0683986418432148));
#79066=CARTESIAN_POINT('Ctrl Pts',(0.00800279069704963,-0.0345296777079064,
0.0683986849746647));
#79067=CARTESIAN_POINT('Ctrl Pts',(0.00788398882256008,-0.0343648066255586,
0.0684036425329222));
#79068=CARTESIAN_POINT('Ctrl Pts',(0.00788790580513354,-0.0346945769586932,
0.0681546382653258));
#79069=CARTESIAN_POINT('Ctrl Pts',(0.0077639559436077,-0.0345296777079064,
0.0681595148427402));
#79070=CARTESIAN_POINT('Ctrl Pts',(0.00764031354911486,-0.0343648066255586,
0.0681695102148508));
#79071=CARTESIAN_POINT('',(0.0078751001439325,-0.0346775396664968,0.0681551557791907));
#79072=CARTESIAN_POINT('',(0.00788790580513014,-0.0346945769586886,0.0681546382653259));
#79073=CARTESIAN_POINT('Origin',(0.0087157432631322,-0.0345626617603281,
0.0847354518265223));
#79074=CARTESIAN_POINT('Ctrl Pts',(0.00787510014551747,-0.0346775396670097,
0.0681551557800743));
#79075=CARTESIAN_POINT('Ctrl Pts',(0.00787688064661579,-0.0346269749928753,
0.0681980770500881));
#79076=CARTESIAN_POINT('Ctrl Pts',(0.00787862954012581,-0.0345757902891929,
0.0682402355118727));
#79077=CARTESIAN_POINT('Ctrl Pts',(0.00788206538008038,-0.0344721681090186,
0.0683230615461074));
#79078=CARTESIAN_POINT('Ctrl Pts',(0.00788375097388189,-0.0344197714292427,
0.068363696647088));
#79079=CARTESIAN_POINT('Ctrl Pts',(0.00788540558804893,-0.0343667727834134,
0.0684035835863732));
#79080=CARTESIAN_POINT('',(0.00800480088120074,-0.0346945769587026,0.0682766400542803));
#79081=CARTESIAN_POINT('Origin',(0.00812378219310841,-0.0315241814719618,
0.07415));
#79082=CARTESIAN_POINT('',(0.00787510014324329,-0.0347116136489629,0.0681551557803994));
#79083=CARTESIAN_POINT('',(0.00786229561583599,-0.0346945769586885,0.0681557006439514));
#79084=CARTESIAN_POINT('Origin',(0.00876090076159747,-0.0345626690069087,
0.0847317081345435));
#79085=CARTESIAN_POINT('Origin',(0.00841057271511297,-0.0345626625822889,
0.0847481130835297));
#79086=CARTESIAN_POINT('Origin',(0.00836526010754044,-0.0345626698054885,
0.0847481183952486));
#79087=CARTESIAN_POINT('Ctrl Pts',(0.00804897197365624,-0.0352450361874068,
0.0683990725915997));
#79088=CARTESIAN_POINT('Ctrl Pts',(0.00783207218728833,-0.0349452760959492,
0.0684018941053252));
#79089=CARTESIAN_POINT('Ctrl Pts',(0.00761600111833985,-0.0346444289841739,
0.068421045382818));
#79090=CARTESIAN_POINT('Ctrl Pts',(0.00804644853620733,-0.0352450361874068,
0.0683991614084979));
#79091=CARTESIAN_POINT('Ctrl Pts',(0.00782955209962371,-0.0349452760959492,
0.0684020780952285));
#79092=CARTESIAN_POINT('Ctrl Pts',(0.00761349153976328,-0.0346444289841739,
0.0684213240230304));
#79093=CARTESIAN_POINT('Ctrl Pts',(0.00779660324423548,-0.0352450361874068,
0.0684079551607973));
#79094=CARTESIAN_POINT('Ctrl Pts',(0.00758003846946215,-0.0349452760959492,
0.06842029491734));
#79095=CARTESIAN_POINT('Ctrl Pts',(0.00736501841337003,-0.0346444289841739,
0.0684489121628801));
#79096=CARTESIAN_POINT('Ctrl Pts',(0.00779410479131576,-0.0352450361874068,
0.0684080430983203));
#79097=CARTESIAN_POINT('Ctrl Pts',(0.00757754333316053,-0.0349452760959492,
0.0684204770855611));
#79098=CARTESIAN_POINT('Ctrl Pts',(0.0073625336821061,-0.0346444289841739,
0.0684491880442786));
#79099=CARTESIAN_POINT('',(0.00776060145150039,-0.0351951634053307,0.0684101174183231));
#79100=CARTESIAN_POINT('',(0.00752505549724609,-0.0348678972935789,0.0684298906178893));
#79101=CARTESIAN_POINT('Origin',(0.00968827090518434,-0.0345636767883711,
0.0850440762627313));
#79102=CARTESIAN_POINT('Origin',(0.0063747315425424,-0.0346946199326766,
0.0574400884190866));
#79103=CARTESIAN_POINT('',(0.00764951777273953,-0.0346945769330288,0.0684182290470105));
#79104=CARTESIAN_POINT('',(0.0075873573485229,-0.0346945769458128,0.0684247354091863));
#79105=CARTESIAN_POINT('',(0.00788540558804949,-0.0350221583435275,0.0684035835867768));
#79106=CARTESIAN_POINT('Origin',(0.00921621127826716,-0.0345628458713778,
0.0851351976181047));
#79107=CARTESIAN_POINT('',(0.00788545987515186,-0.035195136029876,0.0684048192832028));
#79108=CARTESIAN_POINT('Origin',(0.00742875437489389,-0.0351951838366844,
0.0573953113939836));
#79109=CARTESIAN_POINT('',(0.00776056930729773,-0.035195137132875,0.0684101218304813));
#79110=CARTESIAN_POINT('Ctrl Pts',(0.00811026844799484,-0.0350241211494342,
0.06815001521846));
#79111=CARTESIAN_POINT('Ctrl Pts',(0.00802762111771867,-0.0349144232818961,
0.068150201364758));
#79112=CARTESIAN_POINT('Ctrl Pts',(0.00794492816680862,-0.0348045283579411,
0.0681520960018471));
#79113=CARTESIAN_POINT('Ctrl Pts',(0.00786229560473368,-0.0346945769439157,
0.0681557006444357));
#79114=CARTESIAN_POINT('Ctrl Pts',(0.00803533929009677,-0.0350241211494342,
0.0682350255890013));
#79115=CARTESIAN_POINT('Ctrl Pts',(0.0079538629428192,-0.0349144232818961,
0.0682362438537273));
#79116=CARTESIAN_POINT('Ctrl Pts',(0.00787236301042293,-0.0348045283579411,
0.0682391470219615));
#79117=CARTESIAN_POINT('Ctrl Pts',(0.00779094402234273,-0.0346945769439157,
0.068243735259748));
#79118=CARTESIAN_POINT('Ctrl Pts',(0.00796041013219871,-0.0350241211494342,
0.0683200359595427));
#79119=CARTESIAN_POINT('Ctrl Pts',(0.00788010476791974,-0.0349144232818961,
0.0683222863426966));
#79120=CARTESIAN_POINT('Ctrl Pts',(0.00779979785403725,-0.0348045283579411,
0.068326198042076));
#79121=CARTESIAN_POINT('Ctrl Pts',(0.00771959243995177,-0.0346945769439157,
0.0683317698750604));
#79122=CARTESIAN_POINT('Ctrl Pts',(0.00788548097430065,-0.0350241211494342,
0.0684050463300841));
#79123=CARTESIAN_POINT('Ctrl Pts',(0.00780634659302027,-0.0349144232818961,
0.0684083288316659));
#79124=CARTESIAN_POINT('Ctrl Pts',(0.00772723269765157,-0.0348045283579411,
0.0684132490621905));
#79125=CARTESIAN_POINT('Ctrl Pts',(0.00764824085756082,-0.0346945769439157,
0.0684198044903728));
#79126=CARTESIAN_POINT('',(0.00775590669457766,-0.0346945769458128,0.0682869648453788));
#79127=CARTESIAN_POINT('Ctrl Pts',(0.00787510014337482,-0.0347116136492813,
0.0681551557836804));
#79128=CARTESIAN_POINT('Ctrl Pts',(0.0078768799245296,-0.0347621546532016,
0.0681980600092714));
#79129=CARTESIAN_POINT('Ctrl Pts',(0.00787862841232228,-0.0348133084096431,
0.0682402098626383));
#79130=CARTESIAN_POINT('Ctrl Pts',(0.00788206426041952,-0.0349168561544575,
0.0683230360019436));
#79131=CARTESIAN_POINT('Ctrl Pts',(0.00788375025789453,-0.0349692089015915,
0.0683636794348842));
#79132=CARTESIAN_POINT('Ctrl Pts',(0.00788540558803104,-0.0350221583435,
0.0684035835868141));
#79133=CARTESIAN_POINT('Ctrl Pts',(0.00776164580514364,-0.0351951371254927,
0.0684111125737866));
#79134=CARTESIAN_POINT('Ctrl Pts',(0.00764299790862322,-0.0350307338985342,
0.0684185995163758));
#79135=CARTESIAN_POINT('Ctrl Pts',(0.00752476083944801,-0.0348659306906632,
0.0684309839069909));
#79136=CARTESIAN_POINT('Ctrl Pts',(0.00776056930730941,-0.0351951371254927,
0.068410121830597));
#79137=CARTESIAN_POINT('Ctrl Pts',(0.00764190092779522,-0.0350307338985342,
0.0684176310291034));
#79138=CARTESIAN_POINT('Ctrl Pts',(0.0075236443129899,-0.0348659306906632,
0.0684300385032024));
#79139=CARTESIAN_POINT('Ctrl Pts',(0.00758014714814886,-0.0351951371254927,
0.0682440722392592));
#79140=CARTESIAN_POINT('Ctrl Pts',(0.00745804579752596,-0.0350307338985342,
0.0682553115526956));
#79141=CARTESIAN_POINT('Ctrl Pts',(0.00733651331474012,-0.0348659306906632,
0.0682715878427632));
#79142=CARTESIAN_POINT('Origin',(0.00697142147160639,-0.0308609188509344,
0.0631406035306795));
#79143=CARTESIAN_POINT('',(0.00768190931389185,-0.0351951371254927,0.068337727952692));
#79144=CARTESIAN_POINT('Origin',(0.00836523134608927,-0.0351840467441094,
0.0750968093562229));
#79145=CARTESIAN_POINT('Origin',(0.00609052858765088,-0.0352322613840174,
0.062358635348931));
#79146=CARTESIAN_POINT('',(0.00729024535054908,-0.0351951142564659,0.0684593909890488));
#79147=CARTESIAN_POINT('',(0.00716729424068905,-0.0351951372916786,0.0684801119237786));
#79148=CARTESIAN_POINT('Origin',(0.0078674724186718,-0.0352875123591893,
0.0743743206838547));
#79149=CARTESIAN_POINT('Origin',(0.0156243487284059,-0.0298325076521828,
0.0743415513817782));
#79150=CARTESIAN_POINT('Origin',(0.00994290486824038,-0.0338733259208977,
0.0659684674412729));
#79151=CARTESIAN_POINT('Ctrl Pts',(0.0107946224263853,-0.0321934096636941,
0.0690564012531785));
#79152=CARTESIAN_POINT('Ctrl Pts',(0.01070344943444,-0.0320508460844559,
0.0690085944848839));
#79153=CARTESIAN_POINT('Ctrl Pts',(0.0106110607136982,-0.0319086045663538,
0.0689632734014443));
#79154=CARTESIAN_POINT('Ctrl Pts',(0.0105176632270694,-0.0317669892868597,
0.0689205192100429));
#79155=CARTESIAN_POINT('Ctrl Pts',(0.0107195350790821,-0.0321934096636941,
0.069019087409866));
#79156=CARTESIAN_POINT('Ctrl Pts',(0.0106276941871107,-0.0320508460844559,
0.0689726246693307));
#79157=CARTESIAN_POINT('Ctrl Pts',(0.0105346741813155,-0.0319086045663538,
0.068928664545405));
#79158=CARTESIAN_POINT('Ctrl Pts',(0.0104406831426264,-0.0317669892868597,
0.0688872852029833));
#79159=CARTESIAN_POINT('Ctrl Pts',(0.0106444477317788,-0.0321934096636941,
0.0689817735665535));
#79160=CARTESIAN_POINT('Ctrl Pts',(0.0105519389397814,-0.0320508460844559,
0.0689366548537775));
#79161=CARTESIAN_POINT('Ctrl Pts',(0.0104582876489329,-0.0319086045663538,
0.0688940556893655));
#79162=CARTESIAN_POINT('Ctrl Pts',(0.0103637030581834,-0.0317669892868597,
0.0688540511959236));
#79163=CARTESIAN_POINT('Ctrl Pts',(0.0105693603844755,-0.0321934096636941,
0.0689444597232408));
#79164=CARTESIAN_POINT('Ctrl Pts',(0.010476183692452,-0.0320508460844559,
0.0689006850382243));
#79165=CARTESIAN_POINT('Ctrl Pts',(0.0103819011165501,-0.0319086045663538,
0.0688594468333262));
#79166=CARTESIAN_POINT('Ctrl Pts',(0.0102867229737405,-0.0317669892868597,
0.0688208171888639));
#79167=CARTESIAN_POINT('',(0.0105707037119558,-0.0321934096636941,0.0689451272752735));
#79168=CARTESIAN_POINT('',(0.010354797701258,-0.0318665617511289,0.0688489911534236));
#79169=CARTESIAN_POINT('Origin',(0.00290980286696623,-0.0326371944420151,
0.0837953293979655));
#79170=CARTESIAN_POINT('Origin',(0.0146067627215476,-0.0316939261508845,
0.0587461012863982));
#79171=CARTESIAN_POINT('',(0.0106829910913967,-0.0320197221621863,0.0689994622628841));
#79172=CARTESIAN_POINT('Ctrl Pts',(0.0106828519156328,-0.0320197392094772,
0.0689993404228847));
#79173=CARTESIAN_POINT('Ctrl Pts',(0.010656643682924,-0.031979271657607,
0.0689863190954539));
#79174=CARTESIAN_POINT('Ctrl Pts',(0.0106302168710053,-0.0319386439829744,
0.0689734382910022));
#79175=CARTESIAN_POINT('Ctrl Pts',(0.0106035400311454,-0.0318979099381675,
0.0689606920896429));
#79176=CARTESIAN_POINT('Ctrl Pts',(0.0105768637185712,-0.0318571766984964,
0.0689479461402207));
#79177=CARTESIAN_POINT('Ctrl Pts',(0.0105500737424975,-0.0318163871833599,
0.0689353979642012));
#79178=CARTESIAN_POINT('Ctrl Pts',(0.0105232637429612,-0.0317755399638303,
0.0689230875334388));
#79179=CARTESIAN_POINT('',(0.0106826438271765,-0.0321934096636183,0.0690007547021243));
#79180=CARTESIAN_POINT('Origin',(0.0116881152669688,-0.0324103521494481,
0.0669303005759181));
#79181=CARTESIAN_POINT('',(0.0106266737695762,-0.0321934096636662,0.0689729409887089));
#79182=CARTESIAN_POINT('Ctrl Pts',(0.0105713498077764,-0.0321934096636618,
0.0689470498380344));
#79183=CARTESIAN_POINT('Ctrl Pts',(0.0104995970701007,-0.0320835708272592,
0.0689132959731054));
#79184=CARTESIAN_POINT('Ctrl Pts',(0.0104271874174485,-0.0319739230346488,
0.0688810466059669));
#79185=CARTESIAN_POINT('Ctrl Pts',(0.0103542166595999,-0.0318646057455573,
0.0688503358873456));
#79186=CARTESIAN_POINT('Ctrl Pts',(0.0105352517812921,-0.0321934096636618,
0.0688396343026195));
#79187=CARTESIAN_POINT('Ctrl Pts',(0.0104620176996683,-0.0320835708272592,
0.0688063782576089));
#79188=CARTESIAN_POINT('Ctrl Pts',(0.0103881378646649,-0.0319739230346488,
0.068774657077969));
#79189=CARTESIAN_POINT('Ctrl Pts',(0.0103137099151944,-0.0318646057455573,
0.068744504094286));
#79190=CARTESIAN_POINT('Ctrl Pts',(0.0104991537548079,-0.0321934096636618,
0.0687322187672045));
#79191=CARTESIAN_POINT('Ctrl Pts',(0.0104244383292359,-0.0320835708272592,
0.0686994605421124));
#79192=CARTESIAN_POINT('Ctrl Pts',(0.0103490883118814,-0.0319739230346488,
0.0686682675499711));
#79193=CARTESIAN_POINT('Ctrl Pts',(0.0102732031707889,-0.0318646057455573,
0.0686386723012265));
#79194=CARTESIAN_POINT('Ctrl Pts',(0.0104630557283236,-0.0321934096636618,
0.0686248032317896));
#79195=CARTESIAN_POINT('Ctrl Pts',(0.0103868589588035,-0.0320835708272592,
0.0685925428266158));
#79196=CARTESIAN_POINT('Ctrl Pts',(0.0103100387590979,-0.0319739230346488,
0.0685618780219732));
#79197=CARTESIAN_POINT('Ctrl Pts',(0.0102326964263834,-0.0318646057455573,
0.0685328405081669));
#79198=CARTESIAN_POINT('',(0.0104512484717458,-0.0321763980308269,0.0686198191078848));
#79199=CARTESIAN_POINT('',(0.0104630557282936,-0.0321934096636184,0.0686248032317769));
#79200=CARTESIAN_POINT('Origin',(0.00347116593862575,-0.0326386230878191,
0.083623303336139));
#79201=CARTESIAN_POINT('Ctrl Pts',(0.0104512484705094,-0.0321763980306278,
0.0686198191108053));
#79202=CARTESIAN_POINT('Ctrl Pts',(0.0104345997576559,-0.0321259596174827,
0.0686593773181772));
#79203=CARTESIAN_POINT('Ctrl Pts',(0.010418239505362,-0.0320749164631402,
0.0686982501282784));
#79204=CARTESIAN_POINT('Ctrl Pts',(0.0103860827556678,-0.0319716057793924,
0.0687746562375072));
#79205=CARTESIAN_POINT('Ctrl Pts',(0.010370298787618,-0.031919378669013,
0.0688121597662465));
#79206=CARTESIAN_POINT('Ctrl Pts',(0.0103547977005306,-0.0318665617525313,
0.0688489911551285));
#79207=CARTESIAN_POINT('',(0.0105168797201347,-0.0321934096636663,0.0687849652535352));
#79208=CARTESIAN_POINT('Origin',(0.00812378219310841,-0.0315241814719618,
0.07415));
#79209=CARTESIAN_POINT('',(0.0104512484718894,-0.0322104233323627,0.068619819107543));
#79210=CARTESIAN_POINT('',(0.0104394305973831,-0.0321934096636183,0.0686148602124426));
#79211=CARTESIAN_POINT('Origin',(0.00351009208260348,-0.0326387237493397,
0.0836465390198752));
#79212=CARTESIAN_POINT('Origin',(0.00460209302538108,-0.0326386240213093,
0.0840992745560143));
#79213=CARTESIAN_POINT('Origin',(0.00455826793499113,-0.0326387245235589,
0.0840876784787476));
#79214=CARTESIAN_POINT('Ctrl Pts',(0.0105024377931778,-0.0327445246967096,
0.0689135773149736));
#79215=CARTESIAN_POINT('Ctrl Pts',(0.0103049428830077,-0.032443687833936,
0.068823864852417));
#79216=CARTESIAN_POINT('Ctrl Pts',(0.01010125152568,-0.0321434074405927,
0.0687492833772971));
#79217=CARTESIAN_POINT('Ctrl Pts',(0.0102726275908998,-0.0327445246967096,
0.0688151533802376));
#79218=CARTESIAN_POINT('Ctrl Pts',(0.0100714205613462,-0.032443687833936,
0.0687341083511532));
#79219=CARTESIAN_POINT('Ctrl Pts',(0.00986468049688743,-0.0321434074405927,
0.0686684492982461));
#79220=CARTESIAN_POINT('',(0.0102390586088646,-0.0326943950436612,0.0688017544292594));
#79221=CARTESIAN_POINT('',(0.0100175422025775,-0.0323666188837389,0.0687193648597483));
#79222=CARTESIAN_POINT('Origin',(0.0041269508842937,-0.0326395579111481,
0.0844622204949339));
#79223=CARTESIAN_POINT('Origin',(0.0136542190453974,-0.0321933825603012,
0.0582906567238054));
#79224=CARTESIAN_POINT('',(0.0101351242805322,-0.0321934096532688,0.0687618066103723));
#79225=CARTESIAN_POINT('',(0.0100761095784306,-0.0321934096584275,0.0687412271234611));
#79226=CARTESIAN_POINT('',(0.0103547977016218,-0.0325210109756239,0.0688489911525471));
#79227=CARTESIAN_POINT('Origin',(0.00368979084779726,-0.0326393129157865,
0.0842620317531794));
#79228=CARTESIAN_POINT('',(0.0103542707108206,-0.0326943950436593,0.0688502433100797));
#79229=CARTESIAN_POINT('Origin',(0.0146455201351887,-0.0326943765538048,
0.0586540138571446));
#79230=CARTESIAN_POINT('',(0.0102966646598526,-0.0326943950436702,0.0688259988696796));
#79231=CARTESIAN_POINT('Ctrl Pts',(0.0106662248648126,-0.0325229783203769,
0.0687152980522278));
#79232=CARTESIAN_POINT('Ctrl Pts',(0.0105913076173117,-0.032413025309245,
0.068680250535598));
#79233=CARTESIAN_POINT('Ctrl Pts',(0.010515676729576,-0.0323031222208069,
0.0686467580941132));
#79234=CARTESIAN_POINT('Ctrl Pts',(0.0104394305932463,-0.0321934096576658,
0.068614860210712));
#79235=CARTESIAN_POINT('Ctrl Pts',(0.0105622312703106,-0.0325229783203769,
0.068760314433011));
#79236=CARTESIAN_POINT('Ctrl Pts',(0.0104879345726343,-0.032413025309245,
0.0687267004658072));
#79237=CARTESIAN_POINT('Ctrl Pts',(0.0104129537954161,-0.0323031222208069,
0.0686946285194523));
#79238=CARTESIAN_POINT('Ctrl Pts',(0.0103373864333454,-0.0321934096576658,
0.0686641362867163));
#79239=CARTESIAN_POINT('Ctrl Pts',(0.0104582376758086,-0.0325229783203769,
0.0688053308137942));
#79240=CARTESIAN_POINT('Ctrl Pts',(0.010384561527957,-0.032413025309245,
0.0687731503960163));
#79241=CARTESIAN_POINT('Ctrl Pts',(0.0103102308612563,-0.0323031222208069,
0.0687424989447914));
#79242=CARTESIAN_POINT('Ctrl Pts',(0.0102353422734446,-0.0321934096576658,
0.0687134123627207));
#79243=CARTESIAN_POINT('Ctrl Pts',(0.0103542440813066,-0.0325229783203769,
0.0688503471945773));
#79244=CARTESIAN_POINT('Ctrl Pts',(0.0102811884832796,-0.032413025309245,
0.0688196003262255));
#79245=CARTESIAN_POINT('Ctrl Pts',(0.0102075079270964,-0.0323031222208069,
0.0687903693701304));
#79246=CARTESIAN_POINT('Ctrl Pts',(0.0101332981135437,-0.0321934096576658,
0.0687626884387251));
#79247=CARTESIAN_POINT('',(0.0102872774394729,-0.0321934096584275,0.0686883334114516));
#79248=CARTESIAN_POINT('Ctrl Pts',(0.0104512484705346,-0.0322104233328949,
0.0686198191107456));
#79249=CARTESIAN_POINT('Ctrl Pts',(0.0104345771984191,-0.0322609421830998,
0.0686594309200968));
#79250=CARTESIAN_POINT('Ctrl Pts',(0.0104182059255511,-0.0323120888239943,
0.0686983299156378));
#79251=CARTESIAN_POINT('Ctrl Pts',(0.0103860489323641,-0.0324156524631822,
0.0687747366034181));
#79252=CARTESIAN_POINT('Ctrl Pts',(0.0103702764302917,-0.0324680267167324,
0.0688122128884162));
#79253=CARTESIAN_POINT('Ctrl Pts',(0.0103547977016009,-0.0325210109755913,
0.0688489911525853));
#79254=CARTESIAN_POINT('Origin',(0.0149552170010535,-0.026283458251215,
0.078053188991479));
#79255=CARTESIAN_POINT('Origin',(0.0173551804691235,-0.0342770991216957,
0.0662375992804839));
#79256=CARTESIAN_POINT('Ctrl Pts',(0.0102398239626242,-0.0326943950436604,
0.0688036321737721));
#79257=CARTESIAN_POINT('Ctrl Pts',(0.0101661409938175,-0.0325844576448134,
0.0687744691523033));
#79258=CARTESIAN_POINT('Ctrl Pts',(0.0100918496712552,-0.0324744968375322,
0.0687468279515219));
#79259=CARTESIAN_POINT('Ctrl Pts',(0.0100170456697988,-0.0323646534831894,
0.0687207426740401));
#79260=CARTESIAN_POINT('Ctrl Pts',(0.0101970525519996,-0.0326943950436604,
0.0686986953641456));
#79261=CARTESIAN_POINT('Ctrl Pts',(0.0101219233572837,-0.0325844576448134,
0.0686701218128773));
#79262=CARTESIAN_POINT('Ctrl Pts',(0.0100461978976708,-0.0324744968375322,
0.0686431000343372));
#79263=CARTESIAN_POINT('Ctrl Pts',(0.00996997367457563,-0.0323646534831894,
0.0686176633121527));
#79264=CARTESIAN_POINT('Ctrl Pts',(0.010154281141375,-0.0326943950436604,
0.0685937585545191));
#79265=CARTESIAN_POINT('Ctrl Pts',(0.0100777057207499,-0.0325844576448134,
0.0685657744734514));
#79266=CARTESIAN_POINT('Ctrl Pts',(0.0100005461240864,-0.0324744968375322,
0.0685393721171524));
#79267=CARTESIAN_POINT('Ctrl Pts',(0.00992290167935243,-0.0323646534831894,
0.0685145839502653));
#79268=CARTESIAN_POINT('Ctrl Pts',(0.0101115097307504,-0.0326943950436604,
0.0684888217448926));
#79269=CARTESIAN_POINT('Ctrl Pts',(0.0100334880842161,-0.0325844576448134,
0.0684614271340255));
#79270=CARTESIAN_POINT('Ctrl Pts',(0.00995489435050194,-0.0324744968375322,
0.0684356441999677));
#79271=CARTESIAN_POINT('Ctrl Pts',(0.00987582968412923,-0.0323646534831894,
0.0684115045883779));
#79272=CARTESIAN_POINT('',(0.0100994128174638,-0.0326773559991341,0.068484588839611));
#79273=CARTESIAN_POINT('',(0.0101115097307497,-0.0326943950436594,0.0684888217448924));
#79274=CARTESIAN_POINT('Origin',(0.0046792468833737,-0.0326395670827019,
0.084180292496662));
#79275=CARTESIAN_POINT('Ctrl Pts',(0.0100994128163548,-0.032677355998742,
0.0684845888427716));
#79276=CARTESIAN_POINT('Ctrl Pts',(0.0100852694638655,-0.0326267922585946,
0.0685251469845875));
#79277=CARTESIAN_POINT('Ctrl Pts',(0.0100713767920861,-0.0325756109579296,
0.0685649862626271));
#79278=CARTESIAN_POINT('Ctrl Pts',(0.0100440809865966,-0.0324719985462368,
0.068643260996348));
#79279=CARTESIAN_POINT('Ctrl Pts',(0.0100306888004874,-0.0324196091621778,
0.0686816650581751));
#79280=CARTESIAN_POINT('Ctrl Pts',(0.0100175422025614,-0.0323666188837757,
0.0687193648597944));
#79281=CARTESIAN_POINT('',(0.0101752841698171,-0.0326943950436702,0.0686452880870859));
#79282=CARTESIAN_POINT('Origin',(0.00812378219310841,-0.0315241814719618,
0.07415));
#79283=CARTESIAN_POINT('',(0.0100994128174488,-0.0327114338379886,0.0684845888396533));
#79284=CARTESIAN_POINT('',(0.0100873068912882,-0.0326943950436593,0.0684803817800796));
#79285=CARTESIAN_POINT('Origin',(0.00472227965081183,-0.0326395672612986,
0.0841944774514547));
#79286=CARTESIAN_POINT('Origin',(0.00458436906086605,-0.0326395676967327,
0.0841472085234683));
#79287=CARTESIAN_POINT('Origin',(0.00454184827979971,-0.0326395680217033,
0.0841315559643501));
#79288=CARTESIAN_POINT('Ctrl Pts',(0.0101689096987611,-0.0332451089994433,
0.0687745392303894));
#79289=CARTESIAN_POINT('Ctrl Pts',(0.00996617087885437,-0.0329451141710254,
0.0686974059845477));
#79290=CARTESIAN_POINT('Ctrl Pts',(0.00975819802713791,-0.0326442513127493,
0.0686357629828349));
#79291=CARTESIAN_POINT('Ctrl Pts',(0.00993337231292476,-0.0332451089994433,
0.0686907410211401));
#79292=CARTESIAN_POINT('Ctrl Pts',(0.00972747299184772,-0.0329451141710254,
0.0686224912131459));
#79293=CARTESIAN_POINT('Ctrl Pts',(0.00951701775446562,-0.0326442513127493,
0.0685699444742397));
#79294=CARTESIAN_POINT('Ctrl Pts',(0.0099310169390664,-0.0332451089994433,
0.0686899030390476));
#79295=CARTESIAN_POINT('Ctrl Pts',(0.00972508601297765,-0.0329451141710254,
0.0686217420654319));
#79296=CARTESIAN_POINT('Ctrl Pts',(0.0095146059517389,-0.0326442513127493,
0.0685692862891537));
#79297=CARTESIAN_POINT('',(0.00989906547608922,-0.0331951640388616,0.0686794886651091));
#79298=CARTESIAN_POINT('',(0.0096728128861654,-0.0328677532355001,0.068611170793228));
#79299=CARTESIAN_POINT('Origin',(0.00546039648536102,-0.0326402808281567,
0.0848452074883621));
#79300=CARTESIAN_POINT('Origin',(0.0126501866039726,-0.0326944278779143,
0.0579636533031569));
#79301=CARTESIAN_POINT('',(0.00979282788793583,-0.0326943950436593,0.0686461457624153));
#79302=CARTESIAN_POINT('',(0.00973263744377394,-0.0326943950436694,0.0686293124493114));
#79303=CARTESIAN_POINT('',(0.0100175422025802,-0.0330220786163545,0.0687193648597492));
#79304=CARTESIAN_POINT('Origin',(0.00498990723212481,-0.0326396682762087,
0.0847462503893336));
#79305=CARTESIAN_POINT('',(0.0100170948752985,-0.0331951640388587,0.0687206476364617));
#79306=CARTESIAN_POINT('Origin',(0.0136495077187538,-0.0331952026560047,
0.0583041728748783));
#79307=CARTESIAN_POINT('',(0.00995808017570384,-0.0331951640388701,0.0687000681507954));
#79308=CARTESIAN_POINT('Ctrl Pts',(0.010319959281971,-0.0330240426238172,
0.0685663805471387));
#79309=CARTESIAN_POINT('Ctrl Pts',(0.0102430394841509,-0.0329142774063519,
0.068536126068108));
#79310=CARTESIAN_POINT('Ctrl Pts',(0.0101654558944131,-0.032804347972669,
0.0685074466532019));
#79311=CARTESIAN_POINT('Ctrl Pts',(0.0100873068912882,-0.0326943950436593,
0.0684803817800796));
#79312=CARTESIAN_POINT('Ctrl Pts',(0.0102189975298273,-0.0330240426238172,
0.0686178379138465));
#79313=CARTESIAN_POINT('Ctrl Pts',(0.0101427866073661,-0.0329142774063519,
0.0685889742813138));
#79314=CARTESIAN_POINT('Ctrl Pts',(0.0100659409990697,-0.032804347972669,
0.0685616717518596));
#79315=CARTESIAN_POINT('Ctrl Pts',(0.00998855818663668,-0.0326943950436593,
0.068535968013214));
#79316=CARTESIAN_POINT('Ctrl Pts',(0.0101180357776836,-0.0330240426238172,
0.0686692952805543));
#79317=CARTESIAN_POINT('Ctrl Pts',(0.0100425337305813,-0.0329142774063519,
0.0686418224945197));
#79318=CARTESIAN_POINT('Ctrl Pts',(0.00996642610372621,-0.032804347972669,
0.0686158968505174));
#79319=CARTESIAN_POINT('Ctrl Pts',(0.00988980948198516,-0.0326943950436593,
0.0685915542463484));
#79320=CARTESIAN_POINT('Ctrl Pts',(0.0100170740255399,-0.0330240426238172,
0.0687207526472621));
#79321=CARTESIAN_POINT('Ctrl Pts',(0.00994228085379651,-0.0329142774063519,
0.0686946707077255));
#79322=CARTESIAN_POINT('Ctrl Pts',(0.00986691120838275,-0.032804347972669,
0.0686701219491752));
#79323=CARTESIAN_POINT('Ctrl Pts',(0.00979106077733364,-0.0326943950436593,
0.0686471404794828));
#79324=CARTESIAN_POINT('',(0.00994006738962203,-0.0326943950436693,0.0685632637712575));
#79325=CARTESIAN_POINT('Ctrl Pts',(0.010099412816352,-0.0327114338383347,
0.06848458884278));
#79326=CARTESIAN_POINT('Ctrl Pts',(0.0100852718163742,-0.032761987683071,
0.0685251402384234));
#79327=CARTESIAN_POINT('Ctrl Pts',(0.0100713802936745,-0.0328131562603779,
0.0685649762213077));
#79328=CARTESIAN_POINT('Ctrl Pts',(0.0100440845132367,-0.0329167375858778,
0.0686432508831895));
#79329=CARTESIAN_POINT('Ctrl Pts',(0.0100306911315659,-0.0329691088920621,
0.0686816583734653));
#79330=CARTESIAN_POINT('Ctrl Pts',(0.0100175422025619,-0.0330220786163186,
0.0687193648597932));
#79331=CARTESIAN_POINT('Ctrl Pts',(0.00989994736492207,-0.0331951640388604,
0.0686813149388771));
#79332=CARTESIAN_POINT('Ctrl Pts',(0.00978688580747801,-0.033030642201062,
0.0686445938627211));
#79333=CARTESIAN_POINT('Ctrl Pts',(0.00967240313964828,-0.0328657861914645,
0.0686125771175346));
#79334=CARTESIAN_POINT('Ctrl Pts',(0.00989906547609221,-0.0331951640388604,
0.0686794886651103));
#79335=CARTESIAN_POINT('Ctrl Pts',(0.00978596616160892,-0.033030642201062,
0.0686427858214403));
#79336=CARTESIAN_POINT('Ctrl Pts',(0.00967144652257091,-0.0328657861914645,
0.0686107888536987));
#79337=CARTESIAN_POINT('Ctrl Pts',(0.00975211908072219,-0.0331951640388604,
0.0683751823422348));
#79338=CARTESIAN_POINT('Ctrl Pts',(0.0096327284281165,-0.0330306422010619,
0.0683415175210759));
#79339=CARTESIAN_POINT('Ctrl Pts',(0.00951204839152569,-0.0328657861914645,
0.0683128160074971));
#79340=CARTESIAN_POINT('',(0.00973978025258226,-0.0331781648281902,0.0683717173600123));
#79341=CARTESIAN_POINT('',(0.00975211908072106,-0.0331951640388588,0.0683751823422345));
#79342=CARTESIAN_POINT('Origin',(0.00597986164658149,-0.0326412092584411,
0.0844605176198909));
#79343=CARTESIAN_POINT('Ctrl Pts',(0.00973978025373896,-0.033178164828644,
0.0683717173614345));
#79344=CARTESIAN_POINT('Ctrl Pts',(0.00972820352374881,-0.0331276811546772,
0.068413112021642));
#79345=CARTESIAN_POINT('Ctrl Pts',(0.00971683586621816,-0.0330765663497772,
0.0684537592315872));
#79346=CARTESIAN_POINT('Ctrl Pts',(0.00969450877310779,-0.0329730614463314,
0.0685335936303563));
#79347=CARTESIAN_POINT('Ctrl Pts',(0.00968355835202192,-0.0329207133373986,
0.0685727485663901));
#79348=CARTESIAN_POINT('Ctrl Pts',(0.0096728129019712,-0.0328677532289359,
0.0686111707886005));
#79349=CARTESIAN_POINT('',(0.00982559227841514,-0.0331951640388701,0.0685273355036818));
#79350=CARTESIAN_POINT('Origin',(0.00812378219310841,-0.0315241814719618,
0.07415));
#79351=CARTESIAN_POINT('',(0.00973978025154155,-0.0332121607144241,0.0683717173613322));
#79352=CARTESIAN_POINT('',(0.0097274340502593,-0.0331951640388587,0.0683682787406282));
#79353=CARTESIAN_POINT('Origin',(0.00602498555138481,-0.0326413655988795,
0.0844649937999266));
#79354=CARTESIAN_POINT('Origin',(0.00460796994952319,-0.032641209838483,
0.0840768460134683));
#79355=CARTESIAN_POINT('Origin',(0.00456707180094442,-0.0326413663911616,
0.0840572609498495));
#79356=CARTESIAN_POINT('Ctrl Pts',(0.00982736602910231,-0.0337436976235975,
0.0686567380261141));
#79357=CARTESIAN_POINT('Ctrl Pts',(0.00977795879838256,-0.0336723290703325,
0.068641415734908));
#79358=CARTESIAN_POINT('Ctrl Pts',(0.00972828396086462,-0.033601104548885,
0.0686269846028399));
#79359=CARTESIAN_POINT('Ctrl Pts',(0.00956968204470073,-0.0333736987606857,
0.0685809088567926));
#79360=CARTESIAN_POINT('Ctrl Pts',(0.00940869739996884,-0.0331450831799192,
0.0685440105323699));
#79361=CARTESIAN_POINT('Ctrl Pts',(0.009587031938753,-0.0337436976235975,
0.0685878938178176));
#79362=CARTESIAN_POINT('Ctrl Pts',(0.0095370055127902,-0.0336723290703325,
0.0685747331278437));
#79363=CARTESIAN_POINT('Ctrl Pts',(0.00948675046059336,-0.033601104548885,
0.0685624743846825));
#79364=CARTESIAN_POINT('Ctrl Pts',(0.00932629603389381,-0.0333736987606857,
0.0685233346460888));
#79365=CARTESIAN_POINT('Ctrl Pts',(0.0091638599595174,-0.0331450831799192,
0.0684934672068642));
#79366=CARTESIAN_POINT('Ctrl Pts',(0.0095846285978495,-0.0337436976235975,
0.0685872053757347));
#79367=CARTESIAN_POINT('Ctrl Pts',(0.00953459597993428,-0.0336723290703325,
0.0685740663017731));
#79368=CARTESIAN_POINT('Ctrl Pts',(0.00948433512559065,-0.033601104548885,
0.0685618292825009));
#79369=CARTESIAN_POINT('Ctrl Pts',(0.00932386217378574,-0.0333736987606857,
0.0685227589039818));
#79370=CARTESIAN_POINT('Ctrl Pts',(0.00916141158511288,-0.0331450831799192,
0.068492961773609));
#79371=CARTESIAN_POINT('',(0.00955206611123276,-0.0336938721132548,0.0685788125099555));
#79372=CARTESIAN_POINT('',(0.00932197026244842,-0.0333679870047996,0.0685248359712446));
#79373=CARTESIAN_POINT('Ctrl Pts',(0.00955206611125787,-0.0336938721132548,
0.0685788125099619));
#79374=CARTESIAN_POINT('Ctrl Pts',(0.00953031915298532,-0.0336629187933894,
0.0685732372478075));
#79375=CARTESIAN_POINT('Ctrl Pts',(0.00950854650451064,-0.0336319952301032,
0.0685677911059402));
#79376=CARTESIAN_POINT('Ctrl Pts',(0.00948675046060606,-0.0336011045488942,
0.0685624743846858));
#79377=CARTESIAN_POINT('Ctrl Pts',(0.009432056728263,-0.0335235892595445,
0.0685491329117786));
#79378=CARTESIAN_POINT('Ctrl Pts',(0.00937711846022698,-0.0334458668665561,
0.0685365828131935));
#79379=CARTESIAN_POINT('Ctrl Pts',(0.00932197027405363,-0.0333679869962484,
0.068524835973455));
#79380=CARTESIAN_POINT('Ctrl Pts',(0.00932192691853327,-0.0333679692468933,
0.0685248260356988));
#79381=CARTESIAN_POINT('Ctrl Pts',(0.00932183829732831,-0.0333391895415735,
0.0685252705399856));
#79382=CARTESIAN_POINT('Ctrl Pts',(0.0093217750559261,-0.0333104081132863,
0.0685256043525627));
#79383=CARTESIAN_POINT('Ctrl Pts',(0.00932169678684232,-0.033253269890485,
0.0685260472410793));
#79384=CARTESIAN_POINT('Ctrl Pts',(0.00932168105404384,-0.033224917447262,
0.0685261595976384));
#79385=CARTESIAN_POINT('Ctrl Pts',(0.0093216870395485,-0.0331960985234834,
0.0685261646253599));
#79386=CARTESIAN_POINT('Ctrl Pts',(0.00932168714260407,-0.0331956312691392,
0.0685261646777334));
#79387=CARTESIAN_POINT('Ctrl Pts',(0.00932168725141207,-0.033195164038861,
0.06852616470091));
#79388=CARTESIAN_POINT('',(0.00944394454052274,-0.0331951640388587,0.0685522061152209));
#79389=CARTESIAN_POINT('',(0.00938281589597739,-0.0331951640388687,0.0685391854080754));
#79390=CARTESIAN_POINT('',(0.00967281289801524,-0.0335216366567727,0.0686111708032634));
#79391=CARTESIAN_POINT('Origin',(0.00636530768705754,-0.0326434571528351,
0.0849338873136656));
#79392=CARTESIAN_POINT('',(0.00967244699959201,-0.0336938721132327,0.0686124791361874));
#79393=CARTESIAN_POINT('Origin',(0.012613717613471,-0.0336938867896221,
0.0580954568811573));
#79394=CARTESIAN_POINT('',(0.00961225655542239,-0.0336938721132538,0.0685956458230815));
#79395=CARTESIAN_POINT('Ctrl Pts',(0.00996502634716105,-0.0335235895815172,
0.0684394991493578));
#79396=CARTESIAN_POINT('Ctrl Pts',(0.0098864100600104,-0.0334144449262749,
0.0684141507985011));
#79397=CARTESIAN_POINT('Ctrl Pts',(0.00980717977441849,-0.0333049234473147,
0.0683903974787876));
#79398=CARTESIAN_POINT('Ctrl Pts',(0.00972743405025945,-0.0331951640388587,
0.068368278740628));
#79399=CARTESIAN_POINT('Ctrl Pts',(0.00986749472538496,-0.0335235895815172,
0.0684971945151993));
#79400=CARTESIAN_POINT('Ctrl Pts',(0.00978967272853683,-0.0334144449262749,
0.0684731888791384));
#79401=CARTESIAN_POINT('Ctrl Pts',(0.00971126538526795,-0.0333049234473147,
0.0684507634073975));
#79402=CARTESIAN_POINT('Ctrl Pts',(0.0096323703569659,-0.0331951640388587,
0.0684299558571563));
#79403=CARTESIAN_POINT('Ctrl Pts',(0.00976996310360887,-0.0335235895815172,
0.0685548898810407));
#79404=CARTESIAN_POINT('Ctrl Pts',(0.00969293539706327,-0.0334144449262749,
0.0685322269597758));
#79405=CARTESIAN_POINT('Ctrl Pts',(0.00961535099611742,-0.0333049234473147,
0.0685111293360074));
#79406=CARTESIAN_POINT('Ctrl Pts',(0.00953730666367236,-0.0331951640388587,
0.0684916329736847));
#79407=CARTESIAN_POINT('Ctrl Pts',(0.00967243148183278,-0.0335235895815172,
0.0686125852468822));
#79408=CARTESIAN_POINT('Ctrl Pts',(0.00959619806558971,-0.0334144449262749,
0.0685912650404131));
#79409=CARTESIAN_POINT('Ctrl Pts',(0.00951943660696689,-0.0333049234473147,
0.0685714952646172));
#79410=CARTESIAN_POINT('Ctrl Pts',(0.00944224297037881,-0.0331951640388587,
0.068553310090213));
#79411=CARTESIAN_POINT('',(0.00958568929540102,-0.0331951640388687,0.0684602424279345));
#79412=CARTESIAN_POINT('Ctrl Pts',(0.00973978025069291,-0.0332121607145999,
0.0683717173643448));
#79413=CARTESIAN_POINT('Ctrl Pts',(0.00972822298409216,-0.0332625444109513,
0.0684130423848801));
#79414=CARTESIAN_POINT('Ctrl Pts',(0.00971686486733106,-0.0333135300746303,
0.0684536553104628));
#79415=CARTESIAN_POINT('Ctrl Pts',(0.00969453791753884,-0.0334167203140639,
0.0685334892098206));
#79416=CARTESIAN_POINT('Ctrl Pts',(0.0096835777319374,-0.0334688847587326,
0.0685726792632041));
#79417=CARTESIAN_POINT('Ctrl Pts',(0.00967281289765872,-0.0335216366562399,
0.0686111708038939));
#79418=CARTESIAN_POINT('Ctrl Pts',(0.0095530606999123,-0.0336938721132547,
0.0685805793924302));
#79419=CARTESIAN_POINT('Ctrl Pts',(0.00952046103296096,-0.0336474569765037,
0.0685722133510435));
#79420=CARTESIAN_POINT('Ctrl Pts',(0.00948776566468227,-0.033601104548885,
0.0685642295031653));
#79421=CARTESIAN_POINT('Ctrl Pts',(0.00940498850935112,-0.0334837508592655,
0.068544016235943));
#79422=CARTESIAN_POINT('Ctrl Pts',(0.00932164874262919,-0.0333660264659096,
0.0685262647036357));
#79423=CARTESIAN_POINT('Ctrl Pts',(0.00955206611126368,-0.0336938721132547,
0.0685788125099635));
#79424=CARTESIAN_POINT('Ctrl Pts',(0.00951945610216294,-0.0336474569765037,
0.0685704522902343));
#79425=CARTESIAN_POINT('Ctrl Pts',(0.00948675046059336,-0.033601104548885,
0.0685624743846825));
#79426=CARTESIAN_POINT('Ctrl Pts',(0.00940394729565166,-0.0334837508592655,
0.0685422761620644));
#79427=CARTESIAN_POINT('Ctrl Pts',(0.0093205819765435,-0.0333660264659096,
0.0685245404384735));
#79428=CARTESIAN_POINT('Ctrl Pts',(0.00938530754500726,-0.0336938721132547,
0.0682825666325416));
#79429=CARTESIAN_POINT('Ctrl Pts',(0.00935096351048089,-0.0336474569765037,
0.0682751825060373));
#79430=CARTESIAN_POINT('Ctrl Pts',(0.00931653538870579,-0.033601104548885,
0.0682682009257848));
#79431=CARTESIAN_POINT('Ctrl Pts',(0.00922937129990751,-0.0334837508592655,
0.0682505251697544));
#79432=CARTESIAN_POINT('Ctrl Pts',(0.00914172171785406,-0.0333660264659096,
0.0682354400282854));
#79433=CARTESIAN_POINT('',(0.00937377008003389,-0.0336769361243754,0.0682816501226887));
#79434=CARTESIAN_POINT('',(0.00938630212891338,-0.0336938721132327,0.0682843335066086));
#79435=CARTESIAN_POINT('Ctrl Pts',(0.00937377008003363,-0.0336769361243751,
0.0682816501226887));
#79436=CARTESIAN_POINT('Ctrl Pts',(0.00937585938891902,-0.033679758666967,
0.0682820951559353));
#79437=CARTESIAN_POINT('Ctrl Pts',(0.00937794838111765,-0.0336825812712137,
0.0682825412881353));
#79438=CARTESIAN_POINT('Ctrl Pts',(0.00938212573710684,-0.033688226609505,
0.0682834357509796));
#79439=CARTESIAN_POINT('Ctrl Pts',(0.00938421410081141,-0.033691049343433,
0.0682838840816254));
#79440=CARTESIAN_POINT('Ctrl Pts',(0.00938630212891564,-0.0336938721132299,
0.0682843335066159));
#79441=CARTESIAN_POINT('Ctrl Pts',(0.00937377008003389,-0.0336769361243754,
0.0682816501226887));
#79442=CARTESIAN_POINT('Ctrl Pts',(0.00936503832843738,-0.0336279018525336,
0.0683226432986591));
#79443=CARTESIAN_POINT('Ctrl Pts',(0.00935618095953362,-0.0335767826051515,
0.0683642262133951));
#79444=CARTESIAN_POINT('Ctrl Pts',(0.00933882560463971,-0.0334733172106813,
0.0684457048387705));
#79445=CARTESIAN_POINT('Ctrl Pts',(0.00933031595447219,-0.0334209631477606,
0.0684856553095198));
#79446=CARTESIAN_POINT('Ctrl Pts',(0.00932197027682847,-0.0333679869844681,
0.0685248359742998));
#79447=CARTESIAN_POINT('',(0.00946918412008307,-0.0336938721132538,0.0684315730082921));
#79448=CARTESIAN_POINT('Origin',(0.00812378219310841,-0.0315241814719618,
0.07415));
#79449=CARTESIAN_POINT('',(0.00937377007976809,-0.0337108120655697,0.0682816501239629));
#79450=CARTESIAN_POINT('',(0.00936123232798906,-0.0336938721132327,0.0682789935135702));
#79451=CARTESIAN_POINT('Origin',(0.00487213367656529,-0.034556251928565,
0.0840510377659916));
#79452=CARTESIAN_POINT('Ctrl Pts',(0.00936123232799071,-0.0336938721132336,
0.0682789935135684));
#79453=CARTESIAN_POINT('Ctrl Pts',(0.00936332227440066,-0.0336910493199299,
0.0682794340180156));
#79454=CARTESIAN_POINT('Ctrl Pts',(0.00936541205519568,-0.0336882265977529,
0.0682798756530937));
#79455=CARTESIAN_POINT('Ctrl Pts',(0.00936959130360236,-0.0336825812712303,
0.0682807611888089));
#79456=CARTESIAN_POINT('Ctrl Pts',(0.0093716807711426,-0.0336797586669754,
0.0682812050894407));
#79457=CARTESIAN_POINT('Ctrl Pts',(0.00937377008003416,-0.0336769361243751,
0.0682816501226888));
#79458=CARTESIAN_POINT('Origin',(0.00705830094378643,-0.034556251861001,
0.0845167005544149));
#79459=CARTESIAN_POINT('Ctrl Pts',(0.00947912980566762,-0.0342436276873911,
0.0685606209782186));
#79460=CARTESIAN_POINT('Ctrl Pts',(0.00926832290066522,-0.0339430054201811,
0.0685095032003237));
#79461=CARTESIAN_POINT('Ctrl Pts',(0.00905426447550039,-0.0336441434784052,
0.0684744094825159));
#79462=CARTESIAN_POINT('Ctrl Pts',(0.0092349476775481,-0.0342436276873911,
0.0685070011282839));
#79463=CARTESIAN_POINT('Ctrl Pts',(0.00902211846656726,-0.0339430054201811,
0.0684650928311712));
#79464=CARTESIAN_POINT('Ctrl Pts',(0.00880673717641047,-0.0336441434784052,
0.0684393347593488));
#79465=CARTESIAN_POINT('Ctrl Pts',(0.0092325058562669,-0.0342436276873911,
0.0685064649297845));
#79466=CARTESIAN_POINT('Ctrl Pts',(0.00901965642222629,-0.0339430054201811,
0.0684646487274797));
#79467=CARTESIAN_POINT('Ctrl Pts',(0.00880426190341958,-0.0336441434784052,
0.0684389840121171));
#79468=CARTESIAN_POINT('',(0.00919942996230135,-0.0341934961088741,0.068500123286599));
#79469=CARTESIAN_POINT('',(0.00896639895363432,-0.0338664212862939,0.0684607010976068));
#79470=CARTESIAN_POINT('Origin',(0.00557044497237628,-0.0345610720406228,
0.0848366961130874));
#79471=CARTESIAN_POINT('Origin',(0.0105729984233713,-0.0336938005072981,
0.0576127721447583));
#79472=CARTESIAN_POINT('',(0.00908985111544924,-0.0336938721132327,0.0684803584031009));
#79473=CARTESIAN_POINT('',(0.00902802551735347,-0.0336938721132427,0.0684712016886965));
#79474=CARTESIAN_POINT('',(0.00932197027683366,-0.0340203938281605,0.0685248359743009));
#79475=CARTESIAN_POINT('Origin',(0.00512241414220757,-0.0345589643243073,
0.0846611822701679));
#79476=CARTESIAN_POINT('',(0.00932168725141203,-0.034193496108874,0.06852616470091));
#79477=CARTESIAN_POINT('Origin',(0.0116173839760832,-0.0341934220717635,
0.0577485028575781));
#79478=CARTESIAN_POINT('',(0.0092605586068667,-0.0341934961088841,0.0685131439937645));
#79479=CARTESIAN_POINT('Ctrl Pts',(0.0096028304090113,-0.0340223579322397,
0.0683351555158321));
#79480=CARTESIAN_POINT('Ctrl Pts',(0.00952262853782355,-0.0339125849573575,
0.0683147555834151));
#79481=CARTESIAN_POINT('Ctrl Pts',(0.00944206079236394,-0.0338030433565231,
0.0682960299781646));
#79482=CARTESIAN_POINT('Ctrl Pts',(0.00936123232798963,-0.0336938721132327,
0.0682789935135698));
#79483=CARTESIAN_POINT('Ctrl Pts',(0.00950911390975521,-0.0340223579322397,
0.06839886106973));
#79484=CARTESIAN_POINT('Ctrl Pts',(0.00942979070430676,-0.0339125849573575,
0.0683797537322607));
#79485=CARTESIAN_POINT('Ctrl Pts',(0.00935012776087007,-0.0338030433565231,
0.0683623016273272));
#79486=CARTESIAN_POINT('Ctrl Pts',(0.00927022893334515,-0.0336938721132327,
0.0683465180423977));
#79487=CARTESIAN_POINT('Ctrl Pts',(0.00941539741049911,-0.0340223579322397,
0.0684625666236279));
#79488=CARTESIAN_POINT('Ctrl Pts',(0.00933695287078998,-0.0339125849573575,
0.0684447518811061));
#79489=CARTESIAN_POINT('Ctrl Pts',(0.0092581947293762,-0.0338030433565231,
0.0684285732764898));
#79490=CARTESIAN_POINT('Ctrl Pts',(0.00917922553870066,-0.0336938721132327,
0.0684140425712256));
#79491=CARTESIAN_POINT('Ctrl Pts',(0.00932168091124302,-0.0340223579322397,
0.0685262721775258));
#79492=CARTESIAN_POINT('Ctrl Pts',(0.0092441150372732,-0.0339125849573575,
0.0685097500299517));
#79493=CARTESIAN_POINT('Ctrl Pts',(0.00916626169788233,-0.0338030433565231,
0.0684948449256524));
#79494=CARTESIAN_POINT('Ctrl Pts',(0.00908822214405618,-0.0336938721132327,
0.0684815671000535));
#79495=CARTESIAN_POINT('',(0.00922554172172915,-0.0336938721132427,0.0683796759583456));
#79496=CARTESIAN_POINT('Ctrl Pts',(0.00937377007901281,-0.0337108120662708,
0.0682816501274828));
#79497=CARTESIAN_POINT('Ctrl Pts',(0.00936481198745918,-0.0337611408994052,
0.0683237059073984));
#79498=CARTESIAN_POINT('Ctrl Pts',(0.00935601736120198,-0.0338121088780783,
0.0683649942626355));
#79499=CARTESIAN_POINT('Ctrl Pts',(0.00933874702749835,-0.0339153382773248,
0.0684460737368694));
#79500=CARTESIAN_POINT('Ctrl Pts',(0.00933027862647408,-0.0339675558473126,
0.0684858305542207));
#79501=CARTESIAN_POINT('Ctrl Pts',(0.00932197027682019,-0.0340203938281304,
0.0685248359743387));
#79502=CARTESIAN_POINT('Ctrl Pts',(0.00920053384070664,-0.0341934961088741,
0.0685018247078726));
#79503=CARTESIAN_POINT('Ctrl Pts',(0.00908376226624132,-0.0340287516182428,
0.0684795637158362));
#79504=CARTESIAN_POINT('Ctrl Pts',(0.00896617040716373,-0.0338644633275951,
0.068462148003154));
#79505=CARTESIAN_POINT('Ctrl Pts',(0.00919942996230142,-0.0341934961088741,
0.0685001232865991));
#79506=CARTESIAN_POINT('Ctrl Pts',(0.00908262321229166,-0.0340287516182428,
0.0684778851163791));
#79507=CARTESIAN_POINT('Ctrl Pts',(0.00896499715096946,-0.0338644633275951,
0.0684604936598445));
#79508=CARTESIAN_POINT('Ctrl Pts',(0.00901550258770956,-0.0341934961088741,
0.0682166337768639));
#79509=CARTESIAN_POINT('Ctrl Pts',(0.00889283491542242,-0.0340287516182428,
0.0681981981602134));
#79510=CARTESIAN_POINT('Ctrl Pts',(0.0087695101022927,-0.0338644633275951,
0.0681848482444032));
#79511=CARTESIAN_POINT('',(0.00900282677761839,-0.0341764758832387,0.0682147425827495));
#79512=CARTESIAN_POINT('',(0.00901550258770958,-0.0341934961088741,0.0682166337768639));
#79513=CARTESIAN_POINT('Origin',(0.00607042016919592,-0.0345621026741051,
0.0845188009261542));
#79514=CARTESIAN_POINT('Ctrl Pts',(0.00900282677907111,-0.0341764758837478,
0.0682147425838354));
#79515=CARTESIAN_POINT('Ctrl Pts',(0.00899653805236467,-0.0341260050040109,
0.0682572037910506));
#79516=CARTESIAN_POINT('Ctrl Pts',(0.00899035867635939,-0.034074926914751,
0.0682989269279109));
#79517=CARTESIAN_POINT('Ctrl Pts',(0.00897821365523165,-0.0339715436305192,
0.0683809293698836));
#79518=CARTESIAN_POINT('Ctrl Pts',(0.00897225261175909,-0.0339192778237909,
0.0684211775640896));
#79519=CARTESIAN_POINT('Ctrl Pts',(0.00896639895499798,-0.0338664212855148,
0.0684607010967668));
#79520=CARTESIAN_POINT('',(0.00910746627501547,-0.0341934961088841,0.0683583785317415));
#79521=CARTESIAN_POINT('Origin',(0.00812378219310841,-0.0315241814719618,
0.07415));
#79522=CARTESIAN_POINT('',(0.00900282677667802,-0.0342105180190385,0.0682147425833554));
#79523=CARTESIAN_POINT('',(0.00899014695537364,-0.0341934961088739,0.0682128784669065));
#79524=CARTESIAN_POINT('Origin',(0.00611419109639066,-0.0345621711952478,
0.0845305732891805));
#79525=CARTESIAN_POINT('Origin',(0.00708356742671601,-0.0345621034907608,
0.0846688553305032));
#79526=CARTESIAN_POINT('Origin',(0.00703826376628337,-0.0345621719649244,
0.0846674314698193));
#79527=CARTESIAN_POINT('Ctrl Pts',(0.00909133493960705,-0.0346945769586965,
0.068480578165699));
#79528=CARTESIAN_POINT('Ctrl Pts',(0.00897258662937496,-0.0345275153362944,
0.0684603123860367));
#79529=CARTESIAN_POINT('Ctrl Pts',(0.00885317026463046,-0.0343603235965185,
0.0684437758896621));
#79530=CARTESIAN_POINT('Ctrl Pts',(0.00873343975286591,-0.034193496108874,
0.0684310123350075));
#79531=CARTESIAN_POINT('Ctrl Pts',(0.00900840620054512,-0.0346945769586965,
0.0684682959589172));
#79532=CARTESIAN_POINT('Ctrl Pts',(0.00888940063457446,-0.0345275153362944,
0.0684497671548973));
#79533=CARTESIAN_POINT('Ctrl Pts',(0.00876978157383706,-0.0343603235965185,
0.0684349761738923));
#79534=CARTESIAN_POINT('Ctrl Pts',(0.00864990344858244,-0.034193496108874,
0.0684239615029649));
#79535=CARTESIAN_POINT('Ctrl Pts',(0.00892547746148334,-0.0346945769586965,
0.0684560137521339));
#79536=CARTESIAN_POINT('Ctrl Pts',(0.00880621463977408,-0.0345275153362944,
0.0684392219237586));
#79537=CARTESIAN_POINT('Ctrl Pts',(0.00868639288304374,-0.0343603235965185,
0.0684261764581236));
#79538=CARTESIAN_POINT('Ctrl Pts',(0.008566367144299,-0.034193496108874,
0.0684169106709219));
#79539=CARTESIAN_POINT('Ctrl Pts',(0.00884254872242126,-0.0346945769586965,
0.0684437315453535));
#79540=CARTESIAN_POINT('Ctrl Pts',(0.00872302864497345,-0.0345275153362944,
0.0684286766926186));
#79541=CARTESIAN_POINT('Ctrl Pts',(0.00860300419225025,-0.0343603235965185,
0.0684173767423528));
#79542=CARTESIAN_POINT('Ctrl Pts',(0.00848283084001552,-0.034193496108874,
0.0684098598388795));
#79543=CARTESIAN_POINT('',(0.00884254872302055,-0.0346945769586966,0.0684437315454424));
#79544=CARTESIAN_POINT('',(0.00860750220904207,-0.0343667727831449,0.068419019285803));
#79545=CARTESIAN_POINT('Origin',(0.00692295317821726,-0.0345626457063574,
0.0851473958191031));
#79546=CARTESIAN_POINT('Origin',(0.00953704488077846,-0.034193477102925,
0.0574059994983898));
#79547=CARTESIAN_POINT('',(0.00873194505769415,-0.034193496108874,0.0684308861761511));
#79548=CARTESIAN_POINT('',(0.00866966650343826,-0.034193496108884,0.0684256295918562));
#79549=CARTESIAN_POINT('',(0.00896639895474167,-0.0345211942962698,0.0684607010983054));
#79550=CARTESIAN_POINT('Origin',(0.00644781684592441,-0.0345625596119992,
0.0850736648505043));
#79551=CARTESIAN_POINT('',(0.00896619991923768,-0.0346945769586885,0.0684620449742721));
#79552=CARTESIAN_POINT('Origin',(0.0105870954200286,-0.0346945685853848,
0.0575178587106754));
#79553=CARTESIAN_POINT('',(0.00890437432113911,-0.0346945769587026,0.0684528882598673));
#79554=CARTESIAN_POINT('Ctrl Pts',(0.00923479379353328,-0.0345231616327842,
0.0682537593990969));
#79555=CARTESIAN_POINT('Ctrl Pts',(0.00915352241809257,-0.0344132092796988,
0.0682384456683642));
#79556=CARTESIAN_POINT('Ctrl Pts',(0.00907193848344034,-0.0343032738558979,
0.0682248137620447));
#79557=CARTESIAN_POINT('Ctrl Pts',(0.00899014695537362,-0.0341934961088739,
0.0682128784669065));
#79558=CARTESIAN_POINT('Ctrl Pts',(0.00914526249066111,-0.0345231616327842,
0.068323223648495));
#79559=CARTESIAN_POINT('Ctrl Pts',(0.00906494858210052,-0.0344132092796988,
0.0683091439807224));
#79560=CARTESIAN_POINT('Ctrl Pts',(0.00898434759054642,-0.0343032738558979,
0.0682967262692438));
#79561=CARTESIAN_POINT('Ctrl Pts',(0.00890356318268683,-0.0341934961088739,
0.0682859837775601));
#79562=CARTESIAN_POINT('Ctrl Pts',(0.00905573118778895,-0.0345231616327842,
0.0683926878978931));
#79563=CARTESIAN_POINT('Ctrl Pts',(0.00897637474610847,-0.0344132092796988,
0.0683798422930806));
#79564=CARTESIAN_POINT('Ctrl Pts',(0.00889675669765251,-0.0343032738558979,
0.068368638776443));
#79565=CARTESIAN_POINT('Ctrl Pts',(0.00881697941000005,-0.0341934961088739,
0.0683590890882136));
#79566=CARTESIAN_POINT('Ctrl Pts',(0.00896619988491678,-0.0345231616327842,
0.0684621521472912));
#79567=CARTESIAN_POINT('Ctrl Pts',(0.00888780091011641,-0.0344132092796988,
0.0684505406054388));
#79568=CARTESIAN_POINT('Ctrl Pts',(0.0088091658047586,-0.0343032738558979,
0.0684405512836422));
#79569=CARTESIAN_POINT('Ctrl Pts',(0.00873039563731326,-0.0341934961088739,
0.0684321943988672));
#79570=CARTESIAN_POINT('',(0.00886104600654389,-0.0341934961088839,0.0683218823215388));
#79571=CARTESIAN_POINT('Ctrl Pts',(0.00900282677616696,-0.0342105180195411,
0.0682147425867688));
#79572=CARTESIAN_POINT('Ctrl Pts',(0.00899653096611941,-0.0342610556240986,
0.0682572515265621));
#79573=CARTESIAN_POINT('Ctrl Pts',(0.00899034813112771,-0.0343122189869487,
0.0682989976654116));
#79574=CARTESIAN_POINT('Ctrl Pts',(0.00897820299148925,-0.034415811969519,
0.0683810009351696));
#79575=CARTESIAN_POINT('Ctrl Pts',(0.00897224565430533,-0.0344681990450086,
0.0684212245260606));
#79576=CARTESIAN_POINT('Ctrl Pts',(0.00896639895472783,-0.0345211942962507,
0.0684607010983291));
#79577=CARTESIAN_POINT('Ctrl Pts',(0.00884375696040208,-0.0346945769586932,
0.0684453598974565));
#79578=CARTESIAN_POINT('Ctrl Pts',(0.00872581756275587,-0.034529677707698,
0.0684304749285805));
#79579=CARTESIAN_POINT('Ctrl Pts',(0.00860736373340941,-0.0343648066251421,
0.0684204772224062));
#79580=CARTESIAN_POINT('Ctrl Pts',(0.00884254872302953,-0.0346945769586932,
0.0684437315454436));
#79581=CARTESIAN_POINT('Ctrl Pts',(0.00872457566035763,-0.034529677707698,
0.0684288715560203));
#79582=CARTESIAN_POINT('Ctrl Pts',(0.00860608922717556,-0.0343648066251421,
0.0684189001993606));
#79583=CARTESIAN_POINT('Ctrl Pts',(0.00864118383350006,-0.0346945769586932,
0.0681723503329051));
#79584=CARTESIAN_POINT('Ctrl Pts',(0.00851760015628211,-0.034529677707698,
0.0681616534200916));
#79585=CARTESIAN_POINT('Ctrl Pts',(0.00839367996653584,-0.0343648066251421,
0.0681560734745996));
#79586=CARTESIAN_POINT('',(0.00862841428707689,-0.034677539666497,0.0681712587910915));
#79587=CARTESIAN_POINT('',(0.0086411838334966,-0.0346945769586886,0.0681723503329048));
#79588=CARTESIAN_POINT('Origin',(0.00738436647832412,-0.0345626618200292,
0.0847261748801848));
#79589=CARTESIAN_POINT('Ctrl Pts',(0.00862841428853804,-0.0346775396670096,
0.0681712587921676));
#79590=CARTESIAN_POINT('Ctrl Pts',(0.00862480128828991,-0.0346269749928196,
0.0682140647711545));
#79591=CARTESIAN_POINT('Ctrl Pts',(0.00862125253491084,-0.0345757902890802,
0.0682561099954001));
#79592=CARTESIAN_POINT('Ctrl Pts',(0.00861428042754002,-0.0344721681087925,
0.0683387135466323));
#79593=CARTESIAN_POINT('Ctrl Pts',(0.00861085980132514,-0.0344197714289547,
0.0683792394886702));
#79594=CARTESIAN_POINT('Ctrl Pts',(0.00860750220928402,-0.0343667727830614,
0.0684190192857122));
#79595=CARTESIAN_POINT('',(0.00874186627826858,-0.0346945769587026,0.0683080409391836));
#79596=CARTESIAN_POINT('Origin',(0.00812378219310841,-0.0315241814719618,
0.07415));
#79597=CARTESIAN_POINT('',(0.00862841428624165,-0.0347116136489629,0.0681712587922044));
#79598=CARTESIAN_POINT('',(0.00861564243684597,-0.0346945769586885,0.0681701945265211));
#79599=CARTESIAN_POINT('Origin',(0.00742963708757855,-0.034562669108892,
0.0847281199836829));
#79600=CARTESIAN_POINT('Origin',(0.00708001546907962,-0.0345626625512408,
0.0847004881000318));
#79601=CARTESIAN_POINT('Origin',(0.00703505963744553,-0.0345626698804197,
0.0846948142349712));
#79602=CARTESIAN_POINT('Ctrl Pts',(0.00877034420266972,-0.0352450361874068,
0.068435044165226));
#79603=CARTESIAN_POINT('Ctrl Pts',(0.00855480110646341,-0.0349452760959493,
0.0684106586788882));
#79604=CARTESIAN_POINT('Ctrl Pts',(0.00833803353089584,-0.034644428984174,
0.0684025780570867));
#79605=CARTESIAN_POINT('Ctrl Pts',(0.00876782953156976,-0.0352450361874068,
0.0684348160112013));
#79606=CARTESIAN_POINT('Ctrl Pts',(0.0085522778303932,-0.0349452760959493,
0.0684105253672403));
#79607=CARTESIAN_POINT('Ctrl Pts',(0.00833550881821709,-0.034644428984174,
0.06840253996654));
#79608=CARTESIAN_POINT('Ctrl Pts',(0.00851885219493944,-0.0352450361874068,
0.0684122265038036));
#79609=CARTESIAN_POINT('Ctrl Pts',(0.00830244851651108,-0.0349452760959493,
0.0683973261941819));
#79610=CARTESIAN_POINT('Ctrl Pts',(0.0080855372658654,-0.034644428984174,
0.068398768625282));
#79611=CARTESIAN_POINT('Ctrl Pts',(0.00851636242157314,-0.0352450361874068,
0.0684120006087297));
#79612=CARTESIAN_POINT('Ctrl Pts',(0.00829995022337226,-0.0349452760959493,
0.0683971942024513));
#79613=CARTESIAN_POINT('Ctrl Pts',(0.00808303755034189,-0.034644428984174,
0.0683987309118695));
#79614=CARTESIAN_POINT('',(0.00848286328436634,-0.0351951634053313,0.0684098594901857));
#79615=CARTESIAN_POINT('',(0.00824669644126924,-0.0348678972934172,0.0683999550361109));
#79616=CARTESIAN_POINT('Origin',(0.00831054463921628,-0.0345636767887066,
0.0851542556470295));
#79617=CARTESIAN_POINT('Origin',(0.00848283195180577,-0.0346946199326463,
0.0573526369146102));
#79618=CARTESIAN_POINT('',(0.00837163887693946,-0.0346945769330288,0.0684039846796013));
#79619=CARTESIAN_POINT('',(0.00830915314282402,-0.0346945769458128,0.0684026489702012));
#79620=CARTESIAN_POINT('',(0.00860750220925616,-0.0350221583435276,0.0684190192858483));
#79621=CARTESIAN_POINT('Origin',(0.00783078680931817,-0.0345628458717247,
0.085185493723715));
#79622=CARTESIAN_POINT('',(0.00860740119445584,-0.0351951360298762,0.0684202520424167));
#79623=CARTESIAN_POINT('Origin',(0.00953415430134055,-0.0351951838366932,
0.0574403170438433));
#79624=CARTESIAN_POINT('',(0.00848283084063969,-0.035195137132875,0.0684098598388155));
#79625=CARTESIAN_POINT('Ctrl Pts',(0.00886237250191847,-0.0350241211494343,
0.0681956331691984));
#79626=CARTESIAN_POINT('Ctrl Pts',(0.00878035354020962,-0.0349144232818962,
0.0681854593905283));
#79627=CARTESIAN_POINT('Ctrl Pts',(0.00869807518692388,-0.0348045283579412,
0.0681769749129075));
#79628=CARTESIAN_POINT('Ctrl Pts',(0.00861564242577058,-0.0346945769439158,
0.06817019452561));
#79629=CARTESIAN_POINT('Ctrl Pts',(0.00877737955818422,-0.0350241211494343,
0.0682705820939291));
#79630=CARTESIAN_POINT('Ctrl Pts',(0.00869639298718329,-0.0349144232818962,
0.0682615790582105));
#79631=CARTESIAN_POINT('Ctrl Pts',(0.00861517184263443,-0.0348045283579412,
0.0682542446840336));
#79632=CARTESIAN_POINT('Ctrl Pts',(0.00853381980891576,-0.0346945769439158,
0.068248592237145));
#79633=CARTESIAN_POINT('Ctrl Pts',(0.00869238661444998,-0.0350241211494343,
0.0683455310186597));
#79634=CARTESIAN_POINT('Ctrl Pts',(0.00861243243415695,-0.0349144232818962,
0.0683376987258926));
#79635=CARTESIAN_POINT('Ctrl Pts',(0.00853226849834498,-0.0348045283579412,
0.0683315144551596));
#79636=CARTESIAN_POINT('Ctrl Pts',(0.00845199719206094,-0.0346945769439158,
0.06832698994868));
#79637=CARTESIAN_POINT('Ctrl Pts',(0.00860739367071574,-0.0350241211494343,
0.0684204799433904));
#79638=CARTESIAN_POINT('Ctrl Pts',(0.00852847188113062,-0.0349144232818962,
0.0684138183935748));
#79639=CARTESIAN_POINT('Ctrl Pts',(0.00844936515405553,-0.0348045283579412,
0.0684087842262857));
#79640=CARTESIAN_POINT('Ctrl Pts',(0.00837017457520612,-0.0346945769439158,
0.068405387660215));
#79641=CARTESIAN_POINT('',(0.00849364065719382,-0.0346945769458128,0.0682870896029957));
#79642=CARTESIAN_POINT('Ctrl Pts',(0.00862841428596019,-0.0347116136492814,
0.0681712587954768));
#79643=CARTESIAN_POINT('Ctrl Pts',(0.00862480270768245,-0.0347621546531972,
0.0682140477741575));
#79644=CARTESIAN_POINT('Ctrl Pts',(0.00862125463071028,-0.0348133084096332,
0.0682560844069658));
#79645=CARTESIAN_POINT('Ctrl Pts',(0.00861428251825559,-0.0349168561544578,
0.0683386880633838));
#79646=CARTESIAN_POINT('Ctrl Pts',(0.00861086124826331,-0.0349692089015921,
0.0683792223222317));
#79647=CARTESIAN_POINT('Ctrl Pts',(0.00860750220923327,-0.0350221583435,
0.0684190192858831));
#79648=CARTESIAN_POINT('Ctrl Pts',(0.00848377467691702,-0.0351951371254934,
0.06841097769077));
#79649=CARTESIAN_POINT('Ctrl Pts',(0.00836512399177465,-0.0350307338985347,
0.068403535072054));
#79650=CARTESIAN_POINT('Ctrl Pts',(0.00824626708148386,-0.0348659306906634,
0.0684010027738433));
#79651=CARTESIAN_POINT('Ctrl Pts',(0.00848283084063733,-0.0351951371254934,
0.0684098598389319));
#79652=CARTESIAN_POINT('Ctrl Pts',(0.00836415704460963,-0.0350307338985347,
0.0684024367334387));
#79653=CARTESIAN_POINT('Ctrl Pts',(0.00824527784968418,-0.0348659306906634,
0.0683999248869747));
#79654=CARTESIAN_POINT('Ctrl Pts',(0.00832464289630539,-0.0351951371254934,
0.0682225067056039));
#79655=CARTESIAN_POINT('Ctrl Pts',(0.0082020956918058,-0.0350307338985347,
0.0682183540366006));
#79656=CARTESIAN_POINT('Ctrl Pts',(0.00807948156888189,-0.0348659306906634,
0.068219269924209));
#79657=CARTESIAN_POINT('Origin',(0.00836035143919025,-0.0308609188508941,
0.0630829868146784));
#79658=CARTESIAN_POINT('',(0.00841386446357033,-0.0351951371254934,0.0683281780970498));
#79659=CARTESIAN_POINT('Origin',(0.00824466076921519,-0.03518404674411,
0.0751196050847292));
#79660=CARTESIAN_POINT('Origin',(0.00758442489567276,-0.0352322614919394,
0.0621970607340446));
#79661=CARTESIAN_POINT('',(0.00801004046581113,-0.0351951142564661,0.0683997932730299));
#79662=CARTESIAN_POINT('',(0.00788546184042353,-0.0351951372916786,0.0684049409568311));
#79663=CARTESIAN_POINT('Origin',(0.00784137974656666,-0.0352875121444807,
0.0743403964868405));
#79664=CARTESIAN_POINT('Origin',(0.015541196766919,-0.0298325076521634,
0.0752801111993773));
#79665=CARTESIAN_POINT('Origin',(0.0109540556667107,-0.0338732909226762,
0.0662609219776647));
#79666=CARTESIAN_POINT('Ctrl Pts',(0.0114119592548226,-0.0321934096636941,
0.0694313108434516));
#79667=CARTESIAN_POINT('Ctrl Pts',(0.0113274969660167,-0.0320508460844714,
0.0693724540399162));
#79668=CARTESIAN_POINT('Ctrl Pts',(0.0112415169958787,-0.0319086045663848,
0.0693159109496467));
#79669=CARTESIAN_POINT('Ctrl Pts',(0.0111542144973951,-0.0317669892869059,
0.069261788078814));
#79670=CARTESIAN_POINT('Ctrl Pts',(0.0113421406583195,-0.0321934096636941,
0.0693848802909014));
#79671=CARTESIAN_POINT('Ctrl Pts',(0.0112568472847337,-0.0320508460844714,
0.069327273206995));
#79672=CARTESIAN_POINT('Ctrl Pts',(0.011170070433957,-0.0319086045663848,
0.0692720012236699));
#79673=CARTESIAN_POINT('Ctrl Pts',(0.0110820067494801,-0.0317669892869059,
0.0692191679689228));
#79674=CARTESIAN_POINT('Ctrl Pts',(0.0112723220618163,-0.0321934096636941,
0.0693384497383512));
#79675=CARTESIAN_POINT('Ctrl Pts',(0.0111861976034507,-0.0320508460844714,
0.0692820923740737));
#79676=CARTESIAN_POINT('Ctrl Pts',(0.0110986238720354,-0.0319086045663848,
0.0692280914976931));
#79677=CARTESIAN_POINT('Ctrl Pts',(0.0110097990015652,-0.0317669892869059,
0.0691765478590318));
#79678=CARTESIAN_POINT('Ctrl Pts',(0.0112025034653132,-0.0321934096636941,
0.0692920191858011));
#79679=CARTESIAN_POINT('Ctrl Pts',(0.0111155479221677,-0.0320508460844714,
0.0692369115411526));
#79680=CARTESIAN_POINT('Ctrl Pts',(0.0110271773101137,-0.0319086045663848,
0.0691841817717163));
#79681=CARTESIAN_POINT('Ctrl Pts',(0.0109375912536502,-0.0317669892869059,
0.0691339277491406));
#79682=CARTESIAN_POINT('',(0.0112037525338003,-0.0321934096636941,0.0692928498375633));
#79683=CARTESIAN_POINT('',(0.0110015980574996,-0.0318665617511295,0.0691704115792809));
#79684=CARTESIAN_POINT('Origin',(0.00174203632914428,-0.0326371944419843,
0.0830657882059943));
#79685=CARTESIAN_POINT('Origin',(0.0164862628977425,-0.0316939261508995,
0.0596800985292627));
#79686=CARTESIAN_POINT('',(0.0113083445140224,-0.0320197221621859,0.069360829717921));
#79687=CARTESIAN_POINT('Ctrl Pts',(0.011308221706302,-0.0320197392094768,
0.0693606913953178));
#79688=CARTESIAN_POINT('Ctrl Pts',(0.0112838521384082,-0.0319792716576065,
0.0693444879823917));
#79689=CARTESIAN_POINT('Ctrl Pts',(0.011259248102668,-0.0319386439829744,
0.06932839658914));
#79690=CARTESIAN_POINT('Ctrl Pts',(0.0112343791402907,-0.0318979099381675,
0.0693124074007847));
#79691=CARTESIAN_POINT('Ctrl Pts',(0.0112095106694653,-0.0318571766984965,
0.0692964185284665));
#79692=CARTESIAN_POINT('Ctrl Pts',(0.0111845046438307,-0.0318163871833603,
0.0692806116242346));
#79693=CARTESIAN_POINT('Ctrl Pts',(0.011159448955242,-0.0317755399638303,
0.0692650380809617));
#79694=CARTESIAN_POINT('',(0.0113078380024955,-0.0321934096636183,0.0693620684421445));
#79695=CARTESIAN_POINT('Origin',(0.0125300026055346,-0.0324016312812858,
0.0674874531578453));
#79696=CARTESIAN_POINT('',(0.0112557952681579,-0.0321934096636663,0.0693274591398639));
#79697=CARTESIAN_POINT('Ctrl Pts',(0.0112041525739548,-0.0321934096636618,
0.0692948382176211));
#79698=CARTESIAN_POINT('Ctrl Pts',(0.011137196109084,-0.0320835708272592,
0.0692523575093689));
#79699=CARTESIAN_POINT('Ctrl Pts',(0.0110693993456345,-0.0319739230346488,
0.0692112871022145));
#79700=CARTESIAN_POINT('Ctrl Pts',(0.0110008530576767,-0.0318646057455572,
0.0691716728857455));
#79701=CARTESIAN_POINT('Ctrl Pts',(0.0111818019275799,-0.0321934096636618,
0.0691837454034018));
#79702=CARTESIAN_POINT('Ctrl Pts',(0.0111133134062204,-0.0320835708272592,
0.0691415729279822));
#79703=CARTESIAN_POINT('Ctrl Pts',(0.0110439918537996,-0.0319739230346488,
0.0691008422807022));
#79704=CARTESIAN_POINT('Ctrl Pts',(0.0109739299618877,-0.0318646057455572,
0.0690615987667271));
#79705=CARTESIAN_POINT('Ctrl Pts',(0.011159451281205,-0.0321934096636618,
0.0690726525891825));
#79706=CARTESIAN_POINT('Ctrl Pts',(0.0110894307033567,-0.0320835708272592,
0.0690307883465955));
#79707=CARTESIAN_POINT('Ctrl Pts',(0.0110185843619647,-0.0319739230346488,
0.06899039745919));
#79708=CARTESIAN_POINT('Ctrl Pts',(0.0109470068660988,-0.0318646057455572,
0.0689515246477087));
#79709=CARTESIAN_POINT('Ctrl Pts',(0.0111371006348302,-0.0321934096636618,
0.0689615597749632));
#79710=CARTESIAN_POINT('Ctrl Pts',(0.0110655480004931,-0.0320835708272592,
0.0689200037652088));
#79711=CARTESIAN_POINT('Ctrl Pts',(0.0109931768701297,-0.0319739230346488,
0.0688799526376777));
#79712=CARTESIAN_POINT('Ctrl Pts',(0.0109200837703098,-0.0318646057455572,
0.0688414505286903));
#79713=CARTESIAN_POINT('',(0.0111260111583635,-0.0321763980308461,0.0689551351107169));
#79714=CARTESIAN_POINT('',(0.0111371006348019,-0.0321934096636184,0.0689615597749468));
#79715=CARTESIAN_POINT('Origin',(0.00232053340556324,-0.0326386231341034,
0.0829654760549868));
#79716=CARTESIAN_POINT('Ctrl Pts',(0.01112601115677,-0.0321763980306278,
0.0689551351134602));
#79717=CARTESIAN_POINT('Ctrl Pts',(0.0111045357659456,-0.032125959617482,
0.0689922947555354));
#79718=CARTESIAN_POINT('Ctrl Pts',(0.0110834324641401,-0.0320749164631395,
0.0690288105585962));
#79719=CARTESIAN_POINT('Ctrl Pts',(0.0110419530552891,-0.0319716057793937,
0.0691005838734109));
#79720=CARTESIAN_POINT('Ctrl Pts',(0.0110215931100143,-0.031919378669013,
0.069135813419871));
#79721=CARTESIAN_POINT('Ctrl Pts',(0.0110015980565636,-0.0318665617525324,
0.0691704115808816));
#79722=CARTESIAN_POINT('',(0.0111704265843111,-0.0321934096636663,0.0691272048062651));
#79723=CARTESIAN_POINT('Origin',(0.00812378219310841,-0.0315241814719618,
0.07415));
#79724=CARTESIAN_POINT('',(0.0111260111585486,-0.0322104233323797,0.0689551351103958));
#79725=CARTESIAN_POINT('',(0.0111149079858696,-0.0321934096636183,0.0689487341452394));
#79726=CARTESIAN_POINT('Origin',(0.00235624051314064,-0.0326387238286708,
0.0829934069770395));
#79727=CARTESIAN_POINT('Origin',(0.0033828877309766,-0.0326386239491269,
0.0835794368688629));
#79728=CARTESIAN_POINT('Origin',(0.0033408619234511,-0.0326387246148537,
0.0835624393439663));
#79729=CARTESIAN_POINT('Ctrl Pts',(0.0111399791707251,-0.0327445246967096,
0.0692529926697814));
#79730=CARTESIAN_POINT('Ctrl Pts',(0.0109552855199338,-0.032443687833936,
0.0691392349410836));
#79731=CARTESIAN_POINT('Ctrl Pts',(0.010762547867239,-0.0321434074405927,
0.0690397122667085));
#79732=CARTESIAN_POINT('Ctrl Pts',(0.0109243168805336,-0.0327445246967096,
0.0691265419814108));
#79733=CARTESIAN_POINT('Ctrl Pts',(0.0107348540640651,-0.032443687833936,
0.0690209180889579));
#79734=CARTESIAN_POINT('Ctrl Pts',(0.0105379734681785,-0.0321434074405927,
0.0689298653765085));
#79735=CARTESIAN_POINT('',(0.0108926919338008,-0.0326943950436612,0.0691090413760972));
#79736=CARTESIAN_POINT('',(0.0106832484016998,-0.0323666188837389,0.0689995381054628));
#79737=CARTESIAN_POINT('Origin',(0.00286600315301682,-0.0326395579112592,
0.0838799697641049));
#79738=CARTESIAN_POINT('Origin',(0.0155983125060639,-0.0321933825603078,
0.0591088598334281));
#79739=CARTESIAN_POINT('',(0.0107945839480072,-0.0321934096532689,0.0690563821322444));
#79740=CARTESIAN_POINT('',(0.0107386138880983,-0.0321934096584275,0.0690285684172921));
#79741=CARTESIAN_POINT('',(0.0110015980579694,-0.0325210109756238,0.069170411578458));
#79742=CARTESIAN_POINT('Origin',(0.00245738055630698,-0.03263931291576,
0.0836265688898258));
#79743=CARTESIAN_POINT('',(0.0110009182856955,-0.0326943950436593,0.0691715878128933));
#79744=CARTESIAN_POINT('Origin',(0.0165362565107906,-0.0326943765538283,
0.0595935949407701));
#79745=CARTESIAN_POINT('',(0.0109468051097582,-0.0326943950436702,0.0691403145945052));
#79746=CARTESIAN_POINT('Ctrl Pts',(0.0113273257135278,-0.0325229783203769,
0.0690768048615494));
#79747=CARTESIAN_POINT('Ctrl Pts',(0.0112573918294877,-0.032413025309245,
0.0690326440841773));
#79748=CARTESIAN_POINT('Ctrl Pts',(0.0111865550298829,-0.032303122220807,
0.0689899366768802));
#79749=CARTESIAN_POINT('Ctrl Pts',(0.0111149079819824,-0.0321934096576658,
0.068948734143004));
#79750=CARTESIAN_POINT('Ctrl Pts',(0.0112185100910129,-0.0325229783203769,
0.0691084324212555));
#79751=CARTESIAN_POINT('Ctrl Pts',(0.0111490121921917,-0.032413025309245,
0.0690657716648601));
#79752=CARTESIAN_POINT('Ctrl Pts',(0.011078642341541,-0.032303122220807,
0.0690245550321178));
#79753=CARTESIAN_POINT('Ctrl Pts',(0.0110074925408185,-0.0321934096576658,
0.0689848321379043));
#79754=CARTESIAN_POINT('Ctrl Pts',(0.011109694468498,-0.0325229783203769,
0.0691400599809615));
#79755=CARTESIAN_POINT('Ctrl Pts',(0.0110406325548958,-0.032413025309245,
0.0690988992455428));
#79756=CARTESIAN_POINT('Ctrl Pts',(0.010970729653199,-0.032303122220807,
0.0690591733873553));
#79757=CARTESIAN_POINT('Ctrl Pts',(0.0109000770996546,-0.0321934096576658,
0.0690209301328046));
#79758=CARTESIAN_POINT('Ctrl Pts',(0.0110008788459832,-0.0325229783203769,
0.0691716875406675));
#79759=CARTESIAN_POINT('Ctrl Pts',(0.0109322529175998,-0.032413025309245,
0.0691320268262256));
#79760=CARTESIAN_POINT('Ctrl Pts',(0.010862816964857,-0.032303122220807,
0.0690937917425929));
#79761=CARTESIAN_POINT('Ctrl Pts',(0.0107926616584907,-0.0321934096576658,
0.0690570281277049));
#79762=CARTESIAN_POINT('',(0.0109547459674448,-0.0321934096584275,0.0690025581388497));
#79763=CARTESIAN_POINT('Ctrl Pts',(0.0111260111568023,-0.0322104233328951,
0.0689551351134042));
#79764=CARTESIAN_POINT('Ctrl Pts',(0.0111045066664953,-0.0322609421830959,
0.0689923451073623));
#79765=CARTESIAN_POINT('Ctrl Pts',(0.011083389149112,-0.0323120888239857,
0.0690288855081357));
#79766=CARTESIAN_POINT('Ctrl Pts',(0.0110419094261723,-0.0324156524631821,
0.0691006593664293));
#79767=CARTESIAN_POINT('Ctrl Pts',(0.0110215642710091,-0.0324680267167318,
0.0691358633210402));
#79768=CARTESIAN_POINT('Ctrl Pts',(0.011001598057944,-0.0325210109755912,
0.0691704115784933));
#79769=CARTESIAN_POINT('Origin',(0.0144121497996153,-0.0262834582512331,
0.0788786169947828));
#79770=CARTESIAN_POINT('Origin',(0.0182740287853487,-0.0342770848922325,
0.0674570010021419));
#79771=CARTESIAN_POINT('Ctrl Pts',(0.0108932159087258,-0.0326943950436604,
0.0691110002382951));
#79772=CARTESIAN_POINT('Ctrl Pts',(0.0108237690479174,-0.0325844576448134,
0.0690728322512219));
#79773=CARTESIAN_POINT('Ctrl Pts',(0.0107535278956968,-0.0324744968375322,
0.0690360978378822));
#79774=CARTESIAN_POINT('Ctrl Pts',(0.01068258309831,-0.0323646534831895,
0.0690008428232186));
#79775=CARTESIAN_POINT('Ctrl Pts',(0.0108639338331196,-0.0326943950436604,
0.0690015302075579));
#79776=CARTESIAN_POINT('Ctrl Pts',(0.0107929782701189,-0.0325844576448134,
0.0689637657823671));
#79777=CARTESIAN_POINT('Ctrl Pts',(0.0107212366552543,-0.0324744968375322,
0.0689274661619053));
#79778=CARTESIAN_POINT('Ctrl Pts',(0.0106488015495679,-0.0323646534831895,
0.0688926765875164));
#79779=CARTESIAN_POINT('Ctrl Pts',(0.0108346517575133,-0.0326943950436604,
0.0688920601768208));
#79780=CARTESIAN_POINT('Ctrl Pts',(0.0107621874923204,-0.0325844576448134,
0.0688546993135122));
#79781=CARTESIAN_POINT('Ctrl Pts',(0.0106889454148117,-0.0324744968375322,
0.0688188344859283));
#79782=CARTESIAN_POINT('Ctrl Pts',(0.0106150200008259,-0.0323646534831895,
0.0687845103518142));
#79783=CARTESIAN_POINT('Ctrl Pts',(0.0108053696819071,-0.0326943950436604,
0.0687825901460836));
#79784=CARTESIAN_POINT('Ctrl Pts',(0.010731396714522,-0.0325844576448134,
0.0687456328446574));
#79785=CARTESIAN_POINT('Ctrl Pts',(0.0106566541743692,-0.0324744968375322,
0.0687102028099514));
#79786=CARTESIAN_POINT('Ctrl Pts',(0.0105812384520838,-0.0323646534831895,
0.0686763441161119));
#79787=CARTESIAN_POINT('',(0.0107938986801022,-0.0326773559991343,0.0687768744732653));
#79788=CARTESIAN_POINT('',(0.0108053696819065,-0.0326943950436595,0.0687825901460834));
#79789=CARTESIAN_POINT('Origin',(0.00344927916746203,-0.0326395670565505,
0.0836694858002616));
#79790=CARTESIAN_POINT('Ctrl Pts',(0.0107938986786049,-0.0326773559987421,
0.0687768744762628));
#79791=CARTESIAN_POINT('Ctrl Pts',(0.0107747835676132,-0.0326267922585945,
0.0688153401729154));
#79792=CARTESIAN_POINT('Ctrl Pts',(0.0107560072581608,-0.0325756109579297,
0.0688531240928712));
#79793=CARTESIAN_POINT('Ctrl Pts',(0.0107191162627669,-0.032471998546237,
0.0689273605353723));
#79794=CARTESIAN_POINT('Ctrl Pts',(0.010701016372794,-0.0324196091621769,
0.0689637832837125));
#79795=CARTESIAN_POINT('Ctrl Pts',(0.0106832484016781,-0.0323666188837756,
0.0689995381055065));
#79796=CARTESIAN_POINT('',(0.0108490308078636,-0.0326943950436702,0.0689458157611003));
#79797=CARTESIAN_POINT('Origin',(0.00812378219310841,-0.0315241814719618,
0.07415));
#79798=CARTESIAN_POINT('',(0.0107938986800819,-0.0327114338380068,0.0687768744733054));
#79799=CARTESIAN_POINT('',(0.0107824154971443,-0.0326943950436593,0.0687711833127829));
#79800=CARTESIAN_POINT('Origin',(0.00349019476756723,-0.0326395672881448,
0.0836889521683736));
#79801=CARTESIAN_POINT('Origin',(0.00335929596177808,-0.0326395676539919,
0.0836247712427188));
#79802=CARTESIAN_POINT('Origin',(0.00331907223276828,-0.0326395680355474,
0.0836039130573845));
#79803=CARTESIAN_POINT('Ctrl Pts',(0.0108265071376824,-0.0332451089994433,
0.0690732487874648));
#79804=CARTESIAN_POINT('Ctrl Pts',(0.0106350343330425,-0.0329451141710254,
0.0689713138484372));
#79805=CARTESIAN_POINT('Ctrl Pts',(0.0104364273261115,-0.0326442513127493,
0.0688840910102056));
#79806=CARTESIAN_POINT('Ctrl Pts',(0.0106033297350171,-0.0332451089994433,
0.0689605906899326));
#79807=CARTESIAN_POINT('Ctrl Pts',(0.0104076079607119,-0.0329451141710254,
0.0688670730243603));
#79808=CARTESIAN_POINT('Ctrl Pts',(0.0102053980784369,-0.0326442513127493,
0.0687885635967636));
#79809=CARTESIAN_POINT('Ctrl Pts',(0.0106010979609905,-0.0332451089994433,
0.0689594641089573));
#79810=CARTESIAN_POINT('Ctrl Pts',(0.0104053336969887,-0.0329451141710254,
0.0688660306161196));
#79811=CARTESIAN_POINT('Ctrl Pts',(0.0102030877859601,-0.0326442513127493,
0.0687876083226291));
#79812=CARTESIAN_POINT('',(0.0105707037120035,-0.0331951640388616,0.0689451272752959));
#79813=CARTESIAN_POINT('',(0.0103547976911229,-0.0328677532355004,0.0688489911415425));
#79814=CARTESIAN_POINT('Origin',(0.00414093313941138,-0.032640280828004,
0.0844270618394905));
#79815=CARTESIAN_POINT('Origin',(0.0146431817190043,-0.0326944278779173,
0.0586585963809617));
#79816=CARTESIAN_POINT('',(0.0104694828127754,-0.0326943950436593,0.0688987321908995));
#79817=CARTESIAN_POINT('',(0.010411876761808,-0.0326943950436693,0.0688744877504997));
#79818=CARTESIAN_POINT('',(0.0106832484017023,-0.0330220786163545,0.0689995381054641));
#79819=CARTESIAN_POINT('Origin',(0.00368655644724267,-0.0326396682762806,
0.0842699171074804));
#79820=CARTESIAN_POINT('',(0.0106826438271766,-0.0331951640388587,0.0690007547021243));
#79821=CARTESIAN_POINT('Origin',(0.0155919445563444,-0.0331952026560276,
0.0591216790399452));
#79822=CARTESIAN_POINT('',(0.0106266737696,-0.0331951640388701,0.0689729409887201));
#79823=CARTESIAN_POINT('Ctrl Pts',(0.0110024548506785,-0.0330240426238172,
0.0688856630302979));
#79824=CARTESIAN_POINT('Ctrl Pts',(0.0109299334801259,-0.032914277406352,
0.068846006509885));
#79825=CARTESIAN_POINT('Ctrl Pts',(0.0108565561439731,-0.0328043479726691,
0.0688078294385581));
#79826=CARTESIAN_POINT('Ctrl Pts',(0.0107824154971443,-0.0326943950436593,
0.0687711833127828));
#79827=CARTESIAN_POINT('Ctrl Pts',(0.0108958398939461,-0.0330240426238172,
0.0689240607774371));
#79828=CARTESIAN_POINT('Ctrl Pts',(0.0108238474897694,-0.032914277406352,
0.0688858729819231));
#79829=CARTESIAN_POINT('Ctrl Pts',(0.010751029746348,-0.0328043479726691,
0.0688491544324955));
#79830=CARTESIAN_POINT('Ctrl Pts',(0.0106774786531833,-0.0326943950436593,
0.0688139547374019));
#79831=CARTESIAN_POINT('Ctrl Pts',(0.0107892249372137,-0.0330240426238172,
0.0689624585245763));
#79832=CARTESIAN_POINT('Ctrl Pts',(0.010717761499413,-0.032914277406352,
0.0689257394539612));
#79833=CARTESIAN_POINT('Ctrl Pts',(0.0106455033487229,-0.0328043479726691,
0.0688904794264329));
#79834=CARTESIAN_POINT('Ctrl Pts',(0.0105725418092224,-0.0326943950436593,
0.0688567261620209));
#79835=CARTESIAN_POINT('Ctrl Pts',(0.0106826099804813,-0.0330240426238172,
0.0690008562717155));
#79836=CARTESIAN_POINT('Ctrl Pts',(0.0106116755090565,-0.032914277406352,
0.0689656059259994));
#79837=CARTESIAN_POINT('Ctrl Pts',(0.0105399769510978,-0.0328043479726691,
0.0689318044203703));
#79838=CARTESIAN_POINT('Ctrl Pts',(0.0104676049652615,-0.0326943950436593,
0.06889949758664));
#79839=CARTESIAN_POINT('',(0.0106259491549698,-0.0326943950436694,0.0688349577518512));
#79840=CARTESIAN_POINT('Ctrl Pts',(0.0107938986786009,-0.0327114338383348,
0.0687768744762708));
#79841=CARTESIAN_POINT('Ctrl Pts',(0.010774786747092,-0.0327619876830663,
0.0688153337747907));
#79842=CARTESIAN_POINT('Ctrl Pts',(0.010756011990653,-0.0328131562603672,
0.0688531145695884));
#79843=CARTESIAN_POINT('Ctrl Pts',(0.0107191210291131,-0.0329167375858782,
0.0689273509439647));
#79844=CARTESIAN_POINT('Ctrl Pts',(0.0107010195233077,-0.0329691088920629,
0.068963776943875));
#79845=CARTESIAN_POINT('Ctrl Pts',(0.0106832484016786,-0.0330220786163187,
0.0689995381055054));
#79846=CARTESIAN_POINT('Ctrl Pts',(0.0105713497540828,-0.0331951640388604,
0.0689470496783287));
#79847=CARTESIAN_POINT('Ctrl Pts',(0.0104637820920036,-0.0330306422010619,
0.0688964477882399));
#79848=CARTESIAN_POINT('Ctrl Pts',(0.0103542149164065,-0.0328657861914644,
0.0688503350217061));
#79849=CARTESIAN_POINT('Ctrl Pts',(0.0105707037120064,-0.0331951640388604,
0.0689451272752974));
#79850=CARTESIAN_POINT('Ctrl Pts',(0.010463096305477,-0.0330306422010619,
0.0688945387417142));
#79851=CARTESIAN_POINT('Ctrl Pts',(0.0103534899714295,-0.0328657861914644,
0.0688484409629531));
#79852=CARTESIAN_POINT('Ctrl Pts',(0.0104630557282946,-0.0331951640388604,
0.0686248032317774));
#79853=CARTESIAN_POINT('Ctrl Pts',(0.0103488258275382,-0.0330306422010619,
0.06857644025124));
#79854=CARTESIAN_POINT('Ctrl Pts',(0.0102326946425863,-0.0328657861914644,
0.0685328398384559));
#79855=CARTESIAN_POINT('',(0.0104512484729271,-0.0331781648281907,0.0686198191067445));
#79856=CARTESIAN_POINT('',(0.0104630557282936,-0.0331951640388588,0.0686248032317769));
#79857=CARTESIAN_POINT('Origin',(0.00470451661030899,-0.032641209230929,
0.0841105116536204));
#79858=CARTESIAN_POINT('Ctrl Pts',(0.0104512484738955,-0.033178164828644,
0.0686198191083014));
#79859=CARTESIAN_POINT('Ctrl Pts',(0.0104345749032635,-0.0331276811546787,
0.0686594364102444));
#79860=CARTESIAN_POINT('Ctrl Pts',(0.0104182024368507,-0.0330765663497806,
0.0686983383595207));
#79861=CARTESIAN_POINT('Ctrl Pts',(0.0103860454961961,-0.0329730614463516,
0.068774744913422));
#79862=CARTESIAN_POINT('Ctrl Pts',(0.0103702740077172,-0.0329207133374511,
0.0688122186493851));
#79863=CARTESIAN_POINT('Ctrl Pts',(0.010354797707384,-0.0328677532289362,
0.0688489911389325));
#79864=CARTESIAN_POINT('',(0.0105168797201585,-0.0331951640388701,0.0687849652535464));
#79865=CARTESIAN_POINT('Origin',(0.00812378219310841,-0.0315241814719618,
0.07415));
#79866=CARTESIAN_POINT('',(0.010451248471729,-0.0332121607144433,0.0686198191079238));
#79867=CARTESIAN_POINT('',(0.0104394305973826,-0.0331951640388587,0.0686148602124429));
#79868=CARTESIAN_POINT('Origin',(0.00474872370061134,-0.032641365599196,
0.0841206079314246));
#79869=CARTESIAN_POINT('Origin',(0.00339152961651254,-0.032641209865241,
0.0835579214911582));
#79870=CARTESIAN_POINT('Origin',(0.00335340817838117,-0.0326413662232479,
0.0835333653520963));
#79871=CARTESIAN_POINT('Ctrl Pts',(0.0105024210477226,-0.0337436976235975,
0.0689135697083491));
#79872=CARTESIAN_POINT('Ctrl Pts',(0.0104553238000768,-0.0336723290703325,
0.0688921758699981));
#79873=CARTESIAN_POINT('Ctrl Pts',(0.010407849363936,-0.033601104548885,
0.0688716326237038));
#79874=CARTESIAN_POINT('Ctrl Pts',(0.0102562728934941,-0.0333736987606857,
0.0688060421076739));
#79875=CARTESIAN_POINT('Ctrl Pts',(0.0101011822470827,-0.0331450831799191,
0.0687492580114819));
#79876=CARTESIAN_POINT('Ctrl Pts',(0.010272610530698,-0.0337436976235975,
0.0688151465085186));
#79877=CARTESIAN_POINT('Ctrl Pts',(0.0102246280498765,-0.0336723290703325,
0.0687958196207865));
#79878=CARTESIAN_POINT('Ctrl Pts',(0.0101763057016965,-0.033601104548885,
0.0687773589132818));
#79879=CARTESIAN_POINT('Ctrl Pts',(0.0100220220160757,-0.0333736987606857,
0.0687184175310795));
#79880=CARTESIAN_POINT('Ctrl Pts',(0.00986461018139935,-0.0331450831799191,
0.0686684269670849));
#79881=CARTESIAN_POINT('Ctrl Pts',(0.0102703124255278,-0.0337436976235975,
0.0688141622765203));
#79882=CARTESIAN_POINT('Ctrl Pts',(0.0102223210923745,-0.0336723290703325,
0.0687948560582944));
#79883=CARTESIAN_POINT('Ctrl Pts',(0.0101739902650741,-0.033601104548885,
0.0687764161761776));
#79884=CARTESIAN_POINT('Ctrl Pts',(0.0100196795073015,-0.0333736987606857,
0.0687175412853135));
#79885=CARTESIAN_POINT('Ctrl Pts',(0.00986224446074252,-0.0331450831799191,
0.0686676186566409));
#79886=CARTESIAN_POINT('',(0.0102390586088509,-0.0336938721132548,0.068801754429254));
#79887=CARTESIAN_POINT('',(0.0100175421957065,-0.0333679869945434,0.0687193648573588));
#79888=CARTESIAN_POINT('Ctrl Pts',(0.0102390586088633,-0.0336938721132647,
0.0688017544292584));
#79889=CARTESIAN_POINT('Ctrl Pts',(0.0102181818974938,-0.0336629187933931,
0.0687934975131143));
#79890=CARTESIAN_POINT('Ctrl Pts',(0.0101972635154301,-0.0336319952301038,
0.0687853654792674));
#79891=CARTESIAN_POINT('Ctrl Pts',(0.0101763057017087,-0.0336011045488948,
0.0687773589132866));
#79892=CARTESIAN_POINT('Ctrl Pts',(0.0101237153757214,-0.0335235892595452,
0.068757267699548));
#79893=CARTESIAN_POINT('Ctrl Pts',(0.0100707832553676,-0.0334458668660367,
0.0687379309708968));
#79894=CARTESIAN_POINT('Ctrl Pts',(0.0100175421958193,-0.0333679869945383,
0.0687193648570566));
#79895=CARTESIAN_POINT('Ctrl Pts',(0.0100175004318051,-0.0333679692459107,
0.0687193495652948));
#79896=CARTESIAN_POINT('Ctrl Pts',(0.0100173567982299,-0.033339189537294,
0.0687197794573971));
#79897=CARTESIAN_POINT('Ctrl Pts',(0.0100172522176963,-0.0333104081058071,
0.0687201027115236));
#79898=CARTESIAN_POINT('Ctrl Pts',(0.0100171190569288,-0.0332532697893318,
0.0687205322986892));
#79899=CARTESIAN_POINT('Ctrl Pts',(0.0100170893695625,-0.0332249169603541,
0.068720641797861));
#79900=CARTESIAN_POINT('Ctrl Pts',(0.0100170946743579,-0.0331960985432907,
0.0687206475348756));
#79901=CARTESIAN_POINT('Ctrl Pts',(0.0100170947702574,-0.0331956312491536,
0.0687206475998321));
#79902=CARTESIAN_POINT('Ctrl Pts',(0.0100170948752981,-0.0331951640388592,
0.0687206476364617));
#79903=CARTESIAN_POINT('',(0.0101351242745059,-0.0331951640388587,0.0687618066078137));
#79904=CARTESIAN_POINT('',(0.0100761095749122,-0.0331951640388687,0.0687412271221477));
#79905=CARTESIAN_POINT('',(0.0103547977016224,-0.0335216366567721,0.068848991152983));
#79906=CARTESIAN_POINT('Origin',(0.00502759431603476,-0.0326434571528016,
0.0846284578461628));
#79907=CARTESIAN_POINT('',(0.0103542707108206,-0.0336938721132327,0.0688502433100797));
#79908=CARTESIAN_POINT('Origin',(0.0145904810943599,-0.0336938867896154,
0.0587847899417411));
#79909=CARTESIAN_POINT('',(0.0102966646598458,-0.0336938721132538,0.0688259988696769));
#79910=CARTESIAN_POINT('Ctrl Pts',(0.0106662231239361,-0.0335235895815172,
0.0687152972378179));
#79911=CARTESIAN_POINT('Ctrl Pts',(0.0105914037404695,-0.0334144449262749,
0.0686802955327995));
#79912=CARTESIAN_POINT('Ctrl Pts',(0.010515775289712,-0.0333049234473147,
0.0686467993272172));
#79913=CARTESIAN_POINT('Ctrl Pts',(0.0104394305973828,-0.0331951640388587,
0.0686148602124428));
#79914=CARTESIAN_POINT('Ctrl Pts',(0.0105622294213664,-0.0335235895815172,
0.0687603137049349));
#79915=CARTESIAN_POINT('Ctrl Pts',(0.010488029778199,-0.0334144449262748,
0.0687267436779772));
#79916=CARTESIAN_POINT('Ctrl Pts',(0.0104130513571384,-0.0333049234473147,
0.068694667991912));
#79917=CARTESIAN_POINT('Ctrl Pts',(0.0103373863172536,-0.0331951640388587,
0.0686641363464102));
#79918=CARTESIAN_POINT('Ctrl Pts',(0.0104582357187967,-0.0335235895815172,
0.068805330172052));
#79919=CARTESIAN_POINT('Ctrl Pts',(0.0103846558159284,-0.0334144449262748,
0.0687731918231549));
#79920=CARTESIAN_POINT('Ctrl Pts',(0.0103103274245648,-0.0333049234473147,
0.0687425366566068));
#79921=CARTESIAN_POINT('Ctrl Pts',(0.0102353420371244,-0.0331951640388587,
0.0687134124803776));
#79922=CARTESIAN_POINT('Ctrl Pts',(0.010354242016227,-0.0335235895815172,
0.0688503466391691));
#79923=CARTESIAN_POINT('Ctrl Pts',(0.0102812818536578,-0.0334144449262748,
0.0688196399683326));
#79924=CARTESIAN_POINT('Ctrl Pts',(0.0102076034919911,-0.0333049234473147,
0.0687904053213016));
#79925=CARTESIAN_POINT('Ctrl Pts',(0.0101332977569952,-0.0331951640388587,
0.0687626886143449));
#79926=CARTESIAN_POINT('',(0.0102872774359542,-0.0331951640388687,0.0686883334101383));
#79927=CARTESIAN_POINT('Ctrl Pts',(0.0104512484705087,-0.0332121607146001,
0.0686198191108072));
#79928=CARTESIAN_POINT('Ctrl Pts',(0.0104346029379576,-0.0332625444109475,
0.068659369761615));
#79929=CARTESIAN_POINT('Ctrl Pts',(0.010418244234053,-0.0333135300746226,
0.0686982388926455));
#79930=CARTESIAN_POINT('Ctrl Pts',(0.0103860874981719,-0.0334167203140633,
0.0687746449690538));
#79931=CARTESIAN_POINT('Ctrl Pts',(0.0103703019207934,-0.033468884758732,
0.068812152321659));
#79932=CARTESIAN_POINT('Ctrl Pts',(0.010354797701189,-0.0335216366562388,
0.0688489911535642));
#79933=CARTESIAN_POINT('Ctrl Pts',(0.010239435998588,-0.033693872113239,
0.0688026803298203));
#79934=CARTESIAN_POINT('Ctrl Pts',(0.0102081363621296,-0.0336474569764958,
0.0687902967060484));
#79935=CARTESIAN_POINT('Ctrl Pts',(0.0101766939043906,-0.033601104548885,
0.0687782803325739));
#79936=CARTESIAN_POINT('Ctrl Pts',(0.0100970888304696,-0.0334837508592656,
0.0687478576376741));
#79937=CARTESIAN_POINT('Ctrl Pts',(0.0100166172257038,-0.0333660264659097,
0.0687198071655686));
#79938=CARTESIAN_POINT('Ctrl Pts',(0.01023905860887,-0.033693872113239,
0.0688017544292617));
#79939=CARTESIAN_POINT('Ctrl Pts',(0.0102077535528084,-0.0336474569764958,
0.0687893730144771));
#79940=CARTESIAN_POINT('Ctrl Pts',(0.0101763057016965,-0.033601104548885,
0.0687773589132818));
#79941=CARTESIAN_POINT('Ctrl Pts',(0.0100966869729955,-0.0334837508592656,
0.0687469419712704));
#79942=CARTESIAN_POINT('Ctrl Pts',(0.0100162018899158,-0.0333660264659097,
0.0687188976541466));
#79943=CARTESIAN_POINT('Ctrl Pts',(0.0101107444374813,-0.033693872113239,
0.0684869441487776));
#79944=CARTESIAN_POINT('Ctrl Pts',(0.0100775966923829,-0.0336474569764958,
0.0684753137994173));
#79945=CARTESIAN_POINT('Ctrl Pts',(0.0100443150706655,-0.033601104548885,
0.0684640722831846));
#79946=CARTESIAN_POINT('Ctrl Pts',(0.00996005365640166,-0.0334837508592656,
0.06843561134867));
#79947=CARTESIAN_POINT('Ctrl Pts',(0.00987498588704208,-0.0333660264659097,
0.0684096597525077));
#79948=CARTESIAN_POINT('',(0.0100994128180023,-0.0336769361243753,0.068484588838047));
#79949=CARTESIAN_POINT('',(0.0101115097307497,-0.0336938721132327,0.0684888217448924));
#79950=CARTESIAN_POINT('Ctrl Pts',(0.010099412818002,-0.033676936124375,
0.0684845888380469));
#79951=CARTESIAN_POINT('Ctrl Pts',(0.0101014298746358,-0.0336797586670073,
0.0684852922219222));
#79952=CARTESIAN_POINT('Ctrl Pts',(0.0101034464793446,-0.0336825812712942,
0.0684859966563938));
#79953=CARTESIAN_POINT('Ctrl Pts',(0.0101074787891163,-0.0336882266087494,
0.0684874076274563));
#79954=CARTESIAN_POINT('Ctrl Pts',(0.0101094944941804,-0.033691049341922,
0.0684881141640662));
#79955=CARTESIAN_POINT('Ctrl Pts',(0.0101115097307509,-0.0336938721132301,
0.0684888217448993));
#79956=CARTESIAN_POINT('Ctrl Pts',(0.0100994128180023,-0.0336769361243754,
0.0684845888380471));
#79957=CARTESIAN_POINT('Ctrl Pts',(0.0100856121074421,-0.0336279018378428,
0.0685241644037756));
#79958=CARTESIAN_POINT('Ctrl Pts',(0.0100716128563743,-0.0335767825754274,
0.0685643093135892));
#79959=CARTESIAN_POINT('Ctrl Pts',(0.0100441823742831,-0.0334733171799184,
0.0686429702522584));
#79960=CARTESIAN_POINT('Ctrl Pts',(0.0100307327075941,-0.0334209631321928,
0.0686815391480939));
#79961=CARTESIAN_POINT('Ctrl Pts',(0.0100175422025775,-0.0333679869844681,
0.0687193648597483));
#79962=CARTESIAN_POINT('',(0.0101752841698103,-0.0336938721132538,0.0686452880870832));
#79963=CARTESIAN_POINT('Origin',(0.00812378219310841,-0.0315241814719618,
0.07415));
#79964=CARTESIAN_POINT('',(0.0100994128175795,-0.0337108120655561,0.0684845888392771));
#79965=CARTESIAN_POINT('',(0.0100873068912882,-0.0336938721132327,0.0684803817800796));
#79966=CARTESIAN_POINT('Origin',(0.00365684478420917,-0.0345562519868347,
0.0835654253639754));
#79967=CARTESIAN_POINT('Ctrl Pts',(0.0100873068912913,-0.0336938721132343,
0.0684803817800769));
#79968=CARTESIAN_POINT('Ctrl Pts',(0.0100893251502616,-0.0336910493167714,
0.0684810807515388));
#79969=CARTESIAN_POINT('Ctrl Pts',(0.0100913430998275,-0.0336882265961736,
0.068481780822788));
#79970=CARTESIAN_POINT('Ctrl Pts',(0.0100953784054197,-0.0336825812712429,
0.0684831831741107));
#79971=CARTESIAN_POINT('Ctrl Pts',(0.0100973957613872,-0.0336797586669816,
0.0684838854541783));
#79972=CARTESIAN_POINT('Ctrl Pts',(0.0100994128180026,-0.033676936124375,
0.0684845888380471));
#79973=CARTESIAN_POINT('Origin',(0.00576741051423809,-0.0345562518742467,
0.0843014157688912));
#79974=CARTESIAN_POINT('Ctrl Pts',(0.0101689774313362,-0.034243627687391,
0.0687745650001576));
#79975=CARTESIAN_POINT('Ctrl Pts',(0.0099662395581409,-0.033943005420181,
0.0686974291901479));
#79976=CARTESIAN_POINT('Ctrl Pts',(0.00975826745672531,-0.0336441434784052,
0.0686357835621895));
#79977=CARTESIAN_POINT('Ctrl Pts',(0.0099334411014061,-0.034243627687391,
0.0686907638230592));
#79978=CARTESIAN_POINT('Ctrl Pts',(0.00972754261471318,-0.033943005420181,
0.0686225114121775));
#79979=CARTESIAN_POINT('Ctrl Pts',(0.00951708801279247,-0.0336441434784052,
0.0685699620169003));
#79980=CARTESIAN_POINT('Ctrl Pts',(0.0099310857381068,-0.034243627687391,
0.0686899258112882));
#79981=CARTESIAN_POINT('Ctrl Pts',(0.0097251556452789,-0.033943005420181,
0.0686217622343978));
#79982=CARTESIAN_POINT('Ctrl Pts',(0.00951467621835315,-0.0336441434784052,
0.0685693038014475));
#79983=CARTESIAN_POINT('',(0.00989906547609107,-0.034193496108874,0.0686794886651097));
#79984=CARTESIAN_POINT('',(0.00967281289662403,-0.0338664212864422,0.0686111708017387));
#79985=CARTESIAN_POINT('Origin',(0.00425118061923489,-0.0345610720404941,
0.0844324103120104));
#79986=CARTESIAN_POINT('Origin',(0.0126263498928281,-0.0336938005073008,
0.0580501413238942));
#79987=CARTESIAN_POINT('',(0.0097928278879358,-0.0336938721132327,0.0686461457624153));
#79988=CARTESIAN_POINT('',(0.0097326374437739,-0.0336938721132427,0.0686293124493113));
#79989=CARTESIAN_POINT('',(0.0100175422025825,-0.0340203938281605,0.06871936485975));
#79990=CARTESIAN_POINT('Origin',(0.00382868036302869,-0.0345589643244605,
0.0842021272954969));
#79991=CARTESIAN_POINT('',(0.0100170948752984,-0.034193496108874,0.0687206476364617));
#79992=CARTESIAN_POINT('Origin',(0.0136454885882588,-0.0341934220717668,
0.058315697980597));
#79993=CARTESIAN_POINT('',(0.00995808017570475,-0.0341934961088841,0.0687000681507957));
#79994=CARTESIAN_POINT('Ctrl Pts',(0.0103199609339328,-0.0340223579322396,
0.0685663811968963));
#79995=CARTESIAN_POINT('Ctrl Pts',(0.0102429482679489,-0.0339125849573575,
0.0685360901641857));
#79996=CARTESIAN_POINT('Ctrl Pts',(0.0101653627638831,-0.0338030433565231,
0.0685074143998663));
#79997=CARTESIAN_POINT('Ctrl Pts',(0.0100873068912889,-0.0336938721132327,
0.0684803817800792));
#79998=CARTESIAN_POINT('Ctrl Pts',(0.0102189989941991,-0.0340223579322396,
0.0686178386215836));
#79999=CARTESIAN_POINT('Ctrl Pts',(0.0101426960603082,-0.0339125849573575,
0.0685889401173418));
#80000=CARTESIAN_POINT('Ctrl Pts',(0.0100658486117185,-0.0338030433565231,
0.0685616412131723));
#80001=CARTESIAN_POINT('Ctrl Pts',(0.00998855801804967,-0.0336938721132327,
0.0685359681081126));
#80002=CARTESIAN_POINT('Ctrl Pts',(0.0101180370544654,-0.0340223579322396,
0.068669296046271));
#80003=CARTESIAN_POINT('Ctrl Pts',(0.0100424438526675,-0.0339125849573575,
0.0686417900704979));
#80004=CARTESIAN_POINT('Ctrl Pts',(0.00996633445955384,-0.0338030433565231,
0.0686158680264783));
#80005=CARTESIAN_POINT('Ctrl Pts',(0.00988980914481046,-0.0336938721132327,
0.068591554436146));
#80006=CARTESIAN_POINT('Ctrl Pts',(0.0100170751147317,-0.0340223579322396,
0.0687207534709584));
#80007=CARTESIAN_POINT('Ctrl Pts',(0.00994219164502685,-0.0339125849573575,
0.068694640023654));
#80008=CARTESIAN_POINT('Ctrl Pts',(0.0098668203073892,-0.0338030433565231,
0.0686700948397844));
#80009=CARTESIAN_POINT('Ctrl Pts',(0.00979106027157125,-0.0336938721132327,
0.0686471407641794));
#80010=CARTESIAN_POINT('',(0.00994006738962203,-0.0336938721132427,0.0685632637712574));
#80011=CARTESIAN_POINT('Ctrl Pts',(0.0100994128163883,-0.0337108120662709,
0.0684845888426755));
#80012=CARTESIAN_POINT('Ctrl Pts',(0.0100852543751759,-0.0337611408994033,
0.0685251902536224));
#80013=CARTESIAN_POINT('Ctrl Pts',(0.0100713542941038,-0.0338121088780741,
0.0685650507788977));
#80014=CARTESIAN_POINT('Ctrl Pts',(0.0100440581894573,-0.0339153382773246,
0.0686433263704953));
#80015=CARTESIAN_POINT('Ctrl Pts',(0.01003067371383,-0.0339675558473111,
0.0686817083213825));
#80016=CARTESIAN_POINT('Ctrl Pts',(0.0100175422025644,-0.0340203938281304,
0.068719364859786));
#80017=CARTESIAN_POINT('Ctrl Pts',(0.00989994740545553,-0.0341934961088741,
0.0686813150228184));
#80018=CARTESIAN_POINT('Ctrl Pts',(0.00978688665184713,-0.0340287516182428,
0.0686445942063371));
#80019=CARTESIAN_POINT('Ctrl Pts',(0.00967240480728664,-0.0338644633275951,
0.0686125776538122));
#80020=CARTESIAN_POINT('Ctrl Pts',(0.00989906547609109,-0.0341934961088741,
0.0686794886651098));
#80021=CARTESIAN_POINT('Ctrl Pts',(0.00978596696397589,-0.0340287516182428,
0.0686427860818234));
#80022=CARTESIAN_POINT('Ctrl Pts',(0.0096714481467643,-0.0338644633275951,
0.068610789307501));
#80023=CARTESIAN_POINT('Ctrl Pts',(0.00975211908072102,-0.0341934961088741,
0.0683751823422345));
#80024=CARTESIAN_POINT('Ctrl Pts',(0.0096327292751165,-0.0340287516182428,
0.0683415177599062));
#80025=CARTESIAN_POINT('Ctrl Pts',(0.00951205010308995,-0.0338644633275951,
0.0683128164145612));
#80026=CARTESIAN_POINT('',(0.00973978025265297,-0.0341764758832392,0.0683717173604828));
#80027=CARTESIAN_POINT('',(0.00975211908072106,-0.034193496108874,0.0683751823422345));
#80028=CARTESIAN_POINT('Origin',(0.00478705626700944,-0.0345621026283397,
0.0841796852961523));
#80029=CARTESIAN_POINT('Ctrl Pts',(0.00973978025395748,-0.0341764758837484,
0.0683717173617427));
#80030=CARTESIAN_POINT('Ctrl Pts',(0.00972821931534931,-0.0341260050040601,
0.0684130555631635));
#80031=CARTESIAN_POINT('Ctrl Pts',(0.0097168593699231,-0.0340749269148501,
0.068453675219413));
#80032=CARTESIAN_POINT('Ctrl Pts',(0.00969453248471447,-0.0339715436306823,
0.0685335088728231));
#80033=CARTESIAN_POINT('Ctrl Pts',(0.00968357400950415,-0.0339192778238538,
0.0685726925812178));
#80034=CARTESIAN_POINT('Ctrl Pts',(0.00967281289844593,-0.0338664212856951,
0.0686111708012219));
#80035=CARTESIAN_POINT('',(0.00982559227841607,-0.0341934961088841,0.0685273355036821));
#80036=CARTESIAN_POINT('Origin',(0.00812378219310841,-0.0315241814719618,
0.07415));
#80037=CARTESIAN_POINT('',(0.00973978025164394,-0.0342105180190556,0.0683717173609663));
#80038=CARTESIAN_POINT('',(0.00972743405025934,-0.0341934961088739,0.0683682787406281));
#80039=CARTESIAN_POINT('Origin',(0.00482900654019169,-0.0345621712168763,
0.0841968505876941));
#80040=CARTESIAN_POINT('Origin',(0.00577340770126758,-0.0345621034657148,
0.084455537330222));
#80041=CARTESIAN_POINT('Origin',(0.00572863976026522,-0.0345621719545859,
0.0844484466111688));
#80042=CARTESIAN_POINT('Ctrl Pts',(0.00979427246813991,-0.0346945769586966,
0.0686465497645994));
#80043=CARTESIAN_POINT('Ctrl Pts',(0.00967900049949819,-0.0345275153362944,
0.068611560676961));
#80044=CARTESIAN_POINT('Ctrl Pts',(0.00956259834102009,-0.0343603235965185,
0.0685801877366656));
#80045=CARTESIAN_POINT('Ctrl Pts',(0.00944541163767919,-0.034193496108874,
0.068552518614256));
#80046=CARTESIAN_POINT('Ctrl Pts',(0.00971353701564637,-0.0346945769586966,
0.0686239706796645));
#80047=CARTESIAN_POINT('Ctrl Pts',(0.00959779211903051,-0.0345275153362944,
0.0685906726284033));
#80048=CARTESIAN_POINT('Ctrl Pts',(0.00948097009179245,-0.0343603235965185,
0.0685610060350233));
#80049=CARTESIAN_POINT('Ctrl Pts',(0.00936341774568531,-0.034193496108874,
0.0685350535049942));
#80050=CARTESIAN_POINT('Ctrl Pts',(0.00963280156315282,-0.0346945769586966,
0.0686013915947291));
#80051=CARTESIAN_POINT('Ctrl Pts',(0.00951658373856283,-0.0345275153362944,
0.0685697845798461));
#80052=CARTESIAN_POINT('Ctrl Pts',(0.00939934184256478,-0.0343603235965185,
0.0685418243333825));
#80053=CARTESIAN_POINT('Ctrl Pts',(0.00928142385369134,-0.034193496108874,
0.0685175883957352));
#80054=CARTESIAN_POINT('Ctrl Pts',(0.00955206611065928,-0.0346945769586966,
0.0685788125097948));
#80055=CARTESIAN_POINT('Ctrl Pts',(0.00943537535809516,-0.0345275153362944,
0.068548896531288));
#80056=CARTESIAN_POINT('Ctrl Pts',(0.00931771359333718,-0.0343603235965185,
0.0685226426317385));
#80057=CARTESIAN_POINT('Ctrl Pts',(0.00919942996169755,-0.034193496108874,
0.0685001232864705));
#80058=CARTESIAN_POINT('',(0.00955206611124268,-0.0346945769586966,0.068578812509958));
#80059=CARTESIAN_POINT('',(0.00932197027664225,-0.0343667727831454,0.068524835974231));
#80060=CARTESIAN_POINT('Origin',(0.00555408289492608,-0.034562645706327,
0.0849101742849005));
#80061=CARTESIAN_POINT('Origin',(0.011624481658412,-0.0341934771028874,
0.0577151599463111));
#80062=CARTESIAN_POINT('',(0.00944394454052274,-0.034193496108874,0.0685522061152209));
#80063=CARTESIAN_POINT('',(0.00938281589597739,-0.034193496108884,0.0685391854080754));
#80064=CARTESIAN_POINT('',(0.00967281289796297,-0.0345211942962692,0.0686111708028464));
#80065=CARTESIAN_POINT('Origin',(0.00509193409485608,-0.0345625596120452,
0.0847774743351235));
#80066=CARTESIAN_POINT('',(0.00967244699959198,-0.0346945769586885,0.0686124791361874));
#80067=CARTESIAN_POINT('Origin',(0.0126522315959922,-0.0346945685853837,
0.0579577431490891));
#80068=CARTESIAN_POINT('',(0.00961225655542733,-0.0346945769587026,0.0685956458230828));
#80069=CARTESIAN_POINT('Ctrl Pts',(0.00996502803560501,-0.0345231616327842,
0.0684394996937654));
#80070=CARTESIAN_POINT('Ctrl Pts',(0.00988631682862492,-0.0344132092796988,
0.0684141207120934));
#80071=CARTESIAN_POINT('Ctrl Pts',(0.00980708473856406,-0.0343032738558979,
0.06839037111909));
#80072=CARTESIAN_POINT('Ctrl Pts',(0.00972743405025934,-0.0341934961088739,
0.0683682787406281));
#80073=CARTESIAN_POINT('Ctrl Pts',(0.00986749653480353,-0.0345231616327842,
0.0684971949491148));
#80074=CARTESIAN_POINT('Ctrl Pts',(0.00978958057569002,-0.0344132092796988,
0.068473160301868));
#80075=CARTESIAN_POINT('Ctrl Pts',(0.00971117149896178,-0.0343032738558979,
0.0684507385248535));
#80076=CARTESIAN_POINT('Ctrl Pts',(0.0096323704915066,-0.0341934961088739,
0.0684299557698666));
#80077=CARTESIAN_POINT('Ctrl Pts',(0.00976996503400206,-0.0345231616327842,
0.0685548902044643));
#80078=CARTESIAN_POINT('Ctrl Pts',(0.00969284432275511,-0.0344132092796988,
0.0685321998916426));
#80079=CARTESIAN_POINT('Ctrl Pts',(0.0096152582593595,-0.0343032738558979,
0.0685111059306169));
#80080=CARTESIAN_POINT('Ctrl Pts',(0.00953730693275385,-0.0341934961088739,
0.0684916327991051));
#80081=CARTESIAN_POINT('Ctrl Pts',(0.00967243353320058,-0.0345231616327842,
0.0686125854598137));
#80082=CARTESIAN_POINT('Ctrl Pts',(0.00959610806982021,-0.0344132092796988,
0.0685912394814172));
#80083=CARTESIAN_POINT('Ctrl Pts',(0.00951934501975722,-0.0343032738558979,
0.0685714733363804));
#80084=CARTESIAN_POINT('Ctrl Pts',(0.00944224337400111,-0.0341934961088739,
0.0685533098283437));
#80085=CARTESIAN_POINT('',(0.00958568929540103,-0.0341934961088839,0.0684602424279345));
#80086=CARTESIAN_POINT('Ctrl Pts',(0.00973978025070836,-0.0342105180195413,
0.0683717173642896));
#80087=CARTESIAN_POINT('Ctrl Pts',(0.00972820630212458,-0.0342610556240955,
0.068413102034162));
#80088=CARTESIAN_POINT('Ctrl Pts',(0.0097168400420636,-0.0343122189869412,
0.0684537440775323));
#80089=CARTESIAN_POINT('Ctrl Pts',(0.00969451293551567,-0.0344158119695182,
0.0685335785373973));
#80090=CARTESIAN_POINT('Ctrl Pts',(0.00968356122100284,-0.034468199045008,
0.0685727383009274));
#80091=CARTESIAN_POINT('Ctrl Pts',(0.00967281289794548,-0.0345211942962497,
0.0686111708028684));
#80092=CARTESIAN_POINT('Ctrl Pts',(0.00955306073468827,-0.0346945769586932,
0.0685805794542282));
#80093=CARTESIAN_POINT('Ctrl Pts',(0.00943791690570001,-0.034529677707698,
0.068551030131706));
#80094=CARTESIAN_POINT('Ctrl Pts',(0.00932165016502144,-0.0343648066251421,
0.0685262650589709));
#80095=CARTESIAN_POINT('Ctrl Pts',(0.00955206611125146,-0.0346945769586932,
0.0685788125099604));
#80096=CARTESIAN_POINT('Ctrl Pts',(0.00943688575194071,-0.034529677707698,
0.0685492837505741));
#80097=CARTESIAN_POINT('Ctrl Pts',(0.00932058336204766,-0.0343648066251421,
0.0685245407332356));
#80098=CARTESIAN_POINT('Ctrl Pts',(0.0093863021289167,-0.0346945769586932,
0.0682843335066093));
#80099=CARTESIAN_POINT('Ctrl Pts',(0.00926503362457833,-0.034529677707698,
0.0682582318002669));
#80100=CARTESIAN_POINT('Ctrl Pts',(0.009142789935153,-0.0343648066251421,
0.0682371645362269));
#80101=CARTESIAN_POINT('',(0.00937377008064706,-0.0346775396664974,0.0682816501233835));
#80102=CARTESIAN_POINT('',(0.00938630212891341,-0.0346945769586885,0.0682843335066086));
#80103=CARTESIAN_POINT('Origin',(0.00606465087396489,-0.0345626617849754,
0.0845501050758799));
#80104=CARTESIAN_POINT('Ctrl Pts',(0.00937377008196102,-0.0346775396670097,
0.0682816501246353));
#80105=CARTESIAN_POINT('Ctrl Pts',(0.00936482055953663,-0.0346269749928194,
0.0683236657366887));
#80106=CARTESIAN_POINT('Ctrl Pts',(0.00935603012522731,-0.03457579028908,
0.0683649346450465));
#80107=CARTESIAN_POINT('Ctrl Pts',(0.00933876002482597,-0.0344721681087937,
0.0684460130058423));
#80108=CARTESIAN_POINT('Ctrl Pts',(0.00933028712391344,-0.0344197714289673,
0.06848579067057));
#80109=CARTESIAN_POINT('Ctrl Pts',(0.00932197027689282,-0.0343667727830624,
0.0685248359741716));
#80110=CARTESIAN_POINT('',(0.00946918412008804,-0.0346945769587026,0.0684315730082934));
#80111=CARTESIAN_POINT('Origin',(0.00812378219310841,-0.0315241814719618,
0.07415));
#80112=CARTESIAN_POINT('',(0.00937377007967882,-0.034711613648963,0.0682816501243834));
#80113=CARTESIAN_POINT('',(0.00936123232798914,-0.0346945769586885,0.0682789935135702));
#80114=CARTESIAN_POINT('Origin',(0.00610932057602584,-0.034562669183425,
0.084557708751051));
#80115=CARTESIAN_POINT('Origin',(0.00576591901831826,-0.0345626625264326,
0.0844864758811781));
#80116=CARTESIAN_POINT('Origin',(0.0057220288670672,-0.0345626698720476,
0.0844752120881819));
#80117=CARTESIAN_POINT('Ctrl Pts',(0.00948151976255504,-0.0352450361874068,
0.068561144006316));
#80118=CARTESIAN_POINT('Ctrl Pts',(0.00927073259989667,-0.0349452760959493,
0.0685099360936015));
#80119=CARTESIAN_POINT('Ctrl Pts',(0.00905668707186739,-0.034644428984174,
0.0684747510087387));
#80120=CARTESIAN_POINT('Ctrl Pts',(0.00947905351566946,-0.0352450361874068,
0.0685606024794936));
#80121=CARTESIAN_POINT('Ctrl Pts',(0.00926824592899184,-0.0349452760959493,
0.0685094875828067));
#80122=CARTESIAN_POINT('Ctrl Pts',(0.00905418704131359,-0.034644428984174,
0.0684743967881435));
#80123=CARTESIAN_POINT('Ctrl Pts',(0.00923487065571117,-0.0352450361874068,
0.0685069859624248));
#80124=CARTESIAN_POINT('Ctrl Pts',(0.00902204088890987,-0.0349452760959493,
0.0684650805734222));
#80125=CARTESIAN_POINT('Ctrl Pts',(0.00880665926370981,-0.034644428984174,
0.0684393254420825));
#80126=CARTESIAN_POINT('Ctrl Pts',(0.00923242882711158,-0.0352450361874068,
0.0685064497972541));
#80127=CARTESIAN_POINT('Ctrl Pts',(0.00901957883850905,-0.0349452760959493,
0.0684646365033283));
#80128=CARTESIAN_POINT('Ctrl Pts',(0.00880418398593377,-0.034644428984174,
0.0684389747286218));
#80129=CARTESIAN_POINT('',(0.00919946219391866,-0.0351951634053319,0.0685001270068821));
#80130=CARTESIAN_POINT('',(0.00896639895473392,-0.0348678972925388,0.0684607010982874));
#80131=CARTESIAN_POINT('Origin',(0.00692987301931678,-0.0345636767880432,
0.0850908913454142));
#80132=CARTESIAN_POINT('Origin',(0.0105852836484402,-0.0346946199340767,
0.0575300926224854));
#80133=CARTESIAN_POINT('',(0.00908985113317312,-0.0346945769330288,0.0684803584062982));
#80134=CARTESIAN_POINT('',(0.00902802552651304,-0.0346945769458128,0.0684712016902573));
#80135=CARTESIAN_POINT('',(0.00932197027684797,-0.0350221583435276,0.0685248359743039));
#80136=CARTESIAN_POINT('Origin',(0.0064499830532711,-0.0345628458717242,
0.0850617534996283));
#80137=CARTESIAN_POINT('',(0.00932171555320903,-0.035195136029876,0.0685260463497064));
#80138=CARTESIAN_POINT('Origin',(0.0116173115732708,-0.035195183836691,
0.0577488443566961));
#80139=CARTESIAN_POINT('',(0.00919942996232486,-0.0351951371328749,0.0685001232864853));
#80140=CARTESIAN_POINT('Ctrl Pts',(0.00960282854545952,-0.0350241211494342,
0.0683351550418249));
#80141=CARTESIAN_POINT('Ctrl Pts',(0.00952273144033991,-0.0349144232818961,
0.0683147817847539));
#80142=CARTESIAN_POINT('Ctrl Pts',(0.0094421652634605,-0.0348045283579412,
0.0682960519977036));
#80143=CARTESIAN_POINT('Ctrl Pts',(0.00936123231711517,-0.0346945769439157,
0.0682789935112782));
#80144=CARTESIAN_POINT('Ctrl Pts',(0.00950911220538419,-0.0350241211494342,
0.0683988605314295));
#80145=CARTESIAN_POINT('Ctrl Pts',(0.00942989261726361,-0.0349144232818961,
0.0683797781785178));
#80146=CARTESIAN_POINT('Ctrl Pts',(0.00935023116653086,-0.0348045283579412,
0.0683623219293919));
#80147=CARTESIAN_POINT('Ctrl Pts',(0.00927022905734283,-0.0346945769439157,
0.0683465179402924));
#80148=CARTESIAN_POINT('Ctrl Pts',(0.00941539586530886,-0.0350241211494342,
0.0684625660210341));
#80149=CARTESIAN_POINT('Ctrl Pts',(0.00933705379418732,-0.0349144232818961,
0.0684447745722818));
#80150=CARTESIAN_POINT('Ctrl Pts',(0.00925829706960123,-0.0348045283579412,
0.0684285918610801));
#80151=CARTESIAN_POINT('Ctrl Pts',(0.00917922579757049,-0.0346945769439157,
0.0684140423693066));
#80152=CARTESIAN_POINT('Ctrl Pts',(0.00932167952523353,-0.0350241211494342,
0.0685262715106388));
#80153=CARTESIAN_POINT('Ctrl Pts',(0.00924421497111102,-0.0349144232818961,
0.0685097709660457));
#80154=CARTESIAN_POINT('Ctrl Pts',(0.00916636297267159,-0.0348045283579412,
0.0684948617927684));
#80155=CARTESIAN_POINT('Ctrl Pts',(0.00908822253779814,-0.0346945769439157,
0.0684815667983207));
#80156=CARTESIAN_POINT('',(0.00922554173088876,-0.0346945769458128,0.0683796759599063));
#80157=CARTESIAN_POINT('Ctrl Pts',(0.00937377007898878,-0.0347116136492817,
0.0682816501275956));
#80158=CARTESIAN_POINT('Ctrl Pts',(0.00936482409802611,-0.0347621546531941,
0.0683236490516123));
#80159=CARTESIAN_POINT('Ctrl Pts',(0.00935603541158321,-0.0348133084096261,
0.0683649095210523));
#80160=CARTESIAN_POINT('Ctrl Pts',(0.00933876529295336,-0.0349168561544579,
0.0684459879855739));
#80161=CARTESIAN_POINT('Ctrl Pts',(0.00933029071096543,-0.0349692089015914,
0.0684857738208522));
#80162=CARTESIAN_POINT('Ctrl Pts',(0.0093219702768209,-0.0350221583434999,
0.0685248359743356));
#80163=CARTESIAN_POINT('Ctrl Pts',(0.00920022625217223,-0.0351951371254941,
0.0685013506178967));
#80164=CARTESIAN_POINT('Ctrl Pts',(0.0090834439702777,-0.0350307338980939,
0.068479095812359));
#80165=CARTESIAN_POINT('Ctrl Pts',(0.00896584166303073,-0.0348659306897793,
0.068461686761144));
#80166=CARTESIAN_POINT('Ctrl Pts',(0.00919942996230845,-0.0351951371254941,
0.0685001232866004));
#80167=CARTESIAN_POINT('Ctrl Pts',(0.00908262230610942,-0.0350307338980939,
0.068477884943856));
#80168=CARTESIAN_POINT('Ctrl Pts',(0.00896499532666516,-0.0348659306897793,
0.0684604933901143));
#80169=CARTESIAN_POINT('Ctrl Pts',(0.00906597095118402,-0.0351951371254941,
0.0682944212821137));
#80170=CARTESIAN_POINT('Ctrl Pts',(0.00894491053510396,-0.0350307338980939,
0.0682749421206894));
#80171=CARTESIAN_POINT('Ctrl Pts',(0.00882314846967821,-0.0348659306897793,
0.0682604831617183));
#80172=CARTESIAN_POINT('Origin',(0.00974555209516449,-0.0308609197410205,
0.0631999048410406));
#80173=CARTESIAN_POINT('',(0.00914124484255691,-0.0351951371254941,0.0684104418506048));
#80174=CARTESIAN_POINT('Origin',(0.00812218386499098,-0.0351840467441105,
0.0751271095618081));
#80175=CARTESIAN_POINT('Origin',(0.00908679811530163,-0.0352322614053928,
0.06222345922568));
#80176=CARTESIAN_POINT('',(0.00873162935605851,-0.0351951142564663,0.0684308797521022));
#80177=CARTESIAN_POINT('',(0.00860738789448549,-0.0351951372916787,0.0684203730029262));
#80178=CARTESIAN_POINT('Origin',(0.00781973432811109,-0.0352875126913164,
0.0743035585178548));
#80179=CARTESIAN_POINT('Origin',(0.0153410677464602,-0.0298325076523007,
0.0762008484880468));
#80180=CARTESIAN_POINT('Origin',(0.0119206263900213,-0.0338732385636012,
0.066677789022853));
#80181=CARTESIAN_POINT('Ctrl Pts',(0.0119774395667351,-0.0321934096636942,
0.0698806369805316));
#80182=CARTESIAN_POINT('Ctrl Pts',(0.0119010200018148,-0.0320508460844833,
0.0698116583487073));
#80183=CARTESIAN_POINT('Ctrl Pts',(0.0118228047377682,-0.0319086045664086,
0.0697447849699195));
#80184=CARTESIAN_POINT('Ctrl Pts',(0.0117429740399792,-0.0317669892869414,
0.0696801469696607));
#80185=CARTESIAN_POINT('Ctrl Pts',(0.0119139908020065,-0.0321934096636942,
0.0698258219562938));
#80186=CARTESIAN_POINT('Ctrl Pts',(0.011836590074256,-0.0320508460844833,
0.069757979027143));
#80187=CARTESIAN_POINT('Ctrl Pts',(0.0117574249012691,-0.0319086045664086,
0.0696922668566142));
#80188=CARTESIAN_POINT('Ctrl Pts',(0.0116766773879117,-0.0317669892869414,
0.0696288129015313));
#80189=CARTESIAN_POINT('Ctrl Pts',(0.0118505420372779,-0.0321934096636942,
0.0697710069320561));
#80190=CARTESIAN_POINT('Ctrl Pts',(0.0117721601466973,-0.0320508460844833,
0.0697042997055786));
#80191=CARTESIAN_POINT('Ctrl Pts',(0.0116920450647701,-0.0319086045664086,
0.0696397487433092));
#80192=CARTESIAN_POINT('Ctrl Pts',(0.0116103807358444,-0.0317669892869414,
0.0695774788334018));
#80193=CARTESIAN_POINT('Ctrl Pts',(0.0117870932725493,-0.0321934096636942,
0.0697161919078182));
#80194=CARTESIAN_POINT('Ctrl Pts',(0.0117077302191384,-0.0320508460844833,
0.0696506203840143));
#80195=CARTESIAN_POINT('Ctrl Pts',(0.011626665228271,-0.0319086045664086,
0.069587230630004));
#80196=CARTESIAN_POINT('Ctrl Pts',(0.0115440840837769,-0.0317669892869414,
0.0695261447652723));
#80197=CARTESIAN_POINT('',(0.011788228383487,-0.0321934096636942,0.0697171725594356));
#80198=CARTESIAN_POINT('',(0.0116030135384361,-0.0318665617511301,0.069570363089195));
#80199=CARTESIAN_POINT('Origin',(0.000674913735238927,-0.0326371944422868,
0.0821956397080663));
#80200=CARTESIAN_POINT('Origin',(0.018233881790812,-0.031693926150954,0.0608422947860181));
#80201=CARTESIAN_POINT('',(0.0118834754864822,-0.0320197221621852,0.0697977252492182));
#80202=CARTESIAN_POINT('Ctrl Pts',(0.0118833709835563,-0.0320197392094763,
0.0697975726254411));
#80203=CARTESIAN_POINT('Ctrl Pts',(0.0118612244031211,-0.0319792716576062,
0.069778442664521));
#80204=CARTESIAN_POINT('Ctrl Pts',(0.0118388311639004,-0.0319386439829743,
0.0697593944533535));
#80205=CARTESIAN_POINT('Ctrl Pts',(0.0118161622773984,-0.0318979099381674,
0.0697404144370541));
#80206=CARTESIAN_POINT('Ctrl Pts',(0.0117934938389622,-0.0318571766984966,
0.0697214347959076));
#80207=CARTESIAN_POINT('Ctrl Pts',(0.0117706661237289,-0.0318163871833605,
0.0697026184477855));
#80208=CARTESIAN_POINT('Ctrl Pts',(0.0117477598892644,-0.0317755399638303,
0.0696840273960825));
#80209=CARTESIAN_POINT('',(0.0118828177156378,-0.0321934096636183,0.0697988907230038));
#80210=CARTESIAN_POINT('Origin',(0.013336754182227,-0.0324029947590523,
0.0680846214846591));
#80211=CARTESIAN_POINT('',(0.0118355230495724,-0.0321934096636663,0.0697580316412297));
#80212=CARTESIAN_POINT('Ctrl Pts',(0.0117883760591032,-0.0321934096636618,
0.0697191953988487));
#80213=CARTESIAN_POINT('Ctrl Pts',(0.0117272718104862,-0.0320835708272592,
0.0696686577934193));
#80214=CARTESIAN_POINT('Ctrl Pts',(0.0116651571316989,-0.0319739230346488,
0.0696194140511041));
#80215=CARTESIAN_POINT('Ctrl Pts',(0.0116021163295406,-0.0318646057455573,
0.0695715210766456));
#80216=CARTESIAN_POINT('Ctrl Pts',(0.0117801252758827,-0.0321934096636618,
0.069606177305869));
#80217=CARTESIAN_POINT('Ctrl Pts',(0.0117174624196823,-0.0320835708272592,
0.0695557534851704));
#80218=CARTESIAN_POINT('Ctrl Pts',(0.0116537923921365,-0.0319739230346488,
0.0695066557168894));
#80219=CARTESIAN_POINT('Ctrl Pts',(0.0115892014756718,-0.0318646057455573,
0.0694589405662804));
#80220=CARTESIAN_POINT('Ctrl Pts',(0.0117718744926621,-0.0321934096636618,
0.0694931592128893));
#80221=CARTESIAN_POINT('Ctrl Pts',(0.0117076530288784,-0.0320835708272592,
0.0694428491769216));
#80222=CARTESIAN_POINT('Ctrl Pts',(0.0116424276525741,-0.0319739230346488,
0.0693938973826746));
#80223=CARTESIAN_POINT('Ctrl Pts',(0.0115762866218029,-0.0318646057455573,
0.0693463600559153));
#80224=CARTESIAN_POINT('Ctrl Pts',(0.0117636237094416,-0.0321934096636618,
0.0693801411199095));
#80225=CARTESIAN_POINT('Ctrl Pts',(0.0116978436380745,-0.0320835708272592,
0.0693299448686727));
#80226=CARTESIAN_POINT('Ctrl Pts',(0.0116310629130117,-0.0319739230346488,
0.0692811390484598));
#80227=CARTESIAN_POINT('Ctrl Pts',(0.0115633717679341,-0.0318646057455573,
0.0692337795455501));
#80228=CARTESIAN_POINT('',(0.0117534269007546,-0.0321763980308461,0.0693723772361148));
#80229=CARTESIAN_POINT('',(0.0117636237094156,-0.0321934096636185,0.0693801411198898));
#80230=CARTESIAN_POINT('Origin',(0.00126142167047686,-0.0326386230766307,
0.0821686235382898));
#80231=CARTESIAN_POINT('Ctrl Pts',(0.0117534268988288,-0.0321763980306276,
0.0693723772386375));
#80232=CARTESIAN_POINT('Ctrl Pts',(0.0117274635097776,-0.0321259596174846,
0.0694065522856601));
#80233=CARTESIAN_POINT('Ctrl Pts',(0.0117019499701367,-0.0320749164631432,
0.0694401352056522));
#80234=CARTESIAN_POINT('Ctrl Pts',(0.0116518020571826,-0.0319716057793938,
0.0695061438180066));
#80235=CARTESIAN_POINT('Ctrl Pts',(0.011627187223183,-0.0319193786690137,
0.0695385437911935));
#80236=CARTESIAN_POINT('Ctrl Pts',(0.0116030135373063,-0.0318665617525335,
0.069570363090666));
#80237=CARTESIAN_POINT('',(0.0117759260464613,-0.0321934096636664,0.0695486568396727));
#80238=CARTESIAN_POINT('Origin',(0.00812378219310841,-0.0315241814719618,
0.07415));
#80239=CARTESIAN_POINT('',(0.0117534269009785,-0.0322104233323795,0.0693723772358195));
#80240=CARTESIAN_POINT('',(0.0117432135337924,-0.0321934096636183,0.0693646351476514));
#80241=CARTESIAN_POINT('Origin',(0.00129334652218236,-0.0326387238943641,
0.0822008092625748));
#80242=CARTESIAN_POINT('Origin',(0.00223844929347,-0.0326386239132421,0.0829108912217361));
#80243=CARTESIAN_POINT('Origin',(0.00219888526709953,-0.032638724647286,
0.0828887605941058));
#80244=CARTESIAN_POINT('Ctrl Pts',(0.0117299533201467,-0.0327445246967097,
0.0696696367555168));
#80245=CARTESIAN_POINT('Ctrl Pts',(0.0115609736579378,-0.032443687833936,
0.0695336277880152));
#80246=CARTESIAN_POINT('Ctrl Pts',(0.0113822292977948,-0.0321434074405927,
0.0694107334464117));
#80247=CARTESIAN_POINT('Ctrl Pts',(0.0115318400651885,-0.0327445246967097,
0.0695171535164056));
#80248=CARTESIAN_POINT('Ctrl Pts',(0.0113571094036004,-0.032443687833936,
0.0693886165124647));
#80249=CARTESIAN_POINT('Ctrl Pts',(0.0111731932008937,-0.0321434074405927,
0.0692736060961405));
#80250=CARTESIAN_POINT('',(0.0115026578980598,-0.0326943950436612,0.0694958272517568));
#80251=CARTESIAN_POINT('',(0.0113085902897616,-0.0323666188837389,0.069360937211991));
#80252=CARTESIAN_POINT('Origin',(0.00168797373835554,-0.0326395579111556,
0.0831442715978149));
#80253=CARTESIAN_POINT('Origin',(0.0174245285709706,-0.0321933825603032,
0.0601642709255512));
#80254=CARTESIAN_POINT('',(0.011411923476348,-0.0321934096532689,0.0694312870506711));
#80255=CARTESIAN_POINT('',(0.0113598807399114,-0.0321934096584275,0.0693966777465776));
#80256=CARTESIAN_POINT('',(0.0116030135390043,-0.032521010975624,0.0695703630884385));
#80257=CARTESIAN_POINT('Origin',(0.00131433280402838,-0.0326393129156693,
0.0828416548734633));
#80258=CARTESIAN_POINT('',(0.0116021917056727,-0.0326943950436593,0.0695714448498568));
#80259=CARTESIAN_POINT('Origin',(0.0182943225340461,-0.0326943765538181,
0.0607627388341716));
#80260=CARTESIAN_POINT('',(0.0115524248018762,-0.0326943950436702,0.0695336360508168));
#80261=CARTESIAN_POINT('Ctrl Pts',(0.0119379047672226,-0.032522978320377,
0.0695183189887841));
#80262=CARTESIAN_POINT('Ctrl Pts',(0.0118740571457712,-0.032413025309245,
0.0694657413925093));
#80263=CARTESIAN_POINT('Ctrl Pts',(0.0118091315729429,-0.032303122220807,
0.069414492540725));
#80264=CARTESIAN_POINT('Ctrl Pts',(0.0117432135302167,-0.0321934096576658,
0.0693646351449463));
#80265=CARTESIAN_POINT('Ctrl Pts',(0.011825983204065,-0.032522978320377,
0.0695360589419031));
#80266=CARTESIAN_POINT('Ctrl Pts',(0.0117623801274794,-0.032413025309245,
0.0694850241819289));
#80267=CARTESIAN_POINT('Ctrl Pts',(0.0116977309779776,-0.032303122220807,
0.0694353128737191));
#80268=CARTESIAN_POINT('Ctrl Pts',(0.0116321208134636,-0.0321934096576658,
0.0693869857717991));
#80269=CARTESIAN_POINT('Ctrl Pts',(0.0117140616409074,-0.032522978320377,
0.0695537988950221));
#80270=CARTESIAN_POINT('Ctrl Pts',(0.0116507031091875,-0.032413025309245,
0.0695043069713484));
#80271=CARTESIAN_POINT('Ctrl Pts',(0.0115863303830124,-0.032303122220807,
0.0694561332067131));
#80272=CARTESIAN_POINT('Ctrl Pts',(0.0115210280967104,-0.0321934096576658,
0.0694093363986518));
#80273=CARTESIAN_POINT('Ctrl Pts',(0.0116021400777498,-0.032522978320377,
0.069571538848141));
#80274=CARTESIAN_POINT('Ctrl Pts',(0.0115390260908957,-0.032413025309245,
0.069523589760768));
#80275=CARTESIAN_POINT('Ctrl Pts',(0.0114749297880471,-0.032303122220807,
0.0694769535397072));
#80276=CARTESIAN_POINT('Ctrl Pts',(0.0114099353799573,-0.0321934096576658,
0.0694316870255046));
#80277=CARTESIAN_POINT('',(0.0115775685055598,-0.0321934096584275,0.0693979610993311));
#80278=CARTESIAN_POINT('Ctrl Pts',(0.0117534268988682,-0.0322104233328948,
0.0693723772385859));
#80279=CARTESIAN_POINT('Ctrl Pts',(0.0117274283290297,-0.0322609421830896,
0.0694065985933172));
#80280=CARTESIAN_POINT('Ctrl Pts',(0.0117018976029963,-0.0323120888239738,
0.0694402041353746));
#80281=CARTESIAN_POINT('Ctrl Pts',(0.0116517493103102,-0.0324156524631823,
0.069506213247562));
#80282=CARTESIAN_POINT('Ctrl Pts',(0.0116271523573068,-0.0324680267167318,
0.0695385896843918));
#80283=CARTESIAN_POINT('Ctrl Pts',(0.0116030135389745,-0.0325210109755913,
0.0695703630884703));
#80284=CARTESIAN_POINT('Origin',(0.0137699112845517,-0.0262834582512301,
0.0796294718833777));
#80285=CARTESIAN_POINT('Origin',(0.0190328750298983,-0.0342770935979982,
0.0687819385306052));
#80286=CARTESIAN_POINT('Ctrl Pts',(0.0115029322307526,-0.0326943950436604,
0.0694978363392128));
#80287=CARTESIAN_POINT('Ctrl Pts',(0.011438816696423,-0.0325844576448134,
0.069451265318492));
#80288=CARTESIAN_POINT('Ctrl Pts',(0.0113737334594747,-0.0324744968375322,
0.0694060170162363));
#80289=CARTESIAN_POINT('Ctrl Pts',(0.0113077667079925,-0.0323646534831894,
0.0693621482570324));
#80290=CARTESIAN_POINT('Ctrl Pts',(0.0114876012859894,-0.0326943950436604,
0.0693855594951439));
#80291=CARTESIAN_POINT('Ctrl Pts',(0.0114219383663192,-0.0325844576448134,
0.0693391997635751));
#80292=CARTESIAN_POINT('Ctrl Pts',(0.0113553120043256,-0.0324744968375322,
0.0692941947678907));
#80293=CARTESIAN_POINT('Ctrl Pts',(0.0112878083609354,-0.0323646534831894,
0.0692506009936677));
#80294=CARTESIAN_POINT('Ctrl Pts',(0.0114722703412261,-0.0326943950436604,
0.069273282651075));
#80295=CARTESIAN_POINT('Ctrl Pts',(0.0114050600362155,-0.0325844576448134,
0.0692271342086583));
#80296=CARTESIAN_POINT('Ctrl Pts',(0.0113368905491766,-0.0324744968375322,
0.0691823725195451));
#80297=CARTESIAN_POINT('Ctrl Pts',(0.0112678500138783,-0.0323646534831894,
0.069139053730303));
#80298=CARTESIAN_POINT('Ctrl Pts',(0.0114569393964629,-0.0326943950436604,
0.0691610058070061));
#80299=CARTESIAN_POINT('Ctrl Pts',(0.0113881817061117,-0.0325844576448134,
0.0691150686537415));
#80300=CARTESIAN_POINT('Ctrl Pts',(0.0113184690940275,-0.0324744968375322,
0.0690705502711994));
#80301=CARTESIAN_POINT('Ctrl Pts',(0.0112478916668211,-0.0323646534831894,
0.0690275064669383));
#80302=CARTESIAN_POINT('',(0.0114462752106906,-0.0326773559991343,0.0691538975062259));
#80303=CARTESIAN_POINT('',(0.0114569393964622,-0.0326943950436595,0.0691610058070057));
#80304=CARTESIAN_POINT('Origin',(0.00229303105636561,-0.032639567058775,
0.0830085512661952));
#80305=CARTESIAN_POINT('Ctrl Pts',(0.0114462752088285,-0.032677355998742,
0.0691538975090129));
#80306=CARTESIAN_POINT('Ctrl Pts',(0.0114224897960546,-0.0326267922585966,
0.0691896641334863));
#80307=CARTESIAN_POINT('Ctrl Pts',(0.0113991259625462,-0.0325756109579332,
0.0692247968203686));
#80308=CARTESIAN_POINT('Ctrl Pts',(0.0113532215702813,-0.032471998546237,
0.0692938242186076));
#80309=CARTESIAN_POINT('Ctrl Pts',(0.0113306994225228,-0.0324196091621781,
0.0693276912449599));
#80310=CARTESIAN_POINT('Ctrl Pts',(0.0113085902897346,-0.0323666188837756,
0.0693609372120315));
#80311=CARTESIAN_POINT('',(0.011479798647271,-0.0326943950436703,0.0693284165293912));
#80312=CARTESIAN_POINT('Origin',(0.00812378219310841,-0.0315241814719618,
0.07415));
#80313=CARTESIAN_POINT('',(0.0114462752106653,-0.0327114338379885,0.0691538975062631));
#80314=CARTESIAN_POINT('',(0.0114355958676051,-0.0326943950436593,0.0691468119977928));
#80315=CARTESIAN_POINT('Origin',(0.0023311841216073,-0.0326395674607007,
0.0830329919927061));
#80316=CARTESIAN_POINT('Origin',(0.00220936153178273,-0.0326395675911541,
0.0829529113907568));
#80317=CARTESIAN_POINT('Origin',(0.00217206945053782,-0.0326395680949288,
0.0829271762291045));
#80318=CARTESIAN_POINT('Ctrl Pts',(0.0114414809896982,-0.0332451089994433,
0.0694520217438662));
#80319=CARTESIAN_POINT('Ctrl Pts',(0.0112642938408344,-0.0329451141710254,
0.0693268926865341));
#80320=CARTESIAN_POINT('Ctrl Pts',(0.0110781848298304,-0.0326442513127493,
0.0692154655680471));
#80321=CARTESIAN_POINT('Ctrl Pts',(0.0112341832111637,-0.0332451089994433,
0.0693122804435478));
#80322=CARTESIAN_POINT('Ctrl Pts',(0.0110517256329297,-0.0329451141710254,
0.0691949697498483));
#80323=CARTESIAN_POINT('Ctrl Pts',(0.0108609500763995,-0.0326442513127493,
0.0690917357741336));
#80324=CARTESIAN_POINT('Ctrl Pts',(0.0112321102333783,-0.0332451089994433,
0.0693108830305446));
#80325=CARTESIAN_POINT('Ctrl Pts',(0.0110495999508507,-0.0329451141710254,
0.0691936505204814));
#80326=CARTESIAN_POINT('Ctrl Pts',(0.0108587777288652,-0.0326442513127493,
0.0690904984761945));
#80327=CARTESIAN_POINT('',(0.0112037525338448,-0.0331951640388616,0.0692928498375915));
#80328=CARTESIAN_POINT('',(0.0110015980489326,-0.0328677532355008,0.0691704115662241));
#80329=CARTESIAN_POINT('Origin',(0.0028842817016618,-0.0326402808280941,
0.0838468407867844));
#80330=CARTESIAN_POINT('Origin',(0.0165333618382668,-0.0326944278779039,
0.059597848045385));
#80331=CARTESIAN_POINT('',(0.0111091446375892,-0.0326943950436593,0.0692341342496886));
#80332=CARTESIAN_POINT('',(0.0110550314616524,-0.0326943950436693,0.0692028610313009));
#80333=CARTESIAN_POINT('',(0.011308590289764,-0.0330220786163545,0.0693609372119926));
#80334=CARTESIAN_POINT('Origin',(0.0024531833626679,-0.0326396682763794,
0.0836339866880716));
#80335=CARTESIAN_POINT('',(0.0113078380024956,-0.0331951640388587,0.0693620684421445));
#80336=CARTESIAN_POINT('Origin',(0.0174166038075984,-0.0331952026560207,
0.0601761906990763));
#80337=CARTESIAN_POINT('',(0.0112557952681802,-0.0331951640388701,0.069327459139878));
#80338=CARTESIAN_POINT('Ctrl Pts',(0.0116395520319408,-0.0330240426238172,
0.0692879672522316));
#80339=CARTESIAN_POINT('Ctrl Pts',(0.0115725727939913,-0.032914277406352,
0.0692395340974531));
#80340=CARTESIAN_POINT('Ctrl Pts',(0.0115045589158483,-0.0328043479726691,
0.0691924614449262));
#80341=CARTESIAN_POINT('Ctrl Pts',(0.0114355958676054,-0.0326943950436593,
0.0691468119977927));
#80342=CARTESIAN_POINT('Ctrl Pts',(0.011528965252176,-0.0330240426238172,
0.0693126998243922));
#80343=CARTESIAN_POINT('Ctrl Pts',(0.0114623267295038,-0.032914277406352,
0.0692657901102445));
#80344=CARTESIAN_POINT('Ctrl Pts',(0.0113946852302704,-0.0328043479726691,
0.0692202346143025));
#80345=CARTESIAN_POINT('Ctrl Pts',(0.0113261258010506,-0.0326943950436593,
0.0691760940829798));
#80346=CARTESIAN_POINT('Ctrl Pts',(0.0114183784724112,-0.0330240426238172,
0.0693374323965528));
#80347=CARTESIAN_POINT('Ctrl Pts',(0.0113520806650162,-0.032914277406352,
0.0692920461230358));
#80348=CARTESIAN_POINT('Ctrl Pts',(0.0112848115446925,-0.0328043479726691,
0.0692480077836788));
#80349=CARTESIAN_POINT('Ctrl Pts',(0.0112166557344957,-0.0326943950436593,
0.0692053761681669));
#80350=CARTESIAN_POINT('Ctrl Pts',(0.0113077916926463,-0.0330240426238172,
0.0693621649687135));
#80351=CARTESIAN_POINT('Ctrl Pts',(0.0112418346005287,-0.032914277406352,
0.0693183021358272));
#80352=CARTESIAN_POINT('Ctrl Pts',(0.0111749378591146,-0.0328043479726691,
0.0692757809530551));
#80353=CARTESIAN_POINT('Ctrl Pts',(0.0111071856679408,-0.0326943950436593,
0.069234658253354));
#80354=CARTESIAN_POINT('',(0.0112723702526072,-0.0326943950436693,0.0691904731237507));
#80355=CARTESIAN_POINT('Ctrl Pts',(0.0114462752088236,-0.0327114338383348,
0.0691538975090203));
#80356=CARTESIAN_POINT('Ctrl Pts',(0.0114224937523609,-0.0327619876830622,
0.0691896581843056));
#80357=CARTESIAN_POINT('Ctrl Pts',(0.011399131851307,-0.0328131562603595,
0.0692247879653157));
#80358=CARTESIAN_POINT('Ctrl Pts',(0.0113532275011655,-0.0329167375858782,
0.0692938153002127));
#80359=CARTESIAN_POINT('Ctrl Pts',(0.0113307033427855,-0.0329691088920628,
0.0693276853499788));
#80360=CARTESIAN_POINT('Ctrl Pts',(0.0113085902897355,-0.0330220786163187,
0.0693609372120307));
#80361=CARTESIAN_POINT('Ctrl Pts',(0.011204152540701,-0.0331951640388604,
0.0692948380524451));
#80362=CARTESIAN_POINT('Ctrl Pts',(0.0111037751802755,-0.0330306422010619,
0.0692311533704583));
#80363=CARTESIAN_POINT('Ctrl Pts',(0.0110008514367224,-0.0328657861914645,
0.0691716718084518));
#80364=CARTESIAN_POINT('Ctrl Pts',(0.0112037525338475,-0.0331951640388604,
0.0692928498375933));
#80365=CARTESIAN_POINT('Ctrl Pts',(0.0111033340683546,-0.0330306422010619,
0.0692291734254917));
#80366=CARTESIAN_POINT('Ctrl Pts',(0.0110003695966612,-0.0328657861914645,
0.0691697018252196));
#80367=CARTESIAN_POINT('Ctrl Pts',(0.0111371006348029,-0.0331951640388604,
0.0689615597749474));
#80368=CARTESIAN_POINT('Ctrl Pts',(0.0110298329596683,-0.0330306422010619,
0.0688992613481253));
#80369=CARTESIAN_POINT('Ctrl Pts',(0.0109200820845154,-0.0328657861914645,
0.0688414496406912));
#80370=CARTESIAN_POINT('',(0.0111260111596784,-0.0331781648281912,0.0689551351097334));
#80371=CARTESIAN_POINT('',(0.0111371006348019,-0.0331951640388588,0.0689615597749468));
#80372=CARTESIAN_POINT('Origin',(0.00348309549379353,-0.0326412092206366,
0.0836034223100902));
#80373=CARTESIAN_POINT('Ctrl Pts',(0.0111260111604432,-0.033178164828644,
0.0689551351114003));
#80374=CARTESIAN_POINT('Ctrl Pts',(0.0111045037013377,-0.0331276811546776,
0.0689923502665628));
#80375=CARTESIAN_POINT('Ctrl Pts',(0.0110833846296175,-0.0330765663497784,
0.0690288934481934));
#80376=CARTESIAN_POINT('Ctrl Pts',(0.0110419049755672,-0.0329730614463203,
0.0691006671802621));
#80377=CARTESIAN_POINT('Ctrl Pts',(0.0110215611454689,-0.0329207133373788,
0.0691358687330006));
#80378=CARTESIAN_POINT('Ctrl Pts',(0.0110015980653927,-0.0328677532289366,
0.0691704115656726));
#80379=CARTESIAN_POINT('',(0.0111704265843334,-0.0331951640388702,0.0691272048062792));
#80380=CARTESIAN_POINT('Origin',(0.00812378219310841,-0.0315241814719618,
0.07415));
#80381=CARTESIAN_POINT('',(0.0111260111583418,-0.0332121607144241,0.0689551351107534));
#80382=CARTESIAN_POINT('',(0.0111149079858691,-0.0331951640388587,0.0689487341452396));
#80383=CARTESIAN_POINT('Origin',(0.00352568836954617,-0.0326413657536576,
0.0836189795529282));
#80384=CARTESIAN_POINT('Origin',(0.00224971951351425,-0.0326412097728248,
0.0828906286422365));
#80385=CARTESIAN_POINT('Origin',(0.00221497665047648,-0.0326413663048814,
0.0828614882365986));
#80386=CARTESIAN_POINT('Ctrl Pts',(0.0111399635106757,-0.0337436976235975,
0.0692529830243751));
#80387=CARTESIAN_POINT('Ctrl Pts',(0.0110959189978337,-0.0336723290703325,
0.0692258550324901));
#80388=CARTESIAN_POINT('Ctrl Pts',(0.0110513936632877,-0.033601104548885,
0.0691995236512357));
#80389=CARTESIAN_POINT('Ctrl Pts',(0.0109092330900541,-0.0333736987606857,
0.069115452766843));
#80390=CARTESIAN_POINT('Ctrl Pts',(0.0107624823141038,-0.0331450831799192,
0.0690396784179996));
#80391=CARTESIAN_POINT('Ctrl Pts',(0.0109243008161114,-0.0337436976235975,
0.0691265330256671));
#80392=CARTESIAN_POINT('Ctrl Pts',(0.010879118992817,-0.0336723290703325,
0.0691013447367416));
#80393=CARTESIAN_POINT('Ctrl Pts',(0.0108334914209511,-0.033601104548885,
0.0690769732012787));
#80394=CARTESIAN_POINT('Ctrl Pts',(0.0106878116222958,-0.0333736987606857,
0.0689991597162749));
#80395=CARTESIAN_POINT('Ctrl Pts',(0.0105379065059857,-0.0331450831799192,
0.0689298344085676));
#80396=CARTESIAN_POINT('Ctrl Pts',(0.0109221441891658,-0.0337436976235975,
0.06912526852568));
#80397=CARTESIAN_POINT('Ctrl Pts',(0.0108769509927668,-0.0336723290703325,
0.0691000996337841));
#80398=CARTESIAN_POINT('Ctrl Pts',(0.0108313123985277,-0.033601104548885,
0.0690757476967791));
#80399=CARTESIAN_POINT('Ctrl Pts',(0.0106855974076183,-0.0333736987606857,
0.0689979967857692));
#80400=CARTESIAN_POINT('Ctrl Pts',(0.0105356607479045,-0.0331450831799192,
0.0689287359684733));
#80401=CARTESIAN_POINT('',(0.0108926919337879,-0.0336938721132548,0.0691090413760902));
#80402=CARTESIAN_POINT('',(0.0106832483951838,-0.0333679869945434,0.0689995381022298));
#80403=CARTESIAN_POINT('Ctrl Pts',(0.0108926919338001,-0.0336938721132647,
0.0691090413760963));
#80404=CARTESIAN_POINT('Ctrl Pts',(0.010873014707535,-0.0336629187933931,
0.0690982330224601));
#80405=CARTESIAN_POINT('Ctrl Pts',(0.0108532804872594,-0.0336319952301038,
0.0690875433436641));
#80406=CARTESIAN_POINT('Ctrl Pts',(0.0108334914209631,-0.0336011045488948,
0.0690769732012853));
#80407=CARTESIAN_POINT('Ctrl Pts',(0.0107838338821881,-0.0335235892595452,
0.0690504490971577));
#80408=CARTESIAN_POINT('Ctrl Pts',(0.0107337426821419,-0.0334458668660368,
0.0690246306905843));
#80409=CARTESIAN_POINT('Ctrl Pts',(0.0106832483953328,-0.0333679869945383,
0.0689995381019455));
#80410=CARTESIAN_POINT('Ctrl Pts',(0.0106832088772076,-0.0333679692459107,
0.0689995176963455));
#80411=CARTESIAN_POINT('Ctrl Pts',(0.0106830124964596,-0.0333391895374034,
0.0689999261965583));
#80412=CARTESIAN_POINT('Ctrl Pts',(0.0106828682260881,-0.0333104081060166,
0.0690002337943113));
#80413=CARTESIAN_POINT('Ctrl Pts',(0.0106826822739281,-0.0332532698340219,
0.0690006433042667));
#80414=CARTESIAN_POINT('Ctrl Pts',(0.0106826390953484,-0.0332249171825216,
0.0690007482188445));
#80415=CARTESIAN_POINT('Ctrl Pts',(0.010682643640639,-0.0331960985342078,
0.069000754576199));
#80416=CARTESIAN_POINT('Ctrl Pts',(0.0106826437275517,-0.0331956312583094,
0.0690007546526169));
#80417=CARTESIAN_POINT('Ctrl Pts',(0.0106826438271752,-0.0331951640388587,
0.0690007547021237));
#80418=CARTESIAN_POINT('',(0.0107945839423478,-0.0331951640388587,0.0690563821289519));
#80419=CARTESIAN_POINT('',(0.0107386138847722,-0.0331951640388687,0.0690285684155481));
#80420=CARTESIAN_POINT('',(0.0110015980579165,-0.0335216366567716,0.0691704115788894));
#80421=CARTESIAN_POINT('Origin',(0.00373870967775345,-0.0326434571529732,
0.0841577768371651));
#80422=CARTESIAN_POINT('',(0.0110009182856956,-0.0336938721132327,0.0691715878128933));
#80423=CARTESIAN_POINT('Origin',(0.0164652605990008,-0.0336938867896302,
0.0597164414344764));
#80424=CARTESIAN_POINT('',(0.0109468051097517,-0.0336938721132538,0.0691403145945018));
#80425=CARTESIAN_POINT('Ctrl Pts',(0.0113273240884512,-0.0335235895815172,
0.0690768038353716));
#80426=CARTESIAN_POINT('Ctrl Pts',(0.011257481555041,-0.0334144449262749,
0.0690327007739887));
#80427=CARTESIAN_POINT('Ctrl Pts',(0.0111866476449646,-0.0333049234473147,
0.0689899899377093));
#80428=CARTESIAN_POINT('Ctrl Pts',(0.0111149079858693,-0.0331951640388587,
0.0689487341452395));
#80429=CARTESIAN_POINT('Ctrl Pts',(0.0112185083479003,-0.0335235895815172,
0.0691084314671863));
#80430=CARTESIAN_POINT('Ctrl Pts',(0.0111491012311111,-0.0334144449262749,
0.0690658264687105));
#80431=CARTESIAN_POINT('Ctrl Pts',(0.0110787341867489,-0.0333049234473147,
0.0690246064210513));
#80432=CARTESIAN_POINT('Ctrl Pts',(0.0110074924181604,-0.0331951640388587,
0.0689848321825771));
#80433=CARTESIAN_POINT('Ctrl Pts',(0.0111096926073494,-0.0335235895815172,
0.0691400590990009));
#80434=CARTESIAN_POINT('Ctrl Pts',(0.0110407209071812,-0.0334144449262749,
0.0690989521634323));
#80435=CARTESIAN_POINT('Ctrl Pts',(0.0109708207285332,-0.0333049234473147,
0.0690592229043934));
#80436=CARTESIAN_POINT('Ctrl Pts',(0.0109000768504515,-0.0331951640388587,
0.0690209302199148));
#80437=CARTESIAN_POINT('Ctrl Pts',(0.0110008768667985,-0.0335235895815172,
0.0691716867308156));
#80438=CARTESIAN_POINT('Ctrl Pts',(0.0109323405832513,-0.0334144449262749,
0.0691320778581541));
#80439=CARTESIAN_POINT('Ctrl Pts',(0.0108629072703175,-0.0333049234473147,
0.0690938393877355));
#80440=CARTESIAN_POINT('Ctrl Pts',(0.0107926612827427,-0.0331951640388587,
0.0690570282572524));
#80441=CARTESIAN_POINT('',(0.0109547459641184,-0.0331951640388687,0.0690025581371058));
#80442=CARTESIAN_POINT('Ctrl Pts',(0.0111260111567689,-0.0332121607146002,
0.0689551351134619));
#80443=CARTESIAN_POINT('Ctrl Pts',(0.01110453986826,-0.0332625444109438,
0.0689922876571531));
#80444=CARTESIAN_POINT('Ctrl Pts',(0.0110834385637455,-0.0333135300746151,
0.0690288000042159));
#80445=CARTESIAN_POINT('Ctrl Pts',(0.0110419591727085,-0.0334167203140627,
0.0691005732882063));
#80446=CARTESIAN_POINT('Ctrl Pts',(0.0110215971515384,-0.0334688847587306,
0.0691358064266762));
#80447=CARTESIAN_POINT('Ctrl Pts',(0.0110015980574129,-0.0335216366562379,
0.0691704115794121));
#80448=CARTESIAN_POINT('Ctrl Pts',(0.0108929503015822,-0.033693872113239,
0.0691100072751299));
#80449=CARTESIAN_POINT('Ctrl Pts',(0.0108634495517166,-0.0336474569764958,
0.0690937984152836));
#80450=CARTESIAN_POINT('Ctrl Pts',(0.0108337610780916,-0.033601104548885,
0.0690779360096034));
#80451=CARTESIAN_POINT('Ctrl Pts',(0.0107585966886809,-0.0334837508592656,
0.0690377760454171));
#80452=CARTESIAN_POINT('Ctrl Pts',(0.0106822752829264,-0.0333660264659097,
0.0689998609932269));
#80453=CARTESIAN_POINT('Ctrl Pts',(0.0108926919338059,-0.033693872113239,
0.0691090413761001));
#80454=CARTESIAN_POINT('Ctrl Pts',(0.0108631855302128,-0.0336474569764958,
0.0690928340285662));
#80455=CARTESIAN_POINT('Ctrl Pts',(0.0108334914209511,-0.033601104548885,
0.0690769732012787));
#80456=CARTESIAN_POINT('Ctrl Pts',(0.0107583127634042,-0.0334837508592656,
0.0690368172332199));
#80457=CARTESIAN_POINT('Ctrl Pts',(0.0106819772141925,-0.0333660264659097,
0.0689989065981968));
#80458=CARTESIAN_POINT('Ctrl Pts',(0.0108048457483965,-0.033693872113239,
0.0687806314386948));
#80459=CARTESIAN_POINT('Ctrl Pts',(0.0107734170524618,-0.0336474569764958,
0.0687649382840344));
#80460=CARTESIAN_POINT('Ctrl Pts',(0.010741806801852,-0.033601104548885,
0.0687496141172468));
#80461=CARTESIAN_POINT('Ctrl Pts',(0.0106617769149603,-0.0334837508592656,
0.0687108168501874));
#80462=CARTESIAN_POINT('Ctrl Pts',(0.0105806325278338,-0.0333660264659097,
0.0686744080715062));
#80463=CARTESIAN_POINT('',(0.0107938986808316,-0.0336769361243753,0.0687768744717819));
#80464=CARTESIAN_POINT('',(0.0108053696819065,-0.0336938721132327,0.0687825901460834));
#80465=CARTESIAN_POINT('Ctrl Pts',(0.0107938986808316,-0.0336769361243753,
0.0687768744717819));
#80466=CARTESIAN_POINT('Ctrl Pts',(0.0107958116749797,-0.0336797586669839,
0.0687778251134874));
#80467=CARTESIAN_POINT('Ctrl Pts',(0.0107977240890918,-0.0336825812712471,
0.0687787767408637));
#80468=CARTESIAN_POINT('Ctrl Pts',(0.0108015477607022,-0.0336882266077742,
0.0687806819681071));
#80469=CARTESIAN_POINT('Ctrl Pts',(0.0108034590181517,-0.0336910493399714,
0.0687816355679669));
#80470=CARTESIAN_POINT('Ctrl Pts',(0.0108053696819068,-0.0336938721132305,
0.0687825901460893));
#80471=CARTESIAN_POINT('Ctrl Pts',(0.0107938986808316,-0.0336769361243754,
0.068776874471782));
#80472=CARTESIAN_POINT('Ctrl Pts',(0.0107752466593742,-0.0336279018378449,
0.0688144082846725));
#80473=CARTESIAN_POINT('Ctrl Pts',(0.0107563263052245,-0.0335767825754299,
0.0688524820684775));
#80474=CARTESIAN_POINT('Ctrl Pts',(0.0107192532908787,-0.0334733171799203,
0.0689270847911321));
#80475=CARTESIAN_POINT('Ctrl Pts',(0.0107010757143986,-0.0334209631321945,
0.0689636638694876));
#80476=CARTESIAN_POINT('Ctrl Pts',(0.0106832484016998,-0.0333679869844681,
0.0689995381054628));
#80477=CARTESIAN_POINT('',(0.0108490308078572,-0.0336938721132538,0.0689458157610968));
#80478=CARTESIAN_POINT('Origin',(0.00812378219310841,-0.0315241814719618,
0.07415));
#80479=CARTESIAN_POINT('',(0.0107938986802588,-0.0337108120655415,0.0687768744729486));
#80480=CARTESIAN_POINT('',(0.0107824154971444,-0.0336938721132327,0.0687711833127828));
#80481=CARTESIAN_POINT('Origin',(0.00251200221662774,-0.0345562520221669,
0.0829313261019018));
#80482=CARTESIAN_POINT('Ctrl Pts',(0.0107824154971489,-0.0336938721132347,
0.0687711833127797));
#80483=CARTESIAN_POINT('Ctrl Pts',(0.0107843302391102,-0.0336910493139422,
0.0687721297285144));
#80484=CARTESIAN_POINT('Ctrl Pts',(0.0107862445333863,-0.0336882265947589,
0.0687730771951645));
#80485=CARTESIAN_POINT('Ctrl Pts',(0.0107900722571568,-0.0336825812713119,
0.0687749742459279));
#80486=CARTESIAN_POINT('Ctrl Pts',(0.0107919856866616,-0.0336797586670162,
0.0687759238300656));
#80487=CARTESIAN_POINT('Ctrl Pts',(0.0107938986808319,-0.033676936124375,
0.0687768744717821));
#80488=CARTESIAN_POINT('Origin',(0.00451368155345254,-0.0345562519193588,
0.0839260370577549));
#80489=CARTESIAN_POINT('Ctrl Pts',(0.0108265711063576,-0.034243627687391,
0.0690732828431734));
#80490=CARTESIAN_POINT('Ctrl Pts',(0.0106350995623394,-0.033943005420181,
0.0689713454788514));
#80491=CARTESIAN_POINT('Ctrl Pts',(0.0104364936289488,-0.0336441434784052,
0.0688841201291205));
#80492=CARTESIAN_POINT('Ctrl Pts',(0.0106033951232425,-0.034243627687391,
0.0689606219335347));
#80493=CARTESIAN_POINT('Ctrl Pts',(0.0104076745029704,-0.033943005420181,
0.0688671017901755));
#80494=CARTESIAN_POINT('Ctrl Pts',(0.0102054655840775,-0.0336441434784052,
0.0687885898067987));
#80495=CARTESIAN_POINT('Ctrl Pts',(0.0106011633634114,-0.034243627687391,
0.0689594953244383));
#80496=CARTESIAN_POINT('Ctrl Pts',(0.0104054002523767,-0.033943005420181,
0.0688660593532888));
#80497=CARTESIAN_POINT('Ctrl Pts',(0.0102031553036288,-0.0336441434784052,
0.0687876345035754));
#80498=CARTESIAN_POINT('',(0.0105707037120053,-0.0341934961088741,0.0689451272752967));
#80499=CARTESIAN_POINT('',(0.0103547976992636,-0.0338664212891259,0.0688489911502866));
#80500=CARTESIAN_POINT('Origin',(0.00299297806214719,-0.0345610818078395,
0.0838659572887302));
#80501=CARTESIAN_POINT('Origin',(0.0146086594711115,-0.0336938005044541,
0.0587413997481238));
#80502=CARTESIAN_POINT('',(0.0104694828127754,-0.0336938721132327,0.0688987321908995));
#80503=CARTESIAN_POINT('',(0.010411876761808,-0.0336938721132427,0.0688744877504997));
#80504=CARTESIAN_POINT('',(0.0106832484017046,-0.0340203938281605,0.0689995381054652));
#80505=CARTESIAN_POINT('Origin',(0.00260268290546713,-0.034558964324509,
0.0835845442688159));
#80506=CARTESIAN_POINT('',(0.0106826438271766,-0.034193496108874,0.0690007547021244));
#80507=CARTESIAN_POINT('Origin',(0.0155865124599212,-0.0341934220717751,
0.0591326094498503));
#80508=CARTESIAN_POINT('',(0.0106266737696009,-0.034193496108884,0.0689729409887205));
#80509=CARTESIAN_POINT('Ctrl Pts',(0.0110024564081781,-0.0340223579322397,
0.0688856638819777));
#80510=CARTESIAN_POINT('Ctrl Pts',(0.0109298474831456,-0.0339125849573575,
0.0688459594566543));
#80511=CARTESIAN_POINT('Ctrl Pts',(0.0108564677902201,-0.0338030433565231,
0.0688077857671993));
#80512=CARTESIAN_POINT('Ctrl Pts',(0.0107824154971451,-0.0336938721132326,
0.0687711833127826));
#80513=CARTESIAN_POINT('Ctrl Pts',(0.0108958412580681,-0.0340223579322397,
0.068924061663128));
#80514=CARTESIAN_POINT('Ctrl Pts',(0.0108237619385833,-0.0339125849573575,
0.0688858277387887));
#80515=CARTESIAN_POINT('Ctrl Pts',(0.0107509419150112,-0.0338030433565231,
0.0688491125554094));
#80516=CARTESIAN_POINT('Ctrl Pts',(0.0106774784740318,-0.0336938721132326,
0.0688139548104227));
#80517=CARTESIAN_POINT('Ctrl Pts',(0.0107892261079581,-0.0340223579322397,
0.0689624594442784));
#80518=CARTESIAN_POINT('Ctrl Pts',(0.010717676394021,-0.0339125849573575,
0.068925696020923));
#80519=CARTESIAN_POINT('Ctrl Pts',(0.0106454160398023,-0.0338030433565231,
0.0688904393436196));
#80520=CARTESIAN_POINT('Ctrl Pts',(0.0105725414509186,-0.0336938721132326,
0.0688567263080628));
#80521=CARTESIAN_POINT('Ctrl Pts',(0.0106826109578481,-0.0340223579322397,
0.0690008572254287));
#80522=CARTESIAN_POINT('Ctrl Pts',(0.0106115908494587,-0.0339125849573575,
0.0689655643030574));
#80523=CARTESIAN_POINT('Ctrl Pts',(0.0105398901645934,-0.0338030433565231,
0.0689317661318297));
#80524=CARTESIAN_POINT('Ctrl Pts',(0.0104676044278054,-0.0336938721132326,
0.0688994978057029));
#80525=CARTESIAN_POINT('',(0.0106259491549699,-0.0336938721132427,0.0688349577518512));
#80526=CARTESIAN_POINT('Ctrl Pts',(0.0107938986786503,-0.0337108120662711,
0.0687768744761719));
#80527=CARTESIAN_POINT('Ctrl Pts',(0.010774763174856,-0.0337611408993995,
0.0688153812096439));
#80528=CARTESIAN_POINT('Ctrl Pts',(0.0107559768515518,-0.0338121088780665,
0.0688531852806615));
#80529=CARTESIAN_POINT('Ctrl Pts',(0.0107190854518366,-0.0339153382773247,
0.068927422536786));
#80530=CARTESIAN_POINT('Ctrl Pts',(0.0107009959827818,-0.0339675558473121,
0.0689638243149171));
#80531=CARTESIAN_POINT('Ctrl Pts',(0.0106832484016821,-0.0340203938281304,
0.0689995381054985));
#80532=CARTESIAN_POINT('Ctrl Pts',(0.0105713497830771,-0.0341934961088741,
0.0689470497646084));
#80533=CARTESIAN_POINT('Ctrl Pts',(0.0104637828866879,-0.03402875161944,
0.0688964482332763));
#80534=CARTESIAN_POINT('Ctrl Pts',(0.0103542165044892,-0.033864463329982,
0.0688503357613862));
#80535=CARTESIAN_POINT('Ctrl Pts',(0.0105707037120054,-0.0341934961088741,
0.0689451272752969));
#80536=CARTESIAN_POINT('Ctrl Pts',(0.0104630970696646,-0.03402875161944,
0.0688945391009751));
#80537=CARTESIAN_POINT('Ctrl Pts',(0.0103534915275316,-0.033864463329982,
0.0688484416174124));
#80538=CARTESIAN_POINT('Ctrl Pts',(0.0104630557282936,-0.0341934961088741,
0.068624803231777));
#80539=CARTESIAN_POINT('Ctrl Pts',(0.0103488266387562,-0.03402875161944,
0.0685764405946958));
#80540=CARTESIAN_POINT('Ctrl Pts',(0.010232696291323,-0.033864463329982,
0.0685328404574597));
#80541=CARTESIAN_POINT('',(0.0104512484729383,-0.0341764758832396,0.0686198191072201));
#80542=CARTESIAN_POINT('',(0.0104630557282936,-0.034193496108874,0.068624803231777));
#80543=CARTESIAN_POINT('Origin',(0.00355631448922339,-0.0345621026280434,
0.0836823955081816));
#80544=CARTESIAN_POINT('Ctrl Pts',(0.0104512484740739,-0.0341764758837489,
0.0686198191086342));
#80545=CARTESIAN_POINT('Ctrl Pts',(0.0104345976465681,-0.0341260050043703,
0.068659382375928));
#80546=CARTESIAN_POINT('Ctrl Pts',(0.0104182362849394,-0.0340749269154777,
0.0686982579551276));
#80547=CARTESIAN_POINT('Ctrl Pts',(0.0103860796441643,-0.0339715436320037,
0.0687746637951318));
#80548=CARTESIAN_POINT('Ctrl Pts',(0.0103702965590176,-0.0339192778255033,
0.068812165066936));
#80549=CARTESIAN_POINT('Ctrl Pts',(0.0103547977028726,-0.0338664212876329,
0.0688489911496625));
#80550=CARTESIAN_POINT('',(0.0105168797201595,-0.0341934961088841,0.0687849652535469));
#80551=CARTESIAN_POINT('Origin',(0.00812378219310841,-0.0315241814719618,
0.07415));
#80552=CARTESIAN_POINT('',(0.0104512484718765,-0.0342105180190387,0.0686198191075735));
#80553=CARTESIAN_POINT('',(0.0104394305973826,-0.0341934961088739,0.0686148602124429));
#80554=CARTESIAN_POINT('Origin',(0.00359578260681611,-0.0345621712411221,
0.0837046830863977));
#80555=CARTESIAN_POINT('Origin',(0.00450031454071362,-0.0345621033373562,
0.0840796952059308));
#80556=CARTESIAN_POINT('Origin',(0.00445678854298556,-0.0345621719856087,
0.0840670494826787));
#80557=CARTESIAN_POINT('Ctrl Pts',(0.010470865367133,-0.0346945769586966,
0.0688993140613139));
#80558=CARTESIAN_POINT('Ctrl Pts',(0.0103608876478873,-0.0345275153362944,
0.0688501534645131));
#80559=CARTESIAN_POINT('Ctrl Pts',(0.01024933542725,-0.0343603235965185,
0.0688044388503067));
#80560=CARTESIAN_POINT('Ctrl Pts',(0.0101365406366484,-0.034193496108874,
0.0687623005187312));
#80561=CARTESIAN_POINT('Ctrl Pts',(0.0103935964475227,-0.0346945769586966,
0.0688667941838835));
#80562=CARTESIAN_POINT('Ctrl Pts',(0.0102829375864239,-0.0345275153362944,
0.0688192520155407));
#80563=CARTESIAN_POINT('Ctrl Pts',(0.0101707549458408,-0.0343603235965185,
0.0687751776696851));
#80564=CARTESIAN_POINT('Ctrl Pts',(0.0100573822496017,-0.034193496108874,
0.0687346965674563));
#80565=CARTESIAN_POINT('Ctrl Pts',(0.0103163275279121,-0.0346945769586966,
0.0688342743064553));
#80566=CARTESIAN_POINT('Ctrl Pts',(0.0102049875249603,-0.0345275153362944,
0.068788350566571));
#80567=CARTESIAN_POINT('Ctrl Pts',(0.0100921744644315,-0.0343603235965185,
0.0687459164890658));
#80568=CARTESIAN_POINT('Ctrl Pts',(0.00997822386255483,-0.034193496108874,
0.0687070926161821));
#80569=CARTESIAN_POINT('Ctrl Pts',(0.0102390586083021,-0.0346945769586966,
0.0688017544290226));
#80570=CARTESIAN_POINT('Ctrl Pts',(0.0101270374634973,-0.0345275153362944,
0.0687574491175959));
#80571=CARTESIAN_POINT('Ctrl Pts',(0.0100135939830225,-0.0343603235965185,
0.068716655308442));
#80572=CARTESIAN_POINT('Ctrl Pts',(0.00989906547550811,-0.034193496108874,
0.0686794886649065));
#80573=CARTESIAN_POINT('',(0.0102390586088605,-0.0346945769586966,0.0688017544292578));
#80574=CARTESIAN_POINT('',(0.0100175422024024,-0.034366772783146,0.0687193648596557));
#80575=CARTESIAN_POINT('Origin',(0.00422573830431933,-0.0345626457063142,
0.0845032583751714));
#80576=CARTESIAN_POINT('Origin',(0.0136567081479814,-0.0341934771029089,
0.058283507172973));
#80577=CARTESIAN_POINT('',(0.0101351242745058,-0.034193496108874,0.0687618066078136));
#80578=CARTESIAN_POINT('',(0.0100761095749121,-0.034193496108884,0.0687412271221477));
#80579=CARTESIAN_POINT('',(0.0103547977016228,-0.0345211942962687,0.0688489911525628));
#80580=CARTESIAN_POINT('Origin',(0.00378386539959845,-0.0345625596121401,
0.0843136821996429));
#80581=CARTESIAN_POINT('',(0.0103542707108205,-0.0346945769586885,0.0688502433100797));
#80582=CARTESIAN_POINT('Origin',(0.0146459511829038,-0.0346945685853839,
0.0586529890756434));
#80583=CARTESIAN_POINT('',(0.0102966646598505,-0.0346945769587026,0.0688259988696787));
#80584=CARTESIAN_POINT('Ctrl Pts',(0.0106662247308337,-0.0345231616327842,
0.0687152979895507));
#80585=CARTESIAN_POINT('Ctrl Pts',(0.0105913150150681,-0.0344132092796988,
0.068680253998641));
#80586=CARTESIAN_POINT('Ctrl Pts',(0.0105156843069898,-0.034303273855898,
0.0686467612642227));
#80587=CARTESIAN_POINT('Ctrl Pts',(0.0104394305973826,-0.034193496108874,
0.0686148602124428));
#80588=CARTESIAN_POINT('Ctrl Pts',(0.0105622311621331,-0.0345231616327842,
0.0687603143622092));
#80589=CARTESIAN_POINT('Ctrl Pts',(0.0104879419336865,-0.0344132092796988,
0.0687267037762327));
#80590=CARTESIAN_POINT('Ctrl Pts',(0.0104129613297634,-0.034303273855898,
0.0686946315384999));
#80591=CARTESIAN_POINT('Ctrl Pts',(0.0103373864616736,-0.034193496108874,
0.0686641362766711));
#80592=CARTESIAN_POINT('Ctrl Pts',(0.0104582375934324,-0.0345231616327842,
0.0688053307348676));
#80593=CARTESIAN_POINT('Ctrl Pts',(0.010384568852305,-0.0344132092796988,
0.0687731535538245));
#80594=CARTESIAN_POINT('Ctrl Pts',(0.0103102383525372,-0.034303273855898,
0.0687425018127771));
#80595=CARTESIAN_POINT('Ctrl Pts',(0.0102353423259647,-0.034193496108874,
0.0687134123408994));
#80596=CARTESIAN_POINT('Ctrl Pts',(0.0103542440247318,-0.0345231616327842,
0.068850347107526));
#80597=CARTESIAN_POINT('Ctrl Pts',(0.0102811957709235,-0.0344132092796988,
0.0688196033314162));
#80598=CARTESIAN_POINT('Ctrl Pts',(0.0102075153753109,-0.034303273855898,
0.0687903720870543));
#80599=CARTESIAN_POINT('Ctrl Pts',(0.0101332981902558,-0.034193496108874,
0.0687626884051277));
#80600=CARTESIAN_POINT('',(0.0102872774359542,-0.0341934961088839,0.0686883334101383));
#80601=CARTESIAN_POINT('Ctrl Pts',(0.0104512484705309,-0.0342105180195415,
0.0686198191107543));
#80602=CARTESIAN_POINT('Ctrl Pts',(0.0104345789114949,-0.0342610556240919,
0.0686594268497396));
#80603=CARTESIAN_POINT('Ctrl Pts',(0.0104182084790762,-0.0343122189869339,
0.0686983238483292));
#80604=CARTESIAN_POINT('Ctrl Pts',(0.0103860515174253,-0.0344158119695181,
0.0687747304611784));
#80605=CARTESIAN_POINT('Ctrl Pts',(0.010370278140664,-0.0344681990450068,
0.0688122088244829));
#80606=CARTESIAN_POINT('Ctrl Pts',(0.010354797701602,-0.0345211942962487,
0.0688489911525828));
#80607=CARTESIAN_POINT('Ctrl Pts',(0.0102398239325642,-0.0346945769586932,
0.0688036321000172));
#80608=CARTESIAN_POINT('Ctrl Pts',(0.0101292915592006,-0.034529677707698,
0.068759884434317));
#80609=CARTESIAN_POINT('Ctrl Pts',(0.0100170455031449,-0.034364806625142,
0.0687207425550122));
#80610=CARTESIAN_POINT('Ctrl Pts',(0.0102390586088688,-0.0346945769586932,
0.0688017544292611));
#80611=CARTESIAN_POINT('Ctrl Pts',(0.010128487415991,-0.034529677707698,
0.0687580225860868));
#80612=CARTESIAN_POINT('Ctrl Pts',(0.0100162032275512,-0.034364806625142,
0.0687188981202339));
#80613=CARTESIAN_POINT('Ctrl Pts',(0.0101115097307529,-0.0346945769586932,
0.0684888217448935));
#80614=CARTESIAN_POINT('Ctrl Pts',(0.00999446887604978,-0.034529677707698,
0.0684477268845236));
#80615=CARTESIAN_POINT('Ctrl Pts',(0.00987582954295247,-0.034364806625142,
0.0684115045452745));
#80616=CARTESIAN_POINT('',(0.0100994128185244,-0.0346775396664979,0.0684845888388123));
#80617=CARTESIAN_POINT('',(0.0101115097307497,-0.0346945769586887,0.0684888217448924));
#80618=CARTESIAN_POINT('Origin',(0.0047774089511205,-0.0345626617882452,
0.0842100195120109));
#80619=CARTESIAN_POINT('Ctrl Pts',(0.0100994128196703,-0.0346775396670096,
0.0684845888402199));
#80620=CARTESIAN_POINT('Ctrl Pts',(0.0100852679143845,-0.0346269749928194,
0.0685251514740384));
#80621=CARTESIAN_POINT('Ctrl Pts',(0.0100713744295451,-0.03457579028908,
0.0685649932311711));
#80622=CARTESIAN_POINT('Ctrl Pts',(0.0100440786959155,-0.0344721681088028,
0.0686432677473408));
#80623=CARTESIAN_POINT('Ctrl Pts',(0.0100306871430088,-0.0344197714289582,
0.0686816698172453));
#80624=CARTESIAN_POINT('Ctrl Pts',(0.0100175422026577,-0.0343667727830634,
0.0687193648596285));
#80625=CARTESIAN_POINT('',(0.0101752841698151,-0.0346945769587026,0.0686452880870851));
#80626=CARTESIAN_POINT('Origin',(0.00812378219310841,-0.0315241814719618,
0.07415));
#80627=CARTESIAN_POINT('',(0.0100994128174384,-0.0347116136489814,0.0684845888396831));
#80628=CARTESIAN_POINT('',(0.0100873068912883,-0.0346945769586885,0.0684803817800795));
#80629=CARTESIAN_POINT('Origin',(0.00482077341001143,-0.0345626692432209,
0.0842231616457031));
#80630=CARTESIAN_POINT('Origin',(0.00448900754622532,-0.0345626624903524,
0.0841094508668875));
#80631=CARTESIAN_POINT('Origin',(0.00444687538083543,-0.0345626699464334,
0.0840927749539778));
#80632=CARTESIAN_POINT('Ctrl Pts',(0.0101712829898971,-0.0352450361874068,
0.0687753834450469));
#80633=CARTESIAN_POINT('Ctrl Pts',(0.00996857600025991,-0.0349452760959493,
0.0686981606853295));
#80634=CARTESIAN_POINT('Ctrl Pts',(0.00976062814561051,-0.034644428984174,
0.0686364260272122));
#80635=CARTESIAN_POINT('Ctrl Pts',(0.0101689040614125,-0.0352450361874068,
0.0687745370856283));
#80636=CARTESIAN_POINT('Ctrl Pts',(0.0099661651508061,-0.0349452760959493,
0.068697404048671));
#80637=CARTESIAN_POINT('Ctrl Pts',(0.00975819222415695,-0.034644428984174,
0.0686357612628389));
#80638=CARTESIAN_POINT('Ctrl Pts',(0.00993336658769556,-0.0352450361874068,
0.0686907391233917));
#80639=CARTESIAN_POINT('Ctrl Pts',(0.00972746718508211,-0.0349452760959493,
0.068622489528026));
#80640=CARTESIAN_POINT('Ctrl Pts',(0.00951701188221981,-0.034644428984174,
0.0685699430080529));
#80641=CARTESIAN_POINT('Ctrl Pts',(0.00993101121295839,-0.0352450361874068,
0.0686899011437694));
#80642=CARTESIAN_POINT('Ctrl Pts',(0.00972508020542487,-0.0349452760959493,
0.0686217403828196));
#80643=CARTESIAN_POINT('Ctrl Pts',(0.00951460007880043,-0.034644428984174,
0.068569284825505));
#80644=CARTESIAN_POINT('',(0.0098990969872778,-0.0351951634053324,0.0686794963957505));
#80645=CARTESIAN_POINT('',(0.00967281289795655,-0.0348678972925388,0.0686111708028286));
#80646=CARTESIAN_POINT('Origin',(0.00556803005911865,-0.0345636767881918,
0.084854982652011));
#80647=CARTESIAN_POINT('Origin',(0.0126488990635694,-0.0346946199341088,
0.0579696530374064));
#80648=CARTESIAN_POINT('',(0.00979282790512056,-0.0346945769330288,0.0686461457678075));
#80649=CARTESIAN_POINT('',(0.00973263745266564,-0.0346945769458128,0.0686293124520078));
#80650=CARTESIAN_POINT('',(0.0100175422025963,-0.0350221583435276,0.0687193648597549));
#80651=CARTESIAN_POINT('Origin',(0.00509557610916057,-0.0345628458717967,
0.0847659284061648));
#80652=CARTESIAN_POINT('',(0.0100171377872637,-0.035195136029876,0.0687205337656475));
#80653=CARTESIAN_POINT('Origin',(0.0136453737232144,-0.0351951838366821,
0.0583160276328767));
#80654=CARTESIAN_POINT('',(0.00989906547612863,-0.0351951371328749,0.0686794886649999));
#80655=CARTESIAN_POINT('Ctrl Pts',(0.0103199591444846,-0.0350241211494343,
0.0685663804930619));
#80656=CARTESIAN_POINT('Ctrl Pts',(0.0102430470751497,-0.0349144232818962,
0.0685361290560242));
#80657=CARTESIAN_POINT('Ctrl Pts',(0.0101654636514139,-0.0348045283579412,
0.0685074493394749));
#80658=CARTESIAN_POINT('Ctrl Pts',(0.0100873068807874,-0.0346945769439157,
0.0684803817764428));
#80659=CARTESIAN_POINT('Ctrl Pts',(0.0102189973707346,-0.0350241211494343,
0.0686178378739136));
#80660=CARTESIAN_POINT('Ctrl Pts',(0.0101427941057225,-0.0349144232818962,
0.0685889771439134));
#80661=CARTESIAN_POINT('Ctrl Pts',(0.0100659486574713,-0.0348045283579412,
0.0685616743153149));
#80662=CARTESIAN_POINT('Ctrl Pts',(0.00998855815386677,-0.0346945769439157,
0.0685359680223534));
#80663=CARTESIAN_POINT('Ctrl Pts',(0.0101180355969845,-0.0350241211494343,
0.0686692952547653));
#80664=CARTESIAN_POINT('Ctrl Pts',(0.0100425411362953,-0.0349144232818962,
0.0686418252318026));
#80665=CARTESIAN_POINT('Ctrl Pts',(0.0099664336635288,-0.0348045283579412,
0.0686158992911549));
#80666=CARTESIAN_POINT('Ctrl Pts',(0.00988980942694615,-0.0346945769439157,
0.068591554268264));
#80667=CARTESIAN_POINT('Ctrl Pts',(0.0100170738232344,-0.0350241211494343,
0.068720752635617));
#80668=CARTESIAN_POINT('Ctrl Pts',(0.00994228816686812,-0.0349144232818962,
0.0686946733196917));
#80669=CARTESIAN_POINT('Ctrl Pts',(0.00986691866958626,-0.0348045283579412,
0.068670124266995));
#80670=CARTESIAN_POINT('Ctrl Pts',(0.00979106070002554,-0.0346945769439157,
0.0686471405141747));
#80671=CARTESIAN_POINT('',(0.00994006739851381,-0.0346945769458128,0.0685632637739539));
#80672=CARTESIAN_POINT('Ctrl Pts',(0.0100994128163504,-0.0347116136492819,
0.0684845888427845));
#80673=CARTESIAN_POINT('Ctrl Pts',(0.0100852735162157,-0.034762154653018,
0.0685251353638779));
#80674=CARTESIAN_POINT('Ctrl Pts',(0.0100713828231747,-0.0348133084092587,
0.0685649689675707));
#80675=CARTESIAN_POINT('Ctrl Pts',(0.0100440877442627,-0.0349168535524575,
0.068643241617724));
#80676=CARTESIAN_POINT('Ctrl Pts',(0.0100306921521641,-0.0349692115648189,
0.0686816554467496));
#80677=CARTESIAN_POINT('Ctrl Pts',(0.0100175422025655,-0.0350221583435,
0.0687193648597829));
#80678=CARTESIAN_POINT('Ctrl Pts',(0.00989970166157871,-0.0351951371254949,
0.0686808061201181));
#80679=CARTESIAN_POINT('Ctrl Pts',(0.00978662950959834,-0.0350307338980944,
0.0686440900993564));
#80680=CARTESIAN_POINT('Ctrl Pts',(0.00967213646435204,-0.0348659306897796,
0.0686120788462681));
#80681=CARTESIAN_POINT('Ctrl Pts',(0.00989906547609839,-0.0351951371254948,
0.0686794886651122));
#80682=CARTESIAN_POINT('Ctrl Pts',(0.00978596608656237,-0.0350307338980944,
0.0686427857970862));
#80683=CARTESIAN_POINT('Ctrl Pts',(0.00967144637065151,-0.0348659306897796,
0.0686107888112521));
#80684=CARTESIAN_POINT('Ctrl Pts',(0.00979244012651159,-0.0351951371254948,
0.0684586818329578));
#80685=CARTESIAN_POINT('Ctrl Pts',(0.00967477569425959,-0.0350307338980944,
0.0684241833771355));
#80686=CARTESIAN_POINT('Ctrl Pts',(0.00955578594716994,-0.0348659306897796,
0.0683945775979893));
#80687=CARTESIAN_POINT('Origin',(0.0111051747892662,-0.0308609197409787,
0.0634895112778859));
#80688=CARTESIAN_POINT('',(0.00985257922775907,-0.0351951371254948,0.068583221864822));
#80689=CARTESIAN_POINT('Origin',(0.00799973216735054,-0.0351840467441115,
0.0751192044374587));
#80690=CARTESIAN_POINT('Origin',(0.0105739807007534,-0.03523226137531,0.0624382776241762));
#80691=CARTESIAN_POINT('',(0.0094436321334361,-0.0351951142564665,0.0685521601739209));
#80692=CARTESIAN_POINT('',(0.00932168719774462,-0.0351951372916786,0.0685261646894785));
#80693=CARTESIAN_POINT('Origin',(0.00780291615939653,-0.0352875117313075,
0.0742641367432437));
#80694=CARTESIAN_POINT('Origin',(0.0150271178216191,-0.029832507652297,
0.0770892426711197));
#80695=CARTESIAN_POINT('Origin',(0.0128271015320566,-0.0338732790926143,
0.0672126203309357));
#80696=CARTESIAN_POINT('Ctrl Pts',(0.012482145399802,-0.0321934096636941,
0.0703972935228224));
#80697=CARTESIAN_POINT('Ctrl Pts',(0.0124149737409575,-0.0320508460844994,
0.0703192808969426));
#80698=CARTESIAN_POINT('Ctrl Pts',(0.0123457566844405,-0.0319086045664406,
0.070243131862772));
#80699=CARTESIAN_POINT('Ctrl Pts',(0.0122746567651399,-0.0317669892869893,
0.0701689981129682));
#80700=CARTESIAN_POINT('Ctrl Pts',(0.0124260670917702,-0.0321934096636941,
0.0703349584925741));
#80701=CARTESIAN_POINT('Ctrl Pts',(0.0123577796655692,-0.0320508460844994,
0.0702579496417028));
#80702=CARTESIAN_POINT('Ctrl Pts',(0.0122874746524418,-0.0319086045664406,
0.0701828336041581));
#80703=CARTESIAN_POINT('Ctrl Pts',(0.0122153167467269,-0.0317669892869893,
0.0701097596555202));
#80704=CARTESIAN_POINT('Ctrl Pts',(0.0123699887837384,-0.0321934096636941,
0.0702726234623258));
#80705=CARTESIAN_POINT('Ctrl Pts',(0.0123005855901808,-0.0320508460844994,
0.0701966183864629));
#80706=CARTESIAN_POINT('Ctrl Pts',(0.012229192620443,-0.0319086045664406,
0.0701225353455443));
#80707=CARTESIAN_POINT('Ctrl Pts',(0.012155976728314,-0.0317669892869893,
0.0700505211980724));
#80708=CARTESIAN_POINT('Ctrl Pts',(0.0123139104757066,-0.0321934096636941,
0.0702102884320775));
#80709=CARTESIAN_POINT('Ctrl Pts',(0.0122433915147925,-0.0320508460844994,
0.0701352871312231));
#80710=CARTESIAN_POINT('Ctrl Pts',(0.0121709105884443,-0.0319086045664406,
0.0700622370869305));
#80711=CARTESIAN_POINT('Ctrl Pts',(0.0120966367099011,-0.0317669892869893,
0.0699912827406245));
#80712=CARTESIAN_POINT('',(0.0123149137277173,-0.0321934096636941,0.0702114036180884));
#80713=CARTESIAN_POINT('',(0.012149559462665,-0.0318665617511309,0.0700425382089351));
#80714=CARTESIAN_POINT('Origin',(-0.000274735752390532,-0.0326371944420916,
0.0811986066656033));
#80715=CARTESIAN_POINT('Origin',(0.0198220583471527,-0.0316939261509129,
0.062214361471898));
#80716=CARTESIAN_POINT('',(0.0123993138497735,-0.0320197221621844,0.0703032587532579));
#80717=CARTESIAN_POINT('Ctrl Pts',(0.0123992292997157,-0.0320197392094758,
0.070303094235275));
#80718=CARTESIAN_POINT('Ctrl Pts',(0.0123796549715422,-0.0319792716576056,
0.0702813394172722));
#80719=CARTESIAN_POINT('Ctrl Pts',(0.0123598256836007,-0.0319386439829741,
0.0702596347898578));
#80720=CARTESIAN_POINT('Ctrl Pts',(0.0123397143748557,-0.0318979099381672,
0.0702379632718098));
#80721=CARTESIAN_POINT('Ctrl Pts',(0.0123196034636246,-0.0318571766984966,
0.0702162921821141));
#80722=CARTESIAN_POINT('Ctrl Pts',(0.0122993140654981,-0.0318163871833606,
0.070194763135152));
#80723=CARTESIAN_POINT('Ctrl Pts',(0.0122789185301591,-0.0317755399638303,
0.07017344776701));
#80724=CARTESIAN_POINT('',(0.0123985151930508,-0.0321934096636182,0.0703043325963879));
#80725=CARTESIAN_POINT('Origin',(0.0140999142739366,-0.0324111592547179,
0.068745425676449));
#80726=CARTESIAN_POINT('',(0.012356714460394,-0.0321934096636662,0.0702578681072482));
#80727=CARTESIAN_POINT('Ctrl Pts',(0.0123148067098626,-0.0321934096636618,
0.070213429015471));
#80728=CARTESIAN_POINT('Ctrl Pts',(0.012260518328002,-0.0320835708272592,
0.0701556315210916));
#80729=CARTESIAN_POINT('Ctrl Pts',(0.0122050653194668,-0.0319739230346488,
0.0700989910468487));
#80730=CARTESIAN_POINT('Ctrl Pts',(0.0121485241942168,-0.0318646057455573,
0.0700435746152177));
#80731=CARTESIAN_POINT('Ctrl Pts',(0.0123207859095765,-0.0321934096636618,
0.0701002680065709));
#80732=CARTESIAN_POINT('Ctrl Pts',(0.0122649369492106,-0.0320835708272592,
0.0700423880543674));
#80733=CARTESIAN_POINT('Ctrl Pts',(0.0122079225609088,-0.0319739230346488,
0.0699856974662205));
#80734=CARTESIAN_POINT('Ctrl Pts',(0.0121498212572286,-0.0318646057455573,
0.0699302631754066));
#80735=CARTESIAN_POINT('Ctrl Pts',(0.0123267651092905,-0.0321934096636618,
0.0699871069976707));
#80736=CARTESIAN_POINT('Ctrl Pts',(0.0122693555704193,-0.0320835708272592,
0.0699291445876432));
#80737=CARTESIAN_POINT('Ctrl Pts',(0.0122107798023508,-0.0319739230346488,
0.0698724038855923));
#80738=CARTESIAN_POINT('Ctrl Pts',(0.0121511183202404,-0.0318646057455573,
0.0698169517355954));
#80739=CARTESIAN_POINT('Ctrl Pts',(0.0123327443090045,-0.0321934096636618,
0.0698739459887705));
#80740=CARTESIAN_POINT('Ctrl Pts',(0.012273774191628,-0.0320835708272592,
0.0698159011209191));
#80741=CARTESIAN_POINT('Ctrl Pts',(0.0122136370437928,-0.0319739230346488,
0.0697591103049642));
#80742=CARTESIAN_POINT('Ctrl Pts',(0.0121524153832521,-0.0318646057455573,
0.0697036402957843));
#80743=CARTESIAN_POINT('',(0.0123236009778616,-0.0321763980308462,0.069864965326513));
#80744=CARTESIAN_POINT('',(0.0123327443089812,-0.0321934096636184,0.0698739459887476));
#80745=CARTESIAN_POINT('Origin',(0.0003105334440736,-0.032638623101237,
0.0812453123874431));
#80746=CARTESIAN_POINT('Ctrl Pts',(0.0123236009756338,-0.0321763980306277,
0.0698649653287753));
#80747=CARTESIAN_POINT('Ctrl Pts',(0.012293559046511,-0.0321259596174869,
0.0698956168198389));
#80748=CARTESIAN_POINT('Ctrl Pts',(0.0122640376327977,-0.0320749164631494,
0.0699257372340511));
#80749=CARTESIAN_POINT('Ctrl Pts',(0.0122060120782834,-0.031971605779395,
0.0699849401486972));
#80750=CARTESIAN_POINT('Ctrl Pts',(0.0121775305461949,-0.0319193786690147,
0.0700139995816793));
#80751=CARTESIAN_POINT('Ctrl Pts',(0.0121495594613591,-0.0318665617525348,
0.0700425382102534));
#80752=CARTESIAN_POINT('',(0.0123238290183593,-0.0321934096636663,0.070042674803428));
#80753=CARTESIAN_POINT('Origin',(0.00812378219310841,-0.0315241814719618,
0.07415));
#80754=CARTESIAN_POINT('',(0.0123236009781209,-0.032210423332362,0.0698649653262478));
#80755=CARTESIAN_POINT('',(0.0123144384873291,-0.0321934096636183,0.0698560042124233));
#80756=CARTESIAN_POINT('Origin',(0.000338172652233866,-0.0326387239418652,
0.0812812454835279));
#80757=CARTESIAN_POINT('Origin',(0.00118682613749727,-0.0326386238749014,
0.0821041810387247));
#80758=CARTESIAN_POINT('Origin',(0.0011503477403256,-0.0326387246157369,
0.0820772662926032));
#80759=CARTESIAN_POINT('Ctrl Pts',(0.0122630559966726,-0.0327445246967097,
0.0701569388460572));
#80760=CARTESIAN_POINT('Ctrl Pts',(0.0121124552332627,-0.032443687833936,
0.070000823582417));
#80761=CARTESIAN_POINT('Ctrl Pts',(0.0119505230710078,-0.0321434074405927,
0.0698564956907656));
#80762=CARTESIAN_POINT('Ctrl Pts',(0.0120856161413255,-0.0327445246967097,
0.069980827807975));
#80763=CARTESIAN_POINT('Ctrl Pts',(0.0119283732415301,-0.032443687833936,
0.0698314047978827));
#80764=CARTESIAN_POINT('Ctrl Pts',(0.0117603219003864,-0.0321434074405927,
0.0696942504606531));
#80765=CARTESIAN_POINT('',(0.0120593369740092,-0.0326943950436612,0.0699560122119241));
#80766=CARTESIAN_POINT('',(0.0118837058516271,-0.0323666188837389,0.0697978626995335));
#80767=CARTESIAN_POINT('Origin',(0.000611440867388505,-0.0326395579112146,
0.0822667283954489));
#80768=CARTESIAN_POINT('Origin',(0.0191040660565653,-0.0321933825603054,
0.0614402451953115));
#80769=CARTESIAN_POINT('',(0.0119774070524119,-0.0321934096532689,0.0698806088911313));
#80770=CARTESIAN_POINT('',(0.01193011238449,-0.0321934096584275,0.0698397498072968));
#80771=CARTESIAN_POINT('',(0.0121495594633223,-0.0325210109756239,0.0700425382082568));
#80772=CARTESIAN_POINT('Origin',(0.000278674135473845,-0.0326393129159324,
0.0819196682680485));
#80773=CARTESIAN_POINT('',(0.0121486085297355,-0.0326943950436593,0.0700435084366343));
#80774=CARTESIAN_POINT('Origin',(0.0198919937411281,-0.0326943765538128,
0.0621430083161342));
#80775=CARTESIAN_POINT('',(0.0121039727518823,-0.0326943950436702,0.0699997603242893));
#80776=CARTESIAN_POINT('Ctrl Pts',(0.0124883328294781,-0.0325229783203769,
0.0700328774923979));
#80777=CARTESIAN_POINT('Ctrl Pts',(0.0124315783857464,-0.032413025309245,
0.0699727122573219));
#80778=CARTESIAN_POINT('Ctrl Pts',(0.0123735879547627,-0.032303122220807,
0.0699137301860576));
#80779=CARTESIAN_POINT('Ctrl Pts',(0.0123144384841223,-0.0321934096576658,
0.0698560042092912));
#80780=CARTESIAN_POINT('Ctrl Pts',(0.0123750703955872,-0.0325229783203769,
0.0700364500692717));
#80781=CARTESIAN_POINT('Ctrl Pts',(0.0123183651997495,-0.032413025309245,
0.0699778461543701));
#80782=CARTESIAN_POINT('Ctrl Pts',(0.012260456307104,-0.032303122220807,
0.0699204241477193));
#80783=CARTESIAN_POINT('Ctrl Pts',(0.0122014204902863,-0.0321934096576658,
0.0698642549853593));
#80784=CARTESIAN_POINT('Ctrl Pts',(0.0122618079616962,-0.0325229783203769,
0.0700400226461456));
#80785=CARTESIAN_POINT('Ctrl Pts',(0.0122051520137526,-0.032413025309245,
0.0699829800514183));
#80786=CARTESIAN_POINT('Ctrl Pts',(0.0121473246594452,-0.032303122220807,
0.069927118109381));
#80787=CARTESIAN_POINT('Ctrl Pts',(0.0120884024964504,-0.0321934096576658,
0.0698725057614275));
#80788=CARTESIAN_POINT('Ctrl Pts',(0.0121485455278052,-0.0325229783203769,
0.0700435952230195));
#80789=CARTESIAN_POINT('Ctrl Pts',(0.0120919388277557,-0.032413025309245,
0.0699881139484665));
#80790=CARTESIAN_POINT('Ctrl Pts',(0.0120341930117865,-0.032303122220807,
0.0699338120710428));
#80791=CARTESIAN_POINT('Ctrl Pts',(0.0119753845026145,-0.0321934096576658,
0.0698807565374957));
#80792=CARTESIAN_POINT('',(0.0121459227703356,-0.0321934096584275,0.0698683065520066));
#80793=CARTESIAN_POINT('Ctrl Pts',(0.01232360097568,-0.0322104233328938,
0.0698649653287282));
#80794=CARTESIAN_POINT('Ctrl Pts',(0.0122935183392906,-0.0322609421830787,
0.0698956583530241));
#80795=CARTESIAN_POINT('Ctrl Pts',(0.0122639770394119,-0.0323120888239514,
0.0699257990568896));
#80796=CARTESIAN_POINT('Ctrl Pts',(0.0122059510455046,-0.0324156524631821,
0.0699850024198442));
#80797=CARTESIAN_POINT('Ctrl Pts',(0.012177490203303,-0.032468026716732,
0.0700140407431437));
#80798=CARTESIAN_POINT('Ctrl Pts',(0.0121495594632888,-0.0325210109755912,
0.0700425382082847));
#80799=CARTESIAN_POINT('Origin',(0.0130386299408862,-0.0262834582512054,
0.0802939122271317));
#80800=CARTESIAN_POINT('Origin',(0.0196196688966671,-0.0342770993098472,
0.0701915402537489));
#80801=CARTESIAN_POINT('Ctrl Pts',(0.0120593573380794,-0.0326943950436604,
0.069958039840129));
#80802=CARTESIAN_POINT('Ctrl Pts',(0.0120015842705057,-0.0325844576448134,
0.0699038002385773));
#80803=CARTESIAN_POINT('Ctrl Pts',(0.0119426853503551,-0.0324744968375322,
0.0698507516401625));
#80804=CARTESIAN_POINT('Ctrl Pts',(0.0118827369798552,-0.0323646534831894,
0.0697989609729569));
#80805=CARTESIAN_POINT('Ctrl Pts',(0.0120582193023163,-0.0326943950436604,
0.0698447268556302));
#80806=CARTESIAN_POINT('Ctrl Pts',(0.011998884569445,-0.0325844576448134,
0.0697905029383443));
#80807=CARTESIAN_POINT('Ctrl Pts',(0.0119384241978517,-0.0324744968375322,
0.0697375023231039));
#80808=CARTESIAN_POINT('Ctrl Pts',(0.0118769165895386,-0.0323646534831894,
0.0696857918489081));
#80809=CARTESIAN_POINT('Ctrl Pts',(0.0120570812665532,-0.0326943950436604,
0.0697314138711315));
#80810=CARTESIAN_POINT('Ctrl Pts',(0.0119961848683844,-0.0325844576448134,
0.0696772056381113));
#80811=CARTESIAN_POINT('Ctrl Pts',(0.0119341630453483,-0.0324744968375322,
0.0696242530060453));
#80812=CARTESIAN_POINT('Ctrl Pts',(0.0118710961992221,-0.0323646534831894,
0.0695726227248592));
#80813=CARTESIAN_POINT('Ctrl Pts',(0.0120559432307901,-0.0326943950436604,
0.0696181008866328));
#80814=CARTESIAN_POINT('Ctrl Pts',(0.0119934851673237,-0.0325844576448134,
0.0695639083378783));
#80815=CARTESIAN_POINT('Ctrl Pts',(0.011929901892845,-0.0324744968375322,
0.0695110036889868));
#80816=CARTESIAN_POINT('Ctrl Pts',(0.0118652758089055,-0.0323646534831894,
0.0694594536008104));
#80817=CARTESIAN_POINT('',(0.0120462540416307,-0.0326773559991344,0.0696097120600405));
#80818=CARTESIAN_POINT('',(0.0120559432307895,-0.0326943950436595,0.0696181008866323));
#80819=CARTESIAN_POINT('Origin',(0.00122873732670427,-0.0326395670818651,
0.0822079120823499));
#80820=CARTESIAN_POINT('Ctrl Pts',(0.012046254039433,-0.0326773559987419,
0.0696097120625729));
#80821=CARTESIAN_POINT('Ctrl Pts',(0.0120181734350441,-0.0326267922585961,
0.069642215553835));
#80822=CARTESIAN_POINT('Ctrl Pts',(0.0119905905390908,-0.0325756109579332,
0.0696741429441854));
#80823=CARTESIAN_POINT('Ctrl Pts',(0.0119363966896439,-0.0324719985462367,
0.0697368726948545));
#80824=CARTESIAN_POINT('Ctrl Pts',(0.0119098074718235,-0.0324196091621777,
0.0697676498959831));
#80825=CARTESIAN_POINT('Ctrl Pts',(0.0118837058515953,-0.0323666188837757,
0.0697978626995705));
#80826=CARTESIAN_POINT('',(0.0120576401024093,-0.0326943950436703,0.0697870565492882));
#80827=CARTESIAN_POINT('Origin',(0.00812378219310841,-0.0315241814719618,
0.07415));
#80828=CARTESIAN_POINT('',(0.0120462540416011,-0.032711433837988,0.069609712060074));
#80829=CARTESIAN_POINT('',(0.0120365469580376,-0.0326943950436593,0.0696013439463572));
#80830=CARTESIAN_POINT('Origin',(0.00126352644271611,-0.0326395674874853,
0.0822369417702879));
#80831=CARTESIAN_POINT('Origin',(0.00115270127190298,-0.0326395675869598,
0.0821422241959825));
#80832=CARTESIAN_POINT('Origin',(0.0011189287679231,-0.032639568138318,
0.0821120180695751));
#80833=CARTESIAN_POINT('Ctrl Pts',(0.0120041327497945,-0.0332451089994434,
0.0699048846238029));
#80834=CARTESIAN_POINT('Ctrl Pts',(0.0118440256038911,-0.0329451141710254,
0.069758534808149));
#80835=CARTESIAN_POINT('Ctrl Pts',(0.0116733496390936,-0.0326442513127493,
0.0696246606816282));
#80836=CARTESIAN_POINT('Ctrl Pts',(0.011815983805192,-0.0332451089994434,
0.0697402639244818));
#80837=CARTESIAN_POINT('Ctrl Pts',(0.0116496678880329,-0.0329451141710254,
0.0696010102623728));
#80838=CARTESIAN_POINT('Ctrl Pts',(0.0114733353017379,-0.0326442513127493,
0.0694746798000061));
#80839=CARTESIAN_POINT('Ctrl Pts',(0.011814102315746,-0.0332451089994434,
0.0697386177174885));
#80840=CARTESIAN_POINT('Ctrl Pts',(0.0116477243108743,-0.0329451141710254,
0.069599435016915));
#80841=CARTESIAN_POINT('Ctrl Pts',(0.0114713351583643,-0.0326442513127493,
0.06947317999119));
#80842=CARTESIAN_POINT('',(0.0117882283835276,-0.0331951640388616,0.0697171725594692));
#80843=CARTESIAN_POINT('',(0.0116030135315722,-0.0328677532355012,0.0695703630751684));
#80844=CARTESIAN_POINT('Origin',(0.00171026031731824,-0.0326402808279703,
0.0831136947616987));
#80845=CARTESIAN_POINT('Origin',(0.0182909184960013,-0.0326944278779088,
0.0607665962590047));
#80846=CARTESIAN_POINT('',(0.0117017255132845,-0.0326943950436593,0.069647062447956));
#80847=CARTESIAN_POINT('',(0.0116519586094886,-0.0326943950436694,0.0696092536489164));
#80848=CARTESIAN_POINT('',(0.0118837058516293,-0.0330220786163545,0.0697978626995353));
#80849=CARTESIAN_POINT('Origin',(0.00130923900946434,-0.0326396682765535,
0.0828484881322693));
#80850=CARTESIAN_POINT('',(0.0118828177156378,-0.0331951640388588,0.0697988907230038));
#80851=CARTESIAN_POINT('Origin',(0.0190947098355173,-0.0331952026560135,
0.0614510777399818));
#80852=CARTESIAN_POINT('',(0.0118355230495927,-0.0331951640388701,0.0697580316412465));
#80853=CARTESIAN_POINT('Ctrl Pts',(0.012221203422627,-0.0330240426238172,
0.0697669486350351));
#80854=CARTESIAN_POINT('Ctrl Pts',(0.0121608226198746,-0.032914277406352,
0.0697105026656744));
#80855=CARTESIAN_POINT('Ctrl Pts',(0.0120992448192292,-0.0328043479726691,
0.0696552767957977));
#80856=CARTESIAN_POINT('Ctrl Pts',(0.0120365469580396,-0.0326943950436593,
0.0696013439463569));
#80857=CARTESIAN_POINT('Ctrl Pts',(0.0121083888394075,-0.0330240426238172,
0.0697776259847796));
#80858=CARTESIAN_POINT('Ctrl Pts',(0.0120481551275503,-0.032914277406352,
0.0697227341462127));
#80859=CARTESIAN_POINT('Ctrl Pts',(0.0119867566193549,-0.0328043479726691,
0.069669060141141));
#80860=CARTESIAN_POINT('Ctrl Pts',(0.0119242700772341,-0.0326943950436593,
0.0696166748961364));
#80861=CARTESIAN_POINT('Ctrl Pts',(0.011995574256188,-0.0330240426238172,
0.0697883033345242));
#80862=CARTESIAN_POINT('Ctrl Pts',(0.011935487635226,-0.032914277406352,
0.069734965626751));
#80863=CARTESIAN_POINT('Ctrl Pts',(0.0118742684194807,-0.0328043479726691,
0.0696828434864842));
#80864=CARTESIAN_POINT('Ctrl Pts',(0.0118119931964286,-0.0326943950436593,
0.0696320058459159));
#80865=CARTESIAN_POINT('Ctrl Pts',(0.0118827596729685,-0.0330240426238172,
0.0697989806842687));
#80866=CARTESIAN_POINT('Ctrl Pts',(0.0118228201429016,-0.032914277406352,
0.0697471971072893));
#80867=CARTESIAN_POINT('Ctrl Pts',(0.0117617802196065,-0.0328043479726691,
0.0696966268318275));
#80868=CARTESIAN_POINT('Ctrl Pts',(0.0116997163156231,-0.0326943950436593,
0.0696473367956954));
#80869=CARTESIAN_POINT('',(0.011869136235671,-0.0326943950436694,0.0696242031971666));
#80870=CARTESIAN_POINT('Ctrl Pts',(0.0120462540394279,-0.0327114338383338,
0.0696097120625789));
#80871=CARTESIAN_POINT('Ctrl Pts',(0.0120181781057898,-0.0327619876830519,
0.069642210147415));
#80872=CARTESIAN_POINT('Ctrl Pts',(0.0119905974912604,-0.0328131562603384,
0.0696741348970017));
#80873=CARTESIAN_POINT('Ctrl Pts',(0.0119364036915331,-0.0329167375858776,
0.0697368645901201));
#80874=CARTESIAN_POINT('Ctrl Pts',(0.0119098121000111,-0.0329691088920627,
0.0697676445388245));
#80875=CARTESIAN_POINT('Ctrl Pts',(0.0118837058515961,-0.0330220786163186,
0.0697978626995695));
#80876=CARTESIAN_POINT('Ctrl Pts',(0.0117883760468137,-0.0331951640388604,
0.0697191952308074));
#80877=CARTESIAN_POINT('Ctrl Pts',(0.0116967719989783,-0.0330306422010619,
0.0696434321024011));
#80878=CARTESIAN_POINT('Ctrl Pts',(0.0116021148563886,-0.0328657861914645,
0.0695715198046872));
#80879=CARTESIAN_POINT('Ctrl Pts',(0.01178822838353,-0.0331951640388604,
0.0697171725594713));
#80880=CARTESIAN_POINT('Ctrl Pts',(0.0116965825182616,-0.0330306422010619,
0.0696414124839086));
#80881=CARTESIAN_POINT('Ctrl Pts',(0.0116018837201488,-0.0328657861914645,
0.0695695049647883));
#80882=CARTESIAN_POINT('Ctrl Pts',(0.0117636237094165,-0.0331951640388604,
0.0693801411198905));
#80883=CARTESIAN_POINT('Ctrl Pts',(0.0116650099352193,-0.0330306422010619,
0.0693048897301902));
#80884=CARTESIAN_POINT('Ctrl Pts',(0.0115633702067286,-0.0328657861914645,
0.0692337784532672));
#80885=CARTESIAN_POINT('',(0.0117534269021824,-0.0331781648281916,0.0693723772353038));
#80886=CARTESIAN_POINT('',(0.0117636237094156,-0.0331951640388588,0.0693801411198898));
#80887=CARTESIAN_POINT('Origin',(0.00233486059486569,-0.0326412092479985,
0.0829472470704646));
#80888=CARTESIAN_POINT('Ctrl Pts',(0.0117534269027313,-0.033178164828644,
0.0693723772370544));
#80889=CARTESIAN_POINT('Ctrl Pts',(0.0117274247406303,-0.0331276811546768,
0.0694066033402079));
#80890=CARTESIAN_POINT('Ctrl Pts',(0.0117018921239798,-0.033076566349777,
0.0694402114463882));
#80891=CARTESIAN_POINT('Ctrl Pts',(0.0116517439154597,-0.0329730614463061,
0.0695062204419807));
#80892=CARTESIAN_POINT('Ctrl Pts',(0.0116271485781008,-0.0329207133373501,
0.0695385946619604));
#80893=CARTESIAN_POINT('Ctrl Pts',(0.0116030135479716,-0.0328677532289369,
0.0695703630766842));
#80894=CARTESIAN_POINT('',(0.0117759260464816,-0.0331951640388701,0.0695486568396894));
#80895=CARTESIAN_POINT('Origin',(0.00812378219310841,-0.0315241814719618,
0.07415));
#80896=CARTESIAN_POINT('',(0.0117534269007285,-0.0332121607144239,0.0693723772361483));
#80897=CARTESIAN_POINT('',(0.0117432135337918,-0.0331951640388587,0.0693646351476515));
#80898=CARTESIAN_POINT('Origin',(0.00237516798546861,-0.0326413658408602,
0.0829680195320731));
#80899=CARTESIAN_POINT('Origin',(0.00120054720875783,-0.0326412098231721,
0.0820854907417792));
#80900=CARTESIAN_POINT('Origin',(0.00116973075216782,-0.0326413664870062,
0.0820522257248164));
#80901=CARTESIAN_POINT('Ctrl Pts',(0.0117299389924713,-0.0337436976235975,
0.069669625223443));
#80902=CARTESIAN_POINT('Ctrl Pts',(0.0116896418227116,-0.0336723290703325,
0.0696371909026615));
#80903=CARTESIAN_POINT('Ctrl Pts',(0.0116487677808844,-0.033601104548885,
0.0696054866480589));
#80904=CARTESIAN_POINT('Ctrl Pts',(0.0115182650620217,-0.0333736987606857,
0.0695042612433717));
#80905=CARTESIAN_POINT('Ctrl Pts',(0.0113821685039338,-0.0331450831799191,
0.0694106916486237));
#80906=CARTESIAN_POINT('Ctrl Pts',(0.0115318252498913,-0.0337436976235975,
0.0695171426178747));
#80907=CARTESIAN_POINT('Ctrl Pts',(0.0114901566284677,-0.0336723290703325,
0.0694864901621189));
#80908=CARTESIAN_POINT('Ctrl Pts',(0.0114479434069807,-0.033601104548885,
0.0694565921523709));
#80909=CARTESIAN_POINT('Ctrl Pts',(0.0113131649527408,-0.0333736987606857,
0.0693611337297076));
#80910=CARTESIAN_POINT('Ctrl Pts',(0.01117313064803,-0.0331450831799191,
0.0692735669798031));
#80911=CARTESIAN_POINT('Ctrl Pts',(0.0115298441124655,-0.0337436976235975,
0.069515617791819));
#80912=CARTESIAN_POINT('Ctrl Pts',(0.0114881617765253,-0.0336723290703325,
0.0694849831547135));
#80913=CARTESIAN_POINT('Ctrl Pts',(0.0114459351632417,-0.033601104548885,
0.069455103207414));
#80914=CARTESIAN_POINT('Ctrl Pts',(0.011311113951648,-0.0333736987606857,
0.0693597024545709));
#80915=CARTESIAN_POINT('Ctrl Pts',(0.011171040269471,-0.0331450831799191,
0.0692721957331149));
#80916=CARTESIAN_POINT('',(0.0115026578980479,-0.0336938721132548,0.0694958272517481));
#80917=CARTESIAN_POINT('',(0.0113085902837036,-0.0333679869945434,0.0693609372079656));
#80918=CARTESIAN_POINT('Ctrl Pts',(0.0115026578980595,-0.0336938721132648,
0.069495827251756));
#80919=CARTESIAN_POINT('Ctrl Pts',(0.0114844904785115,-0.0336629187933931,
0.0694826379148211));
#80920=CARTESIAN_POINT('Ctrl Pts',(0.0114662516404663,-0.0336319952301039,
0.0694695591736962));
#80921=CARTESIAN_POINT('Ctrl Pts',(0.011447943406992,-0.0336011045488949,
0.0694565921523791));
#80922=CARTESIAN_POINT('Ctrl Pts',(0.0114020017844801,-0.0335235892595453,
0.0694240534588295));
#80923=CARTESIAN_POINT('Ctrl Pts',(0.0113555414728891,-0.0334458668660368,
0.0693921605460286));
#80924=CARTESIAN_POINT('Ctrl Pts',(0.0113085902838861,-0.0333679869945384,
0.0693609372077037));
#80925=CARTESIAN_POINT('Ctrl Pts',(0.0113085536348728,-0.0333679692459108,
0.0693609120100735));
#80926=CARTESIAN_POINT('Ctrl Pts',(0.0113083076039904,-0.0333391895374089,
0.0693612926761041));
#80927=CARTESIAN_POINT('Ctrl Pts',(0.0113081259190156,-0.033310408106043,
0.0693615797664861));
#80928=CARTESIAN_POINT('Ctrl Pts',(0.0113078901079837,-0.0332532698453461,
0.0693619627412726));
#80929=CARTESIAN_POINT('Ctrl Pts',(0.0113078341202312,-0.0332249172387362,
0.0693620614167115));
#80930=CARTESIAN_POINT('Ctrl Pts',(0.0113078378332342,-0.0331960985319339,
0.0693620682938483));
#80931=CARTESIAN_POINT('Ctrl Pts',(0.0113078379098615,-0.0331956312606037,
0.0693620683805414));
#80932=CARTESIAN_POINT('Ctrl Pts',(0.011307838002495,-0.0331951640388587,
0.0693620684421443));
#80933=CARTESIAN_POINT('',(0.0114119234711446,-0.0331951640388587,0.0694312870466964));
#80934=CARTESIAN_POINT('',(0.0113598807368301,-0.0331951640388687,0.0693966777444304));
#80935=CARTESIAN_POINT('',(0.0116030135388988,-0.0335216366567709,0.0695703630888588));
#80936=CARTESIAN_POINT('Origin',(0.0025189802526022,-0.0326434571526564,
0.0835292672104726));
#80937=CARTESIAN_POINT('',(0.0116021917056727,-0.0336938721132328,0.0695714448498568));
#80938=CARTESIAN_POINT('Origin',(0.0182084903229778,-0.0336938867896242,
0.0608757189737409));
#80939=CARTESIAN_POINT('',(0.0115524248018703,-0.0336938721132538,0.0695336360508124));
#80940=CARTESIAN_POINT('Ctrl Pts',(0.0119379032835746,-0.0335235895815171,
0.0695183177670219));
#80941=CARTESIAN_POINT('Ctrl Pts',(0.0118741390586945,-0.0334144449262748,
0.0694658088808983));
#80942=CARTESIAN_POINT('Ctrl Pts',(0.0118092167823753,-0.0333049234473147,
0.0694145569893242));
#80943=CARTESIAN_POINT('Ctrl Pts',(0.011743213533793,-0.0331951640388587,
0.0693646351476513));
#80944=CARTESIAN_POINT('Ctrl Pts',(0.011825981594274,-0.0335235895815171,
0.0695360577768871));
#80945=CARTESIAN_POINT('Ctrl Pts',(0.0117624615955566,-0.0334144449262748,
0.0694850897131702));
#80946=CARTESIAN_POINT('Ctrl Pts',(0.0116978156582176,-0.0333049234473147,
0.0694353753686924));
#80947=CARTESIAN_POINT('Ctrl Pts',(0.0116321206861739,-0.0331951640388587,
0.0693869858007465));
#80948=CARTESIAN_POINT('Ctrl Pts',(0.0117140599049735,-0.0335235895815171,
0.0695537977867523));
#80949=CARTESIAN_POINT('Ctrl Pts',(0.0116507841324187,-0.0334144449262748,
0.0695043705454422));
#80950=CARTESIAN_POINT('Ctrl Pts',(0.01158641453406,-0.0333049234473147,
0.0694561937480607));
#80951=CARTESIAN_POINT('Ctrl Pts',(0.0115210278385547,-0.0331951640388587,
0.0694093364538417));
#80952=CARTESIAN_POINT('Ctrl Pts',(0.0116021382156729,-0.0335235895815171,
0.0695715377966175));
#80953=CARTESIAN_POINT('Ctrl Pts',(0.0115391066692808,-0.0334144449262748,
0.0695236513777141));
#80954=CARTESIAN_POINT('Ctrl Pts',(0.0114750134099023,-0.0333049234473147,
0.0694770121274289));
#80955=CARTESIAN_POINT('Ctrl Pts',(0.0114099349909356,-0.0331951640388587,
0.0694316871069369));
#80956=CARTESIAN_POINT('',(0.0115775685024782,-0.0331951640388687,0.069397961097184));
#80957=CARTESIAN_POINT('Ctrl Pts',(0.0117534268988279,-0.0332121607145998,
0.069372377238639));
#80958=CARTESIAN_POINT('Ctrl Pts',(0.0117274684694097,-0.0332625444109364,
0.0694065457574039));
#80959=CARTESIAN_POINT('Ctrl Pts',(0.0117019573444652,-0.0333135300745996,
0.0694401254989722));
#80960=CARTESIAN_POINT('Ctrl Pts',(0.0116518094530428,-0.0334167203140615,
0.069506134082985));
#80961=CARTESIAN_POINT('Ctrl Pts',(0.0116271921093181,-0.0334688847587301,
0.0695385373596798));
#80962=CARTESIAN_POINT('Ctrl Pts',(0.0116030135383331,-0.0335216366562365,
0.0695703630893147));
#80963=CARTESIAN_POINT('Ctrl Pts',(0.011502793169285,-0.0336938721132391,
0.0694968179164566));
#80964=CARTESIAN_POINT('Ctrl Pts',(0.0114755565504605,-0.0336474569764958,
0.0694770394439383));
#80965=CARTESIAN_POINT('Ctrl Pts',(0.0114480902659135,-0.033601104548885,
0.0694575811656658));
#80966=CARTESIAN_POINT('Ctrl Pts',(0.0113785519483352,-0.0334837508592656,
0.0694083172788185));
#80967=CARTESIAN_POINT('Ctrl Pts',(0.0113075843757529,-0.0333660264659097,
0.0693611355895662));
#80968=CARTESIAN_POINT('Ctrl Pts',(0.0115026578980645,-0.0336938721132391,
0.0694958272517603));
#80969=CARTESIAN_POINT('Ctrl Pts',(0.0114754154805508,-0.0336474569764958,
0.0694760495710293));
#80970=CARTESIAN_POINT('Ctrl Pts',(0.0114479434069807,-0.033601104548885,
0.0694565921523709));
#80971=CARTESIAN_POINT('Ctrl Pts',(0.0113783904329272,-0.0334837508592656,
0.0694073304418688));
#80972=CARTESIAN_POINT('Ctrl Pts',(0.0113074082747952,-0.0333660264659097,
0.0693601513623077));
#80973=CARTESIAN_POINT('Ctrl Pts',(0.0114566650854551,-0.0336938721132391,
0.069158996878329));
#80974=CARTESIAN_POINT('Ctrl Pts',(0.0114274510879935,-0.0336474569764958,
0.0691394884087922));
#80975=CARTESIAN_POINT('Ctrl Pts',(0.0113980107210265,-0.033601104548885,
0.0691203232627141));
#80976=CARTESIAN_POINT('Ctrl Pts',(0.0113234744806307,-0.0334837508592656,
0.0690718015191877));
#80977=CARTESIAN_POINT('Ctrl Pts',(0.0112475331711956,-0.0333660264659097,
0.069025509746177));
#80978=CARTESIAN_POINT('',(0.0114462752115993,-0.0336769361243754,0.0691538975048465));
#80979=CARTESIAN_POINT('',(0.0114569393964622,-0.0336938721132327,0.0691610058070057));
#80980=CARTESIAN_POINT('Ctrl Pts',(0.0114462752115991,-0.0336769361243751,
0.0691538975048463));
#80981=CARTESIAN_POINT('Ctrl Pts',(0.0114480539742393,-0.0336797586670174,
0.0691550804122145));
#80982=CARTESIAN_POINT('Ctrl Pts',(0.0114498320378798,-0.0336825812713142,
0.0691562642247834));
#80983=CARTESIAN_POINT('Ctrl Pts',(0.011453386769613,-0.0336882266065813,
0.0691586336613392));
#80984=CARTESIAN_POINT('Ctrl Pts',(0.0114551634377228,-0.0336910493375859,
0.0691598192853521));
#80985=CARTESIAN_POINT('Ctrl Pts',(0.0114569393964618,-0.033693872113231,
0.0691610058070105));
#80986=CARTESIAN_POINT('Ctrl Pts',(0.0114462752115993,-0.0336769361243754,
0.0691538975048466));
#80987=CARTESIAN_POINT('Ctrl Pts',(0.0114230655246271,-0.0336279007642973,
0.0691887983983469));
#80988=CARTESIAN_POINT('Ctrl Pts',(0.0113995253676171,-0.0335767878888534,
0.0692241962265806));
#80989=CARTESIAN_POINT('Ctrl Pts',(0.0113533932582843,-0.0334733199122758,
0.0692935660477545));
#80990=CARTESIAN_POINT('Ctrl Pts',(0.011330773841734,-0.0334209645148407,
0.0693275793392299));
#80991=CARTESIAN_POINT('Ctrl Pts',(0.0113085902897616,-0.0333679869844681,
0.069360937211991));
#80992=CARTESIAN_POINT('',(0.0114797986472651,-0.0336938721132538,0.069328416529387));
#80993=CARTESIAN_POINT('Origin',(0.00812378219310841,-0.0315241814719618,
0.07415));
#80994=CARTESIAN_POINT('',(0.0114462752108855,-0.0337108120655561,0.0691538975059313));
#80995=CARTESIAN_POINT('',(0.0114355958676053,-0.0336938721132327,0.0691468119977928));
#80996=CARTESIAN_POINT('Origin',(0.00145566079514954,-0.0345562520628783,
0.0821587400759693));
#80997=CARTESIAN_POINT('Ctrl Pts',(0.0114355958676116,-0.0336938721132354,
0.0691468119977896));
#80998=CARTESIAN_POINT('Ctrl Pts',(0.0114373768958059,-0.033691049310948,
0.0691479909328059));
#80999=CARTESIAN_POINT('Ctrl Pts',(0.0114391573452941,-0.0336882265932618,
0.0691491708524663));
#81000=CARTESIAN_POINT('Ctrl Pts',(0.011442717121866,-0.0336825812713166,
0.0691515326847868));
#81001=CARTESIAN_POINT('Ctrl Pts',(0.0114444964489586,-0.0336797586670186,
0.069152714597478));
#81002=CARTESIAN_POINT('Ctrl Pts',(0.0114462752115996,-0.0336769361243751,
0.0691538975048466));
#81003=CARTESIAN_POINT('Origin',(0.00331688607508279,-0.034556251966675,
0.0833964844080882));
#81004=CARTESIAN_POINT('Ctrl Pts',(0.0114415401856491,-0.0342436276873911,
0.0694520635484362));
#81005=CARTESIAN_POINT('Ctrl Pts',(0.0112643545914368,-0.033943005420181,
0.0693269322429318));
#81006=CARTESIAN_POINT('Ctrl Pts',(0.0110782469602823,-0.0336441434784052,
0.0692155027672996));
#81007=CARTESIAN_POINT('Ctrl Pts',(0.0112342441679217,-0.0342436276873911,
0.0693123196361024));
#81008=CARTESIAN_POINT('Ctrl Pts',(0.01105178804517,-0.033943005420181,
0.0691950066287928));
#81009=CARTESIAN_POINT('Ctrl Pts',(0.0108610137647496,-0.0336441434784052,
0.0690917702381949));
#81010=CARTESIAN_POINT('Ctrl Pts',(0.0112321712077444,-0.0342436276873911,
0.069310922196979));
#81011=CARTESIAN_POINT('Ctrl Pts',(0.0110496623797073,-0.033943005420181,
0.0691936873726515));
#81012=CARTESIAN_POINT('Ctrl Pts',(0.0108588414327943,-0.0336441434784052,
0.0690905329129039));
#81013=CARTESIAN_POINT('',(0.0112037525338465,-0.0341934961088741,0.0692928498375926));
#81014=CARTESIAN_POINT('',(0.0110015980565918,-0.0338664212864015,0.0691704115772006));
#81015=CARTESIAN_POINT('Origin',(0.00181571405895566,-0.0345610720403922,
0.0831462926353022));
#81016=CARTESIAN_POINT('Origin',(0.0164887661466842,-0.0336938005072906,
0.0596756914227284));
#81017=CARTESIAN_POINT('',(0.0111091446375892,-0.0336938721132327,0.0692341342496886));
#81018=CARTESIAN_POINT('',(0.0110550314616524,-0.0336938721132427,0.069202861031301));
#81019=CARTESIAN_POINT('',(0.0113085902897661,-0.0340203938281605,0.0693609372119939));
#81020=CARTESIAN_POINT('Origin',(0.00146375648181164,-0.0345589643247137,
0.0828181728425343));
#81021=CARTESIAN_POINT('',(0.0113078380024956,-0.034193496108874,0.0693620684421446));
#81022=CARTESIAN_POINT('Origin',(0.0174098449021397,-0.03419342207177,0.0601863542975626));
#81023=CARTESIAN_POINT('',(0.011255795268181,-0.0341934961088841,0.0693274591398785));
#81024=CARTESIAN_POINT('Ctrl Pts',(0.0116395534704149,-0.0340223579322396,
0.0692879682924021));
#81025=CARTESIAN_POINT('Ctrl Pts',(0.0115724933724561,-0.0339125849573575,
0.0692394766369716));
#81026=CARTESIAN_POINT('Ctrl Pts',(0.0115044767322633,-0.0338030433565231,
0.0691924070442675));
#81027=CARTESIAN_POINT('Ctrl Pts',(0.0114355958676059,-0.0336938721132327,
0.0691468119977926));
#81028=CARTESIAN_POINT('Ctrl Pts',(0.0115289664945347,-0.0340223579322396,
0.069312700874069));
#81029=CARTESIAN_POINT('Ctrl Pts',(0.0114622475233824,-0.0339125849573575,
0.0692657345014588));
#81030=CARTESIAN_POINT('Ctrl Pts',(0.0113946033401003,-0.0338030433565231,
0.0692201820592443));
#81031=CARTESIAN_POINT('Ctrl Pts',(0.0113261256141595,-0.0336938721132327,
0.0691760941329712));
#81032=CARTESIAN_POINT('Ctrl Pts',(0.0114183795186545,-0.0340223579322396,
0.0693374334557359));
#81033=CARTESIAN_POINT('Ctrl Pts',(0.0113520016743087,-0.0339125849573575,
0.0692919923659461));
#81034=CARTESIAN_POINT('Ctrl Pts',(0.0112847299479373,-0.0338030433565231,
0.0692479570742211));
#81035=CARTESIAN_POINT('Ctrl Pts',(0.0112166553607131,-0.0336938721132327,
0.0692053762681498));
#81036=CARTESIAN_POINT('Ctrl Pts',(0.0113077925427743,-0.0340223579322396,
0.0693621660374028));
#81037=CARTESIAN_POINT('Ctrl Pts',(0.0112417558252349,-0.0339125849573575,
0.0693182502304333));
#81038=CARTESIAN_POINT('Ctrl Pts',(0.0111748565557743,-0.0338030433565231,
0.0692757320891979));
#81039=CARTESIAN_POINT('Ctrl Pts',(0.0111071851072667,-0.0336938721132327,
0.0692346584033284));
#81040=CARTESIAN_POINT('',(0.0112723702526072,-0.0336938721132427,0.0691904731237507));
#81041=CARTESIAN_POINT('Ctrl Pts',(0.0114462752088848,-0.0337108120662714,
0.0691538975089284));
#81042=CARTESIAN_POINT('Ctrl Pts',(0.0114224644208348,-0.0337611408993968,
0.0691897022907372));
#81043=CARTESIAN_POINT('Ctrl Pts',(0.0113990881268399,-0.0338121088780606,
0.0692248537147147));
#81044=CARTESIAN_POINT('Ctrl Pts',(0.0113531832314666,-0.0339153382773249,
0.0692938818694883));
#81045=CARTESIAN_POINT('Ctrl Pts',(0.011330674050718,-0.0339675558473115,
0.0693277293970754));
#81046=CARTESIAN_POINT('Ctrl Pts',(0.0113085902897396,-0.0340203938281304,
0.0693609372120242));
#81047=CARTESIAN_POINT('Ctrl Pts',(0.0112041525590857,-0.0341934961088741,
0.0692948381438295));
#81048=CARTESIAN_POINT('Ctrl Pts',(0.0111037759126635,-0.0340287516182428,
0.0692311539132652));
#81049=CARTESIAN_POINT('Ctrl Pts',(0.011000852918602,-0.0338644633275951,
0.069171672742606));
#81050=CARTESIAN_POINT('Ctrl Pts',(0.0112037525338465,-0.0341934961088741,
0.0692928498375927));
#81051=CARTESIAN_POINT('Ctrl Pts',(0.0111033347807592,-0.0340287516182428,
0.0692291738772351));
#81052=CARTESIAN_POINT('Ctrl Pts',(0.0110003710569715,-0.0338644633275951,
0.0691697026686855));
#81053=CARTESIAN_POINT('Ctrl Pts',(0.0111371006348019,-0.0341934961088741,
0.0689615597749468));
#81054=CARTESIAN_POINT('Ctrl Pts',(0.0110298337206636,-0.0340287516182428,
0.0688992617900928));
#81055=CARTESIAN_POINT('Ctrl Pts',(0.0109200836410751,-0.0338644633275951,
0.0688414504606155));
#81056=CARTESIAN_POINT('',(0.0111260111596299,-0.0341764758832402,0.0689551351102066));
#81057=CARTESIAN_POINT('',(0.0111371006348019,-0.034193496108874,0.0689615597749468));
#81058=CARTESIAN_POINT('Origin',(0.0023976043209724,-0.0345621026484597,
0.0830347742799198));
#81059=CARTESIAN_POINT('Ctrl Pts',(0.0111260111605787,-0.0341764758837497,
0.0689551351117523));
#81060=CARTESIAN_POINT('Ctrl Pts',(0.0111045330374642,-0.03412600500405,
0.0689922995090502));
#81061=CARTESIAN_POINT('Ctrl Pts',(0.0110834282878793,-0.0340749269148291,
0.0690288179205656));
#81062=CARTESIAN_POINT('Ctrl Pts',(0.0110419490205638,-0.0339715436306513,
0.0691005909823929));
#81063=CARTESIAN_POINT('Ctrl Pts',(0.0110215902339459,-0.0339192778237239,
0.069135818400637));
#81064=CARTESIAN_POINT('Ctrl Pts',(0.0110015980587762,-0.033866421285529,
0.0691704115771299));
#81065=CARTESIAN_POINT('',(0.0111704265843342,-0.0341934961088841,0.0691272048062798));
#81066=CARTESIAN_POINT('Origin',(0.00812378219310841,-0.0315241814719618,
0.07415));
#81067=CARTESIAN_POINT('',(0.011126011158532,-0.0342105180190558,0.0689551351104245));
#81068=CARTESIAN_POINT('',(0.0111149079858692,-0.0341934961088739,0.0689487341452396));
#81069=CARTESIAN_POINT('Origin',(0.0024339678015844,-0.0345621713328949,
0.0830618326692768));
#81070=CARTESIAN_POINT('Origin',(0.00328436615201417,-0.034562103451728,
0.0835472554685422));
#81071=CARTESIAN_POINT('Origin',(0.00324276790918069,-0.0345621719436217,
0.0835292544665853));
#81072=CARTESIAN_POINT('Ctrl Pts',(0.0111104433623922,-0.0346945769586966,
0.0692348848118891));
#81073=CARTESIAN_POINT('Ctrl Pts',(0.0110074943068725,-0.0345275153362944,
0.0691723279979046));
#81074=CARTESIAN_POINT('Ctrl Pts',(0.0109025512692336,-0.0343603235965186,
0.0691129926565617));
#81075=CARTESIAN_POINT('Ctrl Pts',(0.0107959272325995,-0.034193496108874,
0.0690570496624815));
#81076=CARTESIAN_POINT('Ctrl Pts',(0.0110378595526856,-0.0346945769586966,
0.0691929369998567));
#81077=CARTESIAN_POINT('Ctrl Pts',(0.0109340318834479,-0.0345275153362944,
0.0691319004828274));
#81078=CARTESIAN_POINT('Ctrl Pts',(0.0108282578167764,-0.0343603235965186,
0.0690741134632593));
#81079=CARTESIAN_POINT('Ctrl Pts',(0.0107208527255505,-0.034193496108874,
0.069019742199995));
#81080=CARTESIAN_POINT('Ctrl Pts',(0.0109652757429788,-0.0346945769586966,
0.069150989187823));
#81081=CARTESIAN_POINT('Ctrl Pts',(0.0108605694600231,-0.0345275153362944,
0.0690914729677503));
#81082=CARTESIAN_POINT('Ctrl Pts',(0.0107539643643192,-0.0343603235965186,
0.0690352342699574));
#81083=CARTESIAN_POINT('Ctrl Pts',(0.0106457782185016,-0.034193496108874,
0.0689824347375092));
#81084=CARTESIAN_POINT('Ctrl Pts',(0.0108926919332724,-0.0346945769586966,
0.0691090413757918));
#81085=CARTESIAN_POINT('Ctrl Pts',(0.0107871070365987,-0.0345275153362944,
0.0690510454526731));
#81086=CARTESIAN_POINT('Ctrl Pts',(0.010679670911862,-0.0343603235965186,
0.0689963550766543));
#81087=CARTESIAN_POINT('Ctrl Pts',(0.0105707037114525,-0.034193496108874,
0.0689451272750221));
#81088=CARTESIAN_POINT('',(0.0108926919337969,-0.0346945769586966,0.0691090413760951));
#81089=CARTESIAN_POINT('',(0.0106832484015388,-0.0343667727831467,0.0689995381053479));
#81090=CARTESIAN_POINT('Origin',(0.00295886819440771,-0.0345626457066113,
0.0839330653948164));
#81091=CARTESIAN_POINT('Origin',(0.0156016783748921,-0.0341934771029074,
0.0591020787832341));
#81092=CARTESIAN_POINT('',(0.0107945839423478,-0.034193496108874,0.0690563821289519));
#81093=CARTESIAN_POINT('',(0.0107386138847722,-0.0341934961088839,0.0690285684155482));
#81094=CARTESIAN_POINT('',(0.0110015980579696,-0.0345211942962679,0.0691704115784725));
#81095=CARTESIAN_POINT('Origin',(0.00254423978503176,-0.0345625596119848,
0.0836896027246084));
#81096=CARTESIAN_POINT('',(0.0110009182856956,-0.0346945769586886,0.0691715878128933));
#81097=CARTESIAN_POINT('Origin',(0.0165368126483697,-0.0346945685853955,
0.0595926322947342));
#81098=CARTESIAN_POINT('',(0.0109468051097562,-0.0346945769587026,0.0691403145945042));
#81099=CARTESIAN_POINT('Ctrl Pts',(0.011327325588461,-0.0345231616327842,
0.0690768047825745));
#81100=CARTESIAN_POINT('Ctrl Pts',(0.0112573987348763,-0.0344132092796988,
0.0690326484470979));
#81101=CARTESIAN_POINT('Ctrl Pts',(0.0111865621502266,-0.0343032738558979,
0.0689899407716941));
#81102=CARTESIAN_POINT('Ctrl Pts',(0.0111149079858692,-0.0341934961088739,
0.0689487341452396));
#81103=CARTESIAN_POINT('Ctrl Pts',(0.0112185099925623,-0.0345231616327842,
0.0691084323374537));
#81104=CARTESIAN_POINT('Ctrl Pts',(0.0111490190802936,-0.0344132092796988,
0.0690657758717664));
#81105=CARTESIAN_POINT('Ctrl Pts',(0.0110786494380908,-0.0343032738558979,
0.0690245589716633));
#81106=CARTESIAN_POINT('Ctrl Pts',(0.0110074925701824,-0.0341934961088739,
0.0689848321314887));
#81107=CARTESIAN_POINT('Ctrl Pts',(0.0111096943966636,-0.0345231616327842,
0.0691400598923328));
#81108=CARTESIAN_POINT('Ctrl Pts',(0.0110406394257109,-0.0344132092796988,
0.0690989032964349));
#81109=CARTESIAN_POINT('Ctrl Pts',(0.010970736725955,-0.0343032738558979,
0.0690591771716325));
#81110=CARTESIAN_POINT('Ctrl Pts',(0.0109000771544955,-0.0341934961088739,
0.0690209301177378));
#81111=CARTESIAN_POINT('Ctrl Pts',(0.0110008788007649,-0.0345231616327842,
0.0691716874472119));
#81112=CARTESIAN_POINT('Ctrl Pts',(0.0109322597711282,-0.0344132092796988,
0.0691320307211034));
#81113=CARTESIAN_POINT('Ctrl Pts',(0.0108628240138192,-0.0343032738558979,
0.0690937953716017));
#81114=CARTESIAN_POINT('Ctrl Pts',(0.0107926617388087,-0.0341934961088739,
0.069057028103987));
#81115=CARTESIAN_POINT('',(0.0109547459641185,-0.0341934961088839,0.0690025581371058));
#81116=CARTESIAN_POINT('Ctrl Pts',(0.0111260111567977,-0.0342105180195417,
0.0689551351134124));
#81117=CARTESIAN_POINT('Ctrl Pts',(0.0111045088762136,-0.0342610556240891,
0.0689923412838073));
#81118=CARTESIAN_POINT('Ctrl Pts',(0.0110833924429362,-0.0343122189869276,
0.0690288798087129));
#81119=CARTESIAN_POINT('Ctrl Pts',(0.0110419127606765,-0.0344158119695171,
0.0691006535966165));
#81120=CARTESIAN_POINT('Ctrl Pts',(0.0110215664772404,-0.0344681990450065,
0.0691358595035188));
#81121=CARTESIAN_POINT('Ctrl Pts',(0.0110015980579457,-0.0345211942962475,
0.06917041157849));
#81122=CARTESIAN_POINT('Ctrl Pts',(0.0108932158881468,-0.0346945769586932,
0.0691110001613542));
#81123=CARTESIAN_POINT('Ctrl Pts',(0.0107890381319647,-0.034529677707698,
0.0690537440792977));
#81124=CARTESIAN_POINT('Ctrl Pts',(0.0106825829478883,-0.034364806625142,
0.069000842684242));
#81125=CARTESIAN_POINT('Ctrl Pts',(0.0108926919338048,-0.0346945769586932,
0.0691090413760995));
#81126=CARTESIAN_POINT('Ctrl Pts',(0.0107884736811236,-0.034529677707698,
0.0690517961264283));
#81127=CARTESIAN_POINT('Ctrl Pts',(0.0106819784828642,-0.034364806625142,
0.0689989072282593));
#81128=CARTESIAN_POINT('Ctrl Pts',(0.0108053696819096,-0.0346945769586932,
0.0687825901460849));
#81129=CARTESIAN_POINT('Ctrl Pts',(0.0106944022810373,-0.034529677707698,
0.0687271502221844));
#81130=CARTESIAN_POINT('Ctrl Pts',(0.0105812383174226,-0.034364806625142,
0.0686763440556544));
#81131=CARTESIAN_POINT('',(0.0107938986812547,-0.0346775396664983,0.0687768744726056));
#81132=CARTESIAN_POINT('',(0.0108053696819065,-0.0346945769586886,0.0687825901460834));
#81133=CARTESIAN_POINT('Origin',(0.00354294131826202,-0.034562661799158,
0.0837112814624101));
#81134=CARTESIAN_POINT('Ctrl Pts',(0.0107938986822142,-0.0346775396670097,
0.0687768744741467));
#81135=CARTESIAN_POINT('Ctrl Pts',(0.0107747814676729,-0.034626974992819,
0.0688153444327645));
#81136=CARTESIAN_POINT('Ctrl Pts',(0.0107560040408587,-0.034575790289079,
0.068853130710362));
#81137=CARTESIAN_POINT('Ctrl Pts',(0.0107191131440188,-0.034472168108786,
0.0689273669460453));
#81138=CARTESIAN_POINT('Ctrl Pts',(0.0107010141319057,-0.0344197714289279,
0.0689637877975386));
#81139=CARTESIAN_POINT('Ctrl Pts',(0.0106832484017948,-0.0343667727830644,
0.0689995381053532));
#81140=CARTESIAN_POINT('',(0.0108490308078617,-0.0346945769587026,0.0689458157610992));
#81141=CARTESIAN_POINT('Origin',(0.00812378219310841,-0.0315241814719618,
0.07415));
#81142=CARTESIAN_POINT('',(0.0107938986800678,-0.0347116136489631,0.0687768744733336));
#81143=CARTESIAN_POINT('',(0.0107824154971444,-0.0346945769586886,0.0687711833127828));
#81144=CARTESIAN_POINT('Origin',(0.00358431661738086,-0.0345626693127164,
0.0837297549436195));
#81145=CARTESIAN_POINT('Origin',(0.00326941861635258,-0.0345626624503165,
0.0835753595068454));
#81146=CARTESIAN_POINT('Origin',(0.00322970878627792,-0.0345626699997882,
0.0835535346774191));
#81147=CARTESIAN_POINT('Ctrl Pts',(0.010828755906556,-0.0352450361874068,
0.06907438379749));
#81148=CARTESIAN_POINT('Ctrl Pts',(0.010637325900258,-0.0349452760959493,
0.0689723640398209));
#81149=CARTESIAN_POINT('Ctrl Pts',(0.0104387551808783,-0.034644428984174,
0.0688850534008862));
#81150=CARTESIAN_POINT('Ctrl Pts',(0.0108265018135958,-0.0352450361874068,
0.0690732459530688));
#81151=CARTESIAN_POINT('Ctrl Pts',(0.0106350288927912,-0.0349452760959493,
0.0689713112099108));
#81152=CARTESIAN_POINT('Ctrl Pts',(0.0104364217844615,-0.034644428984174,
0.068884088576466));
#81153=CARTESIAN_POINT('Ctrl Pts',(0.010603324292784,-0.0352450361874068,
0.0689605880895869));
#81154=CARTESIAN_POINT('Ctrl Pts',(0.010407602410936,-0.0349452760959493,
0.0688670706247474));
#81155=CARTESIAN_POINT('Ctrl Pts',(0.0102053924362575,-0.034644428984174,
0.0687885614061507));
#81156=CARTESIAN_POINT('Ctrl Pts',(0.0106010925175759,-0.0352450361874068,
0.0689594615109521));
#81157=CARTESIAN_POINT('Ctrl Pts',(0.0104053281461174,-0.0349452760959493,
0.0688660282188958));
#81158=CARTESIAN_POINT('Ctrl Pts',(0.0102030821427755,-0.034644428984174,
0.0687876061344475));
#81159=CARTESIAN_POINT('',(0.0105707340058111,-0.035195163405333,0.0689451388943784));
#81160=CARTESIAN_POINT('',(0.0103547977016177,-0.0348678972925388,0.0688489911525454));
#81161=CARTESIAN_POINT('Origin',(0.00424649283679008,-0.0345636767883801,
0.0844502499871526));
#81162=CARTESIAN_POINT('Origin',(0.0146411541169871,-0.0346946199340748,
0.0586643881659914));
#81163=CARTESIAN_POINT('',(0.0104694828291501,-0.0346945769330288,0.0688987321984019));
#81164=CARTESIAN_POINT('',(0.0104118767702916,-0.0346945769458128,0.0688744877542892));
#81165=CARTESIAN_POINT('',(0.0106832484017177,-0.0350221583435276,0.0689995381054717));
#81166=CARTESIAN_POINT('Origin',(0.0037889257843654,-0.034562845871725,
0.0843026837793098));
#81167=CARTESIAN_POINT('',(0.0106827006725637,-0.0351951360298761,0.06900064710751));
#81168=CARTESIAN_POINT('Origin',(0.0155863574445573,-0.0351951838366672,
0.059132922238279));
#81169=CARTESIAN_POINT('',(0.0105707037120564,-0.0351951371328749,0.0689451272751924));
#81170=CARTESIAN_POINT('Ctrl Pts',(0.011002454721054,-0.0350241211494343,
0.0688856629594157));
#81171=CARTESIAN_POINT('Ctrl Pts',(0.0109299406367822,-0.0349144232818962,
0.0688460104256449));
#81172=CARTESIAN_POINT('Ctrl Pts',(0.0108565635031284,-0.0348045283579413,
0.0688078330758591));
#81173=CARTESIAN_POINT('Ctrl Pts',(0.0107824154871822,-0.0346945769439158,
0.0687711833078586));
#81174=CARTESIAN_POINT('Ctrl Pts',(0.0108958397411129,-0.0350241211494343,
0.0689240607178794));
#81175=CARTESIAN_POINT('Ctrl Pts',(0.0108238545702202,-0.0349144232818962,
0.0688858767617434));
#81176=CARTESIAN_POINT('Ctrl Pts',(0.0107510370230749,-0.0348045283579413,
0.0688491579355894));
#81177=CARTESIAN_POINT('Ctrl Pts',(0.0106774786195265,-0.0346945769439158,
0.0688139547423621));
#81178=CARTESIAN_POINT('Ctrl Pts',(0.0107892247611718,-0.0350241211494343,
0.068962458476343));
#81179=CARTESIAN_POINT('Ctrl Pts',(0.0107177685036583,-0.0349144232818962,
0.0689257430978419));
#81180=CARTESIAN_POINT('Ctrl Pts',(0.0106455105430213,-0.0348045283579413,
0.0688904827953198));
#81181=CARTESIAN_POINT('Ctrl Pts',(0.0105725417518708,-0.0346945769439158,
0.0688567261768656));
#81182=CARTESIAN_POINT('Ctrl Pts',(0.0106826097812307,-0.0350241211494343,
0.0690008562348067));
#81183=CARTESIAN_POINT('Ctrl Pts',(0.0106116824370963,-0.0349144232818962,
0.0689656094339404));
#81184=CARTESIAN_POINT('Ctrl Pts',(0.0105399840629677,-0.0348045283579413,
0.0689318076550501));
#81185=CARTESIAN_POINT('Ctrl Pts',(0.0104676048842151,-0.0346945769439158,
0.068899497611369));
#81186=CARTESIAN_POINT('',(0.0106259491634536,-0.0346945769458128,0.0688349577556408));
#81187=CARTESIAN_POINT('Ctrl Pts',(0.0107938986785989,-0.034711613649282,
0.068776874476275));
#81188=CARTESIAN_POINT('Ctrl Pts',(0.0107747890444062,-0.0347621546531884,
0.0688153291518623));
#81189=CARTESIAN_POINT('Ctrl Pts',(0.0107560154092216,-0.0348133084096149,
0.0688531076903387));
#81190=CARTESIAN_POINT('Ctrl Pts',(0.0107191244689285,-0.0349168561544585,
0.0689273440219596));
#81191=CARTESIAN_POINT('Ctrl Pts',(0.0107010217966311,-0.0349692089015926,
0.0689637723692235));
#81192=CARTESIAN_POINT('Ctrl Pts',(0.0106832484016836,-0.0350221583435,
0.0689995381054956));
#81193=CARTESIAN_POINT('Ctrl Pts',(0.0105711697600845,-0.0351951371254955,
0.0689465140769634));
#81194=CARTESIAN_POINT('Ctrl Pts',(0.0104635909534011,-0.0350307338980949,
0.068895915874558));
#81195=CARTESIAN_POINT('Ctrl Pts',(0.0103540127938739,-0.0348659306897799,
0.0688498072561803));
#81196=CARTESIAN_POINT('Ctrl Pts',(0.0105707037120127,-0.0351951371254955,
0.0689451272753003));
#81197=CARTESIAN_POINT('Ctrl Pts',(0.010463096234075,-0.0350307338980949,
0.0688945387081464));
#81198=CARTESIAN_POINT('Ctrl Pts',(0.0103534898260282,-0.0348659306897799,
0.0688484409018007));
#81199=CARTESIAN_POINT('Ctrl Pts',(0.0104925935694216,-0.0351951371254955,
0.0687126978711248));
#81200=CARTESIAN_POINT('Ctrl Pts',(0.0103801807593836,-0.0350307338980949,
0.0686637241821611));
#81201=CARTESIAN_POINT('Ctrl Pts',(0.0102658398700227,-0.0348659306897799,
0.0686194384836624));
#81202=CARTESIAN_POINT('Origin',(0.0124177791409169,-0.0308609197410729,
0.0639472399902608));
#81203=CARTESIAN_POINT('',(0.0105366494509915,-0.0351951371254955,0.0688437932956629));
#81204=CARTESIAN_POINT('Origin',(0.00787923681271507,-0.035184046744108,
0.0750960143801669));
#81205=CARTESIAN_POINT('Origin',(0.0120225865149937,-0.0352322613456278,
0.0628375482580576));
#81206=CARTESIAN_POINT('',(0.0101348200888148,-0.0351951142564667,0.0687617218737844));
#81207=CARTESIAN_POINT('',(0.010017094823487,-0.0351951372916786,0.0687206476183941));
#81208=CARTESIAN_POINT('Origin',(0.00779116391085792,-0.0352875111809641,
0.0742229691622023));
#81209=CARTESIAN_POINT('Origin',(0.0146042981700701,-0.0298325076522842,
0.0779312832414659));
#81210=CARTESIAN_POINT('Origin',(0.0136596643096826,-0.0338732158687684,
0.0678567639966745));
#81211=CARTESIAN_POINT('Ctrl Pts',(0.0129181172415396,-0.0321934096636941,
0.0709731324880165));
#81212=CARTESIAN_POINT('Ctrl Pts',(0.0128612528259533,-0.0320508460845115,
0.0708873161737934));
#81213=CARTESIAN_POINT('Ctrl Pts',(0.0128021255712917,-0.0319086045664646,
0.0708030923999977));
#81214=CARTESIAN_POINT('Ctrl Pts',(0.012740877718676,-0.0317669892870252,
0.0707206320341683));
#81215=CARTESIAN_POINT('Ctrl Pts',(0.0128702937786217,-0.0321934096636941,
0.070904260512422));
#81216=CARTESIAN_POINT('Ctrl Pts',(0.0128121965874705,-0.0320508460845115,
0.0708193002154108));
#81217=CARTESIAN_POINT('Ctrl Pts',(0.0127518604862539,-0.0319086045664646,
0.0707359649356342));
#81218=CARTESIAN_POINT('Ctrl Pts',(0.0126894301614559,-0.0317669892870252,
0.0706544234132635));
#81219=CARTESIAN_POINT('Ctrl Pts',(0.012822470315704,-0.0321934096636941,
0.0708353885368273));
#81220=CARTESIAN_POINT('Ctrl Pts',(0.0127631403489876,-0.0320508460845115,
0.0707512842570281));
#81221=CARTESIAN_POINT('Ctrl Pts',(0.0127015954012161,-0.0319086045664646,
0.0706688374712705));
#81222=CARTESIAN_POINT('Ctrl Pts',(0.0126379826042359,-0.0317669892870252,
0.0705882147923585));
#81223=CARTESIAN_POINT('Ctrl Pts',(0.0127746468527862,-0.0321934096636941,
0.0707665165612328));
#81224=CARTESIAN_POINT('Ctrl Pts',(0.0127140841105046,-0.0320508460845115,
0.0706832682986455));
#81225=CARTESIAN_POINT('Ctrl Pts',(0.0126513303161783,-0.0319086045664646,
0.0706017100069068));
#81226=CARTESIAN_POINT('Ctrl Pts',(0.0125865350470158,-0.0317669892870252,
0.0705220061714537));
#81227=CARTESIAN_POINT('',(0.0127755024239863,-0.0321934096636941,0.0707677486944873));
#81228=CARTESIAN_POINT('',(0.0126326164744703,-0.0318665617511315,0.0705794904547992));
#81229=CARTESIAN_POINT('Origin',(-0.00109193559559531,-0.0326371944421813,
0.0800904128854678));
#81230=CARTESIAN_POINT('Origin',(0.0212257461308028,-0.0316939261508822,
0.0637746603378429));
#81231=CARTESIAN_POINT('',(0.0128477245247605,-0.0320197221621845,0.0708694576646901));
#81232=CARTESIAN_POINT('Ctrl Pts',(0.0128476612609758,-0.0320197392094754,
0.0708692838470487));
#81233=CARTESIAN_POINT('Ctrl Pts',(0.0128309678839123,-0.031979271657605,
0.0708452472584388));
#81234=CARTESIAN_POINT('Ctrl Pts',(0.0128140152669662,-0.0319386439829738,
0.0708212285097176));
#81235=CARTESIAN_POINT('Ctrl Pts',(0.0127967787033311,-0.0318979099381669,
0.0707972072627064));
#81236=CARTESIAN_POINT('Ctrl Pts',(0.0127795424803885,-0.0318571766984965,
0.0707731864904916));
#81237=CARTESIAN_POINT('Ctrl Pts',(0.0127621113752979,-0.0318163871833607,
0.0707492842706211));
#81238=CARTESIAN_POINT('Ctrl Pts',(0.0127445481888604,-0.0317755399638303,
0.0707255807421288));
#81239=CARTESIAN_POINT('',(0.0128467975774529,-0.0321934096636184,0.0708704229420174));
#81240=CARTESIAN_POINT('Origin',(0.0147312197857156,-0.0324113359903585,
0.0695363024491413));
#81241=CARTESIAN_POINT('',(0.0128111500007296,-0.0321934096636663,0.0708190858182624));
#81242=CARTESIAN_POINT('Ctrl Pts',(0.0127751424003961,-0.0321934096636617,
0.0707697447081129));
#81243=CARTESIAN_POINT('Ctrl Pts',(0.0127285260455041,-0.0320835708272592,
0.0707055988257963));
#81244=CARTESIAN_POINT('Ctrl Pts',(0.0126806092342916,-0.0319739230346488,
0.07064245487374));
#81245=CARTESIAN_POINT('Ctrl Pts',(0.0126314594732712,-0.0318646057455572,
0.0705803889351675));
#81246=CARTESIAN_POINT('Ctrl Pts',(0.0127952572874932,-0.0321934096636617,
0.0706582254000018));
#81247=CARTESIAN_POINT('Ctrl Pts',(0.0127471029944293,-0.0320835708272592,
0.0705938021177154));
#81248=CARTESIAN_POINT('Ctrl Pts',(0.0126976433963337,-0.0319739230346488,
0.0705304127541433));
#81249=CARTESIAN_POINT('Ctrl Pts',(0.0126469479977051,-0.0318646057455572,
0.0704681335550053));
#81250=CARTESIAN_POINT('Ctrl Pts',(0.0128153721745904,-0.0321934096636617,
0.0705467060918906));
#81251=CARTESIAN_POINT('Ctrl Pts',(0.0127656799433545,-0.0320835708272592,
0.0704820054096346));
#81252=CARTESIAN_POINT('Ctrl Pts',(0.0127146775583757,-0.0319739230346488,
0.0704183706345465));
#81253=CARTESIAN_POINT('Ctrl Pts',(0.0126624365221389,-0.0318646057455573,
0.070355878174843));
#81254=CARTESIAN_POINT('Ctrl Pts',(0.0128354870616876,-0.0321934096636617,
0.0704351867837794));
#81255=CARTESIAN_POINT('Ctrl Pts',(0.0127842568922798,-0.0320835708272592,
0.0703702087015537));
#81256=CARTESIAN_POINT('Ctrl Pts',(0.0127317117204177,-0.0319739230346488,
0.0703063285149497));
#81257=CARTESIAN_POINT('Ctrl Pts',(0.0126779250465728,-0.0318646057455573,
0.0702436227946807));
#81258=CARTESIAN_POINT('',(0.0128275414038829,-0.0321763980308272,0.0704251309734677));
#81259=CARTESIAN_POINT('',(0.0128354870616674,-0.0321934096636184,0.0704351867837538));
#81260=CARTESIAN_POINT('Origin',(-0.00051713526300068,-0.0326386231325254,
0.080210103995993));
#81261=CARTESIAN_POINT('Ctrl Pts',(0.0128275414013882,-0.0321763980306274,
0.0704251309754336));
#81262=CARTESIAN_POINT('Ctrl Pts',(0.0127938947113604,-0.0321259596174857,
0.0704517755182162));
#81263=CARTESIAN_POINT('Ctrl Pts',(0.0127608309939017,-0.0320749164631472,
0.0704779584097262));
#81264=CARTESIAN_POINT('Ctrl Pts',(0.0126958428954888,-0.0319716057793956,
0.0705294219613292));
#81265=CARTESIAN_POINT('Ctrl Pts',(0.0126639438360868,-0.0319193786690155,
0.0705546825694891));
#81266=CARTESIAN_POINT('Ctrl Pts',(0.0126326164730091,-0.0318665617525358,
0.0705794904559439));
#81267=CARTESIAN_POINT('',(0.0128054947428368,-0.0321934096636663,0.0706014677391306));
#81268=CARTESIAN_POINT('Origin',(0.00812378219310841,-0.0315241814719618,
0.07415));
#81269=CARTESIAN_POINT('',(0.0128275414041736,-0.0322104233323615,0.070425130973237));
#81270=CARTESIAN_POINT('',(0.0128195742877292,-0.0321934096636183,0.070415092155874));
#81271=CARTESIAN_POINT('Origin',(-0.000494217309984561,-0.0326387239311533,
0.0802492176941288));
#81272=CARTESIAN_POINT('Origin',(0.000244603150060192,-0.032638623943266,
0.0811720287119732));
#81273=CARTESIAN_POINT('Origin',(0.000211785609694622,-0.0326387246802686,
0.0811407543132531));
#81274=CARTESIAN_POINT('Ctrl Pts',(0.012730879852634,-0.0327445246967096,
0.0707072138963343));
#81275=CARTESIAN_POINT('Ctrl Pts',(0.0126010330520267,-0.0324436878339359,
0.0705334543675219));
#81276=CARTESIAN_POINT('Ctrl Pts',(0.012458466854592,-0.0321434074405927,
0.0703699690628913));
#81277=CARTESIAN_POINT('Ctrl Pts',(0.0125769117294142,-0.0327445246967096,
0.0705102524355553));
#81278=CARTESIAN_POINT('Ctrl Pts',(0.0124396364058737,-0.0324436878339359,
0.0703422999094418));
#81279=CARTESIAN_POINT('Ctrl Pts',(0.0122901001963318,-0.0321434074405927,
0.0701851646571368));
#81280=CARTESIAN_POINT('',(0.0125539500000773,-0.0326943950436612,0.0704823388648763));
#81281=CARTESIAN_POINT('',(0.0123995251713282,-0.0323666188837389,0.0703034239921451));
#81282=CARTESIAN_POINT('Origin',(-0.000346617892861598,-0.0326395579109293,
0.0812611795379471));
#81283=CARTESIAN_POINT('Origin',(0.0206104378674234,-0.0321933825603114,
0.062916659848448));
#81284=CARTESIAN_POINT('',(0.0124821166624009,-0.0321934096532689,0.0703972615797893));
#81285=CARTESIAN_POINT('',(0.0124403159281592,-0.0321934096584275,0.0703507970883738));
#81286=CARTESIAN_POINT('',(0.0126326164752063,-0.0325210109756239,0.0705794904542097));
#81287=CARTESIAN_POINT('Origin',(-0.000633262491841339,-0.0326393129156863,
0.0808751493528338));
#81288=CARTESIAN_POINT('',(0.012631551438155,-0.0326943950436593,0.0705803338484653));
#81289=CARTESIAN_POINT('Origin',(0.021304072888729,-0.0326943765538186,
0.0637126349329132));
#81290=CARTESIAN_POINT('',(0.0125927507191262,-0.0326943950436702,0.0705313363566808));
#81291=CARTESIAN_POINT('Ctrl Pts',(0.0129699293209419,-0.0325229783203769,
0.0706123654774067));
#81292=CARTESIAN_POINT('Ctrl Pts',(0.0129211631064109,-0.032413025309245,
0.0705455614452278));
#81293=CARTESIAN_POINT('Ctrl Pts',(0.0128710223610104,-0.0323031222208069,
0.0704797763369814));
#81294=CARTESIAN_POINT('Ctrl Pts',(0.0128195742849418,-0.0321934096576658,
0.0704150921523647));
#81295=CARTESIAN_POINT('Ctrl Pts',(0.0128571122325598,-0.0325229783203769,
0.0706017143363639));
#81296=CARTESIAN_POINT('Ctrl Pts',(0.0128081991922824,-0.032413025309245,
0.0705364654852812));
#81297=CARTESIAN_POINT('Ctrl Pts',(0.0127579438143233,-0.0323031222208069,
0.0704722383595365));
#81298=CARTESIAN_POINT('Ctrl Pts',(0.0127064133752996,-0.0321934096576658,
0.0704091129579808));
#81299=CARTESIAN_POINT('Ctrl Pts',(0.0127442951441776,-0.0325229783203769,
0.0705910631953211));
#81300=CARTESIAN_POINT('Ctrl Pts',(0.0126952352781539,-0.032413025309245,
0.0705273695253346));
#81301=CARTESIAN_POINT('Ctrl Pts',(0.0126448652676362,-0.0323031222208069,
0.0704647003820916));
#81302=CARTESIAN_POINT('Ctrl Pts',(0.0125932524656573,-0.0321934096576658,
0.0704031337635969));
#81303=CARTESIAN_POINT('Ctrl Pts',(0.0126314780557955,-0.0325229783203769,
0.0705804120542783));
#81304=CARTESIAN_POINT('Ctrl Pts',(0.0125822713640254,-0.032413025309245,
0.070518273565388));
#81305=CARTESIAN_POINT('Ctrl Pts',(0.0125317867209491,-0.0323031222208069,
0.0704571624046467));
#81306=CARTESIAN_POINT('Ctrl Pts',(0.0124800915560151,-0.0321934096576658,
0.0703971545692129));
#81307=CARTESIAN_POINT('',(0.0126508454754985,-0.0321934096584275,0.0704061768681168));
#81308=CARTESIAN_POINT('Ctrl Pts',(0.0128275414014406,-0.0322104233328928,
0.0704251309753922));
#81309=CARTESIAN_POINT('Ctrl Pts',(0.0127938491196484,-0.0322609421830675,
0.0704518116219258));
#81310=CARTESIAN_POINT('Ctrl Pts',(0.0127607631298716,-0.0323120888239297,
0.0704780121506965));
#81311=CARTESIAN_POINT('Ctrl Pts',(0.0126957745393272,-0.0324156524631819,
0.0705294760920144));
#81312=CARTESIAN_POINT('Ctrl Pts',(0.0126638986524107,-0.032468026716732,
0.0705547183500784));
#81313=CARTESIAN_POINT('Ctrl Pts',(0.0126326164751696,-0.0325210109755912,
0.0705794904542332));
#81314=CARTESIAN_POINT('Origin',(0.0122298385122406,-0.0262834582511817,
0.0808614594048683));
#81315=CARTESIAN_POINT('Origin',(0.0200250990363695,-0.0342770846373871,
0.0716635617413367));
#81316=CARTESIAN_POINT('Ctrl Pts',(0.0125537160743714,-0.0326943950436604,
0.0704843530569219));
#81317=CARTESIAN_POINT('Ctrl Pts',(0.0125031965893412,-0.0325844576448134,
0.0704233002654571));
#81318=CARTESIAN_POINT('Ctrl Pts',(0.0124514108571436,-0.0324744968375322,
0.0703632879789696));
#81319=CARTESIAN_POINT('Ctrl Pts',(0.0123984262892402,-0.0323646534831894,
0.0703043921735224));
#81320=CARTESIAN_POINT('Ctrl Pts',(0.0125667888951122,-0.0326943950436604,
0.0703717909454488));
#81321=CARTESIAN_POINT('Ctrl Pts',(0.012514718093222,-0.0325844576448134,
0.0703105579860131));
#81322=CARTESIAN_POINT('Ctrl Pts',(0.0124613772082064,-0.0324744968375322,
0.0702503976025801));
#81323=CARTESIAN_POINT('Ctrl Pts',(0.0124068356466964,-0.0323646534831894,
0.0701913859334797));
#81324=CARTESIAN_POINT('Ctrl Pts',(0.0125798617158531,-0.0326943950436604,
0.0702592288339757));
#81325=CARTESIAN_POINT('Ctrl Pts',(0.0125262395971029,-0.0325844576448134,
0.0701978157065692));
#81326=CARTESIAN_POINT('Ctrl Pts',(0.0124713435592691,-0.0324744968375322,
0.0701375072261906));
#81327=CARTESIAN_POINT('Ctrl Pts',(0.0124152450041526,-0.0323646534831894,
0.0700783796934372));
#81328=CARTESIAN_POINT('Ctrl Pts',(0.0125929345365939,-0.0326943950436604,
0.0701466667225027));
#81329=CARTESIAN_POINT('Ctrl Pts',(0.0125377611009837,-0.0325844576448134,
0.0700850734271252));
#81330=CARTESIAN_POINT('Ctrl Pts',(0.0124813099103318,-0.0324744968375322,
0.0700246168498011));
#81331=CARTESIAN_POINT('Ctrl Pts',(0.0124236543616088,-0.0323646534831894,
0.0699653734533945));
#81332=CARTESIAN_POINT('',(0.0125843731483486,-0.0326773559991344,0.070137129666905));
#81333=CARTESIAN_POINT('',(0.0125929345365934,-0.0326943950436594,0.0701466667225021));
#81334=CARTESIAN_POINT('Origin',(0.000273182598529205,-0.0326395671180591,
0.081280194740831));
#81335=CARTESIAN_POINT('Ctrl Pts',(0.0125843731458498,-0.0326773559987417,
0.0701371296691427));
#81336=CARTESIAN_POINT('Ctrl Pts',(0.0125524401977528,-0.0326267922585975,
0.0701658574277184));
#81337=CARTESIAN_POINT('Ctrl Pts',(0.012521073238102,-0.0325756109579366,
0.0701940760075177));
#81338=CARTESIAN_POINT('Ctrl Pts',(0.012459444600851,-0.032471998546237,
0.0702495188249775));
#81339=CARTESIAN_POINT('Ctrl Pts',(0.0124292076408168,-0.0324196091621768,
0.0702767208260358));
#81340=CARTESIAN_POINT('Ctrl Pts',(0.012399525171292,-0.0323666188837756,
0.0703034239921777));
#81341=CARTESIAN_POINT('',(0.0125734422683454,-0.0326943950436702,0.0703145027936992));
#81342=CARTESIAN_POINT('Origin',(0.00812378219310841,-0.0315241814719618,
0.07415));
#81343=CARTESIAN_POINT('',(0.0125843731483153,-0.0327114338380057,0.0701371296669343));
#81344=CARTESIAN_POINT('',(0.0125757914107548,-0.0326943950436593,0.070127610918123));
#81345=CARTESIAN_POINT('Origin',(0.000304059173981302,-0.032639567556057,
0.0813133555451849));
#81346=CARTESIAN_POINT('Origin',(0.000205979022221549,-0.032639567528189,
0.0812054949052792));
#81347=CARTESIAN_POINT('Origin',(0.000176258798741688,-0.0326395682305313,
0.0811712942880879));
#81348=CARTESIAN_POINT('Ctrl Pts',(0.0125055890636029,-0.0332451089994434,
0.0704246955091312));
#81349=CARTESIAN_POINT('Ctrl Pts',(0.012365086905994,-0.0329451141710254,
0.0702594329591735));
#81350=CARTESIAN_POINT('Ctrl Pts',(0.0122125356493249,-0.0326442513127493,
0.0701052230995668));
#81351=CARTESIAN_POINT('Ctrl Pts',(0.0123395561741835,-0.0332451089994434,
0.0702377915775753));
#81352=CARTESIAN_POINT('Ctrl Pts',(0.0121920048194651,-0.0329451141710254,
0.0700787910604944));
#81353=CARTESIAN_POINT('Ctrl Pts',(0.0120328960736271,-0.0326442513127493,
0.0699313564183334));
#81354=CARTESIAN_POINT('',(0.0123149137277534,-0.0331951640388616,0.0702114036181268));
#81355=CARTESIAN_POINT('',(0.0121495594633191,-0.0328677532092642,0.0700425382082537));
#81356=CARTESIAN_POINT('Origin',(0.000637477768746615,-0.0326401908898243,
0.0822392685832872));
#81357=CARTESIAN_POINT('Origin',(0.0198883945788821,-0.0326944279134316,
0.0621466781364469));
#81358=CARTESIAN_POINT('',(0.0122378800854608,-0.0326943950436593,0.0701310046613436));
#81359=CARTESIAN_POINT('',(0.0121932443076082,-0.0326943950436694,0.070087256548999));
#81360=CARTESIAN_POINT('',(0.0123995251713301,-0.0330220786163546,0.0703034239921472));
#81361=CARTESIAN_POINT('Origin',(0.000272764073846864,-0.0326396682762954,
0.0819258092225879));
#81362=CARTESIAN_POINT('',(0.0123985151930507,-0.0331951640388588,0.0703043325963879));
#81363=CARTESIAN_POINT('Origin',(0.0205997976903381,-0.0331952026560079,
0.0629262342684439));
#81364=CARTESIAN_POINT('',(0.0123567144604121,-0.0331951640388701,0.0702578681072674));
#81365=CARTESIAN_POINT('Ctrl Pts',(0.0127382360328429,-0.0330240426238172,
0.0703150533561725));
#81366=CARTESIAN_POINT('Ctrl Pts',(0.0126854059066167,-0.032914277406352,
0.0702514847588856));
#81367=CARTESIAN_POINT('Ctrl Pts',(0.0126312353021698,-0.0328043479726692,
0.0701889766166173));
#81368=CARTESIAN_POINT('Ctrl Pts',(0.0125757914107584,-0.0326943950436594,
0.0701276109181229));
#81369=CARTESIAN_POINT('Ctrl Pts',(0.0126249727995383,-0.0330240426238172,
0.070311507095317));
#81370=CARTESIAN_POINT('Ctrl Pts',(0.0125720938201138,-0.032914277406352,
0.0702494988094159));
#81371=CARTESIAN_POINT('Ctrl Pts',(0.0125179065941085,-0.0328043479726692,
0.0701885527663376));
#81372=CARTESIAN_POINT('Ctrl Pts',(0.0124624783891836,-0.0326943950436594,
0.0701287489542584));
#81373=CARTESIAN_POINT('Ctrl Pts',(0.0125117095662337,-0.0330240426238172,
0.0703079608344614));
#81374=CARTESIAN_POINT('Ctrl Pts',(0.012458781733611,-0.032914277406352,
0.0702475128599461));
#81375=CARTESIAN_POINT('Ctrl Pts',(0.0124045778860471,-0.0328043479726691,
0.0701881289160579));
#81376=CARTESIAN_POINT('Ctrl Pts',(0.0123491653676087,-0.0326943950436594,
0.0701298869903938));
#81377=CARTESIAN_POINT('Ctrl Pts',(0.012398446332929,-0.0330240426238172,
0.0703044145736059));
#81378=CARTESIAN_POINT('Ctrl Pts',(0.0123454696471081,-0.032914277406352,
0.0702455269104764));
#81379=CARTESIAN_POINT('Ctrl Pts',(0.0122912491779858,-0.0328043479726691,
0.0701877050657782));
#81380=CARTESIAN_POINT('Ctrl Pts',(0.0122358523460338,-0.0326943950436594,
0.0701310250265293));
#81381=CARTESIAN_POINT('',(0.0124068357481178,-0.0326943950436693,0.0701293077897432));
#81382=CARTESIAN_POINT('Ctrl Pts',(0.0125843731458447,-0.0327114338383328,
0.0701371296691474));
#81383=CARTESIAN_POINT('Ctrl Pts',(0.0125524455092796,-0.032761987683039,
0.0701658526493228));
#81384=CARTESIAN_POINT('Ctrl Pts',(0.0125210811440439,-0.0328131562603137,
0.0701940688951149));
#81385=CARTESIAN_POINT('Ctrl Pts',(0.0124594525633205,-0.0329167375858776,
0.070249511661721));
#81386=CARTESIAN_POINT('Ctrl Pts',(0.01242921290394,-0.0329691088920628,
0.0702767160911853));
#81387=CARTESIAN_POINT('Ctrl Pts',(0.0123995251712929,-0.0330220786163187,
0.070303423992177));
#81388=CARTESIAN_POINT('Ctrl Pts',(0.0123148067187297,-0.0331951640388604,
0.0702134288472416));
#81389=CARTESIAN_POINT('Ctrl Pts',(0.0122605884084061,-0.0330855618127442,
0.0701557059560538));
#81390=CARTESIAN_POINT('Ctrl Pts',(0.012205137979225,-0.032975722417194,
0.0700990620531625));
#81391=CARTESIAN_POINT('Ctrl Pts',(0.0121485228807675,-0.0328657861694598,
0.0700435731575748));
#81392=CARTESIAN_POINT('Ctrl Pts',(0.0123207859154805,-0.0331951640388604,
0.0701002678944106));
#81393=CARTESIAN_POINT('Ctrl Pts',(0.0122650090417729,-0.0330855618127442,
0.0700424626518737));
#81394=CARTESIAN_POINT('Ctrl Pts',(0.0122079972235993,-0.032975722417194,
0.0699857685511122));
#81395=CARTESIAN_POINT('Ctrl Pts',(0.0121498199068405,-0.0328657861694598,
0.0699302617734918));
#81396=CARTESIAN_POINT('Ctrl Pts',(0.0123267651122312,-0.0331951640388604,
0.0699871069415795));
#81397=CARTESIAN_POINT('Ctrl Pts',(0.0122694296751397,-0.0330855618127442,
0.0699292193476936));
#81398=CARTESIAN_POINT('Ctrl Pts',(0.0122108564679736,-0.032975722417194,
0.0698724750490619));
#81399=CARTESIAN_POINT('Ctrl Pts',(0.0121511169329135,-0.0328657861694598,
0.0698169503894089));
#81400=CARTESIAN_POINT('Ctrl Pts',(0.012332744308982,-0.0331951640388604,
0.0698739459887484));
#81401=CARTESIAN_POINT('Ctrl Pts',(0.0122738503085065,-0.0330855618127442,
0.0698159760435136));
#81402=CARTESIAN_POINT('Ctrl Pts',(0.0122137157123479,-0.032975722417194,
0.0697591815470117));
#81403=CARTESIAN_POINT('Ctrl Pts',(0.0121524139589865,-0.0328657861694598,
0.069703639005326));
#81404=CARTESIAN_POINT('',(0.0123236009781538,-0.0331781648279009,0.0698649653262148));
#81405=CARTESIAN_POINT('',(0.0123327443089812,-0.0331951640388588,0.0698739459887476));
#81406=CARTESIAN_POINT('Origin',(0.00127792040768298,-0.0326412092999731,
0.0821523339323979));
#81407=CARTESIAN_POINT('Ctrl Pts',(0.0123236009756894,-0.0331781648273353,
0.0698649653287185));
#81408=CARTESIAN_POINT('Ctrl Pts',(0.0122935140830046,-0.0331276810207345,
0.0698956626956716));
#81409=CARTESIAN_POINT('Ctrl Pts',(0.0122639706921897,-0.0330765665168817,
0.0699258055328992));
#81410=CARTESIAN_POINT('Ctrl Pts',(0.0122059446106328,-0.0329730612715187,
0.0699850089852818));
#81411=CARTESIAN_POINT('Ctrl Pts',(0.0121774859444844,-0.0329207135598912,
0.0700140450883752));
#81412=CARTESIAN_POINT('Ctrl Pts',(0.0121495594632872,-0.0328677532092985,
0.0700425382082862));
#81413=CARTESIAN_POINT('',(0.0123238290183773,-0.0331951640388702,0.0700426748034472));
#81414=CARTESIAN_POINT('Origin',(0.00812378219310841,-0.0315241814719618,
0.07415));
#81415=CARTESIAN_POINT('',(0.0123236009778316,-0.0332121607144425,0.0698649653265427));
#81416=CARTESIAN_POINT('',(0.0123144384873285,-0.0331951640388587,0.0698560042124233));
#81417=CARTESIAN_POINT('Origin',(0.00131530656577935,-0.0326413659023442,
0.0821779943499873));
#81418=CARTESIAN_POINT('Origin',(0.000260558269677515,-0.0326412097716166,
0.0811552055021783));
#81419=CARTESIAN_POINT('Origin',(0.000234154020173135,-0.03264136646171,
0.0811183405156123));
#81420=CARTESIAN_POINT('Ctrl Pts',(0.0122630432273274,-0.0337436976235975,
0.0701569256091833));
#81421=CARTESIAN_POINT('Ctrl Pts',(0.0122271289110894,-0.0336723290703325,
0.0701196964681194));
#81422=CARTESIAN_POINT('Ctrl Pts',(0.0121905507700376,-0.033601104548885,
0.0700831193352028));
#81423=CARTESIAN_POINT('Ctrl Pts',(0.0120737640113806,-0.0333736987606857,
0.0699663357953221));
#81424=CARTESIAN_POINT('Ctrl Pts',(0.0119504679951764,-0.0331450831799192,
0.0698564466030744));
#81425=CARTESIAN_POINT('Ctrl Pts',(0.0120856028087995,-0.0337436976235975,
0.069980815138533));
#81426=CARTESIAN_POINT('Ctrl Pts',(0.0120481045282982,-0.0336723290703325,
0.0699451819234852));
#81427=CARTESIAN_POINT('Ctrl Pts',(0.01200997138491,-0.033601104548885,
0.069910228948926));
#81428=CARTESIAN_POINT('Ctrl Pts',(0.0118882198118214,-0.0333736987606857,
0.0697986310249529));
#81429=CARTESIAN_POINT('Ctrl Pts',(0.0117602647433478,-0.0331450831799192,
0.0696942038128069));
#81430=CARTESIAN_POINT('Ctrl Pts',(0.0120838284046142,-0.0337436976235975,
0.0699790540338265));
#81431=CARTESIAN_POINT('Ctrl Pts',(0.0120463142844703,-0.0336723290703325,
0.0699434367780388));
#81432=CARTESIAN_POINT('Ctrl Pts',(0.0120081655910587,-0.033601104548885,
0.0699085000450632));
#81433=CARTESIAN_POINT('Ctrl Pts',(0.0118863643698258,-0.0333736987606857,
0.0697969539772491));
#81434=CARTESIAN_POINT('Ctrl Pts',(0.0117583627108295,-0.0331450831799192,
0.0696925813849042));
#81435=CARTESIAN_POINT('',(0.0120593369739985,-0.0336938721132548,0.069956012211914));
#81436=CARTESIAN_POINT('',(0.0118837058461226,-0.0333679869945434,0.0697978626947793));
#81437=CARTESIAN_POINT('Ctrl Pts',(0.0120593369740092,-0.0336938721132648,
0.0699560122119234));
#81438=CARTESIAN_POINT('Ctrl Pts',(0.0120429658722373,-0.0336629187933931,
0.0699406498954123));
#81439=CARTESIAN_POINT('Ctrl Pts',(0.0120265100537939,-0.0336319952301039,
0.0699253883515189));
#81440=CARTESIAN_POINT('Ctrl Pts',(0.0120099713849204,-0.0336011045488949,
0.0699102289489357));
#81441=CARTESIAN_POINT('Ctrl Pts',(0.0119684702055025,-0.0335235892595452,
0.069872188820599));
#81442=CARTESIAN_POINT('Ctrl Pts',(0.0119263734892345,-0.0334458668660368,
0.0698347243718573));
#81443=CARTESIAN_POINT('Ctrl Pts',(0.0118837058463353,-0.0333679869945384,
0.0697978626945436));
#81444=CARTESIAN_POINT('Ctrl Pts',(0.0118836726444111,-0.0333679692459107,
0.0697978331022651));
#81445=CARTESIAN_POINT('Ctrl Pts',(0.0118833808434531,-0.0333391895375576,
0.069798179930783));
#81446=CARTESIAN_POINT('Ctrl Pts',(0.0118831646091521,-0.0333104081063368,
0.0697984419862041));
#81447=CARTESIAN_POINT('Ctrl Pts',(0.0118828826583311,-0.0332532698941694,
0.0697987923858657));
#81448=CARTESIAN_POINT('Ctrl Pts',(0.0118828147431512,-0.0332249174808968,
0.0697988832651797));
#81449=CARTESIAN_POINT('Ctrl Pts',(0.0118828175663909,-0.0331960985220354,
0.0697988905547451));
#81450=CARTESIAN_POINT('Ctrl Pts',(0.0118828176314533,-0.033195631270599,
0.0697988906502747));
#81451=CARTESIAN_POINT('Ctrl Pts',(0.0118828177156373,-0.0331951640388596,
0.0697988907230034));
#81452=CARTESIAN_POINT('',(0.0119774070477464,-0.0331951640388587,0.069880608886537));
#81453=CARTESIAN_POINT('',(0.0119301123817021,-0.0331951640388687,0.0698397498047804));
#81454=CARTESIAN_POINT('',(0.0121495594631661,-0.0335216366567703,0.0700425382086595));
#81455=CARTESIAN_POINT('Origin',(0.00138764190188798,-0.0326434571528776,
0.0827528409360664));
#81456=CARTESIAN_POINT('',(0.0121486085297355,-0.0336938721132327,0.0700435084366343));
#81457=CARTESIAN_POINT('Origin',(0.0197926776181876,-0.0336938867896162,
0.0622443393975074));
#81458=CARTESIAN_POINT('',(0.012103972751877,-0.0336938721132538,0.0699997603242842));
#81459=CARTESIAN_POINT('Ctrl Pts',(0.0124883315106566,-0.0335235895815172,
0.0700328760943192));
#81460=CARTESIAN_POINT('Ctrl Pts',(0.0124316511942238,-0.0334144449262749,
0.0699727894799563));
#81461=CARTESIAN_POINT('Ctrl Pts',(0.012373664414742,-0.0333049234473147,
0.069913804806034));
#81462=CARTESIAN_POINT('Ctrl Pts',(0.0123144384873313,-0.0331951640388587,
0.0698560042124231));
#81463=CARTESIAN_POINT('Ctrl Pts',(0.0123750689445051,-0.0335235895815172,
0.070036448711682));
#81464=CARTESIAN_POINT('Ctrl Pts',(0.0123184378121842,-0.0334144449262749,
0.0699779213795356));
#81465=CARTESIAN_POINT('Ctrl Pts',(0.0122605324869179,-0.0333049234473147,
0.0699204967631495));
#81466=CARTESIAN_POINT('Ctrl Pts',(0.0122014203603723,-0.0331951640388587,
0.0698642549981249));
#81467=CARTESIAN_POINT('Ctrl Pts',(0.0122618063783537,-0.0335235895815173,
0.0700400213290447));
#81468=CARTESIAN_POINT('Ctrl Pts',(0.0122052244301446,-0.0334144449262749,
0.0699830532791149));
#81469=CARTESIAN_POINT('Ctrl Pts',(0.0121474005590938,-0.0333049234473147,
0.0699271887202649));
#81470=CARTESIAN_POINT('Ctrl Pts',(0.0120884022334132,-0.0331951640388587,
0.0698725057838268));
#81471=CARTESIAN_POINT('Ctrl Pts',(0.0121485438122022,-0.0335235895815173,
0.0700435939464075));
#81472=CARTESIAN_POINT('Ctrl Pts',(0.012092011048105,-0.0334144449262749,
0.0699881851786942));
#81473=CARTESIAN_POINT('Ctrl Pts',(0.0120342686312697,-0.0333049234473147,
0.0699338806773804));
#81474=CARTESIAN_POINT('Ctrl Pts',(0.0119753841064541,-0.0331951640388587,
0.0698807565695286));
#81475=CARTESIAN_POINT('',(0.0121459227675475,-0.0331951640388687,0.0698683065494902));
#81476=CARTESIAN_POINT('Ctrl Pts',(0.0123236009756333,-0.0332121607145988,
0.0698649653287758));
#81477=CARTESIAN_POINT('Ctrl Pts',(0.0122935647852482,-0.0332625444109243,
0.0698956109646606));
#81478=CARTESIAN_POINT('Ctrl Pts',(0.0122640461655568,-0.0333135300745759,
0.0699257285281495));
#81479=CARTESIAN_POINT('Ctrl Pts',(0.0122060206359464,-0.0334167203140609,
0.0699849314173864));
#81480=CARTESIAN_POINT('Ctrl Pts',(0.012177536199884,-0.0334688847587289,
0.0700139938132749));
#81481=CARTESIAN_POINT('Ctrl Pts',(0.0121495594625472,-0.0335216366562355,
0.0700425382090413));
#81482=CARTESIAN_POINT('Ctrl Pts',(0.0120593470153702,-0.033693872113239,
0.0699570120189169));
#81483=CARTESIAN_POINT('Ctrl Pts',(0.012034804065336,-0.0336474569764958,
0.0699339758520533));
#81484=CARTESIAN_POINT('Ctrl Pts',(0.0120099931295819,-0.033601104548885,
0.0699112285698606));
#81485=CARTESIAN_POINT('Ctrl Pts',(0.0119471775446443,-0.0334837508592656,
0.0698536376812768));
#81486=CARTESIAN_POINT('Ctrl Pts',(0.0118826830062478,-0.0333660264659097,
0.0697979334383868));
#81487=CARTESIAN_POINT('Ctrl Pts',(0.0120593369740134,-0.0336938721132391,
0.0699560122119281));
#81488=CARTESIAN_POINT('Ctrl Pts',(0.0120347881717771,-0.0336474569764958,
0.0699329761038399));
#81489=CARTESIAN_POINT('Ctrl Pts',(0.01200997138491,-0.033601104548885,
0.069910228948926));
#81490=CARTESIAN_POINT('Ctrl Pts',(0.0119471409862994,-0.0334837508592656,
0.0698526383825828));
#81491=CARTESIAN_POINT('Ctrl Pts',(0.0118826316502837,-0.0333660264659097,
0.0697969349007517));
#81492=CARTESIAN_POINT('Ctrl Pts',(0.0120559228683337,-0.0336938721132391,
0.0696160734186727));
#81493=CARTESIAN_POINT('Ctrl Pts',(0.0120293842915368,-0.0336474569764958,
0.0695930572944779));
#81494=CARTESIAN_POINT('Ctrl Pts',(0.0120025781003864,-0.033601104548885,
0.0695703534149116));
#81495=CARTESIAN_POINT('Ctrl Pts',(0.0119347109875234,-0.0334837508592656,
0.0695128724117991));
#81496=CARTESIAN_POINT('Ctrl Pts',(0.0118651703955946,-0.0333660264659097,
0.0694574276933728));
#81497=CARTESIAN_POINT('',(0.0120462540427042,-0.0336769361243753,0.0696097120587865));
#81498=CARTESIAN_POINT('',(0.0120559432307895,-0.0336938721132327,0.0696181008866323));
#81499=CARTESIAN_POINT('Ctrl Pts',(0.0120462540427042,-0.0336769361243753,
0.0696097120587865));
#81500=CARTESIAN_POINT('Ctrl Pts',(0.0120478705216501,-0.033679758666993,
0.069611108576638));
#81501=CARTESIAN_POINT('Ctrl Pts',(0.0120494861936565,-0.0336825812712652,
0.0696125059049446));
#81502=CARTESIAN_POINT('Ctrl Pts',(0.0120527159254343,-0.0336882266053286,
0.0696153021832117));
#81503=CARTESIAN_POINT('Ctrl Pts',(0.0120543299851789,-0.0336910493350804,
0.069616701133161));
#81504=CARTESIAN_POINT('Ctrl Pts',(0.0120559432307888,-0.0336938721132314,
0.0696181008866358));
#81505=CARTESIAN_POINT('Ctrl Pts',(0.0120462540427042,-0.0336769361243754,
0.0696097120587866));
#81506=CARTESIAN_POINT('Ctrl Pts',(0.0120188537291051,-0.0336279018378417,
0.0696414281088157));
#81507=CARTESIAN_POINT('Ctrl Pts',(0.0119910592276754,-0.0335767825754279,
0.0696736004339502));
#81508=CARTESIAN_POINT('Ctrl Pts',(0.0119365979875693,-0.0334733171799195,
0.0697366396911326));
#81509=CARTESIAN_POINT('Ctrl Pts',(0.0119098946462121,-0.0334209631321942,
0.0697675489910333));
#81510=CARTESIAN_POINT('Ctrl Pts',(0.0118837058516271,-0.033367986984468,
0.0697978626995336));
#81511=CARTESIAN_POINT('',(0.012057640102404,-0.0336938721132538,0.0697870565492832));
#81512=CARTESIAN_POINT('Origin',(0.00812378219310841,-0.0315241814719618,
0.07415));
#81513=CARTESIAN_POINT('',(0.0120462540418611,-0.0337108120655557,0.0696097120597726));
#81514=CARTESIAN_POINT('',(0.0120365469580377,-0.0336938721132327,0.0696013439463572));
#81515=CARTESIAN_POINT('Origin',(0.000504479743886488,-0.034556252137451,
0.0812598512727581));
#81516=CARTESIAN_POINT('Ctrl Pts',(0.0120365469580457,-0.0336938721132359,
0.0696013439463543));
#81517=CARTESIAN_POINT('Ctrl Pts',(0.0120381661841294,-0.0336910493082178,
0.0696027368084859));
#81518=CARTESIAN_POINT('Ctrl Pts',(0.01203978471031,-0.0336882265918966,
0.0696041305729465));
#81519=CARTESIAN_POINT('Ctrl Pts',(0.0120430204001186,-0.0336825812713121,
0.06960691993915));
#81520=CARTESIAN_POINT('Ctrl Pts',(0.012044637563745,-0.0336797586670163,
0.0696083155409235));
#81521=CARTESIAN_POINT('Ctrl Pts',(0.0120462540427044,-0.033676936124375,
0.0696097120587867));
#81522=CARTESIAN_POINT('Origin',(0.00219589820400869,-0.0345562520449254,
0.0827211093173939));
#81523=CARTESIAN_POINT('Ctrl Pts',(0.0120041862394658,-0.0342436276873911,
0.0699049335179514));
#81524=CARTESIAN_POINT('Ctrl Pts',(0.0118440809177256,-0.0339430054201811,
0.0697585816667022));
#81525=CARTESIAN_POINT('Ctrl Pts',(0.0116734066173258,-0.0336441434784053,
0.0696247053745641));
#81526=CARTESIAN_POINT('Ctrl Pts',(0.0118160393691582,-0.0342436276873911,
0.0697403104478991));
#81527=CARTESIAN_POINT('Ctrl Pts',(0.0116497251859766,-0.0339430054201811,
0.0696010546728438));
#81528=CARTESIAN_POINT('Ctrl Pts',(0.011473394168394,-0.0336441434784053,
0.069474721974575));
#81529=CARTESIAN_POINT('Ctrl Pts',(0.0118141579004551,-0.0342436276873911,
0.0697386642171985));
#81530=CARTESIAN_POINT('Ctrl Pts',(0.0116477816286591,-0.0339430054201811,
0.0695994794029052));
#81531=CARTESIAN_POINT('Ctrl Pts',(0.0114713940439047,-0.0336441434784053,
0.069473222140575));
#81532=CARTESIAN_POINT('',(0.0117882283835291,-0.0341934961088741,0.0697171725594705));
#81533=CARTESIAN_POINT('',(0.011603013537796,-0.0338664212864857,0.0695703630870027));
#81534=CARTESIAN_POINT('Origin',(0.000737920614214256,-0.0345610720403814,
0.0822847436040769));
#81535=CARTESIAN_POINT('Origin',(0.0182369173441908,-0.0336938005072859,
0.0608382359259433));
#81536=CARTESIAN_POINT('',(0.0117017255132845,-0.0336938721132327,0.069647062447956));
#81537=CARTESIAN_POINT('',(0.0116519586094886,-0.0336938721132427,0.0696092536489164));
#81538=CARTESIAN_POINT('',(0.0118837058516312,-0.0340203938281605,0.069797862699537));
#81539=CARTESIAN_POINT('Origin',(0.000429862642817593,-0.0345589643244208,
0.0819150991526489));
#81540=CARTESIAN_POINT('',(0.0118828177156378,-0.034193496108874,0.0697988907230037));
#81541=CARTESIAN_POINT('Origin',(0.0190867304027485,-0.0341934220717863,
0.0614603140868351));
#81542=CARTESIAN_POINT('',(0.0118355230495935,-0.0341934961088841,0.0697580316412471));
#81543=CARTESIAN_POINT('Ctrl Pts',(0.0122212047193902,-0.0340223579322397,
0.0697669498472922));
#81544=CARTESIAN_POINT('Ctrl Pts',(0.0121607510263096,-0.0339125849573575,
0.0697104357041282));
#81545=CARTESIAN_POINT('Ctrl Pts',(0.0120991701018965,-0.0338030433565231,
0.0696552125237701));
#81546=CARTESIAN_POINT('Ctrl Pts',(0.0120365469580398,-0.0336938721132326,
0.0696013439463569));
#81547=CARTESIAN_POINT('Ctrl Pts',(0.0121083899404104,-0.0340223579322397,
0.0697776271818883));
#81548=CARTESIAN_POINT('Ctrl Pts',(0.0120480835156215,-0.0339125849573575,
0.0697226690487597));
#81549=CARTESIAN_POINT('Ctrl Pts',(0.0119866819618085,-0.0338030433565231,
0.0696689977369353));
#81550=CARTESIAN_POINT('Ctrl Pts',(0.011924269885551,-0.0336938721132326,
0.06961667492231));
#81551=CARTESIAN_POINT('Ctrl Pts',(0.0119955751614305,-0.0340223579322397,
0.0697883045164844));
#81552=CARTESIAN_POINT('Ctrl Pts',(0.0119354160049335,-0.0339125849573575,
0.0697349023933912));
#81553=CARTESIAN_POINT('Ctrl Pts',(0.0118741938217205,-0.0338030433565231,
0.0696827829501006));
#81554=CARTESIAN_POINT('Ctrl Pts',(0.0118119928130621,-0.0336938721132326,
0.0696320058982631));
#81555=CARTESIAN_POINT('Ctrl Pts',(0.0118827603824507,-0.0340223579322397,
0.0697989818510805));
#81556=CARTESIAN_POINT('Ctrl Pts',(0.0118227484942454,-0.0339125849573575,
0.0697471357380227));
#81557=CARTESIAN_POINT('Ctrl Pts',(0.0117617056816325,-0.0338030433565231,
0.0696965681632658));
#81558=CARTESIAN_POINT('Ctrl Pts',(0.0116997157405733,-0.0336938721132326,
0.0696473368742162));
#81559=CARTESIAN_POINT('',(0.0118691362356711,-0.0336938721132427,0.0696242031971666));
#81560=CARTESIAN_POINT('Ctrl Pts',(0.0120462540395,-0.0337108120662705,
0.0696097120624956));
#81561=CARTESIAN_POINT('Ctrl Pts',(0.0120181434775496,-0.033761140899387,
0.0696422502298396));
#81562=CARTESIAN_POINT('Ctrl Pts',(0.0119905458709879,-0.0338121088780417,
0.0696741946478196));
#81563=CARTESIAN_POINT('Ctrl Pts',(0.0119363514275711,-0.0339153382773249,
0.0697369250860129));
#81564=CARTESIAN_POINT('Ctrl Pts',(0.0119097775183549,-0.0339675558473121,
0.0697676845673276));
#81565=CARTESIAN_POINT('Ctrl Pts',(0.0118837058516012,-0.0340203938281304,
0.0697978626995637));
#81566=CARTESIAN_POINT('Ctrl Pts',(0.0117883760535999,-0.0341934961088741,
0.0697191953237756));
#81567=CARTESIAN_POINT('Ctrl Pts',(0.0116967726575594,-0.0340287516182428,
0.0696434327327204));
#81568=CARTESIAN_POINT('Ctrl Pts',(0.0116021162095027,-0.0338644633275951,
0.0695715209172042));
#81569=CARTESIAN_POINT('Ctrl Pts',(0.0117882283835291,-0.0341934961088741,
0.0697171725594706));
#81570=CARTESIAN_POINT('Ctrl Pts',(0.0116965831684302,-0.0340287516182428,
0.0696414130213777));
#81571=CARTESIAN_POINT('Ctrl Pts',(0.0116018850632298,-0.0338644633275951,
0.0695695059846287));
#81572=CARTESIAN_POINT('Ctrl Pts',(0.0117636237094156,-0.0341934961088741,
0.0693801411198898));
#81573=CARTESIAN_POINT('Ctrl Pts',(0.0116650106348207,-0.0340287516182428,
0.0693048902640504));
#81574=CARTESIAN_POINT('Ctrl Pts',(0.0115633716482505,-0.0338644633275951,
0.0692337794618147));
#81575=CARTESIAN_POINT('',(0.011753426902075,-0.0341764758832406,0.0693723772357672));
#81576=CARTESIAN_POINT('',(0.0117636237094156,-0.034193496108874,0.0693801411198898));
#81577=CARTESIAN_POINT('Origin',(0.00132919932341822,-0.0345621026952721,
0.0822470348610732));
#81578=CARTESIAN_POINT('Ctrl Pts',(0.011753426902822,-0.0341764758837503,
0.0693723772374202));
#81579=CARTESIAN_POINT('Ctrl Pts',(0.0117274602070376,-0.0341260050040526,
0.0694065566597228));
#81580=CARTESIAN_POINT('Ctrl Pts',(0.0117019449041078,-0.0340749269148332,
0.0694401419861458));
#81581=CARTESIAN_POINT('Ctrl Pts',(0.0116517971633035,-0.0339715436306987,
0.069506150365217));
#81582=CARTESIAN_POINT('Ctrl Pts',(0.0116271837455901,-0.033919277823838,
0.0695385483721489));
#81583=CARTESIAN_POINT('Ctrl Pts',(0.0116030135399985,-0.0338664212855889,
0.069570363087186));
#81584=CARTESIAN_POINT('',(0.0117759260464824,-0.0341934961088841,0.0695486568396901));
#81585=CARTESIAN_POINT('Origin',(0.00812378219310841,-0.0315241814719618,
0.07415));
#81586=CARTESIAN_POINT('',(0.0117534269009585,-0.0342105180190554,0.0693723772358458));
#81587=CARTESIAN_POINT('',(0.0117432135337919,-0.0341934961088739,0.0693646351476515));
#81588=CARTESIAN_POINT('Origin',(0.00136188502771765,-0.0345621713746481,
0.0822784370868789));
#81589=CARTESIAN_POINT('Origin',(0.00214473761887886,-0.034562103232909,
0.082866615634891));
#81590=CARTESIAN_POINT('Origin',(0.00210572411884494,-0.0345621720636347,
0.082843542882067));
#81591=CARTESIAN_POINT('Ctrl Pts',(0.0117029199268719,-0.0346945769586965,
0.0696479698651322));
#81592=CARTESIAN_POINT('Ctrl Pts',(0.0116086231031826,-0.0345275153362944,
0.06957300339229));
#81593=CARTESIAN_POINT('Ctrl Pts',(0.0115119442629357,-0.0343603235965186,
0.0695009830775888));
#81594=CARTESIAN_POINT('Ctrl Pts',(0.0114131725050209,-0.034193496108874,
0.0694321176754391));
#81595=CARTESIAN_POINT('Ctrl Pts',(0.0116361659168294,-0.0346945769586965,
0.0695972556603406));
#81596=CARTESIAN_POINT('Ctrl Pts',(0.0115408068638159,-0.0345275153362944,
0.0695236873769656));
#81597=CARTESIAN_POINT('Ctrl Pts',(0.0114431094912697,-0.0343603235965186,
0.0694530990195095));
#81598=CARTESIAN_POINT('Ctrl Pts',(0.0113433658475022,-0.034193496108874,
0.0693856950625174));
#81599=CARTESIAN_POINT('Ctrl Pts',(0.0115694119067865,-0.0346945769586965,
0.0695465414555489));
#81600=CARTESIAN_POINT('Ctrl Pts',(0.0114729906244489,-0.0345275153362944,
0.06947437136164));
#81601=CARTESIAN_POINT('Ctrl Pts',(0.0113742747196035,-0.0343603235965186,
0.069405214961429));
#81602=CARTESIAN_POINT('Ctrl Pts',(0.0112735591899837,-0.034193496108874,
0.0693392724495953));
#81603=CARTESIAN_POINT('Ctrl Pts',(0.0115026578967444,-0.0346945769586965,
0.0694958272507573));
#81604=CARTESIAN_POINT('Ctrl Pts',(0.0114051743850824,-0.0345275153362944,
0.0694250553463166));
#81605=CARTESIAN_POINT('Ctrl Pts',(0.0113054399479375,-0.0343603235965186,
0.0693573309033509));
#81606=CARTESIAN_POINT('Ctrl Pts',(0.011203752532465,-0.034193496108874,
0.0692928498366739));
#81607=CARTESIAN_POINT('',(0.0115026578980562,-0.0346945769586966,0.0694958272517541));
#81608=CARTESIAN_POINT('',(0.0113085902893507,-0.0343667727836511,0.0693609372115995));
#81609=CARTESIAN_POINT('Origin',(0.00177344996204906,-0.0345626474179267,
0.0832085862090796));
#81610=CARTESIAN_POINT('Origin',(0.0174287120583264,-0.0341934771024118,
0.0601579612037074));
#81611=CARTESIAN_POINT('',(0.0114119234711446,-0.034193496108874,0.0694312870466964));
#81612=CARTESIAN_POINT('',(0.0113598807368301,-0.034193496108884,0.0693966777444305));
#81613=CARTESIAN_POINT('',(0.0116030135390037,-0.0345211942962673,0.0695703630884519));
#81614=CARTESIAN_POINT('Origin',(0.00139260688655039,-0.0345625596123107,
0.0829150780159028));
#81615=CARTESIAN_POINT('',(0.0116021917056726,-0.0346945769586885,0.0695714448498568));
#81616=CARTESIAN_POINT('Origin',(0.0182949952110115,-0.0346945685853857,
0.0607618536886375));
#81617=CARTESIAN_POINT('',(0.0115524248018744,-0.0346945769587026,0.0695336360508154));
#81618=CARTESIAN_POINT('Ctrl Pts',(0.0119379046530404,-0.0345231616327842,
0.0695183188947568));
#81619=CARTESIAN_POINT('Ctrl Pts',(0.01187406344989,-0.0344132092796988,
0.0694657465865016));
#81620=CARTESIAN_POINT('Ctrl Pts',(0.0118091381239245,-0.0343032738558979,
0.0694144974956657));
#81621=CARTESIAN_POINT('Ctrl Pts',(0.011743213533793,-0.0341934961088739,
0.0693646351476512));
#81622=CARTESIAN_POINT('Ctrl Pts',(0.011825983116894,-0.0345231616327842,
0.0695360588464229));
#81623=CARTESIAN_POINT('Ctrl Pts',(0.0117623864340015,-0.0344132092796988,
0.0694850292189705));
#81624=CARTESIAN_POINT('Ctrl Pts',(0.0116977375248132,-0.0343032738558979,
0.0694353176716336));
#81625=CARTESIAN_POINT('Ctrl Pts',(0.0116321208434002,-0.0341934961088739,
0.0693869857691142));
#81626=CARTESIAN_POINT('Ctrl Pts',(0.0117140615807476,-0.0345231616327842,
0.069553798798089));
#81627=CARTESIAN_POINT('Ctrl Pts',(0.0116507094181129,-0.0344132092796988,
0.0695043118514394));
#81628=CARTESIAN_POINT('Ctrl Pts',(0.011586336925702,-0.0343032738558979,
0.0694561378476015));
#81629=CARTESIAN_POINT('Ctrl Pts',(0.0115210281530074,-0.0341934961088739,
0.0694093363905773));
#81630=CARTESIAN_POINT('Ctrl Pts',(0.0116021400446012,-0.0345231616327842,
0.0695715387497551));
#81631=CARTESIAN_POINT('Ctrl Pts',(0.0115390324022244,-0.0344132092796988,
0.0695235944839084));
#81632=CARTESIAN_POINT('Ctrl Pts',(0.0114749363265907,-0.0343032738558979,
0.0694769580235694));
#81633=CARTESIAN_POINT('Ctrl Pts',(0.0114099354626146,-0.0341934961088739,
0.0694316870120403));
#81634=CARTESIAN_POINT('',(0.0115775685024782,-0.0341934961088839,0.069397961097184));
#81635=CARTESIAN_POINT('Ctrl Pts',(0.0117534268988626,-0.034210518019541,
0.0693723772385932));
#81636=CARTESIAN_POINT('Ctrl Pts',(0.0117274310005431,-0.034261055624081,
0.0694065950768619));
#81637=CARTESIAN_POINT('Ctrl Pts',(0.0117019015851772,-0.034312218986911,
0.069440198893716));
#81638=CARTESIAN_POINT('Ctrl Pts',(0.0116517533416707,-0.0344158119695163,
0.0695062079411695));
#81639=CARTESIAN_POINT('Ctrl Pts',(0.0116271550246041,-0.0344681990450054,
0.0695385861734861));
#81640=CARTESIAN_POINT('Ctrl Pts',(0.0116030135389773,-0.0345211942962463,
0.0695703630884668));
#81641=CARTESIAN_POINT('Ctrl Pts',(0.0115029322199276,-0.0346945769586932,
0.0694978362599221));
#81642=CARTESIAN_POINT('Ctrl Pts',(0.0114067520264886,-0.0345296777079064,
0.0694279747242158));
#81643=CARTESIAN_POINT('Ctrl Pts',(0.0113077665763584,-0.0343648066255586,
0.0693621481000903));
#81644=CARTESIAN_POINT('Ctrl Pts',(0.0115026578980635,-0.0346945769586932,
0.0694958272517595));
#81645=CARTESIAN_POINT('Ctrl Pts',(0.0114064361698022,-0.0345296777079064,
0.0694259713874637));
#81646=CARTESIAN_POINT('Ctrl Pts',(0.0113074094547454,-0.0343648066255586,
0.0693601521465749));
#81647=CARTESIAN_POINT('Ctrl Pts',(0.0114569393964651,-0.0346945769586932,
0.0691610058070076));
#81648=CARTESIAN_POINT('Ctrl Pts',(0.0113537954717544,-0.0345296777079064,
0.0690920951403816));
#81649=CARTESIAN_POINT('Ctrl Pts',(0.0112478915410667,-0.0343648066255586,
0.0690275063902431));
#81650=CARTESIAN_POINT('',(0.0114462752119167,-0.0346775396664988,0.0691538975057157));
#81651=CARTESIAN_POINT('',(0.0114569393964623,-0.0346945769586886,0.0691610058070057));
#81652=CARTESIAN_POINT('Origin',(0.00238071619513352,-0.0345626617890403,
0.0830617564758974));
#81653=CARTESIAN_POINT('Ctrl Pts',(0.0114462752126745,-0.0346775396670097,
0.0691538975073658));
#81654=CARTESIAN_POINT('Ctrl Pts',(0.0114224871787978,-0.0346269749928753,
0.0691896680965144));
#81655=CARTESIAN_POINT('Ctrl Pts',(0.0113991219412728,-0.0345757902891938,
0.0692248029823673));
#81656=CARTESIAN_POINT('Ctrl Pts',(0.011353217672773,-0.0344721681090558,
0.0692938301876703));
#81657=CARTESIAN_POINT('Ctrl Pts',(0.0113306966337414,-0.0344197714293279,
0.0693276954420808));
#81658=CARTESIAN_POINT('Ctrl Pts',(0.0113085902900172,-0.0343667727834186,
0.069360937211672));
#81659=CARTESIAN_POINT('',(0.0114797986472692,-0.0346945769587026,0.0693284165293899));
#81660=CARTESIAN_POINT('Origin',(0.00812378219310841,-0.0315241814719618,
0.07415));
#81661=CARTESIAN_POINT('',(0.0114462752106478,-0.034711613648963,0.0691538975062894));
#81662=CARTESIAN_POINT('',(0.0114355958676054,-0.0346945769586885,0.0691468119977928));
#81663=CARTESIAN_POINT('Origin',(0.00241945019131871,-0.0345626692919776,
0.0830852695700954));
#81664=CARTESIAN_POINT('Origin',(0.00212638595541208,-0.0345626624076629,
0.0828926245201263));
#81665=CARTESIAN_POINT('Origin',(0.00208972466723691,-0.0345626700069096,
0.082865994882105));
#81666=CARTESIAN_POINT('Ctrl Pts',(0.011443569771881,-0.0352450361874068,
0.0694534296494727));
#81667=CARTESIAN_POINT('Ctrl Pts',(0.0112664357144761,-0.0349452760959493,
0.0693282218063741));
#81668=CARTESIAN_POINT('Ctrl Pts',(0.0110803737092312,-0.034644428984174,
0.0692167121275547));
#81669=CARTESIAN_POINT('Ctrl Pts',(0.0114414760628377,-0.0352450361874068,
0.0694520182645352));
#81670=CARTESIAN_POINT('Ctrl Pts',(0.0112642887741763,-0.0349452760959493,
0.0693268893869689));
#81671=CARTESIAN_POINT('Ctrl Pts',(0.0110781796369064,-0.034644428984174,
0.0692154624589451));
#81672=CARTESIAN_POINT('Ctrl Pts',(0.011234178137754,-0.0352450361874068,
0.069312277181614));
#81673=CARTESIAN_POINT('Ctrl Pts',(0.0110517204276667,-0.0349452760959493,
0.0691949666735857));
#81674=CARTESIAN_POINT('Ctrl Pts',(0.010860944753267,-0.034644428984174,
0.0690917328936418));
#81675=CARTESIAN_POINT('Ctrl Pts',(0.0112321051585031,-0.0352450361874068,
0.0693108797707847));
#81676=CARTESIAN_POINT('Ctrl Pts',(0.0110495947442016,-0.0349452760959493,
0.069193647446452));
#81677=CARTESIAN_POINT('Ctrl Pts',(0.0108587724044306,-0.034644428984174,
0.0690904955979887));
#81678=CARTESIAN_POINT('',(0.0112037811325199,-0.0351951634053335,0.0692928651618755));
#81679=CARTESIAN_POINT('',(0.0110015980579655,-0.0348678972925388,0.0691704115784557));
#81680=CARTESIAN_POINT('Origin',(0.00298610278410784,-0.0345636767883213,
0.0838830762270324));
#81681=CARTESIAN_POINT('Origin',(0.0165306241745782,-0.0346946199340667,
0.0596033399503948));
#81682=CARTESIAN_POINT('',(0.0111091446528959,-0.0346945769330288,0.069234134259183));
#81683=CARTESIAN_POINT('',(0.0110550314695942,-0.0346945769458128,0.0692028610361239));
#81684=CARTESIAN_POINT('',(0.0113085902897783,-0.0350221583435276,0.069360937212002));
#81685=CARTESIAN_POINT('Origin',(0.00255063873445146,-0.0345628458716655,
0.0836793252647309));
#81686=CARTESIAN_POINT('',(0.0113079078848194,-0.0351951360298761,0.0693619688205612));
#81687=CARTESIAN_POINT('Origin',(0.0174096517011827,-0.035195183836678,
0.0601866450520421));
#81688=CARTESIAN_POINT('',(0.0112037525339102,-0.0351951371328748,0.0692928498374955));
#81689=CARTESIAN_POINT('Ctrl Pts',(0.0116395519122222,-0.0350241211494342,
0.0692879671656622));
#81690=CARTESIAN_POINT('Ctrl Pts',(0.0115725794034403,-0.0349144232818962,
0.069239538879303));
#81691=CARTESIAN_POINT('Ctrl Pts',(0.0115045657610997,-0.0348045283579412,
0.0691924659758927));
#81692=CARTESIAN_POINT('Ctrl Pts',(0.011435595858339,-0.0346945769439158,
0.0691468119916587));
#81693=CARTESIAN_POINT('Ctrl Pts',(0.0115289651080124,-0.0350241211494342,
0.0693126997461491));
#81694=CARTESIAN_POINT('Ctrl Pts',(0.0114623332803859,-0.0349144232818962,
0.0692657947476756));
#81695=CARTESIAN_POINT('Ctrl Pts',(0.0113946920105639,-0.0348045283579412,
0.0692202390017892));
#81696=CARTESIAN_POINT('Ctrl Pts',(0.0113261257670373,-0.0346945769439158,
0.0691760940836826));
#81697=CARTESIAN_POINT('Ctrl Pts',(0.0114183783038026,-0.0350241211494342,
0.0693374323266359));
#81698=CARTESIAN_POINT('Ctrl Pts',(0.0113520871573316,-0.0349144232818962,
0.0692920506160481));
#81699=CARTESIAN_POINT('Ctrl Pts',(0.0112848182600282,-0.0348045283579412,
0.0692480120276857));
#81700=CARTESIAN_POINT('Ctrl Pts',(0.0112166556757357,-0.0346945769439157,
0.0692053761757064));
#81701=CARTESIAN_POINT('Ctrl Pts',(0.0113077914995927,-0.0350241211494342,
0.0693621649071228));
#81702=CARTESIAN_POINT('Ctrl Pts',(0.0112418410342772,-0.0349144232818962,
0.0693183064844206));
#81703=CARTESIAN_POINT('Ctrl Pts',(0.0111749445094924,-0.0348045283579412,
0.0692757850535821));
#81704=CARTESIAN_POINT('Ctrl Pts',(0.011107185584434,-0.0346945769439157,
0.0692346582677302));
#81705=CARTESIAN_POINT('',(0.0112723702605491,-0.0346945769458128,0.0691904731285738));
#81706=CARTESIAN_POINT('Ctrl Pts',(0.011446275208821,-0.034711613649282,
0.0691538975090242));
#81707=CARTESIAN_POINT('Ctrl Pts',(0.0114224966109672,-0.034762154653183,
0.0691896538857593));
#81708=CARTESIAN_POINT('Ctrl Pts',(0.0113991361051192,-0.0348133084096039,
0.069224781568769));
#81709=CARTESIAN_POINT('Ctrl Pts',(0.0113532317814142,-0.0349168561544586,
0.0692938088639129));
#81710=CARTESIAN_POINT('Ctrl Pts',(0.0113307061715391,-0.0349692089015924,
0.0693276810963227));
#81711=CARTESIAN_POINT('Ctrl Pts',(0.0113085902897415,-0.0350221583435,
0.0693609372120215));
#81712=CARTESIAN_POINT('Ctrl Pts',(0.0112040410946606,-0.0351951371254961,
0.0692942841152269));
#81713=CARTESIAN_POINT('Ctrl Pts',(0.01110365221532,-0.0350307338980954,
0.0692306016950558));
#81714=CARTESIAN_POINT('Ctrl Pts',(0.0110007170545465,-0.0348659306897802,
0.0691711228718443));
#81715=CARTESIAN_POINT('Ctrl Pts',(0.0112037525338538,-0.0351951371254961,
0.0692928498375973));
#81716=CARTESIAN_POINT('Ctrl Pts',(0.0111033340017231,-0.0350307338980954,
0.0692291733832398));
#81717=CARTESIAN_POINT('Ctrl Pts',(0.0110003694600711,-0.0348659306897802,
0.069169701746326));
#81718=CARTESIAN_POINT('Ctrl Pts',(0.0111553894418679,-0.0351951371254961,
0.0690524634119508));
#81719=CARTESIAN_POINT('Ctrl Pts',(0.0110500010712104,-0.0350307338980954,
0.0689897868341761));
#81720=CARTESIAN_POINT('Ctrl Pts',(0.0109421122637075,-0.0348659306897802,
0.0689315196282454));
#81721=CARTESIAN_POINT('Origin',(0.0136626645957855,-0.0308609197410717,
0.0645658723227696));
#81722=CARTESIAN_POINT('',(0.01118266731619,-0.0351951371254961,0.0691880467760055));
#81723=CARTESIAN_POINT('Origin',(0.00776259808483813,-0.0351840467441113,
0.0750579051108912));
#81724=CARTESIAN_POINT('Origin',(0.0134096467068773,-0.0352322613132216,
0.0634154466215648));
#81725=CARTESIAN_POINT('',(0.0107942927752421,-0.035195114256467,0.0690562599384998));
#81726=CARTESIAN_POINT('',(0.0106826437780381,-0.0351951372916787,0.0690007546777055));
#81727=CARTESIAN_POINT('Origin',(0.00778461305072263,-0.0352875117104394,
0.0741807531841194));
#81728=CARTESIAN_POINT('Origin',(0.0140792769102759,-0.0298325076522913,
0.0787136907162318));
#81729=CARTESIAN_POINT('Origin',(0.0144049968005323,-0.0338731295099351,
0.0686001892186881));
#81730=CARTESIAN_POINT('Ctrl Pts',(0.0132784795555664,-0.0321934096636942,
0.0715990725516433));
#81731=CARTESIAN_POINT('Ctrl Pts',(0.0132328191690395,-0.032050846084523,
0.0715068059236173));
#81732=CARTESIAN_POINT('Ctrl Pts',(0.0131847141883583,-0.0319086045664877,
0.0714158356694231));
#81733=CARTESIAN_POINT('Ctrl Pts',(0.013134284317649,-0.0317669892870596,
0.0713263491367977));
#81734=CARTESIAN_POINT('Ctrl Pts',(0.0132396651423412,-0.0321934096636942,
0.0715247497828995));
#81735=CARTESIAN_POINT('Ctrl Pts',(0.0131926744136476,-0.032050846084523,
0.0714331779143863));
#81736=CARTESIAN_POINT('Ctrl Pts',(0.0131432587606993,-0.0319086045664877,
0.0713429376395227));
#81737=CARTESIAN_POINT('Ctrl Pts',(0.0130915405803324,-0.0317669892870596,
0.0712542145019387));
#81738=CARTESIAN_POINT('Ctrl Pts',(0.0132008507291159,-0.0321934096636942,
0.0714504270141559));
#81739=CARTESIAN_POINT('Ctrl Pts',(0.0131525296582558,-0.032050846084523,
0.0713595499051552));
#81740=CARTESIAN_POINT('Ctrl Pts',(0.0131018033330405,-0.0319086045664877,
0.0712700396096223));
#81741=CARTESIAN_POINT('Ctrl Pts',(0.0130487968430159,-0.0317669892870596,
0.0711820798670797));
#81742=CARTESIAN_POINT('Ctrl Pts',(0.0131620363158906,-0.0321934096636942,
0.0713761042454123));
#81743=CARTESIAN_POINT('Ctrl Pts',(0.0131123849028638,-0.032050846084523,
0.0712859218959241));
#81744=CARTESIAN_POINT('Ctrl Pts',(0.0130603479053815,-0.0319086045664877,
0.0711971415797219));
#81745=CARTESIAN_POINT('Ctrl Pts',(0.0130060531056993,-0.0317669892870596,
0.0711099452322206));
#81746=CARTESIAN_POINT('',(0.0131627307134113,-0.0321934096636942,0.0713774338944332));
#81747=CARTESIAN_POINT('',(0.0130445664762117,-0.0318665617511322,0.0711727517691103));
#81748=CARTESIAN_POINT('Origin',(-0.00176379806423547,-0.0326371944423759,
0.0788885352453787));
#81749=CARTESIAN_POINT('Origin',(0.0224228080824538,-0.0316939261509285,
0.0654985844740454));
#81750=CARTESIAN_POINT('',(0.013221635807231,-0.0320197221621834,0.0714873926884516));
#81751=CARTESIAN_POINT('Ctrl Pts',(0.0132215948274271,-0.0320197392094745,
0.0714872123123591));
#81752=CARTESIAN_POINT('Ctrl Pts',(0.0132080456660022,-0.0319792716576044,
0.0714612730245034));
#81753=CARTESIAN_POINT('Ctrl Pts',(0.0131942370729477,-0.0319386439829733,
0.0714353189444909));
#81754=CARTESIAN_POINT('Ctrl Pts',(0.0131801470853275,-0.0318979099381666,
0.0714093267979314));
#81755=CARTESIAN_POINT('Ctrl Pts',(0.0131660573762056,-0.0318571766984964,
0.0713833351651248));
#81756=CARTESIAN_POINT('Ctrl Pts',(0.0131517594630909,-0.0318163871833608,
0.0713574367246318));
#81757=CARTESIAN_POINT('Ctrl Pts',(0.0131373056074969,-0.0317755399638303,
0.0713317188545931));
#81758=CARTESIAN_POINT('',(0.0132205951878513,-0.0321934096636183,0.0714882341769757));
#81759=CARTESIAN_POINT('Origin',(0.0152562378528542,-0.0324111610893099,
0.0704014176396957));
#81760=CARTESIAN_POINT('',(0.0131916629506413,-0.0321934096636663,0.0714328340357144));
#81761=CARTESIAN_POINT('Ctrl Pts',(0.0131621233618727,-0.0321934096636618,
0.0713793690459745));
#81762=CARTESIAN_POINT('Ctrl Pts',(0.0131239142017133,-0.0320835708272592,
0.0713098863946038));
#81763=CARTESIAN_POINT('Ctrl Pts',(0.0130842892645605,-0.0319739230346488,
0.0712412347825782));
#81764=CARTESIAN_POINT('Ctrl Pts',(0.0130433059888615,-0.0318646057455572,
0.071173498153992));
#81765=CARTESIAN_POINT('Ctrl Pts',(0.0131960567125676,-0.0321934096636618,
0.0712712501647596));
#81766=CARTESIAN_POINT('Ctrl Pts',(0.0131563565087732,-0.0320835708272592,
0.0712012995460367));
#81767=CARTESIAN_POINT('Ctrl Pts',(0.0131152317082915,-0.0319739230346488,
0.0711322110951696));
#81768=CARTESIAN_POINT('Ctrl Pts',(0.0130727417114348,-0.0318646057455572,
0.0710640691678818));
#81769=CARTESIAN_POINT('Ctrl Pts',(0.0132299900632624,-0.0321934096636618,
0.0711631312835448));
#81770=CARTESIAN_POINT('Ctrl Pts',(0.0131887988158331,-0.0320835708272592,
0.0710927126974697));
#81771=CARTESIAN_POINT('Ctrl Pts',(0.0131461741520224,-0.0319739230346488,
0.0710231874077611));
#81772=CARTESIAN_POINT('Ctrl Pts',(0.013102177434008,-0.0318646057455572,
0.0709546401817716));
#81773=CARTESIAN_POINT('Ctrl Pts',(0.0132639234139572,-0.0321934096636618,
0.07105501240233));
#81774=CARTESIAN_POINT('Ctrl Pts',(0.013221241122893,-0.0320835708272592,
0.0709841258489027));
#81775=CARTESIAN_POINT('Ctrl Pts',(0.0131771165957533,-0.0319739230346488,
0.0709141637203525));
#81776=CARTESIAN_POINT('Ctrl Pts',(0.0131316131565813,-0.0318646057455572,
0.0708452111956613));
#81777=CARTESIAN_POINT('',(0.013257300737261,-0.0321763980308463,0.0710440400301001));
#81778=CARTESIAN_POINT('',(0.0132639234139403,-0.0321934096636184,0.071055012402302));
#81779=CARTESIAN_POINT('Origin',(-0.00120853150640208,-0.0326386231565666,
0.0790793241204305));
#81780=CARTESIAN_POINT('Ctrl Pts',(0.0132573007345385,-0.0321763980306274,
0.0710440400317385));
#81781=CARTESIAN_POINT('Ctrl Pts',(0.0132205799120103,-0.0321259596174894,
0.0710662574258813));
#81782=CARTESIAN_POINT('Ctrl Pts',(0.0131844953253848,-0.0320749164631545,
0.0710880898748471));
#81783=CARTESIAN_POINT('Ctrl Pts',(0.0131135695842014,-0.0319716057793966,
0.0711310024524596));
#81784=CARTESIAN_POINT('Ctrl Pts',(0.0130787560647087,-0.0319193786690175,
0.0711520658609163));
#81785=CARTESIAN_POINT('Ctrl Pts',(0.013044566474618,-0.0318665617525371,
0.0711727517700634));
#81786=CARTESIAN_POINT('',(0.0132133270636858,-0.0321934096636663,0.0712162231483776));
#81787=CARTESIAN_POINT('Origin',(0.00812378219310841,-0.0315241814719618,
0.07415));
#81788=CARTESIAN_POINT('',(0.0132573007375785,-0.0322104233323779,0.0710440400299074));
#81789=CARTESIAN_POINT('',(0.0132506546416669,-0.0321934096636183,0.0710330818271523));
#81790=CARTESIAN_POINT('Origin',(-0.00119069648195176,-0.0326387240834481,
0.0791210015576047));
#81791=CARTESIAN_POINT('Origin',(-0.000573360558493453,-0.0326386239212449,
0.080129134790157));
#81792=CARTESIAN_POINT('Origin',(-0.000601999677916885,-0.0326387246941709,
0.0800939939734251));
#81793=CARTESIAN_POINT('Ctrl Pts',(0.013126047026358,-0.0327445246967098,
0.0713117837400871));
#81794=CARTESIAN_POINT('Ctrl Pts',(0.0130190019501655,-0.0324436878339361,
0.0711231202376705));
#81795=CARTESIAN_POINT('Ctrl Pts',(0.0128980500716496,-0.0321434074405927,
0.0709430557809763));
#81796=CARTESIAN_POINT('Ctrl Pts',(0.0129979788045448,-0.0327445246967098,
0.0710970780565069));
#81797=CARTESIAN_POINT('Ctrl Pts',(0.0128828359711157,-0.0324436878339361,
0.0709132447260388));
#81798=CARTESIAN_POINT('Ctrl Pts',(0.0127541731685286,-0.0321434074405927,
0.0707386066754554));
#81799=CARTESIAN_POINT('',(0.0129786966333756,-0.0326943950436612,0.0710665067248839));
#81800=CARTESIAN_POINT('',(0.0128479134700578,-0.0323666188837389,0.0708696480862338));
#81801=CARTESIAN_POINT('Origin',(-0.00117109338435085,-0.0326395579111445,
0.0801434831307089));
#81802=CARTESIAN_POINT('Origin',(0.0219198877202798,-0.0321933825602988,
0.0645702310453205));
#81803=CARTESIAN_POINT('',(0.0129180927342665,-0.0321934096532689,0.0709730971951112));
#81804=CARTESIAN_POINT('',(0.0128824451562546,-0.0321934096584275,0.0709217600689009));
#81805=CARTESIAN_POINT('',(0.0130445664770146,-0.0325210109756239,0.0711727517686187));
#81806=CARTESIAN_POINT('Origin',(-0.00140709529368095,-0.0326393129158039,
0.0797245708145731));
#81807=CARTESIAN_POINT('',(0.0130434041327693,-0.0326943950436595,0.0711734550279211));
#81808=CARTESIAN_POINT('Origin',(0.0225082911806531,-0.0326943765538162,
0.0654468653035667));
#81809=CARTESIAN_POINT('',(0.0130110503830824,-0.0326943950436703,0.0711199808764126));
#81810=CARTESIAN_POINT('Ctrl Pts',(0.0133750991772516,-0.032522978320377,
0.0712476440721177));
#81811=CARTESIAN_POINT('Ctrl Pts',(0.0133350902642561,-0.032413025309245,
0.07117525478233));
#81812=CARTESIAN_POINT('Ctrl Pts',(0.0132935899539462,-0.032303122220807,
0.0711037041075568));
#81813=CARTESIAN_POINT('Ctrl Pts',(0.0132506546393428,-0.0321934096576658,
0.0710330818233217));
#81814=CARTESIAN_POINT('Ctrl Pts',(0.0132645066272558,-0.032522978320377,
0.0712229371880149));
#81815=CARTESIAN_POINT('Ctrl Pts',(0.0132241571304032,-0.032413025309245,
0.0711520724141105));
#81816=CARTESIAN_POINT('Ctrl Pts',(0.013182347824462,-0.032303122220807,
0.0710820530694124));
#81817=CARTESIAN_POINT('Ctrl Pts',(0.0131391354290384,-0.0321934096576658,
0.0710129669539527));
#81818=CARTESIAN_POINT('Ctrl Pts',(0.01315391407726,-0.032522978320377,
0.0711982303039122));
#81819=CARTESIAN_POINT('Ctrl Pts',(0.0131132239965503,-0.032413025309245,
0.0711288900458909));
#81820=CARTESIAN_POINT('Ctrl Pts',(0.0130711056949777,-0.032303122220807,
0.071060402031268));
#81821=CARTESIAN_POINT('Ctrl Pts',(0.013027616218734,-0.0321934096576658,
0.0709928520845838));
#81822=CARTESIAN_POINT('Ctrl Pts',(0.0130433215272641,-0.032522978320377,
0.0711735234198095));
#81823=CARTESIAN_POINT('Ctrl Pts',(0.0130022908626975,-0.032413025309245,
0.0711057076776714));
#81824=CARTESIAN_POINT('Ctrl Pts',(0.0129598635654934,-0.032303122220807,
0.0710387509931235));
#81825=CARTESIAN_POINT('Ctrl Pts',(0.0129160970084296,-0.0321934096576658,
0.0709727372152148));
#81826=CARTESIAN_POINT('',(0.0130843736883616,-0.0321934096584275,0.0710030895114684));
#81827=CARTESIAN_POINT('Ctrl Pts',(0.0132573007345965,-0.0322104233328919,
0.0710440400317035));
#81828=CARTESIAN_POINT('Ctrl Pts',(0.0132205301548116,-0.0322609421830587,
0.0710662875307434));
#81829=CARTESIAN_POINT('Ctrl Pts',(0.0131844212609603,-0.032312088823912,
0.0710881346864311));
#81830=CARTESIAN_POINT('Ctrl Pts',(0.0131134949826744,-0.0324156524631815,
0.0711310475890096));
#81831=CARTESIAN_POINT('Ctrl Pts',(0.0130787067528211,-0.0324680267167321,
0.0711520956963494));
#81832=CARTESIAN_POINT('Ctrl Pts',(0.0130445664769752,-0.0325210109755913,
0.0711727517686373));
#81833=CARTESIAN_POINT('Origin',(0.011356292122591,-0.0262834582511563,
0.0813231628585625));
#81834=CARTESIAN_POINT('Origin',(0.0202428260747771,-0.0342770653632561,
0.0731747792278278));
#81835=CARTESIAN_POINT('Ctrl Pts',(0.0129782121070416,-0.0326943950436604,
0.0710684757157585));
#81836=CARTESIAN_POINT('Ctrl Pts',(0.0129357429270127,-0.0325844576448134,
0.0710015725733731));
#81837=CARTESIAN_POINT('Ctrl Pts',(0.0128918870747002,-0.0324744968375322,
0.0709355430284206));
#81838=CARTESIAN_POINT('Ctrl Pts',(0.0128467019076805,-0.0323646534831894,
0.0708704709067663));
#81839=CARTESIAN_POINT('Ctrl Pts',(0.013005289618094,-0.0326943950436604,
0.0709584396490503));
#81840=CARTESIAN_POINT('Ctrl Pts',(0.0129613039348363,-0.0325844576448134,
0.070891163327814));
#81841=CARTESIAN_POINT('Ctrl Pts',(0.0129159237540192,-0.0324744968375322,
0.0708247919413732));
#81842=CARTESIAN_POINT('Ctrl Pts',(0.0128692083923189,-0.0323646534831894,
0.0707594097266419));
#81843=CARTESIAN_POINT('Ctrl Pts',(0.0130323671291464,-0.0326943950436604,
0.0708484035823421));
#81844=CARTESIAN_POINT('Ctrl Pts',(0.0129868649426599,-0.0325844576448134,
0.0707807540822548));
#81845=CARTESIAN_POINT('Ctrl Pts',(0.0129399604333382,-0.0324744968375322,
0.0707140408543257));
#81846=CARTESIAN_POINT('Ctrl Pts',(0.0128917148769573,-0.0323646534831894,
0.0706483485465175));
#81847=CARTESIAN_POINT('Ctrl Pts',(0.0130594446401988,-0.0326943950436604,
0.0707383675156339));
#81848=CARTESIAN_POINT('Ctrl Pts',(0.0130124259504834,-0.0325844576448134,
0.0706703448366956));
#81849=CARTESIAN_POINT('Ctrl Pts',(0.0129639971126573,-0.0324744968375322,
0.0706032897672782));
#81850=CARTESIAN_POINT('Ctrl Pts',(0.0129142213615957,-0.0323646534831894,
0.0705372873663931));
#81851=CARTESIAN_POINT('',(0.0130521460710747,-0.0326773559991345,0.0707278326360949));
#81852=CARTESIAN_POINT('',(0.0130594446401983,-0.0326943950436595,0.0707383675156333));
#81853=CARTESIAN_POINT('Origin',(-0.000558563097022123,-0.0326395669463386,
0.0802400300320104));
#81854=CARTESIAN_POINT('Ctrl Pts',(0.0130521460683142,-0.0326773559987418,
0.0707278326380026));
#81855=CARTESIAN_POINT('Ctrl Pts',(0.0130168643781785,-0.032626792258602,
0.070752331609977));
#81856=CARTESIAN_POINT('Ctrl Pts',(0.0129822080305232,-0.0325756109579454,
0.0707763963553641));
#81857=CARTESIAN_POINT('Ctrl Pts',(0.012914116525888,-0.0324719985462361,
0.0708236778732658));
#81858=CARTESIAN_POINT('Ctrl Pts',(0.0128807086785635,-0.0324196091621767,
0.0708468756824462));
#81859=CARTESIAN_POINT('Ctrl Pts',(0.0128479134700177,-0.0323666188837756,
0.0708696480862616));
#81860=CARTESIAN_POINT('',(0.0130190706367969,-0.0326943950436703,0.0709024371202686));
#81861=CARTESIAN_POINT('Origin',(0.00812378219310841,-0.0315241814719618,
0.07415));
#81862=CARTESIAN_POINT('',(0.0130521460710381,-0.0327114338379869,0.0707278326361197));
#81863=CARTESIAN_POINT('',(0.0130448250186083,-0.0326943950436593,0.0707173133685686));
#81864=CARTESIAN_POINT('Origin',(-0.000532086577476713,-0.0326395676484836,
0.0802767990880925));
#81865=CARTESIAN_POINT('Origin',(-0.000615874592565635,-0.0326395675647529,
0.0801574963132246));
#81866=CARTESIAN_POINT('Origin',(-0.000641074086288608,-0.0326395682454631,
0.0801198404787709));
#81867=CARTESIAN_POINT('Ctrl Pts',(0.012937941665499,-0.0332451089994434,
0.0710032566716696));
#81868=CARTESIAN_POINT('Ctrl Pts',(0.0128192602991421,-0.0329451141710254,
0.070821687676544));
#81869=CARTESIAN_POINT('Ctrl Pts',(0.0126872395750486,-0.0326442513127493,
0.0706495740654579));
#81870=CARTESIAN_POINT('Ctrl Pts',(0.012796643269112,-0.0332451089994434,
0.0707970170945306));
#81871=CARTESIAN_POINT('Ctrl Pts',(0.0126701834498412,-0.0329451141710254,
0.0706207772556143));
#81872=CARTESIAN_POINT('Ctrl Pts',(0.012530807784429,-0.0326442513127493,
0.0704545635660392));
#81873=CARTESIAN_POINT('Ctrl Pts',(0.0127952302851482,-0.0332451089994434,
0.0707949546987592));
#81874=CARTESIAN_POINT('Ctrl Pts',(0.0126686926813482,-0.0329451141710254,
0.070618768151405));
#81875=CARTESIAN_POINT('Ctrl Pts',(0.0125292434665228,-0.0326442513127493,
0.070452613461045));
#81876=CARTESIAN_POINT('',(0.0127755024240173,-0.0331951640388616,0.07076774869453));
#81877=CARTESIAN_POINT('',(0.0126326164713081,-0.0328677532355019,0.0705794904395078));
#81878=CARTESIAN_POINT('Origin',(-0.000317427338547305,-0.0326402808280624,
0.0812371057761744));
#81879=CARTESIAN_POINT('Origin',(0.0212998163304004,-0.0326944278779125,
0.0637155244168665));
#81880=CARTESIAN_POINT('',(0.0127091528762318,-0.0326943950436593,0.0706783288320532));
#81881=CARTESIAN_POINT('',(0.0126703521572034,-0.0326943950436693,0.0706293313402693));
#81882=CARTESIAN_POINT('',(0.0128479134700594,-0.0330220786163545,0.0708696480862361));
#81883=CARTESIAN_POINT('Origin',(-0.000639895617482721,-0.0326396682763836,
0.0808805011570728));
#81884=CARTESIAN_POINT('',(0.012846797577453,-0.0331951640388588,0.0708704229420175));
#81885=CARTESIAN_POINT('Origin',(0.021908131514598,-0.0331952026560088,
0.0645783964944561));
#81886=CARTESIAN_POINT('',(0.0128111500007451,-0.0331951640388702,0.0708190858182837));
#81887=CARTESIAN_POINT('Ctrl Pts',(0.013182495949465,-0.0330240426238172,
0.0709236374767695));
#81888=CARTESIAN_POINT('Ctrl Pts',(0.0131380496624148,-0.032914277406352,
0.0708539487663096));
#81889=CARTESIAN_POINT('Ctrl Pts',(0.0130921405569585,-0.0328043479726691,
0.070785144142394));
#81890=CARTESIAN_POINT('Ctrl Pts',(0.0130448250186134,-0.0326943950436593,
0.0707173133685692));
#81891=CARTESIAN_POINT('Ctrl Pts',(0.0130705702949247,-0.0330240426238172,
0.0709059235319659));
#81892=CARTESIAN_POINT('Ctrl Pts',(0.0130258799810269,-0.032914277406352,
0.0708377767064413));
#81893=CARTESIAN_POINT('Ctrl Pts',(0.0129797586021355,-0.0328043479726691,
0.0707705197808633));
#81894=CARTESIAN_POINT('Ctrl Pts',(0.0129322628703094,-0.0326943950436593,
0.0707042405435509));
#81895=CARTESIAN_POINT('Ctrl Pts',(0.0129586446403843,-0.0330240426238172,
0.0708882095871624));
#81896=CARTESIAN_POINT('Ctrl Pts',(0.0129137102996391,-0.032914277406352,
0.0708216046465729));
#81897=CARTESIAN_POINT('Ctrl Pts',(0.0128673766473124,-0.0328043479726691,
0.0707558954193326));
#81898=CARTESIAN_POINT('Ctrl Pts',(0.0128197007220053,-0.0326943950436593,
0.0706911677185326));
#81899=CARTESIAN_POINT('Ctrl Pts',(0.012846718985844,-0.0330240426238172,
0.0708704956423588));
#81900=CARTESIAN_POINT('Ctrl Pts',(0.0128015406182512,-0.032914277406352,
0.0708054325867045));
#81901=CARTESIAN_POINT('Ctrl Pts',(0.0127549946924894,-0.0328043479726691,
0.0707412710578018));
#81902=CARTESIAN_POINT('Ctrl Pts',(0.0127071385737012,-0.0326943950436593,
0.0706780948935143));
#81903=CARTESIAN_POINT('',(0.01287698894743,-0.0326943950436694,0.0706978211003209));
#81904=CARTESIAN_POINT('Ctrl Pts',(0.0130521460683091,-0.0327114338383318,
0.0707278326380061));
#81905=CARTESIAN_POINT('Ctrl Pts',(0.013016870246718,-0.0327619876830289,
0.0707523275349686));
#81906=CARTESIAN_POINT('Ctrl Pts',(0.0129822167655523,-0.0328131562602937,
0.0707763902899169));
#81907=CARTESIAN_POINT('Ctrl Pts',(0.0129141253233661,-0.0329167375858772,
0.0708236717644552));
#81908=CARTESIAN_POINT('Ctrl Pts',(0.0128807144936195,-0.032969108892063,
0.0708468716445758));
#81909=CARTESIAN_POINT('Ctrl Pts',(0.0128479134700188,-0.0330220786163187,
0.0708696480862609));
#81910=CARTESIAN_POINT('Ctrl Pts',(0.0127751424302828,-0.0331951640388604,
0.0707697445422947));
#81911=CARTESIAN_POINT('Ctrl Pts',(0.0127052578159129,-0.0330306422010619,
0.0706735806515658));
#81912=CARTESIAN_POINT('Ctrl Pts',(0.0126314583627242,-0.0328657861914644,
0.0705803873368121));
#81913=CARTESIAN_POINT('Ctrl Pts',(0.0127755024240191,-0.0331951640388604,
0.0707677486945326));
#81914=CARTESIAN_POINT('Ctrl Pts',(0.0127055765467763,-0.0330306422010619,
0.070671577361164));
#81915=CARTESIAN_POINT('Ctrl Pts',(0.0126317355583615,-0.0328657861914644,
0.0705783783155682));
#81916=CARTESIAN_POINT('Ctrl Pts',(0.0128354870616681,-0.0331951640388604,
0.0704351867837546));
#81917=CARTESIAN_POINT('Ctrl Pts',(0.0127586856801389,-0.0330306422010619,
0.0703377753064612));
#81918=CARTESIAN_POINT('Ctrl Pts',(0.0126779238060552,-0.0328657861914644,
0.0702436213484575));
#81919=CARTESIAN_POINT('',(0.012827541405468,-0.0331781648281926,0.0704251309730369));
#81920=CARTESIAN_POINT('',(0.0128354870616674,-0.0331951640388588,0.0704351867837537));
#81921=CARTESIAN_POINT('Origin',(0.000328943744506286,-0.0326412092589798,
0.0812312191671869));
#81922=CARTESIAN_POINT('Ctrl Pts',(0.0128275414055619,-0.033178164828644,
0.0704251309748706));
#81923=CARTESIAN_POINT('Ctrl Pts',(0.0127938444634669,-0.0331276811546771,
0.070451815327297));
#81924=CARTESIAN_POINT('Ctrl Pts',(0.0127607560047859,-0.0330765663497773,
0.0704780178694669));
#81925=CARTESIAN_POINT('Ctrl Pts',(0.0126957675247983,-0.0329730614463247,
0.0705294817187533));
#81926=CARTESIAN_POINT('Ctrl Pts',(0.0126638937540996,-0.0329207133374092,
0.0705547222313894));
#81927=CARTESIAN_POINT('Ctrl Pts',(0.0126326164868155,-0.0328677532289375,
0.0705794904450544));
#81928=CARTESIAN_POINT('',(0.0128054947428523,-0.0331951640388702,0.0706014677391519));
#81929=CARTESIAN_POINT('Origin',(0.00812378219310841,-0.0315241814719618,
0.07415));
#81930=CARTESIAN_POINT('',(0.0128275414038497,-0.0332121607144228,0.0704251309734935));
#81931=CARTESIAN_POINT('',(0.0128195742877286,-0.0331951640388587,0.070415092155874));
#81932=CARTESIAN_POINT('Origin',(0.00036281909636309,-0.0326413659571202,
0.0812613627328244));
#81933=CARTESIAN_POINT('Origin',(-0.0005554229849607,-0.0326412097086312,
0.0801144440300772));
#81934=CARTESIAN_POINT('Origin',(-0.000576998278988514,-0.032641366643145,
0.0800745605478936));
#81935=CARTESIAN_POINT('Ctrl Pts',(0.0127100841162299,-0.0336938721132648,
0.0706795048005746));
#81936=CARTESIAN_POINT('Ctrl Pts',(0.0126374324053212,-0.0335278710435225,
0.0705834946745518));
#81937=CARTESIAN_POINT('Ctrl Pts',(0.0125617954005258,-0.0333620469224385,
0.0704897966634334));
#81938=CARTESIAN_POINT('Ctrl Pts',(0.0124831199004146,-0.0331951640388588,
0.0703983767496028));
#81939=CARTESIAN_POINT('Ctrl Pts',(0.0126580394108509,-0.0336938721132648,
0.0706137828220148));
#81940=CARTESIAN_POINT('Ctrl Pts',(0.0125840118691422,-0.0335278710435225,
0.0705188622053191));
#81941=CARTESIAN_POINT('Ctrl Pts',(0.0125070336842901,-0.0333620469224385,
0.0704262964659372));
#81942=CARTESIAN_POINT('Ctrl Pts',(0.0124270511761946,-0.0331951640388588,
0.0703360523724446));
#81943=CARTESIAN_POINT('Ctrl Pts',(0.0126059947054719,-0.0336938721132648,
0.070548060843455));
#81944=CARTESIAN_POINT('Ctrl Pts',(0.0125305913329632,-0.0335278710435225,
0.0704542297360864));
#81945=CARTESIAN_POINT('Ctrl Pts',(0.0124522719680544,-0.0333620469224385,
0.0703627962684409));
#81946=CARTESIAN_POINT('Ctrl Pts',(0.0123709824519747,-0.0331951640388588,
0.0702737279952865));
#81947=CARTESIAN_POINT('Ctrl Pts',(0.0125539500000929,-0.0336938721132648,
0.0704823388648952));
#81948=CARTESIAN_POINT('Ctrl Pts',(0.0124771707967842,-0.0335278710435225,
0.0703895972668538));
#81949=CARTESIAN_POINT('Ctrl Pts',(0.0123975102518187,-0.0333620469224385,
0.0702992960709447));
#81950=CARTESIAN_POINT('Ctrl Pts',(0.0123149137277548,-0.0331951640388588,
0.0702114036181283));
#81951=CARTESIAN_POINT('',(0.0125539500000679,-0.0336938721132548,0.0704823388648649));
#81952=CARTESIAN_POINT('',(0.0123995251928226,-0.0333679846208724,0.0703034239711086));
#81953=CARTESIAN_POINT('Ctrl Pts',(0.0125539500000827,-0.0336938721132391,
0.0704823388648661));
#81954=CARTESIAN_POINT('Ctrl Pts',(0.0125396333981384,-0.0336629187933924,
0.0704650458416958));
#81955=CARTESIAN_POINT('Ctrl Pts',(0.0125252201173784,-0.0336319952301063,
0.0704478421786947));
#81956=CARTESIAN_POINT('Ctrl Pts',(0.0124743055998606,-0.0335235892595475,
0.0703877878201039));
#81957=CARTESIAN_POINT('Ctrl Pts',(0.0124372363719196,-0.0334458668645783,
0.0703453426725633));
#81958=CARTESIAN_POINT('Ctrl Pts',(0.0123995251747037,-0.0333679869902226,
0.0703034239873527));
#81959=CARTESIAN_POINT('Ctrl Pts',(0.0123995257414162,-0.0333679128829522,
0.0703034234792778));
#81960=CARTESIAN_POINT('Ctrl Pts',(0.0123991887346561,-0.0333391359256882,
0.0703037266598301));
#81961=CARTESIAN_POINT('Ctrl Pts',(0.0123989361660613,-0.0333103578181722,
0.0703039538774858));
#81962=CARTESIAN_POINT('Ctrl Pts',(0.0123987678149064,-0.0332815781851602,
0.0703041053308148));
#81963=CARTESIAN_POINT('Ctrl Pts',(0.0123985993192564,-0.0332527738506924,
0.0703042569141356));
#81964=CARTESIAN_POINT('Ctrl Pts',(0.0123985151930517,-0.0332239691459984,
0.0703043325963891));
#81965=CARTESIAN_POINT('Ctrl Pts',(0.0123985151930517,-0.0331951640388606,
0.0703043325963891));
#81966=CARTESIAN_POINT('',(0.0124821166583467,-0.0331951640388587,0.0703972615746475));
#81967=CARTESIAN_POINT('',(0.0124403159257087,-0.0331951640388687,0.0703507970855277));
#81968=CARTESIAN_POINT('',(0.0126326164750483,-0.0335216366556738,0.0705794904543482));
#81969=CARTESIAN_POINT('Origin',(0.000362536508306777,-0.0326434571528194,
0.0818407427209279));
#81970=CARTESIAN_POINT('',(0.012631551438155,-0.0336938721132328,0.0705803338484653));
#81971=CARTESIAN_POINT('Origin',(0.0211928399800403,-0.0336938867896311,
0.0638007196656732));
#81972=CARTESIAN_POINT('',(0.0125927507191215,-0.0336938721132538,0.0705313363566751));
#81973=CARTESIAN_POINT('Ctrl Pts',(0.0129699281877454,-0.0335235895815172,
0.0706123639250602));
#81974=CARTESIAN_POINT('Ctrl Pts',(0.0129212256622093,-0.0334144449262749,
0.0705456471842605));
#81975=CARTESIAN_POINT('Ctrl Pts',(0.0128710888657169,-0.0333049234473147,
0.0704798599515335));
#81976=CARTESIAN_POINT('Ctrl Pts',(0.012819574287733,-0.0331951640388587,
0.0704150921558742));
#81977=CARTESIAN_POINT('Ctrl Pts',(0.0128571109630711,-0.0335235895815172,
0.0706017128076103));
#81978=CARTESIAN_POINT('Ctrl Pts',(0.0128082618039332,-0.0334144449262749,
0.070536549218025));
#81979=CARTESIAN_POINT('Ctrl Pts',(0.01275801029231,-0.0333049234473147,
0.0704723199502347));
#81980=CARTESIAN_POINT('Ctrl Pts',(0.01270641324481,-0.0331951640388587,
0.0704091129543632));
#81981=CARTESIAN_POINT('Ctrl Pts',(0.0127442937383968,-0.0335235895815172,
0.0705910616901604));
#81982=CARTESIAN_POINT('Ctrl Pts',(0.0126952979456571,-0.0334144449262749,
0.0705274512517894));
#81983=CARTESIAN_POINT('Ctrl Pts',(0.012644931718903,-0.0333049234473147,
0.0704647799489359));
#81984=CARTESIAN_POINT('Ctrl Pts',(0.012593252201887,-0.0331951640388587,
0.0704031337528521));
#81985=CARTESIAN_POINT('Ctrl Pts',(0.0126314765137225,-0.0335235895815172,
0.0705804105727106));
#81986=CARTESIAN_POINT('Ctrl Pts',(0.012582334087381,-0.0334144449262749,
0.0705183532855539));
#81987=CARTESIAN_POINT('Ctrl Pts',(0.0125318531454961,-0.0333049234473147,
0.0704572399476371));
#81988=CARTESIAN_POINT('Ctrl Pts',(0.0124800911589639,-0.0331951640388587,
0.0703971545513411));
#81989=CARTESIAN_POINT('',(0.0126508454730476,-0.0331951640388687,0.0704061768652707));
#81990=CARTESIAN_POINT('Ctrl Pts',(0.0128275414013884,-0.0332121607145979,
0.0704251309754337));
#81991=CARTESIAN_POINT('Ctrl Pts',(0.0127939011387833,-0.0332625444107923,
0.070451770428392));
#81992=CARTESIAN_POINT('Ctrl Pts',(0.0127608405506896,-0.0333135300743102,
0.0704779508417744));
#81993=CARTESIAN_POINT('Ctrl Pts',(0.0126958524803037,-0.0334167203135638,
0.070529414371183));
#81994=CARTESIAN_POINT('Ctrl Pts',(0.0126639501685649,-0.0334688847580745,
0.0705546775548508));
#81995=CARTESIAN_POINT('Ctrl Pts',(0.0126326164748062,-0.0335216366554488,
0.0705794904545209));
#81996=CARTESIAN_POINT('Ctrl Pts',(0.012553950000081,-0.0336938721132391,
0.0704823388648808));
#81997=CARTESIAN_POINT('Ctrl Pts',(0.0125324819623981,-0.0336474569764958,
0.0704564076226211));
#81998=CARTESIAN_POINT('Ctrl Pts',(0.0125107118377876,-0.033601104548885,
0.0704307294676731));
#81999=CARTESIAN_POINT('Ctrl Pts',(0.0124555948875392,-0.0334837508592656,
0.070365718283123));
#82000=CARTESIAN_POINT('Ctrl Pts',(0.0123985757244046,-0.0333660264659097,
0.070302368876206));
#82001=CARTESIAN_POINT('Ctrl Pts',(0.0125931684438169,-0.0336938721132391,
0.0701446526896404));
#82002=CARTESIAN_POINT('Ctrl Pts',(0.0125697238168942,-0.0336474569764958,
0.0701184918888154));
#82003=CARTESIAN_POINT('Ctrl Pts',(0.0125459745512081,-0.033601104548885,
0.0700926073295044));
#82004=CARTESIAN_POINT('Ctrl Pts',(0.0124858468707896,-0.0334837508592656,
0.0700270735765623));
#82005=CARTESIAN_POINT('Ctrl Pts',(0.0124238036930434,-0.0333660264659097,
0.0699633503090509));
#82006=CARTESIAN_POINT('',(0.0125843731495699,-0.0336769361243754,0.0701371296657961));
#82007=CARTESIAN_POINT('',(0.0125929345365934,-0.0336938721132327,0.070146666722502));
#82008=CARTESIAN_POINT('Ctrl Pts',(0.0125843731495697,-0.0336769361243751,
0.0701371296657959));
#82009=CARTESIAN_POINT('Ctrl Pts',(0.0125858018519977,-0.0336797586669916,
0.0701387177702196));
#82010=CARTESIAN_POINT('Ctrl Pts',(0.0125872296522721,-0.0336825812712627,
0.0701403065775715));
#82011=CARTESIAN_POINT('Ctrl Pts',(0.0125900834494012,-0.0336882266040365,
0.0701434855983503));
#82012=CARTESIAN_POINT('Ctrl Pts',(0.0125915094462306,-0.0336910493324964,
0.0701450758117581));
#82013=CARTESIAN_POINT('Ctrl Pts',(0.0125929345365926,-0.0336938721132319,
0.0701466667225041));
#82014=CARTESIAN_POINT('Ctrl Pts',(0.0125843731495699,-0.0336769361243754,
0.0701371296657961));
#82015=CARTESIAN_POINT('Ctrl Pts',(0.0125532146497868,-0.0336279031428258,
0.0701651607093637));
#82016=CARTESIAN_POINT('Ctrl Pts',(0.0125216078565492,-0.0335767852155843,
0.0701935950500561));
#82017=CARTESIAN_POINT('Ctrl Pts',(0.0124596750994393,-0.0334733199122746,
0.0702493114621073));
#82018=CARTESIAN_POINT('Ctrl Pts',(0.0124293075518341,-0.0334209645148378,
0.070276630943336));
#82019=CARTESIAN_POINT('Ctrl Pts',(0.0123995251713282,-0.0333679869844681,
0.0703034239921451));
#82020=CARTESIAN_POINT('',(0.0125734422683407,-0.0336938721132538,0.0703145027936935));
#82021=CARTESIAN_POINT('Origin',(0.00812378219310841,-0.0315241814719618,
0.07415));
#82022=CARTESIAN_POINT('',(0.012584373148611,-0.033710812065555,0.0701371296666677));
#82023=CARTESIAN_POINT('',(0.0125757914107549,-0.0336938721132327,0.070127610918123));
#82024=CARTESIAN_POINT('Origin',(-0.000326540335926023,-0.0345562521474037,
0.0802488360553175));
#82025=CARTESIAN_POINT('Ctrl Pts',(0.0125757914107646,-0.0336938721132364,
0.0701276109181209));
#82026=CARTESIAN_POINT('Ctrl Pts',(0.0125772232981681,-0.033691049305624,
0.070129195741416));
#82027=CARTESIAN_POINT('Ctrl Pts',(0.0125786543761196,-0.0336882265905996,
0.07013078137002));
#82028=CARTESIAN_POINT('Ctrl Pts',(0.0125815149506136,-0.0336825812712941,
0.0701339542799855));
#82029=CARTESIAN_POINT('Ctrl Pts',(0.0125829444471341,-0.0336797586670073,
0.0701355415613637));
#82030=CARTESIAN_POINT('Ctrl Pts',(0.0125843731495701,-0.0336769361243751,
0.0701371296657963));
#82031=CARTESIAN_POINT('Origin',(0.00116839656982703,-0.0345562520431624,
0.0819105626205519));
#82032=CARTESIAN_POINT('Ctrl Pts',(0.0125056360034304,-0.0342436276873911,
0.0704247507217681));
#82033=CARTESIAN_POINT('Ctrl Pts',(0.0123651359107284,-0.033943005420181,
0.0702594863808946));
#82034=CARTESIAN_POINT('Ctrl Pts',(0.0122125865767564,-0.0336441434784052,
0.0701052745813516));
#82035=CARTESIAN_POINT('Ctrl Pts',(0.0123396054690808,-0.0342436276873911,
0.070237844698153));
#82036=CARTESIAN_POINT('Ctrl Pts',(0.0121920560994895,-0.033943005420181,
0.0700788423021119));
#82037=CARTESIAN_POINT('Ctrl Pts',(0.0120329491902269,-0.0336441434784052,
0.0699314056382915));
#82038=CARTESIAN_POINT('Ctrl Pts',(0.0123379451637373,-0.0342436276873911,
0.0702359756379168));
#82039=CARTESIAN_POINT('Ctrl Pts',(0.0121903253013771,-0.033943005420181,
0.0700770358613241));
#82040=CARTESIAN_POINT('Ctrl Pts',(0.0120311528163616,-0.0336441434784052,
0.0699296669488608));
#82041=CARTESIAN_POINT('',(0.0123149137277548,-0.0341934961088741,0.0702114036181282));
#82042=CARTESIAN_POINT('',(0.0121495594626338,-0.0338664212862451,0.0700425382074119));
#82043=CARTESIAN_POINT('Origin',(-0.000223393381571894,-0.0345610720405284,
0.0812949048066704));
#82044=CARTESIAN_POINT('Origin',(0.0198255785810367,-0.0336938005073078,
0.0622107149897495));
#82045=CARTESIAN_POINT('',(0.0122378800854608,-0.0336938721132327,0.0701310046613436));
#82046=CARTESIAN_POINT('',(0.0121932443076082,-0.0336938721132427,0.070087256548999));
#82047=CARTESIAN_POINT('',(0.0123995251713318,-0.0340203938281605,0.0703034239921491));
#82048=CARTESIAN_POINT('Origin',(-0.000482693489046462,-0.0345589643244883,
0.0808895652102122));
#82049=CARTESIAN_POINT('',(0.0123985151930508,-0.034193496108874,0.0703043325963879));
#82050=CARTESIAN_POINT('Origin',(0.0205907235866023,-0.0341934220717551,
0.0629343977337704));
#82051=CARTESIAN_POINT('',(0.0123567144604128,-0.0341934961088841,0.0702578681072681));
#82052=CARTESIAN_POINT('Ctrl Pts',(0.0127382371674446,-0.0340223579322397,
0.070315054721398));
#82053=CARTESIAN_POINT('Ctrl Pts',(0.0126853432700955,-0.0339125849573575,
0.0702514093522981));
#82054=CARTESIAN_POINT('Ctrl Pts',(0.0126311692294267,-0.0338030433565231,
0.0701889034868289));
#82055=CARTESIAN_POINT('Ctrl Pts',(0.0125757914107587,-0.0336938721132327,
0.070127610918123));
#82056=CARTESIAN_POINT('Ctrl Pts',(0.0126249737418219,-0.0340223579322397,
0.0703115084209783));
#82057=CARTESIAN_POINT('Ctrl Pts',(0.0125720309317409,-0.0339125849573575,
0.0702494252499211));
#82058=CARTESIAN_POINT('Ctrl Pts',(0.01251784034658,-0.0338030433565231,
0.0701884814971361));
#82059=CARTESIAN_POINT('Ctrl Pts',(0.0124624781957316,-0.0336938721132327,
0.0701287489562014));
#82060=CARTESIAN_POINT('Ctrl Pts',(0.0125117103161992,-0.0340223579322397,
0.0703079621205585));
#82061=CARTESIAN_POINT('Ctrl Pts',(0.0124587185933862,-0.0339125849573575,
0.0702474411475441));
#82062=CARTESIAN_POINT('Ctrl Pts',(0.0124045114637332,-0.0338030433565231,
0.0701880595074433));
#82063=CARTESIAN_POINT('Ctrl Pts',(0.0123491649807044,-0.0336938721132327,
0.0701298869942798));
#82064=CARTESIAN_POINT('Ctrl Pts',(0.0123984468905764,-0.0340223579322397,
0.0703044158201387));
#82065=CARTESIAN_POINT('Ctrl Pts',(0.0123454062550316,-0.0339125849573575,
0.0702454570451671));
#82066=CARTESIAN_POINT('Ctrl Pts',(0.0122911825808865,-0.0338030433565231,
0.0701876375177504));
#82067=CARTESIAN_POINT('Ctrl Pts',(0.0122358517656772,-0.0336938721132327,
0.0701310250323582));
#82068=CARTESIAN_POINT('',(0.0124068357481178,-0.0336938721132427,0.0701293077897433));
#82069=CARTESIAN_POINT('Ctrl Pts',(0.0125843731459267,-0.0337108120662694,
0.0701371296690737));
#82070=CARTESIAN_POINT('Ctrl Pts',(0.0125524061304323,-0.0337611408993759,
0.0701658880756172));
#82071=CARTESIAN_POINT('Ctrl Pts',(0.0125210224420479,-0.0338121088780195,
0.0701941217050455));
#82072=CARTESIAN_POINT('Ctrl Pts',(0.0124593931293299,-0.0339153382773244,
0.070249565130174));
#82073=CARTESIAN_POINT('Ctrl Pts',(0.0124291735780691,-0.0339675558473119,
0.0702767514698207));
#82074=CARTESIAN_POINT('Ctrl Pts',(0.0123995251712986,-0.0340203938281304,
0.0703034239921718));
#82075=CARTESIAN_POINT('Ctrl Pts',(0.0123148067138119,-0.0341934961088741,
0.0702134289403001));
#82076=CARTESIAN_POINT('Ctrl Pts',(0.0122334212084299,-0.0340287516182428,
0.0701267828100733));
#82077=CARTESIAN_POINT('Ctrl Pts',(0.0121485240951087,-0.033864463327595,
0.0700435744419888));
#82078=CARTESIAN_POINT('Ctrl Pts',(0.0123149137277548,-0.0341934961088741,
0.0702114036181283));
#82079=CARTESIAN_POINT('Ctrl Pts',(0.0122334863504325,-0.0340287516182428,
0.0701247552754726));
#82080=CARTESIAN_POINT('Ctrl Pts',(0.0121485473095084,-0.033864463327595,
0.0700415464274487));
#82081=CARTESIAN_POINT('Ctrl Pts',(0.0123327443089812,-0.0341934961088741,
0.0698739459887476));
#82082=CARTESIAN_POINT('Ctrl Pts',(0.0122443402610246,-0.0340287516182428,
0.0697869290128721));
#82083=CARTESIAN_POINT('Ctrl Pts',(0.0121524152750071,-0.033864463327595,
0.0697036401977087));
#82084=CARTESIAN_POINT('',(0.0123236009792153,-0.0341764758832411,0.0698649653263334));
#82085=CARTESIAN_POINT('',(0.0123327443089812,-0.034193496108874,0.0698739459887476));
#82086=CARTESIAN_POINT('Origin',(0.000367949148720214,-0.0345621026500832,
0.0813316002940054));
#82087=CARTESIAN_POINT('Ctrl Pts',(0.0123236009797485,-0.0341764758837509,
0.0698649653280674));
#82088=CARTESIAN_POINT('Ctrl Pts',(0.012293555221579,-0.0341260050040218,
0.0698956207454876));
#82089=CARTESIAN_POINT('Ctrl Pts',(0.0122640317568554,-0.0340749269147712,
0.0699257433261768));
#82090=CARTESIAN_POINT('Ctrl Pts',(0.0122060064023127,-0.0339715436305228,
0.0699849460310153));
#82091=CARTESIAN_POINT('Ctrl Pts',(0.0121775265216962,-0.0339192778235013,
0.0700140036908399));
#82092=CARTESIAN_POINT('Ctrl Pts',(0.0121495594643107,-0.0338664212852959,
0.070042538207297));
#82093=CARTESIAN_POINT('',(0.012323829018378,-0.0341934961088841,0.0700426748034479));
#82094=CARTESIAN_POINT('Origin',(0.00812378219310841,-0.0315241814719618,
0.07415));
#82095=CARTESIAN_POINT('',(0.0123236009780977,-0.0342105180190549,0.0698649653262714));
#82096=CARTESIAN_POINT('',(0.0123144384873286,-0.0341934961088739,0.0698560042124233));
#82097=CARTESIAN_POINT('Origin',(0.000396441343576246,-0.0345621714110604,
0.0813668513846585));
#82098=CARTESIAN_POINT('Origin',(0.00109940268487801,-0.0345621032237729,
0.082048509369557));
#82099=CARTESIAN_POINT('Origin',(0.00106358853260313,-0.0345621720573663,
0.0820207289396908));
#82100=CARTESIAN_POINT('Ctrl Pts',(0.012238951351207,-0.0346945769586966,
0.0701320546229771));
#82101=CARTESIAN_POINT('Ctrl Pts',(0.0121547938765877,-0.0345275153362944,
0.0700458607573369));
#82102=CARTESIAN_POINT('Ctrl Pts',(0.0120679039167965,-0.0343603235965185,
0.0699622912726633));
#82103=CARTESIAN_POINT('Ctrl Pts',(0.0119785421272265,-0.034193496108874,
0.0698815895109745));
#82104=CARTESIAN_POINT('Ctrl Pts',(0.0121790798919958,-0.0346945769586966,
0.0700733738191504));
#82105=CARTESIAN_POINT('Ctrl Pts',(0.0120936933244458,-0.0345275153362944,
0.0699884339851946));
#82106=CARTESIAN_POINT('Ctrl Pts',(0.0120056133919598,-0.0343603235965185,
0.0699061575104035));
#82107=CARTESIAN_POINT('Ctrl Pts',(0.011915104212505,-0.034193496108874,
0.0698267838603386));
#82108=CARTESIAN_POINT('Ctrl Pts',(0.0121192084327849,-0.0346945769586966,
0.0700146930153222));
#82109=CARTESIAN_POINT('Ctrl Pts',(0.0120325927723039,-0.0345275153362944,
0.0699310072130522));
#82110=CARTESIAN_POINT('Ctrl Pts',(0.011943322867123,-0.0343603235965185,
0.0698500237481442));
#82111=CARTESIAN_POINT('Ctrl Pts',(0.0118516662977839,-0.034193496108874,
0.0697719782097026));
#82112=CARTESIAN_POINT('Ctrl Pts',(0.0120593369735733,-0.0346945769586966,
0.0699560122114968));
#82113=CARTESIAN_POINT('Ctrl Pts',(0.011971492220162,-0.0345275153362944,
0.0698735804409099));
#82114=CARTESIAN_POINT('Ctrl Pts',(0.0118810323422863,-0.0343603235965185,
0.0697938899858841));
#82115=CARTESIAN_POINT('Ctrl Pts',(0.0117882283830619,-0.034193496108874,
0.069717172559067));
#82116=CARTESIAN_POINT('',(0.0120593369740059,-0.0346945769586966,0.069956012211921));
#82117=CARTESIAN_POINT('',(0.0118837058515021,-0.034366772783148,0.0697978626993801));
#82118=CARTESIAN_POINT('Origin',(0.000688184036314178,-0.0345626457063121,
0.0823412505265048));
#82119=CARTESIAN_POINT('Origin',(0.0191090129876251,-0.0341934771028923,
0.0614345146097458));
#82120=CARTESIAN_POINT('',(0.0119774070477464,-0.034193496108874,0.069880608886537));
#82121=CARTESIAN_POINT('',(0.0119301123817021,-0.0341934961088841,0.0698397498047804));
#82122=CARTESIAN_POINT('',(0.0121495594633213,-0.0345211942962664,0.070042538208269));
#82123=CARTESIAN_POINT('Origin',(0.000347128644582184,-0.0345625596120204,
0.0820023227910331));
#82124=CARTESIAN_POINT('',(0.0121486085297354,-0.0346945769586887,0.0700435084366343));
#82125=CARTESIAN_POINT('Origin',(0.0198927720703194,-0.0346945685853879,
0.0621422144752763));
#82126=CARTESIAN_POINT('',(0.0121039727518807,-0.0346945769587026,0.0699997603242877));
#82127=CARTESIAN_POINT('Ctrl Pts',(0.0124883327279811,-0.0345231616327842,
0.0700328773848013));
#82128=CARTESIAN_POINT('Ctrl Pts',(0.0124315839891756,-0.0344132092796988,
0.0699727182004737));
#82129=CARTESIAN_POINT('Ctrl Pts',(0.0123735938330692,-0.0343032738558979,
0.0699137359229829));
#82130=CARTESIAN_POINT('Ctrl Pts',(0.0123144384873313,-0.0341934961088739,
0.0698560042124231));
#82131=CARTESIAN_POINT('Ctrl Pts',(0.0123750703210705,-0.0345231616327842,
0.0700364499636191));
#82132=CARTESIAN_POINT('Ctrl Pts',(0.0123183708252341,-0.0344132092796988,
0.0699778519421101));
#82133=CARTESIAN_POINT('Ctrl Pts',(0.0122604622009777,-0.0343032738558979,
0.069920429728337));
#82134=CARTESIAN_POINT('Ctrl Pts',(0.0122014205203234,-0.0341934961088739,
0.0698642549864478));
#82135=CARTESIAN_POINT('Ctrl Pts',(0.0122618079141598,-0.0345231616327842,
0.0700400225424369));
#82136=CARTESIAN_POINT('Ctrl Pts',(0.0122051576612927,-0.0344132092796988,
0.0699829856837465));
#82137=CARTESIAN_POINT('Ctrl Pts',(0.0121473305688863,-0.0343032738558979,
0.0699271235336912));
#82138=CARTESIAN_POINT('Ctrl Pts',(0.0120884025533155,-0.0341934961088739,
0.0698725057604725));
#82139=CARTESIAN_POINT('Ctrl Pts',(0.0121485455072491,-0.0345231616327842,
0.0700435951212548));
#82140=CARTESIAN_POINT('Ctrl Pts',(0.0120919444973512,-0.0344132092796988,
0.0699881194253828));
#82141=CARTESIAN_POINT('Ctrl Pts',(0.0120341989367948,-0.0343032738558979,
0.0699338173390453));
#82142=CARTESIAN_POINT('Ctrl Pts',(0.0119753845863076,-0.0341934961088739,
0.0698807565344973));
#82143=CARTESIAN_POINT('',(0.0121459227675475,-0.0341934961088839,0.0698683065494902));
#82144=CARTESIAN_POINT('Ctrl Pts',(0.0123236009756735,-0.03421051801954,
0.0698649653287348));
#82145=CARTESIAN_POINT('Ctrl Pts',(0.012293521430468,-0.0342610556240684,
0.0698956551991256));
#82146=CARTESIAN_POINT('Ctrl Pts',(0.0122639816471471,-0.0343122189868869,
0.0699257943556619));
#82147=CARTESIAN_POINT('Ctrl Pts',(0.0122059557101443,-0.0344158119695154,
0.0699849976605572));
#82148=CARTESIAN_POINT('Ctrl Pts',(0.0121774932896023,-0.034468199045003,
0.0700140375942222));
#82149=CARTESIAN_POINT('Ctrl Pts',(0.0121495594632927,-0.034521194296245,
0.0700425382082808));
#82150=CARTESIAN_POINT('Ctrl Pts',(0.0120593573372814,-0.0346945769586932,
0.0699580397604875));
#82151=CARTESIAN_POINT('Ctrl Pts',(0.0119726915254654,-0.034529677707698,
0.0698766745291053));
#82152=CARTESIAN_POINT('Ctrl Pts',(0.0118827368687214,-0.034364806625142,
0.0697989608009381));
#82153=CARTESIAN_POINT('Ctrl Pts',(0.0120593369740125,-0.0346945769586932,
0.0699560122119273));
#82154=CARTESIAN_POINT('Ctrl Pts',(0.0119726292440646,-0.034529677707698,
0.0698746474015413));
#82155=CARTESIAN_POINT('Ctrl Pts',(0.0118826327224075,-0.034364806625142,
0.0697969358265254));
#82156=CARTESIAN_POINT('Ctrl Pts',(0.0120559432307921,-0.0346945769586932,
0.0696181008866346));
#82157=CARTESIAN_POINT('Ctrl Pts',(0.0119622494232922,-0.034529677707698,
0.0695368062394883));
#82158=CARTESIAN_POINT('Ctrl Pts',(0.0118652756935101,-0.034364806625142,
0.0694594535087634));
#82159=CARTESIAN_POINT('',(0.0120462540429111,-0.0346775396664993,0.0696097120596878));
#82160=CARTESIAN_POINT('',(0.0120559432307895,-0.0346945769586886,0.0696181008866323));
#82161=CARTESIAN_POINT('Origin',(0.00130906264192214,-0.034562661834901,
0.0822716875907431));
#82162=CARTESIAN_POINT('Ctrl Pts',(0.0120462540434552,-0.0346775396670097,
0.0696097120614208));
#82163=CARTESIAN_POINT('Ctrl Pts',(0.0120181703416947,-0.0346269749928187,
0.0696422191576203));
#82164=CARTESIAN_POINT('Ctrl Pts',(0.0119905857771611,-0.0345757902890786,
0.0696741485536673));
#82165=CARTESIAN_POINT('Ctrl Pts',(0.0119363920746166,-0.0344721681088032,
0.0697368781285126));
#82166=CARTESIAN_POINT('Ctrl Pts',(0.0119098041788283,-0.0344197714289985,
0.069767653710673));
#82167=CARTESIAN_POINT('Ctrl Pts',(0.0118837058517475,-0.0343667727830668,
0.0697978626994496));
#82168=CARTESIAN_POINT('',(0.0120576401024077,-0.0346945769587026,0.0697870565492867));
#82169=CARTESIAN_POINT('Origin',(0.00812378219310841,-0.0315241814719618,
0.07415));
#82170=CARTESIAN_POINT('',(0.0120462540415805,-0.0347116136489625,0.0696097120600979));
#82171=CARTESIAN_POINT('',(0.0120365469580378,-0.0346945769586885,0.0696013439463572));
#82172=CARTESIAN_POINT('Origin',(0.00134454427527055,-0.034562669423854,
0.0822998697148694));
#82173=CARTESIAN_POINT('Origin',(0.00107793587347129,-0.0345626624041072,
0.0820720131763714));
#82174=CARTESIAN_POINT('Origin',(0.00104490125481206,-0.0345626700230594,
0.0820409986768044));
#82175=CARTESIAN_POINT('Ctrl Pts',(0.0120060286039437,-0.0352450361874068,
0.0699065432214784));
#82176=CARTESIAN_POINT('Ctrl Pts',(0.011845984005332,-0.0349452760959493,
0.0697601218954314));
#82177=CARTESIAN_POINT('Ctrl Pts',(0.0116753650231926,-0.034644428984174,
0.0696261717509751));
#82178=CARTESIAN_POINT('Ctrl Pts',(0.0120041282978596,-0.0352450361874068,
0.0699048805544081));
#82179=CARTESIAN_POINT('Ctrl Pts',(0.0118440209907302,-0.0349452760959493,
0.0697585308995812));
#82180=CARTESIAN_POINT('Ctrl Pts',(0.0116733448767912,-0.034644428984174,
0.0696246569461966));
#82181=CARTESIAN_POINT('Ctrl Pts',(0.0118159791806163,-0.0352450361874068,
0.0697402600524025));
#82182=CARTESIAN_POINT('Ctrl Pts',(0.0116496631093728,-0.0349452760959493,
0.0696010065579749));
#82183=CARTESIAN_POINT('Ctrl Pts',(0.0114733303816012,-0.034644428984174,
0.0694746762750623));
#82184=CARTESIAN_POINT('Ctrl Pts',(0.0118140976894439,-0.0352450361874068,
0.0697386138473825));
#82185=CARTESIAN_POINT('Ctrl Pts',(0.0116477195305592,-0.0349452760959493,
0.069599431314559));
#82186=CARTESIAN_POINT('Ctrl Pts',(0.0114713302366493,-0.034644428984174,
0.069473176468351));
#82187=CARTESIAN_POINT('',(0.0117882548360518,-0.0351951634053341,0.0697171913472817));
#82188=CARTESIAN_POINT('',(0.0116030135390007,-0.0348678972925388,0.0695703630884358));
#82189=CARTESIAN_POINT('Origin',(0.00180673700457118,-0.0345636767884998,
0.0831624060402997));
#82190=CARTESIAN_POINT('Origin',(0.0182875125888102,-0.0346946199340978,
0.0607717005939312));
#82191=CARTESIAN_POINT('',(0.0117017255272817,-0.0346945769330288,0.0696470624592927));
#82192=CARTESIAN_POINT('',(0.0116519586167633,-0.0346945769458128,0.0696092536546967));
#82193=CARTESIAN_POINT('',(0.0118837058516422,-0.0350221583435276,0.0697978626995465));
#82194=CARTESIAN_POINT('Origin',(0.00140024348590816,-0.0345628458718178,
0.0829056835978697));
#82195=CARTESIAN_POINT('',(0.0118828995328131,-0.0351951360298762,0.0697988006455434));
#82196=CARTESIAN_POINT('Origin',(0.0190865024647824,-0.0351951838366724,
0.061460578494381));
#82197=CARTESIAN_POINT('',(0.0117882283836044,-0.0351951371328748,0.0697171725593821));
#82198=CARTESIAN_POINT('Ctrl Pts',(0.0122212033147025,-0.0350241211494343,
0.0697669485341435));
#82199=CARTESIAN_POINT('Ctrl Pts',(0.0121608285778814,-0.0349144232818962,
0.0697105082382016));
#82200=CARTESIAN_POINT('Ctrl Pts',(0.012099251042623,-0.0348045283579412,
0.0696552821489737));
#82201=CARTESIAN_POINT('Ctrl Pts',(0.012036546949615,-0.0346945769439158,
0.06960134393911));
#82202=CARTESIAN_POINT('Ctrl Pts',(0.0121083887061872,-0.0350241211494343,
0.0697776258890849));
#82203=CARTESIAN_POINT('Ctrl Pts',(0.0120481610455526,-0.0349144232818962,
0.0697227395681195));
#82204=CARTESIAN_POINT('Ctrl Pts',(0.0119867627962859,-0.0348045283579412,
0.0696690653438272));
#82205=CARTESIAN_POINT('Ctrl Pts',(0.011924270043401,-0.0346945769439158,
0.0696166748925707));
#82206=CARTESIAN_POINT('Ctrl Pts',(0.0119955740976719,-0.0350241211494343,
0.0697883032440263));
#82207=CARTESIAN_POINT('Ctrl Pts',(0.0119354935132237,-0.0349144232818962,
0.0697349708980374));
#82208=CARTESIAN_POINT('Ctrl Pts',(0.0118742745499488,-0.0348045283579412,
0.0696828485386806));
#82209=CARTESIAN_POINT('Ctrl Pts',(0.011811993137187,-0.0346945769439158,
0.0696320058460315));
#82210=CARTESIAN_POINT('Ctrl Pts',(0.0118827594891566,-0.0350241211494343,
0.0697989805989677));
#82211=CARTESIAN_POINT('Ctrl Pts',(0.0118228259808948,-0.0349144232818962,
0.0697472022279553));
#82212=CARTESIAN_POINT('Ctrl Pts',(0.0117617863036118,-0.0348045283579412,
0.0696966317335341));
#82213=CARTESIAN_POINT('Ctrl Pts',(0.011699716230973,-0.0346945769439158,
0.0696473367994923));
#82214=CARTESIAN_POINT('',(0.0118691362429459,-0.0346945769458128,0.0696242032029469));
#82215=CARTESIAN_POINT('Ctrl Pts',(0.0120462540394248,-0.034711613649281,
0.0696097120625826));
#82216=CARTESIAN_POINT('Ctrl Pts',(0.0120181814806057,-0.0347621546531728,
0.0696422062410426));
#82217=CARTESIAN_POINT('Ctrl Pts',(0.0119906025132298,-0.0348133084095833,
0.069674129084038));
#82218=CARTESIAN_POINT('Ctrl Pts',(0.0119364087447131,-0.0349168561544578,
0.0697368587410297));
#82219=CARTESIAN_POINT('Ctrl Pts',(0.0119098154395837,-0.0349692089015919,
0.0697676406732463));
#82220=CARTESIAN_POINT('Ctrl Pts',(0.0118837058516033,-0.0350221583435,
0.0697978626995612));
#82221=CARTESIAN_POINT('Ctrl Pts',(0.0117883349063016,-0.0351951371254968,
0.0697186316936575));
#82222=CARTESIAN_POINT('Ctrl Pts',(0.0116967191469006,-0.0350307338980959,
0.0696428693655287));
#82223=CARTESIAN_POINT('Ctrl Pts',(0.0116020503338566,-0.0348659306897807,
0.0695709583540564));
#82224=CARTESIAN_POINT('Ctrl Pts',(0.0117882283835361,-0.0351951371254968,
0.0697171725594763));
#82225=CARTESIAN_POINT('Ctrl Pts',(0.0116965824574513,-0.0350307338980959,
0.0696414124336389));
#82226=CARTESIAN_POINT('Ctrl Pts',(0.011601883594524,-0.0348659306897807,
0.0695695048693978));
#82227=CARTESIAN_POINT('Ctrl Pts',(0.011770375057007,-0.0351951371254967,
0.0694726201498912));
#82228=CARTESIAN_POINT('Ctrl Pts',(0.0116736731632914,-0.0350307338980959,
0.0693972291303782));
#82229=CARTESIAN_POINT('Ctrl Pts',(0.0115739379085905,-0.0348659306897807,
0.0693258993256601));
#82230=CARTESIAN_POINT('Origin',(0.0148201985662875,-0.0308609197410856,
0.0653356520739864));
#82231=CARTESIAN_POINT('',(0.0117804447357082,-0.0351951371254968,0.0696105532228179));
#82232=CARTESIAN_POINT('Origin',(0.00765165544607738,-0.0351840467441093,
0.0750054776357416));
#82233=CARTESIAN_POINT('Origin',(0.0147132492090122,-0.0352322613180634,
0.0641627590476698));
#82234=CARTESIAN_POINT('',(0.0114116499145033,-0.0351951142564672,0.069431129326838));
#82235=CARTESIAN_POINT('',(0.0113078379568051,-0.0351951372916787,0.0693620684117596));
#82236=CARTESIAN_POINT('Origin',(0.00778340221991616,-0.0352875121180037,
0.074138041142237));
#82237=CARTESIAN_POINT('Origin',(0.0134603339411495,-0.029832507652317,
0.0794241260621529));
#82238=CARTESIAN_POINT('Origin',(0.0150506355830869,-0.0338732794983985,
0.069431195039007));
#82239=CARTESIAN_POINT('Ctrl Pts',(0.0135575492129203,-0.0321934096636942,
0.0722652422649808));
#82240=CARTESIAN_POINT('Ctrl Pts',(0.0135238129470215,-0.0320508460845295,
0.0721679804229908));
#82241=CARTESIAN_POINT('Ctrl Pts',(0.0134874888845993,-0.0319086045665006,
0.0720716983436474));
#82242=CARTESIAN_POINT('Ctrl Pts',(0.0134486723049796,-0.0317669892870789,
0.0719765969003001));
#82243=CARTESIAN_POINT('Ctrl Pts',(0.0135283559758708,-0.0321934096636942,
0.0721866408175494));
#82244=CARTESIAN_POINT('Ctrl Pts',(0.0134932127814944,-0.0320508460845295,
0.0720899015206002));
#82245=CARTESIAN_POINT('Ctrl Pts',(0.0134554968911776,-0.0319086045665006,
0.071994179393689));
#82246=CARTESIAN_POINT('Ctrl Pts',(0.0134153064818377,-0.0317669892870789,
0.0718996738577699));
#82247=CARTESIAN_POINT('Ctrl Pts',(0.0134991627388212,-0.0321934096636942,
0.0721080393701181));
#82248=CARTESIAN_POINT('Ctrl Pts',(0.0134626126159674,-0.0320508460845295,
0.0720118226182097));
#82249=CARTESIAN_POINT('Ctrl Pts',(0.0134235048977559,-0.0319086045665006,
0.0719166604437308));
#82250=CARTESIAN_POINT('Ctrl Pts',(0.013381940658696,-0.0317669892870789,
0.0718227508152399));
#82251=CARTESIAN_POINT('Ctrl Pts',(0.0134699695017717,-0.0321934096636942,
0.0720294379226868));
#82252=CARTESIAN_POINT('Ctrl Pts',(0.0134320124504403,-0.0320508460845295,
0.0719337437158192));
#82253=CARTESIAN_POINT('Ctrl Pts',(0.0133915129043343,-0.0319086045665006,
0.0718391414937724));
#82254=CARTESIAN_POINT('Ctrl Pts',(0.0133485748355541,-0.0317669892870789,
0.0717458277727096));
#82255=CARTESIAN_POINT('',(0.0134704917745492,-0.0321934096636942,0.0720308441181146));
#82256=CARTESIAN_POINT('',(0.0133789127702746,-0.0318665617511327,0.0718129660665446));
#82257=CARTESIAN_POINT('Origin',(-0.00227972748522134,-0.0326371944424414,
0.0776119280737242));
#82258=CARTESIAN_POINT('Origin',(0.0233943658975282,-0.0316939261509014,
0.0673589466646818));
#82259=CARTESIAN_POINT('',(0.0135151508928967,-0.0320197221621821,0.0721473186200811));
#82260=CARTESIAN_POINT('Ctrl Pts',(0.0135151328433497,-0.032019739209474,
0.072147134530176));
#82261=CARTESIAN_POINT('Ctrl Pts',(0.0135049415759329,-0.0319792716576038,
0.0721197016211392));
#82262=CARTESIAN_POINT('Ctrl Pts',(0.0134944947765313,-0.0319386439829729,
0.0720922215211813));
#82263=CARTESIAN_POINT('Ctrl Pts',(0.0134837735724475,-0.0318979099381661,
0.0720646683867518));
#82264=CARTESIAN_POINT('Ctrl Pts',(0.0134730525802759,-0.0318571766984961,
0.0720371157969292));
#82265=CARTESIAN_POINT('Ctrl Pts',(0.0134621133457679,-0.0318163871833608,
0.0720096295696911));
#82266=CARTESIAN_POINT('Ctrl Pts',(0.0134509967669547,-0.0317755399638303,
0.07198230294428));
#82267=CARTESIAN_POINT('',(0.0135140130126341,-0.0321934096636183,0.0721480230490248));
#82268=CARTESIAN_POINT('Origin',(0.0156707126887725,-0.032411291842895,
0.0713245685473849));
#82269=CARTESIAN_POINT('',(0.0134922523936017,-0.0321934096636663,0.0720894335835798));
#82270=CARTESIAN_POINT('Ctrl Pts',(0.0134696466733588,-0.0321934096636618,
0.0720326878890758));
#82271=CARTESIAN_POINT('Ctrl Pts',(0.0134404472892126,-0.0320835708272592,
0.07195896425157));
#82272=CARTESIAN_POINT('Ctrl Pts',(0.0134097391350493,-0.0319739230346488,
0.0718858876565074));
#82273=CARTESIAN_POINT('Ctrl Pts',(0.0133775686754118,-0.0318646057455572,
0.0718135485850041));
#82274=CARTESIAN_POINT('Ctrl Pts',(0.0135168633384403,-0.0321934096636618,
0.0719296745341005));
#82275=CARTESIAN_POINT('Ctrl Pts',(0.0134862433198451,-0.0320835708272592,
0.0718552997419847));
#82276=CARTESIAN_POINT('Ctrl Pts',(0.0134541018796477,-0.0319739230346488,
0.0717816017699644));
#82277=CARTESIAN_POINT('Ctrl Pts',(0.0134204873771956,-0.0318646057455572,
0.071708671753426));
#82278=CARTESIAN_POINT('Ctrl Pts',(0.0135640800035218,-0.0321934096636618,
0.0718266611791252));
#82279=CARTESIAN_POINT('Ctrl Pts',(0.0135320393504776,-0.0320835708272592,
0.0717516352323994));
#82280=CARTESIAN_POINT('Ctrl Pts',(0.013498464624246,-0.0319739230346488,
0.0716773158834214));
#82281=CARTESIAN_POINT('Ctrl Pts',(0.0134634060789795,-0.0318646057455572,
0.0716037949218479));
#82282=CARTESIAN_POINT('Ctrl Pts',(0.0136112966686033,-0.0321934096636618,
0.0717236478241499));
#82283=CARTESIAN_POINT('Ctrl Pts',(0.01357783538111,-0.0320835708272592,
0.0716479707228141));
#82284=CARTESIAN_POINT('Ctrl Pts',(0.0135428273688444,-0.0319739230346488,
0.0715730299968783));
#82285=CARTESIAN_POINT('Ctrl Pts',(0.0135063247807634,-0.0318646057455572,
0.0714989180902697));
#82286=CARTESIAN_POINT('',(0.0136061014165828,-0.032176398030847,0.0717119319308681));
#82287=CARTESIAN_POINT('',(0.0136112966685892,-0.0321934096636184,0.0717236478241218));
#82288=CARTESIAN_POINT('Origin',(-0.00175275152612349,-0.0326386231579772,
0.0778708058591182));
#82289=CARTESIAN_POINT('Ctrl Pts',(0.0136061014136762,-0.0321763980306286,
0.0717119319321528));
#82290=CARTESIAN_POINT('Ctrl Pts',(0.0135668855679636,-0.0321259596175053,
0.0717293717960751));
#82291=CARTESIAN_POINT('Ctrl Pts',(0.0135283491876663,-0.0320749164631853,
0.0717465094917317));
#82292=CARTESIAN_POINT('Ctrl Pts',(0.0134526043450023,-0.0319716057793979,
0.0717801943383765));
#82293=CARTESIAN_POINT('Ctrl Pts',(0.0134154253954175,-0.0319193786690191,
0.0717967283645963));
#82294=CARTESIAN_POINT('Ctrl Pts',(0.0133789127685737,-0.0318665617525381,
0.071812966067291));
#82295=CARTESIAN_POINT('',(0.0135408942215792,-0.0321934096636663,0.0718772459711283));
#82296=CARTESIAN_POINT('Origin',(0.00812378219310841,-0.0315241814719618,
0.07415));
#82297=CARTESIAN_POINT('',(0.0136061014169218,-0.0322104233323605,0.071711931930717));
#82298=CARTESIAN_POINT('',(0.0136008811544457,-0.0321934096636183,0.0717002271599731));
#82299=CARTESIAN_POINT('Origin',(-0.00174028061319681,-0.0326387240308083,
0.0779143900164998));
#82300=CARTESIAN_POINT('Origin',(-0.00125416538273813,-0.0326386238850291,
0.078991946492578));
#82301=CARTESIAN_POINT('Origin',(-0.00127817429069414,-0.0326387246683772,
0.0789534933216108));
#82302=CARTESIAN_POINT('Ctrl Pts',(0.0134423254954534,-0.0327445246967097,
0.0719611139497267));
#82303=CARTESIAN_POINT('Ctrl Pts',(0.0133597703084729,-0.032443687833936,
0.0717605218098416));
#82304=CARTESIAN_POINT('Ctrl Pts',(0.0132623402322532,-0.0321434074405927,
0.0715667179251309));
#82305=CARTESIAN_POINT('Ctrl Pts',(0.0133421768874091,-0.0327445246967097,
0.0717320500802344));
#82306=CARTESIAN_POINT('Ctrl Pts',(0.0132509824153575,-0.032443687833936,
0.0715352351068499));
#82307=CARTESIAN_POINT('Ctrl Pts',(0.0131452221089815,-0.0321434074405927,
0.0713458484043696));
#82308=CARTESIAN_POINT('',(0.0133268783657655,-0.0326943950436612,0.0716993031158297));
#82309=CARTESIAN_POINT('',(0.0132217993964906,-0.0323666188837389,0.0714876052895898));
#82310=CARTESIAN_POINT('Origin',(-0.00184898313512725,-0.0326395579109298,
0.0789312659146129));
#82311=CARTESIAN_POINT('Origin',(0.0230117647175438,-0.032193382560301,
0.0663748808834647));
#82312=CARTESIAN_POINT('',(0.013278459664916,-0.0321934096532689,0.0715990344654563));
#82313=CARTESIAN_POINT('',(0.0132495274267339,-0.0321934096584275,0.0715436343215988));
#82314=CARTESIAN_POINT('',(0.0133789127711315,-0.0325210109756239,0.0718129660661585));
#82315=CARTESIAN_POINT('Origin',(-0.00203062046382032,-0.0326393129156523,
0.0784860779647287));
#82316=CARTESIAN_POINT('',(0.0133776714505554,-0.0326943950436593,0.0718135180996885));
#82317=CARTESIAN_POINT('Origin',(0.0234856570143876,-0.0326943765538184,
0.0673183490763511));
#82318=CARTESIAN_POINT('',(0.0133522749081705,-0.0326943950436702,0.0717564106077691));
#82319=CARTESIAN_POINT('Ctrl Pts',(0.0136974526277365,-0.0325229783203769,
0.071928694553595));
#82320=CARTESIAN_POINT('Ctrl Pts',(0.0136668319807345,-0.032413025309245,
0.0718518616285417));
#82321=CARTESIAN_POINT('Ctrl Pts',(0.0136346265902,-0.032303122220807,0.0717756737841252));
#82322=CARTESIAN_POINT('Ctrl Pts',(0.0136008811526212,-0.0321934096576658,
0.0717002271558818));
#82323=CARTESIAN_POINT('Ctrl Pts',(0.0135908287267053,-0.0325229783203769,
0.0718903215687538));
#82324=CARTESIAN_POINT('Ctrl Pts',(0.0135596791089464,-0.032413025309245,
0.0718149584518445));
#82325=CARTESIAN_POINT('Ctrl Pts',(0.0135269752327534,-0.032303122220807,
0.0717402511350864));
#82326=CARTESIAN_POINT('Ctrl Pts',(0.0134927623662196,-0.0321934096576658,
0.0716662938350337));
#82327=CARTESIAN_POINT('Ctrl Pts',(0.0134842048256741,-0.0325229783203769,
0.0718519485839126));
#82328=CARTESIAN_POINT('Ctrl Pts',(0.0134525262371584,-0.032413025309245,
0.0717780552751473));
#82329=CARTESIAN_POINT('Ctrl Pts',(0.0134193238753068,-0.032303122220807,
0.0717048284860477));
#82330=CARTESIAN_POINT('Ctrl Pts',(0.013384643579818,-0.0321934096576658,
0.0716323605141857));
#82331=CARTESIAN_POINT('Ctrl Pts',(0.0133775809246429,-0.0325229783203769,
0.0718135755990713));
#82332=CARTESIAN_POINT('Ctrl Pts',(0.0133453733653703,-0.032413025309245,
0.0717411520984501));
#82333=CARTESIAN_POINT('Ctrl Pts',(0.0133116725178602,-0.032303122220807,
0.0716694058370089));
#82334=CARTESIAN_POINT('Ctrl Pts',(0.0132765247934164,-0.0321934096576658,
0.0715984271933376));
#82335=CARTESIAN_POINT('',(0.0134396704100311,-0.0321934096584275,0.0716496308130976));
#82336=CARTESIAN_POINT('Ctrl Pts',(0.0136061014137376,-0.0322104233328912,
0.0717119319321256));
#82337=CARTESIAN_POINT('Ctrl Pts',(0.0135668324299691,-0.0322609421830511,
0.0717293954273236));
#82338=CARTESIAN_POINT('Ctrl Pts',(0.0135282700908689,-0.032312088823898,
0.0717465446672346));
#82339=CARTESIAN_POINT('Ctrl Pts',(0.0134525246746201,-0.0324156524631812,
0.0717802297689611));
#82340=CARTESIAN_POINT('Ctrl Pts',(0.0134153727329965,-0.0324680267167319,
0.0717967517843503));
#82341=CARTESIAN_POINT('Ctrl Pts',(0.0133789127710902,-0.0325210109755913,
0.071812966066172));
#82342=CARTESIAN_POINT('Origin',(0.0104317671203413,-0.0262834582511411,
0.0816717412489181));
#82343=CARTESIAN_POINT('Origin',(0.0202695860884835,-0.0342770968612105,
0.0747014319232182));
#82344=CARTESIAN_POINT('Ctrl Pts',(0.0133261508800732,-0.0326943950436604,
0.0717011958533709));
#82345=CARTESIAN_POINT('Ctrl Pts',(0.0132924017693845,-0.0325844576448134,
0.0716294974625865));
#82346=CARTESIAN_POINT('Ctrl Pts',(0.0132571674299463,-0.0324744968375322,
0.071558491984537));
#82347=CARTESIAN_POINT('Ctrl Pts',(0.0132204942608865,-0.0323646534831894,
0.0714882697729062));
#82348=CARTESIAN_POINT('Ctrl Pts',(0.0133668060529127,-0.0326943950436604,
0.0715954211659316));
#82349=CARTESIAN_POINT('Ctrl Pts',(0.0133315991687882,-0.0325844576448134,
0.0715231624706695));
#82350=CARTESIAN_POINT('Ctrl Pts',(0.01329489536473,-0.0324744968375322,
0.0714516267976334));
#82351=CARTESIAN_POINT('Ctrl Pts',(0.0132567429319998,-0.0323646534831894,
0.071380905153855));
#82352=CARTESIAN_POINT('Ctrl Pts',(0.0134074612257521,-0.0326943950436604,
0.0714896464784924));
#82353=CARTESIAN_POINT('Ctrl Pts',(0.0133707965681918,-0.0325844576448134,
0.0714168274787526));
#82354=CARTESIAN_POINT('Ctrl Pts',(0.0133326232995138,-0.0324744968375322,
0.0713447616107299));
#82355=CARTESIAN_POINT('Ctrl Pts',(0.013292991603113,-0.0323646534831894,
0.0712735405348038));
#82356=CARTESIAN_POINT('Ctrl Pts',(0.0134481163985916,-0.0326943950436604,
0.0713838717910531));
#82357=CARTESIAN_POINT('Ctrl Pts',(0.0134099939675955,-0.0325844576448134,
0.0713104924868356));
#82358=CARTESIAN_POINT('Ctrl Pts',(0.0133703512342975,-0.0324744968375322,
0.0712378964238264));
#82359=CARTESIAN_POINT('Ctrl Pts',(0.0133292402742263,-0.0323646534831894,
0.0711661759157526));
#82360=CARTESIAN_POINT('',(0.0134421957513835,-0.0326773559991349,0.0713725052289173));
#82361=CARTESIAN_POINT('',(0.0134481163985908,-0.0326943950436594,0.0713838717910534));
#82362=CARTESIAN_POINT('Origin',(-0.0012533835582576,-0.0326395670550634,
0.0791038218523109));
#82363=CARTESIAN_POINT('Ctrl Pts',(0.0134421957484051,-0.0326773559987424,
0.0713725052304646));
#82364=CARTESIAN_POINT('Ctrl Pts',(0.0134041217295636,-0.0326267922586104,
0.0713923890524141));
#82365=CARTESIAN_POINT('Ctrl Pts',(0.0133667225452122,-0.0325756109579621,
0.071411920447978));
#82366=CARTESIAN_POINT('Ctrl Pts',(0.013293242016891,-0.0324719985462366,
0.0714502950085406));
#82367=CARTESIAN_POINT('Ctrl Pts',(0.0132571901439852,-0.0324196091621778,
0.071469122782535));
#82368=CARTESIAN_POINT('Ctrl Pts',(0.0132217993964473,-0.0323666188837757,
0.0714876052896124));
#82369=CARTESIAN_POINT('',(0.0133874973821882,-0.0326943950436703,0.0715415874534516));
#82370=CARTESIAN_POINT('Origin',(0.00812378219310841,-0.0315241814719618,
0.07415));
#82371=CARTESIAN_POINT('',(0.0134421957513442,-0.0327114338380046,0.0713725052289375));
#82372=CARTESIAN_POINT('',(0.0134362508414151,-0.0326943950436593,0.0713611513377796));
#82373=CARTESIAN_POINT('Origin',(-0.00123172383876959,-0.0326395677682108,
0.0791436191567031));
#82374=CARTESIAN_POINT('Origin',(-0.00129989860108158,-0.0326395675544282,
0.0790147558839406));
#82375=CARTESIAN_POINT('Origin',(-0.00132017994648858,-0.0326395682222787,
0.0789742386681461));
#82376=CARTESIAN_POINT('Ctrl Pts',(0.013294372096676,-0.0332451089994434,
0.071631443856269));
#82377=CARTESIAN_POINT('Ctrl Pts',(0.0131993831976154,-0.0329451141710254,
0.0714364318674927));
#82378=CARTESIAN_POINT('Ctrl Pts',(0.0130899750517819,-0.0326442513127494,
0.0712491288393898));
#82379=CARTESIAN_POINT('Ctrl Pts',(0.0131800365534401,-0.0332451089994434,
0.0714091211548799));
#82380=CARTESIAN_POINT('Ctrl Pts',(0.0130766626165102,-0.0329451141710254,
0.0712184214016686));
#82381=CARTESIAN_POINT('Ctrl Pts',(0.0129592180690264,-0.0326442513127494,
0.0710360499538552));
#82382=CARTESIAN_POINT('Ctrl Pts',(0.0131788931980078,-0.0332451089994434,
0.0714068979278661));
#82383=CARTESIAN_POINT('Ctrl Pts',(0.0130754354106992,-0.0329451141710254,
0.0712162412970104));
#82384=CARTESIAN_POINT('Ctrl Pts',(0.0129579104991988,-0.0326442513127494,
0.0710339191649999));
#82385=CARTESIAN_POINT('',(0.0131627307134367,-0.0331951640388616,0.0713774338944794));
#82386=CARTESIAN_POINT('',(0.0130445664749898,-0.0328677532355023,0.0711727517535438));
#82387=CARTESIAN_POINT('Origin',(-0.00113911576405468,-0.0326402808282269,
0.0801232577444776));
#82388=CARTESIAN_POINT('Origin',(0.022503705724796,-0.0326944278779141,
0.0654491979966907));
#82389=CARTESIAN_POINT('',(0.0131081116321623,-0.0326943950436593,0.0712804033309572));
#82390=CARTESIAN_POINT('',(0.0130757578824758,-0.0326943950436694,0.0712269291794491));
#82391=CARTESIAN_POINT('',(0.0132217993964919,-0.0330220786163545,0.0714876052895923));
#82392=CARTESIAN_POINT('Origin',(-0.00141434687361303,-0.0326396682762052,
0.079729049067357));
#82393=CARTESIAN_POINT('',(0.0132205951878513,-0.0331951640388588,0.0714882341769756));
#82394=CARTESIAN_POINT('Origin',(0.0229990778064989,-0.0331952026560082,
0.0663815084928096));
#82395=CARTESIAN_POINT('',(0.013191662950654,-0.0331951640388702,0.0714328340357375));
#82396=CARTESIAN_POINT('Ctrl Pts',(0.01354697692822,-0.0330240426238172,
0.0715831032616936));
#82397=CARTESIAN_POINT('Ctrl Pts',(0.0135116154248435,-0.032914277406352,
0.0715083934706549));
#82398=CARTESIAN_POINT('Ctrl Pts',(0.0134746918323956,-0.0328043479726691,
0.0714343774551129));
#82399=CARTESIAN_POINT('Ctrl Pts',(0.0134362508414215,-0.0326943950436593,
0.0713611513377811));
#82400=CARTESIAN_POINT('Ctrl Pts',(0.0134381539868773,-0.0330240426238172,
0.0715515009924333));
#82401=CARTESIAN_POINT('Ctrl Pts',(0.0134023571314531,-0.032914277406352,
0.0714782903434326));
#82402=CARTESIAN_POINT('Ctrl Pts',(0.0133650289613723,-0.0328043479726691,
0.0714057832172486));
#82403=CARTESIAN_POINT('Ctrl Pts',(0.0133262147387084,-0.0326943950436593,
0.0713340738178687));
#82404=CARTESIAN_POINT('Ctrl Pts',(0.0133293310455345,-0.0330240426238172,
0.071519898723173));
#82405=CARTESIAN_POINT('Ctrl Pts',(0.0132930988380627,-0.032914277406352,
0.0714481872162104));
#82406=CARTESIAN_POINT('Ctrl Pts',(0.0132553660903489,-0.0328043479726691,
0.0713771889793842));
#82407=CARTESIAN_POINT('Ctrl Pts',(0.0132161786359954,-0.0326943950436593,
0.0713069962979563));
#82408=CARTESIAN_POINT('Ctrl Pts',(0.0132205081041918,-0.0330240426238172,
0.0714882964539127));
#82409=CARTESIAN_POINT('Ctrl Pts',(0.0131838405446724,-0.032914277406352,
0.0714180840889881));
#82410=CARTESIAN_POINT('Ctrl Pts',(0.0131457032193256,-0.0328043479726691,
0.0713485947415199));
#82411=CARTESIAN_POINT('Ctrl Pts',(0.0131061425332823,-0.0326943950436593,
0.0712799187780439));
#82412=CARTESIAN_POINT('',(0.0132721812367987,-0.0326943950436693,0.0713207773343784));
#82413=CARTESIAN_POINT('Ctrl Pts',(0.0134421957483998,-0.032711433838331,
0.0713725052304673));
#82414=CARTESIAN_POINT('Ctrl Pts',(0.0134041280627768,-0.032761987682735,
0.0713923857449491));
#82415=CARTESIAN_POINT('Ctrl Pts',(0.0133667319719703,-0.0328131562596795,
0.0714119155249218));
#82416=CARTESIAN_POINT('Ctrl Pts',(0.0132932515104146,-0.0329167375861618,
0.0714502900506167));
#82417=CARTESIAN_POINT('Ctrl Pts',(0.0132571964188637,-0.0329691088926659,
0.0714691195055349));
#82418=CARTESIAN_POINT('Ctrl Pts',(0.0132217993964484,-0.0330220786163186,
0.0714876052896119));
#82419=CARTESIAN_POINT('Ctrl Pts',(0.0131621234123062,-0.0331951640388604,
0.0713793688852099));
#82420=CARTESIAN_POINT('Ctrl Pts',(0.0131048423903713,-0.033030642201062,
0.0712752044107868));
#82421=CARTESIAN_POINT('Ctrl Pts',(0.0130433050873985,-0.0328657861914645,
0.071173496429052));
#82422=CARTESIAN_POINT('Ctrl Pts',(0.0131627307134382,-0.0331951640388604,
0.0713774338944822));
#82423=CARTESIAN_POINT('Ctrl Pts',(0.0131054096868106,-0.033030642201062,
0.0712732568644976));
#82424=CARTESIAN_POINT('Ctrl Pts',(0.0130438318943943,-0.0328657861914645,
0.0711715379913659));
#82425=CARTESIAN_POINT('Ctrl Pts',(0.0132639234139576,-0.0331951640388604,
0.07105501240225));
#82426=CARTESIAN_POINT('Ctrl Pts',(0.0131999365296955,-0.033030642201062,
0.0709487432780609));
#82427=CARTESIAN_POINT('Ctrl Pts',(0.0131316121071198,-0.0328657861914645,
0.0708452096053105));
#82428=CARTESIAN_POINT('',(0.0132573007388876,-0.033178164828193,0.071044040029871));
#82429=CARTESIAN_POINT('',(0.0132639234139403,-0.0331951640388588,0.071055012402302));
#82430=CARTESIAN_POINT('Origin',(-0.000497103510496023,-0.0326412092060213,
0.0801984292855081));
#82431=CARTESIAN_POINT('Ctrl Pts',(0.01325730073875,-0.033178164828644,
0.0710440400317029));
#82432=CARTESIAN_POINT('Ctrl Pts',(0.0132205250709329,-0.033127681154677,
0.0710662906233262));
#82433=CARTESIAN_POINT('Ctrl Pts',(0.0131844134752943,-0.0330765663497778,
0.0710881394671044));
#82434=CARTESIAN_POINT('Ctrl Pts',(0.0131134873182336,-0.0329730614463164,
0.0711310522922301));
#82435=CARTESIAN_POINT('Ctrl Pts',(0.0130787014066564,-0.0329207133373767,
0.0711520989331467));
#82436=CARTESIAN_POINT('Ctrl Pts',(0.0130445664896799,-0.0328677532289379,
0.0711727517609904));
#82437=CARTESIAN_POINT('',(0.0132133270636985,-0.0331951640388702,0.0712162231484007));
#82438=CARTESIAN_POINT('Origin',(0.00812378219310841,-0.0315241814719618,
0.07415));
#82439=CARTESIAN_POINT('',(0.013257300737225,-0.0332121607144415,0.0710440400301211));
#82440=CARTESIAN_POINT('',(0.0132506546416663,-0.0331951640388587,0.0710330818271522));
#82441=CARTESIAN_POINT('Origin',(-0.000467273682971033,-0.0326413661553068,
0.0802325807301716));
#82442=CARTESIAN_POINT('Origin',(-0.00123452790923341,-0.0326412096447147,
0.0789796196542873));
#82443=CARTESIAN_POINT('Origin',(-0.00125093443179604,-0.0326413665784978,
0.0789373466122632));
#82444=CARTESIAN_POINT('Ctrl Pts',(0.0131260379500619,-0.0337436976235975,
0.0713117677434667));
#82445=CARTESIAN_POINT('Ctrl Pts',(0.0131005104590007,-0.0336723290703325,
0.0712667766970761));
#82446=CARTESIAN_POINT('Ctrl Pts',(0.0130741778505704,-0.033601104548885,
0.0712222520882799));
#82447=CARTESIAN_POINT('Ctrl Pts',(0.0129901030480482,-0.0333736987606857,
0.0710800938322218));
#82448=CARTESIAN_POINT('Ctrl Pts',(0.0128980089337392,-0.0331450831799192,
0.070942994538663));
#82449=CARTESIAN_POINT('Ctrl Pts',(0.0129979690416467,-0.0337436976235975,
0.0710970624694343));
#82450=CARTESIAN_POINT('Ctrl Pts',(0.0129705104588115,-0.0336723290703325,
0.0710532232942153));
#82451=CARTESIAN_POINT('Ctrl Pts',(0.0129422677895439,-0.033601104548885,
0.0710098851044995));
#82452=CARTESIAN_POINT('Ctrl Pts',(0.0128520945411301,-0.0333736987606857,
0.0708715148495486));
#82453=CARTESIAN_POINT('Ctrl Pts',(0.012754129408031,-0.0331450831799192,
0.0707385472787596));
#82454=CARTESIAN_POINT('Ctrl Pts',(0.0129966883525625,-0.0337436976235975,
0.0710949154166939));
#82455=CARTESIAN_POINT('Ctrl Pts',(0.0129692104588095,-0.0336723290703325,
0.0710510877601868));
#82456=CARTESIAN_POINT('Ctrl Pts',(0.0129409486889336,-0.033601104548885,
0.0710077614346617));
#82457=CARTESIAN_POINT('Ctrl Pts',(0.0128507144560609,-0.0333736987606857,
0.0708694290597219));
#82458=CARTESIAN_POINT('Ctrl Pts',(0.012752690612774,-0.0331450831799192,
0.0707365028061606));
#82459=CARTESIAN_POINT('',(0.0129786966333677,-0.0336938721132548,0.0710665067248715));
#82460=CARTESIAN_POINT('',(0.0128479134659113,-0.0333679869945434,0.070869648080258));
#82461=CARTESIAN_POINT('Ctrl Pts',(0.0129786966333755,-0.0336938721132648,
0.0710665067248828));
#82462=CARTESIAN_POINT('Ctrl Pts',(0.0129666603126299,-0.0336629187933932,
0.0710475557163417));
#82463=CARTESIAN_POINT('Ctrl Pts',(0.0129545168756118,-0.033631995230104,
0.0710286812462819));
#82464=CARTESIAN_POINT('Ctrl Pts',(0.0129422677895513,-0.033601104548895,
0.0710098851045111));
#82465=CARTESIAN_POINT('Ctrl Pts',(0.0129115306412241,-0.0335235892595454,
0.0709627191531304));
#82466=CARTESIAN_POINT('Ctrl Pts',(0.0128800735002384,-0.0334458668660369,
0.0709159626913196));
#82467=CARTESIAN_POINT('Ctrl Pts',(0.012847913466173,-0.0333679869945385,
0.0708696480800845));
#82468=CARTESIAN_POINT('Ctrl Pts',(0.0128478886666482,-0.0333679692459107,
0.0708696111605181));
#82469=CARTESIAN_POINT('Ctrl Pts',(0.01284751978041,-0.0333391895371493,
0.0708698745248455));
#82470=CARTESIAN_POINT('Ctrl Pts',(0.0128472451689676,-0.0333104081054902,
0.0708700745720281));
#82471=CARTESIAN_POINT('Ctrl Pts',(0.0128468849339141,-0.0332532696730203,
0.0708703438459546));
#82472=CARTESIAN_POINT('Ctrl Pts',(0.0128467965568541,-0.0332249163812529,
0.0708704149850103));
#82473=CARTESIAN_POINT('Ctrl Pts',(0.0128467974744775,-0.0331960985669457,
0.0708704227415418));
#82474=CARTESIAN_POINT('Ctrl Pts',(0.0128467975140083,-0.0331956312253307,
0.070870422850649));
#82475=CARTESIAN_POINT('Ctrl Pts',(0.0128467975774544,-0.0331951640388588,
0.0708704229420197));
#82476=CARTESIAN_POINT('',(0.0129180927308873,-0.0331951640388587,0.0709730971895031));
#82477=CARTESIAN_POINT('',(0.0128824451541801,-0.0331951640388687,0.0709217600657703));
#82478=CARTESIAN_POINT('',(0.0130445664767656,-0.033521636656769,0.071172751768968));
#82479=CARTESIAN_POINT('Origin',(-0.000540169405658373,-0.0326434571528753,
0.0808073568996008));
#82480=CARTESIAN_POINT('',(0.0130434041327693,-0.0336938721132327,0.0711734550279212));
#82481=CARTESIAN_POINT('Origin',(0.0223868954136058,-0.0336938867896333,
0.0655203142496365));
#82482=CARTESIAN_POINT('',(0.0130110503830785,-0.0336938721132538,0.0711199808764064));
#82483=CARTESIAN_POINT('Ctrl Pts',(0.0133750982475513,-0.0335235895815173,
0.0712476423899846));
#82484=CARTESIAN_POINT('Ctrl Pts',(0.0133351415808332,-0.0334144449262749,
0.0711753476856053));
#82485=CARTESIAN_POINT('Ctrl Pts',(0.0132936454545612,-0.0333049234473147,
0.071103795398033));
#82486=CARTESIAN_POINT('Ctrl Pts',(0.0132506546416721,-0.0331951640388587,
0.0710330818271533));
#82487=CARTESIAN_POINT('Ctrl Pts',(0.0132645055593811,-0.0335235895815173,
0.0712229355122069));
#82488=CARTESIAN_POINT('Ctrl Pts',(0.0132242087538469,-0.0334144449262749,
0.0711521633339172));
#82489=CARTESIAN_POINT('Ctrl Pts',(0.0131824035522238,-0.0333049234473147,
0.0710821423486446));
#82490=CARTESIAN_POINT('Ctrl Pts',(0.0131391353000311,-0.0331951640388587,
0.0710129669340089));
#82491=CARTESIAN_POINT('Ctrl Pts',(0.0131539128712108,-0.0335235895815172,
0.0711982286344292));
#82492=CARTESIAN_POINT('Ctrl Pts',(0.0131132759268607,-0.0334144449262749,
0.0711289789822291));
#82493=CARTESIAN_POINT('Ctrl Pts',(0.0130711616498865,-0.0333049234473147,
0.0710604892992561));
#82494=CARTESIAN_POINT('Ctrl Pts',(0.0130276159583901,-0.0331951640388587,
0.0709928520408646));
#82495=CARTESIAN_POINT('Ctrl Pts',(0.0130433201830405,-0.0335235895815172,
0.0711735217566515));
#82496=CARTESIAN_POINT('Ctrl Pts',(0.0130023430998744,-0.0334144449262749,
0.071105794630541));
#82497=CARTESIAN_POINT('Ctrl Pts',(0.0129599197475492,-0.0333049234473147,
0.0710388362498676));
#82498=CARTESIAN_POINT('Ctrl Pts',(0.0129160966167491,-0.0331951640388587,
0.0709727371477202));
#82499=CARTESIAN_POINT('',(0.0130843736862868,-0.0331951640388687,0.0710030895083376));
#82500=CARTESIAN_POINT('Ctrl Pts',(0.0132573007345394,-0.0332121607145969,
0.071044040031738));
#82501=CARTESIAN_POINT('Ctrl Pts',(0.0132205869265907,-0.0332625444109045,
0.0710662531818125));
#82502=CARTESIAN_POINT('Ctrl Pts',(0.0131845057551647,-0.0333135300745367,
0.0710880835644541));
#82503=CARTESIAN_POINT('Ctrl Pts',(0.0131135800443987,-0.0334167203140589,
0.0711309961236631));
#82504=CARTESIAN_POINT('Ctrl Pts',(0.0130787629753201,-0.0334688847587269,
0.0711520616797525));
#82505=CARTESIAN_POINT('Ctrl Pts',(0.0130445664760702,-0.0335216366562331,
0.0711727517691849));
#82506=CARTESIAN_POINT('Ctrl Pts',(0.0129784577173806,-0.0336938721132391,
0.0710674776182864));
#82507=CARTESIAN_POINT('Ctrl Pts',(0.012960414690991,-0.0336474569764958,
0.0710390615914907));
#82508=CARTESIAN_POINT('Ctrl Pts',(0.0129420402554495,-0.033601104548885,
0.0710108587281842));
#82509=CARTESIAN_POINT('Ctrl Pts',(0.0128955204092062,-0.0334837508592656,
0.0709394555625372));
#82510=CARTESIAN_POINT('Ctrl Pts',(0.0128469051672095,-0.0333660264659097,
0.070869462231394));
#82511=CARTESIAN_POINT('Ctrl Pts',(0.0129786966333786,-0.033693872113239,
0.0710665067248888));
#82512=CARTESIAN_POINT('Ctrl Pts',(0.0129606479240279,-0.0336474569764958,
0.0710380892996385));
#82513=CARTESIAN_POINT('Ctrl Pts',(0.0129422677895439,-0.033601104548885,
0.0710098851044995));
#82514=CARTESIAN_POINT('Ctrl Pts',(0.0128957335148884,-0.0334837508592656,
0.0709384785669586));
#82515=CARTESIAN_POINT('Ctrl Pts',(0.0128471037508992,-0.0333660264659097,
0.070868482292946));
#82516=CARTESIAN_POINT('Ctrl Pts',(0.0130599291282446,-0.033693872113239,
0.070736398680371));
#82517=CARTESIAN_POINT('Ctrl Pts',(0.0130399481869677,-0.0336474569764958,
0.0707075057743724));
#82518=CARTESIAN_POINT('Ctrl Pts',(0.013019630386853,-0.033601104548885,
0.0706788487502797));
#82519=CARTESIAN_POINT('Ctrl Pts',(0.0129681903883177,-0.0334837508592656,
0.0706062957539401));
#82520=CARTESIAN_POINT('Ctrl Pts',(0.0129146230827298,-0.0333660264659097,
0.0705352988913386));
#82521=CARTESIAN_POINT('',(0.0130521460724243,-0.0336769361243753,0.0707278326351485));
#82522=CARTESIAN_POINT('',(0.0130594446401983,-0.0336938721132327,0.0707383675156333));
#82523=CARTESIAN_POINT('Ctrl Pts',(0.0130521460724241,-0.033676936124375,
0.0707278326351483));
#82524=CARTESIAN_POINT('Ctrl Pts',(0.0130533644668488,-0.0336797586670023,
0.0707295872807962));
#82525=CARTESIAN_POINT('Ctrl Pts',(0.0130545818781333,-0.0336825812712842,
0.0707313425107595));
#82526=CARTESIAN_POINT('Ctrl Pts',(0.0130570147345841,-0.0336882266024761,
0.0707348541386481));
#82527=CARTESIAN_POINT('Ctrl Pts',(0.0130582301797444,-0.0336910493293757,
0.0707366105365684));
#82528=CARTESIAN_POINT('Ctrl Pts',(0.013059444640198,-0.0336938721132324,
0.0707383675156339));
#82529=CARTESIAN_POINT('Ctrl Pts',(0.0130521460724243,-0.0336769361243753,
0.0707278326351486));
#82530=CARTESIAN_POINT('Ctrl Pts',(0.0130177183665245,-0.033627900751621,
0.070751738615807));
#82531=CARTESIAN_POINT('Ctrl Pts',(0.0129828004637717,-0.0335767878632059,
0.070775984980357));
#82532=CARTESIAN_POINT('Ctrl Pts',(0.012914371179375,-0.0334733198857308,
0.0708235010464587));
#82533=CARTESIAN_POINT('Ctrl Pts',(0.0128808190586996,-0.0334209645014064,
0.0708467990364622));
#82534=CARTESIAN_POINT('Ctrl Pts',(0.0128479134700578,-0.0333679869844681,
0.0708696480862338));
#82535=CARTESIAN_POINT('',(0.013019070636793,-0.0336938721132538,0.0709024371202624));
#82536=CARTESIAN_POINT('Origin',(0.00812378219310841,-0.0315241814719618,
0.07415));
#82537=CARTESIAN_POINT('',(0.0130521460713649,-0.0337108120655546,0.0707278326358923));
#82538=CARTESIAN_POINT('',(0.0130448250186083,-0.0336938721132327,0.0707173133685686));
#82539=CARTESIAN_POINT('Origin',(-0.00102429383614181,-0.0345562523061984,
0.0791416383900627));
#82540=CARTESIAN_POINT('Ctrl Pts',(0.0130448250186194,-0.0336938721132369,
0.0707173133685675));
#82541=CARTESIAN_POINT('Ctrl Pts',(0.0130460469851738,-0.0336910493032244,
0.0707190651596254));
#82542=CARTESIAN_POINT('Ctrl Pts',(0.0130472680461666,-0.0336882265893999,
0.0707208176459574));
#82543=CARTESIAN_POINT('Ctrl Pts',(0.0130497083925903,-0.0336825812712979,
0.0707243240608837));
#82544=CARTESIAN_POINT('Ctrl Pts',(0.0130509276779969,-0.0336797586670092,
0.0707260779894966));
#82545=CARTESIAN_POINT('Ctrl Pts',(0.0130521460724245,-0.033676936124375,
0.0707278326351488));
#82546=CARTESIAN_POINT('Origin',(0.000250585409215087,-0.0345562519856471,
0.0809776272350968));
#82547=CARTESIAN_POINT('Ctrl Pts',(0.0129379813152136,-0.034243627687391,
0.0710033173320588));
#82548=CARTESIAN_POINT('Ctrl Pts',(0.0128193022219425,-0.033943005420181,
0.0708217468189407));
#82549=CARTESIAN_POINT('Ctrl Pts',(0.0126872836485237,-0.0336441434784053,
0.0706496315241931));
#82550=CARTESIAN_POINT('Ctrl Pts',(0.0127966855175306,-0.034243627687391,
0.0707970759745255));
#82551=CARTESIAN_POINT('Ctrl Pts',(0.0126702279032296,-0.033943005420181,
0.0706208345202676));
#82552=CARTESIAN_POINT('Ctrl Pts',(0.0125308543132922,-0.0336441434784053,
0.0704546190551583));
#82553=CARTESIAN_POINT('',(0.0127755024240185,-0.0341934961088741,0.0707677486945316));
#82554=CARTESIAN_POINT('',(0.012632616474384,-0.0338664212865005,0.0705794904525109));
#82555=CARTESIAN_POINT('Origin',(-0.00105306743210708,-0.0345610720407014,
0.080192386592122));
#82556=CARTESIAN_POINT('Origin',(0.0212296958108869,-0.033693800507293,
0.0637714840387905));
#82557=CARTESIAN_POINT('',(0.0127091528762319,-0.0336938721132327,0.0706783288320532));
#82558=CARTESIAN_POINT('',(0.0126703521572034,-0.0336938721132427,0.0706293313402693));
#82559=CARTESIAN_POINT('',(0.0128479134700608,-0.0340203938281606,0.0708696480862382));
#82560=CARTESIAN_POINT('Origin',(-0.00125952035885906,-0.0345589643248295,
0.0797577442985207));
#82561=CARTESIAN_POINT('',(0.0128467975774529,-0.034193496108874,0.0708704229420174));
#82562=CARTESIAN_POINT('Origin',(0.0218981057441369,-0.0341934220717705,
0.0645853582045632));
#82563=CARTESIAN_POINT('',(0.0128111500007457,-0.034193496108884,0.0708190858182845));
#82564=CARTESIAN_POINT('Ctrl Pts',(0.0131824969040118,-0.0340223579322397,
0.0709236389734332));
#82565=CARTESIAN_POINT('Ctrl Pts',(0.0131379969707527,-0.0339125849573575,
0.070853866103888));
#82566=CARTESIAN_POINT('Ctrl Pts',(0.0130920841708115,-0.0338030433565231,
0.0707850633081453));
#82567=CARTESIAN_POINT('Ctrl Pts',(0.0130448250186137,-0.0336938721132327,
0.0707173133685692));
#82568=CARTESIAN_POINT('Ctrl Pts',(0.0130705710636286,-0.0340223579322397,
0.0709059249652735));
#82569=CARTESIAN_POINT('Ctrl Pts',(0.0130258268079969,-0.0339125849573575,
0.070837695844982));
#82570=CARTESIAN_POINT('Ctrl Pts',(0.012979701809388,-0.0338030433565231,
0.0707704407706237));
#82571=CARTESIAN_POINT('Ctrl Pts',(0.0129322626781393,-0.0336938721132327,
0.0707042405212325));
#82572=CARTESIAN_POINT('Ctrl Pts',(0.0129586452232454,-0.0340223579322397,
0.0708882109571139));
#82573=CARTESIAN_POINT('Ctrl Pts',(0.0129136566452411,-0.0339125849573575,
0.0708215255860761));
#82574=CARTESIAN_POINT('Ctrl Pts',(0.0128673194479645,-0.0338030433565231,
0.0707558182331021));
#82575=CARTESIAN_POINT('Ctrl Pts',(0.0128197003376649,-0.0336938721132327,
0.0706911676738957));
#82576=CARTESIAN_POINT('Ctrl Pts',(0.0128467193828622,-0.0340223579322397,
0.0708704969489542));
#82577=CARTESIAN_POINT('Ctrl Pts',(0.0128014864824853,-0.0339125849573575,
0.0708053553271701));
#82578=CARTESIAN_POINT('Ctrl Pts',(0.012754937086541,-0.0338030433565231,
0.0707411956955805));
#82579=CARTESIAN_POINT('Ctrl Pts',(0.0127071379971904,-0.0336938721132327,
0.0706780948265589));
#82580=CARTESIAN_POINT('',(0.0128769889474301,-0.0336938721132427,0.0706978211003209));
#82581=CARTESIAN_POINT('Ctrl Pts',(0.0130521460683998,-0.0337108120662685,
0.0707278326379432));
#82582=CARTESIAN_POINT('Ctrl Pts',(0.0130168267382924,-0.0337611408993663,
0.070752357746438));
#82583=CARTESIAN_POINT('Ctrl Pts',(0.0129821519075985,-0.0338121088780013,
0.0707764353261151));
#82584=CARTESIAN_POINT('Ctrl Pts',(0.012914059656656,-0.0339153382773242,
0.0708237173622393));
#82585=CARTESIAN_POINT('Ctrl Pts',(0.0128806710437265,-0.0339675558473114,
0.0708469018154012));
#82586=CARTESIAN_POINT('Ctrl Pts',(0.012847913470025,-0.0340203938281305,
0.0708696480862567));
#82587=CARTESIAN_POINT('Ctrl Pts',(0.0127751424137356,-0.0341934961088741,
0.0707697446340297));
#82588=CARTESIAN_POINT('Ctrl Pts',(0.0127285306936894,-0.0340836138575045,
0.0707056051306595));
#82589=CARTESIAN_POINT('Ctrl Pts',(0.0126806141063763,-0.0339738896631393,
0.070642460934376));
#82590=CARTESIAN_POINT('Ctrl Pts',(0.012631459396656,-0.0338644633275951,
0.0705803887508831));
#82591=CARTESIAN_POINT('Ctrl Pts',(0.0127952572963795,-0.0341934961088741,
0.0706582253506043));
#82592=CARTESIAN_POINT('Ctrl Pts',(0.0127471077914455,-0.0340836138575045,
0.0705938084749125));
#82593=CARTESIAN_POINT('Ctrl Pts',(0.0126976484174645,-0.0339738896631393,
0.0705304188606276));
#82594=CARTESIAN_POINT('Ctrl Pts',(0.0126469479149285,-0.0338644633275951,
0.0704681333951926));
#82595=CARTESIAN_POINT('Ctrl Pts',(0.0128153721790234,-0.0341934961088741,
0.070546706067179));
#82596=CARTESIAN_POINT('Ctrl Pts',(0.0127656848892016,-0.0340836138575045,
0.0704820118191656));
#82597=CARTESIAN_POINT('Ctrl Pts',(0.0127146827285526,-0.0339738896631393,
0.0704183767868792));
#82598=CARTESIAN_POINT('Ctrl Pts',(0.012662436433201,-0.0338644633275951,
0.0703558780395021));
#82599=CARTESIAN_POINT('Ctrl Pts',(0.0128354870616673,-0.0341934961088741,
0.0704351867837537));
#82600=CARTESIAN_POINT('Ctrl Pts',(0.0127842619869577,-0.0340836138575045,
0.0703702151634186));
#82601=CARTESIAN_POINT('Ctrl Pts',(0.0127317170396408,-0.0339738896631393,
0.0703063347131308));
#82602=CARTESIAN_POINT('Ctrl Pts',(0.0126779249514735,-0.0338644633275951,
0.0702436226838116));
#82603=CARTESIAN_POINT('',(0.012827541403907,-0.0341764758832422,0.0704251309734487));
#82604=CARTESIAN_POINT('',(0.0128354870616674,-0.034193496108874,0.0704351867837538));
#82605=CARTESIAN_POINT('Origin',(-0.000470986983591591,-0.0345621026585572,
0.0803029075861101));
#82606=CARTESIAN_POINT('Ctrl Pts',(0.0128275414013896,-0.0341764758830167,
0.0704251309754324));
#82607=CARTESIAN_POINT('Ctrl Pts',(0.0127938903004274,-0.0341260048543041,
0.0704517790111985));
#82608=CARTESIAN_POINT('Ctrl Pts',(0.0127608244346899,-0.0340749271282664,
0.0704779636039045));
#82609=CARTESIAN_POINT('Ctrl Pts',(0.0126958363144475,-0.033971543441391,
0.0705294271727942));
#82610=CARTESIAN_POINT('Ctrl Pts',(0.0126639394902065,-0.0339192781018031,
0.0705546860109566));
#82611=CARTESIAN_POINT('Ctrl Pts',(0.0126326164764418,-0.0338664212856164,
0.0705794904532255));
#82612=CARTESIAN_POINT('',(0.0128054947428529,-0.0341934961088841,0.0706014677391527));
#82613=CARTESIAN_POINT('Origin',(0.00812378219310841,-0.0315241814719618,
0.07415));
#82614=CARTESIAN_POINT('',(0.0128275414041477,-0.0342105180190543,0.0704251309732576));
#82615=CARTESIAN_POINT('',(0.0128195742877287,-0.0341934961088739,0.070415092155874));
#82616=CARTESIAN_POINT('Origin',(-0.000447137499422179,-0.0345621714823014,
0.0803414515509757));
#82617=CARTESIAN_POINT('Origin',(0.000164846308348061,-0.0345621031779462,
0.0811058389789641));
#82618=CARTESIAN_POINT('Origin',(0.000132796574955342,-0.0345621721125304,
0.0810737889136887));
#82619=CARTESIAN_POINT('Ctrl Pts',(0.0127100840996449,-0.0346945769586966,
0.0706795047796305));
#82620=CARTESIAN_POINT('Ctrl Pts',(0.0126373931877438,-0.0345275153362944,
0.070583442849943));
#82621=CARTESIAN_POINT('Ctrl Pts',(0.0125616624149798,-0.0343603235965186,
0.0704896421359921));
#82622=CARTESIAN_POINT('Ctrl Pts',(0.0124831198825586,-0.034193496108874,
0.0703983767297546));
#82623=CARTESIAN_POINT('Ctrl Pts',(0.0126580393994472,-0.0346945769586966,
0.070613782807614));
#82624=CARTESIAN_POINT('Ctrl Pts',(0.0125839719145285,-0.0345275153362944,
0.0705188109750097));
#82625=CARTESIAN_POINT('Ctrl Pts',(0.0125068984952447,-0.0343603235965186,
0.0704261439320513));
#82626=CARTESIAN_POINT('Ctrl Pts',(0.0124270511639208,-0.034193496108874,
0.0703360523588014));
#82627=CARTESIAN_POINT('Ctrl Pts',(0.0126059946992497,-0.0346945769586966,
0.0705480608355949));
#82628=CARTESIAN_POINT('Ctrl Pts',(0.0125305506413133,-0.0345275153362944,
0.070454179100074));
#82629=CARTESIAN_POINT('Ctrl Pts',(0.0124521345755095,-0.0343603235965186,
0.0703626457281086));
#82630=CARTESIAN_POINT('Ctrl Pts',(0.012370982445283,-0.034193496108874,
0.0702737279878472));
#82631=CARTESIAN_POINT('Ctrl Pts',(0.0125539499990518,-0.0346945769586966,
0.070482338863581));
#82632=CARTESIAN_POINT('Ctrl Pts',(0.0124771293680981,-0.0345275153362944,
0.0703895472251431));
#82633=CARTESIAN_POINT('Ctrl Pts',(0.0123973706557744,-0.0343603235965186,
0.0702991475241697));
#82634=CARTESIAN_POINT('Ctrl Pts',(0.0123149137266452,-0.034193496108874,
0.0702114036168948));
#82635=CARTESIAN_POINT('',(0.0125539500000745,-0.0346945769586966,0.0704823388648728));
#82636=CARTESIAN_POINT('',(0.0123995251710299,-0.0343667727836525,0.0703034239916618));
#82637=CARTESIAN_POINT('Origin',(-0.000279821455984584,-0.0345626474180612,
0.0813447306597584));
#82638=CARTESIAN_POINT('Origin',(0.0206160592004556,-0.0341934771024245,
0.0629115888748403));
#82639=CARTESIAN_POINT('',(0.0124821166583467,-0.034193496108874,0.0703972615746475));
#82640=CARTESIAN_POINT('',(0.0124403159257087,-0.034193496108884,0.0703507970855277));
#82641=CARTESIAN_POINT('',(0.0126326164752049,-0.0345211942962658,0.0705794904542206));
#82642=CARTESIAN_POINT('Origin',(-0.000575707125566571,-0.0345625596120814,
0.0809657317445962));
#82643=CARTESIAN_POINT('',(0.012631551438155,-0.0346945769586885,0.0705803338484653));
#82644=CARTESIAN_POINT('Origin',(0.021304944390607,-0.0346945685853822,
0.0637119446714151));
#82645=CARTESIAN_POINT('',(0.0125927507191247,-0.0346945769587026,0.0705313363566791));
#82646=CARTESIAN_POINT('Ctrl Pts',(0.0129699292337307,-0.0345231616327842,
0.0706123653579376));
#82647=CARTESIAN_POINT('Ctrl Pts',(0.012921167920781,-0.0344132092796988,
0.0705455680438119));
#82648=CARTESIAN_POINT('Ctrl Pts',(0.0128710274739373,-0.034303273855898,
0.0704797827654166));
#82649=CARTESIAN_POINT('Ctrl Pts',(0.0128195742877331,-0.0341934961088739,
0.0704150921558742));
#82650=CARTESIAN_POINT('Ctrl Pts',(0.0128571121718725,-0.0345231616327842,
0.0706017142222049));
#82651=CARTESIAN_POINT('Ctrl Pts',(0.0128082040480123,-0.0344132092796988,
0.0705364719324432));
#82652=CARTESIAN_POINT('Ctrl Pts',(0.0127579489622852,-0.034303273855898,
0.0704722446348476));
#82653=CARTESIAN_POINT('Ctrl Pts',(0.0127064134049634,-0.0341934961088739,
0.0704091129628253));
#82654=CARTESIAN_POINT('Ctrl Pts',(0.0127442951100142,-0.0345231616327842,
0.0705910630864722));
#82655=CARTESIAN_POINT('Ctrl Pts',(0.0126952401752436,-0.0344132092796988,
0.0705273758210745));
#82656=CARTESIAN_POINT('Ctrl Pts',(0.0126448704506332,-0.034303273855898,
0.0704647065042788));
#82657=CARTESIAN_POINT('Ctrl Pts',(0.0125932525221938,-0.0341934961088739,
0.0704031337697765));
#82658=CARTESIAN_POINT('Ctrl Pts',(0.012631478048156,-0.0345231616327842,
0.0705804119507396));
#82659=CARTESIAN_POINT('Ctrl Pts',(0.0125822763024749,-0.0344132092796988,
0.0705182797097059));
#82660=CARTESIAN_POINT('Ctrl Pts',(0.0125317919389812,-0.034303273855898,
0.0704571683737098));
#82661=CARTESIAN_POINT('Ctrl Pts',(0.0124800916394241,-0.0341934961088739,
0.0703971545767276));
#82662=CARTESIAN_POINT('',(0.0126508454730477,-0.0341934961088839,0.0704061768652707));
#82663=CARTESIAN_POINT('Ctrl Pts',(0.0128275414014334,-0.034210518019539,
0.070425130975398));
#82664=CARTESIAN_POINT('Ctrl Pts',(0.012793852581739,-0.0342610556240575,
0.0704518088803242));
#82665=CARTESIAN_POINT('Ctrl Pts',(0.0127607682904933,-0.0343122189868655,
0.0704780080640417));
#82666=CARTESIAN_POINT('Ctrl Pts',(0.0126957797636824,-0.0344158119695142,
0.0705294719548897));
#82667=CARTESIAN_POINT('Ctrl Pts',(0.0126639021090382,-0.0344681990450031,
0.0705547156128029));
#82668=CARTESIAN_POINT('Ctrl Pts',(0.0126326164751746,-0.0345211942962439,
0.0705794904542292));
#82669=CARTESIAN_POINT('Ctrl Pts',(0.0125537160836053,-0.0346945769586932,
0.0704843529774302));
#82670=CARTESIAN_POINT('Ctrl Pts',(0.0124779314252381,-0.0345296777079064,
0.0703927672288805));
#82671=CARTESIAN_POINT('Ctrl Pts',(0.0123984262007714,-0.0343648066255586,
0.0703043919887749));
#82672=CARTESIAN_POINT('Ctrl Pts',(0.0125539500000802,-0.0346945769586932,
0.0704823388648798));
#82673=CARTESIAN_POINT('Ctrl Pts',(0.0124781237013612,-0.0345296777079064,
0.0703907482802726));
#82674=CARTESIAN_POINT('Ctrl Pts',(0.0123985766722452,-0.0343648066255586,
0.0703023699292757));
#82675=CARTESIAN_POINT('Ctrl Pts',(0.0125929345365957,-0.0346945769586932,
0.0701466667225046));
#82676=CARTESIAN_POINT('Ctrl Pts',(0.0125101684538558,-0.0345296777079064,
0.0700542701601905));
#82677=CARTESIAN_POINT('Ctrl Pts',(0.0124236542588785,-0.0343648066255586,
0.069965373347835));
#82678=CARTESIAN_POINT('',(0.0125843731496633,-0.0346775396664998,0.0701371296667152));
#82679=CARTESIAN_POINT('',(0.0125929345365934,-0.0346945769586886,0.070146666722502));
#82680=CARTESIAN_POINT('Origin',(0.000344881563629885,-0.0345626617441152,
0.0813535348122937));
#82681=CARTESIAN_POINT('Ctrl Pts',(0.0125843731499848,-0.0346775396670096,
0.0701371296685037));
#82682=CARTESIAN_POINT('Ctrl Pts',(0.012552436677156,-0.034626974992875,
0.0701658606153561));
#82683=CARTESIAN_POINT('Ctrl Pts',(0.0125210678107356,-0.0345757902891939,
0.0701940809758775));
#82684=CARTESIAN_POINT('Ctrl Pts',(0.012459439341323,-0.0344721681090197,
0.0702495236372595));
#82685=CARTESIAN_POINT('Ctrl Pts',(0.0124292038958194,-0.0344197714292389,
0.0702767241977988));
#82686=CARTESIAN_POINT('Ctrl Pts',(0.0123995251716564,-0.0343667727834209,
0.0703034239918986));
#82687=CARTESIAN_POINT('',(0.0125734422683439,-0.0346945769587026,0.0703145027936974));
#82688=CARTESIAN_POINT('Origin',(0.00812378219310841,-0.0315241814719618,
0.07415));
#82689=CARTESIAN_POINT('',(0.0125843731482918,-0.034711613648962,0.0701371296669554));
#82690=CARTESIAN_POINT('',(0.0125757914107549,-0.0346945769586885,0.070127610918123));
#82691=CARTESIAN_POINT('Origin',(0.000376550837136767,-0.0345626695995449,
0.08138594164082));
#82692=CARTESIAN_POINT('Origin',(0.000140603155004497,-0.0345626624283481,
0.0811264668912053));
#82693=CARTESIAN_POINT('Origin',(0.00011171584856058,-0.0345626699717168,
0.0810915567704016));
#82694=CARTESIAN_POINT('Ctrl Pts',(0.012507262090966,-0.0352450361874069,
0.0704265786417996));
#82695=CARTESIAN_POINT('Ctrl Pts',(0.0123668309500735,-0.0349452760959493,
0.0702612529845839));
#82696=CARTESIAN_POINT('Ctrl Pts',(0.0122143457543109,-0.034644428984174,
0.0701069748482866));
#82697=CARTESIAN_POINT('Ctrl Pts',(0.0125055851568032,-0.0352450361874069,
0.0704246909138495));
#82698=CARTESIAN_POINT('Ctrl Pts',(0.0123650828190828,-0.0349452760959493,
0.0702594285032436));
#82699=CARTESIAN_POINT('Ctrl Pts',(0.0122125313927483,-0.034644428984174,
0.0701052187967155));
#82700=CARTESIAN_POINT('Ctrl Pts',(0.0123395520713741,-0.0352450361874069,
0.0702377871564155));
#82701=CARTESIAN_POINT('Ctrl Pts',(0.0121920005427703,-0.0349452760959493,
0.0700787867863819));
#82702=CARTESIAN_POINT('Ctrl Pts',(0.0120328916340797,-0.034644428984174,
0.0699313523045283));
#82703=CARTESIAN_POINT('Ctrl Pts',(0.0123378917405198,-0.0352450361874069,
0.0702359181188412));
#82704=CARTESIAN_POINT('Ctrl Pts',(0.0121902697200072,-0.0349452760959493,
0.0700769803692133));
#82705=CARTESIAN_POINT('Ctrl Pts',(0.012031095236493,-0.034644428984174,
0.0699296136396064));
#82706=CARTESIAN_POINT('',(0.0123149376169544,-0.0351951634053344,0.0702114255731725));
#82707=CARTESIAN_POINT('',(0.0121495594633167,-0.0348678972925434,0.0700425382082514));
#82708=CARTESIAN_POINT('Origin',(0.000726994801887408,-0.0345636767881071,
0.0822996048271035));
#82709=CARTESIAN_POINT('Origin',(0.0198841147875398,-0.0346946199340696,
0.0621510463800824));
#82710=CARTESIAN_POINT('',(0.0122378800979282,-0.0346945769330288,0.070131004674344));
#82711=CARTESIAN_POINT('',(0.012193244314101,-0.0346945769458128,0.0700872565556455));
#82712=CARTESIAN_POINT('',(0.0123995251713416,-0.0350221583435276,0.07030342399216));
#82713=CARTESIAN_POINT('Origin',(0.000355882459382666,-0.0345628458716893,
0.0819939595706483));
#82714=CARTESIAN_POINT('',(0.0123986076547722,-0.0351951360298763,0.0703042534836261));
#82715=CARTESIAN_POINT('Origin',(0.020590464340695,-0.0351951838366766,
0.0629346315196116));
#82716=CARTESIAN_POINT('',(0.0123149137278407,-0.0351951371328748,0.0702114036180501));
#82717=CARTESIAN_POINT('Ctrl Pts',(0.0127382359384145,-0.0350241211494343,
0.0703150532425499));
#82718=CARTESIAN_POINT('Ctrl Pts',(0.01268541111922,-0.0349144232818962,
0.0702514910342081));
#82719=CARTESIAN_POINT('Ctrl Pts',(0.0126312408055594,-0.0348045283579412,
0.07018898270758));
#82720=CARTESIAN_POINT('Ctrl Pts',(0.0125757914033085,-0.0346945769439157,
0.0701276109098772));
#82721=CARTESIAN_POINT('Ctrl Pts',(0.0126249726793622,-0.0350241211494343,
0.0703115069836799));
#82722=CARTESIAN_POINT('Ctrl Pts',(0.0125720990119058,-0.0349144232818962,
0.0702495049302917));
#82723=CARTESIAN_POINT('Ctrl Pts',(0.012517912070263,-0.0348045283579412,
0.0701885587021738));
#82724=CARTESIAN_POINT('Ctrl Pts',(0.0124624783560641,-0.0346945769439157,
0.0701287489464803));
#82725=CARTESIAN_POINT('Ctrl Pts',(0.0125117094203098,-0.0350241211494343,
0.0703079607248099));
#82726=CARTESIAN_POINT('Ctrl Pts',(0.0124587869045915,-0.0349144232818962,
0.0702475188263754));
#82727=CARTESIAN_POINT('Ctrl Pts',(0.0124045833349665,-0.0348045283579412,
0.0701881346967676));
#82728=CARTESIAN_POINT('Ctrl Pts',(0.0123491653088197,-0.0346945769439157,
0.0701298869830835));
#82729=CARTESIAN_POINT('Ctrl Pts',(0.0123984461612575,-0.0350241211494343,
0.0703044144659399));
#82730=CARTESIAN_POINT('Ctrl Pts',(0.0123454747972773,-0.0349144232818962,
0.0702455327224591));
#82731=CARTESIAN_POINT('Ctrl Pts',(0.0122912545996701,-0.0348045283579412,
0.0701877106913614));
#82732=CARTESIAN_POINT('Ctrl Pts',(0.0122358522615753,-0.0346945769439157,
0.0701310250196867));
#82733=CARTESIAN_POINT('',(0.0124068357546108,-0.0346945769458128,0.0701293077963898));
#82734=CARTESIAN_POINT('Ctrl Pts',(0.0125843731458412,-0.03471161364928,
0.0701371296691506));
#82735=CARTESIAN_POINT('Ctrl Pts',(0.0125524493470817,-0.0347621546531611,
0.0701658491967306));
#82736=CARTESIAN_POINT('Ctrl Pts',(0.0125210868549705,-0.0348133084095595,
0.0701940637574084));
#82737=CARTESIAN_POINT('Ctrl Pts',(0.0124594583097403,-0.0349168561544576,
0.0702495064920837));
#82738=CARTESIAN_POINT('Ctrl Pts',(0.0124292167016644,-0.0349692089015923,
0.070276712674648));
#82739=CARTESIAN_POINT('Ctrl Pts',(0.0123995251713011,-0.0350221583435,
0.0703034239921697));
#82740=CARTESIAN_POINT('Ctrl Pts',(0.0123148365325578,-0.0351951371254972,
0.0702128645974501));
#82741=CARTESIAN_POINT('Ctrl Pts',(0.0122334387283513,-0.0350307338980977,
0.0701262171785373));
#82742=CARTESIAN_POINT('Ctrl Pts',(0.0121485292467718,-0.0348659306897838,
0.0700430080584134));
#82743=CARTESIAN_POINT('Ctrl Pts',(0.0123149137277612,-0.0351951371254972,
0.0702114036181352));
#82744=CARTESIAN_POINT('Ctrl Pts',(0.012233485718724,-0.0350307338980977,
0.07012475460326));
#82745=CARTESIAN_POINT('Ctrl Pts',(0.0121485459921608,-0.0348659306897838,
0.0700415451369357));
#82746=CARTESIAN_POINT('Ctrl Pts',(0.0123278517243137,-0.0351951371254972,
0.0699665419621991));
#82747=CARTESIAN_POINT('Ctrl Pts',(0.0122413613541713,-0.0350307338980977,
0.0698796254623627));
#82748=CARTESIAN_POINT('Ctrl Pts',(0.0121513525368188,-0.0348659306897838,
0.0697963579724886));
#82749=CARTESIAN_POINT('Origin',(0.015872126049036,-0.0308609197384878,
0.0662444393516408));
#82750=CARTESIAN_POINT('',(0.0123205544025452,-0.0351951371254972,0.0701046494570405));
#82751=CARTESIAN_POINT('Origin',(0.00754815852817955,-0.0351840467441105,
0.0749395587671898));
#82752=CARTESIAN_POINT('Origin',(0.0159131566122411,-0.0352322613691046,
0.0650672331811612));
#82753=CARTESIAN_POINT('',(0.0119771554157214,-0.0351951142564674,0.0698804181246087));
#82754=CARTESIAN_POINT('',(0.0118828176741158,-0.0351951372916787,0.0697988906871318));
#82755=CARTESIAN_POINT('Origin',(0.00778760626108306,-0.03528751189993,
0.0740954534426918));
#82756=CARTESIAN_POINT('Origin',(0.0127572303630695,-0.0298325076523433,
0.0800513852894583));
#82757=CARTESIAN_POINT('Origin',(0.0155875963746084,-0.033873220915644,
0.0703365895131585));
#82758=CARTESIAN_POINT('Ctrl Pts',(0.0137509251183969,-0.0321934096636942,
0.0729611357336992));
#82759=CARTESIAN_POINT('Ctrl Pts',(0.0137296450141914,-0.0320508460845377,
0.0728604125550963));
#82760=CARTESIAN_POINT('Ctrl Pts',(0.0137056747221907,-0.0319086045665171,
0.0727603370765129));
#82761=CARTESIAN_POINT('Ctrl Pts',(0.0136790835943085,-0.0317669892871035,
0.0726611205290178));
#82762=CARTESIAN_POINT('Ctrl Pts',(0.0137318134523105,-0.0321934096636942,
0.0728794951993604));
#82763=CARTESIAN_POINT('Ctrl Pts',(0.0137090720214192,-0.0320508460845377,
0.0727791141104791));
#82764=CARTESIAN_POINT('Ctrl Pts',(0.0136836506958537,-0.0319086045665171,
0.0726794197266451));
#82765=CARTESIAN_POINT('Ctrl Pts',(0.0136556218843043,-0.0317669892871035,
0.0725806222011489));
#82766=CARTESIAN_POINT('Ctrl Pts',(0.0137127017862241,-0.0321934096636942,
0.0727978546650216));
#82767=CARTESIAN_POINT('Ctrl Pts',(0.013688499028647,-0.0320508460845377,
0.0726978156658619));
#82768=CARTESIAN_POINT('Ctrl Pts',(0.0136616266695168,-0.0319086045665171,
0.0725985023767772));
#82769=CARTESIAN_POINT('Ctrl Pts',(0.0136321601743,-0.0317669892871035,
0.0725001238732799));
#82770=CARTESIAN_POINT('Ctrl Pts',(0.0136935901201377,-0.0321934096636942,
0.0727162141306828));
#82771=CARTESIAN_POINT('Ctrl Pts',(0.0136679260358748,-0.0320508460845377,
0.0726165172212447));
#82772=CARTESIAN_POINT('Ctrl Pts',(0.0136396026431798,-0.0319086045665171,
0.0725175850269093));
#82773=CARTESIAN_POINT('Ctrl Pts',(0.0136086984642957,-0.0317669892871035,
0.0724196255454111));
#82774=CARTESIAN_POINT('',(0.0136939320316184,-0.0321934096636942,0.0727176746959757));
#82775=CARTESIAN_POINT('',(0.013630382515873,-0.0318665617511334,0.0724900367851861));
#82776=CARTESIAN_POINT('Origin',(-0.00263158734375825,-0.0326371944422963,
0.076280724228609));
#82777=CARTESIAN_POINT('Origin',(0.0241250974477546,-0.0316939261509355,
0.0693264077590119));
#82778=CARTESIAN_POINT('',(0.0137236408735195,-0.0320197221621819,0.0728388280334148));
#82779=CARTESIAN_POINT('Ctrl Pts',(0.0137236460388813,-0.0320197392094732,
0.0728386431329055));
#82780=CARTESIAN_POINT('Ctrl Pts',(0.0137169733878477,-0.0319792716576029,
0.0728101492360508));
#82781=CARTESIAN_POINT('Ctrl Pts',(0.0137100531343661,-0.0319386439829723,
0.0727815764937398));
#82782=CARTESIAN_POINT('Ctrl Pts',(0.0137028697936117,-0.0318979099381655,
0.0727528969008297));
#82783=CARTESIAN_POINT('Ctrl Pts',(0.0136956865948412,-0.0318571766984958,
0.0727242178747919));
#82784=CARTESIAN_POINT('Ctrl Pts',(0.013688278557203,-0.0318163871833608,
0.072695577335032));
#82785=CARTESIAN_POINT('Ctrl Pts',(0.0136806745702592,-0.0317755399638303,
0.0726670729114552));
#82786=CARTESIAN_POINT('',(0.0137224236774251,-0.0321934096636183,0.0728393842935138));
#82787=CARTESIAN_POINT('Origin',(0.0159646654076172,-0.0324111993426145,
0.0722928894874314));
#82788=CARTESIAN_POINT('',(0.0137081778545317,-0.0321934096636662,0.0727785294947547));
#82789=CARTESIAN_POINT('Ctrl Pts',(0.0136928625085267,-0.0321934096636618,
0.0727193980089872));
#82790=CARTESIAN_POINT('Ctrl Pts',(0.0136731333921247,-0.0320835708272592,
0.0726425960511502));
#82791=CARTESIAN_POINT('Ctrl Pts',(0.0136518263068861,-0.0319739230346489,
0.0725662469346086));
#82792=CARTESIAN_POINT('Ctrl Pts',(0.0136289760106762,-0.0318646057455573,
0.0724904462505591));
#82793=CARTESIAN_POINT('Ctrl Pts',(0.0137526178529808,-0.0321934096636618,
0.0726231147623967));
#82794=CARTESIAN_POINT('Ctrl Pts',(0.0137315609155695,-0.0320835708272592,
0.0725454887317892));
#82795=CARTESIAN_POINT('Ctrl Pts',(0.0137089097253686,-0.0319739230346489,
0.0724683434996594));
#82796=CARTESIAN_POINT('Ctrl Pts',(0.0136847008381052,-0.0318646057455573,
0.0723917755437976));
#82797=CARTESIAN_POINT('Ctrl Pts',(0.0138123731974348,-0.0321934096636618,
0.0725268315158063));
#82798=CARTESIAN_POINT('Ctrl Pts',(0.0137899884390143,-0.0320835708272592,
0.0724483814124281));
#82799=CARTESIAN_POINT('Ctrl Pts',(0.0137659931438512,-0.0319739230346489,
0.0723704400647102));
#82800=CARTESIAN_POINT('Ctrl Pts',(0.0137404256655343,-0.0318646057455573,
0.0722931048370361));
#82801=CARTESIAN_POINT('Ctrl Pts',(0.0138721285418889,-0.0321934096636618,
0.0724305482692159));
#82802=CARTESIAN_POINT('Ctrl Pts',(0.0138484159624591,-0.0320835708272592,
0.0723512740930671));
#82803=CARTESIAN_POINT('Ctrl Pts',(0.0138230765623337,-0.0319739230346489,
0.072272536629761));
#82804=CARTESIAN_POINT('Ctrl Pts',(0.0137961504929634,-0.0318646057455573,
0.0721944341302745));
#82805=CARTESIAN_POINT('',(0.0138684426467717,-0.0321763980308286,0.0724182736215178));
#82806=CARTESIAN_POINT('',(0.0138721285418775,-0.0321934096636184,0.0724305482691878));
#82807=CARTESIAN_POINT('Origin',(-0.00214121275700354,-0.0326386231564428,
0.0766036082940997));
#82808=CARTESIAN_POINT('Ctrl Pts',(0.0138684426437268,-0.0321763980306299,
0.0724182736224286));
#82809=CARTESIAN_POINT('Ctrl Pts',(0.013827350232142,-0.0321259596175181,
0.0724306609190619));
#82810=CARTESIAN_POINT('Ctrl Pts',(0.01378696979991,-0.0320749164632105,
0.0724428335897142));
#82811=CARTESIAN_POINT('Ctrl Pts',(0.0137076003971833,-0.0319716057793985,
0.0724667594752309));
#82812=CARTESIAN_POINT('Ctrl Pts',(0.0136686423517508,-0.0319193786690198,
0.0724785033677434));
#82813=CARTESIAN_POINT('Ctrl Pts',(0.0136303825140914,-0.0318665617525393,
0.0724900367857141));
#82814=CARTESIAN_POINT('',(0.0137830302867579,-0.0321934096636663,0.0725741114825918));
#82815=CARTESIAN_POINT('Origin',(0.00812378219310841,-0.0315241814719618,
0.07415));
#82816=CARTESIAN_POINT('',(0.0138684426471269,-0.032210423332377,0.0724182736214106));
#82817=CARTESIAN_POINT('',(0.0138647305447439,-0.0321934096636183,0.0724060068739045));
#82818=CARTESIAN_POINT('Origin',(-0.00213430260582455,-0.0326387241818522,
0.0766484115498298));
#82819=CARTESIAN_POINT('Origin',(-0.00178707430780203,-0.0326386237460637,
0.0777783976214467));
#82820=CARTESIAN_POINT('Origin',(-0.00180607434721047,-0.032638724687269,
0.0777372387427542));
#82821=CARTESIAN_POINT('Ctrl Pts',(0.0136747273595271,-0.0327445246967096,
0.0726449641999562));
#82822=CARTESIAN_POINT('Ctrl Pts',(0.0136179640063733,-0.0324436878339359,
0.0724356068804763));
#82823=CARTESIAN_POINT('Ctrl Pts',(0.0135455922629537,-0.0321434074405927,
0.072231119970784));
#82824=CARTESIAN_POINT('Ctrl Pts',(0.0136040777686263,-0.0327445246967096,
0.0724051546186098));
#82825=CARTESIAN_POINT('Ctrl Pts',(0.0135382698492535,-0.0324436878339359,
0.0721984618920109));
#82826=CARTESIAN_POINT('Ctrl Pts',(0.0134570799422983,-0.0321434074405927,
0.0719973132790659));
#82827=CARTESIAN_POINT('',(0.0135930041633336,-0.0326943950436612,0.0723707484606142));
#82828=CARTESIAN_POINT('',(0.0135152865462182,-0.0323666188837389,0.0721475500479665));
#82829=CARTESIAN_POINT('Origin',(-0.00236959641976738,-0.0326395579112551,
0.077643645278268));
#82830=CARTESIAN_POINT('Origin',(0.0238688493646319,-0.0321933825603049,
0.0683021490546249));
#82831=CARTESIAN_POINT('',(0.01355753425258,-0.0321934096532689,0.0722652019861543));
#82832=CARTESIAN_POINT('',(0.0135357736329072,-0.0321934096584275,0.0722066125180125));
#82833=CARTESIAN_POINT('',(0.0136303825167703,-0.0325210109756239,0.0724900367849113));
#82834=CARTESIAN_POINT('Origin',(-0.00249400463831448,-0.0326393129156579,
0.077179202574978));
#82835=CARTESIAN_POINT('',(0.0136290817962303,-0.0326943950436593,0.0724904288867702));
#82836=CARTESIAN_POINT('Origin',(0.0242207569404267,-0.0326943765538118,
0.0692975721206675));
#82837=CARTESIAN_POINT('',(0.013611042979792,-0.0326943950436702,0.0724305886737022));
#82838=CARTESIAN_POINT('Ctrl Pts',(0.0139319059659176,-0.0325229783203769,
0.0726447763489058));
#82839=CARTESIAN_POINT('Ctrl Pts',(0.0139111564908043,-0.032413025309245,
0.0725647114897128));
#82840=CARTESIAN_POINT('Ctrl Pts',(0.0138887539182925,-0.032303122220807,
0.0724850880034719));
#82841=CARTESIAN_POINT('Ctrl Pts',(0.0138647305434476,-0.0321934096576658,
0.0724060068696172));
#82842=CARTESIAN_POINT('Ctrl Pts',(0.0138309322364644,-0.0325229783203769,
0.0725933424282199));
#82843=CARTESIAN_POINT('Ctrl Pts',(0.0138094737458793,-0.032413025309245,
0.0725146694896793));
#82844=CARTESIAN_POINT('Ctrl Pts',(0.0137863910590984,-0.032303122220807,
0.0724364523798745));
#82845=CARTESIAN_POINT('Ctrl Pts',(0.0137617172787974,-0.0321934096576658,
0.0723587902460305));
#82846=CARTESIAN_POINT('Ctrl Pts',(0.0137299585070112,-0.0325229783203769,
0.072541908507534));
#82847=CARTESIAN_POINT('Ctrl Pts',(0.0137077910009542,-0.032413025309245,
0.0724646274896458));
#82848=CARTESIAN_POINT('Ctrl Pts',(0.0136840281999043,-0.032303122220807,
0.0723878167562771));
#82849=CARTESIAN_POINT('Ctrl Pts',(0.0136587040141473,-0.0321934096576658,
0.0723115736224438));
#82850=CARTESIAN_POINT('Ctrl Pts',(0.013628984777558,-0.0325229783203769,
0.0724904745868481));
#82851=CARTESIAN_POINT('Ctrl Pts',(0.0136061082560291,-0.032413025309245,
0.0724145854896122));
#82852=CARTESIAN_POINT('Ctrl Pts',(0.0135816653407102,-0.032303122220807,
0.0723391811326797));
#82853=CARTESIAN_POINT('Ctrl Pts',(0.0135556907494971,-0.0321934096576658,
0.0722643569988571));
#82854=CARTESIAN_POINT('',(0.0137111323989621,-0.0321934096584275,0.0723356044304525));
#82855=CARTESIAN_POINT('Ctrl Pts',(0.0138684426437907,-0.0322104233328904,
0.0724182736224094));
#82856=CARTESIAN_POINT('Ctrl Pts',(0.013827294551371,-0.032260942183044,
0.0724306777040157));
#82857=CARTESIAN_POINT('Ctrl Pts',(0.0137868869181465,-0.0323120888238839,
0.0724428585743929));
#82858=CARTESIAN_POINT('Ctrl Pts',(0.0137075169143957,-0.0324156524631812,
0.0724667846410882));
#82859=CARTESIAN_POINT('Ctrl Pts',(0.0136685871693151,-0.0324680267167316,
0.0724785200024743));
#82860=CARTESIAN_POINT('Ctrl Pts',(0.0136303825167275,-0.0325210109755912,
0.0724900367849197));
#82861=CARTESIAN_POINT('Origin',(0.00947084381705225,-0.0262834582511158,
0.0819016972865226));
#82862=CARTESIAN_POINT('Origin',(0.0201046183452919,-0.0342770676166929,
0.0762193053832568));
#82863=CARTESIAN_POINT('Ctrl Pts',(0.013592045191167,-0.0326943950436604,
0.0723725350952205));
#82864=CARTESIAN_POINT('Ctrl Pts',(0.0135675483934548,-0.0325844576448134,
0.0722971721824901));
#82865=CARTESIAN_POINT('Ctrl Pts',(0.0135414912334718,-0.0324744968375322,
0.0722223105701491));
#82866=CARTESIAN_POINT('Ctrl Pts',(0.0135139084201555,-0.0323646534831894,
0.0721480457147681));
#82867=CARTESIAN_POINT('Ctrl Pts',(0.0136456368694318,-0.0326943950436604,
0.0722726899170576));
#82868=CARTESIAN_POINT('Ctrl Pts',(0.0136197640180347,-0.0325844576448134,
0.0721965884105592));
#82869=CARTESIAN_POINT('Ctrl Pts',(0.0135923154316513,-0.0324744968375322,
0.072121016611225));
#82870=CARTESIAN_POINT('Ctrl Pts',(0.0135633276145464,-0.0323646534831894,
0.0720460708609689));
#82871=CARTESIAN_POINT('Ctrl Pts',(0.0136992285476966,-0.0326943950436604,
0.0721728447388946));
#82872=CARTESIAN_POINT('Ctrl Pts',(0.0136719796426146,-0.0325844576448134,
0.0720960046386282));
#82873=CARTESIAN_POINT('Ctrl Pts',(0.0136431396298308,-0.0324744968375322,
0.0720197226523008));
#82874=CARTESIAN_POINT('Ctrl Pts',(0.0136127468089373,-0.0323646534831894,
0.0719440960071696));
#82875=CARTESIAN_POINT('Ctrl Pts',(0.0137528202259614,-0.0326943950436604,
0.0720729995607317));
#82876=CARTESIAN_POINT('Ctrl Pts',(0.0137241952671946,-0.0325844576448134,
0.0719954208666973));
#82877=CARTESIAN_POINT('Ctrl Pts',(0.0136939638280103,-0.0324744968375322,
0.0719184286933768));
#82878=CARTESIAN_POINT('Ctrl Pts',(0.0136621660033283,-0.0323646534831894,
0.0718421211533704));
#82879=CARTESIAN_POINT('',(0.0137483708728123,-0.0326773559991177,0.0720609805734748));
#82880=CARTESIAN_POINT('',(0.0137528202259598,-0.0326943950436594,0.0720729995607336));
#82881=CARTESIAN_POINT('Origin',(-0.00180032032256985,-0.0326395670310402,
0.0778894890183537));
#82882=CARTESIAN_POINT('Ctrl Pts',(0.0137483708696632,-0.0326773559987436,
0.0720609805746371));
#82883=CARTESIAN_POINT('Ctrl Pts',(0.0137081049721412,-0.0326267922586234,
0.0720759356668118));
#82884=CARTESIAN_POINT('Ctrl Pts',(0.0136685527585761,-0.032575610957988,
0.0720906256907771));
#82885=CARTESIAN_POINT('Ctrl Pts',(0.0135908420383873,-0.032471998546237,
0.0721194881042563));
#82886=CARTESIAN_POINT('Ctrl Pts',(0.0135527146994713,-0.0324196091621772,
0.0721336489178222));
#82887=CARTESIAN_POINT('Ctrl Pts',(0.0135152865461725,-0.0323666188837756,
0.0721475500479834));
#82888=CARTESIAN_POINT('',(0.0136729121946567,-0.0326943950436702,0.0722218740106839));
#82889=CARTESIAN_POINT('Origin',(0.00812378219310841,-0.0315241814719618,
0.07415));
#82890=CARTESIAN_POINT('',(0.0137483708727707,-0.0327114338380042,0.0720609805734901));
#82891=CARTESIAN_POINT('',(0.0137438958601232,-0.0326943950436593,0.0720489711163711));
#82892=CARTESIAN_POINT('Origin',(-0.00178381914769819,-0.0326395676808559,
0.0779316872169131));
#82893=CARTESIAN_POINT('Origin',(-0.00183530563046278,-0.0326395675415347,
0.0777952954196774));
#82894=CARTESIAN_POINT('Origin',(-0.0018503487587794,-0.0326395682909456,
0.0777525558319516));
#82895=CARTESIAN_POINT('Ctrl Pts',(0.013569259236313,-0.0332451089994433,
0.0722993501757676));
#82896=CARTESIAN_POINT('Ctrl Pts',(0.0134994608362305,-0.0329451141710254,
0.0720939706488981));
#82897=CARTESIAN_POINT('Ctrl Pts',(0.0134143907004741,-0.0326442513127493,
0.071894432084421));
#82898=CARTESIAN_POINT('Ctrl Pts',(0.0134836896860458,-0.0332451089994433,
0.0720644505119385));
#82899=CARTESIAN_POINT('Ctrl Pts',(0.0134050319001948,-0.0329451141710254,
0.0718622982934587));
#82900=CARTESIAN_POINT('Ctrl Pts',(0.0133113706413111,-0.0326442513127493,
0.0716666451940825));
#82901=CARTESIAN_POINT('Ctrl Pts',(0.0134828339905431,-0.0332451089994433,
0.0720621015153002));
#82902=CARTESIAN_POINT('Ctrl Pts',(0.0134040876108344,-0.0329451141710254,
0.0718599815699044));
#82903=CARTESIAN_POINT('Ctrl Pts',(0.0133103404407195,-0.0326442513127493,
0.0716643673251791));
#82904=CARTESIAN_POINT('',(0.0134704917745687,-0.0331951640388616,0.0720308441181636));
#82905=CARTESIAN_POINT('',(0.0133789127710123,-0.0328677532355027,0.0718129660509484));
#82906=CARTESIAN_POINT('Origin',(-0.00181472275481337,-0.0326402808281768,
0.0789152078698814));
#82907=CARTESIAN_POINT('Origin',(0.02348081544725,-0.0326944278779034,0.0673200888768139));
#82908=CARTESIAN_POINT('',(0.0134284645353448,-0.0326943950436593,0.071927733083546));
#82909=CARTESIAN_POINT('',(0.0134030679929601,-0.0326943950436694,0.0718706255916273));
#82910=CARTESIAN_POINT('',(0.0135152865462192,-0.0330220786163545,0.0721475500479691));
#82911=CARTESIAN_POINT('Origin',(-0.00203837613684075,-0.0326396682761693,
0.0784896120410405));
#82912=CARTESIAN_POINT('',(0.013514013012634,-0.0331951640388587,0.0721480230490247));
#82913=CARTESIAN_POINT('Origin',(0.0238554318344169,-0.0331952026560145,
0.0683071343098413));
#82914=CARTESIAN_POINT('',(0.0134922523936113,-0.0331951640388701,0.0720894335836041));
#82915=CARTESIAN_POINT('Ctrl Pts',(0.0138259308863425,-0.0330240426238172,
0.072283050541571));
#82916=CARTESIAN_POINT('Ctrl Pts',(0.0138002118386719,-0.0329142774063519,
0.0722044978879874));
#82917=CARTESIAN_POINT('Ctrl Pts',(0.0137728560663424,-0.0328043479726691,
0.0721264377575992));
#82918=CARTESIAN_POINT('Ctrl Pts',(0.0137438958601305,-0.0326943950436593,
0.072048971116374));
#82919=CARTESIAN_POINT('Ctrl Pts',(0.0137219268609901,-0.0330240426238172,
0.0722380583345183));
#82920=CARTESIAN_POINT('Ctrl Pts',(0.0136955880018336,-0.0329142774063519,
0.0721609384377102));
#82921=CARTESIAN_POINT('Ctrl Pts',(0.0136676417281043,-0.0328043479726691,
0.0720843245916136));
#82922=CARTESIAN_POINT('Ctrl Pts',(0.0136381211380807,-0.0326943950436593,
0.0720083159302318));
#82923=CARTESIAN_POINT('Ctrl Pts',(0.0136179228356377,-0.0330240426238172,
0.0721930661274656));
#82924=CARTESIAN_POINT('Ctrl Pts',(0.0135909641649953,-0.0329142774063519,
0.0721173789874329));
#82925=CARTESIAN_POINT('Ctrl Pts',(0.0135624273898662,-0.0328043479726691,
0.0720422114256281));
#82926=CARTESIAN_POINT('Ctrl Pts',(0.0135323464160309,-0.0326943950436593,
0.0719676607440896));
#82927=CARTESIAN_POINT('Ctrl Pts',(0.0135139188102854,-0.0330240426238172,
0.0721480739204129));
#82928=CARTESIAN_POINT('Ctrl Pts',(0.013486340328157,-0.0329142774063519,
0.0720738195371556));
#82929=CARTESIAN_POINT('Ctrl Pts',(0.0134572130516281,-0.0328043479726691,
0.0720000982596426));
#82930=CARTESIAN_POINT('Ctrl Pts',(0.0134265716939811,-0.0326943950436593,
0.0719270055579474));
#82931=CARTESIAN_POINT('',(0.013586180197744,-0.0326943950436693,0.0719883520999685));
#82932=CARTESIAN_POINT('Ctrl Pts',(0.0137483708696573,-0.0327114338383302,
0.0720609805746394));
#82933=CARTESIAN_POINT('Ctrl Pts',(0.0137081116697189,-0.0327619876830128,
0.0720759331792754));
#82934=CARTESIAN_POINT('Ctrl Pts',(0.013668562727585,-0.0328131562602624,
0.0720906219882037));
#82935=CARTESIAN_POINT('Ctrl Pts',(0.0135908520786755,-0.0329167375858768,
0.0721194843752092));
#82936=CARTESIAN_POINT('Ctrl Pts',(0.0135527213360146,-0.032969108892062,
0.0721336464529543));
#82937=CARTESIAN_POINT('Ctrl Pts',(0.0135152865461737,-0.0330220786163187,
0.0721475500479831));
#82938=CARTESIAN_POINT('Ctrl Pts',(0.0134696467435439,-0.0331951640388604,
0.0720326877358995));
#82939=CARTESIAN_POINT('Ctrl Pts',(0.013425872669978,-0.0330306422010619,
0.0719221654137687));
#82940=CARTESIAN_POINT('Ctrl Pts',(0.0133775679972495,-0.0328657861914645,
0.0718135467606821));
#82941=CARTESIAN_POINT('Ctrl Pts',(0.0134704917745698,-0.0331951640388604,
0.0720308441181666));
#82942=CARTESIAN_POINT('Ctrl Pts',(0.0134266795853892,-0.0330306422010619,
0.0719203043255611));
#82943=CARTESIAN_POINT('Ctrl Pts',(0.0133783361075426,-0.0328657861914645,
0.0718116697922867));
#82944=CARTESIAN_POINT('Ctrl Pts',(0.0136112966685905,-0.0331951640388604,
0.071723647824121));
#82945=CARTESIAN_POINT('Ctrl Pts',(0.0135611333929865,-0.0330306422010619,
0.0716101969806073));
#82946=CARTESIAN_POINT('Ctrl Pts',(0.0135063239388799,-0.0328657861914645,
0.0714989163809781));
#82947=CARTESIAN_POINT('',(0.0136061014182251,-0.0331781648281936,0.0717119319308448));
#82948=CARTESIAN_POINT('',(0.0136112966685892,-0.0331951640388588,0.0717236478241218));
#82949=CARTESIAN_POINT('Origin',(-0.00118719467340796,-0.0326412092817283,
0.0790702521208667));
#82950=CARTESIAN_POINT('Ctrl Pts',(0.0136061014178578,-0.033178164828644,
0.0717119319326457));
#82951=CARTESIAN_POINT('Ctrl Pts',(0.0135668269985692,-0.0331276811546773,
0.0717293978583441));
#82952=CARTESIAN_POINT('Ctrl Pts',(0.0135282617674078,-0.033076566349778,
0.0717465484344126));
#82953=CARTESIAN_POINT('Ctrl Pts',(0.0134525164811448,-0.0329730614463152,
0.0717802334744865));
#82954=CARTESIAN_POINT('Ctrl Pts',(0.0134153670233181,-0.0329207133373891,
0.0717967543255685));
#82955=CARTESIAN_POINT('Ctrl Pts',(0.0133789127846533,-0.0328677532289382,
0.0718129660601775));
#82956=CARTESIAN_POINT('',(0.0135408942215889,-0.0331951640388702,0.0718772459711527));
#82957=CARTESIAN_POINT('Origin',(0.00812378219310841,-0.0315241814719618,
0.07415));
#82958=CARTESIAN_POINT('',(0.0136061014165443,-0.0332121607144411,0.0717119319308847));
#82959=CARTESIAN_POINT('',(0.0136008811544451,-0.0331951640388587,0.0717002271599729));
#82960=CARTESIAN_POINT('Origin',(-0.00116187982707517,-0.0326413661437492,
0.0791078728231921));
#82961=CARTESIAN_POINT('Origin',(-0.00176604658340047,-0.0326412096066327,
0.0777686292935566));
#82962=CARTESIAN_POINT('Origin',(-0.00177702545824643,-0.0326413667295984,
0.0777246335526917));
#82963=CARTESIAN_POINT('Ctrl Pts',(0.0134423184956348,-0.0337436976235975,
0.0719610969416829));
#82964=CARTESIAN_POINT('Ctrl Pts',(0.0134226311697909,-0.0336723290703325,
0.0719132612201318));
#82965=CARTESIAN_POINT('Ctrl Pts',(0.0134020866150368,-0.033601104548885,
0.0718657873502121));
#82966=CARTESIAN_POINT('Ctrl Pts',(0.013336491921354,-0.0333736987606857,
0.0717142126876021));
#82967=CARTESIAN_POINT('Ctrl Pts',(0.0132623070944247,-0.0331450831799192,
0.0715666520097842));
#82968=CARTESIAN_POINT('Ctrl Pts',(0.0133421691550725,-0.0337436976235975,
0.0717320333924551));
#82969=CARTESIAN_POINT('Ctrl Pts',(0.0133204215969514,-0.0336723290703325,
0.0716850984292509));
#82970=CARTESIAN_POINT('Ctrl Pts',(0.0132978333450206,-0.033601104548885,
0.0716385622290417));
#82971=CARTESIAN_POINT('Ctrl Pts',(0.0132257135310861,-0.0333736987606857,
0.0714899813600757));
#82972=CARTESIAN_POINT('Ctrl Pts',(0.0131451861379285,-0.0331450831799192,
0.0713457839913899));
#82973=CARTESIAN_POINT('Ctrl Pts',(0.0133411676616669,-0.0337436976235975,
0.0717297427569627));
#82974=CARTESIAN_POINT('Ctrl Pts',(0.013319399501223,-0.0336723290703325,
0.0716828168013421));
#82975=CARTESIAN_POINT('Ctrl Pts',(0.0132967908123204,-0.033601104548885,
0.07163628997783));
#82976=CARTESIAN_POINT('Ctrl Pts',(0.0132246057471835,-0.0333736987606857,
0.0714877390468003));
#82977=CARTESIAN_POINT('Ctrl Pts',(0.0131440149283635,-0.0331450831799192,
0.071343575311206));
#82978=CARTESIAN_POINT('',(0.0133268783657592,-0.0336938721132548,0.0716993031158164));
#82979=CARTESIAN_POINT('',(0.0132217993931271,-0.0333679869945434,0.0714876052831402));
#82980=CARTESIAN_POINT('Ctrl Pts',(0.0133268783657653,-0.0336938721132649,
0.0716993031158282));
#82981=CARTESIAN_POINT('Ctrl Pts',(0.0133173121461836,-0.0336629187933932,
0.0716789929906506));
#82982=CARTESIAN_POINT('Ctrl Pts',(0.0133076300621579,-0.033631995230104,
0.0716587453751967));
#82983=CARTESIAN_POINT('Ctrl Pts',(0.0132978333450263,-0.033601104548895,
0.0716385622290537));
#82984=CARTESIAN_POINT('Ctrl Pts',(0.013273250029495,-0.0335235892595454,
0.071587915809097));
#82985=CARTESIAN_POINT('Ctrl Pts',(0.0132479010760106,-0.0334458668660369,
0.0715375854107547));
#82986=CARTESIAN_POINT('Ctrl Pts',(0.013221799393407,-0.0333679869945385,
0.0714876052830018));
#82987=CARTESIAN_POINT('Ctrl Pts',(0.0132217794166821,-0.0333679692459108,
0.0714875655463521));
#82988=CARTESIAN_POINT('Ctrl Pts',(0.0132213804309152,-0.0333391895372506,
0.071487780600257));
#82989=CARTESIAN_POINT('Ctrl Pts',(0.0132210829123114,-0.0333104081057283,
0.0714879446520744));
#82990=CARTESIAN_POINT('Ctrl Pts',(0.0132206917694677,-0.0332532697643015,
0.071488166652919));
#82991=CARTESIAN_POINT('Ctrl Pts',(0.0132205951714736,-0.0332249168356299,
0.0714882261525571));
#82992=CARTESIAN_POINT('Ctrl Pts',(0.0132205951108887,-0.0331960985483764,
0.0714882339653226));
#82993=CARTESIAN_POINT('Ctrl Pts',(0.0132205951363545,-0.0331956312440266,
0.0714882340783684));
#82994=CARTESIAN_POINT('Ctrl Pts',(0.0132205951878506,-0.0331951640388588,
0.0714882341769745));
#82995=CARTESIAN_POINT('',(0.0132784596622649,-0.0331951640388587,0.07159903445947));
#82996=CARTESIAN_POINT('',(0.0132495274250681,-0.0331951640388688,0.0715436343182328));
#82997=CARTESIAN_POINT('',(0.013378912770842,-0.0335216366567682,0.0718129660664729));
#82998=CARTESIAN_POINT('Origin',(-0.00130623962662685,-0.0326434571526819,
0.0796689805829238));
#82999=CARTESIAN_POINT('',(0.0133776714505554,-0.0336938721132328,0.0718135180996883));
#83000=CARTESIAN_POINT('Origin',(0.0233560129331568,-0.033693886789623,
0.0673760040209701));
#83001=CARTESIAN_POINT('',(0.0133522749081673,-0.0336938721132538,0.0717564106077624));
#83002=CARTESIAN_POINT('Ctrl Pts',(0.0136974519161943,-0.0335235895815172,
0.0719286927682037));
#83003=CARTESIAN_POINT('Ctrl Pts',(0.0136668712487971,-0.0334144449262748,
0.0718519602309195));
#83004=CARTESIAN_POINT('Ctrl Pts',(0.0136346702114454,-0.0333049234473147,
0.0717757713108203));
#83005=CARTESIAN_POINT('Ctrl Pts',(0.013600881154452,-0.0331951640388587,
0.0717002271599751));
#83006=CARTESIAN_POINT('Ctrl Pts',(0.0135908278772855,-0.0335235895815172,
0.0718903197723197));
#83007=CARTESIAN_POINT('Ctrl Pts',(0.0135597189300505,-0.0334144449262748,
0.0718150551248545));
#83008=CARTESIAN_POINT('Ctrl Pts',(0.0135270193314304,-0.0333049234473147,
0.0717403466948658));
#83009=CARTESIAN_POINT('Ctrl Pts',(0.0134927622407293,-0.0331951640388587,
0.0716662937990782));
#83010=CARTESIAN_POINT('Ctrl Pts',(0.0134842038383766,-0.0335235895815172,
0.0718519467764358));
#83011=CARTESIAN_POINT('Ctrl Pts',(0.0134525666113038,-0.0334144449262748,
0.0717781500187896));
#83012=CARTESIAN_POINT('Ctrl Pts',(0.0134193684514153,-0.0333049234473147,
0.0717049220789113));
#83013=CARTESIAN_POINT('Ctrl Pts',(0.0133846433270065,-0.0331951640388587,
0.0716323604381814));
#83014=CARTESIAN_POINT('Ctrl Pts',(0.0133775797994678,-0.0335235895815172,
0.0718135737805518));
#83015=CARTESIAN_POINT('Ctrl Pts',(0.0133454142925572,-0.0334144449262748,
0.0717412449127246));
#83016=CARTESIAN_POINT('Ctrl Pts',(0.0133117175714003,-0.0333049234473147,
0.0716694974629568));
#83017=CARTESIAN_POINT('Ctrl Pts',(0.0132765244132838,-0.0331951640388587,
0.0715984270772845));
#83018=CARTESIAN_POINT('',(0.013439670408365,-0.0331951640388687,0.0716496308097315));
#83019=CARTESIAN_POINT('Ctrl Pts',(0.0136061014136768,-0.0332121607145961,
0.0717119319321526));
#83020=CARTESIAN_POINT('Ctrl Pts',(0.0135668930591495,-0.0332625444108954,
0.0717293684646345));
#83021=CARTESIAN_POINT('Ctrl Pts',(0.0135283603260961,-0.0333135300745199,
0.0717465045383006));
#83022=CARTESIAN_POINT('Ctrl Pts',(0.0134526155159261,-0.0334167203140579,
0.0717801893704949));
#83023=CARTESIAN_POINT('Ctrl Pts',(0.0134154327755747,-0.0334688847587263,
0.0717967250825318));
#83024=CARTESIAN_POINT('Ctrl Pts',(0.0133789127701246,-0.033521636656232,
0.0718129660666014));
#83025=CARTESIAN_POINT('Ctrl Pts',(0.0133265196484848,-0.0336938721132388,
0.0717002364093335));
#83026=CARTESIAN_POINT('Ctrl Pts',(0.0133121803692709,-0.0336474569764957,
0.0716697830605558));
#83027=CARTESIAN_POINT('Ctrl Pts',(0.0132974855776959,-0.033601104548885,
0.0716394996578291));
#83028=CARTESIAN_POINT('Ctrl Pts',(0.0132602817439722,-0.0334837508592656,
0.0715628290447157));
#83029=CARTESIAN_POINT('Ctrl Pts',(0.0132208223381995,-0.0333660264659097,
0.0714872945264145));
#83030=CARTESIAN_POINT('Ctrl Pts',(0.0133268783657679,-0.0336938721132388,
0.0716993031158349));
#83031=CARTESIAN_POINT('Ctrl Pts',(0.0133125336236774,-0.0336474569764957,
0.071668847667366));
#83032=CARTESIAN_POINT('Ctrl Pts',(0.0132978333450206,-0.033601104548885,
0.0716385622290417));
#83033=CARTESIAN_POINT('Ctrl Pts',(0.0132606156192675,-0.0334837508592656,
0.0715618864622633));
#83034=CARTESIAN_POINT('Ctrl Pts',(0.0132211421748518,-0.0333660264659097,
0.0714863472042099));
#83035=CARTESIAN_POINT('Ctrl Pts',(0.0134488438267941,-0.0336938721132388,
0.0713819792030978));
#83036=CARTESIAN_POINT('Ctrl Pts',(0.0134326416825432,-0.0336474569764957,
0.0713508098503131));
#83037=CARTESIAN_POINT('Ctrl Pts',(0.0134160757718449,-0.033601104548885,
0.0713198322998276));
#83038=CARTESIAN_POINT('Ctrl Pts',(0.0133741346946984,-0.0334837508592656,
0.0712414042641836));
#83039=CARTESIAN_POINT('Ctrl Pts',(0.0133298880496777,-0.0333660264659097,
0.0711642534694269));
#83040=CARTESIAN_POINT('',(0.01344219575284,-0.0336769361243754,0.0713725052281484));
#83041=CARTESIAN_POINT('',(0.0134481163985911,-0.033693872113232,0.0713838717910539));
#83042=CARTESIAN_POINT('Ctrl Pts',(0.01344219575284,-0.0336769361243754,
0.0713725052281484));
#83043=CARTESIAN_POINT('Ctrl Pts',(0.0134431846244391,-0.0336797586669775,
0.0713743987431874));
#83044=CARTESIAN_POINT('Ctrl Pts',(0.0134441724474163,-0.0336825812712343,
0.0713762927147142));
#83045=CARTESIAN_POINT('Ctrl Pts',(0.01344614599607,-0.0336882266015139,
0.0713800815695215));
#83046=CARTESIAN_POINT('Ctrl Pts',(0.0134471317217169,-0.0336910493274514,
0.0713819764527443));
#83047=CARTESIAN_POINT('Ctrl Pts',(0.0134481163985909,-0.0336938721132327,
0.0713838717910531));
#83048=CARTESIAN_POINT('Ctrl Pts',(0.01344219575284,-0.0336769361243754,
0.0713725052281485));
#83049=CARTESIAN_POINT('Ctrl Pts',(0.0134050433058289,-0.0336279007516236,
0.0713919077673034));
#83050=CARTESIAN_POINT('Ctrl Pts',(0.0133673618658974,-0.0335767878632084,
0.0714115865683656));
#83051=CARTESIAN_POINT('Ctrl Pts',(0.0132935168246351,-0.033473319885732,
0.0714501514926104));
#83052=CARTESIAN_POINT('Ctrl Pts',(0.0132573092600289,-0.0334209645014059,
0.0714690605752273));
#83053=CARTESIAN_POINT('Ctrl Pts',(0.0132217993964906,-0.0333679869844681,
0.0714876052895897));
#83054=CARTESIAN_POINT('',(0.0133874973821852,-0.0336938721132534,0.0715415874534452));
#83055=CARTESIAN_POINT('Origin',(0.00812378219310841,-0.0315241814719618,
0.07415));
#83056=CARTESIAN_POINT('',(0.0134421957516969,-0.0337108120655395,0.0713725052287529));
#83057=CARTESIAN_POINT('',(0.0134362508414152,-0.0336938721132327,0.0713611513377796));
#83058=CARTESIAN_POINT('Origin',(-0.00157777664322337,-0.0345562523507427,
0.0779557197821598));
#83059=CARTESIAN_POINT('Ctrl Pts',(0.0134362508414275,-0.0336938721132373,
0.07136115133778));
#83060=CARTESIAN_POINT('Ctrl Pts',(0.0134372436155188,-0.0336910493011037,
0.0713630424698828));
#83061=CARTESIAN_POINT('Ctrl Pts',(0.0134382354029273,-0.0336882265883395,
0.071364934176149));
#83062=CARTESIAN_POINT('Ctrl Pts',(0.0134402170357983,-0.0336825812712955,
0.0713687187977454));
#83063=CARTESIAN_POINT('Ctrl Pts',(0.0134412068812303,-0.0336797586670082,
0.0713706117130889));
#83064=CARTESIAN_POINT('Ctrl Pts',(0.01344219575284,-0.0336769361243754,
0.0713725052281484));
#83065=CARTESIAN_POINT('Origin',(-0.000543060617466345,-0.03455625200519,
0.0799370161395398));
#83066=CARTESIAN_POINT('Ctrl Pts',(0.013294403830978,-0.0342436276873909,
0.0716315090077599));
#83067=CARTESIAN_POINT('Ctrl Pts',(0.0131994173773341,-0.0339430054201809,
0.0714364957978541));
#83068=CARTESIAN_POINT('Ctrl Pts',(0.0130900115762353,-0.0336441434784052,
0.0712491913689167));
#83069=CARTESIAN_POINT('Ctrl Pts',(0.0131800710890971,-0.0342436276873909,
0.0714091848657195));
#83070=CARTESIAN_POINT('Ctrl Pts',(0.0130766995422061,-0.0339430054201809,
0.07121848378626));
#83071=CARTESIAN_POINT('Ctrl Pts',(0.0129592572763648,-0.0336441434784052,
0.0710361108370388));
#83072=CARTESIAN_POINT('Ctrl Pts',(0.0131789277616783,-0.0342436276873909,
0.071406961624299));
#83073=CARTESIAN_POINT('Ctrl Pts',(0.0130754723638549,-0.0339430054201809,
0.0712163036661441));
#83074=CARTESIAN_POINT('Ctrl Pts',(0.0129579497333661,-0.0336441434784052,
0.07103398003172));
#83075=CARTESIAN_POINT('',(0.0131627307134377,-0.0341934961088741,0.0713774338944811));
#83076=CARTESIAN_POINT('',(0.0130445664769882,-0.0338664212865394,0.0711727517674418));
#83077=CARTESIAN_POINT('Origin',(-0.00173801708148712,-0.0345610720403692,
0.0789945763319301));
#83078=CARTESIAN_POINT('Origin',(0.0224271245308364,-0.0336938005072992,
0.0654959279369191));
#83079=CARTESIAN_POINT('',(0.0131081116321623,-0.0336938721132327,0.0712804033309572));
#83080=CARTESIAN_POINT('',(0.0130757578824758,-0.0336938721132427,0.0712269291794493));
#83081=CARTESIAN_POINT('',(0.0132217993964931,-0.0340203938281605,0.0714876052895945));
#83082=CARTESIAN_POINT('Origin',(-0.00188836694114705,-0.0345589643244413,
0.078537485909832));
#83083=CARTESIAN_POINT('',(0.0132205951878513,-0.0341934961088739,0.0714882341769755));
#83084=CARTESIAN_POINT('Origin',(0.0229882585815279,-0.0341934220717601,
0.0663871587920726));
#83085=CARTESIAN_POINT('',(0.0131916629506545,-0.034193496108884,0.0714328340357383));
#83086=CARTESIAN_POINT('Ctrl Pts',(0.0135469776876582,-0.0340223579322396,
0.0715831048661921));
#83087=CARTESIAN_POINT('Ctrl Pts',(0.0135115735090194,-0.0339125849573575,
0.0715083048560346));
#83088=CARTESIAN_POINT('Ctrl Pts',(0.013474646022088,-0.0338030433565231,
0.0714342901912081));
#83089=CARTESIAN_POINT('Ctrl Pts',(0.0134362508414217,-0.0336938721132326,
0.0713611513377812));
#83090=CARTESIAN_POINT('Ctrl Pts',(0.0134381545698786,-0.0340223579322396,
0.071551502510783));
#83091=CARTESIAN_POINT('Ctrl Pts',(0.0134023145123364,-0.0339125849573575,
0.0714782034552423));
#83092=CARTESIAN_POINT('Ctrl Pts',(0.0133649825190614,-0.0338030433565231,
0.0714056977120096));
#83093=CARTESIAN_POINT('Ctrl Pts',(0.0133262145508509,-0.0336938721132326,
0.071334073771641));
#83094=CARTESIAN_POINT('Ctrl Pts',(0.0133293314520991,-0.0340223579322396,
0.0715199001553738));
#83095=CARTESIAN_POINT('Ctrl Pts',(0.0132930555156534,-0.0339125849573575,
0.0714481020544499));
#83096=CARTESIAN_POINT('Ctrl Pts',(0.0132553190160347,-0.0338030433565231,
0.071377105232811));
#83097=CARTESIAN_POINT('Ctrl Pts',(0.01321617826028,-0.0336938721132326,
0.0713069962055009));
#83098=CARTESIAN_POINT('Ctrl Pts',(0.0132205083343196,-0.0340223579322396,
0.0714882977999647));
#83099=CARTESIAN_POINT('Ctrl Pts',(0.0131837965189704,-0.0339125849573575,
0.0714180006536575));
#83100=CARTESIAN_POINT('Ctrl Pts',(0.0131456555130081,-0.0338030433565231,
0.0713485127536124));
#83101=CARTESIAN_POINT('Ctrl Pts',(0.0131061419697092,-0.0336938721132326,
0.0712799186393607));
#83102=CARTESIAN_POINT('',(0.0132721812367987,-0.0336938721132427,0.0713207773343784));
#83103=CARTESIAN_POINT('Ctrl Pts',(0.0134421957484976,-0.0337108120662676,
0.0713725052304164));
#83104=CARTESIAN_POINT('Ctrl Pts',(0.0134040811107114,-0.033761140899359,
0.071392410265253));
#83105=CARTESIAN_POINT('Ctrl Pts',(0.0133666619805022,-0.0338121088779862,
0.0714119520773659));
#83106=CARTESIAN_POINT('Ctrl Pts',(0.0132931806468089,-0.033915338277324,
0.0714503270585271));
#83107=CARTESIAN_POINT('Ctrl Pts',(0.0132571495305818,-0.0339675558473112,
0.0714691439925283));
#83108=CARTESIAN_POINT('Ctrl Pts',(0.0132217993964553,-0.0340203938281304,
0.0714876052896084));
#83109=CARTESIAN_POINT('Ctrl Pts',(0.0131621233843922,-0.0341934961088741,
0.0713793689741472));
#83110=CARTESIAN_POINT('Ctrl Pts',(0.0131048427706686,-0.0340287516182427,
0.0712752052392823));
#83111=CARTESIAN_POINT('Ctrl Pts',(0.0130433059359474,-0.0338644633275951,
0.0711734979615582));
#83112=CARTESIAN_POINT('Ctrl Pts',(0.0131627307134377,-0.0341934961088741,
0.0713774338944813));
#83113=CARTESIAN_POINT('Ctrl Pts',(0.0131054100934665,-0.0340287516182427,
0.0712732576035668));
#83114=CARTESIAN_POINT('Ctrl Pts',(0.0130438327677312,-0.0338644633275951,
0.0711715394340106));
#83115=CARTESIAN_POINT('Ctrl Pts',(0.0132639234139404,-0.0341934961088741,
0.0710550124023017));
#83116=CARTESIAN_POINT('Ctrl Pts',(0.0131999369836259,-0.0340287516182427,
0.0709487440320251));
#83117=CARTESIAN_POINT('Ctrl Pts',(0.0131316130761275,-0.0338644633275951,
0.0708452110737472));
#83118=CARTESIAN_POINT('',(0.0132573007386171,-0.0341764758832421,0.0710440400302624));
#83119=CARTESIAN_POINT('',(0.0132639234139403,-0.034193496108874,0.0710550124023019));
#83120=CARTESIAN_POINT('Origin',(-0.00117437858495977,-0.0345621027089467,
0.0791771798535414));
#83121=CARTESIAN_POINT('Ctrl Pts',(0.013257300738701,-0.0341764758837522,
0.0710440400320756));
#83122=CARTESIAN_POINT('Ctrl Pts',(0.0132205752309949,-0.0341260050040497,
0.0710662602769656));
#83123=CARTESIAN_POINT('Ctrl Pts',(0.013184488119031,-0.0340749269148259,
0.0710880943142688));
#83124=CARTESIAN_POINT('Ctrl Pts',(0.0131135626237488,-0.0339715436306283,
0.071131006738375));
#83125=CARTESIAN_POINT('Ctrl Pts',(0.01307875114497,-0.033919277823851,
0.071152068839989));
#83126=CARTESIAN_POINT('Ctrl Pts',(0.0130445664784764,-0.0338664212857068,
0.0711727517677738));
#83127=CARTESIAN_POINT('',(0.013213327063699,-0.0341934961088841,0.0712162231484015));
#83128=CARTESIAN_POINT('Origin',(0.00812378219310841,-0.0315241814719618,
0.07415));
#83129=CARTESIAN_POINT('',(0.0132573007375502,-0.0342105180190539,0.0710440400299246));
#83130=CARTESIAN_POINT('',(0.0132506546416664,-0.0341934961088739,0.0710330818271522));
#83131=CARTESIAN_POINT('Origin',(-0.00115554781581669,-0.0345621715476278,
0.0792184088855479));
#83132=CARTESIAN_POINT('Origin',(-0.000644192738700177,-0.0345621032405993,
0.0800534709426069));
#83133=CARTESIAN_POINT('Origin',(-0.000671972938710301,-0.0345621721347048,
0.0800176567189358));
#83134=CARTESIAN_POINT('Ctrl Pts',(0.0131088881272831,-0.0346945769586966,
0.0712816867190697));
#83135=CARTESIAN_POINT('Ctrl Pts',(0.013048810157204,-0.0345275153362944,
0.0711772716793509));
#83136=CARTESIAN_POINT('Ctrl Pts',(0.0129854328909929,-0.0343603235965185,
0.0710747190294156));
#83137=CARTESIAN_POINT('Ctrl Pts',(0.0129189482783755,-0.034193496108874,
0.0709743292886055));
#83138=CARTESIAN_POINT('Ctrl Pts',(0.0130654909626485,-0.0346945769586966,
0.0712099600543431));
#83139=CARTESIAN_POINT('Ctrl Pts',(0.0130039106488589,-0.0345275153362944,
0.0711064539856128));
#83140=CARTESIAN_POINT('Ctrl Pts',(0.0129390592366552,-0.0343603235965185,
0.0710048577890994));
#83141=CARTESIAN_POINT('Ctrl Pts',(0.0128711329935898,-0.034193496108874,
0.0709054690905808));
#83142=CARTESIAN_POINT('Ctrl Pts',(0.0130220937980139,-0.0346945769586966,
0.0711382333896164));
#83143=CARTESIAN_POINT('Ctrl Pts',(0.0129590111405138,-0.0345275153362944,
0.0710356362918747));
#83144=CARTESIAN_POINT('Ctrl Pts',(0.0128926855823176,-0.0343603235965185,
0.0709349965487832));
#83145=CARTESIAN_POINT('Ctrl Pts',(0.0128233177088041,-0.034193496108874,
0.0708366088925562));
#83146=CARTESIAN_POINT('Ctrl Pts',(0.0129786966333793,-0.0346945769586966,
0.0710665067248898));
#83147=CARTESIAN_POINT('Ctrl Pts',(0.0129141116321687,-0.0345275153362944,
0.0709648185981367));
#83148=CARTESIAN_POINT('Ctrl Pts',(0.0128463119279799,-0.0343603235965185,
0.0708651353084671));
#83149=CARTESIAN_POINT('Ctrl Pts',(0.0127755024240184,-0.034193496108874,
0.0707677486945316));
#83150=CARTESIAN_POINT('',(0.0129786966333732,-0.0346945769586966,0.0710665067248801));
#83151=CARTESIAN_POINT('',(0.0128479134699673,-0.0343667727831647,0.0708696480860459));
#83152=CARTESIAN_POINT('Origin',(-0.00111529414379012,-0.0345626457065037,
0.0802347492617079));
#83153=CARTESIAN_POINT('Origin',(0.021926103880993,-0.0341934771029166,
0.064565910045707));
#83154=CARTESIAN_POINT('',(0.0129180927308873,-0.034193496108874,0.0709730971895031));
#83155=CARTESIAN_POINT('',(0.0128824451541801,-0.034193496108884,0.0709217600657703));
#83156=CARTESIAN_POINT('',(0.013044566477013,-0.034521194296265,0.0711727517686283));
#83157=CARTESIAN_POINT('Origin',(-0.0013613467526906,-0.0345625596120561,
0.0798216525375073));
#83158=CARTESIAN_POINT('',(0.0130434041327692,-0.0346945769586885,0.0711734550279211));
#83159=CARTESIAN_POINT('Origin',(0.0225092423963709,-0.034694568585389,
0.065446289832958));
#83160=CARTESIAN_POINT('',(0.0130110503830812,-0.0346945769587025,0.0711199808764106));
#83161=CARTESIAN_POINT('Ctrl Pts',(0.0133750991057015,-0.0345231616327841,
0.0712476439426601));
#83162=CARTESIAN_POINT('Ctrl Pts',(0.0133350942136416,-0.0344132092796988,
0.0711752619322828));
#83163=CARTESIAN_POINT('Ctrl Pts',(0.0132935942208596,-0.0343032738558979,
0.0711037111261214));
#83164=CARTESIAN_POINT('Ctrl Pts',(0.0132506546416721,-0.0341934961088739,
0.0710330818271533));
#83165=CARTESIAN_POINT('Ctrl Pts',(0.0132645065813549,-0.0345231616327841,
0.07122293706715));
#83166=CARTESIAN_POINT('Ctrl Pts',(0.0132241611398005,-0.0344132092796988,
0.071152079419019));
#83167=CARTESIAN_POINT('Ctrl Pts',(0.0131823521453256,-0.0343032738558979,
0.0710820599404515));
#83168=CARTESIAN_POINT('Ctrl Pts',(0.0131391354578611,-0.0341934961088739,
0.0710129669624769));
#83169=CARTESIAN_POINT('Ctrl Pts',(0.0131539140570083,-0.0345231616327841,
0.0711982301916399));
#83170=CARTESIAN_POINT('Ctrl Pts',(0.0131132280659595,-0.0344132092796988,
0.0711288969057552));
#83171=CARTESIAN_POINT('Ctrl Pts',(0.0130711100697917,-0.0343032738558979,
0.0710604087547815));
#83172=CARTESIAN_POINT('Ctrl Pts',(0.0130276162740501,-0.0341934961088739,
0.0709928520978005));
#83173=CARTESIAN_POINT('Ctrl Pts',(0.0130433215326617,-0.0345231616327841,
0.0711735233161298));
#83174=CARTESIAN_POINT('Ctrl Pts',(0.0130022949921185,-0.0344132092796988,
0.0711057143924914));
#83175=CARTESIAN_POINT('Ctrl Pts',(0.0129598679942577,-0.0343032738558979,
0.0710387575691116));
#83176=CARTESIAN_POINT('Ctrl Pts',(0.012916097090239,-0.0341934961088739,
0.0709727372331242));
#83177=CARTESIAN_POINT('',(0.0130843736862868,-0.0341934961088839,0.0710030895083377));
#83178=CARTESIAN_POINT('Ctrl Pts',(0.0132573007345886,-0.0342105180195382,
0.0710440400317084));
#83179=CARTESIAN_POINT('Ctrl Pts',(0.0132205339332162,-0.034261055624049,
0.0710662852446752));
#83180=CARTESIAN_POINT('Ctrl Pts',(0.013184426893082,-0.0343122189868487,
0.0710881312787986));
#83181=CARTESIAN_POINT('Ctrl Pts',(0.0131135006843536,-0.0344158119695131,
0.0711310441392924));
#83182=CARTESIAN_POINT('Ctrl Pts',(0.0130787105252643,-0.0344681990450021,
0.0711520934138882));
#83183=CARTESIAN_POINT('Ctrl Pts',(0.0130445664769814,-0.0345211942962426,
0.0711727517686336));
#83184=CARTESIAN_POINT('Ctrl Pts',(0.0129782121260746,-0.0346945769586932,
0.0710684756384207));
#83185=CARTESIAN_POINT('Ctrl Pts',(0.0129357471627973,-0.034584662917547,
0.071001579140244));
#83186=CARTESIAN_POINT('Ctrl Pts',(0.0128918915542897,-0.0344746925049099,
0.0709355493739828));
#83187=CARTESIAN_POINT('Ctrl Pts',(0.0128467018428174,-0.034364806625142,
0.070870470712514));
#83188=CARTESIAN_POINT('Ctrl Pts',(0.0130052896307832,-0.0346945769586932,
0.0709584395974925));
#83189=CARTESIAN_POINT('Ctrl Pts',(0.0129613083152435,-0.034584662917547,
0.0708911699576144));
#83190=CARTESIAN_POINT('Ctrl Pts',(0.0129159283790597,-0.0344746925049099,
0.0708247983434604));
#83191=CARTESIAN_POINT('Ctrl Pts',(0.0128692083194506,-0.034364806625142,
0.0707594095578561));
#83192=CARTESIAN_POINT('Ctrl Pts',(0.0130323671354917,-0.0346945769586932,
0.0708484035565642));
#83193=CARTESIAN_POINT('Ctrl Pts',(0.0129868694676897,-0.034584662917547,
0.0707807607749848));
#83194=CARTESIAN_POINT('Ctrl Pts',(0.0129399652038296,-0.0344746925049099,
0.070714047312938));
#83195=CARTESIAN_POINT('Ctrl Pts',(0.0128917147960837,-0.034364806625142,
0.0706483484031981));
#83196=CARTESIAN_POINT('Ctrl Pts',(0.0130594446402003,-0.0346945769586932,
0.070738367515636));
#83197=CARTESIAN_POINT('Ctrl Pts',(0.0130124306201359,-0.034584662917547,
0.0706703515923552));
#83198=CARTESIAN_POINT('Ctrl Pts',(0.0129640020285996,-0.0344746925049099,
0.0706032962824155));
#83199=CARTESIAN_POINT('Ctrl Pts',(0.0129142212727169,-0.034364806625142,
0.0705372872485401));
#83200=CARTESIAN_POINT('',(0.0130521460711012,-0.034677539666344,0.0707278326360764));
#83201=CARTESIAN_POINT('',(0.0130594446401983,-0.0346945769586886,0.0707383675156333));
#83202=CARTESIAN_POINT('Origin',(-0.000496621982559035,-0.0345626618638833,
0.0803217779571767));
#83203=CARTESIAN_POINT('Ctrl Pts',(0.0130521460683195,-0.0346775396659408,
0.0707278326379988));
#83204=CARTESIAN_POINT('Ctrl Pts',(0.013016860365398,-0.0346269748528212,
0.0707523343963796));
#83205=CARTESIAN_POINT('Ctrl Pts',(0.0129822020560721,-0.0345757904815282,
0.0707764005039156));
#83206=CARTESIAN_POINT('Ctrl Pts',(0.0129141105025331,-0.0344721679344067,
0.0708236820557754));
#83207=CARTESIAN_POINT('Ctrl Pts',(0.0128807046965108,-0.0344197716859604,
0.0708468784475121));
#83208=CARTESIAN_POINT('Ctrl Pts',(0.0128479134701608,-0.0343667727830949,
0.0708696480861622));
#83209=CARTESIAN_POINT('',(0.0130190706367957,-0.0346945769587026,0.0709024371202667));
#83210=CARTESIAN_POINT('Origin',(0.00812378219310841,-0.0315241814719618,
0.07415));
#83211=CARTESIAN_POINT('',(0.0130521460710122,-0.0347116136489614,0.0707278326361377));
#83212=CARTESIAN_POINT('',(0.0130448250186084,-0.0346945769586885,0.0707173133685687));
#83213=CARTESIAN_POINT('Origin',(-0.00046926371922708,-0.0345626696275047,
0.0803578983563592));
#83214=CARTESIAN_POINT('Origin',(-0.000670830339955459,-0.0345626623641555,
0.0800708976830043));
#83215=CARTESIAN_POINT('Origin',(-0.000695114068535318,-0.0345626701139946,
0.0800326423598664));
#83216=CARTESIAN_POINT('Ctrl Pts',(0.012939365481435,-0.0352450361874067,
0.0710053346412036));
#83217=CARTESIAN_POINT('Ctrl Pts',(0.0128207624812432,-0.0349452760959492,
0.0708237119371942));
#83218=CARTESIAN_POINT('Ctrl Pts',(0.0126888158544847,-0.034644428984174,
0.0706515388674267));
#83219=CARTESIAN_POINT('Ctrl Pts',(0.012937938365447,-0.0352450361874067,
0.0710032516229711));
#83220=CARTESIAN_POINT('Ctrl Pts',(0.0128192568029334,-0.0349452760959492,
0.0708216827435245));
#83221=CARTESIAN_POINT('Ctrl Pts',(0.0126872358913267,-0.034644428984174,
0.0706495692630452));
#83222=CARTESIAN_POINT('Ctrl Pts',(0.0127966397527728,-0.0352450361874067,
0.0707970121940144));
#83223=CARTESIAN_POINT('Ctrl Pts',(0.0126701797425577,-0.0349452760959492,
0.0706207724791924));
#83224=CARTESIAN_POINT('Ctrl Pts',(0.0125308038954853,-0.034644428984174,
0.0704545589282497));
#83225=CARTESIAN_POINT('Ctrl Pts',(0.012795226766646,-0.0352450361874067,
0.0707949497997249));
#83226=CARTESIAN_POINT('Ctrl Pts',(0.012668688971954,-0.0349452760959492,
0.0706187633765491));
#83227=CARTESIAN_POINT('Ctrl Pts',(0.0125292395755269,-0.034644428984174,
0.0704526088249018));
#83228=CARTESIAN_POINT('',(0.0127755233731481,-0.0351951634053348,0.0707677734705648));
#83229=CARTESIAN_POINT('',(0.0126326164752035,-0.0348678972925388,0.0705794904542061));
#83230=CARTESIAN_POINT('Origin',(-0.000236095645883816,-0.0345636767883841,
0.0813082794769825));
#83231=CARTESIAN_POINT('Origin',(0.0212952490697888,-0.0346946199340833,
0.0637196226839455));
#83232=CARTESIAN_POINT('',(0.0127091528869729,-0.0346945769330288,0.0706783288465125));
#83233=CARTESIAN_POINT('',(0.0126703521628121,-0.0346945769458128,0.0706293313476771));
#83234=CARTESIAN_POINT('',(0.0128479134700692,-0.0350221583435276,0.0708696480862502));
#83235=CARTESIAN_POINT('Origin',(-0.000565974147668837,-0.0345628458717359,
0.080958531614612));
#83236=CARTESIAN_POINT('',(0.0128468992255452,-0.035195136029876,0.0708703560416109));
#83237=CARTESIAN_POINT('Origin',(0.0218978191987488,-0.0351951838366798,
0.0645855575956237));
#83238=CARTESIAN_POINT('',(0.0127755024241135,-0.0351951371328748,0.0707677486944647));
#83239=CARTESIAN_POINT('Ctrl Pts',(0.0131824958700217,-0.0350241211494342,
0.0709236373522079));
#83240=CARTESIAN_POINT('Ctrl Pts',(0.0131380540474086,-0.0349144232818962,
0.0708539556454617));
#83241=CARTESIAN_POINT('Ctrl Pts',(0.0130921452535521,-0.0348045283579412,
0.0707851508750852));
#83242=CARTESIAN_POINT('Ctrl Pts',(0.0130448250122557,-0.0346945769439158,
0.0707173133594548));
#83243=CARTESIAN_POINT('Ctrl Pts',(0.0130705701896879,-0.0350241211494342,
0.0709059234061471));
#83244=CARTESIAN_POINT('Ctrl Pts',(0.0130258843647308,-0.0349144232818962,
0.0708377834297562));
#83245=CARTESIAN_POINT('Ctrl Pts',(0.0129797632911513,-0.0348045283579412,
0.0707705263562377));
#83246=CARTESIAN_POINT('Ctrl Pts',(0.0129322628384259,-0.0346945769439158,
0.0707042405316832));
#83247=CARTESIAN_POINT('Ctrl Pts',(0.0129586445093541,-0.0350241211494342,
0.0708882094600864));
#83248=CARTESIAN_POINT('Ctrl Pts',(0.012913714682053,-0.0349144232818962,
0.0708216112140508));
#83249=CARTESIAN_POINT('Ctrl Pts',(0.0128673813287505,-0.0348045283579412,
0.0707559018373903));
#83250=CARTESIAN_POINT('Ctrl Pts',(0.0128197006645961,-0.0346945769439158,
0.0706911677039117));
#83251=CARTESIAN_POINT('Ctrl Pts',(0.0128467188290203,-0.0350241211494342,
0.0708704955140256));
#83252=CARTESIAN_POINT('Ctrl Pts',(0.0128015449993752,-0.0349144232818962,
0.0708054389983453));
#83253=CARTESIAN_POINT('Ctrl Pts',(0.0127549993663496,-0.0348045283579412,
0.0707412773185428));
#83254=CARTESIAN_POINT('Ctrl Pts',(0.0127071384907663,-0.0346945769439158,
0.0706780948761401));
#83255=CARTESIAN_POINT('',(0.0128769889530388,-0.0346945769458128,0.0706978211077288));
#83256=CARTESIAN_POINT('Ctrl Pts',(0.0130521460683053,-0.0347116136492791,
0.0707278326380088));
#83257=CARTESIAN_POINT('Ctrl Pts',(0.0130168744869824,-0.034762154653151,
0.0707523245906052));
#83258=CARTESIAN_POINT('Ctrl Pts',(0.0129822230753714,-0.0348133084095402,
0.0707763859084918));
#83259=CARTESIAN_POINT('Ctrl Pts',(0.0129141316724007,-0.0349168561544574,
0.0708236673557995));
#83260=CARTESIAN_POINT('Ctrl Pts',(0.0128807186896037,-0.034969208901592,
0.0708468687309598));
#83261=CARTESIAN_POINT('Ctrl Pts',(0.0128479134700278,-0.0350221583435,
0.0708696480862548));
#83262=CARTESIAN_POINT('Ctrl Pts',(0.0127752427282663,-0.0351951371254977,
0.0707691884784717));
#83263=CARTESIAN_POINT('Ctrl Pts',(0.0127053465712501,-0.0350307338980969,
0.0706730224503303));
#83264=CARTESIAN_POINT('Ctrl Pts',(0.0126315354943806,-0.0348659306897816,
0.0705798274790847));
#83265=CARTESIAN_POINT('Ctrl Pts',(0.0127755024240242,-0.0351951371254977,
0.0707677486945395));
#83266=CARTESIAN_POINT('Ctrl Pts',(0.0127055765003785,-0.0350307338980969,
0.0706715772973513));
#83267=CARTESIAN_POINT('Ctrl Pts',(0.0126317354604065,-0.0348659306897816,
0.0705783781919335));
#83268=CARTESIAN_POINT('Ctrl Pts',(0.012819027703724,-0.0351951371254977,
0.0705264394068399));
#83269=CARTESIAN_POINT('Ctrl Pts',(0.0127441128619576,-0.0350307338980969,
0.0704293681518025));
#83270=CARTESIAN_POINT('Ctrl Pts',(0.0126652499747703,-0.0348659306897816,
0.070335476154828));
#83271=CARTESIAN_POINT('Origin',(0.0168018575233885,-0.0308609197410378,
0.0672779020548871));
#83272=CARTESIAN_POINT('',(0.0127944784646092,-0.0351951371254977,0.0706625432859009));
#83273=CARTESIAN_POINT('Origin',(0.00745373953934053,-0.0351840467441105,
0.0748611880852274));
#83274=CARTESIAN_POINT('Origin',(0.0169900980219168,-0.0352322613677157,
0.0661151297357092));
#83275=CARTESIAN_POINT('',(0.012481890919325,-0.0351951142564676,0.0703970407790791));
#83276=CARTESIAN_POINT('',(0.0123985151563521,-0.0351951372916788,0.0703043325555947));
#83277=CARTESIAN_POINT('Origin',(0.00779709879998335,-0.0352875117969581,
0.0740537454871082));
#83278=CARTESIAN_POINT('Origin',(0.0119810545394734,-0.029832507652371,
0.0805855761454313));
#83279=CARTESIAN_POINT('Origin',(0.0160064406244031,-0.0338733155346509,
0.0713020587946091));
#83280=CARTESIAN_POINT('Ctrl Pts',(0.0138555576184494,-0.0321934096636942,
0.0736757783020904));
#83281=CARTESIAN_POINT('Ctrl Pts',(0.0138470692758913,-0.0320508460845456,
0.0735731822515703));
#83282=CARTESIAN_POINT('Ctrl Pts',(0.0138358307801348,-0.0319086045665327,
0.0734708916238262));
#83283=CARTESIAN_POINT('Ctrl Pts',(0.01382188446196,-0.0317669892871269,
0.0733691246764067));
#83284=CARTESIAN_POINT('Ctrl Pts',(0.013846828925717,-0.0321934096636942,
0.0735923862008404));
#83285=CARTESIAN_POINT('Ctrl Pts',(0.0138368479042596,-0.0320508460845456,
0.0734899463897633));
#83286=CARTESIAN_POINT('Ctrl Pts',(0.0138241220529342,-0.0319086045665327,
0.073387851988994));
#83287=CARTESIAN_POINT('Ctrl Pts',(0.0138086968702754,-0.0317669892871269,
0.0732863205699169));
#83288=CARTESIAN_POINT('Ctrl Pts',(0.0138381002329847,-0.0321934096636942,
0.0735089940995902));
#83289=CARTESIAN_POINT('Ctrl Pts',(0.013826626532628,-0.0320508460845456,
0.0734067105279564));
#83290=CARTESIAN_POINT('Ctrl Pts',(0.0138124133257338,-0.0319086045665327,
0.0733048123541618));
#83291=CARTESIAN_POINT('Ctrl Pts',(0.0137955092785906,-0.0317669892871269,
0.0732035164634271));
#83292=CARTESIAN_POINT('Ctrl Pts',(0.0138293715402524,-0.0321934096636942,
0.0734256019983401));
#83293=CARTESIAN_POINT('Ctrl Pts',(0.0138164051609964,-0.0320508460845456,
0.0733234746661493));
#83294=CARTESIAN_POINT('Ctrl Pts',(0.0138007045985332,-0.0319086045665327,
0.0732217727193296));
#83295=CARTESIAN_POINT('Ctrl Pts',(0.013782321686906,-0.0317669892871269,
0.0731207123569373));
#83296=CARTESIAN_POINT('',(0.0138295276982879,-0.0321934096636942,0.0734270938995109));
#83297=CARTESIAN_POINT('',(0.0137950098848978,-0.0318665617511339,0.0731932861153394));
#83298=CARTESIAN_POINT('Origin',(-0.00281382859954108,-0.0326371944419269,
0.0749159175898794));
#83299=CARTESIAN_POINT('Origin',(0.0246034787141099,-0.0316939261509209,
0.0713699398195629));
#83300=CARTESIAN_POINT('',(0.0138438177375588,-0.0320197221621814,0.0735510154119181));
#83301=CARTESIAN_POINT('Ctrl Pts',(0.0138438460363689,-0.0320197392094725,
0.0735508326167958));
#83302=CARTESIAN_POINT('Ctrl Pts',(0.0138407972334113,-0.0319792716576023,
0.0735217270978981));
#83303=CARTESIAN_POINT('Ctrl Pts',(0.013837512662381,-0.0319386439829719,
0.0734925123224487));
#83304=CARTESIAN_POINT('Ctrl Pts',(0.0138339804705309,-0.0318979099381651,
0.0734631585653704));
#83305=CARTESIAN_POINT('Ctrl Pts',(0.013830448348497,-0.0318571766984956,
0.07343380538849));
#83306=CARTESIAN_POINT('Ctrl Pts',(0.0138266883369074,-0.0318163871833607,
0.0734044622146292));
#83307=CARTESIAN_POINT('Ctrl Pts',(0.0138227168612495,-0.0317755399638304,
0.0733752295246743));
#83308=CARTESIAN_POINT('',(0.0138425404215422,-0.0321934096636182,0.0735514147306182));
#83309=CARTESIAN_POINT('Origin',(0.0161356974395084,-0.0324112133758613,
0.0732902449803353));
#83310=CARTESIAN_POINT('',(0.0138360340599251,-0.0321934096636661,0.0734892543150745));
#83311=CARTESIAN_POINT('Ctrl Pts',(0.0138282506203132,-0.0321934096636618,
0.0734286695768972));
#83312=CARTESIAN_POINT('Ctrl Pts',(0.0138183029116065,-0.0320835708272592,
0.0733500005114833));
#83313=CARTESIAN_POINT('Ctrl Pts',(0.0138067329207551,-0.0319739230346489,
0.0732715829446392));
#83314=CARTESIAN_POINT('Ctrl Pts',(0.0137935631507942,-0.0318646057455573,
0.0731935160701121));
#83315=CARTESIAN_POINT('Ctrl Pts',(0.0138996022666618,-0.0321934096636618,
0.0733406348830072));
#83316=CARTESIAN_POINT('Ctrl Pts',(0.0138884404909162,-0.0320835708272592,
0.073260981822782));
#83317=CARTESIAN_POINT('Ctrl Pts',(0.0138756367735125,-0.0319739230346489,
0.0731816059569377));
#83318=CARTESIAN_POINT('Ctrl Pts',(0.0138612152900516,-0.0318646057455573,
0.0731026075841559));
#83319=CARTESIAN_POINT('Ctrl Pts',(0.0139709539130104,-0.0321934096636618,
0.0732526001891172));
#83320=CARTESIAN_POINT('Ctrl Pts',(0.0139585780702258,-0.0320835708272592,
0.0731719631340806));
#83321=CARTESIAN_POINT('Ctrl Pts',(0.0139445406262699,-0.0319739230346489,
0.0730916289692363));
#83322=CARTESIAN_POINT('Ctrl Pts',(0.0139288674293091,-0.0318646057455573,
0.0730116990981997));
#83323=CARTESIAN_POINT('Ctrl Pts',(0.014042305559359,-0.0321934096636618,
0.0731645654952272));
#83324=CARTESIAN_POINT('Ctrl Pts',(0.0140287156495354,-0.0320835708272592,
0.0730829444453793));
#83325=CARTESIAN_POINT('Ctrl Pts',(0.0140134444790273,-0.0319739230346489,
0.0730016519815349));
#83326=CARTESIAN_POINT('Ctrl Pts',(0.0139965195685665,-0.0318646057455573,
0.0729207906122435));
#83327=CARTESIAN_POINT('',(0.0140401871499127,-0.0321763980308293,0.0731519256716395));
#83328=CARTESIAN_POINT('',(0.01404230555935,-0.0321934096636184,0.0731645654951994));
#83329=CARTESIAN_POINT('Origin',(-0.00236778886702764,-0.0326386231555595,
0.075297715851378));
#83330=CARTESIAN_POINT('Ctrl Pts',(0.0140401871467773,-0.0321763980306311,
0.0731519256721621));
#83331=CARTESIAN_POINT('Ctrl Pts',(0.0139978662211999,-0.0321259596175317,
0.0731590650464409));
#83332=CARTESIAN_POINT('Ctrl Pts',(0.0139562785605731,-0.0320749164632375,
0.0731660807218032));
#83333=CARTESIAN_POINT('Ctrl Pts',(0.0138745363006747,-0.031971605779399,
0.0731798703206801));
#83334=CARTESIAN_POINT('Ctrl Pts',(0.0138344135510431,-0.0319193786690198,
0.0731866388712851));
#83335=CARTESIAN_POINT('Ctrl Pts',(0.0137950098830636,-0.0318665617525401,
0.0731932861156406));
#83336=CARTESIAN_POINT('',(0.013935916628829,-0.0321934096636663,0.0732958296973652));
#83337=CARTESIAN_POINT('Origin',(0.00812378219310841,-0.0315241814719618,
0.07415));
#83338=CARTESIAN_POINT('',(0.0140401871502783,-0.0322104233323598,0.0731519256715778));
#83339=CARTESIAN_POINT('',(0.0140380417500605,-0.0321934096636183,0.0731392904012454));
#83340=CARTESIAN_POINT('Origin',(-0.00236654846093717,-0.0326387242423214,
0.0753430317953394));
#83341=CARTESIAN_POINT('Origin',(-0.00216368296648192,-0.032638623759595,
0.0765076269337747));
#83342=CARTESIAN_POINT('Origin',(-0.0021773745728056,-0.0326387247245503,
0.0764644112947523));
#83343=CARTESIAN_POINT('Ctrl Pts',(0.0138195875023524,-0.0327445246967096,
0.0733525497638174));
#83344=CARTESIAN_POINT('Ctrl Pts',(0.0137895111750135,-0.0324436878339359,
0.0731377289547349));
#83345=CARTESIAN_POINT('Ctrl Pts',(0.0137433391100204,-0.0321434074405927,
0.0729257839007813));
#83346=CARTESIAN_POINT('Ctrl Pts',(0.0137795511148478,-0.0327445246967096,
0.0731057764109699));
#83347=CARTESIAN_POINT('Ctrl Pts',(0.0137401675783539,-0.0324436878339359,
0.0728924655989273));
#83348=CARTESIAN_POINT('Ctrl Pts',(0.0136848284841527,-0.0321434074405927,
0.072682727309304));
#83349=CARTESIAN_POINT('',(0.0137728770632765,-0.0326943950436612,0.0730702536650482));
#83350=CARTESIAN_POINT('',(0.0137237464515687,-0.0323666188837389,0.0728390746382923));
#83351=CARTESIAN_POINT('Origin',(-0.00272472285463082,-0.0326395579110699,
0.0763009277693971));
#83352=CARTESIAN_POINT('Origin',(0.0244776248529026,-0.0321933825603003,
0.0703216411890648));
#83353=CARTESIAN_POINT('',(0.0137509153243003,-0.0321934096532689,0.0729610938974545));
#83354=CARTESIAN_POINT('',(0.0137366695011081,-0.0321934096584275,0.0729002390959408));
#83355=CARTESIAN_POINT('',(0.0137950098858213,-0.0325210109756239,0.07319328611518));
#83356=CARTESIAN_POINT('Origin',(-0.00278993997179763,-0.0326393129160773,
0.0758245548504547));
#83357=CARTESIAN_POINT('',(0.0137936702784574,-0.0326943950436593,0.0731935121016875));
#83358=CARTESIAN_POINT('Origin',(0.0247019979769415,-0.0326943765538214,
0.0713533209336769));
#83359=CARTESIAN_POINT('',(0.0137832736708769,-0.0326943950436702,0.0731318828833779));
#83360=CARTESIAN_POINT('Ctrl Pts',(0.0140747617225964,-0.0325229783203769,
0.0733845964203715));
#83361=CARTESIAN_POINT('Ctrl Pts',(0.0140642106509895,-0.032413025309245,
0.0733025622976969));
#83362=CARTESIAN_POINT('Ctrl Pts',(0.0140519641984515,-0.0323031222208069,
0.0732207588795742));
#83363=CARTESIAN_POINT('Ctrl Pts',(0.0140380417493126,-0.0321934096576658,
0.0731392903968298));
#83364=CARTESIAN_POINT('Ctrl Pts',(0.0139810305807535,-0.0325229783203769,
0.0733209127074952));
#83365=CARTESIAN_POINT('Ctrl Pts',(0.0139696016305573,-0.032413025309245,
0.0732401706665611));
#83366=CARTESIAN_POINT('Ctrl Pts',(0.0139565041609481,-0.0323031222208069,
0.0731596772942558));
#83367=CARTESIAN_POINT('Ctrl Pts',(0.0139417585871346,-0.0321934096576658,
0.0730795351048643));
#83368=CARTESIAN_POINT('Ctrl Pts',(0.0138872994389107,-0.0325229783203769,
0.0732572289946189));
#83369=CARTESIAN_POINT('Ctrl Pts',(0.0138749926101251,-0.032413025309245,
0.0731777790354253));
#83370=CARTESIAN_POINT('Ctrl Pts',(0.0138610441234446,-0.0323031222208069,
0.0730985957089374));
#83371=CARTESIAN_POINT('Ctrl Pts',(0.0138454754249566,-0.0321934096576658,
0.0730197798128988));
#83372=CARTESIAN_POINT('Ctrl Pts',(0.0137935682970678,-0.0325229783203769,
0.0731935452817426));
#83373=CARTESIAN_POINT('Ctrl Pts',(0.0137803835896929,-0.032413025309245,
0.0731153874042896));
#83374=CARTESIAN_POINT('Ctrl Pts',(0.0137655840859412,-0.0323031222208069,
0.073037514123619));
#83375=CARTESIAN_POINT('Ctrl Pts',(0.0137491922627787,-0.0321934096576658,
0.0729600245209332));
#83376=CARTESIAN_POINT('',(0.0138944785374258,-0.0321934096584275,0.0730501921498067));
#83377=CARTESIAN_POINT('Ctrl Pts',(0.0140401871468428,-0.0322104233328898,
0.0731519256721512));
#83378=CARTESIAN_POINT('Ctrl Pts',(0.0139978088757692,-0.0322609421830383,
0.0731590747203904));
#83379=CARTESIAN_POINT('Ctrl Pts',(0.013956193200933,-0.0323120888238738,
0.0731660951216333));
#83380=CARTESIAN_POINT('Ctrl Pts',(0.0138744503220553,-0.032415652463181,
0.0731798848249295));
#83381=CARTESIAN_POINT('Ctrl Pts',(0.0138343567188523,-0.0324680267167321,
0.0731866484586531));
#83382=CARTESIAN_POINT('Ctrl Pts',(0.0137950098857779,-0.0325210109755913,
0.0731932861151829));
#83383=CARTESIAN_POINT('Origin',(0.00848867654725678,-0.0262834582511018,
0.0820094044272593));
#83384=CARTESIAN_POINT('Origin',(0.0197508774515317,-0.0342771005519637,
0.0777046541217103));
#83385=CARTESIAN_POINT('Ctrl Pts',(0.0137717017281994,-0.0326943950436604,
0.0730719060204244));
#83386=CARTESIAN_POINT('Ctrl Pts',(0.0137568435725974,-0.0325844576448134,
0.0729940671039015));
#83387=CARTESIAN_POINT('Ctrl Pts',(0.0137403745290482,-0.0324744968375322,
0.0729165299696155));
#83388=CARTESIAN_POINT('Ctrl Pts',(0.0137223170689186,-0.0323646534831894,
0.0728393936716174));
#83389=CARTESIAN_POINT('Ctrl Pts',(0.0138373847391094,-0.0326943950436604,
0.0729795649696422));
#83390=CARTESIAN_POINT('Ctrl Pts',(0.013821253950762,-0.0325844576448134,
0.0729008208181258));
#83391=CARTESIAN_POINT('Ctrl Pts',(0.0138034934626575,-0.0324744968375322,
0.0728224047049132));
#83392=CARTESIAN_POINT('Ctrl Pts',(0.0137841274163702,-0.0323646534831894,
0.0727444167874314));
#83393=CARTESIAN_POINT('Ctrl Pts',(0.0139030677500193,-0.0326943950436604,
0.0728872239188599));
#83394=CARTESIAN_POINT('Ctrl Pts',(0.0138856643289266,-0.0325844576448134,
0.0728075745323501));
#83395=CARTESIAN_POINT('Ctrl Pts',(0.0138666123962667,-0.0324744968375322,
0.072728279440211));
#83396=CARTESIAN_POINT('Ctrl Pts',(0.0138459377638218,-0.0323646534831894,
0.0726494399032454));
#83397=CARTESIAN_POINT('Ctrl Pts',(0.0139687507609293,-0.0326943950436604,
0.0727948828680776));
#83398=CARTESIAN_POINT('Ctrl Pts',(0.0139500747070912,-0.0325844576448134,
0.0727143282465744));
#83399=CARTESIAN_POINT('Ctrl Pts',(0.0139297313298759,-0.0324744968375322,
0.0726341541755087));
#83400=CARTESIAN_POINT('Ctrl Pts',(0.0139077481112734,-0.0323646534831894,
0.0725544630190594));
#83401=CARTESIAN_POINT('',(0.013965842870796,-0.0326773559991184,0.0727824010023084));
#83402=CARTESIAN_POINT('',(0.0139687507609263,-0.0326943950436594,0.0727948828680809));
#83403=CARTESIAN_POINT('Origin',(-0.00219074803479047,-0.0326395670083038,
0.0766161821969714));
#83404=CARTESIAN_POINT('Ctrl Pts',(0.0139658428675258,-0.0326773559987448,
0.0727824010030674));
#83405=CARTESIAN_POINT('Ctrl Pts',(0.0139240201085822,-0.0326267922586369,
0.0727921915147323));
#83406=CARTESIAN_POINT('Ctrl Pts',(0.0138829386278392,-0.0325756109580141,
0.0728018084966481));
#83407=CARTESIAN_POINT('Ctrl Pts',(0.0138022232602602,-0.0324719985462373,
0.0728207035855371));
#83408=CARTESIAN_POINT('Ctrl Pts',(0.013762621746245,-0.0324196091621769,
0.0728299741141848));
#83409=CARTESIAN_POINT('Ctrl Pts',(0.0137237464515212,-0.0323666188837756,
0.0728390746383034));
#83410=CARTESIAN_POINT('',(0.0138708139121114,-0.0326943950436703,0.0729325682665746));
#83411=CARTESIAN_POINT('Origin',(0.00812378219310841,-0.0315241814719618,
0.07415));
#83412=CARTESIAN_POINT('',(0.0139658428707525,-0.0327114338379856,0.0727824010023186));
#83413=CARTESIAN_POINT('',(0.0139629083290093,-0.0326943950436593,0.0727699253755513));
#83414=CARTESIAN_POINT('Origin',(-0.00217966575170809,-0.0326395678566254,
0.076660115510202));
#83415=CARTESIAN_POINT('Origin',(-0.00221365196606142,-0.0326395673332969,
0.0765183462250016));
#83416=CARTESIAN_POINT('Origin',(-0.00222321968390699,-0.0326395683021248,
0.0764740585239133));
#83417=CARTESIAN_POINT('Ctrl Pts',(0.0137582679500085,-0.0332451089994433,
0.072996442348519));
#83418=CARTESIAN_POINT('Ctrl Pts',(0.0137147608113688,-0.0329451141710253,
0.0727839342413828));
#83419=CARTESIAN_POINT('Ctrl Pts',(0.0136553702925488,-0.0326442513127493,
0.0725753069828916));
#83420=CARTESIAN_POINT('Ctrl Pts',(0.0137028138756343,-0.0332451089994433,
0.0727526702302706));
#83421=CARTESIAN_POINT('Ctrl Pts',(0.0136501127211329,-0.0329451141710253,
0.0725422536077679));
#83422=CARTESIAN_POINT('Ctrl Pts',(0.0135817118448526,-0.0326442513127493,
0.0723364044230834));
#83423=CARTESIAN_POINT('Ctrl Pts',(0.0137022593348906,-0.0332451089994433,
0.0727502325090882));
#83424=CARTESIAN_POINT('Ctrl Pts',(0.0136494662402306,-0.0329451141710253,
0.0725398368014318));
#83425=CARTESIAN_POINT('Ctrl Pts',(0.0135809752603756,-0.0326442513127493,
0.0723340153974852));
#83426=CARTESIAN_POINT('',(0.0136939320316315,-0.0331951640388616,0.0727176746960267));
#83427=CARTESIAN_POINT('',(0.0136303825185583,-0.0328677532355029,0.072490036769806));
#83428=CARTESIAN_POINT('Origin',(-0.00233359358554788,-0.0326402808279494,
0.0776320078208817));
#83429=CARTESIAN_POINT('Origin',(0.0242157355164786,-0.0326944278779144,
0.0692986914638948));
#83430=CARTESIAN_POINT('',(0.0136651594291266,-0.0326943950436593,0.0726101093129251));
#83431=CARTESIAN_POINT('',(0.0136471206126884,-0.0326943950436693,0.0725502690998577));
#83432=CARTESIAN_POINT('',(0.0137237464515693,-0.0330220786163545,0.0728390746382951));
#83433=CARTESIAN_POINT('Origin',(-0.00250214209269808,-0.0326396682761368,
0.0771817367404983));
#83434=CARTESIAN_POINT('',(0.0137224236774251,-0.0331951640388587,0.0728393842935138));
#83435=CARTESIAN_POINT('Origin',(0.0244636883437946,-0.0331952026560045,
0.070324905639891));
#83436=CARTESIAN_POINT('',(0.0137081778545383,-0.0331951640388701,0.0727785294947803));
#83437=CARTESIAN_POINT('Ctrl Pts',(0.0140149585532739,-0.0330240426238172,
0.0730124407296694));
#83438=CARTESIAN_POINT('Ctrl Pts',(0.0139992875660548,-0.0329142774063519,
0.0729312840358132));
#83439=CARTESIAN_POINT('Ctrl Pts',(0.0139819310307149,-0.032804347972669,
0.0728504108454657));
#83440=CARTESIAN_POINT('Ctrl Pts',(0.0139629083290171,-0.0326943950436593,
0.0727699253755555));
#83441=CARTESIAN_POINT('Ctrl Pts',(0.0139174136495208,-0.0330240426238172,
0.0729547681388066));
#83442=CARTESIAN_POINT('Ctrl Pts',(0.0139009481661748,-0.0329142774063519,
0.0728749552210329));
#83443=CARTESIAN_POINT('Ctrl Pts',(0.0138828245182282,-0.032804347972669,
0.0727954429011437));
#83444=CARTESIAN_POINT('Ctrl Pts',(0.0138630631181841,-0.0326943950436593,
0.0727163336797551));
#83445=CARTESIAN_POINT('Ctrl Pts',(0.0138198687457676,-0.0330240426238172,
0.0728970955479438));
#83446=CARTESIAN_POINT('Ctrl Pts',(0.0138026087662949,-0.0329142774063519,
0.0728186264062527));
#83447=CARTESIAN_POINT('Ctrl Pts',(0.0137837180057414,-0.032804347972669,
0.0727404749568217));
#83448=CARTESIAN_POINT('Ctrl Pts',(0.0137632179073512,-0.0326943950436593,
0.0726627419839548));
#83449=CARTESIAN_POINT('Ctrl Pts',(0.0137223238420145,-0.0330240426238172,
0.072839422957081));
#83450=CARTESIAN_POINT('Ctrl Pts',(0.0137042693664149,-0.0329142774063519,
0.0727622975914724));
#83451=CARTESIAN_POINT('Ctrl Pts',(0.0136846114932546,-0.032804347972669,
0.0726855070124997));
#83452=CARTESIAN_POINT('Ctrl Pts',(0.0136633726965182,-0.0326943950436593,
0.0726091502881544));
#83453=CARTESIAN_POINT('',(0.013814033879078,-0.0326943950436693,0.0726900173442482));
#83454=CARTESIAN_POINT('Ctrl Pts',(0.0139658428675191,-0.0327114338383296,
0.0727824010030691));
#83455=CARTESIAN_POINT('Ctrl Pts',(0.0139240270651122,-0.0327619876830069,
0.0727921898862414));
#83456=CARTESIAN_POINT('Ctrl Pts',(0.0138829489822835,-0.032813156260251,
0.0728018060727214));
#83457=CARTESIAN_POINT('Ctrl Pts',(0.0138022336887511,-0.0329167375858767,
0.0728207011442764));
#83458=CARTESIAN_POINT('Ctrl Pts',(0.0137626286393872,-0.0329691088920621,
0.0728299725005327));
#83459=CARTESIAN_POINT('Ctrl Pts',(0.0137237464515224,-0.0330220786163187,
0.0728390746383033));
#83460=CARTESIAN_POINT('Ctrl Pts',(0.0136928625973565,-0.0331951640388604,
0.0727193978658153));
#83461=CARTESIAN_POINT('Ctrl Pts',(0.0136632858154489,-0.0330306422010619,
0.0726042606990196));
#83462=CARTESIAN_POINT('Ctrl Pts',(0.0136289755665096,-0.0328657861914645,
0.0724904443556262));
#83463=CARTESIAN_POINT('Ctrl Pts',(0.0136939320316322,-0.0331951640388604,
0.0727176746960298));
#83464=CARTESIAN_POINT('Ctrl Pts',(0.0136643196242942,-0.0330306422010619,
0.0726025154193661));
#83465=CARTESIAN_POINT('Ctrl Pts',(0.0136299728665419,-0.0328657861914645,
0.0724886784574339));
#83466=CARTESIAN_POINT('Ctrl Pts',(0.0138721285418799,-0.0331951640388604,
0.0724305482691856));
#83467=CARTESIAN_POINT('Ctrl Pts',(0.0138365799797552,-0.0330306422010619,
0.0723117048939216));
#83468=CARTESIAN_POINT('Ctrl Pts',(0.0137961498719495,-0.0328657861914645,
0.0721944323289454));
#83469=CARTESIAN_POINT('',(0.0138684426484039,-0.033178164828194,0.0724182736217006));
#83470=CARTESIAN_POINT('',(0.0138721285418775,-0.0331951640388588,0.0724305482691878));
#83471=CARTESIAN_POINT('Origin',(-0.00173044589592493,-0.0326412092727118,
0.0778644796218298));
#83472=CARTESIAN_POINT('Ctrl Pts',(0.0138684426478127,-0.033178164828644,
0.0724182736234421));
#83473=CARTESIAN_POINT('Ctrl Pts',(0.0138272888581054,-0.0331276811546767,
0.0724306794351338));
#83474=CARTESIAN_POINT('Ctrl Pts',(0.0137868781881544,-0.0330765663497773,
0.0724428612686628));
#83475=CARTESIAN_POINT('Ctrl Pts',(0.0137075083211081,-0.0329730614463219,
0.0724667872904782));
#83476=CARTESIAN_POINT('Ctrl Pts',(0.0136685811861452,-0.0329207133373689,
0.0724785218080462));
#83477=CARTESIAN_POINT('Ctrl Pts',(0.0136303825309352,-0.0328677532289385,
0.0724900367806722));
#83478=CARTESIAN_POINT('',(0.0137830302867645,-0.0331951640388701,0.0725741114826173));
#83479=CARTESIAN_POINT('Origin',(0.00812378219310841,-0.0315241814719618,
0.07415));
#83480=CARTESIAN_POINT('',(0.0138684426467313,-0.0332121607144407,0.0724182736215296));
#83481=CARTESIAN_POINT('',(0.0138647305447434,-0.0331951640388587,0.0724060068739042));
#83482=CARTESIAN_POINT('Origin',(-0.00171004585797308,-0.0326413662843359,
0.0779049762786882));
#83483=CARTESIAN_POINT('Origin',(-0.00214159684043429,-0.0326412095209627,
0.0765005709823073));
#83484=CARTESIAN_POINT('Origin',(-0.00214697489037763,-0.0326413667193929,
0.0764555462101574));
#83485=CARTESIAN_POINT('Ctrl Pts',(0.0136747225465772,-0.0337436976235975,
0.0726449464487163));
#83486=CARTESIAN_POINT('Ctrl Pts',(0.0136611858668398,-0.0336723290703325,
0.0725950204499091));
#83487=CARTESIAN_POINT('Ctrl Pts',(0.0136467533656632,-0.033601104548885,
0.072545346010154));
#83488=CARTESIAN_POINT('Ctrl Pts',(0.0136006732483236,-0.0333736987606857,
0.0723867453639679));
#83489=CARTESIAN_POINT('Ctrl Pts',(0.0135455676478104,-0.0331450831799191,
0.0722310504219283));
#83490=CARTESIAN_POINT('Ctrl Pts',(0.0136040721887949,-0.0337436976235975,
0.0724051370932999));
#83491=CARTESIAN_POINT('Ctrl Pts',(0.0135883786273709,-0.0336723290703325,
0.072355846534518));
#83492=CARTESIAN_POINT('Ctrl Pts',(0.0135718010230033,-0.033601104548885,
0.0723068462274921));
#83493=CARTESIAN_POINT('Ctrl Pts',(0.0135188720160962,-0.0333736987606857,
0.0721503979535722));
#83494=CARTESIAN_POINT('Ctrl Pts',(0.0134570523279748,-0.0331450831799191,
0.0719972448656332));
#83495=CARTESIAN_POINT('Ctrl Pts',(0.0136033656852171,-0.0337436976235975,
0.0724027389997458));
#83496=CARTESIAN_POINT('Ctrl Pts',(0.0135876505549762,-0.0336723290703325,
0.0723534547953641));
#83497=CARTESIAN_POINT('Ctrl Pts',(0.0135710514995767,-0.033601104548885,
0.0723044612296655));
#83498=CARTESIAN_POINT('Ctrl Pts',(0.0135180540037739,-0.0333736987606857,
0.0721480344794682));
#83499=CARTESIAN_POINT('Ctrl Pts',(0.0134561671747764,-0.0331450831799191,
0.0719949068100703));
#83500=CARTESIAN_POINT('',(0.0135930041633291,-0.0336938721132548,0.0723707484606003));
#83501=CARTESIAN_POINT('',(0.013515286543691,-0.0333679869945434,0.0721475500411451));
#83502=CARTESIAN_POINT('Ctrl Pts',(0.0135930041633334,-0.0336938721132649,
0.0723707484606119));
#83503=CARTESIAN_POINT('Ctrl Pts',(0.013586058909913,-0.0336629187933932,
0.0723493995216046));
#83504=CARTESIAN_POINT('Ctrl Pts',(0.0135789908711286,-0.033631995230104,
0.0723280980777477));
#83505=CARTESIAN_POINT('Ctrl Pts',(0.0135718010230072,-0.033601104548895,
0.072306846227504));
#83506=CARTESIAN_POINT('Ctrl Pts',(0.0135537592338432,-0.0335235892595454,
0.0722535180632687));
#83507=CARTESIAN_POINT('Ctrl Pts',(0.0135349182359992,-0.0334458668660369,
0.0722004074688427));
#83508=CARTESIAN_POINT('Ctrl Pts',(0.0135152865439844,-0.0333679869945385,
0.0721475500410432));
#83509=CARTESIAN_POINT('Ctrl Pts',(0.0135152717051053,-0.0333679692459108,
0.0721475081139829));
#83510=CARTESIAN_POINT('Ctrl Pts',(0.0135148489120665,-0.033339189537435,
0.0721476714659582));
#83511=CARTESIAN_POINT('Ctrl Pts',(0.0135145331783367,-0.0333104081060453,
0.0721477969351972));
#83512=CARTESIAN_POINT('Ctrl Pts',(0.0135141172959473,-0.0332532698004612,
0.0721479681621957));
#83513=CARTESIAN_POINT('Ctrl Pts',(0.0135140140017528,-0.0332249170152948,
0.0721480150847957));
#83514=CARTESIAN_POINT('Ctrl Pts',(0.0135140129628318,-0.0331960985410407,
0.0721480228294679));
#83515=CARTESIAN_POINT('Ctrl Pts',(0.0135140129739025,-0.0331956312514202,
0.072148022944742));
#83516=CARTESIAN_POINT('Ctrl Pts',(0.0135140130126346,-0.0331951640388587,
0.0721480230490263));
#83517=CARTESIAN_POINT('',(0.0135575342506988,-0.0331951640388587,0.072265201979884));
#83518=CARTESIAN_POINT('',(0.0135357736316764,-0.0331951640388687,0.0722066125144644));
#83519=CARTESIAN_POINT('',(0.0136303825164448,-0.0335216366567676,0.072490036785186));
#83520=CARTESIAN_POINT('Origin',(-0.00192359277031526,-0.0326434571527816,
0.0784435666451609));
#83521=CARTESIAN_POINT('',(0.0136290817962303,-0.0336938721132327,0.0724904288867702));
#83522=CARTESIAN_POINT('Origin',(0.0240849090392403,-0.0336938867896239,
0.0693385236516236));
#83523=CARTESIAN_POINT('',(0.0136110429797897,-0.0336938721132537,0.0724305886736952));
#83524=CARTESIAN_POINT('Ctrl Pts',(0.013931905483755,-0.0335235895815172,
0.072644774488413));
#83525=CARTESIAN_POINT('Ctrl Pts',(0.0139111830910717,-0.0334144449262748,
0.0725648142361747));
#83526=CARTESIAN_POINT('Ctrl Pts',(0.0138887849722353,-0.0333049234473147,
0.0724851902283316));
#83527=CARTESIAN_POINT('Ctrl Pts',(0.0138647305447509,-0.0331951640388587,
0.0724060068739076));
#83528=CARTESIAN_POINT('Ctrl Pts',(0.0138309316188954,-0.0335235895815172,
0.0725933405394907));
#83529=CARTESIAN_POINT('Ctrl Pts',(0.0138095011366411,-0.0334144449262748,
0.0725147703913015));
#83530=CARTESIAN_POINT('Ctrl Pts',(0.013786422833228,-0.0333049234473147,
0.0724365527131662));
#83531=CARTESIAN_POINT('Ctrl Pts',(0.013761717158803,-0.0331951640388587,
0.0723587901946304));
#83532=CARTESIAN_POINT('Ctrl Pts',(0.0137299577540358,-0.0335235895815172,
0.0725419065905685));
#83533=CARTESIAN_POINT('Ctrl Pts',(0.0137078191822104,-0.0334144449262748,
0.0724647265464284));
#83534=CARTESIAN_POINT('Ctrl Pts',(0.0136840606942207,-0.0333049234473147,
0.0723879151980009));
#83535=CARTESIAN_POINT('Ctrl Pts',(0.0136587037728552,-0.0331951640388587,
0.0723115735153532));
#83536=CARTESIAN_POINT('Ctrl Pts',(0.0136289838891762,-0.0335235895815172,
0.0724904726416463));
#83537=CARTESIAN_POINT('Ctrl Pts',(0.0136061372277798,-0.0334144449262748,
0.0724146827015552));
#83538=CARTESIAN_POINT('Ctrl Pts',(0.0135816985552134,-0.0333049234473147,
0.0723392776828355));
#83539=CARTESIAN_POINT('Ctrl Pts',(0.0135556903869073,-0.0331951640388587,
0.072264356836076));
#83540=CARTESIAN_POINT('',(0.0137111323977311,-0.0331951640388687,0.0723356044269041));
#83541=CARTESIAN_POINT('Ctrl Pts',(0.013868442643727,-0.0332121607145954,
0.0724182736224286));
#83542=CARTESIAN_POINT('Ctrl Pts',(0.0138273580817934,-0.0332625444108882,
0.0724306585527866));
#83543=CARTESIAN_POINT('Ctrl Pts',(0.0137869814713308,-0.033313530074506,
0.0724428300713604));
#83544=CARTESIAN_POINT('Ctrl Pts',(0.0137076121026617,-0.0334167203140572,
0.0724667559466105));
#83545=CARTESIAN_POINT('Ctrl Pts',(0.0136686500850658,-0.0334688847587245,
0.0724785010365378));
#83546=CARTESIAN_POINT('Ctrl Pts',(0.0136303825157164,-0.0335216366562309,
0.0724900367852243));
#83547=CARTESIAN_POINT('Ctrl Pts',(0.0135925313019532,-0.033693872113239,
0.0723716294356234));
#83548=CARTESIAN_POINT('Ctrl Pts',(0.013582121908914,-0.0336474569764958,
0.0723396190323659));
#83549=CARTESIAN_POINT('Ctrl Pts',(0.0135713385069467,-0.033601104548885,
0.0723077326775702));
#83550=CARTESIAN_POINT('Ctrl Pts',(0.013544037412425,-0.0334837508592656,
0.07222700375836));
#83551=CARTESIAN_POINT('Ctrl Pts',(0.0135143561412772,-0.0333660264659097,
0.0721471192773766));
#83552=CARTESIAN_POINT('Ctrl Pts',(0.0135930041633354,-0.033693872113239,
0.0723707484606199));
#83553=CARTESIAN_POINT('Ctrl Pts',(0.0135825896136571,-0.0336474569764958,
0.0723387352895478));
#83554=CARTESIAN_POINT('Ctrl Pts',(0.0135718010230033,-0.033601104548885,
0.0723068462274921));
#83555=CARTESIAN_POINT('Ctrl Pts',(0.0135444867919205,-0.0334837508592656,
0.0722261104541222));
#83556=CARTESIAN_POINT('Ctrl Pts',(0.0135147921868771,-0.0333660264659097,
0.0721462195112524));
#83557=CARTESIAN_POINT('Ctrl Pts',(0.0137537791223436,-0.033693872113239,
0.0720712130673268));
#83558=CARTESIAN_POINT('Ctrl Pts',(0.013741611292612,-0.0336474569764958,
0.0720382588270689));
#83559=CARTESIAN_POINT('Ctrl Pts',(0.0137290585256377,-0.033601104548885,
0.0720054492846667));
#83560=CARTESIAN_POINT('Ctrl Pts',(0.0136972778057211,-0.0334837508592656,
0.0719223830666911));
#83561=CARTESIAN_POINT('Ctrl Pts',(0.0136630496172911,-0.0333660264659097,
0.0718402950539));
#83562=CARTESIAN_POINT('',(0.0137483708743525,-0.0336769361243753,0.0720609805728954));
#83563=CARTESIAN_POINT('',(0.0137528202259598,-0.0336938721132327,0.0720729995607336));
#83564=CARTESIAN_POINT('Ctrl Pts',(0.0137483708743524,-0.033676936124375,
0.0720609805728951));
#83565=CARTESIAN_POINT('Ctrl Pts',(0.0137491146280473,-0.0336797586670014,
0.0720629830954948));
#83566=CARTESIAN_POINT('Ctrl Pts',(0.0137498572841759,-0.0336825812712824,
0.0720649859395555));
#83567=CARTESIAN_POINT('Ctrl Pts',(0.0137513404008548,-0.0336882265995455,
0.0720689922679143));
#83568=CARTESIAN_POINT('Ctrl Pts',(0.0137520808614061,-0.0336910493235148,
0.0720709957522001));
#83569=CARTESIAN_POINT('Ctrl Pts',(0.0137528202259612,-0.0336938721132335,
0.0720729995607319));
#83570=CARTESIAN_POINT('Ctrl Pts',(0.0137483708743525,-0.0336769361243753,
0.0720609805728955));
#83571=CARTESIAN_POINT('Ctrl Pts',(0.0137090804728812,-0.0336279018378422,
0.0720755733576525));
#83572=CARTESIAN_POINT('Ctrl Pts',(0.0136692248297723,-0.0335767825754289,
0.0720903760778966));
#83573=CARTESIAN_POINT('Ctrl Pts',(0.013591130687504,-0.0334733171799211,
0.0721193808975532));
#83574=CARTESIAN_POINT('Ctrl Pts',(0.0135528397023023,-0.0334209631321962,
0.0721336024907219));
#83575=CARTESIAN_POINT('Ctrl Pts',(0.0135152865462182,-0.0333679869844681,
0.0721475500479664));
#83576=CARTESIAN_POINT('',(0.0136729121946544,-0.0336938721132538,0.0722218740106769));
#83577=CARTESIAN_POINT('Origin',(0.00812378219310841,-0.0315241814719618,
0.07415));
#83578=CARTESIAN_POINT('',(0.0137483708731438,-0.0337108120655536,0.0720609805733511));
#83579=CARTESIAN_POINT('',(0.0137438958601233,-0.0336938721132327,0.0720489711163712));
#83580=CARTESIAN_POINT('Origin',(-0.00197825994128331,-0.0345562523539059,
0.0767097827342115));
#83581=CARTESIAN_POINT('Ctrl Pts',(0.0137438958601364,-0.0336938721132376,
0.0720489711163732));
#83582=CARTESIAN_POINT('Ctrl Pts',(0.0137446437846619,-0.0336910492993832,
0.0720509717651413));
#83583=CARTESIAN_POINT('Ctrl Pts',(0.0137453906576377,-0.0336882265874791,
0.0720529728580518));
#83584=CARTESIAN_POINT('Ctrl Pts',(0.0137468823256519,-0.0336825812712948,
0.0720569760006223));
#83585=CARTESIAN_POINT('Ctrl Pts',(0.0137476271206561,-0.0336797586670076,
0.0720589780502916));
#83586=CARTESIAN_POINT('Ctrl Pts',(0.0137483708743526,-0.033676936124375,
0.0720609805728957));
#83587=CARTESIAN_POINT('Origin',(-0.00120002537656662,-0.0345562520009487,
0.078805140333065));
#83588=CARTESIAN_POINT('Ctrl Pts',(0.0135692825547336,-0.034243627687391,
0.0722994187908822));
#83589=CARTESIAN_POINT('Ctrl Pts',(0.013499486733833,-0.033943005420181,
0.0720940383590042));
#83590=CARTESIAN_POINT('Ctrl Pts',(0.0134144190998935,-0.0336441434784053,
0.0718944986986117));
#83591=CARTESIAN_POINT('Ctrl Pts',(0.0134837159642933,-0.034243627687391,
0.0720645180488647));
#83592=CARTESIAN_POINT('Ctrl Pts',(0.013405060715858,-0.033943005420181,
0.071862364814146));
#83593=CARTESIAN_POINT('Ctrl Pts',(0.0133114019088017,-0.0336441434784053,
0.0716667105111667));
#83594=CARTESIAN_POINT('Ctrl Pts',(0.0134828602983889,-0.034243627687391,
0.0720621690414445));
#83595=CARTESIAN_POINT('Ctrl Pts',(0.0134041164556783,-0.033943005420181,
0.0718600480786975));
#83596=CARTESIAN_POINT('Ctrl Pts',(0.0133103717368908,-0.0336441434784053,
0.0716644326292922));
#83597=CARTESIAN_POINT('',(0.0134704917745694,-0.0341934961088741,0.0720308441181655));
#83598=CARTESIAN_POINT('',(0.013378912770339,-0.0338664212890971,0.071812966062671));
#83599=CARTESIAN_POINT('Origin',(-0.00226744349518236,-0.0345610818078965,
0.0777203509298478));
#83600=CARTESIAN_POINT('Origin',(0.0233989667081556,-0.0336938005044555,
0.0673568171623248));
#83601=CARTESIAN_POINT('',(0.0134284645353448,-0.0336938721132327,0.071927733083546));
#83602=CARTESIAN_POINT('',(0.0134030679929601,-0.0336938721132427,0.0718706255916271));
#83603=CARTESIAN_POINT('',(0.0135152865462201,-0.0340203938281605,0.0721475500479715));
#83604=CARTESIAN_POINT('Origin',(-0.00235931595101076,-0.0345589643245916,
0.0772480342467954));
#83605=CARTESIAN_POINT('',(0.013514013012634,-0.034193496108874,0.0721480230490246));
#83606=CARTESIAN_POINT('Origin',(0.023843989668344,-0.0341934220717674,
0.068311383821032));
#83607=CARTESIAN_POINT('',(0.0134922523936117,-0.0341934961088841,0.0720894335836051));
#83608=CARTESIAN_POINT('Ctrl Pts',(0.0138259314386953,-0.0340223579322397,
0.0722830522286004));
#83609=CARTESIAN_POINT('Ctrl Pts',(0.0138001813597235,-0.0339125849573575,
0.0722044047186742));
#83610=CARTESIAN_POINT('Ctrl Pts',(0.0137728215543302,-0.0338030433565231,
0.0721263454402424));
#83611=CARTESIAN_POINT('Ctrl Pts',(0.0137438958601307,-0.0336938721132327,
0.072048971116374));
#83612=CARTESIAN_POINT('Ctrl Pts',(0.0137219272490947,-0.0340223579322397,
0.0722380599139648));
#83613=CARTESIAN_POINT('Ctrl Pts',(0.0136955566087592,-0.0339125849573575,
0.0721608468930675));
#83614=CARTESIAN_POINT('Ctrl Pts',(0.013667606368653,-0.0338030433565231,
0.072084233939844));
#83615=CARTESIAN_POINT('Ctrl Pts',(0.0136381209574983,-0.0336938721132327,
0.0720083158608237));
#83616=CARTESIAN_POINT('Ctrl Pts',(0.0136179230594941,-0.0340223579322397,
0.0721930675993291));
#83617=CARTESIAN_POINT('Ctrl Pts',(0.0135909318577949,-0.0339125849573575,
0.0721172890674607));
#83618=CARTESIAN_POINT('Ctrl Pts',(0.0135623911829759,-0.0338030433565231,
0.0720421224394456));
#83619=CARTESIAN_POINT('Ctrl Pts',(0.0135323460548659,-0.0336938721132327,
0.0719676606052735));
#83620=CARTESIAN_POINT('Ctrl Pts',(0.0135139188698935,-0.0340223579322397,
0.0721480752846935));
#83621=CARTESIAN_POINT('Ctrl Pts',(0.0134863071068306,-0.0339125849573575,
0.072073731241854));
#83622=CARTESIAN_POINT('Ctrl Pts',(0.0134571759972988,-0.0338030433565231,
0.0720000109390472));
#83623=CARTESIAN_POINT('Ctrl Pts',(0.0134265711522335,-0.0336938721132327,
0.0719270053497232));
#83624=CARTESIAN_POINT('',(0.0135861801977441,-0.0336938721132427,0.0719883520999686));
#83625=CARTESIAN_POINT('Ctrl Pts',(0.0137483708697607,-0.033710812066267,
0.0720609805746009));
#83626=CARTESIAN_POINT('Ctrl Pts',(0.0137080620149036,-0.0337611408993504,
0.0720759516214903));
#83627=CARTESIAN_POINT('Ctrl Pts',(0.0136684887072169,-0.033812108877969,
0.0720906494799894));
#83628=CARTESIAN_POINT('Ctrl Pts',(0.013590777135298,-0.0339153382773238,
0.0721195122098083));
#83629=CARTESIAN_POINT('Ctrl Pts',(0.013552671748,-0.0339675558473113,0.0721336648703589));
#83630=CARTESIAN_POINT('Ctrl Pts',(0.0135152865461808,-0.0340203938281304,
0.0721475500479803));
#83631=CARTESIAN_POINT('Ctrl Pts',(0.0134696467056173,-0.0341934961088741,
0.0720326878186427));
#83632=CARTESIAN_POINT('Ctrl Pts',(0.0134258729446295,-0.03402875161944,
0.0719221662821851));
#83633=CARTESIAN_POINT('Ctrl Pts',(0.0133775686485661,-0.033864463329982,
0.0718135483870032));
#83634=CARTESIAN_POINT('Ctrl Pts',(0.0134704917745694,-0.0341934961088741,
0.0720308441181656));
#83635=CARTESIAN_POINT('Ctrl Pts',(0.0134266798965269,-0.03402875161944,
0.0719203051105733));
#83636=CARTESIAN_POINT('Ctrl Pts',(0.013378336793884,-0.033864463329982,
0.0718116713345922));
#83637=CARTESIAN_POINT('Ctrl Pts',(0.0136112966685901,-0.0341934961088741,
0.07172364782412));
#83638=CARTESIAN_POINT('Ctrl Pts',(0.0135611337492273,-0.03402875161944,
0.0716101977862927));
#83639=CARTESIAN_POINT('Ctrl Pts',(0.01350632471702,-0.033864463329982,
0.0714989179608504));
#83640=CARTESIAN_POINT('',(0.0136061014179077,-0.0341764758832425,0.0717119319311992));
#83641=CARTESIAN_POINT('',(0.0136112966685892,-0.0341934961088741,0.0717236478241218));
#83642=CARTESIAN_POINT('Origin',(-0.00173113244827768,-0.0345621027123507,
0.077972170446947));
#83643=CARTESIAN_POINT('Ctrl Pts',(0.0136061014177631,-0.0341764758837528,
0.0717119319330092));
#83644=CARTESIAN_POINT('Ctrl Pts',(0.0135668805667642,-0.034126005004375,
0.0717293740378841));
#83645=CARTESIAN_POINT('Ctrl Pts',(0.013528341482203,-0.0340749269154831,
0.0717465129927412));
#83646=CARTESIAN_POINT('Ctrl Pts',(0.0134525969032517,-0.0339715436319927,
0.0717801977176824));
#83647=CARTESIAN_POINT('Ctrl Pts',(0.0134154201420956,-0.0339192778252677,
0.0717967307031266));
#83648=CARTESIAN_POINT('Ctrl Pts',(0.0133789127738472,-0.0338664212873856,
0.0718129660649879));
#83649=CARTESIAN_POINT('',(0.0135408942215893,-0.0341934961088841,0.0718772459711537));
#83650=CARTESIAN_POINT('Origin',(0.00812378219310841,-0.0315241814719618,
0.07415));
#83651=CARTESIAN_POINT('',(0.0136061014168916,-0.0342105180190533,0.0717119319307304));
#83652=CARTESIAN_POINT('',(0.0136008811544452,-0.0341934961088739,0.071700227159973));
#83653=CARTESIAN_POINT('Origin',(-0.00171761757791809,-0.0345621716515909,
0.0780154343705276));
#83654=CARTESIAN_POINT('Origin',(-0.00131495569966945,-0.0345621032136264,
0.0789080016038157));
#83655=CARTESIAN_POINT('Origin',(-0.00133802805002015,-0.0345621721622157,
0.0788689880464507));
#83656=CARTESIAN_POINT('Ctrl Pts',(0.0134290740563898,-0.0346945769586965,
0.071929103672409));
#83657=CARTESIAN_POINT('Ctrl Pts',(0.01338255649361,-0.0345275153362943,
0.0718179822102097));
#83658=CARTESIAN_POINT('Ctrl Pts',(0.0133325322312999,-0.0343603235965184,
0.0717082949408414));
#83659=CARTESIAN_POINT('Ctrl Pts',(0.0132791540405434,-0.0341934961088739,
0.0716003640716408));
#83660=CARTESIAN_POINT('Ctrl Pts',(0.0133950088260619,-0.0346945769586965,
0.0718525034866133));
#83661=CARTESIAN_POINT('Ctrl Pts',(0.0133468868417216,-0.0345275153362943,
0.0717420955343021));
#83662=CARTESIAN_POINT('Ctrl Pts',(0.0132952801820946,-0.0343603235965184,
0.0716331724169535));
#83663=CARTESIAN_POINT('Ctrl Pts',(0.013240346264704,-0.0341934961088739,
0.0715260540123242));
#83664=CARTESIAN_POINT('Ctrl Pts',(0.0133609435957339,-0.0346945769586965,
0.0717759033008173));
#83665=CARTESIAN_POINT('Ctrl Pts',(0.0133112171898329,-0.0345275153362943,
0.0716662088583944));
#83666=CARTESIAN_POINT('Ctrl Pts',(0.013258028132889,-0.0343603235965184,
0.0715580498930654));
#83667=CARTESIAN_POINT('Ctrl Pts',(0.0132015384888642,-0.0341934961088739,
0.0714517439530069));
#83668=CARTESIAN_POINT('Ctrl Pts',(0.0133268783654062,-0.0346945769586965,
0.0716993031150217));
#83669=CARTESIAN_POINT('Ctrl Pts',(0.0132755475379449,-0.0345275153362943,
0.0715903221824868));
#83670=CARTESIAN_POINT('Ctrl Pts',(0.0132207760836841,-0.0343603235965184,
0.0714829273691776));
#83671=CARTESIAN_POINT('Ctrl Pts',(0.013162730713025,-0.0341934961088739,
0.071377433893691));
#83672=CARTESIAN_POINT('',(0.0133268783657636,-0.0346945769586966,0.0716993031158257));
#83673=CARTESIAN_POINT('',(0.0132217993964057,-0.0343667727832827,0.0714876052893058));
#83674=CARTESIAN_POINT('Origin',(-0.00180506282623017,-0.0345626461567213,
0.0790288053154406));
#83675=CARTESIAN_POINT('Origin',(0.0230184725557128,-0.0341934771027923,
0.0663713712913561));
#83676=CARTESIAN_POINT('',(0.0132784596622649,-0.0341934961088739,0.07159903445947));
#83677=CARTESIAN_POINT('',(0.0132495274250681,-0.0341934961088839,0.0715436343182328));
#83678=CARTESIAN_POINT('',(0.01337891277113,-0.0345211942962645,0.0718129660661669));
#83679=CARTESIAN_POINT('Origin',(-0.00199740023052754,-0.0345625596122438,
0.0785881279815846));
#83680=CARTESIAN_POINT('',(0.0133776714505554,-0.0346945769586885,0.0718135180996884));
#83681=CARTESIAN_POINT('Origin',(0.0234866728168181,-0.0346945685853836,
0.0673178972777572));
#83682=CARTESIAN_POINT('',(0.0133522749081695,-0.0346945769587025,0.0717564106077671));
#83683=CARTESIAN_POINT('Ctrl Pts',(0.0136974525729759,-0.0345231616327842,
0.0719286944161906));
#83684=CARTESIAN_POINT('Ctrl Pts',(0.0136668350028512,-0.0344132092796988,
0.0718518692171043));
#83685=CARTESIAN_POINT('Ctrl Pts',(0.0136346299438081,-0.034303273855898,
0.0717756812821324));
#83686=CARTESIAN_POINT('Ctrl Pts',(0.013600881154452,-0.0341934961088739,
0.0717002271599751));
#83687=CARTESIAN_POINT('Ctrl Pts',(0.0135908286963147,-0.0345231616327842,
0.071890321443089));
#83688=CARTESIAN_POINT('Ctrl Pts',(0.0135596822087806,-0.0344132092796988,
0.071814965904028));
#83689=CARTESIAN_POINT('Ctrl Pts',(0.0135269786583763,-0.034303273855898,
0.0717402584934932));
#83690=CARTESIAN_POINT('Ctrl Pts',(0.0134927623937467,-0.0341934961088739,
0.0716662938471031));
#83691=CARTESIAN_POINT('Ctrl Pts',(0.0134842048196535,-0.0345231616327842,
0.0718519484699873));
#83692=CARTESIAN_POINT('Ctrl Pts',(0.0134525294147101,-0.0344132092796988,
0.0717780625909517));
#83693=CARTESIAN_POINT('Ctrl Pts',(0.0134193273729444,-0.034303273855898,
0.071704835704854));
#83694=CARTESIAN_POINT('Ctrl Pts',(0.0133846436330414,-0.0341934961088739,
0.0716323605342312));
#83695=CARTESIAN_POINT('Ctrl Pts',(0.0133775809429924,-0.0345231616327842,
0.0718135754968856));
#83696=CARTESIAN_POINT('Ctrl Pts',(0.0133453766206395,-0.0344132092796988,
0.0717411592778754));
#83697=CARTESIAN_POINT('Ctrl Pts',(0.0133116760875126,-0.034303273855898,
0.0716694129162147));
#83698=CARTESIAN_POINT('Ctrl Pts',(0.0132765248723361,-0.0341934961088739,
0.0715984272213592));
#83699=CARTESIAN_POINT('',(0.0134396704083651,-0.0341934961088839,0.0716496308097315));
#83700=CARTESIAN_POINT('Ctrl Pts',(0.0136061014137292,-0.0342105180195373,
0.0717119319321293));
#83701=CARTESIAN_POINT('Ctrl Pts',(0.0135668364651007,-0.0342610556240407,
0.0717293936328412));
#83702=CARTESIAN_POINT('Ctrl Pts',(0.0135282761056708,-0.0343122189868325,
0.0717465419923636));
#83703=CARTESIAN_POINT('Ctrl Pts',(0.0134525307637046,-0.034415811969512,
0.0717802270610555));
#83704=CARTESIAN_POINT('Ctrl Pts',(0.0134153767617617,-0.034468199045001,
0.0717967499926991));
#83705=CARTESIAN_POINT('Ctrl Pts',(0.0133789127710976,-0.0345211942962416,
0.0718129660661687));
#83706=CARTESIAN_POINT('Ctrl Pts',(0.0133261509086851,-0.0346945769586932,
0.0717011957789349));
#83707=CARTESIAN_POINT('Ctrl Pts',(0.0132755236141497,-0.0345296777077528,
0.0715936404868541));
#83708=CARTESIAN_POINT('Ctrl Pts',(0.0132204942209498,-0.0343648066252516,
0.0714882695720313));
#83709=CARTESIAN_POINT('Ctrl Pts',(0.0133268783657674,-0.0346945769586932,
0.0716993031158339));
#83710=CARTESIAN_POINT('Ctrl Pts',(0.0132762119417616,-0.0345296777077528,
0.0715917327840927));
#83711=CARTESIAN_POINT('Ctrl Pts',(0.0132211428309239,-0.0343648066252516,
0.0714863484597176));
#83712=CARTESIAN_POINT('Ctrl Pts',(0.0134481163985928,-0.0346945769586932,
0.0713838717910554));
#83713=CARTESIAN_POINT('Ctrl Pts',(0.0133909286551414,-0.0345296777077528,
0.0712737949487716));
#83714=CARTESIAN_POINT('Ctrl Pts',(0.0133292402008602,-0.0343648066252516,
0.0711661757877611));
#83715=CARTESIAN_POINT('',(0.0134421957527042,-0.0346775396665007,0.0713725052290604));
#83716=CARTESIAN_POINT('',(0.0134481163985908,-0.0346945769586886,0.0713838717910534));
#83717=CARTESIAN_POINT('Origin',(-0.00120217637793559,-0.0345626618147741,
0.0791926885719967));
#83718=CARTESIAN_POINT('Ctrl Pts',(0.0134421957525685,-0.0346775396670096,
0.0713725052308742));
#83719=CARTESIAN_POINT('Ctrl Pts',(0.0134041175267979,-0.0346269749928325,
0.0713923912643912));
#83720=CARTESIAN_POINT('Ctrl Pts',(0.0133667160526948,-0.0345757902891079,
0.0714119239105586));
#83721=CARTESIAN_POINT('Ctrl Pts',(0.0132932357257123,-0.0344721681088438,
0.0714502983617085));
#83722=CARTESIAN_POINT('Ctrl Pts',(0.0132571856779471,-0.0344197714289854,
0.0714691251171155));
#83723=CARTESIAN_POINT('Ctrl Pts',(0.0132217993966978,-0.0343667727831633,
0.0714876052895225));
#83724=CARTESIAN_POINT('',(0.0133874973821872,-0.0346945769587026,0.0715415874534496));
#83725=CARTESIAN_POINT('Origin',(0.00812378219310841,-0.0315241814719618,
0.07415));
#83726=CARTESIAN_POINT('',(0.0134421957513162,-0.0347116136489609,0.0713725052289522));
#83727=CARTESIAN_POINT('',(0.0134362508414153,-0.0346945769586885,0.0713611513377796));
#83728=CARTESIAN_POINT('Origin',(-0.00117956073235415,-0.034562669603157,
0.0792319529103707));
#83729=CARTESIAN_POINT('Origin',(-0.00134356747308092,-0.0345626622155451,
0.0789219522010525));
#83730=CARTESIAN_POINT('Origin',(-0.00136286474894159,-0.0345626702618841,
0.0788809552601594));
#83731=CARTESIAN_POINT('Ctrl Pts',(0.0132955128131795,-0.0352450361874068,
0.0716336616595897));
#83732=CARTESIAN_POINT('Ctrl Pts',(0.013200607555348,-0.0349452760959492,
0.0714386066385497));
#83733=CARTESIAN_POINT('Ctrl Pts',(0.0130912795710791,-0.0346444289841739,
0.0712512544006321));
#83734=CARTESIAN_POINT('Ctrl Pts',(0.0132943694554156,-0.0352450361874068,
0.0716314384337749));
#83735=CARTESIAN_POINT('Ctrl Pts',(0.0131993803472466,-0.0349452760959492,
0.0714364265351804));
#83736=CARTESIAN_POINT('Ctrl Pts',(0.0130899719990091,-0.0346444289841739,
0.0712491236131528));
#83737=CARTESIAN_POINT('Ctrl Pts',(0.0131800336772834,-0.0352450361874068,
0.0714091158489037));
#83738=CARTESIAN_POINT('Ctrl Pts',(0.0130766595352339,-0.0349452760959492,
0.0712184161949422));
#83739=CARTESIAN_POINT('Ctrl Pts',(0.0129592147900247,-0.0346444289841739,
0.0710360448619749));
#83740=CARTESIAN_POINT('',(0.01316274824,-0.0351951633467201,0.0713774613991309));
#83741=CARTESIAN_POINT('',(0.0130445664770105,-0.0348678972925434,0.071172751768612));
#83742=CARTESIAN_POINT('Origin',(-0.00106747175712535,-0.0345631633301949,
0.080204957386172));
#83743=CARTESIAN_POINT('Origin',(0.0224986601168685,-0.0346946199341027,
0.0654526903452147));
#83744=CARTESIAN_POINT('',(0.0131081116410078,-0.0346945769330288,0.0712804033466476));
#83745=CARTESIAN_POINT('',(0.0130757578871117,-0.0346945769458128,0.0712269291875016));
#83746=CARTESIAN_POINT('',(0.0132217993964998,-0.0350221583435276,0.0714876052896075));
#83747=CARTESIAN_POINT('Origin',(-0.00135078810670648,-0.0345628458719986,
0.0798157290478429));
#83748=CARTESIAN_POINT('',(0.0132207044192628,-0.035195136029876,0.0714881805439839));
#83749=CARTESIAN_POINT('Origin',(0.0229879493288178,-0.0351951838366849,
0.0663873207389187));
#83750=CARTESIAN_POINT('',(0.0131627307160144,-0.0351951371328747,0.0713774338991642));
#83751=CARTESIAN_POINT('Ctrl Pts',(0.0135469768650149,-0.0350241211494343,
0.0715831031281574));
#83752=CARTESIAN_POINT('Ctrl Pts',(0.0135116189130739,-0.0349144232818962,
0.0715084008451483));
#83753=CARTESIAN_POINT('Ctrl Pts',(0.0134746956481253,-0.0348045283579412,
0.0714343847233541));
#83754=CARTESIAN_POINT('Ctrl Pts',(0.0134362508362562,-0.0346945769439157,
0.0713611513279417));
#83755=CARTESIAN_POINT('Ctrl Pts',(0.0134381538982397,-0.0350241211494343,
0.071551500854417));
#83756=CARTESIAN_POINT('Ctrl Pts',(0.0134023606379354,-0.0349144232818962,
0.071478297563156));
#83757=CARTESIAN_POINT('Ctrl Pts',(0.0133650327893009,-0.0348045283579412,
0.0714057903284638));
#83758=CARTESIAN_POINT('Ctrl Pts',(0.0133262147085638,-0.0346945769439157,
0.0713340738020986));
#83759=CARTESIAN_POINT('Ctrl Pts',(0.0133293309314644,-0.0350241211494343,
0.0715198985806766));
#83760=CARTESIAN_POINT('Ctrl Pts',(0.0132931023627968,-0.0349144232818962,
0.0714481942811638));
#83761=CARTESIAN_POINT('Ctrl Pts',(0.0132553699304765,-0.0348045283579412,
0.0713771959335734));
#83762=CARTESIAN_POINT('Ctrl Pts',(0.0132161785808714,-0.0346945769439157,
0.0713069962762554));
#83763=CARTESIAN_POINT('Ctrl Pts',(0.0132205079646892,-0.0350241211494343,
0.0714882963069362));
#83764=CARTESIAN_POINT('Ctrl Pts',(0.0131838440876582,-0.0349144232818962,
0.0714180909991716));
#83765=CARTESIAN_POINT('Ctrl Pts',(0.0131457070716521,-0.0348045283579412,
0.0713486015386831));
#83766=CARTESIAN_POINT('Ctrl Pts',(0.013106142453179,-0.0346945769439157,
0.0712799187504123));
#83767=CARTESIAN_POINT('',(0.0132721812414348,-0.0346945769458128,0.0713207773424309));
#83768=CARTESIAN_POINT('Ctrl Pts',(0.0134421957483956,-0.0347116136492782,
0.0713725052304696));
#83769=CARTESIAN_POINT('Ctrl Pts',(0.0134041326384174,-0.0347621546531421,
0.0713923833553611));
#83770=CARTESIAN_POINT('Ctrl Pts',(0.0133667387807672,-0.0348133084095238,
0.0714119119691021));
#83771=CARTESIAN_POINT('Ctrl Pts',(0.0132932583621568,-0.0349168561544572,
0.0714502864723691));
#83772=CARTESIAN_POINT('Ctrl Pts',(0.0132572009473367,-0.0349692089015923,
0.0714691171405796));
#83773=CARTESIAN_POINT('Ctrl Pts',(0.0132217993964582,-0.0350221583435,
0.0714876052896068));
#83774=CARTESIAN_POINT('Ctrl Pts',(0.0131622926126873,-0.0351951371254981,
0.0713788297767868));
#83775=CARTESIAN_POINT('Ctrl Pts',(0.0131241291376846,-0.0350856248736071,
0.0713094413773164));
#83776=CARTESIAN_POINT('Ctrl Pts',(0.013084500336438,-0.0349758427080755,
0.0712407847106068));
#83777=CARTESIAN_POINT('Ctrl Pts',(0.0130434517796293,-0.0348659306897848,
0.0711729506531316));
#83778=CARTESIAN_POINT('Ctrl Pts',(0.0131869140273343,-0.0351951371254981,
0.0713003807067396));
#83779=CARTESIAN_POINT('Ctrl Pts',(0.0131476701823497,-0.0350856248736071,
0.0712306532307539));
#83780=CARTESIAN_POINT('Ctrl Pts',(0.0131069531167853,-0.0349758427080755,
0.0711616795363528));
#83781=CARTESIAN_POINT('Ctrl Pts',(0.0130648097707083,-0.0348659306897848,
0.0710935509877194));
#83782=CARTESIAN_POINT('Ctrl Pts',(0.0132115354419813,-0.0351951371254981,
0.0712219316366923));
#83783=CARTESIAN_POINT('Ctrl Pts',(0.0131712112270149,-0.0350856248736071,
0.0711518650841914));
#83784=CARTESIAN_POINT('Ctrl Pts',(0.0131294058971327,-0.0349758427080755,
0.0710825743620988));
#83785=CARTESIAN_POINT('Ctrl Pts',(0.0130861677617873,-0.0348659306897848,
0.0710141513223072));
#83786=CARTESIAN_POINT('Ctrl Pts',(0.0132361568566283,-0.0351951371254981,
0.071143482566645));
#83787=CARTESIAN_POINT('Ctrl Pts',(0.01319475227168,-0.0350856248736071,
0.0710730769376289));
#83788=CARTESIAN_POINT('Ctrl Pts',(0.01315185867748,-0.0349758427080755,
0.0710034691878447));
#83789=CARTESIAN_POINT('Ctrl Pts',(0.0131075257528663,-0.0348659306897848,
0.0709347516568949));
#83790=CARTESIAN_POINT('Origin',(0.0175947305641669,-0.0308609197384946,
0.0684197418359026));
#83791=CARTESIAN_POINT('',(0.0131947428563328,-0.0351951371254981,0.0712754363904484));
#83792=CARTESIAN_POINT('Origin',(0.00736988752340133,-0.03518404674411,
0.0747716015423331));
#83793=CARTESIAN_POINT('Origin',(0.017927210120105,-0.0352322613839716,
0.0672897386084101));
#83794=CARTESIAN_POINT('',(0.0129178964449081,-0.0351951142564678,0.0709728498423726));
#83795=CARTESIAN_POINT('',(0.0128467975461564,-0.0351951372916786,0.0708704228969463));
#83796=CARTESIAN_POINT('Origin',(0.00781164895014946,-0.0352875127425782,
0.0740136130634983));
#83797=CARTESIAN_POINT('Origin',(0.0111440472267538,-0.0298325076523627,
0.081018274121231));
#83798=CARTESIAN_POINT('Origin',(0.0163016666201714,-0.0338731404305814,
0.0723126509480677));
#83799=CARTESIAN_POINT('Ctrl Pts',(0.0138697965960476,-0.0321934096636941,
0.0743978996299439));
#83800=CARTESIAN_POINT('Ctrl Pts',(0.0138742338813685,-0.0320508460845488,
0.074295048708508));
#83801=CARTESIAN_POINT('Ctrl Pts',(0.0138759044196463,-0.0319086045665392,
0.0741921561159053));
#83802=CARTESIAN_POINT('Ctrl Pts',(0.013874822852946,-0.0317669892871366,
0.0740894436941117));
#83803=CARTESIAN_POINT('Ctrl Pts',(0.013871588533368,-0.0321934096636941,
0.0743140711050352));
#83804=CARTESIAN_POINT('Ctrl Pts',(0.0138745253280139,-0.0320508460845488,
0.0742111881087748));
#83805=CARTESIAN_POINT('Ctrl Pts',(0.0138746956452045,-0.0319086045665392,
0.0741083037807555));
#83806=CARTESIAN_POINT('Ctrl Pts',(0.0138721173557796,-0.0317669892871366,
0.0740056396792251));
#83807=CARTESIAN_POINT('Ctrl Pts',(0.0138733804706884,-0.0321934096636941,
0.0742302425801266));
#83808=CARTESIAN_POINT('Ctrl Pts',(0.0138748167746594,-0.0320508460845488,
0.0741273275090414));
#83809=CARTESIAN_POINT('Ctrl Pts',(0.0138734868707628,-0.0319086045665392,
0.0740244514456057));
#83810=CARTESIAN_POINT('Ctrl Pts',(0.0138694118586132,-0.0317669892871366,
0.0739218356643386));
#83811=CARTESIAN_POINT('Ctrl Pts',(0.0138751724080088,-0.0321934096636941,
0.0741464140552179));
#83812=CARTESIAN_POINT('Ctrl Pts',(0.0138751082213048,-0.0320508460845489,
0.0740434669093081));
#83813=CARTESIAN_POINT('Ctrl Pts',(0.0138722780963211,-0.0319086045665392,
0.0739405991104559));
#83814=CARTESIAN_POINT('Ctrl Pts',(0.0138667063614468,-0.0317669892871366,
0.0738380316494521));
#83815=CARTESIAN_POINT('',(0.0138751403498937,-0.0321934096636941,0.074147913764094));
#83816=CARTESIAN_POINT('',(0.013870198605396,-0.0318665617511344,0.073911623394967));
#83817=CARTESIAN_POINT('Origin',(-0.00282357719959373,-0.0326371944423954,
0.0735390319721531));
#83818=CARTESIAN_POINT('Origin',(0.0248219653144219,-0.0316939261509308,
0.0734573150399617));
#83819=CARTESIAN_POINT('',(0.0138737862240784,-0.0320197221621802,0.0742726491351916));
#83820=CARTESIAN_POINT('Ctrl Pts',(0.0138738372100478,-0.0320197392094717,
0.0742724713282445));
#83821=CARTESIAN_POINT('Ctrl Pts',(0.0138744603366102,-0.0319792716576016,
0.0742432131987236));
#83822=CARTESIAN_POINT('Ctrl Pts',(0.0138748632476785,-0.0319386439829712,
0.0742138171245965));
#83823=CARTESIAN_POINT('Ctrl Pts',(0.0138750379095079,-0.0318979099381644,
0.0741842521296344));
#83824=CARTESIAN_POINT('Ctrl Pts',(0.013875212567885,-0.0318571766984951,
0.0741546877190454));
#83825=CARTESIAN_POINT('Ctrl Pts',(0.0138751598799729,-0.0318163871833605,
0.0741251046704643));
#83826=CARTESIAN_POINT('Ctrl Pts',(0.0138748835481446,-0.0317755399638303,
0.074095604731115));
#83827=CARTESIAN_POINT('',(0.0138724689321763,-0.0321934096636185,0.074272885214998));
#83828=CARTESIAN_POINT('Origin',(0.0161800533289082,-0.0324111828247256,
0.0743011809090815));
#83829=CARTESIAN_POINT('',(0.013873804641045,-0.0321934096636664,0.074210399489556));
#83830=CARTESIAN_POINT('Ctrl Pts',(0.0138736758573183,-0.0321934096636618,
0.0741493169564813));
#83831=CARTESIAN_POINT('Ctrl Pts',(0.0138736664376159,-0.0320835708272592,
0.0740700214416468));
#83832=CARTESIAN_POINT('Ctrl Pts',(0.0138720160068189,-0.0319739230346488,
0.0739907721163737));
#83833=CARTESIAN_POINT('Ctrl Pts',(0.0138687344582465,-0.0318646057455573,
0.0739116702126153));
#83834=CARTESIAN_POINT('Ctrl Pts',(0.0139554985474753,-0.0321934096636618,
0.0740709191750039));
#83835=CARTESIAN_POINT('Ctrl Pts',(0.0139544079612666,-0.0320835708272592,
0.0739904952615033));
#83836=CARTESIAN_POINT('Ctrl Pts',(0.0139516536389322,-0.0319739230346488,
0.0739101405667658));
#83837=CARTESIAN_POINT('Ctrl Pts',(0.0139472469946829,-0.0318646057455573,
0.0738299576285942));
#83838=CARTESIAN_POINT('Ctrl Pts',(0.0140373212376322,-0.0321934096636618,
0.0739925213935266));
#83839=CARTESIAN_POINT('Ctrl Pts',(0.0140351494849173,-0.0320835708272592,
0.0739109690813598));
#83840=CARTESIAN_POINT('Ctrl Pts',(0.0140312912710454,-0.0319739230346488,
0.073829509017158));
#83841=CARTESIAN_POINT('Ctrl Pts',(0.0140257595311193,-0.0318646057455573,
0.073748245044573));
#83842=CARTESIAN_POINT('Ctrl Pts',(0.0141191439277891,-0.0321934096636618,
0.0739141236120492));
#83843=CARTESIAN_POINT('Ctrl Pts',(0.014115891008568,-0.0320835708272592,
0.0738314429012163));
#83844=CARTESIAN_POINT('Ctrl Pts',(0.0141109289031586,-0.0319739230346488,
0.0737488774675501));
#83845=CARTESIAN_POINT('Ctrl Pts',(0.0141042720675557,-0.0318646057455573,
0.0736665324605519));
#83846=CARTESIAN_POINT('',(0.0141186264125959,-0.032176398030849,0.0739013179501406));
#83847=CARTESIAN_POINT('',(0.0141191439277825,-0.0321934096636184,0.0739141236120217));
#83848=CARTESIAN_POINT('Origin',(-0.00242890665718246,-0.0326386230140034,
0.073973723431972));
#83849=CARTESIAN_POINT('Ctrl Pts',(0.0141186264094195,-0.0321763980306323,
0.0739013179502667));
#83850=CARTESIAN_POINT('Ctrl Pts',(0.0140757443961277,-0.0321259596175455,
0.0739030968099963));
#83851=CARTESIAN_POINT('Ctrl Pts',(0.0140336053693588,-0.0320749164632659,
0.0739048448486798));
#83852=CARTESIAN_POINT('Ctrl Pts',(0.0139507793765562,-0.0319716057794,
0.0739082806906997));
#83853=CARTESIAN_POINT('Ctrl Pts',(0.0139101246824559,-0.0319193786690211,
0.0739099671553107));
#83854=CARTESIAN_POINT('Ctrl Pts',(0.013870198603538,-0.0318665617525411,
0.0739116233950369));
#83855=CARTESIAN_POINT('',(0.0139971421388481,-0.0321934096636663,0.0740310186880679));
#83856=CARTESIAN_POINT('Origin',(0.00812378219310841,-0.0315241814719618,
0.07415));
#83857=CARTESIAN_POINT('',(0.0141186264129662,-0.0322104233323764,0.0739013179501252));
#83858=CARTESIAN_POINT('',(0.0141180815491566,-0.0321934096636183,0.0738885134227272));
#83859=CARTESIAN_POINT('Origin',(-0.00243335535698296,-0.0326387242963926,
0.0740188372389752));
#83860=CARTESIAN_POINT('Origin',(-0.00237805205674754,-0.0326386237958717,
0.0751996751081487));
#83861=CARTESIAN_POINT('Origin',(-0.00238621941514002,-0.0326387247895164,
0.0751550842654159));
#83862=CARTESIAN_POINT('Ctrl Pts',(0.0138746213929418,-0.0327445246967096,
0.0740727115942768));
#83863=CARTESIAN_POINT('Ctrl Pts',(0.0138717064130665,-0.0324436878339359,
0.0738558151480787));
#83864=CARTESIAN_POINT('Ctrl Pts',(0.0138524621875469,-0.0321434074405926,
0.0736397544499746));
#83865=CARTESIAN_POINT('Ctrl Pts',(0.0138658296065809,-0.0327445246967096,
0.073822866233118));
#83866=CARTESIAN_POINT('Ctrl Pts',(0.0138534915548631,-0.0324436878339359,
0.0736063013745631));
#83867=CARTESIAN_POINT('Ctrl Pts',(0.0138248760039893,-0.0321434074405926,
0.0733912811063806));
#83868=CARTESIAN_POINT('',(0.0138636603625111,-0.0326943950436612,0.0737867871141936));
#83869=CARTESIAN_POINT('',(0.0138438915753067,-0.0323666188837389,0.0735512733046812));
#83870=CARTESIAN_POINT('Origin',(-0.00290876188441187,-0.0326395579112152,
0.0749242888442998));
#83871=CARTESIAN_POINT('Origin',(0.0248284905272715,-0.0321933825603021,
0.0724015091066871));
#83872=CARTESIAN_POINT('',(0.0138555531450554,-0.0321934096532689,0.0736757355682102));
#83873=CARTESIAN_POINT('',(0.0138490467834857,-0.0321934096584274,0.0736135751498974));
#83874=CARTESIAN_POINT('',(0.013870198606331,-0.0325210109756238,0.0739116233949256));
#83875=CARTESIAN_POINT('Origin',(-0.00291375938666434,-0.0326393129156296,
0.0744434983967485));
#83876=CARTESIAN_POINT('',(0.0138688412385515,-0.0326943950436593,0.0739116797021394));
#83877=CARTESIAN_POINT('Origin',(0.0249217906147906,-0.0326943765538174,
0.0734531747542535));
#83878=CARTESIAN_POINT('',(0.0138662508005413,-0.0326943950436702,0.0738492334081765));
#83879=CARTESIAN_POINT('Ctrl Pts',(0.0141237669771519,-0.0325229783203769,
0.0741364873635179));
#83880=CARTESIAN_POINT('Ctrl Pts',(0.0141235807057535,-0.032413025309245,
0.0740537777044809));
#83881=CARTESIAN_POINT('Ctrl Pts',(0.0141216835070616,-0.032303122220807,
0.0739710844432473));
#83882=CARTESIAN_POINT('Ctrl Pts',(0.0141180815489685,-0.0321934096576658,
0.0738885134182532));
#83883=CARTESIAN_POINT('Ctrl Pts',(0.0140387566190187,-0.0325229783203769,
0.0740615581886461));
#83884=CARTESIAN_POINT('Ctrl Pts',(0.0140375374505832,-0.032413025309245,
0.0739800203955368));
#83885=CARTESIAN_POINT('Ctrl Pts',(0.0140346317530654,-0.032303122220807,
0.0738985201892968));
#83886=CARTESIAN_POINT('Ctrl Pts',(0.0140300469322471,-0.0321934096576658,
0.0738171618345591));
#83887=CARTESIAN_POINT('Ctrl Pts',(0.0139537462608854,-0.0325229783203769,
0.0739866290137742));
#83888=CARTESIAN_POINT('Ctrl Pts',(0.0139514941954129,-0.032413025309245,
0.0739062630865928));
#83889=CARTESIAN_POINT('Ctrl Pts',(0.0139475799990693,-0.032303122220807,
0.0738259559353461));
#83890=CARTESIAN_POINT('Ctrl Pts',(0.0139420123155258,-0.0321934096576658,
0.073745810250865));
#83891=CARTESIAN_POINT('Ctrl Pts',(0.0138687359027521,-0.0325229783203769,
0.0739116998389024));
#83892=CARTESIAN_POINT('Ctrl Pts',(0.0138654509402426,-0.032413025309245,
0.0738325057776488));
#83893=CARTESIAN_POINT('Ctrl Pts',(0.0138605282450731,-0.032303122220807,
0.0737533916813956));
#83894=CARTESIAN_POINT('Ctrl Pts',(0.0138539776988044,-0.0321934096576658,
0.073674458667171));
#83895=CARTESIAN_POINT('',(0.0139868173472928,-0.0321934096584275,0.073782124495952));
#83896=CARTESIAN_POINT('Ctrl Pts',(0.0141186264094853,-0.0322104233328894,
0.073901317950264));
#83897=CARTESIAN_POINT('Ctrl Pts',(0.0140756862904063,-0.0322609421830354,
0.0739030992203759));
#83898=CARTESIAN_POINT('Ctrl Pts',(0.0140335188780103,-0.0323120888238673,
0.0739048484365637));
#83899=CARTESIAN_POINT('Ctrl Pts',(0.0139506922580386,-0.032415652463181,
0.0739082843046003));
#83900=CARTESIAN_POINT('Ctrl Pts',(0.0139100670967876,-0.0324680267167313,
0.0739099695441171));
#83901=CARTESIAN_POINT('Ctrl Pts',(0.0138701986062875,-0.0325210109755912,
0.0739116233949229));
#83902=CARTESIAN_POINT('Origin',(0.00750075467550516,-0.026283458251078,
0.0819931640652065));
#83903=CARTESIAN_POINT('Origin',(0.0192136187594495,-0.0342770745984023,
0.0791338237432995));
#83904=CARTESIAN_POINT('Ctrl Pts',(0.0138622872002598,-0.0326943950436604,
0.0737882791317084));
#83905=CARTESIAN_POINT('Ctrl Pts',(0.0138573020087576,-0.0325844576448133,
0.0737091917776052));
#83906=CARTESIAN_POINT('Ctrl Pts',(0.0138506808082973,-0.0324744968375322,
0.0736302019283006));
#83907=CARTESIAN_POINT('Ctrl Pts',(0.0138424334782875,-0.0323646534831894,
0.0735514106731837));
#83908=CARTESIAN_POINT('Ctrl Pts',(0.0139390256834958,-0.0326943950436604,
0.0737048984818396));
#83909=CARTESIAN_POINT('Ctrl Pts',(0.0139328913503664,-0.0325844576448133,
0.0736247535276142));
#83910=CARTESIAN_POINT('Ctrl Pts',(0.0139250990540479,-0.0324744968375322,
0.0735447297694723));
#83911=CARTESIAN_POINT('Ctrl Pts',(0.0139156601926969,-0.0323646534831894,
0.0734649296008111));
#83912=CARTESIAN_POINT('Ctrl Pts',(0.0140157641667319,-0.0326943950436604,
0.0736215178319709));
#83913=CARTESIAN_POINT('Ctrl Pts',(0.0140084806919753,-0.0325844576448133,
0.0735403152776232));
#83914=CARTESIAN_POINT('Ctrl Pts',(0.0139995172997985,-0.0324744968375322,
0.073459257610644));
#83915=CARTESIAN_POINT('Ctrl Pts',(0.0139888869071063,-0.0323646534831894,
0.0733784485284386));
#83916=CARTESIAN_POINT('Ctrl Pts',(0.0140925026499679,-0.0326943950436604,
0.0735381371821021));
#83917=CARTESIAN_POINT('Ctrl Pts',(0.0140840700335841,-0.0325844576448133,
0.0734558770276322));
#83918=CARTESIAN_POINT('Ctrl Pts',(0.0140739355455492,-0.0324744968375322,
0.0733737854518156));
#83919=CARTESIAN_POINT('Ctrl Pts',(0.0140621136215156,-0.0323646534831894,
0.073291967456066));
#83920=CARTESIAN_POINT('',(0.0140911820820146,-0.0326773559991189,0.0735253892843));
#83921=CARTESIAN_POINT('',(0.0140925026499634,-0.0326943950436594,0.0735381371821062));
#83922=CARTESIAN_POINT('Origin',(-0.00241850945560545,-0.0326395669502595,
0.0753039822634916));
#83923=CARTESIAN_POINT('Ctrl Pts',(0.0140911820786748,-0.032677355998746,
0.0735253892846437));
#83924=CARTESIAN_POINT('Ctrl Pts',(0.0140484620282019,-0.0326267922586494,
0.0735298608135839));
#83925=CARTESIAN_POINT('Ctrl Pts',(0.0140064991597738,-0.0325756109580394,
0.0735342530879027));
#83926=CARTESIAN_POINT('Ctrl Pts',(0.0139240520743678,-0.0324719985462376,
0.0735428828653572));
#83927=CARTESIAN_POINT('Ctrl Pts',(0.013883600924787,-0.0324196091621774,
0.073547116907312));
#83928=CARTESIAN_POINT('Ctrl Pts',(0.0138438915752582,-0.0323666188837756,
0.0735512733046863));
#83929=CARTESIAN_POINT('',(0.0139780815062472,-0.0326943950436703,0.0736624621481599));
#83930=CARTESIAN_POINT('Origin',(0.00812378219310841,-0.0315241814719618,
0.07415));
#83931=CARTESIAN_POINT('',(0.0140911820819701,-0.0327114338379853,0.0735253892843048));
#83932=CARTESIAN_POINT('',(0.0140898342906075,-0.0326943950436593,0.0735126442359757));
#83933=CARTESIAN_POINT('Origin',(-0.00241302076069148,-0.0326395678925681,
0.0753489579910992));
#83934=CARTESIAN_POINT('Origin',(-0.0024289706066625,-0.0326395674317057,
0.0752040471793359));
#83935=CARTESIAN_POINT('Origin',(-0.00243291222228821,-0.0326395682946239,
0.075158909412172));
#83936=CARTESIAN_POINT('Ctrl Pts',(0.013858417457439,-0.0332451089994433,
0.0737117268145363));
#83937=CARTESIAN_POINT('Ctrl Pts',(0.0138418877138084,-0.0329451141710254,
0.073495441506929));
#83938=CARTESIAN_POINT('Ctrl Pts',(0.0138091134358847,-0.0326442513127493,
0.0732810157309182));
#83939=CARTESIAN_POINT('Ctrl Pts',(0.0138339534028375,-0.0332451089994433,
0.073462926673796));
#83940=CARTESIAN_POINT('Ctrl Pts',(0.0138080400083743,-0.0329451141710254,
0.0732475640431037));
#83941=CARTESIAN_POINT('Ctrl Pts',(0.0137659782373769,-0.0326442513127493,
0.0730347651377216));
#83942=CARTESIAN_POINT('Ctrl Pts',(0.0138337087622915,-0.0332451089994433,
0.0734604386723885));
#83943=CARTESIAN_POINT('Ctrl Pts',(0.01380770153132,-0.0329451141710254,
0.0732450852684655));
#83944=CARTESIAN_POINT('Ctrl Pts',(0.0137655468853918,-0.0326442513127493,
0.0730323026317896));
#83945=CARTESIAN_POINT('',(0.0138295276982946,-0.0331951640388616,0.0734270938995632));
#83946=CARTESIAN_POINT('',(0.0137950098894886,-0.0328677532355034,0.0731932861004177));
#83947=CARTESIAN_POINT('Origin',(-0.00268754535352905,-0.0326402808277667,
0.0762938944285065));
#83948=CARTESIAN_POINT('Origin',(0.0246968758612786,-0.0326944278779091,
0.0713538021235014));
#83949=CARTESIAN_POINT('',(0.0138144634936381,-0.0326943950436593,0.0733167705383256));
#83950=CARTESIAN_POINT('',(0.0138040668860577,-0.0326943950436693,0.0732551413200166));
#83951=CARTESIAN_POINT('',(0.013843891575307,-0.0330220786163545,0.073551273304684));
#83952=CARTESIAN_POINT('Origin',(-0.00279833087479486,-0.032639668275823,
0.0758260491408386));
#83953=CARTESIAN_POINT('',(0.0138425404215422,-0.0331951640388587,0.0735514147306181));
#83954=CARTESIAN_POINT('Origin',(0.0248142547232573,-0.0331952026560103,
0.0724030006817456));
#83955=CARTESIAN_POINT('',(0.0138360340599284,-0.0331951640388701,0.0734892543151006));
#83956=CARTESIAN_POINT('Ctrl Pts',(0.014111078849787,-0.0330240426238172,
0.073759770907006));
#83957=CARTESIAN_POINT('Ctrl Pts',(0.0141057030638493,-0.0329142774063519,
0.0736772900624198));
#83958=CARTESIAN_POINT('Ctrl Pts',(0.0140986194884296,-0.0328043479726691,
0.0735948792306362));
#83959=CARTESIAN_POINT('Ctrl Pts',(0.0140898342906153,-0.0326943950436593,
0.0735126442359812));
#83960=CARTESIAN_POINT('Ctrl Pts',(0.0140215314090359,-0.0330240426238172,
0.0736903274635429));
#83961=CARTESIAN_POINT('Ctrl Pts',(0.014015198972009,-0.0329142774063519,
0.0736090802221948));
#83962=CARTESIAN_POINT('Ctrl Pts',(0.0140071837705996,-0.0328043479726691,
0.073527923385296));
#83963=CARTESIAN_POINT('Ctrl Pts',(0.0139974932096187,-0.0326943950436593,
0.0734469612035796));
#83964=CARTESIAN_POINT('Ctrl Pts',(0.0139319839682848,-0.0330240426238172,
0.0736208840200798));
#83965=CARTESIAN_POINT('Ctrl Pts',(0.0139246948801687,-0.0329142774063519,
0.0735408703819699));
#83966=CARTESIAN_POINT('Ctrl Pts',(0.0139157480527695,-0.0328043479726691,
0.0734609675399557));
#83967=CARTESIAN_POINT('Ctrl Pts',(0.0139051521286221,-0.0326943950436593,
0.0733812781711779));
#83968=CARTESIAN_POINT('Ctrl Pts',(0.0138424365275337,-0.0330240426238172,
0.0735514405766166));
#83969=CARTESIAN_POINT('Ctrl Pts',(0.0138341907883284,-0.0329142774063519,
0.0734726605417449));
#83970=CARTESIAN_POINT('Ctrl Pts',(0.0138243123349394,-0.0328043479726691,
0.0733940116946154));
#83971=CARTESIAN_POINT('Ctrl Pts',(0.0138128110476255,-0.0326943950436593,
0.0733155951387763));
#83972=CARTESIAN_POINT('',(0.0139521488921328,-0.0326943950436693,0.0734147073871606));
#83973=CARTESIAN_POINT('Ctrl Pts',(0.0140911820786676,-0.0327114338383291,
0.0735253892846446));
#83974=CARTESIAN_POINT('Ctrl Pts',(0.0140484691339741,-0.0327619876830032,
0.0735298600698193));
#83975=CARTESIAN_POINT('Ctrl Pts',(0.014006509736354,-0.0328131562602444,
0.0735342519808468));
#83976=CARTESIAN_POINT('Ctrl Pts',(0.0139240627265978,-0.0329167375858767,
0.073542881750383));
#83977=CARTESIAN_POINT('Ctrl Pts',(0.0138836079658183,-0.0329691088920624,
0.0735471161703238));
#83978=CARTESIAN_POINT('Ctrl Pts',(0.0138438915752594,-0.0330220786163187,
0.0735512733046862));
#83979=CARTESIAN_POINT('Ctrl Pts',(0.0138282507263866,-0.0331951640388604,
0.0734286694459876));
#83980=CARTESIAN_POINT('Ctrl Pts',(0.0138133376796565,-0.0330306422010619,
0.0733107332164269));
#83981=CARTESIAN_POINT('Ctrl Pts',(0.013793562947628,-0.0328657861914645,
0.0731935141344525));
#83982=CARTESIAN_POINT('Ctrl Pts',(0.0138295276982949,-0.0331951640388604,
0.0734270938995663));
#83983=CARTESIAN_POINT('Ctrl Pts',(0.0138145820781527,-0.0330306422010619,
0.0733091312694302));
#83984=CARTESIAN_POINT('Ctrl Pts',(0.0137947737093823,-0.0328657861914645,
0.0731918871557328));
#83985=CARTESIAN_POINT('Ctrl Pts',(0.0140423055593539,-0.0331951640388604,
0.0731645654951962));
#83986=CARTESIAN_POINT('Ctrl Pts',(0.0140219323327688,-0.0330306422010619,
0.0730422038192032));
#83987=CARTESIAN_POINT('Ctrl Pts',(0.0139965191782159,-0.0328657861914645,
0.0729207887472848));
#83988=CARTESIAN_POINT('',(0.0140401871515089,-0.0331781648281943,0.0731519256720257));
#83989=CARTESIAN_POINT('',(0.0140423055593501,-0.0331951640388588,0.0731645654951994));
#83990=CARTESIAN_POINT('Origin',(-0.00211829006564492,-0.0326412093227545,
0.0766001274957886));
#83991=CARTESIAN_POINT('Ctrl Pts',(0.0140401871507031,-0.033178164828644,
0.07315192567368));
#83992=CARTESIAN_POINT('Ctrl Pts',(0.0139978030104248,-0.033127681154676,
0.0731590757243037));
#83993=CARTESIAN_POINT('Ctrl Pts',(0.0139561842020887,-0.0330765663497757,
0.0731660967005014));
#83994=CARTESIAN_POINT('Ctrl Pts',(0.0138744414644628,-0.0329730614463108,
0.0731798863764052));
#83995=CARTESIAN_POINT('Ctrl Pts',(0.0138343505565534,-0.0329207133373549,
0.0731866495000993));
#83996=CARTESIAN_POINT('Ctrl Pts',(0.013795009900406,-0.0328677532289388,
0.0731932861127498));
#83997=CARTESIAN_POINT('',(0.0139359166288323,-0.0331951640388701,0.0732958296973913));
#83998=CARTESIAN_POINT('Origin',(0.00812378219310841,-0.0315241814719618,
0.07415));
#83999=CARTESIAN_POINT('',(0.014040187149871,-0.0332121607144211,0.0731519256716465));
#84000=CARTESIAN_POINT('',(0.01403804175006,-0.0331951640388587,0.073139290401245));
#84001=CARTESIAN_POINT('Origin',(-0.00210312635413019,-0.0326413663376525,
0.0766428616037648));
#84002=CARTESIAN_POINT('Origin',(-0.00235525584752046,-0.032641209647175,
0.0751954430371073));
#84003=CARTESIAN_POINT('Origin',(-0.00235494846232508,-0.0326413667796312,
0.0751500991739546));
#84004=CARTESIAN_POINT('Ctrl Pts',(0.0138195849521744,-0.0337436976235975,
0.0733525315493287));
#84005=CARTESIAN_POINT('Ctrl Pts',(0.0138124124000694,-0.0336723290703325,
0.0733013026360912));
#84006=CARTESIAN_POINT('Ctrl Pts',(0.0138043195616353,-0.033601104548885,
0.0732502110220896));
#84007=CARTESIAN_POINT('Ctrl Pts',(0.0137784807316163,-0.0333736987606857,
0.0730870856192612));
#84008=CARTESIAN_POINT('Ctrl Pts',(0.0137433234057579,-0.0331450831799191,
0.0729257118152436));
#84009=CARTESIAN_POINT('Ctrl Pts',(0.0137795477755188,-0.0337436976235975,
0.073105758324514));
#84010=CARTESIAN_POINT('Ctrl Pts',(0.0137701557076303,-0.0336723290703325,
0.0730548895117111));
#84011=CARTESIAN_POINT('Ctrl Pts',(0.0137598501895499,-0.033601104548885,
0.0730041978619816));
#84012=CARTESIAN_POINT('Ctrl Pts',(0.0137269467117273,-0.0333736987606857,
0.0728423494658455));
#84013=CARTESIAN_POINT('Ctrl Pts',(0.0136848096620531,-0.0331450831799191,
0.0726826559743393));
#84014=CARTESIAN_POINT('Ctrl Pts',(0.0137791474037523,-0.0337436976235975,
0.0731032905922659));
#84015=CARTESIAN_POINT('Ctrl Pts',(0.0137697331407059,-0.0336723290703325,
0.0730524253804672));
#84016=CARTESIAN_POINT('Ctrl Pts',(0.0137594054958291,-0.033601104548885,
0.0730017377303805));
#84017=CARTESIAN_POINT('Ctrl Pts',(0.0137264313715284,-0.0333736987606857,
0.0728399021043113));
#84018=CARTESIAN_POINT('Ctrl Pts',(0.0136842245246161,-0.0331450831799191,
0.0726802254159302));
#84019=CARTESIAN_POINT('',(0.0137728770632737,-0.0336938721132548,0.0730702536650338));
#84020=CARTESIAN_POINT('',(0.0137237464482251,-0.0333679870047996,0.0728390746239767));
#84021=CARTESIAN_POINT('Ctrl Pts',(0.0137728770632776,-0.0336938721132591,
0.0730702536650529));
#84022=CARTESIAN_POINT('Ctrl Pts',(0.0137686623068125,-0.0336629187933937,
0.0730482025977288));
#84023=CARTESIAN_POINT('Ctrl Pts',(0.0137643197804625,-0.0336319952301075,
0.073026183261959));
#84024=CARTESIAN_POINT('Ctrl Pts',(0.0137598501895513,-0.0336011045488985,
0.0730041978619883));
#84025=CARTESIAN_POINT('Ctrl Pts',(0.0137486344565473,-0.0335235892595488,
0.0729490289704813));
#84026=CARTESIAN_POINT('Ctrl Pts',(0.013736598548414,-0.0334458668665605,
0.0728939757672621));
#84027=CARTESIAN_POINT('Ctrl Pts',(0.0137237464511504,-0.0333679869962528,
0.072839074635416));
#84028=CARTESIAN_POINT('Ctrl Pts',(0.0137237369832191,-0.0333679692468935,
0.072839031174882));
#84029=CARTESIAN_POINT('Ctrl Pts',(0.0137232970506411,-0.0333391895415326,
0.0728391402487389));
#84030=CARTESIAN_POINT('Ctrl Pts',(0.013722968081111,-0.0333104081131989,
0.0728392251566906));
#84031=CARTESIAN_POINT('Ctrl Pts',(0.0137225340181308,-0.0332532698752625,
0.072839342909496));
#84032=CARTESIAN_POINT('Ctrl Pts',(0.0137224256564151,-0.0332249173718078,
0.0728393765136672));
#84033=CARTESIAN_POINT('Ctrl Pts',(0.0137224236555687,-0.0331960985265627,
0.0728393840696058));
#84034=CARTESIAN_POINT('Ctrl Pts',(0.0137224236520676,-0.0331956312660268,
0.0728393841851924));
#84035=CARTESIAN_POINT('Ctrl Pts',(0.0137224236774247,-0.0331951640388597,
0.0728393842935123));
#84036=CARTESIAN_POINT('',(0.0137509153232184,-0.0331951640388587,0.072961093890999));
#84037=CARTESIAN_POINT('',(0.0137366695003317,-0.0331951640388687,0.0729002390922664));
#84038=CARTESIAN_POINT('',(0.0137950098854651,-0.0335216366567671,0.0731932861154109));
#84039=CARTESIAN_POINT('Origin',(-0.00238249280895044,-0.0326434571527336,
0.0771504405968173));
#84040=CARTESIAN_POINT('',(0.0137936702784574,-0.0336938721132327,0.0731935121016875));
#84041=CARTESIAN_POINT('Origin',(0.0245620886186969,-0.0336938867896244,
0.0713769228819775));
#84042=CARTESIAN_POINT('',(0.0137832736708755,-0.0336938721132538,0.0731318828833706));
#84043=CARTESIAN_POINT('Ctrl Pts',(0.0140747614774173,-0.0335235895815172,
0.0733845945141182));
#84044=CARTESIAN_POINT('Ctrl Pts',(0.0140642241639594,-0.0334144449262748,
0.0733026675678697));
#84045=CARTESIAN_POINT('Ctrl Pts',(0.0140519821953524,-0.0333049234473147,
0.0732208641904514));
#84046=CARTESIAN_POINT('Ctrl Pts',(0.0140380417500679,-0.0331951640388587,
0.0731392904012499));
#84047=CARTESIAN_POINT('Ctrl Pts',(0.0139810302047748,-0.0335235895815172,
0.0733209107562573));
#84048=CARTESIAN_POINT('Ctrl Pts',(0.0139696161590081,-0.0334144449262748,
0.0732402742055166));
#84049=CARTESIAN_POINT('Ctrl Pts',(0.0139565231094332,-0.0333049234473147,
0.073159780818744));
#84050=CARTESIAN_POINT('Ctrl Pts',(0.0139417584745285,-0.0331951640388587,
0.0730795350388303));
#84051=CARTESIAN_POINT('Ctrl Pts',(0.0138872989321322,-0.0335235895815172,
0.0732572269983964));
#84052=CARTESIAN_POINT('Ctrl Pts',(0.0138750081540568,-0.0334144449262748,
0.0731778808431635));
#84053=CARTESIAN_POINT('Ctrl Pts',(0.013861064023514,-0.0333049234473147,
0.0730986974470365));
#84054=CARTESIAN_POINT('Ctrl Pts',(0.0138454751989892,-0.0331951640388587,
0.0730197796764107));
#84055=CARTESIAN_POINT('Ctrl Pts',(0.0137935676594896,-0.0335235895815172,
0.0731935432405355));
#84056=CARTESIAN_POINT('Ctrl Pts',(0.0137804001491055,-0.0334144449262748,
0.0731154874808105));
#84057=CARTESIAN_POINT('Ctrl Pts',(0.0137656049375948,-0.0333049234473147,
0.0730376140753291));
#84058=CARTESIAN_POINT('Ctrl Pts',(0.0137491919234499,-0.0331951640388587,
0.0729600243139911));
#84059=CARTESIAN_POINT('',(0.0138944785366492,-0.0331951640388687,0.073050192146132));
#84060=CARTESIAN_POINT('Ctrl Pts',(0.014040187146777,-0.0332121607145949,
0.0731519256721623));
#84061=CARTESIAN_POINT('Ctrl Pts',(0.0139978743055216,-0.0332625444108814,
0.0731590636826476));
#84062=CARTESIAN_POINT('Ctrl Pts',(0.0139562905809177,-0.0333135300744919,
0.0731660786940115));
#84063=CARTESIAN_POINT('Ctrl Pts',(0.0138745483561059,-0.033416720314056,
0.0731798682869693));
#84064=CARTESIAN_POINT('Ctrl Pts',(0.0138344215155566,-0.033468884758724,
0.073186637527703));
#84065=CARTESIAN_POINT('Ctrl Pts',(0.0137950098847373,-0.0335216366562299,
0.0731932861153583));
#84066=CARTESIAN_POINT('Ctrl Pts',(0.0137717018154838,-0.0336938721132589,
0.0730719058977375));
#84067=CARTESIAN_POINT('Ctrl Pts',(0.0137653913729524,-0.0336474569765057,
0.0730388467500022));
#84068=CARTESIAN_POINT('Ctrl Pts',(0.0137586943637518,-0.033601104548885,
0.0730058637391982));
#84069=CARTESIAN_POINT('Ctrl Pts',(0.0137417390761985,-0.0334837508592655,
0.0729223583391302));
#84070=CARTESIAN_POINT('Ctrl Pts',(0.0137223167960186,-0.0333660264659096,
0.0728393920288039));
#84071=CARTESIAN_POINT('Ctrl Pts',(0.0137728770632802,-0.0336938721132589,
0.0730702536650682));
#84072=CARTESIAN_POINT('Ctrl Pts',(0.0137665569496827,-0.0336474569765057,
0.0730371876382175));
#84073=CARTESIAN_POINT('Ctrl Pts',(0.0137598501895499,-0.033601104548885,
0.0730041978619816));
#84074=CARTESIAN_POINT('Ctrl Pts',(0.0137428702148784,-0.0334837508592655,
0.0729206753333953));
#84075=CARTESIAN_POINT('Ctrl Pts',(0.0137234227508674,-0.0333660264659096,
0.0728376926336029));
#84076=CARTESIAN_POINT('Ctrl Pts',(0.0139699260031527,-0.0336938721132589,
0.0727932306432676));
#84077=CARTESIAN_POINT('Ctrl Pts',(0.0139619843818822,-0.0336474569765057,
0.0727590112235839));
#84078=CARTESIAN_POINT('Ctrl Pts',(0.013953642723264,-0.033601104548885,
0.0727248871153407));
#84079=CARTESIAN_POINT('Ctrl Pts',(0.0139325235615145,-0.0334837508592655,
0.072638492718912));
#84080=CARTESIAN_POINT('Ctrl Pts',(0.0139088536286531,-0.0333660264659096,
0.0725527620650849));
#84081=CARTESIAN_POINT('',(0.0139658428723954,-0.0336769361243753,0.0727824010019275));
#84082=CARTESIAN_POINT('',(0.0139687507609263,-0.0336938721132327,0.0727948828680808));
#84083=CARTESIAN_POINT('Ctrl Pts',(0.0139658428723954,-0.0336769361243754,
0.0727824010019274));
#84084=CARTESIAN_POINT('Ctrl Pts',(0.0139663297787378,-0.0336797586670034,
0.0727844809510949));
#84085=CARTESIAN_POINT('Ctrl Pts',(0.0139668155558788,-0.0336825812712859,
0.0727865610816272));
#84086=CARTESIAN_POINT('Ctrl Pts',(0.0139677848513756,-0.0336882265979406,
0.072790721701514));
#84087=CARTESIAN_POINT('Ctrl Pts',(0.0139682683697385,-0.0336910493203049,
0.0727928021908584));
#84088=CARTESIAN_POINT('Ctrl Pts',(0.0139687507609291,-0.0336938721132341,
0.0727948828680782));
#84089=CARTESIAN_POINT('Ctrl Pts',(0.0139658428723954,-0.0336769361243753,
0.0727824010019274));
#84090=CARTESIAN_POINT('Ctrl Pts',(0.0139250333282574,-0.0336279018398638,
0.0727919543247597));
#84091=CARTESIAN_POINT('Ctrl Pts',(0.0138836366876243,-0.0335767825795099,
0.0728016450841278));
#84092=CARTESIAN_POINT('Ctrl Pts',(0.0138025230730602,-0.0334733171841404,
0.0728206334007677));
#84093=CARTESIAN_POINT('Ctrl Pts',(0.0137627515838202,-0.0334209631343284,
0.0728299437198176));
#84094=CARTESIAN_POINT('Ctrl Pts',(0.0137237464515687,-0.033367986984468,
0.0728390746382923));
#84095=CARTESIAN_POINT('',(0.01387081391211,-0.0336938721132538,0.0729325682665674));
#84096=CARTESIAN_POINT('Origin',(0.00812378219310841,-0.0315241814719618,
0.07415));
#84097=CARTESIAN_POINT('',(0.0139658428711401,-0.0337108120655386,0.0727824010022275));
#84098=CARTESIAN_POINT('',(0.0139629083290094,-0.0336938721132327,0.0727699253755514));
#84099=CARTESIAN_POINT('Origin',(-0.00221942796324656,-0.0345562523571996,
0.0754234764236254));
#84100=CARTESIAN_POINT('Ctrl Pts',(0.013962908329023,-0.0336938721132379,
0.0727699253755552));
#84101=CARTESIAN_POINT('Ctrl Pts',(0.0139633996084448,-0.0336910492977519,
0.0727720039896108));
#84102=CARTESIAN_POINT('Ctrl Pts',(0.0139638897885156,-0.0336882265866634,
0.0727740829107104));
#84103=CARTESIAN_POINT('Ctrl Pts',(0.0139648679673416,-0.0336825812712735,
0.0727782414422964));
#84104=CARTESIAN_POINT('Ctrl Pts',(0.0139653559660541,-0.0336797586669969,
0.0727803210527646));
#84105=CARTESIAN_POINT('Ctrl Pts',(0.0139658428723954,-0.0336769361243749,
0.0727824010019277));
#84106=CARTESIAN_POINT('Origin',(-0.00170994795491135,-0.0345562520832892,
0.0775998502734302));
#84107=CARTESIAN_POINT('Ctrl Pts',(0.0137582824848021,-0.0342436276873911,
0.0729965133451561));
#84108=CARTESIAN_POINT('Ctrl Pts',(0.0137147780184345,-0.033943005420181,
0.0727840046634048));
#84109=CARTESIAN_POINT('Ctrl Pts',(0.0136553901190583,-0.0336441434784052,
0.0725753766312008));
#84110=CARTESIAN_POINT('Ctrl Pts',(0.0137028314820487,-0.0342436276873911,
0.0727527405281857));
#84111=CARTESIAN_POINT('Ctrl Pts',(0.0136501329723233,-0.033943005420181,
0.07254232321548));
#84112=CARTESIAN_POINT('Ctrl Pts',(0.0135817346793883,-0.0336441434784052,
0.0723364731439784));
#84113=CARTESIAN_POINT('Ctrl Pts',(0.0137022769720212,-0.0342436276873911,
0.0727503028000161));
#84114=CARTESIAN_POINT('Ctrl Pts',(0.0136494865218622,-0.033943005420181,
0.0725399064010008));
#84115=CARTESIAN_POINT('Ctrl Pts',(0.0135809981249916,-0.0336441434784052,
0.0723340841091063));
#84116=CARTESIAN_POINT('',(0.013693932031632,-0.0341934961088741,0.0727176746960286));
#84117=CARTESIAN_POINT('',(0.013630382516674,-0.0338664212865844,0.0724900367830602));
#84118=CARTESIAN_POINT('Origin',(-0.00263298766439013,-0.0345610720407349,
0.0763898453086364));
#84119=CARTESIAN_POINT('Origin',(0.024129938861581,-0.0336938005073086,
0.0693249078803981));
#84120=CARTESIAN_POINT('',(0.0136651594291266,-0.0336938721132327,0.0726101093129251));
#84121=CARTESIAN_POINT('',(0.0136471206126884,-0.0336938721132427,0.0725502690998577));
#84122=CARTESIAN_POINT('',(0.0137237464515699,-0.0340203938281605,0.0728390746382975));
#84123=CARTESIAN_POINT('Origin',(-0.0026649402405618,-0.0345589643241833,
0.0759097247337609));
#84124=CARTESIAN_POINT('',(0.0137224236774251,-0.034193496108874,0.0728393842935138));
#84125=CARTESIAN_POINT('Origin',(0.0244518037981792,-0.0341934220717627,
0.0703276875602538));
#84126=CARTESIAN_POINT('',(0.0137081778545386,-0.0341934961088841,0.0727785294947812));
#84127=CARTESIAN_POINT('Ctrl Pts',(0.0140149588898305,-0.0340223579322397,
0.0730124424726243));
#84128=CARTESIAN_POINT('Ctrl Pts',(0.0139992690046534,-0.0339125849573575,
0.0729311877811427));
#84129=CARTESIAN_POINT('Ctrl Pts',(0.0139819083612731,-0.0338030433565231,
0.0728503149305569));
#84130=CARTESIAN_POINT('Ctrl Pts',(0.0139629083290173,-0.0336938721132327,
0.0727699253755556));
#84131=CARTESIAN_POINT('Ctrl Pts',(0.0139174138366079,-0.0340223579322397,
0.0729547697544411));
#84132=CARTESIAN_POINT('Ctrl Pts',(0.0139009284942303,-0.0339125849573575,
0.0728748604636516));
#84133=CARTESIAN_POINT('Ctrl Pts',(0.0138828007992761,-0.0338030433565231,
0.0727953485324761));
#84134=CARTESIAN_POINT('Ctrl Pts',(0.0138630629477248,-0.0336938721132327,
0.0727163335882615));
#84135=CARTESIAN_POINT('Ctrl Pts',(0.0138198687833854,-0.0340223579322397,
0.0728970970362579));
#84136=CARTESIAN_POINT('Ctrl Pts',(0.0138025879838073,-0.0339125849573575,
0.0728185331461605));
#84137=CARTESIAN_POINT('Ctrl Pts',(0.0137836932372792,-0.0338030433565231,
0.0727403821343953));
#84138=CARTESIAN_POINT('Ctrl Pts',(0.0137632175664323,-0.0336938721132327,
0.0726627418009673));
#84139=CARTESIAN_POINT('Ctrl Pts',(0.0137223237301629,-0.0340223579322397,
0.0728394243180747));
#84140=CARTESIAN_POINT('Ctrl Pts',(0.0137042474733842,-0.0339125849573575,
0.0727622058286694));
#84141=CARTESIAN_POINT('Ctrl Pts',(0.0136845856752823,-0.0338030433565231,
0.0726854157363145));
#84142=CARTESIAN_POINT('Ctrl Pts',(0.0136633721851398,-0.0336938721132327,
0.0726091500136732));
#84143=CARTESIAN_POINT('',(0.013814033879078,-0.0336938721132427,0.0726900173442483));
#84144=CARTESIAN_POINT('Ctrl Pts',(0.0139658428676264,-0.0337108120662662,
0.0727824010030439));
#84145=CARTESIAN_POINT('Ctrl Pts',(0.013923975490418,-0.0337611408993437,
0.0727922019596353));
#84146=CARTESIAN_POINT('Ctrl Pts',(0.0138828720999542,-0.033812108877957,
0.072801824070514));
#84147=CARTESIAN_POINT('Ctrl Pts',(0.0138021558477243,-0.0339153382773235,
0.0728207193664956));
#84148=CARTESIAN_POINT('Ctrl Pts',(0.0137625771340758,-0.0339675558473117,
0.0728299845576844));
#84149=CARTESIAN_POINT('Ctrl Pts',(0.0137237464515299,-0.0340203938281304,
0.0728390746383015));
#84150=CARTESIAN_POINT('Ctrl Pts',(0.0136928625482014,-0.0341934961088741,
0.0727193979450169));
#84151=CARTESIAN_POINT('Ctrl Pts',(0.0136632859777598,-0.0340287516182428,
0.0726042615960629));
#84152=CARTESIAN_POINT('Ctrl Pts',(0.0136289760072808,-0.0338644633275951,
0.0724904460510118));
#84153=CARTESIAN_POINT('Ctrl Pts',(0.0136939320316319,-0.0341934961088741,
0.0727176746960287));
#84154=CARTESIAN_POINT('Ctrl Pts',(0.0136643198343752,-0.0340287516182428,
0.0726025162363473));
#84155=CARTESIAN_POINT('Ctrl Pts',(0.0136299733536702,-0.0338644633275951,
0.0724886800719453));
#84156=CARTESIAN_POINT('Ctrl Pts',(0.0138721285418795,-0.0341934961088741,
0.0724305482691845));
#84157=CARTESIAN_POINT('Ctrl Pts',(0.0138365802319494,-0.0340287516182428,
0.072311705737039));
#84158=CARTESIAN_POINT('Ctrl Pts',(0.0137961504453558,-0.0338644633275951,
0.0721944339921828));
#84159=CARTESIAN_POINT('',(0.0138684426480446,-0.0341764758832429,0.0724182736220124));
#84160=CARTESIAN_POINT('',(0.0138721285418775,-0.034193496108874,0.0724305482691878));
#84161=CARTESIAN_POINT('Origin',(-0.00213246844137344,-0.0345621026629259,
0.0767068832286424));
#84162=CARTESIAN_POINT('Ctrl Pts',(0.0138684426476736,-0.0341764758837534,
0.0724182736237905));
#84163=CARTESIAN_POINT('Ctrl Pts',(0.0138273449891587,-0.0341260050040849,
0.0724306625164513));
#84164=CARTESIAN_POINT('Ctrl Pts',(0.0137869617159301,-0.0340749269148957,
0.0724428360975123));
#84165=CARTESIAN_POINT('Ctrl Pts',(0.0137075925896597,-0.0339715436307851,
0.0724667618954668));
#84166=CARTESIAN_POINT('Ctrl Pts',(0.0136686368456731,-0.0339192778238039,
0.0724785050297447));
#84167=CARTESIAN_POINT('Ctrl Pts',(0.0136303825183667,-0.0338664212856659,
0.0724900367844655));
#84168=CARTESIAN_POINT('',(0.0137830302867648,-0.0341934961088841,0.0725741114826183));
#84169=CARTESIAN_POINT('Origin',(0.00812378219310841,-0.0315241814719618,
0.07415));
#84170=CARTESIAN_POINT('',(0.0138684426470952,-0.0342105180190359,0.0724182736214201));
#84171=CARTESIAN_POINT('',(0.0138647305447434,-0.0341934961088739,0.0724060068739043));
#84172=CARTESIAN_POINT('Origin',(-0.00212448227071318,-0.0345621716560879,
0.076751499706941));
#84173=CARTESIAN_POINT('Origin',(-0.0018368641682059,-0.0345621029931306,
0.0776874954962821));
#84174=CARTESIAN_POINT('Origin',(-0.00185486469899319,-0.0345621722856476,
0.0776458982597908));
#84175=CARTESIAN_POINT('Ctrl Pts',(0.013665592363582,-0.0346945769586966,
0.0726115454875291));
#84176=CARTESIAN_POINT('Ctrl Pts',(0.0136333688178547,-0.0345275153362944,
0.0724954700546888));
#84177=CARTESIAN_POINT('Ctrl Pts',(0.0135974864719452,-0.0343603235965185,
0.0723803779996495));
#84178=CARTESIAN_POINT('Ctrl Pts',(0.0135580565090045,-0.034193496108874,
0.0722666081363406));
#84179=CARTESIAN_POINT('Ctrl Pts',(0.0136413962967475,-0.0346945769586966,
0.0725312798116086));
#84180=CARTESIAN_POINT('Ctrl Pts',(0.0136074915543014,-0.0345275153362944,
0.0724157111750757));
#84181=CARTESIAN_POINT('Ctrl Pts',(0.013569943515107,-0.0343603235965185,
0.0723011789195167));
#84182=CARTESIAN_POINT('Ctrl Pts',(0.0135288682640893,-0.034193496108874,
0.0721880201300037));
#84183=CARTESIAN_POINT('Ctrl Pts',(0.0136172002299135,-0.0346945769586966,
0.0724510141356857));
#84184=CARTESIAN_POINT('Ctrl Pts',(0.0135816142907487,-0.0345275153362944,
0.0723359522954619));
#84185=CARTESIAN_POINT('Ctrl Pts',(0.0135424005582692,-0.0343603235965185,
0.0722219798393845));
#84186=CARTESIAN_POINT('Ctrl Pts',(0.0134996800191743,-0.034193496108874,
0.0721094321236683));
#84187=CARTESIAN_POINT('Ctrl Pts',(0.0135930041630785,-0.0346945769586966,
0.0723707484597675));
#84188=CARTESIAN_POINT('Ctrl Pts',(0.0135557370271948,-0.0345275153362944,
0.0722561934158495));
#84189=CARTESIAN_POINT('Ctrl Pts',(0.0135148576014305,-0.0343603235965185,
0.072142780759251));
#84190=CARTESIAN_POINT('Ctrl Pts',(0.013470491774259,-0.034193496108874,
0.0720308441173299));
#84191=CARTESIAN_POINT('',(0.0135930041633322,-0.0346945769586966,0.07237074846061));
#84192=CARTESIAN_POINT('',(0.0135152865461708,-0.0343667727832834,0.0721475500476732));
#84193=CARTESIAN_POINT('Origin',(-0.00233824736348184,-0.0345626461565297,
0.0777459202266467));
#84194=CARTESIAN_POINT('Origin',(0.0238759442165926,-0.0341934771027844,
0.0682995079518087));
#84195=CARTESIAN_POINT('',(0.0135575342506988,-0.034193496108874,0.072265201979884));
#84196=CARTESIAN_POINT('',(0.0135357736316764,-0.034193496108884,0.0722066125144644));
#84197=CARTESIAN_POINT('',(0.0136303825167689,-0.0345211942962639,0.0724900367849185));
#84198=CARTESIAN_POINT('Origin',(-0.00247383661447089,-0.0345625596118539,
0.0772846114966054));
#84199=CARTESIAN_POINT('',(0.0136290817962303,-0.0346945769586886,0.0724904288867703));
#84200=CARTESIAN_POINT('Origin',(0.0242218213462858,-0.0346945685853862,
0.0692972511550581));
#84201=CARTESIAN_POINT('',(0.0136110429797913,-0.0346945769587026,0.0724305886737002));
#84202=CARTESIAN_POINT('Ctrl Pts',(0.0139319059288102,-0.0345231616327842,
0.0726447762057216));
#84203=CARTESIAN_POINT('Ctrl Pts',(0.0139111585379916,-0.0344132092796988,
0.0725647193972091));
#84204=CARTESIAN_POINT('Ctrl Pts',(0.0138887563057069,-0.0343032738558979,
0.0724850958626736));
#84205=CARTESIAN_POINT('Ctrl Pts',(0.0138647305447509,-0.0341934961088739,
0.0724060068739077));
#84206=CARTESIAN_POINT('Ctrl Pts',(0.0138309322220635,-0.0345231616327842,
0.072593342299737));
#84207=CARTESIAN_POINT('Ctrl Pts',(0.0138094758872641,-0.0344132092796988,
0.0725146772716124));
#84208=CARTESIAN_POINT('Ctrl Pts',(0.0137863935354563,-0.0343032738558979,
0.0724364601096024));
#84209=CARTESIAN_POINT('Ctrl Pts',(0.0137617173045948,-0.0341934961088739,
0.0723587902614548));
#84210=CARTESIAN_POINT('Ctrl Pts',(0.0137299585153168,-0.0345231616327842,
0.0725419083937524));
#84211=CARTESIAN_POINT('Ctrl Pts',(0.0137077932365365,-0.0344132092796988,
0.0724646351460157));
#84212=CARTESIAN_POINT('Ctrl Pts',(0.0136840307652057,-0.0343032738558979,
0.0723878243565312));
#84213=CARTESIAN_POINT('Ctrl Pts',(0.0136587040644386,-0.0341934961088739,
0.0723115736490019));
#84214=CARTESIAN_POINT('Ctrl Pts',(0.0136289848085701,-0.0345231616327842,
0.0724904744877679));
#84215=CARTESIAN_POINT('Ctrl Pts',(0.013606110585809,-0.0344132092796988,
0.072414593020419));
#84216=CARTESIAN_POINT('Ctrl Pts',(0.013581667994955,-0.0343032738558979,
0.0723391886034599));
#84217=CARTESIAN_POINT('Ctrl Pts',(0.0135556908242825,-0.0341934961088739,
0.0722643570365489));
#84218=CARTESIAN_POINT('',(0.0137111323977311,-0.0341934961088839,0.0723356044269041));
#84219=CARTESIAN_POINT('Ctrl Pts',(0.0138684426437819,-0.0342105180195366,
0.0724182736224121));
#84220=CARTESIAN_POINT('Ctrl Pts',(0.0138272987795925,-0.0342610556240338,
0.0724306764294195));
#84221=CARTESIAN_POINT('Ctrl Pts',(0.0137868932207699,-0.0343122189868186,
0.0724428566744688));
#84222=CARTESIAN_POINT('Ctrl Pts',(0.013707523294857,-0.0344158119695113,
0.0724667827176998));
#84223=CARTESIAN_POINT('Ctrl Pts',(0.0136685913908666,-0.0344681990449995,
0.0724785187298886));
#84224=CARTESIAN_POINT('Ctrl Pts',(0.013630382516736,-0.0345211942962405,
0.0724900367849169));
#84225=CARTESIAN_POINT('Ctrl Pts',(0.0135920452288826,-0.0346945769586932,
0.0723725350249574));
#84226=CARTESIAN_POINT('Ctrl Pts',(0.0135552973982297,-0.0345296777077528,
0.0722594825559492));
#84227=CARTESIAN_POINT('Ctrl Pts',(0.01351390840571,-0.0343648066252516,
0.0721480455104717));
#84228=CARTESIAN_POINT('Ctrl Pts',(0.013593004163335,-0.0346945769586932,
0.0723707484606187));
#84229=CARTESIAN_POINT('Ctrl Pts',(0.0135562193967285,-0.0345296777077528,
0.0722576761663191));
#84230=CARTESIAN_POINT('Ctrl Pts',(0.0135147926804191,-0.0343648066252516,
0.0721462208390877));
#84231=CARTESIAN_POINT('Ctrl Pts',(0.0137528202259623,-0.0346945769586932,
0.0720729995607341));
#84232=CARTESIAN_POINT('Ctrl Pts',(0.0137098797115331,-0.0345296777077528,
0.0719566231824231));
#84233=CARTESIAN_POINT('Ctrl Pts',(0.0136621659465823,-0.0343648066252516,
0.0718421210171928));
#84234=CARTESIAN_POINT('',(0.0137483708741045,-0.0346775396665011,0.0720609805737824));
#84235=CARTESIAN_POINT('',(0.0137528202259598,-0.0346945769586885,0.0720729995607336));
#84236=CARTESIAN_POINT('Origin',(-0.00176065482130531,-0.0345626617948099,
0.0779840729315746));
#84237=CARTESIAN_POINT('Ctrl Pts',(0.0137483708737416,-0.0346775396670097,
0.0720609805755654));
#84238=CARTESIAN_POINT('Ctrl Pts',(0.0137081005252722,-0.0346269749928341,
0.072075937334604));
#84239=CARTESIAN_POINT('Ctrl Pts',(0.0136685458832602,-0.0345757902891105,
0.0720906283123326));
#84240=CARTESIAN_POINT('Ctrl Pts',(0.0135908353765566,-0.034472168108849,
0.0721194906424885));
#84241=CARTESIAN_POINT('Ctrl Pts',(0.0135527099760803,-0.0344197714290295,
0.072133650674239));
#84242=CARTESIAN_POINT('Ctrl Pts',(0.013515286546433,-0.0343667727831644,
0.0721475500479254));
#84243=CARTESIAN_POINT('',(0.013672912194656,-0.0346945769587026,0.0722218740106818));
#84244=CARTESIAN_POINT('Origin',(0.00812378219310841,-0.0315241814719618,
0.07415));
#84245=CARTESIAN_POINT('',(0.0137483708727411,-0.0347116136489605,0.072060980573501));
#84246=CARTESIAN_POINT('',(0.0137438958601234,-0.0346945769586885,0.0720489711163712));
#84247=CARTESIAN_POINT('Origin',(-0.00174313866280795,-0.0345626697892552,
0.0780258618694538));
#84248=CARTESIAN_POINT('Origin',(-0.00186699873920255,-0.0345626621421502,
0.0776977502616594));
#84249=CARTESIAN_POINT('Origin',(-0.00188100566606441,-0.0345626702099699,
0.0776546580696877));
#84250=CARTESIAN_POINT('Ctrl Pts',(0.0135701215504443,-0.0352450361874068,
0.0723017169506921));
#84251=CARTESIAN_POINT('Ctrl Pts',(0.0135004124113659,-0.0349452760959492,
0.072096304891175));
#84252=CARTESIAN_POINT('Ctrl Pts',(0.0134154288318132,-0.034644428984174,
0.0718967271632779));
#84253=CARTESIAN_POINT('Ctrl Pts',(0.0135692572954986,-0.0352450361874068,
0.0722993444649938));
#84254=CARTESIAN_POINT('Ctrl Pts',(0.0134994586766537,-0.0349452760959492,
0.0720939650013869));
#84255=CARTESIAN_POINT('Ctrl Pts',(0.0134143883267945,-0.034644428984174,
0.0718944265167805));
#84256=CARTESIAN_POINT('Ctrl Pts',(0.0134836874988876,-0.0352450361874068,
0.0720644448909032));
#84257=CARTESIAN_POINT('Ctrl Pts',(0.0134050294972302,-0.0349452760959492,
0.0718622927451332));
#84258=CARTESIAN_POINT('Ctrl Pts',(0.013311368027917,-0.034644428984174,
0.0716666397348567));
#84259=CARTESIAN_POINT('Ctrl Pts',(0.0134828318009215,-0.0352450361874068,
0.0720620958951623));
#84260=CARTESIAN_POINT('Ctrl Pts',(0.013404085205436,-0.0349452760959492,
0.0718599760225706));
#84261=CARTESIAN_POINT('Ctrl Pts',(0.0133103378249283,-0.034644428984174,
0.0716643618670375));
#84262=CARTESIAN_POINT('',(0.0134705059039946,-0.0351951634053353,0.0720308733256515));
#84263=CARTESIAN_POINT('',(0.0133789127711297,-0.0348678972925388,0.0718129660661543));
#84264=CARTESIAN_POINT('Origin',(-0.00175364642638072,-0.0345636767886418,
0.0790043718872262));
#84265=CARTESIAN_POINT('Origin',(0.0234753725359348,-0.0346946199340819,
0.0673229226914049));
#84266=CARTESIAN_POINT('',(0.0134284645421554,-0.0346945769330288,0.0719277331002202));
#84267=CARTESIAN_POINT('',(0.0134030679965503,-0.0346945769458128,0.0718706256001972));
#84268=CARTESIAN_POINT('',(0.0135152865462252,-0.0350221583435276,0.0721475500479853));
#84269=CARTESIAN_POINT('Origin',(-0.00198618243163102,-0.0345628458712737,
0.0785835745506406));
#84270=CARTESIAN_POINT('',(0.0135141281047203,-0.0351951360298762,0.0721479835292734));
#84271=CARTESIAN_POINT('Origin',(0.0238436625345186,-0.0351951838366798,
0.0683115056739125));
#84272=CARTESIAN_POINT('',(0.013470491774678,-0.0351951371328748,0.0720308441181244));
#84273=CARTESIAN_POINT('Ctrl Pts',(0.0138259308403723,-0.0350241211494342,
0.072283050401166));
#84274=CARTESIAN_POINT('Ctrl Pts',(0.0138002143751275,-0.0349144232818962,
0.0722045056415219));
#84275=CARTESIAN_POINT('Ctrl Pts',(0.0137728589410318,-0.0348045283579412,
0.0721264454467658));
#84276=CARTESIAN_POINT('Ctrl Pts',(0.0137438958562392,-0.0346945769439158,
0.0720489711059647));
#84277=CARTESIAN_POINT('Ctrl Pts',(0.0137219267903495,-0.0350241211494342,
0.072238058186481));
#84278=CARTESIAN_POINT('Ctrl Pts',(0.0136955905757949,-0.0349144232818962,
0.0721609460399827));
#84279=CARTESIAN_POINT('Ctrl Pts',(0.013667644634577,-0.0348045283579412,
0.0720843321265214));
#84280=CARTESIAN_POINT('Ctrl Pts',(0.0136381211101503,-0.0346945769439158,
0.0720083159108078));
#84281=CARTESIAN_POINT('Ctrl Pts',(0.0136179227403266,-0.0350241211494342,
0.0721930659717961));
#84282=CARTESIAN_POINT('Ctrl Pts',(0.0135909667764623,-0.0349144232818962,
0.0721173864384435));
#84283=CARTESIAN_POINT('Ctrl Pts',(0.0135624303281222,-0.0348045283579412,
0.0720422188062771));
#84284=CARTESIAN_POINT('Ctrl Pts',(0.0135323463640614,-0.0346945769439158,
0.0719676607156509));
#84285=CARTESIAN_POINT('Ctrl Pts',(0.0135139186903038,-0.0350241211494342,
0.0721480737571111));
#84286=CARTESIAN_POINT('Ctrl Pts',(0.0134863429771297,-0.0349144232818962,
0.0720738268369042));
#84287=CARTESIAN_POINT('Ctrl Pts',(0.0134572160216674,-0.0348045283579412,
0.0720001054860327));
#84288=CARTESIAN_POINT('Ctrl Pts',(0.0134265716179725,-0.0346945769439158,
0.071927005520494));
#84289=CARTESIAN_POINT('',(0.0135861802013343,-0.0346945769458128,0.0719883521085386));
#84290=CARTESIAN_POINT('Ctrl Pts',(0.0137483708696529,-0.0347116136492775,
0.0720609805746409));
#84291=CARTESIAN_POINT('Ctrl Pts',(0.0137081165090017,-0.0347621546531341,
0.0720759313819251));
#84292=CARTESIAN_POINT('Ctrl Pts',(0.0136685699287866,-0.0348133084095077,
0.072090619313617));
#84293=CARTESIAN_POINT('Ctrl Pts',(0.0135908593246316,-0.0349168561544569,
0.0721194816840003));
#84294=CARTESIAN_POINT('Ctrl Pts',(0.0135527261247601,-0.0349692089015922,
0.0721336446743741));
#84295=CARTESIAN_POINT('Ctrl Pts',(0.0135152865461839,-0.0350221583435,
0.0721475500479793));
#84296=CARTESIAN_POINT('Ctrl Pts',(0.0134698821779314,-0.0351951371254984,
0.0720321740849387));
#84297=CARTESIAN_POINT('Ctrl Pts',(0.0134260974559055,-0.0350307338980976,
0.0719216468220068));
#84298=CARTESIAN_POINT('Ctrl Pts',(0.0133777819366284,-0.0348659306897824,
0.0718130236737781));
#84299=CARTESIAN_POINT('Ctrl Pts',(0.0134704917745731,-0.0351951371254984,
0.072030844118175));
#84300=CARTESIAN_POINT('Ctrl Pts',(0.0134266795563188,-0.0350307338980976,
0.071920304252215));
#84301=CARTESIAN_POINT('Ctrl Pts',(0.013378336043412,-0.0348659306897824,
0.0718116696481763));
#84302=CARTESIAN_POINT('Ctrl Pts',(0.0135726608071045,-0.0351951371254984,
0.0718079403023807));
#84303=CARTESIAN_POINT('Ctrl Pts',(0.0135242401923132,-0.0350307338980976,
0.071695288155776));
#84304=CARTESIAN_POINT('Ctrl Pts',(0.0134712049178788,-0.0348659306897824,
0.0715847335460256));
#84305=CARTESIAN_POINT('Origin',(0.0182382410915186,-0.0308609197410726,
0.069651951223391));
#84306=CARTESIAN_POINT('',(0.0135150351691523,-0.0351951371254984,0.0719336630802996));
#84307=CARTESIAN_POINT('Origin',(0.00729792487674236,-0.0351840467441107,
0.0746722119717951));
#84308=CARTESIAN_POINT('Origin',(0.0187096461764174,-0.0352322614198991,
0.0685725714915023));
#84309=CARTESIAN_POINT('',(0.0132782959248752,-0.0351951142564679,0.0715987644615895));
#84310=CARTESIAN_POINT('',(0.0132205951624505,-0.0351951372916786,0.0714882341283375));
#84311=CARTESIAN_POINT('Origin',(0.00783124796754103,-0.03528751231571,
0.0739755489261077));
#84312=CARTESIAN_POINT('Origin',(0.0102594085301971,-0.0298325076522881,
0.0813426553113457));
#84313=CARTESIAN_POINT('Origin',(0.0164673641357985,-0.0338731817900826,
0.0733520452999505));
#84314=CARTESIAN_POINT('Ctrl Pts',(0.0137934174940089,-0.0321934096636942,
0.0751161114325452));
#84315=CARTESIAN_POINT('Ctrl Pts',(0.013810710428568,-0.032050846084551,
0.075014627660664));
#84316=CARTESIAN_POINT('Ctrl Pts',(0.013825263655493,-0.0319086045665435,
0.0749127557808521));
#84317=CARTESIAN_POINT('Ctrl Pts',(0.0138370638972198,-0.031766989287143,
0.0748107177209326));
#84318=CARTESIAN_POINT('Ctrl Pts',(0.01380570180146,-0.0321934096636942,
0.0750331685098925));
#84319=CARTESIAN_POINT('Ctrl Pts',(0.0138215100972028,-0.032050846084551,
0.074931464854758));
#84320=CARTESIAN_POINT('Ctrl Pts',(0.0138345738969051,-0.0319086045665435,
0.074829413146801));
#84321=CARTESIAN_POINT('Ctrl Pts',(0.0138448831618781,-0.031766989287143,
0.0747272354370263));
#84322=CARTESIAN_POINT('Ctrl Pts',(0.0138179861089111,-0.0321934096636942,
0.0749502255872398));
#84323=CARTESIAN_POINT('Ctrl Pts',(0.0138323097658377,-0.032050846084551,
0.074848302048852));
#84324=CARTESIAN_POINT('Ctrl Pts',(0.0138438841383172,-0.0319086045665435,
0.07474607051275));
#84325=CARTESIAN_POINT('Ctrl Pts',(0.0138527024265365,-0.031766989287143,
0.07464375315312));
#84326=CARTESIAN_POINT('Ctrl Pts',(0.0138302704163622,-0.0321934096636942,
0.0748672826645872));
#84327=CARTESIAN_POINT('Ctrl Pts',(0.0138431094344726,-0.032050846084551,
0.074765139242946));
#84328=CARTESIAN_POINT('Ctrl Pts',(0.0138531943797292,-0.0319086045665435,
0.0746627278786989));
#84329=CARTESIAN_POINT('Ctrl Pts',(0.0138605216911947,-0.031766989287143,
0.0745602708692137));
#84330=CARTESIAN_POINT('',(0.0138300506476721,-0.0321934096636942,0.0748687665298636));
#84331=CARTESIAN_POINT('',(0.0138547629063297,-0.0318665617511349,0.0746337200160556));
#84332=CARTESIAN_POINT('Origin',(-0.00266067940269165,-0.0326371944422615,
0.0721717816860202));
#84333=CARTESIAN_POINT('Origin',(0.0247771115982228,-0.0316939261509145,
0.0755556143725815));
#84334=CARTESIAN_POINT('',(0.0138130737121441,-0.0320197221621798,0.074992348608336));
#84335=CARTESIAN_POINT('Ctrl Pts',(0.0138131465811933,-0.032019739209471,
0.074992178593686));
#84336=CARTESIAN_POINT('Ctrl Pts',(0.0138174318101975,-0.0319792716576008,
0.0749632292717222));
#84337=CARTESIAN_POINT('Ctrl Pts',(0.0138215158492161,-0.0319386439829705,
0.0749341154925669));
#84338=CARTESIAN_POINT('Ctrl Pts',(0.0138253946102038,-0.0318979099381637,
0.0749048055173526));
#84339=CARTESIAN_POINT('Ctrl Pts',(0.013829273294525,-0.0318571766984946,
0.074875496121471));
#84340=CARTESIAN_POINT('Ctrl Pts',(0.0138329287612101,-0.0318163871833603,
0.0748461397405178));
#84341=CARTESIAN_POINT('Ctrl Pts',(0.0138363519311294,-0.0317755399638303,
0.0748168377834398));
#84342=CARTESIAN_POINT('',(0.0138117372188363,-0.0321934096636183,0.0749924177261294));
#84343=CARTESIAN_POINT('Origin',(0.016097707842897,-0.0324112005641101,
0.0753097251637006));
#84344=CARTESIAN_POINT('',(0.0138208939332642,-0.0321934096636663,0.0749305921280065));
#84345=CARTESIAN_POINT('Ctrl Pts',(0.0138284218364189,-0.0321934096636618,
0.0748699751080699));
#84346=CARTESIAN_POINT('Ctrl Pts',(0.0138383508542749,-0.0320835708272592,
0.0747913036814525));
#84347=CARTESIAN_POINT('Ctrl Pts',(0.013846646011812,-0.0319739230346489,
0.0747124724069512));
#84348=CARTESIAN_POINT('Ctrl Pts',(0.0138533044366094,-0.0318646057455573,
0.0746335829582368));
#84349=CARTESIAN_POINT('Ctrl Pts',(0.013919425177682,-0.0321934096636618,
0.0748024506188517));
#84350=CARTESIAN_POINT('Ctrl Pts',(0.0139284229802062,-0.0320835708272592,
0.0747225241852344));
#84351=CARTESIAN_POINT('Ctrl Pts',(0.0139357614902496,-0.0319739230346489,
0.0746424579031413));
#84352=CARTESIAN_POINT('Ctrl Pts',(0.0139414391806242,-0.0318646057455573,
0.0745623549324136));
#84353=CARTESIAN_POINT('Ctrl Pts',(0.0140104285189451,-0.0321934096636618,
0.0747349261296334));
#84354=CARTESIAN_POINT('Ctrl Pts',(0.0140184951061375,-0.0320835708272592,
0.0746537446890163));
#84355=CARTESIAN_POINT('Ctrl Pts',(0.0140248769686871,-0.0319739230346489,
0.0745724433993313));
#84356=CARTESIAN_POINT('Ctrl Pts',(0.0140295739246389,-0.0318646057455573,
0.0744911269065904));
#84357=CARTESIAN_POINT('Ctrl Pts',(0.0141014318602082,-0.0321934096636618,
0.0746674016404153));
#84358=CARTESIAN_POINT('Ctrl Pts',(0.0141085672320688,-0.0320835708272592,
0.0745849651927983));
#84359=CARTESIAN_POINT('Ctrl Pts',(0.0141139924471247,-0.0319739230346489,
0.0745024288955213));
#84360=CARTESIAN_POINT('Ctrl Pts',(0.0141177086686537,-0.0318646057455573,
0.0744198988807672));
#84361=CARTESIAN_POINT('',(0.0141025234007916,-0.0321763980308495,0.0746546320931235));
#84362=CARTESIAN_POINT('',(0.0141014318602036,-0.0321934096636185,0.0746674016403882));
#84363=CARTESIAN_POINT('Origin',(-0.00232360210459169,-0.032638623159475,
0.0726525106268163));
#84364=CARTESIAN_POINT('Ctrl Pts',(0.0141025233976242,-0.0321763980306333,
0.0746546320928512));
#84365=CARTESIAN_POINT('Ctrl Pts',(0.0140597565715851,-0.0321259596175605,
0.0746510223843539));
#84366=CARTESIAN_POINT('Ctrl Pts',(0.0140177307362986,-0.032074916463295,
0.0746474752187469));
#84367=CARTESIAN_POINT('Ctrl Pts',(0.0139351272259753,-0.031971605779401,
0.0746405031186233));
#84368=CARTESIAN_POINT('Ctrl Pts',(0.0138945817362173,-0.0319193786690213,
0.0746370809006859));
#84369=CARTESIAN_POINT('Ctrl Pts',(0.0138547629044771,-0.031866561752542,
0.0746337200158928));
#84370=CARTESIAN_POINT('',(0.0139657412539479,-0.0321934096636664,0.0747680840851359));
#84371=CARTESIAN_POINT('Origin',(0.00812378219310841,-0.0315241814719618,
0.07415));
#84372=CARTESIAN_POINT('',(0.0141025234011606,-0.0322104233323761,0.0746546320931547));
#84373=CARTESIAN_POINT('',(0.0141035876665869,-0.0321934096636183,0.0746418602437372));
#84374=CARTESIAN_POINT('Origin',(-0.0023336699492245,-0.0326387244457676,
0.0726967111254948));
#84375=CARTESIAN_POINT('Origin',(-0.00242680112296162,-0.0326386236421912,
0.0738751690576688));
#84376=CARTESIAN_POINT('Origin',(-0.00242931534677929,-0.0326387248002166,
0.073829906406133));
#84377=CARTESIAN_POINT('Ctrl Pts',(0.013838961113965,-0.0327445246967099,
0.0747940923090646));
#84378=CARTESIAN_POINT('Ctrl Pts',(0.0138632534525274,-0.0324436878339361,
0.0745785408122748));
#84379=CARTESIAN_POINT('Ctrl Pts',(0.0138712405594134,-0.0321434074405928,
0.0743617718762977));
#84380=CARTESIAN_POINT('Ctrl Pts',(0.0138615525804706,-0.0327445246967099,
0.0745451151501902));
#84381=CARTESIAN_POINT('Ctrl Pts',(0.0138764545919749,-0.0324436878339361,
0.0743287116023121));
#84382=CARTESIAN_POINT('Ctrl Pts',(0.01387501386876,-0.0321434074405928,
0.0741118003536464));
#84383=CARTESIAN_POINT('',(0.0138639223541771,-0.0326943950436612,0.074509048647521));
#84384=CARTESIAN_POINT('',(0.0138738271570598,-0.0323666188837389,0.0742729142487172));
#84385=CARTESIAN_POINT('Origin',(-0.00291881110367563,-0.0326395579114917,
0.073535438921432));
#84386=CARTESIAN_POINT('Origin',(0.0249159129258074,-0.0321933825603069,
0.0745089517599611));
#84387=CARTESIAN_POINT('',(0.0138697975139044,-0.0321934096532689,0.0743978566723672));
#84388=CARTESIAN_POINT('',(0.0138711332231658,-0.0321934096584275,0.0743353709441848));
#84389=CARTESIAN_POINT('',(0.0138547629072614,-0.0325210109756238,0.0746337200161324));
#84390=CARTESIAN_POINT('Origin',(-0.00286351017779509,-0.0326393129154698,
0.0730578132976465));
#84391=CARTESIAN_POINT('',(0.0138534091855672,-0.0326943950436595,0.0746336057560539));
#84392=CARTESIAN_POINT('Origin',(0.0248766686670716,-0.0326943765538132,
0.0755640180815124));
#84393=CARTESIAN_POINT('',(0.0138586657698822,-0.0326943950436703,0.0745713272017975));
#84394=CARTESIAN_POINT('Ctrl Pts',(0.0140781488874457,-0.0325229783203769,
0.0748885914090138));
#84395=CARTESIAN_POINT('Ctrl Pts',(0.014088330353867,-0.032413025309245,
0.0748065105943457));
#84396=CARTESIAN_POINT('Ctrl Pts',(0.0140968123289778,-0.032303122220807,
0.0747242316121296));
#84397=CARTESIAN_POINT('Ctrl Pts',(0.0141035876669614,-0.0321934096576658,
0.0746418602392752));
#84398=CARTESIAN_POINT('Ctrl Pts',(0.0140031999771526,-0.0325229783203769,
0.0748035984499946));
#84399=CARTESIAN_POINT('Ctrl Pts',(0.0140122098174925,-0.032413025309245,
0.074722550804416));
#84400=CARTESIAN_POINT('Ctrl Pts',(0.0140195417166517,-0.032303122220807,
0.0746413290711794));
#84401=CARTESIAN_POINT('Ctrl Pts',(0.0140251899541918,-0.0321934096576658,
0.0745600376209509));
#84402=CARTESIAN_POINT('Ctrl Pts',(0.0139282510668594,-0.0325229783203769,
0.0747186054909755));
#84403=CARTESIAN_POINT('Ctrl Pts',(0.0139360892811179,-0.032413025309245,
0.0746385910144862));
#84404=CARTESIAN_POINT('Ctrl Pts',(0.0139422711043256,-0.032303122220807,
0.0745584265302292));
#84405=CARTESIAN_POINT('Ctrl Pts',(0.0139467922414221,-0.0321934096576658,
0.0744782150026266));
#84406=CARTESIAN_POINT('Ctrl Pts',(0.0138533021565663,-0.0325229783203769,
0.0746336125319563));
#84407=CARTESIAN_POINT('Ctrl Pts',(0.0138599687447434,-0.032413025309245,
0.0745546312245564));
#84408=CARTESIAN_POINT('Ctrl Pts',(0.0138650004919996,-0.032303122220807,
0.074475523989279));
#84409=CARTESIAN_POINT('Ctrl Pts',(0.0138683945286525,-0.0321934096576658,
0.0743963923843022));
#84410=CARTESIAN_POINT('',(0.0139866925903711,-0.0321934096584275,0.0745198584585543));
#84411=CARTESIAN_POINT('Ctrl Pts',(0.014102523397689,-0.0322104233328891,
0.0746546320928567));
#84412=CARTESIAN_POINT('Ctrl Pts',(0.0140596986219331,-0.0322609421830332,
0.0746510174931481));
#84413=CARTESIAN_POINT('Ctrl Pts',(0.0140176444772595,-0.0323120888238626,
0.0746474679380973));
#84414=CARTESIAN_POINT('Ctrl Pts',(0.0139350403414708,-0.0324156524631808,
0.0746404957851817));
#84415=CARTESIAN_POINT('Ctrl Pts',(0.0138945243052323,-0.0324680267167313,
0.0746370760532579));
#84416=CARTESIAN_POINT('Ctrl Pts',(0.0138547629072187,-0.0325210109755912,
0.0746337200161243));
#84417=CARTESIAN_POINT('Origin',(0.00652265831989126,-0.0262834582510687,
0.0818532323205447));
#84418=CARTESIAN_POINT('Origin',(0.0185015283592357,-0.0342770720633309,
0.0804844431153851));
#84419=CARTESIAN_POINT('Ctrl Pts',(0.0138623730203407,-0.0326943950436604,
0.0745103567971669));
#84420=CARTESIAN_POINT('Ctrl Pts',(0.0138673394123863,-0.0325844576448134,
0.0744312682603022));
#84421=CARTESIAN_POINT('Ctrl Pts',(0.0138706704753014,-0.0324744968375322,
0.0743520714130887));
#84422=CARTESIAN_POINT('Ctrl Pts',(0.0138723633407325,-0.0323646534831895,
0.0742728677860138));
#84423=CARTESIAN_POINT('Ctrl Pts',(0.0139489567641809,-0.0326943950436604,
0.0744372515108694));
#84424=CARTESIAN_POINT('Ctrl Pts',(0.0139529156283674,-0.0325844576448134,
0.0743569696877393));
#84425=CARTESIAN_POINT('Ctrl Pts',(0.0139552144130027,-0.0324744968375322,
0.0742766003071378));
#84426=CARTESIAN_POINT('Ctrl Pts',(0.01395585159307,-0.0323646534831895,
0.0741962463836274));
#84427=CARTESIAN_POINT('Ctrl Pts',(0.0140355405080212,-0.0326943950436604,
0.0743641462245718));
#84428=CARTESIAN_POINT('Ctrl Pts',(0.0140384918443486,-0.0325844576448134,
0.0742826711151764));
#84429=CARTESIAN_POINT('Ctrl Pts',(0.0140397583507041,-0.0324744968375322,
0.0742011292011868));
#84430=CARTESIAN_POINT('Ctrl Pts',(0.0140393398454075,-0.0323646534831895,
0.0741196249812409));
#84431=CARTESIAN_POINT('Ctrl Pts',(0.0141221242518614,-0.0326943950436604,
0.0742910409382743));
#84432=CARTESIAN_POINT('Ctrl Pts',(0.0141240680603297,-0.0325844576448134,
0.0742083725426135));
#84433=CARTESIAN_POINT('Ctrl Pts',(0.0141243022884054,-0.0324744968375322,
0.0741256580952359));
#84434=CARTESIAN_POINT('Ctrl Pts',(0.0141228280977449,-0.0323646534831895,
0.0740430035788545));
#84435=CARTESIAN_POINT('',(0.0141224118322334,-0.0326773559991375,0.0742782280504027));
#84436=CARTESIAN_POINT('',(0.0141221242518551,-0.0326943950436594,0.0742910409382789));
#84437=CARTESIAN_POINT('Origin',(-0.00248001269496984,-0.0326395671409485,
0.0739735830128659));
#84438=CARTESIAN_POINT('Ctrl Pts',(0.0141224118288766,-0.032677355998747,
0.0742782280503258));
#84439=CARTESIAN_POINT('Ctrl Pts',(0.0140794682075917,-0.0326267922586638,
0.0742773100778611));
#84440=CARTESIAN_POINT('Ctrl Pts',(0.0140372857309823,-0.0325756109580676,
0.0742764083757955));
#84441=CARTESIAN_POINT('Ctrl Pts',(0.0139544071675347,-0.0324719985462378,
0.0742746367450648));
#84442=CARTESIAN_POINT('Ctrl Pts',(0.0139137443211812,-0.0324196091621775,
0.0742737675269559));
#84443=CARTESIAN_POINT('Ctrl Pts',(0.013873827157011,-0.0323666188837757,
0.0742729142487162));
#84444=CARTESIAN_POINT('',(0.0139930233030261,-0.0326943950436702,0.07440004479291));
#84445=CARTESIAN_POINT('Origin',(0.00812378219310841,-0.0315241814719618,
0.07415));
#84446=CARTESIAN_POINT('',(0.0141224118321884,-0.0327114338380032,0.074278228050402));
#84447=CARTESIAN_POINT('',(0.0141226720466812,-0.0326943950436593,0.0742654145775365));
#84448=CARTESIAN_POINT('Origin',(-0.0024802039674448,-0.0326395680058319,
0.0740188921177947));
#84449=CARTESIAN_POINT('Origin',(-0.00247786602655803,-0.0326395674544514,
0.0738731251037909));
#84450=CARTESIAN_POINT('Origin',(-0.00247611923823949,-0.0326395684171705,
0.0738278493802772));
#84451=CARTESIAN_POINT('Ctrl Pts',(0.0138681283410459,-0.0332451089994431,
0.0744339231104998));
#84452=CARTESIAN_POINT('Ctrl Pts',(0.0138788366763559,-0.0329451141710252,
0.0742172715509252));
#84453=CARTESIAN_POINT('Ctrl Pts',(0.0138731955092698,-0.0326442513127493,
0.0740004288799743));
#84454=CARTESIAN_POINT('Ctrl Pts',(0.0138750401189723,-0.0332451089994431,
0.0741840186741128));
#84455=CARTESIAN_POINT('Ctrl Pts',(0.013876323154258,-0.0329451141710252,
0.0739671064325688));
#84456=CARTESIAN_POINT('Ctrl Pts',(0.0138612638277986,-0.0326442513127493,
0.0737507137723472));
#84457=CARTESIAN_POINT('Ctrl Pts',(0.0138751092367515,-0.0332451089994431,
0.074181519629749));
#84458=CARTESIAN_POINT('Ctrl Pts',(0.013876298019037,-0.0329451141710252,
0.0739646047813852));
#84459=CARTESIAN_POINT('Ctrl Pts',(0.0138611445109838,-0.0326442513127493,
0.0737482166212709));
#84460=CARTESIAN_POINT('',(0.0138751403498937,-0.0331951640388616,0.0741479137641467));
#84461=CARTESIAN_POINT('',(0.0138701986143845,-0.0328677532463078,0.0739116233757935));
#84462=CARTESIAN_POINT('Origin',(-0.00287100067133277,-0.0326403163408478,
0.0749219214001807));
#84463=CARTESIAN_POINT('Origin',(0.0249166461355166,-0.0326944278639039,
0.0734528619142166));
#84464=CARTESIAN_POINT('',(0.013874022114592,-0.0326943950436593,0.0740365722900837));
#84465=CARTESIAN_POINT('',(0.0138714316765818,-0.0326943950436693,0.0739741259961216));
#84466=CARTESIAN_POINT('',(0.0138738271570598,-0.0330220786163545,0.07427291424872));
#84467=CARTESIAN_POINT('Origin',(-0.00292227140940239,-0.0326396682764843,
0.0744439292436767));
#84468=CARTESIAN_POINT('',(0.0138724689321763,-0.0331951640388585,0.074272885214998));
#84469=CARTESIAN_POINT('Origin',(0.0249016024348994,-0.033195202656007,
0.0745086472152203));
#84470=CARTESIAN_POINT('',(0.013873804641045,-0.0331951640388701,0.0742103994895824));
#84471=CARTESIAN_POINT('Ctrl Pts',(0.0141127759013865,-0.0330240426238172,
0.0745132552302507));
#84472=CARTESIAN_POINT('Ctrl Pts',(0.0141177800960856,-0.0329142774063519,
0.0744307510071253));
#84473=CARTESIAN_POINT('Ctrl Pts',(0.0141210811928021,-0.0328043479726691,
0.0743481022019528));
#84474=CARTESIAN_POINT('Ctrl Pts',(0.0141226720466888,-0.0326943950436593,
0.0742654145775435));
#84475=CARTESIAN_POINT('Ctrl Pts',(0.0140326381402712,-0.0330240426238172,
0.0744331360987742));
#84476=CARTESIAN_POINT('Ctrl Pts',(0.0140365386158779,-0.0329142774063519,
0.0743517358513826));
#84477=CARTESIAN_POINT('Ctrl Pts',(0.01403875826552,-0.0328043479726691,
0.0742702143892727));
#84478=CARTESIAN_POINT('Ctrl Pts',(0.0140392913695379,-0.0326943950436593,
0.0741886760691986));
#84479=CARTESIAN_POINT('Ctrl Pts',(0.0139525003791559,-0.0330240426238172,
0.0743530169672976));
#84480=CARTESIAN_POINT('Ctrl Pts',(0.0139552971356702,-0.0329142774063519,
0.0742727206956399));
#84481=CARTESIAN_POINT('Ctrl Pts',(0.013956435338238,-0.0328043479726691,
0.0741923265765927));
#84482=CARTESIAN_POINT('Ctrl Pts',(0.013955910692387,-0.0326943950436593,
0.0741119375608538));
#84483=CARTESIAN_POINT('Ctrl Pts',(0.0138723626180405,-0.0330240426238172,
0.0742728978358211));
#84484=CARTESIAN_POINT('Ctrl Pts',(0.0138740556554625,-0.0329142774063519,
0.0741937055398971));
#84485=CARTESIAN_POINT('Ctrl Pts',(0.0138741124109559,-0.0328043479726691,
0.0741144387639126));
#84486=CARTESIAN_POINT('Ctrl Pts',(0.0138725300152361,-0.0326943950436593,
0.0740351990525089));
#84487=CARTESIAN_POINT('',(0.0139983470806466,-0.0326943950436694,0.0741509934338202));
#84488=CARTESIAN_POINT('Ctrl Pts',(0.0141224118288687,-0.0327114338383286,
0.0742782280503256));
#84489=CARTESIAN_POINT('Ctrl Pts',(0.0140794753505426,-0.032761987682999,
0.0742773102305505));
#84490=CARTESIAN_POINT('Ctrl Pts',(0.0140372963628984,-0.0328131562602354,
0.0742764086030658));
#84491=CARTESIAN_POINT('Ctrl Pts',(0.013954417875512,-0.0329167375858764,
0.074274636973961));
#84492=CARTESIAN_POINT('Ctrl Pts',(0.0139137513990614,-0.0329691088920617,
0.0742737676782542));
#84493=CARTESIAN_POINT('Ctrl Pts',(0.0138738271570123,-0.0330220786163186,
0.0742729142487162));
#84494=CARTESIAN_POINT('Ctrl Pts',(0.0138736759789704,-0.0331951640388604,
0.0741493168398912));
#84495=CARTESIAN_POINT('Ctrl Pts',(0.0138736618550735,-0.0330306422053993,
0.0740304414754913));
#84496=CARTESIAN_POINT('Ctrl Pts',(0.0138687344995519,-0.0328657862001531,
0.0739116682730077));
#84497=CARTESIAN_POINT('Ctrl Pts',(0.0138751403498937,-0.0331951640388604,
0.0741479137641499));
#84498=CARTESIAN_POINT('Ctrl Pts',(0.0138750972183061,-0.0330306422053993,
0.0740290081248209));
#84499=CARTESIAN_POINT('Ctrl Pts',(0.0138701396285862,-0.0328657862001531,
0.0739102058721961));
#84500=CARTESIAN_POINT('Ctrl Pts',(0.0141191439277879,-0.0331951640388604,
0.0739141236120178));
#84501=CARTESIAN_POINT('Ctrl Pts',(0.0141142673348248,-0.0330306422053993,
0.0737901733552893));
#84502=CARTESIAN_POINT('Ctrl Pts',(0.0141042719145513,-0.0328657862001531,
0.0736665305678915));
#84503=CARTESIAN_POINT('',(0.014118626414131,-0.0331781648281946,0.0739013179507237));
#84504=CARTESIAN_POINT('',(0.0141191439277825,-0.0331951640388588,0.0739141236120217));
#84505=CARTESIAN_POINT('Origin',(-0.00234461068657464,-0.0326412092868086,
0.0752971355224949));
#84506=CARTESIAN_POINT('Ctrl Pts',(0.0141186264131232,-0.033178164828644,
0.0739013179522645));
#84507=CARTESIAN_POINT('Ctrl Pts',(0.0140756803467012,-0.0331276811561049,
0.0739030994812001));
#84508=CARTESIAN_POINT('Ctrl Pts',(0.0140335097546218,-0.0330765663526692,
0.073904848875029));
#84509=CARTESIAN_POINT('Ctrl Pts',(0.0139506832804901,-0.0329730614522121,
0.0739082847334986));
#84510=CARTESIAN_POINT('Ctrl Pts',(0.0139100608577159,-0.0329207133440476,
0.0739099698047962));
#84511=CARTESIAN_POINT('Ctrl Pts',(0.0138701986272946,-0.0328677532371616,
0.0739116233940857));
#84512=CARTESIAN_POINT('',(0.0139971421388481,-0.0331951640388701,0.0740310186880942));
#84513=CARTESIAN_POINT('Origin',(0.00812378219310841,-0.0315241814719618,
0.07415));
#84514=CARTESIAN_POINT('',(0.0141186264125533,-0.0332121607144208,0.0739013179501391));
#84515=CARTESIAN_POINT('',(0.0141180815491561,-0.0331951640388587,0.0738885134227268));
#84516=CARTESIAN_POINT('Origin',(-0.00233492240592973,-0.0326413664721645,
0.0753414329439625));
#84517=CARTESIAN_POINT('Origin',(-0.00240365414503775,-0.0326412095253733,
0.0738738275177619));
#84518=CARTESIAN_POINT('Origin',(-0.00239766618021565,-0.032641366848677,
0.0738288799872682));
#84519=CARTESIAN_POINT('Ctrl Pts',(0.0138746211457535,-0.0337436976235975,
0.0740726932037927));
#84520=CARTESIAN_POINT('Ctrl Pts',(0.0138739258367123,-0.0336723290703325,
0.0740209692866892));
#84521=CARTESIAN_POINT('Ctrl Pts',(0.0138723002899173,-0.033601104548885,
0.0739692662437147));
#84522=CARTESIAN_POINT('Ctrl Pts',(0.0138671102410036,-0.0333736987606857,
0.073804188669293));
#84523=CARTESIAN_POINT('Ctrl Pts',(0.0138524556418306,-0.0331450831799192,
0.0736396809645867));
#84524=CARTESIAN_POINT('Ctrl Pts',(0.0138658285604175,-0.0337436976235975,
0.0738228478707503));
#84525=CARTESIAN_POINT('Ctrl Pts',(0.0138628861045857,-0.0336723290703325,
0.0737712030354918));
#84526=CARTESIAN_POINT('Ctrl Pts',(0.0138590151969688,-0.033601104548885,
0.0737196194806567));
#84527=CARTESIAN_POINT('Ctrl Pts',(0.0138466561557316,-0.0333736987606857,
0.0735549234081949));
#84528=CARTESIAN_POINT('Ctrl Pts',(0.0138248662709494,-0.0331450831799192,
0.0733912079748788));
#84529=CARTESIAN_POINT('Ctrl Pts',(0.0138657406345641,-0.0337436976235975,
0.0738203494174199));
#84530=CARTESIAN_POINT('Ctrl Pts',(0.0138627757072645,-0.0336723290703325,
0.0737687053729798));
#84531=CARTESIAN_POINT('Ctrl Pts',(0.0138588823460393,-0.033601104548885,
0.0737171230130261));
#84532=CARTESIAN_POINT('Ctrl Pts',(0.0138464516148788,-0.0333736987606857,
0.0735524307555839));
#84533=CARTESIAN_POINT('Ctrl Pts',(0.0138245903772406,-0.0331450831799192,
0.0733887232449818));
#84534=CARTESIAN_POINT('',(0.0138636603625101,-0.0336938721132548,0.0737867871141789));
#84535=CARTESIAN_POINT('',(0.0138438915742658,-0.0333679869984219,0.0735512732946507));
#84536=CARTESIAN_POINT('Ctrl Pts',(0.0138636603625113,-0.0336938721132649,
0.0737867871141894));
#84537=CARTESIAN_POINT('Ctrl Pts',(0.0138622425722313,-0.0336629187933933,
0.0737643816770694));
#84538=CARTESIAN_POINT('Ctrl Pts',(0.0138606940425518,-0.0336319952301041,
0.0737419917074741));
#84539=CARTESIAN_POINT('Ctrl Pts',(0.0138590151969695,-0.0336011045488951,
0.0737196194806673));
#84540=CARTESIAN_POINT('Ctrl Pts',(0.013854802398935,-0.0335235892595454,
0.0736634799082639));
#84541=CARTESIAN_POINT('Ctrl Pts',(0.0138497613933903,-0.0334458668673269,
0.073607352314263));
#84542=CARTESIAN_POINT('Ctrl Pts',(0.013843891574694,-0.0333679869984151,
0.0735512732946152));
#84543=CARTESIAN_POINT('Ctrl Pts',(0.0138438876290188,-0.0333679692463168,
0.0735512289972965));
#84544=CARTESIAN_POINT('Ctrl Pts',(0.0138434374948324,-0.0333391895389005,
0.0735512820729176));
#84545=CARTESIAN_POINT('Ctrl Pts',(0.0138431004775288,-0.0333104081085247,
0.0735513250805207));
#84546=CARTESIAN_POINT('Ctrl Pts',(0.0138426550780635,-0.0332532697574909,
0.0735513875024129));
#84547=CARTESIAN_POINT('Ctrl Pts',(0.0138425433603199,-0.0332249167958317,
0.0735514072639117));
#84548=CARTESIAN_POINT('Ctrl Pts',(0.0138425404278977,-0.0331960985500285,
0.0735514145054824));
#84549=CARTESIAN_POINT('Ctrl Pts',(0.0138425404099617,-0.0331956312423641,
0.0735514146199809));
#84550=CARTESIAN_POINT('Ctrl Pts',(0.0138425404215423,-0.0331951640388589,
0.0735514147306191));
#84551=CARTESIAN_POINT('',(0.0138555531447897,-0.0331951640388587,0.073675735561671));
#84552=CARTESIAN_POINT('',(0.013849046783176,-0.0331951640388687,0.0736135751461546));
#84553=CARTESIAN_POINT('',(0.0138701986059499,-0.0335216366567665,0.0739116233951092));
#84554=CARTESIAN_POINT('Origin',(-0.00267570261449968,-0.0326434571523602,
0.0758099958083109));
#84555=CARTESIAN_POINT('',(0.0138688412385516,-0.0336938721132326,0.0739116797021393));
#84556=CARTESIAN_POINT('Origin',(0.0247800263967618,-0.0336938867896239,
0.0734590558084178));
#84557=CARTESIAN_POINT('',(0.0138662508005408,-0.0336938721132537,0.0738492334081691));
#84558=CARTESIAN_POINT('Ctrl Pts',(0.0141237669728231,-0.0335235895815172,
0.074136485441567));
#84559=CARTESIAN_POINT('Ctrl Pts',(0.0141235809183186,-0.0334144449262748,
0.0740538838381913));
#84560=CARTESIAN_POINT('Ctrl Pts',(0.0141216881630988,-0.0333049234473147,
0.0739711911793267));
#84561=CARTESIAN_POINT('Ctrl Pts',(0.0141180815491639,-0.0331951640388587,
0.0738885134227331));
#84562=CARTESIAN_POINT('Ctrl Pts',(0.0140387564905596,-0.0335235895815172,
0.0740615562056717));
#84563=CARTESIAN_POINT('Ctrl Pts',(0.0140375388876008,-0.0334144449262748,
0.0739801249389546));
#84564=CARTESIAN_POINT('Ctrl Pts',(0.0140346375770773,-0.0333049234473147,
0.0738986252723384));
#84565=CARTESIAN_POINT('Ctrl Pts',(0.0140300468288053,-0.0331951640388587,
0.0738171617549326));
#84566=CARTESIAN_POINT('Ctrl Pts',(0.013953746008296,-0.0335235895815172,
0.0739866269697765));
#84567=CARTESIAN_POINT('Ctrl Pts',(0.0139514968568831,-0.0334144449262748,
0.0739063660397179));
#84568=CARTESIAN_POINT('Ctrl Pts',(0.0139475869910557,-0.0333049234473147,
0.0738260593653501));
#84569=CARTESIAN_POINT('Ctrl Pts',(0.0139420121084467,-0.0331951640388587,
0.073745810087132));
#84570=CARTESIAN_POINT('Ctrl Pts',(0.0138687355260324,-0.0335235895815172,
0.0739116977338812));
#84571=CARTESIAN_POINT('Ctrl Pts',(0.0138654548261653,-0.0334144449262748,
0.0738326071404812));
#84572=CARTESIAN_POINT('Ctrl Pts',(0.0138605364050342,-0.0333049234473147,
0.0737534934583618));
#84573=CARTESIAN_POINT('Ctrl Pts',(0.013853977388088,-0.0331951640388587,
0.0736744584193315));
#84574=CARTESIAN_POINT('',(0.0139868173469829,-0.0331951640388687,0.0737821244922089));
#84575=CARTESIAN_POINT('Ctrl Pts',(0.0141186264094187,-0.0332121607145943,
0.0739013179502668));
#84576=CARTESIAN_POINT('Ctrl Pts',(0.0140757525876135,-0.0332625444108878,
0.0739030964701918));
#84577=CARTESIAN_POINT('Ctrl Pts',(0.0140336175490379,-0.0333135300745024,
0.0739048443434276));
#84578=CARTESIAN_POINT('Ctrl Pts',(0.0139507915918182,-0.033416720314055,
0.0739082801839715));
#84579=CARTESIAN_POINT('Ctrl Pts',(0.013910132752562,-0.033468884758723,
0.0739099668205414));
#84580=CARTESIAN_POINT('Ctrl Pts',(0.0138701986052339,-0.0335216366562289,
0.0739116233949667));
#84581=CARTESIAN_POINT('Ctrl Pts',(0.0138622873042957,-0.033693872113259,
0.0737882790186871));
#84582=CARTESIAN_POINT('Ctrl Pts',(0.0138601700313599,-0.0336474569765058,
0.0737546896440262));
#84583=CARTESIAN_POINT('Ctrl Pts',(0.0138576596974606,-0.033601104548885,
0.0737211273562836));
#84584=CARTESIAN_POINT('Ctrl Pts',(0.0138513041091911,-0.0334837508592655,
0.0736361553601917));
#84585=CARTESIAN_POINT('Ctrl Pts',(0.0138424334154072,-0.0333660264659096,
0.0735514090067958));
#84586=CARTESIAN_POINT('Ctrl Pts',(0.0138636603625123,-0.033693872113259,
0.0737867871142139));
#84587=CARTESIAN_POINT('Ctrl Pts',(0.0138615343569645,-0.0336474569765058,
0.0737531897025877));
#84588=CARTESIAN_POINT('Ctrl Pts',(0.0138590151969688,-0.033601104548885,
0.0737196194806567));
#84589=CARTESIAN_POINT('Ctrl Pts',(0.0138526372630524,-0.0334837508592655,
0.0736346273970239));
#84590=CARTESIAN_POINT('Ctrl Pts',(0.0138437436381987,-0.0333660264659096,
0.0735498616270559));
#84591=CARTESIAN_POINT('Ctrl Pts',(0.0140938757037212,-0.033693872113259,
0.0735366452824997));
#84592=CARTESIAN_POINT('Ctrl Pts',(0.0140902855350262,-0.0336474569765058,
0.0735017003440875));
#84593=CARTESIAN_POINT('Ctrl Pts',(0.0140862865377063,-0.033601104548885,
0.0734667998275823));
#84594=CARTESIAN_POINT('Ctrl Pts',(0.0140761619959217,-0.0334837508592655,
0.0733784397439421));
#84595=CARTESIAN_POINT('Ctrl Pts',(0.0140634236076107,-0.0333660264659096,
0.0732904184727033));
#84596=CARTESIAN_POINT('',(0.014091182083648,-0.0336769361243753,0.0735253892841232));
#84597=CARTESIAN_POINT('',(0.0140925026499634,-0.0336938721132327,0.0735381371821062));
#84598=CARTESIAN_POINT('Ctrl Pts',(0.014091182083648,-0.033676936124375,
0.0735253892841229));
#84599=CARTESIAN_POINT('Ctrl Pts',(0.0140914044638328,-0.0336797586669926,
0.0735275138578085));
#84600=CARTESIAN_POINT('Ctrl Pts',(0.0140916257009893,-0.0336825812712647,
0.0735296384699023));
#84601=CARTESIAN_POINT('Ctrl Pts',(0.0140920658892346,-0.0336882265963423,
0.0735338877658103));
#84602=CARTESIAN_POINT('Ctrl Pts',(0.0140922848403331,-0.0336910493171086,
0.0735360124495905));
#84603=CARTESIAN_POINT('Ctrl Pts',(0.0140925026499678,-0.0336938721132347,
0.0735381371821031));
#84604=CARTESIAN_POINT('Ctrl Pts',(0.014091182083648,-0.0336769361243753,
0.0735253892841232));
#84605=CARTESIAN_POINT('Ctrl Pts',(0.014049494974309,-0.0336278994733738,
0.0735297526946009));
#84606=CARTESIAN_POINT('Ctrl Pts',(0.0140072143570136,-0.0335767852771506,
0.0735341782278523));
#84607=CARTESIAN_POINT('Ctrl Pts',(0.0139243583391074,-0.0334733172093594,
0.0735428508084751));
#84608=CARTESIAN_POINT('Ctrl Pts',(0.0138837335575755,-0.0334209631470897,
0.0735471030245721));
#84609=CARTESIAN_POINT('Ctrl Pts',(0.0138438915753067,-0.033367986984468,
0.0735512733046812));
#84610=CARTESIAN_POINT('',(0.0139780815062468,-0.0336938721132538,0.0736624621481526));
#84611=CARTESIAN_POINT('Origin',(0.00812378219310841,-0.0315241814719618,
0.07415));
#84612=CARTESIAN_POINT('',(0.014091182082366,-0.0337108120655667,0.073525389284263));
#84613=CARTESIAN_POINT('',(0.0140898342906075,-0.0336938721132327,0.0735126442359757));
#84614=CARTESIAN_POINT('Origin',(-0.00229747738884879,-0.0345562524843932,
0.0741170865180477));
#84615=CARTESIAN_POINT('Ctrl Pts',(0.0140898342906212,-0.0336938721132382,
0.0735126442359816));
#84616=CARTESIAN_POINT('Ctrl Pts',(0.0140900611768464,-0.0336910492963934,
0.0735147680342053));
#84617=CARTESIAN_POINT('Ctrl Pts',(0.0140902869337414,-0.0336882265859841,
0.073516891997733));
#84618=CARTESIAN_POINT('Ctrl Pts',(0.014090736197069,-0.0336825812712925,
0.0735211403358452));
#84619=CARTESIAN_POINT('Ctrl Pts',(0.0140909597034621,-0.0336797586670065,
0.0735232647104274));
#84620=CARTESIAN_POINT('Ctrl Pts',(0.014091182083648,-0.033676936124375,
0.0735253892841235));
#84621=CARTESIAN_POINT('Origin',(-0.00206478689373644,-0.0345562520240462,
0.0763401538921394));
#84622=CARTESIAN_POINT('Ctrl Pts',(0.0138584229793833,-0.034243627687391,
0.0737117990730362));
#84623=CARTESIAN_POINT('Ctrl Pts',(0.0138418959589715,-0.033943005420181,
0.0734955135302695));
#84624=CARTESIAN_POINT('Ctrl Pts',(0.0138091243768085,-0.0336441434784052,
0.0732810873149503));
#84625=CARTESIAN_POINT('Ctrl Pts',(0.013833962059755,-0.034243627687391,
0.0734629986240596));
#84626=CARTESIAN_POINT('Ctrl Pts',(0.0138080513757184,-0.033943005420181,
0.0732476356400853));
#84627=CARTESIAN_POINT('Ctrl Pts',(0.0137659922788434,-0.0336441434784052,
0.0730348361786582));
#84628=CARTESIAN_POINT('Ctrl Pts',(0.0138337174505587,-0.034243627687391,
0.0734605106195699));
#84629=CARTESIAN_POINT('Ctrl Pts',(0.0138077129298858,-0.033943005420181,
0.0732451568611834));
#84630=CARTESIAN_POINT('Ctrl Pts',(0.0137655609578638,-0.0336441434784052,
0.0730323736672953));
#84631=CARTESIAN_POINT('',(0.0138295276982948,-0.0341934961088741,0.0734270938995651));
#84632=CARTESIAN_POINT('',(0.0137950098862559,-0.0338664212872184,0.0731932861130012));
#84633=CARTESIAN_POINT('Origin',(-0.00282889432060436,-0.0345610751539435,
0.0750239983549795));
#84634=CARTESIAN_POINT('Origin',(0.0246084682439468,-0.0336938005063909,
0.0713690468206104));
#84635=CARTESIAN_POINT('',(0.0138144634936381,-0.0336938721132327,0.0733167705383256));
#84636=CARTESIAN_POINT('',(0.0138040668860578,-0.0336938721132427,0.0732551413200166));
#84637=CARTESIAN_POINT('',(0.0138438915753073,-0.0340203938281605,0.0735512733046865));
#84638=CARTESIAN_POINT('Origin',(-0.00280041993298706,-0.0345589643241736,
0.074543663310025));
#84639=CARTESIAN_POINT('',(0.0138425404215422,-0.034193496108874,0.0735514147306181));
#84640=CARTESIAN_POINT('Origin',(0.0248021152592256,-0.0341934220717659,
0.0724042714765647));
#84641=CARTESIAN_POINT('',(0.0138360340599285,-0.034193496108884,0.0734892543151016));
#84642=CARTESIAN_POINT('Ctrl Pts',(0.0141110789652396,-0.0340223579322397,
0.0737597726783989));
#84643=CARTESIAN_POINT('Ctrl Pts',(0.0141056967127191,-0.0339125849573575,
0.0736771922403857));
#84644=CARTESIAN_POINT('Ctrl Pts',(0.0140986090190687,-0.0338030433565231,
0.0735947812308107));
#84645=CARTESIAN_POINT('Ctrl Pts',(0.0140898342906155,-0.0336938721132327,
0.0735126442359814));
#84646=CARTESIAN_POINT('Ctrl Pts',(0.0140215313921552,-0.0340223579322397,
0.0736903290898859));
#84647=CARTESIAN_POINT('Ctrl Pts',(0.0140151913314326,-0.0339125849573575,
0.0736089837464554));
#84648=CARTESIAN_POINT('Ctrl Pts',(0.0140071720662088,-0.0338030433565231,
0.0735278267879805));
#84649=CARTESIAN_POINT('Ctrl Pts',(0.0139974930519707,-0.0336938721132327,
0.0734469610914432));
#84650=CARTESIAN_POINT('Ctrl Pts',(0.0139319838190708,-0.0340223579322397,
0.0736208855013728));
#84651=CARTESIAN_POINT('Ctrl Pts',(0.0139246859501462,-0.0339125849573575,
0.073540775252525));
#84652=CARTESIAN_POINT('Ctrl Pts',(0.0139157351133489,-0.0338030433565231,
0.0734608723451504));
#84653=CARTESIAN_POINT('Ctrl Pts',(0.013905151813326,-0.0336938721132327,
0.073381277946905));
#84654=CARTESIAN_POINT('Ctrl Pts',(0.0138424362459864,-0.0340223579322397,
0.0735514419128598));
#84655=CARTESIAN_POINT('Ctrl Pts',(0.0138341805688597,-0.0339125849573575,
0.0734725667585947));
#84656=CARTESIAN_POINT('Ctrl Pts',(0.013824298160489,-0.0338030433565231,
0.0733939179023202));
#84657=CARTESIAN_POINT('Ctrl Pts',(0.0138128105746813,-0.0336938721132327,
0.0733155948023667));
#84658=CARTESIAN_POINT('',(0.0139521488921328,-0.0336938721132427,0.0734147073871607));
#84659=CARTESIAN_POINT('Ctrl Pts',(0.0140911820787772,-0.0337108120662658,
0.0735253892846331));
#84660=CARTESIAN_POINT('Ctrl Pts',(0.0140484164527642,-0.0337611408993402,
0.0735298655839877));
#84661=CARTESIAN_POINT('Ctrl Pts',(0.0140064312045429,-0.033812108877951,
0.0735342602008106));
#84662=CARTESIAN_POINT('Ctrl Pts',(0.0139239832155212,-0.0339153382773235,
0.073542890072847));
#84663=CARTESIAN_POINT('Ctrl Pts',(0.0138835553554806,-0.0339675558473112,
0.073547121677074));
#84664=CARTESIAN_POINT('Ctrl Pts',(0.0138438915752671,-0.0340203938281304,
0.0735512733046854));
#84665=CARTESIAN_POINT('Ctrl Pts',(0.0138282506681329,-0.0341934961088741,
0.0734286695178605));
#84666=CARTESIAN_POINT('Ctrl Pts',(0.0138133377287219,-0.0340287516186244,
0.0733107341264604));
#84667=CARTESIAN_POINT('Ctrl Pts',(0.0137935631729445,-0.0338644633283559,
0.0731935158716945));
#84668=CARTESIAN_POINT('Ctrl Pts',(0.0138295276982948,-0.0341934961088741,
0.0734270938995652));
#84669=CARTESIAN_POINT('Ctrl Pts',(0.0138145821842169,-0.0340287516186244,
0.0733091321065726));
#84670=CARTESIAN_POINT('Ctrl Pts',(0.0137947739904092,-0.0338644633283559,
0.0731918888191096));
#84671=CARTESIAN_POINT('Ctrl Pts',(0.0140423055593536,-0.0341934961088741,
0.073164565495195));
#84672=CARTESIAN_POINT('Ctrl Pts',(0.014021932477351,-0.0340287516186244,
0.0730422046875642));
#84673=CARTESIAN_POINT('Ctrl Pts',(0.0139965195387595,-0.0338644633283559,
0.0729207904698361));
#84674=CARTESIAN_POINT('',(0.0140401871511133,-0.0341764758832433,0.07315192567229));
#84675=CARTESIAN_POINT('',(0.0140423055593501,-0.034193496108874,0.0731645654951994));
#84676=CARTESIAN_POINT('Origin',(-0.00237205740712093,-0.0345621027371333,
0.0754012723049952));
#84677=CARTESIAN_POINT('Ctrl Pts',(0.0140401871505218,-0.0341764758837539,
0.0731519256740081));
#84678=CARTESIAN_POINT('Ctrl Pts',(0.0139978608193925,-0.0341260050041454,
0.0731590659741078));
#84679=CARTESIAN_POINT('Ctrl Pts',(0.0139562702261054,-0.0340749269150179,
0.0731660821966222));
#84680=CARTESIAN_POINT('Ctrl Pts',(0.0138745282515552,-0.0339715436310111,
0.07317987174326));
#84681=CARTESIAN_POINT('Ctrl Pts',(0.0138344078804317,-0.0339192778242667,
0.073186639830027));
#84682=CARTESIAN_POINT('Ctrl Pts',(0.0137950098878868,-0.0338664212862372,
0.073193286114866));
#84683=CARTESIAN_POINT('',(0.0139359166288325,-0.0341934961088841,0.0732958296973923));
#84684=CARTESIAN_POINT('Origin',(0.00812378219310841,-0.0315241814719618,
0.07415));
#84685=CARTESIAN_POINT('',(0.0140401871502457,-0.0342105180190355,0.0731519256715834));
#84686=CARTESIAN_POINT('',(0.0140380417500601,-0.0341934961088739,0.0731392904012451));
#84687=CARTESIAN_POINT('Origin',(-0.00236972593437885,-0.0345621716939992,
0.0754465379162919));
#84688=CARTESIAN_POINT('Origin',(-0.00220168714295083,-0.0345621031391709,
0.0764112014501524));
#84689=CARTESIAN_POINT('Origin',(-0.00221433234995836,-0.0345621722388305,
0.0763676759181593));
#84690=CARTESIAN_POINT('Ctrl Pts',(0.0138147130138689,-0.0346945769586965,
0.0733182496493391));
#84691=CARTESIAN_POINT('Ctrl Pts',(0.0137972916697596,-0.0345275153362944,
0.0731990508247738));
#84692=CARTESIAN_POINT('Ctrl Pts',(0.0137761171262808,-0.0343603235965186,
0.0730803690545241));
#84693=CARTESIAN_POINT('Ctrl Pts',(0.0137512572252257,-0.034193496108874,
0.0729625544158142));
#84694=CARTESIAN_POINT('Ctrl Pts',(0.0138007676969557,-0.0346945769586965,
0.0732355843209515));
#84695=CARTESIAN_POINT('Ctrl Pts',(0.013781614894446,-0.0345275153362944,
0.0731166775866324));
#84696=CARTESIAN_POINT('Ctrl Pts',(0.0137587176306923,-0.0343603235965186,
0.0729983424349513));
#84697=CARTESIAN_POINT('Ctrl Pts',(0.0137321488272934,-0.034193496108874,
0.0728809278422631));
#84698=CARTESIAN_POINT('Ctrl Pts',(0.0137868223800424,-0.0346945769586965,
0.0731529189925634));
#84699=CARTESIAN_POINT('Ctrl Pts',(0.0137659381191324,-0.0345275153362944,
0.0730343043484912));
#84700=CARTESIAN_POINT('Ctrl Pts',(0.0137413181351039,-0.0343603235965186,
0.0729163158153789));
#84701=CARTESIAN_POINT('Ctrl Pts',(0.0137130404293612,-0.034193496108874,
0.0727993012687119));
#84702=CARTESIAN_POINT('Ctrl Pts',(0.0137728770631294,-0.0346945769586965,
0.0730702536641762));
#84703=CARTESIAN_POINT('Ctrl Pts',(0.0137502613438188,-0.0345275153362944,
0.0729519311103494));
#84704=CARTESIAN_POINT('Ctrl Pts',(0.0137239186395152,-0.0343603235965186,
0.0728342891958057));
#84705=CARTESIAN_POINT('Ctrl Pts',(0.0136939320314287,-0.034193496108874,
0.0727176746951608));
#84706=CARTESIAN_POINT('',(0.0137728770632756,-0.0346945769586966,0.0730702536650438));
#84707=CARTESIAN_POINT('',(0.0137237464515596,-0.034366772783284,0.0728390746379946));
#84708=CARTESIAN_POINT('Origin',(-0.0027064394453972,-0.0345626461567451,
0.0764063253273736));
#84709=CARTESIAN_POINT('Origin',(0.0244849948321285,-0.0341934771027848,
0.0703199103678021));
#84710=CARTESIAN_POINT('',(0.0137509153232184,-0.034193496108874,0.072961093890999));
#84711=CARTESIAN_POINT('',(0.0137366695003317,-0.0341934961088841,0.0729002390922665));
#84712=CARTESIAN_POINT('',(0.0137950098858203,-0.0345211942962632,0.0731932861151862));
#84713=CARTESIAN_POINT('Origin',(-0.00278314221978826,-0.0345625596120791,
0.0759316603151603));
#84714=CARTESIAN_POINT('',(0.0137936702784574,-0.0346945769586885,0.0731935121016875));
#84715=CARTESIAN_POINT('Origin',(0.0247030942457456,-0.0346945685853855,
0.0713531360797733));
#84716=CARTESIAN_POINT('',(0.0137832736708765,-0.0346945769587026,0.0731318828833757));
#84717=CARTESIAN_POINT('Ctrl Pts',(0.0140747617037272,-0.0345231616327842,
0.0733845962736656));
#84718=CARTESIAN_POINT('Ctrl Pts',(0.014064211690962,-0.0344132092796988,
0.0733025703994207));
#84719=CARTESIAN_POINT('Ctrl Pts',(0.0140519655820212,-0.034303273855898,
0.0732207669760262));
#84720=CARTESIAN_POINT('Ctrl Pts',(0.0140380417500679,-0.0341934961088739,
0.0731392904012499));
#84721=CARTESIAN_POINT('Ctrl Pts',(0.0139810305825693,-0.0345231616327842,
0.0733209125782205));
#84722=CARTESIAN_POINT('Ctrl Pts',(0.0139696027797218,-0.0344132092796988,
0.073240178655518));
#84723=CARTESIAN_POINT('Ctrl Pts',(0.0139565056489873,-0.034303273855898,
0.0731596852734025));
#84724=CARTESIAN_POINT('Ctrl Pts',(0.0139417586107953,-0.0341934961088739,
0.0730795351234002));
#84725=CARTESIAN_POINT('Ctrl Pts',(0.0138872994614113,-0.0345231616327842,
0.0732572288827755));
#84726=CARTESIAN_POINT('Ctrl Pts',(0.0138749938684816,-0.0344132092796988,
0.0731777869116153));
#84727=CARTESIAN_POINT('Ctrl Pts',(0.0138610457159534,-0.034303273855898,
0.0730986035707788));
#84728=CARTESIAN_POINT('Ctrl Pts',(0.0138454754715228,-0.0341934961088739,
0.0730197798455506));
#84729=CARTESIAN_POINT('Ctrl Pts',(0.0137935683402534,-0.0345231616327842,
0.0731935451873305));
#84730=CARTESIAN_POINT('Ctrl Pts',(0.0137803849572414,-0.0344132092796988,
0.0731153951677126));
#84731=CARTESIAN_POINT('Ctrl Pts',(0.0137655857829194,-0.034303273855898,
0.0730375218681551));
#84732=CARTESIAN_POINT('Ctrl Pts',(0.0137491923322503,-0.0341934961088739,
0.072960024567701));
#84733=CARTESIAN_POINT('',(0.0138944785366492,-0.0341934961088839,0.073050192146132));
#84734=CARTESIAN_POINT('Ctrl Pts',(0.0140401871468337,-0.034210518019536,
0.0731519256721527));
#84735=CARTESIAN_POINT('Ctrl Pts',(0.0139978132303992,-0.0342610556240281,
0.0731590739857814));
#84736=CARTESIAN_POINT('Ctrl Pts',(0.0139561996919832,-0.0343122189868071,
0.0731660940266185));
#84737=CARTESIAN_POINT('Ctrl Pts',(0.0138744568932699,-0.0344158119695103,
0.0731798837163913));
#84738=CARTESIAN_POINT('Ctrl Pts',(0.0138343610666141,-0.0344681990449984,
0.0731866477252027));
#84739=CARTESIAN_POINT('Ctrl Pts',(0.0137950098857875,-0.0345211942962394,
0.0731932861151812));
#84740=CARTESIAN_POINT('Ctrl Pts',(0.0137717017744239,-0.0346945769586932,
0.0730719059554424));
#84741=CARTESIAN_POINT('Ctrl Pts',(0.013749412942895,-0.0345296777077528,
0.0729551392144772));
#84742=CARTESIAN_POINT('Ctrl Pts',(0.0137223170801922,-0.0343648066252516,
0.0728393934671215));
#84743=CARTESIAN_POINT('Ctrl Pts',(0.0137728770632773,-0.0346945769586932,
0.0730702536650528));
#84744=CARTESIAN_POINT('Ctrl Pts',(0.0137505540718136,-0.0345296777077528,
0.0729534626258222));
#84745=CARTESIAN_POINT('Ctrl Pts',(0.0137234230740957,-0.0343648066252516,
0.0728376940128251));
#84746=CARTESIAN_POINT('Ctrl Pts',(0.0139687507609298,-0.0346945769586932,
0.0727948828680803));
#84747=CARTESIAN_POINT('Ctrl Pts',(0.0139407346730868,-0.0345296777077528,
0.0726740422787478));
#84748=CARTESIAN_POINT('Ctrl Pts',(0.0139077480720424,-0.0343648066252516,
0.0725544628768436));
#84749=CARTESIAN_POINT('',(0.0139658428720393,-0.0346775396665016,0.0727824010027757));
#84750=CARTESIAN_POINT('',(0.0139687507609263,-0.0346945769586886,0.0727948828680809));
#84751=CARTESIAN_POINT('Origin',(-0.00216324988500243,-0.0345626618546312,
0.0767149915967936));
#84752=CARTESIAN_POINT('Ctrl Pts',(0.0139658428714545,-0.0346775396670097,
0.0727824010045));
#84753=CARTESIAN_POINT('Ctrl Pts',(0.013924015487737,-0.0346269749928339,
0.0727921926120357));
#84754=CARTESIAN_POINT('Ctrl Pts',(0.0138829314781485,-0.03457579028911,
0.0728018102358312));
#84755=CARTESIAN_POINT('Ctrl Pts',(0.0138022163328588,-0.0344721681088797,
0.0728207052688002));
#84756=CARTESIAN_POINT('Ctrl Pts',(0.0137626168400041,-0.0344197714290866,
0.0728299752647442));
#84757=CARTESIAN_POINT('Ctrl Pts',(0.0137237464517877,-0.0343667727831654,
0.0728390746382783));
#84758=CARTESIAN_POINT('',(0.013870813912111,-0.0346945769587026,0.0729325682665724));
#84759=CARTESIAN_POINT('Origin',(0.00812378219310841,-0.0315241814719618,
0.07415));
#84760=CARTESIAN_POINT('',(0.0139658428707218,-0.0347116136489602,0.0727824010023258));
#84761=CARTESIAN_POINT('',(0.0139629083290095,-0.0346945769586885,0.0727699253755514));
#84762=CARTESIAN_POINT('Origin',(-0.00215110916414497,-0.034562669838981,
0.0767586463341342));
#84763=CARTESIAN_POINT('Origin',(-0.0022328693252026,-0.0345626621621979,
0.0764175983069814));
#84764=CARTESIAN_POINT('Origin',(-0.00224136492537223,-0.0345626702062483,
0.0763730903455221));
#84765=CARTESIAN_POINT('Ctrl Pts',(0.0137588268289809,-0.0352450361874068,
0.0729988985373347));
#84766=CARTESIAN_POINT('Ctrl Pts',(0.0137154123249175,-0.0349452760959493,
0.0727863693414509));
#84767=CARTESIAN_POINT('Ctrl Pts',(0.0136561125882577,-0.034644428984174,
0.072577714076724));
#84768=CARTESIAN_POINT('Ctrl Pts',(0.0137582667402476,-0.0352450361874068,
0.0729964364395278));
#84769=CARTESIAN_POINT('Ctrl Pts',(0.0137147593766418,-0.0349452760959493,
0.0727839283677371));
#84770=CARTESIAN_POINT('Ctrl Pts',(0.0136553686353968,-0.034644428984174,
0.0725753011616529));
#84771=CARTESIAN_POINT('Ctrl Pts',(0.0137028124102251,-0.0352450361874068,
0.0727526643794353));
#84772=CARTESIAN_POINT('Ctrl Pts',(0.0136501110325061,-0.0349452760959493,
0.0725422478020213));
#84773=CARTESIAN_POINT('Ctrl Pts',(0.0135817099362883,-0.034644428984174,
0.0723363986793601));
#84774=CARTESIAN_POINT('Ctrl Pts',(0.0137022578669249,-0.0352450361874068,
0.0727502266588344));
#84775=CARTESIAN_POINT('Ctrl Pts',(0.0136494645490647,-0.0349452760959493,
0.0725398309963641));
#84776=CARTESIAN_POINT('Ctrl Pts',(0.0135809733492973,-0.034644428984174,
0.0723340096545372));
#84777=CARTESIAN_POINT('',(0.0136939423889737,-0.0351951634053355,0.0727177054440917));
#84778=CARTESIAN_POINT('',(0.013630382516768,-0.0348678972925434,0.0724900367849038));
#84779=CARTESIAN_POINT('Origin',(-0.00228417407676976,-0.0345636767881962,
0.0777281236473546));
#84780=CARTESIAN_POINT('Origin',(0.0242099803342668,-0.0346946199340747,
0.0693008206829229));
#84781=CARTESIAN_POINT('',(0.013665159433795,-0.0346945769330288,0.0726101093303203));
#84782=CARTESIAN_POINT('',(0.0136471206151762,-0.0346945769458128,0.0725502691088101));
#84783=CARTESIAN_POINT('',(0.0137237464515733,-0.0350221583435275,0.0728390746383119));
#84784=CARTESIAN_POINT('Origin',(-0.00246213657583445,-0.0345628458712538,
0.0772814999335259));
#84785=CARTESIAN_POINT('',(0.0137225428151149,-0.0351951360298762,0.0728393595102533));
#84786=CARTESIAN_POINT('Origin',(0.0244514640108223,-0.0351951838366837,
0.0703277676145716));
#84787=CARTESIAN_POINT('',(0.0136939320317448,-0.0351951371328747,0.0727176746960014));
#84788=CARTESIAN_POINT('Ctrl Pts',(0.0140149585252636,-0.0350241211494342,
0.07301244058461));
#84789=CARTESIAN_POINT('Ctrl Pts',(0.0139992891107342,-0.0349144232818962,
0.0729312920461109));
#84790=CARTESIAN_POINT('Ctrl Pts',(0.0139819329190284,-0.0348045283579412,
0.0728504188342951));
#84791=CARTESIAN_POINT('Ctrl Pts',(0.0139629083264611,-0.0346945769439157,
0.0727699253647406));
#84792=CARTESIAN_POINT('Ctrl Pts',(0.0139174135979912,-0.0350241211494342,
0.072954767983083));
#84793=CARTESIAN_POINT('Ctrl Pts',(0.0139009497670223,-0.0349144232818962,
0.0728749630859621));
#84794=CARTESIAN_POINT('Ctrl Pts',(0.0138828264574081,-0.0348045283579412,
0.0727954507409142));
#84795=CARTESIAN_POINT('Ctrl Pts',(0.0138630630929085,-0.0346945769439157,
0.0727163336569837));
#84796=CARTESIAN_POINT('Ctrl Pts',(0.0138198686707187,-0.0350241211494342,
0.0728970953815561));
#84797=CARTESIAN_POINT('Ctrl Pts',(0.0138026104233105,-0.0349144232818962,
0.0728186341258134));
#84798=CARTESIAN_POINT('Ctrl Pts',(0.0137837199957878,-0.0348045283579412,
0.0727404826475332));
#84799=CARTESIAN_POINT('Ctrl Pts',(0.0137632178593558,-0.0346945769439157,
0.0726627419492268));
#84800=CARTESIAN_POINT('Ctrl Pts',(0.0137223237434462,-0.0350241211494342,
0.0728394227800291));
#84801=CARTESIAN_POINT('Ctrl Pts',(0.0137042710795987,-0.0349144232818962,
0.0727623051656646));
#84802=CARTESIAN_POINT('Ctrl Pts',(0.0136846135341675,-0.0348045283579412,
0.0726855145541522));
#84803=CARTESIAN_POINT('Ctrl Pts',(0.0136633726258032,-0.0346945769439157,
0.07260915024147));
#84804=CARTESIAN_POINT('',(0.0138140338815658,-0.0346945769458128,0.0726900173532006));
#84805=CARTESIAN_POINT('Ctrl Pts',(0.0139658428675145,-0.0347116136492769,
0.0727824010030701));
#84806=CARTESIAN_POINT('Ctrl Pts',(0.0139240320915038,-0.0347621546531278,
0.0727921887095867));
#84807=CARTESIAN_POINT('Ctrl Pts',(0.0138829564619176,-0.0348133084094943,
0.0728018043217741));
#84808=CARTESIAN_POINT('Ctrl Pts',(0.0138022412148688,-0.0349168561544567,
0.0728206993824475));
#84809=CARTESIAN_POINT('Ctrl Pts',(0.0137626336132877,-0.0349692089015918,
0.0728299713361659));
#84810=CARTESIAN_POINT('Ctrl Pts',(0.0137237464515331,-0.0350221583434999,
0.0728390746383007));
#84811=CARTESIAN_POINT('Ctrl Pts',(0.0136931605528093,-0.0351951371254986,
0.0727189177728991));
#84812=CARTESIAN_POINT('Ctrl Pts',(0.0136635738256549,-0.035030733898099,
0.0726037743696569));
#84813=CARTESIAN_POINT('Ctrl Pts',(0.0136292533790862,-0.034865930689785,
0.0724899522071348));
#84814=CARTESIAN_POINT('Ctrl Pts',(0.0136939320316345,-0.0351951371254986,
0.0727176746960388));
#84815=CARTESIAN_POINT('Ctrl Pts',(0.013664319604646,-0.035030733898099,
0.0726025153429559));
#84816=CARTESIAN_POINT('Ctrl Pts',(0.0136299728209793,-0.034865930689785,
0.0724886783064241));
#84817=CARTESIAN_POINT('Ctrl Pts',(0.0138232326868359,-0.0351951371254986,
0.0725093337186266));
#84818=CARTESIAN_POINT('Ctrl Pts',(0.0137893129408568,-0.035030733898099,
0.0723915011556234));
#84819=CARTESIAN_POINT('Ctrl Pts',(0.013750552032128,-0.034865930689785,
0.0722751712195549));
#84820=CARTESIAN_POINT('Origin',(0.0187222405616067,-0.0308609197384197,
0.0709550975151248));
#84821=CARTESIAN_POINT('',(0.0137503042019611,-0.0351951371254986,0.07262684272735));
#84822=CARTESIAN_POINT('Origin',(0.00723898649331173,-0.03518404674411,
0.0745645868065024));
#84823=CARTESIAN_POINT('Origin',(0.0193252105781808,-0.0352322614052578,
0.0699433117626999));
#84824=CARTESIAN_POINT('',(0.0135574056441349,-0.0351951142564681,0.0722649135892815));
#84825=CARTESIAN_POINT('',(0.0135140129935295,-0.0351951372916787,0.0721480229975867));
#84826=CARTESIAN_POINT('Origin',(0.00785544741042606,-0.0352875120570874,
0.0739402521274073));
#84827=CARTESIAN_POINT('Origin',(0.00934108973055431,-0.0298325076522736,
0.0815536040304091));
#84828=CARTESIAN_POINT('Origin',(0.0165013373209963,-0.0338732939252014,
0.0744038860642835));
#84829=CARTESIAN_POINT('Ctrl Pts',(0.0136276248563989,-0.0321934096636942,
0.0758190870807282));
#84830=CARTESIAN_POINT('Ctrl Pts',(0.0136575007202879,-0.0320508460845519,
0.0757205709181067));
#84831=CARTESIAN_POINT('Ctrl Pts',(0.0136847071227777,-0.0319086045665452,
0.0756213263314847));
#84832=CARTESIAN_POINT('Ctrl Pts',(0.0137092030760702,-0.0317669892871456,
0.0755215718345981));
#84833=CARTESIAN_POINT('Ctrl Pts',(0.013650207803114,-0.0321934096636942,
0.0757383378197694));
#84834=CARTESIAN_POINT('Ctrl Pts',(0.0136786382936863,-0.0320508460845519,
0.0756394174331563));
#84835=CARTESIAN_POINT('Ctrl Pts',(0.0137043895519749,-0.0319086045665452,
0.0755398077616578));
#84836=CARTESIAN_POINT('Ctrl Pts',(0.0137274237880785,-0.0317669892871456,
0.0754397278471591));
#84837=CARTESIAN_POINT('Ctrl Pts',(0.0136727907498291,-0.0321934096636942,
0.0756575885588107));
#84838=CARTESIAN_POINT('Ctrl Pts',(0.0136997758670848,-0.0320508460845519,
0.0755582639482058));
#84839=CARTESIAN_POINT('Ctrl Pts',(0.0137240719811719,-0.0319086045665452,
0.075458289191831));
#84840=CARTESIAN_POINT('Ctrl Pts',(0.0137456445000869,-0.0317669892871456,
0.07535788385972));
#84841=CARTESIAN_POINT('Ctrl Pts',(0.0136953736965441,-0.0321934096636942,
0.075576839297852));
#84842=CARTESIAN_POINT('Ctrl Pts',(0.0137209134404833,-0.0320508460845519,
0.0754771104632554));
#84843=CARTESIAN_POINT('Ctrl Pts',(0.013743754410369,-0.0319086045665452,
0.0753767706220041));
#84844=CARTESIAN_POINT('Ctrl Pts',(0.0137638652120951,-0.0317669892871456,
0.075276039872281));
#84845=CARTESIAN_POINT('',(0.0136949696831625,-0.0321934096636942,0.0755782839180869));
#84846=CARTESIAN_POINT('',(0.0137489462178941,-0.0318665617511353,0.0753481880835307));
#84847=CARTESIAN_POINT('Origin',(-0.00232770420397269,-0.032637194442055,
0.0708357290845033));
#84848=CARTESIAN_POINT('Origin',(0.0244696249328875,-0.0316939261509185,
0.0776317462801823));
#84849=CARTESIAN_POINT('',(0.0136626376743362,-0.0320197221621788,0.0756987637407324));
#84850=CARTESIAN_POINT('Ctrl Pts',(0.0136627312772773,-0.0320197392094702,
0.0756986041996119));
#84851=CARTESIAN_POINT('Ctrl Pts',(0.0136706110281021,-0.0319792716576,
0.0756704202333062));
#84852=CARTESIAN_POINT('Ctrl Pts',(0.013678311787336,-0.0319386439829698,
0.0756420478908117));
#84853=CARTESIAN_POINT('Ctrl Pts',(0.013685833477104,-0.031897909938163,
0.0756134551711632));
#84854=CARTESIAN_POINT('Ctrl Pts',(0.0136933550182004,-0.0318571766984942,
0.0755848630166707));
#84855=CARTESIAN_POINT('Ctrl Pts',(0.0137006609905895,-0.03181638718336,
0.0755561962710094));
#84856=CARTESIAN_POINT('Ctrl Pts',(0.0137077296768219,-0.0317755399638303,
0.0755275544055704));
#84857=CARTESIAN_POINT('',(0.013661303056921,-0.0321934096636183,0.0756986648064836));
#84858=CARTESIAN_POINT('Origin',(0.0158306274447591,-0.0324028746691825,
0.0762840964422932));
#84859=CARTESIAN_POINT('',(0.0136781363700518,-0.0321934096636663,0.0756384743622952));
#84860=CARTESIAN_POINT('Ctrl Pts',(0.0136932022405579,-0.0321934096636618,
0.0755792788221118));
#84861=CARTESIAN_POINT('Ctrl Pts',(0.0137129131094296,-0.0320835708272592,
0.0755024721791053));
#84862=CARTESIAN_POINT('Ctrl Pts',(0.0137310230357111,-0.0319739230346488,
0.0754253021716664));
#84863=CARTESIAN_POINT('Ctrl Pts',(0.0137475164265416,-0.0318646057455573,
0.0753478693117285));
#84864=CARTESIAN_POINT('Ctrl Pts',(0.0137919510558728,-0.0321934096636618,
0.0755236925266851));
#84865=CARTESIAN_POINT('Ctrl Pts',(0.0138108953464091,-0.0320835708272592,
0.0754455240605551));
#84866=CARTESIAN_POINT('Ctrl Pts',(0.0138282109561431,-0.0319739230346488,
0.0753670088842042));
#84867=CARTESIAN_POINT('Ctrl Pts',(0.0138438834405726,-0.0318646057455573,
0.0752882491526201));
#84868=CARTESIAN_POINT('Ctrl Pts',(0.0138906998711876,-0.0321934096636618,
0.0754681062312584));
#84869=CARTESIAN_POINT('Ctrl Pts',(0.0139088775833886,-0.0320835708272592,
0.0753885759420049));
#84870=CARTESIAN_POINT('Ctrl Pts',(0.013925398876575,-0.0319739230346488,
0.075308715596742));
#84871=CARTESIAN_POINT('Ctrl Pts',(0.0139402504546036,-0.0318646057455573,
0.0752286289935117));
#84872=CARTESIAN_POINT('Ctrl Pts',(0.0139894486865025,-0.0321934096636618,
0.0754125199358316));
#84873=CARTESIAN_POINT('Ctrl Pts',(0.0140068598203681,-0.0320835708272592,
0.0753316278234546));
#84874=CARTESIAN_POINT('Ctrl Pts',(0.014022586797007,-0.0319739230346488,
0.0752504223092798));
#84875=CARTESIAN_POINT('Ctrl Pts',(0.0140366174686345,-0.0318646057455573,
0.0751690088344033));
#84876=CARTESIAN_POINT('',(0.0139921320686152,-0.0321763980308501,0.0753999878865454));
#84877=CARTESIAN_POINT('',(0.0139894486864999,-0.0321934096636184,0.075412519935805));
#84878=CARTESIAN_POINT('Origin',(-0.00205353621687885,-0.0326386231150955,
0.0713549143724822));
#84879=CARTESIAN_POINT('Ctrl Pts',(0.0139921320655067,-0.0321763980306344,
0.075399987885879));
#84880=CARTESIAN_POINT('Ctrl Pts',(0.013950154885113,-0.0321259596175737,
0.0753910465364169));
#84881=CARTESIAN_POINT('Ctrl Pts',(0.0139089050138353,-0.0320749164633211,
0.0753822601074425));
#84882=CARTESIAN_POINT('Ctrl Pts',(0.0138278266926965,-0.0319716057794015,
0.075364990019354));
#84883=CARTESIAN_POINT('Ctrl Pts',(0.0137880298338754,-0.0319193786690214,
0.0753565130892893));
#84884=CARTESIAN_POINT('Ctrl Pts',(0.0137489462160759,-0.0318665617525426,
0.075348188083138));
#84885=CARTESIAN_POINT('',(0.0138422091848412,-0.0321934096636663,0.075495401926956));
#84886=CARTESIAN_POINT('Origin',(0.00812378219310841,-0.0315241814719618,
0.07415));
#84887=CARTESIAN_POINT('',(0.0139921320689771,-0.032210423332376,0.0753999878866226));
#84888=CARTESIAN_POINT('',(0.0139947886795379,-0.0321934096636183,0.0753874501348803));
#84889=CARTESIAN_POINT('Origin',(-0.00206906439733519,-0.0326387243756408,
0.0713975045508542));
#84890=CARTESIAN_POINT('Origin',(-0.00230916111180189,-0.0326386236553222,
0.072554997489267));
#84891=CARTESIAN_POINT('Origin',(-0.00230598258356715,-0.0326387247569551,
0.0725097765576227));
#84892=CARTESIAN_POINT('Ctrl Pts',(0.013713169049324,-0.0327445246967096,
0.0755053153033758));
#84893=CARTESIAN_POINT('Ctrl Pts',(0.0137642856016332,-0.032443687833936,
0.0752945081318633));
#84894=CARTESIAN_POINT('Ctrl Pts',(0.0137993780794782,-0.0321434074405927,
0.0750804495336249));
#84895=CARTESIAN_POINT('Ctrl Pts',(0.0137667874877737,-0.0327445246967096,
0.0752611328653132));
#84896=CARTESIAN_POINT('Ctrl Pts',(0.0138086945488767,-0.032443687833936,
0.0750483034413352));
#84897=CARTESIAN_POINT('Ctrl Pts',(0.0138344513743864,-0.0321434074405927,
0.0748329220321544));
#84898=CARTESIAN_POINT('',(0.0137736589065096,-0.0326943950436612,0.0752256477691917));
#84899=CARTESIAN_POINT('',(0.013813081094821,-0.0323666188837389,0.0749926167616255));
#84900=CARTESIAN_POINT('Origin',(-0.00275471203025378,-0.032639557911195,
0.0721562809946593));
#84901=CARTESIAN_POINT('Origin',(0.024738513391894,-0.0321933825603012,
0.0766107332495159));
#84902=CARTESIAN_POINT('',(0.0137934237886414,-0.0321934096532689,0.0751160689287386));
#84903=CARTESIAN_POINT('',(0.0138025805038011,-0.0321934096584275,0.0750542433279473));
#84904=CARTESIAN_POINT('',(0.0137489462188077,-0.0325210109756238,0.0753481880837245));
#84905=CARTESIAN_POINT('Origin',(-0.00263998480464471,-0.03263931291567,
0.0716893526347667));
#84906=CARTESIAN_POINT('',(0.0137476174921984,-0.0326943950436593,0.0753479050583036));
#84907=CARTESIAN_POINT('Origin',(0.0245673437198019,-0.0326943765538141,
0.0776525614440418));
#84908=CARTESIAN_POINT('',(0.013760638199364,-0.0326943950436702,0.0752867764137576));
#84909=CARTESIAN_POINT('Ctrl Pts',(0.0139386268780033,-0.0325229783203769,
0.0756290474267761));
#84910=CARTESIAN_POINT('Ctrl Pts',(0.0139590155144368,-0.032413025309245,
0.0755488899199571));
#84911=CARTESIAN_POINT('Ctrl Pts',(0.0139777428975359,-0.032303122220807,
0.0754683228054589));
#84912=CARTESIAN_POINT('Ctrl Pts',(0.0139947886804688,-0.0321934096576658,
0.0753874501305006));
#84913=CARTESIAN_POINT('Ctrl Pts',(0.013874921404638,-0.0325229783203769,
0.0755353310733458));
#84914=CARTESIAN_POINT('Ctrl Pts',(0.0138940181631889,-0.032413025309245,
0.075456051745084));
#84915=CARTESIAN_POINT('Ctrl Pts',(0.0139114720305956,-0.032303122220807,
0.0753763894001035));
#84916=CARTESIAN_POINT('Ctrl Pts',(0.0139272642504138,-0.0321934096576658,
0.0752964468691155));
#84917=CARTESIAN_POINT('Ctrl Pts',(0.0138112159312727,-0.0325229783203769,
0.0754416147199155));
#84918=CARTESIAN_POINT('Ctrl Pts',(0.013829020811941,-0.032413025309245,
0.0753632135702109));
#84919=CARTESIAN_POINT('Ctrl Pts',(0.0138452011636553,-0.032303122220807,
0.0752844559947481));
#84920=CARTESIAN_POINT('Ctrl Pts',(0.0138597398203589,-0.0321934096576658,
0.0752054436077304));
#84921=CARTESIAN_POINT('Ctrl Pts',(0.0137475104579075,-0.0325229783203769,
0.0753478983664852));
#84922=CARTESIAN_POINT('Ctrl Pts',(0.0137640234606932,-0.032413025309245,
0.0752703753953377));
#84923=CARTESIAN_POINT('Ctrl Pts',(0.0137789302967149,-0.032303122220807,
0.0751925225893928));
#84924=CARTESIAN_POINT('Ctrl Pts',(0.013792215390304,-0.0321934096576658,
0.0751144403463453));
#84925=CARTESIAN_POINT('',(0.0138941062341519,-0.0321934096584275,0.0752517595323228));
#84926=CARTESIAN_POINT('Ctrl Pts',(0.0139921320655695,-0.032210423332889,
0.0753999878858924));
#84927=CARTESIAN_POINT('Ctrl Pts',(0.0139500980054311,-0.0322609421830331,
0.07539103442076));
#84928=CARTESIAN_POINT('Ctrl Pts',(0.0139088203474602,-0.032312088823864,
0.0753822420730741));
#84929=CARTESIAN_POINT('Ctrl Pts',(0.0138277414124259,-0.0324156524631807,
0.0753649718542227));
#84930=CARTESIAN_POINT('Ctrl Pts',(0.0137879734632952,-0.0324680267167304,
0.0753565010820737));
#84931=CARTESIAN_POINT('Ctrl Pts',(0.0137489462187663,-0.0325210109755912,
0.0753481880837111));
#84932=CARTESIAN_POINT('Origin',(0.00556981264422981,-0.0262834582510643,
0.0815918160004898));
#84933=CARTESIAN_POINT('Origin',(0.0176257925203611,-0.0342770795666837,
0.0817351922229394));
#84934=CARTESIAN_POINT('Ctrl Pts',(0.0137719578350082,-0.0326943950436604,
0.0752267514206673));
#84935=CARTESIAN_POINT('Ctrl Pts',(0.0137867974876322,-0.0325844576448133,
0.0751489089745126));
#84936=CARTESIAN_POINT('Ctrl Pts',(0.0138000282810706,-0.0324744968375322,
0.0750707541109808));
#84937=CARTESIAN_POINT('Ctrl Pts',(0.0138116346444435,-0.0323646534831894,
0.0749923872004608));
#84938=CARTESIAN_POINT('Ctrl Pts',(0.0138670213620897,-0.0326943950436604,
0.0751650744119771));
#84939=CARTESIAN_POINT('Ctrl Pts',(0.0138810109899389,-0.0325844576448133,
0.0750859218122511));
#84940=CARTESIAN_POINT('Ctrl Pts',(0.0138933646023211,-0.0324744968375322,
0.0750064742823324));
#84941=CARTESIAN_POINT('Ctrl Pts',(0.0139040677750964,-0.0323646534831894,
0.0749268338333477));
#84942=CARTESIAN_POINT('Ctrl Pts',(0.0139620848891712,-0.0326943950436604,
0.0751033974032868));
#84943=CARTESIAN_POINT('Ctrl Pts',(0.0139752244922456,-0.0325844576448133,
0.0750229346499896));
#84944=CARTESIAN_POINT('Ctrl Pts',(0.0139867009235716,-0.0324744968375322,
0.0749421944536841));
#84945=CARTESIAN_POINT('Ctrl Pts',(0.0139965009057492,-0.0323646534831894,
0.0748612804662345));
#84946=CARTESIAN_POINT('Ctrl Pts',(0.0140571484162527,-0.0326943950436604,
0.0750417203945965));
#84947=CARTESIAN_POINT('Ctrl Pts',(0.0140694379945524,-0.0325844576448133,
0.0749599474877281));
#84948=CARTESIAN_POINT('Ctrl Pts',(0.014080037244822,-0.0324744968375322,
0.0748779146250358));
#84949=CARTESIAN_POINT('Ctrl Pts',(0.014088934036402,-0.0323646534831894,
0.0747957270991214));
#84950=CARTESIAN_POINT('',(0.0140590396096356,-0.03267735599912,0.075029044583551));
#84951=CARTESIAN_POINT('',(0.0140571484162444,-0.0326943950436586,0.0750417203946018));
#84952=CARTESIAN_POINT('Origin',(-0.00237428766991534,-0.0326395662655541,
0.0726459673924195));
#84953=CARTESIAN_POINT('Ctrl Pts',(0.0140590396063146,-0.032677355998748,
0.0750290445830547));
#84954=CARTESIAN_POINT('Ctrl Pts',(0.0140165496609305,-0.0326267922588588,
0.0750227515861847));
#84955=CARTESIAN_POINT('Ctrl Pts',(0.0139748128191324,-0.0325756109584749,
0.0750165701281463));
#84956=CARTESIAN_POINT('Ctrl Pts',(0.0138928098216551,-0.0324719985460571,
0.0750044250288342));
#84957=CARTESIAN_POINT('Ctrl Pts',(0.0138525765557734,-0.0324196091617933,
0.0749984662587221));
#84958=CARTESIAN_POINT('Ctrl Pts',(0.0138130810947728,-0.0323666188837756,
0.0749926167616184));
#84959=CARTESIAN_POINT('',(0.013915403661387,-0.0326943950436699,0.0751336840819068));
#84960=CARTESIAN_POINT('Origin',(0.00812378219310841,-0.0315241814719618,
0.07415));
#84961=CARTESIAN_POINT('',(0.0140590396095908,-0.0327114338379849,0.0750290445835446));
#84962=CARTESIAN_POINT('',(0.0140609037262011,-0.0326943950436593,0.0750163647622643));
#84963=CARTESIAN_POINT('Origin',(-0.00238015612243249,-0.0326395679685205,
0.0726908941291813));
#84964=CARTESIAN_POINT('Origin',(-0.00235956710230526,-0.0326395672643911,
0.0725465692571309));
#84965=CARTESIAN_POINT('Origin',(-0.00235215963958844,-0.0326395684013067,
0.0725018696955815));
#84966=CARTESIAN_POINT('Ctrl Pts',(0.0137872474543938,-0.0332451089994434,
0.0751516417694037));
#84967=CARTESIAN_POINT('Ctrl Pts',(0.0138250249917997,-0.0329451141710255,
0.0749380406823774));
#84968=CARTESIAN_POINT('Ctrl Pts',(0.013846605900126,-0.0326442513127494,
0.0747222008549427));
#84969=CARTESIAN_POINT('Ctrl Pts',(0.0138254260619812,-0.0332451089994434,
0.0749045741796176));
#84970=CARTESIAN_POINT('Ctrl Pts',(0.0138538852927829,-0.0329451141710255,
0.0746895331628477));
#84971=CARTESIAN_POINT('Ctrl Pts',(0.0138660659054358,-0.0326442513127494,
0.0744729593893048));
#84972=CARTESIAN_POINT('Ctrl Pts',(0.0138258078480571,-0.0332451089994434,
0.0749021035037198));
#84973=CARTESIAN_POINT('Ctrl Pts',(0.0138541738957927,-0.0329451141710255,
0.0746870480876524));
#84974=CARTESIAN_POINT('Ctrl Pts',(0.0138662605054889,-0.0326442513127494,
0.0744704669746484));
#84975=CARTESIAN_POINT('',(0.0138300506476655,-0.0331951640388616,0.0748687665299159));
#84976=CARTESIAN_POINT('',(0.0138547629144851,-0.032867753235504,0.0746337200027452));
#84977=CARTESIAN_POINT('Origin',(-0.0028810524814235,-0.0326402808280916,
0.0735378722145668));
#84978=CARTESIAN_POINT('Origin',(0.0248715877881015,-0.0326944278779112,
0.0755632105462519));
#84979=CARTESIAN_POINT('',(0.0138428960169573,-0.0326943950436593,0.0747581628645857));
#84980=CARTESIAN_POINT('',(0.0138481526012722,-0.0326943950436694,0.0746958843103298));
#84981=CARTESIAN_POINT('',(0.0138130810948206,-0.0330220786163545,0.0749926167616284));
#84982=CARTESIAN_POINT('Origin',(-0.00287200908005241,-0.0326396682761396,
0.0730571739081459));
#84983=CARTESIAN_POINT('',(0.0138117372188363,-0.0331951640388589,0.0749924177261293));
#84984=CARTESIAN_POINT('Origin',(0.0247243538844031,-0.033195202656011,
0.0766086377178643));
#84985=CARTESIAN_POINT('',(0.0138208939332609,-0.0331951640388702,0.0749305921280326));
#84986=CARTESIAN_POINT('Ctrl Pts',(0.0140200229445547,-0.0330240426238172,
0.0752610108015162));
#84987=CARTESIAN_POINT('Ctrl Pts',(0.014035328200751,-0.032914277406352,
0.075179784340736));
#84988=CARTESIAN_POINT('Ctrl Pts',(0.0140489619093364,-0.0328043479726691,
0.075098200983204));
#84989=CARTESIAN_POINT('Ctrl Pts',(0.014060903726208,-0.0326943950436594,
0.0750163647622724));
#84990=CARTESIAN_POINT('Ctrl Pts',(0.01395055868344,-0.0330240426238172,
0.0751714795085905));
#84991=CARTESIAN_POINT('Ctrl Pts',(0.0139646305588501,-0.032914277406352,
0.0750912099856829));
#84992=CARTESIAN_POINT('Ctrl Pts',(0.013977050054343,-0.0328043479726691,
0.0750106095405181));
#84993=CARTESIAN_POINT('Ctrl Pts',(0.0139877984159907,-0.0326943950436593,
0.0749297809901024));
#84994=CARTESIAN_POINT('Ctrl Pts',(0.0138810944223254,-0.0330240426238172,
0.0750819482156648));
#84995=CARTESIAN_POINT('Ctrl Pts',(0.0138939329169493,-0.032914277406352,
0.0750026356306298));
#84996=CARTESIAN_POINT('Ctrl Pts',(0.0139051381993496,-0.0328043479726691,
0.0749230180978321));
#84997=CARTESIAN_POINT('Ctrl Pts',(0.0139146931057734,-0.0326943950436593,
0.0748431972179323));
#84998=CARTESIAN_POINT('Ctrl Pts',(0.0138116301612107,-0.0330240426238172,
0.0749924169227391));
#84999=CARTESIAN_POINT('Ctrl Pts',(0.0138232352750485,-0.032914277406352,
0.0749140612755767));
#85000=CARTESIAN_POINT('Ctrl Pts',(0.0138332263443562,-0.0328043479726691,
0.0748354266551462));
#85001=CARTESIAN_POINT('Ctrl Pts',(0.0138415877955562,-0.0326943950436593,
0.0747566134457623));
#85002=CARTESIAN_POINT('',(0.0139518998715892,-0.0326943950436694,0.074887263813435));
#85003=CARTESIAN_POINT('Ctrl Pts',(0.0140590396063062,-0.0327114338383285,
0.0750290445830535));
#85004=CARTESIAN_POINT('Ctrl Pts',(0.0140165567282563,-0.0327619876829988,
0.075022752632895));
#85005=CARTESIAN_POINT('Ctrl Pts',(0.0139748233384161,-0.0328131562602352,
0.0750165716861023));
#85006=CARTESIAN_POINT('Ctrl Pts',(0.0138928204166615,-0.0329167375858765,
0.0750044265980051));
#85007=CARTESIAN_POINT('Ctrl Pts',(0.0138525835591661,-0.0329691088920618,
0.0749984672959634));
#85008=CARTESIAN_POINT('Ctrl Pts',(0.0138130810947739,-0.0330220786163186,
0.0749926167616186));
#85009=CARTESIAN_POINT('Ctrl Pts',(0.0138284219717157,-0.0331951640388604,
0.0748699750076524));
#85010=CARTESIAN_POINT('Ctrl Pts',(0.0138433069933938,-0.0330306422010619,
0.0747520352377044));
#85011=CARTESIAN_POINT('Ctrl Pts',(0.013853304721205,-0.0328657861914645,
0.0746335810328641));
#85012=CARTESIAN_POINT('Ctrl Pts',(0.013830050647665,-0.0331951640388604,
0.0748687665299189));
#85013=CARTESIAN_POINT('Ctrl Pts',(0.0138449106848409,-0.0330306422010619,
0.0747507930881399));
#85014=CARTESIAN_POINT('Ctrl Pts',(0.0138548820578066,-0.0328657861914645,
0.0746323062728766));
#85015=CARTESIAN_POINT('Ctrl Pts',(0.0141014318602109,-0.0331951640388604,
0.0746674016403838));
#85016=CARTESIAN_POINT('Ctrl Pts',(0.0141121288073988,-0.0330306422010619,
0.0745438175660289));
#85017=CARTESIAN_POINT('Ctrl Pts',(0.0141177087543631,-0.0328657861914645,
0.0744198969773231));
#85018=CARTESIAN_POINT('',(0.0141025234022412,-0.033178164828195,0.0746546320938944));
#85019=CARTESIAN_POINT('',(0.0141014318602036,-0.0331951640388588,0.0746674016403882));
#85020=CARTESIAN_POINT('Origin',(-0.00240583847027637,-0.0326412092720937,
0.0739760525074001));
#85021=CARTESIAN_POINT('Ctrl Pts',(0.0141025234010472,-0.033178164828644,
0.0746546320952973));
#85022=CARTESIAN_POINT('Ctrl Pts',(0.0140596926911923,-0.0331276811546766,
0.0746510170068694));
#85023=CARTESIAN_POINT('Ctrl Pts',(0.0140176353684742,-0.0330765663497773,
0.0746474672294402));
#85024=CARTESIAN_POINT('Ctrl Pts',(0.013935031376349,-0.0329730614463479,
0.0746404950851237));
#85025=CARTESIAN_POINT('Ctrl Pts',(0.0138945180775977,-0.0329207133374377,
0.0746370755294888));
#85026=CARTESIAN_POINT('Ctrl Pts',(0.0138547629219927,-0.0328677532289394,
0.0746337200174055));
#85027=CARTESIAN_POINT('',(0.0139657412539446,-0.0331951640388701,0.0747680840851621));
#85028=CARTESIAN_POINT('Origin',(0.00812378219310841,-0.0315241814719618,
0.07415));
#85029=CARTESIAN_POINT('',(0.0141025234007489,-0.0332121607144205,0.0746546320931199));
#85030=CARTESIAN_POINT('',(0.0141035876665865,-0.0331951640388587,0.0746418602437367));
#85031=CARTESIAN_POINT('Origin',(-0.00240177833528214,-0.0326413665497158,
0.0740212147868483));
#85032=CARTESIAN_POINT('Origin',(-0.00228602857041441,-0.0326412096280679,
0.0725565677200206));
#85033=CARTESIAN_POINT('Origin',(-0.00227445427339749,-0.0326413667757252,
0.0725127248825164));
#85034=CARTESIAN_POINT('Ctrl Pts',(0.0138389631736647,-0.0337436976235975,
0.0747940740326138));
#85035=CARTESIAN_POINT('Ctrl Pts',(0.0138447560731261,-0.0336723290703325,
0.0747426708287153));
#85036=CARTESIAN_POINT('Ctrl Pts',(0.0138496234538143,-0.033601104548885,
0.0746911717446415));
#85037=CARTESIAN_POINT('Ctrl Pts',(0.0138651640361777,-0.0333736987606856,
0.0745267453705877));
#85038=CARTESIAN_POINT('Ctrl Pts',(0.0138712432754734,-0.0331450831799191,
0.0743616981499681));
#85039=CARTESIAN_POINT('Ctrl Pts',(0.0138615538439715,-0.0337436976235975,
0.0745450968014961));
#85040=CARTESIAN_POINT('Ctrl Pts',(0.0138651074044827,-0.0336723290703325,
0.0744934904136851));
#85041=CARTESIAN_POINT('Ctrl Pts',(0.0138677321538547,-0.033601104548885,
0.0744418284572187));
#85042=CARTESIAN_POINT('Ctrl Pts',(0.0138761124586661,-0.0333736987606856,
0.0742768820638785));
#85043=CARTESIAN_POINT('Ctrl Pts',(0.0138750133782756,-0.0331450831799191,
0.0741117265789348));
#85044=CARTESIAN_POINT('Ctrl Pts',(0.0138617797506745,-0.0337436976235975,
0.0745426070291849));
#85045=CARTESIAN_POINT('Ctrl Pts',(0.0138653109177962,-0.0336723290703325,
0.0744909986095348));
#85046=CARTESIAN_POINT('Ctrl Pts',(0.0138679132408551,-0.033601104548885,
0.0744393350243445));
#85047=CARTESIAN_POINT('Ctrl Pts',(0.013876221942891,-0.0333736987606856,
0.0742743834308115));
#85048=CARTESIAN_POINT('Ctrl Pts',(0.0138750510793037,-0.0331450831799191,
0.0741092268632245));
#85049=CARTESIAN_POINT('',(0.0138639223541781,-0.0336938721132548,0.0745090486475063));
#85050=CARTESIAN_POINT('',(0.0138738271572256,-0.0333679869945434,0.0742729142414415));
#85051=CARTESIAN_POINT('Ctrl Pts',(0.0138639223541781,-0.033693872113265,
0.0745090486475155));
#85052=CARTESIAN_POINT('Ctrl Pts',(0.0138653238894816,-0.0336629187933933,
0.0744866421877192));
#85053=CARTESIAN_POINT('Ctrl Pts',(0.0138665937777099,-0.0336319952301041,
0.0744642346874896));
#85054=CARTESIAN_POINT('Ctrl Pts',(0.0138677321538542,-0.0336011045488951,
0.0744418284572279));
#85055=CARTESIAN_POINT('Ctrl Pts',(0.0138705887291307,-0.0335235892595453,
0.0743856035585208));
#85056=CARTESIAN_POINT('Ctrl Pts',(0.0138726221261806,-0.0334458668660369,
0.0743292867427685));
#85057=CARTESIAN_POINT('Ctrl Pts',(0.0138738271575316,-0.0333679869945386,
0.0742729142414548));
#85058=CARTESIAN_POINT('Ctrl Pts',(0.013873828795071,-0.0333679692459109,
0.0742728697961073));
#85059=CARTESIAN_POINT('Ctrl Pts',(0.0138733755581721,-0.033339189537426,
0.0742728660364243));
#85060=CARTESIAN_POINT('Ctrl Pts',(0.0138730358080678,-0.0333104081060745,
0.0742728664654439));
#85061=CARTESIAN_POINT('Ctrl Pts',(0.0138725860978153,-0.0332532698357313,
0.0742728725717586));
#85062=CARTESIAN_POINT('Ctrl Pts',(0.0138724727837111,-0.0332249171907008,
0.0742728781730112));
#85063=CARTESIAN_POINT('Ctrl Pts',(0.013872468966693,-0.0331960985338784,
0.0742728849926027));
#85064=CARTESIAN_POINT('Ctrl Pts',(0.0138724689345538,-0.0331956312586429,
0.0742728851037769));
#85065=CARTESIAN_POINT('Ctrl Pts',(0.0138724689321763,-0.033195164038859,
0.074272885214998));
#85066=CARTESIAN_POINT('',(0.013869797514459,-0.0331951640388587,0.0743978566658474));
#85067=CARTESIAN_POINT('',(0.0138711332233277,-0.0331951640388687,0.0743353709404327));
#85068=CARTESIAN_POINT('',(0.0138547629068615,-0.033521636656766,0.074633720016266));
#85069=CARTESIAN_POINT('Origin',(-0.00279859809327077,-0.0326434571526035,
0.0744433718934559));
#85070=CARTESIAN_POINT('',(0.0138534091855672,-0.0336938721132326,0.0746336057560541));
#85071=CARTESIAN_POINT('Origin',(0.0247352852322952,-0.0336938867896224,
0.0755520847427957));
#85072=CARTESIAN_POINT('',(0.0138586657698826,-0.0336938721132536,0.0745713272017903));
#85073=CARTESIAN_POINT('Ctrl Pts',(0.0140781491240354,-0.0335235895815172,
0.0748885895016754));
#85074=CARTESIAN_POINT('Ctrl Pts',(0.0140883172626749,-0.0334144449262748,
0.0748066159178015));
#85075=CARTESIAN_POINT('Ctrl Pts',(0.0140968035707229,-0.0333049234473147,
0.0747243380901192));
#85076=CARTESIAN_POINT('Ctrl Pts',(0.0141035876665938,-0.0331951640388587,
0.0746418602437443));
#85077=CARTESIAN_POINT('Ctrl Pts',(0.014003200098239,-0.0335235895815172,
0.0748035964665564));
#85078=CARTESIAN_POINT('Ctrl Pts',(0.0140121981404142,-0.0334144449262748,
0.0747226547035836));
#85079=CARTESIAN_POINT('Ctrl Pts',(0.0140195343243421,-0.0333049234473147,
0.074641434055552));
#85080=CARTESIAN_POINT('Ctrl Pts',(0.0140251898615454,-0.0331951640388587,
0.0745600375289875));
#85081=CARTESIAN_POINT('Ctrl Pts',(0.0139282510724427,-0.0335235895815172,
0.0747186034314374));
#85082=CARTESIAN_POINT('Ctrl Pts',(0.0139360790181536,-0.0334144449262748,
0.0746386934893658));
#85083=CARTESIAN_POINT('Ctrl Pts',(0.0139422650779614,-0.0333049234473147,
0.0745585300209849));
#85084=CARTESIAN_POINT('Ctrl Pts',(0.0139467920564971,-0.0331951640388587,
0.0744782148142308));
#85085=CARTESIAN_POINT('Ctrl Pts',(0.0138533020466464,-0.0335235895815172,
0.0746336103963184));
#85086=CARTESIAN_POINT('Ctrl Pts',(0.0138599598958929,-0.0334144449262748,
0.0745547322751479));
#85087=CARTESIAN_POINT('Ctrl Pts',(0.0138649958315807,-0.0333049234473147,
0.0744756259864177));
#85088=CARTESIAN_POINT('Ctrl Pts',(0.0138683942514488,-0.0331951640388587,
0.074396392099474));
#85089=CARTESIAN_POINT('',(0.0139866925905328,-0.0331951640388687,0.074519858454802));
#85090=CARTESIAN_POINT('Ctrl Pts',(0.0141025233976227,-0.0332121607145939,
0.0746546320928511));
#85091=CARTESIAN_POINT('Ctrl Pts',(0.0140597647410649,-0.0332625444108758,
0.074651023073894));
#85092=CARTESIAN_POINT('Ctrl Pts',(0.0140177428832558,-0.0333135300744814,
0.0746474762439968));
#85093=CARTESIAN_POINT('Ctrl Pts',(0.0139351394084258,-0.0334167203140546,
0.074640504146869));
#85094=CARTESIAN_POINT('Ctrl Pts',(0.013894589784646,-0.0334688847587227,
0.0746370815800088));
#85095=CARTESIAN_POINT('Ctrl Pts',(0.0138547629061685,-0.0335216366562281,
0.0746337200160356));
#85096=CARTESIAN_POINT('Ctrl Pts',(0.0138631583902534,-0.033693872113239,
0.0745096936854851));
#85097=CARTESIAN_POINT('Ctrl Pts',(0.0138652637967536,-0.0336474569764958,
0.0744760992120762));
#85098=CARTESIAN_POINT('Ctrl Pts',(0.0138669757932624,-0.033601104548885,
0.0744424823941408));
#85099=CARTESIAN_POINT('Ctrl Pts',(0.0138713101748101,-0.0334837508592656,
0.0743573723401193));
#85100=CARTESIAN_POINT('Ctrl Pts',(0.013873120665654,-0.0333660264659097,
0.0742721712234493));
#85101=CARTESIAN_POINT('Ctrl Pts',(0.0138639223541767,-0.033693872113239,
0.0745090486475269));
#85102=CARTESIAN_POINT('Ctrl Pts',(0.0138660239850557,-0.0336474569764958,
0.0744754497023837));
#85103=CARTESIAN_POINT('Ctrl Pts',(0.0138677321538547,-0.033601104548885,
0.0744418284572187));
#85104=CARTESIAN_POINT('Ctrl Pts',(0.0138720568445213,-0.0334837508592656,
0.07435670719447));
#85105=CARTESIAN_POINT('Ctrl Pts',(0.0138738573166017,-0.0333660264659097,
0.0742714951611556));
#85106=CARTESIAN_POINT('Ctrl Pts',(0.0141236734632555,-0.033693872113239,
0.074289732892016));
#85107=CARTESIAN_POINT('Ctrl Pts',(0.0141244913662408,-0.0336474569764958,
0.0742546135374367));
#85108=CARTESIAN_POINT('Ctrl Pts',(0.0141248980967959,-0.033601104548885,
0.0742194870146711));
#85109=CARTESIAN_POINT('Ctrl Pts',(0.0141259278450482,-0.0334837508592656,
0.0741305547351223));
#85110=CARTESIAN_POINT('Ctrl Pts',(0.0141243218932809,-0.0333660264659097,
0.0740416309945008));
#85111=CARTESIAN_POINT('',(0.0141224118338749,-0.0336769361243753,0.0742782280504327));
#85112=CARTESIAN_POINT('',(0.0141221242518552,-0.0336938721132327,0.0742910409382789));
#85113=CARTESIAN_POINT('Ctrl Pts',(0.0141224118338749,-0.033676936124375,
0.0742782280504324));
#85114=CARTESIAN_POINT('Ctrl Pts',(0.0141223661808355,-0.0336797586669966,
0.0742803637428505));
#85115=CARTESIAN_POINT('Ctrl Pts',(0.0141223193889672,-0.0336825812712728,
0.0742824993301146));
#85116=CARTESIAN_POINT('Ctrl Pts',(0.0141222235282267,-0.0336882265947832,
0.0742867702880857));
#85117=CARTESIAN_POINT('Ctrl Pts',(0.0141221744593723,-0.0336910493139906,
0.0742889056587687));
#85118=CARTESIAN_POINT('Ctrl Pts',(0.0141221242518612,-0.0336938721132353,
0.0742910409382756));
#85119=CARTESIAN_POINT('Ctrl Pts',(0.0141224118338748,-0.0336769361243754,
0.0742782280504327));
#85120=CARTESIAN_POINT('Ctrl Pts',(0.014080508590939,-0.0336279018505204,
0.0742773323173286));
#85121=CARTESIAN_POINT('Ctrl Pts',(0.0140380025168502,-0.0335767826010746,
0.0742764236979712));
#85122=CARTESIAN_POINT('Ctrl Pts',(0.0139547150328192,-0.0334733172064637,
0.0742746433260626));
#85123=CARTESIAN_POINT('Ctrl Pts',(0.0139138776469841,-0.0334209631456282,
0.0742737703769581));
#85124=CARTESIAN_POINT('Ctrl Pts',(0.0138738271570598,-0.0333679869844681,
0.0742729142487173));
#85125=CARTESIAN_POINT('',(0.0139930233030266,-0.0336938721132538,0.0744000447929027));
#85126=CARTESIAN_POINT('Origin',(0.00812378219310841,-0.0315241814719618,
0.07415));
#85127=CARTESIAN_POINT('',(0.0141224118325865,-0.0337108120655527,0.0742782280504102));
#85128=CARTESIAN_POINT('',(0.0141226720466813,-0.0336938721132327,0.0742654145775366));
#85129=CARTESIAN_POINT('Origin',(-0.00221117739885073,-0.0345562524779775,
0.0728112158998784));
#85130=CARTESIAN_POINT('Ctrl Pts',(0.0141226720466944,-0.0336938721132384,
0.0742654145775444));
#85131=CARTESIAN_POINT('Ctrl Pts',(0.0141226309613475,-0.0336910492958727,
0.0742675500657631));
#85132=CARTESIAN_POINT('Ctrl Pts',(0.0141225887348685,-0.0336882265857238,
0.0742696855758484));
#85133=CARTESIAN_POINT('Ctrl Pts',(0.0141225019976713,-0.0336825812712687,
0.0742739567219923));
#85134=CARTESIAN_POINT('Ctrl Pts',(0.0141224574869142,-0.0336797586669946,
0.0742760923580164));
#85135=CARTESIAN_POINT('Ctrl Pts',(0.0141224118338749,-0.033676936124375,
0.074278228050433));
#85136=CARTESIAN_POINT('Origin',(-0.00225894604208123,-0.0345562520800193,
0.0750459176398226));
#85137=CARTESIAN_POINT('Ctrl Pts',(0.0138681247630567,-0.034243627687391,
0.0744339954913032));
#85138=CARTESIAN_POINT('Ctrl Pts',(0.0138788358295853,-0.0339430054201809,
0.0742173440397331));
#85139=CARTESIAN_POINT('Ctrl Pts',(0.0138731973920629,-0.0336441434784052,
0.0740005012708061));
#85140=CARTESIAN_POINT('Ctrl Pts',(0.0138750396898682,-0.034243627687391,
0.0741840911420269));
#85141=CARTESIAN_POINT('Ctrl Pts',(0.0138763254584859,-0.0339430054201809,
0.0739671788896928));
#85142=CARTESIAN_POINT('Ctrl Pts',(0.0138612688547536,-0.0336441434784052,
0.073750786012967));
#85143=CARTESIAN_POINT('Ctrl Pts',(0.0138751088391363,-0.034243627687391,
0.0741815920985342));
#85144=CARTESIAN_POINT('Ctrl Pts',(0.0138763003547749,-0.0339430054201809,
0.0739646772381924));
#85145=CARTESIAN_POINT('Ctrl Pts',(0.0138611495693806,-0.0336441434784052,
0.0737482888603886));
#85146=CARTESIAN_POINT('',(0.0138751403498937,-0.034193496108874,0.0741479137641487));
#85147=CARTESIAN_POINT('',(0.0138701986066189,-0.033866421286332,0.0739116233931666));
#85148=CARTESIAN_POINT('Origin',(-0.00285207083601065,-0.0345610720404536,
0.0736443765677451));
#85149=CARTESIAN_POINT('Origin',(0.0248270276664345,-0.033693800507288,
0.0734570671026286));
#85150=CARTESIAN_POINT('',(0.013874022114592,-0.0336938721132327,0.0740365722900837));
#85151=CARTESIAN_POINT('',(0.0138714316765818,-0.0336938721132426,0.0739741259961215));
#85152=CARTESIAN_POINT('',(0.0138738271570597,-0.0340203938281605,0.0742729142487225));
#85153=CARTESIAN_POINT('Origin',(-0.0027636184318799,-0.0345589643244419,
0.0731713935802988));
#85154=CARTESIAN_POINT('',(0.0138724689321763,-0.0341934961088739,0.074272885214998));
#85155=CARTESIAN_POINT('Origin',(0.0248893994280871,-0.0341934220717642,
0.0745083861920761));
#85156=CARTESIAN_POINT('',(0.013873804641045,-0.034193496108884,0.0742103994895834));
#85157=CARTESIAN_POINT('Ctrl Pts',(0.0141127757939143,-0.0340223579322396,
0.0745132570021457));
#85158=CARTESIAN_POINT('Ctrl Pts',(0.0141177860553879,-0.0339125849573574,
0.0744306531604395));
#85159=CARTESIAN_POINT('Ctrl Pts',(0.0141210830886303,-0.0338030433565231,
0.0743480036627263));
#85160=CARTESIAN_POINT('Ctrl Pts',(0.014122672046689,-0.0336938721132327,
0.0742654145775436));
#85161=CARTESIAN_POINT('Ctrl Pts',(0.0140326379196887,-0.0340223579322396,
0.0744331377101772));
#85162=CARTESIAN_POINT('Ctrl Pts',(0.0140365431271662,-0.0339125849573574,
0.074351639178765));
#85163=CARTESIAN_POINT('Ctrl Pts',(0.0140387587602758,-0.0338030433565231,
0.0742701170867068));
#85164=CARTESIAN_POINT('Ctrl Pts',(0.0140392912271874,-0.0336938721132327,
0.0741886759381879));
#85165=CARTESIAN_POINT('Ctrl Pts',(0.0139525000454631,-0.0340223579322396,
0.0743530184182088));
#85166=CARTESIAN_POINT('Ctrl Pts',(0.0139553001989445,-0.0339125849573574,
0.0742726251970905));
#85167=CARTESIAN_POINT('Ctrl Pts',(0.0139564344319213,-0.0338030433565231,
0.0741922305106874));
#85168=CARTESIAN_POINT('Ctrl Pts',(0.0139559104076859,-0.0336938721132327,
0.0741119372988321));
#85169=CARTESIAN_POINT('Ctrl Pts',(0.0138723621712376,-0.0340223579322396,
0.0742728991262404));
#85170=CARTESIAN_POINT('Ctrl Pts',(0.0138740572707228,-0.0339125849573574,
0.0741936112154159));
#85171=CARTESIAN_POINT('Ctrl Pts',(0.0138741101035668,-0.0338030433565231,
0.074114343934668));
#85172=CARTESIAN_POINT('Ctrl Pts',(0.0138725295881843,-0.0336938721132327,
0.0740351986594764));
#85173=CARTESIAN_POINT('',(0.0139983470806467,-0.0336938721132427,0.0741509934338202));
#85174=CARTESIAN_POINT('Ctrl Pts',(0.014122411828979,-0.0337108120662654,
0.0742782280503281));
#85175=CARTESIAN_POINT('Ctrl Pts',(0.0140794223936299,-0.0337611408993377,
0.0742773090985317));
#85176=CARTESIAN_POINT('Ctrl Pts',(0.0140372174200965,-0.0338121088779457,
0.0742764069155668));
#85177=CARTESIAN_POINT('Ctrl Pts',(0.0139543379483227,-0.0339153382773231,
0.0742746352654196));
#85178=CARTESIAN_POINT('Ctrl Pts',(0.0139136985133928,-0.0339675558473107,
0.0742737665477584));
#85179=CARTESIAN_POINT('Ctrl Pts',(0.0138738271570199,-0.0340203938281304,
0.0742729142487164));
#85180=CARTESIAN_POINT('Ctrl Pts',(0.0138736759116553,-0.0341934961088741,
0.0741493169043875));
#85181=CARTESIAN_POINT('Ctrl Pts',(0.0138736617891916,-0.0340287516182428,
0.074030442381591));
#85182=CARTESIAN_POINT('Ctrl Pts',(0.0138687345045831,-0.0338644633275951,
0.0739116700184927));
#85183=CARTESIAN_POINT('Ctrl Pts',(0.0138751403498937,-0.0341934961088741,
0.0741479137641487));
#85184=CARTESIAN_POINT('Ctrl Pts',(0.013875097218611,-0.0340287516182428,
0.0740290089652454));
#85185=CARTESIAN_POINT('Ctrl Pts',(0.0138701396986365,-0.0338644633275951,
0.0739102075508671));
#85186=CARTESIAN_POINT('Ctrl Pts',(0.0141191439277879,-0.034193496108874,
0.0739141236120166));
#85187=CARTESIAN_POINT('Ctrl Pts',(0.0141142673692925,-0.0340287516182428,
0.0737901742313691));
#85188=CARTESIAN_POINT('Ctrl Pts',(0.0141042720557859,-0.0338644633275951,
0.073666532314959));
#85189=CARTESIAN_POINT('',(0.0141186264137054,-0.0341764758832436,0.0739013179509364));
#85190=CARTESIAN_POINT('',(0.0141191439277825,-0.034193496108874,0.0739141236120217));
#85191=CARTESIAN_POINT('Origin',(-0.00244612043510156,-0.0345621026295853,
0.0740759282701026));
#85192=CARTESIAN_POINT('Ctrl Pts',(0.0141186264129026,-0.0341764758837543,
0.0739013179525675));
#85193=CARTESIAN_POINT('Ctrl Pts',(0.0140757389205321,-0.0341260050040233,
0.0739030970533271));
#85194=CARTESIAN_POINT('Ctrl Pts',(0.0140335969155405,-0.0340749269147708,
0.0739048452672929));
#85195=CARTESIAN_POINT('Ctrl Pts',(0.013950771212202,-0.0339715436304957,
0.0739082810932569));
#85196=CARTESIAN_POINT('Ctrl Pts',(0.0139101189358853,-0.033919277823606,
0.0739099673957978));
#85197=CARTESIAN_POINT('Ctrl Pts',(0.0138701986078372,-0.033866421285466,
0.0739116233948971));
#85198=CARTESIAN_POINT('',(0.0139971421388481,-0.0341934961088841,0.0740310186880953));
#85199=CARTESIAN_POINT('Origin',(0.00812378219310841,-0.0315241814719618,
0.07415));
#85200=CARTESIAN_POINT('',(0.0141186264129331,-0.0342105180190352,0.0739013179501266));
#85201=CARTESIAN_POINT('',(0.0141180815491561,-0.0341934961088739,0.0738885134227268));
#85202=CARTESIAN_POINT('Origin',(-0.00244948063736381,-0.0345621718631018,
0.0741211287917469));
#85203=CARTESIAN_POINT('Origin',(-0.00240367129296537,-0.0345621029826751,
0.0750992465279169));
#85204=CARTESIAN_POINT('Origin',(-0.00241076155520861,-0.0345621722654536,
0.0750544795851669));
#85205=CARTESIAN_POINT('Ctrl Pts',(0.0138740842855151,-0.0346945769586965,
0.0740380710110408));
#85206=CARTESIAN_POINT('Ctrl Pts',(0.0138717398880274,-0.0345275153362944,
0.07391762863142));
#85207=CARTESIAN_POINT('Ctrl Pts',(0.0138656070821789,-0.0343603235965185,
0.0737972288283738));
#85208=CARTESIAN_POINT('Ctrl Pts',(0.0138557092984996,-0.034193496108874,
0.0736772274214943));
#85209=CARTESIAN_POINT('Ctrl Pts',(0.0138706096445053,-0.0346945769586965,
0.0739543097118885));
#85210=CARTESIAN_POINT('Ctrl Pts',(0.0138665108330707,-0.0345275153362944,
0.0738339401100148));
#85211=CARTESIAN_POINT('Ctrl Pts',(0.0138586254482872,-0.0343603235965185,
0.0737136682782436));
#85212=CARTESIAN_POINT('Ctrl Pts',(0.0138469820984099,-0.034193496108874,
0.0735938495806466));
#85213=CARTESIAN_POINT('Ctrl Pts',(0.0138671350034952,-0.0346945769586965,
0.0738705484127371));
#85214=CARTESIAN_POINT('Ctrl Pts',(0.0138612817781137,-0.0345275153362944,
0.07375025158861));
#85215=CARTESIAN_POINT('Ctrl Pts',(0.0138516438143953,-0.0343603235965185,
0.0736301077281143));
#85216=CARTESIAN_POINT('Ctrl Pts',(0.0138382548983204,-0.034193496108874,
0.0735104717398013));
#85217=CARTESIAN_POINT('Ctrl Pts',(0.0138636603624858,-0.0346945769586965,
0.0737867871135838));
#85218=CARTESIAN_POINT('Ctrl Pts',(0.0138560527231573,-0.0345275153362944,
0.0736665630672044));
#85219=CARTESIAN_POINT('Ctrl Pts',(0.0138446621805036,-0.0343603235965185,
0.0735465471779831));
#85220=CARTESIAN_POINT('Ctrl Pts',(0.0138295276982305,-0.034193496108874,
0.0734270938989512));
#85221=CARTESIAN_POINT('',(0.0138636603625108,-0.0346945769586966,0.0737867871141892));
#85222=CARTESIAN_POINT('',(0.013843891575329,-0.034366772783152,0.0735512733044807));
#85223=CARTESIAN_POINT('Origin',(-0.00290383243116199,-0.0345626457065536,
0.075031147453749));
#85224=CARTESIAN_POINT('Origin',(0.0248360194119435,-0.0341934771029141,
0.0724007168948601));
#85225=CARTESIAN_POINT('',(0.0138555531447897,-0.034193496108874,0.073675735561671));
#85226=CARTESIAN_POINT('',(0.0138490467831759,-0.034193496108884,0.0736135751461545));
#85227=CARTESIAN_POINT('',(0.0138701986063303,-0.0345211942962626,0.0739116233949307));
#85228=CARTESIAN_POINT('Origin',(-0.00292043911146928,-0.0345625596119892,
0.0745506112866318));
#85229=CARTESIAN_POINT('',(0.0138688412385515,-0.0346945769586885,0.0739116797021393));
#85230=CARTESIAN_POINT('Origin',(0.024922901402722,-0.0346945685853913,
0.0734531286106225));
#85231=CARTESIAN_POINT('',(0.0138662508005412,-0.0346945769587026,0.0738492334081743));
#85232=CARTESIAN_POINT('Ctrl Pts',(0.0141237669768187,-0.0345231616327841,
0.0741364872156039));
#85233=CARTESIAN_POINT('Ctrl Pts',(0.0141235807221103,-0.0344132092796987,
0.0740537858726633));
#85234=CARTESIAN_POINT('Ctrl Pts',(0.0141216838649669,-0.0343032738558979,
0.0739710926492636));
#85235=CARTESIAN_POINT('Ctrl Pts',(0.0141180815491638,-0.0341934961088739,
0.073888513422733));
#85236=CARTESIAN_POINT('Ctrl Pts',(0.0140387566370225,-0.0345231616327841,
0.0740615580606184));
#85237=CARTESIAN_POINT('Ctrl Pts',(0.0140375375894044,-0.0344132092796987,
0.0739800284655269));
#85238=CARTESIAN_POINT('Ctrl Pts',(0.0140346322293188,-0.0343032738558979,
0.0738985282920262));
#85239=CARTESIAN_POINT('Ctrl Pts',(0.0140300469533981,-0.0341934961088739,
0.0738171618559144));
#85240=CARTESIAN_POINT('Ctrl Pts',(0.0139537462972263,-0.0345231616327841,
0.0739866289056329));
#85241=CARTESIAN_POINT('Ctrl Pts',(0.0139514944566985,-0.0344132092796987,
0.0739062710583905));
#85242=CARTESIAN_POINT('Ctrl Pts',(0.0139475805936706,-0.0343032738558979,
0.0738259639347888));
#85243=CARTESIAN_POINT('Ctrl Pts',(0.0139420123576324,-0.0341934961088739,
0.0737458102890957));
#85244=CARTESIAN_POINT('Ctrl Pts',(0.0138687359574301,-0.0345231616327841,
0.0739116997506474));
#85245=CARTESIAN_POINT('Ctrl Pts',(0.0138654513239927,-0.0344132092796987,
0.0738325136512541));
#85246=CARTESIAN_POINT('Ctrl Pts',(0.0138605289580224,-0.0343032738558979,
0.0737533995775514));
#85247=CARTESIAN_POINT('Ctrl Pts',(0.0138539777618667,-0.0341934961088739,
0.0736744587222771));
#85248=CARTESIAN_POINT('',(0.0139868173469829,-0.0341934961088839,0.0737821244922089));
#85249=CARTESIAN_POINT('Ctrl Pts',(0.014118626409476,-0.0342105180195356,
0.0739013179502644));
#85250=CARTESIAN_POINT('Ctrl Pts',(0.0140756907027709,-0.0342610556240236,
0.0739030990373393));
#85251=CARTESIAN_POINT('Ctrl Pts',(0.0140335254551187,-0.0343122189867999,
0.0739048481637278));
#85252=CARTESIAN_POINT('Ctrl Pts',(0.0139506989163743,-0.0344158119695098,
0.0739082840283949));
#85253=CARTESIAN_POINT('Ctrl Pts',(0.0139100715021913,-0.0344681990449982,
0.0739099693613693));
#85254=CARTESIAN_POINT('Ctrl Pts',(0.0138701986062979,-0.0345211942962385,
0.0739116233949225));
#85255=CARTESIAN_POINT('Ctrl Pts',(0.0138622872541964,-0.0346945769586932,
0.073788279073106));
#85256=CARTESIAN_POINT('Ctrl Pts',(0.0138548089299784,-0.034529677707698,
0.0736696395414039));
#85257=CARTESIAN_POINT('Ctrl Pts',(0.0138424335150294,-0.034364806625142,
0.0735514104717111));
#85258=CARTESIAN_POINT('Ctrl Pts',(0.0138636603625113,-0.0346945769586932,
0.0737867871141982));
#85259=CARTESIAN_POINT('Ctrl Pts',(0.0138561511930985,-0.034529677707698,
0.0736681191944533));
#85260=CARTESIAN_POINT('Ctrl Pts',(0.0138437437860077,-0.034364806625142,
0.0735498630358351));
#85261=CARTESIAN_POINT('Ctrl Pts',(0.0140925026499682,-0.0346945769586932,
0.0735381371821048));
#85262=CARTESIAN_POINT('Ctrl Pts',(0.0140798528191484,-0.034529677707698,
0.0734147381099904));
#85263=CARTESIAN_POINT('Ctrl Pts',(0.0140621136004066,-0.034364806625142,
0.073291967309973));
#85264=CARTESIAN_POINT('',(0.0140911820831894,-0.0346775396665019,0.0735253892849195));
#85265=CARTESIAN_POINT('',(0.0140925026499634,-0.0346945769586886,0.0735381371821062));
#85266=CARTESIAN_POINT('Origin',(-0.00240361219251233,-0.0345626617870493,
0.0754054589616631));
#85267=CARTESIAN_POINT('Ctrl Pts',(0.0140911820823922,-0.0346775396670096,
0.0735253892865576));
#85268=CARTESIAN_POINT('Ctrl Pts',(0.0140484573062415,-0.0346269749928188,
0.0735298613230917));
#85269=CARTESIAN_POINT('Ctrl Pts',(0.0140064918484378,-0.0345757902890792,
0.0735342539172826));
#85270=CARTESIAN_POINT('Ctrl Pts',(0.0139240449905657,-0.0344721681088079,
0.0735428836671196));
#85271=CARTESIAN_POINT('Ctrl Pts',(0.013883595912953,-0.0344197714289862,
0.0735471174338918));
#85272=CARTESIAN_POINT('Ctrl Pts',(0.013843891575457,-0.0343667727830735,
0.0735512733047019));
#85273=CARTESIAN_POINT('',(0.0139780815062471,-0.0346945769587026,0.0736624621481577));
#85274=CARTESIAN_POINT('Origin',(0.00812378219310841,-0.0315241814719618,
0.07415));
#85275=CARTESIAN_POINT('',(0.0140911820819387,-0.0347116136489598,0.073525389284308));
#85276=CARTESIAN_POINT('',(0.0140898342906076,-0.0346945769586885,0.0735126442359758));
#85277=CARTESIAN_POINT('Origin',(-0.00239703850763679,-0.0345626698387949,
0.0754502910047274));
#85278=CARTESIAN_POINT('Origin',(-0.00243540937305093,-0.0345626621451001,
0.075101684961038));
#85279=CARTESIAN_POINT('Origin',(-0.00243825970237095,-0.0345626702598509,
0.0750564632766638));
#85280=CARTESIAN_POINT('Ctrl Pts',(0.0138586640873972,-0.0352450361874068,
0.0737142336816784));
#85281=CARTESIAN_POINT('Ctrl Pts',(0.0138422288910126,-0.0349452760959493,
0.0734979390618055));
#85282=CARTESIAN_POINT('Ctrl Pts',(0.0138095481895168,-0.034644428984174,
0.0732834968784183));
#85283=CARTESIAN_POINT('Ctrl Pts',(0.0138584169978104,-0.0352450361874068,
0.073711720800516));
#85284=CARTESIAN_POINT('Ctrl Pts',(0.0138418870265576,-0.0349452760959493,
0.0734954354997799));
#85285=CARTESIAN_POINT('Ctrl Pts',(0.0138091125213945,-0.034644428984174,
0.0732810097478855));
#85286=CARTESIAN_POINT('Ctrl Pts',(0.0138339526822875,-0.0352450361874068,
0.0734629206854316));
#85287=CARTESIAN_POINT('Ctrl Pts',(0.0138080390607158,-0.0349452760959493,
0.073247558071496));
#85288=CARTESIAN_POINT('Ctrl Pts',(0.0137659770637416,-0.034644428984174,
0.0730347592000829));
#85289=CARTESIAN_POINT('Ctrl Pts',(0.0138337080391323,-0.0352450361874068,
0.0734604326842808));
#85290=CARTESIAN_POINT('Ctrl Pts',(0.0138077005810574,-0.0349452760959493,
0.0732450792972131));
#85291=CARTESIAN_POINT('Ctrl Pts',(0.0137655457091651,-0.034644428984174,
0.0730322966946049));
#85292=CARTESIAN_POINT('',(0.0138295341202117,-0.0351951634053356,0.0734271257032898));
#85293=CARTESIAN_POINT('',(0.0137950098858205,-0.0348678972925388,0.0731932861151756));
#85294=CARTESIAN_POINT('Origin',(-0.00265056203983165,-0.0345636767886071,
0.0763954462590038));
#85295=CARTESIAN_POINT('Origin',(0.0246908991536606,-0.0346946199340847,
0.0713551929864585));
#85296=CARTESIAN_POINT('',(0.0138144634960909,-0.0346945769330288,0.0733167705561675));
#85297=CARTESIAN_POINT('',(0.0138040668874039,-0.0346945769458128,0.0732551413292101));
#85298=CARTESIAN_POINT('',(0.0138438915753088,-0.0350221583435275,0.0735512733047011));
#85299=CARTESIAN_POINT('Origin',(-0.00277114445682109,-0.0345628458713436,
0.0759300396914979));
#85300=CARTESIAN_POINT('',(0.0138426617259621,-0.0351951360298763,0.073551405074696));
#85301=CARTESIAN_POINT('Origin',(0.0248017680866508,-0.0351951838366776,
0.0724043080274679));
#85302=CARTESIAN_POINT('',(0.0138295276984102,-0.0351951371328747,0.0734270938995524));
#85303=CARTESIAN_POINT('Ctrl Pts',(0.0141110788401785,-0.0350241211494342,
0.0737597707595798));
#85304=CARTESIAN_POINT('Ctrl Pts',(0.0141057035923919,-0.0349144232818961,
0.0736772982031536));
#85305=CARTESIAN_POINT('Ctrl Pts',(0.0140986203605874,-0.0348045283579412,
0.0735948873931399));
#85306=CARTESIAN_POINT('Ctrl Pts',(0.0140898342894349,-0.0346945769439158,
0.0735126442249313));
#85307=CARTESIAN_POINT('Ctrl Pts',(0.01402153137743,-0.0350241211494342,
0.0736903273025889));
#85308=CARTESIAN_POINT('Ctrl Pts',(0.0140151995744963,-0.0349144232818961,
0.0736090882257461));
#85309=CARTESIAN_POINT('Ctrl Pts',(0.0140071847119047,-0.0348045283579412,
0.0735279314062912));
#85310=CARTESIAN_POINT('Ctrl Pts',(0.0139974931873964,-0.0346945769439158,
0.0734469611778199));
#85311=CARTESIAN_POINT('Ctrl Pts',(0.0139319839146816,-0.0350241211494342,
0.0736208838455979));
#85312=CARTESIAN_POINT('Ctrl Pts',(0.0139246955566008,-0.0349144232818961,
0.0735408782483386));
#85313=CARTESIAN_POINT('Ctrl Pts',(0.013915749063222,-0.0348045283579412,
0.0734609754194426));
#85314=CARTESIAN_POINT('Ctrl Pts',(0.0139051520853578,-0.0346945769439158,
0.0733812781307084));
#85315=CARTESIAN_POINT('Ctrl Pts',(0.0138424364519331,-0.0350241211494342,
0.0735514403886069));
#85316=CARTESIAN_POINT('Ctrl Pts',(0.0138341915387052,-0.0349144232818961,
0.0734726682709311));
#85317=CARTESIAN_POINT('Ctrl Pts',(0.0138243134145394,-0.0348045283579412,
0.0733940194325939));
#85318=CARTESIAN_POINT('Ctrl Pts',(0.0138128109833192,-0.0346945769439158,
0.073315595083597));
#85319=CARTESIAN_POINT('',(0.013952148893479,-0.0346945769458128,0.0734147073963542));
#85320=CARTESIAN_POINT('Ctrl Pts',(0.0140911820786628,-0.0347116136492764,
0.073525389284645));
#85321=CARTESIAN_POINT('Ctrl Pts',(0.0140484742682065,-0.0347621546531224,
0.0735298595324166));
#85322=CARTESIAN_POINT('Ctrl Pts',(0.0140065173764627,-0.0348133084094853,
0.0735342511811529));
#85323=CARTESIAN_POINT('Ctrl Pts',(0.0139240704141856,-0.0349168561544567,
0.0735428809457194));
#85324=CARTESIAN_POINT('Ctrl Pts',(0.0138836130464321,-0.034969208901592,
0.0735471156385334));
#85325=CARTESIAN_POINT('Ctrl Pts',(0.0138438915752704,-0.0350221583434999,
0.073551273304685));
#85326=CARTESIAN_POINT('Ctrl Pts',(0.0138286065039693,-0.0351951371254987,
0.0734282304824678));
#85327=CARTESIAN_POINT('Ctrl Pts',(0.0138136843720475,-0.0350307338980978,
0.073310286819166));
#85328=CARTESIAN_POINT('Ctrl Pts',(0.013793900252131,-0.0348659306897824,
0.0731930606858455));
#85329=CARTESIAN_POINT('Ctrl Pts',(0.0138295276982961,-0.0351951371254987,
0.0734270938995756));
#85330=CARTESIAN_POINT('Ctrl Pts',(0.0138145820682361,-0.0350307338980978,
0.0733091311911591));
#85331=CARTESIAN_POINT('Ctrl Pts',(0.0137947736831052,-0.0348659306897824,
0.0731918870002012));
#85332=CARTESIAN_POINT('Ctrl Pts',(0.0139839208275945,-0.0351951371254987,
0.0732366014222163));
#85333=CARTESIAN_POINT('Ctrl Pts',(0.0139650368850841,-0.0350307338980978,
0.0731154467327211));
#85334=CARTESIAN_POINT('Ctrl Pts',(0.0139411616247454,-0.0348659306897824,
0.0729951760629167));
#85335=CARTESIAN_POINT('Origin',(0.0190390960087422,-0.0308609197410804,
0.0723086293392043));
#85336=CARTESIAN_POINT('',(0.0138968396215688,-0.0351951371254987,0.0733440434744802));
#85337=CARTESIAN_POINT('Origin',(0.00719400186664153,-0.0351840467441097,
0.0744504233596003));
#85338=CARTESIAN_POINT('Origin',(0.0197640715593353,-0.0352322614264454,
0.0713804061305721));
#85339=CARTESIAN_POINT('',(0.0137508238756827,-0.0351951142564683,0.0729607916557664));
#85340=CARTESIAN_POINT('',(0.0137224236649182,-0.0351951372916787,0.0728393842400868));
#85341=CARTESIAN_POINT('Origin',(0.0078838425506991,-0.0352875121025588,
0.0739082761889738));
#85342=CARTESIAN_POINT('Origin',(0.00840357326387426,-0.0298325076522763,
0.0816477934911835));
#85343=CARTESIAN_POINT('Origin',(0.0164034792812193,-0.0338732827791975,
0.0754518908483954));
#85344=CARTESIAN_POINT('Ctrl Pts',(0.0133750333321527,-0.0321934096636942,
0.0764957402285839));
#85345=CARTESIAN_POINT('Ctrl Pts',(0.0134170209651515,-0.0320508460845506,
0.0764017453339559));
#85346=CARTESIAN_POINT('Ctrl Pts',(0.013456451481987,-0.0319086045665427,
0.0763066931869392));
#85347=CARTESIAN_POINT('Ctrl Pts',(0.0134932568310288,-0.0317669892871418,
0.0762107954410903));
#85348=CARTESIAN_POINT('Ctrl Pts',(0.0134075587715715,-0.0321934096636942,
0.0764184580934016));
#85349=CARTESIAN_POINT('Ctrl Pts',(0.0134481630911541,-0.0320508460845506,
0.0763238810088974));
#85350=CARTESIAN_POINT('Ctrl Pts',(0.0134861956953029,-0.0319086045665427,
0.0762282842778795));
#85351=CARTESIAN_POINT('Ctrl Pts',(0.0135215916388741,-0.0317669892871418,
0.0761318804786917));
#85352=CARTESIAN_POINT('Ctrl Pts',(0.0134400842109905,-0.0321934096636942,
0.0763411759582195));
#85353=CARTESIAN_POINT('Ctrl Pts',(0.0134793052171566,-0.0320508460845506,
0.0762460166838389));
#85354=CARTESIAN_POINT('Ctrl Pts',(0.0135159399086188,-0.0319086045665427,
0.0761498753688198));
#85355=CARTESIAN_POINT('Ctrl Pts',(0.0135499264467195,-0.0317669892871418,
0.076052965516293));
#85356=CARTESIAN_POINT('Ctrl Pts',(0.0134726096504094,-0.0321934096636942,
0.0762638938230372));
#85357=CARTESIAN_POINT('Ctrl Pts',(0.0135104473431592,-0.0320508460845506,
0.0761681523587804));
#85358=CARTESIAN_POINT('Ctrl Pts',(0.0135456841219348,-0.0319086045665427,
0.0760714664597601));
#85359=CARTESIAN_POINT('Ctrl Pts',(0.0135782612545649,-0.0317669892871418,
0.0759740505538944));
#85360=CARTESIAN_POINT('',(0.0134720277638687,-0.0321934096636942,0.0762652764157065));
#85361=CARTESIAN_POINT('',(0.0135544173324776,-0.0318665617511356,0.0760437600091658));
#85362=CARTESIAN_POINT('Origin',(-0.0018299028211601,-0.032637194442213,
0.0695519445147125));
#85363=CARTESIAN_POINT('Origin',(0.0239043545394918,-0.0316939261509371,
0.0796529690538259));
#85364=CARTESIAN_POINT('',(0.0134248505768375,-0.0320197221621774,0.0763807539437511));
#85365=CARTESIAN_POINT('Ctrl Pts',(0.0134249634374963,-0.0320197392094696,
0.0763806073922188));
#85366=CARTESIAN_POINT('Ctrl Pts',(0.0134363134417641,-0.0319792716575994,
0.0763536332595562));
#85367=CARTESIAN_POINT('Ctrl Pts',(0.0134475094756399,-0.0319386439829692,
0.0763264498025123));
#85368=CARTESIAN_POINT('Ctrl Pts',(0.0134585554726475,-0.0318979099381624,
0.0762990252626989));
#85369=CARTESIAN_POINT('Ctrl Pts',(0.0134696012513228,-0.0318571766984938,
0.0762716012649517));
#85370=CARTESIAN_POINT('Ctrl Pts',(0.0134804425098669,-0.0318163871833599,
0.0762440762462864));
#85371=CARTESIAN_POINT('Ctrl Pts',(0.0134910452350077,-0.0317755399638304,
0.076216546171814));
#85372=CARTESIAN_POINT('',(0.0134235388830286,-0.0321934096636185,0.0763804885177123));
#85373=CARTESIAN_POINT('Origin',(0.015559901238655,-0.0324113659936054,
0.0772567846722962));
#85374=CARTESIAN_POINT('',(0.0134477833234587,-0.0321934096636663,0.0763228824667194));
#85375=CARTESIAN_POINT('Ctrl Pts',(0.0134701495635384,-0.0321934096636618,
0.0762660419553193));
#85376=CARTESIAN_POINT('Ctrl Pts',(0.0134993314312489,-0.0320835708272592,
0.076192311382566));
#85377=CARTESIAN_POINT('Ctrl Pts',(0.013526970521919,-0.0319739230346488,
0.0761180196593057));
#85378=CARTESIAN_POINT('Ctrl Pts',(0.0135530387681566,-0.0318646057455573,
0.0760432645506017));
#85379=CARTESIAN_POINT('Ctrl Pts',(0.0135750865250978,-0.0321934096636618,
0.0762232704827687));
#85380=CARTESIAN_POINT('Ctrl Pts',(0.0136036785408677,-0.0320835708272592,
0.0761480927475324));
#85381=CARTESIAN_POINT('Ctrl Pts',(0.0136306981727829,-0.0319739230346488,
0.0760723669081574));
#85382=CARTESIAN_POINT('Ctrl Pts',(0.0136561182868257,-0.0318646057455573,
0.0759961925037328));
#85383=CARTESIAN_POINT('Ctrl Pts',(0.0136800234866572,-0.0321934096636618,
0.0761804990102181));
#85384=CARTESIAN_POINT('Ctrl Pts',(0.0137080256504864,-0.0320835708272592,
0.0761038741124988));
#85385=CARTESIAN_POINT('Ctrl Pts',(0.0137344258236468,-0.0319739230346488,
0.0760267141570091));
#85386=CARTESIAN_POINT('Ctrl Pts',(0.0137591978054947,-0.0318646057455573,
0.0759491204568639));
#85387=CARTESIAN_POINT('Ctrl Pts',(0.0137849604482166,-0.0321934096636618,
0.0761377275376675));
#85388=CARTESIAN_POINT('Ctrl Pts',(0.0138123727601052,-0.0320835708272592,
0.0760596554774652));
#85389=CARTESIAN_POINT('Ctrl Pts',(0.0138381534745107,-0.0319739230346488,
0.0759810614058609));
#85390=CARTESIAN_POINT('Ctrl Pts',(0.0138622773241637,-0.0318646057455573,
0.075902048409995));
#85391=CARTESIAN_POINT('',(0.0137891933533198,-0.0321763980308505,0.0761256306242902));
#85392=CARTESIAN_POINT('',(0.0137849604482159,-0.0321934096636184,0.0761377275376413));
#85393=CARTESIAN_POINT('Origin',(-0.00162296792311563,-0.0326386230949013,
0.0701013982530169));
#85394=CARTESIAN_POINT('Ctrl Pts',(0.013789193350319,-0.0321763980306353,
0.0761256306232402));
#85395=CARTESIAN_POINT('Ctrl Pts',(0.0137486678207805,-0.0321259596175861,
0.0761114986432377));
#85396=CARTESIAN_POINT('Ctrl Pts',(0.0137088444486216,-0.032074916463345,
0.0760976115181317));
#85397=CARTESIAN_POINT('Ctrl Pts',(0.0136305699702279,-0.0319716057794018,
0.0760703158016795));
#85398=CARTESIAN_POINT('Ctrl Pts',(0.0135921493625819,-0.0319193786690228,
0.0760569178457389));
#85399=CARTESIAN_POINT('Ctrl Pts',(0.0135544173307223,-0.0318665617525432,
0.0760437600085492));
#85400=CARTESIAN_POINT('',(0.0136284941060523,-0.0321934096636664,0.0762015019766839));
#85401=CARTESIAN_POINT('Origin',(0.00812378219310841,-0.0315241814719618,
0.07415));
#85402=CARTESIAN_POINT('',(0.013789193353669,-0.032210423332359,0.076125630624412));
#85403=CARTESIAN_POINT('',(0.0137934004130286,-0.0321934096636183,0.0761135246981795));
#85404=CARTESIAN_POINT('Origin',(-0.00164371153138138,-0.0326387243762393,
0.0701417064010209));
#85405=CARTESIAN_POINT('Origin',(-0.00202698748102215,-0.0326386237268996,
0.0712599801182748));
#85406=CARTESIAN_POINT('Origin',(-0.00201816615670545,-0.0326387247445193,
0.0712155140851446));
#85407=CARTESIAN_POINT('Ctrl Pts',(0.0134992290150224,-0.0327445246967099,
0.0761951641657272));
#85408=CARTESIAN_POINT('Ctrl Pts',(0.0135763636425132,-0.032443687833936,
0.0759924258745165));
#85409=CARTESIAN_POINT('Ctrl Pts',(0.0136380080619782,-0.0321434074405927,
0.0757844534459835));
#85410=CARTESIAN_POINT('Ctrl Pts',(0.013583028830612,-0.0327445246967099,
0.075959627351392));
#85411=CARTESIAN_POINT('Ctrl Pts',(0.0136512800419259,-0.032443687833936,
0.0757537284984683));
#85412=CARTESIAN_POINT('Ctrl Pts',(0.0137038282156356,-0.0321434074405927,
0.0755432736222576));
#85413=CARTESIAN_POINT('',(0.0135942935279991,-0.0326943950436612,0.0759252832829815));
#85414=CARTESIAN_POINT('',(0.0136626113902798,-0.0323666188837389,0.0756990307048482));
#85415=CARTESIAN_POINT('Origin',(-0.00241905260426027,-0.0326395579112032,
0.0708085652071837));
#85416=CARTESIAN_POINT('Origin',(0.0242990896511115,-0.03219338256031,0.0786737074993454));
#85417=CARTESIAN_POINT('',(0.0136276364285373,-0.0321934096532689,0.0758190457010026));
#85418=CARTESIAN_POINT('',(0.0136444697427272,-0.0321934096584275,0.0757588552542595));
#85419=CARTESIAN_POINT('',(0.0135544173333586,-0.0325210109756238,0.0760437600094734));
#85420=CARTESIAN_POINT('Origin',(-0.00224670839597938,-0.0326393129158107,
0.0703596978508215));
#85421=CARTESIAN_POINT('',(0.0135531345566467,-0.0326943950436595,0.0760433126821901));
#85422=CARTESIAN_POINT('Origin',(0.0239986938429456,-0.0326943765538175,
0.0796858678152558));
#85423=CARTESIAN_POINT('',(0.0135737140423329,-0.0326943950436703,0.0759842979825958));
#85424=CARTESIAN_POINT('Ctrl Pts',(0.0137074012942602,-0.0325229783203769,
0.076346177983078));
#85425=CARTESIAN_POINT('Ctrl Pts',(0.0137376755597297,-0.032413025309245,
0.0762692079158743));
#85426=CARTESIAN_POINT('Ctrl Pts',(0.0137663530087985,-0.032303122220807,
0.0761916232606182));
#85427=CARTESIAN_POINT('Ctrl Pts',(0.0137934004145011,-0.0321934096576658,
0.0761135246939511));
#85428=CARTESIAN_POINT('Ctrl Pts',(0.0136559439311935,-0.0325229783203769,
0.0762452161981136));
#85429=CARTESIAN_POINT('Ctrl Pts',(0.0136848264406652,-0.032413025309245,
0.0761689554695345));
#85430=CARTESIAN_POINT('Ctrl Pts',(0.0137121270184039,-0.032303122220807,
0.0760921088355785));
#85431=CARTESIAN_POINT('Ctrl Pts',(0.01373781416776,-0.0321934096576658,
0.0760147759653));
#85432=CARTESIAN_POINT('Ctrl Pts',(0.0136044865681269,-0.0325229783203769,
0.0761442544131492));
#85433=CARTESIAN_POINT('Ctrl Pts',(0.0136319773216007,-0.032413025309245,
0.0760687030231947));
#85434=CARTESIAN_POINT('Ctrl Pts',(0.0136579010280093,-0.032303122220807,
0.0759925944105388));
#85435=CARTESIAN_POINT('Ctrl Pts',(0.0136822279210189,-0.0321934096576658,
0.0759160272366489));
#85436=CARTESIAN_POINT('Ctrl Pts',(0.0135530292050603,-0.0325229783203769,
0.0760432926281848));
#85437=CARTESIAN_POINT('Ctrl Pts',(0.0135791282025363,-0.032413025309245,
0.0759684505768548));
#85438=CARTESIAN_POINT('Ctrl Pts',(0.0136036750376147,-0.032303122220807,
0.0758930799854991));
#85439=CARTESIAN_POINT('Ctrl Pts',(0.0136266416742778,-0.0321934096576658,
0.0758172785079978));
#85440=CARTESIAN_POINT('',(0.013710518420781,-0.0321934096584275,0.0759662852001075));
#85441=CARTESIAN_POINT('Ctrl Pts',(0.013789193350379,-0.0322104233328888,
0.0761256306232612));
#85442=CARTESIAN_POINT('Ctrl Pts',(0.0137486129080943,-0.0322609421830356,
0.0761114794941978));
#85443=CARTESIAN_POINT('Ctrl Pts',(0.0137087627101504,-0.0323120888238684,
0.0760975830144516));
#85444=CARTESIAN_POINT('Ctrl Pts',(0.0136304876391121,-0.0324156524631808,
0.0760702870913336));
#85445=CARTESIAN_POINT('Ctrl Pts',(0.0135920949414026,-0.0324680267167306,
0.0760568988680963));
#85446=CARTESIAN_POINT('Ctrl Pts',(0.0135544173333192,-0.0325210109755912,
0.0760437600094549));
#85447=CARTESIAN_POINT('Origin',(0.00465724459401615,-0.0262834582510581,
0.081213037796583));
#85448=CARTESIAN_POINT('Origin',(0.0166002198596635,-0.0342771039346039,
0.0828663732632542));
#85449=CARTESIAN_POINT('Ctrl Pts',(0.0135924675457463,-0.0326943950436604,
0.0759261650310439));
#85450=CARTESIAN_POINT('Ctrl Pts',(0.0136169464287621,-0.0325844576448134,
0.0758507962974757));
#85451=CARTESIAN_POINT('Ctrl Pts',(0.0136398682952076,-0.0324744968375322,
0.0757749159665108));
#85452=CARTESIAN_POINT('Ctrl Pts',(0.0136612051172386,-0.0323646534831894,
0.0756986216655388));
#85453=CARTESIAN_POINT('Ctrl Pts',(0.0136945116474589,-0.0326943950436604,
0.075876888983232));
#85454=CARTESIAN_POINT('Ctrl Pts',(0.0137183114141827,-0.0325844576448134,
0.0758001138906913));
#85455=CARTESIAN_POINT('Ctrl Pts',(0.0137405250304648,-0.0324744968375322,
0.0757228411464619));
#85456=CARTESIAN_POINT('Ctrl Pts',(0.0137611254005196,-0.0323646534831894,
0.0756451701494581));
#85457=CARTESIAN_POINT('Ctrl Pts',(0.0137965557491715,-0.0326943950436604,
0.0758276129354202));
#85458=CARTESIAN_POINT('Ctrl Pts',(0.0138196763996034,-0.0325844576448134,
0.0757494314839068));
#85459=CARTESIAN_POINT('Ctrl Pts',(0.013841181765722,-0.0324744968375322,
0.0756707663264129));
#85460=CARTESIAN_POINT('Ctrl Pts',(0.0138610456838007,-0.0323646534831894,
0.0755917186333774));
#85461=CARTESIAN_POINT('Ctrl Pts',(0.0138985998508842,-0.0326943950436604,
0.0757783368876083));
#85462=CARTESIAN_POINT('Ctrl Pts',(0.013921041385024,-0.0325844576448134,
0.0756987490771223));
#85463=CARTESIAN_POINT('Ctrl Pts',(0.0139418385009792,-0.0324744968375322,
0.075618691506364));
#85464=CARTESIAN_POINT('Ctrl Pts',(0.0139609659670817,-0.0323646534831894,
0.0755382671172967));
#85465=CARTESIAN_POINT('',(0.0139020648320283,-0.0326773559991386,0.0757659980585012));
#85466=CARTESIAN_POINT('',(0.0138985998508739,-0.0326943950436594,0.0757783368876127));
#85467=CARTESIAN_POINT('Origin',(-0.00210300197949981,-0.0326395669973887,
0.07134206908712));
#85468=CARTESIAN_POINT('Ctrl Pts',(0.0139020648287955,-0.0326773559987492,
0.0757659980575934));
#85469=CARTESIAN_POINT('Ctrl Pts',(0.0138606986508299,-0.0326267922586907,
0.0757544292805956));
#85470=CARTESIAN_POINT('Ctrl Pts',(0.0138200656584954,-0.0325756109581209,
0.0757430655518155));
#85471=CARTESIAN_POINT('Ctrl Pts',(0.0137402314641275,-0.0324719985462385,
0.0757207385195185));
#85472=CARTESIAN_POINT('Ctrl Pts',(0.0137010622816187,-0.0324196091621774,
0.0757097841708231));
#85473=CARTESIAN_POINT('Ctrl Pts',(0.0136626113902329,-0.0323666188837756,
0.0756990307048351));
#85474=CARTESIAN_POINT('',(0.0137464466894465,-0.0326943950436703,0.0758518100853071));
#85475=CARTESIAN_POINT('Origin',(0.00812378219310841,-0.0315241814719618,
0.07415));
#85476=CARTESIAN_POINT('',(0.0139020648319844,-0.0327114338380031,0.0757659980584892));
#85477=CARTESIAN_POINT('',(0.0139055034524797,-0.0326943950436593,0.07575365185715));
#85478=CARTESIAN_POINT('Origin',(-0.00211445486482875,-0.0326395680973115,
0.0713859069133253));
#85479=CARTESIAN_POINT('Origin',(-0.00207593974010854,-0.0326395673974004,
0.0712453008667923));
#85480=CARTESIAN_POINT('Origin',(-0.00206298814364472,-0.0326395684136933,
0.0712018820662543));
#85481=CARTESIAN_POINT('Ctrl Pts',(0.013617050337381,-0.0332451089994434,
0.075853563939252));
#85482=CARTESIAN_POINT('Ctrl Pts',(0.0136813013025508,-0.0329451141710254,
0.0756463819415156));
#85483=CARTESIAN_POINT('Ctrl Pts',(0.0137297639424734,-0.0326442513127493,
0.0754349488806122));
#85484=CARTESIAN_POINT('Ctrl Pts',(0.0136858936751811,-0.0332451089994434,
0.0756132295995488));
#85485=CARTESIAN_POINT('Ctrl Pts',(0.0137410802824282,-0.0329451141710254,
0.0754034511328469));
#85486=CARTESIAN_POINT('Ctrl Pts',(0.0137803087386556,-0.0326442513127493,
0.0751901117437663));
#85487=CARTESIAN_POINT('Ctrl Pts',(0.013686582108559,-0.0332451089994434,
0.0756108262561518));
#85488=CARTESIAN_POINT('Ctrl Pts',(0.013741678072227,-0.0329451141710254,
0.0754010218247602));
#85489=CARTESIAN_POINT('Ctrl Pts',(0.0137808141866174,-0.0326442513127493,
0.0751876633723979));
#85490=CARTESIAN_POINT('',(0.0136949696831494,-0.0331951640388616,0.0755782839181379));
#85491=CARTESIAN_POINT('',(0.0137489462276525,-0.0328677532355042,0.0753481880713479));
#85492=CARTESIAN_POINT('Origin',(-0.00271755611842626,-0.0326402808279871,
0.0721634275105179));
#85493=CARTESIAN_POINT('Origin',(0.0245624040873967,-0.0326944278779078,
0.0776511236085911));
#85494=CARTESIAN_POINT('',(0.0137215760778875,-0.0326943950436593,0.0754701623474143));
#85495=CARTESIAN_POINT('',(0.013734596785053,-0.0326943950436693,0.0754090337028689));
#85496=CARTESIAN_POINT('',(0.0136626113902791,-0.0330220786163545,0.0756990307048509));
#85497=CARTESIAN_POINT('Origin',(-0.00264833655376976,-0.0326396682764074,
0.0716876530920411));
#85498=CARTESIAN_POINT('',(0.013661303056921,-0.0331951640388588,0.0756986648064837));
#85499=CARTESIAN_POINT('Origin',(0.0242853043275887,-0.0331952026560181,
0.078669854226103));
#85500=CARTESIAN_POINT('',(0.0136781363700452,-0.0331951640388702,0.0756384743623208));
#85501=CARTESIAN_POINT('Ctrl Pts',(0.013834282748829,-0.0330240426238172,
0.0759912450687558));
#85502=CARTESIAN_POINT('Ctrl Pts',(0.0138596476934892,-0.0329142774063519,
0.0759125773601296));
#85503=CARTESIAN_POINT('Ctrl Pts',(0.0138833990022148,-0.0328043479726691,
0.075833346068522));
#85504=CARTESIAN_POINT('Ctrl Pts',(0.0139055034524855,-0.0326943950436593,
0.0757536518571589));
#85505=CARTESIAN_POINT('Ctrl Pts',(0.0137765874806087,-0.0330240426238172,
0.0758937135763538));
#85506=CARTESIAN_POINT('Ctrl Pts',(0.0138006088339408,-0.0329142774063519,
0.0758158406762571));
#85507=CARTESIAN_POINT('Ctrl Pts',(0.0138230323124214,-0.0328043479726691,
0.075737432365206));
#85508=CARTESIAN_POINT('Ctrl Pts',(0.0138438264236151,-0.0326943950436593,
0.0756585882989735));
#85509=CARTESIAN_POINT('Ctrl Pts',(0.0137188922123885,-0.0330240426238172,
0.0757961820839519));
#85510=CARTESIAN_POINT('Ctrl Pts',(0.0137415699743924,-0.0329142774063519,
0.0757191039923847));
#85511=CARTESIAN_POINT('Ctrl Pts',(0.013762665622628,-0.0328043479726691,
0.07564151866189));
#85512=CARTESIAN_POINT('Ctrl Pts',(0.0137821493947446,-0.0326943950436593,
0.0755635247407881));
#85513=CARTESIAN_POINT('Ctrl Pts',(0.0136611969441682,-0.0330240426238172,
0.0756986505915499));
#85514=CARTESIAN_POINT('Ctrl Pts',(0.013682531114844,-0.0329142774063519,
0.0756223673085122));
#85515=CARTESIAN_POINT('Ctrl Pts',(0.0137022989328347,-0.0328043479726691,
0.075545604958574));
#85516=CARTESIAN_POINT('Ctrl Pts',(0.0137204723658742,-0.0326943950436593,
0.0754684611826027));
#85517=CARTESIAN_POINT('',(0.0138135397651936,-0.0326943950436694,0.0756119071022922));
#85518=CARTESIAN_POINT('Ctrl Pts',(0.0139020648287864,-0.0327114338383284,
0.0757659980575908));
#85519=CARTESIAN_POINT('Ctrl Pts',(0.0138607055313769,-0.032761987683,0.0757544312048612));
#85520=CARTESIAN_POINT('Ctrl Pts',(0.0138200758998282,-0.0328131562602372,
0.0757430684159838));
#85521=CARTESIAN_POINT('Ctrl Pts',(0.0137402417787694,-0.0329167375858765,
0.075720741404189));
#85522=CARTESIAN_POINT('Ctrl Pts',(0.0137010690995078,-0.0329691088920621,
0.0757097860775654));
#85523=CARTESIAN_POINT('Ctrl Pts',(0.0136626113902341,-0.0330220786163187,
0.0756990307048355));
#85524=CARTESIAN_POINT('Ctrl Pts',(0.0136932023873735,-0.0331951640388604,
0.0755792787394434));
#85525=CARTESIAN_POINT('Ctrl Pts',(0.0137227518089432,-0.0330306422010619,
0.0754641345477069));
#85526=CARTESIAN_POINT('Ctrl Pts',(0.0137475169502063,-0.0328657861914645,
0.0753478674372073));
#85527=CARTESIAN_POINT('Ctrl Pts',(0.0136949696831486,-0.0331951640388604,
0.075578283918141));
#85528=CARTESIAN_POINT('Ctrl Pts',(0.0137244985374257,-0.0330306422010619,
0.0754631031886974));
#85529=CARTESIAN_POINT('Ctrl Pts',(0.0137492416188289,-0.0328657861914645,
0.0753468004217798));
#85530=CARTESIAN_POINT('Ctrl Pts',(0.0139894486865091,-0.0331951640388604,
0.0754125199358008));
#85531=CARTESIAN_POINT('Ctrl Pts',(0.0140155504767293,-0.0330306422010619,
0.0752912510417652));
#85532=CARTESIAN_POINT('Ctrl Pts',(0.0140366177922328,-0.0328657861914645,
0.0751690069567108));
#85533=CARTESIAN_POINT('',(0.0139921320699566,-0.0331781648281952,0.075399987887492));
#85534=CARTESIAN_POINT('',(0.0139894486864998,-0.0331951640388588,0.075412519935805));
#85535=CARTESIAN_POINT('Origin',(-0.00230100785000773,-0.0326412091906117,
0.0726577128430273));
#85536=CARTESIAN_POINT('Ctrl Pts',(0.0139921320685952,-0.033178164828644,
0.0753999878887349));
#85537=CARTESIAN_POINT('Ctrl Pts',(0.0139500921824034,-0.0331276811546773,
0.0753910331949971));
#85538=CARTESIAN_POINT('Ctrl Pts',(0.0139088113993209,-0.0330765663497786,
0.0753822402283719));
#85539=CARTESIAN_POINT('Ctrl Pts',(0.0138277326057297,-0.0329730614463383,
0.0753649700360556));
#85540=CARTESIAN_POINT('Ctrl Pts',(0.0137879673504078,-0.0329207133374314,
0.075356499781904));
#85541=CARTESIAN_POINT('Ctrl Pts',(0.0137489462332635,-0.0328677532289396,
0.075348188086834));
#85542=CARTESIAN_POINT('',(0.0138422091848346,-0.0331951640388702,0.0754954019269815));
#85543=CARTESIAN_POINT('Origin',(0.00812378219310841,-0.0315241814719618,
0.07415));
#85544=CARTESIAN_POINT('',(0.0139921320685731,-0.0332121607144397,0.0753999878865365));
#85545=CARTESIAN_POINT('',(0.0139947886795375,-0.0331951640388587,0.0753874501348798));
#85546=CARTESIAN_POINT('Origin',(-0.00230263995881673,-0.032641366587239,
0.0727030277353702));
#85547=CARTESIAN_POINT('Origin',(-0.00200423392533245,-0.0326412095231821,
0.0712644370570124));
#85548=CARTESIAN_POINT('Origin',(-0.00198725603646544,-0.0326413668431202,
0.0712223907886903));
#85549=CARTESIAN_POINT('Ctrl Pts',(0.0137131733834289,-0.0337436976235975,
0.0755052974291894));
#85550=CARTESIAN_POINT('Ctrl Pts',(0.013725363133908,-0.0336723290703325,
0.0754550255977284));
#85551=CARTESIAN_POINT('Ctrl Pts',(0.0137366466805782,-0.033601104548885,
0.0754045426438751));
#85552=CARTESIAN_POINT('Ctrl Pts',(0.0137726728099513,-0.0333736987606857,
0.0752433605723316));
#85553=CARTESIAN_POINT('Ctrl Pts',(0.0137993900144804,-0.0331450831799193,
0.0750803767290625));
#85554=CARTESIAN_POINT('Ctrl Pts',(0.0137667910410127,-0.0337436976235975,
0.0752611148196628));
#85555=CARTESIAN_POINT('Ctrl Pts',(0.0137767845760948,-0.0336723290703325,
0.0752103607428634));
#85556=CARTESIAN_POINT('Ctrl Pts',(0.0137858635885902,-0.033601104548885,
0.0751594351246805));
#85557=CARTESIAN_POINT('Ctrl Pts',(0.0138148510770372,-0.0333736987606857,
0.0749968397136192));
#85558=CARTESIAN_POINT('Ctrl Pts',(0.0138344601341928,-0.0331450831799193,
0.0748328487777047));
#85559=CARTESIAN_POINT('Ctrl Pts',(0.0137673272175885,-0.0337436976235975,
0.0752586729935675));
#85560=CARTESIAN_POINT('Ctrl Pts',(0.0137772987905167,-0.0336723290703325,
0.0752079140943148));
#85561=CARTESIAN_POINT('Ctrl Pts',(0.0137863557576704,-0.033601104548885,
0.0751569840494886));
#85562=CARTESIAN_POINT('Ctrl Pts',(0.013815272859708,-0.0333736987606857,
0.0749943745050321));
#85563=CARTESIAN_POINT('Ctrl Pts',(0.0138348108353899,-0.0331450831799193,
0.0748303734981911));
#85564=CARTESIAN_POINT('',(0.0137736589065124,-0.0336938721132548,0.0752256477691773));
#85565=CARTESIAN_POINT('',(0.0138130810958987,-0.0333679869945434,0.0749926167544268));
#85566=CARTESIAN_POINT('Ctrl Pts',(0.0137736589065116,-0.033693872113265,
0.075225647769185));
#85567=CARTESIAN_POINT('Ctrl Pts',(0.0137778576643496,-0.0336629187933933,
0.0752035936499681));
#85568=CARTESIAN_POINT('Ctrl Pts',(0.0137819259435898,-0.0336319952301041,
0.0751815219987686));
#85569=CARTESIAN_POINT('Ctrl Pts',(0.0137858635885888,-0.0336011045488951,
0.0751594351246881));
#85570=CARTESIAN_POINT('Ctrl Pts',(0.0137957444872779,-0.0335235892595455,
0.0751040115999173));
#85571=CARTESIAN_POINT('Ctrl Pts',(0.0138048202190069,-0.033445866866037,
0.0750483937113056));
#85572=CARTESIAN_POINT('Ctrl Pts',(0.0138130810961996,-0.0333679869945386,
0.0749926167544781));
#85573=CARTESIAN_POINT('Ctrl Pts',(0.0138130882913061,-0.0333679692459662,
0.0749925728648361));
#85574=CARTESIAN_POINT('Ctrl Pts',(0.0138126390995285,-0.0333391895375448,
0.0749925123291621));
#85575=CARTESIAN_POINT('Ctrl Pts',(0.0138123019746852,-0.0333104081062116,
0.0749924701728113));
#85576=CARTESIAN_POINT('Ctrl Pts',(0.0138118550452382,-0.0332532698397309,
0.0749924198673398));
#85577=CARTESIAN_POINT('Ctrl Pts',(0.0138117419226178,-0.0332249172105485,
0.0749924112222633));
#85578=CARTESIAN_POINT('Ctrl Pts',(0.0138117372809526,-0.0331960985330548,
0.0749924175098249));
#85579=CARTESIAN_POINT('Ctrl Pts',(0.0138117372351345,-0.0331956312594731,
0.074992417616085));
#85580=CARTESIAN_POINT('Ctrl Pts',(0.013811737218836,-0.0331951640388587,
0.0749924177261313));
#85581=CARTESIAN_POINT('',(0.0137934237900075,-0.0331951640388587,0.0751160689223408));
#85582=CARTESIAN_POINT('',(0.0138025805044319,-0.0331951640388689,0.0750542433242451));
#85583=CARTESIAN_POINT('',(0.0137489462183953,-0.0335216366567655,0.0753481880838062));
#85584=CARTESIAN_POINT('Origin',(-0.00274924111042168,-0.032643457152848,
0.0730721213285905));
#85585=CARTESIAN_POINT('',(0.0137476174921985,-0.0336938721132328,0.0753479050583037));
#85586=CARTESIAN_POINT('Origin',(0.0244285706859872,-0.0336938867896299,
0.0776230026007841));
#85587=CARTESIAN_POINT('',(0.0137606381993654,-0.0336938721132539,0.0752867764137505));
#85588=CARTESIAN_POINT('Ctrl Pts',(0.0139386273517803,-0.0335235895815171,
0.0756290455641303));
#85589=CARTESIAN_POINT('Ctrl Pts',(0.0139589893259433,-0.0334144449262748,
0.0755489927721446));
#85590=CARTESIAN_POINT('Ctrl Pts',(0.0139777208631117,-0.0333049234473147,
0.0754684273461374));
#85591=CARTESIAN_POINT('Ctrl Pts',(0.0139947886795439,-0.0331951640388587,
0.0753874501348884));
#85592=CARTESIAN_POINT('Ctrl Pts',(0.0138749217733604,-0.0335235895815171,
0.0755353291207238));
#85593=CARTESIAN_POINT('Ctrl Pts',(0.0138939935561692,-0.0334144449262748,
0.0754561533614498));
#85594=CARTESIAN_POINT('Ctrl Pts',(0.0139114515385457,-0.0333049234473147,
0.075376492630141));
#85595=CARTESIAN_POINT('Ctrl Pts',(0.0139272641700241,-0.0331951640388587,
0.0752964467662657));
#85596=CARTESIAN_POINT('Ctrl Pts',(0.0138112161949406,-0.0335235895815171,
0.0754416126773173));
#85597=CARTESIAN_POINT('Ctrl Pts',(0.0138289977863952,-0.0334144449262748,
0.075363313950755));
#85598=CARTESIAN_POINT('Ctrl Pts',(0.0138451822139797,-0.0333049234473147,
0.0752845579141447));
#85599=CARTESIAN_POINT('Ctrl Pts',(0.0138597396605043,-0.0331951640388587,
0.0752054433976429));
#85600=CARTESIAN_POINT('Ctrl Pts',(0.0137475106165207,-0.0335235895815171,
0.0753478962339108));
#85601=CARTESIAN_POINT('Ctrl Pts',(0.0137640020166211,-0.0334144449262748,
0.0752704745400602));
#85602=CARTESIAN_POINT('Ctrl Pts',(0.0137789128894136,-0.0333049234473147,
0.0751926231981483));
#85603=CARTESIAN_POINT('Ctrl Pts',(0.0137922151509845,-0.0331951640388587,
0.0751144400290202));
#85604=CARTESIAN_POINT('',(0.0138941062347825,-0.0331951640388687,0.0752517595286203));
#85605=CARTESIAN_POINT('Ctrl Pts',(0.0139921320655044,-0.0332121607145939,
0.0753999878858787));
#85606=CARTESIAN_POINT('Ctrl Pts',(0.0139501629037396,-0.0332625444108773,
0.0753910482444246));
#85607=CARTESIAN_POINT('Ctrl Pts',(0.013908916936489,-0.0333135300744848,
0.0753822626470206));
#85608=CARTESIAN_POINT('Ctrl Pts',(0.0138278386502114,-0.0334167203140541,
0.0753649925663576));
#85609=CARTESIAN_POINT('Ctrl Pts',(0.0137880377336986,-0.0334688847587219,
0.0753565147719912));
#85610=CARTESIAN_POINT('Ctrl Pts',(0.013748946217736,-0.0335216366562274,
0.0753481880834917));
#85611=CARTESIAN_POINT('Ctrl Pts',(0.0137728201219758,-0.0336938721132391,
0.0752261919707698));
#85612=CARTESIAN_POINT('Ctrl Pts',(0.0137791194306991,-0.0336474569764958,
0.0751931262772226));
#85613=CARTESIAN_POINT('Ctrl Pts',(0.0137850312320981,-0.033601104548885,
0.0751599891079957));
#85614=CARTESIAN_POINT('Ctrl Pts',(0.0137999985540321,-0.0334837508592656,
0.0750760934142263));
#85615=CARTESIAN_POINT('Ctrl Pts',(0.0138124733000704,-0.0333660264659097,
0.0749917910484813));
#85616=CARTESIAN_POINT('Ctrl Pts',(0.0137736589065085,-0.0336938721132391,
0.0752256477691974));
#85617=CARTESIAN_POINT('Ctrl Pts',(0.0137799550298394,-0.0336474569764958,
0.075192577165966));
#85618=CARTESIAN_POINT('Ctrl Pts',(0.0137858635885902,-0.033601104548885,
0.0751594351246804));
#85619=CARTESIAN_POINT('Ctrl Pts',(0.0138008227008845,-0.0334837508592656,
0.0750755270959784));
#85620=CARTESIAN_POINT('Ctrl Pts',(0.0138132888753787,-0.0333660264659097,
0.074991212643986));
#85621=CARTESIAN_POINT('Ctrl Pts',(0.0140588493533195,-0.0336938721132391,
0.0750406168303471));
#85622=CARTESIAN_POINT('Ctrl Pts',(0.0140640624291655,-0.0336474569764958,
0.0750058769127942));
#85623=CARTESIAN_POINT('Ctrl Pts',(0.0140688684732108,-0.033601104548885,
0.074971078350008));
#85624=CARTESIAN_POINT('Ctrl Pts',(0.0140810362717547,-0.0334837508592656,
0.0748829763897245));
#85625=CARTESIAN_POINT('Ctrl Pts',(0.0140905880833494,-0.0333660264659097,
0.07479455256023));
#85626=CARTESIAN_POINT('',(0.0140590396112592,-0.0336769361243754,0.0750290445837871));
#85627=CARTESIAN_POINT('',(0.0140571484162445,-0.0336938721132327,0.0750417203946012));
#85628=CARTESIAN_POINT('Ctrl Pts',(0.0140590396112593,-0.0336769361243751,
0.0750290445837868));
#85629=CARTESIAN_POINT('Ctrl Pts',(0.0140587266449707,-0.0336797586670006,
0.0750311577137922));
#85630=CARTESIAN_POINT('Ctrl Pts',(0.0140584125620124,-0.0336825812712807,
0.0750332705967396));
#85631=CARTESIAN_POINT('Ctrl Pts',(0.0140577821643453,-0.0336882265933959,
0.0750374958613505));
#85632=CARTESIAN_POINT('Ctrl Pts',(0.0140574658496594,-0.0336910493112157,
0.0750396082430009));
#85633=CARTESIAN_POINT('Ctrl Pts',(0.0140571484162523,-0.0336938721132359,
0.0750417203945982));
#85634=CARTESIAN_POINT('Ctrl Pts',(0.0140590396112592,-0.0336769361243754,
0.075029044583787));
#85635=CARTESIAN_POINT('Ctrl Pts',(0.0140175781345869,-0.0336279007642955,
0.0750229039088446));
#85636=CARTESIAN_POINT('Ctrl Pts',(0.0139755263106284,-0.0335767878888528,
0.0750166758001912));
#85637=CARTESIAN_POINT('Ctrl Pts',(0.0138931165229763,-0.0334733199122762,
0.0750044704529951));
#85638=CARTESIAN_POINT('Ctrl Pts',(0.0138527094975521,-0.0334209645148418,
0.0749984859481377));
#85639=CARTESIAN_POINT('Ctrl Pts',(0.0138130810948211,-0.0333679869844681,
0.0749926167616255));
#85640=CARTESIAN_POINT('',(0.0139154036613885,-0.0336938721132538,0.0751336840818993));
#85641=CARTESIAN_POINT('Origin',(0.00812378219310841,-0.0315241814719618,
0.07415));
#85642=CARTESIAN_POINT('',(0.0140590396099847,-0.0337108120655525,0.0750290445836027));
#85643=CARTESIAN_POINT('',(0.0140609037262012,-0.0336938721132327,0.0750163647622644));
#85644=CARTESIAN_POINT('Origin',(-0.00196188876620853,-0.034556252508419,
0.0715264587038875));
#85645=CARTESIAN_POINT('Ctrl Pts',(0.0140609037262135,-0.0336938721132384,
0.0750163647622739));
#85646=CARTESIAN_POINT('Ctrl Pts',(0.0140605953171296,-0.0336910492952914,
0.0750184782626061));
#85647=CARTESIAN_POINT('Ctrl Pts',(0.014060285773266,-0.0336882265854332,
0.0750205916409574));
#85648=CARTESIAN_POINT('Ctrl Pts',(0.0140596644034946,-0.0336825812712899,
0.0750248182365514));
#85649=CARTESIAN_POINT('Ctrl Pts',(0.0140593525775484,-0.0336797586670054,
0.0750269314537783));
#85650=CARTESIAN_POINT('Ctrl Pts',(0.0140590396112593,-0.0336769361243754,
0.0750290445837871));
#85651=CARTESIAN_POINT('Origin',(-0.00228936319632219,-0.0345562520762143,
0.0737375521816172));
#85652=CARTESIAN_POINT('Ctrl Pts',(0.0137872348328979,-0.034243627687391,
0.0751517131310215));
#85653=CARTESIAN_POINT('Ctrl Pts',(0.0138250150664495,-0.0339430054201809,
0.0749381124934607));
#85654=CARTESIAN_POINT('Ctrl Pts',(0.0138465986950957,-0.0336441434784052,
0.0747222729109276));
#85655=CARTESIAN_POINT('Ctrl Pts',(0.0138254165536227,-0.034243627687391,
0.0749046460223194));
#85656=CARTESIAN_POINT('Ctrl Pts',(0.0138538784975556,-0.0339430054201809,
0.0746896053374219));
#85657=CARTESIAN_POINT('Ctrl Pts',(0.0138660618386013,-0.0336441434784052,
0.0744730316903302));
#85658=CARTESIAN_POINT('Ctrl Pts',(0.01382579837083,-0.034243627687391,
0.0749021753512324));
#85659=CARTESIAN_POINT('Ctrl Pts',(0.0138541671318667,-0.0339430054201809,
0.0746871202658616));
#85660=CARTESIAN_POINT('Ctrl Pts',(0.0138662564700364,-0.0336441434784052,
0.0744705392781243));
#85661=CARTESIAN_POINT('',(0.0138300506476653,-0.0341934961088741,0.0748687665299178));
#85662=CARTESIAN_POINT('',(0.0138547629078723,-0.0338664212862961,0.0746337200149233));
#85663=CARTESIAN_POINT('Origin',(-0.00270215153662594,-0.0345610720404767,
0.0722727244082535));
#85664=CARTESIAN_POINT('Origin',(0.0247821651368593,-0.0336938005073037,
0.0755560024812745));
#85665=CARTESIAN_POINT('',(0.0138428960169573,-0.0336938721132327,0.0747581628645857));
#85666=CARTESIAN_POINT('',(0.0138481526012722,-0.0336938721132427,0.07469588431033));
#85667=CARTESIAN_POINT('',(0.0138130810948203,-0.0340203938281605,0.0749926167616308));
#85668=CARTESIAN_POINT('Origin',(-0.00255511611877068,-0.0345589643245864,
0.0718145570586121));
#85669=CARTESIAN_POINT('',(0.0138117372188363,-0.0341934961088739,0.0749924177261294));
#85670=CARTESIAN_POINT('Origin',(0.0247122797882539,-0.0341934220717659,
0.0766068495011657));
#85671=CARTESIAN_POINT('',(0.0138208939332608,-0.034193496108884,0.0749305921280336));
#85672=CARTESIAN_POINT('Ctrl Pts',(0.0140200226158527,-0.0340223579322396,
0.0752610125459693));
#85673=CARTESIAN_POINT('Ctrl Pts',(0.0140353463765039,-0.0339125849573575,
0.0751796880124991));
#85674=CARTESIAN_POINT('Ctrl Pts',(0.0140489761404553,-0.0338030433565231,
0.0750981034585989));
#85675=CARTESIAN_POINT('Ctrl Pts',(0.0140609037262082,-0.0336938721132327,
0.0750163647622726));
#85676=CARTESIAN_POINT('Ctrl Pts',(0.0139505582626346,-0.0340223579322396,
0.0751714810796408));
#85677=CARTESIAN_POINT('Ctrl Pts',(0.0139646471508573,-0.0339125849573575,
0.075091114640772));
#85678=CARTESIAN_POINT('Ctrl Pts',(0.0139770627404427,-0.0338030433565231,
0.0750105130672212));
#85679=CARTESIAN_POINT('Ctrl Pts',(0.0139877982911827,-0.0336938721132327,
0.0749297808422835));
#85680=CARTESIAN_POINT('Ctrl Pts',(0.0138810939094166,-0.0340223579322396,
0.0750819496133122));
#85681=CARTESIAN_POINT('Ctrl Pts',(0.0138939479252108,-0.0339125849573575,
0.0750025412690449));
#85682=CARTESIAN_POINT('Ctrl Pts',(0.0139051493404301,-0.0338030433565231,
0.0749229226758435));
#85683=CARTESIAN_POINT('Ctrl Pts',(0.0139146928561573,-0.0336938721132327,
0.0748431969222943));
#85684=CARTESIAN_POINT('Ctrl Pts',(0.0138116295561985,-0.0340223579322396,
0.0749924181469836));
#85685=CARTESIAN_POINT('Ctrl Pts',(0.0138232486995642,-0.0339125849573575,
0.0749139678973179));
#85686=CARTESIAN_POINT('Ctrl Pts',(0.0138332359404174,-0.0338030433565231,
0.0748353322844658));
#85687=CARTESIAN_POINT('Ctrl Pts',(0.0138415874211319,-0.0336938721132327,
0.0747566130023051));
#85688=CARTESIAN_POINT('',(0.0139518998715892,-0.0336938721132427,0.0748872638134351));
#85689=CARTESIAN_POINT('Ctrl Pts',(0.0140590396064153,-0.0337108120662652,
0.0750290445830697));
#85690=CARTESIAN_POINT('Ctrl Pts',(0.0140165043308049,-0.0337611408993368,
0.0750227448725414));
#85691=CARTESIAN_POINT('Ctrl Pts',(0.013974745229603,-0.0338121088779436,
0.0750165601177533));
#85692=CARTESIAN_POINT('Ctrl Pts',(0.0138927413338591,-0.0339153382773232,
0.0750044148854029));
#85693=CARTESIAN_POINT('Ctrl Pts',(0.0138525312322051,-0.0339675558473114,
0.0749984595460499));
#85694=CARTESIAN_POINT('Ctrl Pts',(0.0138130810947816,-0.0340203938281304,
0.0749926167616198));
#85695=CARTESIAN_POINT('Ctrl Pts',(0.0138284218968565,-0.0341934961088741,
0.074869975063197));
#85696=CARTESIAN_POINT('Ctrl Pts',(0.0138433068140832,-0.0340287516182428,
0.0747520361315048));
#85697=CARTESIAN_POINT('Ctrl Pts',(0.0138533045069107,-0.0338644633275951,
0.0746335827714525));
#85698=CARTESIAN_POINT('Ctrl Pts',(0.0138300506476652,-0.0341934961088741,
0.0748687665299179));
#85699=CARTESIAN_POINT('Ctrl Pts',(0.0138449105794185,-0.0340287516182428,
0.0747507939250858));
#85700=CARTESIAN_POINT('Ctrl Pts',(0.0138548819163858,-0.0338644633275951,
0.0746323079533354));
#85701=CARTESIAN_POINT('Ctrl Pts',(0.014101431860211,-0.0341934961088741,
0.0746674016403827));
#85702=CARTESIAN_POINT('Ctrl Pts',(0.0141121287315108,-0.0340287516182428,
0.0745438184427786));
#85703=CARTESIAN_POINT('Ctrl Pts',(0.0141177086752243,-0.0338644633275951,
0.0744198987348472));
#85704=CARTESIAN_POINT('',(0.0141025234017923,-0.0341764758832439,0.074654632094052));
#85705=CARTESIAN_POINT('',(0.0141014318602036,-0.034193496108874,0.0746674016403882));
#85706=CARTESIAN_POINT('Origin',(-0.00235348998283771,-0.0345621027072709,
0.0727517521663097));
#85707=CARTESIAN_POINT('Ctrl Pts',(0.0141025234007908,-0.0341764758837548,
0.0746546320955703));
#85708=CARTESIAN_POINT('Ctrl Pts',(0.0140597511086489,-0.0341260050040147,
0.0746510219394901));
#85709=CARTESIAN_POINT('Ctrl Pts',(0.0140177222966369,-0.0340749269147527,
0.0746474745745116));
#85710=CARTESIAN_POINT('Ctrl Pts',(0.0139351190755364,-0.0339715436304845,
0.0746405024947405));
#85711=CARTESIAN_POINT('Ctrl Pts',(0.0138945760049236,-0.0339192778237439,
0.0746370804190492));
#85712=CARTESIAN_POINT('Ctrl Pts',(0.0138547629087952,-0.0338664212855138,
0.074633720016296));
#85713=CARTESIAN_POINT('',(0.0139657412539445,-0.0341934961088841,0.0747680840851631));
#85714=CARTESIAN_POINT('Origin',(0.00812378219310841,-0.0315241814719618,
0.07415));
#85715=CARTESIAN_POINT('',(0.0141025234011276,-0.0342105180190351,0.074654632093152));
#85716=CARTESIAN_POINT('',(0.0141035876665865,-0.0341934961088739,0.0746418602437368));
#85717=CARTESIAN_POINT('Origin',(-0.00236248866054473,-0.0345621718794165,
0.0727961752181882));
#85718=CARTESIAN_POINT('Origin',(-0.00243963130953617,-0.0345621030710607,
0.0737723217671398));
#85719=CARTESIAN_POINT('Origin',(-0.00244105481376565,-0.0345621723112166,
0.0737270191282932));
#85720=CARTESIAN_POINT('Ctrl Pts',(0.0138427698581003,-0.0346945769586966,
0.0747596575597633));
#85721=CARTESIAN_POINT('Ctrl Pts',(0.0138555393797831,-0.0345275153362944,
0.0746398710733623));
#85722=CARTESIAN_POINT('Ctrl Pts',(0.0138645450295769,-0.0343603235965185,
0.0745196520143369));
#85723=CARTESIAN_POINT('Ctrl Pts',(0.0138697654572347,-0.034193496108874,
0.0743993563331597));
#85724=CARTESIAN_POINT('Ctrl Pts',(0.0138498206901431,-0.0346945769586966,
0.0746761212554798));
#85725=CARTESIAN_POINT('Ctrl Pts',(0.0138608405104866,-0.0345275153362944,
0.0745561870865787));
#85726=CARTESIAN_POINT('Ctrl Pts',(0.0138680913618999,-0.0343603235965185,
0.0744358753333516));
#85727=CARTESIAN_POINT('Ctrl Pts',(0.0138715570881254,-0.034193496108874,
0.0743155421432836));
#85728=CARTESIAN_POINT('Ctrl Pts',(0.0138568715221862,-0.0346945769586966,
0.074592584951197));
#85729=CARTESIAN_POINT('Ctrl Pts',(0.0138661416411903,-0.0345275153362944,
0.0744725030997953));
#85730=CARTESIAN_POINT('Ctrl Pts',(0.0138716376942231,-0.0343603235965185,
0.0743520986523658));
#85731=CARTESIAN_POINT('Ctrl Pts',(0.0138733487190162,-0.034193496108874,
0.0742317279534062));
#85732=CARTESIAN_POINT('Ctrl Pts',(0.0138639223542286,-0.0346945769586966,
0.0745090486469129));
#85733=CARTESIAN_POINT('Ctrl Pts',(0.0138714427718934,-0.0345275153362944,
0.0743888191130115));
#85734=CARTESIAN_POINT('Ctrl Pts',(0.0138751840265459,-0.0343603235965185,
0.0742683219713809));
#85735=CARTESIAN_POINT('Ctrl Pts',(0.0138751403499068,-0.034193496108874,
0.0741479137635315));
#85736=CARTESIAN_POINT('',(0.0138639223541774,-0.0346945769586966,0.0745090486475165));
#85737=CARTESIAN_POINT('',(0.0138738271571082,-0.0343667727831525,0.0742729142485203));
#85738=CARTESIAN_POINT('Origin',(-0.00292731345553948,-0.0345626457063063,
0.0736420727438767));
#85739=CARTESIAN_POINT('Origin',(0.0249234817099851,-0.0341934771028971,
0.0745091106384679));
#85740=CARTESIAN_POINT('',(0.013869797514459,-0.034193496108874,0.0743978566658474));
#85741=CARTESIAN_POINT('',(0.0138711332233277,-0.0341934961088839,0.0743353709404327));
#85742=CARTESIAN_POINT('',(0.0138547629072613,-0.034521194296262,0.0746337200161366));
#85743=CARTESIAN_POINT('Origin',(-0.00288356203575707,-0.0345625596117302,
0.0731632443790331));
#85744=CARTESIAN_POINT('',(0.0138534091855672,-0.0346945769586885,0.0746336057560541));
#85745=CARTESIAN_POINT('Origin',(0.0248777764432598,-0.0346945685853899,
0.0755641119509239));
#85746=CARTESIAN_POINT('',(0.0138586657698823,-0.0346945769587026,0.0745713272017954));
#85747=CARTESIAN_POINT('Ctrl Pts',(0.0140781489056537,-0.0345231616327841,
0.0748885912622242));
#85748=CARTESIAN_POINT('Ctrl Pts',(0.0140883293463501,-0.0344132092796988,
0.0748065187001696));
#85749=CARTESIAN_POINT('Ctrl Pts',(0.0140968116555745,-0.0343032738558979,
0.0747242397982963));
#85750=CARTESIAN_POINT('Ctrl Pts',(0.0141035876665937,-0.0341934961088739,
0.0746418602437442));
#85751=CARTESIAN_POINT('Ctrl Pts',(0.0140032000110606,-0.0345231616327841,
0.0748035983252329));
#85752=CARTESIAN_POINT('Ctrl Pts',(0.0140122089437811,-0.0344132092796988,
0.0747225588281706));
#85753=CARTESIAN_POINT('Ctrl Pts',(0.0140195411736084,-0.0343032738558979,
0.0746413371697067));
#85754=CARTESIAN_POINT('Ctrl Pts',(0.0140251899724995,-0.0341934961088739,
0.0745600376447887));
#85755=CARTESIAN_POINT('Ctrl Pts',(0.0139282511164675,-0.0345231616327841,
0.0747186053882416));
#85756=CARTESIAN_POINT('Ctrl Pts',(0.0139360885412121,-0.0344132092796988,
0.0746385989561717));
#85757=CARTESIAN_POINT('Ctrl Pts',(0.0139422706916424,-0.0343032738558979,
0.0745584345411171));
#85758=CARTESIAN_POINT('Ctrl Pts',(0.0139467922784052,-0.0341934961088739,
0.0744782150458331));
#85759=CARTESIAN_POINT('Ctrl Pts',(0.0138533022218744,-0.0345231616327841,
0.0746336124512502));
#85760=CARTESIAN_POINT('Ctrl Pts',(0.013859968138643,-0.0344132092796988,
0.0745546390841727));
#85761=CARTESIAN_POINT('Ctrl Pts',(0.0138650002096763,-0.034303273855898,
0.0744755319125275));
#85762=CARTESIAN_POINT('Ctrl Pts',(0.0138683945843109,-0.0341934961088739,
0.0743963924468776));
#85763=CARTESIAN_POINT('',(0.0139866925905328,-0.0341934961088839,0.074519858454802));
#85764=CARTESIAN_POINT('Ctrl Pts',(0.0141025233976798,-0.0342105180195353,
0.074654632092856));
#85765=CARTESIAN_POINT('Ctrl Pts',(0.0140597030224438,-0.0342610556240235,
0.0746510178645706));
#85766=CARTESIAN_POINT('Ctrl Pts',(0.014017651036698,-0.0343122189867991,
0.0746474684917428));
#85767=CARTESIAN_POINT('Ctrl Pts',(0.0139350469819218,-0.0344158119695089,
0.074640496345665));
#85768=CARTESIAN_POINT('Ctrl Pts',(0.0138945286988031,-0.0344681990449974,
0.0746370764240947));
#85769=CARTESIAN_POINT('Ctrl Pts',(0.0138547629072297,-0.0345211942962376,
0.0746337200161253));
#85770=CARTESIAN_POINT('Ctrl Pts',(0.0138623730811969,-0.0346945769586931,
0.0745103567457866));
#85771=CARTESIAN_POINT('Ctrl Pts',(0.0138698232019357,-0.034529677707698,
0.0743917154396721));
#85772=CARTESIAN_POINT('Ctrl Pts',(0.0138723634024359,-0.034364806625142,
0.0742728675907348));
#85773=CARTESIAN_POINT('Ctrl Pts',(0.0138639223541768,-0.0346945769586931,
0.0745090486475256));
#85774=CARTESIAN_POINT('Ctrl Pts',(0.0138713454309097,-0.034529677707698,
0.0743903753112884));
#85775=CARTESIAN_POINT('Ctrl Pts',(0.0138738572866782,-0.034364806625142,
0.0742714965773515));
#85776=CARTESIAN_POINT('Ctrl Pts',(0.0141221242518614,-0.0346945769586931,
0.0742910409382769));
#85777=CARTESIAN_POINT('Ctrl Pts',(0.0141250401734628,-0.034529677707698,
0.074167029460503));
#85778=CARTESIAN_POINT('Ctrl Pts',(0.0141228280951127,-0.034364806625142,
0.0740430034312678));
#85779=CARTESIAN_POINT('',(0.0141224118333211,-0.0346775396665023,0.0742782280511647));
#85780=CARTESIAN_POINT('',(0.0141221242518551,-0.0346945769586886,0.0742910409382789));
#85781=CARTESIAN_POINT('Origin',(-0.00247795130349033,-0.0345626617742155,
0.074076126929863));
#85782=CARTESIAN_POINT('Ctrl Pts',(0.0141224118323239,-0.0346775396670097,
0.0742782280526905));
#85783=CARTESIAN_POINT('Ctrl Pts',(0.0140794634589947,-0.0346269749928184,
0.0742773099915325));
#85784=CARTESIAN_POINT('Ctrl Pts',(0.0140372783733264,-0.0345757902890787,
0.0742764082822817));
#85785=CARTESIAN_POINT('Ctrl Pts',(0.0139544000390993,-0.0344721681088035,
0.0742746366526692));
#85786=CARTESIAN_POINT('Ctrl Pts',(0.0139137392828609,-0.0344197714289755,
0.0742737674212339));
#85787=CARTESIAN_POINT('Ctrl Pts',(0.0138738271572069,-0.0343667727830744,
0.0742729142487566));
#85788=CARTESIAN_POINT('',(0.0139930233030263,-0.0346945769587026,0.0744000447929077));
#85789=CARTESIAN_POINT('Origin',(0.00812378219310841,-0.0315241814719618,
0.07415));
#85790=CARTESIAN_POINT('',(0.0141224118321568,-0.034711613648978,0.0742782280504013));
#85791=CARTESIAN_POINT('',(0.0141226720466814,-0.0346945769586885,0.0742654145775367));
#85792=CARTESIAN_POINT('Origin',(-0.00247704821473885,-0.034562669910531,
0.0741214292513686));
#85793=CARTESIAN_POINT('Origin',(-0.00247142466767664,-0.0345626621993952,
0.0737707630919827));
#85794=CARTESIAN_POINT('Origin',(-0.00246858475451511,-0.0345626701270886,
0.0737255405042681));
#85795=CARTESIAN_POINT('Ctrl Pts',(0.0138680588324882,-0.0352450361874068,
0.0744364411211761));
#85796=CARTESIAN_POINT('Ctrl Pts',(0.0138788621366473,-0.0349452760959493,
0.0742197921726778));
#85797=CARTESIAN_POINT('Ctrl Pts',(0.0138733158645005,-0.034644428984174,
0.0740029449519637));
#85798=CARTESIAN_POINT('Ctrl Pts',(0.0138681286387982,-0.0352450361874068,
0.0744339170862953));
#85799=CARTESIAN_POINT('Ctrl Pts',(0.0138788367474198,-0.0349452760959493,
0.0742172655050089));
#85800=CARTESIAN_POINT('Ctrl Pts',(0.0138731953518635,-0.034644428984174,
0.0740004228295035));
#85801=CARTESIAN_POINT('Ctrl Pts',(0.0138750401546451,-0.0352450361874068,
0.0741840126426598));
#85802=CARTESIAN_POINT('Ctrl Pts',(0.0138763229625129,-0.0349452760959493,
0.0739671003892759));
#85803=CARTESIAN_POINT('Ctrl Pts',(0.0138612634076013,-0.034644428984174,
0.0737507077344328));
#85804=CARTESIAN_POINT('Ctrl Pts',(0.0138751092698036,-0.0352450361874068,
0.0741815135982235));
#85805=CARTESIAN_POINT('Ctrl Pts',(0.0138762978246639,-0.0349452760959493,
0.0739645987381186));
#85806=CARTESIAN_POINT('Ctrl Pts',(0.0138611440881586,-0.034644428984174,
0.0737482105834822));
#85807=CARTESIAN_POINT('',(0.0138751427351082,-0.0351951634053356,0.0741479461219711));
#85808=CARTESIAN_POINT('',(0.0138701986062541,-0.0348678972934091,0.0739116233943468));
#85809=CARTESIAN_POINT('Origin',(-0.00284703215792656,-0.0345636767885614,
0.0750273568423855));
#85810=CARTESIAN_POINT('Origin',(0.0249105444510711,-0.0346946199326491,
0.0734536263611325));
#85811=CARTESIAN_POINT('',(0.0138740221147906,-0.0346945769330288,0.0740365723080913));
#85812=CARTESIAN_POINT('',(0.013871431676765,-0.0346945769458128,0.0739741260054113));
#85813=CARTESIAN_POINT('',(0.0138738271570594,-0.0350221583435276,0.0742729142487372));
#85814=CARTESIAN_POINT('Origin',(-0.00290833283662269,-0.0345628458712561,
0.0745505071604989));
#85815=CARTESIAN_POINT('',(0.0138725904902828,-0.0351951360298763,0.0742728908386952));
#85816=CARTESIAN_POINT('Origin',(0.0248890503995137,-0.0351951838366758,
0.0745083795262769));
#85817=CARTESIAN_POINT('',(0.0138751403500098,-0.0351951371328746,0.0741479137641504));
#85818=CARTESIAN_POINT('Ctrl Pts',(0.014112775910331,-0.0350241211494342,
0.0745132550827827));
#85819=CARTESIAN_POINT('Ctrl Pts',(0.014117779600156,-0.0349144232818961,
0.074430759149911));
#85820=CARTESIAN_POINT('Ctrl Pts',(0.0141210810350496,-0.0348045283579412,
0.0743481104094029));
#85821=CARTESIAN_POINT('Ctrl Pts',(0.0141226720469026,-0.0346945769439157,
0.0742654145664327));
#85822=CARTESIAN_POINT('Ctrl Pts',(0.0140326381290873,-0.0350241211494342,
0.074433135935128));
#85823=CARTESIAN_POINT('Ctrl Pts',(0.0140365382105035,-0.0349144232818961,
0.0743517438673352));
#85824=CARTESIAN_POINT('Ctrl Pts',(0.0140387581941054,-0.0348045283579412,
0.0742702224649968));
#85825=CARTESIAN_POINT('Ctrl Pts',(0.0140392913507192,-0.0346945769439157,
0.0741886760408568));
#85826=CARTESIAN_POINT('Ctrl Pts',(0.0139525003478436,-0.0350241211494342,
0.0743530167874733));
#85827=CARTESIAN_POINT('Ctrl Pts',(0.013955296820851,-0.0349144232818961,
0.0742727285847594));
#85828=CARTESIAN_POINT('Ctrl Pts',(0.0139564353531612,-0.0348045283579412,
0.0741923345205907));
#85829=CARTESIAN_POINT('Ctrl Pts',(0.0139559106545359,-0.0346945769439157,
0.0741119375152809));
#85830=CARTESIAN_POINT('Ctrl Pts',(0.0138723625665999,-0.0350241211494342,
0.0742728976398186));
#85831=CARTESIAN_POINT('Ctrl Pts',(0.0138740554311984,-0.0349144232818961,
0.0741937133021835));
#85832=CARTESIAN_POINT('Ctrl Pts',(0.013874112512217,-0.0348045283579412,
0.0741144465761847));
#85833=CARTESIAN_POINT('Ctrl Pts',(0.0138725299583526,-0.0346945769439157,
0.0740351989897051));
#85834=CARTESIAN_POINT('',(0.0139983470808299,-0.0346945769458128,0.07415099344311));
#85835=CARTESIAN_POINT('Ctrl Pts',(0.0141224118288639,-0.034711613649276,
0.0742782280503256));
#85836=CARTESIAN_POINT('Ctrl Pts',(0.0140794805116427,-0.0347621546531202,
0.0742773103408754));
#85837=CARTESIAN_POINT('Ctrl Pts',(0.0140373040429872,-0.0348133084094808,
0.0742764087672371));
#85838=CARTESIAN_POINT('Ctrl Pts',(0.0139544256033316,-0.0349168561544568,
0.0742746371391526));
#85839=CARTESIAN_POINT('Ctrl Pts',(0.0139137565062636,-0.0349692089015918,
0.074273767787427));
#85840=CARTESIAN_POINT('Ctrl Pts',(0.0138738271570232,-0.0350221583435,
0.0742729142487165));
#85841=CARTESIAN_POINT('Ctrl Pts',(0.013874083967851,-0.0351951371254987,
0.0741489259284914));
#85842=CARTESIAN_POINT('Ctrl Pts',(0.0138740617620965,-0.035030733898539,
0.0740300420474763));
#85843=CARTESIAN_POINT('Ctrl Pts',(0.0138691259762484,-0.0348659306906667,
0.0739112606698267));
#85844=CARTESIAN_POINT('Ctrl Pts',(0.0138751403498936,-0.0351951371254987,
0.0741479137641592));
#85845=CARTESIAN_POINT('Ctrl Pts',(0.0138750972182767,-0.035030733898539,
0.0740290080431083));
#85846=CARTESIAN_POINT('Ctrl Pts',(0.0138701396217749,-0.0348659306906667,
0.0739102057089735));
#85847=CARTESIAN_POINT('Ctrl Pts',(0.0140521910814103,-0.0351951371254987,
0.0739782739670158));
#85848=CARTESIAN_POINT('Ctrl Pts',(0.0140486407534324,-0.035030733898539,
0.073855707833186));
#85849=CARTESIAN_POINT('Ctrl Pts',(0.0140400276686389,-0.0348659306906667,
0.0737333931702829));
#85850=CARTESIAN_POINT('Origin',(0.0191838114618603,-0.0308609188508581,
0.0736911989231954));
#85851=CARTESIAN_POINT('',(0.0139523304768724,-0.0351951371254987,0.0740739546374729));
#85852=CARTESIAN_POINT('Origin',(0.00716368043114226,-0.0351840467441104,
0.0743315220568552));
#85853=CARTESIAN_POINT('Origin',(0.0200194708629429,-0.0352322613860026,
0.0728611531253263));
#85854=CARTESIAN_POINT('',(0.0138555002984642,-0.0351951142564684,0.0736754242482386));
#85855=CARTESIAN_POINT('',(0.01384254041583,-0.0351951372916788,0.0735514146760448));
#85856=CARTESIAN_POINT('Origin',(0.00791606459898444,-0.0352875118039944,
0.0738801088396702));
#85857=CARTESIAN_POINT('Origin',(0.00746164432488242,-0.0298325076522886,
0.0816237382696252));
#85858=CARTESIAN_POINT('Origin',(0.016174955010655,-0.0338733209737903,
0.0764792659156153));
#85859=CARTESIAN_POINT('Ctrl Pts',(0.0130396264404983,-0.0321934096636942,
0.0771353996517576));
#85860=CARTESIAN_POINT('Ctrl Pts',(0.0130930636725526,-0.0320508460845492,
0.0770474083807612));
#85861=CARTESIAN_POINT('Ctrl Pts',(0.0131440964609289,-0.0319086045665399,
0.0769580477024896));
#85862=CARTESIAN_POINT('Ctrl Pts',(0.0131926307633795,-0.0317669892871375,
0.076867519072417));
#85863=CARTESIAN_POINT('Ctrl Pts',(0.0130815814270117,-0.0321934096636942,
0.0770628034277897));
#85864=CARTESIAN_POINT('Ctrl Pts',(0.0131337192212289,-0.0320508460845492,
0.0769740611825147));
#85865=CARTESIAN_POINT('Ctrl Pts',(0.0131834333743513,-0.0319086045665399,
0.0768839850095321));
#85866=CARTESIAN_POINT('Ctrl Pts',(0.0132306328102157,-0.0317669892871375,
0.0767927776711573));
#85867=CARTESIAN_POINT('Ctrl Pts',(0.0131235364135251,-0.0321934096636942,
0.0769902072038219));
#85868=CARTESIAN_POINT('Ctrl Pts',(0.0131743747699051,-0.0320508460845492,
0.0769007139842681));
#85869=CARTESIAN_POINT('Ctrl Pts',(0.0132227702877738,-0.0319086045665399,
0.0768099223165747));
#85870=CARTESIAN_POINT('Ctrl Pts',(0.013268634857052,-0.0317669892871375,
0.0767180362698976));
#85871=CARTESIAN_POINT('Ctrl Pts',(0.0131654914000384,-0.0321934096636942,
0.0769176109798541));
#85872=CARTESIAN_POINT('Ctrl Pts',(0.0132150303185813,-0.0320508460845492,
0.0768273667860216));
#85873=CARTESIAN_POINT('Ctrl Pts',(0.0132621072011962,-0.0319086045665399,
0.0767358596236172));
#85874=CARTESIAN_POINT('Ctrl Pts',(0.0133066369038883,-0.0317669892871375,
0.0766432948686379));
#85875=CARTESIAN_POINT('',(0.0131647408170369,-0.0321934096636942,0.0769189097406456));
#85876=CARTESIAN_POINT('',(0.013274244086809,-0.0318665617511358,0.0767094662081792));
#85877=CARTESIAN_POINT('Origin',(-0.00117512587987898,-0.0326371944420287,
0.0683406740270635));
#85878=CARTESIAN_POINT('Origin',(0.0230902151182577,-0.0316939261509049,
0.0815874066423466));
#85879=CARTESIAN_POINT('',(0.0131034624642231,-0.0320197221621771,0.0770275638244887));
#85880=CARTESIAN_POINT('Ctrl Pts',(0.0131035928027192,-0.0320197392094689,
0.0770274325737502));
#85881=CARTESIAN_POINT('Ctrl Pts',(0.0131182340640825,-0.0319792716575987,
0.0770020936729162));
#85882=CARTESIAN_POINT('Ctrl Pts',(0.013132748804458,-0.0319386439829682,
0.076976527800679));
#85883=CARTESIAN_POINT('Ctrl Pts',(0.0131471449067337,-0.0318979099381615,
0.0769507039420763));
#85884=CARTESIAN_POINT('Ctrl Pts',(0.0131615407244598,-0.0318571766984932,
0.0769248805939013));
#85885=CARTESIAN_POINT('Ctrl Pts',(0.0131757462960352,-0.0318163871833596,
0.076898931388219));
#85886=CARTESIAN_POINT('Ctrl Pts',(0.0131897158487752,-0.0317755399638304,
0.0768729472704333));
#85887=CARTESIAN_POINT('',(0.0131021943802151,-0.0321934096636182,0.0770271360925871));
#85888=CARTESIAN_POINT('Origin',(0.0151107385009172,-0.0324111866099997,
0.0781636326709294));
#85889=CARTESIAN_POINT('',(0.013133467598636,-0.0321934096636662,0.0769730229166264));
#85890=CARTESIAN_POINT('Ctrl Pts',(0.0131627814793221,-0.0321934096636618,
0.0769194338428291));
#85891=CARTESIAN_POINT('Ctrl Pts',(0.0132009741303853,-0.0320835708272592,
0.0768499421155059));
#85892=CARTESIAN_POINT('Ctrl Pts',(0.0132377065004733,-0.0319739230346489,
0.0767797003012799));
#85893=CARTESIAN_POINT('Ctrl Pts',(0.0132729384903025,-0.0318646057455573,
0.0767088018765306));
#85894=CARTESIAN_POINT('Ctrl Pts',(0.013272251668556,-0.0321934096636618,
0.0768901517248274));
#85895=CARTESIAN_POINT('Ctrl Pts',(0.0133100404963907,-0.0320835708272592,
0.0768191503182785));
#85896=CARTESIAN_POINT('Ctrl Pts',(0.0133463380347512,-0.0319739230346489,
0.0767474080576029));
#85897=CARTESIAN_POINT('Ctrl Pts',(0.0133811048880234,-0.0318646057455573,
0.0766750202961999));
#85898=CARTESIAN_POINT('Ctrl Pts',(0.0133817218577899,-0.0321934096636618,
0.0768608696068256));
#85899=CARTESIAN_POINT('Ctrl Pts',(0.0134191068623962,-0.0320835708272592,
0.0767883585210511));
#85900=CARTESIAN_POINT('Ctrl Pts',(0.0134549695690291,-0.0319739230346489,
0.0767151158139259));
#85901=CARTESIAN_POINT('Ctrl Pts',(0.0134892712857444,-0.0318646057455573,
0.0766412387158692));
#85902=CARTESIAN_POINT('Ctrl Pts',(0.0134911920470238,-0.0321934096636618,
0.0768315874888238));
#85903=CARTESIAN_POINT('Ctrl Pts',(0.0135281732284017,-0.0320835708272592,
0.0767575667238238));
#85904=CARTESIAN_POINT('Ctrl Pts',(0.0135636011033069,-0.0319739230346489,
0.0766828235702489));
#85905=CARTESIAN_POINT('Ctrl Pts',(0.0135974376834654,-0.0318646057455573,
0.0766074571355385));
#85906=CARTESIAN_POINT('',(0.0134969077196753,-0.032176398030832,0.0768201164869055));
#85907=CARTESIAN_POINT('',(0.013491192047025,-0.0321934096636185,0.0768315874887981));
#85908=CARTESIAN_POINT('Origin',(-0.00103868750143187,-0.0326386231233297,
0.0689117309547281));
#85909=CARTESIAN_POINT('Ctrl Pts',(0.0134969077168294,-0.0321763980306362,
0.0768201164854885));
#85910=CARTESIAN_POINT('Ctrl Pts',(0.0134584729499547,-0.0321259596175984,
0.0768010167447148));
#85911=CARTESIAN_POINT('Ctrl Pts',(0.0134207041152833,-0.0320749164633703,
0.0767822479317384));
#85912=CARTESIAN_POINT('Ctrl Pts',(0.013346467914919,-0.0319716057794025,
0.0767453570566718));
#85913=CARTESIAN_POINT('Ctrl Pts',(0.0133100294743802,-0.0319193786690223,
0.0767272493686233));
#85914=CARTESIAN_POINT('Ctrl Pts',(0.0132742440851441,-0.0318665617525436,
0.0767094662073484));
#85915=CARTESIAN_POINT('',(0.0133279664320409,-0.0321934096636663,0.0768752486147319));
#85916=CARTESIAN_POINT('Origin',(0.00812378219310841,-0.0315241814719618,
0.07415));
#85917=CARTESIAN_POINT('',(0.0134969077200062,-0.0322104233323591,0.07682011648707));
#85918=CARTESIAN_POINT('',(0.0135025988803254,-0.0321934096636183,0.0768086333040356));
#85919=CARTESIAN_POINT('Origin',(-0.00106431922441187,-0.0326387244918799,
0.0689491214002542));
#85920=CARTESIAN_POINT('Origin',(-0.00158472984669416,-0.0326386235719424,
0.0700105398946128));
#85921=CARTESIAN_POINT('Origin',(-0.00157040526565379,-0.0326387248819868,
0.0699675304009003));
#85922=CARTESIAN_POINT('Ctrl Pts',(0.0132005149732031,-0.0327445246967096,
0.0768527595674627));
#85923=CARTESIAN_POINT('Ctrl Pts',(0.0133024512167218,-0.032443687833936,
0.0766612874605166));
#85924=CARTESIAN_POINT('Ctrl Pts',(0.0133896754084872,-0.0321434074405928,
0.0764626810511237));
#85925=CARTESIAN_POINT('Ctrl Pts',(0.013313174592781,-0.0327445246967096,
0.07662958293312));
#85926=CARTESIAN_POINT('Ctrl Pts',(0.0134066935919321,-0.032443687833936,
0.0764338617991594));
#85927=CARTESIAN_POINT('Ctrl Pts',(0.0134852043977516,-0.0321434074405928,
0.0762316524550363));
#85928=CARTESIAN_POINT('',(0.0133286549178122,-0.0326943950436612,0.0765969215188958));
#85929=CARTESIAN_POINT('',(0.013424791040563,-0.0323666188837389,0.0763810155085093));
#85930=CARTESIAN_POINT('Origin',(-0.00191712637556098,-0.0326395579112203,
0.0695135458424481));
#85931=CARTESIAN_POINT('Origin',(0.0236045717473434,-0.0321933825603084,
0.080665340028318));
#85932=CARTESIAN_POINT('',(0.0133750499992974,-0.0321934096532689,0.0764957006255223));
#85933=CARTESIAN_POINT('',(0.013399294441097,-0.0321934096584275,0.0764380945721288));
#85934=CARTESIAN_POINT('',(0.0132742440876436,-0.0325210109756239,0.0767094662085955));
#85935=CARTESIAN_POINT('Origin',(-0.00168988315583584,-0.0326393129156433,
0.0690898183963548));
#85936=CARTESIAN_POINT('',(0.0132730274909841,-0.0326943950436593,0.0767088616340681));
#85937=CARTESIAN_POINT('Origin',(0.0231796872344863,-0.0326943765538153,
0.0816318698022489));
#85938=CARTESIAN_POINT('',(0.0133008412044081,-0.0326943950436702,0.076652891576492));
#85939=CARTESIAN_POINT('Ctrl Pts',(0.0133881187017994,-0.0325229783203769,
0.0770286735006535));
#85940=CARTESIAN_POINT('Ctrl Pts',(0.0134278011530535,-0.032413025309245,
0.0769561047370046));
#85941=CARTESIAN_POINT('Ctrl Pts',(0.0134659764075891,-0.0323031222208069,
0.0768827260973508));
#85942=CARTESIAN_POINT('Ctrl Pts',(0.0135025988823162,-0.0321934096576658,
0.0768086333000249));
#85943=CARTESIAN_POINT('Ctrl Pts',(0.0133497209623862,-0.0325229783203769,
0.0769220585118155));
#85944=CARTESIAN_POINT('Ctrl Pts',(0.0133879337283506,-0.032413025309245,
0.0768500190601648));
#85945=CARTESIAN_POINT('Ctrl Pts',(0.0134246504700018,-0.0323031222208069,
0.0767772000545567));
#85946=CARTESIAN_POINT('Ctrl Pts',(0.0134598274472057,-0.0321934096576658,
0.0767036964305483));
#85947=CARTESIAN_POINT('Ctrl Pts',(0.0133113232229729,-0.0325229783203769,
0.0768154435229776));
#85948=CARTESIAN_POINT('Ctrl Pts',(0.0133480663036478,-0.032413025309245,
0.076743933383325));
#85949=CARTESIAN_POINT('Ctrl Pts',(0.0133833245324145,-0.0323031222208069,
0.0766716740117626));
#85950=CARTESIAN_POINT('Ctrl Pts',(0.0134170560120952,-0.0321934096576658,
0.0765987595610717));
#85951=CARTESIAN_POINT('Ctrl Pts',(0.0132729254835597,-0.0325229783203769,
0.0767088285341397));
#85952=CARTESIAN_POINT('Ctrl Pts',(0.0133081988789449,-0.032413025309245,
0.0766378477064852));
#85953=CARTESIAN_POINT('Ctrl Pts',(0.0133419985948273,-0.0323031222208069,
0.0765661479689685));
#85954=CARTESIAN_POINT('Ctrl Pts',(0.0133742845769847,-0.0321934096576658,
0.0764938226915951));
#85955=CARTESIAN_POINT('',(0.0134388244397454,-0.0321934096584275,0.0766521669652904));
#85956=CARTESIAN_POINT('Ctrl Pts',(0.0134969077168855,-0.032210423332889,
0.0768201164855165));
#85957=CARTESIAN_POINT('Ctrl Pts',(0.0134584208702708,-0.0322609421830388,
0.0768009908642805));
#85958=CARTESIAN_POINT('Ctrl Pts',(0.0134206265937799,-0.0323120888238748,
0.0767822094082601));
#85959=CARTESIAN_POINT('Ctrl Pts',(0.0133463898313685,-0.0324156524631808,
0.0767453182538903));
#85960=CARTESIAN_POINT('Ctrl Pts',(0.0133099778608568,-0.032468026716732,
0.0767272237198424));
#85961=CARTESIAN_POINT('Ctrl Pts',(0.0132742440876067,-0.0325210109755912,
0.0767094662085722));
#85962=CARTESIAN_POINT('Origin',(0.00379934591254904,-0.0262834582510528,
0.080722871267367));
#85963=CARTESIAN_POINT('Origin',(0.015440934589309,-0.0342771100866737,
0.083860041158149));
#85964=CARTESIAN_POINT('Ctrl Pts',(0.013326732821639,-0.0326943950436603,
0.0765975674578511));
#85965=CARTESIAN_POINT('Ctrl Pts',(0.0133604648884385,-0.0325844576448133,
0.0765258610468212));
#85966=CARTESIAN_POINT('Ctrl Pts',(0.0133927163363644,-0.0324744968375322,
0.0764534519265712));
#85967=CARTESIAN_POINT('Ctrl Pts',(0.0134234471226241,-0.0323646534831894,
0.0763804334418495));
#85968=CARTESIAN_POINT('Ctrl Pts',(0.0134341482015404,-0.0326943950436603,
0.076561469483628));
#85969=CARTESIAN_POINT('Ctrl Pts',(0.0134673827706003,-0.0325844576448133,
0.0764882826873452));
#85970=CARTESIAN_POINT('Ctrl Pts',(0.0134991060687837,-0.0324744968375322,
0.0764144033661421));
#85971=CARTESIAN_POINT('Ctrl Pts',(0.0135292787559763,-0.0323646534831894,
0.0763399267391404));
#85972=CARTESIAN_POINT('Ctrl Pts',(0.0135415635814418,-0.0326943950436603,
0.0765253715094049));
#85973=CARTESIAN_POINT('Ctrl Pts',(0.013574300652762,-0.0325844576448133,
0.0764507043278692));
#85974=CARTESIAN_POINT('Ctrl Pts',(0.013605495801203,-0.0324744968375322,
0.0763753548057129));
#85975=CARTESIAN_POINT('Ctrl Pts',(0.0136351103893286,-0.0323646534831894,
0.0762994200364314));
#85976=CARTESIAN_POINT('Ctrl Pts',(0.0136489789613431,-0.0326943950436603,
0.0764892735351818));
#85977=CARTESIAN_POINT('Ctrl Pts',(0.0136812185349238,-0.0325844576448133,
0.0764131259683932));
#85978=CARTESIAN_POINT('Ctrl Pts',(0.0137118855336223,-0.0324744968375322,
0.0763363062452838));
#85979=CARTESIAN_POINT('Ctrl Pts',(0.0137409420226808,-0.0323646534831894,
0.0762589133337223));
#85980=CARTESIAN_POINT('',(0.0136539630854264,-0.0326773559991209,0.0764774662787185));
#85981=CARTESIAN_POINT('',(0.0136489789613314,-0.0326943950436594,0.0764892735351852));
#85982=CARTESIAN_POINT('Origin',(-0.00167043362836957,-0.0326395670146922,
0.0700824545246432));
#85983=CARTESIAN_POINT('Ctrl Pts',(0.0136539630823324,-0.0326773559987497,
0.0764774662774134));
#85984=CARTESIAN_POINT('Ctrl Pts',(0.0136143730414135,-0.0326267922588807,
0.0764608041668955));
#85985=CARTESIAN_POINT('Ctrl Pts',(0.013575484705366,-0.0325756109585183,
0.0764444373802571));
#85986=CARTESIAN_POINT('Ctrl Pts',(0.0134990783461931,-0.0324719985460573,
0.0764122805253699));
#85987=CARTESIAN_POINT('Ctrl Pts',(0.0134615909682089,-0.0324196091617922,
0.0763965033546255));
#85988=CARTESIAN_POINT('Ctrl Pts',(0.0134247910405181,-0.0323666188837756,
0.0763810155084904));
#85989=CARTESIAN_POINT('',(0.0134888169395818,-0.0326943950436703,0.0765430975270505));
#85990=CARTESIAN_POINT('Origin',(0.00812378219310841,-0.0315241814719618,
0.07415));
#85991=CARTESIAN_POINT('',(0.0136539630853841,-0.0327114338379849,0.076477466278701));
#85992=CARTESIAN_POINT('',(0.0136589219806651,-0.0326943950436593,0.0764656484042732));
#85993=CARTESIAN_POINT('Origin',(-0.00168729056429505,-0.0326395680341498,
0.0701245113554134));
#85994=CARTESIAN_POINT('Origin',(-0.00163145640073906,-0.0326395673206855,
0.0699898411083458));
#85995=CARTESIAN_POINT('Origin',(-0.00161316525169613,-0.0326395684286114,
0.0699483880173138));
#85996=CARTESIAN_POINT('Ctrl Pts',(0.0133602211002138,-0.0332451089994433,
0.0765286198881184));
#85997=CARTESIAN_POINT('Ctrl Pts',(0.0134499322170449,-0.0329451141710254,
0.076331124363541));
#85998=CARTESIAN_POINT('Ctrl Pts',(0.0135245123037821,-0.0326442513127494,
0.0761274324948434));
#85999=CARTESIAN_POINT('Ctrl Pts',(0.0134586434676643,-0.0332451089994433,
0.0762988090146041));
#86000=CARTESIAN_POINT('Ctrl Pts',(0.0135396871255938,-0.0329451141710254,
0.0760976014297058));
#86001=CARTESIAN_POINT('Ctrl Pts',(0.0136053447692069,-0.0326442513127494,
0.0758908609146963));
#86002=CARTESIAN_POINT('Ctrl Pts',(0.0134596276913388,-0.0332451089994433,
0.076296510905869));
#86003=CARTESIAN_POINT('Ctrl Pts',(0.0135405846746793,-0.0329451141710254,
0.0760952662003675));
#86004=CARTESIAN_POINT('Ctrl Pts',(0.0136061530938611,-0.0326442513127494,
0.0758884951988948));
#86005=CARTESIAN_POINT('',(0.0134720277638493,-0.0331951640388616,0.0762652764157555));
#86006=CARTESIAN_POINT('',(0.013554417343685,-0.0328677532355043,0.0760437599983026));
#86007=CARTESIAN_POINT('Origin',(-0.00238308537357132,-0.0326402808283806,
0.0708203122407319));
#86008=CARTESIAN_POINT('Origin',(0.0239939736023976,-0.0326944278779173,
0.0796838215450741));
#86009=CARTESIAN_POINT('',(0.0135119755852948,-0.0326943950436593,0.0761613420813975));
#86010=CARTESIAN_POINT('',(0.0135325550709807,-0.0326943950436694,0.0761023273818038));
#86011=CARTESIAN_POINT('',(0.0134247910405619,-0.0330220786163545,0.0763810155085119));
#86012=CARTESIAN_POINT('Origin',(-0.00225478128003319,-0.0326396682762709,
0.0703569649581177));
#86013=CARTESIAN_POINT('',(0.0134235388830287,-0.0331951640388587,0.0763804885177121));
#86014=CARTESIAN_POINT('Origin',(0.023591378025755,-0.0331952026560144,
0.080659789479558));
#86015=CARTESIAN_POINT('',(0.013447783323449,-0.0331951640388701,0.0763228824667439));
#86016=CARTESIAN_POINT('Ctrl Pts',(0.0135584845480517,-0.0330240426238172,
0.0766924418013544));
#86017=CARTESIAN_POINT('Ctrl Pts',(0.0135935091608463,-0.032914277406352,
0.0766175734816411));
#86018=CARTESIAN_POINT('Ctrl Pts',(0.013627003497385,-0.0328043479726691,
0.0765419437807571));
#86019=CARTESIAN_POINT('Ctrl Pts',(0.0136589219806696,-0.0326943950436593,
0.0764656484042827));
#86020=CARTESIAN_POINT('Ctrl Pts',(0.0135134681615712,-0.0330240426238172,
0.0765884482393739));
#86021=CARTESIAN_POINT('Ctrl Pts',(0.0135470601617336,-0.032914277406352,
0.0765142000642417));
#86022=CARTESIAN_POINT('Ctrl Pts',(0.0135791339915511,-0.0328043479726691,
0.0764392204332085));
#86023=CARTESIAN_POINT('Ctrl Pts',(0.0136096459167354,-0.0326943950436593,
0.0763636042691828));
#86024=CARTESIAN_POINT('Ctrl Pts',(0.0134684517750907,-0.0330240426238172,
0.0764844546773935));
#86025=CARTESIAN_POINT('Ctrl Pts',(0.0135006111626208,-0.032914277406352,
0.0764108266468424));
#86026=CARTESIAN_POINT('Ctrl Pts',(0.0135312644857172,-0.0328043479726691,
0.0763364970856598));
#86027=CARTESIAN_POINT('Ctrl Pts',(0.0135603698528012,-0.0326943950436593,
0.0762615601340828));
#86028=CARTESIAN_POINT('Ctrl Pts',(0.0134234353886103,-0.0330240426238172,
0.076380461115413));
#86029=CARTESIAN_POINT('Ctrl Pts',(0.0134541621635081,-0.032914277406352,
0.0763074532294431));
#86030=CARTESIAN_POINT('Ctrl Pts',(0.0134833949798833,-0.0328043479726691,
0.0762337737381112));
#86031=CARTESIAN_POINT('Ctrl Pts',(0.013511093788867,-0.0326943950436593,
0.0761595159989829));
#86032=CARTESIAN_POINT('',(0.0135854487829899,-0.0326943950436693,0.0763134952428454));
#86033=CARTESIAN_POINT('Ctrl Pts',(0.0136539630823231,-0.0327114338383285,
0.0764774662774096));
#86034=CARTESIAN_POINT('Ctrl Pts',(0.0136143796263787,-0.0327619876830041,
0.0764608069382849));
#86035=CARTESIAN_POINT('Ctrl Pts',(0.0135754945066797,-0.0328131562602455,
0.07644444150529));
#86036=CARTESIAN_POINT('Ctrl Pts',(0.0134990882181012,-0.0329167375858761,
0.0764122846801135));
#86037=CARTESIAN_POINT('Ctrl Pts',(0.0134615974936266,-0.0329691088920614,
0.0763965061009534));
#86038=CARTESIAN_POINT('Ctrl Pts',(0.0134247910405192,-0.0330220786163187,
0.0763810155084909));
#86039=CARTESIAN_POINT('Ctrl Pts',(0.0134701497195573,-0.0331951640388604,
0.0762660418917036));
#86040=CARTESIAN_POINT('Ctrl Pts',(0.0135138975289884,-0.0330306422010619,
0.0761555091708662));
#86041=CARTESIAN_POINT('Ctrl Pts',(0.0135530395226318,-0.0328657861914645,
0.0760432627564943));
#86042=CARTESIAN_POINT('Ctrl Pts',(0.0134720277638481,-0.0331951640388604,
0.0762652764157584));
#86043=CARTESIAN_POINT('Ctrl Pts',(0.0135157597475548,-0.0330306422010619,
0.0761547048675594));
#86044=CARTESIAN_POINT('Ctrl Pts',(0.013554884324221,-0.0328657861914645,
0.0760424203130974));
#86045=CARTESIAN_POINT('Ctrl Pts',(0.0137849604482271,-0.0331951640388604,
0.0761377275376377));
#86046=CARTESIAN_POINT('Ctrl Pts',(0.0138260554406554,-0.0330306422010619,
0.0760206863068229));
#86047=CARTESIAN_POINT('Ctrl Pts',(0.0138622778805476,-0.0328657861914645,
0.0759020465876663));
#86048=CARTESIAN_POINT('',(0.0137891933545318,-0.0331781648281955,0.0761256306253974));
#86049=CARTESIAN_POINT('',(0.0137849604482159,-0.0331951640388588,0.0761377275376413));
#86050=CARTESIAN_POINT('Origin',(-0.00203177214281177,-0.0326412091605797,
0.0713629073520702));
#86051=CARTESIAN_POINT('Ctrl Pts',(0.0137891933530245,-0.033178164828644,
0.0761256306264603));
#86052=CARTESIAN_POINT('Ctrl Pts',(0.0137486072846126,-0.0331276811546759,
0.0761114775482818));
#86053=CARTESIAN_POINT('Ctrl Pts',(0.0137087540637734,-0.0330765663497757,
0.0760975800627967));
#86054=CARTESIAN_POINT('Ctrl Pts',(0.0136304791297395,-0.0329730614463427,
0.0760702841837328));
#86055=CARTESIAN_POINT('Ctrl Pts',(0.0135920890396722,-0.0329207133374321,
0.0760568968120312));
#86056=CARTESIAN_POINT('Ctrl Pts',(0.0135544173473107,-0.0328677532289397,
0.0760437600143701));
#86057=CARTESIAN_POINT('',(0.0136284941060426,-0.0331951640388701,0.0762015019767084));
#86058=CARTESIAN_POINT('Origin',(0.00812378219310841,-0.0315241814719618,
0.07415));
#86059=CARTESIAN_POINT('',(0.0137891933532789,-0.0332121607144397,0.0761256306242759));
#86060=CARTESIAN_POINT('',(0.0137934004130283,-0.0331951640388587,0.0761135246981789));
#86061=CARTESIAN_POINT('Origin',(-0.00203907066499096,-0.0326413666255414,
0.0714076603317704));
#86062=CARTESIAN_POINT('Origin',(-0.00156271436733097,-0.0326412093978695,
0.0700178134636139));
#86063=CARTESIAN_POINT('Origin',(-0.00154060066727734,-0.0326413667802714,
0.0699782266867448));
#86064=CARTESIAN_POINT('Ctrl Pts',(0.0134992355551813,-0.0337436976235975,
0.0761951469756912));
#86065=CARTESIAN_POINT('Ctrl Pts',(0.0135176299170312,-0.0336723290703325,
0.0761467993334805));
#86066=CARTESIAN_POINT('Ctrl Pts',(0.0135351516814119,-0.033601104548885,
0.0760981286561872));
#86067=CARTESIAN_POINT('Ctrl Pts',(0.0135910952042136,-0.0333736987606857,
0.0759427328247077));
#86068=CARTESIAN_POINT('Ctrl Pts',(0.0136380290277007,-0.0331450831799192,
0.075784382711359));
#86069=CARTESIAN_POINT('Ctrl Pts',(0.0135830346175524,-0.0337436976235975,
0.0759596098933756));
#86070=CARTESIAN_POINT('Ctrl Pts',(0.0135993105231873,-0.0336723290703325,
0.0759105085496979));
#86071=CARTESIAN_POINT('Ctrl Pts',(0.0136147006173555,-0.033601104548885,
0.0758611223972187));
#86072=CARTESIAN_POINT('Ctrl Pts',(0.013663838139429,-0.0333736987606857,
0.0757034421951985));
#86073=CARTESIAN_POINT('Ctrl Pts',(0.0137038460875853,-0.0331450831799192,
0.0755432020433358));
#86074=CARTESIAN_POINT('Ctrl Pts',(0.0135838726081761,-0.0337436976235975,
0.0759572545225524));
#86075=CARTESIAN_POINT('Ctrl Pts',(0.0136001273292488,-0.0336723290703325,
0.0759081456418601));
#86076=CARTESIAN_POINT('Ctrl Pts',(0.013615496106715,-0.033601104548885,
0.075858752334629));
#86077=CARTESIAN_POINT('Ctrl Pts',(0.0136645655687811,-0.0333736987606857,
0.0757010492889033));
#86078=CARTESIAN_POINT('Ctrl Pts',(0.0137045042581842,-0.0331450831799192,
0.0755407902366555));
#86079=CARTESIAN_POINT('',(0.0135942935280036,-0.0336938721132548,0.0759252832829675));
#86080=CARTESIAN_POINT('',(0.0136626113922525,-0.0333679869945434,0.07569903069784));
#86081=CARTESIAN_POINT('Ctrl Pts',(0.0135942935280024,-0.033693872113265,
0.0759252832829736));
#86082=CARTESIAN_POINT('Ctrl Pts',(0.0136012232914556,-0.0336629187933933,
0.0759039293109708));
#86083=CARTESIAN_POINT('Ctrl Pts',(0.0136080258025137,-0.0336319952301041,
0.0758825415919257));
#86084=CARTESIAN_POINT('Ctrl Pts',(0.0136147006173536,-0.0336011045488951,
0.0758611223972248));
#86085=CARTESIAN_POINT('Ctrl Pts',(0.0136314500117803,-0.0335235892595455,
0.0758073743084842));
#86086=CARTESIAN_POINT('Ctrl Pts',(0.0136474249484776,-0.033445866866037,
0.0757533324743409));
#86087=CARTESIAN_POINT('Ctrl Pts',(0.0136626113925438,-0.0333679869945386,
0.0756990306979284));
#86088=CARTESIAN_POINT('Ctrl Pts',(0.0136626240317451,-0.0333679692459663,
0.0756989880561563));
#86089=CARTESIAN_POINT('Ctrl Pts',(0.013662185969107,-0.0333391895373257,
0.0756988716991663));
#86090=CARTESIAN_POINT('Ctrl Pts',(0.0136618567861838,-0.0333104081057764,
0.0756987876222839));
#86091=CARTESIAN_POINT('Ctrl Pts',(0.0136614196850596,-0.0332532697346145,
0.0756986816981781));
#86092=CARTESIAN_POINT('Ctrl Pts',(0.0136613085378268,-0.0332249166877988,
0.0756986589465388));
#86093=CARTESIAN_POINT('Ctrl Pts',(0.01366130314572,-0.0331960985544231,
0.075698664599457));
#86094=CARTESIAN_POINT('Ctrl Pts',(0.0136613030868818,-0.033195631237939,
0.0756986646993534));
#86095=CARTESIAN_POINT('Ctrl Pts',(0.0136613030569208,-0.0331951640388594,
0.0756986648064842));
#86096=CARTESIAN_POINT('',(0.0136276364306931,-0.0331951640388587,0.0758190456948274));
#86097=CARTESIAN_POINT('',(0.013644469743817,-0.0331951640388688,0.0757588552506657));
#86098=CARTESIAN_POINT('',(0.0135544173329402,-0.0335216366567652,0.0760437600095019));
#86099=CARTESIAN_POINT('Origin',(-0.00252841005498943,-0.0326434571526939,
0.0717178695547645));
#86100=CARTESIAN_POINT('',(0.0135531345566467,-0.0336938721132327,0.0760433126821901));
#86101=CARTESIAN_POINT('Origin',(0.0238647199702471,-0.0336938867896168,
0.0796391486340378));
#86102=CARTESIAN_POINT('',(0.0135737140423351,-0.0336938721132538,0.0759842979825888));
#86103=CARTESIAN_POINT('Ctrl Pts',(0.0137074019977526,-0.0335235895815172,
0.0763461761944996));
#86104=CARTESIAN_POINT('Ctrl Pts',(0.0137376366869429,-0.0334144449262749,
0.0762693066747529));
#86105=CARTESIAN_POINT('Ctrl Pts',(0.0137663180457009,-0.0333049234473147,
0.0761917242153164));
#86106=CARTESIAN_POINT('Ctrl Pts',(0.0137934004130336,-0.0331951640388587,
0.0761135246981882));
#86107=CARTESIAN_POINT('Ctrl Pts',(0.0136559445417368,-0.0335235895815172,
0.0762452143071017));
#86108=CARTESIAN_POINT('Ctrl Pts',(0.0136847892917715,-0.0334144449262749,
0.0761690532005474));
#86109=CARTESIAN_POINT('Ctrl Pts',(0.0137120937497854,-0.0333049234473147,
0.0760922086832813));
#86110=CARTESIAN_POINT('Ctrl Pts',(0.0137378141008947,-0.0331951640388587,
0.0760147758531855));
#86111=CARTESIAN_POINT('Ctrl Pts',(0.013604487085721,-0.0335235895815172,
0.0761442524197038));
#86112=CARTESIAN_POINT('Ctrl Pts',(0.0136319418966,-0.0334144449262749,
0.076068799726342));
#86113=CARTESIAN_POINT('Ctrl Pts',(0.01365786945387,-0.0333049234473147,
0.0759926931512462));
#86114=CARTESIAN_POINT('Ctrl Pts',(0.0136822277887558,-0.0331951640388587,
0.0759160270081828));
#86115=CARTESIAN_POINT('Ctrl Pts',(0.0135530296297052,-0.0335235895815172,
0.0760432905323059));
#86116=CARTESIAN_POINT('Ctrl Pts',(0.0135790945014285,-0.0334144449262749,
0.0759685462521365));
#86117=CARTESIAN_POINT('Ctrl Pts',(0.0136036451579545,-0.0333049234473147,
0.075893177619211));
#86118=CARTESIAN_POINT('Ctrl Pts',(0.0136266414766169,-0.0331951640388587,
0.0758172781631801));
#86119=CARTESIAN_POINT('',(0.0137105184218707,-0.0331951640388687,0.0759662851965132));
#86120=CARTESIAN_POINT('Ctrl Pts',(0.013789193350316,-0.0332121607145939,
0.0761256306232392));
#86121=CARTESIAN_POINT('Ctrl Pts',(0.0137486755620964,-0.033262544410879,
0.0761115013427737));
#86122=CARTESIAN_POINT('Ctrl Pts',(0.0137088559589482,-0.033313530074487,
0.0760976155319822));
#86123=CARTESIAN_POINT('Ctrl Pts',(0.0136305815142302,-0.0334167203140537,
0.0760703198272733));
#86124=CARTESIAN_POINT('Ctrl Pts',(0.0135921569892141,-0.0334688847587207,
0.0760569205052826));
#86125=CARTESIAN_POINT('Ctrl Pts',(0.013554417332325,-0.0335216366562267,
0.0760437600091083));
#86126=CARTESIAN_POINT('Ctrl Pts',(0.0135933931509884,-0.0336938721132389,
0.0759257180657895));
#86127=CARTESIAN_POINT('Ctrl Pts',(0.0136037870180731,-0.0336474569764957,
0.0758937026178437));
#86128=CARTESIAN_POINT('Ctrl Pts',(0.0136138053917227,-0.033601104548885,
0.0758615676902795));
#86129=CARTESIAN_POINT('Ctrl Pts',(0.0136391696104349,-0.0334837508592656,
0.0757802094419696));
#86130=CARTESIAN_POINT('Ctrl Pts',(0.0136621118774707,-0.0333660264659097,
0.0756981353258173));
#86131=CARTESIAN_POINT('Ctrl Pts',(0.0135942935279973,-0.0336938721132389,
0.0759252832829869));
#86132=CARTESIAN_POINT('Ctrl Pts',(0.013604684850154,-0.0336474569764957,
0.0758932625648357));
#86133=CARTESIAN_POINT('Ctrl Pts',(0.0136147006173555,-0.033601104548885,
0.0758611223972187));
#86134=CARTESIAN_POINT('Ctrl Pts',(0.0136400582371406,-0.0334837508592656,
0.0757797508823002));
#86135=CARTESIAN_POINT('Ctrl Pts',(0.0136629935150297,-0.0333660264659097,
0.0756976637009048));
#86136=CARTESIAN_POINT('Ctrl Pts',(0.0139004256888299,-0.0336938721132389,
0.0757774552092352));
#86137=CARTESIAN_POINT('Ctrl Pts',(0.0139099517242165,-0.0336474569764957,
0.0757436425979612));
#86138=CARTESIAN_POINT('Ctrl Pts',(0.0139190812875663,-0.033601104548885,
0.0757097207892773));
#86139=CARTESIAN_POINT('Ctrl Pts',(0.01394219524295,-0.0334837508592656,
0.0756238385688022));
#86140=CARTESIAN_POINT('Ctrl Pts',(0.013962754180132,-0.0333660264659097,
0.0755373091470478));
#86141=CARTESIAN_POINT('',(0.0139020648336084,-0.0336769361243753,0.0757659980589394));
#86142=CARTESIAN_POINT('',(0.0138985998508737,-0.033693872113232,0.0757783368876132));
#86143=CARTESIAN_POINT('Ctrl Pts',(0.0139020648336085,-0.0336769361243753,
0.0757659980589393));
#86144=CARTESIAN_POINT('Ctrl Pts',(0.0139014894897374,-0.0336797586669941,
0.0757680553012016));
#86145=CARTESIAN_POINT('Ctrl Pts',(0.0139009130689664,-0.0336825812712675,
0.0757701121583982));
#86146=CARTESIAN_POINT('Ctrl Pts',(0.0138997580762776,-0.0336882265924994,
0.0757742250951142));
#86147=CARTESIAN_POINT('Ctrl Pts',(0.0138991795043904,-0.033691049309423,
0.0757762811746089));
#86148=CARTESIAN_POINT('Ctrl Pts',(0.0138985998508829,-0.033693872113236,
0.0757783368876103));
#86149=CARTESIAN_POINT('Ctrl Pts',(0.0139020648336084,-0.0336769361243753,
0.0757659980589394));
#86150=CARTESIAN_POINT('Ctrl Pts',(0.0138616988599108,-0.0336278994719898,
0.0757547090066031));
#86151=CARTESIAN_POINT('Ctrl Pts',(0.0138207581875897,-0.0335767852743495,
0.0757432592297203));
#86152=CARTESIAN_POINT('Ctrl Pts',(0.0137405280206276,-0.0334733172064609,
0.0757208214567442));
#86153=CARTESIAN_POINT('Ctrl Pts',(0.0137011907099758,-0.0334209631456226,
0.075709820088065));
#86154=CARTESIAN_POINT('Ctrl Pts',(0.0136626113902799,-0.0333679869844681,
0.0756990307048481));
#86155=CARTESIAN_POINT('',(0.0137464466894487,-0.0336938721132534,0.0758518100853004));
#86156=CARTESIAN_POINT('Origin',(0.00812378219310841,-0.0315241814719618,
0.07415));
#86157=CARTESIAN_POINT('',(0.0139020648323678,-0.0337108120655378,0.0757659980585962));
#86158=CARTESIAN_POINT('',(0.0139055034524797,-0.0336938721132327,0.07575365185715));
#86159=CARTESIAN_POINT('Origin',(-0.00155354328806278,-0.0345562524833384,
0.0702830764010626));
#86160=CARTESIAN_POINT('Ctrl Pts',(0.0139055034524908,-0.0336938721132385,
0.0757536518571611));
#86161=CARTESIAN_POINT('Ctrl Pts',(0.013904932583456,-0.0336910492952032,
0.0757557100380685));
#86162=CARTESIAN_POINT('Ctrl Pts',(0.0139043606039045,-0.033688226585389,
0.0757577679556348));
#86163=CARTESIAN_POINT('Ctrl Pts',(0.0139032144009328,-0.0336825812712763,
0.0757618833449552));
#86164=CARTESIAN_POINT('Ctrl Pts',(0.0139026401774804,-0.0336797586669984,
0.075763940816674));
#86165=CARTESIAN_POINT('Ctrl Pts',(0.0139020648336084,-0.033676936124375,
0.0757659980589397));
#86166=CARTESIAN_POINT('Origin',(-0.00215555888469551,-0.0345562520271967,
0.0724356912422816));
#86167=CARTESIAN_POINT('Ctrl Pts',(0.0136170288714271,-0.0342436276873911,
0.0758536331562695));
#86168=CARTESIAN_POINT('Ctrl Pts',(0.0136812824551496,-0.0339430054201811,
0.0756464519423711));
#86169=CARTESIAN_POINT('Ctrl Pts',(0.0137297477632473,-0.0336441434784052,
0.0754350194653847));
#86170=CARTESIAN_POINT('Ctrl Pts',(0.0136858752375207,-0.0342436276873911,
0.0756132996840362));
#86171=CARTESIAN_POINT('Ctrl Pts',(0.0137410644949106,-0.0339430054201811,
0.0754035218866354));
#86172=CARTESIAN_POINT('Ctrl Pts',(0.013780295642168,-0.0336441434784052,
0.0751901829649674));
#86173=CARTESIAN_POINT('Ctrl Pts',(0.0136865637011816,-0.0342436276873911,
0.0756108963493139));
#86174=CARTESIAN_POINT('Ctrl Pts',(0.0137416623153082,-0.0339430054201811,
0.075401092586078));
#86175=CARTESIAN_POINT('Ctrl Pts',(0.0137808011209572,-0.0336441434784052,
0.0751877345999632));
#86176=CARTESIAN_POINT('',(0.0136949696831489,-0.0341934961088741,0.0755782839181398));
#86177=CARTESIAN_POINT('',(0.0137489462195366,-0.0338664212863854,0.0753481880820869));
#86178=CARTESIAN_POINT('Origin',(-0.00238150079543393,-0.034561072040523,
0.0709306780062336));
#86179=CARTESIAN_POINT('Origin',(0.024474590049207,-0.0336938005073029,
0.0776327643813499));
#86180=CARTESIAN_POINT('',(0.0137215760778875,-0.0336938721132327,0.0754701623474144));
#86181=CARTESIAN_POINT('',(0.013734596785053,-0.0336938721132427,0.075409033702869));
#86182=CARTESIAN_POINT('',(0.0136626113902784,-0.0340203938281605,0.0756990307048533));
#86183=CARTESIAN_POINT('Origin',(-0.00217820120041667,-0.0345589643244919,
0.0704945518675342));
#86184=CARTESIAN_POINT('',(0.013661303056921,-0.0341934961088741,0.0756986648064836));
#86185=CARTESIAN_POINT('Origin',(0.0242735496589752,-0.0341934220717668,
0.0786665664771319));
#86186=CARTESIAN_POINT('',(0.013678136370045,-0.0341934961088841,0.0756384743623218));
#86187=CARTESIAN_POINT('Ctrl Pts',(0.0138342822040808,-0.0340223579322396,
0.0759912467582561));
#86188=CARTESIAN_POINT('Ctrl Pts',(0.0138596777990503,-0.0339125849573575,
0.0759124840694955));
#86189=CARTESIAN_POINT('Ctrl Pts',(0.0138834253441911,-0.0338030433565231,
0.0758332510965597));
#86190=CARTESIAN_POINT('Ctrl Pts',(0.0139055034524856,-0.0336938721132327,
0.0757536518571592));
#86191=CARTESIAN_POINT('Ctrl Pts',(0.0137765868662166,-0.0340223579322396,
0.075893715082275));
#86192=CARTESIAN_POINT('Ctrl Pts',(0.013800637245001,-0.0339125849573575,
0.0758157481626994));
#86193=CARTESIAN_POINT('Ctrl Pts',(0.0138230569897976,-0.0338030433565231,
0.0757373382426199));
#86194=CARTESIAN_POINT('Ctrl Pts',(0.0138438263183178,-0.0336938721132327,
0.0756585881366776));
#86195=CARTESIAN_POINT('Ctrl Pts',(0.0137188915283524,-0.0340223579322396,
0.075796183406294));
#86196=CARTESIAN_POINT('Ctrl Pts',(0.0137415966909517,-0.0339125849573575,
0.0757190122559032));
#86197=CARTESIAN_POINT('Ctrl Pts',(0.0137626886354041,-0.0338030433565231,
0.07564142538868));
#86198=CARTESIAN_POINT('Ctrl Pts',(0.01378214918415,-0.0336938721132327,
0.0755635244161961));
#86199=CARTESIAN_POINT('Ctrl Pts',(0.0136611961904882,-0.0340223579322396,
0.0756986517303129));
#86200=CARTESIAN_POINT('Ctrl Pts',(0.0136825561369025,-0.0339125849573575,
0.0756222763491071));
#86201=CARTESIAN_POINT('Ctrl Pts',(0.0137023202810106,-0.0338030433565231,
0.0755455125347402));
#86202=CARTESIAN_POINT('Ctrl Pts',(0.0137204720499822,-0.0336938721132327,
0.0754684606957146));
#86203=CARTESIAN_POINT('',(0.0138135397651936,-0.0336938721132427,0.0756119071022923));
#86204=CARTESIAN_POINT('Ctrl Pts',(0.0139020648288926,-0.0337108120662651,
0.0757659980576206));
#86205=CARTESIAN_POINT('Ctrl Pts',(0.0138606545197245,-0.0337611408993388,
0.0757544169385582));
#86206=CARTESIAN_POINT('Ctrl Pts',(0.0138199998568237,-0.0338121088779471,
0.0757430471492243));
#86207=CARTESIAN_POINT('Ctrl Pts',(0.0137401647875367,-0.0339153382773231,
0.0757207198722408));
#86208=CARTESIAN_POINT('Ctrl Pts',(0.0137010181564829,-0.0339675558473108,
0.0757097718304552));
#86209=CARTESIAN_POINT('Ctrl Pts',(0.0136626113902414,-0.0340203938281304,
0.0756990307048375));
#86210=CARTESIAN_POINT('Ctrl Pts',(0.0136932023061429,-0.0341934961088741,
0.0755792787851676));
#86211=CARTESIAN_POINT('Ctrl Pts',(0.0137227515190235,-0.0340287516182428,
0.0754641354119857));
#86212=CARTESIAN_POINT('Ctrl Pts',(0.0137475165196988,-0.0338644633275951,
0.075347869135228));
#86213=CARTESIAN_POINT('Ctrl Pts',(0.0136949696831488,-0.0341934961088741,
0.0755782839181399));
#86214=CARTESIAN_POINT('Ctrl Pts',(0.0137244983279374,-0.0340287516182428,
0.0754631040058308));
#86215=CARTESIAN_POINT('Ctrl Pts',(0.0137492412679059,-0.0338644633275951,
0.0753468020712627));
#86216=CARTESIAN_POINT('Ctrl Pts',(0.0139894486865093,-0.0341934961088741,
0.0754125199357997));
#86217=CARTESIAN_POINT('Ctrl Pts',(0.0140155502915538,-0.0340287516182428,
0.0752912519020902));
#86218=CARTESIAN_POINT('Ctrl Pts',(0.0140366174934418,-0.0338644633275951,
0.0751690086904575));
#86219=CARTESIAN_POINT('',(0.0139921320694915,-0.0341764758832442,0.0753999878875921));
#86220=CARTESIAN_POINT('',(0.0139894486864998,-0.034193496108874,0.075412519935805));
#86221=CARTESIAN_POINT('Origin',(-0.00209562656239066,-0.0345621027449978,
0.0714496273328017));
#86222=CARTESIAN_POINT('Ctrl Pts',(0.0139921320683069,-0.0341764758837551,
0.0753999878889735));
#86223=CARTESIAN_POINT('Ctrl Pts',(0.0139501495210267,-0.0341260050040482,
0.0753910454103771));
#86224=CARTESIAN_POINT('Ctrl Pts',(0.0139088967215007,-0.0340749269148198,
0.0753822584105242));
#86225=CARTESIAN_POINT('Ctrl Pts',(0.0138278186848013,-0.0339715436305913,
0.0753649883788871));
#86226=CARTESIAN_POINT('Ctrl Pts',(0.0137880242080292,-0.0339192778235948,
0.0753565118931052));
#86227=CARTESIAN_POINT('Ctrl Pts',(0.0137489462203027,-0.0338664212855055,
0.0753481880840776));
#86228=CARTESIAN_POINT('',(0.0138422091848344,-0.0341934961088841,0.0754954019269825));
#86229=CARTESIAN_POINT('Origin',(0.00812378219310841,-0.0315241814719618,
0.07415));
#86230=CARTESIAN_POINT('',(0.0139921320689447,-0.0342105180190349,0.0753999878866158));
#86231=CARTESIAN_POINT('',(0.0139947886795375,-0.0341934961088739,0.0753874501348798));
#86232=CARTESIAN_POINT('Origin',(-0.00211012187497052,-0.0345621719126634,
0.0714925722877832));
#86233=CARTESIAN_POINT('Origin',(-0.0023089998855343,-0.0345621029764121,
0.0724513529978932));
#86234=CARTESIAN_POINT('Origin',(-0.00230473429099848,-0.0345621723551039,
0.0724062293487591));
#86235=CARTESIAN_POINT('Ctrl Pts',(0.013721263578851,-0.0346945769586966,
0.0754716294445764));
#86236=CARTESIAN_POINT('Ctrl Pts',(0.0137489456367192,-0.0345275153362944,
0.0753543879558428));
#86237=CARTESIAN_POINT('Ctrl Pts',(0.0137729477176782,-0.0343603235965185,
0.0752362455672146));
#86238=CARTESIAN_POINT('Ctrl Pts',(0.0137932040274104,-0.0341934961088739,
0.0751175527464929));
#86239=CARTESIAN_POINT('Ctrl Pts',(0.0137387286881129,-0.0346945769586966,
0.0753896355525826));
#86240=CARTESIAN_POINT('Ctrl Pts',(0.0137646933510848,-0.0345275153362944,
0.0752720282501428));
#86241=CARTESIAN_POINT('Ctrl Pts',(0.0137869660884367,-0.0343603235965185,
0.075153573963679));
#86242=CARTESIAN_POINT('Ctrl Pts',(0.0138054862341921,-0.0341934961088739,
0.075034624007431));
#86243=CARTESIAN_POINT('Ctrl Pts',(0.0137561937973755,-0.0346945769586966,
0.0753076416605875));
#86244=CARTESIAN_POINT('Ctrl Pts',(0.0137804410654508,-0.0345275153362944,
0.0751896685444432));
#86245=CARTESIAN_POINT('Ctrl Pts',(0.0138009844591957,-0.0343603235965185,
0.0750709023601439));
#86246=CARTESIAN_POINT('Ctrl Pts',(0.0138177684409741,-0.0341934961088739,
0.0749516952683679));
#86247=CARTESIAN_POINT('Ctrl Pts',(0.0137736589066369,-0.0346945769586966,
0.0752256477685948));
#86248=CARTESIAN_POINT('Ctrl Pts',(0.013796188779816,-0.0345275153362944,
0.0751073088387428));
#86249=CARTESIAN_POINT('Ctrl Pts',(0.0138150028299539,-0.0343603235965185,
0.0749882307566079));
#86250=CARTESIAN_POINT('Ctrl Pts',(0.0138300506477557,-0.0341934961088739,
0.0748687665293071));
#86251=CARTESIAN_POINT('',(0.0137736589065105,-0.0346945769586966,0.0752256477691874));
#86252=CARTESIAN_POINT('',(0.0138130810948949,-0.0343667727831529,0.0749926167614355));
#86253=CARTESIAN_POINT('Origin',(-0.00277651210024045,-0.0345626457061547,
0.0722610083501191));
#86254=CARTESIAN_POINT('Origin',(0.0247460026132076,-0.0341934771028947,
0.0766118392771571));
#86255=CARTESIAN_POINT('',(0.0137934237900075,-0.034193496108874,0.0751160689223408));
#86256=CARTESIAN_POINT('',(0.0138025805044319,-0.0341934961088839,0.0750542433242452));
#86257=CARTESIAN_POINT('',(0.0137489462188082,-0.0345211942962618,0.0753481880837279));
#86258=CARTESIAN_POINT('Origin',(-0.00267309256536622,-0.0345625596124823,
0.0717914391957437));
#86259=CARTESIAN_POINT('',(0.0137476174921984,-0.0346945769586885,0.0753479050583037));
#86260=CARTESIAN_POINT('Origin',(0.0245684310177836,-0.0346945685853916,
0.0776527933114799));
#86261=CARTESIAN_POINT('',(0.0137606381993645,-0.0346945769587026,0.0752867764137555));
#86262=CARTESIAN_POINT('Ctrl Pts',(0.0139386269144654,-0.0345231616327842,
0.0756290472834263));
#86263=CARTESIAN_POINT('Ctrl Pts',(0.0139590134989354,-0.0344132092796988,
0.0755488978355889));
#86264=CARTESIAN_POINT('Ctrl Pts',(0.0139777412034438,-0.034303273855898,
0.0754683308426755));
#86265=CARTESIAN_POINT('Ctrl Pts',(0.0139947886795439,-0.034193496108874,
0.0753874501348884));
#86266=CARTESIAN_POINT('Ctrl Pts',(0.0138749214539155,-0.0345231616327842,
0.0755353309538178));
#86267=CARTESIAN_POINT('Ctrl Pts',(0.0138940162907239,-0.0344132092796988,
0.075456059596064));
#86268=CARTESIAN_POINT('Ctrl Pts',(0.0139114704768197,-0.034303273855898,
0.0753763973667102));
#86269=CARTESIAN_POINT('Ctrl Pts',(0.0139272642655895,-0.034193496108874,
0.0752964468950599));
#86270=CARTESIAN_POINT('Ctrl Pts',(0.0138112159933657,-0.0345231616327842,
0.0754416146242093));
#86271=CARTESIAN_POINT('Ctrl Pts',(0.0138290190825124,-0.0344132092796988,
0.075363221356539));
#86272=CARTESIAN_POINT('Ctrl Pts',(0.0138451997501957,-0.034303273855898,
0.0752844638907449));
#86273=CARTESIAN_POINT('Ctrl Pts',(0.0138597398516351,-0.034193496108874,
0.0752054436552315));
#86274=CARTESIAN_POINT('Ctrl Pts',(0.0137475105328158,-0.0345231616327842,
0.0753478982946008));
#86275=CARTESIAN_POINT('Ctrl Pts',(0.013764021874301,-0.0344132092796988,
0.0752703831170141));
#86276=CARTESIAN_POINT('Ctrl Pts',(0.0137789290235716,-0.034303273855898,
0.0751925304147796));
#86277=CARTESIAN_POINT('Ctrl Pts',(0.0137922154376807,-0.034193496108874,
0.0751144404154031));
#86278=CARTESIAN_POINT('',(0.0138941062347825,-0.0341934961088839,0.0752517595286203));
#86279=CARTESIAN_POINT('Ctrl Pts',(0.0139921320655605,-0.0342105180195352,
0.0753999878858906));
#86280=CARTESIAN_POINT('Ctrl Pts',(0.0139501023246918,-0.0342610556240224,
0.0753910353407842));
#86281=CARTESIAN_POINT('Ctrl Pts',(0.0139088267857885,-0.0343122189867966,
0.0753822434444702));
#86282=CARTESIAN_POINT('Ctrl Pts',(0.0138277479302679,-0.0344158119695087,
0.0753649732425556));
#86283=CARTESIAN_POINT('Ctrl Pts',(0.0137879777757433,-0.0344681990449964,
0.0753565020006467));
#86284=CARTESIAN_POINT('Ctrl Pts',(0.0137489462187776,-0.034521194296237,
0.0753481880837135));
#86285=CARTESIAN_POINT('Ctrl Pts',(0.0137719579018241,-0.0346945769586932,
0.0752267513773195));
#86286=CARTESIAN_POINT('Ctrl Pts',(0.0137942189746654,-0.034529677707698,
0.0751099793410628));
#86287=CARTESIAN_POINT('Ctrl Pts',(0.0138116347301353,-0.034364806625142,
0.0749923870144551));
#86288=CARTESIAN_POINT('Ctrl Pts',(0.0137736589065087,-0.0346945769586932,
0.0752256477691962));
#86289=CARTESIAN_POINT('Ctrl Pts',(0.0137958971630329,-0.034529677707698,
0.0751088405658712));
#86290=CARTESIAN_POINT('Ctrl Pts',(0.0138132886681948,-0.034364806625142,
0.0749912140452645));
#86291=CARTESIAN_POINT('Ctrl Pts',(0.0140571484162524,-0.0346945769586932,
0.0750417203945992));
#86292=CARTESIAN_POINT('Ctrl Pts',(0.0140755841044496,-0.034529677707698,
0.0749190522462509));
#86293=CARTESIAN_POINT('Ctrl Pts',(0.0140889340522881,-0.034364806625142,
0.0747957269523684));
#86294=CARTESIAN_POINT('',(0.014059039610619,-0.0346775396665025,0.0750290445844434));
#86295=CARTESIAN_POINT('',(0.0140571484162445,-0.0346945769586886,0.0750417203946012));
#86296=CARTESIAN_POINT('Origin',(-0.00238509473027414,-0.0345626617186812,
0.0727479599732545));
#86297=CARTESIAN_POINT('Ctrl Pts',(0.0140590396094374,-0.0346775396670096,
0.0750290445858327));
#86298=CARTESIAN_POINT('Ctrl Pts',(0.0140165449604337,-0.0346269749928185,
0.0750227509053555));
#86299=CARTESIAN_POINT('Ctrl Pts',(0.0139748055309025,-0.0345757902890792,
0.0750165691131565));
#86300=CARTESIAN_POINT('Ctrl Pts',(0.0138928027611549,-0.0344721681087934,
0.0750044240437503));
#86301=CARTESIAN_POINT('Ctrl Pts',(0.0138525715707228,-0.0344197714289811,
0.0749984655224078));
#86302=CARTESIAN_POINT('Ctrl Pts',(0.0138130810949626,-0.0343667727830751,
0.0749926167616832));
#86303=CARTESIAN_POINT('',(0.0139154036613875,-0.0346945769587026,0.0751336840819043));
#86304=CARTESIAN_POINT('Origin',(0.00812378219310841,-0.0315241814719618,
0.07415));
#86305=CARTESIAN_POINT('',(0.0140590396095596,-0.0347116136489778,0.0750290445835401));
#86306=CARTESIAN_POINT('',(0.0140609037262012,-0.0346945769586885,0.0750163647622645));
#86307=CARTESIAN_POINT('Origin',(-0.00238987658608596,-0.0345626699728473,
0.0727930181104228));
#86308=CARTESIAN_POINT('Origin',(-0.00234034722035878,-0.0345626621420261,
0.0724458218881048));
#86309=CARTESIAN_POINT('Origin',(-0.00233186185881384,-0.0345626703330979,
0.0724013121759761));
#86310=CARTESIAN_POINT('Ctrl Pts',(0.0137868629035117,-0.0352450361874067,
0.075154131213081));
#86311=CARTESIAN_POINT('Ctrl Pts',(0.0138247343336543,-0.0349452760959492,
0.0749405446192951));
#86312=CARTESIAN_POINT('Ctrl Pts',(0.0138464099588815,-0.034644428984174,
0.0747247121714631));
#86313=CARTESIAN_POINT('Ctrl Pts',(0.0137872485048313,-0.0352450361874067,
0.0751516358300198));
#86314=CARTESIAN_POINT('Ctrl Pts',(0.0138250258200575,-0.0349452760959492,
0.0749380346930414));
#86315=CARTESIAN_POINT('Ctrl Pts',(0.013846606502286,-0.034644428984174,
0.0747221948324533));
#86316=CARTESIAN_POINT('Ctrl Pts',(0.0138254268533143,-0.0352450361874067,
0.0749045682001953));
#86317=CARTESIAN_POINT('Ctrl Pts',(0.0138538858599753,-0.0349452760959492,
0.0746895271431759));
#86318=CARTESIAN_POINT('Ctrl Pts',(0.0138660662453032,-0.034644428984174,
0.0744729533463366));
#86319=CARTESIAN_POINT('Ctrl Pts',(0.0138258086367991,-0.0352450361874067,
0.074902097523897));
#86320=CARTESIAN_POINT('Ctrl Pts',(0.0138541744603744,-0.0349452760959492,
0.0746870420676772));
#86321=CARTESIAN_POINT('Ctrl Pts',(0.0138662608427333,-0.034644428984174,
0.0744704609314754));
#86322=CARTESIAN_POINT('',(0.0138300489585611,-0.0351951634053356,0.0748687989315356));
#86323=CARTESIAN_POINT('',(0.0138547629072621,-0.0348678972925434,0.0746337200161246));
#86324=CARTESIAN_POINT('Origin',(-0.00287048597998444,-0.0345636767886427,
0.0736454309840678));
#86325=CARTESIAN_POINT('Origin',(0.0248654530858629,-0.0346946199341076,
0.0755630697984134));
#86326=CARTESIAN_POINT('',(0.0138428960148987,-0.0346945769330288,0.0747581628824752));
#86327=CARTESIAN_POINT('',(0.0138481526002897,-0.0346945769458128,0.0746958843195694));
#86328=CARTESIAN_POINT('',(0.0138130810948181,-0.0350221583435276,0.0749926167616453));
#86329=CARTESIAN_POINT('Origin',(-0.0028715381721229,-0.0345628458715597,
0.0731646583917354));
#86330=CARTESIAN_POINT('',(0.0138118571135841,-0.0351951360298762,0.0749924385407569));
#86331=CARTESIAN_POINT('Origin',(0.0247119344431038,-0.035195183836679,
0.0766067984976786));
#86332=CARTESIAN_POINT('',(0.0138300506477803,-0.0351951371328746,0.0748687665299341));
#86333=CARTESIAN_POINT('Ctrl Pts',(0.0140200229719114,-0.0350241211494343,
0.0752610106563321));
#86334=CARTESIAN_POINT('Ctrl Pts',(0.0140353266881703,-0.0349144232818962,
0.0751797923571569));
#86335=CARTESIAN_POINT('Ctrl Pts',(0.0140489607241615,-0.0348045283579412,
0.0750982091061643));
#86336=CARTESIAN_POINT('Ctrl Pts',(0.0140609037278127,-0.0346945769439157,
0.0750163647512761));
#86337=CARTESIAN_POINT('Ctrl Pts',(0.0139505586928547,-0.0350241211494343,
0.0751714793448331));
#86338=CARTESIAN_POINT('Ctrl Pts',(0.0139646291520069,-0.0349144232818962,
0.0750912178876204));
#86339=CARTESIAN_POINT('Ctrl Pts',(0.0139770489713349,-0.0348045283579412,
0.075010617543612));
#86340=CARTESIAN_POINT('Ctrl Pts',(0.0139877984008727,-0.0346945769439157,
0.0749297809596255));
#86341=CARTESIAN_POINT('Ctrl Pts',(0.013881094413798,-0.0350241211494343,
0.075081948033334));
#86342=CARTESIAN_POINT('Ctrl Pts',(0.0138939316158436,-0.0349144232818962,
0.0750026434180839));
#86343=CARTESIAN_POINT('Ctrl Pts',(0.0139051372185082,-0.0348045283579412,
0.0749230259810597));
#86344=CARTESIAN_POINT('Ctrl Pts',(0.0139146930739326,-0.0346945769439157,
0.0748431971679748));
#86345=CARTESIAN_POINT('Ctrl Pts',(0.0138116301347413,-0.0350241211494343,
0.074992416721835));
#86346=CARTESIAN_POINT('Ctrl Pts',(0.0138232340796803,-0.0349144232818962,
0.0749140689485474));
#86347=CARTESIAN_POINT('Ctrl Pts',(0.0138332254656815,-0.0348045283579412,
0.0748354344185074));
#86348=CARTESIAN_POINT('Ctrl Pts',(0.0138415877469926,-0.0346945769439157,
0.0747566133763242));
#86349=CARTESIAN_POINT('',(0.0139518998706068,-0.0346945769458128,0.0748872638226747));
#86350=CARTESIAN_POINT('Ctrl Pts',(0.0140590396063014,-0.0347116136492757,
0.0750290445830529));
#86351=CARTESIAN_POINT('Ctrl Pts',(0.0140165618348323,-0.03476215465312,
0.0750227533892073));
#86352=CARTESIAN_POINT('Ctrl Pts',(0.0139748309373691,-0.0348133084094805,
0.0750165728115495));
#86353=CARTESIAN_POINT('Ctrl Pts',(0.0138928280628412,-0.0349168561544566,
0.0750044277304468));
#86354=CARTESIAN_POINT('Ctrl Pts',(0.013852588612414,-0.0349692089015913,
0.0749984680443775));
#86355=CARTESIAN_POINT('Ctrl Pts',(0.0138130810947848,-0.0350221583435,
0.0749926167616203));
#86356=CARTESIAN_POINT('Ctrl Pts',(0.0138288757376796,-0.0351951371254987,
0.0748696383132657));
#86357=CARTESIAN_POINT('Ctrl Pts',(0.0138437538082903,-0.035030733898099,
0.0747516890837268));
#86358=CARTESIAN_POINT('Ctrl Pts',(0.0138537441967495,-0.034865930689785,
0.0746332257143997));
#86359=CARTESIAN_POINT('Ctrl Pts',(0.0138300506476639,-0.0351951371254987,
0.0748687665299282));
#86360=CARTESIAN_POINT('Ctrl Pts',(0.013844910694701,-0.035030733898099,
0.0747507930098626));
#86361=CARTESIAN_POINT('Ctrl Pts',(0.0138548820710341,-0.034865930689785,
0.0746323061156986));
#86362=CARTESIAN_POINT('Ctrl Pts',(0.0140269667855979,-0.0351951371254987,
0.0747226547339397));
#86363=CARTESIAN_POINT('Ctrl Pts',(0.0140388060629266,-0.035030733898099,
0.0746006100962716));
#86364=CARTESIAN_POINT('Ctrl Pts',(0.0140455909870978,-0.034865930689785,
0.0744781804149227));
#86365=CARTESIAN_POINT('Origin',(0.0191541016189813,-0.0308609197383775,
0.0750810075408726));
#86366=CARTESIAN_POINT('',(0.013915901643935,-0.0351951371254987,0.0748050650812598));
#86367=CARTESIAN_POINT('Origin',(0.00714850037396323,-0.0351840467441105,
0.0742097580428411));
#86368=CARTESIAN_POINT('Origin',(0.020087224815563,-0.0352322614134536,
0.0743622414773902));
#86369=CARTESIAN_POINT('',(0.0138697841027619,-0.0351951142564685,0.0743975411838139));
#86370=CARTESIAN_POINT('',(0.0138724689333491,-0.0351951372916788,0.0742728851601393));
#86371=CARTESIAN_POINT('Origin',(0.00795151354200019,-0.0352875119606938,
0.0738562016325136));
#86372=CARTESIAN_POINT('Origin',(0.00653015769557002,-0.0298325076522644,
0.0814818177310111));
#86373=CARTESIAN_POINT('Origin',(0.015819487519279,-0.0338733536828882,
0.0774699035959178));
#86374=CARTESIAN_POINT('Ctrl Pts',(0.0126266937484795,-0.0321934096636942,
0.0777279775390318));
#86375=CARTESIAN_POINT('Ctrl Pts',(0.0126907378425213,-0.0320508460845409,
0.0776473775665703));
#86376=CARTESIAN_POINT('Ctrl Pts',(0.0127525680848831,-0.0319086045665233,
0.0775651176283178));
#86377=CARTESIAN_POINT('Ctrl Pts',(0.0128120659258028,-0.0317669892871128,
0.0774813858045927));
#86378=CARTESIAN_POINT('Ctrl Pts',(0.0126774166268874,-0.0321934096636942,
0.0776612121120972));
#86379=CARTESIAN_POINT('Ctrl Pts',(0.012740265651582,-0.0320508460845409,
0.0775797042242675));
#86380=CARTESIAN_POINT('Ctrl Pts',(0.0128008773317886,-0.0319086045665233,
0.0774965691643733));
#86381=CARTESIAN_POINT('Ctrl Pts',(0.0128591358966499,-0.0317669892871128,
0.077411996681018));
#86382=CARTESIAN_POINT('Ctrl Pts',(0.0127281395052951,-0.0321934096636942,
0.0775944466851627));
#86383=CARTESIAN_POINT('Ctrl Pts',(0.0127897934606427,-0.0320508460845409,
0.0775120308819648));
#86384=CARTESIAN_POINT('Ctrl Pts',(0.0128491865786941,-0.0319086045665233,
0.0774280207004287));
#86385=CARTESIAN_POINT('Ctrl Pts',(0.0129062058674971,-0.0317669892871128,
0.0773426075574432));
#86386=CARTESIAN_POINT('Ctrl Pts',(0.012778862383703,-0.0321934096636942,
0.0775276812582281));
#86387=CARTESIAN_POINT('Ctrl Pts',(0.0128393212697036,-0.0320508460845409,
0.0774443575396621));
#86388=CARTESIAN_POINT('Ctrl Pts',(0.0128974958255996,-0.0319086045665233,
0.0773594722364842));
#86389=CARTESIAN_POINT('Ctrl Pts',(0.0129532758383442,-0.0317669892871128,
0.0772732184338684));
#86390=CARTESIAN_POINT('',(0.0127779549413831,-0.0321934096636942,0.0775288757049082));
#86391=CARTESIAN_POINT('',(0.0129128449803401,-0.031866561751136,0.0773348080961386));
#86392=CARTESIAN_POINT('Origin',(-0.000373699603126572,-0.0326371944422049,
0.0672210200799123));
#86393=CARTESIAN_POINT('Origin',(0.0220400460991528,-0.0316939261509554,
0.083404551897409));
#86394=CARTESIAN_POINT('',(0.0127035418190161,-0.0320197221621763,0.077628992804741));
#86395=CARTESIAN_POINT('Ctrl Pts',(0.0127036875798339,-0.0320197392094682,
0.0776288789246988));
#86396=CARTESIAN_POINT('Ctrl Pts',(0.0127213891968547,-0.031979271657598,
0.0776055748652964));
#86397=CARTESIAN_POINT('Ctrl Pts',(0.0127389937376033,-0.0319386439829675,
0.0775820297669435));
#86398=CARTESIAN_POINT('Ctrl Pts',(0.0127565129100146,-0.0318979099381607,
0.0775582138472279));
#86399=CARTESIAN_POINT('Ctrl Pts',(0.0127740317361464,-0.0318571766984925,
0.0775343983982515));
#86400=CARTESIAN_POINT('Ctrl Pts',(0.0127913775904035,-0.0318163871833591,
0.0775104342400269));
#86401=CARTESIAN_POINT('Ctrl Pts',(0.0128084936625507,-0.0317755399638303,
0.0774864058639879));
#86402=CARTESIAN_POINT('',(0.0127023373432517,-0.0321934096636184,0.0776284095125642));
#86403=CARTESIAN_POINT('Origin',(0.0145533252831688,-0.0324113096967968,
0.0790082204358468));
#86404=CARTESIAN_POINT('',(0.0127401461423274,-0.0321934096636663,0.0775786426087462));
#86405=CARTESIAN_POINT('Ctrl Pts',(0.01277594536621,-0.0321934096636618,
0.077529150104258));
#86406=CARTESIAN_POINT('Ctrl Pts',(0.0128225464797032,-0.0320835708272592,
0.077464993148417));
#86407=CARTESIAN_POINT('Ctrl Pts',(0.0128677928377901,-0.0319739230346489,
0.077399908998596));
#86408=CARTESIAN_POINT('Ctrl Pts',(0.0129116329416846,-0.0318646057455573,
0.0773339853683124));
#86409=CARTESIAN_POINT('Ctrl Pts',(0.0128882223728398,-0.0321934096636618,
0.0775138191372984));
#86410=CARTESIAN_POINT('Ctrl Pts',(0.0129346120603504,-0.0320835708272592,
0.0774481137940323));
#86411=CARTESIAN_POINT('Ctrl Pts',(0.0129796150712931,-0.0319739230346489,
0.0773814865303636));
#86412=CARTESIAN_POINT('Ctrl Pts',(0.01302318036975,-0.0318646057455573,
0.077314027010222));
#86413=CARTESIAN_POINT('Ctrl Pts',(0.0130004993794696,-0.0321934096636618,
0.0774984881703387));
#86414=CARTESIAN_POINT('Ctrl Pts',(0.0130466776409976,-0.0320835708272592,
0.0774312344396476));
#86415=CARTESIAN_POINT('Ctrl Pts',(0.013091437304796,-0.0319739230346489,
0.0773630640621313));
#86416=CARTESIAN_POINT('Ctrl Pts',(0.0131347277978154,-0.0318646057455573,
0.0772940686521315));
#86417=CARTESIAN_POINT('Ctrl Pts',(0.0131127763860994,-0.0321934096636618,
0.077483157203379));
#86418=CARTESIAN_POINT('Ctrl Pts',(0.0131587432216448,-0.0320835708272592,
0.0774143550852629));
#86419=CARTESIAN_POINT('Ctrl Pts',(0.0132032595382989,-0.0319739230346489,
0.077344641593899));
#86420=CARTESIAN_POINT('Ctrl Pts',(0.0132462752258808,-0.0318646057455573,
0.0772741102940411));
#86421=CARTESIAN_POINT('',(0.0131198846867272,-0.0321763980308324,0.0774724930174722));
#86422=CARTESIAN_POINT('',(0.0131127763861026,-0.0321934096636184,0.0774831572033539));
#86423=CARTESIAN_POINT('Origin',(-0.000309909663595976,-0.0326386230113314,
0.0678046743817851));
#86424=CARTESIAN_POINT('Ctrl Pts',(0.013119884684081,-0.032176398030637,
0.0774724930157105));
#86425=CARTESIAN_POINT('Ctrl Pts',(0.0130841468191009,-0.0321259596176084,
0.0774487267284882));
#86426=CARTESIAN_POINT('Ctrl Pts',(0.0130490281589977,-0.0320749164633889,
0.0774253722230343));
#86427=CARTESIAN_POINT('Ctrl Pts',(0.0129800009858953,-0.0319716057794026,
0.077379467980489));
#86428=CARTESIAN_POINT('Ctrl Pts',(0.0129461193684401,-0.0319193786690236,
0.0773569361293911));
#86429=CARTESIAN_POINT('Ctrl Pts',(0.0129128449787917,-0.0318665617525439,
0.0773348080951066));
#86430=CARTESIAN_POINT('',(0.0129453656637528,-0.0321934096636663,0.077506016454141));
#86431=CARTESIAN_POINT('Origin',(0.00812378219310841,-0.0315241814719618,
0.07415));
#86432=CARTESIAN_POINT('',(0.0131198846870346,-0.0322104233323591,0.0774724930176767));
#86433=CARTESIAN_POINT('',(0.0131269701953155,-0.0321934096636183,0.0774618136744965));
#86434=CARTESIAN_POINT('Origin',(-0.000340025323281201,-0.0326387245328339,
0.0678385573848768));
#86435=CARTESIAN_POINT('Origin',(-0.000989363387862653,-0.0326386236000299,
0.068826381625835));
#86436=CARTESIAN_POINT('Origin',(-0.000969761349190316,-0.0326387248904986,
0.0687855065180588));
#86437=CARTESIAN_POINT('Ctrl Pts',(0.0128217378227486,-0.0327445246967096,
0.0774677308362694));
#86438=CARTESIAN_POINT('Ctrl Pts',(0.0129468680868411,-0.0324436878339359,
0.0772905445430941));
#86439=CARTESIAN_POINT('Ctrl Pts',(0.0130582964732978,-0.0321434074405926,
0.077104436294559));
#86440=CARTESIAN_POINT('Ctrl Pts',(0.0129614805368145,-0.0327445246967096,
0.0772604340107619));
#86441=CARTESIAN_POINT('Ctrl Pts',(0.0130787924733207,-0.0324436878339359,
0.0770779772349648));
#86442=CARTESIAN_POINT('Ctrl Pts',(0.0131820277489421,-0.0321434074405926,
0.0768872023850803));
#86443=CARTESIAN_POINT('',(0.0129809323555165,-0.0326943950436612,0.0772299703407371));
#86444=CARTESIAN_POINT('',(0.0131033706146527,-0.0323666188837389,0.0770278158648571));
#86445=CARTESIAN_POINT('Origin',(-0.00125684902059955,-0.0326395579112007,
0.068291646129512));
#86446=CARTESIAN_POINT('Origin',(0.0226659123405023,-0.0321933825603058,
0.0825542222542162));
#86447=CARTESIAN_POINT('',(0.0130396479397987,-0.032193409653269,0.077135362449924));
#86448=CARTESIAN_POINT('',(0.013070921159878,-0.0321934096584274,0.077081249271754));
#86449=CARTESIAN_POINT('',(0.0129128449811149,-0.0325210109756239,0.077334808096657));
#86450=CARTESIAN_POINT('Origin',(-0.000978290550343325,-0.0326393129159159,
0.0678997410280831));
#86451=CARTESIAN_POINT('',(0.0129117137509639,-0.0326943950436593,0.0773340558093872));
#86452=CARTESIAN_POINT('Origin',(0.0221232398451764,-0.0326943765538176,
0.0834598785069575));
#86453=CARTESIAN_POINT('',(0.0129463230532502,-0.0326943950436702,0.0772820130750721));
#86454=CARTESIAN_POINT('Ctrl Pts',(0.0129858143778344,-0.0325229783203769,
0.0776657706174871));
#86455=CARTESIAN_POINT('Ctrl Pts',(0.0130342791989117,-0.032413025309245,
0.0775987476101464));
#86456=CARTESIAN_POINT('Ctrl Pts',(0.0130813502123452,-0.032303122220807,
0.0775307322110764));
#86457=CARTESIAN_POINT('Ctrl Pts',(0.0131269701977931,-0.0321934096576658,
0.0774618136707666));
#86458=CARTESIAN_POINT('Ctrl Pts',(0.0129610818173628,-0.0325229783203769,
0.0775551838068385));
#86459=CARTESIAN_POINT('Ctrl Pts',(0.0130080222016736,-0.032413025309245,
0.077488501737303));
#86460=CARTESIAN_POINT('Ctrl Pts',(0.0130535760622879,-0.032303122220807,
0.0774208587592611));
#86461=CARTESIAN_POINT('Ctrl Pts',(0.0130976881053954,-0.0321934096576658,
0.0773523435775825));
#86462=CARTESIAN_POINT('Ctrl Pts',(0.0129363492568912,-0.0325229783203769,
0.0774445969961899));
#86463=CARTESIAN_POINT('Ctrl Pts',(0.0129817652044356,-0.032413025309245,
0.0773782558644595));
#86464=CARTESIAN_POINT('Ctrl Pts',(0.0130258019122307,-0.032303122220807,
0.0773109853074458));
#86465=CARTESIAN_POINT('Ctrl Pts',(0.0130684060129976,-0.0321934096576658,
0.0772428734843984));
#86466=CARTESIAN_POINT('Ctrl Pts',(0.0129116166964196,-0.0325229783203769,
0.0773340101855413));
#86467=CARTESIAN_POINT('Ctrl Pts',(0.0129555082071976,-0.032413025309245,
0.0772680099916161));
#86468=CARTESIAN_POINT('Ctrl Pts',(0.0129980277621734,-0.032303122220807,
0.0772011118556305));
#86469=CARTESIAN_POINT('Ctrl Pts',(0.0130391239205998,-0.0321934096576658,
0.0771334033912143));
#86470=CARTESIAN_POINT('',(0.0130833090674282,-0.0321934096584275,0.0772985880627087));
#86471=CARTESIAN_POINT('Ctrl Pts',(0.0131198846841324,-0.0322104233328892,
0.0774724930157448));
#86472=CARTESIAN_POINT('Ctrl Pts',(0.013084098393749,-0.0322609421830435,
0.0774486945248067));
#86473=CARTESIAN_POINT('Ctrl Pts',(0.0130489560770285,-0.0323120888238835,
0.0774253242872924));
#86474=CARTESIAN_POINT('Ctrl Pts',(0.0129799283813352,-0.0324156524631806,
0.0773794196972153));
#86475=CARTESIAN_POINT('Ctrl Pts',(0.01294607137655,-0.0324680267167298,
0.0773569042139691));
#86476=CARTESIAN_POINT('Ctrl Pts',(0.0129128449810812,-0.0325210109755912,
0.0773348080966293));
#86477=CARTESIAN_POINT('Origin',(0.00300964617453292,-0.0262834582510559,
0.0801290466318158));
#86478=CARTESIAN_POINT('Origin',(0.0141662311167886,-0.0342770764397661,
0.0847004464407597));
#86479=CARTESIAN_POINT('Ctrl Pts',(0.0129789444580278,-0.0326943950436604,
0.0772303702837421));
#86480=CARTESIAN_POINT('Ctrl Pts',(0.013021397733767,-0.0325844576448134,
0.0771634570481876));
#86481=CARTESIAN_POINT('Ctrl Pts',(0.0130624701385734,-0.0324744968375322,
0.0770956610737341));
#86482=CARTESIAN_POINT('Ctrl Pts',(0.0131021102462047,-0.0323646534831894,
0.0770270699503859));
#86483=CARTESIAN_POINT('Ctrl Pts',(0.0130900371114099,-0.0326943950436604,
0.0772080196697253));
#86484=CARTESIAN_POINT('Ctrl Pts',(0.0131321823537985,-0.0325844576448134,
0.0771395753691973));
#86485=CARTESIAN_POINT('Ctrl Pts',(0.0131729150385204,-0.0324744968375322,
0.0770702545920493));
#86486=CARTESIAN_POINT('Ctrl Pts',(0.0132121842015494,-0.0323646534831894,
0.0770001468759478));
#86487=CARTESIAN_POINT('Ctrl Pts',(0.0132011297647921,-0.0326943950436604,
0.0771856690557084));
#86488=CARTESIAN_POINT('Ctrl Pts',(0.0132429669738299,-0.0325844576448133,
0.0771156936902071));
#86489=CARTESIAN_POINT('Ctrl Pts',(0.0132833599384673,-0.0324744968375322,
0.0770448481103644));
#86490=CARTESIAN_POINT('Ctrl Pts',(0.013322258156894,-0.0323646534831894,
0.0769732238015097));
#86491=CARTESIAN_POINT('Ctrl Pts',(0.0133122224181742,-0.0326943950436604,
0.0771633184416916));
#86492=CARTESIAN_POINT('Ctrl Pts',(0.0133537515938614,-0.0325844576448133,
0.0770918120112168));
#86493=CARTESIAN_POINT('Ctrl Pts',(0.0133938048384143,-0.0324744968375322,
0.0770194416286796));
#86494=CARTESIAN_POINT('Ctrl Pts',(0.0134323321122387,-0.0323646534831894,
0.0769463007270716));
#86495=CARTESIAN_POINT('',(0.0133186470825827,-0.032677355999139,0.0771522289653595));
#86496=CARTESIAN_POINT('',(0.0133122224181615,-0.0326943950436595,0.0771633184416936));
#86497=CARTESIAN_POINT('Origin',(-0.00108340451308647,-0.032639567087523,
0.0688869875836626));
#86498=CARTESIAN_POINT('Ctrl Pts',(0.0133186470796761,-0.03267735599875,
0.0771522289636776));
#86499=CARTESIAN_POINT('Ctrl Pts',(0.0132814575341154,-0.0326267922587063,
0.0771307362909582));
#86500=CARTESIAN_POINT('Ctrl Pts',(0.0132449271463918,-0.0325756109581517,
0.077109624560341));
#86501=CARTESIAN_POINT('Ctrl Pts',(0.0131731535971661,-0.0324719985462385,
0.0770681450160186));
#86502=CARTESIAN_POINT('Ctrl Pts',(0.0131379392222946,-0.0324196091621783,
0.0770477938387531));
#86503=CARTESIAN_POINT('Ctrl Pts',(0.0131033706146104,-0.0323666188837757,
0.0770278158648328));
#86504=CARTESIAN_POINT('',(0.013146577386849,-0.0326943950436703,0.0771966443912254));
#86505=CARTESIAN_POINT('Origin',(0.00812378219310841,-0.0315241814719618,
0.07415));
#86506=CARTESIAN_POINT('',(0.0133186470825428,-0.032711433838003,0.0771522289653367));
#86507=CARTESIAN_POINT('',(0.0133250480478684,-0.0326943950436593,0.0771411257927597));
#86508=CARTESIAN_POINT('Origin',(-0.001105399748007,-0.0326395680729595,
0.0689266000423664));
#86509=CARTESIAN_POINT('Origin',(-0.00103312703808973,-0.0326395672038611,
0.0687999895580363));
#86510=CARTESIAN_POINT('Origin',(-0.00100978475184705,-0.0326395683429341,
0.0687611558268961));
#86511=CARTESIAN_POINT('Ctrl Pts',(0.0130208100933845,-0.0332451089994434,
0.0771661635804309));
#86512=CARTESIAN_POINT('Ctrl Pts',(0.0131345665639738,-0.0329451141710254,
0.0769814691514128));
#86513=CARTESIAN_POINT('Ctrl Pts',(0.0132340879250057,-0.0326442513127493,
0.0767887308173699));
#86514=CARTESIAN_POINT('Ctrl Pts',(0.0131472593109561,-0.0332451089994434,
0.076950500427863));
#86515=CARTESIAN_POINT('Ctrl Pts',(0.0132528819126693,-0.0329451141710254,
0.0767610368885774));
#86516=CARTESIAN_POINT('Ctrl Pts',(0.0133439332834064,-0.0326442513127493,
0.0765641556690614));
#86517=CARTESIAN_POINT('Ctrl Pts',(0.0131485238031318,-0.0332451089994434,
0.0769483437963373));
#86518=CARTESIAN_POINT('Ctrl Pts',(0.0132540650661562,-0.0329451141710254,
0.0767588325659491));
#86519=CARTESIAN_POINT('Ctrl Pts',(0.0133450317369904,-0.0326442513127493,
0.0765619099175782));
#86520=CARTESIAN_POINT('',(0.0131647408170115,-0.0331951640388616,0.0769189097406918));
#86521=CARTESIAN_POINT('',(0.0132742440992889,-0.0328677532355045,0.0767094661988068));
#86522=CARTESIAN_POINT('Origin',(-0.00188291505151877,-0.032640280827965,
0.0695297081368198));
#86523=CARTESIAN_POINT('Origin',(0.0231752604518522,-0.0326944278779147,
0.0816292485253018));
#86524=CARTESIAN_POINT('',(0.0132174000641565,-0.0326943950436593,0.0768208017492394));
#86525=CARTESIAN_POINT('',(0.0132452137775803,-0.0326943950436693,0.0767648316916638));
#86526=CARTESIAN_POINT('',(0.0131033706146512,-0.0330220786163545,0.0770278158648596));
#86527=CARTESIAN_POINT('Origin',(-0.00169754986071946,-0.0326396682761177,
0.0690860952525217));
#86528=CARTESIAN_POINT('',(0.0131021943802152,-0.0331951640388588,0.0770271360925872));
#86529=CARTESIAN_POINT('Origin',(0.0226535182158981,-0.0331952026560063,
0.0825470620455517));
#86530=CARTESIAN_POINT('',(0.0131334675986233,-0.0331951640388701,0.0769730229166495));
#86531=CARTESIAN_POINT('Ctrl Pts',(0.0131969778446032,-0.0330240426238171,
0.0773535427079646));
#86532=CARTESIAN_POINT('Ctrl Pts',(0.0132411097664658,-0.0329142774063519,
0.0772836544952902));
#86533=CARTESIAN_POINT('Ctrl Pts',(0.0132838189051219,-0.032804347972669,
0.0772128191106915));
#86534=CARTESIAN_POINT('Ctrl Pts',(0.0133250480478717,-0.0326943950436593,
0.0771411257927695));
#86535=CARTESIAN_POINT('Ctrl Pts',(0.0131653502751687,-0.0330240426238171,
0.0772447271170008));
#86536=CARTESIAN_POINT('Ctrl Pts',(0.013207983156252,-0.0329142774063519,
0.0771752746049086));
#86537=CARTESIAN_POINT('Ctrl Pts',(0.0132492015139503,-0.032804347972669,
0.077104906127465));
#86538=CARTESIAN_POINT('Ctrl Pts',(0.013288950061838,-0.0326943950436593,
0.0770337103777238));
#86539=CARTESIAN_POINT('Ctrl Pts',(0.0131337227057343,-0.0330240426238171,
0.077135911526037));
#86540=CARTESIAN_POINT('Ctrl Pts',(0.0131748565460381,-0.0329142774063519,
0.077066894714527));
#86541=CARTESIAN_POINT('Ctrl Pts',(0.0132145841227786,-0.032804347972669,
0.0769969931442386));
#86542=CARTESIAN_POINT('Ctrl Pts',(0.0132528520758044,-0.0326943950436593,
0.0769262949626781));
#86543=CARTESIAN_POINT('Ctrl Pts',(0.0131020951362999,-0.0330240426238171,
0.0770270959350732));
#86544=CARTESIAN_POINT('Ctrl Pts',(0.0131417299358243,-0.0329142774063519,
0.0769585148241454));
#86545=CARTESIAN_POINT('Ctrl Pts',(0.0131799667316069,-0.032804347972669,
0.0768890801610122));
#86546=CARTESIAN_POINT('Ctrl Pts',(0.0132167540897707,-0.0326943950436593,
0.0768188795476324));
#86547=CARTESIAN_POINT('',(0.0132712240560225,-0.0326943950436693,0.0769809637710096));
#86548=CARTESIAN_POINT('Ctrl Pts',(0.013318647079667,-0.0327114338383286,
0.0771522289636724));
#86549=CARTESIAN_POINT('Ctrl Pts',(0.0132814637199353,-0.0327619876830068,
0.0771307398658825));
#86550=CARTESIAN_POINT('Ctrl Pts',(0.0132449363536533,-0.0328131562602515,
0.0771096298814241));
#86551=CARTESIAN_POINT('Ctrl Pts',(0.013173162870366,-0.0329167375858766,
0.077068150375209));
#86552=CARTESIAN_POINT('Ctrl Pts',(0.0131379453517996,-0.0329691088920611,
0.0770477973811317));
#86553=CARTESIAN_POINT('Ctrl Pts',(0.0131033706146114,-0.0330220786163186,
0.0770278158648334));
#86554=CARTESIAN_POINT('Ctrl Pts',(0.0131627816420839,-0.0331951640388604,
0.0769194337992695));
#86555=CARTESIAN_POINT('Ctrl Pts',(0.013220037910288,-0.0330306422010619,
0.0768152557163678));
#86556=CARTESIAN_POINT('Ctrl Pts',(0.0132729394636896,-0.0328657861914645,
0.0767088001911311));
#86557=CARTESIAN_POINT('Ctrl Pts',(0.0131647408170099,-0.0331951640388604,
0.0769189097406946));
#86558=CARTESIAN_POINT('Ctrl Pts',(0.013221986250639,-0.0330306422010619,
0.0768146911531074));
#86559=CARTESIAN_POINT('Ctrl Pts',(0.0132748753046224,-0.0328657861914645,
0.0767081956056004));
#86560=CARTESIAN_POINT('Ctrl Pts',(0.0134911920470379,-0.0331951640388604,
0.0768315874887956));
#86561=CARTESIAN_POINT('Ctrl Pts',(0.0135466321490948,-0.0330306422010619,
0.0767206197313287));
#86562=CARTESIAN_POINT('Ctrl Pts',(0.0135974384638604,-0.0328657861914645,
0.0766074553973127));
#86563=CARTESIAN_POINT('',(0.0134969077207388,-0.0331781648281956,0.0768201164881559));
#86564=CARTESIAN_POINT('',(0.013491192047025,-0.0331951640388588,0.0768315874887981));
#86565=CARTESIAN_POINT('Origin',(-0.00160237718115885,-0.0326412092602053,
0.0701120558230257));
#86566=CARTESIAN_POINT('Ctrl Pts',(0.0134969077191093,-0.033178164828644,
0.076820116489022));
#86567=CARTESIAN_POINT('Ctrl Pts',(0.0134584155350228,-0.0331276811546765,
0.0768009882289008));
#86568=CARTESIAN_POINT('Ctrl Pts',(0.0134206183855283,-0.0330765663497771,
0.0767822053962043));
#86569=CARTESIAN_POINT('Ctrl Pts',(0.0133463817535232,-0.0329730614463557,
0.0767453143027143));
#86570=CARTESIAN_POINT('Ctrl Pts',(0.013309972263362,-0.0329207133374385,
0.0767272209403097));
#86571=CARTESIAN_POINT('Ctrl Pts',(0.0132742441008721,-0.0328677532289399,
0.0767094662152024));
#86572=CARTESIAN_POINT('',(0.0133279664320283,-0.0331951640388702,0.0768752486147549));
#86573=CARTESIAN_POINT('Origin',(0.00812378219310841,-0.0315241814719618,
0.07415));
#86574=CARTESIAN_POINT('',(0.0134969077196362,-0.0332121607144205,0.0768201164868861));
#86575=CARTESIAN_POINT('',(0.0135025988803252,-0.0331951640388587,0.076808633304035));
#86576=CARTESIAN_POINT('Origin',(-0.0016152271314213,-0.0326413666921275,
0.0701555412417527));
#86577=CARTESIAN_POINT('Origin',(-0.000968433154056809,-0.032641209404409,
0.06883635705972));
#86578=CARTESIAN_POINT('Origin',(-0.000941532136059744,-0.0326413667252248,
0.0687998540025973));
#86579=CARTESIAN_POINT('Ctrl Pts',(0.0132005236162736,-0.0337436976235975,
0.0768527433326748));
#86580=CARTESIAN_POINT('Ctrl Pts',(0.0132248324994197,-0.0336723290703325,
0.0768070823509136));
#86581=CARTESIAN_POINT('Ctrl Pts',(0.0132483161528197,-0.033601104548885,
0.0767609915158356));
#86582=CARTESIAN_POINT('Ctrl Pts',(0.0133232948062763,-0.0333736987606857,
0.0766138326095115));
#86583=CARTESIAN_POINT('Ctrl Pts',(0.013389705074288,-0.0331450831799191,
0.0764626135019646));
#86584=CARTESIAN_POINT('Ctrl Pts',(0.0133131825221592,-0.0337436976235975,
0.0766295663380615));
#86585=CARTESIAN_POINT('Ctrl Pts',(0.0133354841175923,-0.0336723290703325,
0.0765828920850269));
#86586=CARTESIAN_POINT('Ctrl Pts',(0.0133569425824548,-0.033601104548885,
0.0765358242473779));
#86587=CARTESIAN_POINT('Ctrl Pts',(0.0134254552100782,-0.0333736987606857,
0.0763855459653781));
#86588=CARTESIAN_POINT('Ctrl Pts',(0.0134852310999934,-0.0331450831799191,
0.076231583680485));
#86589=CARTESIAN_POINT('Ctrl Pts',(0.0133143091112181,-0.0337436976235975,
0.0766273345681153));
#86590=CARTESIAN_POINT('Ctrl Pts',(0.013336590633774,-0.0336723290703325,
0.0765806501823679));
#86591=CARTESIAN_POINT('Ctrl Pts',(0.0133580288467511,-0.033601104548885,
0.0765335725746933));
#86592=CARTESIAN_POINT('Ctrl Pts',(0.0134264768141163,-0.0333736987606857,
0.0763832630989368));
#86593=CARTESIAN_POINT('Ctrl Pts',(0.0134861863602505,-0.0331450831799191,
0.0762292733822702));
#86594=CARTESIAN_POINT('',(0.0133286549178185,-0.0336938721132548,0.0765969215188825));
#86595=CARTESIAN_POINT('',(0.0134247910462803,-0.0333679870047996,0.0763810154949585));
#86596=CARTESIAN_POINT('Ctrl Pts',(0.0133286549178133,-0.0336938721132587,
0.0765969215188945));
#86597=CARTESIAN_POINT('Ctrl Pts',(0.0133382064003763,-0.0336629187933933,
0.0765766044589929));
#86598=CARTESIAN_POINT('Ctrl Pts',(0.0133476358635913,-0.0336319952301071,
0.0765562379692043));
#86599=CARTESIAN_POINT('Ctrl Pts',(0.0133569425824547,-0.0336011045488981,
0.0765358242473785));
#86600=CARTESIAN_POINT('Ctrl Pts',(0.0133802963246631,-0.0335235892595485,
0.0764845992341352));
#86601=CARTESIAN_POINT('Ctrl Pts',(0.0134029185313843,-0.0334458668665602,
0.0764329857278372));
#86602=CARTESIAN_POINT('Ctrl Pts',(0.0134247910419178,-0.0333679869962525,
0.0763810155059306));
#86603=CARTESIAN_POINT('Ctrl Pts',(0.013424808927659,-0.0333679692468938,
0.0763809747805152));
#86604=CARTESIAN_POINT('Ctrl Pts',(0.0134243889027203,-0.0333391895412975,
0.0763808044372332));
#86605=CARTESIAN_POINT('Ctrl Pts',(0.0134240728531347,-0.0333104081127487,
0.0763806797657752));
#86606=CARTESIAN_POINT('Ctrl Pts',(0.0134236524748471,-0.0332532697931203,
0.0763805198937491));
#86607=CARTESIAN_POINT('Ctrl Pts',(0.0134235450558214,-0.0332249169638106,
0.0763804833894381));
#86608=CARTESIAN_POINT('Ctrl Pts',(0.0134235389970316,-0.0331960985432299,
0.0763804883235465));
#86609=CARTESIAN_POINT('Ctrl Pts',(0.013423538926182,-0.0331956312492137,
0.0763804884151774));
#86610=CARTESIAN_POINT('Ctrl Pts',(0.0134235388830291,-0.0331951640388587,
0.0763804885177109));
#86611=CARTESIAN_POINT('',(0.0133750500022088,-0.0331951640388587,0.076495700619667));
#86612=CARTESIAN_POINT('',(0.0133992944426288,-0.0331951640388687,0.0764380945686996));
#86613=CARTESIAN_POINT('',(0.013274244087226,-0.0335216366567648,0.0767094662085707));
#86614=CARTESIAN_POINT('Origin',(-0.00213958756456626,-0.0326434571524483,
0.0704019739310167));
#86615=CARTESIAN_POINT('',(0.0132730274909841,-0.0336938721132327,0.0767088616340682));
#86616=CARTESIAN_POINT('Origin',(0.0230526250392022,-0.0336938867896158,
0.0815687280640452));
#86617=CARTESIAN_POINT('',(0.0133008412044113,-0.0336938721132538,0.0766528915764853));
#86618=CARTESIAN_POINT('Ctrl Pts',(0.0133881196239129,-0.0335235895815172,
0.0770286718143495));
#86619=CARTESIAN_POINT('Ctrl Pts',(0.0134277502090207,-0.0334144449262749,
0.0769561978450879));
#86620=CARTESIAN_POINT('Ctrl Pts',(0.0134659290672072,-0.0333049234473147,
0.0768828218739531));
#86621=CARTESIAN_POINT('Ctrl Pts',(0.0135025988803291,-0.0331951640388587,
0.0768086333040447));
#86622=CARTESIAN_POINT('Ctrl Pts',(0.0133497218051218,-0.0335235895815172,
0.0769220567122362));
#86623=CARTESIAN_POINT('Ctrl Pts',(0.0133878846234432,-0.0334144449262749,
0.0768501113645486));
#86624=CARTESIAN_POINT('Ctrl Pts',(0.0134246049494809,-0.0333049234473147,
0.0767772949452671));
#86625=CARTESIAN_POINT('Ctrl Pts',(0.0134598273949193,-0.0331951640388587,
0.0767036963109375));
#86626=CARTESIAN_POINT('Ctrl Pts',(0.0133113239863307,-0.0335235895815172,
0.0768154416101229));
#86627=CARTESIAN_POINT('Ctrl Pts',(0.0133480190378656,-0.0334144449262749,
0.0767440248840093));
#86628=CARTESIAN_POINT('Ctrl Pts',(0.0133832808317546,-0.0333049234473147,
0.0766717680165811));
#86629=CARTESIAN_POINT('Ctrl Pts',(0.0134170559095094,-0.0331951640388587,
0.0765987593178303));
#86630=CARTESIAN_POINT('Ctrl Pts',(0.0132729261675395,-0.0335235895815172,
0.0767088265080096));
#86631=CARTESIAN_POINT('Ctrl Pts',(0.0133081534522881,-0.0334144449262749,
0.07663793840347));
#86632=CARTESIAN_POINT('Ctrl Pts',(0.0133419567140284,-0.0333049234473147,
0.0765662410878951));
#86633=CARTESIAN_POINT('Ctrl Pts',(0.0133742844240995,-0.0331951640388587,
0.0764938223247231));
#86634=CARTESIAN_POINT('',(0.013438824441277,-0.0331951640388687,0.076652166961861));
#86635=CARTESIAN_POINT('Ctrl Pts',(0.0134969077168258,-0.033212160714594,
0.0768201164854868));
#86636=CARTESIAN_POINT('Ctrl Pts',(0.0134584802918743,-0.0332625444108826,
0.0768010203932022));
#86637=CARTESIAN_POINT('Ctrl Pts',(0.0134207150317549,-0.0333135300744947,
0.0767822533565532));
#86638=CARTESIAN_POINT('Ctrl Pts',(0.013346478863352,-0.0334167203140538,
0.0767453624973694));
#86639=CARTESIAN_POINT('Ctrl Pts',(0.0133100367075453,-0.0334688847587207,
0.0767272529630664));
#86640=CARTESIAN_POINT('Ctrl Pts',(0.0132742440866642,-0.0335216366562262,
0.0767094662081039));
#86641=CARTESIAN_POINT('Ctrl Pts',(0.0133267329643754,-0.0336938721132584,
0.0765975674098968));
#86642=CARTESIAN_POINT('Ctrl Pts',(0.0133410593886174,-0.0336474569765055,
0.076567112812504));
#86643=CARTESIAN_POINT('Ctrl Pts',(0.0133550283216894,-0.033601104548885,
0.0765364925929956));
#86644=CARTESIAN_POINT('Ctrl Pts',(0.0133903944485611,-0.0334837508592655,
0.0764589692372461));
#86645=CARTESIAN_POINT('Ctrl Pts',(0.0134234478674729,-0.0333660264659096,
0.0763804319523758));
#86646=CARTESIAN_POINT('Ctrl Pts',(0.0133286549178037,-0.0336938721132584,
0.0765969215189137));
#86647=CARTESIAN_POINT('Ctrl Pts',(0.0133429775614315,-0.0336474569765055,
0.0765664556716898));
#86648=CARTESIAN_POINT('Ctrl Pts',(0.0133569425824548,-0.033601104548885,
0.0765358242473779));
#86649=CARTESIAN_POINT('Ctrl Pts',(0.0133922988049186,-0.0334837508592655,
0.0764582725236422));
#86650=CARTESIAN_POINT('Ctrl Pts',(0.0134253414831697,-0.0333660264659096,
0.0763797071767308));
#86651=CARTESIAN_POINT('Ctrl Pts',(0.0136509009056519,-0.0336938721132584,
0.0764886276472783));
#86652=CARTESIAN_POINT('Ctrl Pts',(0.0136645896693132,-0.0336474569765055,
0.0764562755873546));
#86653=CARTESIAN_POINT('Ctrl Pts',(0.0136778987733026,-0.033601104548885,
0.0764237654999526));
#86654=CARTESIAN_POINT('Ctrl Pts',(0.0137115943646418,-0.0334837508592655,
0.0763414574332058));
#86655=CARTESIAN_POINT('Ctrl Pts',(0.0137428362006902,-0.0333660264659096,
0.0762581870398619));
#86656=CARTESIAN_POINT('',(0.0136539630869382,-0.0336769361243754,0.0764774662793518));
#86657=CARTESIAN_POINT('',(0.0136489789613314,-0.0336938721132327,0.0764892735351852));
#86658=CARTESIAN_POINT('Ctrl Pts',(0.0136539630869382,-0.0336769361243754,
0.0764774662793518));
#86659=CARTESIAN_POINT('Ctrl Pts',(0.0136531344389964,-0.0336797586670078,
0.0764794351899461));
#86660=CARTESIAN_POINT('Ctrl Pts',(0.013652304770908,-0.0336825812712947,
0.0764814035835397));
#86661=CARTESIAN_POINT('Ctrl Pts',(0.013650643398562,-0.0336882265906967,
0.076485339328277));
#86662=CARTESIAN_POINT('Ctrl Pts',(0.0136498116943304,-0.0336910493058177,
0.0764873066794294));
#86663=CARTESIAN_POINT('Ctrl Pts',(0.0136489789613424,-0.0336938721132368,
0.0764892735351839));
#86664=CARTESIAN_POINT('Ctrl Pts',(0.0136539630869382,-0.0336769361243754,
0.0764774662793518));
#86665=CARTESIAN_POINT('Ctrl Pts',(0.0136153321799088,-0.0336279018525342,
0.0764612078358799));
#86666=CARTESIAN_POINT('Ctrl Pts',(0.0135761455183466,-0.0335767826051548,
0.076444715494104));
#86667=CARTESIAN_POINT('Ctrl Pts',(0.0134993621726489,-0.0334733172106852,
0.0764123999783265));
#86668=CARTESIAN_POINT('Ctrl Pts',(0.0134617138840055,-0.0334209631477636,
0.0763965550857312));
#86669=CARTESIAN_POINT('Ctrl Pts',(0.013424791040563,-0.0333679869844681,
0.0763810155085093));
#86670=CARTESIAN_POINT('',(0.013488816939585,-0.0336938721132538,0.0765430975270439));
#86671=CARTESIAN_POINT('Origin',(0.00812378219310841,-0.0315241814719618,
0.07415));
#86672=CARTESIAN_POINT('',(0.0136539630857512,-0.0337108120655378,0.0764774662788552));
#86673=CARTESIAN_POINT('',(0.0136589219806651,-0.0336938721132327,0.0764656484042733));
#86674=CARTESIAN_POINT('Origin',(-0.000992580517952669,-0.0345562525600667,
0.0691006776982423));
#86675=CARTESIAN_POINT('Ctrl Pts',(0.0136589219806746,-0.0336938721132384,
0.0764656484042855));
#86676=CARTESIAN_POINT('Ctrl Pts',(0.0136580976547706,-0.0336910492956357,
0.0764676188066577));
#86677=CARTESIAN_POINT('Ctrl Pts',(0.0136572722599229,-0.0336882265856054,
0.0764695888090337));
#86678=CARTESIAN_POINT('Ctrl Pts',(0.0136556192999888,-0.0336825812712732,
0.0764735280901084));
#86679=CARTESIAN_POINT('Ctrl Pts',(0.0136547917348769,-0.033679758666997,
0.0764754973687649));
#86680=CARTESIAN_POINT('Ctrl Pts',(0.0136539630869382,-0.0336769361243754,
0.0764774662793518));
#86681=CARTESIAN_POINT('Origin',(-0.00185964346467866,-0.0345562522792228,
0.0711608663359108));
#86682=CARTESIAN_POINT('Ctrl Pts',(0.0133601911283327,-0.034243627687391,
0.0765286858689418));
#86683=CARTESIAN_POINT('Ctrl Pts',(0.0134499047448276,-0.033943005420181,
0.0763311914502129));
#86684=CARTESIAN_POINT('Ctrl Pts',(0.0135244874055163,-0.0336441434784052,
0.076127500495239));
#86685=CARTESIAN_POINT('Ctrl Pts',(0.013458616391475,-0.034243627687391,
0.0762988762356028));
#86686=CARTESIAN_POINT('Ctrl Pts',(0.0135396625947644,-0.033943005420181,
0.0760976696468787));
#86687=CARTESIAN_POINT('Ctrl Pts',(0.0136053228496057,-0.0336441434784052,
0.0758909299328715));
#86688=CARTESIAN_POINT('Ctrl Pts',(0.0134596006441064,-0.034243627687391,
0.0762965781392694));
#86689=CARTESIAN_POINT('Ctrl Pts',(0.0135405601732637,-0.033943005420181,
0.0760953344288453));
#86690=CARTESIAN_POINT('Ctrl Pts',(0.0136061312040465,-0.0336441434784052,
0.0758885642272479));
#86691=CARTESIAN_POINT('',(0.0134720277638486,-0.0341934961088741,0.0762652764157573));
#86692=CARTESIAN_POINT('',(0.0135544173338659,-0.033866421286606,0.0760437600087977));
#86693=CARTESIAN_POINT('Origin',(-0.00189517546600665,-0.0345610720406586,
0.0696394022350303));
#86694=CARTESIAN_POINT('Origin',(0.0239091527297719,-0.033693800507295,
0.0796546019243239));
#86695=CARTESIAN_POINT('',(0.0135119755852947,-0.0336938721132327,0.0761613420813975));
#86696=CARTESIAN_POINT('',(0.0135325550709807,-0.0336938721132427,0.0761023273818038));
#86697=CARTESIAN_POINT('',(0.013424791040561,-0.0340203938281605,0.0763810155085142));
#86698=CARTESIAN_POINT('Origin',(-0.00163881785010329,-0.0345589643243111,
0.0692321952771803));
#86699=CARTESIAN_POINT('',(0.0134235388830286,-0.034193496108874,0.0763804885177123));
#86700=CARTESIAN_POINT('Origin',(0.0235801278517751,-0.0341934220717693,
0.0806550550213423));
#86701=CARTESIAN_POINT('',(0.0134477833234486,-0.0341934961088841,0.0763228824667448));
#86702=CARTESIAN_POINT('Ctrl Pts',(0.0135584837958485,-0.0340223579322396,
0.0766924434092575));
#86703=CARTESIAN_POINT('Ctrl Pts',(0.013593550721433,-0.0339125849573575,
0.0766174846998589));
#86704=CARTESIAN_POINT('Ctrl Pts',(0.0136270415347902,-0.0338030433565231,
0.0765418528592022));
#86705=CARTESIAN_POINT('Ctrl Pts',(0.0136589219806698,-0.0336938721132327,
0.076465648404283));
#86706=CARTESIAN_POINT('Ctrl Pts',(0.0135134673632818,-0.0340223579322396,
0.0765884496564168));
#86707=CARTESIAN_POINT('Ctrl Pts',(0.0135470999437875,-0.0339125849573575,
0.0765141118410311));
#86708=CARTESIAN_POINT('Ctrl Pts',(0.013579170271027,-0.0338030433565231,
0.0764391301457024));
#86709=CARTESIAN_POINT('Ctrl Pts',(0.0136096458326096,-0.0336938721132327,
0.0763636040949694));
#86710=CARTESIAN_POINT('Ctrl Pts',(0.0134684509307151,-0.0340223579322396,
0.0764844559035761));
#86711=CARTESIAN_POINT('Ctrl Pts',(0.013500649166142,-0.0339125849573575,
0.0764107389822032));
#86712=CARTESIAN_POINT('Ctrl Pts',(0.0135312990072637,-0.0338030433565231,
0.0763364074322026));
#86713=CARTESIAN_POINT('Ctrl Pts',(0.0135603696845494,-0.0336938721132327,
0.0762615597856559));
#86714=CARTESIAN_POINT('Ctrl Pts',(0.0134234344981484,-0.0340223579322396,
0.0763804621507353));
#86715=CARTESIAN_POINT('Ctrl Pts',(0.0134541983884965,-0.0339125849573575,
0.0763073661233754));
#86716=CARTESIAN_POINT('Ctrl Pts',(0.0134834277435004,-0.0338030433565231,
0.0762336847187027));
#86717=CARTESIAN_POINT('Ctrl Pts',(0.0135110935364892,-0.0336938721132327,
0.0761595154763423));
#86718=CARTESIAN_POINT('',(0.0135854487829899,-0.0336938721132427,0.0763134952428453));
#86719=CARTESIAN_POINT('Ctrl Pts',(0.0136539630824248,-0.0337108120662652,
0.0764774662774524));
#86720=CARTESIAN_POINT('Ctrl Pts',(0.0136143308050121,-0.0337611408993406,
0.0764607863910214));
#86721=CARTESIAN_POINT('Ctrl Pts',(0.0135754217287318,-0.0338121088779513,
0.0764444108755108));
#86722=CARTESIAN_POINT('Ctrl Pts',(0.0134990145326359,-0.0339153382773231,
0.0764122536683909));
#86723=CARTESIAN_POINT('Ctrl Pts',(0.0134615487379387,-0.0339675558473106,
0.0763964855813318));
#86724=CARTESIAN_POINT('Ctrl Pts',(0.0134247910405263,-0.0340203938281304,
0.076381015508494));
#86725=CARTESIAN_POINT('Ctrl Pts',(0.0134701496332366,-0.0341934961088741,
0.0762660419268864));
#86726=CARTESIAN_POINT('Ctrl Pts',(0.0135138971330321,-0.0340287516182428,
0.0761555099919934));
#86727=CARTESIAN_POINT('Ctrl Pts',(0.0135530388827007,-0.0338644633275951,
0.0760432643871688));
#86728=CARTESIAN_POINT('Ctrl Pts',(0.0134720277638485,-0.0341934961088741,
0.0762652764157574));
#86729=CARTESIAN_POINT('Ctrl Pts',(0.0135157594373044,-0.0340287516182428,
0.0761547056519936));
#86730=CARTESIAN_POINT('Ctrl Pts',(0.0135548837693301,-0.0338644633275951,
0.0760424219055914));
#86731=CARTESIAN_POINT('Ctrl Pts',(0.0137849604482274,-0.0341934961088741,
0.0761377275376366));
#86732=CARTESIAN_POINT('Ctrl Pts',(0.0138260551491127,-0.0340287516182428,
0.0760206871371553));
#86733=CARTESIAN_POINT('Ctrl Pts',(0.0138622773668167,-0.0338644633275951,
0.0759020482702934));
#86734=CARTESIAN_POINT('',(0.0137891933540578,-0.0341764758832445,0.0761256306254384));
#86735=CARTESIAN_POINT('',(0.0137849604482159,-0.0341934961088741,0.0761377275376413));
#86736=CARTESIAN_POINT('Origin',(-0.00167659701415602,-0.0345621027032399,
0.0701900890989704));
#86737=CARTESIAN_POINT('Ctrl Pts',(0.0137891933527088,-0.0341764758837555,
0.076125630626661));
#86738=CARTESIAN_POINT('Ctrl Pts',(0.013748662640142,-0.0341260050040858,
0.0761114968537859));
#86739=CARTESIAN_POINT('Ctrl Pts',(0.0137088364343957,-0.0340749269148957,
0.0760976087953033));
#86740=CARTESIAN_POINT('Ctrl Pts',(0.0136305622312432,-0.0339715436308062,
0.0760703131705489));
#86741=CARTESIAN_POINT('Ctrl Pts',(0.0135921439311717,-0.0339192778238088,
0.076056915953935));
#86742=CARTESIAN_POINT('Ctrl Pts',(0.0135544173348583,-0.0338664212855904,
0.0760437600100322));
#86743=CARTESIAN_POINT('',(0.0136284941060423,-0.0341934961088841,0.0762015019767093));
#86744=CARTESIAN_POINT('Origin',(0.00812378219310841,-0.0315241814719618,
0.07415));
#86745=CARTESIAN_POINT('',(0.0137891933536377,-0.0342105180190519,0.0761256306244011));
#86746=CARTESIAN_POINT('',(0.0137934004130283,-0.0341934961088739,0.076113524698179));
#86747=CARTESIAN_POINT('Origin',(-0.00169636026059117,-0.0345621720468637,
0.0702308784965533));
#86748=CARTESIAN_POINT('Origin',(-0.0020138373063663,-0.0345621029228079,
0.0711571729676889));
#86749=CARTESIAN_POINT('Origin',(-0.00200394991402754,-0.0345621724125657,
0.0711129398881292));
#86750=CARTESIAN_POINT('Ctrl Pts',(0.0135114816743752,-0.0346945769586965,
0.0761627584435455));
#86751=CARTESIAN_POINT('Ctrl Pts',(0.0135536397058397,-0.0345275153362944,
0.0760499109207932));
#86752=CARTESIAN_POINT('Ctrl Pts',(0.0135922596908091,-0.0343603235965185,
0.0759357083786057));
#86753=CARTESIAN_POINT('Ctrl Pts',(0.0136272324285107,-0.034193496108874,
0.0758204902750261));
#86754=CARTESIAN_POINT('Ctrl Pts',(0.0135390856256502,-0.0346945769586965,
0.0760836000564988));
#86755=CARTESIAN_POINT('Ctrl Pts',(0.0135795856530047,-0.0345275153362944,
0.075970174357935));
#86756=CARTESIAN_POINT('Ctrl Pts',(0.0136165290219222,-0.0343603235965185,
0.0758554456330932));
#86757=CARTESIAN_POINT('Ctrl Pts',(0.0136498115134455,-0.034193496108874,
0.0757397548225325));
#86758=CARTESIAN_POINT('Ctrl Pts',(0.0135666895769253,-0.0346945769586965,
0.0760044416694547));
#86759=CARTESIAN_POINT('Ctrl Pts',(0.0136055316001701,-0.0345275153362944,
0.0758904377950791));
#86760=CARTESIAN_POINT('Ctrl Pts',(0.0136407983530358,-0.0343603235965185,
0.075775182887582));
#86761=CARTESIAN_POINT('Ctrl Pts',(0.0136723905983807,-0.034193496108874,
0.0756590193700381));
#86762=CARTESIAN_POINT('Ctrl Pts',(0.0135942935282001,-0.0346945769586965,
0.0759252832824053));
#86763=CARTESIAN_POINT('Ctrl Pts',(0.0136314775473348,-0.0345275153362944,
0.0758107012322185));
#86764=CARTESIAN_POINT('Ctrl Pts',(0.0136650676841485,-0.0343603235965185,
0.0756949201420684));
#86765=CARTESIAN_POINT('Ctrl Pts',(0.0136949696833151,-0.034193496108874,
0.0755782839175453));
#86766=CARTESIAN_POINT('',(0.0135942935280005,-0.0346945769586966,0.0759252832829772));
#86767=CARTESIAN_POINT('',(0.013662611390378,-0.0343667727831535,0.0756990307046681));
#86768=CARTESIAN_POINT('Origin',(-0.00245380659277795,-0.0345626457059982,
0.0709097344829956));
#86769=CARTESIAN_POINT('Origin',(0.0243063813591365,-0.0341934771029176,
0.0786757428621937));
#86770=CARTESIAN_POINT('',(0.0136276364306931,-0.034193496108874,0.0758190456948274));
#86771=CARTESIAN_POINT('',(0.013644469743817,-0.034193496108884,0.0757588552506655));
#86772=CARTESIAN_POINT('',(0.0135544173333597,-0.0345211942962613,0.076043760009476));
#86773=CARTESIAN_POINT('Origin',(-0.00229234993127616,-0.0345625596119914,
0.0704568299268693));
#86774=CARTESIAN_POINT('',(0.0135531345566467,-0.0346945769586887,0.07604331268219));
#86775=CARTESIAN_POINT('Origin',(0.0239997435906502,-0.0346945685853902,
0.0796862338863267));
#86776=CARTESIAN_POINT('',(0.0135737140423336,-0.0346945769587026,0.0759842979825937));
#86777=CARTESIAN_POINT('Ctrl Pts',(0.0137074013484012,-0.0345231616327841,
0.0763461778454283));
#86778=CARTESIAN_POINT('Ctrl Pts',(0.0137376725680293,-0.0344132092796987,
0.0762692155164796));
#86779=CARTESIAN_POINT('Ctrl Pts',(0.0137663503207344,-0.0343032738558979,
0.0761916310221329));
#86780=CARTESIAN_POINT('Ctrl Pts',(0.0137934004130336,-0.034193496108874,
0.0761135246981883));
#86781=CARTESIAN_POINT('Ctrl Pts',(0.0136559439950633,-0.0345231616327841,
0.0762452160857041));
#86782=CARTESIAN_POINT('Ctrl Pts',(0.0136848235989764,-0.0344132092796987,
0.076168963023925));
#86783=CARTESIAN_POINT('Ctrl Pts',(0.0137121244783994,-0.0343032738558979,
0.0760921165446263));
#86784=CARTESIAN_POINT('Ctrl Pts',(0.0137378141795643,-0.034193496108874,
0.0760147759929418));
#86785=CARTESIAN_POINT('Ctrl Pts',(0.0136044866417254,-0.0345231616327841,
0.0761442543259799));
#86786=CARTESIAN_POINT('Ctrl Pts',(0.0136319746299235,-0.0344132092796987,
0.0760687105313704));
#86787=CARTESIAN_POINT('Ctrl Pts',(0.0136578986360644,-0.0343032738558979,
0.0759926020671198));
#86788=CARTESIAN_POINT('Ctrl Pts',(0.013682227946095,-0.034193496108874,
0.0759160272876954));
#86789=CARTESIAN_POINT('Ctrl Pts',(0.0135530292883875,-0.0345231616327841,
0.0760432925662557));
#86790=CARTESIAN_POINT('Ctrl Pts',(0.0135791256608706,-0.0344132092796987,
0.0759684580388158));
#86791=CARTESIAN_POINT('Ctrl Pts',(0.0136036727937294,-0.0343032738558979,
0.0758930875896132));
#86792=CARTESIAN_POINT('Ctrl Pts',(0.0136266417126257,-0.034193496108874,
0.0758172785824489));
#86793=CARTESIAN_POINT('',(0.0137105184218707,-0.0341934961088839,0.0759662851965132));
#86794=CARTESIAN_POINT('Ctrl Pts',(0.0137891933503703,-0.0342105180195351,
0.0761256306232581));
#86795=CARTESIAN_POINT('Ctrl Pts',(0.0137486170779876,-0.0342610556240237,
0.0761114809483146));
#86796=CARTESIAN_POINT('Ctrl Pts',(0.0137087689258297,-0.0343122189868,
0.0760975851819707));
#86797=CARTESIAN_POINT('Ctrl Pts',(0.0136304939315549,-0.0344158119695084,
0.0760702892856214));
#86798=CARTESIAN_POINT('Ctrl Pts',(0.0135920991047184,-0.0344681990449961,
0.0760569003199194));
#86799=CARTESIAN_POINT('Ctrl Pts',(0.0135544173333305,-0.0345211942962363,
0.0760437600094589));
#86800=CARTESIAN_POINT('Ctrl Pts',(0.0135924676174683,-0.0346945769586932,
0.075926164996412));
#86801=CARTESIAN_POINT('Ctrl Pts',(0.0136291885719951,-0.034529677707698,
0.075813103794781));
#86802=CARTESIAN_POINT('Ctrl Pts',(0.0136612052255674,-0.034364806625142,
0.0756986214917398));
#86803=CARTESIAN_POINT('Ctrl Pts',(0.0135942935279976,-0.0346945769586932,
0.0759252832829858));
#86804=CARTESIAN_POINT('Ctrl Pts',(0.0136309962537231,-0.034529677707698,
0.0758121843319466));
#86805=CARTESIAN_POINT('Ctrl Pts',(0.0136629931338528,-0.034364806625142,
0.0756976650651667));
#86806=CARTESIAN_POINT('Ctrl Pts',(0.0138985998508835,-0.0346945769586932,
0.075778336887611));
#86807=CARTESIAN_POINT('Ctrl Pts',(0.0139322645638606,-0.034529677707698,
0.0756589466186663));
#86808=CARTESIAN_POINT('Ctrl Pts',(0.0139609660012355,-0.034364806625142,
0.0755382669736921));
#86809=CARTESIAN_POINT('',(0.013902064832892,-0.0346775396665028,0.0757659980595097));
#86810=CARTESIAN_POINT('',(0.0138985998508739,-0.0346945769586886,0.0757783368876127));
#86811=CARTESIAN_POINT('Origin',(-0.00212650686149166,-0.0345626617939533,
0.0714419038548436));
#86812=CARTESIAN_POINT('Ctrl Pts',(0.0139020648315447,-0.0346775396670096,
0.0757659980607406));
#86813=CARTESIAN_POINT('Ctrl Pts',(0.0138606940728663,-0.0346269749928189,
0.0757544280160451));
#86814=CARTESIAN_POINT('Ctrl Pts',(0.0138200585552095,-0.0345757902890797,
0.0757430636314537));
#86815=CARTESIAN_POINT('Ctrl Pts',(0.0137402245826297,-0.034472168108813,
0.0757207366572577));
#86816=CARTESIAN_POINT('Ctrl Pts',(0.0137010574279038,-0.0344197714290103,
0.0757097828154504));
#86817=CARTESIAN_POINT('Ctrl Pts',(0.0136626113904136,-0.0343667727830759,
0.0756990307049232));
#86818=CARTESIAN_POINT('',(0.0137464466894472,-0.0346945769587026,0.075851810085305));
#86819=CARTESIAN_POINT('Origin',(0.00812378219310841,-0.0315241814719618,
0.07415));
#86820=CARTESIAN_POINT('',(0.0139020648319539,-0.0347116136489593,0.0757659980584807));
#86821=CARTESIAN_POINT('',(0.0139055034524797,-0.0346945769586885,0.0757536518571501));
#86822=CARTESIAN_POINT('Origin',(-0.00213689806546748,-0.0345626700684398,
0.0714860074050638));
#86823=CARTESIAN_POINT('Origin',(-0.0020442441421476,-0.0345626620276843,
0.0711477565467771));
#86824=CARTESIAN_POINT('Origin',(-0.00203024708750737,-0.0345626702762116,
0.0711046614002162));
#86825=CARTESIAN_POINT('Ctrl Pts',(0.0136163568087717,-0.0352450361874067,
0.0758559855559169));
#86826=CARTESIAN_POINT('Ctrl Pts',(0.0136806991098211,-0.0349452760959492,
0.0756488297050176));
#86827=CARTESIAN_POINT('Ctrl Pts',(0.0137292547948641,-0.034644428984174,
0.0754374158367021));
#86828=CARTESIAN_POINT('Ctrl Pts',(0.0136170521239378,-0.0352450361874067,
0.0758535581783566));
#86829=CARTESIAN_POINT('Ctrl Pts',(0.0136813028749403,-0.0349452760959492,
0.0756463761032156));
#86830=CARTESIAN_POINT('Ctrl Pts',(0.0137297652947032,-0.034644428984174,
0.0754349429810827));
#86831=CARTESIAN_POINT('Ctrl Pts',(0.0136858952096946,-0.0352450361874067,
0.0756132237664564));
#86832=CARTESIAN_POINT('Ctrl Pts',(0.0137410815996131,-0.0349452760959492,
0.0754034452317301));
#86833=CARTESIAN_POINT('Ctrl Pts',(0.0137803098332277,-0.034644428984174,
0.0751901057910455));
#86834=CARTESIAN_POINT('Ctrl Pts',(0.0136865836405522,-0.0352450361874067,
0.0756108204223374));
#86835=CARTESIAN_POINT('Ctrl Pts',(0.0137416793868598,-0.0349452760959492,
0.0754010159230152));
#86836=CARTESIAN_POINT('Ctrl Pts',(0.013780815278613,-0.034644428984174,
0.0751876574191451));
#86837=CARTESIAN_POINT('',(0.0136949639463645,-0.0351951634053355,0.0755783158525603));
#86838=CARTESIAN_POINT('',(0.0137489462188087,-0.0348678972925388,0.07534818808372));
#86839=CARTESIAN_POINT('Origin',(-0.00272055362522045,-0.0345636767885179,
0.072271462480856));
#86840=CARTESIAN_POINT('Origin',(0.0245563350308239,-0.0346946199340772,
0.0776502168342705));
#86841=CARTESIAN_POINT('',(0.0137215760736043,-0.0346945769330289,0.0754701623649035));
#86842=CARTESIAN_POINT('',(0.0137345967829202,-0.0346945769458128,0.0754090337119125));
#86843=CARTESIAN_POINT('',(0.0136626113902745,-0.0350221583435276,0.0756990307048674));
#86844=CARTESIAN_POINT('Origin',(-0.00266134073650105,-0.0345628458720691,
0.0717943490485694));
#86845=CARTESIAN_POINT('',(0.0136614193974968,-0.0351951360298762,0.0756987004837829));
#86846=CARTESIAN_POINT('Origin',(0.0242732133076599,-0.0351951838366722,
0.0786664730246426));
#86847=CARTESIAN_POINT('',(0.013694969683261,-0.0351951371328746,0.0755782839181704));
#86848=CARTESIAN_POINT('Ctrl Pts',(0.0138342827941664,-0.0350241211494343,
0.0759912449281452));
#86849=CARTESIAN_POINT('Ctrl Pts',(0.0138596451881117,-0.0349144232818962,
0.075912585123762));
#86850=CARTESIAN_POINT('Ctrl Pts',(0.0138833968083085,-0.0348045283579412,
0.0758333539788886));
#86851=CARTESIAN_POINT('Ctrl Pts',(0.0139055034554557,-0.0346945769439158,
0.0757536518464505));
#86852=CARTESIAN_POINT('Ctrl Pts',(0.0137765875104734,-0.0350241211494343,
0.0758937134150676));
#86853=CARTESIAN_POINT('Ctrl Pts',(0.0138006064478156,-0.0349144232818962,
0.0758158483395613));
#86854=CARTESIAN_POINT('Ctrl Pts',(0.0138230302348995,-0.0348045283579412,
0.0757374401694563));
#86855=CARTESIAN_POINT('Ctrl Pts',(0.013843826412436,-0.0346945769439158,
0.0756585882668422));
#86856=CARTESIAN_POINT('Ctrl Pts',(0.0137188922267805,-0.0350241211494342,
0.0757961819019901));
#86857=CARTESIAN_POINT('Ctrl Pts',(0.0137415677075195,-0.0349144232818962,
0.0757191115553607));
#86858=CARTESIAN_POINT('Ctrl Pts',(0.0137626636614904,-0.0348045283579412,
0.075641526360024));
#86859=CARTESIAN_POINT('Ctrl Pts',(0.0137821493694162,-0.0346945769439158,
0.0755635246872338));
#86860=CARTESIAN_POINT('Ctrl Pts',(0.0136611969430875,-0.0350241211494342,
0.0756986503889125));
#86861=CARTESIAN_POINT('Ctrl Pts',(0.0136825289672234,-0.0349144232818962,
0.07562237477116));
#86862=CARTESIAN_POINT('Ctrl Pts',(0.0137022970880814,-0.0348045283579412,
0.0755456125505917));
#86863=CARTESIAN_POINT('Ctrl Pts',(0.0137204723263965,-0.0346945769439158,
0.0754684611076255));
#86864=CARTESIAN_POINT('',(0.0138135397630608,-0.0346945769458128,0.0756119071113357));
#86865=CARTESIAN_POINT('Ctrl Pts',(0.0139020648287818,-0.0347116136492756,
0.0757659980575896));
#86866=CARTESIAN_POINT('Ctrl Pts',(0.0138607105028954,-0.0347621546531205,
0.0757544325952337));
#86867=CARTESIAN_POINT('Ctrl Pts',(0.0138200832978061,-0.0348133084094813,
0.0757430704849581));
#86868=CARTESIAN_POINT('Ctrl Pts',(0.0137402492227238,-0.0349168561544569,
0.0757207434860214));
#86869=CARTESIAN_POINT('Ctrl Pts',(0.013701074019108,-0.0349692089015919,
0.0757097874534179));
#86870=CARTESIAN_POINT('Ctrl Pts',(0.0136626113902445,-0.0350221583434999,
0.0756990307048384));
#86871=CARTESIAN_POINT('Ctrl Pts',(0.0136936947742535,-0.0351951371254986,
0.0755790015719479));
#86872=CARTESIAN_POINT('Ctrl Pts',(0.0137232384851682,-0.0350307338980977,
0.0754638471240117));
#86873=CARTESIAN_POINT('Ctrl Pts',(0.0137479974935673,-0.0348659306897824,
0.0753475700014242));
#86874=CARTESIAN_POINT('Ctrl Pts',(0.0136949696831463,-0.0351951371254986,
0.0755782839181499));
#86875=CARTESIAN_POINT('Ctrl Pts',(0.013724498557019,-0.0350307338980977,
0.0754631031122722));
#86876=CARTESIAN_POINT('Ctrl Pts',(0.0137492416516522,-0.0348659306897824,
0.075346800267497));
#86877=CARTESIAN_POINT('Ctrl Pts',(0.0139086457423704,-0.0351951371254986,
0.0754580043936221));
#86878=CARTESIAN_POINT('Ctrl Pts',(0.0139356879125394,-0.0350307338980977,
0.0753384059692847));
#86879=CARTESIAN_POINT('Ctrl Pts',(0.0139577638434049,-0.0348659306897824,
0.0752177920590261));
#86880=CARTESIAN_POINT('Origin',(0.0189504380659447,-0.0308609197410153,
0.076456131873351));
#86881=CARTESIAN_POINT('',(0.0137881276272136,-0.0351951371254986,0.0755258447573984));
#86882=CARTESIAN_POINT('Origin',(0.0071487010936216,-0.0351840467441095,
0.0740870516087876));
#86883=CARTESIAN_POINT('Origin',(0.0199662307642446,-0.0352322614040111,
0.0758599766870974));
#86884=CARTESIAN_POINT('',(0.0137934500244489,-0.0351951142564686,0.0751157542470464));
#86885=CARTESIAN_POINT('',(0.0138117372268754,-0.0351951372916787,0.0749924176718502));
#86886=CARTESIAN_POINT('Origin',(0.00798966007799802,-0.0352875122926663,
0.073836919555656));
#86887=CARTESIAN_POINT('Origin',(0.00562380347660242,-0.0298325076522691,
0.0812242700469244));
#86888=CARTESIAN_POINT('Origin',(0.0153427804016229,-0.0338732925202731,
0.0784084029538063));
#86889=CARTESIAN_POINT('Ctrl Pts',(0.0121427474513236,-0.0321934096636942,
0.0782641285831352));
#86890=CARTESIAN_POINT('Ctrl Pts',(0.0122163883937301,-0.0320508460845378,
0.078192191018926));
#86891=CARTESIAN_POINT('Ctrl Pts',(0.0122880409902187,-0.0319086045665173,
0.0781183291090622));
#86892=CARTESIAN_POINT('Ctrl Pts',(0.0123575640531126,-0.0317669892871038,
0.0780427145925674));
#86893=CARTESIAN_POINT('Ctrl Pts',(0.0122014382915331,-0.0321934096636942,
0.0782042468839004));
#86894=CARTESIAN_POINT('Ctrl Pts',(0.0122740073800401,-0.0320508460845378,
0.0781312587816013));
#86895=CARTESIAN_POINT('Ctrl Pts',(0.012344560704925,-0.0319086045665173,
0.0780563759243559));
#86896=CARTESIAN_POINT('Ctrl Pts',(0.0124129596264122,-0.0317669892871038,
0.0779797720546076));
#86897=CARTESIAN_POINT('Ctrl Pts',(0.0122601291317424,-0.0321934096636942,
0.0781443651846656));
#86898=CARTESIAN_POINT('Ctrl Pts',(0.0123316263663501,-0.0320508460845379,
0.0780703265442765));
#86899=CARTESIAN_POINT('Ctrl Pts',(0.0124010804196314,-0.0319086045665173,
0.0779944227396497));
#86900=CARTESIAN_POINT('Ctrl Pts',(0.0124683551997119,-0.0317669892871038,
0.0779168295166477));
#86901=CARTESIAN_POINT('Ctrl Pts',(0.0123188199719519,-0.0321934096636942,
0.0780844834854308));
#86902=CARTESIAN_POINT('Ctrl Pts',(0.0123892453526602,-0.0320508460845379,
0.0780093943069517));
#86903=CARTESIAN_POINT('Ctrl Pts',(0.0124576001343378,-0.0319086045665173,
0.0779324695549435));
#86904=CARTESIAN_POINT('Ctrl Pts',(0.0125237507730115,-0.0317669892871038,
0.0778538869786879));
#86905=CARTESIAN_POINT('',(0.0123177699812209,-0.0321934096636942,0.0780855547808618));
#86906=CARTESIAN_POINT('',(0.0124759194928693,-0.0318665617511361,0.0779099236579099));
#86907=CARTESIAN_POINT('Origin',(0.000561737037247611,-0.0326371944419988,
0.0662106402855537));
#86908=CARTESIAN_POINT('Origin',(0.0207704093038825,-0.0316939261509443,
0.0850757473283274));
#86909=CARTESIAN_POINT('',(0.0122313956286931,-0.0320197221621762,0.0781755559902131));
#86910=CARTESIAN_POINT('Ctrl Pts',(0.0122315545130972,-0.0320197392094677,
0.0781754612768234));
#86911=CARTESIAN_POINT('Ctrl Pts',(0.0122520373207006,-0.0319792716575975,
0.0781545595777905));
#86912=CARTESIAN_POINT('Ctrl Pts',(0.0122724540276985,-0.0319386439829667,
0.078133406573588));
#86913=CARTESIAN_POINT('Ctrl Pts',(0.0122928199824309,-0.03189790993816,
0.0781119741840404));
#86914=CARTESIAN_POINT('Ctrl Pts',(0.012313185534615,-0.031857176698492,
0.07809054221812));
#86915=CARTESIAN_POINT('Ctrl Pts',(0.0123333981170701,-0.0318163871833588,
0.0780689410364438));
#86916=CARTESIAN_POINT('Ctrl Pts',(0.0123533907779421,-0.0317755399638303,
0.0780472473439951));
#86917=CARTESIAN_POINT('',(0.0122302737564742,-0.0321934096636183,0.078174826336627));
#86918=CARTESIAN_POINT('Origin',(0.0138933921029899,-0.032411245654862,
0.0797754222134512));
#86919=CARTESIAN_POINT('',(0.0122740218688575,-0.0321934096636663,0.0781301905587545));
#86920=CARTESIAN_POINT('Ctrl Pts',(0.0123157418607905,-0.0321934096636618,
0.0780855751499363));
#86921=CARTESIAN_POINT('Ctrl Pts',(0.012370016509316,-0.0320835708272592,
0.0780277647590967));
#86922=CARTESIAN_POINT('Ctrl Pts',(0.0124230632933058,-0.0319739230346488,
0.0779688646896027));
#86923=CARTESIAN_POINT('Ctrl Pts',(0.0124748201266384,-0.0318646057455573,
0.0779089555088152));
#86924=CARTESIAN_POINT('Ctrl Pts',(0.0124290550093506,-0.0321934096636618,
0.0780844371125261));
#86925=CARTESIAN_POINT('Ctrl Pts',(0.0124833139634533,-0.0320835708272592,
0.0780250640450567));
#86926=CARTESIAN_POINT('Ctrl Pts',(0.012536312722612,-0.0319739230346488,
0.0779646025301442));
#86927=CARTESIAN_POINT('Ctrl Pts',(0.0125879894154724,-0.0318646057455573,
0.0779031351281948));
#86928=CARTESIAN_POINT('Ctrl Pts',(0.0125423681579107,-0.0321934096636618,
0.0780832990751159));
#86929=CARTESIAN_POINT('Ctrl Pts',(0.0125966114175906,-0.0320835708272592,
0.0780223633310167));
#86930=CARTESIAN_POINT('Ctrl Pts',(0.0126495621519182,-0.0319739230346488,
0.0779603403706857));
#86931=CARTESIAN_POINT('Ctrl Pts',(0.0127011587043063,-0.0318646057455573,
0.0778973147475744));
#86932=CARTESIAN_POINT('Ctrl Pts',(0.0126556813064708,-0.0321934096636618,
0.0780821610377056));
#86933=CARTESIAN_POINT('Ctrl Pts',(0.0127099088717279,-0.0320835708272592,
0.0780196626169768));
#86934=CARTESIAN_POINT('Ctrl Pts',(0.0127628115812245,-0.0319739230346488,
0.0779560782112272));
#86935=CARTESIAN_POINT('Ctrl Pts',(0.0128143279931403,-0.0318646057455573,
0.077891494366954));
#86936=CARTESIAN_POINT('',(0.0126640701329279,-0.0321763980308326,0.0780724718483922));
#86937=CARTESIAN_POINT('',(0.0126556813064761,-0.0321934096636185,0.0780821610376811));
#86938=CARTESIAN_POINT('Origin',(0.000551872876335866,-0.0326386231316345,
0.0667976872454305));
#86939=CARTESIAN_POINT('Ctrl Pts',(0.0126640701305228,-0.0321763980306375,
0.0780724718463136));
#86940=CARTESIAN_POINT('Ctrl Pts',(0.0126315927749162,-0.0321259596176189,
0.0780444138211916));
#86941=CARTESIAN_POINT('Ctrl Pts',(0.0125996781316311,-0.0320749164634115,
0.0780168419377658));
#86942=CARTESIAN_POINT('Ctrl Pts',(0.0125369485855449,-0.0319716057794027,
0.0779626482650633));
#86943=CARTESIAN_POINT('Ctrl Pts',(0.0125061581245192,-0.031919378669023,
0.0779360475916668));
#86944=CARTESIAN_POINT('Ctrl Pts',(0.0124759194914615,-0.0318665617525441,
0.0779099236566928));
#86945=CARTESIAN_POINT('',(0.0124867256438585,-0.0321934096636663,0.0780838579092815));
#86946=CARTESIAN_POINT('Origin',(0.00812378219310841,-0.0315241814719618,
0.07415));
#86947=CARTESIAN_POINT('',(0.0126640701332069,-0.0322104233323761,0.0780724718486335));
#86948=CARTESIAN_POINT('',(0.0126724382467512,-0.0321934096636183,0.078062764764929));
#86949=CARTESIAN_POINT('Origin',(0.000517747781834131,-0.0326387244823149,
0.0668275286705876));
#86950=CARTESIAN_POINT('Origin',(-0.000250277107460089,-0.0326386235201794,
0.0677261798898456));
#86951=CARTESIAN_POINT('Origin',(-0.00022570672338414,-0.0326387249176944,
0.0676880839863557));
#86952=CARTESIAN_POINT('Ctrl Pts',(0.0123688711055919,-0.0327445246967096,
0.0780303795078716));
#86953=CARTESIAN_POINT('Ctrl Pts',(0.0125152220112444,-0.032443687833936,
0.0778702733621565));
#86954=CARTESIAN_POINT('Ctrl Pts',(0.0126490973001736,-0.0321434074405927,
0.0776995983127345));
#86955=CARTESIAN_POINT('Ctrl Pts',(0.0125334930880667,-0.0327445246967096,
0.0778422316859708));
#86956=CARTESIAN_POINT('Ctrl Pts',(0.0126727478826105,-0.032443687833936,
0.0776759167206861));
#86957=CARTESIAN_POINT('Ctrl Pts',(0.0127990795460675,-0.0321434074405927,
0.0774995849983862));
#86958=CARTESIAN_POINT('',(0.0125566096336387,-0.0326943950436612,0.0778144461904198));
#86959=CARTESIAN_POINT('',(0.0127034191046726,-0.0323666188837389,0.0776292313458923));
#86960=CARTESIAN_POINT('Origin',(-0.000448633507967139,-0.0326395579110996,
0.0671621361566276));
#86961=CARTESIAN_POINT('Origin',(0.0214979151808044,-0.0321933825603007,
0.0843105643423937));
#86962=CARTESIAN_POINT('',(0.012626719740879,-0.0321934096532689,0.0777279433251215));
#86963=CARTESIAN_POINT('',(0.0126645285418757,-0.0321934096584275,0.0776781764193205));
#86964=CARTESIAN_POINT('',(0.012475919493572,-0.0325210109756239,0.0779099236585222));
#86965=CARTESIAN_POINT('Origin',(-0.000123152820681168,-0.0326393129157583,
0.0668082339780196));
#86966=CARTESIAN_POINT('',(0.0124748914701047,-0.0326943950436593,0.0779090355225293));
#86967=CARTESIAN_POINT('Origin',(0.0208460127915698,-0.032694376553814,
0.085141064595157));
#86968=CARTESIAN_POINT('',(0.0125157505518817,-0.0326943950436702,0.0778617408564845));
#86969=CARTESIAN_POINT('Ctrl Pts',(0.0125068329018791,-0.0325229783203769,
0.0782474219314632));
#86970=CARTESIAN_POINT('Ctrl Pts',(0.0125633157735996,-0.032413025309245,
0.0781870016732939));
#86971=CARTESIAN_POINT('Ctrl Pts',(0.0126185402079304,-0.0323031222208069,
0.0781254221582815));
#86972=CARTESIAN_POINT('Ctrl Pts',(0.0126724382496766,-0.0321934096576658,
0.0780627647615384));
#86973=CARTESIAN_POINT('Ctrl Pts',(0.0124961555676023,-0.0325229783203769,
0.0781346073190692));
#86974=CARTESIAN_POINT('Ctrl Pts',(0.012551083292358,-0.032413025309245,
0.0780743342477194));
#86975=CARTESIAN_POINT('Ctrl Pts',(0.012604755860341,-0.0323031222208069,
0.0780129340674154));
#86976=CARTESIAN_POINT('Ctrl Pts',(0.0126571072960809,-0.0321934096576658,
0.0779504878534107));
#86977=CARTESIAN_POINT('Ctrl Pts',(0.0124854782333254,-0.0325229783203769,
0.0780217927066752));
#86978=CARTESIAN_POINT('Ctrl Pts',(0.0125388508111164,-0.032413025309245,
0.0779616668221448));
#86979=CARTESIAN_POINT('Ctrl Pts',(0.0125909715127516,-0.0323031222208069,
0.0779004459765494));
#86980=CARTESIAN_POINT('Ctrl Pts',(0.0126417763424852,-0.0321934096576658,
0.077838210945283));
#86981=CARTESIAN_POINT('Ctrl Pts',(0.0124748008990486,-0.0325229783203769,
0.0779089780942812));
#86982=CARTESIAN_POINT('Ctrl Pts',(0.0125266183298748,-0.032413025309245,
0.0778489993965703));
#86983=CARTESIAN_POINT('Ctrl Pts',(0.0125771871651622,-0.0323031222208069,
0.0777879578856833));
#86984=CARTESIAN_POINT('Ctrl Pts',(0.0126264453888895,-0.0321934096576658,
0.0777259340371553));
#86985=CARTESIAN_POINT('',(0.0126495789936254,-0.0321934096584274,0.077895354045503));
#86986=CARTESIAN_POINT('Ctrl Pts',(0.0126640701305689,-0.0322104233328896,
0.0780724718463536));
#86987=CARTESIAN_POINT('Ctrl Pts',(0.0126315487675926,-0.032260942183051,
0.0780443758021299));
#86988=CARTESIAN_POINT('Ctrl Pts',(0.0125996126259685,-0.0323120888238984,
0.0780167853457256));
#86989=CARTESIAN_POINT('Ctrl Pts',(0.0125368826049921,-0.0324156524631807,
0.0779625912627532));
#86990=CARTESIAN_POINT('Ctrl Pts',(0.0125061145111221,-0.0324680267167311,
0.0779360099129284));
#86991=CARTESIAN_POINT('Ctrl Pts',(0.0124759194935421,-0.0325210109755912,
0.0779099236584905));
#86992=CARTESIAN_POINT('Origin',(0.00230059941656284,-0.0262834582510572,
0.079440928859173));
#86993=CARTESIAN_POINT('Origin',(0.0127962631772917,-0.0342770831689207,
0.0853745949748125));
#86994=CARTESIAN_POINT('Ctrl Pts',(0.0125545872851655,-0.0326943950436604,
0.0778145938301346));
#86995=CARTESIAN_POINT('Ctrl Pts',(0.0126050922563256,-0.0325844576448134,
0.0777535290317522));
#86996=CARTESIAN_POINT('Ctrl Pts',(0.0126543378816533,-0.0324744968375323,
0.0776914153861116));
#86997=CARTESIAN_POINT('Ctrl Pts',(0.012702262162479,-0.0323646534831895,
0.0776283333471264));
#86998=CARTESIAN_POINT('Ctrl Pts',(0.012667605214521,-0.0326943950436604,
0.0778063430588587));
#86999=CARTESIAN_POINT('Ctrl Pts',(0.0127179964745893,-0.0325844576448134,
0.0777437206615916));
#87000=CARTESIAN_POINT('Ctrl Pts',(0.0127670961670791,-0.0324744968375323,
0.0776800516585644));
#87001=CARTESIAN_POINT('Ctrl Pts',(0.0128148425077852,-0.0323646534831895,
0.0776154184939263));
#87002=CARTESIAN_POINT('Ctrl Pts',(0.0127806231438765,-0.0326943950436604,
0.0777980922875828));
#87003=CARTESIAN_POINT('Ctrl Pts',(0.012830900692853,-0.0325844576448134,
0.077733912291431));
#87004=CARTESIAN_POINT('Ctrl Pts',(0.0128798544525049,-0.0324744968375323,
0.0776686879310172));
#87005=CARTESIAN_POINT('Ctrl Pts',(0.0129274228530915,-0.0323646534831895,
0.0776025036407263));
#87006=CARTESIAN_POINT('Ctrl Pts',(0.012893641073232,-0.0326943950436604,
0.0777898415163069));
#87007=CARTESIAN_POINT('Ctrl Pts',(0.0129438049111168,-0.0325844576448134,
0.0777241039212704));
#87008=CARTESIAN_POINT('Ctrl Pts',(0.0129926127379307,-0.0324744968375323,
0.07765732420347));
#87009=CARTESIAN_POINT('Ctrl Pts',(0.0130400031983977,-0.0323646534831895,
0.0775895887875262));
#87010=CARTESIAN_POINT('',(0.0129014049571702,-0.0326773559991391,0.0777796447077724));
#87011=CARTESIAN_POINT('',(0.0128936410732186,-0.0326943950436595,0.0777898415163072));
#87012=CARTESIAN_POINT('Origin',(-0.000351172866345553,-0.0326395670215677,
0.0677745215341868));
#87013=CARTESIAN_POINT('Ctrl Pts',(0.0129014049544966,-0.0326773559987503,
0.07777964470574));
#87014=CARTESIAN_POINT('Ctrl Pts',(0.0128672024057852,-0.0326267922587135,
0.0777536604231683));
#87015=CARTESIAN_POINT('Ctrl Pts',(0.0128336060725491,-0.0325756109581668,
0.0777281366932396));
#87016=CARTESIAN_POINT('Ctrl Pts',(0.0127675972446041,-0.0324719985462389,
0.0776779886164975));
#87017=CARTESIAN_POINT('Ctrl Pts',(0.0127352112244493,-0.0324196091621776,
0.0776533843828722));
#87018=CARTESIAN_POINT('Ctrl Pts',(0.0127034191046338,-0.0323666188837756,
0.0776292313458628));
#87019=CARTESIAN_POINT('',(0.0127251253534387,-0.0326943950436703,0.0778021438533735));
#87020=CARTESIAN_POINT('Origin',(0.00812378219310841,-0.0315241814719618,
0.07415));
#87021=CARTESIAN_POINT('',(0.0129014049571333,-0.0327114338380031,0.0777796447077446));
#87022=CARTESIAN_POINT('',(0.0129091470454567,-0.0326943950436593,0.0777694313406825));
#87023=CARTESIAN_POINT('Origin',(-0.00037795912897998,-0.0326395681488619,
0.0678110648869237));
#87024=CARTESIAN_POINT('Origin',(-0.000290388076978256,-0.0326395672708735,
0.0676945109721873));
#87025=CARTESIAN_POINT('Origin',(-0.000262362806127849,-0.0326395685118704,
0.0676589091060391));
#87026=CARTESIAN_POINT('Ctrl Pts',(0.0126041700312253,-0.0332451089994432,
0.0777561405713108));
#87027=CARTESIAN_POINT('Ctrl Pts',(0.0127401778480767,-0.0329451141710253,
0.077587159979329));
#87028=CARTESIAN_POINT('Ctrl Pts',(0.0128630709720886,-0.0326442513127493,
0.0774084147786052));
#87029=CARTESIAN_POINT('Ctrl Pts',(0.0127566519192198,-0.0332451089994432,
0.0775580262764363));
#87030=CARTESIAN_POINT('Ctrl Pts',(0.0128851877331916,-0.0329451141710253,
0.0773832947359585));
#87031=CARTESIAN_POINT('Ctrl Pts',(0.0130001968965448,-0.0326442513127493,
0.0771993777463787));
#87032=CARTESIAN_POINT('Ctrl Pts',(0.0127581767380997,-0.0332451089994432,
0.0775560451334876));
#87033=CARTESIAN_POINT('Ctrl Pts',(0.0128866378320428,-0.0329451141710253,
0.0773812560835247));
#87034=CARTESIAN_POINT('Ctrl Pts',(0.0130015681557894,-0.0326442513127493,
0.0771972873760565));
#87035=CARTESIAN_POINT('',(0.0127779549413521,-0.0331951640388616,0.0775288757049508));
#87036=CARTESIAN_POINT('',(0.0129128449938955,-0.0328677532355046,0.0773348080884048));
#87037=CARTESIAN_POINT('Origin',(-0.0012249331354173,-0.0326402808281172,
0.0683119687951164));
#87038=CARTESIAN_POINT('Origin',(0.0221191769029498,-0.0326944278779093,
0.0834567224738829));
#87039=CARTESIAN_POINT('',(0.012842495146412,-0.0326943950436593,0.0774381412780363));
#87040=CARTESIAN_POINT('',(0.0128771044486979,-0.0326943950436693,0.0773860985437217));
#87041=CARTESIAN_POINT('',(0.0127034191046709,-0.0330220786163545,0.0776292313458946));
#87042=CARTESIAN_POINT('Origin',(-0.000985430167367684,-0.0326396682762316,
0.067895086349666));
#87043=CARTESIAN_POINT('',(0.0127023373432517,-0.0331951640388587,0.0776284095125642));
#87044=CARTESIAN_POINT('Origin',(0.0214865161934399,-0.0331952026560077,
0.0843019072061792));
#87045=CARTESIAN_POINT('',(0.0127401461423119,-0.0331951640388701,0.0775786426087675));
#87046=CARTESIAN_POINT('Ctrl Pts',(0.0127554638151504,-0.0330240426238172,
0.0779641218323661));
#87047=CARTESIAN_POINT('Ctrl Pts',(0.0128080070593101,-0.0329142774063519,
0.0779003159055937));
#87048=CARTESIAN_POINT('Ctrl Pts',(0.0128592574514538,-0.0328043479726691,
0.0778353919536107));
#87049=CARTESIAN_POINT('Ctrl Pts',(0.0129091470454586,-0.0326943950436593,
0.0777694313406921));
#87050=CARTESIAN_POINT('Ctrl Pts',(0.0127377238484254,-0.0330240426238172,
0.0778522002992919));
#87051=CARTESIAN_POINT('Ctrl Pts',(0.0127887252644271,-0.0329142774063519,
0.0777886387578444));
#87052=CARTESIAN_POINT('Ctrl Pts',(0.0128384381118826,-0.0328043479726691,
0.0777239911869161));
#87053=CARTESIAN_POINT('Ctrl Pts',(0.0128867964241291,-0.0326943950436593,
0.0776583386509629));
#87054=CARTESIAN_POINT('Ctrl Pts',(0.0127199838817004,-0.0330240426238172,
0.0777402787662177));
#87055=CARTESIAN_POINT('Ctrl Pts',(0.0127694434695442,-0.032914277406352,
0.077676961610095));
#87056=CARTESIAN_POINT('Ctrl Pts',(0.0128176187723115,-0.0328043479726691,
0.0776125904202215));
#87057=CARTESIAN_POINT('Ctrl Pts',(0.0128644458027996,-0.0326943950436593,
0.0775472459612337));
#87058=CARTESIAN_POINT('Ctrl Pts',(0.0127022439149754,-0.0330240426238172,
0.0776283572331435));
#87059=CARTESIAN_POINT('Ctrl Pts',(0.0127501616746612,-0.032914277406352,
0.0775652844623457));
#87060=CARTESIAN_POINT('Ctrl Pts',(0.0127967994327403,-0.0328043479726691,
0.0775011896535269));
#87061=CARTESIAN_POINT('Ctrl Pts',(0.0128420951814701,-0.0326943950436593,
0.0774361532715045));
#87062=CARTESIAN_POINT('',(0.0128758210959444,-0.0326943950436693,0.0776037863093694));
#87063=CARTESIAN_POINT('Ctrl Pts',(0.0129014049544878,-0.0327114338383289,
0.0777796447057335));
#87064=CARTESIAN_POINT('Ctrl Pts',(0.0128672080947621,-0.0327619876830131,
0.077753664745185));
#87065=CARTESIAN_POINT('Ctrl Pts',(0.0128336145402828,-0.0328131562602634,
0.077728143126327));
#87066=CARTESIAN_POINT('Ctrl Pts',(0.0127676057729972,-0.0329167375858765,
0.0776779950956691));
#87067=CARTESIAN_POINT('Ctrl Pts',(0.012735216861643,-0.0329691088920629,
0.0776533886655483));
#87068=CARTESIAN_POINT('Ctrl Pts',(0.0127034191046347,-0.0330220786163187,
0.0776292313458637));
#87069=CARTESIAN_POINT('Ctrl Pts',(0.0127759455331478,-0.0331951640388604,
0.0775291500814413));
#87070=CARTESIAN_POINT('Ctrl Pts',(0.0128458072945721,-0.0330306422010619,
0.0774329695870756));
#87071=CARTESIAN_POINT('Ctrl Pts',(0.0129116341186329,-0.0328657861914645,
0.0773339838182005));
#87072=CARTESIAN_POINT('Ctrl Pts',(0.0127779549413502,-0.0331951640388604,
0.0775288757049533));
#87073=CARTESIAN_POINT('Ctrl Pts',(0.0128478110302165,-0.0330306422010619,
0.0774326536673613));
#87074=CARTESIAN_POINT('Ctrl Pts',(0.0129136304695413,-0.0328657861914645,
0.0773336266252111));
#87075=CARTESIAN_POINT('Ctrl Pts',(0.013112776386117,-0.0331951640388604,
0.0774831572033527));
#87076=CARTESIAN_POINT('Ctrl Pts',(0.0131816872742748,-0.0330306422010619,
0.0773800129470578));
#87077=CARTESIAN_POINT('Ctrl Pts',(0.0132462762179797,-0.0328657861914645,
0.0772741086673313));
#87078=CARTESIAN_POINT('',(0.0131198846876255,-0.0331781648281957,0.0774724930188458));
#87079=CARTESIAN_POINT('',(0.0131127763861026,-0.0331951640388588,0.0774831572033539));
#87080=CARTESIAN_POINT('Origin',(-0.0010195947541991,-0.0326412093102044,
0.0689248852377839));
#87081=CARTESIAN_POINT('Ctrl Pts',(0.0131198846858996,-0.033178164828644,
0.0774724930195014));
#87082=CARTESIAN_POINT('Ctrl Pts',(0.0130840934308751,-0.0331276811546766,
0.0774486912415261));
#87083=CARTESIAN_POINT('Ctrl Pts',(0.0130489484363515,-0.0330765663497776,
0.0774253192781101));
#87084=CARTESIAN_POINT('Ctrl Pts',(0.0129799208623961,-0.0329730614463504,
0.0773794147647705));
#87085=CARTESIAN_POINT('Ctrl Pts',(0.0129460661715751,-0.0329207133374634,
0.0773569007548111));
#87086=CARTESIAN_POINT('Ctrl Pts',(0.0129128449934111,-0.0328677532289399,
0.0773348081048698));
#87087=CARTESIAN_POINT('',(0.0129453656637373,-0.0331951640388702,0.0775060164541623));
#87088=CARTESIAN_POINT('Origin',(0.00812378219310841,-0.0315241814719618,
0.07415));
#87089=CARTESIAN_POINT('',(0.0131198846866907,-0.0332121607144205,0.0774724930174478));
#87090=CARTESIAN_POINT('',(0.0131269701953153,-0.0331951640388587,0.0774618136744959));
#87091=CARTESIAN_POINT('Origin',(-0.00103779367125268,-0.0326413666455162,
0.0689664173061276));
#87092=CARTESIAN_POINT('Origin',(-0.000230762201290447,-0.0326412093881342,
0.0677386999905375));
#87093=CARTESIAN_POINT('Origin',(-0.000199498376431669,-0.0326413668167375,
0.0677058564566509));
#87094=CARTESIAN_POINT('Ctrl Pts',(0.0128217484324243,-0.0337436976235975,
0.0774677158127615));
#87095=CARTESIAN_POINT('Ctrl Pts',(0.0128515884712579,-0.0336723290703325,
0.0774254615924088));
#87096=CARTESIAN_POINT('Ctrl Pts',(0.0128806636624346,-0.033601104548885,
0.0773826774795486));
#87097=CARTESIAN_POINT('Ctrl Pts',(0.0129734949883911,-0.0333736987606857,
0.0772460762822411));
#87098=CARTESIAN_POINT('Ctrl Pts',(0.0130583343713293,-0.0331450831799192,
0.077104372996156));
#87099=CARTESIAN_POINT('Ctrl Pts',(0.0129614904835795,-0.0337436976235975,
0.0772604185403749));
#87100=CARTESIAN_POINT('Ctrl Pts',(0.0129894660593284,-0.0336723290703325,
0.0772169074588357));
#87101=CARTESIAN_POINT('Ctrl Pts',(0.0130166544820755,-0.033601104548885,
0.0771729002239336));
#87102=CARTESIAN_POINT('Ctrl Pts',(0.013103461730184,-0.0333736987606857,
0.0770323938402334));
#87103=CARTESIAN_POINT('Ctrl Pts',(0.0131820628603656,-0.0331450831799192,
0.0768871374995152));
#87104=CARTESIAN_POINT('Ctrl Pts',(0.012962887904091,-0.0337436976235975,
0.077258345567651));
#87105=CARTESIAN_POINT('Ctrl Pts',(0.0129908448352091,-0.0336723290703325,
0.0772148219174999));
#87106=CARTESIAN_POINT('Ctrl Pts',(0.0130180143902719,-0.033601104548885,
0.0771708024513775));
#87107=CARTESIAN_POINT('Ctrl Pts',(0.0131047613976019,-0.0333736987606857,
0.0770302570158134));
#87108=CARTESIAN_POINT('Ctrl Pts',(0.0131833001452559,-0.0331450831799192,
0.0768849651445488));
#87109=CARTESIAN_POINT('',(0.0129809323555244,-0.0336938721132548,0.0772299703407246));
#87110=CARTESIAN_POINT('',(0.0131033706183091,-0.0333679869945434,0.0770278158585576));
#87111=CARTESIAN_POINT('Ctrl Pts',(0.0129809323555235,-0.033693872113265,
0.0772299703407274));
#87112=CARTESIAN_POINT('Ctrl Pts',(0.0129929549246028,-0.0336629187933933,
0.0772110106051136));
#87113=CARTESIAN_POINT('Ctrl Pts',(0.0130048626317031,-0.0336319952301041,
0.077191986536299));
#87114=CARTESIAN_POINT('Ctrl Pts',(0.013016654482074,-0.0336011045488951,
0.0771729002239361));
#87115=CARTESIAN_POINT('Ctrl Pts',(0.0130462442695989,-0.0335235892595455,
0.0771250061352493));
#87116=CARTESIAN_POINT('Ctrl Pts',(0.0130751569819193,-0.033445866866037,
0.0770766349299063));
#87117=CARTESIAN_POINT('Ctrl Pts',(0.0131033706185681,-0.0333679869945386,
0.0770278158587149));
#87118=CARTESIAN_POINT('Ctrl Pts',(0.0131033934652619,-0.0333679692459665,
0.0770277776998562));
#87119=CARTESIAN_POINT('Ctrl Pts',(0.0131029981019756,-0.0333391895373163,
0.0770275560566834));
#87120=CARTESIAN_POINT('Ctrl Pts',(0.0131027001700079,-0.0333104081057696,
0.0770273927567706));
#87121=CARTESIAN_POINT('Ctrl Pts',(0.0131023031435285,-0.0332532697426299,
0.0770271814578659));
#87122=CARTESIAN_POINT('Ctrl Pts',(0.013102201146355,-0.0332249167276877,
0.0770271317795956));
#87123=CARTESIAN_POINT('Ctrl Pts',(0.0131021945177025,-0.0331960985527834,
0.0770271359141604));
#87124=CARTESIAN_POINT('Ctrl Pts',(0.0131021944358776,-0.0331956312395902,
0.0770271359962724));
#87125=CARTESIAN_POINT('Ctrl Pts',(0.0131021943802153,-0.0331951640388594,
0.0770271360925869));
#87126=CARTESIAN_POINT('',(0.0130396479434198,-0.0331951640388587,0.0771353624444808));
#87127=CARTESIAN_POINT('',(0.0130709211618275,-0.0331951640388687,0.077081249268544));
#87128=CARTESIAN_POINT('',(0.0129128449807048,-0.0335216366567648,0.0773348080965793));
#87129=CARTESIAN_POINT('Origin',(-0.00158890560126417,-0.0326434571530048,
0.0691451869164799));
#87130=CARTESIAN_POINT('',(0.0129117137509639,-0.0336938721132327,0.0773340558093871));
#87131=CARTESIAN_POINT('Origin',(0.0220050936674813,-0.0336938867896241,
0.0833813090403592));
#87132=CARTESIAN_POINT('',(0.0129463230532542,-0.0336938721132538,0.0772820130750659));
#87133=CARTESIAN_POINT('Ctrl Pts',(0.0129858155040267,-0.0335235895815172,
0.0776657690600517));
#87134=CARTESIAN_POINT('Ctrl Pts',(0.0130342169870506,-0.0334144449262748,
0.0775988335990642));
#87135=CARTESIAN_POINT('Ctrl Pts',(0.0130812912412651,-0.0333049234473147,
0.0775308212991283));
#87136=CARTESIAN_POINT('Ctrl Pts',(0.013126970195318,-0.0331951640388587,
0.0774618136745056));
#87137=CARTESIAN_POINT('Ctrl Pts',(0.0129610828790003,-0.0335235895815172,
0.0775551821270721));
#87138=CARTESIAN_POINT('Ctrl Pts',(0.0130079619151661,-0.0334144449262748,
0.0774885871593622));
#87139=CARTESIAN_POINT('Ctrl Pts',(0.0130535190077504,-0.0333049234473147,
0.0774209471964957));
#87140=CARTESIAN_POINT('Ctrl Pts',(0.0130976880685124,-0.0331951640388587,
0.0773523434523616));
#87141=CARTESIAN_POINT('Ctrl Pts',(0.0129363502539739,-0.0335235895815172,
0.0774445951940926));
#87142=CARTESIAN_POINT('Ctrl Pts',(0.0129817068432816,-0.0334144449262748,
0.0773783407196602));
#87143=CARTESIAN_POINT('Ctrl Pts',(0.0130257467742356,-0.0333049234473147,
0.0773110730938632));
#87144=CARTESIAN_POINT('Ctrl Pts',(0.0130684059417069,-0.0331951640388587,
0.0772428732302176));
#87145=CARTESIAN_POINT('Ctrl Pts',(0.0129116176289475,-0.0335235895815172,
0.0773340082611131));
#87146=CARTESIAN_POINT('Ctrl Pts',(0.0129554517713971,-0.0334144449262748,
0.0772680942799582));
#87147=CARTESIAN_POINT('Ctrl Pts',(0.0129979745407209,-0.0333049234473147,
0.0772011989912306));
#87148=CARTESIAN_POINT('Ctrl Pts',(0.0130391238149014,-0.0331951640388587,
0.0771334030080735));
#87149=CARTESIAN_POINT('',(0.0130833090693776,-0.0331951640388687,0.0772985880594984));
#87150=CARTESIAN_POINT('Ctrl Pts',(0.013119884684077,-0.0332121607145942,
0.0774724930157079));
#87151=CARTESIAN_POINT('Ctrl Pts',(0.01308415364584,-0.0332625444108875,
0.0774487312683857));
#87152=CARTESIAN_POINT('Ctrl Pts',(0.0130490383094607,-0.0333135300745053,
0.0774253789732565));
#87153=CARTESIAN_POINT('Ctrl Pts',(0.0129800111660968,-0.0334167203140531,
0.0773794747504879));
#87154=CARTESIAN_POINT('Ctrl Pts',(0.012946126094066,-0.0334688847587198,
0.0773569406020467));
#87155=CARTESIAN_POINT('Ctrl Pts',(0.0129128449802051,-0.033521636656226,
0.0773348080960466));
#87156=CARTESIAN_POINT('Ctrl Pts',(0.0129799521394177,-0.033693872113239,
0.0772301675493867));
#87157=CARTESIAN_POINT('Ctrl Pts',(0.0129979813821922,-0.0336474569764958,
0.0772017427752429));
#87158=CARTESIAN_POINT('Ctrl Pts',(0.0130156766417212,-0.033601104548885,
0.0771731088937324));
#87159=CARTESIAN_POINT('Ctrl Pts',(0.0130604769704531,-0.0334837508592656,
0.0771006144890902));
#87160=CARTESIAN_POINT('Ctrl Pts',(0.0131031094666671,-0.0333660264659097,
0.0770268243920209));
#87161=CARTESIAN_POINT('Ctrl Pts',(0.0129809323555133,-0.033693872113239,
0.077229970340742));
#87162=CARTESIAN_POINT('Ctrl Pts',(0.0129989604439602,-0.0336474569764958,
0.0772015398290681));
#87163=CARTESIAN_POINT('Ctrl Pts',(0.0130166544820755,-0.033601104548885,
0.0771729002239336));
#87164=CARTESIAN_POINT('Ctrl Pts',(0.0130614517184691,-0.0334837508592656,
0.0771003913283911));
#87165=CARTESIAN_POINT('Ctrl Pts',(0.0131040806943073,-0.0333660264659097,
0.0770265868384173));
#87166=CARTESIAN_POINT('Ctrl Pts',(0.0133142101585596,-0.033693872113239,
0.0771629185302985));
#87167=CARTESIAN_POINT('Ctrl Pts',(0.0133318457705099,-0.0336474569764958,
0.07713253723305));
#87168=CARTESIAN_POINT('Ctrl Pts',(0.0133491245226131,-0.033601104548885,
0.0771019515704431));
#87169=CARTESIAN_POINT('Ctrl Pts',(0.0133928703503042,-0.0334837508592656,
0.0770245157048068));
#87170=CARTESIAN_POINT('Ctrl Pts',(0.0134343023828019,-0.0333660264659097,
0.0769458175637212));
#87171=CARTESIAN_POINT('',(0.0133186470840024,-0.0336769361243753,0.0771522289661778));
#87172=CARTESIAN_POINT('',(0.0133122224181615,-0.0336938721132327,0.0771633184416936));
#87173=CARTESIAN_POINT('Ctrl Pts',(0.0133186470840025,-0.0336769361243749,
0.0771522289661776));
#87174=CARTESIAN_POINT('Ctrl Pts',(0.0133175782002636,-0.0336797586670132,
0.0771540784942017));
#87175=CARTESIAN_POINT('Ctrl Pts',(0.0133165083692196,-0.0336825812713061,
0.0771559273814434));
#87176=CARTESIAN_POINT('Ctrl Pts',(0.0133143668181204,-0.0336882265895377,
0.0771596238657232));
#87177=CARTESIAN_POINT('Ctrl Pts',(0.0133132950980859,-0.0336910493035001,
0.0771614714627857));
#87178=CARTESIAN_POINT('Ctrl Pts',(0.0133122224181737,-0.0336938721132372,
0.0771633184416937));
#87179=CARTESIAN_POINT('Ctrl Pts',(0.0133186470840023,-0.0336769361243753,
0.0771522289661778));
#87180=CARTESIAN_POINT('Ctrl Pts',(0.013282359462025,-0.0336279031301491,
0.0771312575353318));
#87181=CARTESIAN_POINT('Ctrl Pts',(0.0132455497517024,-0.033576785189935,
0.0771099843779186));
#87182=CARTESIAN_POINT('Ctrl Pts',(0.013173422021026,-0.033473319885733,
0.0770683001441899));
#87183=CARTESIAN_POINT('Ctrl Pts',(0.0131380555712316,-0.0334209645014095,
0.077047861079414));
#87184=CARTESIAN_POINT('Ctrl Pts',(0.0131033706146526,-0.0333679869844681,
0.0770278158648571));
#87185=CARTESIAN_POINT('',(0.013146577386853,-0.0336938721132538,0.0771966443912191));
#87186=CARTESIAN_POINT('Origin',(0.00812378219310841,-0.0315241814719618,
0.07415));
#87187=CARTESIAN_POINT('',(0.0133186470828877,-0.0337108120655662,0.0771522289655357));
#87188=CARTESIAN_POINT('',(0.0133250480478685,-0.0336938721132327,0.0771411257927597));
#87189=CARTESIAN_POINT('Origin',(-0.000287847130412359,-0.0345562526275983,
0.0679979099388204));
#87190=CARTESIAN_POINT('Ctrl Pts',(0.0133250480478763,-0.0336938721132384,
0.0771411257927729));
#87191=CARTESIAN_POINT('Ctrl Pts',(0.0133239832652973,-0.0336910492960854,
0.0771429773422077));
#87192=CARTESIAN_POINT('Ctrl Pts',(0.0133229174720819,-0.0336882265858302,
0.0771448283612693));
#87193=CARTESIAN_POINT('Ctrl Pts',(0.0133207838233142,-0.0336825812712828,
0.0771485294092638));
#87194=CARTESIAN_POINT('Ctrl Pts',(0.0133197159677367,-0.0336797586670016,
0.0771503794381617));
#87195=CARTESIAN_POINT('Ctrl Pts',(0.0133186470840022,-0.033676936124375,
0.0771522289661781));
#87196=CARTESIAN_POINT('Origin',(-0.00140628322933532,-0.0345562521941869,
0.069933181487582));
#87197=CARTESIAN_POINT('Ctrl Pts',(0.0130207720882508,-0.0342436276873909,
0.0771662252845027));
#87198=CARTESIAN_POINT('Ctrl Pts',(0.0131345309001936,-0.0339430054201809,
0.0769815322659044));
#87199=CARTESIAN_POINT('Ctrl Pts',(0.0132340547003607,-0.0336441434784052,
0.0767887951609819));
#87200=CARTESIAN_POINT('Ctrl Pts',(0.0131472240232456,-0.0342436276873909,
0.0769505637252575));
#87201=CARTESIAN_POINT('Ctrl Pts',(0.0132528490253939,-0.0339430054201809,
0.0767611014933095));
#87202=CARTESIAN_POINT('Ctrl Pts',(0.0133439028863766,-0.0336441434784052,
0.0765642213957533));
#87203=CARTESIAN_POINT('Ctrl Pts',(0.0131484885425955,-0.0342436276873909,
0.0769484071096651));
#87204=CARTESIAN_POINT('Ctrl Pts',(0.0132540322066459,-0.0339430054201809,
0.0767588971855835));
#87205=CARTESIAN_POINT('Ctrl Pts',(0.0133450013682368,-0.0336441434784052,
0.0765619756581011));
#87206=CARTESIAN_POINT('',(0.0131647408170106,-0.0341934961088741,0.0769189097406935));
#87207=CARTESIAN_POINT('',(0.0132742440887522,-0.0338664212863332,0.0767094662071803));
#87208=CARTESIAN_POINT('Origin',(-0.00125084518927599,-0.0345610720405465,
0.0684192612854017));
#87209=CARTESIAN_POINT('Origin',(0.0230947708325115,-0.0336938005072996,
0.0815896279783451));
#87210=CARTESIAN_POINT('',(0.0132174000641565,-0.0336938721132327,0.0768208017492394));
#87211=CARTESIAN_POINT('',(0.0132452137775803,-0.0336938721132427,0.0767648316916638));
#87212=CARTESIAN_POINT('',(0.01310337061465,-0.0340203938281605,0.0770278158648617));
#87213=CARTESIAN_POINT('Origin',(-0.000945472464625923,-0.0345589643243393,
0.0680473954049685));
#87214=CARTESIAN_POINT('',(0.0131021943802151,-0.0341934961088739,0.0770271360925872));
#87215=CARTESIAN_POINT('Origin',(0.0226429506561994,-0.0341934220717619,
0.0825409540025416));
#87216=CARTESIAN_POINT('',(0.0131334675986228,-0.034193496108884,0.0769730229166503));
#87217=CARTESIAN_POINT('Ctrl Pts',(0.0131969768968076,-0.0340223579322396,
0.0773535442089127));
#87218=CARTESIAN_POINT('Ctrl Pts',(0.0132411621266426,-0.0339125849573575,
0.0772835716225015));
#87219=CARTESIAN_POINT('Ctrl Pts',(0.0132838680380833,-0.0338030433565231,
0.0772127336734312));
#87220=CARTESIAN_POINT('Ctrl Pts',(0.0133250480478718,-0.0336938721132327,
0.0771411257927697));
#87221=CARTESIAN_POINT('Ctrl Pts',(0.0131653493055715,-0.0340223579322396,
0.0772447284228175));
#87222=CARTESIAN_POINT('Ctrl Pts',(0.0132080336819127,-0.0339125849573575,
0.0771751920633777));
#87223=CARTESIAN_POINT('Ctrl Pts',(0.0132492488233767,-0.0338030433565231,
0.077104821098927));
#87224=CARTESIAN_POINT('Ctrl Pts',(0.0132889500002103,-0.0336938721132327,
0.0770337101943404));
#87225=CARTESIAN_POINT('Ctrl Pts',(0.0131337217143354,-0.0340223579322396,
0.0771359126367224));
#87226=CARTESIAN_POINT('Ctrl Pts',(0.0131749052371829,-0.0339125849573575,
0.0770668125042538));
#87227=CARTESIAN_POINT('Ctrl Pts',(0.0132146296086701,-0.0338030433565231,
0.0769969085244227));
#87228=CARTESIAN_POINT('Ctrl Pts',(0.0132528519525488,-0.0336938721132327,
0.076926294595911));
#87229=CARTESIAN_POINT('Ctrl Pts',(0.0131020941230993,-0.0340223579322396,
0.0770270968506272));
#87230=CARTESIAN_POINT('Ctrl Pts',(0.013141776792453,-0.0339125849573575,
0.07695843294513));
#87231=CARTESIAN_POINT('Ctrl Pts',(0.0131800103939636,-0.0338030433565231,
0.0768889959499185));
#87232=CARTESIAN_POINT('Ctrl Pts',(0.0132167539048873,-0.0336938721132327,
0.0768188789974817));
#87233=CARTESIAN_POINT('',(0.0132712240560225,-0.0336938721132427,0.0769809637710096));
#87234=CARTESIAN_POINT('Ctrl Pts',(0.0133186470797625,-0.0337108120662653,
0.0771522289637276));
#87235=CARTESIAN_POINT('Ctrl Pts',(0.0132814178587936,-0.033761140899345,
0.0771307133616997));
#87236=CARTESIAN_POINT('Ctrl Pts',(0.0132448679885092,-0.0338121088779593,
0.0771095903716735));
#87237=CARTESIAN_POINT('Ctrl Pts',(0.0131730936527325,-0.033915338277323,
0.0770681103727856));
#87238=CARTESIAN_POINT('Ctrl Pts',(0.0131378995523547,-0.0339675558473115,
0.0770477709126048));
#87239=CARTESIAN_POINT('Ctrl Pts',(0.0131033706146181,-0.0340203938281304,
0.0770278158648373));
#87240=CARTESIAN_POINT('Ctrl Pts',(0.0131627815520343,-0.0341934961088741,
0.076919433823356));
#87241=CARTESIAN_POINT('Ctrl Pts',(0.0132200374145394,-0.0340287516182427,
0.0768152564813936));
#87242=CARTESIAN_POINT('Ctrl Pts',(0.0132729386244269,-0.033864463327595,
0.0767088017287426));
#87243=CARTESIAN_POINT('Ctrl Pts',(0.0131647408170105,-0.0341934961088741,
0.0769189097406936));
#87244=CARTESIAN_POINT('Ctrl Pts',(0.0132219858445194,-0.0340287516182427,
0.0768146918924713));
#87245=CARTESIAN_POINT('Ctrl Pts',(0.0132748745545145,-0.033864463327595,
0.0767081971159909));
#87246=CARTESIAN_POINT('Ctrl Pts',(0.0134911920470384,-0.0341934961088741,
0.0768315874887945));
#87247=CARTESIAN_POINT('Ctrl Pts',(0.0135466317557828,-0.0340287516182427,
0.0767206205185736));
#87248=CARTESIAN_POINT('Ctrl Pts',(0.0135974377432913,-0.033864463327595,
0.0766074570022843));
#87249=CARTESIAN_POINT('',(0.0134969077202634,-0.0341764758832445,0.0768201164881371));
#87250=CARTESIAN_POINT('',(0.013491192047025,-0.034193496108874,0.0768315874887981));
#87251=CARTESIAN_POINT('Origin',(-0.00110300971133633,-0.0345621026930054,
0.0689930009521826));
#87252=CARTESIAN_POINT('Ctrl Pts',(0.0134969077187711,-0.0341764758837556,
0.0768201164891816));
#87253=CARTESIAN_POINT('Ctrl Pts',(0.0134584680344027,-0.0341260050040425,
0.0768010143200461));
#87254=CARTESIAN_POINT('Ctrl Pts',(0.0134206965054292,-0.0340749269148072,
0.0767822442258898));
#87255=CARTESIAN_POINT('Ctrl Pts',(0.0133464605665924,-0.0339715436306174,
0.0767453534762698));
#87256=CARTESIAN_POINT('Ctrl Pts',(0.0133100243228328,-0.033919277823705,
0.0767272468109652));
#87257=CARTESIAN_POINT('Ctrl Pts',(0.0132742440889785,-0.033866421285468,
0.0767094662092968));
#87258=CARTESIAN_POINT('',(0.0133279664320278,-0.0341934961088841,0.0768752486147559));
#87259=CARTESIAN_POINT('Origin',(0.00812378219310841,-0.0315241814719618,
0.07415));
#87260=CARTESIAN_POINT('',(0.0134969077199765,-0.034210518019052,0.0768201164870552));
#87261=CARTESIAN_POINT('',(0.0135025988803252,-0.0341934961088739,0.076808633304035));
#87262=CARTESIAN_POINT('Origin',(-0.00112772924295306,-0.0345621720562641,
0.0690309917632668));
#87263=CARTESIAN_POINT('Origin',(-0.00155879843018354,-0.0345621029387208,
0.0699101917082476));
#87264=CARTESIAN_POINT('Origin',(-0.00154344515286301,-0.0345621724837831,
0.0698675467084598));
#87265=CARTESIAN_POINT('Ctrl Pts',(0.0132167325306213,-0.0346945769586966,
0.0768221450395019));
#87266=CARTESIAN_POINT('Ctrl Pts',(0.0132727016783422,-0.0345275153362944,
0.0767154711555767));
#87267=CARTESIAN_POINT('Ctrl Pts',(0.0133253305070886,-0.0343603235965186,
0.0766070095021413));
#87268=CARTESIAN_POINT('Ctrl Pts',(0.0133744681317945,-0.034193496108874,
0.0764970831740252));
#87269=CARTESIAN_POINT('Ctrl Pts',(0.0132540399932634,-0.0346945769586966,
0.0767470705321401));
#87270=CARTESIAN_POINT('Ctrl Pts',(0.0133084366753693,-0.0345275153362944,
0.0766396152284727));
#87271=CARTESIAN_POINT('Ctrl Pts',(0.013359468056849,-0.0343603235965186,
0.0765304214057763));
#87272=CARTESIAN_POINT('Ctrl Pts',(0.0134069880093603,-0.034193496108874,
0.0764198142540929));
#87273=CARTESIAN_POINT('Ctrl Pts',(0.0132913474559052,-0.0346945769586966,
0.07667199602478));
#87274=CARTESIAN_POINT('Ctrl Pts',(0.0133441716723965,-0.0345275153362944,
0.0765637593013699));
#87275=CARTESIAN_POINT('Ctrl Pts',(0.0133936056066094,-0.0343603235965186,
0.0764538333094117));
#87276=CARTESIAN_POINT('Ctrl Pts',(0.0134395078869257,-0.034193496108874,
0.0763425453341601));
#87277=CARTESIAN_POINT('Ctrl Pts',(0.0133286549185474,-0.0346945769586966,
0.0765969215174165));
#87278=CARTESIAN_POINT('Ctrl Pts',(0.0133799066694237,-0.0345275153362944,
0.0764879033742648));
#87279=CARTESIAN_POINT('Ctrl Pts',(0.01342774315637,-0.0343603235965186,
0.0763772452130463));
#87280=CARTESIAN_POINT('Ctrl Pts',(0.013472027764492,-0.034193496108874,
0.0762652764142282));
#87281=CARTESIAN_POINT('',(0.0133286549178141,-0.0346945769586966,0.0765969215188918));
#87282=CARTESIAN_POINT('',(0.0134247910408858,-0.0343667727836576,0.0763810155080322));
#87283=CARTESIAN_POINT('Origin',(-0.00196428515163209,-0.0345626474178896,
0.0696095594035448));
#87284=CARTESIAN_POINT('Origin',(0.0236115535692648,-0.0341934771024212,
0.0806682671964958));
#87285=CARTESIAN_POINT('',(0.0133750500022089,-0.034193496108874,0.076495700619667));
#87286=CARTESIAN_POINT('',(0.0133992944426288,-0.034193496108884,0.0764380945686997));
#87287=CARTESIAN_POINT('',(0.0132742440876453,-0.0345211942962611,0.0767094662085974));
#87288=CARTESIAN_POINT('Origin',(-0.00174733867117582,-0.034562559612015,
0.0691804641554648));
#87289=CARTESIAN_POINT('',(0.0132730274909841,-0.0346945769586885,0.0767088616340682));
#87290=CARTESIAN_POINT('Origin',(0.0231806829138335,-0.0346945685853897,
0.0816323643750059));
#87291=CARTESIAN_POINT('',(0.0133008412044091,-0.0346945769587026,0.07665289157649));
#87292=CARTESIAN_POINT('Ctrl Pts',(0.0133881187727655,-0.0345231616327842,
0.0770286733708747));
#87293=CARTESIAN_POINT('Ctrl Pts',(0.0134277972323351,-0.0344132092796988,
0.0769561119027172));
#87294=CARTESIAN_POINT('Ctrl Pts',(0.0134659727679454,-0.0343032738558979,
0.0768827334607597));
#87295=CARTESIAN_POINT('Ctrl Pts',(0.0135025988803292,-0.0341934961088739,
0.0768086333040446));
#87296=CARTESIAN_POINT('Ctrl Pts',(0.0133497210398409,-0.0345231616327842,
0.0769220584082974));
#87297=CARTESIAN_POINT('Ctrl Pts',(0.0133879299622532,-0.0344132092796988,
0.0768500261988285));
#87298=CARTESIAN_POINT('Ctrl Pts',(0.0134246469838261,-0.0343032738558979,
0.0767772073844693));
#87299=CARTESIAN_POINT('Ctrl Pts',(0.0134598274554525,-0.0341934961088739,
0.0767036964594516));
#87300=CARTESIAN_POINT('Ctrl Pts',(0.0133113233069162,-0.0345231616327842,
0.07681544344572));
#87301=CARTESIAN_POINT('Ctrl Pts',(0.0133480626921713,-0.0344132092796988,
0.0767439404949398));
#87302=CARTESIAN_POINT('Ctrl Pts',(0.0133833211997068,-0.0343032738558979,
0.0766716813081789));
#87303=CARTESIAN_POINT('Ctrl Pts',(0.0134170560305758,-0.0341934961088739,
0.0765987596148585));
#87304=CARTESIAN_POINT('Ctrl Pts',(0.0132729255739916,-0.0345231616327842,
0.0767088284831427));
#87305=CARTESIAN_POINT('Ctrl Pts',(0.0133081954220894,-0.0344132092796988,
0.0766378547910511));
#87306=CARTESIAN_POINT('Ctrl Pts',(0.0133419954155875,-0.0343032738558979,
0.0765661552318885));
#87307=CARTESIAN_POINT('Ctrl Pts',(0.013374284605699,-0.0341934961088739,
0.0764938227702655));
#87308=CARTESIAN_POINT('',(0.013438824441277,-0.0341934961088839,0.076652166961861));
#87309=CARTESIAN_POINT('Ctrl Pts',(0.0134969077168772,-0.0342105180195352,
0.0768201164855123));
#87310=CARTESIAN_POINT('Ctrl Pts',(0.0134584248250332,-0.0342610556240281,
0.0768009928295567));
#87311=CARTESIAN_POINT('Ctrl Pts',(0.013420632488783,-0.0343122189868086,
0.076782212337718));
#87312=CARTESIAN_POINT('Ctrl Pts',(0.0133463957991769,-0.0344158119695077,
0.0767453212195279));
#87313=CARTESIAN_POINT('Ctrl Pts',(0.0133099818093831,-0.0344681990449958,
0.0767272256820197));
#87314=CARTESIAN_POINT('Ctrl Pts',(0.0132742440876178,-0.0345211942962359,
0.0767094662085777));
#87315=CARTESIAN_POINT('Ctrl Pts',(0.0133267328974969,-0.0346945769586932,
0.0765975674323603));
#87316=CARTESIAN_POINT('Ctrl Pts',(0.0133773346222538,-0.0345296777079064,
0.0764900001081728));
#87317=CARTESIAN_POINT('Ctrl Pts',(0.0134234472521205,-0.0343648066255586,
0.076380433283139));
#87318=CARTESIAN_POINT('Ctrl Pts',(0.0133286549178102,-0.0346945769586932,
0.0765969215189));
#87319=CARTESIAN_POINT('Ctrl Pts',(0.0133792432887634,-0.0345296777079064,
0.0764893144583026));
#87320=CARTESIAN_POINT('Ctrl Pts',(0.0134253409338946,-0.0343648066255586,
0.076379708482738));
#87321=CARTESIAN_POINT('Ctrl Pts',(0.0136489789613425,-0.0346945769586932,
0.0764892735351842));
#87322=CARTESIAN_POINT('Ctrl Pts',(0.0136973417864045,-0.0345296777079064,
0.0763750440016491));
#87323=CARTESIAN_POINT('Ctrl Pts',(0.0137409420744539,-0.0343648066255586,
0.0762589131958239));
#87324=CARTESIAN_POINT('',(0.0136539630861568,-0.0346775396665029,0.0764774662798272));
#87325=CARTESIAN_POINT('',(0.0136489789613314,-0.0346945769586886,0.0764892735351852));
#87326=CARTESIAN_POINT('Origin',(-0.0017062658188191,-0.0345626617714647,
0.0701785561643568));
#87327=CARTESIAN_POINT('Ctrl Pts',(0.013653963084665,-0.0346775396670096,
0.0764774662808801));
#87328=CARTESIAN_POINT('Ctrl Pts',(0.0136143686579338,-0.034626974992875,
0.0764608023385011));
#87329=CARTESIAN_POINT('Ctrl Pts',(0.0135754778985822,-0.034575790289194,
0.0764444345846692));
#87330=CARTESIAN_POINT('Ctrl Pts',(0.0134990717526567,-0.0344721681090205,
0.0764122778154287));
#87331=CARTESIAN_POINT('Ctrl Pts',(0.0134615863230428,-0.0344197714291976,
0.0763965014017779));
#87332=CARTESIAN_POINT('Ctrl Pts',(0.0134247910409318,-0.0343667727834294,
0.0763810155087038));
#87333=CARTESIAN_POINT('',(0.0134888169395828,-0.0346945769587026,0.0765430975270484));
#87334=CARTESIAN_POINT('Origin',(0.00812378219310841,-0.0315241814719618,
0.07415));
#87335=CARTESIAN_POINT('',(0.013653963085355,-0.0347116136489593,0.0764774662786887));
#87336=CARTESIAN_POINT('',(0.0136589219806651,-0.0346945769586885,0.0764656484042733));
#87337=CARTESIAN_POINT('Origin',(-0.00172210266274787,-0.0345626700989541,
0.070221009531519));
#87338=CARTESIAN_POINT('Origin',(-0.00158778538746057,-0.0345626621003631,
0.0698970385973882));
#87339=CARTESIAN_POINT('Origin',(-0.00156849731980765,-0.0345626702685647,
0.0698560375039974));
#87340=CARTESIAN_POINT('Ctrl Pts',(0.0133592295312375,-0.0352450361874068,
0.0765309354874297));
#87341=CARTESIAN_POINT('Ctrl Pts',(0.0134490279866701,-0.0349452760959493,
0.0763334773509347));
#87342=CARTESIAN_POINT('Ctrl Pts',(0.01352369797937,-0.034644428984174,
0.0761298161851315));
#87343=CARTESIAN_POINT('Ctrl Pts',(0.0133602235947146,-0.0352450361874068,
0.0765286143965647));
#87344=CARTESIAN_POINT('Ctrl Pts',(0.0134499345087687,-0.0349452760959493,
0.0763311187683505));
#87345=CARTESIAN_POINT('Ctrl Pts',(0.0135245143847563,-0.034644428984174,
0.0761274268113129));
#87346=CARTESIAN_POINT('Ctrl Pts',(0.013458645721158,-0.0352450361874068,
0.0762988034198331));
#87347=CARTESIAN_POINT('Ctrl Pts',(0.0135396891719982,-0.0349452760959493,
0.076097595740208));
#87348=CARTESIAN_POINT('Ctrl Pts',(0.0136053466012218,-0.034644428984174,
0.0758908551461006));
#87349=CARTESIAN_POINT('Ctrl Pts',(0.0134596299424225,-0.0352450361874068,
0.0762965053100657));
#87350=CARTESIAN_POINT('Ctrl Pts',(0.0135405867186305,-0.0349452760959493,
0.0760952605099267));
#87351=CARTESIAN_POINT('Ctrl Pts',(0.0136061549233864,-0.034644428984174,
0.0758884894294485));
#87352=CARTESIAN_POINT('',(0.0134720180698563,-0.0351951634053353,0.0762653073793554));
#87353=CARTESIAN_POINT('',(0.0135544173333601,-0.0348678972925388,0.0760437600094691));
#87354=CARTESIAN_POINT('Origin',(-0.00239959961656829,-0.0345636767894925,
0.070927119634889));
#87355=CARTESIAN_POINT('Origin',(0.0239880660027397,-0.0346946199340779,
0.0796821614080363));
#87356=CARTESIAN_POINT('',(0.0135119755788547,-0.0346945769330288,0.0761613420982109));
#87357=CARTESIAN_POINT('',(0.0135325550677313,-0.0346945769458128,0.0761023273905086));
#87358=CARTESIAN_POINT('',(0.0134247910405553,-0.0350221583435276,0.0763810155085277));
#87359=CARTESIAN_POINT('Origin',(-0.00228105547016616,-0.0345628458718364,
0.0704611897290196));
#87360=CARTESIAN_POINT('',(0.0134236498346712,-0.0351951360298762,0.0763805384950308));
#87361=CARTESIAN_POINT('Origin',(0.0235798061659101,-0.0351951838366828,
0.080654919438589));
#87362=CARTESIAN_POINT('',(0.0134720277639559,-0.0351951371328746,0.0762652764158017));
#87363=CARTESIAN_POINT('Ctrl Pts',(0.0135584846106547,-0.0350241211494343,
0.0766924416675349));
#87364=CARTESIAN_POINT('Ctrl Pts',(0.0135935057021833,-0.0349144232818962,
0.076617580870048));
#87365=CARTESIAN_POINT('Ctrl Pts',(0.0136270003293466,-0.0348045283579412,
0.0765419513537787));
#87366=CARTESIAN_POINT('Ctrl Pts',(0.0136589219849586,-0.0346945769439157,
0.076465648394031));
#87367=CARTESIAN_POINT('Ctrl Pts',(0.0135134682114149,-0.0350241211494343,
0.0765884480831026));
#87368=CARTESIAN_POINT('Ctrl Pts',(0.013547056833957,-0.0349144232818962,
0.0765142073680578));
#87369=CARTESIAN_POINT('Ctrl Pts',(0.0135791309522792,-0.0348045283579412,
0.0764392279155374));
#87370=CARTESIAN_POINT('Ctrl Pts',(0.0136096459096716,-0.0346945769439157,
0.0763636042359037));
#87371=CARTESIAN_POINT('Ctrl Pts',(0.0134684518121751,-0.0350241211494343,
0.0764844544986704));
#87372=CARTESIAN_POINT('Ctrl Pts',(0.0135006079657307,-0.0349144232818962,
0.0764108338660676));
#87373=CARTESIAN_POINT('Ctrl Pts',(0.0135312615752117,-0.0348045283579412,
0.076336504477296));
#87374=CARTESIAN_POINT('Ctrl Pts',(0.0135603698343847,-0.0346945769439157,
0.0762615600777764));
#87375=CARTESIAN_POINT('Ctrl Pts',(0.0134234354129353,-0.0350241211494343,
0.0763804609142381));
#87376=CARTESIAN_POINT('Ctrl Pts',(0.0134541590975043,-0.0349144232818962,
0.0763074603640774));
#87377=CARTESIAN_POINT('Ctrl Pts',(0.0134833921981443,-0.0348045283579412,
0.0762337810390547));
#87378=CARTESIAN_POINT('Ctrl Pts',(0.0135110937590977,-0.0346945769439157,
0.0761595159196492));
#87379=CARTESIAN_POINT('',(0.0135854487797405,-0.0346945769458128,0.0763134952515503));
#87380=CARTESIAN_POINT('Ctrl Pts',(0.0136539630823187,-0.0347116136492757,
0.0764774662774077));
#87381=CARTESIAN_POINT('Ctrl Pts',(0.0136143843844361,-0.0347621546531239,
0.0764608089407906));
#87382=CARTESIAN_POINT('Ctrl Pts',(0.0135755015870122,-0.0348133084094881,
0.0764444444851627));
#87383=CARTESIAN_POINT('Ctrl Pts',(0.0134990953424351,-0.0349168561544565,
0.076412287678505));
#87384=CARTESIAN_POINT('Ctrl Pts',(0.0134616022019935,-0.0349692089015922,
0.076396508082546));
#87385=CARTESIAN_POINT('Ctrl Pts',(0.0134247910405293,-0.0350221583435,
0.0763810155084952));
#87386=CARTESIAN_POINT('Ctrl Pts',(0.0134706729621182,-0.0351951371254983,
0.0762658286221963));
#87387=CARTESIAN_POINT('Ctrl Pts',(0.0135144163913672,-0.0350307338980975,
0.0761552850102975));
#87388=CARTESIAN_POINT('Ctrl Pts',(0.0135535535553534,-0.0348659306897824,
0.0760430278941345));
#87389=CARTESIAN_POINT('Ctrl Pts',(0.0134720277638447,-0.0351951371254983,
0.0762652764157668));
#87390=CARTESIAN_POINT('Ctrl Pts',(0.0135157597765723,-0.0350307338980975,
0.0761547047941924));
#87391=CARTESIAN_POINT('Ctrl Pts',(0.0135548843761222,-0.0348659306897824,
0.076042420164145));
#87392=CARTESIAN_POINT('Ctrl Pts',(0.0136990939452612,-0.0351951371254983,
0.0761727260426533));
#87393=CARTESIAN_POINT('Ctrl Pts',(0.0137409125370927,-0.0350307338980975,
0.0760574599702441));
#87394=CARTESIAN_POINT('Ctrl Pts',(0.013777931324035,-0.0348659306897824,
0.0759405639844929));
#87395=CARTESIAN_POINT('Origin',(0.0185760316857582,-0.0308609197410827,
0.0777948871241319));
#87396=CARTESIAN_POINT('',(0.0135710234992805,-0.0351951371254983,0.0762249265398228));
#87397=CARTESIAN_POINT('Origin',(0.00716427942480549,-0.0351840467441103,
0.0739653379084833));
#87398=CARTESIAN_POINT('Origin',(0.0196585700113253,-0.0352322614166343,
0.0773307555606667));
#87399=CARTESIAN_POINT('',(0.0136277018975404,-0.0351951142564687,0.0758187367888895));
#87400=CARTESIAN_POINT('',(0.0136613030716997,-0.0351951372916787,0.0756986647536401));
#87401=CARTESIAN_POINT('Origin',(0.00802995437358576,-0.0352875123094998,
0.0738225773521353));
#87402=CARTESIAN_POINT('Origin',(0.00475687541542284,-0.0298325076522812,
0.0808551568982295));
#87403=CARTESIAN_POINT('Origin',(0.0147521803846405,-0.033873240455648,
0.0792797391933933));
#87404=CARTESIAN_POINT('Ctrl Pts',(0.0115954196712322,-0.0321934096636941,
0.0787353973618213));
#87405=CARTESIAN_POINT('Ctrl Pts',(0.0116774961003548,-0.0320508460845284,
0.0786732567042231));
#87406=CARTESIAN_POINT('Ctrl Pts',(0.0117578410467241,-0.0319086045664984,
0.0786089576691867));
#87407=CARTESIAN_POINT('Ctrl Pts',(0.0118362929113632,-0.0317669892870756,
0.0785426529460147));
#87408=CARTESIAN_POINT('Ctrl Pts',(0.0116611528836329,-0.0321934096636941,
0.0786833437604548));
#87409=CARTESIAN_POINT('Ctrl Pts',(0.0117422975780799,-0.0320508460845284,
0.078620026509658));
#87410=CARTESIAN_POINT('Ctrl Pts',(0.0118216798795671,-0.0319086045664984,
0.0785545768024505));
#87411=CARTESIAN_POINT('Ctrl Pts',(0.0118991404658326,-0.0317669892870756,
0.0784871496350933));
#87412=CARTESIAN_POINT('Ctrl Pts',(0.0117268860960335,-0.0321934096636941,
0.0786312901590883));
#87413=CARTESIAN_POINT('Ctrl Pts',(0.0118070990558051,-0.0320508460845284,
0.0785667963150929));
#87414=CARTESIAN_POINT('Ctrl Pts',(0.0118855187124101,-0.0319086045664984,
0.0785001959357143));
#87415=CARTESIAN_POINT('Ctrl Pts',(0.011961988020302,-0.0317669892870756,
0.0784316463241718));
#87416=CARTESIAN_POINT('Ctrl Pts',(0.0117926193084342,-0.0321934096636941,
0.0785792365577218));
#87417=CARTESIAN_POINT('Ctrl Pts',(0.0118719005335303,-0.0320508460845284,
0.0785135661205279));
#87418=CARTESIAN_POINT('Ctrl Pts',(0.0119493575452532,-0.0319086045664984,
0.0784458150689781));
#87419=CARTESIAN_POINT('Ctrl Pts',(0.0120248355747714,-0.0317669892870756,
0.0783761430132503));
#87420=CARTESIAN_POINT('',(0.0117914433282733,-0.0321934096636941,0.0785801678069348));
#87421=CARTESIAN_POINT('',(0.0119703582003404,-0.0318665617511361,0.0784257429775266));
#87422=CARTESIAN_POINT('Origin',(0.00161643164797298,-0.0326371944421894,
0.0653254689367773));
#87423=CARTESIAN_POINT('Origin',(0.0193013276456433,-0.031693926150848,
0.0865746372135666));
#87424=CARTESIAN_POINT('',(0.0116944699207213,-0.0320197221621754,0.0786586337529689));
#87425=CARTESIAN_POINT('Ctrl Pts',(0.01169463942301,-0.0320197392094672,
0.0786585596999187));
#87426=CARTESIAN_POINT('Ctrl Pts',(0.0117175803950843,-0.031979271657597,
0.0786403899935351));
#87427=CARTESIAN_POINT('Ctrl Pts',(0.0117404872846657,-0.0319386439829661,
0.0786219626789956));
#87428=CARTESIAN_POINT('Ctrl Pts',(0.0117633788384472,-0.0318979099381593,
0.0786032518212021));
#87429=CARTESIAN_POINT('Ctrl Pts',(0.01178626993976,-0.0318571766984914,
0.0785845413332429));
#87430=CARTESIAN_POINT('Ctrl Pts',(0.0118090304859134,-0.0318163871833585,
0.078565643791654));
#87431=CARTESIAN_POINT('Ctrl Pts',(0.011831584439305,-0.0317755399638303,
0.078546626905285));
#87432=CARTESIAN_POINT('',(0.0116934483446432,-0.0321934096636182,0.0786577692450465));
#87433=CARTESIAN_POINT('Origin',(0.0131427450436533,-0.0324112239851953,
0.0804540644982482));
#87434=CARTESIAN_POINT('',(0.0117424458364682,-0.0321934096636662,0.0786189685260008));
#87435=CARTESIAN_POINT('Ctrl Pts',(0.0117894286472563,-0.0321934096636617,
0.0785799338245015));
#87436=CARTESIAN_POINT('Ctrl Pts',(0.0118505208871847,-0.0320835708272591,
0.078529381703061));
#87437=CARTESIAN_POINT('Ctrl Pts',(0.0119105315176052,-0.0319739230346488,
0.0784775946031752));
#87438=CARTESIAN_POINT('Ctrl Pts',(0.0119693888441963,-0.0318646057455572,
0.0784246446754529));
#87439=CARTESIAN_POINT('Ctrl Pts',(0.0119019909217039,-0.0321934096636617,
0.0785930066641706));
#87440=CARTESIAN_POINT('Ctrl Pts',(0.0119632634462797,-0.0320835708272591,
0.0785409022212396));
#87441=CARTESIAN_POINT('Ctrl Pts',(0.0120234221315626,-0.0319739230346488,
0.0784875599692914));
#87442=CARTESIAN_POINT('Ctrl Pts',(0.0120823952465098,-0.0318646057455572,
0.0784330540631819));
#87443=CARTESIAN_POINT('Ctrl Pts',(0.0120145531961515,-0.0321934096636617,
0.0786060795038397));
#87444=CARTESIAN_POINT('Ctrl Pts',(0.0120760060053747,-0.0320835708272591,
0.0785524227394181));
#87445=CARTESIAN_POINT('Ctrl Pts',(0.0121363127455201,-0.0319739230346488,
0.0784975253354075));
#87446=CARTESIAN_POINT('Ctrl Pts',(0.0121954016488234,-0.0318646057455572,
0.0784414634509109));
#87447=CARTESIAN_POINT('Ctrl Pts',(0.0121271154705991,-0.0321934096636617,
0.0786191523435088));
#87448=CARTESIAN_POINT('Ctrl Pts',(0.0121887485644697,-0.0320835708272591,
0.0785639432575967));
#87449=CARTESIAN_POINT('Ctrl Pts',(0.0122492033594775,-0.0319739230346488,
0.0785074907015237));
#87450=CARTESIAN_POINT('Ctrl Pts',(0.0123084080511369,-0.0318646057455572,
0.0784498728386399));
#87451=CARTESIAN_POINT('',(0.012136652526081,-0.0321763980308519,0.0786105909550923));
#87452=CARTESIAN_POINT('',(0.0121271154706063,-0.0321934096636184,0.078619152343485));
#87453=CARTESIAN_POINT('Origin',(0.00153306867489026,-0.0326386230729961,
0.0659066505538681));
#87454=CARTESIAN_POINT('Ctrl Pts',(0.0121366525239549,-0.0321763980306382,
0.0786105909527295));
#87455=CARTESIAN_POINT('Ctrl Pts',(0.0121079478650179,-0.0321259596176269,
0.0785786836815249));
#87456=CARTESIAN_POINT('Ctrl Pts',(0.0120797405515362,-0.0320749164634262,
0.078547329245198));
#87457=CARTESIAN_POINT('Ctrl Pts',(0.0120242979148881,-0.0319716057794031,
0.0784857008089321));
#87458=CARTESIAN_POINT('Ctrl Pts',(0.0119970841942555,-0.0319193786690225,
0.0784554508217467));
#87459=CARTESIAN_POINT('Ctrl Pts',(0.0119703581990953,-0.0318665617525441,
0.0784257429761435));
#87460=CARTESIAN_POINT('',(0.0119592793994498,-0.0321934096636663,0.07859966007522));
#87461=CARTESIAN_POINT('Origin',(0.00812378219310841,-0.0315241814719618,
0.07415));
#87462=CARTESIAN_POINT('',(0.0121366525263274,-0.0322104233323596,0.0786105909553662));
#87463=CARTESIAN_POINT('',(0.0121461712749854,-0.0321934096636183,0.0786020092176462));
#87464=CARTESIAN_POINT('Origin',(0.00149547255801582,-0.0326387244654018,
0.0659319795943699));
#87465=CARTESIAN_POINT('Origin',(0.000620872838852224,-0.0326386236434395,
0.0667272857683929));
#87466=CARTESIAN_POINT('Origin',(0.000650024392563257,-0.0326387248628074,
0.0666925696519535));
#87467=CARTESIAN_POINT('Ctrl Pts',(0.0118490568003921,-0.0327445246967096,
0.0785318322766084));
#87468=CARTESIAN_POINT('Ctrl Pts',(0.0120143203063967,-0.0324436878339359,
0.078391331247914));
#87469=CARTESIAN_POINT('Ctrl Pts',(0.0121685312045189,-0.0321434074405927,
0.0782387810450908));
#87470=CARTESIAN_POINT('Ctrl Pts',(0.0120359618642719,-0.0327445246967096,
0.0783658006618596));
#87471=CARTESIAN_POINT('Ctrl Pts',(0.0121949633855566,-0.0324436878339359,
0.0782182503934416));
#87472=CARTESIAN_POINT('Ctrl Pts',(0.0123423991110496,-0.0321434074405927,
0.0780591426553223));
#87473=CARTESIAN_POINT('',(0.0120623785749811,-0.0326943950436612,0.0783411315346456));
#87474=CARTESIAN_POINT('',(0.0122312439848547,-0.0323666188837389,0.0781757772702107));
#87475=CARTESIAN_POINT('Origin',(0.000494774121628024,-0.0326395579112568,
0.0661428289707638));
#87476=CARTESIAN_POINT('Origin',(0.0201189997075469,-0.0321933825603027,
0.0859066686481697));
#87477=CARTESIAN_POINT('',(0.0121427775269064,-0.0321934096532689,0.0782640978967223));
#87478=CARTESIAN_POINT('',(0.012186525641443,-0.0321934096584274,0.0782194621171241));
#87479=CARTESIAN_POINT('',(0.0119703582009599,-0.0325210109756239,0.0784257429782228));
#87480=CARTESIAN_POINT('Origin',(0.000862044000621341,-0.0326393129157105,
0.0658325109636758));
#87481=CARTESIAN_POINT('',(0.0119694495967206,-0.0326943950436593,0.0784247329999422));
#87482=CARTESIAN_POINT('Origin',(0.0193681487055648,-0.0326943765538236,
0.0866489149168529));
#87483=CARTESIAN_POINT('',(0.0120159140858608,-0.0326943950436702,0.078382932267304));
#87484=CARTESIAN_POINT('Ctrl Pts',(0.0119587280979391,-0.0325229783203769,
0.0787644544538986));
#87485=CARTESIAN_POINT('Ctrl Pts',(0.0120223382516747,-0.032413025309245,
0.0787115898084653));
#87486=CARTESIAN_POINT('Ctrl Pts',(0.0120848451845838,-0.0323031222208069,
0.0786574173232481));
#87487=CARTESIAN_POINT('Ctrl Pts',(0.0121461712783128,-0.0321934096576658,
0.078602009214648));
#87488=CARTESIAN_POINT('Ctrl Pts',(0.0119622743777968,-0.0325229783203769,
0.078651191193589));
#87489=CARTESIAN_POINT('Ctrl Pts',(0.0120243231999659,-0.032413025309245,
0.0785982776627653));
#87490=CARTESIAN_POINT('Ctrl Pts',(0.012085268026858,-0.0323031222208069,
0.0785440885977215));
#87491=CARTESIAN_POINT('Ctrl Pts',(0.0121450332418156,-0.0321934096576658,
0.078488696165489));
#87492=CARTESIAN_POINT('Ctrl Pts',(0.0119658206576546,-0.0325229783203769,
0.0785379279332794));
#87493=CARTESIAN_POINT('Ctrl Pts',(0.0120263081482572,-0.032413025309245,
0.0784849655170654));
#87494=CARTESIAN_POINT('Ctrl Pts',(0.0120856908691323,-0.0323031222208069,
0.0784307598721948));
#87495=CARTESIAN_POINT('Ctrl Pts',(0.0121438952053184,-0.0321934096576658,
0.0783753831163299));
#87496=CARTESIAN_POINT('Ctrl Pts',(0.0119693669375123,-0.0325229783203769,
0.0784246646729697));
#87497=CARTESIAN_POINT('Ctrl Pts',(0.0120282930965484,-0.032413025309245,
0.0783716533713655));
#87498=CARTESIAN_POINT('Ctrl Pts',(0.0120861137114065,-0.0323031222208069,
0.0783174311466682));
#87499=CARTESIAN_POINT('Ctrl Pts',(0.0121427571688211,-0.0321934096576658,
0.0782620700671708));
#87500=CARTESIAN_POINT('',(0.0121444744006986,-0.0321934096584275,0.0784330535576338));
#87501=CARTESIAN_POINT('Ctrl Pts',(0.0121366525239949,-0.0322104233328902,
0.078610590952774));
#87502=CARTESIAN_POINT('Ctrl Pts',(0.0121079089697485,-0.0322609421830583,
0.078578640446665));
#87503=CARTESIAN_POINT('Ctrl Pts',(0.0120796826552531,-0.0323120888239129,
0.0785472648893489));
#87504=CARTESIAN_POINT('Ctrl Pts',(0.0120242395988951,-0.0324156524631811,
0.0784856359865455));
#87505=CARTESIAN_POINT('Ctrl Pts',(0.0119970456471616,-0.032468026716731,
0.0784554079739085));
#87506=CARTESIAN_POINT('Ctrl Pts',(0.0119703582009342,-0.0325210109755912,
0.0784257429781876));
#87507=CARTESIAN_POINT('Origin',(0.00168338772958699,-0.0262834582510625,
0.0786693699777735));
#87508=CARTESIAN_POINT('Origin',(0.0113525993087552,-0.0342770963326899,
0.0858717464226988));
#87509=CARTESIAN_POINT('Ctrl Pts',(0.0120603536691667,-0.0326943950436604,
0.0783410245427036));
#87510=CARTESIAN_POINT('Ctrl Pts',(0.0121181138421823,-0.0325844576448134,
0.0782867712098422));
#87511=CARTESIAN_POINT('Ctrl Pts',(0.0121747560551019,-0.0324744968375322,
0.0782313194623111));
#87512=CARTESIAN_POINT('Ctrl Pts',(0.0122302087145849,-0.0323646534831895,
0.0781747413491271));
#87513=CARTESIAN_POINT('Ctrl Pts',(0.012173514514236,-0.0326943950436604,
0.0783470037337604));
#87514=CARTESIAN_POINT('Ctrl Pts',(0.0122313570917106,-0.0325844576448134,
0.0782911908323679));
#87515=CARTESIAN_POINT('Ctrl Pts',(0.0122880494604869,-0.0324744968375322,
0.0782341777016734));
#87516=CARTESIAN_POINT('Ctrl Pts',(0.012343519990555,-0.0323646534831895,
0.0781760383921151));
#87517=CARTESIAN_POINT('Ctrl Pts',(0.0122866753593053,-0.0326943950436604,
0.0783529829248173));
#87518=CARTESIAN_POINT('Ctrl Pts',(0.0123446003412388,-0.0325844576448134,
0.0782956104548937));
#87519=CARTESIAN_POINT('Ctrl Pts',(0.0124013428658719,-0.0324744968375322,
0.0782370359410357));
#87520=CARTESIAN_POINT('Ctrl Pts',(0.0124568312665252,-0.0323646534831895,
0.078177335435103));
#87521=CARTESIAN_POINT('Ctrl Pts',(0.0123998362043746,-0.0326943950436604,
0.0783589621158741));
#87522=CARTESIAN_POINT('Ctrl Pts',(0.0124578435907671,-0.0325844576448134,
0.0783000300774195));
#87523=CARTESIAN_POINT('Ctrl Pts',(0.0125146362712568,-0.0324744968375322,
0.078239894180398));
#87524=CARTESIAN_POINT('Ctrl Pts',(0.0125701425424953,-0.0323646534831895,
0.078178632478091));
#87525=CARTESIAN_POINT('',(0.0124088168667548,-0.0326773559991213,0.078349818784899));
#87526=CARTESIAN_POINT('',(0.0123998362043608,-0.0326943950436594,0.0783589621158728));
#87527=CARTESIAN_POINT('Origin',(0.000514714023868693,-0.0326395669367224,
0.066762600728777));
#87528=CARTESIAN_POINT('Ctrl Pts',(0.0124088168643565,-0.0326773559987506,
0.0783498187825483));
#87529=CARTESIAN_POINT('Ctrl Pts',(0.0123781407071167,-0.0326267922587182,
0.0783197526777822));
#87530=CARTESIAN_POINT('Ctrl Pts',(0.0123480082626104,-0.0325756109581767,
0.07829021947301));
#87531=CARTESIAN_POINT('Ctrl Pts',(0.0122888051545989,-0.0324719985462387,
0.0782321937289757));
#87532=CARTESIAN_POINT('Ctrl Pts',(0.0122597582360467,-0.0324196091621789,
0.078203724462454));
#87533=CARTESIAN_POINT('Ctrl Pts',(0.0122312439848199,-0.0323666188837756,
0.0781757772701765));
#87534=CARTESIAN_POINT('',(0.0122311073896809,-0.0326943950436703,0.0783500468252692));
#87535=CARTESIAN_POINT('Origin',(0.00812378219310841,-0.0315241814719618,
0.07415));
#87536=CARTESIAN_POINT('',(0.0124088168667217,-0.0327114338379851,0.0783498187848666));
#87537=CARTESIAN_POINT('',(0.012417777980685,-0.0326943950436593,0.0783406562942192));
#87538=CARTESIAN_POINT('Origin',(0.000483558929968489,-0.032639568145509,
0.0667954986120342));
#87539=CARTESIAN_POINT('Origin',(0.000585047604623338,-0.032639567204889,
0.0666908392600542));
#87540=CARTESIAN_POINT('Origin',(0.000617313923548154,-0.0326395685020944,
0.066659030667844));
#87541=CARTESIAN_POINT('Ctrl Pts',(0.0121168715764049,-0.0332451089994433,
0.0782892465711775));
#87542=CARTESIAN_POINT('Ctrl Pts',(0.0122729858149996,-0.0329451141710253,
0.0781386447411115));
#87543=CARTESIAN_POINT('Ctrl Pts',(0.0124173126040131,-0.0326442513127493,
0.0779767115922992));
#87544=CARTESIAN_POINT('Ctrl Pts',(0.0122929814043604,-0.0332451089994433,
0.0781118055147743));
#87545=CARTESIAN_POINT('Ctrl Pts',(0.0124424033440211,-0.0329451141710253,
0.0779545615938766));
#87546=CARTESIAN_POINT('Ctrl Pts',(0.012579556536781,-0.0326442513127493,
0.0777865093150257));
#87547=CARTESIAN_POINT('Ctrl Pts',(0.0122947425026399,-0.0332451089994433,
0.0781100311042103));
#87548=CARTESIAN_POINT('Ctrl Pts',(0.0124440975193113,-0.0329451141710253,
0.0779527207624043));
#87549=CARTESIAN_POINT('Ctrl Pts',(0.0125811789761087,-0.0326442513127493,
0.077784607292253));
#87550=CARTESIAN_POINT('',(0.0123177699811848,-0.0331951640388616,0.0780855547809003));
#87551=CARTESIAN_POINT('',(0.0124759195072863,-0.0328677532355047,0.0779099236519366));
#87552=CARTESIAN_POINT('Origin',(-0.000419516393849347,-0.0326402808282463,
0.0671862986931509));
#87553=CARTESIAN_POINT('Origin',(0.0208423773160607,-0.0326944278779179,
0.0851374243729753));
#87554=CARTESIAN_POINT('',(0.0123931733065714,-0.0326943950436593,0.0780036248546381));
#87555=CARTESIAN_POINT('',(0.0124340323883481,-0.0326943950436694,0.0779563301885937));
#87556=CARTESIAN_POINT('',(0.0122312439848527,-0.0330220786163545,0.0781757772702127));
#87557=CARTESIAN_POINT('Origin',(-0.000129652753292978,-0.0326396682763325,
0.0668027211718298));
#87558=CARTESIAN_POINT('',(0.0122302737564742,-0.0331951640388587,0.078174826336627));
#87559=CARTESIAN_POINT('Origin',(0.0201087757104031,-0.0331952026560029,
0.0858966510234808));
#87560=CARTESIAN_POINT('',(0.0122740218688395,-0.0331951640388701,0.0781301905587737));
#87561=CARTESIAN_POINT('Ctrl Pts',(0.0122409053996857,-0.0330240426238172,
0.0785145499770249));
#87562=CARTESIAN_POINT('Ctrl Pts',(0.0123010313277942,-0.0329142774063519,
0.0784578325937355));
#87563=CARTESIAN_POINT('Ctrl Pts',(0.0123600147241259,-0.0328043479726691,
0.0783998439638745));
#87564=CARTESIAN_POINT('Ctrl Pts',(0.0124177779806857,-0.0326943950436593,
0.0783406562942282));
#87565=CARTESIAN_POINT('Ctrl Pts',(0.0122373328055426,-0.0330240426238172,
0.0784012875712757));
#87566=CARTESIAN_POINT('Ctrl Pts',(0.0122958984336657,-0.0329142774063519,
0.0783446194039512));
#87567=CARTESIAN_POINT('Ctrl Pts',(0.0123533217695771,-0.0328043479726691,
0.0782867122703503));
#87568=CARTESIAN_POINT('Ctrl Pts',(0.0124095272067103,-0.0326943950436593,
0.0782276383278962));
#87569=CARTESIAN_POINT('Ctrl Pts',(0.0122337602113996,-0.0330240426238172,
0.0782880251655264));
#87570=CARTESIAN_POINT('Ctrl Pts',(0.0122907655395373,-0.0329142774063519,
0.0782314062141669));
#87571=CARTESIAN_POINT('Ctrl Pts',(0.0123466288150282,-0.032804347972669,
0.078173580576826));
#87572=CARTESIAN_POINT('Ctrl Pts',(0.0124012764327349,-0.0326943950436593,
0.0781146203615641));
#87573=CARTESIAN_POINT('Ctrl Pts',(0.0122301876172566,-0.0330240426238172,
0.0781747627597772));
#87574=CARTESIAN_POINT('Ctrl Pts',(0.0122856326454088,-0.0329142774063519,
0.0781181930243826));
#87575=CARTESIAN_POINT('Ctrl Pts',(0.0123399358604794,-0.032804347972669,
0.0780604488833018));
#87576=CARTESIAN_POINT('Ctrl Pts',(0.0123930256587595,-0.0326943950436593,
0.0780016023952321));
#87577=CARTESIAN_POINT('',(0.0124054756436382,-0.0326943950436693,0.0781721405744387));
#87578=CARTESIAN_POINT('Ctrl Pts',(0.0124088168643483,-0.0327114338383293,
0.0783498187825402));
#87579=CARTESIAN_POINT('Ctrl Pts',(0.0123781458095351,-0.03276198768302,
0.0783197576787295));
#87580=CARTESIAN_POINT('Ctrl Pts',(0.0123480158572798,-0.032813156260278,
0.0782902269166453));
#87581=CARTESIAN_POINT('Ctrl Pts',(0.0122888128036875,-0.0329167375858768,
0.0782322012259481));
#87582=CARTESIAN_POINT('Ctrl Pts',(0.0122597632920272,-0.0329691088920627,
0.078203729417887));
#87583=CARTESIAN_POINT('Ctrl Pts',(0.0122312439848207,-0.0330220786163187,
0.0781757772701774));
#87584=CARTESIAN_POINT('Ctrl Pts',(0.0123157420292715,-0.0331951640388604,
0.0780855751482224));
#87585=CARTESIAN_POINT('Ctrl Pts',(0.012397107522205,-0.0330306422010619,
0.0779989090662443));
#87586=CARTESIAN_POINT('Ctrl Pts',(0.0124748214885866,-0.0328657861914645,
0.0779089541184372));
#87587=CARTESIAN_POINT('Ctrl Pts',(0.0123177699811826,-0.0331951640388604,
0.0780855547809025));
#87588=CARTESIAN_POINT('Ctrl Pts',(0.0123991350530348,-0.0330306422010619,
0.0779988467723189));
#87589=CARTESIAN_POINT('Ctrl Pts',(0.0124768468658241,-0.0328657861914645,
0.0779088499511359));
#87590=CARTESIAN_POINT('Ctrl Pts',(0.0126556813064915,-0.0331951640388604,
0.0780821610376819));
#87591=CARTESIAN_POINT('Ctrl Pts',(0.0127369762148785,-0.0330306422010619,
0.077988466929096));
#87592=CARTESIAN_POINT('Ctrl Pts',(0.012814329181297,-0.0328657861914645,
0.0778914928774142));
#87593=CARTESIAN_POINT('',(0.0126640701336466,-0.0331781648281957,0.0780724718498676));
#87594=CARTESIAN_POINT('',(0.0126556813064761,-0.0331951640388588,0.0780821610376811));
#87595=CARTESIAN_POINT('Origin',(-0.000292616017096561,-0.0326412092982242,
0.0678201178075067));
#87596=CARTESIAN_POINT('Ctrl Pts',(0.0126640701318514,-0.033178164828644,
0.0780724718503024));
#87597=CARTESIAN_POINT('Ctrl Pts',(0.0126315442553613,-0.0331276811546764,
0.0780443719227299));
#87598=CARTESIAN_POINT('Ctrl Pts',(0.0125996056733662,-0.033076566349777,
0.0780167794184189));
#87599=CARTESIAN_POINT('Ctrl Pts',(0.0125368757635288,-0.0329730614463296,
0.0779625854268184));
#87600=CARTESIAN_POINT('Ctrl Pts',(0.0125061097806984,-0.0329207133373935,
0.0779360058286567));
#87601=CARTESIAN_POINT('Ctrl Pts',(0.0124759195047419,-0.03286775322894,
0.0779099236682114));
#87602=CARTESIAN_POINT('',(0.0124867256438404,-0.0331951640388701,0.0780838579093006));
#87603=CARTESIAN_POINT('Origin',(0.00812378219310841,-0.0315241814719618,
0.07415));
#87604=CARTESIAN_POINT('',(0.0126640701328944,-0.0332121607144207,0.0780724718483633));
#87605=CARTESIAN_POINT('',(0.0126724382467511,-0.0331951640388587,0.0780627647649284));
#87606=CARTESIAN_POINT('Origin',(-0.000315876451106127,-0.0326413667720304,
0.0678590414940439));
#87607=CARTESIAN_POINT('Origin',(0.000638664815378747,-0.0326412093957853,
0.0667421529359667));
#87608=CARTESIAN_POINT('Origin',(0.000673798557899307,-0.0326413668042006,
0.0667134867922949));
#87609=CARTESIAN_POINT('Ctrl Pts',(0.012368883514552,-0.0337436976235975,
0.0780303659325736));
#87610=CARTESIAN_POINT('Ctrl Pts',(0.0124037841138351,-0.0336723290703325,
0.0779921848479258));
#87611=CARTESIAN_POINT('Ctrl Pts',(0.012437992309655,-0.033601104548885,
0.0779533821883012));
#87612=CARTESIAN_POINT('Ctrl Pts',(0.0125472123026462,-0.0333736987606857,
0.0778294929824934));
#87613=CARTESIAN_POINT('Ctrl Pts',(0.0126491428327614,-0.0331450831799191,
0.077699540263341));
#87614=CARTESIAN_POINT('Ctrl Pts',(0.0125335048953521,-0.0337436976235975,
0.0778422175842325));
#87615=CARTESIAN_POINT('Ctrl Pts',(0.0125667132598756,-0.0336723290703325,
0.0778025558699368));
#87616=CARTESIAN_POINT('Ctrl Pts',(0.0125992028628391,-0.033601104548885,
0.0777623032581647));
#87617=CARTESIAN_POINT('Ctrl Pts',(0.0127029357292737,-0.0333736987606857,
0.0776337846423694));
#87618=CARTESIAN_POINT('Ctrl Pts',(0.0127991225129448,-0.0331450831799191,
0.0774995250250913));
#87619=CARTESIAN_POINT('Ctrl Pts',(0.0125351511091601,-0.0337436976235975,
0.0778403361007492));
#87620=CARTESIAN_POINT('Ctrl Pts',(0.012568342551336,-0.0336723290703325,
0.0778006595801569));
#87621=CARTESIAN_POINT('Ctrl Pts',(0.0126008149683709,-0.033601104548885,
0.0777603924688633));
#87622=CARTESIAN_POINT('Ctrl Pts',(0.01270449296354,-0.0333736987606857,
0.0776318275589682));
#87623=CARTESIAN_POINT('Ctrl Pts',(0.0128006223097466,-0.0331450831799191,
0.0774975248727087));
#87624=CARTESIAN_POINT('',(0.0125566096336481,-0.0336938721132548,0.0778144461904084));
#87625=CARTESIAN_POINT('',(0.012703419113583,-0.0333679870047996,0.0776292313341869));
#87626=CARTESIAN_POINT('Ctrl Pts',(0.0125566096336415,-0.033693872113258,
0.077814446190417));
#87627=CARTESIAN_POINT('Ctrl Pts',(0.0125709136861504,-0.0336629187933925,
0.0777971427854336));
#87628=CARTESIAN_POINT('Ctrl Pts',(0.0125851118454865,-0.0336319952301064,
0.0777797611585158));
#87629=CARTESIAN_POINT('Ctrl Pts',(0.0125992028628405,-0.0336011045488974,
0.0777623032581634));
#87630=CARTESIAN_POINT('Ctrl Pts',(0.0126345620470564,-0.0335235892595478,
0.0777184954124219));
#87631=CARTESIAN_POINT('Ctrl Pts',(0.0126693092926114,-0.0334458668665594,
0.0776741293533719));
#87632=CARTESIAN_POINT('Ctrl Pts',(0.0127034191066276,-0.0333679869962518,
0.0776292313437298));
#87633=CARTESIAN_POINT('Ctrl Pts',(0.0127034465584522,-0.0333679692468939,
0.0776291963457838));
#87634=CARTESIAN_POINT('Ctrl Pts',(0.0127030820920156,-0.0333391895414168,
0.0776289268982052));
#87635=CARTESIAN_POINT('Ctrl Pts',(0.0127028069762463,-0.033310408112934,
0.0776287275451851));
#87636=CARTESIAN_POINT('Ctrl Pts',(0.0127024395635659,-0.0332532698080884,
0.0776284681520712));
#87637=CARTESIAN_POINT('Ctrl Pts',(0.0127023445977535,-0.0332249170382467,
0.0776284060801511));
#87638=CARTESIAN_POINT('Ctrl Pts',(0.0127023375019387,-0.0331960985401869,
0.0776284093528773));
#87639=CARTESIAN_POINT('Ctrl Pts',(0.0127023374105474,-0.0331956312522822,
0.0776284094239842));
#87640=CARTESIAN_POINT('Ctrl Pts',(0.0127023373432507,-0.0331951640388592,
0.0776284095125653));
#87641=CARTESIAN_POINT('',(0.0126267197451524,-0.0331951640388587,0.0777279433201761));
#87642=CARTESIAN_POINT('',(0.012664528544212,-0.0331951640388687,0.0776781764163801));
#87643=CARTESIAN_POINT('',(0.0124759194931757,-0.0335216366567645,0.0779099236583928));
#87644=CARTESIAN_POINT('Origin',(-0.000885048750426973,-0.032643457152579,
0.0679673287949028));
#87645=CARTESIAN_POINT('',(0.0124748914701048,-0.0336938721132327,0.0779090355225293));
#87646=CARTESIAN_POINT('Origin',(0.0207386455233593,-0.0336938867896231,
0.0850483071168731));
#87647=CARTESIAN_POINT('',(0.0125157505518864,-0.0336938721132537,0.0778617408564788));
#87648=CARTESIAN_POINT('Ctrl Pts',(0.0125068342143895,-0.0335235895815172,
0.0782474205274581));
#87649=CARTESIAN_POINT('Ctrl Pts',(0.0125632432750286,-0.0334144449262749,
0.0781870791869498));
#87650=CARTESIAN_POINT('Ctrl Pts',(0.0126184705361613,-0.0333049234473147,
0.0781255031528116));
#87651=CARTESIAN_POINT('Ctrl Pts',(0.0126724382467524,-0.0331951640388587,
0.0780627647649378));
#87652=CARTESIAN_POINT('Ctrl Pts',(0.012496156831399,-0.0335235895815172,
0.0781346057856069));
#87653=CARTESIAN_POINT('Ctrl Pts',(0.0125510127750048,-0.0334144449262749,
0.0780744114402973));
#87654=CARTESIAN_POINT('Ctrl Pts',(0.0126046881715709,-0.0333049234473147,
0.0780130146564665));
#87655=CARTESIAN_POINT('Ctrl Pts',(0.0126571072751832,-0.0331951640388587,
0.0779504877245545));
#87656=CARTESIAN_POINT('Ctrl Pts',(0.0124854794484085,-0.0335235895815172,
0.0780217910437557));
#87657=CARTESIAN_POINT('Ctrl Pts',(0.0125387822749809,-0.0334144449262749,
0.0779617436936448));
#87658=CARTESIAN_POINT('Ctrl Pts',(0.0125909058069806,-0.0333049234473147,
0.0779005261601214));
#87659=CARTESIAN_POINT('Ctrl Pts',(0.012641776303614,-0.0331951640388587,
0.0778382106841713));
#87660=CARTESIAN_POINT('Ctrl Pts',(0.012474802065418,-0.0335235895815172,
0.0779089763019045));
#87661=CARTESIAN_POINT('Ctrl Pts',(0.012526551774957,-0.0334144449262749,
0.0778490759469923));
#87662=CARTESIAN_POINT('Ctrl Pts',(0.0125771234423902,-0.0333049234473147,
0.0777880376637764));
#87663=CARTESIAN_POINT('Ctrl Pts',(0.0126264453320448,-0.0331951640388587,
0.077725933643788));
#87664=CARTESIAN_POINT('',(0.0126495789959617,-0.0331951640388687,0.0778953540425622));
#87665=CARTESIAN_POINT('Ctrl Pts',(0.0126640701305185,-0.0332121607145946,
0.0780724718463101));
#87666=CARTESIAN_POINT('Ctrl Pts',(0.0126315989788135,-0.033262544410894,
0.0780444191808985));
#87667=CARTESIAN_POINT('Ctrl Pts',(0.0125996873560065,-0.0333135300745174,
0.0780168499069326));
#87668=CARTESIAN_POINT('Ctrl Pts',(0.0125369578369668,-0.033416720314053,
0.0779626562575963));
#87669=CARTESIAN_POINT('Ctrl Pts',(0.0125061642365394,-0.0334688847587201,
0.0779360528719987));
#87670=CARTESIAN_POINT('Ctrl Pts',(0.0124759194927459,-0.0335216366562258,
0.0779099236578027));
#87671=CARTESIAN_POINT('Ctrl Pts',(0.0125545874353461,-0.0336938721132576,
0.0778145938191832));
#87672=CARTESIAN_POINT('Ctrl Pts',(0.0125760375190152,-0.0336474569765051,
0.0777886588457981));
#87673=CARTESIAN_POINT('Ctrl Pts',(0.012597182531302,-0.033601104548885,
0.0777624745491818));
#87674=CARTESIAN_POINT('Ctrl Pts',(0.0126507168408582,-0.0334837508592655,
0.0776961819303098));
#87675=CARTESIAN_POINT('Ctrl Pts',(0.0127022632543466,-0.0333660264659096,
0.0776283320896833));
#87676=CARTESIAN_POINT('Ctrl Pts',(0.0125566096336264,-0.0336938721132576,
0.0778144461904346));
#87677=CARTESIAN_POINT('Ctrl Pts',(0.0125780588531755,-0.0336474569765051,
0.0777884993804519));
#87678=CARTESIAN_POINT('Ctrl Pts',(0.0125992028628391,-0.033601104548885,
0.0777623032581647));
#87679=CARTESIAN_POINT('Ctrl Pts',(0.012652734633984,-0.0334837508592655,
0.0776959806994129));
#87680=CARTESIAN_POINT('Ctrl Pts',(0.012704277622995,-0.0333660264659096,
0.0776281010072723));
#87681=CARTESIAN_POINT('Ctrl Pts',(0.0128956632619176,-0.0336938721132576,
0.0777896938882721));
#87682=CARTESIAN_POINT('Ctrl Pts',(0.0129169675980284,-0.0336474569765051,
0.0777617624848927));
#87683=CARTESIAN_POINT('Ctrl Pts',(0.0129379435020098,-0.033601104548885,
0.077733583601238));
#87684=CARTESIAN_POINT('Ctrl Pts',(0.0129910496682173,-0.0334837508592655,
0.07766224114657));
#87685=CARTESIAN_POINT('Ctrl Pts',(0.0130420184892613,-0.0333660264659096,
0.0775893563744383));
#87686=CARTESIAN_POINT('',(0.0129014049584752,-0.0336769361243754,0.0777796447087626));
#87687=CARTESIAN_POINT('',(0.0128936410732186,-0.0336938721132327,0.0777898415163072));
#87688=CARTESIAN_POINT('Ctrl Pts',(0.0129014049584754,-0.0336769361243751,
0.0777796447087624));
#87689=CARTESIAN_POINT('Ctrl Pts',(0.0129001126958818,-0.0336797586670012,
0.0777813456860429));
#87690=CARTESIAN_POINT('Ctrl Pts',(0.0128988195737642,-0.0336825812712819,
0.0777830459088651));
#87691=CARTESIAN_POINT('Ctrl Pts',(0.012896231617541,-0.0336882265885678,
0.0777864448371688));
#87692=CARTESIAN_POINT('Ctrl Pts',(0.0128949367834719,-0.0336910493015603,
0.0777881435426561));
#87693=CARTESIAN_POINT('Ctrl Pts',(0.0128936410732317,-0.0336938721132376,
0.077789841516309));
#87694=CARTESIAN_POINT('Ctrl Pts',(0.0129014049584752,-0.0336769361243754,
0.0777796447087626));
#87695=CARTESIAN_POINT('Ctrl Pts',(0.0128680310229009,-0.0336279018525357,
0.07775428993828));
#87696=CARTESIAN_POINT('Ctrl Pts',(0.0128341769609851,-0.0335767826051547,
0.0777285704073053));
#87697=CARTESIAN_POINT('Ctrl Pts',(0.012767842447259,-0.0334733172106842,
0.0776781749013019));
#87698=CARTESIAN_POINT('Ctrl Pts',(0.0127353174133851,-0.0334209631477619,
0.0776534650564892));
#87699=CARTESIAN_POINT('Ctrl Pts',(0.0127034191046726,-0.033367986984468,
0.0776292313458923));
#87700=CARTESIAN_POINT('',(0.0127251253534434,-0.0336938721132538,0.0778021438533678));
#87701=CARTESIAN_POINT('Origin',(0.00812378219310841,-0.0315241814719618,
0.07415));
#87702=CARTESIAN_POINT('',(0.0129014049574505,-0.0337108120655664,0.0777796447079852));
#87703=CARTESIAN_POINT('',(0.0129091470454567,-0.0336938721132327,0.0777694313406826));
#87704=CARTESIAN_POINT('Origin',(0.000549542511272994,-0.034556252669366,
0.066992164303698));
#87705=CARTESIAN_POINT('Ctrl Pts',(0.0129091470454626,-0.0336938721132382,
0.0777694313406962));
#87706=CARTESIAN_POINT('Ctrl Pts',(0.0129078585987974,-0.0336910492970996,
0.077771134836855));
#87707=CARTESIAN_POINT('Ctrl Pts',(0.0129065692152446,-0.0336882265863373,
0.0777728376810751));
#87708=CARTESIAN_POINT('Ctrl Pts',(0.0129039885263747,-0.0336825812712489,
0.0777762421284276));
#87709=CARTESIAN_POINT('Ctrl Pts',(0.0129026972210611,-0.0336797586669847,
0.0777779437314923));
#87710=CARTESIAN_POINT('Ctrl Pts',(0.0129014049584751,-0.0336769361243751,
0.0777796447087628));
#87711=CARTESIAN_POINT('Origin',(-0.000802628279970289,-0.0345562522332008,
0.0687719985390831));
#87712=CARTESIAN_POINT('Ctrl Pts',(0.0126041245922024,-0.034243627687391,
0.0777561970255215));
#87713=CARTESIAN_POINT('Ctrl Pts',(0.0127401345551726,-0.0339430054201809,
0.0775872181262872));
#87714=CARTESIAN_POINT('Ctrl Pts',(0.0128630299450369,-0.0336441434784052,
0.0774084744506964));
#87715=CARTESIAN_POINT('Ctrl Pts',(0.0127566089764962,-0.034243627687391,
0.0775580846519893));
#87716=CARTESIAN_POINT('Ctrl Pts',(0.0128851470081222,-0.0339430054201809,
0.0773833547093942));
#87717=CARTESIAN_POINT('Ctrl Pts',(0.0130001585014659,-0.0336441434784052,
0.077199439145038));
#87718=CARTESIAN_POINT('Ctrl Pts',(0.0127581338203391,-0.034243627687391,
0.077556103528254));
#87719=CARTESIAN_POINT('Ctrl Pts',(0.0128865971326517,-0.0339430054201809,
0.0773813160752254));
#87720=CARTESIAN_POINT('Ctrl Pts',(0.0130015297870302,-0.0336441434784052,
0.0771973487919815));
#87721=CARTESIAN_POINT('',(0.0127779549413509,-0.0341934961088741,0.0775288757049524));
#87722=CARTESIAN_POINT('',(0.0129128449824874,-0.0338664212865843,0.0773348080954013));
#87723=CARTESIAN_POINT('Origin',(-0.000458671437912886,-0.0345610720407566,
0.0672894975086063));
#87724=CARTESIAN_POINT('Origin',(0.022044287513203,-0.0336938005072887,
0.0834073266643943));
#87725=CARTESIAN_POINT('',(0.012842495146412,-0.0336938721132327,0.0774381412780363));
#87726=CARTESIAN_POINT('',(0.012877104448698,-0.0336938721132427,0.0773860985437216));
#87727=CARTESIAN_POINT('',(0.0127034191046694,-0.0340203938281605,0.0776292313458965));
#87728=CARTESIAN_POINT('Origin',(-0.000109099515416648,-0.0345589643244507,
0.0669588372527201));
#87729=CARTESIAN_POINT('',(0.0127023373432517,-0.0341934961088739,0.0776284095125642));
#87730=CARTESIAN_POINT('Origin',(0.0214767972526703,-0.0341934220717625,
0.084294523189698));
#87731=CARTESIAN_POINT('',(0.0127401461423113,-0.0341934961088841,0.0775786426087683));
#87732=CARTESIAN_POINT('Ctrl Pts',(0.0127554626867099,-0.0340223579322396,
0.0779641232026885));
#87733=CARTESIAN_POINT('Ctrl Pts',(0.0128080693933258,-0.0339125849573574,
0.0779002402487519));
#87734=CARTESIAN_POINT('Ctrl Pts',(0.0128593169051152,-0.0338030433565231,
0.0778353133480415));
#87735=CARTESIAN_POINT('Ctrl Pts',(0.0129091470454587,-0.0336938721132327,
0.0777694313406923));
#87736=CARTESIAN_POINT('Ctrl Pts',(0.0127377227228115,-0.0340223579322396,
0.0778522014732892));
#87737=CARTESIAN_POINT('Ctrl Pts',(0.012788785736875,-0.0339125849573574,
0.0777885631997224));
#87738=CARTESIAN_POINT('Ctrl Pts',(0.0128384957051617,-0.0338030433565231,
0.0777239127582967));
#87739=CARTESIAN_POINT('Ctrl Pts',(0.0128867963859714,-0.0336938721132327,
0.0776583384613015));
#87740=CARTESIAN_POINT('Ctrl Pts',(0.0127199827589131,-0.0340223579322396,
0.0777402797438898));
#87741=CARTESIAN_POINT('Ctrl Pts',(0.0127695020804241,-0.0339125849573574,
0.077676886150693));
#87742=CARTESIAN_POINT('Ctrl Pts',(0.0128176745052083,-0.0338030433565231,
0.0776125121685519));
#87743=CARTESIAN_POINT('Ctrl Pts',(0.012864445726484,-0.0336938721132327,
0.0775472455819107));
#87744=CARTESIAN_POINT('Ctrl Pts',(0.0127022427950148,-0.0340223579322396,
0.0776283580144904));
#87745=CARTESIAN_POINT('Ctrl Pts',(0.0127502184239732,-0.0339125849573574,
0.0775652091016636));
#87746=CARTESIAN_POINT('Ctrl Pts',(0.0127968533052548,-0.0338030433565231,
0.0775011115788072));
#87747=CARTESIAN_POINT('Ctrl Pts',(0.0128420950669967,-0.0336938721132327,
0.0774361527025199));
#87748=CARTESIAN_POINT('',(0.0128758210959443,-0.0336938721132427,0.0776037863093694));
#87749=CARTESIAN_POINT('Ctrl Pts',(0.0129014049545757,-0.0337108120662656,
0.0777796447058001));
#87750=CARTESIAN_POINT('Ctrl Pts',(0.0128671659171043,-0.0337611408993509,
0.0777536327020706));
#87751=CARTESIAN_POINT('Ctrl Pts',(0.0128335516661034,-0.0338121088779705,
0.0777280953596984));
#87752=CARTESIAN_POINT('Ctrl Pts',(0.0127675421147982,-0.0339153382773232,
0.0776779467334068));
#87753=CARTESIAN_POINT('Ctrl Pts',(0.0127351747407274,-0.0339675558473114,
0.0776533566655421));
#87754=CARTESIAN_POINT('Ctrl Pts',(0.0127034191046408,-0.0340203938281304,
0.0776292313458683));
#87755=CARTESIAN_POINT('Ctrl Pts',(0.0127759454407895,-0.0341934961088741,
0.0775291500940517));
#87756=CARTESIAN_POINT('Ctrl Pts',(0.0128458067068495,-0.0340287516182428,
0.0774329702839352));
#87757=CARTESIAN_POINT('Ctrl Pts',(0.0129116330932742,-0.0338644633275951,
0.0773339852385));
#87758=CARTESIAN_POINT('Ctrl Pts',(0.0127779549413508,-0.0341934961088741,
0.0775288757049524));
#87759=CARTESIAN_POINT('Ctrl Pts',(0.0128478105346324,-0.0340287516182428,
0.077432654349995));
#87760=CARTESIAN_POINT('Ctrl Pts',(0.0129136295360461,-0.0338644633275951,
0.0773336280296782));
#87761=CARTESIAN_POINT('Ctrl Pts',(0.0131127763861176,-0.0341934961088741,
0.0774831572033518));
#87762=CARTESIAN_POINT('Ctrl Pts',(0.0131816867853961,-0.0340287516182428,
0.0773800136788001));
#87763=CARTESIAN_POINT('Ctrl Pts',(0.0132462753019362,-0.0338644633275951,
0.0772741101693359));
#87764=CARTESIAN_POINT('',(0.0131198846871562,-0.0341764758832447,0.0774724930187678));
#87765=CARTESIAN_POINT('',(0.0131127763861026,-0.034193496108874,0.0774831572033539));
#87766=CARTESIAN_POINT('Origin',(-0.000383910481475924,-0.0345621026348341,
0.0678772417603383));
#87767=CARTESIAN_POINT('Ctrl Pts',(0.013119884685544,-0.0341764758837558,
0.0774724930196175));
#87768=CARTESIAN_POINT('Ctrl Pts',(0.0130841422462247,-0.034126005004086,
0.0774487237068725));
#87769=CARTESIAN_POINT('Ctrl Pts',(0.013049021073664,-0.0340749269148957,
0.0774253675926721));
#87770=CARTESIAN_POINT('Ctrl Pts',(0.01297999414439,-0.0339715436308211,
0.0773794635074193));
#87771=CARTESIAN_POINT('Ctrl Pts',(0.0129461145781926,-0.0339192778238913,
0.0773569329463197));
#87772=CARTESIAN_POINT('Ctrl Pts',(0.0129128449824776,-0.0338664212856685,
0.077334808097604));
#87773=CARTESIAN_POINT('',(0.0129453656637368,-0.0341934961088841,0.0775060164541632));
#87774=CARTESIAN_POINT('Origin',(0.00812378219310841,-0.0315241814719618,
0.07415));
#87775=CARTESIAN_POINT('',(0.013119884687007,-0.034210518019052,0.0774724930176583));
#87776=CARTESIAN_POINT('',(0.0131269701953153,-0.0341934961088739,0.0774618136744959));
#87777=CARTESIAN_POINT('Origin',(-0.00041319630938822,-0.0345621720619559,
0.0679118349174756));
#87778=CARTESIAN_POINT('Origin',(-0.000951059373476715,-0.0345621029033183,
0.0687300747565296));
#87779=CARTESIAN_POINT('Origin',(-0.000930482404601438,-0.0345621725052226,
0.0686896903395078));
#87780=CARTESIAN_POINT('Ctrl Pts',(0.0128416645176694,-0.0346945769586965,
0.077439390311912));
#87781=CARTESIAN_POINT('Ctrl Pts',(0.0129105621147524,-0.0345275153362943,
0.0773405723776871));
#87782=CARTESIAN_POINT('Ctrl Pts',(0.0129763697992073,-0.0343603235965185,
0.0772395621180704));
#87783=CARTESIAN_POINT('Ctrl Pts',(0.0130388973812223,-0.0341934961088739,
0.0771366611692789));
#87784=CARTESIAN_POINT('Ctrl Pts',(0.0128880871303978,-0.0346945769586965,
0.0773695836546843));
#87785=CARTESIAN_POINT('Ctrl Pts',(0.0129555225990961,-0.0345275153362943,
0.0772697933802492));
#87786=CARTESIAN_POINT('Ctrl Pts',(0.0130198371977804,-0.0343603235965185,
0.0771678565115172));
#87787=CARTESIAN_POINT('Ctrl Pts',(0.0130808451932546,-0.0341934961088739,
0.0770640773595722));
#87788=CARTESIAN_POINT('Ctrl Pts',(0.0129345097431261,-0.0346945769586965,
0.0772997769974551));
#87789=CARTESIAN_POINT('Ctrl Pts',(0.0130004830834395,-0.0345275153362943,
0.0771990143828112));
#87790=CARTESIAN_POINT('Ctrl Pts',(0.0130633045963531,-0.0343603235965185,
0.0770961509049639));
#87791=CARTESIAN_POINT('Ctrl Pts',(0.0131227930052867,-0.0341934961088739,
0.0769914935498638));
#87792=CARTESIAN_POINT('Ctrl Pts',(0.0129809323558545,-0.0346945769586965,
0.0772299703402289));
#87793=CARTESIAN_POINT('Ctrl Pts',(0.0130454435677835,-0.0345275153362943,
0.0771282353853734));
#87794=CARTESIAN_POINT('Ctrl Pts',(0.0131067719949265,-0.0343603235965185,
0.0770244452984109));
#87795=CARTESIAN_POINT('Ctrl Pts',(0.0131647408173194,-0.0341934961088739,
0.0769189097401589));
#87796=CARTESIAN_POINT('',(0.0129809323555189,-0.0346945769586966,0.0772299703407333));
#87797=CARTESIAN_POINT('',(0.0131033706147947,-0.034366772783154,0.0770278158647057));
#87798=CARTESIAN_POINT('Origin',(-0.00131567092393877,-0.0345626457064043,
0.0683809940206447));
#87799=CARTESIAN_POINT('Origin',(0.0226724682876334,-0.0341934771029036,
0.0825580079216642));
#87800=CARTESIAN_POINT('',(0.0130396479434198,-0.034193496108874,0.0771353624444808));
#87801=CARTESIAN_POINT('',(0.0130709211618275,-0.0341934961088839,0.077081249268544));
#87802=CARTESIAN_POINT('',(0.0129128449811174,-0.0345211942962608,0.0773348080966584));
#87803=CARTESIAN_POINT('Origin',(-0.00104665393795225,-0.0345625596120493,
0.0679824709331373));
#87804=CARTESIAN_POINT('',(0.0129117137509639,-0.0346945769586885,0.0773340558093871));
#87805=CARTESIAN_POINT('Origin',(0.0221241656625528,-0.034694568585385,
0.0834604940055356));
#87806=CARTESIAN_POINT('',(0.0129463230532514,-0.0346945769587025,0.0772820130750702));
#87807=CARTESIAN_POINT('Ctrl Pts',(0.0129858144645065,-0.0345231616327842,
0.0776657704976263));
#87808=CARTESIAN_POINT('Ctrl Pts',(0.0130342744110074,-0.0344132092796988,
0.0775987542279589));
#87809=CARTESIAN_POINT('Ctrl Pts',(0.0130813456785214,-0.0343032738558979,
0.0775307390602543));
#87810=CARTESIAN_POINT('Ctrl Pts',(0.013126970195318,-0.0341934961088739,
0.0774618136745056));
#87811=CARTESIAN_POINT('Ctrl Pts',(0.012961081907181,-0.0345231616327842,
0.0775551837138443));
#87812=CARTESIAN_POINT('Ctrl Pts',(0.0130080175705612,-0.0344132092796988,
0.077488508347659));
#87813=CARTESIAN_POINT('Ctrl Pts',(0.0130535716849201,-0.0343032738558979,
0.0774208655944415));
#87814=CARTESIAN_POINT('Ctrl Pts',(0.0130976881099546,-0.0341934961088739,
0.0773523436072915));
#87815=CARTESIAN_POINT('Ctrl Pts',(0.0129363493498555,-0.0345231616327842,
0.0774445969300623));
#87816=CARTESIAN_POINT('Ctrl Pts',(0.012981760730115,-0.0344132092796988,
0.0773782624673591));
#87817=CARTESIAN_POINT('Ctrl Pts',(0.0130257976913189,-0.0343032738558979,
0.0773109921286286));
#87818=CARTESIAN_POINT('Ctrl Pts',(0.0130684060245911,-0.0341934961088739,
0.0772428735400773));
#87819=CARTESIAN_POINT('Ctrl Pts',(0.01291161679253,-0.0345231616327842,
0.0773340101462804));
#87820=CARTESIAN_POINT('Ctrl Pts',(0.0129555038896688,-0.0344132092796988,
0.0772680165870592));
#87821=CARTESIAN_POINT('Ctrl Pts',(0.0129980236977176,-0.0343032738558979,
0.0772011186628158));
#87822=CARTESIAN_POINT('Ctrl Pts',(0.0130391239392277,-0.0341934961088739,
0.0771334034728632));
#87823=CARTESIAN_POINT('',(0.0130833090693775,-0.0341934961088839,0.0772985880594983));
#87824=CARTESIAN_POINT('Ctrl Pts',(0.0131198846841247,-0.0342105180195354,
0.0774724930157396));
#87825=CARTESIAN_POINT('Ctrl Pts',(0.013084102071013,-0.0342610556240321,
0.0774486969702496));
#87826=CARTESIAN_POINT('Ctrl Pts',(0.0130489615583901,-0.034312218986816,
0.077425327932491));
#87827=CARTESIAN_POINT('Ctrl Pts',(0.0129799339303926,-0.0344158119695075,
0.0773794233874327));
#87828=CARTESIAN_POINT('Ctrl Pts',(0.012946075048014,-0.034468199044995,
0.0773569066555551));
#87829=CARTESIAN_POINT('Ctrl Pts',(0.0129128449810918,-0.0345211942962356,
0.0773348080966363));
#87830=CARTESIAN_POINT('Ctrl Pts',(0.0129789445361091,-0.0346945769586932,
0.077230370268035));
#87831=CARTESIAN_POINT('Ctrl Pts',(0.0130426290118006,-0.034529677707698,
0.077129993221996));
#87832=CARTESIAN_POINT('Ctrl Pts',(0.0131021103943521,-0.0343648066251421,
0.0770270698089874));
#87833=CARTESIAN_POINT('Ctrl Pts',(0.012980932355514,-0.0346945769586932,
0.0772299703407409));
#87834=CARTESIAN_POINT('Ctrl Pts',(0.0130446085629917,-0.034529677707698,
0.0771295521979423));
#87835=CARTESIAN_POINT('Ctrl Pts',(0.0131040799858276,-0.0343648066251421,
0.0770265880650236));
#87836=CARTESIAN_POINT('Ctrl Pts',(0.0133122224181741,-0.0346945769586932,
0.0771633184416937));
#87837=CARTESIAN_POINT('Ctrl Pts',(0.0133745206448003,-0.034529677707698,
0.0770560511112629));
#87838=CARTESIAN_POINT('Ctrl Pts',(0.0134323321810336,-0.0343648066251421,
0.0769463005964721));
#87839=CARTESIAN_POINT('',(0.0133186470831683,-0.0346775396665031,0.0771522289665511));
#87840=CARTESIAN_POINT('',(0.0133122224181615,-0.0346945769586886,0.0771633184416935));
#87841=CARTESIAN_POINT('Origin',(-0.00113099879810727,-0.0345626618834468,
0.0689778404592653));
#87842=CARTESIAN_POINT('Ctrl Pts',(0.0133186470815555,-0.0346775396670097,
0.0771522289674092));
#87843=CARTESIAN_POINT('Ctrl Pts',(0.0132814534144467,-0.0346269749928195,
0.0771307339276362));
#87844=CARTESIAN_POINT('Ctrl Pts',(0.0132449207438227,-0.0345757902890808,
0.0771096209337837));
#87845=CARTESIAN_POINT('Ctrl Pts',(0.0131731473949716,-0.0344721681087884,
0.0770681415008954));
#87846=CARTESIAN_POINT('Ctrl Pts',(0.0131379348580869,-0.0344197714289365,
0.0770477913188639));
#87847=CARTESIAN_POINT('Ctrl Pts',(0.0131033706147641,-0.0343667727830768,
0.0770278158649634));
#87848=CARTESIAN_POINT('',(0.0131465773868502,-0.0346945769587026,0.0771966443912234));
#87849=CARTESIAN_POINT('Origin',(0.00812378219310841,-0.0315241814719618,
0.07415));
#87850=CARTESIAN_POINT('',(0.0133186470825154,-0.0347116136489778,0.0771522289653209));
#87851=CARTESIAN_POINT('',(0.0133250480478685,-0.0346945769586885,0.0771411257927598));
#87852=CARTESIAN_POINT('Origin',(-0.00115203163608611,-0.0345626701708096,
0.0690179742157668));
#87853=CARTESIAN_POINT('Origin',(-0.000978169355718683,-0.0345626620963308,
0.0687133923034704));
#87854=CARTESIAN_POINT('Origin',(-0.000953894743002916,-0.0345626704262437,
0.0686751321063215));
#87855=CARTESIAN_POINT('Ctrl Pts',(0.0130195361216765,-0.0352450361874067,
0.0771683366440036));
#87856=CARTESIAN_POINT('Ctrl Pts',(0.013133374556207,-0.0349452760959492,
0.0769836902546812));
#87857=CARTESIAN_POINT('Ctrl Pts',(0.0132329812661732,-0.034644428984174,
0.0767909936496363));
#87858=CARTESIAN_POINT('Ctrl Pts',(0.0130208132564897,-0.0352450361874067,
0.0771661584448234));
#87859=CARTESIAN_POINT('Ctrl Pts',(0.01313456953889,-0.0349452760959492,
0.076981463887571));
#87860=CARTESIAN_POINT('Ctrl Pts',(0.013234090701906,-0.034644428984174,
0.0767887254394709));
#87861=CARTESIAN_POINT('Ctrl Pts',(0.0131472622478912,-0.0352450361874067,
0.0769504951596458));
#87862=CARTESIAN_POINT('Ctrl Pts',(0.0132528846560204,-0.0349452760959492,
0.0767610315004255));
#87863=CARTESIAN_POINT('Ctrl Pts',(0.0133439358239721,-0.034644428984174,
0.0765641501755652));
#87864=CARTESIAN_POINT('Ctrl Pts',(0.0131485267378052,-0.0352450361874067,
0.076948338526794));
#87865=CARTESIAN_POINT('Ctrl Pts',(0.0132540678071917,-0.0349452760959492,
0.0767588271765541));
#87866=CARTESIAN_POINT('Ctrl Pts',(0.0133450342751927,-0.034644428984174,
0.0765619044229261));
#87867=CARTESIAN_POINT('',(0.0131647273186907,-0.0351951634053349,0.0769189392451548));
#87868=CARTESIAN_POINT('',(0.0132742440876456,-0.0348678972925388,0.0767094662085914));
#87869=CARTESIAN_POINT('Origin',(-0.00191268559069225,-0.0345636767881609,
0.0696336035408099));
#87870=CARTESIAN_POINT('Origin',(0.0231696076725555,-0.0346946199340784,
0.0816268607243761));
#87871=CARTESIAN_POINT('',(0.0132174000556613,-0.0346945769330289,0.076820801765112));
#87872=CARTESIAN_POINT('',(0.0132452137732655,-0.0346945769458128,0.0767648316998928));
#87873=CARTESIAN_POINT('',(0.0131033706146427,-0.0350221583435276,0.0770278158648744));
#87874=CARTESIAN_POINT('Origin',(-0.00173667969852291,-0.0345628458715479,
0.0691862051510017));
#87875=CARTESIAN_POINT('',(0.0131022981931494,-0.0351951360298762,0.0770271995817522));
#87876=CARTESIAN_POINT('Origin',(0.0226426482481184,-0.0351951838366873,
0.0825407796087665));
#87877=CARTESIAN_POINT('',(0.0131647408171114,-0.0351951371328746,0.076918909740751));
#87878=CARTESIAN_POINT('Ctrl Pts',(0.0131969779234846,-0.0350241211494343,
0.0773535425830464));
#87879=CARTESIAN_POINT('Ctrl Pts',(0.0132411054090624,-0.0349144232818962,
0.0772836613919517));
#87880=CARTESIAN_POINT('Ctrl Pts',(0.0132838148129131,-0.0348045283579412,
0.0772128262269371));
#87881=CARTESIAN_POINT('Ctrl Pts',(0.0133250480534117,-0.0346945769439158,
0.0771411257831361));
#87882=CARTESIAN_POINT('Ctrl Pts',(0.0131653503442054,-0.0350241211494343,
0.0772447269682087));
#87883=CARTESIAN_POINT('Ctrl Pts',(0.013207978939305,-0.0349144232818962,
0.0771752814340508));
#87884=CARTESIAN_POINT('Ctrl Pts',(0.0132491975608594,-0.0348045283579412,
0.0771049131698718));
#87885=CARTESIAN_POINT('Ctrl Pts',(0.0132889500590009,-0.0346945769439158,
0.0770337103438218));
#87886=CARTESIAN_POINT('Ctrl Pts',(0.0131337227649262,-0.0350241211494343,
0.077135911353371));
#87887=CARTESIAN_POINT('Ctrl Pts',(0.0131748524695475,-0.0349144232818962,
0.0770669014761498));
#87888=CARTESIAN_POINT('Ctrl Pts',(0.0132145803088056,-0.0348045283579412,
0.0769970001128065));
#87889=CARTESIAN_POINT('Ctrl Pts',(0.0132528520645901,-0.0346945769439158,
0.0769262949045074));
#87890=CARTESIAN_POINT('Ctrl Pts',(0.013102095185647,-0.0350241211494343,
0.0770270957385332));
#87891=CARTESIAN_POINT('Ctrl Pts',(0.0131417259997901,-0.0349144232818962,
0.0769585215182488));
#87892=CARTESIAN_POINT('Ctrl Pts',(0.0131799630567519,-0.0348045283579412,
0.0768890870557412));
#87893=CARTESIAN_POINT('Ctrl Pts',(0.0132167540701793,-0.0346945769439158,
0.0768188794651931));
#87894=CARTESIAN_POINT('',(0.0132712240517077,-0.0346945769458128,0.0769809637792386));
#87895=CARTESIAN_POINT('Ctrl Pts',(0.0133186470796628,-0.034711613649276,
0.07715222896367));
#87896=CARTESIAN_POINT('Ctrl Pts',(0.0132814681894934,-0.0347621546531267,
0.0771307424489404));
#87897=CARTESIAN_POINT('Ctrl Pts',(0.0132449430046785,-0.0348133084094936,
0.0771096337252008));
#87898=CARTESIAN_POINT('Ctrl Pts',(0.0131731695627246,-0.0349168561544566,
0.0770681542428732));
#87899=CARTESIAN_POINT('Ctrl Pts',(0.0131379497746807,-0.0349692089015913,
0.0770477999372138));
#87900=CARTESIAN_POINT('Ctrl Pts',(0.013103370614621,-0.0350221583435,0.0770278158648389));
#87901=CARTESIAN_POINT('Ctrl Pts',(0.0131633274884781,-0.0351951371254979,
0.0769192877911379));
#87902=CARTESIAN_POINT('Ctrl Pts',(0.013220580776051,-0.0350307338980974,
0.0768150983540717));
#87903=CARTESIAN_POINT('Ctrl Pts',(0.0132734788791687,-0.0348659306897824,
0.0767086316061143));
#87904=CARTESIAN_POINT('Ctrl Pts',(0.0131647408170057,-0.0351951371254979,
0.0769189097407023));
#87905=CARTESIAN_POINT('Ctrl Pts',(0.0132219862886231,-0.0350307338980974,
0.0768146910839556));
#87906=CARTESIAN_POINT('Ctrl Pts',(0.013274875374783,-0.0348659306897824,
0.0767081954643276));
#87907=CARTESIAN_POINT('Ctrl Pts',(0.0134016161512906,-0.0351951371254979,
0.0768555480936741));
#87908=CARTESIAN_POINT('Ctrl Pts',(0.0134575516606101,-0.0350307338980974,
0.0767464321880115));
#87909=CARTESIAN_POINT('Ctrl Pts',(0.0135089294952453,-0.0348659306897824,
0.0766350976462934));
#87910=CARTESIAN_POINT('Origin',(0.0180367870874105,-0.0308609197410571,
0.0790761603273267));
#87911=CARTESIAN_POINT('',(0.0132680131219248,-0.0351951371254979,0.0768912854912133));
#87912=CARTESIAN_POINT('Origin',(0.00719498968780964,-0.0351840467441105,
0.0738465364396827));
#87913=CARTESIAN_POINT('Origin',(0.0191690556789188,-0.0352322613362849,
0.0787514059328649));
#87914=CARTESIAN_POINT('',(0.0133751536690105,-0.0351951142564687,0.0764954023547165));
#87915=CARTESIAN_POINT('',(0.0134235389043139,-0.0351951372916787,0.0763804884671374));
#87916=CARTESIAN_POINT('Origin',(0.00807170863840627,-0.0352875125435763,
0.07381338790932));
#87917=CARTESIAN_POINT('Origin',(0.00394304548537184,-0.0298325076522644,
0.0803802994198087));
#87918=CARTESIAN_POINT('Origin',(0.0140569765020341,-0.0338732607737469,
0.0800699940465063));
#87919=CARTESIAN_POINT('Origin',(0.00812378219310841,-0.0315241814719618,
0.07415));
#87920=CARTESIAN_POINT('',(0.0115459495571206,-0.0322104233323599,0.0790783638781051));
#87921=CARTESIAN_POINT('',(0.0115564688245398,-0.0321934096636183,0.0790710428254998));
#87922=CARTESIAN_POINT('Origin',(0.00257773023980595,-0.0326387245949053,
0.0651660339478818));
#87923=CARTESIAN_POINT('',(0.0115459495569106,-0.032176398030852,0.0790783638778025));
#87924=CARTESIAN_POINT('Origin',(0.00161034854614262,-0.032638623529467,
0.0658454522903156));
#87925=CARTESIAN_POINT('',(0.0115354146774751,-0.0321934096636184,0.0790856624470899));
#87926=CARTESIAN_POINT('Origin',(0.00261820415429388,-0.0326386230888073,
0.0651456164874627));
#87927=CARTESIAN_POINT('Origin',(0.00164362107438124,-0.032638724894122,
0.0658146635723998));
#87928=CARTESIAN_POINT('Ctrl Pts',(0.0109933420942546,-0.0321934096636941,
0.079134351684928));
#87929=CARTESIAN_POINT('Ctrl Pts',(0.011082559615781,-0.0320508460845128,
0.0790829879292312));
#87930=CARTESIAN_POINT('Ctrl Pts',(0.011170329824236,-0.0319086045664672,
0.0790292658032143));
#87931=CARTESIAN_POINT('Ctrl Pts',(0.0112564732578548,-0.031766989287029,
0.0789733165384563));
#87932=CARTESIAN_POINT('Ctrl Pts',(0.0110650810268201,-0.0321934096636941,
0.0790909470978186));
#87933=CARTESIAN_POINT('Ctrl Pts',(0.0111535216269072,-0.0320508460845128,
0.0790382992493922));
#87934=CARTESIAN_POINT('Ctrl Pts',(0.0112404809986863,-0.0319086045664672,
0.0789833148732019));
#87935=CARTESIAN_POINT('Ctrl Pts',(0.0113257816500166,-0.031766989287029,
0.0789261277749424));
#87936=CARTESIAN_POINT('Ctrl Pts',(0.0111368199593854,-0.0321934096636941,
0.0790475425107093));
#87937=CARTESIAN_POINT('Ctrl Pts',(0.0112244836380333,-0.0320508460845128,
0.0789936105695533));
#87938=CARTESIAN_POINT('Ctrl Pts',(0.0113106321731366,-0.0319086045664672,
0.0789373639431895));
#87939=CARTESIAN_POINT('Ctrl Pts',(0.0113950900421785,-0.031766989287029,
0.0788789390114283));
#87940=CARTESIAN_POINT('Ctrl Pts',(0.0112085588919508,-0.0321934096636941,
0.0790041379235999));
#87941=CARTESIAN_POINT('Ctrl Pts',(0.0112954456491594,-0.0320508460845128,
0.0789489218897142));
#87942=CARTESIAN_POINT('Ctrl Pts',(0.0113807833475869,-0.0319086045664672,
0.0788914130131771));
#87943=CARTESIAN_POINT('Ctrl Pts',(0.0114643984343405,-0.031766989287029,
0.0788317502479143));
#87944=CARTESIAN_POINT('',(0.0112072754682696,-0.0321934096636941,0.0790049144402385));
#87945=CARTESIAN_POINT('',(0.0114041341063444,-0.031866561751136,0.0788741312761827));
#87946=CARTESIAN_POINT('Origin',(0.0027737510633533,-0.032637194442029,
0.0645794657143673));
#87947=CARTESIAN_POINT('Origin',(0.0176559693908919,-0.0316939261509218,
0.0878775831536998));
#87948=CARTESIAN_POINT('',(0.0111012323342595,-0.0320197221621754,0.0790706076681135));
#87949=CARTESIAN_POINT('Ctrl Pts',(0.0111014097812802,-0.0320197392094669,
0.0790705554432635));
#87950=CARTESIAN_POINT('Ctrl Pts',(0.0111264471249915,-0.0319792716575967,
0.0790554042766529));
#87951=CARTESIAN_POINT('Ctrl Pts',(0.0111514829418241,-0.0319386439829653,
0.0790399932615345));
#87952=CARTESIAN_POINT('Ctrl Pts',(0.011176539081177,-0.0318979099381586,
0.0790242990169));
#87953=CARTESIAN_POINT('Ctrl Pts',(0.0112015947252764,-0.0318571766984909,
0.0790086050824741));
#87954=CARTESIAN_POINT('Ctrl Pts',(0.0112265442877187,-0.0318163871833581,
0.0789927092064922));
#87955=CARTESIAN_POINT('Ctrl Pts',(0.0112513038443118,-0.0317755399638303,
0.0789766690338607));
#87956=CARTESIAN_POINT('',(0.0111003271651873,-0.0321934096636183,0.0790696219396608));
#87957=CARTESIAN_POINT('Origin',(0.0123129570727762,-0.0324111971803128,
0.0810332308586919));
#87958=CARTESIAN_POINT('',(0.0111538013167385,-0.0321934096636663,0.0790372681899597));
#87959=CARTESIAN_POINT('Ctrl Pts',(0.0112053059993892,-0.0321934096636617,
0.0790044297963401));
#87960=CARTESIAN_POINT('Ctrl Pts',(0.011272252369602,-0.0320835708272591,
0.0789619331814523));
#87961=CARTESIAN_POINT('Ctrl Pts',(0.011338280442963,-0.0319739230346488,
0.078918075764676));
#87962=CARTESIAN_POINT('Ctrl Pts',(0.0114033100476125,-0.0318646057455572,
0.0788729201420098));
#87963=CARTESIAN_POINT('Ctrl Pts',(0.0113153422254146,-0.0321934096636617,
0.0790315073465977));
#87964=CARTESIAN_POINT('Ctrl Pts',(0.0113826620161486,-0.0320835708272591,
0.0789874932463957));
#87965=CARTESIAN_POINT('Ctrl Pts',(0.0114490318891518,-0.0319739230346488,
0.0789421114965902));
#87966=CARTESIAN_POINT('Ctrl Pts',(0.0115143713849343,-0.0318646057455572,
0.0788954266770202));
#87967=CARTESIAN_POINT('Ctrl Pts',(0.0114253784514401,-0.0321934096636617,
0.0790585848968552));
#87968=CARTESIAN_POINT('Ctrl Pts',(0.0114930716626951,-0.0320835708272591,
0.0790130533113391));
#87969=CARTESIAN_POINT('Ctrl Pts',(0.0115597833353406,-0.0319739230346488,
0.0789661472285044));
#87970=CARTESIAN_POINT('Ctrl Pts',(0.0116254327222561,-0.0318646057455572,
0.0789179332120306));
#87971=CARTESIAN_POINT('Ctrl Pts',(0.0115354146774656,-0.0321934096636617,
0.0790856624471127));
#87972=CARTESIAN_POINT('Ctrl Pts',(0.0116034813092416,-0.0320835708272591,
0.0790386133762826));
#87973=CARTESIAN_POINT('Ctrl Pts',(0.0116705347815294,-0.0319739230346488,
0.0789901829604186));
#87974=CARTESIAN_POINT('Ctrl Pts',(0.0117364940595778,-0.0318646057455572,
0.0789404397470411));
#87975=CARTESIAN_POINT('Ctrl Pts',(0.0115459495550968,-0.0321763980306386,
0.0790783638751927));
#87976=CARTESIAN_POINT('Ctrl Pts',(0.0115214702824469,-0.0321259596176341,
0.0790431105546337));
#87977=CARTESIAN_POINT('Ctrl Pts',(0.0114974151449519,-0.0320749164634415,
0.0790084680435985));
#87978=CARTESIAN_POINT('Ctrl Pts',(0.0114501337812436,-0.0319716057794034,
0.0789403767610218));
#87979=CARTESIAN_POINT('Ctrl Pts',(0.0114269259776363,-0.0319193786690241,
0.0789069545204173));
#87980=CARTESIAN_POINT('Ctrl Pts',(0.0114041341052815,-0.0318665617525439,
0.0788741312746552));
#87981=CARTESIAN_POINT('',(0.0113713450728824,-0.0321934096636663,0.0790452884436742));
#87982=CARTESIAN_POINT('Ctrl Pts',(0.0112704926892643,-0.0327445246967096,
0.0789641809327634));
#87983=CARTESIAN_POINT('Ctrl Pts',(0.0114520624914076,-0.032443687833936,
0.0788455008062437));
#87984=CARTESIAN_POINT('Ctrl Pts',(0.0116241770007383,-0.0321434074405927,
0.0787134812578467));
#87985=CARTESIAN_POINT('Ctrl Pts',(0.0114767332300399,-0.0327445246967096,
0.0788228839429136));
#87986=CARTESIAN_POINT('Ctrl Pts',(0.011652973929092,-0.032443687833936,
0.0786964253272376));
#87987=CARTESIAN_POINT('Ctrl Pts',(0.0118191885671562,-0.0321434074405927,
0.0785570507973754));
#87988=CARTESIAN_POINT('',(0.0115060334985778,-0.0326943950436612,0.0788017202309093));
#87989=CARTESIAN_POINT('',(0.0116942917389023,-0.0323666188837389,0.0786588342820951));
#87990=CARTESIAN_POINT('Origin',(0.0015584957656978,-0.0326395579111893,
0.0652497996555712));
#87991=CARTESIAN_POINT('Origin',(0.0185509122750033,-0.0321933825603024,
0.0873173634101982));
#87992=CARTESIAN_POINT('',(0.0115954533556887,-0.032193409653269,0.0787353706868489));
#87993=CARTESIAN_POINT('',(0.011644450849865,-0.0321934096584275,0.078696569966362));
#87994=CARTESIAN_POINT('',(0.0114041341068709,-0.0325210109756239,0.078874131276952));
#87995=CARTESIAN_POINT('Origin',(0.00196176277145783,-0.0326393129156889,
0.0649879597203443));
#87996=CARTESIAN_POINT('',(0.0114033592510911,-0.0326943950436593,0.0788730153843445));
#87997=CARTESIAN_POINT('Origin',(0.0177129541740383,-0.0326943765538247,
0.0879596499987013));
#87998=CARTESIAN_POINT('',(0.0114546963748445,-0.0326943950436702,0.0788373678076369));
#87999=CARTESIAN_POINT('Ctrl Pts',(0.0113501439061946,-0.0325229783203769,
0.0792087142730545));
#88000=CARTESIAN_POINT('Ctrl Pts',(0.0114198781718219,-0.032413025309245,
0.0791642389473955));
#88001=CARTESIAN_POINT('Ctrl Pts',(0.0114886818316376,-0.032303122220807,
0.0791183278244265));
#88002=CARTESIAN_POINT('Ctrl Pts',(0.0115564688282168,-0.0321934096576658,
0.0790710428229413));
#88003=CARTESIAN_POINT('Ctrl Pts',(0.011367857873235,-0.0325229783203769,
0.0790967885941045));
#88004=CARTESIAN_POINT('Ctrl Pts',(0.0114360492458256,-0.032413025309245,
0.0790520690817973));
#88005=CARTESIAN_POINT('Ctrl Pts',(0.0115033051953001,-0.032303122220807,
0.0790059457259401));
#88006=CARTESIAN_POINT('Ctrl Pts',(0.0115695416563333,-0.0321934096576658,
0.078958480647226));
#88007=CARTESIAN_POINT('Ctrl Pts',(0.0113855718402754,-0.0325229783203769,
0.0789848629151546));
#88008=CARTESIAN_POINT('Ctrl Pts',(0.0114522203198293,-0.032413025309245,
0.078939899216199));
#88009=CARTESIAN_POINT('Ctrl Pts',(0.0115179285589626,-0.032303122220807,
0.0788935636274538));
#88010=CARTESIAN_POINT('Ctrl Pts',(0.0115826144844499,-0.0321934096576658,
0.0788459184715107));
#88011=CARTESIAN_POINT('Ctrl Pts',(0.0114032858073158,-0.0325229783203769,
0.0788729372362046));
#88012=CARTESIAN_POINT('Ctrl Pts',(0.0114683913938331,-0.032413025309245,
0.0788277293506008));
#88013=CARTESIAN_POINT('Ctrl Pts',(0.0115325519226251,-0.032303122220807,
0.0787811815289674));
#88014=CARTESIAN_POINT('Ctrl Pts',(0.0115956873125665,-0.0321934096576658,
0.0787333562957954));
#88015=CARTESIAN_POINT('',(0.0115759610898133,-0.0321934096584275,0.0789032067565886));
#88016=CARTESIAN_POINT('Ctrl Pts',(0.0115459495551305,-0.0322104233328908,
0.0790783638752414));
#88017=CARTESIAN_POINT('Ctrl Pts',(0.0115214371126354,-0.0322609421830669,
0.0790430627858127));
#88018=CARTESIAN_POINT('Ctrl Pts',(0.0114973657711097,-0.0323120888239312,
0.0790083969388642));
#88019=CARTESIAN_POINT('Ctrl Pts',(0.0114500840494887,-0.0324156524631813,
0.078940305140847));
#88020=CARTESIAN_POINT('Ctrl Pts',(0.0114268931047555,-0.0324680267167303,
0.0789069071792147));
#88021=CARTESIAN_POINT('Ctrl Pts',(0.0114041341068498,-0.0325210109755912,
0.0788741312769138));
#88022=CARTESIAN_POINT('Origin',(0.00116774491061051,-0.0262834582510706,
0.0778265379320862));
#88023=CARTESIAN_POINT('Origin',(0.00985802840244437,-0.034277079370463,
0.0861839400837242));
#88024=CARTESIAN_POINT('Ctrl Pts',(0.0115040379693967,-0.0326943950436604,
0.0788013602946374));
#88025=CARTESIAN_POINT('Ctrl Pts',(0.011568142431835,-0.0325844576448134,
0.0787547740347656));
#88026=CARTESIAN_POINT('Ctrl Pts',(0.0116312879508125,-0.0324744968375323,
0.0787068586925279));
#88027=CARTESIAN_POINT('Ctrl Pts',(0.0116933944673868,-0.0323646534831895,
0.0786576767757881));
#88028=CARTESIAN_POINT('Ctrl Pts',(0.011615557116054,-0.0326943950436604,
0.0788214751526123));
#88029=CARTESIAN_POINT('Ctrl Pts',(0.0116799387989345,-0.0325844576448134,
0.0787733519498904));
#88030=CARTESIAN_POINT('Ctrl Pts',(0.0117433297714754,-0.0324744968375323,
0.0787238938226575));
#88031=CARTESIAN_POINT('Ctrl Pts',(0.0118056496875099,-0.0323646534831895,
0.0786731652598213));
#88032=CARTESIAN_POINT('Ctrl Pts',(0.0117270762627113,-0.0326943950436604,
0.0788415900105872));
#88033=CARTESIAN_POINT('Ctrl Pts',(0.011791735166034,-0.0325844576448134,
0.0787919298650152));
#88034=CARTESIAN_POINT('Ctrl Pts',(0.0118553715921384,-0.0324744968375323,
0.0787409289527872));
#88035=CARTESIAN_POINT('Ctrl Pts',(0.011917904907633,-0.0323646534831895,
0.0786886537438546));
#88036=CARTESIAN_POINT('Ctrl Pts',(0.0118385954093686,-0.0326943950436604,
0.0788617048685621));
#88037=CARTESIAN_POINT('Ctrl Pts',(0.0119035315331335,-0.0325844576448134,
0.07881050778014));
#88038=CARTESIAN_POINT('Ctrl Pts',(0.0119674134128014,-0.0324744968375323,
0.0787579640829168));
#88039=CARTESIAN_POINT('Ctrl Pts',(0.0120301601277561,-0.0323646534831895,
0.0787041422278879));
#88040=CARTESIAN_POINT('',(0.0118486512197805,-0.0326773559991214,0.0788537592109377));
#88041=CARTESIAN_POINT('',(0.0118385954093546,-0.0326943950436594,0.078861704868559));
#88042=CARTESIAN_POINT('Origin',(0.00150060062565762,-0.0326395670099125,
0.0658671835419942));
#88043=CARTESIAN_POINT('Ctrl Pts',(0.0118486512176951,-0.0326773559987507,
0.0788537592083056));
#88044=CARTESIAN_POINT('Ctrl Pts',(0.0118219852332526,-0.0326267922587257,
0.0788200854417806));
#88045=CARTESIAN_POINT('Ctrl Pts',(0.0117957918841262,-0.0325756109581914,
0.0787870085184482));
#88046=CARTESIAN_POINT('Ctrl Pts',(0.0117443281644271,-0.0324719985462387,
0.0787220202077638));
#88047=CARTESIAN_POINT('Ctrl Pts',(0.0117190784347338,-0.0324196091621786,
0.0786901348856845));
#88048=CARTESIAN_POINT('Ctrl Pts',(0.011694291738872,-0.0323666188837757,
0.0786588342820569));
#88049=CARTESIAN_POINT('',(0.0116723144539762,-0.0326943950436703,0.0788317125497442));
#88050=CARTESIAN_POINT('Origin',(0.00812378219310841,-0.0315241814719618,
0.07415));
#88051=CARTESIAN_POINT('',(0.0118486512197516,-0.0327114338379854,0.0788537592109012));
#88052=CARTESIAN_POINT('',(0.0118586900372345,-0.0326943950436593,0.0788457920946194));
#88053=CARTESIAN_POINT('Origin',(0.00146556789155393,-0.0326395682109143,
0.0658959171250404));
#88054=CARTESIAN_POINT('Origin',(0.00157937342544954,-0.0326395672564601,
0.0658048029865228));
#88055=CARTESIAN_POINT('Origin',(0.00161537198770351,-0.0326395685302088,
0.0657772892051259));
#88056=CARTESIAN_POINT('Ctrl Pts',(0.0115665997166451,-0.0332451089994585,
0.0787570741799572));
#88057=CARTESIAN_POINT('Ctrl Pts',(0.0117403583622355,-0.0329451141709491,
0.0786272261925931));
#88058=CARTESIAN_POINT('Ctrl Pts',(0.0119038426966181,-0.0326442513125814,
0.0784846588781363));
#88059=CARTESIAN_POINT('Ctrl Pts',(0.0117635601273721,-0.0332451089994585,
0.0786031047134833));
#88060=CARTESIAN_POINT('Ctrl Pts',(0.0119315117195243,-0.0329451141709491,
0.07846582824269));
#88061=CARTESIAN_POINT('Ctrl Pts',(0.0120886459539547,-0.0326442513125814,
0.078316290959346));
#88062=CARTESIAN_POINT('Ctrl Pts',(0.0117655297314794,-0.0332451089994585,
0.0786015650188185));
#88063=CARTESIAN_POINT('Ctrl Pts',(0.0119334232530972,-0.0329451141709491,
0.0784642142631909));
#88064=CARTESIAN_POINT('Ctrl Pts',(0.012090493986528,-0.0326442513125814,
0.0783146072801581));
#88065=CARTESIAN_POINT('',(0.0117914433282327,-0.0331951640388616,0.0785801678069685));
#88066=CARTESIAN_POINT('',(0.0119703582153917,-0.0328677532355047,0.0784257429734079));
#88067=CARTESIAN_POINT('Origin',(0.00052063326854975,-0.0326402808277589,
0.0661704503204892));
#88068=CARTESIAN_POINT('Origin',(0.0193649979077478,-0.0326944278779025,
0.0866448479610499));
#88069=CARTESIAN_POINT('',(0.011876520618294,-0.032694395043354,0.0785083344653819));
#88070=CARTESIAN_POINT('',(0.0119229851075173,-0.0326943950435166,0.0784665337326721));
#88071=CARTESIAN_POINT('',(0.0116942917389,-0.0330220786163545,0.0786588342820969));
#88072=CARTESIAN_POINT('Origin',(0.000856285506988594,-0.0326396675542845,
0.0658262276307959));
#88073=CARTESIAN_POINT('',(0.0116934483446432,-0.0331951640388587,0.0786577692450465));
#88074=CARTESIAN_POINT('Origin',(0.0185420247646317,-0.0331952026560106,
0.0873061431128978));
#88075=CARTESIAN_POINT('',(0.0117424458364479,-0.0331951640388701,0.0786189685260174));
#88076=CARTESIAN_POINT('Ctrl Pts',(0.0116614174918026,-0.0330240426238182,
0.0789961465612907));
#88077=CARTESIAN_POINT('Ctrl Pts',(0.0117281778820919,-0.0329142774062944,
0.0789474121884741));
#88078=CARTESIAN_POINT('Ctrl Pts',(0.011793964079251,-0.0328043479725528,
0.0788972733960413));
#88079=CARTESIAN_POINT('Ctrl Pts',(0.0118586900373371,-0.0326943950434843,
0.0788457920945455));
#88080=CARTESIAN_POINT('Ctrl Pts',(0.0116720686121853,-0.0330240426238182,
0.0788833294986647));
#88081=CARTESIAN_POINT('Ctrl Pts',(0.0117372748375237,-0.0329142774062944,
0.0788344483962879));
#88082=CARTESIAN_POINT('Ctrl Pts',(0.0118015030616142,-0.0328043479725528,
0.0787841949300757));
#88083=CARTESIAN_POINT('Ctrl Pts',(0.0118646692303477,-0.0326943950434843,
0.0787326312124532));
#88084=CARTESIAN_POINT('Ctrl Pts',(0.011682719732568,-0.0330240426238182,
0.0787705124360388));
#88085=CARTESIAN_POINT('Ctrl Pts',(0.0117463717929555,-0.0329142774062944,
0.0787214846041017));
#88086=CARTESIAN_POINT('Ctrl Pts',(0.0118090420439774,-0.0328043479725527,
0.0786711164641102));
#88087=CARTESIAN_POINT('Ctrl Pts',(0.0118706484233582,-0.0326943950434843,
0.078619470330361));
#88088=CARTESIAN_POINT('Ctrl Pts',(0.0116933708529506,-0.0330240426238182,
0.0786576953734128));
#88089=CARTESIAN_POINT('Ctrl Pts',(0.0117554687483874,-0.0329142774062944,
0.0786085208119155));
#88090=CARTESIAN_POINT('Ctrl Pts',(0.0118165810263407,-0.0328043479725527,
0.0785580379981446));
#88091=CARTESIAN_POINT('Ctrl Pts',(0.0118766276163688,-0.0326943950434843,
0.0785063094482687));
#88092=CARTESIAN_POINT('',(0.0118676053277743,-0.0326943950435166,0.0786770632800107));
#88093=CARTESIAN_POINT('Ctrl Pts',(0.0118486512176875,-0.03271143383833,
0.0788537592082961));
#88094=CARTESIAN_POINT('Ctrl Pts',(0.0118219896686433,-0.0327619876830289,
0.0788200910427856));
#88095=CARTESIAN_POINT('Ctrl Pts',(0.0117957984859586,-0.0328131562602952,
0.0787870168552327));
#88096=CARTESIAN_POINT('Ctrl Pts',(0.0117443348135807,-0.0329167375858764,
0.0787220286043055));
#88097=CARTESIAN_POINT('Ctrl Pts',(0.0117190828297671,-0.0329691088920605,
0.0786901404357263));
#88098=CARTESIAN_POINT('Ctrl Pts',(0.0116942917388726,-0.0330220786163186,
0.0786588342820579));
#88099=CARTESIAN_POINT('Ctrl Pts',(0.0117894288146236,-0.0331951640388604,
0.0785799338439174));
#88100=CARTESIAN_POINT('Ctrl Pts',(0.0118810148566372,-0.0330306422010619,
0.0785041489502114));
#88101=CARTESIAN_POINT('Ctrl Pts',(0.0119693903696656,-0.0328657861914644,
0.0784246434667358));
#88102=CARTESIAN_POINT('Ctrl Pts',(0.0117914433282302,-0.0331951640388604,
0.0785801678069704));
#88103=CARTESIAN_POINT('Ctrl Pts',(0.01188303420728,-0.0330306422010619,
0.0785043412644872));
#88104=CARTESIAN_POINT('Ctrl Pts',(0.0119714128318235,-0.0328657861914644,
0.0784247939679032));
#88105=CARTESIAN_POINT('Ctrl Pts',(0.0121271154706225,-0.0331951640388604,
0.0786191523434878));
#88106=CARTESIAN_POINT('Ctrl Pts',(0.0122195123299703,-0.0330306422010619,
0.0785363859946736));
#88107=CARTESIAN_POINT('Ctrl Pts',(0.0123084094166135,-0.0328657861914644,
0.0784498715097611));
#88108=CARTESIAN_POINT('',(0.012136652526609,-0.0331781648281957,0.078610590956646));
#88109=CARTESIAN_POINT('',(0.0121271154706064,-0.0331951640388588,0.078619152343485));
#88110=CARTESIAN_POINT('Origin',(0.000567094400286078,-0.0326412092823903,
0.0668151764484132));
#88111=CARTESIAN_POINT('Ctrl Pts',(0.0121366525247728,-0.033178164828644,
0.0786105909568528));
#88112=CARTESIAN_POINT('Ctrl Pts',(0.012107904979319,-0.0331276811546757,
0.0785786360323269));
#88113=CARTESIAN_POINT('Ctrl Pts',(0.0120796765003694,-0.0330765663497754,
0.0785472581373964));
#88114=CARTESIAN_POINT('Ctrl Pts',(0.0120242335428182,-0.0329730614463344,
0.0784856293391694));
#88115=CARTESIAN_POINT('Ctrl Pts',(0.0119970414659523,-0.0329207133374308,
0.0784554033289843));
#88116=CARTESIAN_POINT('Ctrl Pts',(0.0119703582108274,-0.03286775322894,
0.0784257429892357));
#88117=CARTESIAN_POINT('',(0.0119592793994295,-0.0331951640388701,0.0785996600752367));
#88118=CARTESIAN_POINT('Origin',(0.00812378219310841,-0.0315241814719618,
0.07415));
#88119=CARTESIAN_POINT('',(0.0121366525260512,-0.0332121607144401,0.078610590955059));
#88120=CARTESIAN_POINT('',(0.0121461712749854,-0.0331951640388587,0.0786020092176456));
#88121=CARTESIAN_POINT('Origin',(0.000539138682391462,-0.0326413666972893,
0.0668508777240834));
#88122=CARTESIAN_POINT('Origin',(0.00162613652128707,-0.0326412094582721,
0.0658624320638465));
#88123=CARTESIAN_POINT('Origin',(0.00166458628039381,-0.0326413667783289,
0.0658383954743563));
#88124=CARTESIAN_POINT('Ctrl Pts',(0.0118490708129398,-0.0337436976235975,
0.0785318203636108));
#88125=CARTESIAN_POINT('Ctrl Pts',(0.0118884815693732,-0.0336723290703325,
0.0784983145531811));
#88126=CARTESIAN_POINT('Ctrl Pts',(0.0119272832861533,-0.033601104548885,
0.0784641052879139));
#88127=CARTESIAN_POINT('Ctrl Pts',(0.0120511694816449,-0.0333736987606857,
0.0783548818803893));
#88128=CARTESIAN_POINT('Ctrl Pts',(0.0121685836535868,-0.0331450831799191,
0.0782387291601807));
#88129=CARTESIAN_POINT('Ctrl Pts',(0.0120359753458697,-0.0337436976235975,
0.0783657881511631));
#88130=CARTESIAN_POINT('Ctrl Pts',(0.0120738927834215,-0.0336723290703325,
0.0783306012930381));
#88131=CARTESIAN_POINT('Ctrl Pts',(0.0121111711861542,-0.033601104548885,
0.0782947381121293));
#88132=CARTESIAN_POINT('Ctrl Pts',(0.0122301937416443,-0.0333736987606857,
0.0781802340795834));
#88133=CARTESIAN_POINT('Ctrl Pts',(0.0123424492557671,-0.0331450831799191,
0.0780590885401124));
#88134=CARTESIAN_POINT('Ctrl Pts',(0.012037844391199,-0.0337436976235975,
0.0783641278290386));
#88135=CARTESIAN_POINT('Ctrl Pts',(0.012075746895562,-0.0336723290703325,
0.0783289241604367));
#88136=CARTESIAN_POINT('Ctrl Pts',(0.0121130100651542,-0.033601104548885,
0.0782930444403715));
#88137=CARTESIAN_POINT('Ctrl Pts',(0.0122319839842443,-0.0333736987606857,
0.0781784876015754));
#88138=CARTESIAN_POINT('Ctrl Pts',(0.0123441879117889,-0.0331450831799191,
0.0780572921339118));
#88139=CARTESIAN_POINT('',(0.0120623785749918,-0.0336938721132548,0.0783411315346355));
#88140=CARTESIAN_POINT('',(0.0122312439899657,-0.0333679869945434,0.0781757772650163));
#88141=CARTESIAN_POINT('Ctrl Pts',(0.0120623785749929,-0.033693872113265,
0.0783411315346356));
#88142=CARTESIAN_POINT('Ctrl Pts',(0.012078738527467,-0.0336629187933934,
0.0783257573453283));
#88143=CARTESIAN_POINT('Ctrl Pts',(0.0120950032255789,-0.0336319952301041,
0.0783102922789536));
#88144=CARTESIAN_POINT('Ctrl Pts',(0.0121111711861547,-0.0336011045488951,
0.078294738112129));
#88145=CARTESIAN_POINT('Ctrl Pts',(0.0121517421316042,-0.0335235892595455,
0.0782557073852299));
#88146=CARTESIAN_POINT('Ctrl Pts',(0.0121917759274989,-0.0334458668660371,
0.0782160461494159));
#88147=CARTESIAN_POINT('Ctrl Pts',(0.0122312439901772,-0.0333679869945386,
0.0781757772652327));
#88148=CARTESIAN_POINT('Ctrl Pts',(0.0122312756088197,-0.0333679692459666,
0.0781757459869489));
#88149=CARTESIAN_POINT('Ctrl Pts',(0.0122309477870204,-0.03333918953733,
0.0781754329842461));
#88150=CARTESIAN_POINT('Ctrl Pts',(0.0122306998261648,-0.0333104081058397,
0.0781752007220402));
#88151=CARTESIAN_POINT('Ctrl Pts',(0.0122303678211688,-0.0332532697887149,
0.0781748973252528));
#88152=CARTESIAN_POINT('Ctrl Pts',(0.0122302813836111,-0.0332249169570396,
0.0781748238408584));
#88153=CARTESIAN_POINT('Ctrl Pts',(0.0122302739339486,-0.0331960985434463,
0.0781748261980636));
#88154=CARTESIAN_POINT('Ctrl Pts',(0.0122302738343412,-0.033195631249,0.0781748262571799));
#88155=CARTESIAN_POINT('Ctrl Pts',(0.0122302737564736,-0.0331951640388607,
0.0781748263366275));
#88156=CARTESIAN_POINT('',(0.0121427775317648,-0.0331951640388587,0.0782640978923525));
#88157=CARTESIAN_POINT('',(0.0121865256441295,-0.0331951640388687,0.0782194621144997));
#88158=CARTESIAN_POINT('',(0.011970358200584,-0.0335216366567644,0.0784257429780441));
#88159=CARTESIAN_POINT('Origin',(-3.91172530374529E-5,-0.0326434571528741,
0.0668869750910637));
#88160=CARTESIAN_POINT('',(0.0119694495967205,-0.0336938721132327,0.0784247329999423));
#88161=CARTESIAN_POINT('Origin',(0.0192732533708569,-0.0336938867896295,
0.0865434324267544));
#88162=CARTESIAN_POINT('',(0.0120159140858662,-0.0336938721132537,0.0783829322672988));
#88163=CARTESIAN_POINT('Ctrl Pts',(0.0119587295760685,-0.0335235895815172,
0.0787644532254655));
#88164=CARTESIAN_POINT('Ctrl Pts',(0.0120222566097394,-0.0334144449262748,
0.0787116576244225));
#88165=CARTESIAN_POINT('Ctrl Pts',(0.012084765910891,-0.0333049234473147,
0.078657488946924));
#88166=CARTESIAN_POINT('Ctrl Pts',(0.0121461712749855,-0.0331951640388587,
0.0786020092176541));
#88167=CARTESIAN_POINT('Ctrl Pts',(0.0119622758238219,-0.0335235895815172,
0.0786511898306141));
#88168=CARTESIAN_POINT('Ctrl Pts',(0.0120242435638676,-0.0334144449262748,
0.0785983454084889));
#88169=CARTESIAN_POINT('Ctrl Pts',(0.0120851907713478,-0.0333049234473147,
0.0785441600676514));
#88170=CARTESIAN_POINT('Ctrl Pts',(0.0121450332372326,-0.0331951640388587,
0.0784886960350297));
#88171=CARTESIAN_POINT('Ctrl Pts',(0.0119658220715754,-0.0335235895815172,
0.0785379264357627));
#88172=CARTESIAN_POINT('Ctrl Pts',(0.0120262305179959,-0.0334144449262748,
0.0784850331925552));
#88173=CARTESIAN_POINT('Ctrl Pts',(0.0120856156318045,-0.0333049234473147,
0.0784308311883788));
#88174=CARTESIAN_POINT('Ctrl Pts',(0.0121438951994796,-0.0331951640388587,
0.0783753828524054));
#88175=CARTESIAN_POINT('Ctrl Pts',(0.0119693683193289,-0.0335235895815172,
0.0784246630409113));
#88176=CARTESIAN_POINT('Ctrl Pts',(0.0120282174721241,-0.0334144449262748,
0.0783717209766216));
#88177=CARTESIAN_POINT('Ctrl Pts',(0.0120860404922612,-0.0333049234473147,
0.0783175023091062));
#88178=CARTESIAN_POINT('Ctrl Pts',(0.0121427571617266,-0.0331951640388587,
0.078262069669781));
#88179=CARTESIAN_POINT('',(0.0121444744033851,-0.0331951640388687,0.078433053555009));
#88180=CARTESIAN_POINT('Ctrl Pts',(0.0121366525239504,-0.0332121607145951,
0.0786105909527245));
#88181=CARTESIAN_POINT('Ctrl Pts',(0.0121079533482372,-0.033262544410902,
0.0785786897765133));
#88182=CARTESIAN_POINT('Ctrl Pts',(0.0120797487043566,-0.0333135300745334,
0.0785473383076279));
#88183=CARTESIAN_POINT('Ctrl Pts',(0.0120243060916295,-0.0334167203140529,
0.078485709897952));
#88184=CARTESIAN_POINT('Ctrl Pts',(0.0119970895962799,-0.03346888475872,
0.0784554568264812));
#88185=CARTESIAN_POINT('Ctrl Pts',(0.0119703582002306,-0.0335216366562256,
0.0784257429774055));
#88186=CARTESIAN_POINT('Ctrl Pts',(0.0120613801103767,-0.0336938721132391,
0.0783410787777918));
#88187=CARTESIAN_POINT('Ctrl Pts',(0.0120859118852105,-0.0336474569764958,
0.0783180307105484));
#88188=CARTESIAN_POINT('Ctrl Pts',(0.012110172172384,-0.033601104548885,
0.0782946970471753));
#88189=CARTESIAN_POINT('Ctrl Pts',(0.0121715936417173,-0.0334837508592656,
0.0782356215762601));
#88190=CARTESIAN_POINT('Ctrl Pts',(0.0122312376105811,-0.0333660264659097,
0.0781747520014537));
#88191=CARTESIAN_POINT('Ctrl Pts',(0.0120623785749768,-0.0336938721132391,
0.0783411315346495));
#88192=CARTESIAN_POINT('Ctrl Pts',(0.012086910658614,-0.0336474569764958,
0.0783180776230615));
#88193=CARTESIAN_POINT('Ctrl Pts',(0.0121111711861542,-0.033601104548885,
0.0782947381121293));
#88194=CARTESIAN_POINT('Ctrl Pts',(0.0121725932640411,-0.0334837508592656,
0.0782356478365389));
#88195=CARTESIAN_POINT('Ctrl Pts',(0.0122322374024979,-0.0333660264659097,
0.0781747634455257));
#88196=CARTESIAN_POINT('Ctrl Pts',(0.012401860950161,-0.0336938721132391,
0.078359069099365));
#88197=CARTESIAN_POINT('Ctrl Pts',(0.0124264980283168,-0.0336474569764958,
0.0783340280847828));
#88198=CARTESIAN_POINT('Ctrl Pts',(0.0124508402816319,-0.033601104548885,
0.0783087003779206));
#88199=CARTESIAN_POINT('Ctrl Pts',(0.0125124692703907,-0.0334837508592656,
0.0782445764473504));
#88200=CARTESIAN_POINT('Ctrl Pts',(0.012572171071226,-0.0333660264659097,
0.0781786544805695));
#88201=CARTESIAN_POINT('',(0.0124088168679248,-0.0336769361243753,0.0783498187860456));
#88202=CARTESIAN_POINT('',(0.0123998362043608,-0.0336938721132327,0.0783589621158728));
#88203=CARTESIAN_POINT('Ctrl Pts',(0.0124088168679248,-0.0336769361243754,
0.0783498187860455));
#88204=CARTESIAN_POINT('Ctrl Pts',(0.0124073216062175,-0.0336797586670156,
0.0783513443871703));
#88205=CARTESIAN_POINT('Ctrl Pts',(0.0124058255863224,-0.0336825812713104,
0.0783528691320589));
#88206=CARTESIAN_POINT('Ctrl Pts',(0.0124028320387384,-0.0336882265876415,
0.0783559169013605));
#88207=CARTESIAN_POINT('Ctrl Pts',(0.0124013345110642,-0.0336910492997076,
0.078357439925808));
#88208=CARTESIAN_POINT('Ctrl Pts',(0.0123998362043744,-0.0336938721132379,
0.0783589621158764));
#88209=CARTESIAN_POINT('Ctrl Pts',(0.0124088168679248,-0.0336769361243754,
0.0783498187860455));
#88210=CARTESIAN_POINT('Ctrl Pts',(0.0123788824302282,-0.0336278994593125,
0.0783204796503493));
#88211=CARTESIAN_POINT('Ctrl Pts',(0.0123485218101857,-0.0335767852487005,
0.0782907228077369));
#88212=CARTESIAN_POINT('Ctrl Pts',(0.0122890250589367,-0.033473317179916,
0.0782324092601074));
#88213=CARTESIAN_POINT('Ctrl Pts',(0.0122598534681551,-0.033420963132189,
0.0782038178006946));
#88214=CARTESIAN_POINT('Ctrl Pts',(0.0122312439848548,-0.0333679869844682,
0.0781757772702107));
#88215=CARTESIAN_POINT('',(0.0122311073896863,-0.0336938721132538,0.0783500468252642));
#88216=CARTESIAN_POINT('Origin',(0.00812378219310841,-0.0315241814719618,
0.07415));
#88217=CARTESIAN_POINT('',(0.0124088168670061,-0.0337108120655666,0.078349818785145));
#88218=CARTESIAN_POINT('',(0.012417777980685,-0.0336938721132327,0.0783406562942192));
#88219=CARTESIAN_POINT('Origin',(0.00150638244369434,-0.0345562526942704,
0.0660993020739212));
#88220=CARTESIAN_POINT('Ctrl Pts',(0.012417777980689,-0.033693872113238,
0.0783406562942328));
#88221=CARTESIAN_POINT('Ctrl Pts',(0.0124162861899165,-0.0336910492985901,
0.0783421848718215));
#88222=CARTESIAN_POINT('Ctrl Pts',(0.0124147935501724,-0.0336882265870826,
0.0783437126864011));
#88223=CARTESIAN_POINT('Ctrl Pts',(0.0124118065200469,-0.0336825812713082,
0.0783467668429596));
#88224=CARTESIAN_POINT('Ctrl Pts',(0.0124103121296314,-0.0336797586670143,
0.0783482931849215));
#88225=CARTESIAN_POINT('Ctrl Pts',(0.0124088168679246,-0.033676936124375,
0.0783498187860458));
#88226=CARTESIAN_POINT('Origin',(-5.81985527356521E-5,-0.034556252294033,
0.0676956299121895));
#88227=CARTESIAN_POINT('Ctrl Pts',(0.0121168194200936,-0.034243627687391,
0.0782892968852102));
#88228=CARTESIAN_POINT('Ctrl Pts',(0.0122729355757268,-0.0339430054201809,
0.0781386970035239));
#88229=CARTESIAN_POINT('Ctrl Pts',(0.0124172644215758,-0.0336441434784052,
0.077976765651805));
#88230=CARTESIAN_POINT('Ctrl Pts',(0.0122929314838561,-0.034243627687391,
0.0781118580478681));
#88231=CARTESIAN_POINT('Ctrl Pts',(0.0124423554234164,-0.0339430054201809,
0.0779546159901993));
#88232=CARTESIAN_POINT('Ctrl Pts',(0.0125795107491663,-0.0336441434784052,
0.0777865654173588));
#88233=CARTESIAN_POINT('Ctrl Pts',(0.0122946926044938,-0.034243627687391,
0.0781100836594947));
#88234=CARTESIAN_POINT('Ctrl Pts',(0.0124440496218933,-0.0339430054201809,
0.0779527751800661));
#88235=CARTESIAN_POINT('Ctrl Pts',(0.0125811332124422,-0.0336441434784052,
0.0777846634150143));
#88236=CARTESIAN_POINT('',(0.0123177699811834,-0.0341934961088741,0.0780855547809017));
#88237=CARTESIAN_POINT('',(0.0124759194944158,-0.0338664212864897,0.077909923657779));
#88238=CARTESIAN_POINT('Origin',(0.00046885273275643,-0.0345610720403415,
0.0662679279544497));
#88239=CARTESIAN_POINT('Origin',(0.0207742693606469,-0.0336938005072936,
0.0850790319675171));
#88240=CARTESIAN_POINT('',(0.0123931733065714,-0.0336938721132327,0.078003624854638));
#88241=CARTESIAN_POINT('',(0.0124340323883481,-0.0336938721132427,0.0779563301885937));
#88242=CARTESIAN_POINT('',(0.012231243984851,-0.0340203938281605,0.0781757772702145));
#88243=CARTESIAN_POINT('Origin',(0.000857110895691337,-0.0345589643242984,
0.0659836880327022));
#88244=CARTESIAN_POINT('',(0.0122302737564741,-0.034193496108874,0.078174826336627));
#88245=CARTESIAN_POINT('Origin',(0.0201000588175834,-0.0341934220717647,
0.0858881071786148));
#88246=CARTESIAN_POINT('',(0.0122740218688388,-0.0341934961088841,0.0781301905587744));
#88247=CARTESIAN_POINT('Ctrl Pts',(0.0122409041083963,-0.0340223579322396,
0.0785145511951107));
#88248=CARTESIAN_POINT('Ctrl Pts',(0.0123011026526042,-0.0339125849573575,
0.0784577653459942));
#88249=CARTESIAN_POINT('Ctrl Pts',(0.0123600835608676,-0.0338030433565231,
0.0783997734296534));
#88250=CARTESIAN_POINT('Ctrl Pts',(0.0124177779806857,-0.0336938721132327,
0.0783406562942283));
#88251=CARTESIAN_POINT('Ctrl Pts',(0.0122373315416637,-0.0340223579322396,
0.0784012885949387));
#88252=CARTESIAN_POINT('Ctrl Pts',(0.012295967899214,-0.0339125849573575,
0.078344552020835));
#88253=CARTESIAN_POINT('Ctrl Pts',(0.0123533887384284,-0.0338030433565231,
0.0782866416785159));
#88254=CARTESIAN_POINT('Ctrl Pts',(0.0124095271926243,-0.0336938721132327,
0.0782276381349478));
#88255=CARTESIAN_POINT('Ctrl Pts',(0.0122337589749311,-0.0340223579322396,
0.0782880259947666));
#88256=CARTESIAN_POINT('Ctrl Pts',(0.0122908331458238,-0.0339125849573575,
0.0782313386956758));
#88257=CARTESIAN_POINT('Ctrl Pts',(0.0123466939159893,-0.0338030433565231,
0.0781735099273784));
#88258=CARTESIAN_POINT('Ctrl Pts',(0.0124012764045629,-0.0336938721132327,
0.0781146199756672));
#88259=CARTESIAN_POINT('Ctrl Pts',(0.0122301864081985,-0.0340223579322396,
0.0781747633945945));
#88260=CARTESIAN_POINT('Ctrl Pts',(0.0122856983924335,-0.0339125849573575,
0.0781181253705167));
#88261=CARTESIAN_POINT('Ctrl Pts',(0.0123399990935502,-0.0338030433565231,
0.0780603781762409));
#88262=CARTESIAN_POINT('Ctrl Pts',(0.0123930256165015,-0.0336938721132327,
0.0780016018163867));
#88263=CARTESIAN_POINT('',(0.0124054756436382,-0.0336938721132427,0.0781721405744386));
#88264=CARTESIAN_POINT('Ctrl Pts',(0.012408816864427,-0.0337108120662662,
0.0783498187826173));
#88265=CARTESIAN_POINT('Ctrl Pts',(0.0123781079805278,-0.0337611408993578,
0.0783197206020225));
#88266=CARTESIAN_POINT('Ctrl Pts',(0.0123479594656285,-0.0338121088779845,
0.078290171646447));
#88267=CARTESIAN_POINT('Ctrl Pts',(0.0122887557088512,-0.0339153382773235,
0.0782321452665488));
#88268=CARTESIAN_POINT('Ctrl Pts',(0.0122597255139114,-0.0339675558473122,
0.0782036923910593));
#88269=CARTESIAN_POINT('Ctrl Pts',(0.0122312439848262,-0.0340203938281304,
0.0781757772701829));
#88270=CARTESIAN_POINT('Ctrl Pts',(0.0123157419360611,-0.0341934961088741,
0.0780855751491577));
#88271=CARTESIAN_POINT('Ctrl Pts',(0.0123971068517772,-0.0340287516182428,
0.0779989096839477));
#88272=CARTESIAN_POINT('Ctrl Pts',(0.0124748202933024,-0.0338644633275951,
0.0779089553990256));
#88273=CARTESIAN_POINT('Ctrl Pts',(0.0123177699811834,-0.0341934961088741,
0.0780855547809017));
#88274=CARTESIAN_POINT('Ctrl Pts',(0.0123991344758018,-0.0340287516182428,
0.0779988473874565));
#88275=CARTESIAN_POINT('Ctrl Pts',(0.0124768457636635,-0.0338644633275951,
0.0779088512275303));
#88276=CARTESIAN_POINT('Ctrl Pts',(0.0126556813064923,-0.0341934961088741,
0.078082161037681));
#88277=CARTESIAN_POINT('Ctrl Pts',(0.0127369756381432,-0.0340287516182428,
0.0779884675937955));
#88278=CARTESIAN_POINT('Ctrl Pts',(0.0128143280842256,-0.0338644633275951,
0.0778914942527643));
#88279=CARTESIAN_POINT('',(0.0126640701331909,-0.0341764758832446,0.0780724718497314));
#88280=CARTESIAN_POINT('',(0.0126556813064761,-0.034193496108874,0.0780821610376811));
#88281=CARTESIAN_POINT('Origin',(0.000469360212365722,-0.0345621026190861,
0.0668604076600941));
#88282=CARTESIAN_POINT('Ctrl Pts',(0.0126640701314842,-0.0341764758837558,
0.078072471850373));
#88283=CARTESIAN_POINT('Ctrl Pts',(0.0126315886167829,-0.0341260050040584,
0.0780444102502477));
#88284=CARTESIAN_POINT('Ctrl Pts',(0.012599671682457,-0.0340749269148397,
0.0780168364558454));
#88285=CARTESIAN_POINT('Ctrl Pts',(0.0125369423585455,-0.0339715436307112,
0.0779626429697402));
#88286=CARTESIAN_POINT('Ctrl Pts',(0.0125061537708994,-0.0339192778237382,
0.0779360438332403));
#88287=CARTESIAN_POINT('Ctrl Pts',(0.0124759194946897,-0.0338664212854664,
0.0779099236595325));
#88288=CARTESIAN_POINT('',(0.0124867256438398,-0.0341934961088841,0.0780838579093015));
#88289=CARTESIAN_POINT('Origin',(0.00812378219310841,-0.0315241814719618,
0.07415));
#88290=CARTESIAN_POINT('',(0.0126640701331818,-0.0342105180190352,0.0780724718486117));
#88291=CARTESIAN_POINT('',(0.012672438246751,-0.0341934961088739,0.0780627647649283));
#88292=CARTESIAN_POINT('Origin',(0.000435969997987811,-0.0345621721966557,
0.0668910575975215));
#88293=CARTESIAN_POINT('Origin',(-0.000200204842937758,-0.0345621029191649,
0.0676354332226913));
#88294=CARTESIAN_POINT('Origin',(-0.000174728215152024,-0.034562172372312,
0.0675979463160218));
#88295=CARTESIAN_POINT('Ctrl Pts',(0.0123921926821259,-0.0346945769586966,
0.0780047599341273));
#88296=CARTESIAN_POINT('Ctrl Pts',(0.0124729321723079,-0.0345275153362944,
0.0779153563674564));
#88297=CARTESIAN_POINT('Ctrl Pts',(0.0125508808859761,-0.0343603235965185,
0.0778233904937933));
#88298=CARTESIAN_POINT('Ctrl Pts',(0.0126258123279797,-0.034193496108874,
0.0777291377337591));
#88299=CARTESIAN_POINT('Ctrl Pts',(0.0124469983329902,-0.0346945769586966,
0.0779413220191414));
#88300=CARTESIAN_POINT('Ctrl Pts',(0.0125264090906437,-0.0345275153362944,
0.0778507705261702));
#88301=CARTESIAN_POINT('Ctrl Pts',(0.0126029926268795,-0.0343603235965185,
0.0777576982167093));
#88302=CARTESIAN_POINT('Ctrl Pts',(0.0126765265327713,-0.034193496108874,
0.0776623837237165));
#88303=CARTESIAN_POINT('Ctrl Pts',(0.0125018039838545,-0.0346945769586966,
0.0778778841041562));
#88304=CARTESIAN_POINT('Ctrl Pts',(0.0125798860089796,-0.0345275153362944,
0.0777861846848856));
#88305=CARTESIAN_POINT('Ctrl Pts',(0.012655104367783,-0.0343603235965185,
0.0776920059396272));
#88306=CARTESIAN_POINT('Ctrl Pts',(0.0127272407375627,-0.034193496108874,
0.0775956297136759));
#88307=CARTESIAN_POINT('Ctrl Pts',(0.0125566096347188,-0.0346945769586966,
0.0778144461891698));
#88308=CARTESIAN_POINT('Ctrl Pts',(0.0126333629273152,-0.0345275153362944,
0.077721598843598));
#88309=CARTESIAN_POINT('Ctrl Pts',(0.0127072161086863,-0.0343603235965185,
0.0776263136625413));
#88310=CARTESIAN_POINT('Ctrl Pts',(0.0127779549423545,-0.034193496108874,
0.0775288757036314));
#88311=CARTESIAN_POINT('',(0.0125566096336416,-0.0346945769586966,0.0778144461904163));
#88312=CARTESIAN_POINT('',(0.0127034191051059,-0.0343667727836579,0.0776292313455091));
#88313=CARTESIAN_POINT('Origin',(-0.000518188304912433,-0.0345626474181758,
0.067243405364632));
#88314=CARTESIAN_POINT('Origin',(0.0215039495486088,-0.034193477102429,
0.0843151360524152));
#88315=CARTESIAN_POINT('',(0.0126267197451524,-0.0341934961088739,0.0777279433201761));
#88316=CARTESIAN_POINT('',(0.0126645285442121,-0.034193496108884,0.0776781764163802));
#88317=CARTESIAN_POINT('',(0.0124759194935752,-0.0345211942962607,0.0779099236585232));
#88318=CARTESIAN_POINT('Origin',(-0.000201345948739516,-0.0345625596121062,
0.0668817433285368));
#88319=CARTESIAN_POINT('',(0.0124748914701046,-0.0346945769586886,0.0779090355225294));
#88320=CARTESIAN_POINT('Origin',(0.0208468542829956,-0.0346945685853896,
0.085141791143449));
#88321=CARTESIAN_POINT('',(0.0125157505518831,-0.0346945769587026,0.0778617408564829));
#88322=CARTESIAN_POINT('Ctrl Pts',(0.0125068330028904,-0.0345231616327841,
0.0782474218234103));
#88323=CARTESIAN_POINT('Ctrl Pts',(0.0125633101940176,-0.0344132092796987,
0.0781870076388393));
#88324=CARTESIAN_POINT('Ctrl Pts',(0.0126185348514276,-0.0343032738558979,
0.0781254283852128));
#88325=CARTESIAN_POINT('Ctrl Pts',(0.0126724382467524,-0.0341934961088739,
0.0780627647649376));
#88326=CARTESIAN_POINT('Ctrl Pts',(0.0124961556683675,-0.0345231616327841,
0.0781346072380655));
#88327=CARTESIAN_POINT('Ctrl Pts',(0.012551077869266,-0.0344132092796987,
0.0780743402255184));
#88328=CARTESIAN_POINT('Ctrl Pts',(0.0126047506608148,-0.0343032738558979,
0.0780129403000687));
#88329=CARTESIAN_POINT('Ctrl Pts',(0.0126571072968806,-0.0341934961088739,
0.0779504878834568));
#88330=CARTESIAN_POINT('Ctrl Pts',(0.0124854783338447,-0.0345231616327841,
0.0780217926527206));
#88331=CARTESIAN_POINT('Ctrl Pts',(0.0125388455445144,-0.0344132092796988,
0.0779616728121975));
#88332=CARTESIAN_POINT('Ctrl Pts',(0.012590966470202,-0.0343032738558979,
0.0779004522149246));
#88333=CARTESIAN_POINT('Ctrl Pts',(0.0126417763470089,-0.0341934961088739,
0.0778382110019759));
#88334=CARTESIAN_POINT('Ctrl Pts',(0.0124748009993219,-0.0345231616327841,
0.0779089780673758));
#88335=CARTESIAN_POINT('Ctrl Pts',(0.0125266132197628,-0.0344132092796988,
0.0778490053988766));
#88336=CARTESIAN_POINT('Ctrl Pts',(0.0125771822795893,-0.0343032738558979,
0.0777879641297806));
#88337=CARTESIAN_POINT('Ctrl Pts',(0.0126264453971372,-0.0341934961088739,
0.0777259341204951));
#88338=CARTESIAN_POINT('',(0.0126495789959617,-0.0341934961088839,0.0778953540425622));
#88339=CARTESIAN_POINT('Ctrl Pts',(0.0126640701305619,-0.0342105180195359,
0.0780724718463475));
#88340=CARTESIAN_POINT('Ctrl Pts',(0.0126315521093654,-0.034261055624039,
0.0780443786891735));
#88341=CARTESIAN_POINT('Ctrl Pts',(0.0125996176072439,-0.0343122189868302,
0.0780167896491778));
#88342=CARTESIAN_POINT('Ctrl Pts',(0.0125368876477865,-0.0344158119695079,
0.0779625956193533));
#88343=CARTESIAN_POINT('Ctrl Pts',(0.0125061178476239,-0.0344681990449959,
0.0779360127954183));
#88344=CARTESIAN_POINT('Ctrl Pts',(0.0124759194935518,-0.0345211942962354,
0.0779099236584989));
#88345=CARTESIAN_POINT('Ctrl Pts',(0.0125545873649794,-0.0346945769586931,
0.0778145938243097));
#88346=CARTESIAN_POINT('Ctrl Pts',(0.0126303502492178,-0.0345296777079064,
0.0777229900626341));
#88347=CARTESIAN_POINT('Ctrl Pts',(0.0127022623273767,-0.0343648066255586,
0.0776283332256064));
#88348=CARTESIAN_POINT('Ctrl Pts',(0.0125566096336358,-0.0346945769586931,
0.0778144461904233));
#88349=CARTESIAN_POINT('Ctrl Pts',(0.0126323694656481,-0.0345296777079064,
0.0777228006197742));
#88350=CARTESIAN_POINT('Ctrl Pts',(0.0127042767661856,-0.0343648066255586,
0.0776281021356496));
#88351=CARTESIAN_POINT('Ctrl Pts',(0.0128936410732322,-0.0346945769586931,
0.0777898415163088));
#88352=CARTESIAN_POINT('Ctrl Pts',(0.0129688922210175,-0.0345296777079064,
0.0776912280591307));
#88353=CARTESIAN_POINT('Ctrl Pts',(0.0130400032828396,-0.0343648066255586,
0.0775895886668355));
#88354=CARTESIAN_POINT('',(0.0129014049576017,-0.0346775396665031,0.0777796447090279));
#88355=CARTESIAN_POINT('',(0.0128936410732186,-0.0346945769586886,0.0777898415163072));
#88356=CARTESIAN_POINT('Origin',(-0.000409778919642414,-0.0345626618041964,
0.0678586927481973));
#88357=CARTESIAN_POINT('Ctrl Pts',(0.0129014049558933,-0.0346775396670096,
0.0777796447096775));
#88358=CARTESIAN_POINT('Ctrl Pts',(0.0128671986149924,-0.034626974993105,
0.0777536575622933));
#88359=CARTESIAN_POINT('Ctrl Pts',(0.0128336001753502,-0.0345757902896753,
0.0777281322931075));
#88360=CARTESIAN_POINT('Ctrl Pts',(0.0127675915318585,-0.0344721681087866,
0.0776779843517497));
#88361=CARTESIAN_POINT('Ctrl Pts',(0.0127352072103651,-0.0344197714287363,
0.0776533813357851));
#88362=CARTESIAN_POINT('Ctrl Pts',(0.0127034191049817,-0.03436677278343,
0.0776292313461726));
#88363=CARTESIAN_POINT('',(0.0127251253534401,-0.0346945769587026,0.0778021438533718));
#88364=CARTESIAN_POINT('Origin',(0.00812378219310841,-0.0315241814719618,
0.07415));
#88365=CARTESIAN_POINT('',(0.0129014049571081,-0.0347116136489595,0.0777796447077254));
#88366=CARTESIAN_POINT('',(0.0129091470454567,-0.0346945769586885,0.0777694313406826));
#88367=CARTESIAN_POINT('Origin',(-0.000435675480596656,-0.0345626702815683,
0.0678958740026416));
#88368=CARTESIAN_POINT('Origin',(-0.000225010134284166,-0.0345626620959895,
0.0676154845536354));
#88369=CARTESIAN_POINT('Origin',(-0.000196131731250116,-0.0345626704986924,
0.0675805685326128));
#88370=CARTESIAN_POINT('Ctrl Pts',(0.0126026337480803,-0.0352450361874068,
0.0777581368286348));
#88371=CARTESIAN_POINT('Ctrl Pts',(0.0127387168615924,-0.0349452760959492,
0.077589214170347));
#88372=CARTESIAN_POINT('Ctrl Pts',(0.0128616894315066,-0.0346444289841739,
0.0774105210666332));
#88373=CARTESIAN_POINT('Ctrl Pts',(0.0126041738130506,-0.0352450361874068,
0.0777561358726414));
#88374=CARTESIAN_POINT('Ctrl Pts',(0.012740181459269,-0.0349452760959492,
0.0775871551298502));
#88375=CARTESIAN_POINT('Ctrl Pts',(0.0128630744011217,-0.0346444289841739,
0.0774084097911503));
#88376=CARTESIAN_POINT('Ctrl Pts',(0.0127566554932788,-0.0352450361874068,
0.0775580214178564));
#88377=CARTESIAN_POINT('Ctrl Pts',(0.0128851911302251,-0.0349452760959492,
0.0773832897341268));
#88378=CARTESIAN_POINT('Ctrl Pts',(0.013000200105595,-0.0346444289841739,
0.0771993726146177));
#88379=CARTESIAN_POINT('Ctrl Pts',(0.0127581803100811,-0.0352450361874068,
0.0775560402733086));
#88380=CARTESIAN_POINT('Ctrl Pts',(0.0128866412269346,-0.0349452760959492,
0.0773812510801696));
#88381=CARTESIAN_POINT('Ctrl Pts',(0.0130015713626397,-0.0346444289841739,
0.0771972822428523));
#88382=CARTESIAN_POINT('',(0.0127779378515802,-0.0351951634053346,0.0775289032849739));
#88383=CARTESIAN_POINT('',(0.0129128449811174,-0.0348678972925388,0.0773348080966532));
#88384=CARTESIAN_POINT('Origin',(-0.00126749047167203,-0.0345636767889031,
0.0684113137140681));
#88385=CARTESIAN_POINT('Origin',(0.022113868460618,-0.0346946199341121,
0.083453644271531));
#88386=CARTESIAN_POINT('',(0.0128424951359957,-0.0346945769330289,0.0774381412927178));
#88387=CARTESIAN_POINT('',(0.0128771044433858,-0.0346945769458128,0.077386098551345));
#88388=CARTESIAN_POINT('',(0.0127034191046605,-0.0350221583435276,0.0776292313459082));
#88389=CARTESIAN_POINT('Origin',(-0.00103679855261937,-0.0345628458713947,
0.0679895025826022));
#88390=CARTESIAN_POINT('',(0.0127024323802842,-0.0351951360298763,0.0776284855123135));
#88391=CARTESIAN_POINT('Origin',(0.0214765190564826,-0.0351951838366868,
0.0842943123085817));
#88392=CARTESIAN_POINT('',(0.0127779549414438,-0.0351951371328746,0.0775288757050221));
#88393=CARTESIAN_POINT('Ctrl Pts',(0.0127554639090662,-0.0350241211494343,
0.0779641217183193));
#88394=CARTESIAN_POINT('Ctrl Pts',(0.0128080018718853,-0.0349144232818962,
0.0779003222017455));
#88395=CARTESIAN_POINT('Ctrl Pts',(0.0128592524996112,-0.0348045283579412,
0.0778353985008526));
#88396=CARTESIAN_POINT('Ctrl Pts',(0.0129091470521623,-0.0346945769439157,
0.0777694313318289));
#88397=CARTESIAN_POINT('Ctrl Pts',(0.0127377239355663,-0.0350241211494343,
0.0778522001603256));
#88398=CARTESIAN_POINT('Ctrl Pts',(0.0127887202248136,-0.0349144232818962,
0.077788645004613));
#88399=CARTESIAN_POINT('Ctrl Pts',(0.0128384333073155,-0.0348045283579412,
0.0777239976783375));
#88400=CARTESIAN_POINT('Ctrl Pts',(0.0128867964255634,-0.0346945769439157,
0.0776583386169725));
#88401=CARTESIAN_POINT('Ctrl Pts',(0.0127199839620663,-0.0350241211494343,
0.0777402786023319));
#88402=CARTESIAN_POINT('Ctrl Pts',(0.0127694385777419,-0.0349144232818962,
0.0776769678074806));
#88403=CARTESIAN_POINT('Ctrl Pts',(0.0128176141150197,-0.0348045283579412,
0.0776125968558225));
#88404=CARTESIAN_POINT('Ctrl Pts',(0.0128644457989645,-0.0346945769439157,
0.0775472459021162));
#88405=CARTESIAN_POINT('Ctrl Pts',(0.0127022439885664,-0.0350241211494343,
0.0776283570443381));
#88406=CARTESIAN_POINT('Ctrl Pts',(0.0127501569306702,-0.0349144232818962,
0.0775652906103481));
#88407=CARTESIAN_POINT('Ctrl Pts',(0.012796794922724,-0.0348045283579412,
0.0775011960333074));
#88408=CARTESIAN_POINT('Ctrl Pts',(0.0128420951723656,-0.0346945769439157,
0.0774361531872598));
#88409=CARTESIAN_POINT('',(0.0128758210906322,-0.0346945769458128,0.0776037863169928));
#88410=CARTESIAN_POINT('Ctrl Pts',(0.012901404954484,-0.0347116136492762,
0.0777796447057305));
#88411=CARTESIAN_POINT('Ctrl Pts',(0.0128672122053332,-0.0347621546531334,
0.0777536678680586));
#88412=CARTESIAN_POINT('Ctrl Pts',(0.012833620657109,-0.0348133084095068,
0.0777281477733883));
#88413=CARTESIAN_POINT('Ctrl Pts',(0.0127676119278375,-0.0349168561544567,
0.0776779997716103));
#88414=CARTESIAN_POINT('Ctrl Pts',(0.0127352209292868,-0.034969208901592,
0.0776533917558094));
#88415=CARTESIAN_POINT('Ctrl Pts',(0.0127034191046435,-0.0350221583435,
0.0776292313458702));
#88416=CARTESIAN_POINT('Ctrl Pts',(0.0127765053750515,-0.0351951371254975,
0.0775290736373207));
#88417=CARTESIAN_POINT('Ctrl Pts',(0.0128463656024019,-0.0350307338980971,
0.0774328815047496));
#88418=CARTESIAN_POINT('Ctrl Pts',(0.0129121904099651,-0.0348659306897824,
0.0773338841692132));
#88419=CARTESIAN_POINT('Ctrl Pts',(0.0127779549413452,-0.0351951371254975,
0.0775288757049602));
#88420=CARTESIAN_POINT('Ctrl Pts',(0.0128478110765682,-0.0350307338980971,
0.0774326536035154));
#88421=CARTESIAN_POINT('Ctrl Pts',(0.0129136305568548,-0.0348659306897824,
0.0773336264938456));
#88422=CARTESIAN_POINT('Ctrl Pts',(0.0130209037629744,-0.0351951371254975,
0.0774957020350415));
#88423=CARTESIAN_POINT('Ctrl Pts',(0.0130900740533857,-0.0350307338980971,
0.0773944571191407));
#88424=CARTESIAN_POINT('Ctrl Pts',(0.0131550006765698,-0.0348659306897824,
0.0772904398336865));
#88425=CARTESIAN_POINT('Origin',(0.0173412084800945,-0.0308609197410323,
0.0802797450395314));
#88426=CARTESIAN_POINT('',(0.0128838751498071,-0.0351951371254975,0.0775144127328426));
#88427=CARTESIAN_POINT('Origin',(0.00724034756344459,-0.0351840467441114,
0.0737325207725142));
#88428=CARTESIAN_POINT('Origin',(0.0185052740279725,-0.0352322612843293,
0.0800994752299718));
#88429=CARTESIAN_POINT('',(0.0130397881752884,-0.0351951142564687,0.0771350795243343));
#88430=CARTESIAN_POINT('',(0.0131021944076713,-0.0351951372916787,0.0770271360450789));
#88431=CARTESIAN_POINT('Origin',(0.00811441848004271,-0.0352875113587952,
0.0738095910710146));
#88432=CARTESIAN_POINT('Origin',(0.00319514827069109,-0.0298325076522705,
0.0798071863977184));
#88433=CARTESIAN_POINT('Origin',(0.0132682144054627,-0.0338732916933875,
0.0807668555657059));
#88434=CARTESIAN_POINT('Origin',(0.00812378219310841,-0.0315241814719618,
0.07415));
#88435=CARTESIAN_POINT('',(0.0112297421631025,-0.032711433838004,0.0792835185442903));
#88436=CARTESIAN_POINT('',(0.0112407003659563,-0.0326943950436593,0.0792768724485572));
#88437=CARTESIAN_POINT('Origin',(0.00255258075290883,-0.032639568195616,
0.065126507472656));
#88438=CARTESIAN_POINT('',(0.0112297421631267,-0.0326773559991214,0.0792835185443304));
#88439=CARTESIAN_POINT('Origin',(0.00267690876419085,-0.0326395671481778,
0.0650503754881189));
#88440=CARTESIAN_POINT('',(0.0112187697908064,-0.0326943950436594,0.0792901412208319));
#88441=CARTESIAN_POINT('Origin',(0.0025909384096225,-0.032639567029855,
0.0651023909603269));
#88442=CARTESIAN_POINT('Origin',(0.00271607179587666,-0.0326395685042469,
0.0650275905864274));
#88443=CARTESIAN_POINT('Origin',(0.00812378219310841,-0.0315241814719618,
0.07415));
#88444=CARTESIAN_POINT('',(0.0109012769642797,-0.0322104233323771,0.0794684135584242));
#88445=CARTESIAN_POINT('',(0.0109126308553288,-0.0321934096636183,0.0794624686483067));
#88446=CARTESIAN_POINT('Origin',(0.00374745183614647,-0.0326387245399829,
0.0645417703628711));
#88447=CARTESIAN_POINT('',(0.0109012769641094,-0.032176398030833,0.079468413558098));
#88448=CARTESIAN_POINT('Origin',(0.00270254459298124,-0.0326386235886941,
0.0650945863296164));
#88449=CARTESIAN_POINT('',(0.010889910402055,-0.0321934096636184,0.0794743342054824));
#88450=CARTESIAN_POINT('Origin',(0.0037901657731102,-0.0326386231182652,
0.0645265867379557));
#88451=CARTESIAN_POINT('Origin',(0.00273941365981018,-0.0326387249493187,
0.0650682106328434));
#88452=CARTESIAN_POINT('Ctrl Pts',(0.0103460098434445,-0.0321934096636941,
0.0794546998044557));
#88453=CARTESIAN_POINT('Ctrl Pts',(0.0104409614437598,-0.0320508460845056,
0.0794149229877757));
#88454=CARTESIAN_POINT('Ctrl Pts',(0.0105347727256777,-0.0319086045664529,
0.0793726250008024));
#88455=CARTESIAN_POINT('Ctrl Pts',(0.0106272491948647,-0.0317669892870077,
0.0793279135477917));
#88456=CARTESIAN_POINT('Ctrl Pts',(0.0104226231303532,-0.0321934096636941,
0.0794206287478709));
#88457=CARTESIAN_POINT('Ctrl Pts',(0.0105169648749808,-0.0320508460845056,
0.0793794805898398));
#88458=CARTESIAN_POINT('Ctrl Pts',(0.010610129915808,-0.0319086045664529,
0.0793358286811301));
#88459=CARTESIAN_POINT('Ctrl Pts',(0.0107019253899721,-0.0317669892870077,
0.0792897835266752));
#88460=CARTESIAN_POINT('Ctrl Pts',(0.0104992364172618,-0.0321934096636941,
0.0793865576912862));
#88461=CARTESIAN_POINT('Ctrl Pts',(0.0105929683062018,-0.0320508460845056,
0.0793440381919037));
#88462=CARTESIAN_POINT('Ctrl Pts',(0.0106854871059383,-0.0319086045664529,
0.0792990323614578));
#88463=CARTESIAN_POINT('Ctrl Pts',(0.0107766015850794,-0.0317669892870077,
0.0792516535055587));
#88464=CARTESIAN_POINT('Ctrl Pts',(0.0105758497041705,-0.0321934096636941,
0.0793524866347013));
#88465=CARTESIAN_POINT('Ctrl Pts',(0.0106689717374229,-0.0320508460845056,
0.0793085957939678));
#88466=CARTESIAN_POINT('Ctrl Pts',(0.0107608442960687,-0.0319086045664529,
0.0792622360417856));
#88467=CARTESIAN_POINT('Ctrl Pts',(0.0108512777801867,-0.0317669892870077,
0.0792135234844422));
#88468=CARTESIAN_POINT('',(0.010574479077327,-0.0321934096636941,0.0793530961726343));
#88469=CARTESIAN_POINT('',(0.0107861769030896,-0.0318665617511359,0.0792480172025542));
#88470=CARTESIAN_POINT('Origin',(0.0040154436663245,-0.0326371944423981,
0.0639843955346272));
#88471=CARTESIAN_POINT('Origin',(0.0158602828240402,-0.0316939261509356,
0.0889640369233801));
#88472=CARTESIAN_POINT('',(0.010461038580429,-0.0320197221621739,0.0794049806609027));
#88473=CARTESIAN_POINT('Ctrl Pts',(0.0104612211737369,-0.0320197392094664,
0.0794049510878703));
#88474=CARTESIAN_POINT('Ctrl Pts',(0.0104879600352183,-0.0319792716575962,
0.0793930574039811));
#88475=CARTESIAN_POINT('Ctrl Pts',(0.0105147299495146,-0.0319386439829649,
0.0793809057291985));
#88476=CARTESIAN_POINT('Ctrl Pts',(0.0105415555241534,-0.0318979099381581,
0.0793684756053362));
#88477=CARTESIAN_POINT('Ctrl Pts',(0.0105683805685643,-0.0318571766984905,
0.0793560457271647));
#88478=CARTESIAN_POINT('Ctrl Pts',(0.0105951256777918,-0.0318163871833577,
0.0793434022042498));
#88479=CARTESIAN_POINT('Ctrl Pts',(0.0106217003645882,-0.0317755399638303,
0.0793305917084602));
#88480=CARTESIAN_POINT('',(0.01046026409342,-0.0321934096636183,0.079403889257447));
#88481=CARTESIAN_POINT('Origin',(0.0114171723695981,-0.0324111793032775,
0.0815038783672763));
#88482=CARTESIAN_POINT('',(0.0105173715853835,-0.0321934096636663,0.0793784927150506));
#88483=CARTESIAN_POINT('Ctrl Pts',(0.0105725858802839,-0.0321934096636618,
0.0793523685103946));
#88484=CARTESIAN_POINT('Ctrl Pts',(0.0106443305965311,-0.0320835708272592,
0.0793185975990625));
#88485=CARTESIAN_POINT('Ctrl Pts',(0.0107153348106724,-0.0319739230346488,
0.0792833615230574));
#88486=CARTESIAN_POINT('Ctrl Pts',(0.0107855111376682,-0.0318646057455573,
0.0792467123365913));
#88487=CARTESIAN_POINT('Ctrl Pts',(0.0106783607208703,-0.0321934096636618,
0.0793930237420977));
#88488=CARTESIAN_POINT('Ctrl Pts',(0.0107506661044475,-0.0320835708272592,
0.0793577941132779));
#88489=CARTESIAN_POINT('Ctrl Pts',(0.0108222004726264,-0.0319739230346488,
0.0793210885629191));
#88490=CARTESIAN_POINT('Ctrl Pts',(0.0108928759063637,-0.0318646057455573,
0.0792829610773814));
#88491=CARTESIAN_POINT('Ctrl Pts',(0.0107841355614567,-0.0321934096636618,
0.0794336789738009));
#88492=CARTESIAN_POINT('Ctrl Pts',(0.0108570016123639,-0.0320835708272592,
0.0793969906274932));
#88493=CARTESIAN_POINT('Ctrl Pts',(0.0109290661345804,-0.0319739230346488,
0.0793588156027809));
#88494=CARTESIAN_POINT('Ctrl Pts',(0.0110002406750592,-0.0318646057455573,
0.0793192098181715));
#88495=CARTESIAN_POINT('Ctrl Pts',(0.0108899104020431,-0.0321934096636618,
0.079474334205504));
#88496=CARTESIAN_POINT('Ctrl Pts',(0.0109633371202803,-0.0320835708272592,
0.0794361871417086));
#88497=CARTESIAN_POINT('Ctrl Pts',(0.0110359317965343,-0.0319739230346488,
0.0793965426426427));
#88498=CARTESIAN_POINT('Ctrl Pts',(0.0111076054437547,-0.0318646057455573,
0.0793554585589616));
#88499=CARTESIAN_POINT('Ctrl Pts',(0.0109012769626364,-0.0321763980306388,
0.0794684135552823));
#88500=CARTESIAN_POINT('Ctrl Pts',(0.0108814091290246,-0.0321259596176398,
0.0794303701512932));
#88501=CARTESIAN_POINT('Ctrl Pts',(0.0108618855314024,-0.0320749164634525,
0.0793929858986422));
#88502=CARTESIAN_POINT('Ctrl Pts',(0.0108235110959878,-0.0319716057794028,
0.0793195056099573));
#88503=CARTESIAN_POINT('Ctrl Pts',(0.0108046752103315,-0.0319193786690229,
0.0792834382046323));
#88504=CARTESIAN_POINT('Ctrl Pts',(0.0107861769022256,-0.0318665617525437,
0.0792480172009062));
#88505=CARTESIAN_POINT('',(0.010732194739701,-0.0321934096636663,0.0794137151890684));
#88506=CARTESIAN_POINT('Ctrl Pts',(0.010640079839047,-0.0327445246967097,
0.0793217504200265));
#88507=CARTESIAN_POINT('Ctrl Pts',(0.0108351355948679,-0.032443687833936,
0.0792268467028444));
#88508=CARTESIAN_POINT('Ctrl Pts',(0.0110224886820328,-0.0321434074405927,
0.0791175202003684));
#88509=CARTESIAN_POINT('Ctrl Pts',(0.0106423030738584,-0.0327445246967097,
0.0793206070797563));
#88510=CARTESIAN_POINT('Ctrl Pts',(0.010837315707896,-0.032443687833936,
0.0792256195119026));
#88511=CARTESIAN_POINT('Ctrl Pts',(0.0110246194798068,-0.0321434074405927,
0.0791162126450747));
#88512=CARTESIAN_POINT('Ctrl Pts',(0.0108646265549997,-0.0327445246967097,
0.0792062730527424));
#88513=CARTESIAN_POINT('Ctrl Pts',(0.0110553270107139,-0.032443687833936,
0.0791029004177201));
#88514=CARTESIAN_POINT('Ctrl Pts',(0.0112376992572152,-0.0321434074405927,
0.0789854571157094));
#88515=CARTESIAN_POINT('',(0.0108963482986283,-0.0326943950436612,0.0791889485203287));
#88516=CARTESIAN_POINT('',(0.0111010304244936,-0.0323666188837389,0.0790707842839038));
#88517=CARTESIAN_POINT('Origin',(0.00272575589853286,-0.0326395579110424,
0.064497131816589));
#88518=CARTESIAN_POINT('Origin',(0.0168183829353055,-0.032193382560293,
0.0885204007911214));
#88519=CARTESIAN_POINT('',(0.0109933788563795,-0.0321934096536377,0.0791343294423074));
#88520=CARTESIAN_POINT('',(0.0110468530104245,-0.0321934096584275,0.0791019756912412));
#88521=CARTESIAN_POINT('',(0.0107861769035146,-0.0325210109756239,0.0792480172033843));
#88522=CARTESIAN_POINT('Origin',(0.00315866026972931,-0.0326393129159093,
0.0642878993250712));
#88523=CARTESIAN_POINT('',(0.0107855480161328,-0.0326943950436593,0.0792468129947429));
#88524=CARTESIAN_POINT('Origin',(0.0159065328648442,-0.0326943765538137,
0.089052598576396));
#88525=CARTESIAN_POINT('',(0.0108409481573906,-0.0326943950436702,0.0792178807575459));
#88526=CARTESIAN_POINT('Ctrl Pts',(0.0106906780628999,-0.0325229783203769,
0.0795731951461946));
#88527=CARTESIAN_POINT('Ctrl Pts',(0.0107654366893927,-0.032413025309245,
0.0795378105427639));
#88528=CARTESIAN_POINT('Ctrl Pts',(0.0108394520012984,-0.032303122220807,
0.0795008848278783));
#88529=CARTESIAN_POINT('Ctrl Pts',(0.0109126308592978,-0.0321934096576658,
0.079462468646228));
#88530=CARTESIAN_POINT('Ctrl Pts',(0.0107222803572808,-0.0325229783203769,
0.0794643721834226));
#88531=CARTESIAN_POINT('Ctrl Pts',(0.0107955388616117,-0.032413025309245,
0.079428551943055));
#88532=CARTESIAN_POINT('Ctrl Pts',(0.0108680452671686,-0.032303122220807,
0.0793912216892592));
#88533=CARTESIAN_POINT('Ctrl Pts',(0.0109397083857194,-0.0321934096576658,
0.079352432516709));
#88534=CARTESIAN_POINT('Ctrl Pts',(0.0107538826516618,-0.0325229783203769,
0.0793555492206506));
#88535=CARTESIAN_POINT('Ctrl Pts',(0.0108256410338306,-0.032413025309245,
0.079319293343346));
#88536=CARTESIAN_POINT('Ctrl Pts',(0.0108966385330388,-0.032303122220807,
0.0792815585506402));
#88537=CARTESIAN_POINT('Ctrl Pts',(0.0109667859121409,-0.0321934096576658,
0.0792423963871901));
#88538=CARTESIAN_POINT('Ctrl Pts',(0.0107854849460427,-0.0325229783203769,
0.0792467262578786));
#88539=CARTESIAN_POINT('Ctrl Pts',(0.0108557432060496,-0.032413025309245,
0.079210034743637));
#88540=CARTESIAN_POINT('Ctrl Pts',(0.010925231798909,-0.032303122220807,
0.0791718954120211));
#88541=CARTESIAN_POINT('Ctrl Pts',(0.0109938634385624,-0.0321934096576658,
0.0791323602576712));
#88542=CARTESIAN_POINT('',(0.0109530048554953,-0.0321934096584275,0.0792983990455642));
#88543=CARTESIAN_POINT('Ctrl Pts',(0.0109012769626633,-0.0322104233328916,
0.079468413555334));
#88544=CARTESIAN_POINT('Ctrl Pts',(0.0108813822077813,-0.0322609421830778,
0.0794303186018514));
#88545=CARTESIAN_POINT('Ctrl Pts',(0.0108618454586623,-0.0323120888239514,
0.0793929091663844));
#88546=CARTESIAN_POINT('Ctrl Pts',(0.0108234707327709,-0.0324156524631813,
0.0793194283214878));
#88547=CARTESIAN_POINT('Ctrl Pts',(0.0108046485300895,-0.0324680267167303,
0.0792833871166656));
#88548=CARTESIAN_POINT('Ctrl Pts',(0.0107861769034984,-0.0325210109755912,
0.0792480172033438));
#88549=CARTESIAN_POINT('Origin',(0.000761802954915682,-0.0262834582510798,
0.0769257246869562));
#88550=CARTESIAN_POINT('Origin',(0.00833608579388862,-0.0342770918174247,
0.0863064460005147));
#88551=CARTESIAN_POINT('Ctrl Pts',(0.0108944136167676,-0.0326943950436604,
0.0791883413161367));
#88552=CARTESIAN_POINT('Ctrl Pts',(0.010963851402962,-0.0325844576448134,
0.079150156822402));
#88553=CARTESIAN_POINT('Ctrl Pts',(0.0110325043854416,-0.0324744968375322,
0.079110533539028));
#88554=CARTESIAN_POINT('Ctrl Pts',(0.0111002853022404,-0.0323646534831894,
0.0790695234469394));
#88555=CARTESIAN_POINT('Ctrl Pts',(0.0110025323414518,-0.0326943950436604,
0.0792222746177034));
#88556=CARTESIAN_POINT('Ctrl Pts',(0.0110724377921395,-0.0325844576448134,
0.0791826000453065));
#88557=CARTESIAN_POINT('Ctrl Pts',(0.0111415276549402,-0.0324744968375322,
0.0791414769057466));
#88558=CARTESIAN_POINT('Ctrl Pts',(0.011209714134637,-0.0323646534831894,
0.0790989591093723));
#88559=CARTESIAN_POINT('Ctrl Pts',(0.011110651066136,-0.0326943950436604,
0.0792562079192702));
#88560=CARTESIAN_POINT('Ctrl Pts',(0.0111810241813171,-0.0325844576448134,
0.0792150432682109));
#88561=CARTESIAN_POINT('Ctrl Pts',(0.0112505509244387,-0.0324744968375322,
0.0791724202724651));
#88562=CARTESIAN_POINT('Ctrl Pts',(0.0113191429670336,-0.0323646534831894,
0.0791283947718053));
#88563=CARTESIAN_POINT('Ctrl Pts',(0.0112187697908201,-0.0326943950436604,
0.0792901412208369));
#88564=CARTESIAN_POINT('Ctrl Pts',(0.0112896105704947,-0.0325844576448134,
0.0792474864911154));
#88565=CARTESIAN_POINT('Ctrl Pts',(0.0113595741939372,-0.0324744968375322,
0.0792033636391837));
#88566=CARTESIAN_POINT('Ctrl Pts',(0.0114285717994302,-0.0323646534831894,
0.0791578304342382));
#88567=CARTESIAN_POINT('Ctrl Pts',(0.011229742161387,-0.0326773559987508,
0.0792835185414584));
#88568=CARTESIAN_POINT('Ctrl Pts',(0.0112075068882425,-0.0326267922587282,
0.0792467681685858));
#88569=CARTESIAN_POINT('Ctrl Pts',(0.0111856657192562,-0.0325756109581965,
0.0792106691695312));
#88570=CARTESIAN_POINT('Ctrl Pts',(0.0111427530014782,-0.0324719985462387,
0.0791397431966829));
#88571=CARTESIAN_POINT('Ctrl Pts',(0.0111216986639644,-0.0324196091621777,
0.0791049446696223));
#88572=CARTESIAN_POINT('Ctrl Pts',(0.0111010304244683,-0.0323666188837756,
0.0790707842838621));
#88573=CARTESIAN_POINT('',(0.0110575590447274,-0.0326943950436702,0.0792395448705903));
#88574=CARTESIAN_POINT('Ctrl Pts',(0.0109620325679172,-0.0332451089994433,
0.0791522454767732));
#88575=CARTESIAN_POINT('Ctrl Pts',(0.0111506953427584,-0.0329451141710254,
0.0790451991125171));
#88576=CARTESIAN_POINT('Ctrl Pts',(0.0113307589768031,-0.0326442513127493,
0.0789242460042235));
#88577=CARTESIAN_POINT('Ctrl Pts',(0.0111767373780794,-0.0332451089994433,
0.0790241757906911));
#88578=CARTESIAN_POINT('Ctrl Pts',(0.0113605699256834,-0.0329451141710254,
0.0789090317020339));
#88579=CARTESIAN_POINT('Ctrl Pts',(0.011535207100951,-0.0326442513127493,
0.0787803677065814));
#88580=CARTESIAN_POINT('',(0.0112072754682251,-0.0331951640388616,0.0790049144402668));
#88581=CARTESIAN_POINT('',(0.0114041341068746,-0.0328677532092642,0.0788741312769494));
#88582=CARTESIAN_POINT('Origin',(0.00158059036077552,-0.0326401908899661,
0.0652805208277939));
#88583=CARTESIAN_POINT('Origin',(0.0177100237123225,-0.0326944279134184,
0.0879554269733298));
#88584=CARTESIAN_POINT('',(0.0113006850036053,-0.0326943950436593,0.0789443105377789));
#88585=CARTESIAN_POINT('',(0.0113520221273582,-0.0326943950436693,0.0789086629610717));
#88586=CARTESIAN_POINT('',(0.0111010304244912,-0.0330220786163546,0.0790707842839053));
#88587=CARTESIAN_POINT('Origin',(0.00195683802494221,-0.0326396682762585,
0.0649810036409999));
#88588=CARTESIAN_POINT('',(0.0111003271651873,-0.0331951640388587,0.0790696219396608));
#88589=CARTESIAN_POINT('Origin',(0.016810972093738,-0.0331952026560192,
0.0885081548797547));
#88590=CARTESIAN_POINT('',(0.0111538013167162,-0.0331951640388701,0.0790372681899738));
#88591=CARTESIAN_POINT('Ctrl Pts',(0.0110261389619798,-0.0330240426238172,
0.0794013165193361));
#88592=CARTESIAN_POINT('Ctrl Pts',(0.0110984809631435,-0.032914277406352,
0.0793613337272157));
#88593=CARTESIAN_POINT('Ctrl Pts',(0.0111700324734335,-0.0328043479726691,
0.0793198354909738));
#88594=CARTESIAN_POINT('Ctrl Pts',(0.0112407003659551,-0.0326943950436593,
0.0792768724485639));
#88595=CARTESIAN_POINT('Ctrl Pts',(0.011050845822357,-0.0330240426238172,
0.0792907239923048));
#88596=CARTESIAN_POINT('Ctrl Pts',(0.0111216643037157,-0.032914277406352,
0.079250400839112));
#88597=CARTESIAN_POINT('Ctrl Pts',(0.0111916844984564,-0.0328043479726691,
0.0792085935675254));
#88598=CARTESIAN_POINT('Ctrl Pts',(0.0112608152305108,-0.0326943950436593,
0.0791653532654215));
#88599=CARTESIAN_POINT('Ctrl Pts',(0.0110755526827341,-0.0330240426238172,
0.0791801314652736));
#88600=CARTESIAN_POINT('Ctrl Pts',(0.0111448476442879,-0.032914277406352,
0.0791394679510084));
#88601=CARTESIAN_POINT('Ctrl Pts',(0.0112133365234794,-0.0328043479726691,
0.079097351644077));
#88602=CARTESIAN_POINT('Ctrl Pts',(0.0112809300950666,-0.0326943950436593,
0.079053834082279));
#88603=CARTESIAN_POINT('Ctrl Pts',(0.0111002595431113,-0.0330240426238172,
0.0790695389382423));
#88604=CARTESIAN_POINT('Ctrl Pts',(0.0111680309848601,-0.032914277406352,
0.0790285350629047));
#88605=CARTESIAN_POINT('Ctrl Pts',(0.0112349885485024,-0.0328043479726691,
0.0789861097206286));
#88606=CARTESIAN_POINT('Ctrl Pts',(0.0113010449596223,-0.0326943950436593,
0.0789423148991366));
#88607=CARTESIAN_POINT('',(0.0112706926847908,-0.0326943950436693,0.079110591493178));
#88608=CARTESIAN_POINT('Ctrl Pts',(0.0112297421613803,-0.0327114338383308,
0.0792835185414474));
#88609=CARTESIAN_POINT('Ctrl Pts',(0.0112075105866604,-0.0327619876830409,
0.0792467742813165));
#88610=CARTESIAN_POINT('Ctrl Pts',(0.0111856712241432,-0.0328131562603187,
0.0792106782679871));
#88611=CARTESIAN_POINT('Ctrl Pts',(0.0111427585458354,-0.0329167375858767,
0.0791397523603752));
#88612=CARTESIAN_POINT('Ctrl Pts',(0.0111217023287364,-0.0329691088920623,
0.0791049507267435));
#88613=CARTESIAN_POINT('Ctrl Pts',(0.0111010304244689,-0.0330220786163187,
0.0790707842838632));
#88614=CARTESIAN_POINT('Ctrl Pts',(0.0112053061629769,-0.0331951640388604,
0.0790044298365731));
#88615=CARTESIAN_POINT('Ctrl Pts',(0.0112721661213289,-0.0330855618127442,
0.0789619880728187));
#88616=CARTESIAN_POINT('Ctrl Pts',(0.0113381970792849,-0.032975722417194,
0.0789181338321737));
#88617=CARTESIAN_POINT('Ctrl Pts',(0.0114033117255521,-0.0328657861694598,
0.0788729191249603));
#88618=CARTESIAN_POINT('Ctrl Pts',(0.0113153423344818,-0.0331951640388604,
0.0790315073734137));
#88619=CARTESIAN_POINT('Ctrl Pts',(0.0113825752311698,-0.0330855618127442,
0.0789875500838217));
#88620=CARTESIAN_POINT('Ctrl Pts',(0.0114489480729757,-0.032975722417194,
0.0789421715168187));
#88621=CARTESIAN_POINT('Ctrl Pts',(0.0115143730150545,-0.0328657861694598,
0.0788954256132438));
#88622=CARTESIAN_POINT('Ctrl Pts',(0.0114253785059866,-0.0331951640388604,
0.0790585849102543));
#88623=CARTESIAN_POINT('Ctrl Pts',(0.0114929843410107,-0.0330855618127442,
0.0790131120948247));
#88624=CARTESIAN_POINT('Ctrl Pts',(0.0115596990666664,-0.032975722417194,
0.0789662092014639));
#88625=CARTESIAN_POINT('Ctrl Pts',(0.0116254343045569,-0.0328657861694598,
0.0789179321015274));
#88626=CARTESIAN_POINT('Ctrl Pts',(0.0115354146774915,-0.0331951640388604,
0.0790856624470949));
#88627=CARTESIAN_POINT('Ctrl Pts',(0.0116033934508515,-0.0330855618127442,
0.0790386741058277));
#88628=CARTESIAN_POINT('Ctrl Pts',(0.0116704500603572,-0.032975722417194,
0.078990246886109));
#88629=CARTESIAN_POINT('Ctrl Pts',(0.0117364955940593,-0.0328657861694598,
0.0789404385898109));
#88630=CARTESIAN_POINT('',(0.0115459495571488,-0.0331781648279232,0.0790783638781455));
#88631=CARTESIAN_POINT('',(0.0115354146774751,-0.0331951640388588,0.0790856624470899));
#88632=CARTESIAN_POINT('Origin',(0.00154597830059997,-0.0326412092733268,
0.065925909637409));
#88633=CARTESIAN_POINT('Ctrl Pts',(0.0115459495551421,-0.0331781648273463,
0.079078363875258));
#88634=CARTESIAN_POINT('Ctrl Pts',(0.0115214336445196,-0.0331276810208762,
0.079043057791277));
#88635=CARTESIAN_POINT('Ctrl Pts',(0.011497360599278,-0.0330765665171629,
0.0790083894907572));
#88636=CARTESIAN_POINT('Ctrl Pts',(0.0114500788061185,-0.032973061271521,
0.0789402975897152));
#88637=CARTESIAN_POINT('Ctrl Pts',(0.0114268896345128,-0.0329207135598926,
0.0789069021816162));
#88638=CARTESIAN_POINT('Ctrl Pts',(0.0114041341068486,-0.0328677532092985,
0.0788741312769121));
#88639=CARTESIAN_POINT('',(0.0113713450728601,-0.0331951640388701,0.0790452884436883));
#88640=CARTESIAN_POINT('Origin',(0.00812378219310841,-0.0315241814719618,
0.07415));
#88641=CARTESIAN_POINT('',(0.011545949556885,-0.0332121607144212,0.0790783638777656));
#88642=CARTESIAN_POINT('',(0.0115564688245398,-0.0331951640388587,0.0790710428254991));
#88643=CARTESIAN_POINT('Origin',(0.00151376860635569,-0.0326413667272291,
0.0659578257290841));
#88644=CARTESIAN_POINT('Origin',(0.00271608011466119,-0.0326412094323411,
0.0651134110508832));
#88645=CARTESIAN_POINT('Origin',(0.0027572391845267,-0.0326413668283485,
0.0650943830840143));
#88646=CARTESIAN_POINT('Ctrl Pts',(0.0112705080844135,-0.0337436976235975,
0.0789641708699412));
#88647=CARTESIAN_POINT('Ctrl Pts',(0.0113138074668253,-0.0336723290703325,
0.0789358687403755));
#88648=CARTESIAN_POINT('Ctrl Pts',(0.0113565907783128,-0.033601104548885,
0.0789067923700146));
#88649=CARTESIAN_POINT('Ctrl Pts',(0.011493189416996,-0.0333736987606857,
0.0788139572791567));
#88650=CARTESIAN_POINT('Ctrl Pts',(0.0116242355391332,-0.0331450831799191,
0.0787134363556759));
#88651=CARTESIAN_POINT('Ctrl Pts',(0.0114767481733374,-0.0337436976235975,
0.0788228732205599));
#88652=CARTESIAN_POINT('Ctrl Pts',(0.0115187767032764,-0.0336723290703325,
0.0787927161363779));
#88653=CARTESIAN_POINT('Ctrl Pts',(0.0115602560030983,-0.033601104548885,
0.078761807970119));
#88654=CARTESIAN_POINT('Ctrl Pts',(0.0116926911908432,-0.0333736987606857,
0.078663124317817));
#88655=CARTESIAN_POINT('Ctrl Pts',(0.0118192450989018,-0.0331450831799191,
0.0785570033936798));
#88656=CARTESIAN_POINT('Ctrl Pts',(0.0114788105742266,-0.0337436976235975,
0.0788214602440662));
#88657=CARTESIAN_POINT('Ctrl Pts',(0.0115208263956409,-0.0336723290703325,
0.0787912846103379));
#88658=CARTESIAN_POINT('Ctrl Pts',(0.0115622926553462,-0.033601104548885,
0.07876035812612));
#88659=CARTESIAN_POINT('Ctrl Pts',(0.0116946862085817,-0.0333736987606857,
0.0786616159882036));
#88660=CARTESIAN_POINT('Ctrl Pts',(0.0118211951944995,-0.0331450831799191,
0.0785554390640598));
#88661=CARTESIAN_POINT('',(0.0115060334985897,-0.0336938721132548,0.0788017202309007));
#88662=CARTESIAN_POINT('',(0.0116942917446253,-0.0333679869945434,0.078658834277581));
#88663=CARTESIAN_POINT('Ctrl Pts',(0.0115060334985922,-0.033693872113265,
0.0788017202308998));
#88664=CARTESIAN_POINT('Ctrl Pts',(0.011524191344814,-0.0336629187933934,
0.0787885177174118));
#88665=CARTESIAN_POINT('Ctrl Pts',(0.0115422660776993,-0.0336319952301041,
0.078775213104912));
#88666=CARTESIAN_POINT('Ctrl Pts',(0.0115602560031003,-0.0336011045488951,
0.0787618079701178));
#88667=CARTESIAN_POINT('Ctrl Pts',(0.0116053988817375,-0.0335235892595455,
0.0787281698999402));
#88668=CARTESIAN_POINT('Ctrl Pts',(0.0116500878701258,-0.033445866866037,
0.078693838969908));
#88669=CARTESIAN_POINT('Ctrl Pts',(0.011694291744808,-0.0333679869945386,
0.0786588342778223));
#88670=CARTESIAN_POINT('Ctrl Pts',(0.0116943270343373,-0.0333679692459667,
0.0786588072090433));
#88671=CARTESIAN_POINT('Ctrl Pts',(0.0116940410271472,-0.0333391895375561,
0.0786584555875025));
#88672=CARTESIAN_POINT('Ctrl Pts',(0.011693824131719,-0.0333104081062525,
0.0786581940790117));
#88673=CARTESIAN_POINT('Ctrl Pts',(0.0116935327705736,-0.033253269827004,
0.0786578514635641));
#88674=CARTESIAN_POINT('Ctrl Pts',(0.0116934562254131,-0.0332249171466895,
0.0786577677241525));
#88675=CARTESIAN_POINT('Ctrl Pts',(0.0116934485380219,-0.0331960985356852,
0.0786577691298677));
#88676=CARTESIAN_POINT('Ctrl Pts',(0.011693448431858,-0.0331956312568221,
0.0786577691759818));
#88677=CARTESIAN_POINT('Ctrl Pts',(0.0116934483446455,-0.0331951640388597,
0.0786577692450447));
#88678=CARTESIAN_POINT('',(0.0115954533610552,-0.0331951640388587,0.0787353706831235));
#88679=CARTESIAN_POINT('',(0.0116444508528592,-0.0331951640388687,0.078696569964095));
#88680=CARTESIAN_POINT('',(0.0114041341065212,-0.0335216366567644,0.0788741312767267));
#88681=CARTESIAN_POINT('Origin',(0.000935548044213429,-0.0326434571526759,
0.0659211636290065));
#88682=CARTESIAN_POINT('',(0.0114033592510911,-0.0336938721132327,0.0788730153843445));
#88683=CARTESIAN_POINT('Origin',(0.0176320276870547,-0.0336938867896355,
0.0878431056559906));
#88684=CARTESIAN_POINT('',(0.0114546963748504,-0.0336938721132538,0.0788373678076325));
#88685=CARTESIAN_POINT('Ctrl Pts',(0.0113501455266319,-0.0335235895815172,
0.0792087132395667));
#88686=CARTESIAN_POINT('Ctrl Pts',(0.0114197886740644,-0.0334144449262748,
0.0791642959961559));
#88687=CARTESIAN_POINT('Ctrl Pts',(0.0114885942062146,-0.0333049234473147,
0.0791183889477));
#88688=CARTESIAN_POINT('Ctrl Pts',(0.011556468824539,-0.0331951640388587,
0.0790710428255066));
#88689=CARTESIAN_POINT('Ctrl Pts',(0.0113678594786838,-0.0335235895815172,
0.0790967874231122));
#88690=CARTESIAN_POINT('Ctrl Pts',(0.0114359617468911,-0.0334144449262748,
0.0790521263122758));
#88691=CARTESIAN_POINT('Ctrl Pts',(0.0115032195914152,-0.0333049234473147,
0.0790060069496254));
#88692=CARTESIAN_POINT('Ctrl Pts',(0.0115695416681373,-0.0331951640388587,
0.0789584805172211));
#88693=CARTESIAN_POINT('Ctrl Pts',(0.0113855734307357,-0.0335235895815172,
0.0789848616066576));
#88694=CARTESIAN_POINT('Ctrl Pts',(0.0114521348197178,-0.0334144449262748,
0.0789399566283957));
#88695=CARTESIAN_POINT('Ctrl Pts',(0.0115178449766157,-0.0333049234473147,
0.0788936249515508));
#88696=CARTESIAN_POINT('Ctrl Pts',(0.0115826145117357,-0.0331951640388587,
0.0788459182089356));
#88697=CARTESIAN_POINT('Ctrl Pts',(0.0114032873827875,-0.0335235895815172,
0.078872935790203));
#88698=CARTESIAN_POINT('Ctrl Pts',(0.0114683078925445,-0.0334144449262748,
0.0788277869445156));
#88699=CARTESIAN_POINT('Ctrl Pts',(0.0115324703618162,-0.0333049234473147,
0.0787812429534761));
#88700=CARTESIAN_POINT('Ctrl Pts',(0.0115956873553341,-0.0331951640388587,
0.07873335590065));
#88701=CARTESIAN_POINT('',(0.0115759610928075,-0.0331951640388687,0.0789032067543213));
#88702=CARTESIAN_POINT('Ctrl Pts',(0.0115459495550925,-0.0332121607145958,
0.0790783638751866));
#88703=CARTESIAN_POINT('Ctrl Pts',(0.011521474958517,-0.0332625444109105,
0.0790431172887799));
#88704=CARTESIAN_POINT('Ctrl Pts',(0.0114974220976462,-0.0333135300745512,
0.0790084780563661));
#88705=CARTESIAN_POINT('Ctrl Pts',(0.0114501407543524,-0.0334167203140533,
0.0789403868031891));
#88706=CARTESIAN_POINT('Ctrl Pts',(0.0114269305844705,-0.0334688847587202,
0.0789069611548547));
#88707=CARTESIAN_POINT('Ctrl Pts',(0.0114041341062497,-0.0335216366562257,
0.0788741312760496));
#88708=CARTESIAN_POINT('Ctrl Pts',(0.0115050495193523,-0.0336938721132389,
0.0788015427492615));
#88709=CARTESIAN_POINT('Ctrl Pts',(0.0115322765426092,-0.0336474569764957,
0.0787817510695775));
#88710=CARTESIAN_POINT('Ctrl Pts',(0.0115592700136535,-0.033601104548885,
0.0787616420193482));
#88711=CARTESIAN_POINT('Ctrl Pts',(0.0116276112761496,-0.0334837508592655,
0.0787107305275279));
#88712=CARTESIAN_POINT('Ctrl Pts',(0.0116944139151403,-0.0333660264659097,
0.0786578162989802));
#88713=CARTESIAN_POINT('Ctrl Pts',(0.0115060334985732,-0.0336938721132389,
0.0788017202309126));
#88714=CARTESIAN_POINT('Ctrl Pts',(0.0115332615606891,-0.0336474569764957,
0.0787819227916717));
#88715=CARTESIAN_POINT('Ctrl Pts',(0.0115602560030983,-0.033601104548885,
0.078761807970119));
#88716=CARTESIAN_POINT('Ctrl Pts',(0.0116285997248671,-0.0334837508592655,
0.0787108818666348));
#88717=CARTESIAN_POINT('Ctrl Pts',(0.0116954043890766,-0.0333660264659097,
0.078657952959966));
#88718=CARTESIAN_POINT('Ctrl Pts',(0.0118405907808433,-0.0336938721132389,
0.0788620647763927));
#88719=CARTESIAN_POINT('Ctrl Pts',(0.0118681720596084,-0.0336474569764957,
0.0788403090623608));
#88720=CARTESIAN_POINT('Ctrl Pts',(0.0118954967703852,-0.033601104548885,
0.0788182319653524));
#88721=CARTESIAN_POINT('Ctrl Pts',(0.0119646766557272,-0.0334837508592655,
0.07876233783157));
#88722=CARTESIAN_POINT('Ctrl Pts',(0.0120321699032904,-0.0333660264659097,
0.0787044182989356));
#88723=CARTESIAN_POINT('',(0.0118486512207968,-0.0336769361243753,0.0788537592122224));
#88724=CARTESIAN_POINT('',(0.0118385954093542,-0.033693872113232,0.0788617048685593));
#88725=CARTESIAN_POINT('Ctrl Pts',(0.0118486512207971,-0.033676936124375,
0.0788537592122222));
#88726=CARTESIAN_POINT('Ctrl Pts',(0.0118469765411615,-0.0336797586670006,
0.0788550853775348));
#88727=CARTESIAN_POINT('Ctrl Pts',(0.0118453012166317,-0.0336825812712807,
0.0788564105983367));
#88728=CARTESIAN_POINT('Ctrl Pts',(0.0118419492873817,-0.0336882265874452,
0.0788590591439903));
#88729=CARTESIAN_POINT('Ctrl Pts',(0.0118402726826985,-0.0336910492993153,
0.0788603824688577));
#88730=CARTESIAN_POINT('Ctrl Pts',(0.011838595409368,-0.0336938721132378,
0.0788617048685643));
#88731=CARTESIAN_POINT('Ctrl Pts',(0.0118486512207968,-0.0336769361243753,
0.0788537592122224));
#88732=CARTESIAN_POINT('Ctrl Pts',(0.0118226306795899,-0.0336279007516194,
0.0788209005104803));
#88733=CARTESIAN_POINT('Ctrl Pts',(0.0117962396464481,-0.0335767878632062,
0.0787875739520604));
#88734=CARTESIAN_POINT('Ctrl Pts',(0.0117445206321308,-0.0334733198857316,
0.0787222632557021));
#88735=CARTESIAN_POINT('Ctrl Pts',(0.0117191618603002,-0.0334209645014074,
0.0786902402353689));
#88736=CARTESIAN_POINT('Ctrl Pts',(0.0116942917389024,-0.0333679869844683,
0.0786588342820951));
#88737=CARTESIAN_POINT('',(0.011672314453982,-0.0336938721132534,0.07883171254974));
#88738=CARTESIAN_POINT('Origin',(0.00812378219310841,-0.0315241814719618,
0.07415));
#88739=CARTESIAN_POINT('',(0.0118486512199988,-0.0337108120655385,0.0788537592112131));
#88740=CARTESIAN_POINT('',(0.0118586900372345,-0.0336938721132327,0.0788457920946194));
#88741=CARTESIAN_POINT('Origin',(0.00256758261447966,-0.0345562526817935,
0.0653334041418887));
#88742=CARTESIAN_POINT('Ctrl Pts',(0.0118586900372366,-0.0336938721132377,
0.0788457920946326));
#88743=CARTESIAN_POINT('Ctrl Pts',(0.011857018429022,-0.0336910493001332,
0.0788471216472421));
#88744=CARTESIAN_POINT('Ctrl Pts',(0.0118553460727901,-0.0336882265878542,
0.0788484503375465));
#88745=CARTESIAN_POINT('Ctrl Pts',(0.0118519998085138,-0.0336825812713067,
0.0788511060373876));
#88746=CARTESIAN_POINT('Ctrl Pts',(0.0118503259004399,-0.0336797586670136,
0.078852433046904));
#88747=CARTESIAN_POINT('Ctrl Pts',(0.0118486512207966,-0.033676936124375,
0.0788537592122226));
#88748=CARTESIAN_POINT('Origin',(0.000815265691572346,-0.0345562523865742,
0.0667210503996088));
#88749=CARTESIAN_POINT('Ctrl Pts',(0.0115665416655903,-0.0342436276873911,
0.0787571175603229));
#88750=CARTESIAN_POINT('Ctrl Pts',(0.0117403019688528,-0.033943005420181,
0.0786272717462829));
#88751=CARTESIAN_POINT('Ctrl Pts',(0.0119037881185698,-0.0336441434784052,
0.0784847064725858));
#88752=CARTESIAN_POINT('Ctrl Pts',(0.0117635040163719,-0.0342436276873911,
0.0786031505756328));
#88753=CARTESIAN_POINT('Ctrl Pts',(0.0119314573590779,-0.033943005420181,
0.0784658762040717));
#88754=CARTESIAN_POINT('Ctrl Pts',(0.0120885934958144,-0.0336441434784052,
0.0783163408806692));
#88755=CARTESIAN_POINT('Ctrl Pts',(0.0117654736398797,-0.0342436276873911,
0.0786016109057859));
#88756=CARTESIAN_POINT('Ctrl Pts',(0.0119333689129802,-0.033943005420181,
0.0784642622486496));
#88757=CARTESIAN_POINT('Ctrl Pts',(0.0120904415495869,-0.0336441434784052,
0.07831465722475));
#88758=CARTESIAN_POINT('',(0.0117914433282312,-0.0341934961088741,0.0785801678069697));
#88759=CARTESIAN_POINT('',(0.0119703582026119,-0.0338664212864873,0.0784257429773084));
#88760=CARTESIAN_POINT('Origin',(0.00151709971471466,-0.0345610720404953,
0.0653706633845988));
#88761=CARTESIAN_POINT('Origin',(0.0193047456575757,-0.0336938005072917,
0.0865783796737805));
#88762=CARTESIAN_POINT('',(0.0118765206184609,-0.0336938721132327,0.0785083344652383));
#88763=CARTESIAN_POINT('',(0.0119229851076007,-0.0336938721132427,0.0784665337326003));
#88764=CARTESIAN_POINT('',(0.0116942917388981,-0.0340203938281605,0.0786588342820984));
#88765=CARTESIAN_POINT('Origin',(0.00193792105499299,-0.0345589643245715,
0.0651373264308059));
#88766=CARTESIAN_POINT('',(0.0116934483446432,-0.034193496108874,0.0786577692450465));
#88767=CARTESIAN_POINT('Origin',(0.0185344473858077,-0.0341934220717648,
0.0872965741613755));
#88768=CARTESIAN_POINT('',(0.0117424458364472,-0.0341934961088841,0.0786189685260182));
#88769=CARTESIAN_POINT('Ctrl Pts',(0.0116614160580294,-0.0340223579322396,
0.0789961476079296));
#88770=CARTESIAN_POINT('Ctrl Pts',(0.0117282570728263,-0.0339125849573574,
0.0789473544103959));
#88771=CARTESIAN_POINT('Ctrl Pts',(0.0117940412134068,-0.0338030433565231,
0.0788972120455879));
#88772=CARTESIAN_POINT('Ctrl Pts',(0.011858690037234,-0.0336938721132326,
0.0788457920946276));
#88773=CARTESIAN_POINT('Ctrl Pts',(0.011672067229974,-0.0340223579322396,
0.0788833303558494));
#88774=CARTESIAN_POINT('Ctrl Pts',(0.011737352200625,-0.0339125849573574,
0.0788343902508751));
#88775=CARTESIAN_POINT('Ctrl Pts',(0.0118015783498311,-0.0338030433565231,
0.0787841332883549));
#88776=CARTESIAN_POINT('Ctrl Pts',(0.011864669240455,-0.0336938721132326,
0.078732631019343));
#88777=CARTESIAN_POINT('Ctrl Pts',(0.0116827184019186,-0.0340223579322396,
0.0787705131037693));
#88778=CARTESIAN_POINT('Ctrl Pts',(0.0117464473284237,-0.0339125849573574,
0.0787214260913545));
#88779=CARTESIAN_POINT('Ctrl Pts',(0.0118091154862554,-0.0338030433565231,
0.0786710545311219));
#88780=CARTESIAN_POINT('Ctrl Pts',(0.0118706484436759,-0.0336938721132326,
0.0786194699440584));
#88781=CARTESIAN_POINT('Ctrl Pts',(0.0116933695738632,-0.0340223579322396,
0.0786576958516891));
#88782=CARTESIAN_POINT('Ctrl Pts',(0.0117555424562223,-0.0339125849573574,
0.0786084619318338));
#88783=CARTESIAN_POINT('Ctrl Pts',(0.0118166526226797,-0.0338030433565231,
0.0785579757738889));
#88784=CARTESIAN_POINT('Ctrl Pts',(0.0118766276468969,-0.0336938721132326,
0.0785063088687738));
#88785=CARTESIAN_POINT('',(0.0118676053278577,-0.0336938721132427,0.0786770632799389));
#88786=CARTESIAN_POINT('Ctrl Pts',(0.0118486512177558,-0.0337108120662667,
0.0788537592083825));
#88787=CARTESIAN_POINT('Ctrl Pts',(0.011821956784873,-0.0337611408993659,
0.0788200495172082));
#88788=CARTESIAN_POINT('Ctrl Pts',(0.0117957494661654,-0.0338121088780008,
0.0787869549531089));
#88789=CARTESIAN_POINT('Ctrl Pts',(0.0117442851825266,-0.0339153382773234,
0.0787219659302822));
#88790=CARTESIAN_POINT('Ctrl Pts',(0.0117190462010022,-0.0339675637691194,
0.0786900941809752));
#88791=CARTESIAN_POINT('Ctrl Pts',(0.0116942879989058,-0.0340204018098272,
0.0786588295592332));
#88792=CARTESIAN_POINT('Ctrl Pts',(0.011789428722031,-0.0341934961088741,
0.0785799338331629));
#88793=CARTESIAN_POINT('Ctrl Pts',(0.0118810141140772,-0.0340287516182428,
0.0785041494790173));
#88794=CARTESIAN_POINT('Ctrl Pts',(0.0119693890233064,-0.0338644633275951,
0.0784246445874175));
#88795=CARTESIAN_POINT('Ctrl Pts',(0.0117914433282311,-0.0341934961088741,
0.0785801678069697));
#88796=CARTESIAN_POINT('Ctrl Pts',(0.0118830335575015,-0.0340287516182428,
0.0785043418024279));
#88797=CARTESIAN_POINT('Ctrl Pts',(0.011971411578379,-0.0338644633275951,
0.0784247950960955));
#88798=CARTESIAN_POINT('Ctrl Pts',(0.0121271154706234,-0.0341934961088741,
0.078619152343487));
#88799=CARTESIAN_POINT('Ctrl Pts',(0.0122195116744737,-0.0340287516182428,
0.0785363865818478));
#88800=CARTESIAN_POINT('Ctrl Pts',(0.0123084081558157,-0.0338644633275951,
0.0784498727367667));
#88801=CARTESIAN_POINT('',(0.0121366525261739,-0.0341764758832446,0.0786105909564536));
#88802=CARTESIAN_POINT('',(0.0121271154706064,-0.034193496108874,0.078619152343485));
#88803=CARTESIAN_POINT('Origin',(0.00144334588065161,-0.0345621026416435,
0.0659585348654658));
#88804=CARTESIAN_POINT('Ctrl Pts',(0.0121366525243996,-0.0341764758837558,
0.0786105909568769));
#88805=CARTESIAN_POINT('Ctrl Pts',(0.012107944187226,-0.0341260050040581,
0.0785786796175815));
#88806=CARTESIAN_POINT('Ctrl Pts',(0.0120797348402744,-0.0340749269148394,
0.0785473229981994));
#88807=CARTESIAN_POINT('Ctrl Pts',(0.0120242924006475,-0.0339715436306688,
0.0784856947748888));
#88808=CARTESIAN_POINT('Ctrl Pts',(0.0119970803460565,-0.0339192778238052,
0.0784554465473427));
#88809=CARTESIAN_POINT('Ctrl Pts',(0.0119703582020076,-0.0338664212855959,
0.0784257429794382));
#88810=CARTESIAN_POINT('',(0.0119592793994288,-0.0341934961088841,0.0785996600752375));
#88811=CARTESIAN_POINT('Origin',(0.00812378219310841,-0.0315241814719618,
0.07415));
#88812=CARTESIAN_POINT('',(0.0121366525263052,-0.0342105180190354,0.0786105909553415));
#88813=CARTESIAN_POINT('',(0.0121461712749854,-0.0341934961088739,0.0786020092176454));
#88814=CARTESIAN_POINT('Origin',(0.00140637764150144,-0.0345621722724057,
0.0659847582638457));
#88815=CARTESIAN_POINT('Origin',(0.000681924122869572,-0.0345621028456128,
0.0666435303060728));
#88816=CARTESIAN_POINT('Origin',(0.000711897734075975,-0.0345621725703317,
0.0666095320673899));
#88817=CARTESIAN_POINT('Ctrl Pts',(0.011875405463354,-0.0346945769586966,
0.0785093376894498));
#88818=CARTESIAN_POINT('Ctrl Pts',(0.0119667135366431,-0.0345275153362944,
0.0784307584379865));
#88819=CARTESIAN_POINT('Ctrl Pts',(0.0120555739817455,-0.0343603235965185,
0.0783492873070423));
#88820=CARTESIAN_POINT('Ctrl Pts',(0.0121417275701354,-0.034193496108874,
0.0782651691580946));
#88821=CARTESIAN_POINT('Ctrl Pts',(0.0119377298340476,-0.0346945769586966,
0.0784532689710457));
#88822=CARTESIAN_POINT('Ctrl Pts',(0.0120278635255811,-0.0345275153362944,
0.0783733843106849));
#88823=CARTESIAN_POINT('Ctrl Pts',(0.0121155082312643,-0.0343603235965185,
0.0782906443664228));
#88824=CARTESIAN_POINT('Ctrl Pts',(0.0122004083739621,-0.034193496108874,
0.0782052976988833));
#88825=CARTESIAN_POINT('Ctrl Pts',(0.0120000542047416,-0.0346945769586966,
0.0783972002526438));
#88826=CARTESIAN_POINT('Ctrl Pts',(0.0120890135145195,-0.0345275153362944,
0.0783160101833845));
#88827=CARTESIAN_POINT('Ctrl Pts',(0.0121754424807835,-0.0343603235965185,
0.078232001425804));
#88828=CARTESIAN_POINT('Ctrl Pts',(0.0122590891777892,-0.034193496108874,
0.0781454262396725));
#88829=CARTESIAN_POINT('Ctrl Pts',(0.0120623785754349,-0.0346945769586966,
0.0783411315342375));
#88830=CARTESIAN_POINT('Ctrl Pts',(0.012150163503457,-0.0345275153362944,
0.0782586360560816));
#88831=CARTESIAN_POINT('Ctrl Pts',(0.0122353767303018,-0.0343603235965185,
0.0781733584851839));
#88832=CARTESIAN_POINT('Ctrl Pts',(0.0123177699816155,-0.034193496108874,
0.0780855547804608));
#88833=CARTESIAN_POINT('',(0.0120623785749843,-0.0346945769586966,0.0783411315346425));
#88834=CARTESIAN_POINT('',(0.012231243985032,-0.0343667727831542,0.078175777270098));
#88835=CARTESIAN_POINT('Origin',(0.000415580299837392,-0.0345626457064528,
0.0662147414213684));
#88836=CARTESIAN_POINT('Origin',(0.0201244088264278,-0.0341934771029137,
0.0859119651688161));
#88837=CARTESIAN_POINT('',(0.0121427775317648,-0.034193496108874,0.0782640978923525));
#88838=CARTESIAN_POINT('',(0.0121865256441295,-0.034193496108884,0.0782194621144998));
#88839=CARTESIAN_POINT('',(0.011970358200964,-0.0345211942962608,0.0784257429782233));
#88840=CARTESIAN_POINT('Origin',(0.000775254284101102,-0.0345625596120131,
0.0658956404734609));
#88841=CARTESIAN_POINT('',(0.0119694495967205,-0.0346945769586885,0.0784247329999423));
#88842=CARTESIAN_POINT('Origin',(0.0193688924135947,-0.0346945685853941,
0.0866497412808417));
#88843=CARTESIAN_POINT('',(0.0120159140858624,-0.0346945769587026,0.0783829322673024));
#88844=CARTESIAN_POINT('Ctrl Pts',(0.0119587282116965,-0.0345231616327842,
0.0787644543593578));
#88845=CARTESIAN_POINT('Ctrl Pts',(0.0120223319684082,-0.0344132092796988,
0.0787115950276637));
#88846=CARTESIAN_POINT('Ctrl Pts',(0.0120848390898771,-0.0343032738558979,
0.0786574228297305));
#88847=CARTESIAN_POINT('Ctrl Pts',(0.0121461712749856,-0.0341934961088739,
0.0786020092176541));
#88848=CARTESIAN_POINT('Ctrl Pts',(0.01196227448792,-0.0345231616327842,
0.0786511911258532));
#88849=CARTESIAN_POINT('Ctrl Pts',(0.0120243170704197,-0.0344132092796988,
0.0785982829137341));
#88850=CARTESIAN_POINT('Ctrl Pts',(0.0120852620871731,-0.0343032738558979,
0.0785440941295551));
#88851=CARTESIAN_POINT('Ctrl Pts',(0.0121450332388432,-0.0341934961088739,
0.0784886961953984));
#88852=CARTESIAN_POINT('Ctrl Pts',(0.0119658207641435,-0.0345231616327842,
0.0785379278923486));
#88853=CARTESIAN_POINT('Ctrl Pts',(0.0120263021724312,-0.0344132092796988,
0.0784849707998045));
#88854=CARTESIAN_POINT('Ctrl Pts',(0.012085685084469,-0.0343032738558979,
0.0784307654293796));
#88855=CARTESIAN_POINT('Ctrl Pts',(0.0121438952027009,-0.0341934961088739,
0.0783753831731428));
#88856=CARTESIAN_POINT('Ctrl Pts',(0.0119693670403671,-0.0345231616327842,
0.0784246646588441));
#88857=CARTESIAN_POINT('Ctrl Pts',(0.0120282872744428,-0.0344132092796988,
0.078371658685875));
#88858=CARTESIAN_POINT('Ctrl Pts',(0.0120861080817649,-0.0343032738558979,
0.0783174367292042));
#88859=CARTESIAN_POINT('Ctrl Pts',(0.0121427571665586,-0.0341934961088739,
0.0782620701508871));
#88860=CARTESIAN_POINT('',(0.0121444744033851,-0.0341934961088839,0.078433053555009));
#88861=CARTESIAN_POINT('Ctrl Pts',(0.0121366525239888,-0.0342105180195365,
0.0786105909527672));
#88862=CARTESIAN_POINT('Ctrl Pts',(0.0121079119233284,-0.0342610556240453,
0.0785786437297793));
#88863=CARTESIAN_POINT('Ctrl Pts',(0.0120796870578849,-0.0343122189868431,
0.0785472697831875));
#88864=CARTESIAN_POINT('Ctrl Pts',(0.0120242440558992,-0.0344158119695077,
0.0784856409408228));
#88865=CARTESIAN_POINT('Ctrl Pts',(0.0119970485960829,-0.0344681990449947,
0.0784554112518445));
#88866=CARTESIAN_POINT('Ctrl Pts',(0.0119703582009428,-0.0345211942962355,
0.0784257429781971));
#88867=CARTESIAN_POINT('Ctrl Pts',(0.0120603537487011,-0.0346945769586932,
0.0783410245469078));
#88868=CARTESIAN_POINT('Ctrl Pts',(0.0121470002157346,-0.034529677707698,
0.0782596387154246));
#88869=CARTESIAN_POINT('Ctrl Pts',(0.0122302088932423,-0.0343648066251421,
0.0781747412490137));
#88870=CARTESIAN_POINT('Ctrl Pts',(0.0120623785749777,-0.0346945769586932,
0.0783411315346486));
#88871=CARTESIAN_POINT('Ctrl Pts',(0.012149027253907,-0.034529677707698,
0.0782597038413149));
#88872=CARTESIAN_POINT('Ctrl Pts',(0.0122322364112318,-0.0343648066251421,
0.0781747644574042));
#88873=CARTESIAN_POINT('Ctrl Pts',(0.012399836204375,-0.0346945769586932,
0.0783589621158761));
#88874=CARTESIAN_POINT('Ctrl Pts',(0.0124868535179547,-0.034529677707698,
0.0782705577248319));
#88875=CARTESIAN_POINT('Ctrl Pts',(0.0125701426416088,-0.0343648066251421,
0.0781786323687029));
#88876=CARTESIAN_POINT('',(0.0124088168670256,-0.034677539666503,0.0783498187861985));
#88877=CARTESIAN_POINT('',(0.0123998362043608,-0.0346945769586887,0.0783589621158728));
#88878=CARTESIAN_POINT('Origin',(0.000446020694324284,-0.0345626618039033,
0.066838762831078));
#88879=CARTESIAN_POINT('Ctrl Pts',(0.0124088168652486,-0.0346775396670096,
0.0783498187866297));
#88880=CARTESIAN_POINT('Ctrl Pts',(0.0123781373046023,-0.0346269749928197,
0.0783197493641814));
#88881=CARTESIAN_POINT('Ctrl Pts',(0.012348002963064,-0.0345757902890816,
0.0782902143681198));
#88882=CARTESIAN_POINT('Ctrl Pts',(0.0122888000214345,-0.0344721681087906,
0.0782321887818647));
#88883=CARTESIAN_POINT('Ctrl Pts',(0.0122597546356236,-0.0344197714289445,
0.0782037209364014));
#88884=CARTESIAN_POINT('Ctrl Pts',(0.0122312439849364,-0.0343667727830771,
0.0781757772703416));
#88885=CARTESIAN_POINT('',(0.0122311073896826,-0.0346945769587026,0.0783500468252676));
#88886=CARTESIAN_POINT('Origin',(0.00812378219310841,-0.0315241814719618,
0.07415));
#88887=CARTESIAN_POINT('',(0.012408816866699,-0.0347116136489781,0.0783498187848444));
#88888=CARTESIAN_POINT('',(0.012417777980685,-0.0346945769586885,0.0783406562942192));
#88889=CARTESIAN_POINT('Origin',(0.000415668195806348,-0.0345626702675865,
0.0668724051349416));
#88890=CARTESIAN_POINT('Origin',(0.000659814792040836,-0.0345626619863005,
0.0666206300659209));
#88891=CARTESIAN_POINT('Origin',(0.000692841233989324,-0.0345626706114569,
0.0665896088296775));
#88892=CARTESIAN_POINT('Ctrl Pts',(0.012115097209926,-0.0352450361874068,
0.0782910345400819));
#88893=CARTESIAN_POINT('Ctrl Pts',(0.0122712788904274,-0.0349452760959493,
0.0781404996240595));
#88894=CARTESIAN_POINT('Ctrl Pts',(0.0124156779694018,-0.034644428984174,
0.0779786281186687));
#88895=CARTESIAN_POINT('Ctrl Pts',(0.0121168759173089,-0.0352450361874068,
0.0782892423835469));
#88896=CARTESIAN_POINT('Ctrl Pts',(0.0122729900055175,-0.0349452760959493,
0.0781386403824747));
#88897=CARTESIAN_POINT('Ctrl Pts',(0.0124173166311011,-0.034644428984174,
0.0779767070739437));
#88898=CARTESIAN_POINT('Ctrl Pts',(0.0122929855591785,-0.0352450361874068,
0.078111801142454));
#88899=CARTESIAN_POINT('Ctrl Pts',(0.0124424073411636,-0.0349452760959493,
0.0779545570572472));
#88900=CARTESIAN_POINT('Ctrl Pts',(0.0125795603637071,-0.034644428984174,
0.0777865046259309));
#88901=CARTESIAN_POINT('Ctrl Pts',(0.0122947466555972,-0.0352450361874068,
0.0781100267300432));
#88902=CARTESIAN_POINT('Ctrl Pts',(0.01244410151452,-0.0349452760959493,
0.0779527162239949));
#88903=CARTESIAN_POINT('Ctrl Pts',(0.0125811828010331,-0.034644428984174,
0.0777846026014507));
#88904=CARTESIAN_POINT('',(0.0123177495694777,-0.0351951634053343,0.0780855800015301));
#88905=CARTESIAN_POINT('',(0.012475919493575,-0.0348678972925388,0.0779099236585187));
#88906=CARTESIAN_POINT('Origin',(-0.000474189373535641,-0.0345636767883037,
0.0672795263998118));
#88907=CARTESIAN_POINT('Origin',(0.0208374958163375,-0.0346946199340759,
0.0851337059576703));
#88908=CARTESIAN_POINT('',(0.0123931732943985,-0.0346945769330289,0.0780036248678973));
#88909=CARTESIAN_POINT('',(0.0124340323821223,-0.0346945769458128,0.0779563301954911));
#88910=CARTESIAN_POINT('',(0.0122312439848407,-0.0350221583435276,0.0781757772702249));
#88911=CARTESIAN_POINT('Origin',(-0.000192449574958003,-0.0345628458716686,
0.0668899547387003));
#88912=CARTESIAN_POINT('',(0.0122303585188129,-0.0351951360298763,0.0781749136483986));
#88913=CARTESIAN_POINT('Origin',(0.0200998093611332,-0.0351951838366795,
0.0858878629742999));
#88914=CARTESIAN_POINT('',(0.0123177699812669,-0.0351951371328746,0.0780855547809824));
#88915=CARTESIAN_POINT('Ctrl Pts',(0.0122409055071548,-0.0350241211494343,
0.0785145498756483));
#88916=CARTESIAN_POINT('Ctrl Pts',(0.0123010253921567,-0.0349144232818962,
0.0784578381900836));
#88917=CARTESIAN_POINT('Ctrl Pts',(0.0123600089907431,-0.0348045283579412,
0.0783998498388591));
#88918=CARTESIAN_POINT('Ctrl Pts',(0.0124177779884474,-0.0346945769439157,
0.0783406562862751));
#88919=CARTESIAN_POINT('Ctrl Pts',(0.0122373329094135,-0.0350241211494343,
0.0784012874443269));
#88920=CARTESIAN_POINT('Ctrl Pts',(0.0122958926508634,-0.0349144232818962,
0.0783446249698312));
#88921=CARTESIAN_POINT('Ctrl Pts',(0.0123533161893045,-0.0348045283579412,
0.0782867181084131));
#88922=CARTESIAN_POINT('Ctrl Pts',(0.0124095272123934,-0.0346945769439157,
0.0782276382943536));
#88923=CARTESIAN_POINT('Ctrl Pts',(0.0122337603116722,-0.0350241211494343,
0.0782880250130055));
#88924=CARTESIAN_POINT('Ctrl Pts',(0.01229075990957,-0.0349144232818962,
0.0782314117495789));
#88925=CARTESIAN_POINT('Ctrl Pts',(0.0123466233878659,-0.0348045283579412,
0.078173586377967));
#88926=CARTESIAN_POINT('Ctrl Pts',(0.0124012764363395,-0.0346945769439157,
0.0781146203024321));
#88927=CARTESIAN_POINT('Ctrl Pts',(0.0122301877139309,-0.0350241211494343,
0.078174762581684));
#88928=CARTESIAN_POINT('Ctrl Pts',(0.0122856271682766,-0.0349144232818962,
0.0781181985293265));
#88929=CARTESIAN_POINT('Ctrl Pts',(0.0123399305864274,-0.0348045283579412,
0.0780604546475209));
#88930=CARTESIAN_POINT('Ctrl Pts',(0.0123930256602855,-0.0346945769439157,
0.0780016023105106));
#88931=CARTESIAN_POINT('',(0.0124054756374125,-0.0346945769458128,0.0781721405813361));
#88932=CARTESIAN_POINT('Ctrl Pts',(0.0124088168643448,-0.0347116136492768,
0.0783498187825369));
#88933=CARTESIAN_POINT('Ctrl Pts',(0.0123781494962928,-0.034762154653141,
0.0783197612921692));
#88934=CARTESIAN_POINT('Ctrl Pts',(0.0123480213434412,-0.0348133084095223,
0.0782902322937043));
#88935=CARTESIAN_POINT('Ctrl Pts',(0.0122888183239445,-0.0349168561544567,
0.0782322066364244));
#88936=CARTESIAN_POINT('Ctrl Pts',(0.0122597669402842,-0.0349692089015915,
0.0782037329935917));
#88937=CARTESIAN_POINT('Ctrl Pts',(0.0122312439848286,-0.0350221583435001,
0.0781757772701851));
#88938=CARTESIAN_POINT('Ctrl Pts',(0.0123163070376437,-0.0351951371254971,
0.0780855694736824));
#88939=CARTESIAN_POINT('Ctrl Pts',(0.0123976724672537,-0.0350307338980969,
0.0779988916529992));
#88940=CARTESIAN_POINT('Ctrl Pts',(0.0124753858827252,-0.0348659306897824,
0.0779089249770034));
#88941=CARTESIAN_POINT('Ctrl Pts',(0.012317769981177,-0.0351951371254971,
0.0780855547809085));
#88942=CARTESIAN_POINT('Ctrl Pts',(0.0123991351070231,-0.0350307338980969,
0.0779988467147856));
#88943=CARTESIAN_POINT('Ctrl Pts',(0.0124768469689137,-0.0348659306897824,
0.0779088498317496));
#88944=CARTESIAN_POINT('Ctrl Pts',(0.0125629608421027,-0.0351951371254971,
0.078083092256691));
#88945=CARTESIAN_POINT('Ctrl Pts',(0.0126442750568056,-0.0350307338980969,
0.0779913150233564));
#88946=CARTESIAN_POINT('Ctrl Pts',(0.0127217265369057,-0.0348659306897824,
0.0778962554088947));
#88947=CARTESIAN_POINT('Origin',(0.0165002655538542,-0.0308609197411036,
0.0813866600107244));
#88948=CARTESIAN_POINT('',(0.0124246676682205,-0.0351951371254971,0.0780844811758722));
#88949=CARTESIAN_POINT('Origin',(0.00729963773095405,-0.0351840467441134,
0.0736250890021826));
#88950=CARTESIAN_POINT('Origin',(0.0176776632668949,-0.0352322613094349,
0.081353645914016));
#88951=CARTESIAN_POINT('',(0.0126268943305477,-0.0351951142564687,0.077727680206653));
#88952=CARTESIAN_POINT('',(0.0127023373764456,-0.0351951372916788,0.0776284094688718));
#88953=CARTESIAN_POINT('Origin',(0.00815708642437748,-0.0352875121843913,
0.0738110393723901));
#88954=CARTESIAN_POINT('Origin',(0.00252497855717473,-0.0298325076522683,
0.0791448561667019));
#88955=CARTESIAN_POINT('Origin',(0.0123983407151583,-0.0338733119721242,
0.0813593929882444));
#88956=CARTESIAN_POINT('Origin',(0.00812378219310841,-0.0315241814719618,
0.07415));
#88957=CARTESIAN_POINT('',(0.0102128016197025,-0.032210423332361,0.0797745886798604));
#88958=CARTESIAN_POINT('',(0.0102248110767376,-0.0321934096636183,0.0797701136670138));
#88959=CARTESIAN_POINT('Origin',(0.00498619218089495,-0.0326387250794343,
0.0640690356156492));
#88960=CARTESIAN_POINT('',(0.0102128016195757,-0.032176398030855,0.0797745886795186));
#88961=CARTESIAN_POINT('Origin',(0.00388023441440586,-0.0326386249069991,
0.0644865279611796));
#88962=CARTESIAN_POINT('',(0.0102007826323785,-0.0321934096636185,0.0797790380328533));
#88963=CARTESIAN_POINT('Origin',(0.00503047312598455,-0.0326386266482349,
0.0640593159491066));
#88964=CARTESIAN_POINT('Origin',(0.00392012137274927,-0.0326387236954171,
0.0644649790481927));
#88965=CARTESIAN_POINT('Origin',(0.00812378219310841,-0.0315241814719618,
0.07415));
#88966=CARTESIAN_POINT('',(0.0109012769640885,-0.0332121607144216,0.079468413558058));
#88967=CARTESIAN_POINT('',(0.010912630855329,-0.0331951640388587,0.079462468648306));
#88968=CARTESIAN_POINT('Origin',(0.00259264235951201,-0.0326413667686659,
0.0651939692242149));
#88969=CARTESIAN_POINT('',(0.0109012769642343,-0.0331781648281954,0.0794684135597341));
#88970=CARTESIAN_POINT('Origin',(0.00389130651643295,-0.032641209385684,
0.0645069026047347));
#88971=CARTESIAN_POINT('',(0.010889910402055,-0.0331951640388588,0.0794743342054824));
#88972=CARTESIAN_POINT('Origin',(0.00262859804245172,-0.0326412092525031,
0.0651663415884814));
#88973=CARTESIAN_POINT('Origin',(0.00393452553582239,-0.0326413669275042,
0.0644931830535462));
#88974=CARTESIAN_POINT('Origin',(0.00812378219310841,-0.0315241814719618,
0.07415));
#88975=CARTESIAN_POINT('',(0.0105618502623162,-0.0327114338380043,0.0796323192236207));
#88976=CARTESIAN_POINT('',(0.0105735550331357,-0.0326943950436593,0.0796270989613361));
#88977=CARTESIAN_POINT('Origin',(0.00372745508006589,-0.0326395683095568,
0.0644994038884998));
#88978=CARTESIAN_POINT('',(0.0105618502623353,-0.0326773559991214,0.0796323192236637));
#88979=CARTESIAN_POINT('Origin',(0.0038603443629257,-0.0326395671738251,
0.0644394545930779));
#88980=CARTESIAN_POINT('',(0.0105501343689866,-0.0326943950436594,0.0796375144754808));
#88981=CARTESIAN_POINT('Origin',(0.00376853268769228,-0.0326395670095084,
0.0644802850492608));
#88982=CARTESIAN_POINT('Origin',(0.00390205414765034,-0.0326395685694152,
0.0644217576004931));
#88983=CARTESIAN_POINT('Ctrl Pts',(0.00997439487967158,-0.0327445246967097,
0.0795954896643306));
#88984=CARTESIAN_POINT('Ctrl Pts',(0.0101797748798699,-0.032443687833936,
0.0795256926658306));
#88985=CARTESIAN_POINT('Ctrl Pts',(0.0103793140219879,-0.0321434074405927,
0.0794406238922183));
#88986=CARTESIAN_POINT('Ctrl Pts',(0.0102092951270713,-0.0327445246967097,
0.0795099217160583));
#88987=CARTESIAN_POINT('Ctrl Pts',(0.0104114478793422,-0.032443687833936,
0.0794312653098958));
#88988=CARTESIAN_POINT('Ctrl Pts',(0.0106071016150094,-0.0321434074405927,
0.0793376053867665));
#88989=CARTESIAN_POINT('',(0.0102429380749441,-0.0326943950436612,0.0794967095814606));
#88990=CARTESIAN_POINT('',(0.0104608161269541,-0.0323666188837389,0.0794051305780213));
#88991=CARTESIAN_POINT('Origin',(0.00397814613099812,-0.0326395579111258,
0.0638966954752427));
#88992=CARTESIAN_POINT('Origin',(0.0149487344831154,-0.0321933825602998,
0.0894968083710972));
#88993=CARTESIAN_POINT('',(0.0103460491034406,-0.032193409653269,0.0794546823445082));
#88994=CARTESIAN_POINT('',(0.0104031565980373,-0.0321934096584275,0.0794292858013028));
#88995=CARTESIAN_POINT('',(0.0101262321451377,-0.0325210109756239,0.0795415043531114));
#88996=CARTESIAN_POINT('Origin',(0.00443386070631231,-0.0326393129158185,
0.0637433701488976));
#88997=CARTESIAN_POINT('',(0.0101257591440836,-0.0326943950436593,0.0795402308195257));
#88998=CARTESIAN_POINT('Origin',(0.0139773724095966,-0.0326943765538131,
0.0899105245446342));
#88999=CARTESIAN_POINT('',(0.0101843486095239,-0.0326943950436702,0.0795184702005032));
#89000=CARTESIAN_POINT('Ctrl Pts',(0.00999073073834982,-0.0325229783203769,
0.0798521489922192));
#89001=CARTESIAN_POINT('Ctrl Pts',(0.0100693347375098,-0.032413025309245,
0.0798264131473505));
#89002=CARTESIAN_POINT('Ctrl Pts',(0.0101473944358221,-0.032303122220807,
0.0797990551811304));
#89003=CARTESIAN_POINT('Ctrl Pts',(0.0102248110809361,-0.0321934096576658,
0.0797701136654483));
#89004=CARTESIAN_POINT('Ctrl Pts',(0.0100357229730105,-0.0325229783203769,
0.0797481449487558));
#89005=CARTESIAN_POINT('Ctrl Pts',(0.0101128932787057,-0.032413025309245,
0.0797217888869163));
#89006=CARTESIAN_POINT('Ctrl Pts',(0.0101895066710162,-0.032303122220807,
0.0796938404555844));
#89007=CARTESIAN_POINT('Ctrl Pts',(0.0102654662768954,-0.0321934096576658,
0.0796643389176207));
#89008=CARTESIAN_POINT('Ctrl Pts',(0.0100807152076711,-0.0325229783203769,
0.0796441409052925));
#89009=CARTESIAN_POINT('Ctrl Pts',(0.0101564518199016,-0.032413025309245,
0.0796171646264821));
#89010=CARTESIAN_POINT('Ctrl Pts',(0.0102316189062103,-0.032303122220807,
0.0795886257300383));
#89011=CARTESIAN_POINT('Ctrl Pts',(0.0103061214728548,-0.0321934096576658,
0.0795585641697932));
#89012=CARTESIAN_POINT('Ctrl Pts',(0.0101257074423317,-0.0325229783203769,
0.0795401368618291));
#89013=CARTESIAN_POINT('Ctrl Pts',(0.0102000103610976,-0.032413025309245,
0.0795125403660479));
#89014=CARTESIAN_POINT('Ctrl Pts',(0.0102737311414044,-0.032303122220807,
0.0794834110044923));
#89015=CARTESIAN_POINT('Ctrl Pts',(0.0103467766688141,-0.0321934096576658,
0.0794527894219656));
#89016=CARTESIAN_POINT('',(0.0102854300896961,-0.0321934096584275,0.0796123980060863));
#89017=CARTESIAN_POINT('Ctrl Pts',(0.0102128016184853,-0.0322104233328928,
0.0797745886765923));
#89018=CARTESIAN_POINT('Ctrl Pts',(0.0101978383033872,-0.0322609421830893,
0.0797343006392277));
#89019=CARTESIAN_POINT('Ctrl Pts',(0.0101831442528801,-0.032312088823975,
0.0796947375843842));
#89020=CARTESIAN_POINT('Ctrl Pts',(0.0101542817150667,-0.0324156524631818,
0.0796170265294315));
#89021=CARTESIAN_POINT('Ctrl Pts',(0.0101401250918172,-0.032468026716731,
0.0795789104727493));
#89022=CARTESIAN_POINT('Ctrl Pts',(0.0101262321451267,-0.0325210109755912,
0.0795415043530692));
#89023=CARTESIAN_POINT('Origin',(0.00047196380965428,-0.0262834582510976,
0.0759811366053846));
#89024=CARTESIAN_POINT('Origin',(0.00681081577538088,-0.0342770849357031,
0.0862371777635268));
#89025=CARTESIAN_POINT('Ctrl Pts',(0.0102410947514925,-0.0326943950436604,
0.0794958646853215));
#89026=CARTESIAN_POINT('Ctrl Pts',(0.0103147707860745,-0.0325844576448134,
0.0794666841500003));
#89027=CARTESIAN_POINT('Ctrl Pts',(0.0103878485335113,-0.0324744968375322,
0.0794359778083386));
#89028=CARTESIAN_POINT('Ctrl Pts',(0.0104602349049862,-0.0323646534831894,
0.0794037862945516));
#89029=CARTESIAN_POINT('Ctrl Pts',(0.0103441079573282,-0.0326943950436604,
0.0795430812820435));
#89030=CARTESIAN_POINT('Ctrl Pts',(0.0104184347251064,-0.0325844576448134,
0.0795124810316786));
#89031=CARTESIAN_POINT('Ctrl Pts',(0.010492133889758,-0.0324744968375322,
0.0794803414162683));
#89032=CARTESIAN_POINT('Ctrl Pts',(0.0105651115915997,-0.0323646534831894,
0.0794467049174037));
#89033=CARTESIAN_POINT('Ctrl Pts',(0.010447121163164,-0.0326943950436604,
0.0795902978787655));
#89034=CARTESIAN_POINT('Ctrl Pts',(0.0105220986641383,-0.0325844576448134,
0.0795582779133568));
#89035=CARTESIAN_POINT('Ctrl Pts',(0.0105964192460048,-0.0324744968375322,
0.079524705024198));
#89036=CARTESIAN_POINT('Ctrl Pts',(0.0106699882782133,-0.0323646534831894,
0.0794896235402558));
#89037=CARTESIAN_POINT('Ctrl Pts',(0.0105501343689998,-0.0326943950436604,
0.0796375144754875));
#89038=CARTESIAN_POINT('Ctrl Pts',(0.0106257626031702,-0.0325844576448134,
0.079604074795035));
#89039=CARTESIAN_POINT('Ctrl Pts',(0.0107007046022515,-0.0324744968375322,
0.0795690686321276));
#89040=CARTESIAN_POINT('Ctrl Pts',(0.0107748649648269,-0.0323646534831894,
0.079532542163108));
#89041=CARTESIAN_POINT('Ctrl Pts',(0.0105618502609686,-0.0326773559987509,
0.079632319220597));
#89042=CARTESIAN_POINT('Ctrl Pts',(0.0105443963626624,-0.0326267922587325,
0.0795930718167121));
#89043=CARTESIAN_POINT('Ctrl Pts',(0.0105272518220983,-0.0325756109582045,
0.079554520044716));
#89044=CARTESIAN_POINT('Ctrl Pts',(0.0104935668654355,-0.0324719985462386,
0.0794787749546622));
#89045=CARTESIAN_POINT('Ctrl Pts',(0.0104770399595816,-0.0324196091621784,
0.0794416120161806));
#89046=CARTESIAN_POINT('Ctrl Pts',(0.0104608161269342,-0.0323666188837756,
0.0794051305779768));
#89047=CARTESIAN_POINT('',(0.0103965362219753,-0.0326943950436703,0.0795671120284807));
#89048=CARTESIAN_POINT('Ctrl Pts',(0.0103104138834163,-0.0332451089994434,
0.0794695298759328));
#89049=CARTESIAN_POINT('Ctrl Pts',(0.0105110432351552,-0.0329451141710254,
0.0793870597124503));
#89050=CARTESIAN_POINT('Ctrl Pts',(0.0107048906302263,-0.0326442513127493,
0.0792897116150461));
#89051=CARTESIAN_POINT('Ctrl Pts',(0.0103127045152811,-0.0332451089994434,
0.0794685283742304));
#89052=CARTESIAN_POINT('Ctrl Pts',(0.0105132960947654,-0.0329451141710254,
0.0793859718181537));
#89053=CARTESIAN_POINT('Ctrl Pts',(0.0107070993174453,-0.0326442513127493,
0.0792885404187481));
#89054=CARTESIAN_POINT('Ctrl Pts',(0.0105417677017643,-0.0332451089994434,
0.0793683782039951));
#89055=CARTESIAN_POINT('Ctrl Pts',(0.0107385820557795,-0.0329451141710254,
0.0792771823884944));
#89056=CARTESIAN_POINT('Ctrl Pts',(0.0109279680393519,-0.0326442513127493,
0.0791714207889529));
#89057=CARTESIAN_POINT('Ctrl Pts',(0.0105440812399477,-0.0332451089994434,
0.0793673666872757));
#89058=CARTESIAN_POINT('Ctrl Pts',(0.0107408574439857,-0.0329451141710254,
0.0792760836152549));
#89059=CARTESIAN_POINT('Ctrl Pts',(0.0109301988134431,-0.0326442513127493,
0.079170237880692));
#89060=CARTESIAN_POINT('',(0.0105744790772793,-0.0331951640388616,0.0793530961726568));
#89061=CARTESIAN_POINT('',(0.010786176918691,-0.0328677532355045,0.0792480172023093));
#89062=CARTESIAN_POINT('Origin',(0.00274393348338891,-0.0326402808279978,
0.0645303162996148));
#89063=CARTESIAN_POINT('Origin',(0.0159044919433389,-0.0326944278779235,
0.08904787609129));
#89064=CARTESIAN_POINT('',(0.0106747477336384,-0.0326943950436593,0.0793046774691565));
#89065=CARTESIAN_POINT('',(0.0107301478748956,-0.0326943950436694,0.0792757452319597));
#89066=CARTESIAN_POINT('',(0.0104608161269515,-0.0330220786163546,0.0794051305780225));
#89067=CARTESIAN_POINT('Origin',(0.0031546461841902,-0.0326396682763683,
0.0642803808623885));
#89068=CARTESIAN_POINT('',(0.0104602640934199,-0.0331951640388588,0.079403889257447));
#89069=CARTESIAN_POINT('Origin',(0.0149429170789886,-0.0331952026560129,
0.0894837301171005));
#89070=CARTESIAN_POINT('',(0.0105173715853596,-0.0331951640388701,0.0793784927150619));
#89071=CARTESIAN_POINT('Ctrl Pts',(0.0103450885321277,-0.0330240426238172,
0.0797236700788876));
#89072=CARTESIAN_POINT('Ctrl Pts',(0.010421871267628,-0.032914277406352,
0.0796930694199537));
#89073=CARTESIAN_POINT('Ctrl Pts',(0.0104980596810234,-0.0328043479726691,
0.0796608661918505));
#89074=CARTESIAN_POINT('Ctrl Pts',(0.010573555033134,-0.0326943950436593,
0.0796270989613414));
#89075=CARTESIAN_POINT('Ctrl Pts',(0.0103834614905519,-0.0330240426238172,
0.0796170461976671));
#89076=CARTESIAN_POINT('Ctrl Pts',(0.0104587753782098,-0.032914277406352,
0.0795859169138459));
#89077=CARTESIAN_POINT('Ctrl Pts',(0.0105334832833355,-0.0328043479726691,
0.0795532151625046));
#89078=CARTESIAN_POINT('Ctrl Pts',(0.0106074883458023,-0.0326943950436593,
0.0795189802012852));
#89079=CARTESIAN_POINT('Ctrl Pts',(0.0104218344489761,-0.0330240426238172,
0.0795104223164465));
#89080=CARTESIAN_POINT('Ctrl Pts',(0.0104956794887916,-0.032914277406352,
0.0794787644077381));
#89081=CARTESIAN_POINT('Ctrl Pts',(0.0105689068856476,-0.0328043479726691,
0.0794455641331588));
#89082=CARTESIAN_POINT('Ctrl Pts',(0.0106414216584705,-0.0326943950436593,
0.0794108614412289));
#89083=CARTESIAN_POINT('Ctrl Pts',(0.0104602074074004,-0.0330240426238172,
0.079403798435226));
#89084=CARTESIAN_POINT('Ctrl Pts',(0.0105325835993734,-0.032914277406352,
0.0793716119016304));
#89085=CARTESIAN_POINT('Ctrl Pts',(0.0106043304879597,-0.0328043479726691,
0.0793379131038129));
#89086=CARTESIAN_POINT('Ctrl Pts',(0.0106753549711388,-0.0326943950436593,
0.0793027426811726));
#89087=CARTESIAN_POINT('',(0.010624151383397,-0.0326943950436693,0.0794658882152563));
#89088=CARTESIAN_POINT('Ctrl Pts',(0.010561850260963,-0.0327114338383315,
0.0796323192205846));
#89089=CARTESIAN_POINT('Ctrl Pts',(0.010544399265784,-0.0327619876830508,
0.0795930783447659));
#89090=CARTESIAN_POINT('Ctrl Pts',(0.0105272561432298,-0.0328131562603382,
0.079554529761353));
#89091=CARTESIAN_POINT('Ctrl Pts',(0.0104935712175586,-0.0329167375858771,
0.0794787847409879));
#89092=CARTESIAN_POINT('Ctrl Pts',(0.0104770428362969,-0.0329691088920626,
0.0794416184848567));
#89093=CARTESIAN_POINT('Ctrl Pts',(0.0104608161269346,-0.0330220786163188,
0.079405130577978));
#89094=CARTESIAN_POINT('Ctrl Pts',(0.0105725860375645,-0.0331951640388604,
0.079352368570823));
#89095=CARTESIAN_POINT('Ctrl Pts',(0.0106801416723178,-0.0330306422010619,
0.0793017411213658));
#89096=CARTESIAN_POINT('Ctrl Pts',(0.0107855129158078,-0.0328657861914644,
0.079246711545217));
#89097=CARTESIAN_POINT('Ctrl Pts',(0.0105744790772765,-0.0331951640388604,
0.0793530961726581));
#89098=CARTESIAN_POINT('Ctrl Pts',(0.0106820497547313,-0.0330306422010619,
0.0793024295858185));
#89099=CARTESIAN_POINT('Ctrl Pts',(0.0107874344104796,-0.0328657861914644,
0.0792473602839994));
#89100=CARTESIAN_POINT('Ctrl Pts',(0.0108899104020711,-0.0331951640388604,
0.0794743342054896));
#89101=CARTESIAN_POINT('Ctrl Pts',(0.0109999875981241,-0.0330306422010619,
0.0794171462782456));
#89102=CARTESIAN_POINT('Ctrl Pts',(0.0111076070968112,-0.0328657861914644,
0.0793554576114121));
#89103=CARTESIAN_POINT('Ctrl Pts',(0.0109012769624029,-0.033178164828644,
0.0794684135594792));
#89104=CARTESIAN_POINT('Ctrl Pts',(0.0108813794405278,-0.0331276811546772,
0.0794303133338342));
#89105=CARTESIAN_POINT('Ctrl Pts',(0.0108618411763031,-0.0330765663497778,
0.0793929010959286));
#89106=CARTESIAN_POINT('Ctrl Pts',(0.0108234665200749,-0.0329730614462884,
0.0793194203768333));
#89107=CARTESIAN_POINT('Ctrl Pts',(0.0108046456353499,-0.0329207133373271,
0.0792833815777759));
#89108=CARTESIAN_POINT('Ctrl Pts',(0.0107861769103332,-0.0328677532289398,
0.079248017216505));
#89109=CARTESIAN_POINT('',(0.0107321947396771,-0.0331951640388701,0.0794137151890796));
#89110=CARTESIAN_POINT('Ctrl Pts',(0.0106734180977772,-0.033693872113265,
0.0793053718598066));
#89111=CARTESIAN_POINT('Ctrl Pts',(0.0107813411936073,-0.0335278710435226,
0.0792519975140652));
#89112=CARTESIAN_POINT('Ctrl Pts',(0.0108875525167375,-0.0333620469224385,
0.0791952575050686));
#89113=CARTESIAN_POINT('Ctrl Pts',(0.0109920954511926,-0.0331951640388587,
0.0791351059479975));
#89114=CARTESIAN_POINT('Ctrl Pts',(0.0107477281647204,-0.033693872113265,
0.0792665640799846));
#89115=CARTESIAN_POINT('Ctrl Pts',(0.0108548388544128,-0.0335278710435226,
0.0792116341194991));
#89116=CARTESIAN_POINT('Ctrl Pts',(0.0109601892735341,-0.0333620469224385,
0.0791533645198656));
#89117=CARTESIAN_POINT('Ctrl Pts',(0.0110638221235362,-0.0331951640388587,
0.0790917087787543));
#89118=CARTESIAN_POINT('Ctrl Pts',(0.0108220382316635,-0.033693872113265,
0.0792277563001626));
#89119=CARTESIAN_POINT('Ctrl Pts',(0.0109283365152184,-0.0335278710435226,
0.0791712707249331));
#89120=CARTESIAN_POINT('Ctrl Pts',(0.0110328260303307,-0.0333620469224385,
0.0791114715346625));
#89121=CARTESIAN_POINT('Ctrl Pts',(0.0111355487958798,-0.0331951640388587,
0.079048311609511));
#89122=CARTESIAN_POINT('Ctrl Pts',(0.0108963482986067,-0.033693872113265,
0.0791889485203406));
#89123=CARTESIAN_POINT('Ctrl Pts',(0.0110018341760239,-0.0335278710435226,
0.0791309073303671));
#89124=CARTESIAN_POINT('Ctrl Pts',(0.0111054627871273,-0.0333620469224385,
0.0790695785494594));
#89125=CARTESIAN_POINT('Ctrl Pts',(0.0112072754682234,-0.0331951640388587,
0.0790049144402678));
#89126=CARTESIAN_POINT('',(0.0108963482986413,-0.0336938721132548,0.0791889485203216));
#89127=CARTESIAN_POINT('',(0.0111010304411501,-0.033367984620877,0.0790707843089641));
#89128=CARTESIAN_POINT('Ctrl Pts',(0.010896348298657,-0.0336938721132388,
0.079188948520342));
#89129=CARTESIAN_POINT('Ctrl Pts',(0.0109160176785375,-0.0336629187933905,
0.0791781258941925));
#89130=CARTESIAN_POINT('Ctrl Pts',(0.0109356173968631,-0.0336319952301045,
0.0791671915572488));
#89131=CARTESIAN_POINT('Ctrl Pts',(0.0110041484568814,-0.033523589259546,
0.0791284319404732));
#89132=CARTESIAN_POINT('Ctrl Pts',(0.0110527878648309,-0.0334458668645768,
0.0790999727380171));
#89133=CARTESIAN_POINT('Ctrl Pts',(0.0111010304285895,-0.0333679869902211,
0.0790707842881225));
#89134=CARTESIAN_POINT('Ctrl Pts',(0.0111010308214529,-0.0333679128829521,
0.0790707849399957));
#89135=CARTESIAN_POINT('Ctrl Pts',(0.0111007961598316,-0.0333391359256885,
0.0790703970921813));
#89136=CARTESIAN_POINT('Ctrl Pts',(0.0111006202934607,-0.033310357818173,
0.0790701064209276));
#89137=CARTESIAN_POINT('Ctrl Pts',(0.0111005030686477,-0.0332815781851602,
0.0790699126722103));
#89138=CARTESIAN_POINT('Ctrl Pts',(0.0111003857431915,-0.0332527738434303,
0.0790697187571504));
#89139=CARTESIAN_POINT('Ctrl Pts',(0.0111003271651869,-0.0332239691038149,
0.079069621939661));
#89140=CARTESIAN_POINT('Ctrl Pts',(0.0111003271651869,-0.0331951640388587,
0.079069621939661));
#89141=CARTESIAN_POINT('',(0.0109933788621512,-0.0331951640388587,0.079134329439054));
#89142=CARTESIAN_POINT('',(0.0110468530136792,-0.0331951640388687,0.0791019756893674));
#89143=CARTESIAN_POINT('',(0.0107861769034134,-0.0335216366558398,0.0792480172031858));
#89144=CARTESIAN_POINT('Origin',(0.00202357608885349,-0.0326434571527828,
0.0650851258327308));
#89145=CARTESIAN_POINT('',(0.0107855480161328,-0.0336938721132327,0.0792468129947429));
#89146=CARTESIAN_POINT('Origin',(0.0158408513303333,-0.0336938867896141,
0.0889268304697));
#89147=CARTESIAN_POINT('',(0.010840948157397,-0.0336938721132538,0.0792178807575423));
#89148=CARTESIAN_POINT('Ctrl Pts',(0.01069067980009,-0.0335235895815172,
0.0795731943239509));
#89149=CARTESIAN_POINT('Ctrl Pts',(0.0107653407472462,-0.0334144449262748,
0.0795378559246344));
#89150=CARTESIAN_POINT('Ctrl Pts',(0.0108393574060506,-0.0333049234473147,
0.079500934486799));
#89151=CARTESIAN_POINT('Ctrl Pts',(0.0109126308553275,-0.0331951640388587,
0.0794624686483122));
#89152=CARTESIAN_POINT('Ctrl Pts',(0.0107222820968345,-0.0335235895815172,
0.07946437122288));
#89153=CARTESIAN_POINT('Ctrl Pts',(0.0107954448797515,-0.0334144449262748,
0.0794285977557297));
#89154=CARTESIAN_POINT('Ctrl Pts',(0.0108679526649334,-0.0333049234473147,
0.0793912717011658));
#89155=CARTESIAN_POINT('Ctrl Pts',(0.0109397084137242,-0.0331951640388587,
0.0793524323892087));
#89156=CARTESIAN_POINT('Ctrl Pts',(0.0107538843935789,-0.0335235895815172,
0.0793555481218091));
#89157=CARTESIAN_POINT('Ctrl Pts',(0.0108255490122568,-0.0334144449262748,
0.0793193395868249));
#89158=CARTESIAN_POINT('Ctrl Pts',(0.0108965479238162,-0.0333049234473147,
0.0792816089155325));
#89159=CARTESIAN_POINT('Ctrl Pts',(0.0109667859721209,-0.0331951640388587,
0.0792423961301052));
#89160=CARTESIAN_POINT('Ctrl Pts',(0.0107854866903234,-0.0335235895815172,
0.0792467250207382));
#89161=CARTESIAN_POINT('Ctrl Pts',(0.010855653144762,-0.0334144449262748,
0.0792100814179201));
#89162=CARTESIAN_POINT('Ctrl Pts',(0.0109251431826991,-0.0333049234473147,
0.0791719461298993));
#89163=CARTESIAN_POINT('Ctrl Pts',(0.0109938635305176,-0.0331951640388587,
0.0791323598710018));
#89164=CARTESIAN_POINT('',(0.0109530048587501,-0.0331951640388687,0.07929839904369));
#89165=CARTESIAN_POINT('Ctrl Pts',(0.0109012769626324,-0.0332121607145966,
0.079468413555275));
#89166=CARTESIAN_POINT('Ctrl Pts',(0.010881412924295,-0.0332625444106898,
0.079430377418568));
#89167=CARTESIAN_POINT('Ctrl Pts',(0.0108618911745105,-0.0333135300740933,
0.0793929967041725));
#89168=CARTESIAN_POINT('Ctrl Pts',(0.0108235167555749,-0.0334167203138383,
0.079319516447042));
#89169=CARTESIAN_POINT('Ctrl Pts',(0.0108046789494215,-0.0334688847584559,
0.0792834453643316));
#89170=CARTESIAN_POINT('Ctrl Pts',(0.0107861769032448,-0.0335216366555605,
0.079248017202858));
#89171=CARTESIAN_POINT('Ctrl Pts',(0.0108963482986233,-0.0336938721132388,
0.0791889485203314));
#89172=CARTESIAN_POINT('Ctrl Pts',(0.0109258429364132,-0.0336474569764957,
0.0791727197708809));
#89173=CARTESIAN_POINT('Ctrl Pts',(0.0109551455752089,-0.033601104548885,
0.0791561468614595));
#89174=CARTESIAN_POINT('Ctrl Pts',(0.0110293331195408,-0.0334837508592656,
0.0791141880651553));
#89175=CARTESIAN_POINT('Ctrl Pts',(0.0111022447600412,-0.0333660264659097,
0.0790700493633073));
#89176=CARTESIAN_POINT('Ctrl Pts',(0.011220704319783,-0.0336938721132388,
0.0792907483770459));
#89177=CARTESIAN_POINT('Ctrl Pts',(0.0112507948259149,-0.0336474569764957,
0.0792726210641708));
#89178=CARTESIAN_POINT('Ctrl Pts',(0.0112806710671415,-0.033601104548885,
0.0792541427460243));
#89179=CARTESIAN_POINT('Ctrl Pts',(0.0113563108409488,-0.0334837508592656,
0.0792073598929091));
#89180=CARTESIAN_POINT('Ctrl Pts',(0.0114305311264073,-0.0333660264659097,
0.0791583562200499));
#89181=CARTESIAN_POINT('',(0.0112297421639733,-0.0336769361243754,0.079283518545733));
#89182=CARTESIAN_POINT('',(0.011218769790806,-0.033693872113232,0.0792901412208322));
#89183=CARTESIAN_POINT('Ctrl Pts',(0.0112297421639733,-0.0336769361243754,
0.079283518545733));
#89184=CARTESIAN_POINT('Ctrl Pts',(0.011227914477107,-0.0336797586669902,
0.0792846243608178));
#89185=CARTESIAN_POINT('Ctrl Pts',(0.0112260862688101,-0.0336825812712596,
0.0792857291580131));
#89186=CARTESIAN_POINT('Ctrl Pts',(0.011222428820045,-0.0336882265869416,
0.0792879367107729));
#89187=CARTESIAN_POINT('Ctrl Pts',(0.0112205995796331,-0.0336910492983079,
0.0792890394663461));
#89188=CARTESIAN_POINT('Ctrl Pts',(0.0112187697908194,-0.033693872113238,
0.0792901412208391));
#89189=CARTESIAN_POINT('Ctrl Pts',(0.0112297421639733,-0.0336769361243754,
0.079283518545733));
#89190=CARTESIAN_POINT('Ctrl Pts',(0.0112080455760862,-0.0336279018505222,
0.0792476585097562));
#89191=CARTESIAN_POINT('Ctrl Pts',(0.0111860368553374,-0.0335767826010775,
0.0792112825818021));
#89192=CARTESIAN_POINT('Ctrl Pts',(0.0111429124074254,-0.0334733172064619,
0.079140006662213));
#89193=CARTESIAN_POINT('Ctrl Pts',(0.0111217676971637,-0.0334209631456238,
0.0791050587674256));
#89194=CARTESIAN_POINT('Ctrl Pts',(0.0111010304244935,-0.033367986984468,
0.0790707842839039));
#89195=CARTESIAN_POINT('',(0.0110575590447336,-0.0336938721132534,0.0792395448705869));
#89196=CARTESIAN_POINT('Ctrl Pts',(0.0096636317672152,-0.0321934096636942,
0.0796913896295103));
#89197=CARTESIAN_POINT('Ctrl Pts',(0.00981230007270001,-0.0319797282160735,
0.0796500774601468));
#89198=CARTESIAN_POINT('Ctrl Pts',(0.00995853940576728,-0.0317669959606461,
0.0796008533008619));
#89199=CARTESIAN_POINT('Ctrl Pts',(0.00990303373244094,-0.0321934096636942,
0.0796192219702425));
#89200=CARTESIAN_POINT('Ctrl Pts',(0.0100497658731131,-0.0319797282160735,
0.0795714869562714));
#89201=CARTESIAN_POINT('Ctrl Pts',(0.010193727441266,-0.0317669959606461,
0.0795159530066551));
#89202=CARTESIAN_POINT('Ctrl Pts',(0.00990446994694649,-0.0321934096636942,
0.0796187890237586));
#89203=CARTESIAN_POINT('Ctrl Pts',(0.0100511904722253,-0.0319797282160735,
0.0795710154780128));
#89204=CARTESIAN_POINT('Ctrl Pts',(0.0101951383756658,-0.0317669959606461,
0.0795154436748543));
#89205=CARTESIAN_POINT('',(0.00990303373254501,-0.0321934096636942,0.0796192219702087));
#89206=CARTESIAN_POINT('',(0.010126232145142,-0.0318665617561286,0.0795415043531098));
#89207=CARTESIAN_POINT('Origin',(0.00532192722094431,-0.0326371944421877,
0.0635496430093242));
#89208=CARTESIAN_POINT('Origin',(0.0139425870835524,-0.0316939261509089,
0.0898168644506043));
#89209=CARTESIAN_POINT('',(0.00978398701925707,-0.0320197259213214,0.0796564807125462));
#89210=CARTESIAN_POINT('Ctrl Pts',(0.00978416991441515,-0.0320197391311199,
0.0796564733134607));
#89211=CARTESIAN_POINT('Ctrl Pts',(0.00981218862409361,-0.0319792715672864,
0.0796480247259767));
#89212=CARTESIAN_POINT('Ctrl Pts',(0.00984027045301016,-0.0319386438886474,
0.0796393239931166));
#89213=CARTESIAN_POINT('Ctrl Pts',(0.00986844231933618,-0.0318979098685815,
0.079630353953209));
#89214=CARTESIAN_POINT('Ctrl Pts',(0.00989661362870992,-0.0318571766538192,
0.0796213840906373));
#89215=CARTESIAN_POINT('Ctrl Pts',(0.00992473250423351,-0.0318163871807252,
0.079612192158285));
#89216=CARTESIAN_POINT('Ctrl Pts',(0.00995270322272097,-0.0317755399642118,
0.0796028133577372));
#89217=CARTESIAN_POINT('',(0.00978335330633817,-0.0321934096636185,0.0796552996031219));
#89218=CARTESIAN_POINT('Origin',(0.0103384426816057,-0.0323427921796758,
0.0814966990457025));
#89219=CARTESIAN_POINT('',(0.0098431935194516,-0.0321934096636664,0.0796372607866753));
#89220=CARTESIAN_POINT('Ctrl Pts',(0.00990124666418742,-0.0321934096636618,
0.0796182627652958));
#89221=CARTESIAN_POINT('Ctrl Pts',(0.00997665826943559,-0.0320835708272593,
0.0795937501449649));
#89222=CARTESIAN_POINT('Ctrl Pts',(0.0100515188454842,-0.0319739230346489,
0.0795676911036986));
#89223=CARTESIAN_POINT('Ctrl Pts',(0.0101257351722283,-0.0318646057455573,
0.0795401263329965));
#89224=CARTESIAN_POINT('Ctrl Pts',(0.0100010919869124,-0.0321934096636618,
0.0796718545211547));
#89225=CARTESIAN_POINT('Ctrl Pts',(0.0100772426642408,-0.0320835708272593,
0.0796459649560085));
#89226=CARTESIAN_POINT('Ctrl Pts',(0.0101528133878765,-0.0319739230346489,
0.0796185144735526));
#89227=CARTESIAN_POINT('Ctrl Pts',(0.0102277101657592,-0.0318646057455573,
0.0795895456152703));
#89228=CARTESIAN_POINT('Ctrl Pts',(0.0101009373096374,-0.0321934096636618,
0.0797254462770135));
#89229=CARTESIAN_POINT('Ctrl Pts',(0.0101778270590461,-0.0320835708272593,
0.0796981797670521));
#89230=CARTESIAN_POINT('Ctrl Pts',(0.0102541079302688,-0.0319739230346489,
0.0796693378434066));
#89231=CARTESIAN_POINT('Ctrl Pts',(0.0103296851592901,-0.0318646057455573,
0.0796389648975441));
#89232=CARTESIAN_POINT('Ctrl Pts',(0.0102007826323624,-0.0321934096636618,
0.0797790380328724));
#89233=CARTESIAN_POINT('Ctrl Pts',(0.0102784114538514,-0.0320835708272593,
0.0797503945780957));
#89234=CARTESIAN_POINT('Ctrl Pts',(0.0103554024726611,-0.0319739230346489,
0.0797201612132606));
#89235=CARTESIAN_POINT('Ctrl Pts',(0.0104316601528211,-0.0318646057455573,
0.0796883841798179));
#89236=CARTESIAN_POINT('Ctrl Pts',(0.0102128016184661,-0.0321763980306411,
0.0797745886765405));
#89237=CARTESIAN_POINT('Ctrl Pts',(0.010197858551582,-0.0321259596179381,
0.0797343551565603));
#89238=CARTESIAN_POINT('Ctrl Pts',(0.0101831743927205,-0.0320749164640418,
0.0796948187345174));
#89239=CARTESIAN_POINT('Ctrl Pts',(0.0101543120737603,-0.0319716057814256,
0.0796171082688167));
#89240=CARTESIAN_POINT('Ctrl Pts',(0.0101401451595835,-0.0319193786724667,
0.0795789645042865));
#89241=CARTESIAN_POINT('Ctrl Pts',(0.010126232145124,-0.0318665617561676,
0.0795415043530615));
#89242=CARTESIAN_POINT('',(0.0100519081824717,-0.0321934096636664,0.079699130001541));
#89243=CARTESIAN_POINT('Origin',(0.00812378219310841,-0.0315241814719618,
0.07415));
#89244=CARTESIAN_POINT('',(0.0112297421633088,-0.0337108120655389,0.0792835185446306));
#89245=CARTESIAN_POINT('',(0.0112407003659563,-0.0336938721132327,0.0792768724485572));
#89246=CARTESIAN_POINT('Origin',(0.0037164075845662,-0.0345562527130611,
0.0647065494387839));
#89247=CARTESIAN_POINT('Ctrl Pts',(0.0112407003659567,-0.0336938721132373,
0.0792768724485696));
#89248=CARTESIAN_POINT('Ctrl Pts',(0.011238875303069,-0.0336910493021816,
0.0792779820083915));
#89249=CARTESIAN_POINT('Ctrl Pts',(0.0112370496041514,-0.0336882265888785,
0.0792790906201662));
#89250=CARTESIAN_POINT('Ctrl Pts',(0.0112333968780567,-0.0336825812713059,
0.079281305981301));
#89251=CARTESIAN_POINT('Ctrl Pts',(0.0112315698508547,-0.0336797586670134,
0.0792824127306391));
#89252=CARTESIAN_POINT('Ctrl Pts',(0.0112297421639734,-0.0336769361243754,
0.079283518545733));
#89253=CARTESIAN_POINT('Origin',(0.00180399000269284,-0.0345562523252851,
0.0658636300553531));
#89254=CARTESIAN_POINT('Ctrl Pts',(0.0109619695376012,-0.0342436276873911,
0.0791522812393508));
#89255=CARTESIAN_POINT('Ctrl Pts',(0.0111506336847112,-0.033943005420181,
0.0790452372390105));
#89256=CARTESIAN_POINT('Ctrl Pts',(0.0113306988640532,-0.0336441434784052,
0.0789242863828657));
#89257=CARTESIAN_POINT('Ctrl Pts',(0.0111766759614705,-0.0342436276873911,
0.0790242142586365));
#89258=CARTESIAN_POINT('Ctrl Pts',(0.0113605099827772,-0.033943005420181,
0.0789090724720263));
#89259=CARTESIAN_POINT('Ctrl Pts',(0.0115351487997555,-0.0336441434784052,
0.0787804106594397));
#89260=CARTESIAN_POINT('Ctrl Pts',(0.0111788230257092,-0.0342436276873911,
0.0790229335888294));
#89261=CARTESIAN_POINT('Ctrl Pts',(0.0113626087457579,-0.033943005420181,
0.0789077108243564));
#89262=CARTESIAN_POINT('Ctrl Pts',(0.0115371932991125,-0.0336441434784052,
0.0787789719022055));
#89263=CARTESIAN_POINT('',(0.0112072754682234,-0.0341934961088741,0.0790049144402678));
#89264=CARTESIAN_POINT('',(0.0114041341081436,-0.0338664212862963,0.078874131276693));
#89265=CARTESIAN_POINT('Origin',(0.00266953802630421,-0.0345610720406482,
0.0646118541980884));
#89266=CARTESIAN_POINT('Origin',(0.0176588912847395,-0.0336938005072858,
0.0878817245803645));
#89267=CARTESIAN_POINT('',(0.0113006850036053,-0.0336938721132327,0.0789443105377789));
#89268=CARTESIAN_POINT('',(0.0113520221273582,-0.0336938721132427,0.0789086629610717));
#89269=CARTESIAN_POINT('',(0.011101030424489,-0.0340203938281605,0.0790707842839066));
#89270=CARTESIAN_POINT('Origin',(0.00311628593912468,-0.0345589643245431,
0.0644331000750157));
#89271=CARTESIAN_POINT('',(0.0111003271651873,-0.034193496108874,0.0790696219396609));
#89272=CARTESIAN_POINT('Origin',(0.0168046534788821,-0.0341934220717595,
0.0884977118607877));
#89273=CARTESIAN_POINT('',(0.0111538013167154,-0.0341934961088841,0.0790372681899744));
#89274=CARTESIAN_POINT('Ctrl Pts',(0.011026137408333,-0.0340223579322397,
0.0794013173780229));
#89275=CARTESIAN_POINT('Ctrl Pts',(0.0110985667709867,-0.0339125849573575,
0.0793612863299448));
#89276=CARTESIAN_POINT('Ctrl Pts',(0.0111701166886898,-0.0338030433565231,
0.0793197842917163));
#89277=CARTESIAN_POINT('Ctrl Pts',(0.0112407003659551,-0.0336938721132327,
0.0792768724485641));
#89278=CARTESIAN_POINT('Ctrl Pts',(0.0110508443436105,-0.0340223579322397,
0.0792907246694937));
#89279=CARTESIAN_POINT('Ctrl Pts',(0.0111217483443756,-0.0339125849573575,
0.0792503528483397));
#89280=CARTESIAN_POINT('Ctrl Pts',(0.0111917669188336,-0.0338030433565231,
0.0792085418479394));
#89281=CARTESIAN_POINT('Ctrl Pts',(0.0112608152648517,-0.0336938721132327,
0.0791653530750319));
#89282=CARTESIAN_POINT('Ctrl Pts',(0.0110755512788879,-0.0340223579322397,
0.0791801319609645));
#89283=CARTESIAN_POINT('Ctrl Pts',(0.0111449299177645,-0.0339125849573575,
0.0791394193667346));
#89284=CARTESIAN_POINT('Ctrl Pts',(0.0112134171489773,-0.0338030433565231,
0.0790972994041623));
#89285=CARTESIAN_POINT('Ctrl Pts',(0.0112809301637483,-0.0336938721132327,
0.0790538337014997));
#89286=CARTESIAN_POINT('Ctrl Pts',(0.0111002582141653,-0.0340223579322397,
0.0790695392524353));
#89287=CARTESIAN_POINT('Ctrl Pts',(0.0111681114911534,-0.0339125849573575,
0.0790284858851296));
#89288=CARTESIAN_POINT('Ctrl Pts',(0.011235067379121,-0.0338030433565231,
0.0789860569603853));
#89289=CARTESIAN_POINT('Ctrl Pts',(0.0113010450626449,-0.0336938721132327,
0.0789423143279675));
#89290=CARTESIAN_POINT('',(0.0112706926847908,-0.0336938721132427,0.0791105914931781));
#89291=CARTESIAN_POINT('Ctrl Pts',(0.0112297421614374,-0.0337108120662675,
0.0792835185415416));
#89292=CARTESIAN_POINT('Ctrl Pts',(0.0112074831667248,-0.0337611408993745,
0.0792467289617537));
#89293=CARTESIAN_POINT('Ctrl Pts',(0.0111856303492812,-0.0338121088780191,
0.0792106107101743));
#89294=CARTESIAN_POINT('Ctrl Pts',(0.011142717161275,-0.0339153382773236,
0.0791396839601347));
#89295=CARTESIAN_POINT('Ctrl Pts',(0.0111216749456874,-0.0339675558473115,
0.0791049054681465));
#89296=CARTESIAN_POINT('Ctrl Pts',(0.0111010304244729,-0.0340203938281304,
0.0790707842838698));
#89297=CARTESIAN_POINT('Ctrl Pts',(0.0112053060724886,-0.0341934961088741,
0.079004429814305));
#89298=CARTESIAN_POINT('Ctrl Pts',(0.011305667584522,-0.0340287516182428,
0.0789407217357598));
#89299=CARTESIAN_POINT('Ctrl Pts',(0.011403310236344,-0.0338644633275951,
0.078872920077117));
#89300=CARTESIAN_POINT('Ctrl Pts',(0.0112072754682234,-0.0341934961088741,
0.0790049144402679));
#89301=CARTESIAN_POINT('Ctrl Pts',(0.0113076469995168,-0.0340287516182428,
0.0789411656460174));
#89302=CARTESIAN_POINT('Ctrl Pts',(0.0114052979792265,-0.0338644633275951,
0.0788733228923564));
#89303=CARTESIAN_POINT('Ctrl Pts',(0.0115354146774924,-0.0341934961088741,
0.0790856624470942));
#89304=CARTESIAN_POINT('Ctrl Pts',(0.0116374556102127,-0.0340287516182428,
0.079015129633204));
#89305=CARTESIAN_POINT('Ctrl Pts',(0.0117364941761993,-0.0338644633275951,
0.0789404396590909));
#89306=CARTESIAN_POINT('',(0.011545949556832,-0.0341764758832445,0.0790783638791647));
#89307=CARTESIAN_POINT('',(0.0115354146774751,-0.034193496108874,0.0790856624470899));
#89308=CARTESIAN_POINT('Origin',(0.00252268601302544,-0.0345621026753412,
0.0651858463722302));
#89309=CARTESIAN_POINT('Ctrl Pts',(0.011545949555018,-0.0341764758837557,
0.0790783638793629));
#89310=CARTESIAN_POINT('Ctrl Pts',(0.0115214671429795,-0.0341260050040178,
0.0790431060617529));
#89311=CARTESIAN_POINT('Ctrl Pts',(0.0114974102616361,-0.0340749269147575,
0.0790084611299829));
#89312=CARTESIAN_POINT('Ctrl Pts',(0.011450129066672,-0.0339715436304948,
0.078940370083328));
#89313=CARTESIAN_POINT('Ctrl Pts',(0.0114269226954664,-0.0339192778237157,
0.0789069497973535));
#89314=CARTESIAN_POINT('Ctrl Pts',(0.0114041341077238,-0.0338664212855168,
0.0788741312782399));
#89315=CARTESIAN_POINT('',(0.0113713450728593,-0.0341934961088841,0.0790452884436889));
#89316=CARTESIAN_POINT('Origin',(0.00812378219310841,-0.0315241814719618,
0.07415));
#89317=CARTESIAN_POINT('',(0.0115459495571016,-0.0342105180190358,0.0790783638780777));
#89318=CARTESIAN_POINT('',(0.0115564688245398,-0.0341934961088739,0.079071042825499));
#89319=CARTESIAN_POINT('Origin',(0.00248272241089273,-0.0345621722253858,
0.0652072295348258));
#89320=CARTESIAN_POINT('Origin',(0.00168141573312356,-0.0345621027514389,
0.0657700090192215));
#89321=CARTESIAN_POINT('Origin',(0.00171541396284715,-0.0345621725656518,
0.0657400355638129));
#89322=CARTESIAN_POINT('Ctrl Pts',(0.0112994529044899,-0.0346945769586965,
0.078945166085276));
#89323=CARTESIAN_POINT('Ctrl Pts',(0.0113998895780257,-0.0345275153362944,
0.0788786503907569));
#89324=CARTESIAN_POINT('Ctrl Pts',(0.0114982603722607,-0.0343603235965185,
0.0788089588509352));
#89325=CARTESIAN_POINT('Ctrl Pts',(0.0115942774134824,-0.0341934961088739,
0.078736301906533));
#89326=CARTESIAN_POINT('Ctrl Pts',(0.0113683131029715,-0.0346945769586965,
0.0788973508001731));
#89327=CARTESIAN_POINT('Ctrl Pts',(0.0114677482662167,-0.0345275153362944,
0.0788293928012267));
#89328=CARTESIAN_POINT('Ctrl Pts',(0.0115650719319724,-0.0343603235965185,
0.0787582900805006));
#89329=CARTESIAN_POINT('Ctrl Pts',(0.0116599993854989,-0.0341934961088739,
0.0786842572063352));
#89330=CARTESIAN_POINT('Ctrl Pts',(0.0114371733014532,-0.0346945769586965,
0.0788495355150717));
#89331=CARTESIAN_POINT('Ctrl Pts',(0.0115356069544074,-0.0345275153362944,
0.078780135211697));
#89332=CARTESIAN_POINT('Ctrl Pts',(0.0116318834916838,-0.0343603235965185,
0.0787076213100663));
#89333=CARTESIAN_POINT('Ctrl Pts',(0.0117257213575149,-0.0341934961088739,
0.078632212506138));
#89334=CARTESIAN_POINT('Ctrl Pts',(0.0115060334999348,-0.0346945769586965,
0.0788017202299672));
#89335=CARTESIAN_POINT('Ctrl Pts',(0.0116034656425987,-0.0345275153362944,
0.0787308776221661));
#89336=CARTESIAN_POINT('Ctrl Pts',(0.0116986950513959,-0.0343603235965185,
0.0786569525396315));
#89337=CARTESIAN_POINT('Ctrl Pts',(0.0117914433295318,-0.0341934961088739,
0.0785801678059397));
#89338=CARTESIAN_POINT('',(0.0115060334985815,-0.0346945769586966,0.0788017202309067));
#89339=CARTESIAN_POINT('',(0.0116942917394192,-0.0343667727836579,0.07865883428183));
#89340=CARTESIAN_POINT('Origin',(0.00147091532982184,-0.0345626474181511,
0.0653112180668012));
#89341=CARTESIAN_POINT('Origin',(0.0185556194816323,-0.0341934771024039,
0.0873232926903192));
#89342=CARTESIAN_POINT('',(0.0115954533610552,-0.0341934961088739,0.0787353706831235));
#89343=CARTESIAN_POINT('',(0.0116444508528592,-0.0341934961088841,0.0786965699640951));
#89344=CARTESIAN_POINT('',(0.0114041341068758,-0.0345211942962608,0.0788741312769521));
#89345=CARTESIAN_POINT('Origin',(0.00186774519205461,-0.0345625596119161,
0.0650397137992776));
#89346=CARTESIAN_POINT('',(0.0114033592510911,-0.0346945769586886,0.0788730153843444));
#89347=CARTESIAN_POINT('Origin',(0.0177135881722783,-0.0346945685853921,
0.0879605632483003));
#89348=CARTESIAN_POINT('',(0.0114546963748463,-0.0346945769587026,0.0788373678076356));
#89349=CARTESIAN_POINT('Ctrl Pts',(0.011350144030904,-0.0345231616327842,
0.0792087141935167));
#89350=CARTESIAN_POINT('Ctrl Pts',(0.0114198712839617,-0.0344132092796988,
0.0791642433379369));
#89351=CARTESIAN_POINT('Ctrl Pts',(0.0114886750948442,-0.0343032738558979,
0.0791183325236193));
#89352=CARTESIAN_POINT('Ctrl Pts',(0.011556468824539,-0.0341934961088739,
0.0790710428255065));
#89353=CARTESIAN_POINT('Ctrl Pts',(0.0113678579909793,-0.0345231616327842,
0.079096788540705));
#89354=CARTESIAN_POINT('Ctrl Pts',(0.0114360425064917,-0.0344132092796988,
0.0790520735231247));
#89355=CARTESIAN_POINT('Ctrl Pts',(0.0115032986091287,-0.0343032738558979,
0.0790059504697136));
#89356=CARTESIAN_POINT('Ctrl Pts',(0.0115695416496358,-0.0341934961088739,
0.078958480676527));
#89357=CARTESIAN_POINT('Ctrl Pts',(0.0113855719510546,-0.0345231616327842,
0.0789848628878932));
#89358=CARTESIAN_POINT('Ctrl Pts',(0.0114522137290217,-0.0344132092796988,
0.0789399037083125));
#89359=CARTESIAN_POINT('Ctrl Pts',(0.0115179221234131,-0.0343032738558979,
0.078893568415808));
#89360=CARTESIAN_POINT('Ctrl Pts',(0.0115826144747325,-0.0341934961088739,
0.0788459185275475));
#89361=CARTESIAN_POINT('Ctrl Pts',(0.0114032859111299,-0.0345231616327842,
0.0788729372350814));
#89362=CARTESIAN_POINT('Ctrl Pts',(0.0114683849515517,-0.0344132092796988,
0.0788277338935004));
#89363=CARTESIAN_POINT('Ctrl Pts',(0.0115325456376976,-0.0343032738558979,
0.0787811863619023));
#89364=CARTESIAN_POINT('Ctrl Pts',(0.0115956872998293,-0.0341934961088739,
0.0787333563785681));
#89365=CARTESIAN_POINT('',(0.0115759610928075,-0.0341934961088839,0.0789032067543212));
#89366=CARTESIAN_POINT('Ctrl Pts',(0.0115459495551251,-0.0342105180195371,
0.0790783638752337));
#89367=CARTESIAN_POINT('Ctrl Pts',(0.0115214396314411,-0.0342610556240559,
0.079043066413219));
#89368=CARTESIAN_POINT('Ctrl Pts',(0.0114973695256638,-0.0343122189868635,
0.0790084023459081));
#89369=CARTESIAN_POINT('Ctrl Pts',(0.0114500878504123,-0.0344158119695081,
0.0789403106146687));
#89370=CARTESIAN_POINT('Ctrl Pts',(0.0114268956195889,-0.0344681990449949,
0.0789069108009003));
#89371=CARTESIAN_POINT('Ctrl Pts',(0.0114041341068571,-0.0345211942962355,
0.0788741312769241));
#89372=CARTESIAN_POINT('Ctrl Pts',(0.0115040380481517,-0.0346945769586932,
0.0788013603088443));
#89373=CARTESIAN_POINT('Ctrl Pts',(0.0116002016312185,-0.0345296777079064,
0.0787314759109219));
#89374=CARTESIAN_POINT('Ctrl Pts',(0.0116933946573247,-0.0343648066255587,
0.0786576766990943));
#89375=CARTESIAN_POINT('Ctrl Pts',(0.0115060334985741,-0.0346945769586932,
0.0788017202309119));
#89376=CARTESIAN_POINT('Ctrl Pts',(0.011602204522775,-0.0345296777079064,
0.078731794578464));
#89377=CARTESIAN_POINT('Ctrl Pts',(0.0116954032785695,-0.0343648066255587,
0.0786579538398135));
#89378=CARTESIAN_POINT('Ctrl Pts',(0.0118385954093691,-0.0346945769586932,
0.0788617048685642));
#89379=CARTESIAN_POINT('Ctrl Pts',(0.0119360065735081,-0.0345296777079064,
0.0787849037339326));
#89380=CARTESIAN_POINT('Ctrl Pts',(0.0120301602395604,-0.0343648066255587,
0.0787041421319887));
#89381=CARTESIAN_POINT('',(0.0118486512198862,-0.034677539666503,0.0788537592122609));
#89382=CARTESIAN_POINT('',(0.0118385954093546,-0.0346945769586886,0.078861704868559));
#89383=CARTESIAN_POINT('Origin',(0.00142290311163744,-0.0345626617986891,
0.065934135429138));
#89384=CARTESIAN_POINT('Ctrl Pts',(0.0118486512180685,-0.0346775396670096,
0.0788537592124665));
#89385=CARTESIAN_POINT('Ctrl Pts',(0.0118219822728979,-0.0346269749928757,
0.0788200817278928));
#89386=CARTESIAN_POINT('Ctrl Pts',(0.0117957872662314,-0.0345757902891947,
0.0787870027896662));
#89387=CARTESIAN_POINT('Ctrl Pts',(0.0117443236918964,-0.0344721681090353,
0.0787220146564573));
#89388=CARTESIAN_POINT('Ctrl Pts',(0.0117190753047894,-0.0344197714292724,
0.0786901309363811));
#89389=CARTESIAN_POINT('Ctrl Pts',(0.0116942917391319,-0.03436677278343,
0.0786588342824434));
#89390=CARTESIAN_POINT('',(0.011672314453978,-0.0346945769587026,0.0788317125497428));
#89391=CARTESIAN_POINT('Origin',(0.00812378219310841,-0.0315241814719618,
0.07415));
#89392=CARTESIAN_POINT('',(0.0118486512197319,-0.0347116136489784,0.0788537592108763));
#89393=CARTESIAN_POINT('',(0.0118586900372345,-0.0346945769586885,0.0788457920946193));
#89394=CARTESIAN_POINT('Origin',(0.00138857391637728,-0.0345626704533082,
0.0659637084523159));
#89395=CARTESIAN_POINT('Origin',(0.00166235086465093,-0.0345626619289644,
0.0657445183313168));
#89396=CARTESIAN_POINT('Origin',(0.00169900477058736,-0.0345626705785499,
0.0657178809380879));
#89397=CARTESIAN_POINT('Ctrl Pts',(0.0115646152496605,-0.0352450361874068,
0.0787586256630979));
#89398=CARTESIAN_POINT('Ctrl Pts',(0.0117384324187514,-0.0349452760959493,
0.0786288525148916));
#89399=CARTESIAN_POINT('Ctrl Pts',(0.0119019807470506,-0.034644428984174,
0.078486355418161));
#89400=CARTESIAN_POINT('Ctrl Pts',(0.011566604548178,-0.0352450361874068,
0.0787570705694002));
#89401=CARTESIAN_POINT('Ctrl Pts',(0.0117403630659476,-0.0349452760959493,
0.0786272223935692));
#89402=CARTESIAN_POINT('Ctrl Pts',(0.0119038472581602,-0.034644428984174,
0.078484654900217));
#89403=CARTESIAN_POINT('Ctrl Pts',(0.0117635647974338,-0.0352450361874068,
0.0786031008963699));
#89404=CARTESIAN_POINT('Ctrl Pts',(0.0119315162536957,-0.0349452760959493,
0.0784658242428426));
#89405=CARTESIAN_POINT('Ctrl Pts',(0.012088650338316,-0.034644428984174,
0.0783162867869505));
#89406=CARTESIAN_POINT('Ctrl Pts',(0.0117655343999264,-0.0352450361874068,
0.0786015611996396));
#89407=CARTESIAN_POINT('Ctrl Pts',(0.0119334277855732,-0.0349452760959493,
0.0784642102613353));
#89408=CARTESIAN_POINT('Ctrl Pts',(0.0120904983691176,-0.034644428984174,
0.0783146031058178));
#89409=CARTESIAN_POINT('',(0.0117914199164955,-0.0351951634053338,0.0785801902704607));
#89410=CARTESIAN_POINT('',(0.0119703582009633,-0.0348678972925388,0.0784257429782198));
#89411=CARTESIAN_POINT('Origin',(0.000454706872257089,-0.0345636767878005,
0.066256090558175));
#89412=CARTESIAN_POINT('Origin',(0.0193606208052998,-0.0346946199340733,
0.0866405471726442));
#89413=CARTESIAN_POINT('',(0.0118765206047234,-0.0346945769330289,0.0785083344768662));
#89414=CARTESIAN_POINT('',(0.0119229851005596,-0.0346945769458128,0.0784665337386631));
#89415=CARTESIAN_POINT('',(0.0116942917388866,-0.0350221583435276,0.0786588342821075));
#89416=CARTESIAN_POINT('Origin',(0.000783051344888556,-0.0345628458717962,
0.0659049021452045));
#89417=CARTESIAN_POINT('',(0.0116935214955351,-0.0351951360298762,0.0786578664918798));
#89418=CARTESIAN_POINT('Origin',(0.0185342304354016,-0.0351951838366766,
0.0872963006705578));
#89419=CARTESIAN_POINT('',(0.0117914433283039,-0.0351951371328746,0.0785801678070603));
#89420=CARTESIAN_POINT('Ctrl Pts',(0.0116614176111308,-0.0350241211494343,
0.0789961464741824));
#89421=CARTESIAN_POINT('Ctrl Pts',(0.0117281712918152,-0.0349144232818962,
0.0789474169967862));
#89422=CARTESIAN_POINT('Ctrl Pts',(0.0117939576546772,-0.0348045283579413,
0.0788972785061695));
#89423=CARTESIAN_POINT('Ctrl Pts',(0.0118586900459313,-0.0346945769439158,
0.0788457920877099));
#89424=CARTESIAN_POINT('Ctrl Pts',(0.0116720687311486,-0.0350241211494343,
0.078883329385735));
#89425=CARTESIAN_POINT('Ctrl Pts',(0.0117372684026965,-0.0349144232818962,
0.0788344531935276));
#89426=CARTESIAN_POINT('Ctrl Pts',(0.0118014967935725,-0.0348045283579413,
0.0787842000227632));
#89427=CARTESIAN_POINT('Ctrl Pts',(0.0118646692400894,-0.0346945769439158,
0.0787326311799696));
#89428=CARTESIAN_POINT('Ctrl Pts',(0.0116827198511664,-0.0350241211494343,
0.0787705122972876));
#89429=CARTESIAN_POINT('Ctrl Pts',(0.0117463655135778,-0.0349144232818962,
0.0787214893902691));
#89430=CARTESIAN_POINT('Ctrl Pts',(0.0118090359324679,-0.0348045283579413,
0.078671121539357));
#89431=CARTESIAN_POINT('Ctrl Pts',(0.0118706484342475,-0.0346945769439158,
0.0786194702722293));
#89432=CARTESIAN_POINT('Ctrl Pts',(0.0116933709711842,-0.0350241211494343,
0.0786576952088402));
#89433=CARTESIAN_POINT('Ctrl Pts',(0.011755462624459,-0.0349144232818962,
0.0786085255870105));
#89434=CARTESIAN_POINT('Ctrl Pts',(0.0118165750713632,-0.0348045283579413,
0.0785580430559507));
#89435=CARTESIAN_POINT('Ctrl Pts',(0.0118766276284056,-0.0346945769439158,
0.078506309364489));
#89436=CARTESIAN_POINT('',(0.0118676053208166,-0.0346945769458128,0.0786770632860016));
#89437=CARTESIAN_POINT('Ctrl Pts',(0.0118486512176845,-0.0347116136492773,
0.0788537592082923));
#89438=CARTESIAN_POINT('Ctrl Pts',(0.0118219928734454,-0.0347621546531506,
0.0788200950898051));
#89439=CARTESIAN_POINT('Ctrl Pts',(0.0117958032549355,-0.0348133084095404,
0.0787870228774897));
#89440=CARTESIAN_POINT('Ctrl Pts',(0.011744339612196,-0.0349168561544569,
0.0787220346639899));
#89441=CARTESIAN_POINT('Ctrl Pts',(0.0117190860011002,-0.0349692089015928,
0.0786901444404812));
#89442=CARTESIAN_POINT('Ctrl Pts',(0.0116942917388795,-0.0350221583435,
0.0786588342820665));
#89443=CARTESIAN_POINT('Ctrl Pts',(0.0117899900789448,-0.0351951371254965,
0.0785799990284488));
#89444=CARTESIAN_POINT('Ctrl Pts',(0.0118815775293839,-0.0350307338980967,
0.0785042024806646));
#89445=CARTESIAN_POINT('Ctrl Pts',(0.0119699539657781,-0.0348659306897824,
0.0784246852924333));
#89446=CARTESIAN_POINT('Ctrl Pts',(0.0117914433282243,-0.0351951371254965,
0.0785801678069754));
#89447=CARTESIAN_POINT('Ctrl Pts',(0.0118830342680536,-0.0350307338980967,
0.0785043412141741));
#89448=CARTESIAN_POINT('Ctrl Pts',(0.0119714129490632,-0.0348659306897824,
0.0784247938623788));
#89449=CARTESIAN_POINT('Ctrl Pts',(0.0120350094220996,-0.0351951371254965,
0.0786084552639372));
#89450=CARTESIAN_POINT('Ctrl Pts',(0.0121271851873534,-0.0350307338980967,
0.0785275930949634));
#89451=CARTESIAN_POINT('Ctrl Pts',(0.012215940068261,-0.0348659306897824,
0.0784429902984002));
#89452=CARTESIAN_POINT('Origin',(0.0155272204812442,-0.030860919741085,
0.0823794485306077));
#89453=CARTESIAN_POINT('',(0.0118976326534671,-0.0351951371254965,0.0785925005004132));
#89454=CARTESIAN_POINT('Origin',(0.00737192514890434,-0.0351840467441131,
0.0735259353918352));
#89455=CARTESIAN_POINT('Origin',(0.0166993788085855,-0.0352322614023337,
0.0824941719226236));
#89456=CARTESIAN_POINT('',(0.0121429837173709,-0.0351951142564686,0.0782638587349102));
#89457=CARTESIAN_POINT('',(0.0122302737948824,-0.0351951372916788,0.0781748262974395));
#89458=CARTESIAN_POINT('Origin',(0.00819929833909993,-0.0352875122865233,
0.0738178766097156));
#89459=CARTESIAN_POINT('Origin',(0.00194310532157468,-0.0298325076522745,
0.0784037540701524));
#89460=CARTESIAN_POINT('Origin',(0.0114610257463966,-0.0338732494652423,
0.0818384554366706));
#89461=CARTESIAN_POINT('Origin',(0.00812378219310841,-0.0315241814719618,
0.07415));
#89462=CARTESIAN_POINT('',(0.00949138119084906,-0.0322104233323586,0.0799920606778519));
#89463=CARTESIAN_POINT('',(0.00950385681755529,-0.0321934096636184,0.0799891261359044));
#89464=CARTESIAN_POINT('Origin',(0.00627440703209637,-0.0326387220729212,
0.0637552752997748));
#89465=CARTESIAN_POINT('',(0.00949138119076482,-0.0321763980308521,0.0799920606774919));
#89466=CARTESIAN_POINT('Origin',(0.00512484983222103,-0.0326386251608966,
0.0640308694007681));
#89467=CARTESIAN_POINT('',(0.00947889932502759,-0.0321934096636185,0.0799949685678179));
#89468=CARTESIAN_POINT('Origin',(0.00631955989060436,-0.0326386231321022,
0.0637511974334642));
#89469=CARTESIAN_POINT('Origin',(0.00516712361018345,-0.0326387236420496,
0.0640144901082834));
#89470=CARTESIAN_POINT('Origin',(0.00812378219310841,-0.0315241814719618,
0.07415));
#89471=CARTESIAN_POINT('',(0.00985550857164737,-0.0327114338380051,0.0798946604538155));
#89472=CARTESIAN_POINT('',(0.0098677753192046,-0.0326943950436593,0.079890948351634));
#89473=CARTESIAN_POINT('Origin',(0.00497166242930612,-0.032639568603193,
0.0640244963981889));
#89474=CARTESIAN_POINT('',(0.00985550857166181,-0.0326773559991423,0.0798946604538637));
#89475=CARTESIAN_POINT('Origin',(0.00511101403725754,-0.0326395686209864,
0.0639816718949373));
#89476=CARTESIAN_POINT('',(0.00984323392392406,-0.0326943950436595,0.0798983463487712));
#89477=CARTESIAN_POINT('Origin',(0.00501481363260089,-0.0326395701950183,
0.0640106676017419));
#89478=CARTESIAN_POINT('Origin',(0.00515461686738233,-0.0326395670478704,
0.0639693413694236));
#89479=CARTESIAN_POINT('Origin',(0.00812378219310841,-0.0315241814719618,
0.07415));
#89480=CARTESIAN_POINT('',(0.0105618502624782,-0.0337108120655393,0.0796323192239842));
#89481=CARTESIAN_POINT('',(0.0105735550331356,-0.0336938721132327,0.0796270989613361));
#89482=CARTESIAN_POINT('Origin',(0.00493473930959288,-0.0345562527080821,
0.0642286235176398));
#89483=CARTESIAN_POINT('',(0.0105618502629987,-0.0336769361243754,0.079632319225162));
#89484=CARTESIAN_POINT('Ctrl Pts',(0.0105735550331346,-0.0336938721132368,
0.0796270989613472));
#89485=CARTESIAN_POINT('Ctrl Pts',(0.0105716052984816,-0.0336910493047713,
0.0796279710301252));
#89486=CARTESIAN_POINT('Ctrl Pts',(0.0105696550489526,-0.0336882265901734,
0.0796288420798184));
#89487=CARTESIAN_POINT('Ctrl Pts',(0.0105657534663952,-0.0336825812712632,
0.0796305821646085));
#89488=CARTESIAN_POINT('Ctrl Pts',(0.0105638021333898,-0.033679758666992,
0.0796314511996638));
#89489=CARTESIAN_POINT('Ctrl Pts',(0.0105618502629988,-0.0336769361243754,
0.079632319225162));
#89490=CARTESIAN_POINT('',(0.0105501343689866,-0.0336938721132327,0.0796375144754808));
#89491=CARTESIAN_POINT('Ctrl Pts',(0.0105618502629987,-0.0336769361243754,
0.079632319225162));
#89492=CARTESIAN_POINT('Ctrl Pts',(0.0105598983926042,-0.0336797586669971,
0.0796331872506618));
#89493=CARTESIAN_POINT('Ctrl Pts',(0.0105579461324662,-0.0336825812712733,
0.0796340542009459));
#89494=CARTESIAN_POINT('Ctrl Pts',(0.0105540408446128,-0.0336882265861437,
0.0796357859463635));
#89495=CARTESIAN_POINT('Ctrl Pts',(0.0105520878169393,-0.0336910492967122,
0.0796366507415207));
#89496=CARTESIAN_POINT('Ctrl Pts',(0.0105501343689991,-0.0336938721132385,
0.0796375144754901));
#89497=CARTESIAN_POINT('Origin',(0.0028923809378903,-0.0345562523741628,
0.0651368906056583));
#89498=CARTESIAN_POINT('Origin',(0.00812378219310841,-0.0315241814719618,
0.07415));
#89499=CARTESIAN_POINT('',(0.0102128016195588,-0.0332121607144412,0.0797745886794734));
#89500=CARTESIAN_POINT('',(0.0102248110767375,-0.0331951640388587,0.0797701136670142));
#89501=CARTESIAN_POINT('Origin',(0.00375874516735174,-0.0326413667221338,
0.0645713542574781));
#89502=CARTESIAN_POINT('',(0.01021280161972,-0.0331781648279234,0.0797745886799076));
#89503=CARTESIAN_POINT('Origin',(0.0051332813547961,-0.0326412094385113,
0.064052471445194));
#89504=CARTESIAN_POINT('',(0.0102007826323748,-0.0331951640388588,0.0797790380328514));
#89505=CARTESIAN_POINT('Origin',(0.00379788014756742,-0.032641209245444,
0.0645484511901365));
#89506=CARTESIAN_POINT('Origin',(0.00517787917726456,-0.0326413669324096,
0.0640442768962168));
#89507=CARTESIAN_POINT('Ctrl Pts',(0.00962885585002558,-0.0332451089994433,
0.0797009349020912));
#89508=CARTESIAN_POINT('Ctrl Pts',(0.00983821278511685,-0.0329451141710254,
0.0796441701204001));
#89509=CARTESIAN_POINT('Ctrl Pts',(0.0100426992038379,-0.0326442513127493,
0.0795717969812538));
#89510=CARTESIAN_POINT('Ctrl Pts',(0.00986866494954309,-0.0332451089994433,
0.079630283675714));
#89511=CARTESIAN_POINT('Ctrl Pts',(0.0100753572300355,-0.0329451141710254,
0.079564474345858));
#89512=CARTESIAN_POINT('Ctrl Pts',(0.010276505291818,-0.0326442513127493,
0.0794832830658313));
#89513=CARTESIAN_POINT('',(0.00990303373249483,-0.0331951640388616,0.079619221970225));
#89514=CARTESIAN_POINT('',(0.0101262321451419,-0.0328677532092642,0.0795415043531098));
#89515=CARTESIAN_POINT('Origin',(0.00399190653859828,-0.0326401908899454,
0.0639319461867883));
#89516=CARTESIAN_POINT('Origin',(0.0139755840460193,-0.0326944279134342,
0.0899057054876056));
#89517=CARTESIAN_POINT('',(0.0100085802132244,-0.0326943950436593,0.0795837520575904));
#89518=CARTESIAN_POINT('',(0.010067169678664,-0.0326943950436694,0.079561991438568));
#89519=CARTESIAN_POINT('',(0.00978374540819871,-0.0330220786163545,0.0796566003236614));
#89520=CARTESIAN_POINT('Origin',(0.00443082058661673,-0.0326396682764334,
0.0637354078735713));
#89521=CARTESIAN_POINT('',(0.00978335330633811,-0.0331951640388587,0.0796552996031219));
#89522=CARTESIAN_POINT('Origin',(0.0129673198884641,-0.0331952026560064,
0.090217483389793));
#89523=CARTESIAN_POINT('',(0.00984319351942647,-0.0331951640388701,0.0796372607866835));
#89524=CARTESIAN_POINT('Ctrl Pts',(0.00962900677436569,-0.0330240426238172,
0.0799581235317457));
#89525=CARTESIAN_POINT('Ctrl Pts',(0.00970901933459606,-0.032914277406352,
0.0799373875966696));
#89526=CARTESIAN_POINT('Ctrl Pts',(0.0097886431143048,-0.0328043479726691,
0.0799149872408496));
#89527=CARTESIAN_POINT('Ctrl Pts',(0.00986777531920278,-0.0326943950436593,
0.079890948351638));
#89528=CARTESIAN_POINT('Ctrl Pts',(0.00968044066635957,-0.0330240426238172,
0.0798571498186368));
#89529=CARTESIAN_POINT('Ctrl Pts',(0.00975906221531795,-0.032914277406352,
0.079835705331589));
#89530=CARTESIAN_POINT('Ctrl Pts',(0.00983727964253634,-0.0328043479726691,
0.0798126248266467));
#89531=CARTESIAN_POINT('Ctrl Pts',(0.00991499193137186,-0.0326943950436593,
0.079787935112101));
#89532=CARTESIAN_POINT('Ctrl Pts',(0.00973187455835346,-0.0330240426238172,
0.079756176105528));
#89533=CARTESIAN_POINT('Ctrl Pts',(0.00980910509603984,-0.032914277406352,
0.0797340230665083));
#89534=CARTESIAN_POINT('Ctrl Pts',(0.00988591617076787,-0.0328043479726691,
0.0797102624124438));
#89535=CARTESIAN_POINT('Ctrl Pts',(0.00996220854354094,-0.0326943950436593,
0.079684921872564));
#89536=CARTESIAN_POINT('Ctrl Pts',(0.00978330845034735,-0.0330240426238172,
0.0796552023924192));
#89537=CARTESIAN_POINT('Ctrl Pts',(0.00985914797676173,-0.032914277406352,
0.0796323408014276));
#89538=CARTESIAN_POINT('Ctrl Pts',(0.00993455269899941,-0.0328043479726691,
0.0796078999982409));
#89539=CARTESIAN_POINT('Ctrl Pts',(0.01000942515571,-0.0326943950436593,
0.0795819086330271));
#89540=CARTESIAN_POINT('',(0.00993817776622448,-0.0326943950436694,0.0797373502046222));
#89541=CARTESIAN_POINT('Ctrl Pts',(0.00985550857068446,-0.0327114338383326,
0.0798946604506341));
#89542=CARTESIAN_POINT('Ctrl Pts',(0.00984311336766662,-0.0327619876830619,
0.0798535418111791));
#89543=CARTESIAN_POINT('Ctrl Pts',(0.00983093684236038,-0.0328131562603596,
0.0798131485918699));
#89544=CARTESIAN_POINT('Ctrl Pts',(0.00980701090072301,-0.0329167375858771,
0.0797337790029739));
#89545=CARTESIAN_POINT('Ctrl Pts',(0.00979527101774495,-0.0329691088920623,
0.0796948342584043));
#89546=CARTESIAN_POINT('Ctrl Pts',(0.00978374540818771,-0.0330220786163186,
0.0796566003236151));
#89547=CARTESIAN_POINT('Ctrl Pts',(0.00990124681263013,-0.0331951640388604,
0.0796182628449475));
#89548=CARTESIAN_POINT('Ctrl Pts',(0.00997656107988286,-0.0330855618127442,
0.0795937818627447));
#89549=CARTESIAN_POINT('Ctrl Pts',(0.0100514236600299,-0.032975722417194,
0.0795677266151953));
#89550=CARTESIAN_POINT('Ctrl Pts',(0.0101257370503822,-0.0328657861694598,
0.079540125765186));
#89551=CARTESIAN_POINT('Ctrl Pts',(0.0100010920858834,-0.0331951640388604,
0.0796718545742519));
#89552=CARTESIAN_POINT('Ctrl Pts',(0.0100771444708781,-0.0330855618127442,
0.0796459984252353));
#89553=CARTESIAN_POINT('Ctrl Pts',(0.0101527172785152,-0.032975722417194,
0.0796185517638996));
#89554=CARTESIAN_POINT('Ctrl Pts',(0.010227712009216,-0.0328657861694598,
0.0795895449903085));
#89555=CARTESIAN_POINT('Ctrl Pts',(0.0101009373591368,-0.0331951640388604,
0.0797254463035562));
#89556=CARTESIAN_POINT('Ctrl Pts',(0.0101777278618733,-0.0330855618127442,
0.0796982149877258));
#89557=CARTESIAN_POINT('Ctrl Pts',(0.0102540108970005,-0.032975722417194,
0.0796693769126038));
#89558=CARTESIAN_POINT('Ctrl Pts',(0.0103296869680498,-0.0328657861694598,
0.079638964215431));
#89559=CARTESIAN_POINT('Ctrl Pts',(0.0102007826323901,-0.0331951640388604,
0.0797790380328606));
#89560=CARTESIAN_POINT('Ctrl Pts',(0.0102783112528686,-0.0330855618127442,
0.0797504315502163));
#89561=CARTESIAN_POINT('Ctrl Pts',(0.0103553045154857,-0.032975722417194,
0.0797202020613081));
#89562=CARTESIAN_POINT('Ctrl Pts',(0.0104316619268837,-0.0328657861694598,
0.0796883834405535));
#89563=CARTESIAN_POINT('Ctrl Pts',(0.010212801618493,-0.0331781648273467,
0.0797745886766133));
#89564=CARTESIAN_POINT('Ctrl Pts',(0.0101978361863283,-0.0331276810208849,
0.079734294939144));
#89565=CARTESIAN_POINT('Ctrl Pts',(0.0101831410958168,-0.0330765665171798,
0.0796947290841366));
#89566=CARTESIAN_POINT('Ctrl Pts',(0.0101542785143168,-0.032973061271521,
0.0796170179115595));
#89567=CARTESIAN_POINT('Ctrl Pts',(0.0101401229734508,-0.0329207135598918,
0.0795789047691451));
#89568=CARTESIAN_POINT('Ctrl Pts',(0.010126232145126,-0.0328677532092985,
0.0795415043530671));
#89569=CARTESIAN_POINT('',(0.0100519081824448,-0.0331951640388701,0.0796991300015482));
#89570=CARTESIAN_POINT('Ctrl Pts',(0.00997206329393836,-0.0337436976235975,
0.0795963394332629));
#89571=CARTESIAN_POINT('Ctrl Pts',(0.0100210484962165,-0.0336723290703325,
0.0795797157129274));
#89572=CARTESIAN_POINT('Ctrl Pts',(0.010069726765511,-0.033601104548885,
0.0795622135925272));
#89573=CARTESIAN_POINT('Ctrl Pts',(0.0102251468367468,-0.0333736987606857,
0.0795063327890642));
#89574=CARTESIAN_POINT('Ctrl Pts',(0.0103771040252922,-0.0331450831799192,
0.0794416251729128));
#89575=CARTESIAN_POINT('Ctrl Pts',(0.00997441229367598,-0.0337436976235975,
0.0795954837462684));
#89576=CARTESIAN_POINT('Ctrl Pts',(0.0100233897997755,-0.0336723290703325,
0.0795788388986732));
#89577=CARTESIAN_POINT('Ctrl Pts',(0.0100720599941239,-0.033601104548885,
0.0795613157928613));
#89578=CARTESIAN_POINT('Ctrl Pts',(0.0102274542836558,-0.0333736987606857,
0.0795053679871355));
#89579=CARTESIAN_POINT('Ctrl Pts',(0.0103793818880073,-0.0331450831799192,
0.0794405949586385));
#89580=CARTESIAN_POINT('Ctrl Pts',(0.0102093122674387,-0.0337436976235975,
0.0795099150468142));
#89581=CARTESIAN_POINT('Ctrl Pts',(0.0102575201556871,-0.0336723290703325,
0.0794911574732549));
#89582=CARTESIAN_POINT('Ctrl Pts',(0.0103053828554093,-0.033601104548885,
0.0794715358262675));
#89583=CARTESIAN_POINT('Ctrl Pts',(0.0104581989745559,-0.0333736987606857,
0.0794088877942661));
#89584=CARTESIAN_POINT('Ctrl Pts',(0.010607168159526,-0.0331450831799192,
0.0793375735312187));
#89585=CARTESIAN_POINT('Ctrl Pts',(0.0102116847571737,-0.0337436976235975,
0.0795090508029497));
#89586=CARTESIAN_POINT('Ctrl Pts',(0.0102598848722818,-0.0336723290703325,
0.0794902718908582));
#89587=CARTESIAN_POINT('Ctrl Pts',(0.0103077394163083,-0.033601104548885,
0.0794706290486049));
#89588=CARTESIAN_POINT('Ctrl Pts',(0.010460529495934,-0.0333736987606857,
0.0794079133443181));
#89589=CARTESIAN_POINT('Ctrl Pts',(0.0106094688008683,-0.0331450831799192,
0.0793365330148017));
#89590=CARTESIAN_POINT('',(0.0102429380749578,-0.0336938721132548,0.0794967095814551));
#89591=CARTESIAN_POINT('',(0.0104608161336227,-0.0333679869945434,0.0794051305750701));
#89592=CARTESIAN_POINT('Ctrl Pts',(0.0102429380749636,-0.033693872113265,
0.0794967095814539));
#89593=CARTESIAN_POINT('Ctrl Pts',(0.0102638087906459,-0.0336629187933933,
0.0794884375219329));
#89594=CARTESIAN_POINT('Ctrl Pts',(0.0102846243951419,-0.0336319952301041,
0.0794800459015819));
#89595=CARTESIAN_POINT('Ctrl Pts',(0.0103053828554147,-0.0336011045488951,
0.0794715358262656));
#89596=CARTESIAN_POINT('Ctrl Pts',(0.0103574729353847,-0.0335235892595454,
0.0794501811353131));
#89597=CARTESIAN_POINT('Ctrl Pts',(0.0104092956921413,-0.033445866866037,
0.079428042474058));
#89598=CARTESIAN_POINT('Ctrl Pts',(0.0104608161337401,-0.0333679869945386,
0.0794051305753502));
#89599=CARTESIAN_POINT('Ctrl Pts',(0.0104608570463099,-0.0333679692459114,
0.0794051131331372));
#89600=CARTESIAN_POINT('Ctrl Pts',(0.0104606674692765,-0.0333391895373239,
0.0794047014313379));
#89601=CARTESIAN_POINT('Ctrl Pts',(0.0104605224225366,-0.0333104081058199,
0.0794043941989144));
#89602=CARTESIAN_POINT('Ctrl Pts',(0.0104603254318856,-0.0332532732632664,
0.0794039899131119));
#89603=CARTESIAN_POINT('Ctrl Pts',(0.0104602721166528,-0.0332249238958137,
0.0794038897693094));
#89604=CARTESIAN_POINT('Ctrl Pts',(0.0104602643111526,-0.0331961055014437,
0.0794038891936719));
#89605=CARTESIAN_POINT('Ctrl Pts',(0.0104602641958236,-0.0331956347265782,
0.0794038892119066));
#89606=CARTESIAN_POINT('Ctrl Pts',(0.0104602640934209,-0.0331951640388588,
0.0794038892574465));
#89607=CARTESIAN_POINT('',(0.0103460491095624,-0.0331951640388587,0.0794546823422364));
#89608=CARTESIAN_POINT('',(0.0104031566015012,-0.0331951640388687,0.0794292857998518));
#89609=CARTESIAN_POINT('',(0.0101262321448569,-0.0335216366567647,0.0795415043528045));
#89610=CARTESIAN_POINT('Origin',(0.00320780802711184,-0.0326434571527953,
0.0643920465162114));
#89611=CARTESIAN_POINT('',(0.0101257591440837,-0.0336938721132327,0.0795402308195257));
#89612=CARTESIAN_POINT('Origin',(0.0139279719481104,-0.0336938867896106,
0.0897775159923261));
#89613=CARTESIAN_POINT('',(0.0101843486095307,-0.0336938721132538,0.0795184702005004));
#89614=CARTESIAN_POINT('Ctrl Pts',(0.00999073256489598,-0.0335235895815172,
0.0798521483941871));
#89615=CARTESIAN_POINT('Ctrl Pts',(0.0100692338640391,-0.0334144449262749,
0.0798264461466324));
#89616=CARTESIAN_POINT('Ctrl Pts',(0.0101472943625728,-0.0333049234473147,
0.0797990925925477));
#89617=CARTESIAN_POINT('Ctrl Pts',(0.0102248110767357,-0.0331951640388587,
0.0797701136670188));
#89618=CARTESIAN_POINT('Ctrl Pts',(0.010035724819235,-0.0335235895815172,
0.0797481442138115));
#89619=CARTESIAN_POINT('Ctrl Pts',(0.0101127942960698,-0.0334144449262749,
0.0797218225592942));
#89620=CARTESIAN_POINT('Ctrl Pts',(0.0101894085308233,-0.0333049234473147,
0.0796938784669947));
#89621=CARTESIAN_POINT('Ctrl Pts',(0.0102654663206594,-0.0331951640388587,
0.0796643387946359));
#89622=CARTESIAN_POINT('Ctrl Pts',(0.010080717073574,-0.0335235895815172,
0.0796441400334359));
#89623=CARTESIAN_POINT('Ctrl Pts',(0.0101563547281006,-0.0334144449262749,
0.079617198971956));
#89624=CARTESIAN_POINT('Ctrl Pts',(0.0102315226990737,-0.0333049234473147,
0.0795886643414417));
#89625=CARTESIAN_POINT('Ctrl Pts',(0.0103061215645831,-0.0331951640388587,
0.0795585639222531));
#89626=CARTESIAN_POINT('Ctrl Pts',(0.0101257093279131,-0.0335235895815172,
0.0795401358530602));
#89627=CARTESIAN_POINT('Ctrl Pts',(0.0101999151601314,-0.0334144449262749,
0.0795125753846178));
#89628=CARTESIAN_POINT('Ctrl Pts',(0.0102736368673242,-0.0333049234473147,
0.0794834502158887));
#89629=CARTESIAN_POINT('Ctrl Pts',(0.0103467768085067,-0.0331951640388587,
0.0794527890498702));
#89630=CARTESIAN_POINT('',(0.0102854300931599,-0.0331951640388687,0.0796123980046354));
#89631=CARTESIAN_POINT('Ctrl Pts',(0.0102128016184622,-0.0332121607145974,
0.0797745886765301));
#89632=CARTESIAN_POINT('Ctrl Pts',(0.0101978614059338,-0.0332625444109337,
0.0797343628417714));
#89633=CARTESIAN_POINT('Ctrl Pts',(0.0101831786367119,-0.033313530074597,
0.079694830161269));
#89634=CARTESIAN_POINT('Ctrl Pts',(0.0101543163298441,-0.0334167203140542,
0.0796171197281268));
#89635=CARTESIAN_POINT('Ctrl Pts',(0.0101401479708421,-0.0334688847587215,
0.079578972073471));
#89636=CARTESIAN_POINT('Ctrl Pts',(0.0101262321447603,-0.0335216366562264,
0.0795415043520825));
#89637=CARTESIAN_POINT('Ctrl Pts',(0.0102420291471262,-0.033693872113239,
0.0794962929700426));
#89638=CARTESIAN_POINT('Ctrl Pts',(0.010273322773968,-0.0336474569764958,
0.0794838941677118));
#89639=CARTESIAN_POINT('Ctrl Pts',(0.0103044691129145,-0.033601104548885,
0.0794711298835416));
#89640=CARTESIAN_POINT('Ctrl Pts',(0.0103833244821347,-0.0334837508592656,
0.0794388136507153));
#89641=CARTESIAN_POINT('Ctrl Pts',(0.010461187626907,-0.0333660264659097,
0.0794041749607128));
#89642=CARTESIAN_POINT('Ctrl Pts',(0.0102429380749387,-0.033693872113239,
0.0794967095814627));
#89643=CARTESIAN_POINT('Ctrl Pts',(0.0102742341403453,-0.0336474569764958,
0.0794843054588758));
#89644=CARTESIAN_POINT('Ctrl Pts',(0.0103053828554093,-0.033601104548885,
0.0794715358262675));
#89645=CARTESIAN_POINT('Ctrl Pts',(0.0103842442404127,-0.0334837508592656,
0.0794392060524259));
#89646=CARTESIAN_POINT('Ctrl Pts',(0.010462112997078,-0.0333660264659097,
0.079404553649094));
#89647=CARTESIAN_POINT('Ctrl Pts',(0.0105519775467729,-0.033693872113239,
0.0796383593048589));
#89648=CARTESIAN_POINT('Ctrl Pts',(0.010584102735015,-0.0336474569764958,
0.0796241462716933));
#89649=CARTESIAN_POINT('Ctrl Pts',(0.0106160593405201,-0.033601104548885,
0.0796095581465242));
#89650=CARTESIAN_POINT('Ctrl Pts',(0.0106969661183747,-0.0334837508592656,
0.0795726243676165));
#89651=CARTESIAN_POINT('Ctrl Pts',(0.0107767429434898,-0.0333660264659097,
0.0795333093717271));
#89652=CARTESIAN_POINT('Ctrl Pts',(0.0105618502629987,-0.0336769361243754,
0.079632319225162));
#89653=CARTESIAN_POINT('Ctrl Pts',(0.0105448196623067,-0.0336279031428237,
0.0795940236620713));
#89654=CARTESIAN_POINT('Ctrl Pts',(0.0105275440335534,-0.0335767852155838,
0.079555177120907));
#89655=CARTESIAN_POINT('Ctrl Pts',(0.0104936928512639,-0.0334733199122769,
0.079479058250498));
#89656=CARTESIAN_POINT('Ctrl Pts',(0.0104770945689073,-0.0334209645148416,
0.079441734812488));
#89657=CARTESIAN_POINT('Ctrl Pts',(0.0104608161269541,-0.0333679869844681,
0.0794051305780214));
#89658=CARTESIAN_POINT('',(0.0103965362219822,-0.0336938721132538,0.079567112028478));
#89659=CARTESIAN_POINT('Ctrl Pts',(0.0103126374997385,-0.034243627687391,
0.0794685559550161));
#89660=CARTESIAN_POINT('Ctrl Pts',(0.0105132301443936,-0.033943005420181,
0.079386001916206));
#89661=CARTESIAN_POINT('Ctrl Pts',(0.0107070346179166,-0.0336441434784052,
0.0792885729448674));
#89662=CARTESIAN_POINT('Ctrl Pts',(0.0105417019481317,-0.034243627687391,
0.0793684086710672));
#89663=CARTESIAN_POINT('Ctrl Pts',(0.0107385174757061,-0.033943005420181,
0.079277215324165));
#89664=CARTESIAN_POINT('Ctrl Pts',(0.010927904814458,-0.0336441434784052,
0.0791714560960379));
#89665=CARTESIAN_POINT('',(0.0105744790772775,-0.0341934961088741,0.0793530961726576));
#89666=CARTESIAN_POINT('',(0.0107861769053515,-0.0338664212865018,0.0792480172028979));
#89667=CARTESIAN_POINT('Origin',(0.00390799302620703,-0.034561072040514,
0.0640034672689447));
#89668=CARTESIAN_POINT('Origin',(0.0158626625724525,-0.033693800507292,
0.0889685119293432));
#89669=CARTESIAN_POINT('',(0.0106747477336384,-0.0336938721132327,0.0793046774691565));
#89670=CARTESIAN_POINT('',(0.0107301478748956,-0.0336938721132427,0.0792757452319597));
#89671=CARTESIAN_POINT('',(0.0104608161269492,-0.0340203938281606,0.0794051305780235));
#89672=CARTESIAN_POINT('Origin',(0.00437362203041919,-0.0345589643244381,
0.0638821150356397));
#89673=CARTESIAN_POINT('',(0.01046026409342,-0.034193496108874,0.079403889257447));
#89674=CARTESIAN_POINT('Origin',(0.0149379570872416,-0.0341934220717664,
0.0894725775394897));
#89675=CARTESIAN_POINT('',(0.0105173715853588,-0.0341934961088841,0.0793784927150624));
#89676=CARTESIAN_POINT('Ctrl Pts',(0.0103450868831099,-0.0340223579322397,
0.0797236707360799));
#89677=CARTESIAN_POINT('Ctrl Pts',(0.0104219623393039,-0.0339125849573575,
0.0796930331509989));
#89678=CARTESIAN_POINT('Ctrl Pts',(0.0104981496491858,-0.0338030433565231,
0.079660825951285));
#89679=CARTESIAN_POINT('Ctrl Pts',(0.0105735550331339,-0.0336938721132327,
0.0796270989613416));
#89680=CARTESIAN_POINT('Ctrl Pts',(0.0103834599385915,-0.0340223579322397,
0.0796170466841801));
#89681=CARTESIAN_POINT('Ctrl Pts',(0.0104588647710227,-0.0339125849573575,
0.0795858798345829));
#89682=CARTESIAN_POINT('Ctrl Pts',(0.0105335715359862,-0.0338030433565231,
0.0795531741807553));
#89683=CARTESIAN_POINT('Ctrl Pts',(0.0106074884037344,-0.0336938721132327,
0.0795189800167009));
#89684=CARTESIAN_POINT('Ctrl Pts',(0.0104218329940731,-0.0340223579322397,
0.0795104226322802));
#89685=CARTESIAN_POINT('Ctrl Pts',(0.0104957672027414,-0.0339125849573575,
0.0794787265181668));
#89686=CARTESIAN_POINT('Ctrl Pts',(0.0105689934227867,-0.0338030433565231,
0.0794455224102258));
#89687=CARTESIAN_POINT('Ctrl Pts',(0.010641421774335,-0.0336938721132327,
0.0794108610720602));
#89688=CARTESIAN_POINT('Ctrl Pts',(0.0104602060495547,-0.0340223579322397,
0.0794037985803804));
#89689=CARTESIAN_POINT('Ctrl Pts',(0.0105326696344601,-0.0339125849573575,
0.0793715732017507));
#89690=CARTESIAN_POINT('Ctrl Pts',(0.0106044153095872,-0.0338030433565231,
0.0793378706396961));
#89691=CARTESIAN_POINT('Ctrl Pts',(0.0106753551449355,-0.0336938721132327,
0.0793027421274195));
#89692=CARTESIAN_POINT('',(0.010624151383397,-0.0336938721132427,0.0794658882152563));
#89693=CARTESIAN_POINT('Ctrl Pts',(0.0105618502610078,-0.0337108120662682,
0.0796323192206852));
#89694=CARTESIAN_POINT('Ctrl Pts',(0.0105443777421099,-0.0337611408993851,
0.0795930299459316));
#89695=CARTESIAN_POINT('Ctrl Pts',(0.0105272240579175,-0.0338121088780384,
0.0795544576132753));
#89696=CARTESIAN_POINT('Ctrl Pts',(0.0104935387321512,-0.0339153382773238,
0.0794787116932433));
#89697=CARTESIAN_POINT('Ctrl Pts',(0.0104770213415777,-0.0339675558473118,
0.0794415701511311));
#89698=CARTESIAN_POINT('Ctrl Pts',(0.0104608161269378,-0.0340203938281305,
0.0794051305779849));
#89699=CARTESIAN_POINT('Ctrl Pts',(0.0105725859505553,-0.0341934961088741,
0.0793523685373797));
#89700=CARTESIAN_POINT('Ctrl Pts',(0.0106443235323612,-0.0340836138575045,
0.0793186009835022));
#89701=CARTESIAN_POINT('Ctrl Pts',(0.0107153279444492,-0.0339738896631393,
0.0792833651731941));
#89702=CARTESIAN_POINT('Ctrl Pts',(0.0107855113330447,-0.0338644633275951,
0.0792467122958646));
#89703=CARTESIAN_POINT('Ctrl Pts',(0.0106783607677275,-0.0341934961088741,
0.0793930237600828));
#89704=CARTESIAN_POINT('Ctrl Pts',(0.0107506589609826,-0.0340836138575045,
0.0793577976341058));
#89705=CARTESIAN_POINT('Ctrl Pts',(0.0108221935334385,-0.0339738896631393,
0.0793210923508709));
#89706=CARTESIAN_POINT('Ctrl Pts',(0.0108928760788564,-0.0338644633275951,
0.0792829610260169));
#89707=CARTESIAN_POINT('Ctrl Pts',(0.0107841355848998,-0.0341934961088741,
0.0794336789827859));
#89708=CARTESIAN_POINT('Ctrl Pts',(0.0108569943896039,-0.0340836138575045,
0.0793969942847094));
#89709=CARTESIAN_POINT('Ctrl Pts',(0.0109290591224277,-0.0339738896631393,
0.0793588195285476));
#89710=CARTESIAN_POINT('Ctrl Pts',(0.011000240824668,-0.0338644633275951,
0.0793192097561692));
#89711=CARTESIAN_POINT('Ctrl Pts',(0.010889910402072,-0.0341934961088741,
0.079474334205489));
#89712=CARTESIAN_POINT('Ctrl Pts',(0.0109633298182253,-0.0340836138575045,
0.079436190935313));
#89713=CARTESIAN_POINT('Ctrl Pts',(0.011035924711417,-0.0339738896631393,
0.0793965467062244));
#89714=CARTESIAN_POINT('Ctrl Pts',(0.0111076055704797,-0.0338644633275951,
0.0793554584863215));
#89715=CARTESIAN_POINT('',(0.0109012769641236,-0.0341764758832481,0.0794684135581252));
#89716=CARTESIAN_POINT('',(0.010889910402055,-0.034193496108874,0.0794743342054824));
#89717=CARTESIAN_POINT('Origin',(0.00369035864568257,-0.0345621026671577,
0.0645545278443666));
#89718=CARTESIAN_POINT('Ctrl Pts',(0.0109012769626372,-0.0341764758830279,
0.079468413555284));
#89719=CARTESIAN_POINT('Ctrl Pts',(0.010881406524438,-0.0341260048544556,
0.0794303651639684));
#89720=CARTESIAN_POINT('Ctrl Pts',(0.010861881658299,-0.0340749271285665,
0.0793929784823163));
#89721=CARTESIAN_POINT('Ctrl Pts',(0.0108235072099956,-0.0339715434413963,
0.0793194981689518));
#89722=CARTESIAN_POINT('Ctrl Pts',(0.0108046726441579,-0.0339192781018088,
0.0792834332908616));
#89723=CARTESIAN_POINT('Ctrl Pts',(0.0107861769042516,-0.0338664212856217,
0.0792480172047858));
#89724=CARTESIAN_POINT('',(0.0107321947396763,-0.0341934961088841,0.0794137151890801));
#89725=CARTESIAN_POINT('Ctrl Pts',(0.00895696931268619,-0.0321934096636942,
0.0798406884434743));
#89726=CARTESIAN_POINT('Ctrl Pts',(0.00910964311196116,-0.0319797282160566,
0.0798183351123587));
#89727=CARTESIAN_POINT('Ctrl Pts',(0.00926089872727212,-0.0317669959606124,
0.079787827748757));
#89728=CARTESIAN_POINT('Ctrl Pts',(0.00920352852800519,-0.0321934096636942,
0.0797990948701785));
#89729=CARTESIAN_POINT('Ctrl Pts',(0.00935508642558856,-0.0319797282160566,
0.0797701266747063));
#89730=CARTESIAN_POINT('Ctrl Pts',(0.00950487306326706,-0.0317669959606124,
0.0797330737957119));
#89731=CARTESIAN_POINT('Ctrl Pts',(0.00920500768011314,-0.0321934096636942,
0.0797988453430151));
#89732=CARTESIAN_POINT('Ctrl Pts',(0.00935655888320595,-0.0319797282160566,
0.0797698374638079));
#89733=CARTESIAN_POINT('Ctrl Pts',(0.00950633670822921,-0.0317669959606124,
0.0797327453171151));
#89734=CARTESIAN_POINT('',(0.00920352852811267,-0.0321934096636942,0.079799094870158));
#89735=CARTESIAN_POINT('',(0.00943470755481606,-0.0318665617561286,0.0797499642584603));
#89736=CARTESIAN_POINT('Origin',(0.00667259770270094,-0.0326371944420838,
0.0632820644467268));
#89737=CARTESIAN_POINT('Origin',(0.0119331252814131,-0.0316939261508561,
0.0904226161825828));
#89738=CARTESIAN_POINT('',(0.00908075077506004,-0.0320197259213198,0.0798211393066617));
#89739=CARTESIAN_POINT('Ctrl Pts',(0.00908093315538712,-0.0320197391311199,
0.0798211548887622));
#89740=CARTESIAN_POINT('Ctrl Pts',(0.00910978981795955,-0.0319792715672862,
0.0798162845963983));
#89741=CARTESIAN_POINT('Ctrl Pts',(0.0091387407042514,-0.0319386438886469,
0.079811172057838));
#89742=CARTESIAN_POINT('Ctrl Pts',(0.00916781467110402,-0.0318979098685809,
0.0798058036204764));
#89743=CARTESIAN_POINT('Ctrl Pts',(0.00919688806317048,-0.031857176653818,
0.0798004352892477));
#89744=CARTESIAN_POINT('Ctrl Pts',(0.00922593726756676,-0.0318163871807232,
0.079794840067621));
#89745=CARTESIAN_POINT('Ctrl Pts',(0.00925486290398387,-0.0317755399642096,
0.0797890408823101));
#89746=CARTESIAN_POINT('',(0.0090802700914209,-0.0321934096636184,0.079819888085349));
#89747=CARTESIAN_POINT('Origin',(0.00940054856919069,-0.032343065755914,
0.0817184413106508));
#89748=CARTESIAN_POINT('',(0.00914189930977679,-0.0321934096636664,0.0798094914777636));
#89749=CARTESIAN_POINT('Ctrl Pts',(0.00920187577157625,-0.0321934096636618,
0.0797979192498066));
#89750=CARTESIAN_POINT('Ctrl Pts',(0.00927976497976191,-0.0320835708272592,
0.0797830514991425));
#89751=CARTESIAN_POINT('Ctrl Pts',(0.00935730132171413,-0.0319739230346489,
0.0797665804592627));
#89752=CARTESIAN_POINT('Ctrl Pts',(0.00943438721239903,-0.0318646057455573,
0.0797485348172249));
#89753=CARTESIAN_POINT('Ctrl Pts',(0.00929421695605448,-0.0321934096636618,
0.0798636023558164));
#89754=CARTESIAN_POINT('Ctrl Pts',(0.00937301198546243,-0.0320835708272592,
0.0798474611482519));
#89755=CARTESIAN_POINT('Ctrl Pts',(0.00945142726909945,-0.0319739230346489,
0.0798296986442053));
#89756=CARTESIAN_POINT('Ctrl Pts',(0.00952936422419915,-0.0318646057455573,
0.0798103452693787));
#89757=CARTESIAN_POINT('Ctrl Pts',(0.00938655814053272,-0.0321934096636618,
0.0799292854618262));
#89758=CARTESIAN_POINT('Ctrl Pts',(0.00946625899116296,-0.0320835708272592,
0.0799118707973613));
#89759=CARTESIAN_POINT('Ctrl Pts',(0.00954555321648478,-0.0319739230346489,
0.0798928168291479));
#89760=CARTESIAN_POINT('Ctrl Pts',(0.00962434123599927,-0.0318646057455573,
0.0798721557215325));
#89761=CARTESIAN_POINT('Ctrl Pts',(0.00947889932501095,-0.0321934096636618,
0.0799949685678361));
#89762=CARTESIAN_POINT('Ctrl Pts',(0.00955950599686348,-0.0320835708272592,
0.0799762804464707));
#89763=CARTESIAN_POINT('Ctrl Pts',(0.0096396791638701,-0.0319739230346489,
0.0799559350140904));
#89764=CARTESIAN_POINT('Ctrl Pts',(0.00971931824779939,-0.0318646057455573,
0.0799339661736864));
#89765=CARTESIAN_POINT('Ctrl Pts',(0.00949138119003686,-0.032176398030639,
0.0799920606743997));
#89766=CARTESIAN_POINT('Ctrl Pts',(0.00948159855085754,-0.0321259596179479,
0.0799502715448598));
#89767=CARTESIAN_POINT('Ctrl Pts',(0.00947198540859514,-0.032074916464065,
0.0799092064662113));
#89768=CARTESIAN_POINT('Ctrl Pts',(0.00945309038158429,-0.0319716057814246,
0.0798284913629612));
#89769=CARTESIAN_POINT('Ctrl Pts',(0.00944381585910628,-0.0319193786724659,
0.0797888727882441));
#89770=CARTESIAN_POINT('Ctrl Pts',(0.0094347075548043,-0.0318665617561676,
0.0797499642584101));
#89771=CARTESIAN_POINT('',(0.00934121392658013,-0.0321934096636664,0.079897031718998));
#89772=CARTESIAN_POINT('Ctrl Pts',(0.00927486369295094,-0.0327445246967098,
0.0797850481480393));
#89773=CARTESIAN_POINT('Ctrl Pts',(0.00948739300823782,-0.0324436878339361,
0.079741634399554));
#89774=CARTESIAN_POINT('Ctrl Pts',(0.00969604844921609,-0.0321434074405928,
0.0796823354082979));
#89775=CARTESIAN_POINT('Ctrl Pts',(0.00927730141791528,-0.0327445246967098,
0.0797844936239206));
#89776=CARTESIAN_POINT('Ctrl Pts',(0.00948980981898312,-0.0324436878339361,
0.0797409879351353));
#89777=CARTESIAN_POINT('Ctrl Pts',(0.00969843747983829,-0.0321434074405928,
0.0796815988401161));
#89778=CARTESIAN_POINT('Ctrl Pts',(0.0095210739143494,-0.0327445246967098,
0.07972904121205));
#89779=CARTESIAN_POINT('Ctrl Pts',(0.00973149089351344,-0.0324436878339361,
0.0796763414932596));
#89780=CARTESIAN_POINT('Ctrl Pts',(0.00993734054205709,-0.0321434074405928,
0.0796079420219492));
#89781=CARTESIAN_POINT('Ctrl Pts',(0.00952353601656339,-0.0327445246967098,
0.0797284811426901));
#89782=CARTESIAN_POINT('Ctrl Pts',(0.00973393187236619,-0.0324436878339361,
0.0796756885641967));
#89783=CARTESIAN_POINT('Ctrl Pts',(0.0099397534629855,-0.0321434074405928,
0.0796071980880857));
#89784=CARTESIAN_POINT('',(0.00955610749708096,-0.0326943950436612,0.0797201498385232));
#89785=CARTESIAN_POINT('',(0.00978374540820148,-0.0323666188837389,0.0796566003236606));
#89786=CARTESIAN_POINT('Origin',(0.0052959155205112,-0.0326395579111105,
0.0634579598715753));
#89787=CARTESIAN_POINT('Origin',(0.0129714528185447,-0.0321933825603156,
0.0902311874680557));
#89788=CARTESIAN_POINT('',(0.0096636728737861,-0.0321934096536378,0.0796913772377324));
#89789=CARTESIAN_POINT('',(0.00972351308965225,-0.0321934096584275,0.0796733384205856));
#89790=CARTESIAN_POINT('',(0.0094347075548117,-0.032521010975624,0.0797499642584613));
#89791=CARTESIAN_POINT('Origin',(0.00576725340923381,-0.0326393129159137,
0.0633629597420143));
#89792=CARTESIAN_POINT('',(0.00943439789959461,-0.0326943950436595,0.0797486414843167));
#89793=CARTESIAN_POINT('Origin',(0.0119558975382756,-0.0326943765538136,
0.090519897504833));
#89794=CARTESIAN_POINT('',(0.00949525269834778,-0.0326943950436704,0.07973439566143));
#89795=CARTESIAN_POINT('Ctrl Pts',(0.00926134051997949,-0.032522978320377,
0.0800411765423401));
#89796=CARTESIAN_POINT('Ctrl Pts',(0.00934255025978414,-0.0324130253092451,
0.0800254953256809));
#89797=CARTESIAN_POINT('Ctrl Pts',(0.00942342329643002,-0.0323031222208071,
0.0800081365595964));
#89798=CARTESIAN_POINT('Ctrl Pts',(0.0095038568219188,-0.0321934096576659,
0.0799891261348738));
#89799=CARTESIAN_POINT('Ctrl Pts',(0.00931901314050244,-0.032522978320377,
0.0799436316240791));
#89800=CARTESIAN_POINT('Ctrl Pts',(0.00939887822574202,-0.0324130253092451,
0.0799271553916072));
#89801=CARTESIAN_POINT('Ctrl Pts',(0.0094783903658427,-0.0323031222208071,
0.0799090295461967));
#89802=CARTESIAN_POINT('Ctrl Pts',(0.00955744853068966,-0.0321934096576659,
0.0798892808996967));
#89803=CARTESIAN_POINT('Ctrl Pts',(0.00937668576102538,-0.032522978320377,
0.079846086705818));
#89804=CARTESIAN_POINT('Ctrl Pts',(0.0094552061916999,-0.0324130253092451,
0.0798288154575335));
#89805=CARTESIAN_POINT('Ctrl Pts',(0.00953335743525537,-0.0323031222208071,
0.079809922532797));
#89806=CARTESIAN_POINT('Ctrl Pts',(0.00961104023946051,-0.0321934096576659,
0.0797894356645198));
#89807=CARTESIAN_POINT('Ctrl Pts',(0.00943435838154833,-0.032522978320377,
0.079748541787557));
#89808=CARTESIAN_POINT('Ctrl Pts',(0.00951153415765779,-0.0324130253092451,
0.0797304755234598));
#89809=CARTESIAN_POINT('Ctrl Pts',(0.00958832450466805,-0.0323031222208071,
0.0797108155193974));
#89810=CARTESIAN_POINT('Ctrl Pts',(0.00966463194823136,-0.0321934096576659,
0.0796895904293427));
#89811=CARTESIAN_POINT('',(0.00958376484526082,-0.0321934096584275,0.0798402516869768));
#89812=CARTESIAN_POINT('Ctrl Pts',(0.00949138119005014,-0.0322104233328915,
0.0799920606744565));
#89813=CARTESIAN_POINT('Ctrl Pts',(0.00948158529515375,-0.0322609421831088,
0.0799502149196166));
#89814=CARTESIAN_POINT('Ctrl Pts',(0.00947196567721331,-0.0323120888240161,
0.0799091221783973));
#89815=CARTESIAN_POINT('Ctrl Pts',(0.00945307050693992,-0.0324156524631812,
0.0798284064631636));
#89816=CARTESIAN_POINT('Ctrl Pts',(0.00944380272152753,-0.032468026716732,
0.0797888166676036));
#89817=CARTESIAN_POINT('Ctrl Pts',(0.00943470755480609,-0.0325210109755913,
0.0797499642584181));
#89818=CARTESIAN_POINT('Origin',(0.000302798411271529,-0.0262834582511148,
0.0750076704056847));
#89819=CARTESIAN_POINT('Origin',(0.00530621998124759,-0.0342770973722091,
0.0859773416106945));
#89820=CARTESIAN_POINT('Ctrl Pts',(0.0095543846023505,-0.0326943950436604,
0.0797190805749539));
#89821=CARTESIAN_POINT('Ctrl Pts',(0.00963113697024279,-0.0325844576448134,
0.0796993641925199));
#89822=CARTESIAN_POINT('Ctrl Pts',(0.00970748700290522,-0.0324744968375323,
0.0796780590499216));
#89823=CARTESIAN_POINT('Ctrl Pts',(0.00978333725273647,-0.0323646534831895,
0.0796551937938388));
#89824=CARTESIAN_POINT('Ctrl Pts',(0.00965066770954531,-0.0326943950436604,
0.0797788358328955));
#89825=CARTESIAN_POINT('Ctrl Pts',(0.00972824361688532,-0.0325844576448134,
0.0797577924887905));
#89826=CARTESIAN_POINT('Ctrl Pts',(0.0098053898035357,-0.0324744968375323,
0.0797351432584642));
#89827=CARTESIAN_POINT('Ctrl Pts',(0.00988200782556948,-0.0323646534831895,
0.0797109185247898));
#89828=CARTESIAN_POINT('Ctrl Pts',(0.00974695081674012,-0.0326943950436604,
0.0798385910908371));
#89829=CARTESIAN_POINT('Ctrl Pts',(0.00982535026352786,-0.0325844576448134,
0.0798162207850612));
#89830=CARTESIAN_POINT('Ctrl Pts',(0.00990329260416619,-0.0324744968375323,
0.0797922274670068));
#89831=CARTESIAN_POINT('Ctrl Pts',(0.00998067839840248,-0.0323646534831895,
0.0797666432557407));
#89832=CARTESIAN_POINT('Ctrl Pts',(0.00984323392393492,-0.0326943950436604,
0.0798983463487787));
#89833=CARTESIAN_POINT('Ctrl Pts',(0.00992245691017039,-0.0325844576448134,
0.0798746490813319));
#89834=CARTESIAN_POINT('Ctrl Pts',(0.0100011954047967,-0.0324744968375323,
0.0798493116755494));
#89835=CARTESIAN_POINT('Ctrl Pts',(0.0100793489712355,-0.0323646534831895,
0.0798223679866917));
#89836=CARTESIAN_POINT('Ctrl Pts',(0.00985550857068935,-0.0326773559987533,
0.07989466045065));
#89837=CARTESIAN_POINT('Ctrl Pts',(0.00984311130562075,-0.032626792258728,
0.0798535349707487));
#89838=CARTESIAN_POINT('Ctrl Pts',(0.00983093377312217,-0.0325756109581931,
0.0798131384102777));
#89839=CARTESIAN_POINT('Ctrl Pts',(0.00980700780946977,-0.0324719985462395,
0.0797337687483512));
#89840=CARTESIAN_POINT('Ctrl Pts',(0.00979526897445343,-0.0324196091621788,
0.0796948274801878));
#89841=CARTESIAN_POINT('Ctrl Pts',(0.00978374540818738,-0.0323666188837757,
0.0796566003236139));
#89842=CARTESIAN_POINT('',(0.00969967071051251,-0.0326943950436704,0.0798092480936573));
#89843=CARTESIAN_POINT('Origin',(0.00812378219310841,-0.0315241814719618,
0.07415));
#89844=CARTESIAN_POINT('',(0.0109012769642642,-0.0342105180190362,0.0794684135583947));
#89845=CARTESIAN_POINT('',(0.010912630855329,-0.0341934961088739,0.0794624686483059));
#89846=CARTESIAN_POINT('Origin',(0.00364803044415716,-0.0345621723243437,
0.0645707338869119));
#89847=CARTESIAN_POINT('Origin',(0.00278250704172717,-0.0345621027604414,
0.0650286450762808));
#89848=CARTESIAN_POINT('Origin',(0.00281999399346116,-0.0345621725530212,
0.0650031692818173));
#89849=CARTESIAN_POINT('Ctrl Pts',(0.0106734181214623,-0.0346945769586966,
0.0793053718474377));
#89850=CARTESIAN_POINT('Ctrl Pts',(0.0107813994489052,-0.0345275153362944,
0.0792519687020998));
#89851=CARTESIAN_POINT('Ctrl Pts',(0.0108877292260835,-0.0343603235965186,
0.0791951558306151));
#89852=CARTESIAN_POINT('Ctrl Pts',(0.010992095474039,-0.034193496108874,
0.0791351059341747));
#89853=CARTESIAN_POINT('Ctrl Pts',(0.0107477281807789,-0.0346945769586966,
0.0792665640715983));
#89854=CARTESIAN_POINT('Ctrl Pts',(0.010854896663819,-0.0345275153362944,
0.0792116044723159));
#89855=CARTESIAN_POINT('Ctrl Pts',(0.0109603644373075,-0.0343603235965186,
0.0791532603075162));
#89856=CARTESIAN_POINT('Ctrl Pts',(0.0110638221390214,-0.034193496108874,
0.0790917087693853));
#89857=CARTESIAN_POINT('Ctrl Pts',(0.0108220382400957,-0.0346945769586966,
0.0792277562957589));
#89858=CARTESIAN_POINT('Ctrl Pts',(0.0109283938787331,-0.0345275153362944,
0.0791712402425335));
#89859=CARTESIAN_POINT('Ctrl Pts',(0.0110329996485315,-0.0343603235965186,
0.0791113647844187));
#89860=CARTESIAN_POINT('Ctrl Pts',(0.0111355488040033,-0.034193496108874,
0.0790483116045955));
#89861=CARTESIAN_POINT('Ctrl Pts',(0.0108963482994122,-0.0346945769586966,
0.0791889485199195));
#89862=CARTESIAN_POINT('Ctrl Pts',(0.0110018910936468,-0.0345275153362944,
0.0791308760127481));
#89863=CARTESIAN_POINT('Ctrl Pts',(0.0111056348597555,-0.0343603235965186,
0.0790694692613185));
#89864=CARTESIAN_POINT('Ctrl Pts',(0.011207275468986,-0.034193496108874,
0.0790049144398064));
#89865=CARTESIAN_POINT('',(0.0108963482986323,-0.0346945769586966,0.0791889485203265));
#89866=CARTESIAN_POINT('',(0.011101030424786,-0.0343667727832864,0.0790707842838023));
#89867=CARTESIAN_POINT('Origin',(0.00263116674820189,-0.0345626461566267,
0.0645470900085804));
#89868=CARTESIAN_POINT('Origin',(0.0168223057555468,-0.0341934771027721,
0.0885268756521276));
#89869=CARTESIAN_POINT('',(0.0109933788621512,-0.034193496108874,0.0791343294390539));
#89870=CARTESIAN_POINT('',(0.0110468530136792,-0.034193496108884,0.0791019756893674));
#89871=CARTESIAN_POINT('',(0.0107861769035202,-0.0345211942962611,0.0792480172033841));
#89872=CARTESIAN_POINT('Origin',(0.00305889754078945,-0.0345625596120682,
0.0643274617802946));
#89873=CARTESIAN_POINT('',(0.0107855480161328,-0.0346945769586886,0.0792468129947429));
#89874=CARTESIAN_POINT('Origin',(0.0159070470656408,-0.0346945685853798,
0.089053584261013));
#89875=CARTESIAN_POINT('',(0.0108409481573925,-0.0346945769587026,0.0792178807575448));
#89876=CARTESIAN_POINT('Ctrl Pts',(0.0106906781965947,-0.0345231616327842,
0.0795731950829144));
#89877=CARTESIAN_POINT('Ctrl Pts',(0.0107654293055647,-0.0344132092796988,
0.0795378140354068));
#89878=CARTESIAN_POINT('Ctrl Pts',(0.0108394447286616,-0.0343032738558979,
0.0795008886456725));
#89879=CARTESIAN_POINT('Ctrl Pts',(0.0109126308553275,-0.0341934961088739,
0.0794624686483121));
#89880=CARTESIAN_POINT('Ctrl Pts',(0.0107222804807894,-0.0345231616327842,
0.0794643721452014));
#89881=CARTESIAN_POINT('Ctrl Pts',(0.0107955316187736,-0.0344132092796988,
0.0794285555046987));
#89882=CARTESIAN_POINT('Ctrl Pts',(0.0108680381383786,-0.0343032738558979,
0.0793912255701605));
#89883=CARTESIAN_POINT('Ctrl Pts',(0.0109397083754022,-0.0341934961088739,
0.0793524325449396));
#89884=CARTESIAN_POINT('Ctrl Pts',(0.0107538827649842,-0.0345231616327842,
0.0793555492074885));
#89885=CARTESIAN_POINT('Ctrl Pts',(0.0108256339319824,-0.0344132092796988,
0.0793192969739906));
#89886=CARTESIAN_POINT('Ctrl Pts',(0.0108966315480957,-0.0343032738558979,
0.0792815624946485));
#89887=CARTESIAN_POINT('Ctrl Pts',(0.0109667858954769,-0.0341934961088739,
0.0792423964415671));
#89888=CARTESIAN_POINT('Ctrl Pts',(0.010785485049179,-0.0345231616327842,
0.0792467262697756));
#89889=CARTESIAN_POINT('Ctrl Pts',(0.0108557362451913,-0.0344132092796988,
0.0792100384432825));
#89890=CARTESIAN_POINT('Ctrl Pts',(0.0109252249578127,-0.0343032738558979,
0.0791718994191365));
#89891=CARTESIAN_POINT('Ctrl Pts',(0.0109938634155516,-0.0341934961088739,
0.0791323603381946));
#89892=CARTESIAN_POINT('',(0.0109530048587501,-0.0341934961088839,0.0792983990436899));
#89893=CARTESIAN_POINT('Ctrl Pts',(0.0109012769626589,-0.0342105180195379,
0.0794684135553258));
#89894=CARTESIAN_POINT('Ctrl Pts',(0.0108813842520914,-0.0342610556240654,
0.0794303225163456));
#89895=CARTESIAN_POINT('Ctrl Pts',(0.0108618485059288,-0.0343122189868824,
0.0793929150013635));
#89896=CARTESIAN_POINT('Ctrl Pts',(0.010823473817671,-0.0344158119695087,
0.0793194342285284));
#89897=CARTESIAN_POINT('Ctrl Pts',(0.0108046505711748,-0.034468199044996,
0.0792833910249845));
#89898=CARTESIAN_POINT('Ctrl Pts',(0.0107861769035042,-0.0345211942962359,
0.0792480172033548));
#89899=CARTESIAN_POINT('Ctrl Pts',(0.0108944136928532,-0.0346945769586932,
0.0791883413400184));
#89900=CARTESIAN_POINT('Ctrl Pts',(0.0109985778350075,-0.0345296777077528,
0.0791310604942161));
#89901=CARTESIAN_POINT('Ctrl Pts',(0.0111002855002113,-0.0343648066252516,
0.0790695233944684));
#89902=CARTESIAN_POINT('Ctrl Pts',(0.0108963482986243,-0.0346945769586932,
0.0791889485203309));
#89903=CARTESIAN_POINT('Ctrl Pts',(0.0110005249938019,-0.0345296777077528,
0.0791316276779232));
#89904=CARTESIAN_POINT('Ctrl Pts',(0.0111022435482061,-0.0343648066252516,
0.0790700500969187));
#89905=CARTESIAN_POINT('Ctrl Pts',(0.0112187697908207,-0.0346945769586932,
0.079290141220839));
#89906=CARTESIAN_POINT('Ctrl Pts',(0.011325038573479,-0.0345296777077528,
0.0792261545422206));
#89907=CARTESIAN_POINT('Ctrl Pts',(0.0114285719225654,-0.0343648066252516,
0.079157830352981));
#89908=CARTESIAN_POINT('',(0.0112297421630657,-0.0346775396665029,0.0792835185456563));
#89909=CARTESIAN_POINT('',(0.0112187697908064,-0.0346945769586885,0.0792901412208319));
#89910=CARTESIAN_POINT('Origin',(0.00250546247597207,-0.0345626617644253,
0.0651590773166458));
#89911=CARTESIAN_POINT('Ctrl Pts',(0.0112297421612359,-0.0346775396670097,
0.0792835185456332));
#89912=CARTESIAN_POINT('Ctrl Pts',(0.0112075044166854,-0.0346269749928345,
0.0792467641129203));
#89913=CARTESIAN_POINT('Ctrl Pts',(0.011185661855744,-0.0345757902891116,
0.0792106629070845));
#89914=CARTESIAN_POINT('Ctrl Pts',(0.0111427492599009,-0.0344721681088468,
0.0791397371284662));
#89915=CARTESIAN_POINT('Ctrl Pts',(0.0111216960535753,-0.0344197714290097,
0.0791049403590022));
#89916=CARTESIAN_POINT('Ctrl Pts',(0.0111010304245763,-0.0343667727831696,
0.0790707842841105));
#89917=CARTESIAN_POINT('',(0.0110575590447293,-0.0346945769587026,0.0792395448705892));
#89918=CARTESIAN_POINT('Origin',(0.00812378219310841,-0.0315241814719618,
0.07415));
#89919=CARTESIAN_POINT('',(0.0112297421630861,-0.0347116136489789,0.0792835185442631));
#89920=CARTESIAN_POINT('',(0.0112407003659563,-0.0346945769586885,0.0792768724485571));
#89921=CARTESIAN_POINT('Origin',(0.00246769736427044,-0.03456267041358,
0.0651841143581137));
#89922=CARTESIAN_POINT('Origin',(0.00276678724085952,-0.0345626619669717,
0.0650009658547634));
#89923=CARTESIAN_POINT('Origin',(0.0028064909336834,-0.0345626705879003,
0.0649791328195147));
#89924=CARTESIAN_POINT('Ctrl Pts',(0.010959869296639,-0.0352450361874068,
0.0791535360063471));
#89925=CARTESIAN_POINT('Ctrl Pts',(0.0111485807537295,-0.0349452760959493,
0.0790465712260271));
#89926=CARTESIAN_POINT('Ctrl Pts',(0.0113286990765173,-0.034644428984174,
0.0789256958022957));
#89927=CARTESIAN_POINT('Ctrl Pts',(0.0109620378138651,-0.0352450361874068,
0.0791522425002436));
#89928=CARTESIAN_POINT('Ctrl Pts',(0.0111507004855723,-0.0349452760959493,
0.0790451959329542));
#89929=CARTESIAN_POINT('Ctrl Pts',(0.011330764001042,-0.034644428984174,
0.0789242426293166));
#89930=CARTESIAN_POINT('Ctrl Pts',(0.0111767424897182,-0.0352450361874068,
0.0790241725889964));
#89931=CARTESIAN_POINT('Ctrl Pts',(0.0113605749254622,-0.0349452760959493,
0.0789090283019799));
#89932=CARTESIAN_POINT('Ctrl Pts',(0.0115352119737776,-0.034644428984174,
0.0787803641165208));
#89933=CARTESIAN_POINT('Ctrl Pts',(0.0111788895364767,-0.0352450361874068,
0.079022891889884));
#89934=CARTESIAN_POINT('Ctrl Pts',(0.0113626736698611,-0.0349452760959493,
0.0789076666256701));
#89935=CARTESIAN_POINT('Ctrl Pts',(0.0115372564535049,-0.034644428984174,
0.0787789253313928));
#89936=CARTESIAN_POINT('',(0.0112072494256749,-0.0351951634053333,0.0790049337923587));
#89937=CARTESIAN_POINT('',(0.0114041341068746,-0.0348678972925388,0.0788741312769493));
#89938=CARTESIAN_POINT('Origin',(0.00150454901844235,-0.0345636767886206,
0.0653571463827068));
#89939=CARTESIAN_POINT('Origin',(0.0177065356927869,-0.034694619934102,
0.0879504038316923));
#89940=CARTESIAN_POINT('',(0.01130068498852,-0.0346945769330288,0.0789443105475923));
#89941=CARTESIAN_POINT('',(0.0113520221196127,-0.0346945769458128,0.0789086629662042));
#89942=CARTESIAN_POINT('',(0.0111010304244765,-0.0350221583435276,0.0790707842839142));
#89943=CARTESIAN_POINT('Origin',(0.00187431997553251,-0.0345628458717802,
0.0650498796708099));
#89944=CARTESIAN_POINT('',(0.0111003875509974,-0.0351951360298762,0.0790697275879148));
#89945=CARTESIAN_POINT('Origin',(0.0168044724593228,-0.0351951838366688,
0.088497413369347));
#89946=CARTESIAN_POINT('',(0.0112072754682841,-0.0351951371328746,0.0790049144403668));
#89947=CARTESIAN_POINT('Ctrl Pts',(0.0110261390912839,-0.0350241211494343,
0.0794013164478708));
#89948=CARTESIAN_POINT('Ctrl Pts',(0.0110984738222298,-0.0349144232818962,
0.079361337671611));
#89949=CARTESIAN_POINT('Ctrl Pts',(0.0111700254591262,-0.0348045283579412,
0.0793198397555504));
#89950=CARTESIAN_POINT('Ctrl Pts',(0.0112407003754508,-0.0346945769439157,
0.0792768724427908));
#89951=CARTESIAN_POINT('Ctrl Pts',(0.0110508459545354,-0.0350241211494343,
0.079290723895176));
#89952=CARTESIAN_POINT('Ctrl Pts',(0.0111216573184126,-0.0349144232818962,
0.0792504047920051));
#89953=CARTESIAN_POINT('Ctrl Pts',(0.0111916776416313,-0.0348045283579412,
0.0792085978344172));
#89954=CARTESIAN_POINT('Ctrl Pts',(0.0112608152443571,-0.0346945769439157,
0.079165353234346));
#89955=CARTESIAN_POINT('Ctrl Pts',(0.0110755528177869,-0.0350241211494343,
0.0791801313424811));
#89956=CARTESIAN_POINT('Ctrl Pts',(0.0111448408145954,-0.0349144232818962,
0.0791394719123993));
#89957=CARTESIAN_POINT('Ctrl Pts',(0.0112133298241363,-0.0348045283579412,
0.0790973559132841));
#89958=CARTESIAN_POINT('Ctrl Pts',(0.0112809301132634,-0.0346945769439157,
0.0790538340259012));
#89959=CARTESIAN_POINT('Ctrl Pts',(0.0111002596810383,-0.0350241211494343,
0.0790695387897863));
#89960=CARTESIAN_POINT('Ctrl Pts',(0.0111680243107782,-0.0349144232818962,
0.0790285390327934));
#89961=CARTESIAN_POINT('Ctrl Pts',(0.0112349820066414,-0.0348045283579412,
0.0789861139921509));
#89962=CARTESIAN_POINT('Ctrl Pts',(0.0113010449821697,-0.0346945769439157,
0.0789423148174564));
#89963=CARTESIAN_POINT('',(0.0112706926770453,-0.0346945769458128,0.0791105914983105));
#89964=CARTESIAN_POINT('Ctrl Pts',(0.0112297421613777,-0.0347116136492782,
0.0792835185414432));
#89965=CARTESIAN_POINT('Ctrl Pts',(0.0112075132589665,-0.0347621546531604,
0.0792467786980937));
#89966=CARTESIAN_POINT('Ctrl Pts',(0.0111856752007276,-0.0348133084095606,
0.0792106848404703));
#89967=CARTESIAN_POINT('Ctrl Pts',(0.0111427625471322,-0.0349168561544574,
0.0791397589737028));
#89968=CARTESIAN_POINT('Ctrl Pts',(0.0111217049731347,-0.0349692089015925,
0.0791049550973945));
#89969=CARTESIAN_POINT('Ctrl Pts',(0.0111010304244746,-0.0350221583435,
0.0790707842838725));
#89970=CARTESIAN_POINT('Ctrl Pts',(0.0112058548317998,-0.0351951371254959,
0.0790045648521835));
#89971=CARTESIAN_POINT('Ctrl Pts',(0.011306219914263,-0.0350307338980963,
0.0789408449341354));
#89972=CARTESIAN_POINT('Ctrl Pts',(0.0114038656223842,-0.0348659306897824,
0.0788730312672282));
#89973=CARTESIAN_POINT('Ctrl Pts',(0.0112072754682162,-0.0351951371254959,
0.0790049144402723));
#89974=CARTESIAN_POINT('Ctrl Pts',(0.0113076477781938,-0.0350307338980963,
0.0789411651514578));
#89975=CARTESIAN_POINT('Ctrl Pts',(0.0114052994937281,-0.0348659306897824,
0.0788733218401601));
#89976=CARTESIAN_POINT('Ctrl Pts',(0.0114453756122413,-0.0351951371254959,
0.0790635057683189));
#89977=CARTESIAN_POINT('Ctrl Pts',(0.0115469592611649,-0.0350307338980963,
0.0789948339084156));
#89978=CARTESIAN_POINT('Ctrl Pts',(0.0116456178253884,-0.0348659306897824,
0.0789220221663916));
#89979=CARTESIAN_POINT('Origin',(0.0144374187644613,-0.0308609197409942,
0.0832424537310675));
#89980=CARTESIAN_POINT('',(0.011311081762565,-0.0351951371254959,0.0790304589382414));
#89981=CARTESIAN_POINT('Origin',(0.00745606980158198,-0.0351840467441142,
0.0734366236531671));
#89982=CARTESIAN_POINT('Origin',(0.0155860364218439,-0.0352322614707685,
0.0835032834717993));
#89983=CARTESIAN_POINT('',(0.0115956878952019,-0.0351951142564685,0.0787351592534177));
#89984=CARTESIAN_POINT('',(0.0116934483876602,-0.0351951372916787,0.0786577692109817));
#89985=CARTESIAN_POINT('Origin',(0.00824036220661084,-0.0352875117674211,
0.073830009294775));
#89986=CARTESIAN_POINT('Origin',(0.00145870505261403,-0.0298325076523997,
0.0775955677308751));
#89987=CARTESIAN_POINT('Origin',(0.0104711808944681,-0.0338733549886737,
0.0821958249366702));
#89988=CARTESIAN_POINT('Origin',(0.00812378219310841,-0.0315241814719618,
0.07415));
#89989=CARTESIAN_POINT('',(0.00912185652150633,-0.0327114338380027,0.0800664049569627));
#89990=CARTESIAN_POINT('',(0.00913449179186172,-0.0326943950436593,0.0800642595569543));
#89991=CARTESIAN_POINT('Origin',(0.00626557442642693,-0.0326395653589518,
0.0637092669314688));
#89992=CARTESIAN_POINT('',(0.00912185652151372,-0.0326773559991391,0.0800664049570073));
#89993=CARTESIAN_POINT('Origin',(0.0064092000078735,-0.0326395686496682,
0.0636842521244812));
#89994=CARTESIAN_POINT('',(0.009109216697909,-0.0326943950436595,0.0800685233662416));
#89995=CARTESIAN_POINT('Origin',(0.00631012128950666,-0.0326395670829588,
0.0637009704823884));
#89996=CARTESIAN_POINT('Origin',(0.00645400448005014,-0.0326395670474682,
0.0636774837085538));
#89997=CARTESIAN_POINT('Origin',(0.00812378219310841,-0.0315241814719618,
0.07415));
#89998=CARTESIAN_POINT('',(0.00949138119075433,-0.033212160714423,0.0799920606774468));
#89999=CARTESIAN_POINT('',(0.00950385681755752,-0.0331951640388587,0.0799891261359001));
#90000=CARTESIAN_POINT('Origin',(0.00499368834011878,-0.032641367224474,
0.0640998014851968));
#90001=CARTESIAN_POINT('',(0.00949138119047968,-0.0331781648281979,0.0799920606791099));
#90002=CARTESIAN_POINT('Origin',(0.0064224159774812,-0.0326412105969763,
0.063757281394915));
#90003=CARTESIAN_POINT('',(0.0094788993250309,-0.0331951640388588,0.0799949685678203));
#90004=CARTESIAN_POINT('Origin',(0.00503538584783144,-0.0326412118339323,
0.0640819743322511));
#90005=CARTESIAN_POINT('Origin',(0.00646769267691926,-0.0326413655043729,
0.0637547409009615));
#90006=CARTESIAN_POINT('Origin',(0.00812378219310841,-0.0315241814719618,
0.07415));
#90007=CARTESIAN_POINT('',(0.00874839290883649,-0.0322104233323589,0.0801173998890733));
#90008=CARTESIAN_POINT('',(0.00876113795713054,-0.0321934096636184,0.0801160520975022));
#90009=CARTESIAN_POINT('Origin',(0.00759179442432658,-0.0326387220923027,
0.0636054529442552));
#90010=CARTESIAN_POINT('',(0.00874839290805402,-0.0321763980308051,0.0801173998898277));
#90011=CARTESIAN_POINT('Origin',(0.0064167606925355,-0.0326386251392104,
0.0637347958322026));
#90012=CARTESIAN_POINT('',(0.00873564501100219,-0.0321934096636185,0.080118720456855));
#90013=CARTESIAN_POINT('Origin',(0.00763710227032919,-0.0326386231416166,
0.0636070659319768));
#90014=CARTESIAN_POINT('Origin',(0.00646075389492646,-0.0326387237046156,
0.0637238440867132));
#90015=CARTESIAN_POINT('Origin',(0.00812378219310841,-0.0315241814719618,
0.07415));
#90016=CARTESIAN_POINT('',(0.010212801619691,-0.0342105180190367,0.0797745886798295));
#90017=CARTESIAN_POINT('',(0.0102248110767376,-0.0341934961088739,0.079770113667014));
#90018=CARTESIAN_POINT('Origin',(0.00488392365083045,-0.0345621723898461,
0.0640853090295975));
#90019=CARTESIAN_POINT('',(0.0102128016191596,-0.0341764758832441,0.0797745886808157));
#90020=CARTESIAN_POINT('Origin',(0.00396783352876945,-0.0345621027326488,
0.064431130373545));
#90021=CARTESIAN_POINT('',(0.0102007826323748,-0.034193496108874,0.0797790380328514));
#90022=CARTESIAN_POINT('Origin',(0.00492794907776644,-0.0345621026475164,
0.0640745358026033));
#90023=CARTESIAN_POINT('Origin',(0.0040082180216118,-0.0345621724697839,
0.0644105540793245));
#90024=CARTESIAN_POINT('Origin',(0.00812378219310841,-0.0315241814719618,
0.07415));
#90025=CARTESIAN_POINT('',(0.00985550857176248,-0.0337108120655544,0.0798946604541967));
#90026=CARTESIAN_POINT('',(0.00986777531920442,-0.0336938721132327,0.0798909483516344));
#90027=CARTESIAN_POINT('Origin',(0.0062033642301923,-0.0345562527952255,
0.0639071636382977));
#90028=CARTESIAN_POINT('',(0.00985550857213072,-0.0336769361243754,0.0798946604554315));
#90029=CARTESIAN_POINT('Ctrl Pts',(0.00986777531920224,-0.0336938721132364,
0.0798909483516442));
#90030=CARTESIAN_POINT('Ctrl Pts',(0.00986573166119598,-0.0336910493069898,
0.0798915691768627));
#90031=CARTESIAN_POINT('Ctrl Pts',(0.00986368761768907,-0.0336882265912827,
0.0798921889272351));
#90032=CARTESIAN_POINT('Ctrl Pts',(0.00985959870904877,-0.0336825812713049,
0.079893426293213));
#90033=CARTESIAN_POINT('Ctrl Pts',(0.00985755384389822,-0.0336797586670127,
0.0798940439087966));
#90034=CARTESIAN_POINT('Ctrl Pts',(0.00985550857213048,-0.033676936124375,
0.0798946604554315));
#90035=CARTESIAN_POINT('',(0.00984323392392004,-0.033693872113232,0.0798983463487693));
#90036=CARTESIAN_POINT('Ctrl Pts',(0.0098555085721307,-0.0336769361243754,
0.0798946604554314));
#90037=CARTESIAN_POINT('Ctrl Pts',(0.00985346330039176,-0.0336797586669733,
0.0798952770020577));
#90038=CARTESIAN_POINT('Ctrl Pts',(0.00985141777674278,-0.0336825812712258,
0.0798958924330988));
#90039=CARTESIAN_POINT('Ctrl Pts',(0.00984732623777634,-0.0336882265864016,
0.0798971210608983));
#90040=CARTESIAN_POINT('Ctrl Pts',(0.00984528022254873,-0.0336910492972279,
0.0798977342576694));
#90041=CARTESIAN_POINT('Ctrl Pts',(0.00984323392393173,-0.0336938721132382,
0.0798983463487797));
#90042=CARTESIAN_POINT('Origin',(0.00406327432682986,-0.0345562523471192,
0.0645522933807731));
#90043=CARTESIAN_POINT('Ctrl Pts',(0.00931122775127138,-0.033693872113265,
0.0797774750382086));
#90044=CARTESIAN_POINT('Ctrl Pts',(0.00942903390460924,-0.0335278710435226,
0.0797526169282116));
#90045=CARTESIAN_POINT('Ctrl Pts',(0.0095460190701494,-0.0333620469224385,
0.0797240731929003));
#90046=CARTESIAN_POINT('Ctrl Pts',(0.0096622366800184,-0.0331951640388587,
0.079691810178179));
#90047=CARTESIAN_POINT('Ctrl Pts',(0.00939285433319994,-0.033693872113265,
0.0797583666383155));
#90048=CARTESIAN_POINT('Ctrl Pts',(0.00951026046928805,-0.0335278710435226,
0.0797317997488816));
#90049=CARTESIAN_POINT('Ctrl Pts',(0.00962679217142473,-0.0333620469224385,
0.0797015603797149));
#90050=CARTESIAN_POINT('Ctrl Pts',(0.00974250236417658,-0.0331951640388587,
0.0796676141088612));
#90051=CARTESIAN_POINT('Ctrl Pts',(0.00947448091512851,-0.033693872113265,
0.0797392582384225));
#90052=CARTESIAN_POINT('Ctrl Pts',(0.00959148703396686,-0.0335278710435226,
0.0797109825695516));
#90053=CARTESIAN_POINT('Ctrl Pts',(0.00970756527270005,-0.0333620469224385,
0.0796790475665296));
#90054=CARTESIAN_POINT('Ctrl Pts',(0.00982276804833477,-0.0331951640388587,
0.0796434180395434));
#90055=CARTESIAN_POINT('Ctrl Pts',(0.00955610749705708,-0.033693872113265,
0.0797201498385294));
#90056=CARTESIAN_POINT('Ctrl Pts',(0.00967271359864567,-0.0335278710435226,
0.0796901653902217));
#90057=CARTESIAN_POINT('Ctrl Pts',(0.00978833837397538,-0.0333620469224385,
0.0796565347533442));
#90058=CARTESIAN_POINT('Ctrl Pts',(0.00990303373249296,-0.0331951640388587,
0.0796192219702256));
#90059=CARTESIAN_POINT('',(0.00955610749709523,-0.0336938721132548,0.0797201498385196));
#90060=CARTESIAN_POINT('',(0.00978374541810405,-0.0333679846208752,0.0796566003520759));
#90061=CARTESIAN_POINT('Ctrl Pts',(0.00955610749710581,-0.0336938721132388,
0.0797201498385436));
#90062=CARTESIAN_POINT('Ctrl Pts',(0.00957785040492485,-0.0336629187933892,
0.0797145588009588));
#90063=CARTESIAN_POINT('Ctrl Pts',(0.00959955362107873,-0.0336319952301031,
0.0797088422380559));
#90064=CARTESIAN_POINT('Ctrl Pts',(0.0096755707765491,-0.0335235892595445,
0.0796883433074983));
#90065=CARTESIAN_POINT('Ctrl Pts',(0.00972975960390407,-0.0334458668645755,
0.079672874332095));
#90066=CARTESIAN_POINT('Ctrl Pts',(0.00978374541112119,-0.0333679869902197,
0.0796566003287654));
#90067=CARTESIAN_POINT('Ctrl Pts',(0.00978374562952784,-0.0333679128829496,
0.0796566010578595));
#90068=CARTESIAN_POINT('Ctrl Pts',(0.00978361479406216,-0.0333391359256877,
0.0796561670370252));
#90069=CARTESIAN_POINT('Ctrl Pts',(0.00978351673985758,-0.033310357818174,
0.0796558417615556));
#90070=CARTESIAN_POINT('Ctrl Pts',(0.00978345138122428,-0.0332815781851602,
0.0796556249471851));
#90071=CARTESIAN_POINT('Ctrl Pts',(0.00978338596645222,-0.033252773832338,
0.0796554079465853));
#90072=CARTESIAN_POINT('Ctrl Pts',(0.00978335330633778,-0.0332239690390847,
0.079655299603122));
#90073=CARTESIAN_POINT('Ctrl Pts',(0.00978335330633771,-0.0331951640388587,
0.079655299603122));
#90074=CARTESIAN_POINT('',(0.00966367288018325,-0.0331951640388587,0.0796913772360182));
#90075=CARTESIAN_POINT('',(0.00972351309327069,-0.0331951640388687,0.0796733384195801));
#90076=CARTESIAN_POINT('',(0.00943470755476085,-0.0335216366559682,0.0797499642582251));
#90077=CARTESIAN_POINT('Origin',(0.00446956781469179,-0.0326434571526632,
0.0638528559558026));
#90078=CARTESIAN_POINT('',(0.0094343978995946,-0.0336938721132327,0.0797486414843167));
#90079=CARTESIAN_POINT('Origin',(0.0119235566863759,-0.0336938867896348,
0.0903817463226168));
#90080=CARTESIAN_POINT('',(0.00949525269835491,-0.0336938721132538,0.0797343956614282));
#90081=CARTESIAN_POINT('Ctrl Pts',(0.00926134240707744,-0.0335235895815171,
0.0800411761779483));
#90082=CARTESIAN_POINT('Ctrl Pts',(0.00934244604582544,-0.0334144449262748,
0.0800255154219531));
#90083=CARTESIAN_POINT('Ctrl Pts',(0.00942331932339555,-0.0333049234473147,
0.0800081611335073));
#90084=CARTESIAN_POINT('Ctrl Pts',(0.0095038568175559,-0.0331951640388587,
0.0799891261359032));
#90085=CARTESIAN_POINT('Ctrl Pts',(0.00931901506428282,-0.0335235895815171,
0.0799436311263217));
#90086=CARTESIAN_POINT('Ctrl Pts',(0.00939877580334664,-0.0334144449262748,
0.0799271763926531));
#90087=CARTESIAN_POINT('Ctrl Pts',(0.00947828823542234,-0.0333049234473147,
0.0799090549576465));
#90088=CARTESIAN_POINT('Ctrl Pts',(0.00955744858952339,-0.0331951640388587,
0.0798892807831653));
#90089=CARTESIAN_POINT('Ctrl Pts',(0.0093766877214882,-0.0335235895815171,
0.0798460860746951));
#90090=CARTESIAN_POINT('Ctrl Pts',(0.00945510556086785,-0.0334144449262748,
0.079828837363353));
#90091=CARTESIAN_POINT('Ctrl Pts',(0.00953325714744913,-0.0333049234473147,
0.0798099487817857));
#90092=CARTESIAN_POINT('Ctrl Pts',(0.00961104036149088,-0.0331951640388587,
0.0797894354304274));
#90093=CARTESIAN_POINT('Ctrl Pts',(0.00943436037869357,-0.0335235895815171,
0.0797485410230685));
#90094=CARTESIAN_POINT('Ctrl Pts',(0.00951143531838905,-0.0334144449262748,
0.079730498334053));
#90095=CARTESIAN_POINT('Ctrl Pts',(0.00958822605947593,-0.0333049234473147,
0.0797108426059249));
#90096=CARTESIAN_POINT('Ctrl Pts',(0.00966463213345837,-0.0331951640388587,
0.0796895900776896));
#90097=CARTESIAN_POINT('',(0.00958376484888039,-0.0331951640388687,0.0798402516859692));
#90098=CARTESIAN_POINT('Ctrl Pts',(0.00949138119003446,-0.0332121607145987,
0.0799920606743897));
#90099=CARTESIAN_POINT('Ctrl Pts',(0.00948160041949585,-0.0332625444108916,
0.0799502795272426));
#90100=CARTESIAN_POINT('Ctrl Pts',(0.00947198818698186,-0.0333135300745102,
0.079909218334825));
#90101=CARTESIAN_POINT('Ctrl Pts',(0.00945309364375762,-0.0334167177151439,
0.0798285052981974));
#90102=CARTESIAN_POINT('Ctrl Pts',(0.00944381724049779,-0.0334688874167211,
0.0797888786892237));
#90103=CARTESIAN_POINT('Ctrl Pts',(0.00943470755466547,-0.0335216366556511,
0.0797499642578176));
#90104=CARTESIAN_POINT('Ctrl Pts',(0.00955610749707543,-0.0336938721132388,
0.0797201498385247));
#90105=CARTESIAN_POINT('Ctrl Pts',(0.00958871143245195,-0.0336474569764957,
0.0797117659632246));
#90106=CARTESIAN_POINT('Ctrl Pts',(0.00962121498994013,-0.033601104548885,
0.0797030009921639));
#90107=CARTESIAN_POINT('Ctrl Pts',(0.00970350652446392,-0.0334837508592656,
0.0796808101006312));
#90108=CARTESIAN_POINT('Ctrl Pts',(0.00978510436048511,-0.0333660264659097,
0.0796561904849163));
#90109=CARTESIAN_POINT('Ctrl Pts',(0.00984495668250204,-0.0336938721132388,
0.0798994155278473));
#90110=CARTESIAN_POINT('Ctrl Pts',(0.00987860991944483,-0.0336474569764957,
0.0798893409224146));
#90111=CARTESIAN_POINT('Ctrl Pts',(0.00991214291446956,-0.033601104548885,
0.0798788730536715));
#90112=CARTESIAN_POINT('Ctrl Pts',(0.00999704074815335,-0.0334837508592656,
0.0798523708167278));
#90113=CARTESIAN_POINT('Ctrl Pts',(0.0100811159847366,-0.0333660264659097,
0.0798233645187791));
#90114=CARTESIAN_POINT('Ctrl Pts',(0.00985550857213072,-0.0336769361243754,
0.0798946604554315));
#90115=CARTESIAN_POINT('Ctrl Pts',(0.00984341164762209,-0.033627901837843,
0.0798545312960567));
#90116=CARTESIAN_POINT('Ctrl Pts',(0.00983114069370158,-0.0335767825754286,
0.0798138248284599));
#90117=CARTESIAN_POINT('Ctrl Pts',(0.00980709668019615,-0.0334733171799197,
0.0797340635594466));
#90118=CARTESIAN_POINT('Ctrl Pts',(0.00979530746094694,-0.0334209631321944,
0.0796949551515336));
#90119=CARTESIAN_POINT('Ctrl Pts',(0.00978374540820146,-0.0333679869844681,
0.0796566003236606));
#90120=CARTESIAN_POINT('',(0.00969967071051763,-0.0336938721132534,0.0798092480936544));
#90121=CARTESIAN_POINT('Ctrl Pts',(0.00962638780623428,-0.034243627687391,
0.0797016603481663));
#90122=CARTESIAN_POINT('Ctrl Pts',(0.00983577212800967,-0.033943005420181,
0.0796449886432224));
#90123=CARTESIAN_POINT('Ctrl Pts',(0.0100402928658562,-0.0336441434784052,
0.0795727062516094));
#90124=CARTESIAN_POINT('Ctrl Pts',(0.00962878590613157,-0.034243627687391,
0.0797009538661194));
#90125=CARTESIAN_POINT('Ctrl Pts',(0.0098381435824973,-0.033943005420181,
0.0796441917153468));
#90126=CARTESIAN_POINT('Ctrl Pts',(0.0100426309378806,-0.0336441434784052,
0.0795718211418938));
#90127=CARTESIAN_POINT('Ctrl Pts',(0.00986859589586089,-0.034243627687391,
0.0796303056614287));
#90128=CARTESIAN_POINT('Ctrl Pts',(0.0100752890312612,-0.033943005420181,
0.0795644989277917));
#90129=CARTESIAN_POINT('Ctrl Pts',(0.0102764381403202,-0.0336441434784052,
0.079483310170329));
#90130=CARTESIAN_POINT('Ctrl Pts',(0.00987101797675716,-0.034243627687391,
0.0796295921145613));
#90131=CARTESIAN_POINT('Ctrl Pts',(0.0100776842002937,-0.033943005420181,
0.0795636940306374));
#90132=CARTESIAN_POINT('Ctrl Pts',(0.0102787995930649,-0.0336441434784052,
0.0794824162095161));
#90133=CARTESIAN_POINT('',(0.00990303373249299,-0.0341934961088741,0.0796192219702256));
#90134=CARTESIAN_POINT('',(0.0101262321469139,-0.0338664212863443,0.0795415043528434));
#90135=CARTESIAN_POINT('Origin',(0.00521293353933639,-0.0345610720404037,
0.0635550972214448));
#90136=CARTESIAN_POINT('Origin',(0.0139443877772785,-0.0336938005072992,
0.0898216022135932));
#90137=CARTESIAN_POINT('',(0.0100085802132244,-0.0336938721132327,0.0795837520575904));
#90138=CARTESIAN_POINT('',(0.010067169678664,-0.0336938721132427,0.079561991438568));
#90139=CARTESIAN_POINT('',(0.00978374540819636,-0.0340203938281605,0.0796566003236621));
#90140=CARTESIAN_POINT('Origin',(0.00569010038791695,-0.0345589643244747,
0.0634930606758832));
#90141=CARTESIAN_POINT('',(0.00978335330633812,-0.0341934961088739,0.0796552996031219));
#90142=CARTESIAN_POINT('Origin',(0.0129637971165719,-0.0341934220717703,
0.0902057970063492));
#90143=CARTESIAN_POINT('',(0.00984319351942556,-0.0341934961088841,0.0796372607866838));
#90144=CARTESIAN_POINT('Ctrl Pts',(0.00962900505598272,-0.0340223579322396,
0.0799581239770792));
#90145=CARTESIAN_POINT('Ctrl Pts',(0.00970911423384991,-0.0339125849573575,
0.0799373630280142));
#90146=CARTESIAN_POINT('Ctrl Pts',(0.00978873741652145,-0.0338030433565231,
0.0799149585935938));
#90147=CARTESIAN_POINT('Ctrl Pts',(0.00986777531920265,-0.0336938721132327,
0.0798909483516383));
#90148=CARTESIAN_POINT('Ctrl Pts',(0.00968043906566049,-0.0340223579322396,
0.0798571501068014));
#90149=CARTESIAN_POINT('Ctrl Pts',(0.00975915555050563,-0.0339125849573575,
0.0798356797485974));
#90150=CARTESIAN_POINT('Ctrl Pts',(0.00983737233566366,-0.0338030433565231,
0.079812595229041));
#90151=CARTESIAN_POINT('Ctrl Pts',(0.00991499201198173,-0.0336938721132327,
0.0797879349362332));
#90152=CARTESIAN_POINT('Ctrl Pts',(0.00973187307533826,-0.0340223579322396,
0.0797561762365236));
#90153=CARTESIAN_POINT('Ctrl Pts',(0.00980919686716136,-0.0339125849573575,
0.0797339964691805));
#90154=CARTESIAN_POINT('Ctrl Pts',(0.00988600725480587,-0.0338030433565231,
0.0797102318644881));
#90155=CARTESIAN_POINT('Ctrl Pts',(0.00996220870476081,-0.0336938721132327,
0.0796849215208281));
#90156=CARTESIAN_POINT('Ctrl Pts',(0.00978330708501602,-0.0340223579322396,
0.0796552023662457));
#90157=CARTESIAN_POINT('Ctrl Pts',(0.00985923818381708,-0.0339125849573575,
0.0796323131897637));
#90158=CARTESIAN_POINT('Ctrl Pts',(0.00993464217394808,-0.0338030433565231,
0.0796078684999353));
#90159=CARTESIAN_POINT('Ctrl Pts',(0.0100094253975399,-0.0336938721132327,
0.079581908105423));
#90160=CARTESIAN_POINT('',(0.0099381777662244,-0.0336938721132427,0.0797373502046224));
#90161=CARTESIAN_POINT('Ctrl Pts',(0.00985550857071632,-0.0337108120662692,
0.0798946604507397));
#90162=CARTESIAN_POINT('Ctrl Pts',(0.00984309807969535,-0.0337611408993968,
0.0798534910963519));
#90163=CARTESIAN_POINT('Ctrl Pts',(0.00983091405260156,-0.0338121088780625,
0.0798130729913432));
#90164=CARTESIAN_POINT('Ctrl Pts',(0.00980698782678264,-0.0339153382773241,
0.0797337024597311));
#90165=CARTESIAN_POINT('Ctrl Pts',(0.00979525575034011,-0.0339675558473111,
0.0796947836118023));
#90166=CARTESIAN_POINT('Ctrl Pts',(0.00978374540818986,-0.0340203938281304,
0.0796566003236224));
#90167=CARTESIAN_POINT('Ctrl Pts',(0.00990124673052261,-0.0341934961088741,
0.0796182628008755));
#90168=CARTESIAN_POINT('Ctrl Pts',(0.0100142987559685,-0.0340287516182428,
0.0795815151218721));
#90169=CARTESIAN_POINT('Ctrl Pts',(0.0101257353711686,-0.0338644633275951,
0.0795401263170781));
#90170=CARTESIAN_POINT('Ctrl Pts',(0.00990303373249295,-0.0341934961088741,
0.0796192219702256));
#90171=CARTESIAN_POINT('Ctrl Pts',(0.0100161055880095,-0.0340287516182428,
0.0795824373463643));
#90172=CARTESIAN_POINT('Ctrl Pts',(0.0101275604893769,-0.0338644633275951,
0.0795410108086892));
#90173=CARTESIAN_POINT('Ctrl Pts',(0.0102007826323912,-0.0341934961088741,
0.0797790380328602));
#90174=CARTESIAN_POINT('Ctrl Pts',(0.0103171585590977,-0.0340287516182428,
0.0797360976850636));
#90175=CARTESIAN_POINT('Ctrl Pts',(0.0104316602876492,-0.0338644633275951,
0.0796883841236326));
#90176=CARTESIAN_POINT('Ctrl Pts',(0.0102128016173517,-0.0341764758837552,
0.0797745886805576));
#90177=CARTESIAN_POINT('Ctrl Pts',(0.0101978566280018,-0.0341260050040553,
0.0797343500238654));
#90178=CARTESIAN_POINT('Ctrl Pts',(0.0101831713820069,-0.0340749269148336,
0.0796948108232568));
#90179=CARTESIAN_POINT('Ctrl Pts',(0.010154309167467,-0.0339715436306863,
0.0796171006270857));
#90180=CARTESIAN_POINT('Ctrl Pts',(0.0101401431541839,-0.0339192778237251,
0.079578959110878));
#90181=CARTESIAN_POINT('Ctrl Pts',(0.0101262321456331,-0.0338664212854771,
0.0795415043545428));
#90182=CARTESIAN_POINT('',(0.0100519081824439,-0.0341934961088841,0.0796991300015486));
#90183=CARTESIAN_POINT('Ctrl Pts',(0.0100071740567672,-0.0346945769586966,
0.0795842743158962));
#90184=CARTESIAN_POINT('Ctrl Pts',(0.0101209971080783,-0.0345275153362944,
0.0795448259192429));
#90185=CARTESIAN_POINT('Ctrl Pts',(0.0102336089840957,-0.0343603235965185,
0.0795017876890168));
#90186=CARTESIAN_POINT('Ctrl Pts',(0.0103446785207095,-0.034193496108874,
0.079455291863277));
#90187=CARTESIAN_POINT('Ctrl Pts',(0.010085762062824,-0.0346945769586966,
0.0795550860710852));
#90188=CARTESIAN_POINT('Ctrl Pts',(0.0101989737546612,-0.0345275153362944,
0.0795139916171801));
#90189=CARTESIAN_POINT('Ctrl Pts',(0.0103109223460903,-0.0343603235965185,
0.0794693261306403));
#90190=CARTESIAN_POINT('Ctrl Pts',(0.0104212787062321,-0.034193496108874,
0.0794212266330705));
#90191=CARTESIAN_POINT('Ctrl Pts',(0.0101643500688808,-0.0346945769586966,
0.0795258978262741));
#90192=CARTESIAN_POINT('Ctrl Pts',(0.0102769504012441,-0.0345275153362944,
0.0794831573151173));
#90193=CARTESIAN_POINT('Ctrl Pts',(0.010388235708085,-0.0343603235965185,
0.0794368645722637));
#90194=CARTESIAN_POINT('Ctrl Pts',(0.0104978788917548,-0.034193496108874,
0.079387161402864));
#90195=CARTESIAN_POINT('Ctrl Pts',(0.0102429380749375,-0.0346945769586966,
0.0794967095814631));
#90196=CARTESIAN_POINT('Ctrl Pts',(0.010354927047827,-0.0345275153362944,
0.0794523230130545));
#90197=CARTESIAN_POINT('Ctrl Pts',(0.0104655490700796,-0.0343603235965185,
0.0794044030138871));
#90198=CARTESIAN_POINT('Ctrl Pts',(0.0105744790772775,-0.034193496108874,
0.0793530961726575));
#90199=CARTESIAN_POINT('',(0.0102429380749483,-0.0346945769586966,0.0794967095814589));
#90200=CARTESIAN_POINT('',(0.010460816127266,-0.0343667727833015,0.0794051305779478));
#90201=CARTESIAN_POINT('Origin',(0.00387804142253948,-0.0345626461565472,
0.0639344045683027));
#90202=CARTESIAN_POINT('Origin',(0.0149518158849197,-0.0341934771027857,
0.0895037233757803));
#90203=CARTESIAN_POINT('',(0.0103460491095624,-0.034193496108874,0.0794546823422364));
#90204=CARTESIAN_POINT('',(0.0104031566015012,-0.034193496108884,0.0794292857998518));
#90205=CARTESIAN_POINT('',(0.0101262321451442,-0.0345211942962613,0.0795415043531111));
#90206=CARTESIAN_POINT('Origin',(0.00432992614611196,-0.0345625596120916,
0.0637701170572003));
#90207=CARTESIAN_POINT('',(0.0101257591440837,-0.0346945769586885,0.0795402308195257));
#90208=CARTESIAN_POINT('Origin',(0.0139777595158368,-0.034694568585392,
0.0899115667198707));
#90209=CARTESIAN_POINT('',(0.010184348609526,-0.0346945769587026,0.0795184702005023));
#90210=CARTESIAN_POINT('Ctrl Pts',(0.00999073087892141,-0.0345231616327842,
0.0798521489461946));
#90211=CARTESIAN_POINT('Ctrl Pts',(0.0100693269741611,-0.0344132092796988,
0.0798264156870141));
#90212=CARTESIAN_POINT('Ctrl Pts',(0.0101473867420356,-0.0343032738558979,
0.0797990580573173));
#90213=CARTESIAN_POINT('Ctrl Pts',(0.0102248110767358,-0.0341934961088739,
0.0797701136670187));
#90214=CARTESIAN_POINT('Ctrl Pts',(0.0100357231003355,-0.0345231616327842,
0.079748144926316));
#90215=CARTESIAN_POINT('Ctrl Pts',(0.0101128856465871,-0.0344132092796988,
0.0797217915127073));
#90216=CARTESIAN_POINT('Ctrl Pts',(0.0101894991120329,-0.0343032738558979,
0.0796938434124094));
#90217=CARTESIAN_POINT('Ctrl Pts',(0.0102654662631213,-0.0341934961088739,
0.0796643389443358));
#90218=CARTESIAN_POINT('Ctrl Pts',(0.0100807153217496,-0.0345231616327842,
0.0796441409064373));
#90219=CARTESIAN_POINT('Ctrl Pts',(0.0101564443190132,-0.0344132092796988,
0.0796171673384005));
#90220=CARTESIAN_POINT('Ctrl Pts',(0.0102316114820302,-0.0343032738558979,
0.0795886287675016));
#90221=CARTESIAN_POINT('Ctrl Pts',(0.0103061214495069,-0.0341934961088739,
0.0795585642216529));
#90222=CARTESIAN_POINT('Ctrl Pts',(0.0101257075431637,-0.0345231616327842,
0.0795401368865587));
#90223=CARTESIAN_POINT('Ctrl Pts',(0.0102000029914392,-0.0344132092796988,
0.0795125431640937));
#90224=CARTESIAN_POINT('Ctrl Pts',(0.0102737238520275,-0.0343032738558979,
0.0794834141225937));
#90225=CARTESIAN_POINT('Ctrl Pts',(0.0103467766358924,-0.0341934961088739,
0.0794527894989701));
#90226=CARTESIAN_POINT('',(0.01028543009316,-0.0341934961088839,0.0796123980046352));
#90227=CARTESIAN_POINT('Ctrl Pts',(0.010212801618482,-0.0342105180195389,
0.0797745886765839));
#90228=CARTESIAN_POINT('Ctrl Pts',(0.0101978398409612,-0.0342610556240768,
0.0797343047790751));
#90229=CARTESIAN_POINT('Ctrl Pts',(0.0101831465448014,-0.0343122189869054,
0.0796947437552769));
#90230=CARTESIAN_POINT('Ctrl Pts',(0.010154284035293,-0.0344158119695089,
0.079617032776534));
#90231=CARTESIAN_POINT('Ctrl Pts',(0.0101401266269656,-0.0344681990449969,
0.0795789146060657));
#90232=CARTESIAN_POINT('Ctrl Pts',(0.010126232145131,-0.0345211942962363,
0.0795415043530806));
#90233=CARTESIAN_POINT('Ctrl Pts',(0.0102410948239851,-0.0346945769586932,
0.0794958647185508));
#90234=CARTESIAN_POINT('Ctrl Pts',(0.0103147635418812,-0.0345846629175835,
0.0794666870802989));
#90235=CARTESIAN_POINT('Ctrl Pts',(0.0103878414609988,-0.034474692504983,
0.0794359810196021));
#90236=CARTESIAN_POINT('Ctrl Pts',(0.0104602351079724,-0.0343648066252516,
0.0794037862673067));
#90237=CARTESIAN_POINT('Ctrl Pts',(0.0103441080056568,-0.0346945769586932,
0.0795430813041972));
#90238=CARTESIAN_POINT('Ctrl Pts',(0.0104184273919688,-0.0345846629175835,
0.0795124840922336));
#90239=CARTESIAN_POINT('Ctrl Pts',(0.0104921267344367,-0.034474692504983,
0.079480344759803));
#90240=CARTESIAN_POINT('Ctrl Pts',(0.0105651117710401,-0.0343648066252516,
0.0794467048775126));
#90241=CARTESIAN_POINT('Ctrl Pts',(0.0104471211873285,-0.0346945769586932,
0.0795902978898435));
#90242=CARTESIAN_POINT('Ctrl Pts',(0.0105220912420564,-0.0345846629175835,
0.0795582811041683));
#90243=CARTESIAN_POINT('Ctrl Pts',(0.0105964120078746,-0.034474692504983,
0.0795247085000038));
#90244=CARTESIAN_POINT('Ctrl Pts',(0.0106699884341078,-0.0343648066252516,
0.0794896234877185));
#90245=CARTESIAN_POINT('Ctrl Pts',(0.0105501343690003,-0.0346945769586932,
0.0796375144754899));
#90246=CARTESIAN_POINT('Ctrl Pts',(0.010625755092144,-0.0345846629175835,
0.0796040781161031));
#90247=CARTESIAN_POINT('Ctrl Pts',(0.0107006972813125,-0.034474692504983,
0.0795690722402047));
#90248=CARTESIAN_POINT('Ctrl Pts',(0.0107748650971756,-0.0343648066252516,
0.0795325420979245));
#90249=CARTESIAN_POINT('',(0.0105618502623488,-0.0346775396663675,0.0796323192236938));
#90250=CARTESIAN_POINT('',(0.0105501343689865,-0.0346945769586885,0.0796375144754808));
#90251=CARTESIAN_POINT('Origin',(0.00367662592449391,-0.0345626617272025,
0.0645258111618288));
#90252=CARTESIAN_POINT('Ctrl Pts',(0.010561850260972,-0.0346775396659522,
0.0796323192206047));
#90253=CARTESIAN_POINT('Ctrl Pts',(0.0105443943775465,-0.034626974852986,
0.0795930673529158));
#90254=CARTESIAN_POINT('Ctrl Pts',(0.0105272488665522,-0.0345757904818561,
0.0795545133987788));
#90255=CARTESIAN_POINT('Ctrl Pts',(0.0104935638856951,-0.0344721679344753,
0.0794787682543209));
#90256=CARTESIAN_POINT('Ctrl Pts',(0.0104770379896808,-0.0344197716860446,
0.0794416075865975));
#90257=CARTESIAN_POINT('Ctrl Pts',(0.0104608161270357,-0.034366772783195,
0.0794051305782049));
#90258=CARTESIAN_POINT('',(0.0103965362219774,-0.0346945769587026,0.0795671120284798));
#90259=CARTESIAN_POINT('Ctrl Pts',(0.00823716696603865,-0.0321934096636942,
0.0799002417026225));
#90260=CARTESIAN_POINT('Ctrl Pts',(0.00834009355419282,-0.0320508460844559,
0.079898212169182));
#90261=CARTESIAN_POINT('Ctrl Pts',(0.00844288800580094,-0.0319086045663539,
0.079893418731684));
#90262=CARTESIAN_POINT('Ctrl Pts',(0.00854532983602395,-0.0317669892868596,
0.0798858899328736));
#90263=CARTESIAN_POINT('Ctrl Pts',(0.00832094259117809,-0.0321934096636942,
0.0798967664673334));
#90264=CARTESIAN_POINT('Ctrl Pts',(0.00842380697427553,-0.0320508460844559,
0.0798932373900978));
#90265=CARTESIAN_POINT('Ctrl Pts',(0.00852649897794681,-0.0319086045663539,
0.0798869472107927));
#90266=CARTESIAN_POINT('Ctrl Pts',(0.00862879860325792,-0.0317669892868596,
0.0798779276767516));
#90267=CARTESIAN_POINT('Ctrl Pts',(0.00840471821631753,-0.0321934096636942,
0.0798932912320445));
#90268=CARTESIAN_POINT('Ctrl Pts',(0.00850752039435823,-0.0320508460844559,
0.0798882626110136));
#90269=CARTESIAN_POINT('Ctrl Pts',(0.00861010995009268,-0.0319086045663539,
0.0798804756899015));
#90270=CARTESIAN_POINT('Ctrl Pts',(0.0087122673704919,-0.0317669892868596,
0.0798699654206294));
#90271=CARTESIAN_POINT('Ctrl Pts',(0.00848849384145697,-0.0321934096636942,
0.0798898159967555));
#90272=CARTESIAN_POINT('Ctrl Pts',(0.00859123381444095,-0.0320508460844559,
0.0798832878319295));
#90273=CARTESIAN_POINT('Ctrl Pts',(0.00869372092223854,-0.0319086045663539,
0.0798740041690102));
#90274=CARTESIAN_POINT('Ctrl Pts',(0.00879573613772587,-0.0317669892868596,
0.0798620031645074));
#90275=CARTESIAN_POINT('',(0.00848699507896817,-0.0321934096636943,0.0798898781693993));
#90276=CARTESIAN_POINT('',(0.00872250888832501,-0.0318665617511176,0.0798701093812739));
#90277=CARTESIAN_POINT('Origin',(0.00804615423106609,-0.0326371944421524,
0.0631858797206531));
#90278=CARTESIAN_POINT('Origin',(0.00986358784496523,-0.0316939261509064,
0.09077173903016));
#90279=CARTESIAN_POINT('',(0.00836242081836886,-0.0320197221621732,0.0798963589143967));
#90280=CARTESIAN_POINT('Ctrl Pts',(0.0083626014758925,-0.032019739209466,
0.0798963986351664));
#90281=CARTESIAN_POINT('Ctrl Pts',(0.00839184099761886,-0.0319792716575958,
0.0798951833989777));
#90282=CARTESIAN_POINT('Ctrl Pts',(0.00842120436430534,-0.0319386439829634,
0.0798937397202264));
#90283=CARTESIAN_POINT('Ctrl Pts',(0.00845072198661272,-0.0318979099381565,
0.0798920576360069));
#90284=CARTESIAN_POINT('Ctrl Pts',(0.00848023902548181,-0.0318571766984891,
0.079890375585035));
#90285=CARTESIAN_POINT('Ctrl Pts',(0.00850976039037138,-0.0318163871833566,
0.0798884654661008));
#90286=CARTESIAN_POINT('Ctrl Pts',(0.00853918476730417,-0.0317755399638303,
0.0798863373630329));
#90287=CARTESIAN_POINT('',(0.00836210249096908,-0.0321934096636184,0.0798950590454431));
#90288=CARTESIAN_POINT('Origin',(0.00847876190393271,-0.0324111959063637,
0.0821999623964788));
#90289=CARTESIAN_POINT('',(0.00842454878497862,-0.0321934096636663,0.0798924686074312));
#90290=CARTESIAN_POINT('Ctrl Pts',(0.00848550269921074,-0.0321934096636619,
0.0798885046738444));
#90291=CARTESIAN_POINT('Ctrl Pts',(0.00860414169261537,-0.0320287467381911,
0.0798810263917523));
#90292=CARTESIAN_POINT('Ctrl Pts',(0.00872237022849805,-0.0318646057455573,
0.079868651062983));
#90293=CARTESIAN_POINT('Ctrl Pts',(0.00848699507888224,-0.0321934096636619,
0.0798898781694046));
#90294=CARTESIAN_POINT('Ctrl Pts',(0.0086056624682088,-0.0320287467381911,
0.0798823690335567));
#90295=CARTESIAN_POINT('Ctrl Pts',(0.00872391810054128,-0.0318646057455573,
0.0798699617037712));
#90296=CARTESIAN_POINT('Ctrl Pts',(0.00873564501098324,-0.0321934096636619,
0.0801187204568708));
#90297=CARTESIAN_POINT('Ctrl Pts',(0.00885904353153239,-0.0320287467381911,
0.0801060706825933));
#90298=CARTESIAN_POINT('Ctrl Pts',(0.00898181378606981,-0.0318646057455573,
0.0800883315658226));
#90299=CARTESIAN_POINT('Ctrl Pts',(0.00874839290636016,-0.0321763980313108,
0.0801173998891418));
#90300=CARTESIAN_POINT('Ctrl Pts',(0.00874392497408026,-0.0321259597686371,
0.0800747143334848));
#90301=CARTESIAN_POINT('Ctrl Pts',(0.00873953437589611,-0.0320749162466965,
0.0800327679795527));
#90302=CARTESIAN_POINT('Ctrl Pts',(0.00873090466420057,-0.0319716059708271,
0.0799503214831995));
#90303=CARTESIAN_POINT('Ctrl Pts',(0.00872666881486074,-0.0319193783877868,
0.0799098524679891));
#90304=CARTESIAN_POINT('Ctrl Pts',(0.00872250888809975,-0.0318665617525138,
0.079870109379442));
#90305=CARTESIAN_POINT('',(0.00861132004499518,-0.0321934096636664,0.0800042993131371));
#90306=CARTESIAN_POINT('Ctrl Pts',(0.00855950338579825,-0.0327445246967097,
0.0798848853229917));
#90307=CARTESIAN_POINT('Ctrl Pts',(0.00877579812169474,-0.0324436878339361,
0.0798684518295582));
#90308=CARTESIAN_POINT('Ctrl Pts',(0.0089902405492005,-0.0321434074405928,
0.0798357728184288));
#90309=CARTESIAN_POINT('Ctrl Pts',(0.00856201626890479,-0.0327445246967097,
0.0798846382531779));
#90310=CARTESIAN_POINT('Ctrl Pts',(0.00877830168641091,-0.0324436878339361,
0.0798681099848087));
#90311=CARTESIAN_POINT('Ctrl Pts',(0.00899272768316337,-0.0321434074405928,
0.0798353371698884));
#90312=CARTESIAN_POINT('Ctrl Pts',(0.00881081657648191,-0.0327445246967097,
0.0798601758953698));
#90313=CARTESIAN_POINT('Ctrl Pts',(0.00902617938108062,-0.0324436878339361,
0.0798342639699983));
#90314=CARTESIAN_POINT('Ctrl Pts',(0.0092389785705746,-0.0321434074405928,
0.0797922036510292));
#90315=CARTESIAN_POINT('Ctrl Pts',(0.00881330457955768,-0.0327445246967097,
0.0798599312717918));
#90316=CARTESIAN_POINT('Ctrl Pts',(0.00902865815802732,-0.0324436878339361,
0.0798339255098502));
#90317=CARTESIAN_POINT('Ctrl Pts',(0.00924144107944872,-0.0321434074405928,
0.0797917723158406));
#90318=CARTESIAN_POINT('',(0.00884668829354451,-0.0326943950436612,0.0798557455051863));
#90319=CARTESIAN_POINT('',(0.00908049607793287,-0.0323666188837389,0.0798212276927121));
#90320=CARTESIAN_POINT('Origin',(0.00665828205650578,-0.0326395579111469,
0.0631878441266393));
#90321=CARTESIAN_POINT('Origin',(0.0109177201753066,-0.0321933825603152,
0.0907119567516225));
#90322=CARTESIAN_POINT('',(0.00895701164822238,-0.0321934096536378,0.0798406813014275));
#90323=CARTESIAN_POINT('',(0.00901864086939592,-0.0321934096584275,0.0798302846934935));
#90324=CARTESIAN_POINT('',(0.00872250888842273,-0.0325210109756239,0.0798701093821988));
#90325=CARTESIAN_POINT('Origin',(0.0071378099786331,-0.0326393129158301,
0.0631526674044951));
#90326=CARTESIAN_POINT('',(0.00872236746249035,-0.0326943950436594,0.0798687582284338));
#90327=CARTESIAN_POINT('Origin',(0.00987398789441971,-0.0326943765538268,
0.0908711073916663));
#90328=CARTESIAN_POINT('',(0.00878452787802743,-0.0326943950436703,0.07986225186682));
#90329=CARTESIAN_POINT('Ctrl Pts',(0.00851401032725098,-0.0325229783203769,
0.0801372967191685));
#90330=CARTESIAN_POINT('Ctrl Pts',(0.00859654508159117,-0.0324130253092451,
0.0801319174328731));
#90331=CARTESIAN_POINT('Ctrl Pts',(0.00867895604047152,-0.0323031222208071,
0.0801248316250349));
#90332=CARTESIAN_POINT('Ctrl Pts',(0.00876113796158937,-0.0321934096576659,
0.0801160520970259));
#90333=CARTESIAN_POINT('Ctrl Pts',(0.00858345380195833,-0.0325229783203769,
0.0800477492677418));
#90334=CARTESIAN_POINT('Ctrl Pts',(0.00866475414663888,-0.0324130253092451,
0.0800414127046661));
#90335=CARTESIAN_POINT('Ctrl Pts',(0.00874591108058209,-0.0323031222208071,
0.080033395300587));
#90336=CARTESIAN_POINT('Ctrl Pts',(0.00882682100991003,-0.0321934096576659,
0.0800237109935033));
#90337=CARTESIAN_POINT('Ctrl Pts',(0.00865289727666568,-0.0325229783203769,
0.079958201816315));
#90338=CARTESIAN_POINT('Ctrl Pts',(0.00873296321168659,-0.0324130253092451,
0.0799509079764592));
#90339=CARTESIAN_POINT('Ctrl Pts',(0.00881286612069266,-0.032303122220807,
0.0799419589761392));
#90340=CARTESIAN_POINT('Ctrl Pts',(0.00889250405823068,-0.0321934096576659,
0.0799313698899808));
#90341=CARTESIAN_POINT('Ctrl Pts',(0.00872234075137304,-0.0325229783203769,
0.0798686543648883));
#90342=CARTESIAN_POINT('Ctrl Pts',(0.0088011722767343,-0.0324130253092451,
0.0798604032482522));
#90343=CARTESIAN_POINT('Ctrl Pts',(0.00887982116080323,-0.032303122220807,
0.0798505226516913));
#90344=CARTESIAN_POINT('Ctrl Pts',(0.00895818710655133,-0.0321934096576659,
0.0798390287864582));
#90345=CARTESIAN_POINT('',(0.00885907480225073,-0.0321934096584275,0.0799783666995701));
#90346=CARTESIAN_POINT('Ctrl Pts',(0.00874839290846872,-0.0322104233328921,
0.0801173998856049));
#90347=CARTESIAN_POINT('Ctrl Pts',(0.00874391892089375,-0.0322609421831179,
0.0800746563458506));
#90348=CARTESIAN_POINT('Ctrl Pts',(0.0087395254426463,-0.0323120888240345,
0.0800326819753405));
#90349=CARTESIAN_POINT('Ctrl Pts',(0.0087308956280255,-0.0324156524631809,
0.0799502345348557));
#90350=CARTESIAN_POINT('Ctrl Pts',(0.00872666283896298,-0.0324680267167311,
0.0799097953551453));
#90351=CARTESIAN_POINT('Ctrl Pts',(0.00872250888842266,-0.0325210109755913,
0.0798701093821553));
#90352=CARTESIAN_POINT('Origin',(0.000256974599154325,-0.0262834582511321,
0.0740206782313454));
#90353=CARTESIAN_POINT('Origin',(0.00384607110080342,-0.0342771004391969,
0.0855309532453021));
#90354=CARTESIAN_POINT('Ctrl Pts',(0.0088451129986142,-0.0326943950436605,
0.0798544687371118));
#90355=CARTESIAN_POINT('Ctrl Pts',(0.0089237312691255,-0.0325844576448134,
0.0798445274466939));
#90356=CARTESIAN_POINT('Ctrl Pts',(0.00900214950138914,-0.0324744968375323,
0.0798329594979849));
#90357=CARTESIAN_POINT('Ctrl Pts',(0.00908026742582625,-0.0323646534831894,
0.0798197810983539));
#90358=CARTESIAN_POINT('Ctrl Pts',(0.00893314756504952,-0.0326943950436605,
0.0799258202801583));
#90359=CARTESIAN_POINT('Ctrl Pts',(0.00901274919355104,-0.0325844576448134,
0.0799146657084206));
#90360=CARTESIAN_POINT('Ctrl Pts',(0.00909212576075179,-0.0324744968375323,
0.0799018640550705));
#90361=CARTESIAN_POINT('Ctrl Pts',(0.00917117579100079,-0.0323646534831894,
0.0798874331251075));
#90362=CARTESIAN_POINT('Ctrl Pts',(0.00902118213148483,-0.0326943950436605,
0.0799971718232049));
#90363=CARTESIAN_POINT('Ctrl Pts',(0.00910176711797658,-0.0325844576448134,
0.0799848039701473));
#90364=CARTESIAN_POINT('Ctrl Pts',(0.00918210202011443,-0.0324744968375323,
0.0799707686121561));
#90365=CARTESIAN_POINT('Ctrl Pts',(0.00926208415617532,-0.0323646534831894,
0.0799550851518611));
#90366=CARTESIAN_POINT('Ctrl Pts',(0.00910921669792015,-0.0326943950436605,
0.0800685233662514));
#90367=CARTESIAN_POINT('Ctrl Pts',(0.00919078504240212,-0.0325844576448134,
0.080054942231874));
#90368=CARTESIAN_POINT('Ctrl Pts',(0.00927207827947707,-0.0324744968375323,
0.0800396731692416));
#90369=CARTESIAN_POINT('Ctrl Pts',(0.00935299252134986,-0.0323646534831894,
0.0800227371786146));
#90370=CARTESIAN_POINT('Ctrl Pts',(0.00912185652095127,-0.0326773559987509,
0.0800664049536984));
#90371=CARTESIAN_POINT('Ctrl Pts',(0.0091147114014,-0.032626792258736,0.0800240499711801));
#90372=CARTESIAN_POINT('Ctrl Pts',(0.00910769292393254,-0.0325756109582124,
0.0799824457001378));
#90373=CARTESIAN_POINT('Ctrl Pts',(0.00909390328002329,-0.0324719985462383,
0.0799007031732955));
#90374=CARTESIAN_POINT('Ctrl Pts',(0.00908713764428535,-0.032419609162178,
0.0798605977025121));
#90375=CARTESIAN_POINT('Ctrl Pts',(0.00908049607792469,-0.0323666188837756,
0.079821227692664));
#90376=CARTESIAN_POINT('',(0.00897795249573675,-0.0326943950436703,0.0799621344357239));
#90377=CARTESIAN_POINT('Ctrl Pts',(0.00891880354331507,-0.0332451089994434,
0.0798462002512828));
#90378=CARTESIAN_POINT('Ctrl Pts',(0.00913363925068852,-0.0329451141710254,
0.0798162155304841));
#90379=CARTESIAN_POINT('Ctrl Pts',(0.0093456060607421,-0.0326442513127494,
0.079770133689378));
#90380=CARTESIAN_POINT('Ctrl Pts',(0.00892127127411304,-0.0332451089994434,
0.0798457998705782));
#90381=CARTESIAN_POINT('Ctrl Pts',(0.00913609188088116,-0.0329451141710254,
0.0798157220777897));
#90382=CARTESIAN_POINT('Ctrl Pts',(0.00934803662266587,-0.0326442513127494,
0.0797695485665407));
#90383=CARTESIAN_POINT('Ctrl Pts',(0.00916804435391047,-0.0332451089994434,
0.0798057618001041));
#90384=CARTESIAN_POINT('Ctrl Pts',(0.00938135490014477,-0.0329451141710254,
0.0797663768083373));
#90385=CARTESIAN_POINT('Ctrl Pts',(0.0095910928150431,-0.0326442513127494,
0.0797110362828126));
#90386=CARTESIAN_POINT('Ctrl Pts',(0.00917053676201642,-0.0332451089994434,
0.0798053574155923));
#90387=CARTESIAN_POINT('Ctrl Pts',(0.00938383205663933,-0.0329451141710254,
0.0797658784211159));
#90388=CARTESIAN_POINT('Ctrl Pts',(0.00959354768258612,-0.0326442513127494,
0.079710445308747));
#90389=CARTESIAN_POINT('',(0.00920352852806092,-0.0331951640388616,0.0797990948701679));
#90390=CARTESIAN_POINT('',(0.00943470756977919,-0.0328677532355042,0.079749964261194));
#90391=CARTESIAN_POINT('Origin',(0.00530526937757678,-0.0326402808281488,
0.0634946223833793));
#90392=CARTESIAN_POINT('Origin',(0.0119550957035538,-0.0326944278779005,
0.0905148157064891));
#90393=CARTESIAN_POINT('',(0.00931268830210941,-0.0326943950436593,0.0797771331301099));
#90394=CARTESIAN_POINT('',(0.00937354310086201,-0.0326943950436694,0.0797628873072233));
#90395=CARTESIAN_POINT('',(0.00908049607793007,-0.0330220786163546,0.0798212276927126));
#90396=CARTESIAN_POINT('Origin',(0.00576523519911172,-0.0326396682762719,
0.0633546792233742));
#90397=CARTESIAN_POINT('',(0.00908027009142097,-0.0331951640388588,0.079819888085349));
#90398=CARTESIAN_POINT('Origin',(0.0109153372257397,-0.0331952026560021,
0.0906978427710935));
#90399=CARTESIAN_POINT('',(0.00914189930975095,-0.0331951640388702,0.0798094914777685));
#90400=CARTESIAN_POINT('Ctrl Pts',(0.0088891867257789,-0.0330240426238172,
0.0801009794069052));
#90401=CARTESIAN_POINT('Ctrl Pts',(0.00897116726486732,-0.032914277406352,
0.0800904352137702));
#90402=CARTESIAN_POINT('Ctrl Pts',(0.00905297069631849,-0.0328043479726691,
0.080078190997226));
#90403=CARTESIAN_POINT('Ctrl Pts',(0.0091344917918614,-0.0326943950436593,
0.0800642595569548));
#90404=CARTESIAN_POINT('Ctrl Pts',(0.00895287040814085,-0.0330240426238172,
0.0800072482776819));
#90405=CARTESIAN_POINT('Ctrl Pts',(0.0090335597096064,-0.032914277406352,
0.0799958267797783));
#90406=CARTESIAN_POINT('Ctrl Pts',(0.00911405312336546,-0.0328043479726691,
0.0799827315145858));
#90407=CARTESIAN_POINT('Ctrl Pts',(0.00919424706935178,-0.0326943950436593,
0.0799679764182612));
#90408=CARTESIAN_POINT('Ctrl Pts',(0.0090165540905028,-0.0330240426238172,
0.0799135171484586));
#90409=CARTESIAN_POINT('Ctrl Pts',(0.00909595215434549,-0.032914277406352,
0.0799012183457865));
#90410=CARTESIAN_POINT('Ctrl Pts',(0.00917513555041244,-0.0328043479726691,
0.0798872720319455));
#90411=CARTESIAN_POINT('Ctrl Pts',(0.00925400234684215,-0.0326943950436593,
0.0798716932795675));
#90412=CARTESIAN_POINT('Ctrl Pts',(0.00908023777286475,-0.0330240426238172,
0.0798197860192353));
#90413=CARTESIAN_POINT('Ctrl Pts',(0.00915834459908457,-0.032914277406352,
0.0798066099117946));
#90414=CARTESIAN_POINT('Ctrl Pts',(0.00923621797745941,-0.0328043479726691,
0.0797918125493052));
#90415=CARTESIAN_POINT('Ctrl Pts',(0.00931375762433253,-0.0326943950436593,
0.0797754101408738));
#90416=CARTESIAN_POINT('',(0.00922359004699556,-0.0326943950436694,0.0799206963435421));
#90417=CARTESIAN_POINT('Ctrl Pts',(0.00912185652094892,-0.0327114338383315,
0.080066404953685));
#90418=CARTESIAN_POINT('Ctrl Pts',(0.00911471258984867,-0.032761987683083,
0.0800240570160902));
#90419=CARTESIAN_POINT('Ctrl Pts',(0.00910769469286847,-0.0328131562604049,
0.0799824561860719));
#90420=CARTESIAN_POINT('Ctrl Pts',(0.00909390506165631,-0.0329167375858767,
0.0799007137344954));
#90421=CARTESIAN_POINT('Ctrl Pts',(0.00908713882192933,-0.0329691088920617,
0.0798606046833739));
#90422=CARTESIAN_POINT('Ctrl Pts',(0.00908049607792491,-0.0330220786163187,
0.0798212276926652));
#90423=CARTESIAN_POINT('Ctrl Pts',(0.00920187590888759,-0.0331951640388604,
0.0797979193474506));
#90424=CARTESIAN_POINT('Ctrl Pts',(0.00931864302028713,-0.033030642201062,
0.0797756304510862));
#90425=CARTESIAN_POINT('Ctrl Pts',(0.00943438913148185,-0.0328657861914645,
0.0797485344929184));
#90426=CARTESIAN_POINT('Ctrl Pts',(0.00920352852805782,-0.0331951640388604,
0.0797990948701685));
#90427=CARTESIAN_POINT('Ctrl Pts',(0.00932031994263588,-0.033030642201062,
0.0797767718069623));
#90428=CARTESIAN_POINT('Ctrl Pts',(0.00943608892409072,-0.0328657861914645,
0.0797496407066721));
#90429=CARTESIAN_POINT('Ctrl Pts',(0.00947889932504337,-0.0331951640388604,
0.0799949685678302));
#90430=CARTESIAN_POINT('Ctrl Pts',(0.00959974030273804,-0.033030642201062,
0.0799669523899477));
#90431=CARTESIAN_POINT('Ctrl Pts',(0.0097193200845696,-0.0328657861914645,
0.0799339656670055));
#90432=CARTESIAN_POINT('Ctrl Pts',(0.00949138118876774,-0.0331781648286476,
0.0799920606784095));
#90433=CARTESIAN_POINT('Ctrl Pts',(0.00948158392494805,-0.0331276811546812,
0.0799502091289448));
#90434=CARTESIAN_POINT('Ctrl Pts',(0.0094719635364457,-0.0330765663497823,
0.0799091132965642));
#90435=CARTESIAN_POINT('Ctrl Pts',(0.00945306840235603,-0.0329730614463283,
0.0798283977204811));
#90436=CARTESIAN_POINT('Ctrl Pts',(0.00944380129521076,-0.0329207133374032,
0.0797888105828929));
#90437=CARTESIAN_POINT('Ctrl Pts',(0.00943470755815306,-0.0328677532289396,
0.0797499642728653));
#90438=CARTESIAN_POINT('',(0.00934121392655591,-0.0331951640388702,0.0798970317190041));
#90439=CARTESIAN_POINT('Origin',(0.00812378219310841,-0.0315241814719618,
0.07415));
#90440=CARTESIAN_POINT('',(0.0105618502623033,-0.0347116136489609,0.0796323192235916));
#90441=CARTESIAN_POINT('',(0.0105735550331357,-0.0346945769586885,0.0796270989613359));
#90442=CARTESIAN_POINT('Origin',(0.00363602083277754,-0.0345626704646042,
0.0645459177258107));
#90443=CARTESIAN_POINT('Origin',(0.00395570707162937,-0.034562661854009,
0.0644016995088073));
#90444=CARTESIAN_POINT('Origin',(0.00399783382564541,-0.0345626705763338,
0.0643850145551682));
#90445=CARTESIAN_POINT('Ctrl Pts',(0.0103103965557986,-0.0352450361874068,
0.0794695375978088));
#90446=CARTESIAN_POINT('Ctrl Pts',(0.0105110262084795,-0.0349452760959493,
0.0793870680838582));
#90447=CARTESIAN_POINT('Ctrl Pts',(0.0107048739522082,-0.034644428984174,
0.079289720610766));
#90448=CARTESIAN_POINT('Ctrl Pts',(0.0103127100929213,-0.0352450361874068,
0.0794685260786632));
#90449=CARTESIAN_POINT('Ctrl Pts',(0.0105133015955316,-0.0349452760959493,
0.0793859693082281));
#90450=CARTESIAN_POINT('Ctrl Pts',(0.0107071047250546,-0.034644428984174,
0.0792885377001574));
#90451=CARTESIAN_POINT('Ctrl Pts',(0.0105417731743749,-0.0352450361874068,
0.079368375668205));
#90452=CARTESIAN_POINT('Ctrl Pts',(0.0107385874422733,-0.0349452760959493,
0.0792771796418894));
#90453=CARTESIAN_POINT('Ctrl Pts',(0.0109279733237086,-0.034644428984174,
0.0791714178379282));
#90454=CARTESIAN_POINT('Ctrl Pts',(0.0105440638051894,-0.0352450361874068,
0.0793673741641004));
#90455=CARTESIAN_POINT('Ctrl Pts',(0.0107408403007407,-0.0349452760959493,
0.079276091745226));
#90456=CARTESIAN_POINT('Ctrl Pts',(0.0109301820096952,-0.034644428984174,
0.0791702466393059));
#90457=CARTESIAN_POINT('',(0.0105744508146227,-0.0351951634053328,0.0793531121081548));
#90458=CARTESIAN_POINT('',(0.0107861769035186,-0.0348678972925388,0.0792480172033822));
#90459=CARTESIAN_POINT('Origin',(0.00265878042524815,-0.0345636767885836,
0.0645968707624761));
#90460=CARTESIAN_POINT('Origin',(0.0159013235930254,-0.0346946199341236,
0.0890426209992575));
#90461=CARTESIAN_POINT('',(0.0106747477174434,-0.0346945769330289,0.0793046774770006));
#90462=CARTESIAN_POINT('',(0.0107301478665679,-0.0346945769458128,0.0792757452360809));
#90463=CARTESIAN_POINT('',(0.0104608161269358,-0.0350221583435276,0.0794051305780295));
#90464=CARTESIAN_POINT('Origin',(0.00306414635805795,-0.0345628458716434,
0.0643383715295872));
#90465=CARTESIAN_POINT('',(0.0104603107618279,-0.0351951360298763,0.079404001640984));
#90466=CARTESIAN_POINT('Origin',(0.0149378146759128,-0.0351951838366768,
0.089472258816035));
#90467=CARTESIAN_POINT('',(0.0105744790773254,-0.0351951371328746,0.0793530961727634));
#90468=CARTESIAN_POINT('Ctrl Pts',(0.0103450886693692,-0.0350241211494342,
0.0797236700241919));
#90469=CARTESIAN_POINT('Ctrl Pts',(0.0104218636886588,-0.0349144232818962,
0.0796930724382525));
#90470=CARTESIAN_POINT('Ctrl Pts',(0.0104980521875328,-0.0348045283579412,
0.0796608695436739));
#90471=CARTESIAN_POINT('Ctrl Pts',(0.0105735550432784,-0.0346945769439157,
0.079627098956804));
#90472=CARTESIAN_POINT('Ctrl Pts',(0.0103834616338616,-0.0350241211494342,
0.0796170461178704));
#90473=CARTESIAN_POINT('Ctrl Pts',(0.0104587679525591,-0.0349144232818962,
0.0795859199600787));
#90474=CARTESIAN_POINT('Ctrl Pts',(0.0105334759457951,-0.0348045283579412,
0.0795532185363627));
#90475=CARTESIAN_POINT('Ctrl Pts',(0.0106074883634341,-0.0346945769439157,
0.0795189801721901));
#90476=CARTESIAN_POINT('Ctrl Pts',(0.010421834598354,-0.0350241211494342,
0.0795104222115489));
#90477=CARTESIAN_POINT('Ctrl Pts',(0.0104956722164594,-0.0349144232818962,
0.0794787674819048));
#90478=CARTESIAN_POINT('Ctrl Pts',(0.0105688997040573,-0.0348045283579412,
0.0794455675290515));
#90479=CARTESIAN_POINT('Ctrl Pts',(0.0106414216835899,-0.0346945769439157,
0.0794108613875762));
#90480=CARTESIAN_POINT('Ctrl Pts',(0.0104602075628463,-0.0350241211494342,
0.0794037983052275));
#90481=CARTESIAN_POINT('Ctrl Pts',(0.0105325764803597,-0.0349144232818962,
0.079371615003731));
#90482=CARTESIAN_POINT('Ctrl Pts',(0.0106043234623195,-0.0348045283579412,
0.0793379165217403));
#90483=CARTESIAN_POINT('Ctrl Pts',(0.0106753550037457,-0.0346945769439157,
0.0793027426029622));
#90484=CARTESIAN_POINT('',(0.0106241513750694,-0.0346945769458128,0.0794658882193774));
#90485=CARTESIAN_POINT('Ctrl Pts',(0.010561850260961,-0.034711613649279,
0.0796323192205801));
#90486=CARTESIAN_POINT('Ctrl Pts',(0.0105444013634492,-0.0347621546531703,
0.0795930830616442));
#90487=CARTESIAN_POINT('Ctrl Pts',(0.010527259264707,-0.0348133084095802,
0.0795545367804084));
#90488=CARTESIAN_POINT('Ctrl Pts',(0.0104935743584344,-0.0349168561544574,
0.0794787918036634));
#90489=CARTESIAN_POINT('Ctrl Pts',(0.0104770449120557,-0.0349692089015921,
0.0794416231524752));
#90490=CARTESIAN_POINT('Ctrl Pts',(0.0104608161269391,-0.0350221583435,
0.0794051305779879));
#90491=CARTESIAN_POINT('Ctrl Pts',(0.0105731134580019,-0.0351951371254953,
0.079352571288223));
#90492=CARTESIAN_POINT('Ctrl Pts',(0.0106806733551835,-0.035030733898096,
0.0793019329010831));
#90493=CARTESIAN_POINT('Ctrl Pts',(0.0107860484038839,-0.0348659306897825,
0.0792468922175369));
#90494=CARTESIAN_POINT('Ctrl Pts',(0.0105744790772703,-0.0351951371254953,
0.0793530961726611));
#90495=CARTESIAN_POINT('Ctrl Pts',(0.0106820498261083,-0.035030733898096,
0.0793024295521997));
#90496=CARTESIAN_POINT('Ctrl Pts',(0.0107874345502788,-0.0348659306897825,
0.0792473602109466));
#90497=CARTESIAN_POINT('Ctrl Pts',(0.0108033582899396,-0.0351951371254953,
0.0794410673515482));
#90498=CARTESIAN_POINT('Ctrl Pts',(0.0109127477877062,-0.035030733898096,
0.0793856687969685));
#90499=CARTESIAN_POINT('Ctrl Pts',(0.0110197541307519,-0.0348659306897825,
0.0793257963941513));
#90500=CARTESIAN_POINT('Origin',(0.0132480472269558,-0.0308609197411241,
0.0839620655045698));
#90501=CARTESIAN_POINT('',(0.0106742652534521,-0.0351951371254953,0.0793914496231688));
#90502=CARTESIAN_POINT('Origin',(0.00755074467756133,-0.035184046744115,
0.0733585622856818));
#90503=CARTESIAN_POINT('Origin',(0.0143548902956506,-0.0352322613037122,
0.0843647549503665));
#90504=CARTESIAN_POINT('',(0.0109936380460948,-0.0351951142564684,0.0791341490714577));
#90505=CARTESIAN_POINT('',(0.0111003272121345,-0.0351951372916787,0.0790696219112562));
#90506=CARTESIAN_POINT('Origin',(0.00827955227021354,-0.0352875117694839,
0.0738471516112963));
#90507=CARTESIAN_POINT('Origin',(0.00107941703142758,-0.0298325076523859,
0.0767330427301951));
#90508=CARTESIAN_POINT('Origin',(0.0094440988976966,-0.0338732150591158,
0.082426931938526));
#90509=CARTESIAN_POINT('Origin',(0.00812378219310841,-0.0315241814719618,
0.07415));
#90510=CARTESIAN_POINT('',(0.00874839290879345,-0.0332121607144206,0.0801173998886622));
#90511=CARTESIAN_POINT('',(0.00876113795713088,-0.0331951640388587,0.0801160520975017));
#90512=CARTESIAN_POINT('Origin',(0.00627798841830207,-0.0326413635833112,
0.0637867391944952));
#90513=CARTESIAN_POINT('',(0.00874839290831179,-0.0331781648281947,0.0801173998902725));
#90514=CARTESIAN_POINT('Origin',(0.00773838482252226,-0.0326412105611727,
0.0636259931678058));
#90515=CARTESIAN_POINT('',(0.00873564501100219,-0.0331951640388588,0.080118720456855));
#90516=CARTESIAN_POINT('Origin',(0.00632159444987085,-0.0326412092830655,
0.0637742933550843));
#90517=CARTESIAN_POINT('Origin',(0.0077836230719809,-0.0326413653378089,
0.0636291472617185));
#90518=CARTESIAN_POINT('Origin',(0.00812378219310841,-0.0315241814719618,
0.07415));
#90519=CARTESIAN_POINT('',(0.00912185652157204,-0.0337108120655696,0.0800664049573521));
#90520=CARTESIAN_POINT('',(0.00913449179186386,-0.0336938721132327,0.0800642595569508));
#90521=CARTESIAN_POINT('Origin',(0.00750227557297375,-0.0345562530068284,
0.0637472403724542));
#90522=CARTESIAN_POINT('',(0.00912185652178286,-0.033676936124379,0.080066404958628));
#90523=CARTESIAN_POINT('Ctrl Pts',(0.00913449179186099,-0.0336938721132359,
0.0800642595569588));
#90524=CARTESIAN_POINT('Ctrl Pts',(0.0091323864415022,-0.0336910493107781,
0.080064619348036));
#90525=CARTESIAN_POINT('Ctrl Pts',(0.0091302808391578,-0.0336882265931775,
0.0800649780251539));
#90526=CARTESIAN_POINT('Ctrl Pts',(0.00912606908823685,-0.0336825812712327,
0.080065693158239));
#90527=CARTESIAN_POINT('Ctrl Pts',(0.00912396293972832,-0.0336797586669777,
0.080066049614173));
#90528=CARTESIAN_POINT('Ctrl Pts',(0.00912185652178378,-0.0336769361243774,
0.0800664049586247));
#90529=CARTESIAN_POINT('',(0.009109216697909,-0.0336938721132328,0.0800685233662416));
#90530=CARTESIAN_POINT('Ctrl Pts',(0.00912185652178066,-0.0336769361243777,
0.0800664049586253));
#90531=CARTESIAN_POINT('Ctrl Pts',(0.00911975010381738,-0.0336797586670032,
0.0800667603030801));
#90532=CARTESIAN_POINT('Ctrl Pts',(0.00911764357575037,-0.0336825812712832,
0.0800671145091738));
#90533=CARTESIAN_POINT('Ctrl Pts',(0.00911343031216495,-0.0336882265860984,
0.0800678206430221));
#90534=CARTESIAN_POINT('Ctrl Pts',(0.00911132357667191,-0.0336910492966202,
0.0800681725708117));
#90535=CARTESIAN_POINT('Ctrl Pts',(0.00910921669791881,-0.0336938721132386,
0.0800685233662538));
#90536=CARTESIAN_POINT('Origin',(0.00529820345362548,-0.0345562530596106,
0.0641190585384484));
#90537=CARTESIAN_POINT('Origin',(0.00812378219310841,-0.0315241814719618,
0.07415));
#90538=CARTESIAN_POINT('',(0.00837246424298519,-0.0327114338379848,0.0801448442196473));
#90539=CARTESIAN_POINT('',(0.00838526877037963,-0.0326943950436593,0.0801442993560501));
#90540=CARTESIAN_POINT('Origin',(0.00758879780582063,-0.0326395653650527,
0.0635587003231629));
#90541=CARTESIAN_POINT('',(0.008372464242277,-0.0326773559992502,0.0801448442207892));
#90542=CARTESIAN_POINT('Origin',(0.00773442609091764,-0.0326395686091014,
0.063551883863096));
#90543=CARTESIAN_POINT('',(0.00835965858108669,-0.0326943950436595,0.0801453617346741));
#90544=CARTESIAN_POINT('Origin',(0.00763403304173427,-0.0326395669694838,
0.0635560519265562));
#90545=CARTESIAN_POINT('Origin',(0.00777972546240625,-0.0326395670659013,
0.063550783508722));
#90546=CARTESIAN_POINT('Origin',(0.00812378219310841,-0.0315241814719618,
0.07415));
#90547=CARTESIAN_POINT('',(0.00799555414271255,-0.032210423332359,0.0801486296392922));
#90548=CARTESIAN_POINT('',(0.00800836761556929,-0.0321934096636183,0.0801488898535757));
#90549=CARTESIAN_POINT('Origin',(0.00891757153313832,-0.0326387221312259,
0.0636219243157334));
#90550=CARTESIAN_POINT('',(0.00799555414184183,-0.0321763980308046,0.0801486296399426));
#90551=CARTESIAN_POINT('Origin',(0.00773559231001018,-0.0326386251174431,
0.0636029764171086));
#90552=CARTESIAN_POINT('',(0.0079827412548295,-0.0321934096636185,0.0801483420587467));
#90553=CARTESIAN_POINT('Origin',(0.00896231991809475,-0.0326386231523553,
0.0636292029887929));
#90554=CARTESIAN_POINT('Origin',(0.00778061111138152,-0.0326387237755826,
0.0635976246480955));
#90555=CARTESIAN_POINT('Origin',(0.00812378219310841,-0.0315241814719618,
0.07415));
#90556=CARTESIAN_POINT('',(0.0098555085716382,-0.0347116136489614,0.0798946604537853));
#90557=CARTESIAN_POINT('',(0.00986777531920451,-0.0346945769586885,0.0798909483516342));
#90558=CARTESIAN_POINT('Origin',(0.00487511900430214,-0.0345626705531907,
0.0640591832160391));
#90559=CARTESIAN_POINT('',(0.00985550857127204,-0.0346775396665025,0.0798946604551301));
#90560=CARTESIAN_POINT('Origin',(0.00521035946764333,-0.0345626618993397,
0.063956169170596));
#90561=CARTESIAN_POINT('',(0.00984323392392057,-0.0346945769586886,0.0798983463487691));
#90562=CARTESIAN_POINT('Origin',(0.00491792381413625,-0.0345626617996805,
0.0640443240441348));
#90563=CARTESIAN_POINT('Origin',(0.00525424527900612,-0.0345626706176323,
0.0639448958454014));
#90564=CARTESIAN_POINT('Origin',(0.00812378219310841,-0.0315241814719618,
0.07415));
#90565=CARTESIAN_POINT('',(0.00949138119084094,-0.0342105180190372,0.0799920606778171));
#90566=CARTESIAN_POINT('',(0.00950385681755749,-0.0341934961088739,0.0799891261359002));
#90567=CARTESIAN_POINT('Origin',(0.00617091115087495,-0.0345621724038967,
0.0637586100252421));
#90568=CARTESIAN_POINT('',(0.00949138119077186,-0.0341764758832668,0.0799920606775218));
#90569=CARTESIAN_POINT('Origin',(0.00521870190545053,-0.0345621027020113,
0.0639868884251929));
#90570=CARTESIAN_POINT('',(0.00947889932502756,-0.034193496108874,0.0799949685678179));
#90571=CARTESIAN_POINT('Origin',(0.00621593979425685,-0.0345621027111292,
0.0637534398504798));
#90572=CARTESIAN_POINT('Origin',(0.00526134665942937,-0.0345621724286372,
0.0639715350338382));
#90573=CARTESIAN_POINT('Ctrl Pts',(0.00892119950492447,-0.034243627687391,
0.079845809918775));
#90574=CARTESIAN_POINT('Ctrl Pts',(0.0091360205173804,-0.0339430054201809,
0.0798157348290657));
#90575=CARTESIAN_POINT('Ctrl Pts',(0.00934796586687492,-0.0336441434784052,
0.0797695639806734));
#90576=CARTESIAN_POINT('Ctrl Pts',(0.00916797308919641,-0.034243627687391,
0.0798057749577337));
#90577=CARTESIAN_POINT('Ctrl Pts',(0.00938128415820492,-0.0339430054201809,
0.0797663926488621));
#90578=CARTESIAN_POINT('Ctrl Pts',(0.00959102279596063,-0.0336441434784052,
0.0797110547572688));
#90579=CARTESIAN_POINT('',(0.00920352852805892,-0.0341934961088741,0.0797990948701683));
#90580=CARTESIAN_POINT('',(0.00943470755858997,-0.0338664212895226,0.0797499642584328));
#90581=CARTESIAN_POINT('Origin',(0.00656379352345093,-0.0345610818076477,
0.0632738144364997));
#90582=CARTESIAN_POINT('Origin',(0.0119343541146342,-0.0336938005044268,
0.090427534726314));
#90583=CARTESIAN_POINT('',(0.00931268830210938,-0.0336938721132327,0.07977713313011));
#90584=CARTESIAN_POINT('',(0.00937354310086199,-0.0336938721132427,0.0797628873072233));
#90585=CARTESIAN_POINT('',(0.00908049607792758,-0.0340203938281605,0.079821227692713));
#90586=CARTESIAN_POINT('Origin',(0.00704495936124007,-0.0345589643245042,
0.0632720726151595));
#90587=CARTESIAN_POINT('Origin',(0.01091330714871,-0.0341934220717635,0.0906858069796352));
#90588=CARTESIAN_POINT('',(0.0091418993097499,-0.0341934961088841,0.0798094914777686));
#90589=CARTESIAN_POINT('Ctrl Pts',(0.00888918496513205,-0.0340223579322396,
0.0801009796333548));
#90590=CARTESIAN_POINT('Ctrl Pts',(0.00897126449508248,-0.0339125849573575,
0.0800904227328744));
#90591=CARTESIAN_POINT('Ctrl Pts',(0.00905306784538844,-0.0338030433565231,
0.0800781743950622));
#90592=CARTESIAN_POINT('Ctrl Pts',(0.00913449179186244,-0.0336938721132327,
0.0800642595569531));
#90593=CARTESIAN_POINT('Ctrl Pts',(0.00895286878394797,-0.0340223579322396,
0.0800072483629521));
#90594=CARTESIAN_POINT('Ctrl Pts',(0.00903365551521813,-0.0339125849573575,
0.0799958130965159));
#90595=CARTESIAN_POINT('Ctrl Pts',(0.00911414879514424,-0.0338030433565231,
0.0799827137678941));
#90596=CARTESIAN_POINT('Ctrl Pts',(0.0091942471713689,-0.0336938721132327,
0.0799679762538819));
#90597=CARTESIAN_POINT('Ctrl Pts',(0.00901655260276389,-0.0340223579322396,
0.0799135170925495));
#90598=CARTESIAN_POINT('Ctrl Pts',(0.00909604653535378,-0.0339125849573575,
0.0799012034601574));
#90599=CARTESIAN_POINT('Ctrl Pts',(0.00917522974490004,-0.0338030433565231,
0.079887253140726));
#90600=CARTESIAN_POINT('Ctrl Pts',(0.00925400255087535,-0.0336938721132326,
0.0798716929508106));
#90601=CARTESIAN_POINT('Ctrl Pts',(0.00908023642157981,-0.0340223579322396,
0.0798197858221469));
#90602=CARTESIAN_POINT('Ctrl Pts',(0.00915843755548943,-0.0339125849573575,
0.0798065938237989));
#90603=CARTESIAN_POINT('Ctrl Pts',(0.00923631069465584,-0.0338030433565231,
0.0797917925135579));
#90604=CARTESIAN_POINT('Ctrl Pts',(0.00931375793038181,-0.0336938721132326,
0.0797754096477394));
#90605=CARTESIAN_POINT('',(0.00922359004699662,-0.0336938721132427,0.0799206963435404));
#90606=CARTESIAN_POINT('Ctrl Pts',(0.00912185652096689,-0.0337108120662708,
0.0800664049537917));
#90607=CARTESIAN_POINT('Ctrl Pts',(0.00911470377868284,-0.0337611408994039,
0.0800240047850855));
#90608=CARTESIAN_POINT('Ctrl Pts',(0.00910768155807646,-0.033812108878075,
0.0799823783253896));
#90609=CARTESIAN_POINT('Ctrl Pts',(0.00909389176307279,-0.0339153382773247,
0.0799006349028868));
#90610=CARTESIAN_POINT('Ctrl Pts',(0.00908713002261463,-0.0339675558473124,
0.0798605525226209));
#90611=CARTESIAN_POINT('Ctrl Pts',(0.00908049607792608,-0.0340203938281304,
0.0798212276926728));
#90612=CARTESIAN_POINT('Ctrl Pts',(0.0092018758347171,-0.0341934961088741,
0.0797979192946915));
#90613=CARTESIAN_POINT('Ctrl Pts',(0.00927975729708932,-0.0340836138583034,
0.0797830530218215));
#90614=CARTESIAN_POINT('Ctrl Pts',(0.00935729376414901,-0.0339738896647348,
0.0797665822886252));
#90615=CARTESIAN_POINT('Ctrl Pts',(0.00943438741192324,-0.0338644633299819,
0.0797485348279564));
#90616=CARTESIAN_POINT('Ctrl Pts',(0.00929421699815897,-0.0341934961088741,
0.0798636023857373));
#90617=CARTESIAN_POINT('Ctrl Pts',(0.00937300419145915,-0.0340836138583034,
0.0798474627829079));
#90618=CARTESIAN_POINT('Ctrl Pts',(0.00945141960596841,-0.0339738896647348,
0.0798297005885188));
#90619=CARTESIAN_POINT('Ctrl Pts',(0.00952936440357235,-0.0338644633299819,
0.0798103452637452));
#90620=CARTESIAN_POINT('Ctrl Pts',(0.00938655816160085,-0.0341934961088741,
0.079929285476783));
#90621=CARTESIAN_POINT('Ctrl Pts',(0.00946625108582898,-0.0340836138583034,
0.0799118725439943));
#90622=CARTESIAN_POINT('Ctrl Pts',(0.00954554544778781,-0.0339738896647348,
0.0798928188884124));
#90623=CARTESIAN_POINT('Ctrl Pts',(0.00962434139522147,-0.0338644633299819,
0.0798721556995341));
#90624=CARTESIAN_POINT('Ctrl Pts',(0.00947889932504273,-0.0341934961088741,
0.0799949685678288));
#90625=CARTESIAN_POINT('Ctrl Pts',(0.00955949798019881,-0.0340836138583034,
0.0799762823050806));
#90626=CARTESIAN_POINT('Ctrl Pts',(0.00963967128960721,-0.0339738896647348,
0.079955937188306));
#90627=CARTESIAN_POINT('Ctrl Pts',(0.00971931838687058,-0.0338644633299819,
0.0799339661353229));
#90628=CARTESIAN_POINT('Ctrl Pts',(0.00949138119003726,-0.0341764758830281,
0.0799920606744016));
#90629=CARTESIAN_POINT('Ctrl Pts',(0.00948159726840954,-0.0341260048548333,
0.0799502660665442));
#90630=CARTESIAN_POINT('Ctrl Pts',(0.00947198350155604,-0.0340749271293304,
0.0799091983197897));
#90631=CARTESIAN_POINT('Ctrl Pts',(0.009453088468083,-0.033971543442926,
0.0798284831889346));
#90632=CARTESIAN_POINT('Ctrl Pts',(0.00944381459525593,-0.0339192781035265,
0.0797888673893735));
#90633=CARTESIAN_POINT('Ctrl Pts',(0.0094347075555425,-0.0338664212877434,
0.0797499642615637));
#90634=CARTESIAN_POINT('',(0.00934121392655325,-0.0341934961088841,0.0798970317190032));
#90635=CARTESIAN_POINT('Ctrl Pts',(0.00931122777606145,-0.0346945769586966,
0.0797774750324058));
#90636=CARTESIAN_POINT('Ctrl Pts',(0.00948807830358499,-0.0344439193968194,
0.0797401580516033));
#90637=CARTESIAN_POINT('Ctrl Pts',(0.00966223670437822,-0.0341934961088739,
0.0796918101708358));
#90638=CARTESIAN_POINT('Ctrl Pts',(0.00931268830210382,-0.0346945769586966,
0.0797771331301111));
#90639=CARTESIAN_POINT('Ctrl Pts',(0.00948952808491488,-0.0344439193968194,
0.0797397702504286));
#90640=CARTESIAN_POINT('Ctrl Pts',(0.00966367288018335,-0.0341934961088739,
0.0796913772360181));
#90641=CARTESIAN_POINT('Ctrl Pts',(0.00955610749707416,-0.0346945769586966,
0.079720149838525));
#90642=CARTESIAN_POINT('Ctrl Pts',(0.00973115650780379,-0.0344439193968194,
0.0796751372024612));
#90643=CARTESIAN_POINT('Ctrl Pts',(0.009903033732493,-0.0341934961088739,
0.0796192219702256));
#90644=CARTESIAN_POINT('Ctrl Pts',(0.00955708048208011,-0.0346945769586966,
0.0797199220672997));
#90645=CARTESIAN_POINT('Ctrl Pts',(0.00973212233481061,-0.0344439193968194,
0.0796748788539503));
#90646=CARTESIAN_POINT('Ctrl Pts',(0.00990399049566172,-0.0341934961088739,
0.0796189335542208));
#90647=CARTESIAN_POINT('',(0.00955610749708528,-0.0346945769586966,0.0797201498385222));
#90648=CARTESIAN_POINT('',(0.00978374540824895,-0.0343667727783613,0.0796566003227611));
#90649=CARTESIAN_POINT('Origin',(0.00519187396474237,-0.0345626461564454,
0.0634828251698361));
#90650=CARTESIAN_POINT('Origin',(0.0129736430949094,-0.0341934771027892,
0.0902384341944277));
#90651=CARTESIAN_POINT('',(0.00966367288018327,-0.034193496108874,0.0796913772360182));
#90652=CARTESIAN_POINT('',(0.0097235130932707,-0.034193496108884,0.0796733384195801));
#90653=CARTESIAN_POINT('',(0.00943470755461163,-0.0345211943011844,0.0797499642575745));
#90654=CARTESIAN_POINT('Origin',(0.00566078612732884,-0.0345625596119786,
0.0633764692885998));
#90655=CARTESIAN_POINT('Origin',(0.0119561510488986,-0.0346945685853894,
0.0905209799622138));
#90656=CARTESIAN_POINT('',(0.0094952526983499,-0.0346945769587026,0.0797343956614295));
#90657=CARTESIAN_POINT('Ctrl Pts',(0.00926134066521218,-0.0345231616327842,
0.0800411765142948));
#90658=CARTESIAN_POINT('Ctrl Pts',(0.00934254223934864,-0.0344132092796988,
0.080025496872311));
#90659=CARTESIAN_POINT('Ctrl Pts',(0.00942341530283064,-0.034303273855898,
0.0800081384488146));
#90660=CARTESIAN_POINT('Ctrl Pts',(0.00950385681755585,-0.034193496108874,
0.0799891261359033));
#90661=CARTESIAN_POINT('Ctrl Pts',(0.00931901326963669,-0.0345231616327842,
0.0799436316177729));
#90662=CARTESIAN_POINT('Ctrl Pts',(0.00939887032470682,-0.0344132092796988,
0.0799271570401337));
#90663=CARTESIAN_POINT('Ctrl Pts',(0.0094783824958765,-0.034303273855898,
0.0799090315323132));
#90664=CARTESIAN_POINT('Ctrl Pts',(0.00955744851367657,-0.034193496108874,
0.0798892809244735));
#90665=CARTESIAN_POINT('Ctrl Pts',(0.0093766858740612,-0.0345231616327842,
0.0798460867212511));
#90666=CARTESIAN_POINT('Ctrl Pts',(0.00945519841006501,-0.0344132092796988,
0.0798288172079564));
#90667=CARTESIAN_POINT('Ctrl Pts',(0.00953334968892237,-0.034303273855898,
0.0798099246158118));
#90668=CARTESIAN_POINT('Ctrl Pts',(0.00961104020979729,-0.034193496108874,
0.0797894357130436));
#90669=CARTESIAN_POINT('Ctrl Pts',(0.00943435847848571,-0.0345231616327842,
0.0797485418247292));
#90670=CARTESIAN_POINT('Ctrl Pts',(0.00951152649542319,-0.0344132092796988,
0.0797304773757791));
#90671=CARTESIAN_POINT('Ctrl Pts',(0.00958831688196824,-0.034303273855898,
0.0797108176993104));
#90672=CARTESIAN_POINT('Ctrl Pts',(0.00966463190591801,-0.034193496108874,
0.0796895905016138));
#90673=CARTESIAN_POINT('',(0.00958376484888037,-0.0341934961088839,0.0798402516859692));
#90674=CARTESIAN_POINT('Ctrl Pts',(0.00949138119004756,-0.0342105180195399,
0.0799920606744457));
#90675=CARTESIAN_POINT('Ctrl Pts',(0.00948158630167239,-0.034261055624461,
0.0799502192192273));
#90676=CARTESIAN_POINT('Ctrl Pts',(0.00947196717751276,-0.0343122189876677,
0.0799091285872833));
#90677=CARTESIAN_POINT('Ctrl Pts',(0.00945307250016098,-0.0344158093694418,
0.0798284149776943));
#90678=CARTESIAN_POINT('Ctrl Pts',(0.00944380326859656,-0.0344682017128875,
0.0797888190045534));
#90679=CARTESIAN_POINT('Ctrl Pts',(0.00943470755419452,-0.0345211942998157,
0.0797499642558054));
#90680=CARTESIAN_POINT('Ctrl Pts',(0.00955438467010664,-0.0346945769586932,
0.079719080617007));
#90681=CARTESIAN_POINT('Ctrl Pts',(0.00966952147126994,-0.0345296777077528,
0.0796895039230667));
#90682=CARTESIAN_POINT('Ctrl Pts',(0.00978333745753671,-0.0343648066252515,
0.0796551937922497));
#90683=CARTESIAN_POINT('Ctrl Pts',(0.00955610749707654,-0.0346945769586932,
0.0797201498385244));
#90684=CARTESIAN_POINT('Ctrl Pts',(0.00967126640363815,-0.0345296777077528,
0.0796905375263556));
#90685=CARTESIAN_POINT('Ctrl Pts',(0.00978510300428032,-0.0343648066252515,
0.0796561908941089));
#90686=CARTESIAN_POINT('Ctrl Pts',(0.00984323392393309,-0.0346945769586932,
0.0798983463487799));
#90687=CARTESIAN_POINT('Ctrl Pts',(0.00996207691725521,-0.0345296777077528,
0.0798627979009019));
#90688=CARTESIAN_POINT('Ctrl Pts',(0.0100793491107082,-0.0343648066252515,
0.0798223679386087));
#90689=CARTESIAN_POINT('Ctrl Pts',(0.00985550856950412,-0.0346775396670096,
0.079894660454654));
#90690=CARTESIAN_POINT('Ctrl Pts',(0.00984310992023194,-0.0346269749924949,
0.0798535304275722));
#90691=CARTESIAN_POINT('Ctrl Pts',(0.00983093158822074,-0.0345757902884401,
0.0798131313832144));
#90692=CARTESIAN_POINT('Ctrl Pts',(0.0098070062949466,-0.0344721707091871,
0.0797337639320363));
#90693=CARTESIAN_POINT('Ctrl Pts',(0.00979526693812728,-0.034419768761444,
0.07969482073193));
#90694=CARTESIAN_POINT('Ctrl Pts',(0.00978374540745166,-0.0343667727795891,
0.0796566003212991));
#90695=CARTESIAN_POINT('',(0.00969967071051292,-0.0346945769587026,0.0798092480936557));
#90696=CARTESIAN_POINT('Ctrl Pts',(0.00962646358114103,-0.0352450361874068,
0.0797016398384676));
#90697=CARTESIAN_POINT('Ctrl Pts',(0.0098358471134729,-0.0349452760959493,
0.0796449652799317));
#90698=CARTESIAN_POINT('Ctrl Pts',(0.0100403668495881,-0.034644428984174,
0.079572680103468));
#90699=CARTESIAN_POINT('Ctrl Pts',(0.00962886167139528,-0.0352450361874068,
0.079700933323689));
#90700=CARTESIAN_POINT('Ctrl Pts',(0.00983821855708501,-0.0349452760959493,
0.0796441683196949));
#90701=CARTESIAN_POINT('Ctrl Pts',(0.0100427049095364,-0.034644428984174,
0.0795717949618532));
#90702=CARTESIAN_POINT('Ctrl Pts',(0.00986867070047367,-0.0352450361874068,
0.0796302818447427));
#90703=CARTESIAN_POINT('Ctrl Pts',(0.0100753629219099,-0.0349452760959493,
0.079564472294803));
#90704=CARTESIAN_POINT('Ctrl Pts',(0.0102765109079304,-0.034644428984174,
0.079483280799033));
#90705=CARTESIAN_POINT('',(0.00990300343087755,-0.0351951633467188,0.079619234032487));
#90706=CARTESIAN_POINT('',(0.0101262321451419,-0.0348678972925388,0.0795415043531098));
#90707=CARTESIAN_POINT('Origin',(0.00389834399728346,-0.034563163330209,
0.0639869625528435));
#90708=CARTESIAN_POINT('Origin',(0.0139734550134733,-0.034694619934117,
0.0898999726470576));
#90709=CARTESIAN_POINT('',(0.0100085801961753,-0.0346945769330289,0.0795837520633418));
#90710=CARTESIAN_POINT('',(0.0100671696698855,-0.0346945769458128,0.079561991441613));
#90711=CARTESIAN_POINT('',(0.00978374540818223,-0.0350221583435275,0.0796566003236664));
#90712=CARTESIAN_POINT('Origin',(0.004333766220623,-0.0345628458714157,
0.0637815986319168));
#90713=CARTESIAN_POINT('',(0.00978338552135528,-0.0351951360298762,0.079655416949585));
#90714=CARTESIAN_POINT('Origin',(0.0129636962171911,-0.0351951838366802,
0.0902054628140545));
#90715=CARTESIAN_POINT('',(0.00990303372741004,-0.0351951371328746,0.0796192219718791));
#90716=CARTESIAN_POINT('Ctrl Pts',(0.0096290069173802,-0.0350241211494342,
0.0799581234946824));
#90717=CARTESIAN_POINT('Ctrl Pts',(0.00970901143709608,-0.0349144232818961,
0.0799373896412717));
#90718=CARTESIAN_POINT('Ctrl Pts',(0.00978863525980772,-0.0348045283579412,
0.0799149896270596));
#90719=CARTESIAN_POINT('Ctrl Pts',(0.00986777532983583,-0.0346945769439157,
0.0798909483484079));
#90720=CARTESIAN_POINT('Ctrl Pts',(0.00968044081854037,-0.0350241211494342,
0.079857149757431));
#90721=CARTESIAN_POINT('Ctrl Pts',(0.00975905446642646,-0.0349144232818961,
0.0798357074231205));
#90722=CARTESIAN_POINT('Ctrl Pts',(0.00983727193999802,-0.0348045283579412,
0.0798126272542633));
#90723=CARTESIAN_POINT('Ctrl Pts',(0.00991499195251126,-0.0346945769439157,
0.0797879350854453));
#90724=CARTESIAN_POINT('Ctrl Pts',(0.00973187471970054,-0.0350241211494342,
0.0797561760201796));
#90725=CARTESIAN_POINT('Ctrl Pts',(0.00980909749575684,-0.0349144232818961,
0.0797340252049694));
#90726=CARTESIAN_POINT('Ctrl Pts',(0.00988590862018833,-0.0348045283579412,
0.0797102648814671));
#90727=CARTESIAN_POINT('Ctrl Pts',(0.00996220857518668,-0.0346945769439157,
0.0796849218224828));
#90728=CARTESIAN_POINT('Ctrl Pts',(0.0097833086208607,-0.0350241211494342,
0.0796552022829283));
#90729=CARTESIAN_POINT('Ctrl Pts',(0.00985914052508721,-0.0349144232818961,
0.0796323429868183));
#90730=CARTESIAN_POINT('Ctrl Pts',(0.00993454530037863,-0.0348045283579412,
0.0796079025086708));
#90731=CARTESIAN_POINT('Ctrl Pts',(0.0100094251978621,-0.0346945769439157,
0.0795819085595203));
#90732=CARTESIAN_POINT('',(0.00993817775744595,-0.0346945769458128,0.0797373502076673));
#90733=CARTESIAN_POINT('Ctrl Pts',(0.00985550857068307,-0.0347116136492799,
0.0798946604506295));
#90734=CARTESIAN_POINT('Ctrl Pts',(0.00984311485760916,-0.0347621546531828,
0.0798535467537695));
#90735=CARTESIAN_POINT('Ctrl Pts',(0.00983093905950229,-0.0348133084096042,
0.0798131559468007));
#90736=CARTESIAN_POINT('Ctrl Pts',(0.00980701313164405,-0.0349168561544573,
0.0797337864036143));
#90737=CARTESIAN_POINT('Ctrl Pts',(0.00979527249212791,-0.0349692089015919,
0.0796948391493789));
#90738=CARTESIAN_POINT('Ctrl Pts',(0.00978374540819085,-0.0350221583435,
0.0796566003236256));
#90739=CARTESIAN_POINT('Ctrl Pts',(0.00990174466699582,-0.0351951371254965,
0.0796185300671819));
#90740=CARTESIAN_POINT('Ctrl Pts',(0.0099770551292594,-0.0350856248736052,
0.079594044661753));
#90741=CARTESIAN_POINT('Ctrl Pts',(0.0100519213945189,-0.0349758427080733,
0.0795679827719899));
#90742=CARTESIAN_POINT('Ctrl Pts',(0.0101262456568789,-0.0348659306897824,
0.0795403721328392));
#90743=CARTESIAN_POINT('Ctrl Pts',(0.00997419059529331,-0.0351951371254965,
0.0796574152587592));
#90744=CARTESIAN_POINT('Ctrl Pts',(0.0100500365692423,-0.0350856248736052,
0.0796319321562741));
#90745=CARTESIAN_POINT('Ctrl Pts',(0.0101254181671598,-0.0349758427080733,
0.0796048606834117));
#90746=CARTESIAN_POINT('Ctrl Pts',(0.0102002368474823,-0.0348659306897824,
0.0795762298288608));
#90747=CARTESIAN_POINT('Ctrl Pts',(0.0100466365235908,-0.0351951371254965,
0.0796963004503364));
#90748=CARTESIAN_POINT('Ctrl Pts',(0.0101230180092252,-0.0350856248736052,
0.0796698196507952));
#90749=CARTESIAN_POINT('Ctrl Pts',(0.0101989149398007,-0.0349758427080734,
0.0796417385948336));
#90750=CARTESIAN_POINT('Ctrl Pts',(0.0102742280380856,-0.0348659306897824,
0.0796120875248825));
#90751=CARTESIAN_POINT('Ctrl Pts',(0.0101190824518883,-0.0351951371254965,
0.0797351856419137));
#90752=CARTESIAN_POINT('Ctrl Pts',(0.0101959994492081,-0.0350856248736052,
0.0797077071453163));
#90753=CARTESIAN_POINT('Ctrl Pts',(0.0102724117124416,-0.0349758427080734,
0.0796786165062554));
#90754=CARTESIAN_POINT('Ctrl Pts',(0.010348219228689,-0.0348659306897824,
0.0796479452209042));
#90755=CARTESIAN_POINT('Origin',(0.0119778629691043,-0.0308609197410555,
0.0845269351437275));
#90756=CARTESIAN_POINT('',(0.00999722610289499,-0.0351951371254965,0.0796697795164507));
#90757=CARTESIAN_POINT('Ctrl Pts',(0.00751557654030228,-0.0321934096636942,
0.0798691102123334));
#90758=CARTESIAN_POINT('Ctrl Pts',(0.00766901285885221,-0.0319797282160096,
0.079885427582138));
#90759=CARTESIAN_POINT('Ctrl Pts',(0.00782310337371433,-0.0317669959605189,
0.0798934944053677));
#90760=CARTESIAN_POINT('Ctrl Pts',(0.00776473354553151,-0.0321934096636942,
0.0798901401610652));
#90761=CARTESIAN_POINT('Ctrl Pts',(0.00791873407036402,-0.0319797282160096,
0.0798997729711736));
#90762=CARTESIAN_POINT('Ctrl Pts',(0.00807302956171172,-0.0317669959605189,
0.0799011345985298));
#90763=CARTESIAN_POINT('Ctrl Pts',(0.00776622828223816,-0.0321934096636942,
0.0798902663234273));
#90764=CARTESIAN_POINT('Ctrl Pts',(0.00792023219184342,-0.0319797282160096,
0.0798998590316861));
#90765=CARTESIAN_POINT('Ctrl Pts',(0.0080745289128811,-0.0317669959605189,
0.0799011804333927));
#90766=CARTESIAN_POINT('',(0.00776473354564076,-0.0321934096636943,0.0798901401610721));
#90767=CARTESIAN_POINT('',(0.00800086794439121,-0.0318665617561286,0.0799000449639514));
#90768=CARTESIAN_POINT('Origin',(0.00942093499841772,-0.032637194442062,
0.0632626057202205));
#90769=CARTESIAN_POINT('Origin',(0.00776661269360889,-0.0316939261509253,
0.0908587271204895));
#90770=CARTESIAN_POINT('',(0.00764033085304629,-0.0320197259213214,0.0798809584455136));
#90771=CARTESIAN_POINT('Ctrl Pts',(0.00764050362844855,-0.0320197391311198,
0.0798810188942161));
#90772=CARTESIAN_POINT('Ctrl Pts',(0.00766966489836095,-0.0319792715672862,
0.0798834779712017));
#90773=CARTESIAN_POINT('Ctrl Pts',(0.00769897767596132,-0.031938643888646,
0.0798857258450869));
#90774=CARTESIAN_POINT('Ctrl Pts',(0.00772847330676439,-0.0318979098685801,
0.0798877564685929));
#90775=CARTESIAN_POINT('Ctrl Pts',(0.0077579683544451,-0.0318571766538172,
0.079889787051954));
#90776=CARTESIAN_POINT('Ctrl Pts',(0.00778749639970253,-0.0318163871807225,
0.0798915918578671));
#90777=CARTESIAN_POINT('Ctrl Pts',(0.00781695548280018,-0.0317755399642095,
0.0798931683778834));
#90778=CARTESIAN_POINT('Origin',(0.0074784479685726,-0.0323427512858111,
0.0817957411220363));
#90779=CARTESIAN_POINT('',(0.00770245499135762,-0.0321934096636663,0.0798848835767754));
#90780=CARTESIAN_POINT('Ctrl Pts',(0.0077634250783826,-0.0321934096636618,
0.0798885904511592));
#90781=CARTESIAN_POINT('Ctrl Pts',(0.00788206584516462,-0.032028746738191,
0.0798960405462253));
#90782=CARTESIAN_POINT('Ctrl Pts',(0.00800091315369981,-0.0318646057455573,
0.0798985807653214));
#90783=CARTESIAN_POINT('Ctrl Pts',(0.00776473354555483,-0.0321934096636618,
0.0798901401610666));
#90784=CARTESIAN_POINT('Ctrl Pts',(0.00788340635134942,-0.032028746738191,
0.0798975632046207));
#90785=CARTESIAN_POINT('Ctrl Pts',(0.00800228455346166,-0.0318646057455573,
0.0799000750711239));
#90786=CARTESIAN_POINT('Ctrl Pts',(0.00798274125480844,-0.0321934096636618,
0.0801483420587596));
#90787=CARTESIAN_POINT('Ctrl Pts',(0.00810675217827977,-0.032028746738191,
0.0801512579673282));
#90788=CARTESIAN_POINT('Ctrl Pts',(0.00823077765355593,-0.0318646057455573,
0.0801490459217784));
#90789=CARTESIAN_POINT('Ctrl Pts',(0.00799555414024659,-0.0321763980313103,
0.0801486296390504));
#90790=CARTESIAN_POINT('Ctrl Pts',(0.00799647135765932,-0.0321259597689058,
0.0801057206915783));
#90791=CARTESIAN_POINT('Ctrl Pts',(0.0079973726528313,-0.0320749162472279,
0.080063554809537));
#90792=CARTESIAN_POINT('Ctrl Pts',(0.00799914427494874,-0.0319716059728889,
0.0799806768399453));
#90793=CARTESIAN_POINT('Ctrl Pts',(0.00800001393905037,-0.0319193783913111,
0.0799399960433909));
#90794=CARTESIAN_POINT('Ctrl Pts',(0.00800086794435303,-0.031866561756148,
0.0799000449639248));
#90795=CARTESIAN_POINT('',(0.00787373740024513,-0.0321934096636664,0.0800192411099193));
#90796=CARTESIAN_POINT('Ctrl Pts',(0.00783732086283825,-0.0327445246967097,
0.0798942750766532));
#90797=CARTESIAN_POINT('Ctrl Pts',(0.00805396973908347,-0.032443687833936,
0.0799050791423469));
#90798=CARTESIAN_POINT('Ctrl Pts',(0.00827081694513738,-0.0321434074405928,
0.0798995336360174));
#90799=CARTESIAN_POINT('Ctrl Pts',(0.00783981990673068,-0.0327445246967097,
0.0798943442114757));
#90800=CARTESIAN_POINT('Ctrl Pts',(0.00805647139043836,-0.032443687833936,
0.0799050540241882));
#90801=CARTESIAN_POINT('Ctrl Pts',(0.00827331409702744,-0.0321434074405928,
0.0798994143362355));
#90802=CARTESIAN_POINT('Ctrl Pts',(0.0080897242959742,-0.0327445246967097,
0.079901257693726));
#90803=CARTESIAN_POINT('Ctrl Pts',(0.00830663652592757,-0.032443687833936,
0.0799025422083154));
#90804=CARTESIAN_POINT('Ctrl Pts',(0.0085230292860335,-0.0321434074405928,
0.0798874843580433));
#90805=CARTESIAN_POINT('',(0.00812586842896101,-0.0326943950436612,0.0799013581567853));
#90806=CARTESIAN_POINT('',(0.00836215879818742,-0.0323666188837389,0.0798964164132224));
#90807=CARTESIAN_POINT('Origin',(0.00804376040539544,-0.0326395579112528,
0.0630906081289521));
#90808=CARTESIAN_POINT('Origin',(0.00881992596082919,-0.0321933825603174,
0.0909315340399853));
#90809=CARTESIAN_POINT('',(0.00823720989640445,-0.0321934096536378,0.0799002399215511));
#90810=CARTESIAN_POINT('',(0.00829965619325201,-0.0321934096584275,0.0798976494835474));
#90811=CARTESIAN_POINT('',(0.00800086794438665,-0.0325210109756239,0.0799000449639513));
#90812=CARTESIAN_POINT('Origin',(0.00852391591854703,-0.0326393129156286,
0.0631158095705174));
#90813=CARTESIAN_POINT('Origin',(0.00776447660749309,-0.0326943765538264,
0.0909586154069157));
#90814=CARTESIAN_POINT('',(0.00806338270354571,-0.0326943950436703,0.0799000224479366));
#90815=CARTESIAN_POINT('Ctrl Pts',(0.00776052600373539,-0.032522978320377,
0.0801389936500988));
#90816=CARTESIAN_POINT('Ctrl Pts',(0.00784308415023136,-0.0324130253092451,
0.0801440011287255));
#90817=CARTESIAN_POINT('Ctrl Pts',(0.00792573336129477,-0.032303122220807,
0.0801473000265561));
#90818=CARTESIAN_POINT('Ctrl Pts',(0.00800836762005261,-0.0321934096576659,
0.0801488898536619));
#90819=CARTESIAN_POINT('Ctrl Pts',(0.00784064516754767,-0.032522978320377,
0.0800588558823081));
#90820=CARTESIAN_POINT('Ctrl Pts',(0.00792209861666714,-0.0324130253092451,
0.0800627589200137));
#90821=CARTESIAN_POINT('Ctrl Pts',(0.00800362045112385,-0.032303122220807,
0.0800649763965177));
#90822=CARTESIAN_POINT('Ctrl Pts',(0.00808510614701406,-0.0321934096576659,
0.080065509156158));
#90823=CARTESIAN_POINT('Ctrl Pts',(0.00792076433135995,-0.032522978320377,
0.0799787181145175));
#90824=CARTESIAN_POINT('Ctrl Pts',(0.00800111308310293,-0.0324130253092451,
0.079981516711302));
#90825=CARTESIAN_POINT('Ctrl Pts',(0.00808150754095293,-0.032303122220807,
0.0799826527664793));
#90826=CARTESIAN_POINT('Ctrl Pts',(0.0081618446739755,-0.0321934096576659,
0.0799821284586541));
#90827=CARTESIAN_POINT('Ctrl Pts',(0.00800088349517223,-0.032522978320377,
0.0798985803467268));
#90828=CARTESIAN_POINT('Ctrl Pts',(0.00808012754953871,-0.0324130253092451,
0.0799002745025902));
#90829=CARTESIAN_POINT('Ctrl Pts',(0.00815939463078201,-0.032303122220807,
0.0799003291364409));
#90830=CARTESIAN_POINT('Ctrl Pts',(0.00823858320093694,-0.0321934096576659,
0.0798987477611502));
#90831=CARTESIAN_POINT('',(0.00812278875555212,-0.0321934096584275,0.0800245648876137));
#90832=CARTESIAN_POINT('Ctrl Pts',(0.00799555414278173,-0.032210423332892,
0.080148629635806));
#90833=CARTESIAN_POINT('Ctrl Pts',(0.0079964726199866,-0.0322609421831223,
0.080105662402296));
#90834=CARTESIAN_POINT('Ctrl Pts',(0.00799737456921036,-0.0323120888240433,
0.0800634683633959));
#90835=CARTESIAN_POINT('Ctrl Pts',(0.00799914620757039,-0.0324156524631811,
0.0799805894430405));
#90836=CARTESIAN_POINT('Ctrl Pts',(0.00800001516846968,-0.0324680267167311,
0.0799399386292009));
#90837=CARTESIAN_POINT('Ctrl Pts',(0.00800086794439211,-0.0325210109755913,
0.0799000449639081));
#90838=CARTESIAN_POINT('Origin',(0.000335215042199046,-0.0262834582511539,
0.0730357255385635));
#90839=CARTESIAN_POINT('Origin',(0.00245340408136264,-0.0342770951788246,
0.0849050601642025));
#90840=CARTESIAN_POINT('Ctrl Pts',(0.00812446557717303,-0.0326943950436605,
0.0798998940196011));
#90841=CARTESIAN_POINT('Ctrl Pts',(0.00824334049677372,-0.0325294772287039,
0.0798998798911275));
#90842=CARTESIAN_POINT('Ctrl Pts',(0.00836211325541952,-0.0323646534831895,
0.0798949525679849));
#90843=CARTESIAN_POINT('Ctrl Pts',(0.00812586842895898,-0.0326943950436605,
0.0799013581567853));
#90844=CARTESIAN_POINT('Ctrl Pts',(0.00824477361854195,-0.0325294772287039,
0.0799013150253609));
#90845=CARTESIAN_POINT('Ctrl Pts',(0.00836357542258684,-0.0323646534831895,
0.0798963574729647));
#90846=CARTESIAN_POINT('Ctrl Pts',(0.00835965858109641,-0.0326943950436605,
0.0801453617346851));
#90847=CARTESIAN_POINT('Ctrl Pts',(0.00848360836899827,-0.0325294772287039,
0.0801404851601669));
#90848=CARTESIAN_POINT('Ctrl Pts',(0.00860725069029517,-0.0323646534831895,
0.0801304897970287));
#90849=CARTESIAN_POINT('Ctrl Pts',(0.00837246424067422,-0.0326773559997669,
0.0801448442199106));
#90850=CARTESIAN_POINT('Ctrl Pts',(0.00837068394198459,-0.0326267924002051,
0.0801019278325357));
#90851=CARTESIAN_POINT('Ctrl Pts',(0.00836893514681326,-0.0325756107621945,
0.0800597717534306));
#90852=CARTESIAN_POINT('Ctrl Pts',(0.00836549930955373,-0.0324719987229852,
0.079976945783095));
#90853=CARTESIAN_POINT('Ctrl Pts',(0.00836381361313338,-0.0324196089018781,
0.0799363081939324));
#90854=CARTESIAN_POINT('Ctrl Pts',(0.00836215879814982,-0.0323666188837573,
0.0798964164131996));
#90855=CARTESIAN_POINT('',(0.00824276350503385,-0.0326943950436704,0.0800233599457397));
#90856=CARTESIAN_POINT('Ctrl Pts',(0.00819858638145413,-0.0332451089994434,
0.0799009274868521));
#90857=CARTESIAN_POINT('Ctrl Pts',(0.00841548616028705,-0.0329451141710254,
0.0798981062007301));
#90858=CARTESIAN_POINT('Ctrl Pts',(0.00863155723893576,-0.0326442513127494,
0.079878955151549));
#90859=CARTESIAN_POINT('Ctrl Pts',(0.00820110981899618,-0.0332451089994434,
0.0799008386726003));
#90860=CARTESIAN_POINT('Ctrl Pts',(0.00841800624814479,-0.0329451141710254,
0.0798979222134742));
#90861=CARTESIAN_POINT('Ctrl Pts',(0.00863406681780555,-0.0326442513127494,
0.0798786765139776));
#90862=CARTESIAN_POINT('Ctrl Pts',(0.00845095512019007,-0.0332451089994434,
0.0798920451823184));
#90863=CARTESIAN_POINT('Ctrl Pts',(0.00866751989742658,-0.0329451141710254,
0.0798797056534881));
#90864=CARTESIAN_POINT('Ctrl Pts',(0.00888253997323141,-0.0326442513127494,
0.0798510886356119));
#90865=CARTESIAN_POINT('Ctrl Pts',(0.00845345357320201,-0.0332451089994434,
0.0798919572474155));
#90866=CARTESIAN_POINT('Ctrl Pts',(0.00867001503391939,-0.0329451141710254,
0.0798795234878883));
#90867=CARTESIAN_POINT('Ctrl Pts',(0.00888502470478567,-0.0326442513127494,
0.0798508127568282));
#90868=CARTESIAN_POINT('',(0.00848699507891553,-0.0331951640388616,0.0798898781694026));
#90869=CARTESIAN_POINT('',(0.00872250890292996,-0.032867753235504,0.0798701093867858));
#90870=CARTESIAN_POINT('Origin',(0.00666296712443024,-0.0326402808280718,
0.0632253898936535));
#90871=CARTESIAN_POINT('Origin',(0.0098738294798772,-0.0326944278779006,
0.0908659651477627));
#90872=CARTESIAN_POINT('',(0.00859804663143739,-0.0326943950436593,0.0798817709516813));
#90873=CARTESIAN_POINT('',(0.00866020704697387,-0.0326943950436694,0.0798752645900675));
#90874=CARTESIAN_POINT('',(0.00836215879818454,-0.0330220786163546,0.0798964164132225));
#90875=CARTESIAN_POINT('Origin',(0.0071368455069605,-0.0326396682763202,
0.0631441992304724));
#90876=CARTESIAN_POINT('Origin',(0.00881933068583198,-0.0331952026560064,
0.0909172326935325));
#90877=CARTESIAN_POINT('',(0.00842454878495234,-0.0331951640388702,0.0798924686074329));
#90878=CARTESIAN_POINT('Ctrl Pts',(0.00813729579048197,-0.0330240426238173,
0.0801499847818743));
#90879=CARTESIAN_POINT('Ctrl Pts',(0.00821995142635422,-0.032914277406352,
0.0801497986189048));
#90880=CARTESIAN_POINT('Ctrl Pts',(0.00830264442056684,-0.0328043479726691,
0.0801479036402456));
#90881=CARTESIAN_POINT('Ctrl Pts',(0.00838526877037963,-0.0326943950436594,
0.0801442993560502));
#90882=CARTESIAN_POINT('Ctrl Pts',(0.00821222493349814,-0.0330240426238173,
0.0800649744324369));
#90883=CARTESIAN_POINT('Ctrl Pts',(0.00829370946898532,-0.032914277406352,
0.0800637560475224));
#90884=CARTESIAN_POINT('Ctrl Pts',(0.00837520944006565,-0.0328043479726691,
0.0800608525422343));
#90885=CARTESIAN_POINT('Ctrl Pts',(0.00845662033676901,-0.0326943950436594,
0.0800562647608141));
#90886=CARTESIAN_POINT('Ctrl Pts',(0.00828715407651431,-0.0330240426238173,
0.0799799640829995));
#90887=CARTESIAN_POINT('Ctrl Pts',(0.00836746751161642,-0.032914277406352,
0.07997771347614));
#90888=CARTESIAN_POINT('Ctrl Pts',(0.00844777445956445,-0.0328043479726691,
0.0799738014442229));
#90889=CARTESIAN_POINT('Ctrl Pts',(0.00852797190315839,-0.0326943950436594,
0.079968230165578));
#90890=CARTESIAN_POINT('Ctrl Pts',(0.00836208321953047,-0.0330240426238173,
0.0798949537335621));
#90891=CARTESIAN_POINT('Ctrl Pts',(0.00844122555424752,-0.032914277406352,
0.0798916709047577));
#90892=CARTESIAN_POINT('Ctrl Pts',(0.00852033947906325,-0.0328043479726691,
0.0798867503462116));
#90893=CARTESIAN_POINT('Ctrl Pts',(0.00859932346954776,-0.0326943950436594,
0.0798801955703419));
#90894=CARTESIAN_POINT('',(0.00849165770091852,-0.0326943950436694,0.0800130351538757));
#90895=CARTESIAN_POINT('Ctrl Pts',(0.00837246424284239,-0.0327114338383319,
0.0801448442163262));
#90896=CARTESIAN_POINT('Ctrl Pts',(0.00837068424772592,-0.0327619876830903,
0.0801019348328769));
#90897=CARTESIAN_POINT('Ctrl Pts',(0.00836893565550443,-0.0328131562604201,
0.0800597824621015));
#90898=CARTESIAN_POINT('Ctrl Pts',(0.00836549980542918,-0.0329167375858768,
0.0799769562751137));
#90899=CARTESIAN_POINT('Ctrl Pts',(0.00836381391659571,-0.0329691088920615,
0.0799363154611364));
#90900=CARTESIAN_POINT('Ctrl Pts',(0.00836215879818539,-0.0330220786163187,
0.0798964164131748));
#90901=CARTESIAN_POINT('Ctrl Pts',(0.0084855028232013,-0.0331951640388604,
0.0798885047879282));
#90902=CARTESIAN_POINT('Ctrl Pts',(0.00860414273050473,-0.033030642201062,
0.0798810264458146));
#90903=CARTESIAN_POINT('Ctrl Pts',(0.0087223721730947,-0.0328657861914645,
0.0798686509817587));
#90904=CARTESIAN_POINT('Ctrl Pts',(0.0084869950789124,-0.0331951640388604,
0.0798898781694028));
#90905=CARTESIAN_POINT('Ctrl Pts',(0.00860566337999729,-0.033030642201062,
0.0798823689758592));
#90906=CARTESIAN_POINT('Ctrl Pts',(0.00872391991698437,-0.0328657861914645,
0.0798699615131906));
#90907=CARTESIAN_POINT('Ctrl Pts',(0.00873564501101464,-0.0331951640388604,
0.0801187204568676));
#90908=CARTESIAN_POINT('Ctrl Pts',(0.00885904447967284,-0.033030642201062,
0.0801060705853973));
#90909=CARTESIAN_POINT('Ctrl Pts',(0.00898181567185892,-0.0328657861914645,
0.0800883312933441));
#90910=CARTESIAN_POINT('Ctrl Pts',(0.0087483929067007,-0.033178164828644,
0.0801173998893635));
#90911=CARTESIAN_POINT('Ctrl Pts',(0.00874391828725666,-0.033127681154678,
0.0800746504291126));
#90912=CARTESIAN_POINT('Ctrl Pts',(0.00873952443194941,-0.0330765663497795,
0.0800326728952462));
#90913=CARTESIAN_POINT('Ctrl Pts',(0.00873089463578463,-0.0329730614463183,
0.0799502255973295));
#90914=CARTESIAN_POINT('Ctrl Pts',(0.00872666218650641,-0.0329207133373643,
0.0799097891396196));
#90915=CARTESIAN_POINT('Ctrl Pts',(0.00872250888993246,-0.0328677532289395,
0.0798701093969079));
#90916=CARTESIAN_POINT('',(0.00861132004496886,-0.0331951640388702,0.0800042993131388));
#90917=CARTESIAN_POINT('Ctrl Pts',(0.00855954660528496,-0.0337436976235976,
0.0798848814832637));
#90918=CARTESIAN_POINT('Ctrl Pts',(0.00861112699849052,-0.0336723290703325,
0.0798809621520986));
#90919=CARTESIAN_POINT('Ctrl Pts',(0.00866262855078964,-0.033601104548885,
0.0798761156862932));
#90920=CARTESIAN_POINT('Ctrl Pts',(0.00882706280539791,-0.0333736987606857,
0.0798606418810075));
#90921=CARTESIAN_POINT('Ctrl Pts',(0.00899033810919476,-0.0331450831799192,
0.0798357573896796));
#90922=CARTESIAN_POINT('Ctrl Pts',(0.00856203460757845,-0.0337436976235976,
0.0798846368517293));
#90923=CARTESIAN_POINT('Ctrl Pts',(0.0086136128005309,-0.0336723290703325,
0.0798806951430946));
#90924=CARTESIAN_POINT('Ctrl Pts',(0.00866511175043273,-0.033601104548885,
0.0798758263430152));
#90925=CARTESIAN_POINT('Ctrl Pts',(0.00882953769610195,-0.0333736987606857,
0.0798602812288169));
#90926=CARTESIAN_POINT('Ctrl Pts',(0.00899280061253565,-0.0331450831799192,
0.0798353260229029));
#90927=CARTESIAN_POINT('Ctrl Pts',(0.00881083483692663,-0.0337436976235976,
0.0798601736982883));
#90928=CARTESIAN_POINT('Ctrl Pts',(0.00886219300456955,-0.0336723290703325,
0.079853994242684));
#90929=CARTESIAN_POINT('Ctrl Pts',(0.00891343171474199,-0.033601104548885,
0.0798468920152118));
#90930=CARTESIAN_POINT('Ctrl Pts',(0.00907702676650588,-0.0333736987606857,
0.079824216009765));
#90931=CARTESIAN_POINT('Ctrl Pts',(0.00923905094662548,-0.0331450831799192,
0.0797921893452301));
#90932=CARTESIAN_POINT('Ctrl Pts',(0.00881334771924304,-0.0337436976235976,
0.0798599266204385));
#90933=CARTESIAN_POINT('Ctrl Pts',(0.00886470366463034,-0.0336723290703325,
0.0798537245635899));
#90934=CARTESIAN_POINT('Ctrl Pts',(0.00891593974638151,-0.033601104548885,
0.079846599778501));
#90935=CARTESIAN_POINT('Ctrl Pts',(0.00907952640611696,-0.0333736987606857,
0.0798238517510526));
#90936=CARTESIAN_POINT('Ctrl Pts',(0.0092415380749998,-0.0331450831799192,
0.0797917536647857));
#90937=CARTESIAN_POINT('',(0.00884668829355914,-0.0336938721132548,0.0798557455051844));
#90938=CARTESIAN_POINT('',(0.00908049609245075,-0.0333679870047996,0.0798212276902747));
#90939=CARTESIAN_POINT('Ctrl Pts',(0.00884668829355328,-0.0336938721132542,
0.0798557455051857));
#90940=CARTESIAN_POINT('Ctrl Pts',(0.00886896049488146,-0.0336629187933887,
0.0798529236635531));
#90941=CARTESIAN_POINT('Ctrl Pts',(0.00889120905000746,-0.0336319952301025,
0.0798499723117194));
#90942=CARTESIAN_POINT('Ctrl Pts',(0.00891343171474876,-0.0336011045488936,
0.0798468920152112));
#90943=CARTESIAN_POINT('Ctrl Pts',(0.00896919598475278,-0.0335235892595438,
0.0798391624972537));
#90944=CARTESIAN_POINT('Ctrl Pts',(0.00902489629397583,-0.0334458668665558,
0.0798306071584675));
#90945=CARTESIAN_POINT('Ctrl Pts',(0.00908049608084341,-0.0333679869962482,
0.0798212276924733));
#90946=CARTESIAN_POINT('Ctrl Pts',(0.00908054005010003,-0.0333679692468943,
0.0798212209721364));
#90947=CARTESIAN_POINT('Ctrl Pts',(0.00908045881507262,-0.0333391895412312,
0.0798207750588555));
#90948=CARTESIAN_POINT('Ctrl Pts',(0.00908039473082887,-0.0333104081126143,
0.0798204414070563));
#90949=CARTESIAN_POINT('Ctrl Pts',(0.00908030447069118,-0.0332532732084331,
0.0798200008325513));
#90950=CARTESIAN_POINT('Ctrl Pts',(0.00908027773360654,-0.0332249236067027,
0.079819890576674));
#90951=CARTESIAN_POINT('Ctrl Pts',(0.0090802703182882,-0.0331961055133883,
0.0798198880777076));
#90952=CARTESIAN_POINT('Ctrl Pts',(0.00908027020192905,-0.0331956347145507,
0.0798198880667067));
#90953=CARTESIAN_POINT('Ctrl Pts',(0.0090802700914211,-0.0331951640388597,
0.0798198880853489));
#90954=CARTESIAN_POINT('',(0.00895701165478286,-0.0331951640388587,0.0798406813005297));
#90955=CARTESIAN_POINT('',(0.00901864087311192,-0.0331951640388688,0.0798302846929493));
#90956=CARTESIAN_POINT('',(0.00872250888822892,-0.0335216366567653,0.07987010938183));
#90957=CARTESIAN_POINT('Origin',(0.00578895674576758,-0.0326434571525012,
0.0634760575075271));
#90958=CARTESIAN_POINT('Origin',(0.00985921721683401,-0.0336938867896249,
0.0907299921631417));
#90959=CARTESIAN_POINT('',(0.00878452787803477,-0.0336938721132539,0.0798622518668191));
#90960=CARTESIAN_POINT('Ctrl Pts',(0.00851401224513785,-0.0335235895815172,
0.0801372965941676));
#90961=CARTESIAN_POINT('Ctrl Pts',(0.00859643917065879,-0.0334144449262749,
0.0801319243092091));
#90962=CARTESIAN_POINT('Ctrl Pts',(0.00867884980736672,-0.0333049234473147,
0.080124842973898));
#90963=CARTESIAN_POINT('Ctrl Pts',(0.00876113795713087,-0.0331951640388588,
0.0801160520975017));
#90964=CARTESIAN_POINT('Ctrl Pts',(0.0085834557729539,-0.0335235895815172,
0.0800477490150239));
#90965=CARTESIAN_POINT('Ctrl Pts',(0.00866464989974497,-0.0334144449262749,
0.0800414207031833));
#90966=CARTESIAN_POINT('Ctrl Pts',(0.00874580657059074,-0.0333049234473147,
0.0800334077113251));
#90967=CARTESIAN_POINT('Ctrl Pts',(0.00882682108288447,-0.0331951640388588,
0.0800237108852655));
#90968=CARTESIAN_POINT('Ctrl Pts',(0.00865289930076994,-0.0335235895815172,
0.0799582014358803));
#90969=CARTESIAN_POINT('Ctrl Pts',(0.00873286062883114,-0.0334144449262749,
0.0799509170971576));
#90970=CARTESIAN_POINT('Ctrl Pts',(0.00881276333381477,-0.0333049234473147,
0.0799419724487521));
#90971=CARTESIAN_POINT('Ctrl Pts',(0.00889250420863806,-0.0331951640388588,
0.0799313696730293));
#90972=CARTESIAN_POINT('Ctrl Pts',(0.00872234282858598,-0.0335235895815172,
0.0798686538567367));
#90973=CARTESIAN_POINT('Ctrl Pts',(0.00880107135791731,-0.0334144449262749,
0.0798604134911319));
#90974=CARTESIAN_POINT('Ctrl Pts',(0.0088797200970388,-0.0333049234473147,
0.0798505371861792));
#90975=CARTESIAN_POINT('Ctrl Pts',(0.00895818733439166,-0.0331951640388588,
0.079839028460793));
#90976=CARTESIAN_POINT('',(0.00885907480596688,-0.0331951640388687,0.0799783666990257));
#90977=CARTESIAN_POINT('Ctrl Pts',(0.00874839290846162,-0.0332121607145976,
0.0801173998855383));
#90978=CARTESIAN_POINT('Ctrl Pts',(0.00874392582848732,-0.0332625444109666,
0.080074722339553));
#90979=CARTESIAN_POINT('Ctrl Pts',(0.00873953572331102,-0.0333135300746638,
0.0800327801946574));
#90980=CARTESIAN_POINT('Ctrl Pts',(0.00873090597774284,-0.0334167203140545,
0.0799503334138866));
#90981=CARTESIAN_POINT('Ctrl Pts',(0.00872666967972461,-0.0334688847587225,
0.0799098607103485));
#90982=CARTESIAN_POINT('Ctrl Pts',(0.00872250888831297,-0.0335216366562276,
0.0798701093811075));
#90983=CARTESIAN_POINT('Ctrl Pts',(0.00884511311559296,-0.0336938721132538,
0.0798544688319359));
#90984=CARTESIAN_POINT('Ctrl Pts',(0.00887850326461507,-0.0336474569765032,
0.079850246642683));
#90985=CARTESIAN_POINT('Ctrl Pts',(0.00891184169966668,-0.033601104548885,
0.0798456338688845));
#90986=CARTESIAN_POINT('Ctrl Pts',(0.0089962469522171,-0.0334837508592655,
0.0798339553861718));
#90987=CARTESIAN_POINT('Ctrl Pts',(0.00908026908254489,-0.0333660264659097,
0.079819780929154));
#90988=CARTESIAN_POINT('Ctrl Pts',(0.00884668829352812,-0.0336938721132538,
0.0798557455051882));
#90989=CARTESIAN_POINT('Ctrl Pts',(0.00888008591534243,-0.0336474569765032,
0.0798515140958961));
#90990=CARTESIAN_POINT('Ctrl Pts',(0.00891343171474199,-0.033601104548885,
0.0798468920152118));
#90991=CARTESIAN_POINT('Ctrl Pts',(0.00899785561212824,-0.0334837508592655,
0.0798351899696039));
#90992=CARTESIAN_POINT('Ctrl Pts',(0.009081895680887,-0.0333660264659097,
0.0798209914075528));
#90993=CARTESIAN_POINT('Ctrl Pts',(0.00911079186838175,-0.0336938721132538,
0.080069800033461));
#90994=CARTESIAN_POINT('Ctrl Pts',(0.00914544242238106,-0.0336474569765032,
0.0800640227383062));
#90995=CARTESIAN_POINT('Ctrl Pts',(0.00918002297156805,-0.033601104548885,
0.080057840210531));
#90996=CARTESIAN_POINT('Ctrl Pts',(0.00926757297152882,-0.0334837508592655,
0.080042187471659));
#90997=CARTESIAN_POINT('Ctrl Pts',(0.00935462070287566,-0.0333660264659097,
0.0800239473182964));
#90998=CARTESIAN_POINT('Ctrl Pts',(0.00912185652178284,-0.033676936124379,
0.080066404958628));
#90999=CARTESIAN_POINT('Ctrl Pts',(0.00911488450272859,-0.0336279018398637,
0.0800250760846962));
#91000=CARTESIAN_POINT('Ctrl Pts',(0.00910781218243291,-0.0335767825795119,
0.0799831526430637));
#91001=CARTESIAN_POINT('Ctrl Pts',(0.00909395450089789,-0.0334733171841433,
0.0799010068014231));
#91002=CARTESIAN_POINT('Ctrl Pts',(0.00908715982610767,-0.0334209631343313,
0.079860729192362));
#91003=CARTESIAN_POINT('Ctrl Pts',(0.00908049607793282,-0.033367986984468,
0.0798212276927121));
#91004=CARTESIAN_POINT('',(0.00897795249574407,-0.0336938721132539,0.079962134435723));
#91005=CARTESIAN_POINT('Origin',(0.00765445669747421,-0.035184046744118,
0.0732929823637694));
#91006=CARTESIAN_POINT('Origin',(0.013025539739254,-0.0352322612269297,
0.0850652437968551));
#91007=CARTESIAN_POINT('',(0.0103463288558176,-0.0351951142564682,0.0794545358812543));
#91008=CARTESIAN_POINT('',(0.010460264143557,-0.0351951372916788,0.0794038892351504));
#91009=CARTESIAN_POINT('Origin',(0.00831624652060065,-0.0352875124757075,
0.0738689662138883));
#91010=CARTESIAN_POINT('Origin',(0.000811222856913943,-0.0298325076523561,
0.0758297816026072));
#91011=CARTESIAN_POINT('Origin',(0.00839652175620651,-0.0338733578222048,
0.0825268187365329));
#91012=CARTESIAN_POINT('Origin',(0.00776557026075048,-0.0351840467441154,
0.0732409181218339));
#91013=CARTESIAN_POINT('Origin',(0.0116188984722422,-0.0352322613082597,
0.085593699579905));
#91014=CARTESIAN_POINT('',(0.00966396877698428,-0.0351951142564682,0.0796912669914274));
#91015=CARTESIAN_POINT('',(0.00978335335887432,-0.0351951372916787,0.0796552995872849));
#91016=CARTESIAN_POINT('Origin',(0.0083499774120584,-0.0352875115206849,
0.0738954205468797));
#91017=CARTESIAN_POINT('Origin',(0.00065835211145613,-0.0298325076523315,
0.074900029315683));
#91018=CARTESIAN_POINT('Origin',(0.00734423629191548,-0.0338732189113031,
0.0824952379909252));
#91019=CARTESIAN_POINT('Origin',(0.000536285841831988,-0.0262834582511432,
0.0720683456196365));
#91020=CARTESIAN_POINT('Origin',(0.00115017850853305,-0.0342770850471981,
0.0841095482703805));
#91021=CARTESIAN_POINT('Origin',(0.00812378219310841,-0.0201741814719619,
0.07415));
#91022=CARTESIAN_POINT('Origin',(0.00812378219310841,-0.0315241814719618,
0.07415));
#91023=CARTESIAN_POINT('Origin',(0.00812378219310841,-0.0355241814719619,
0.07415));
#91024=CARTESIAN_POINT('Ctrl Pts',(0.00876113795712712,-0.034193496108874,
0.0801160520975069));
#91025=CARTESIAN_POINT('Ctrl Pts',(0.00867886963199231,-0.0340836138585569,
0.08012484085603));
#91026=CARTESIAN_POINT('Ctrl Pts',(0.00859645891583077,-0.033973889665241,
0.0801319230271821));
#91027=CARTESIAN_POINT('Ctrl Pts',(0.00851401189180612,-0.0338644633307392,
0.0801372966172012));
#91028=CARTESIAN_POINT('Ctrl Pts',(0.00882682104902294,-0.034193496108874,
0.0800237109328699));
#91029=CARTESIAN_POINT('Ctrl Pts',(0.00874582605386104,-0.0340836138585569,
0.0800334054223306));
#91030=CARTESIAN_POINT('Ctrl Pts',(0.00866466931450355,-0.033973889665241,
0.0800414192387254));
#91031=CARTESIAN_POINT('Ctrl Pts',(0.00858345538911046,-0.0338644633307392,
0.0800477490883149));
#91032=CARTESIAN_POINT('Ctrl Pts',(0.00889250414091876,-0.034193496108874,
0.079931369768233));
#91033=CARTESIAN_POINT('Ctrl Pts',(0.00881278247572977,-0.0340836138585569,
0.0799419699886312));
#91034=CARTESIAN_POINT('Ctrl Pts',(0.00873287971317634,-0.033973889665241,
0.0799509154502688));
#91035=CARTESIAN_POINT('Ctrl Pts',(0.00865289888641481,-0.0338644633307392,
0.0799582015594285));
#91036=CARTESIAN_POINT('Ctrl Pts',(0.00895818723281458,-0.034193496108874,
0.079839028603596));
#91037=CARTESIAN_POINT('Ctrl Pts',(0.0088797388975985,-0.0340836138585569,
0.0798505345549318));
#91038=CARTESIAN_POINT('Ctrl Pts',(0.00880109011184912,-0.033973889665241,
0.0798604116618121));
#91039=CARTESIAN_POINT('Ctrl Pts',(0.00872234238371916,-0.0338644633307393,
0.0798686540305422));
#91040=CARTESIAN_POINT('Origin',(0.00602946434434258,-0.0345610621862962,
0.0633639504231319));
#91041=CARTESIAN_POINT('Ctrl Pts',(0.00908026834983082,-0.0340223579322365,
0.0798197804359761));
#91042=CARTESIAN_POINT('Ctrl Pts',(0.00900206729021133,-0.0339125849573555,
0.0798329728746978));
#91043=CARTESIAN_POINT('Ctrl Pts',(0.00892364812874447,-0.0338030433565222,
0.0798445374630256));
#91044=CARTESIAN_POINT('Ctrl Pts',(0.00884511246131604,-0.0336938721132328,
0.0798544683016339));
#91045=CARTESIAN_POINT('Ctrl Pts',(0.00917117691759601,-0.0340223579322365,
0.0798874325766501));
#91046=CARTESIAN_POINT('Ctrl Pts',(0.00909204275851244,-0.0339125849573555,
0.0799018788816208));
#91047=CARTESIAN_POINT('Ctrl Pts',(0.00901266520114192,-0.0338030433565222,
0.0799146771421296));
#91048=CARTESIAN_POINT('Ctrl Pts',(0.00893314720684988,-0.0336938721132328,
0.0799258199898388));
#91049=CARTESIAN_POINT('Ctrl Pts',(0.00926208548536119,-0.0340223579322365,
0.0799550847173242));
#91050=CARTESIAN_POINT('Ctrl Pts',(0.00918201822681355,-0.0339125849573555,
0.0799707848885438));
#91051=CARTESIAN_POINT('Ctrl Pts',(0.00910168227353937,-0.0338030433565222,
0.0799848168212336));
#91052=CARTESIAN_POINT('Ctrl Pts',(0.00902118195238373,-0.0336938721132328,
0.0799971716780437));
#91053=CARTESIAN_POINT('Ctrl Pts',(0.00935299405312637,-0.0340223579322365,
0.0800227368579982));
#91054=CARTESIAN_POINT('Ctrl Pts',(0.00927199369511466,-0.0339125849573555,
0.0800396908954668));
#91055=CARTESIAN_POINT('Ctrl Pts',(0.00919069934593683,-0.0338030433565222,
0.0800549565003376));
#91056=CARTESIAN_POINT('Ctrl Pts',(0.00910921669791757,-0.0336938721132328,
0.0800685233662486));
#91057=CARTESIAN_POINT('Origin',(0.00557432929956971,-0.0345589643415202,
0.0635201621466345));
#91058=CARTESIAN_POINT('Ctrl Pts',(0.0089927908359826,-0.03424362768739,
0.0798353275172685));
#91059=CARTESIAN_POINT('Ctrl Pts',(0.0087783651738213,-0.0339430054201861,
0.0798681027185399));
#91060=CARTESIAN_POINT('Ctrl Pts',(0.00856207991003499,-0.0336441434784164,
0.079884633389445));
#91061=CARTESIAN_POINT('Ctrl Pts',(0.0092390412442504,-0.03424362768739,
0.0797921912630507));
#91062=CARTESIAN_POINT('Ctrl Pts',(0.00902624249273686,-0.0339430054201861,
0.079834253951576));
#91063=CARTESIAN_POINT('Ctrl Pts',(0.00881087994612146,-0.0336441434784164,
0.0798601682705334));
#91064=CARTESIAN_POINT('Ctrl Pts',(0.00872236994997309,-0.0335235895815127,
0.0798686510179241));
#91065=CARTESIAN_POINT('Ctrl Pts',(0.00864364145972468,-0.0334144449262719,
0.079876891756908));
#91066=CARTESIAN_POINT('Ctrl Pts',(0.00856465227251364,-0.0333049234473133,
0.079883515492144));
#91067=CARTESIAN_POINT('Ctrl Pts',(0.00848550262403521,-0.0331951640388589,
0.0798885046046268));
#91068=CARTESIAN_POINT('Ctrl Pts',(0.00880885115926208,-0.0335235895815127,
0.079941877877251));
#91069=CARTESIAN_POINT('Ctrl Pts',(0.00872911455712463,-0.0334144449262719,
0.0799513092003467));
#91070=CARTESIAN_POINT('Ctrl Pts',(0.0086490915032544,-0.0333049234473133,
0.0799591040606983));
#91071=CARTESIAN_POINT('Ctrl Pts',(0.00856888341969378,-0.0331951640388589,
0.0799652432220389));
#91072=CARTESIAN_POINT('Ctrl Pts',(0.00889533236855107,-0.0335235895815127,
0.080015104736578));
#91073=CARTESIAN_POINT('Ctrl Pts',(0.00881458765452459,-0.0334144449262719,
0.0800257266437853));
#91074=CARTESIAN_POINT('Ctrl Pts',(0.00873353073399516,-0.0333049234473133,
0.0800346926292525));
#91075=CARTESIAN_POINT('Ctrl Pts',(0.00865226421535234,-0.0331951640388589,
0.080041981839451));
#91076=CARTESIAN_POINT('Ctrl Pts',(0.00898181357784006,-0.0335235895815127,
0.0800883315959049));
#91077=CARTESIAN_POINT('Ctrl Pts',(0.00890006075192454,-0.0334144449262719,
0.0801001440872239));
#91078=CARTESIAN_POINT('Ctrl Pts',(0.00881796996473591,-0.0333049234473133,
0.0801102811978068));
#91079=CARTESIAN_POINT('Ctrl Pts',(0.0087356450110109,-0.0331951640388589,
0.0801187204568631));
#91080=CARTESIAN_POINT('Origin',(0.00819772362135878,-0.0326434571771167,
0.0632239306732631));
#91081=CARTESIAN_POINT('Ctrl Pts',(0.00838399210321821,-0.0336938721132464,
0.0801458745264825));
#91082=CARTESIAN_POINT('Ctrl Pts',(0.00834889625996981,-0.0336474569764995,
0.0801473976214333));
#91083=CARTESIAN_POINT('Ctrl Pts',(0.00831378499176157,-0.033601104548885,
0.0801485097708635));
#91084=CARTESIAN_POINT('Ctrl Pts',(0.00822489133855471,-0.0334837508662659,
0.0801513254773534));
#91085=CARTESIAN_POINT('Ctrl Pts',(0.00813595328566807,-0.0333660264799515,
0.0801515058442983));
#91086=CARTESIAN_POINT('Ctrl Pts',(0.00859804663144723,-0.0336938721132464,
0.0798817709516805));
#91087=CARTESIAN_POINT('Ctrl Pts',(0.00856449667406112,-0.0336474569764995,
0.0798845469788159));
#91088=CARTESIAN_POINT('Ctrl Pts',(0.00853091651863692,-0.033601104548885,
0.0798869300711249));
#91089=CARTESIAN_POINT('Ctrl Pts',(0.0084458992907428,-0.0334837508662659,
0.0798929635125836));
#91090=CARTESIAN_POINT('Ctrl Pts',(0.0083607406127759,-0.0333660264799515,
0.0798964750680177));
#91091=CARTESIAN_POINT('Ctrl Pts',(0.00859804663144739,-0.0336938721132427,
0.0798817709516913));
#91092=CARTESIAN_POINT('Ctrl Pts',(0.0085644966740662,-0.0336474569765027,
0.0798845469788263));
#91093=CARTESIAN_POINT('Ctrl Pts',(0.00853091651864692,-0.0336011045488949,
0.0798869300711349));
#91094=CARTESIAN_POINT('Ctrl Pts',(0.00844660736846413,-0.0334847282626114,
0.0798929132622442));
#91095=CARTESIAN_POINT('Ctrl Pts',(0.00836215880828412,-0.0333679869984219,
0.079896416412814));
#91096=CARTESIAN_POINT('Ctrl Pts',(0.0085980466314447,-0.0336938721132429,
0.0798817709516807));
#91097=CARTESIAN_POINT('Ctrl Pts',(0.0084780571365088,-0.0335278710435085,
0.0798916992532303));
#91098=CARTESIAN_POINT('Ctrl Pts',(0.00835779850464323,-0.0333620469224321,
0.0798978612226623));
#91099=CARTESIAN_POINT('Ctrl Pts',(0.00823720990302569,-0.0331951640388602,
0.0799002399214836));
#91100=CARTESIAN_POINT('Ctrl Pts',(0.00868142448093768,-0.0336938721132429,
0.0798730437506859));
#91101=CARTESIAN_POINT('Ctrl Pts',(0.00856161768214375,-0.0335278710435085,
0.0798847174928915));
#91102=CARTESIAN_POINT('Ctrl Pts',(0.00844148694558292,-0.0333620469224321,
0.0798926300182409));
#91103=CARTESIAN_POINT('Ctrl Pts',(0.00832097121086305,-0.0331951640388602,
0.0798967652801135));
#91104=CARTESIAN_POINT('Ctrl Pts',(0.00876480233043065,-0.0336938721132429,
0.0798643165496912));
#91105=CARTESIAN_POINT('Ctrl Pts',(0.0086451782277787,-0.0335278710435085,
0.0798777357325528));
#91106=CARTESIAN_POINT('Ctrl Pts',(0.00852517538652261,-0.0333620469224321,
0.0798873988138196));
#91107=CARTESIAN_POINT('Ctrl Pts',(0.00840473251870041,-0.0331951640388602,
0.0798932906387434));
#91108=CARTESIAN_POINT('Ctrl Pts',(0.00884818017992363,-0.0336938721132429,
0.0798555893486965));
#91109=CARTESIAN_POINT('Ctrl Pts',(0.00872873877341365,-0.0335278710435085,
0.079870753972214));
#91110=CARTESIAN_POINT('Ctrl Pts',(0.00860886382746229,-0.0333620469224321,
0.0798821676093983));
#91111=CARTESIAN_POINT('Ctrl Pts',(0.00848849382653776,-0.0331951640388602,
0.0798898159973733));
#91112=CARTESIAN_POINT('Ctrl Pts',(0.00836211297397097,-0.0330240426238156,
0.0798949524992678));
#91113=CARTESIAN_POINT('Ctrl Pts',(0.00828297065625796,-0.0329142774063509,
0.0798982357379686));
#91114=CARTESIAN_POINT('Ctrl Pts',(0.00820372100949799,-0.0328043479726687,
0.0798998845207034));
#91115=CARTESIAN_POINT('Ctrl Pts',(0.00812446550022084,-0.0326943950436595,
0.0798998939392863));
#91116=CARTESIAN_POINT('Ctrl Pts',(0.00844382547624734,-0.0330240426238156,
0.0799734649374992));
#91117=CARTESIAN_POINT('Ctrl Pts',(0.00836360157320673,-0.0329142774063509,
0.0799778738455274));
#91118=CARTESIAN_POINT('Ctrl Pts',(0.00828324653118004,-0.0328043479726687,
0.0799806264993869));
#91119=CARTESIAN_POINT('Ctrl Pts',(0.0082028631938455,-0.0326943950436595,
0.0799817165377517));
#91120=CARTESIAN_POINT('Ctrl Pts',(0.0085255379785237,-0.0330240426238156,
0.0800519773757305));
#91121=CARTESIAN_POINT('Ctrl Pts',(0.0084442324901555,-0.0329142774063509,
0.0800575119530863));
#91122=CARTESIAN_POINT('Ctrl Pts',(0.00836277205286208,-0.0328043479726687,
0.0800613684780704));
#91123=CARTESIAN_POINT('Ctrl Pts',(0.00828126088747015,-0.0326943950436595,
0.0800635391362171));
#91124=CARTESIAN_POINT('Ctrl Pts',(0.00860725048080007,-0.0330240426238156,
0.0801304898139618));
#91125=CARTESIAN_POINT('Ctrl Pts',(0.00852486340710428,-0.0329142774063509,
0.0801371500606451));
#91126=CARTESIAN_POINT('Ctrl Pts',(0.00844229757454413,-0.0328043479726687,
0.0801421104567539));
#91127=CARTESIAN_POINT('Ctrl Pts',(0.00835965858109481,-0.0326943950436595,
0.0801453617346825));
#91128=CARTESIAN_POINT('Origin',(0.00819579695600056,-0.03263966828562,
0.0631002711133243));
#91129=CARTESIAN_POINT('Ctrl Pts',(0.00800836761556648,-0.0331951640388588,
0.0801488898535787));
#91130=CARTESIAN_POINT('Ctrl Pts',(0.00792574503386902,-0.0330855618127431,
0.0801473002510698));
#91131=CARTESIAN_POINT('Ctrl Pts',(0.007843095745071,-0.0329757224171935,
0.080144001834907));
#91132=CARTESIAN_POINT('Ctrl Pts',(0.00776052579376048,-0.0328657861694599,
0.0801389936373661));
#91133=CARTESIAN_POINT('Ctrl Pts',(0.00808510617188339,-0.0331951640388588,
0.0800655091243034));
#91134=CARTESIAN_POINT('Ctrl Pts',(0.00800363199118756,-0.0330855618127431,
0.08006497644029));
#91135=CARTESIAN_POINT('Ctrl Pts',(0.0079221100865563,-0.0329757224171935,
0.080062759440029));
#91136=CARTESIAN_POINT('Ctrl Pts',(0.007840644990966,-0.0328657861694599,
0.0800588558417936));
#91137=CARTESIAN_POINT('Ctrl Pts',(0.0081618447282003,-0.0331951640388588,
0.0799821283950282));
#91138=CARTESIAN_POINT('Ctrl Pts',(0.0080815189485061,-0.0330855618127431,
0.0799826526295103));
#91139=CARTESIAN_POINT('Ctrl Pts',(0.0080011244280416,-0.0329757224171935,
0.0799815170451511));
#91140=CARTESIAN_POINT('Ctrl Pts',(0.00792076418817151,-0.0328657861694599,
0.0799787180462211));
#91141=CARTESIAN_POINT('Ctrl Pts',(0.00823858328451721,-0.0331951640388588,
0.079898747665753));
#91142=CARTESIAN_POINT('Ctrl Pts',(0.00815940590582465,-0.0330855618127431,
0.0799003288187305));
#91143=CARTESIAN_POINT('Ctrl Pts',(0.0080801387695269,-0.0329757224171935,
0.0799002746502731));
#91144=CARTESIAN_POINT('Ctrl Pts',(0.00800088338537702,-0.0328657861694599,
0.0798985802506486));
#91145=CARTESIAN_POINT('Origin',(0.00867489634889909,-0.0326401908832791,
0.0631419441633169));
#91146=CARTESIAN_POINT('Ctrl Pts',(0.00827330551698484,-0.0332451089994433,
0.0798994145593807));
#91147=CARTESIAN_POINT('Ctrl Pts',(0.00805646279914546,-0.0329451141710259,
0.0799050539238054));
#91148=CARTESIAN_POINT('Ctrl Pts',(0.00783981132859943,-0.0326442513127504,
0.0798943437874235));
#91149=CARTESIAN_POINT('Ctrl Pts',(0.00852302072379411,-0.0332451089994433,
0.0798874849538466));
#91150=CARTESIAN_POINT('Ctrl Pts',(0.00830662793838874,-0.0329451141710259,
0.0799025424813854));
#91151=CARTESIAN_POINT('Ctrl Pts',(0.00808971570751864,-0.0326442513127504,
0.0799012576428604));
#91152=CARTESIAN_POINT('Ctrl Pts',(0.00800091499146258,-0.0325229783203385,
0.0798985810160486));
#91153=CARTESIAN_POINT('Ctrl Pts',(0.00792167092931193,-0.032413025311208,
0.0798968872943917));
#91154=CARTESIAN_POINT('Ctrl Pts',(0.00784247392288333,-0.0323031222247695,
0.0798935545644289));
#91155=CARTESIAN_POINT('Ctrl Pts',(0.00776342526726939,-0.0321934096636185,
0.0798885906748361));
#91156=CARTESIAN_POINT('Ctrl Pts',(0.00807753644924918,-0.0325229783203385,
0.0799820693077831));
#91157=CARTESIAN_POINT('Ctrl Pts',(0.00799714150284369,-0.032413025311208,
0.0799814318112269));
#91158=CARTESIAN_POINT('Ctrl Pts',(0.00791677193734176,-0.0323031222247695,
0.0799791313386489));
#91159=CARTESIAN_POINT('Ctrl Pts',(0.00783653059645855,-0.0321934096636185,
0.0799751744694758));
#91160=CARTESIAN_POINT('Ctrl Pts',(0.00815415790703578,-0.0325229783203385,
0.0800655575995175));
#91161=CARTESIAN_POINT('Ctrl Pts',(0.00807261207637545,-0.032413025311208,
0.0800659763280621));
#91162=CARTESIAN_POINT('Ctrl Pts',(0.0079910699518002,-0.0323031222247695,
0.0800647081128688));
#91163=CARTESIAN_POINT('Ctrl Pts',(0.00790963592564772,-0.0321934096636185,
0.0800617582641156));
#91164=CARTESIAN_POINT('Ctrl Pts',(0.00823077936482238,-0.0325229783203385,
0.080149045891252));
#91165=CARTESIAN_POINT('Ctrl Pts',(0.00814808264990721,-0.032413025311208,
0.0801505208448973));
#91166=CARTESIAN_POINT('Ctrl Pts',(0.00806536796625863,-0.0323031222247695,
0.0801502848870888));
#91167=CARTESIAN_POINT('Ctrl Pts',(0.00798274125483688,-0.0321934096636185,
0.0801483420587554));
#91168=CARTESIAN_POINT('Origin',(0.00819550299769431,-0.0326393375178307,
0.063108791946804));
#91169=CARTESIAN_POINT('Ctrl Pts',(0.00763192194936668,-0.0326943950436594,
0.080129805473483));
#91170=CARTESIAN_POINT('Ctrl Pts',(0.00754950902259242,-0.0325844576448127,
0.0801230267174799));
#91171=CARTESIAN_POINT('Ctrl Pts',(0.00746723045911536,-0.0324744968375319,
0.0801145430472902));
#91172=CARTESIAN_POINT('Ctrl Pts',(0.00738519152910246,-0.0323646534831895,
0.0801043667867468));
#91173=CARTESIAN_POINT('Ctrl Pts',(0.00771374452105953,-0.0326943950436594,
0.0800514078055102));
#91174=CARTESIAN_POINT('Ctrl Pts',(0.00763241206108282,-0.0325844576448127,
0.0800457567178969));
#91175=CARTESIAN_POINT('Ctrl Pts',(0.00755119071883849,-0.0324744968375319,
0.0800384231417286));
#91176=CARTESIAN_POINT('Ctrl Pts',(0.00747018443024492,-0.0323646534831895,
0.0800294179085872));
#91177=CARTESIAN_POINT('Ctrl Pts',(0.00779556709275238,-0.0326943950436594,
0.0799730101375374));
#91178=CARTESIAN_POINT('Ctrl Pts',(0.00771531509957322,-0.0325844576448127,
0.0799684867183139));
#91179=CARTESIAN_POINT('Ctrl Pts',(0.00763515097856162,-0.0324744968375319,
0.079962303236167));
#91180=CARTESIAN_POINT('Ctrl Pts',(0.00755517733138738,-0.0323646534831895,
0.0799544690304276));
#91181=CARTESIAN_POINT('Ctrl Pts',(0.00787738966444523,-0.0326943950436594,
0.0798946124695647));
#91182=CARTESIAN_POINT('Ctrl Pts',(0.00779821813806362,-0.0325844576448127,
0.0798912167187309));
#91183=CARTESIAN_POINT('Ctrl Pts',(0.00771911123828475,-0.0324744968375319,
0.0798861833306055));
#91184=CARTESIAN_POINT('Ctrl Pts',(0.00764017023252984,-0.0323646534831895,
0.0798795201522679));
#91185=CARTESIAN_POINT('Origin',(0.00867633101255401,-0.0326395579067508,
0.063104130100388));
#91186=CARTESIAN_POINT('Ctrl Pts',(0.00791204093642377,-0.0327445246961877,
0.0798974594944391));
#91187=CARTESIAN_POINT('Ctrl Pts',(0.00769527196015635,-0.0324436878365475,
0.0798894735424739));
#91188=CARTESIAN_POINT('Ctrl Pts',(0.00747972033617851,-0.0321434074463188,
0.0798651823526856));
#91189=CARTESIAN_POINT('Ctrl Pts',(0.00816201247917376,-0.0327445246961877,
0.0799012314720613));
#91190=CARTESIAN_POINT('Ctrl Pts',(0.00794510124044614,-0.0324436878365475,
0.0799026733508568));
#91191=CARTESIAN_POINT('Ctrl Pts',(0.00772869761542315,-0.0321434074463188,
0.0798877724925685));
#91192=CARTESIAN_POINT('Ctrl Pts',(0.00725741743083938,-0.0321934096636185,
0.0800871215330967));
#91193=CARTESIAN_POINT('Ctrl Pts',(0.00717553989778692,-0.0320835708272305,
0.0800751736878214));
#91194=CARTESIAN_POINT('Ctrl Pts',(0.00709395711706809,-0.0319739230346347,
0.080061538321491));
#91195=CARTESIAN_POINT('Ctrl Pts',(0.00701277212929694,-0.0318646057455576,
0.0800462408904464));
#91196=CARTESIAN_POINT('Ctrl Pts',(0.00734400130003629,-0.0321934096636185,
0.0800140161409567));
#91197=CARTESIAN_POINT('Ctrl Pts',(0.00726313194731632,-0.0320835708272305,
0.080003262354717));
#91198=CARTESIAN_POINT('Ctrl Pts',(0.00718253205115473,-0.0319739230346347,
0.079990841219059));
#91199=CARTESIAN_POINT('Ctrl Pts',(0.0071023035138616,-0.0318646057455576,
0.0799767765402876));
#91200=CARTESIAN_POINT('Ctrl Pts',(0.00743058516923321,-0.0321934096636185,
0.0799409107488167));
#91201=CARTESIAN_POINT('Ctrl Pts',(0.00735072399684572,-0.0320835708272305,
0.0799313510216126));
#91202=CARTESIAN_POINT('Ctrl Pts',(0.00727110698524138,-0.0319739230346347,
0.0799201441166271));
#91203=CARTESIAN_POINT('Ctrl Pts',(0.00719183489842626,-0.0318646057455576,
0.0799073121901288));
#91204=CARTESIAN_POINT('Ctrl Pts',(0.00751716903843012,-0.0321934096636185,
0.0798678053566767));
#91205=CARTESIAN_POINT('Ctrl Pts',(0.00743831604637512,-0.0320835708272305,
0.0798594396885082));
#91206=CARTESIAN_POINT('Ctrl Pts',(0.00735968191932802,-0.0319739230346347,
0.0798494470141951));
#91207=CARTESIAN_POINT('Ctrl Pts',(0.00728136628299092,-0.0318646057455576,
0.07983784783997));
#91208=CARTESIAN_POINT('Origin',(0.0086698683816937,-0.0326371942644933,
0.0631992123700286));
#91209=CARTESIAN_POINT('Ctrl Pts',(0.00764056873150404,-0.0320218834582349,
0.0798803841538758));
#91210=CARTESIAN_POINT('Ctrl Pts',(0.00758092928557567,-0.0319391099350626,
0.0798753550699015));
#91211=CARTESIAN_POINT('Ctrl Pts',(0.00752140450352376,-0.0318564869454889,
0.0798693977546107));
#91212=CARTESIAN_POINT('Ctrl Pts',(0.00746203733617003,-0.0317740741446463,
0.0798625205946922));
#91213=CARTESIAN_POINT('Ctrl Pts',(0.0076717219673248,-0.0320218834582349,
0.0799189367665705));
#91214=CARTESIAN_POINT('Ctrl Pts',(0.00761168128189862,-0.0319391099350626,
0.0799142319124686));
#91215=CARTESIAN_POINT('Ctrl Pts',(0.00755175044055479,-0.0318564869454889,
0.0799085923651966));
#91216=CARTESIAN_POINT('Ctrl Pts',(0.007491972711483,-0.0317740741446463,
0.0799020263076026));
#91217=CARTESIAN_POINT('Ctrl Pts',(0.00770287520314557,-0.0320218834582349,
0.0799574893792652));
#91218=CARTESIAN_POINT('Ctrl Pts',(0.00764243327822157,-0.0319391099350626,
0.0799531087550357));
#91219=CARTESIAN_POINT('Ctrl Pts',(0.00758209637758582,-0.0318564869454889,
0.0799477869757825));
#91220=CARTESIAN_POINT('Ctrl Pts',(0.00752190808679598,-0.0317740741446463,
0.0799415320205131));
#91221=CARTESIAN_POINT('Ctrl Pts',(0.00773402843896634,-0.0320218834582349,
0.0799960419919599));
#91222=CARTESIAN_POINT('Ctrl Pts',(0.00767318527454453,-0.0319391099350626,
0.0799919855976028));
#91223=CARTESIAN_POINT('Ctrl Pts',(0.00761244231461685,-0.0318564869454889,
0.0799869815863684));
#91224=CARTESIAN_POINT('Ctrl Pts',(0.00755184346210895,-0.0317740741446463,
0.0799810377334236));
#91225=CARTESIAN_POINT('Origin',(0.00819179220557225,-0.0326352985526525,
0.0632314705245195));
#91226=CARTESIAN_POINT('Ctrl Pts',(0.00754600788596507,-0.0322357242816073,
0.0798722636997962));
#91227=CARTESIAN_POINT('Ctrl Pts',(0.00736376120863064,-0.0319819883628706,
0.0798538623374596));
#91228=CARTESIAN_POINT('Ctrl Pts',(0.0071830548081292,-0.0317295851069886,
0.0798239013903267));
#91229=CARTESIAN_POINT('Ctrl Pts',(0.00779523028038902,-0.0322357242816073,
0.0798919664437063));
#91230=CARTESIAN_POINT('Ctrl Pts',(0.00761235609621458,-0.0319819883628706,
0.0798815024914024));
#91231=CARTESIAN_POINT('Ctrl Pts',(0.00743051838048631,-0.0317295851069886,
0.0798594229381006));
#91232=CARTESIAN_POINT('Origin',(0.00653733631511826,-0.0391228853390952,
0.0861234626489958));
#91233=CARTESIAN_POINT('Ctrl Pts',(0.00995668358200857,-0.0352722978779648,
0.0796020305429413));
#91234=CARTESIAN_POINT('Ctrl Pts',(0.00993866330670262,-0.0352466642097253,
0.0796077193350789));
#91235=CARTESIAN_POINT('Ctrl Pts',(0.00992068268751648,-0.0352210183808319,
0.0796134778231547));
#91236=CARTESIAN_POINT('Ctrl Pts',(0.00990274125235295,-0.0351953608940152,
0.0796193067175269));
#91237=CARTESIAN_POINT('Origin',(0.0112580326694923,-0.0352456003065096,
0.0843260366550522));
#91238=CARTESIAN_POINT('Ctrl Pts',(0.00978333676035485,-0.0350241211493338,
0.0796551938002844));
#91239=CARTESIAN_POINT('Ctrl Pts',(0.00970750497639259,-0.0349144232867421,
0.0796780534829736));
#91240=CARTESIAN_POINT('Ctrl Pts',(0.00963115527749999,-0.0348045283677512,
0.0796993593511939));
#91241=CARTESIAN_POINT('Ctrl Pts',(0.00955438444240266,-0.0346945769586886,
0.0797190804756865));
#91242=CARTESIAN_POINT('Ctrl Pts',(0.00988200738449934,-0.0350241211493338,
0.0797109185679786));
#91243=CARTESIAN_POINT('Ctrl Pts',(0.00980540801474475,-0.0349144232867421,
0.0797351373979976));
#91244=CARTESIAN_POINT('Ctrl Pts',(0.0097282621760775,-0.0348045283677512,
0.0797577873605168));
#91245=CARTESIAN_POINT('Ctrl Pts',(0.00965066760291177,-0.0346945769586886,
0.079778835766716));
#91246=CARTESIAN_POINT('Ctrl Pts',(0.00998067800864383,-0.0350241211493338,
0.0797666433356729));
#91247=CARTESIAN_POINT('Ctrl Pts',(0.00990331105309691,-0.0349144232867421,
0.0797922213130217));
#91248=CARTESIAN_POINT('Ctrl Pts',(0.00982536907465503,-0.0348045283677512,
0.0798162153698396));
#91249=CARTESIAN_POINT('Ctrl Pts',(0.00974695076342089,-0.0346945769586886,
0.0798385910577455));
#91250=CARTESIAN_POINT('Ctrl Pts',(0.0100793486327883,-0.0350241211493338,
0.0798223681033672));
#91251=CARTESIAN_POINT('Ctrl Pts',(0.0100012140914491,-0.0349144232867421,
0.0798493052280457));
#91252=CARTESIAN_POINT('Ctrl Pts',(0.00992247597323254,-0.0348045283677512,
0.0798746433791625));
#91253=CARTESIAN_POINT('Ctrl Pts',(0.00984323392393,-0.0346945769586886,
0.079898346348775));
#91254=CARTESIAN_POINT('Origin',(0.00555190943416128,-0.0345629067942252,
0.0634143835178251));
#91255=CARTESIAN_POINT('Ctrl Pts',(0.00954912843121769,-0.0351970973651596,
0.0799070747675207));
#91256=CARTESIAN_POINT('Ctrl Pts',(0.00946937196253186,-0.0350869349321763,
0.0799268210079634));
#91257=CARTESIAN_POINT('Ctrl Pts',(0.00938913891111949,-0.0349764985129723,
0.0799449255131765));
#91258=CARTESIAN_POINT('Ctrl Pts',(0.00930853184056139,-0.0348659306849652,
0.0799613587094737));
#91259=CARTESIAN_POINT('Ctrl Pts',(0.00958799576292898,-0.0351970973651596,
0.0798346192558197));
#91260=CARTESIAN_POINT('Ctrl Pts',(0.00950924306716316,-0.0350869349321763,
0.0798549039504687));
#91261=CARTESIAN_POINT('Ctrl Pts',(0.00943000342602006,-0.0349764985129723,
0.0798735682238201));
#91262=CARTESIAN_POINT('Ctrl Pts',(0.009350378073399,-0.0348659306849652,
0.0798905818527512));
#91263=CARTESIAN_POINT('Ctrl Pts',(0.00962686309464028,-0.0351970973651596,
0.0797621637441187));
#91264=CARTESIAN_POINT('Ctrl Pts',(0.00954911417179447,-0.0350869349321763,
0.079782986892974));
#91265=CARTESIAN_POINT('Ctrl Pts',(0.00947086794092062,-0.0349764985129723,
0.0798022109344636));
#91266=CARTESIAN_POINT('Ctrl Pts',(0.00939222430623661,-0.0348659306849652,
0.0798198049960288));
#91267=CARTESIAN_POINT('Ctrl Pts',(0.00966573042635158,-0.0351970973651596,
0.0796897082324177));
#91268=CARTESIAN_POINT('Ctrl Pts',(0.00958898527642577,-0.0350869349321763,
0.0797110698354793));
#91269=CARTESIAN_POINT('Ctrl Pts',(0.00951173245582118,-0.0349764985129723,
0.0797308536451072));
#91270=CARTESIAN_POINT('Ctrl Pts',(0.00943407053907422,-0.0348659306849652,
0.0797490281393064));
#91271=CARTESIAN_POINT('Origin',(0.00602813602901201,-0.0345637187965951,
0.0633470516033824));
#91272=CARTESIAN_POINT('Ctrl Pts',(0.00969842342285979,-0.0352450361861252,
0.0796816028416335));
#91273=CARTESIAN_POINT('Ctrl Pts',(0.00948979560363212,-0.0349452761023764,
0.0797409914086066));
#91274=CARTESIAN_POINT('Ctrl Pts',(0.00927728708429922,-0.0346444289983475,
0.0797844965583448));
#91275=CARTESIAN_POINT('Ctrl Pts',(0.00993732667225551,-0.0352450361861252,
0.0796079466305705));
#91276=CARTESIAN_POINT('Ctrl Pts',(0.00973147684254131,-0.0349452761023764,
0.0796763455812163));
#91277=CARTESIAN_POINT('Ctrl Pts',(0.00952105972179818,-0.0346444289983475,
0.0797290447666083));
#91278=CARTESIAN_POINT('Ctrl Pts',(0.00931268830210933,-0.0346945769586885,
0.07977713313011));
#91279=CARTESIAN_POINT('Ctrl Pts',(0.00919482574571989,-0.034527515336289,
0.0798020352445747));
#91280=CARTESIAN_POINT('Ctrl Pts',(0.00907614955545729,-0.0343603235965158,
0.0798232371310882));
#91281=CARTESIAN_POINT('Ctrl Pts',(0.00895701165478281,-0.034193496108874,
0.0798406813005298));
#91282=CARTESIAN_POINT('Ctrl Pts',(0.00939431487537028,-0.0346945769586885,
0.0797580247322456));
#91283=CARTESIAN_POINT('Ctrl Pts',(0.00927685255202469,-0.034527515336289,
0.0797846365479687));
#91284=CARTESIAN_POINT('Ctrl Pts',(0.0091585229297958,-0.0343603235965158,
0.0798075611649178));
#91285=CARTESIAN_POINT('Ctrl Pts',(0.00903967698287652,-0.034193496108874,
0.0798267359836661));
#91286=CARTESIAN_POINT('Ctrl Pts',(0.00947594144863123,-0.0346945769586885,
0.0797389163343812));
#91287=CARTESIAN_POINT('Ctrl Pts',(0.00935887935832949,-0.034527515336289,
0.0797672378513627));
#91288=CARTESIAN_POINT('Ctrl Pts',(0.00924089630413431,-0.0343603235965158,
0.0797918851987474));
#91289=CARTESIAN_POINT('Ctrl Pts',(0.00912234231097024,-0.034193496108874,
0.0798127906668024));
#91290=CARTESIAN_POINT('Ctrl Pts',(0.00955756802189218,-0.0346945769586885,
0.0797198079365168));
#91291=CARTESIAN_POINT('Ctrl Pts',(0.00944090616463429,-0.034527515336289,
0.0797498391547567));
#91292=CARTESIAN_POINT('Ctrl Pts',(0.00932326967847282,-0.0343603235965158,
0.079776209232577));
#91293=CARTESIAN_POINT('Ctrl Pts',(0.00920500763906395,-0.034193496108874,
0.0797988453499388));
#91294=CARTESIAN_POINT('Origin',(0.00601624531389674,-0.0345626446731352,
0.0632898437234962));
#91295=CARTESIAN_POINT('Origin',(0.00554884660254213,-0.0345625596230794,
0.0634026738054348));
#91296=CARTESIAN_POINT('Ctrl Pts',(0.00913449179185841,-0.0346945769586886,
0.0800642595569595));
#91297=CARTESIAN_POINT('Ctrl Pts',(0.00905299030585987,-0.034584662917669,
0.0800781876460834));
#91298=CARTESIAN_POINT('Ctrl Pts',(0.0089711868720442,-0.0344746925051587,
0.0800904326969005));
#91299=CARTESIAN_POINT('Ctrl Pts',(0.0088891863711939,-0.0343648066255171,
0.0801009794525156));
#91300=CARTESIAN_POINT('Ctrl Pts',(0.00919424703583845,-0.0346945769586886,
0.0799679764722608));
#91301=CARTESIAN_POINT('Ctrl Pts',(0.00911407237941238,-0.034584662917669,
0.0799827280188495));
#91302=CARTESIAN_POINT('Ctrl Pts',(0.00903357897303276,-0.0344746925051587,
0.0799958241060704));
#91303=CARTESIAN_POINT('Ctrl Pts',(0.00895287002342734,-0.0343648066255171,
0.0800072483796505));
#91304=CARTESIAN_POINT('Ctrl Pts',(0.00925400227981849,-0.0346945769586886,
0.0798716933875621));
#91305=CARTESIAN_POINT('Ctrl Pts',(0.0091751544529649,-0.034584662917669,
0.0798872683916155));
#91306=CARTESIAN_POINT('Ctrl Pts',(0.00909597107402132,-0.0344746925051587,
0.0799012155152404));
#91307=CARTESIAN_POINT('Ctrl Pts',(0.00901655367566078,-0.0343648066255171,
0.0799135173067855));
#91308=CARTESIAN_POINT('Ctrl Pts',(0.00931375752379853,-0.0346945769586886,
0.0797754103028634));
#91309=CARTESIAN_POINT('Ctrl Pts',(0.00923623652651741,-0.034584662917669,
0.0797918087643815));
#91310=CARTESIAN_POINT('Ctrl Pts',(0.00915836317500988,-0.0344746925051587,
0.0798066069244103));
#91311=CARTESIAN_POINT('Ctrl Pts',(0.00908023732789422,-0.0343648066255171,
0.0798197862339205));
#91312=CARTESIAN_POINT('Ctrl Pts',(0.0094343889890219,-0.0345231616327822,
0.0797485346823557));
#91313=CARTESIAN_POINT('Ctrl Pts',(0.00935722107053248,-0.0344132092796975,
0.0797665995518505));
#91314=CARTESIAN_POINT('Ctrl Pts',(0.00927968347597679,-0.0343032738558974,
0.0797830673317564));
#91315=CARTESIAN_POINT('Ctrl Pts',(0.00920187608038533,-0.0341934961088741,
0.0797979194694375));
#91316=CARTESIAN_POINT('Ctrl Pts',(0.00952936591106417,-0.0345231616327822,
0.0798103450408606));
#91317=CARTESIAN_POINT('Ctrl Pts',(0.00945134602380479,-0.0344132092796975,
0.079829719033509));
#91318=CARTESIAN_POINT('Ctrl Pts',(0.009372929426257,-0.0343032738558974,
0.0798474782467216));
#91319=CARTESIAN_POINT('Ctrl Pts',(0.00929421716193573,-0.0341934961088741,
0.0798636025022331));
#91320=CARTESIAN_POINT('Ctrl Pts',(0.00962434283310644,-0.0345231616327822,
0.0798721553993656));
#91321=CARTESIAN_POINT('Ctrl Pts',(0.0095454709770771,-0.0344132092796975,
0.0798928385151674));
#91322=CARTESIAN_POINT('Ctrl Pts',(0.00946617537653722,-0.0343032738558974,
0.0799118891616869));
#91323=CARTESIAN_POINT('Ctrl Pts',(0.00938655824348613,-0.0341934961088741,
0.0799292855350287));
#91324=CARTESIAN_POINT('Ctrl Pts',(0.00971931975514871,-0.0345231616327822,
0.0799339657578705));
#91325=CARTESIAN_POINT('Ctrl Pts',(0.00963959593034941,-0.0344132092796975,
0.0799559579968259));
#91326=CARTESIAN_POINT('Ctrl Pts',(0.00955942132681743,-0.0343032738558974,
0.0799763000766521));
#91327=CARTESIAN_POINT('Ctrl Pts',(0.00947889932503654,-0.0341934961088741,
0.0799949685678243));
#91328=CARTESIAN_POINT('Origin',(0.00805051870546373,-0.0391228853391069,
0.0862278827114944));
#91329=CARTESIAN_POINT('Ctrl Pts',(0.0106255512245337,-0.0352722978779642,
0.0793293161957926));
#91330=CARTESIAN_POINT('Ctrl Pts',(0.0106083860391948,-0.0352466642097249,
0.0793372186694786));
#91331=CARTESIAN_POINT('Ctrl Pts',(0.0105912689324926,-0.0352210183808317,
0.0793451853193));
#91332=CARTESIAN_POINT('Ctrl Pts',(0.0105741995250841,-0.0351953608940152,
0.0793532169091828));
#91333=CARTESIAN_POINT('Origin',(0.0125087137471874,-0.0352456003065102,
0.0838529698196086));
#91334=CARTESIAN_POINT('Ctrl Pts',(0.010460234417295,-0.0350241211493339,
0.079403786362658));
#91335=CARTESIAN_POINT('Ctrl Pts',(0.0103878656675488,-0.0349144232867421,
0.0794359700326123));
#91336=CARTESIAN_POINT('Ctrl Pts',(0.0103147883421944,-0.0348045283677512,
0.0794666770523418));
#91337=CARTESIAN_POINT('Ctrl Pts',(0.0102410945803643,-0.0346945769586886,
0.0794958646068836));
#91338=CARTESIAN_POINT('Ctrl Pts',(0.0105651111594214,-0.0350241211493339,
0.079446705015533));
#91339=CARTESIAN_POINT('Ctrl Pts',(0.0104921512228558,-0.0349144232867421,
0.0794803333195438));
#91340=CARTESIAN_POINT('Ctrl Pts',(0.0104184524952114,-0.0348045283677512,
0.0795124736177594));
#91341=CARTESIAN_POINT('Ctrl Pts',(0.0103441078432417,-0.0346945769586886,
0.0795430812297508));
#91342=CARTESIAN_POINT('Ctrl Pts',(0.0106699879015477,-0.0350241211493339,
0.079489623668408));
#91343=CARTESIAN_POINT('Ctrl Pts',(0.0105964367781628,-0.0349144232867421,
0.0795246966064752));
#91344=CARTESIAN_POINT('Ctrl Pts',(0.0105221166482283,-0.0348045283677512,
0.079558270183177));
#91345=CARTESIAN_POINT('Ctrl Pts',(0.0104471211061191,-0.0346945769586886,
0.0795902978526181));
#91346=CARTESIAN_POINT('Ctrl Pts',(0.0107748646436741,-0.0350241211493339,
0.079532542321283));
#91347=CARTESIAN_POINT('Ctrl Pts',(0.0107007223334698,-0.0349144232867421,
0.0795690598934067));
#91348=CARTESIAN_POINT('Ctrl Pts',(0.0106257808012453,-0.0348045283677512,
0.0796040667485947));
#91349=CARTESIAN_POINT('Ctrl Pts',(0.0105501343689965,-0.0346945769586886,
0.0796375144754854));
#91350=CARTESIAN_POINT('Origin',(0.00422665989078905,-0.0345629067942693,
0.0638213781891361));
#91351=CARTESIAN_POINT('Ctrl Pts',(0.0102594419468846,-0.0351970973651597,
0.0796830352604534));
#91352=CARTESIAN_POINT('Ctrl Pts',(0.0101827892419419,-0.0350869349321763,
0.0797126219320104));
#91353=CARTESIAN_POINT('Ctrl Pts',(0.0101054579482848,-0.0349764985129723,
0.0797406395455647));
#91354=CARTESIAN_POINT('Ctrl Pts',(0.0100275461141839,-0.0348659306849652,
0.0797670459060018));
#91355=CARTESIAN_POINT('Ctrl Pts',(0.0102889217145051,-0.0351970973651597,
0.0796062797137405));
#91356=CARTESIAN_POINT('Ctrl Pts',(0.0102133323536399,-0.0350869349321763,
0.0796362747875257));
#91357=CARTESIAN_POINT('Ctrl Pts',(0.0101370567944662,-0.0349764985129723,
0.079664723247958));
#91358=CARTESIAN_POINT('Ctrl Pts',(0.010060191684662,-0.0348659306849652,
0.0796915824222609));
#91359=CARTESIAN_POINT('Ctrl Pts',(0.0103184014821256,-0.0351970973651597,
0.0795295241670276));
#91360=CARTESIAN_POINT('Ctrl Pts',(0.0102438754653379,-0.0350869349321763,
0.079559927643041));
#91361=CARTESIAN_POINT('Ctrl Pts',(0.0101686556406475,-0.0349764985129723,
0.0795888069503512));
#91362=CARTESIAN_POINT('Ctrl Pts',(0.0100928372551402,-0.0348659306849652,
0.07961611893852));
#91363=CARTESIAN_POINT('Ctrl Pts',(0.0103478812497461,-0.0351970973651597,
0.0794527686203147));
#91364=CARTESIAN_POINT('Ctrl Pts',(0.0102744185770359,-0.0350869349321763,
0.0794835804985563));
#91365=CARTESIAN_POINT('Ctrl Pts',(0.0102002544868289,-0.0349764985129723,
0.0795128906527445));
#91366=CARTESIAN_POINT('Ctrl Pts',(0.0101254828256183,-0.0348659306849652,
0.0795406554547791));
#91367=CARTESIAN_POINT('Origin',(0.00469069237055749,-0.0345637187965033,
0.0636948901884269));
#91368=CARTESIAN_POINT('Ctrl Pts',(0.0103793005773761,-0.0352450361861253,
0.0794406296239892));
#91369=CARTESIAN_POINT('Ctrl Pts',(0.0101797612119527,-0.0349452761023765,
0.0795256978935684));
#91370=CARTESIAN_POINT('Ctrl Pts',(0.0099743810268613,-0.0346444289983475,
0.0795954943720945));
#91371=CARTESIAN_POINT('Ctrl Pts',(0.0106070884321888,-0.0352450361861253,
0.0793376116973946));
#91372=CARTESIAN_POINT('Ctrl Pts',(0.0104114344515231,-0.0349452761023765,
0.0794312711266716));
#91373=CARTESIAN_POINT('Ctrl Pts',(0.010209281491937,-0.0346444289983475,
0.0795099270213863));
#91374=CARTESIAN_POINT('Ctrl Pts',(0.009133422612805,-0.0336938721132462,
0.0800659823155221));
#91375=CARTESIAN_POINT('Ctrl Pts',(0.0090987944051785,-0.0336474569764994,
0.0800718920759333));
#91376=CARTESIAN_POINT('Ctrl Pts',(0.00906409938909167,-0.033601104548885,
0.0800773960645121));
#91377=CARTESIAN_POINT('Ctrl Pts',(0.00897625959288491,-0.0334837508694645,
0.0800913308969353));
#91378=CARTESIAN_POINT('Ctrl Pts',(0.00888804545149575,-0.0333660264863675,
0.0801026567351507));
#91379=CARTESIAN_POINT('Ctrl Pts',(0.00931268830211894,-0.0336938721132462,
0.0797771331301079));
#91380=CARTESIAN_POINT('Ctrl Pts',(0.00927975082462513,-0.0336474569764994,
0.0797840921920854));
#91381=CARTESIAN_POINT('Ctrl Pts',(0.00924673413942139,-0.033601104548885,
0.0797906652024626));
#91382=CARTESIAN_POINT('Ctrl Pts',(0.00916314349076854,-0.0334837508694645,
0.0798073065520604));
#91383=CARTESIAN_POINT('Ctrl Pts',(0.00907909643131272,-0.0333660264863675,
0.0798214636299887));
#91384=CARTESIAN_POINT('Ctrl Pts',(0.00931268830211937,-0.0336938721132426,
0.07977713313012));
#91385=CARTESIAN_POINT('Ctrl Pts',(0.00927975082463032,-0.0336474569765026,
0.0797840921920964));
#91386=CARTESIAN_POINT('Ctrl Pts',(0.00924673413943139,-0.0336011045488949,
0.0797906652024726));
#91387=CARTESIAN_POINT('Ctrl Pts',(0.00916383968703325,-0.033484728265791,
0.0798071679522935));
#91388=CARTESIAN_POINT('Ctrl Pts',(0.00908049609245075,-0.0333679870047996,
0.0798212276902747));
#91389=CARTESIAN_POINT('Ctrl Pts',(0.00943438693042286,-0.0335235895815127,
0.0797485348074296));
#91390=CARTESIAN_POINT('Ctrl Pts',(0.00935731207629897,-0.0334144449262719,
0.0797665778619818));
#91391=CARTESIAN_POINT('Ctrl Pts',(0.00927977591657743,-0.0333049234473133,
0.0797830493373368));
#91392=CARTESIAN_POINT('Ctrl Pts',(0.00920187568831821,-0.0331951640388588,
0.0797979191905567));
#91393=CARTESIAN_POINT('Ctrl Pts',(0.0095293639686092,-0.0335235895815127,
0.0798103452814962));
#91394=CARTESIAN_POINT('Ctrl Pts',(0.00945143817161617,-0.0334144449262719,
0.0798296958819716));
#91395=CARTESIAN_POINT('Ctrl Pts',(0.00937302307848049,-0.0333049234473133,
0.0798474588256224));
#91396=CARTESIAN_POINT('Ctrl Pts',(0.00929421690055794,-0.0331951640388588,
0.0798636023163128));
#91397=CARTESIAN_POINT('Ctrl Pts',(0.00962434100679553,-0.0335235895815127,
0.0798721557555629));
#91398=CARTESIAN_POINT('Ctrl Pts',(0.00954556426693336,-0.0334144449262719,
0.0798928139019615));
#91399=CARTESIAN_POINT('Ctrl Pts',(0.00946627024038355,-0.0333049234473133,
0.079911868313908));
#91400=CARTESIAN_POINT('Ctrl Pts',(0.00938655811279768,-0.0331951640388588,
0.0799292854420688));
#91401=CARTESIAN_POINT('Ctrl Pts',(0.00971931804498187,-0.0335235895815127,
0.0799339662296295));
#91402=CARTESIAN_POINT('Ctrl Pts',(0.00963969036225056,-0.0334144449262719,
0.0799559319219513));
#91403=CARTESIAN_POINT('Ctrl Pts',(0.00955951740228661,-0.0333049234473133,
0.0799762778021936));
#91404=CARTESIAN_POINT('Ctrl Pts',(0.00947889932503741,-0.0331951640388588,
0.0799949685678249));
#91405=CARTESIAN_POINT('Origin',(0.00682774097248567,-0.0326434571769517,
0.0633008186751137));
#91406=CARTESIAN_POINT('Ctrl Pts',(0.00931268830211658,-0.0336938721132428,
0.0797771331301084));
#91407=CARTESIAN_POINT('Ctrl Pts',(0.00919488930632441,-0.0335278710435084,
0.079802021815429));
#91408=CARTESIAN_POINT('Ctrl Pts',(0.00907635124924464,-0.0333620469224321,
0.0798232075990872));
#91409=CARTESIAN_POINT('Ctrl Pts',(0.00895701165478389,-0.0331951640388602,
0.0798406813005296));
#91410=CARTESIAN_POINT('Ctrl Pts',(0.00939431488404191,-0.0336938721132428,
0.0797580247302156));
#91411=CARTESIAN_POINT('Ctrl Pts',(0.00927691590549946,-0.0335278710435084,
0.079784622194973));
#91412=CARTESIAN_POINT('Ctrl Pts',(0.00915872413806543,-0.0333620469224321,
0.0798075287013603));
#91413=CARTESIAN_POINT('Ctrl Pts',(0.00903967699165226,-0.0331951640388602,
0.0798267359821857));
#91414=CARTESIAN_POINT('Ctrl Pts',(0.00947594146596724,-0.0336938721132428,
0.0797389163303228));
#91415=CARTESIAN_POINT('Ctrl Pts',(0.00935894250467452,-0.0335278710435084,
0.079767222574517));
#91416=CARTESIAN_POINT('Ctrl Pts',(0.00924109702688621,-0.0333620469224321,
0.0797918498036334));
#91417=CARTESIAN_POINT('Ctrl Pts',(0.00912234232852063,-0.0331951640388602,
0.0798127906638418));
#91418=CARTESIAN_POINT('Ctrl Pts',(0.00955756804789257,-0.0336938721132428,
0.0797198079304301));
#91419=CARTESIAN_POINT('Ctrl Pts',(0.00944096910384957,-0.0335278710435084,
0.079749822954061));
#91420=CARTESIAN_POINT('Ctrl Pts',(0.009323469915707,-0.0333620469224321,
0.0797761709059064));
#91421=CARTESIAN_POINT('Ctrl Pts',(0.00920500766538901,-0.0331951640388602,
0.0797988453454978));
#91422=CARTESIAN_POINT('Ctrl Pts',(0.00908026713798448,-0.0330240426238156,
0.0798197810654535));
#91423=CARTESIAN_POINT('Ctrl Pts',(0.00900216038000823,-0.0329142774063509,
0.0798329575774273));
#91424=CARTESIAN_POINT('Ctrl Pts',(0.00892374228765528,-0.0328043479726686,
0.079844525973505));
#91425=CARTESIAN_POINT('Ctrl Pts',(0.00884511291220273,-0.0326943950436595,
0.0798544686670751));
#91426=CARTESIAN_POINT('Ctrl Pts',(0.00917117553053269,-0.0330240426238156,
0.079887433117526));
#91427=CARTESIAN_POINT('Ctrl Pts',(0.00909213679962896,-0.0329142774063509,
0.0799018619811748));
#91428=CARTESIAN_POINT('Ctrl Pts',(0.00901276038011862,-0.0328043479726686,
0.0799146640867869));
#91429=CARTESIAN_POINT('Ctrl Pts',(0.00893314750744128,-0.0326943950436595,
0.0799258202334665));
#91430=CARTESIAN_POINT('Ctrl Pts',(0.00926208392308091,-0.0330240426238156,
0.0799550851695986));
#91431=CARTESIAN_POINT('Ctrl Pts',(0.00918211321924968,-0.0329142774063509,
0.0799707663849225));
#91432=CARTESIAN_POINT('Ctrl Pts',(0.00910177847258196,-0.0328043479726686,
0.0799848022000688));
#91433=CARTESIAN_POINT('Ctrl Pts',(0.00902118210267983,-0.0326943950436595,
0.0799971717998579));
#91434=CARTESIAN_POINT('Ctrl Pts',(0.00935299231562913,-0.0330240426238156,
0.080022737221671));
#91435=CARTESIAN_POINT('Ctrl Pts',(0.0092720896388704,-0.0329142774063509,
0.0800396707886701));
#91436=CARTESIAN_POINT('Ctrl Pts',(0.00919079656504529,-0.0328043479726686,
0.0800549403133507));
#91437=CARTESIAN_POINT('Ctrl Pts',(0.00910921669791839,-0.0326943950436595,
0.0800685233662492));
#91438=CARTESIAN_POINT('Origin',(0.00681033084667279,-0.032639668285655,
0.0631783756830151));
#91439=CARTESIAN_POINT('Ctrl Pts',(0.00876113795712716,-0.0331951640388588,
0.0801160520975069));
#91440=CARTESIAN_POINT('Ctrl Pts',(0.00867896765870916,-0.0330855618255042,
0.0801248303837961));
#91441=CARTESIAN_POINT('Ctrl Pts',(0.00859655669269932,-0.0329757224427709,
0.0801319166786189));
#91442=CARTESIAN_POINT('Ctrl Pts',(0.00851401014616768,-0.0328657862078597,
0.0801372967309752));
#91443=CARTESIAN_POINT('Ctrl Pts',(0.00882682103059012,-0.0331951640388588,
0.080023710958784));
#91444=CARTESIAN_POINT('Ctrl Pts',(0.00874592254455342,-0.0330855618255042,
0.0800333938965343));
#91445=CARTESIAN_POINT('Ctrl Pts',(0.00866476561015732,-0.0329757224427709,
0.0800414117811568));
#91446=CARTESIAN_POINT('Ctrl Pts',(0.00858345365009207,-0.0328657862078597,
0.0800477492474656));
#91447=CARTESIAN_POINT('Ctrl Pts',(0.00889250410405308,-0.0331951640388588,
0.079931369820061));
#91448=CARTESIAN_POINT('Ctrl Pts',(0.00881287743039768,-0.0330855618255042,
0.0799419574092724));
#91449=CARTESIAN_POINT('Ctrl Pts',(0.00873297452761533,-0.0329757224427709,
0.0799509068836947));
#91450=CARTESIAN_POINT('Ctrl Pts',(0.00865289715401646,-0.0328657862078597,
0.0799582017639559));
#91451=CARTESIAN_POINT('Ctrl Pts',(0.00895818717751604,-0.0331951640388588,
0.079839028681338));
#91452=CARTESIAN_POINT('Ctrl Pts',(0.00887983231624194,-0.0330855618255042,
0.0798505209220106));
#91453=CARTESIAN_POINT('Ctrl Pts',(0.00880118344507333,-0.0329757224427709,
0.0798604019862326));
#91454=CARTESIAN_POINT('Ctrl Pts',(0.00872234065794085,-0.0328657862078597,
0.0798686542804464));
#91455=CARTESIAN_POINT('Origin',(0.00729087541601512,-0.032640190883449,
0.0631596730550064));
#91456=CARTESIAN_POINT('Ctrl Pts',(0.00899271919874454,-0.0332451089994434,
0.0798353384666383));
#91457=CARTESIAN_POINT('Ctrl Pts',(0.00877829315028171,-0.0329451141710259,
0.079868110961992));
#91458=CARTESIAN_POINT('Ctrl Pts',(0.00856200770526691,-0.0326442513127504,
0.0798846389075943));
#91459=CARTESIAN_POINT('Ctrl Pts',(0.00923897015052509,-0.0332451089994434,
0.0797922053152676));
#91460=CARTESIAN_POINT('Ctrl Pts',(0.00902617089548194,-0.0329451141710259,
0.0798342653172192));
#91461=CARTESIAN_POINT('Ctrl Pts',(0.00881080804937383,-0.0326442513127504,
0.0798601769213243));
#91462=CARTESIAN_POINT('Ctrl Pts',(0.00872237208319403,-0.0325229783203385,
0.0798686510814005));
#91463=CARTESIAN_POINT('Ctrl Pts',(0.00864354060453047,-0.032413025311208,
0.0798769026297948));
#91464=CARTESIAN_POINT('Ctrl Pts',(0.00856455038832971,-0.0323031222247695,
0.0798835221963075));
#91465=CARTESIAN_POINT('Ctrl Pts',(0.00848550291464223,-0.0321934096636185,
0.0798885048720837));
#91466=CARTESIAN_POINT('Ctrl Pts',(0.00880885321546822,-0.0325229783203385,
0.0799418778279532));
#91467=CARTESIAN_POINT('Ctrl Pts',(0.00872901230772316,-0.032413025311208,
0.079951321516843));
#91468=CARTESIAN_POINT('Ctrl Pts',(0.0086489881545835,-0.0323031222247695,
0.0799591121617028));
#91469=CARTESIAN_POINT('Ctrl Pts',(0.00856888361343182,-0.0321934096636185,
0.0799652434003435));
#91470=CARTESIAN_POINT('Ctrl Pts',(0.00889533434774241,-0.0325229783203385,
0.0800151045745059));
#91471=CARTESIAN_POINT('Ctrl Pts',(0.00881448401091586,-0.032413025311208,
0.0800257404038912));
#91472=CARTESIAN_POINT('Ctrl Pts',(0.00873342592083729,-0.0323031222247695,
0.0800347021270982));
#91473=CARTESIAN_POINT('Ctrl Pts',(0.0086522643122214,-0.0321934096636185,
0.0800419819286032));
#91474=CARTESIAN_POINT('Ctrl Pts',(0.00898181548001659,-0.0325229783203385,
0.0800883313210586));
#91475=CARTESIAN_POINT('Ctrl Pts',(0.00889995571410855,-0.032413025311208,
0.0801001592909393));
#91476=CARTESIAN_POINT('Ctrl Pts',(0.00881786368709107,-0.0323031222247695,
0.0801102920924935));
#91477=CARTESIAN_POINT('Ctrl Pts',(0.00873564501101099,-0.0321934096636185,
0.080118720456863));
#91478=CARTESIAN_POINT('Origin',(0.00681110715004839,-0.032639337517817,
0.0631868661705152));
#91479=CARTESIAN_POINT('Ctrl Pts',(0.00838526877037612,-0.0326943950436593,
0.0801442993560545));
#91480=CARTESIAN_POINT('Ctrl Pts',(0.00830265609073561,-0.0325844576448127,
0.0801479031311673));
#91481=CARTESIAN_POINT('Ctrl Pts',(0.0082199630324896,-0.0324744968375319,
0.0801497985956645));
#91482=CARTESIAN_POINT('Ctrl Pts',(0.00813729558030421,-0.0323646534831895,
0.0801499847823517));
#91483=CARTESIAN_POINT('Ctrl Pts',(0.0084566203134214,-0.0326943950436593,
0.0800562647896207));
#91484=CARTESIAN_POINT('Ctrl Pts',(0.0083752209151007,-0.0325844576448127,
0.0800608519227237));
#91485=CARTESIAN_POINT('Ctrl Pts',(0.00829372088658485,-0.0324744968375319,
0.0800637559074518));
#91486=CARTESIAN_POINT('Ctrl Pts',(0.00821222470178364,-0.0323646534831895,
0.0800649744633519));
#91487=CARTESIAN_POINT('Ctrl Pts',(0.00852797185646668,-0.0326943950436593,
0.0799682302231869));
#91488=CARTESIAN_POINT('Ctrl Pts',(0.00844778573946581,-0.0325844576448127,
0.07997380071428));
#91489=CARTESIAN_POINT('Ctrl Pts',(0.0083674787406801,-0.0324744968375319,
0.0799777132192391));
#91490=CARTESIAN_POINT('Ctrl Pts',(0.00828715382326307,-0.0323646534831895,
0.0799799641443521));
#91491=CARTESIAN_POINT('Ctrl Pts',(0.00859932339951197,-0.0326943950436593,
0.0798801956567531));
#91492=CARTESIAN_POINT('Ctrl Pts',(0.00852035056383091,-0.0325844576448127,
0.0798867495058364));
#91493=CARTESIAN_POINT('Ctrl Pts',(0.00844123659477534,-0.0324744968375319,
0.0798916705310263));
#91494=CARTESIAN_POINT('Ctrl Pts',(0.0083620829447425,-0.0323646534831895,
0.0798949538253523));
#91495=CARTESIAN_POINT('Origin',(0.00728755940808319,-0.0326395579067199,
0.0631219773537602));
#91496=CARTESIAN_POINT('Ctrl Pts',(0.00863405826269475,-0.0327445246961877,
0.0798786772760218));
#91497=CARTESIAN_POINT('Ctrl Pts',(0.00841799766936803,-0.0324436878365475,
0.0798979226524051));
#91498=CARTESIAN_POINT('Ctrl Pts',(0.00820110124096409,-0.0321434074463187,
0.079900838787937));
#91499=CARTESIAN_POINT('Ctrl Pts',(0.00888253145931961,-0.0327445246961877,
0.0798510897687218));
#91500=CARTESIAN_POINT('Ctrl Pts',(0.00866751134582941,-0.0324436878365475,
0.0798797064648185));
#91501=CARTESIAN_POINT('Ctrl Pts',(0.00845094655527419,-0.0321434074463187,
0.0798920456703277));
#91502=CARTESIAN_POINT('Ctrl Pts',(0.00800836761556641,-0.0321934096636184,
0.0801488898535788));
#91503=CARTESIAN_POINT('Ctrl Pts',(0.00792563824923524,-0.0320835708272304,
0.0801472981966059));
#91504=CARTESIAN_POINT('Ctrl Pts',(0.00784298980855697,-0.0319739230346347,
0.0801439953829223));
#91505=CARTESIAN_POINT('Ctrl Pts',(0.00776052771216514,-0.0318646057455575,
0.0801389937537248));
#91506=CARTESIAN_POINT('Ctrl Pts',(0.00808510620990588,-0.0321934096636184,
0.08006550908299));
#91507=CARTESIAN_POINT('Ctrl Pts',(0.00800352672938415,-0.0320835708272304,
0.0800649757110394));
#91508=CARTESIAN_POINT('Ctrl Pts',(0.00792200560638128,-0.0319739230346347,
0.0800627543653569));
#91509=CARTESIAN_POINT('Ctrl Pts',(0.00784064692339837,-0.0318646057455575,
0.0800588558927816));
#91510=CARTESIAN_POINT('Ctrl Pts',(0.00816184480424535,-0.0321934096636184,
0.0799821283124011));
#91511=CARTESIAN_POINT('Ctrl Pts',(0.00808141520953306,-0.0320835708272304,
0.0799826532254729));
#91512=CARTESIAN_POINT('Ctrl Pts',(0.0080010214042056,-0.0319739230346346,
0.0799815133477915));
#91513=CARTESIAN_POINT('Ctrl Pts',(0.00792076613463159,-0.0318646057455575,
0.0799787180318383));
#91514=CARTESIAN_POINT('Ctrl Pts',(0.00823858339858482,-0.0321934096636184,
0.0798987475418123));
#91515=CARTESIAN_POINT('Ctrl Pts',(0.00815930368968197,-0.0320835708272304,
0.0799003307399064));
#91516=CARTESIAN_POINT('Ctrl Pts',(0.00808003720202992,-0.0319739230346346,
0.0799002723302261));
#91517=CARTESIAN_POINT('Ctrl Pts',(0.00800088534586482,-0.0318646057455575,
0.0798985801708951));
#91518=CARTESIAN_POINT('Origin',(0.00729306470512945,-0.0326371942645793,
0.0632171198538876));
#91519=CARTESIAN_POINT('Ctrl Pts',(0.00836258658954841,-0.0320218834582342,
0.0798957610688848));
#91520=CARTESIAN_POINT('Ctrl Pts',(0.0083027871071084,-0.0319391099350621,
0.0798982464453459));
#91521=CARTESIAN_POINT('Ctrl Pts',(0.00824298504615354,-0.0318564869454885,
0.0798997965386773));
#91522=CARTESIAN_POINT('Ctrl Pts',(0.00818322406995633,-0.0317740741446461,
0.0799004142862709));
#91523=CARTESIAN_POINT('Ctrl Pts',(0.00839832609641107,-0.0320218834582342,
0.0799301051469319));
#91524=CARTESIAN_POINT('Ctrl Pts',(0.00833816917514486,-0.0319391099350621,
0.0799329624852597));
#91525=CARTESIAN_POINT('Ctrl Pts',(0.0082780040836902,-0.0318564869454885,
0.0799348787336382));
#91526=CARTESIAN_POINT('Ctrl Pts',(0.00821787477463702,-0.0317740741446461,
0.0799358565874493));
#91527=CARTESIAN_POINT('Ctrl Pts',(0.00843406560327374,-0.0320218834582342,
0.0799644492249789));
#91528=CARTESIAN_POINT('Ctrl Pts',(0.00837355124318133,-0.0319391099350621,
0.0799676785251735));
#91529=CARTESIAN_POINT('Ctrl Pts',(0.00831302312122687,-0.0318564869454885,
0.0799699609285991));
#91530=CARTESIAN_POINT('Ctrl Pts',(0.00825252547931771,-0.0317740741446461,
0.0799712988886277));
#91531=CARTESIAN_POINT('Ctrl Pts',(0.00846980511013641,-0.0320218834582342,
0.079998793303026));
#91532=CARTESIAN_POINT('Ctrl Pts',(0.00840893331121779,-0.0319391099350621,
0.0800023945650873));
#91533=CARTESIAN_POINT('Ctrl Pts',(0.00834804215876353,-0.0318564869454885,
0.08000504312356));
#91534=CARTESIAN_POINT('Ctrl Pts',(0.00828717618399839,-0.0317740741446461,
0.0800067411898061));
#91535=CARTESIAN_POINT('Origin',(0.00682280132131256,-0.0326352985526838,
0.0633090424749645));
#91536=CARTESIAN_POINT('Ctrl Pts',(0.008267748577978,-0.0322357172926636,
0.0798995563898468));
#91537=CARTESIAN_POINT('Ctrl Pts',(0.00808466288433491,-0.0319820232604284,
0.07990414077578));
#91538=CARTESIAN_POINT('Ctrl Pts',(0.00790165644468594,-0.0317296613809579,
0.0798970675263033));
#91539=CARTESIAN_POINT('Ctrl Pts',(0.00851747519824071,-0.0322357172926636,
0.079887868142238));
#91540=CARTESIAN_POINT('Ctrl Pts',(0.00833476169868981,-0.0319820232604284,
0.079900404684545));
#91541=CARTESIAN_POINT('Ctrl Pts',(0.0081516207639664,-0.0317296613809579,
0.0799012911605981));
#91542=CARTESIAN_POINT('Ctrl Pts',(0.0101257369179384,-0.0345231616327822,
0.079540125976521));
#91543=CARTESIAN_POINT('Ctrl Pts',(0.0100514416200429,-0.0344132092796975,
0.0795677201038758));
#91544=CARTESIAN_POINT('Ctrl Pts',(0.00997657939268488,-0.0343032738558974,
0.0795937760678668));
#91545=CARTESIAN_POINT('Ctrl Pts',(0.00990124699808852,-0.034193496108874,
0.0796182629444909));
#91546=CARTESIAN_POINT('Ctrl Pts',(0.0102277118106814,-0.0345231616327822,
0.0795895451771336));
#91547=CARTESIAN_POINT('Ctrl Pts',(0.0101527353386821,-0.0344132092796975,
0.0796185448848157));
#91548=CARTESIAN_POINT('Ctrl Pts',(0.0100771628990454,-0.0343032738558974,
0.0796459922670635));
#91549=CARTESIAN_POINT('Ctrl Pts',(0.0100010922095206,-0.034193496108874,
0.0796718546406128));
#91550=CARTESIAN_POINT('Ctrl Pts',(0.0103296867034243,-0.0345231616327822,
0.0796389643777463));
#91551=CARTESIAN_POINT('Ctrl Pts',(0.0102540290573213,-0.0344132092796975,
0.0796693696657557));
#91552=CARTESIAN_POINT('Ctrl Pts',(0.0101777464054059,-0.0343032738558974,
0.0796982084662603));
#91553=CARTESIAN_POINT('Ctrl Pts',(0.0101009374209526,-0.034193496108874,
0.0797254463367347));
#91554=CARTESIAN_POINT('Ctrl Pts',(0.0104316615961673,-0.0345231616327822,
0.079688383578359));
#91555=CARTESIAN_POINT('Ctrl Pts',(0.0103553227759604,-0.0344132092796975,
0.0797201944466957));
#91556=CARTESIAN_POINT('Ctrl Pts',(0.0102783299117663,-0.0343032738558974,
0.079750424665457));
#91557=CARTESIAN_POINT('Ctrl Pts',(0.0102007826323846,-0.034193496108874,
0.0797790380328567));
#91558=CARTESIAN_POINT('Origin',(0.00422215359472562,-0.0345625596230656,
0.0638101446865464));
#91559=CARTESIAN_POINT('Ctrl Pts',(0.00986777531919962,-0.0346945769586886,
0.0798909483516449));
#91560=CARTESIAN_POINT('Ctrl Pts',(0.00978866214920874,-0.034584662917669,
0.0799149814584064));
#91561=CARTESIAN_POINT('Ctrl Pts',(0.00970903847171624,-0.0344746925051586,
0.0799373826422171));
#91562=CARTESIAN_POINT('Ctrl Pts',(0.00962900642829233,-0.0343648066255171,
0.0799581236214394));
#91563=CARTESIAN_POINT('Ctrl Pts',(0.00991499190489023,-0.0346945769586886,
0.0797879351698764));
#91564=CARTESIAN_POINT('Ctrl Pts',(0.00983729830861111,-0.034584662917669,
0.0798126189450539));
#91565=CARTESIAN_POINT('Ctrl Pts',(0.00975908099174143,-0.0344746925051586,
0.0798357002646177));
#91566=CARTESIAN_POINT('Ctrl Pts',(0.00968044029745914,-0.0343648066255171,
0.0798571499680199));
#91567=CARTESIAN_POINT('Ctrl Pts',(0.00996220849058084,-0.0346945769586886,
0.0796849219881079));
#91568=CARTESIAN_POINT('Ctrl Pts',(0.00988593446801348,-0.034584662917669,
0.0797102564317014));
#91569=CARTESIAN_POINT('Ctrl Pts',(0.00980912351176662,-0.0344746925051586,
0.0797340178870183));
#91570=CARTESIAN_POINT('Ctrl Pts',(0.00973187416662595,-0.0343648066255171,
0.0797561763146005));
#91571=CARTESIAN_POINT('Ctrl Pts',(0.0100094250762715,-0.0346945769586886,
0.0795819088063395));
#91572=CARTESIAN_POINT('Ctrl Pts',(0.00993457062741585,-0.034584662917669,
0.0796078939183489));
#91573=CARTESIAN_POINT('Ctrl Pts',(0.00985916603179181,-0.0344746925051586,
0.0796323355094189));
#91574=CARTESIAN_POINT('Ctrl Pts',(0.00978330803579277,-0.0343648066255171,
0.079655202661181));
#91575=CARTESIAN_POINT('Origin',(0.00467172536872588,-0.034562644672989,
0.0636396237114132));
#91576=CARTESIAN_POINT('Ctrl Pts',(0.0100085802132244,-0.0346945769586885,
0.0795837520575904));
#91577=CARTESIAN_POINT('Ctrl Pts',(0.00989476810082433,-0.0345275153362891,
0.079623229906753));
#91578=CARTESIAN_POINT('Ctrl Pts',(0.00977968500876321,-0.0343603235965159,
0.0796591386807315));
#91579=CARTESIAN_POINT('Ctrl Pts',(0.00966367288018324,-0.0341934961088739,
0.0796913772360182));
#91580=CARTESIAN_POINT('Ctrl Pts',(0.0100871682192819,-0.0346945769586885,
0.079554563812779));
#91581=CARTESIAN_POINT('Ctrl Pts',(0.00997396746635576,-0.0345275153362891,
0.0795956877191934));
#91582=CARTESIAN_POINT('Ctrl Pts',(0.00985944412491194,-0.0343603235965159,
0.0796332622028711));
#91583=CARTESIAN_POINT('Ctrl Pts',(0.0097439385558184,-0.0341934961088739,
0.0796671811692697));
#91584=CARTESIAN_POINT('Ctrl Pts',(0.0101657562253394,-0.0346945769586885,
0.0795253755679676));
#91585=CARTESIAN_POINT('Ctrl Pts',(0.0100531668318872,-0.0345275153362891,
0.0795681455316338));
#91586=CARTESIAN_POINT('Ctrl Pts',(0.00993920324106068,-0.0343603235965159,
0.0796073857250107));
#91587=CARTESIAN_POINT('Ctrl Pts',(0.00982420423145356,-0.0341934961088739,
0.0796429851025211));
#91588=CARTESIAN_POINT('Ctrl Pts',(0.010244344231397,-0.0346945769586885,
0.0794961873231562));
#91589=CARTESIAN_POINT('Ctrl Pts',(0.0101323661974186,-0.0345275153362891,
0.0795406033440742));
#91590=CARTESIAN_POINT('Ctrl Pts',(0.0100189623572094,-0.0343603235965159,
0.0795815092471503));
#91591=CARTESIAN_POINT('Ctrl Pts',(0.00990446990708872,-0.0341934961088739,
0.0796187890357726));
#91592=CARTESIAN_POINT('Ctrl Pts',(0.0096984989248846,-0.03424362768739,
0.0796815813484631));
#91593=CARTESIAN_POINT('Ctrl Pts',(0.0094898718950713,-0.033943005420186,
0.0797409727690808));
#91594=CARTESIAN_POINT('Ctrl Pts',(0.00927736394762871,-0.0336441434784162,
0.0797844808221911));
#91595=CARTESIAN_POINT('Ctrl Pts',(0.00993740116890683,-0.03424362768739,
0.0796079218765593));
#91596=CARTESIAN_POINT('Ctrl Pts',(0.00973155225187409,-0.033943005420186,
0.0796763236438477));
#91597=CARTESIAN_POINT('Ctrl Pts',(0.00952113582865493,-0.0336441434784162,
0.0797290257050157));
#91598=CARTESIAN_POINT('Origin',(0.0046941281949332,-0.0345610621863657,
0.0637114892728983));
#91599=CARTESIAN_POINT('Origin',(0.00426216054678368,-0.0345589643415055,
0.0639235127682916));
#91600=CARTESIAN_POINT('Ctrl Pts',(0.00950385681755227,-0.034193496108874,
0.0799891261359099));
#91601=CARTESIAN_POINT('Ctrl Pts',(0.00942333872695702,-0.0340836138595105,
0.0800081565474908));
#91602=CARTESIAN_POINT('Ctrl Pts',(0.00934246547602342,-0.0339738896671456,
0.0800255116750088));
#91603=CARTESIAN_POINT('Ctrl Pts',(0.00926134206153027,-0.0338644633335883,
0.0800411762446778));
#91604=CARTESIAN_POINT('Ctrl Pts',(0.00955744856189494,-0.034193496108874,
0.0798892808346391));
#91605=CARTESIAN_POINT('Ctrl Pts',(0.00947830727886063,-0.0340836138595105,
0.0799090502446293));
#91606=CARTESIAN_POINT('Ctrl Pts',(0.00939879488284858,-0.0339738896671456,
0.0799271725061145));
#91607=CARTESIAN_POINT('Ctrl Pts',(0.0093190146947287,-0.0338644633335883,
0.0799436312467152));
#91608=CARTESIAN_POINT('Ctrl Pts',(0.00961104030623761,-0.034193496108874,
0.0797894355333683));
#91609=CARTESIAN_POINT('Ctrl Pts',(0.00953327583076425,-0.0340836138595105,
0.0798099439417678));
#91610=CARTESIAN_POINT('Ctrl Pts',(0.00945512428967374,-0.0339738896671456,
0.0798288333372201));
#91611=CARTESIAN_POINT('Ctrl Pts',(0.00937668732792713,-0.0338644633335883,
0.0798460862487527));
#91612=CARTESIAN_POINT('Ctrl Pts',(0.00966463205058028,-0.034193496108874,
0.0796895902320975));
#91613=CARTESIAN_POINT('Ctrl Pts',(0.00958824438266786,-0.0340836138595105,
0.0797108376389063));
#91614=CARTESIAN_POINT('Ctrl Pts',(0.0095114536964989,-0.0339738896671456,
0.0797304941683257));
#91615=CARTESIAN_POINT('Ctrl Pts',(0.00943435996112556,-0.0338644633335883,
0.0797485412507902));
#91616=CARTESIAN_POINT('Ctrl Pts',(0.00978333808643704,-0.0340223579322365,
0.0796551930208755));
#91617=CARTESIAN_POINT('Ctrl Pts',(0.00970740711653357,-0.0339125849573551,
0.0796780826249479));
#91618=CARTESIAN_POINT('Ctrl Pts',(0.00963105574082732,-0.0338030433565216,
0.0796993845501226));
#91619=CARTESIAN_POINT('Ctrl Pts',(0.00955438401470863,-0.033693872113232,
0.0797190802102514));
#91620=CARTESIAN_POINT('Ctrl Pts',(0.00988200887454069,-0.0340223579322365,
0.079710917839457));
#91621=CARTESIAN_POINT('Ctrl Pts',(0.00980530931405256,-0.0339125849573551,
0.0797351683710415));
#91622=CARTESIAN_POINT('Ctrl Pts',(0.00972816171980421,-0.0338030433565216,
0.0797578143593813));
#91623=CARTESIAN_POINT('Ctrl Pts',(0.00965066731778236,-0.033693872113232,
0.0797788355897594));
#91624=CARTESIAN_POINT('Ctrl Pts',(0.00998067966264434,-0.0340223579322365,
0.0797666426580385));
#91625=CARTESIAN_POINT('Ctrl Pts',(0.00990321151157155,-0.0339125849573551,
0.0797922541171351));
#91626=CARTESIAN_POINT('Ctrl Pts',(0.0098252676987811,-0.0338030433565216,
0.0798162441686399));
#91627=CARTESIAN_POINT('Ctrl Pts',(0.00974695062085609,-0.033693872113232,
0.0798385909692674));
#91628=CARTESIAN_POINT('Ctrl Pts',(0.010079350450748,-0.0340223579322365,
0.07982236747662));
#91629=CARTESIAN_POINT('Ctrl Pts',(0.0100011137090905,-0.0339125849573551,
0.0798493398632287));
#91630=CARTESIAN_POINT('Ctrl Pts',(0.00992237367775799,-0.0338030433565216,
0.0798746739778985));
#91631=CARTESIAN_POINT('Ctrl Pts',(0.00984323392392981,-0.033693872113232,
0.0798983463487754));
#91632=CARTESIAN_POINT('Origin',(0.00956485650479092,-0.0391228853390991,
0.0861418273486221));
#91633=CARTESIAN_POINT('Ctrl Pts',(0.011254964474949,-0.0352722978779635,
0.0789749209382626));
#91634=CARTESIAN_POINT('Ctrl Pts',(0.0112389250848038,-0.0352466642097244,
0.0789849124667666));
#91635=CARTESIAN_POINT('Ctrl Pts',(0.0112229414375835,-0.0352210183808315,
0.0789949616395067));
#91636=CARTESIAN_POINT('Ctrl Pts',(0.0112070132526816,-0.0351953608940152,
0.0790050692619298));
#91637=CARTESIAN_POINT('Origin',(0.0136902418348352,-0.0352456003065078,
0.0832268813538167));
#91638=CARTESIAN_POINT('Ctrl Pts',(0.0111002848269308,-0.035024121149334,
0.0790695235756326));
#91639=CARTESIAN_POINT('Ctrl Pts',(0.0110325204098152,-0.0349144232867421,
0.0791105236771512));
#91640=CARTESIAN_POINT('Ctrl Pts',(0.0109638679310742,-0.0348045283677512,
0.0791501475803453));
#91641=CARTESIAN_POINT('Ctrl Pts',(0.0108944134371579,-0.0346945769586886,
0.0791883412597654));
#91642=CARTESIAN_POINT('Ctrl Pts',(0.0112097137181652,-0.035024121149334,
0.0790989592608941));
#91643=CARTESIAN_POINT('Ctrl Pts',(0.0111415438365725,-0.0349144232867421,
0.0791414667004539));
#91644=CARTESIAN_POINT('Ctrl Pts',(0.0110724544929114,-0.0348045283677512,
0.0791825904626635));
#91645=CARTESIAN_POINT('Ctrl Pts',(0.0110025322217108,-0.0346945769586886,
0.079222274580122));
#91646=CARTESIAN_POINT('Ctrl Pts',(0.0113191426093997,-0.035024121149334,
0.0791283949461555));
#91647=CARTESIAN_POINT('Ctrl Pts',(0.0112505672633299,-0.0349144232867421,
0.0791724097237565));
#91648=CARTESIAN_POINT('Ctrl Pts',(0.0111810410547486,-0.0348045283677512,
0.0792150333449817));
#91649=CARTESIAN_POINT('Ctrl Pts',(0.0111106510062636,-0.0346945769586886,
0.0792562079004785));
#91650=CARTESIAN_POINT('Ctrl Pts',(0.0114285715006341,-0.035024121149334,
0.079157830631417));
#91651=CARTESIAN_POINT('Ctrl Pts',(0.0113595906900872,-0.0349144232867421,
0.0792033527470592));
#91652=CARTESIAN_POINT('Ctrl Pts',(0.0112896276165859,-0.0348045283677512,
0.0792474762272999));
#91653=CARTESIAN_POINT('Ctrl Pts',(0.0112187697908165,-0.0346945769586886,
0.0792901412208351));
#91654=CARTESIAN_POINT('Origin',(0.00296287029434561,-0.0345629067943208,
0.0643912613970295));
#91655=CARTESIAN_POINT('Ctrl Pts',(0.0109360748324534,-0.0351970973651599,
0.0793717364820537));
#91656=CARTESIAN_POINT('Ctrl Pts',(0.0108637347502008,-0.0350869349321765,
0.0794106969852403));
#91657=CARTESIAN_POINT('Ctrl Pts',(0.0107905247749954,-0.0349764985129724,
0.079448185852633));
#91658=CARTESIAN_POINT('Ctrl Pts',(0.0107165368935177,-0.0348659306849652,
0.0794841489331317));
#91659=CARTESIAN_POINT('Ctrl Pts',(0.0109557021224374,-0.0351970973651599,
0.0792918913811521));
#91660=CARTESIAN_POINT('Ctrl Pts',(0.0108844681858485,-0.0350869349321765,
0.0793311237938417));
#91661=CARTESIAN_POINT('Ctrl Pts',(0.0108123596197771,-0.0349764985129724,
0.0793689077921395));
#91662=CARTESIAN_POINT('Ctrl Pts',(0.0107394669614885,-0.0348659306849652,
0.0794051889265907));
#91663=CARTESIAN_POINT('Ctrl Pts',(0.0109753294124215,-0.03519709736516,
0.0792120462802505));
#91664=CARTESIAN_POINT('Ctrl Pts',(0.0109052016214963,-0.0350869349321765,
0.0792515506024431));
#91665=CARTESIAN_POINT('Ctrl Pts',(0.0108341944645589,-0.0349764985129724,
0.0792896297316459));
#91666=CARTESIAN_POINT('Ctrl Pts',(0.0107623970294593,-0.0348659306849652,
0.0793262289200496));
#91667=CARTESIAN_POINT('Ctrl Pts',(0.0109949567024055,-0.03519709736516,
0.0791322011793488));
#91668=CARTESIAN_POINT('Ctrl Pts',(0.010925935057144,-0.0350869349321765,
0.0791719774110446));
#91669=CARTESIAN_POINT('Ctrl Pts',(0.0108560293093406,-0.0349764985129724,
0.0792103516711524));
#91670=CARTESIAN_POINT('Ctrl Pts',(0.0107853270974301,-0.0348659306849652,
0.0792472689135086));
#91671=CARTESIAN_POINT('Origin',(0.0034073905888549,-0.0345637187967157,
0.0642076121005219));
#91672=CARTESIAN_POINT('Ctrl Pts',(0.0110246068595911,-0.0352450361861253,
0.0791162200167056));
#91673=CARTESIAN_POINT('Ctrl Pts',(0.0108373028029637,-0.0349452761023765,
0.0792256264114625));
#91674=CARTESIAN_POINT('Ctrl Pts',(0.0106422899203209,-0.0346444289983475,
0.0793206134866157));
#91675=CARTESIAN_POINT('Ctrl Pts',(0.0112376869692765,-0.0352450361861253,
0.0789854650288218));
#91676=CARTESIAN_POINT('Ctrl Pts',(0.0110553144178124,-0.0349452761023765,
0.0791029078715807));
#91677=CARTESIAN_POINT('Ctrl Pts',(0.0108646136923163,-0.0346444289983475,
0.0792062800251718));
#91678=CARTESIAN_POINT('Ctrl Pts',(0.0107855128249345,-0.0345231616327822,
0.0792467117641312));
#91679=CARTESIAN_POINT('Ctrl Pts',(0.0107152618288626,-0.0344132092796975,
0.0792833999734737));
#91680=CARTESIAN_POINT('Ctrl Pts',(0.0106442555907482,-0.0343032738558974,
0.0793186332034327));
#91681=CARTESIAN_POINT('Ctrl Pts',(0.0105725862340111,-0.0341934961088741,
0.0793523686463277));
#91682=CARTESIAN_POINT('Ctrl Pts',(0.0108928774834027,-0.0345231616327822,
0.0792829604365364));
#91683=CARTESIAN_POINT('Ctrl Pts',(0.0108221268504157,-0.0344132092796975,
0.0793211285165385));
#91684=CARTESIAN_POINT('Ctrl Pts',(0.0107505903912079,-0.0343032738558974,
0.0793578312062072));
#91685=CARTESIAN_POINT('Ctrl Pts',(0.0106783609566958,-0.0341934961088741,
0.0793930238327139));
#91686=CARTESIAN_POINT('Ctrl Pts',(0.0110002421418708,-0.0345231616327822,
0.0793192091089416));
#91687=CARTESIAN_POINT('Ctrl Pts',(0.0109289918719688,-0.0344132092796975,
0.0793588570596033));
#91688=CARTESIAN_POINT('Ctrl Pts',(0.0108569251916676,-0.0343032738558974,
0.0793970292089817));
#91689=CARTESIAN_POINT('Ctrl Pts',(0.0107841356793805,-0.0341934961088741,
0.0794336790191002));
#91690=CARTESIAN_POINT('Ctrl Pts',(0.011107606800339,-0.0345231616327822,
0.0793554577813468));
#91691=CARTESIAN_POINT('Ctrl Pts',(0.0110358568935219,-0.0344132092796975,
0.0793965856026682));
#91692=CARTESIAN_POINT('Ctrl Pts',(0.0109632599921274,-0.0343032738558974,
0.0794362272117561));
#91693=CARTESIAN_POINT('Ctrl Pts',(0.0108899104020652,-0.0341934961088741,
0.0794743342054864));
#91694=CARTESIAN_POINT('Origin',(0.00295699160068082,-0.0345625596230115,
0.0643806812625355));
#91695=CARTESIAN_POINT('Ctrl Pts',(0.0105735550331317,-0.0346945769586885,
0.0796270989613485));
#91696=CARTESIAN_POINT('Ctrl Pts',(0.0104980778410992,-0.034584662917669,
0.0796608580692974));
#91697=CARTESIAN_POINT('Ctrl Pts',(0.0104218896328888,-0.0344746925051586,
0.0796930621060512));
#91698=CARTESIAN_POINT('Ctrl Pts',(0.0103450882000249,-0.0343648066255171,
0.0797236702112484));
#91699=CARTESIAN_POINT('Ctrl Pts',(0.0106074883267706,-0.0346945769586885,
0.0795189802619239));
#91700=CARTESIAN_POINT('Ctrl Pts',(0.0105335010650637,-0.034584662917669,
0.0795532069878103));
#91701=CARTESIAN_POINT('Ctrl Pts',(0.0104587933715158,-0.0344746925051586,
0.0795859095335193));
#91702=CARTESIAN_POINT('Ctrl Pts',(0.0103834611432831,-0.0343648066255171,
0.0796170463921076));
#91703=CARTESIAN_POINT('Ctrl Pts',(0.0106414216204095,-0.0346945769586886,
0.0794108615624993));
#91704=CARTESIAN_POINT('Ctrl Pts',(0.0105689242890282,-0.034584662917669,
0.0794455559063233));
#91705=CARTESIAN_POINT('Ctrl Pts',(0.0104956971101427,-0.0344746925051586,
0.0794787569609873));
#91706=CARTESIAN_POINT('Ctrl Pts',(0.0104218340865413,-0.0343648066255171,
0.0795104225729668));
#91707=CARTESIAN_POINT('Ctrl Pts',(0.0106753549140484,-0.0346945769586886,
0.0793027428630747));
#91708=CARTESIAN_POINT('Ctrl Pts',(0.0106043475129927,-0.034584662917669,
0.0793379048248363));
#91709=CARTESIAN_POINT('Ctrl Pts',(0.0105326008487697,-0.0344746925051586,
0.0793716043884554));
#91710=CARTESIAN_POINT('Ctrl Pts',(0.0104602070297995,-0.0343648066255171,
0.0794037987538261));
#91711=CARTESIAN_POINT('Origin',(0.00338164642133868,-0.0345626446732309,
0.0641551586121303));
#91712=CARTESIAN_POINT('Ctrl Pts',(0.0106747477336384,-0.0346945769586886,
0.0793046774691565));
#91713=CARTESIAN_POINT('Ctrl Pts',(0.0105667809502284,-0.0345275153362891,
0.0793581084637529));
#91714=CARTESIAN_POINT('Ctrl Pts',(0.0104571058854778,-0.0343603235965159,
0.0794081578223798));
#91715=CARTESIAN_POINT('Ctrl Pts',(0.0103460491095624,-0.034193496108874,
0.0794546823422365));
#91716=CARTESIAN_POINT('Ctrl Pts',(0.0107490577926908,-0.0346945769586886,
0.0792658696934549));
#91717=CARTESIAN_POINT('Ctrl Pts',(0.0106419038536806,-0.0345275153362891,
0.0793208571419903));
#91718=CARTESIAN_POINT('Ctrl Pts',(0.0105329928945294,-0.0343603235965159,
0.079372488920343));
#91719=CARTESIAN_POINT('Ctrl Pts',(0.0104226492950858,-0.034193496108874,
0.0794206171120296));
#91720=CARTESIAN_POINT('Ctrl Pts',(0.0108233678517432,-0.0346945769586886,
0.0792270619177534));
#91721=CARTESIAN_POINT('Ctrl Pts',(0.0107170267571329,-0.0345275153362891,
0.0792836058202278));
#91722=CARTESIAN_POINT('Ctrl Pts',(0.0106088799035809,-0.0343603235965159,
0.0793368200183063));
#91723=CARTESIAN_POINT('Ctrl Pts',(0.0104992494806093,-0.034193496108874,
0.0793865518818228));
#91724=CARTESIAN_POINT('Ctrl Pts',(0.0108976779107956,-0.0346945769586886,
0.0791882541420519));
#91725=CARTESIAN_POINT('Ctrl Pts',(0.0107921496605851,-0.0345275153362891,
0.0792463544984652));
#91726=CARTESIAN_POINT('Ctrl Pts',(0.0106847669126324,-0.0343603235965159,
0.0793011511162696));
#91727=CARTESIAN_POINT('Ctrl Pts',(0.0105758496661327,-0.034193496108874,
0.0793524866516159));
#91728=CARTESIAN_POINT('Ctrl Pts',(0.00950385681755174,-0.0331951640388587,
0.0799891261359108));
#91729=CARTESIAN_POINT('Ctrl Pts',(0.00942343466748559,-0.0330855618255041,
0.0800081338719943));
#91730=CARTESIAN_POINT('Ctrl Pts',(0.00934256168480182,-0.0329757224427708,
0.080025493122117));
#91731=CARTESIAN_POINT('Ctrl Pts',(0.00926134034180358,-0.0328657862078597,
0.0800411765767499));
#91732=CARTESIAN_POINT('Ctrl Pts',(0.00955744854685499,-0.0331951640388587,
0.0798892808626596));
#91733=CARTESIAN_POINT('Ctrl Pts',(0.00947840156344252,-0.0330855618255041,
0.079909026716399));
#91734=CARTESIAN_POINT('Ctrl Pts',(0.00939888948312063,-0.0329757224427708,
0.0799271530386205));
#91735=CARTESIAN_POINT('Ctrl Pts',(0.00931901298729227,-0.0328657862078597,
0.0799436316229969));
#91736=CARTESIAN_POINT('Ctrl Pts',(0.00961104027615824,-0.0331951640388587,
0.0797894355894083));
#91737=CARTESIAN_POINT('Ctrl Pts',(0.00953336845939947,-0.0330855618255041,
0.0798099195608037));
#91738=CARTESIAN_POINT('Ctrl Pts',(0.00945521728143943,-0.0329757224427708,
0.079828812955124));
#91739=CARTESIAN_POINT('Ctrl Pts',(0.00937668563278096,-0.0328657862078597,
0.079846086669244));
#91740=CARTESIAN_POINT('Ctrl Pts',(0.00966463200546148,-0.0331951640388587,
0.0796895903161571));
#91741=CARTESIAN_POINT('Ctrl Pts',(0.00958833535535641,-0.0330855618255041,
0.0797108124052084));
#91742=CARTESIAN_POINT('Ctrl Pts',(0.00951154507975823,-0.0329757224427708,
0.0797304728716274));
#91743=CARTESIAN_POINT('Ctrl Pts',(0.00943435827826964,-0.0328657862078597,
0.079748541715491));
#91744=CARTESIAN_POINT('Origin',(0.00591998992064455,-0.0326401908834881,
0.0633507259648979));
#91745=CARTESIAN_POINT('Ctrl Pts',(0.00978333696304077,-0.0330240426238155,
0.079655193797274));
#91746=CARTESIAN_POINT('Ctrl Pts',(0.00970749755503332,-0.0329142774063509,
0.0796780557810556));
#91747=CARTESIAN_POINT('Ctrl Pts',(0.00963114771724851,-0.0328043479726687,
0.0796993613499594));
#91748=CARTESIAN_POINT('Ctrl Pts',(0.00955438450784236,-0.0326943950436595,
0.0797190805162996));
#91749=CARTESIAN_POINT('Ctrl Pts',(0.00988200756620427,-0.0330240426238155,
0.079710918549913));
#91750=CARTESIAN_POINT('Ctrl Pts',(0.00980540049543922,-0.0329142774063509,
0.0797351398173833));
#91751=CARTESIAN_POINT('Ctrl Pts',(0.00972825451199812,-0.0328043479726687,
0.0797577894778947));
#91752=CARTESIAN_POINT('Ctrl Pts',(0.00965066764653855,-0.0326943950436595,
0.0797788357937915));
#91753=CARTESIAN_POINT('Ctrl Pts',(0.00998067816936777,-0.0330240426238155,
0.0797666433025521));
#91754=CARTESIAN_POINT('Ctrl Pts',(0.00990330343584513,-0.0329142774063509,
0.079792223853711));
#91755=CARTESIAN_POINT('Ctrl Pts',(0.00982536130674774,-0.0328043479726687,
0.07981621760583));
#91756=CARTESIAN_POINT('Ctrl Pts',(0.00974695078523475,-0.0326943950436595,
0.0798385910712835));
#91757=CARTESIAN_POINT('Ctrl Pts',(0.0100793487725313,-0.0330240426238155,
0.0798223680551911));
#91758=CARTESIAN_POINT('Ctrl Pts',(0.010001206376251,-0.0329142774063509,
0.0798493078900387));
#91759=CARTESIAN_POINT('Ctrl Pts',(0.00992246810149735,-0.0328043479726687,
0.0798746457337654));
#91760=CARTESIAN_POINT('Ctrl Pts',(0.00984323392393094,-0.0326943950436595,
0.0798983463487755));
#91761=CARTESIAN_POINT('Origin',(0.00544557864969214,-0.0326396682856814,
0.0634295093221238));
#91762=CARTESIAN_POINT('Ctrl Pts',(0.00969842922484738,-0.0332451089994432,
0.0796816011900205));
#91763=CARTESIAN_POINT('Ctrl Pts',(0.00948980147263735,-0.0329451141710259,
0.0797409899744738));
#91764=CARTESIAN_POINT('Ctrl Pts',(0.0092772930038244,-0.0326442513127504,
0.0797844953464851));
#91765=CARTESIAN_POINT('Ctrl Pts',(0.00993733239698644,-0.0332451089994432,
0.0796079447283767));
#91766=CARTESIAN_POINT('Ctrl Pts',(0.00973148264367773,-0.0329451141710259,
0.0796763438933848));
#91767=CARTESIAN_POINT('Ctrl Pts',(0.00952106558306633,-0.0326442513127504,
0.0797290432986444));
#91768=CARTESIAN_POINT('Ctrl Pts',(0.00943438905477848,-0.0325229783203386,
0.079748534603042));
#91769=CARTESIAN_POINT('Ctrl Pts',(0.00935721337911216,-0.0324130253112081,
0.0797666012896402));
#91770=CARTESIAN_POINT('Ctrl Pts',(0.00927967567603521,-0.0323031222247696,
0.0797830687581102));
#91771=CARTESIAN_POINT('Ctrl Pts',(0.0092018760101549,-0.0321934096636185,
0.0797979194194819));
#91772=CARTESIAN_POINT('Ctrl Pts',(0.00952936600242293,-0.0325229783203386,
0.0798103449748761));
#91773=CARTESIAN_POINT('Ctrl Pts',(0.00945133827214809,-0.0324130253112081,
0.0798297209165968));
#91774=CARTESIAN_POINT('Ctrl Pts',(0.00937292156006982,-0.0323031222247696,
0.0798474798157712));
#91775=CARTESIAN_POINT('Ctrl Pts',(0.00929421711511575,-0.0321934096636185,
0.0798636024689296));
#91776=CARTESIAN_POINT('Ctrl Pts',(0.00962434295006738,-0.0325229783203386,
0.0798721553467102));
#91777=CARTESIAN_POINT('Ctrl Pts',(0.00954546316518402,-0.0324130253112081,
0.0798928405435533));
#91778=CARTESIAN_POINT('Ctrl Pts',(0.00946616744410443,-0.0323031222247696,
0.0799118908734322));
#91779=CARTESIAN_POINT('Ctrl Pts',(0.0093865582200766,-0.0321934096636185,
0.0799292855183772));
#91780=CARTESIAN_POINT('Ctrl Pts',(0.00971931989771183,-0.0325229783203386,
0.0799339657185444));
#91781=CARTESIAN_POINT('Ctrl Pts',(0.00963958805821995,-0.0324130253112081,
0.0799559601705099));
#91782=CARTESIAN_POINT('Ctrl Pts',(0.00955941332813904,-0.0323031222247696,
0.0799763019310933));
#91783=CARTESIAN_POINT('Ctrl Pts',(0.00947889932503745,-0.0321934096636185,
0.0799949685678249));
#91784=CARTESIAN_POINT('Origin',(0.00544741297196231,-0.0326393375178632,
0.0634378355632368));
#91785=CARTESIAN_POINT('Ctrl Pts',(0.00913449179185795,-0.0326943950436594,
0.0800642595569604));
#91786=CARTESIAN_POINT('Ctrl Pts',(0.00905298221065953,-0.0325844576448127,
0.0800781890295027));
#91787=CARTESIAN_POINT('Ctrl Pts',(0.00897117877657155,-0.0324744968375319,
0.0800904337360795));
#91788=CARTESIAN_POINT('Ctrl Pts',(0.00888918651731774,-0.0323646534831895,
0.080100979433722));
#91789=CARTESIAN_POINT('Ctrl Pts',(0.00919424704979836,-0.0326943950436594,
0.0799679764497674));
#91790=CARTESIAN_POINT('Ctrl Pts',(0.00911406443027083,-0.0325844576448127,
0.0799827294617575));
#91791=CARTESIAN_POINT('Ctrl Pts',(0.00903357101961889,-0.0324744968375319,
0.0799958252098081));
#91792=CARTESIAN_POINT('Ctrl Pts',(0.00895287018212779,-0.0323646534831895,
0.0800072483373953));
#91793=CARTESIAN_POINT('Ctrl Pts',(0.00925400230773878,-0.0326943950436594,
0.0798716933425744));
#91794=CARTESIAN_POINT('Ctrl Pts',(0.00917514664988214,-0.0325844576448127,
0.0798872698940122));
#91795=CARTESIAN_POINT('Ctrl Pts',(0.00909596326266623,-0.0324744968375319,
0.0799012166835366));
#91796=CARTESIAN_POINT('Ctrl Pts',(0.00901655384693785,-0.0323646534831895,
0.0799135172410685));
#91797=CARTESIAN_POINT('Ctrl Pts',(0.00931375756567919,-0.0326943950436594,
0.0797754102353815));
#91798=CARTESIAN_POINT('Ctrl Pts',(0.00923622886949344,-0.0325844576448127,
0.0797918103262669));
#91799=CARTESIAN_POINT('Ctrl Pts',(0.00915835550571357,-0.0324744968375319,
0.0798066081572652));
#91800=CARTESIAN_POINT('Ctrl Pts',(0.0090802375117479,-0.0323646534831895,
0.0798197861447417));
#91801=CARTESIAN_POINT('Origin',(0.00591197553634447,-0.0326395579067306,
0.0633137431114539));
#91802=CARTESIAN_POINT('Ctrl Pts',(0.00934802823052416,-0.0327445246961878,
0.0797695503948157));
#91803=CARTESIAN_POINT('Ctrl Pts',(0.00913608342476325,-0.0324436878365476,
0.0798157235884653));
#91804=CARTESIAN_POINT('Ctrl Pts',(0.00892126277817681,-0.0321434074463187,
0.0798458010601179));
#91805=CARTESIAN_POINT('Ctrl Pts',(0.00959108451028239,-0.0327445246961878,
0.0797110384740637));
#91806=CARTESIAN_POINT('Ctrl Pts',(0.00938134651766616,-0.0324436878365476,
0.0797663786850693));
#91807=CARTESIAN_POINT('Ctrl Pts',(0.00916803591769531,-0.0321434074463187,
0.0798057633577341));
#91808=CARTESIAN_POINT('Ctrl Pts',(0.00876113795712711,-0.0321934096636184,
0.080116052097507));
#91809=CARTESIAN_POINT('Ctrl Pts',(0.00867886144904434,-0.0320835708272304,
0.0801248417302177));
#91810=CARTESIAN_POINT('Ctrl Pts',(0.00859645076368787,-0.0319739230346347,
0.0801319235565257));
#91811=CARTESIAN_POINT('Ctrl Pts',(0.00851401203519589,-0.0318646057455576,
0.0801372966078556));
#91812=CARTESIAN_POINT('Ctrl Pts',(0.00882682106313487,-0.0321934096636184,
0.0800237109130306));
#91813=CARTESIAN_POINT('Ctrl Pts',(0.00874581801195238,-0.0320835708272304,
0.0800334063669634));
#91814=CARTESIAN_POINT('Ctrl Pts',(0.0086646612989163,-0.0319739230346347,
0.0800414198432049));
#91815=CARTESIAN_POINT('Ctrl Pts',(0.00858345554527552,-0.0318646057455576,
0.080047749058067));
#91816=CARTESIAN_POINT('Ctrl Pts',(0.00889250416914263,-0.0321934096636184,
0.0799313697285542));
#91817=CARTESIAN_POINT('Ctrl Pts',(0.00881277457486041,-0.0320835708272304,
0.0799419710037092));
#91818=CARTESIAN_POINT('Ctrl Pts',(0.00873287183414474,-0.0319739230346347,
0.0799509161298841));
#91819=CARTESIAN_POINT('Ctrl Pts',(0.00865289905535515,-0.0318646057455576,
0.0799582015082784));
#91820=CARTESIAN_POINT('Ctrl Pts',(0.00895818727515039,-0.0321934096636184,
0.0798390285440778));
#91821=CARTESIAN_POINT('Ctrl Pts',(0.00887973113776844,-0.0320835708272304,
0.079850535640455));
#91822=CARTESIAN_POINT('Ctrl Pts',(0.00880108236937318,-0.0319739230346347,
0.0798604124165632));
#91823=CARTESIAN_POINT('Ctrl Pts',(0.00872234256543479,-0.0318646057455576,
0.0798686539584898));
#91824=CARTESIAN_POINT('Origin',(0.00592936193985411,-0.032637194264516,
0.0634074453883521));
#91825=CARTESIAN_POINT('Ctrl Pts',(0.00908083835960602,-0.0320218834582334,
0.0798205238994861));
#91826=CARTESIAN_POINT('Ctrl Pts',(0.00902182191421492,-0.0319391099350615,
0.079830484540511));
#91827=CARTESIAN_POINT('Ctrl Pts',(0.0089626856885824,-0.0318564869454882,
0.0798395175965668));
#91828=CARTESIAN_POINT('Ctrl Pts',(0.00890347336983581,-0.031774074144646,
0.0798476205094238));
#91829=CARTESIAN_POINT('Ctrl Pts',(0.0091206005041376,-0.0320218834582334,
0.0798501178162585));
#91830=CARTESIAN_POINT('Ctrl Pts',(0.00906127605761572,-0.0319391099350615,
0.0798604922850837));
#91831=CARTESIAN_POINT('Ctrl Pts',(0.00900182555548336,-0.0318564869454882,
0.0798699341087311));
#91832=CARTESIAN_POINT('Ctrl Pts',(0.00894229294157205,-0.031774074144646,
0.0798784404526084));
#91833=CARTESIAN_POINT('Ctrl Pts',(0.00916036264866917,-0.0320218834582334,
0.079879711733031));
#91834=CARTESIAN_POINT('Ctrl Pts',(0.00910073020101652,-0.0319391099350615,
0.0798905000296564));
#91835=CARTESIAN_POINT('Ctrl Pts',(0.00904096542238433,-0.0318564869454882,
0.0799003506208954));
#91836=CARTESIAN_POINT('Ctrl Pts',(0.0089811125133083,-0.031774074144646,
0.079909260395793));
#91837=CARTESIAN_POINT('Ctrl Pts',(0.00920012479320074,-0.0320218834582334,
0.0799093056498034));
#91838=CARTESIAN_POINT('Ctrl Pts',(0.00914018434441733,-0.0319391099350615,
0.0799205077742291));
#91839=CARTESIAN_POINT('Ctrl Pts',(0.0090801052892853,-0.0318564869454882,
0.0799307671330597));
#91840=CARTESIAN_POINT('Ctrl Pts',(0.00901993208504454,-0.031774074144646,
0.0799400803389776));
#91841=CARTESIAN_POINT('Origin',(0.00547432768211527,-0.0326352985528673,
0.0635575828015964));
#91842=CARTESIAN_POINT('Ctrl Pts',(0.00898722884210647,-0.0322357242816073,
0.0798361748904105));
#91843=CARTESIAN_POINT('Ctrl Pts',(0.00880613154654552,-0.0319819883628705,
0.0798636745463319));
#91844=CARTESIAN_POINT('Ctrl Pts',(0.00862365138534982,-0.0317295851069886,
0.0798795947317981));
#91845=CARTESIAN_POINT('Ctrl Pts',(0.0092335213298815,-0.0322357242816073,
0.0797932795472415));
#91846=CARTESIAN_POINT('Ctrl Pts',(0.00905379019536725,-0.0319819883628705,
0.0798286232994688));
#91847=CARTESIAN_POINT('Ctrl Pts',(0.00887217428423548,-0.0317295851069886,
0.0798524586169422));
#91848=CARTESIAN_POINT('Ctrl Pts',(0.0104602356352348,-0.0340223579322365,
0.0794037854231929));
#91849=CARTESIAN_POINT('Ctrl Pts',(0.010387772231802,-0.0339125849573554,
0.0794360112098859));
#91850=CARTESIAN_POINT('Ctrl Pts',(0.0103146927486617,-0.0338030433565221,
0.0794667145278224));
#91851=CARTESIAN_POINT('Ctrl Pts',(0.0102410941227755,-0.0336938721132327,
0.0794958643971455));
#91852=CARTESIAN_POINT('Ctrl Pts',(0.0105651125464053,-0.0340223579322365,
0.0794467041060043));
#91853=CARTESIAN_POINT('Ctrl Pts',(0.0104920571823999,-0.0339125849573554,
0.0794803764188328));
#91854=CARTESIAN_POINT('Ctrl Pts',(0.0104183562149211,-0.0338030433565221,
0.0795125129942392));
#91855=CARTESIAN_POINT('Ctrl Pts',(0.0103441075381826,-0.0336938721132327,
0.0795430810899255));
#91856=CARTESIAN_POINT('Ctrl Pts',(0.0106699894575757,-0.0340223579322365,
0.0794896227888156));
#91857=CARTESIAN_POINT('Ctrl Pts',(0.0105963421329978,-0.0339125849573554,
0.0795247416277796));
#91858=CARTESIAN_POINT('Ctrl Pts',(0.0105220196811805,-0.0338030433565221,
0.0795583114606561));
#91859=CARTESIAN_POINT('Ctrl Pts',(0.0104471209535897,-0.0336938721132327,
0.0795902977827055));
#91860=CARTESIAN_POINT('Ctrl Pts',(0.0107748663687462,-0.0340223579322365,
0.079532541471627));
#91861=CARTESIAN_POINT('Ctrl Pts',(0.0107006270835957,-0.0339125849573554,
0.0795691068367265));
#91862=CARTESIAN_POINT('Ctrl Pts',(0.0106256831474399,-0.0338030433565221,
0.079604109927073));
#91863=CARTESIAN_POINT('Ctrl Pts',(0.0105501343689969,-0.0336938721132327,
0.0796375144754855));
#91864=CARTESIAN_POINT('Origin',(0.00301089187414373,-0.0345589643415107,
0.0644881412024376));
#91865=CARTESIAN_POINT('Ctrl Pts',(0.0102248110767331,-0.034193496108874,
0.0797701136670256));
#91866=CARTESIAN_POINT('Ctrl Pts',(0.0101473130373639,-0.0340836138581107,
0.079799085611151));
#91867=CARTESIAN_POINT('Ctrl Pts',(0.0100692526694187,-0.0339738896643499,
0.0798264399946811));
#91868=CARTESIAN_POINT('Ctrl Pts',(0.00999073222743623,-0.0338644633294062,
0.0798521485046812));
#91869=CARTESIAN_POINT('Ctrl Pts',(0.0102654662997002,-0.034193496108874,
0.0796643388491664));
#91870=CARTESIAN_POINT('Ctrl Pts',(0.010189426832432,-0.0340836138581107,
0.0796938714047413));
#91871=CARTESIAN_POINT('Ctrl Pts',(0.0101128127360598,-0.0339738896643499,
0.0797218163128183));
#91872=CARTESIAN_POINT('Ctrl Pts',(0.0100357244647382,-0.0338644633294062,
0.0797481443805791));
#91873=CARTESIAN_POINT('Ctrl Pts',(0.0103061215226674,-0.034193496108874,
0.0795585640313071));
#91874=CARTESIAN_POINT('Ctrl Pts',(0.0102315406275001,-0.0340836138581107,
0.0795886571983317));
#91875=CARTESIAN_POINT('Ctrl Pts',(0.0101563728027009,-0.0339738896643499,
0.0796171926309556));
#91876=CARTESIAN_POINT('Ctrl Pts',(0.0100807167020402,-0.0338644633294062,
0.0796441402564771));
#91877=CARTESIAN_POINT('Ctrl Pts',(0.0103467767456346,-0.034193496108874,
0.0794527892134478));
#91878=CARTESIAN_POINT('Ctrl Pts',(0.0102736544225682,-0.0340836138581107,
0.0794834429919221));
#91879=CARTESIAN_POINT('Ctrl Pts',(0.010199932869342,-0.0339738896643499,
0.0795125689490928));
#91880=CARTESIAN_POINT('Ctrl Pts',(0.0101257089393421,-0.0338644633294062,
0.079540136132375));
#91881=CARTESIAN_POINT('Origin',(0.00341287973882487,-0.0345610621861447,
0.0642236496744578));
#91882=CARTESIAN_POINT('Ctrl Pts',(0.0103793727902364,-0.03424362768739,
0.0794405988373859));
#91883=CARTESIAN_POINT('Ctrl Pts',(0.010179834565659,-0.033943005420186,
0.0795256698391681));
#91884=CARTESIAN_POINT('Ctrl Pts',(0.00997445531183739,-0.0336441434784162,
0.0795954691264955));
#91885=CARTESIAN_POINT('Ctrl Pts',(0.0106071592389115,-0.03424362768739,
0.0793375778016699));
#91886=CARTESIAN_POINT('Ctrl Pts',(0.0104115065167494,-0.033943005420186,
0.07943123991099));
#91887=CARTESIAN_POINT('Ctrl Pts',(0.0102093546096173,-0.0336441434784162,
0.0795098985713815));
#91888=CARTESIAN_POINT('Ctrl Pts',(0.0100085802132314,-0.0336938721132429,
0.079583752057588));
#91889=CARTESIAN_POINT('Ctrl Pts',(0.00989482947711622,-0.0335278710435085,
0.0796232086172443));
#91890=CARTESIAN_POINT('Ctrl Pts',(0.00977988141079358,-0.0333620469224321,
0.0796590841026647));
#91891=CARTESIAN_POINT('Ctrl Pts',(0.00966367288018423,-0.0331951640388602,
0.079691377236018));
#91892=CARTESIAN_POINT('Ctrl Pts',(0.0100871682276307,-0.0336938721132429,
0.0795545638096783));
#91893=CARTESIAN_POINT('Ctrl Pts',(0.00997402852136208,-0.0335278710435085,
0.0795956655390796));
#91894=CARTESIAN_POINT('Ctrl Pts',(0.00985963967783158,-0.0333620469224321,
0.0796332047772154));
#91895=CARTESIAN_POINT('Ctrl Pts',(0.00974393856433933,-0.0331951640388602,
0.0796671811667011));
#91896=CARTESIAN_POINT('Ctrl Pts',(0.0101657562420301,-0.0336938721132429,
0.0795253755617685));
#91897=CARTESIAN_POINT('Ctrl Pts',(0.0100532275656079,-0.0335278710435085,
0.079568122460915));
#91898=CARTESIAN_POINT('Ctrl Pts',(0.00993939794486958,-0.0333620469224321,
0.0796073254517662));
#91899=CARTESIAN_POINT('Ctrl Pts',(0.00982420424849443,-0.0331951640388602,
0.0796429850973842));
#91900=CARTESIAN_POINT('Ctrl Pts',(0.0102443442564294,-0.0336938721132429,
0.0794961873138587));
#91901=CARTESIAN_POINT('Ctrl Pts',(0.0101324266098538,-0.0335278710435085,
0.0795405793827504));
#91902=CARTESIAN_POINT('Ctrl Pts',(0.0100191562119076,-0.0333620469224321,
0.0795814461263169));
#91903=CARTESIAN_POINT('Ctrl Pts',(0.00990446993264953,-0.0331951640388602,
0.0796187890280672));
#91904=CARTESIAN_POINT('Ctrl Pts',(0.0100085802132344,-0.0336938721132427,
0.0795837520576004));
#91905=CARTESIAN_POINT('Ctrl Pts',(0.00997677465933334,-0.0336474569765026,
0.0795947844058536));
#91906=CARTESIAN_POINT('Ctrl Pts',(0.0099448421372035,-0.0336011045488949,
0.0796054436739975));
#91907=CARTESIAN_POINT('Ctrl Pts',(0.00986466967179713,-0.0334847282606778,
0.0796322057256462));
#91908=CARTESIAN_POINT('Ctrl Pts',(0.00978374541518868,-0.0333679869945434,
0.0796566003215673));
#91909=CARTESIAN_POINT('Origin',(0.00547819766777445,-0.0326434571768956,
0.0635488047474904));
#91910=CARTESIAN_POINT('Ctrl Pts',(0.00986693048984509,-0.033693872113246,
0.0798927915294063));
#91911=CARTESIAN_POINT('Ctrl Pts',(0.00983331602536066,-0.0336474569764993,
0.0799029947548258));
#91912=CARTESIAN_POINT('Ctrl Pts',(0.00979958442252474,-0.033601104548885,
0.0799128037813654));
#91913=CARTESIAN_POINT('Ctrl Pts',(0.00971418376321095,-0.0334837508643205,
0.0799376379802556));
#91914=CARTESIAN_POINT('Ctrl Pts',(0.00962808471679835,-0.0333660264760493,
0.0799599306753055));
#91915=CARTESIAN_POINT('Ctrl Pts',(0.0100085802132335,-0.033693872113246,
0.0795837520575873));
#91916=CARTESIAN_POINT('Ctrl Pts',(0.00997677465932791,-0.0336474569764993,
0.0795947844058422));
#91917=CARTESIAN_POINT('Ctrl Pts',(0.0099448421371935,-0.033601104548885,
0.0796054436739875));
#91918=CARTESIAN_POINT('Ctrl Pts',(0.00986399633638482,-0.0334837508643205,
0.0796324304890475));
#91919=CARTESIAN_POINT('Ctrl Pts',(0.00978238636184186,-0.0333660264760493,
0.0796570098248924));
#91920=CARTESIAN_POINT('Ctrl Pts',(0.0101257348912479,-0.0335235895815128,
0.0795401263586193));
#91921=CARTESIAN_POINT('Ctrl Pts',(0.0100515291897403,-0.0334144449262719,
0.079567687178991));
#91922=CARTESIAN_POINT('Ctrl Pts',(0.00997666884906489,-0.0333049234473133,
0.0795937466294591));
#91923=CARTESIAN_POINT('Ctrl Pts',(0.00990124657415982,-0.0331951640388588,
0.0796182627169481));
#91924=CARTESIAN_POINT('Ctrl Pts',(0.0102277099137026,-0.0335235895815128,
0.0795895456593257));
#91925=CARTESIAN_POINT('Ctrl Pts',(0.0101528238582231,-0.0334144449262719,
0.0796185103666518));
#91926=CARTESIAN_POINT('Ctrl Pts',(0.0100772533786836,-0.0333049234473133,
0.0796459612613693));
#91927=CARTESIAN_POINT('Ctrl Pts',(0.0100010919269015,-0.0331951640388588,
0.0796718544889176));
#91928=CARTESIAN_POINT('Ctrl Pts',(0.0103296849361572,-0.0335235895815128,
0.0796389649600321));
#91929=CARTESIAN_POINT('Ctrl Pts',(0.0102541185267059,-0.0334144449262719,
0.0796693335543126));
#91930=CARTESIAN_POINT('Ctrl Pts',(0.0101778379083023,-0.0333049234473133,
0.0796981758932794));
#91931=CARTESIAN_POINT('Ctrl Pts',(0.0101009372796431,-0.0331951640388588,
0.0797254462608871));
#91932=CARTESIAN_POINT('Ctrl Pts',(0.0104316599586119,-0.0335235895815128,
0.0796883842607385));
#91933=CARTESIAN_POINT('Ctrl Pts',(0.0103554131951887,-0.0334144449262719,
0.0797201567419734));
#91934=CARTESIAN_POINT('Ctrl Pts',(0.010278422437921,-0.0333049234473132,
0.0797503905251896));
#91935=CARTESIAN_POINT('Ctrl Pts',(0.0102007826323847,-0.0331951640388588,
0.0797790380328566));
#91936=CARTESIAN_POINT('Origin',(0.0110564677013646,-0.0391228853390852,
0.0858666537048777));
#91937=CARTESIAN_POINT('Ctrl Pts',(0.0118349971103021,-0.0352722978779628,
0.0785444337952683));
#91938=CARTESIAN_POINT('Ctrl Pts',(0.0118203364661147,-0.0352466642097239,
0.0785563568062168));
#91939=CARTESIAN_POINT('Ctrl Pts',(0.0118057383500412,-0.0352210183808312,
0.0785683300204186));
#91940=CARTESIAN_POINT('Ctrl Pts',(0.0117912025846368,-0.0351953608940152,
0.0785803542721384));
#91941=CARTESIAN_POINT('Origin',(0.0147839835286742,-0.0352456003065068,
0.0824576450467876));
#91942=CARTESIAN_POINT('Ctrl Pts',(0.0116933940119547,-0.035024121149334,
0.0786576769630387));
#91943=CARTESIAN_POINT('Ctrl Pts',(0.0116313026128081,-0.0349144232867422,
0.0787068469000283));
#91944=CARTESIAN_POINT('Ctrl Pts',(0.0115681576712812,-0.0348045283677512,
0.0787547627940635));
#91945=CARTESIAN_POINT('Ctrl Pts',(0.011504037784138,-0.0346945769586886,
0.0788013602612215));
#91946=CARTESIAN_POINT('Ctrl Pts',(0.0118056492933128,-0.035024121149334,
0.078673165462346));
#91947=CARTESIAN_POINT('Ctrl Pts',(0.0117433445464483,-0.0349144232867422,
0.0787238816697402));
#91948=CARTESIAN_POINT('Ctrl Pts',(0.0116799541669921,-0.0348045283677512,
0.0787733403496477));
#91949=CARTESIAN_POINT('Ctrl Pts',(0.0116155569925468,-0.0346945769586886,
0.0788214751303346));
#91950=CARTESIAN_POINT('Ctrl Pts',(0.0119179045746708,-0.035024121149334,
0.0786886539616534));
#91951=CARTESIAN_POINT('Ctrl Pts',(0.0118553864800886,-0.0349144232867422,
0.0787409164394521));
#91952=CARTESIAN_POINT('Ctrl Pts',(0.0117917506627029,-0.0348045283677512,
0.0787919179052318));
#91953=CARTESIAN_POINT('Ctrl Pts',(0.0117270762009556,-0.0346945769586886,
0.0788415899994477));
#91954=CARTESIAN_POINT('Ctrl Pts',(0.0120301598560289,-0.035024121149334,
0.0787041424609608));
#91955=CARTESIAN_POINT('Ctrl Pts',(0.0119674284137288,-0.0349144232867422,
0.0787579512091641));
#91956=CARTESIAN_POINT('Ctrl Pts',(0.0119035471584137,-0.0348045283677512,
0.078810495460816));
#91957=CARTESIAN_POINT('Ctrl Pts',(0.0118385954093645,-0.0346945769586886,
0.0788617048685608));
#91958=CARTESIAN_POINT('Origin',(0.00178047136194146,-0.034562906794219,
0.065115045742413));
#91959=CARTESIAN_POINT('Ctrl Pts',(0.0115683561831177,-0.0351970973651602,
0.0789780878000176));
#91960=CARTESIAN_POINT('Ctrl Pts',(0.0115014695698662,-0.0350869349321767,
0.0790258077044247));
#91961=CARTESIAN_POINT('Ctrl Pts',(0.0114335354781549,-0.0349764985129725,
0.0790721766038223));
#91962=CARTESIAN_POINT('Ctrl Pts',(0.0113646383823896,-0.0348659306849652,
0.0791171292451199));
#91963=CARTESIAN_POINT('Ctrl Pts',(0.0115778214613775,-0.0351970973651602,
0.0788964123498657));
#91964=CARTESIAN_POINT('Ctrl Pts',(0.011512066350798,-0.0350869349321767,
0.0789442633828754));
#91965=CARTESIAN_POINT('Ctrl Pts',(0.0114452619729914,-0.0349764985129725,
0.0789907870428144));
#91966=CARTESIAN_POINT('Ctrl Pts',(0.0113774913269834,-0.0348659306849652,
0.0790359179622504));
#91967=CARTESIAN_POINT('Ctrl Pts',(0.0115872867396373,-0.0351970973651602,
0.0788147368997138));
#91968=CARTESIAN_POINT('Ctrl Pts',(0.0115226631317298,-0.0350869349321767,
0.078862719061326));
#91969=CARTESIAN_POINT('Ctrl Pts',(0.0114569884678279,-0.0349764985129725,
0.0789093974818066));
#91970=CARTESIAN_POINT('Ctrl Pts',(0.0113903442715773,-0.0348659306849652,
0.0789547066793808));
#91971=CARTESIAN_POINT('Ctrl Pts',(0.0115967520178971,-0.0351970973651602,
0.0787330614495619));
#91972=CARTESIAN_POINT('Ctrl Pts',(0.0115332599126616,-0.0350869349321767,
0.0787811747397767));
#91973=CARTESIAN_POINT('Ctrl Pts',(0.0114687149626644,-0.0349764985129725,
0.0788280079207987));
#91974=CARTESIAN_POINT('Ctrl Pts',(0.0114031972161712,-0.0348659306849652,
0.0788734953965113));
#91975=CARTESIAN_POINT('Origin',(0.00219846912065955,-0.0345637187966843,
0.064877131409313));
#91976=CARTESIAN_POINT('Ctrl Pts',(0.011624165403947,-0.0352450361861252,
0.0787134901530824));
#91977=CARTESIAN_POINT('Ctrl Pts',(0.0114520505529786,-0.0349452761023765,
0.0788455092688154));
#91978=CARTESIAN_POINT('Ctrl Pts',(0.0112704804424388,-0.0346444289983475,
0.0789641889376781));
#91979=CARTESIAN_POINT('Ctrl Pts',(0.0118191773678874,-0.0352450361861252,
0.0785570601881776));
#91980=CARTESIAN_POINT('Ctrl Pts',(0.0116529623697057,-0.0349452761023765,
0.0786964343006313));
#91981=CARTESIAN_POINT('Ctrl Pts',(0.0114767213426597,-0.0346444289983475,
0.078822892472485));
#91982=CARTESIAN_POINT('Ctrl Pts',(0.011403311649826,-0.0345231616327822,
0.078872919362593));
#91983=CARTESIAN_POINT('Ctrl Pts',(0.0113382128557516,-0.0344132092796975,
0.0789181230589455));
#91984=CARTESIAN_POINT('Ctrl Pts',(0.011272182417673,-0.0343032738558974,
0.0789619779057887));
#91985=CARTESIAN_POINT('Ctrl Pts',(0.0112053063673641,-0.0341934961088741,
0.0790044298868675));
#91986=CARTESIAN_POINT('Ctrl Pts',(0.0115143728692186,-0.0345231616327822,
0.078895425843573));
#91987=CARTESIAN_POINT('Ctrl Pts',(0.0114489638549906,-0.0344132092796975,
0.078942160362473));
#91988=CARTESIAN_POINT('Ctrl Pts',(0.0113825915489072,-0.0343032738558974,
0.0789875395362214));
#91989=CARTESIAN_POINT('Ctrl Pts',(0.0113153424707378,-0.0341934961088741,
0.0790315074069425));
#91990=CARTESIAN_POINT('Ctrl Pts',(0.0116254340886112,-0.0345231616327822,
0.078917932324553));
#91991=CARTESIAN_POINT('Ctrl Pts',(0.0115597148542295,-0.0344132092796975,
0.0789661976660006));
#91992=CARTESIAN_POINT('Ctrl Pts',(0.0114930006801414,-0.0343032738558974,
0.079013101166654));
#91993=CARTESIAN_POINT('Ctrl Pts',(0.0114253785741115,-0.0341934961088741,
0.0790585849270175));
#91994=CARTESIAN_POINT('Ctrl Pts',(0.0117364953080039,-0.0345231616327822,
0.0789404388055329));
#91995=CARTESIAN_POINT('Ctrl Pts',(0.0116704658534684,-0.0344132092796975,
0.0789902349695282));
#91996=CARTESIAN_POINT('Ctrl Pts',(0.0116034098113757,-0.0343032738558974,
0.0790386627970866));
#91997=CARTESIAN_POINT('Ctrl Pts',(0.0115354146774852,-0.0341934961088741,
0.0790856624470924));
#91998=CARTESIAN_POINT('Origin',(0.00177331298048502,-0.0345625596230865,
0.0651052858307627));
#91999=CARTESIAN_POINT('Ctrl Pts',(0.0112407003659537,-0.0346945769586886,
0.0792768724485713));
#92000=CARTESIAN_POINT('Ctrl Pts',(0.0111700494722858,-0.034584662917669,
0.0793198251564084));
#92001=CARTESIAN_POINT('Ctrl Pts',(0.0110984982669136,-0.0344746925051586,
0.079361324169208));
#92002=CARTESIAN_POINT('Ctrl Pts',(0.0110261386490849,-0.0343648066255171,
0.0794013166922767));
#92003=CARTESIAN_POINT('Ctrl Pts',(0.0112608152192293,-0.0346945769586886,
0.0791653533279674));
#92004=CARTESIAN_POINT('Ctrl Pts',(0.0111917011154095,-0.034584662917669,
0.0792085832286495));
#92005=CARTESIAN_POINT('Ctrl Pts',(0.0111216812301388,-0.0344746925051586,
0.0792503912618223));
#92006=CARTESIAN_POINT('Ctrl Pts',(0.0110508455021963,-0.0343648066255171,
0.0792907242287365));
#92007=CARTESIAN_POINT('Ctrl Pts',(0.0112809300725049,-0.0346945769586886,
0.0790538342073635));
#92008=CARTESIAN_POINT('Ctrl Pts',(0.0112133527585333,-0.034584662917669,
0.0790973413008906));
#92009=CARTESIAN_POINT('Ctrl Pts',(0.011144864193364,-0.0344746925051586,
0.0791394583544365));
#92010=CARTESIAN_POINT('Ctrl Pts',(0.0110755523553077,-0.0343648066255171,
0.0791801317651963));
#92011=CARTESIAN_POINT('Ctrl Pts',(0.0113010449257805,-0.0346945769586886,
0.0789423150867597));
#92012=CARTESIAN_POINT('Ctrl Pts',(0.011235004401657,-0.034584662917669,
0.0789860993731318));
#92013=CARTESIAN_POINT('Ctrl Pts',(0.0111680471565892,-0.0344746925051586,
0.0790285254470508));
#92014=CARTESIAN_POINT('Ctrl Pts',(0.0111002592084191,-0.0343648066255171,
0.0790695393016561));
#92015=CARTESIAN_POINT('Origin',(0.00216635378845963,-0.0345626446731195,
0.0648283181321802));
#92016=CARTESIAN_POINT('Ctrl Pts',(0.0113006850036053,-0.0346945769586886,
0.0789443105377789));
#92017=CARTESIAN_POINT('Ctrl Pts',(0.0112002662498559,-0.0345275153362891,
0.0790108520391062));
#92018=CARTESIAN_POINT('Ctrl Pts',(0.0110977288537038,-0.0343603235965159,
0.0790742526740977));
#92019=CARTESIAN_POINT('Ctrl Pts',(0.0109933788621512,-0.034193496108874,
0.0791343294390539));
#92020=CARTESIAN_POINT('Ctrl Pts',(0.0113695452016306,-0.0346945769586886,
0.0788964952529927));
#92021=CARTESIAN_POINT('Ctrl Pts',(0.0112701279581652,-0.0345275153362891,
0.0789644790587378));
#92022=CARTESIAN_POINT('Ctrl Pts',(0.0111685469721926,-0.0343603235965159,
0.0790293538677774));
#92023=CARTESIAN_POINT('Ctrl Pts',(0.0110651055268785,-0.034193496108874,
0.0790909322744188));
#92024=CARTESIAN_POINT('Ctrl Pts',(0.0114384053996559,-0.0346945769586886,
0.0788486799682066));
#92025=CARTESIAN_POINT('Ctrl Pts',(0.0113399896664746,-0.0345275153362891,
0.0789181060783693));
#92026=CARTESIAN_POINT('Ctrl Pts',(0.0112393650906815,-0.0343603235965159,
0.0789844550614572));
#92027=CARTESIAN_POINT('Ctrl Pts',(0.0111368321916058,-0.034193496108874,
0.0790475351097837));
#92028=CARTESIAN_POINT('Ctrl Pts',(0.0115072655976812,-0.0346945769586886,
0.0788008646834204));
#92029=CARTESIAN_POINT('Ctrl Pts',(0.0114098513747839,-0.0345275153362891,
0.0788717330980009));
#92030=CARTESIAN_POINT('Ctrl Pts',(0.0113101832091703,-0.0343603235965159,
0.0789395562551369));
#92031=CARTESIAN_POINT('Ctrl Pts',(0.011208558856333,-0.034193496108874,
0.0790041379451486));
#92032=CARTESIAN_POINT('Ctrl Pts',(0.0111002859175206,-0.0340223579322365,
0.0790695224909273));
#92033=CARTESIAN_POINT('Ctrl Pts',(0.0110324328717179,-0.0339125849573551,
0.0791105762403342));
#92034=CARTESIAN_POINT('Ctrl Pts',(0.0109637777882479,-0.0338030433565216,
0.0791501967413674));
#92035=CARTESIAN_POINT('Ctrl Pts',(0.0108944129568897,-0.033693872113232,
0.0791883411090325));
#92036=CARTESIAN_POINT('Ctrl Pts',(0.0112097149802182,-0.0340223579322365,
0.0790989581847022));
#92037=CARTESIAN_POINT('Ctrl Pts',(0.0111414559394269,-0.0339125849573551,
0.0791415212462867));
#92038=CARTESIAN_POINT('Ctrl Pts',(0.0110723639070013,-0.0338030433565216,
0.0791826415957684));
#92039=CARTESIAN_POINT('Ctrl Pts',(0.011002531901532,-0.033693872113232,
0.0792222744796335));
#92040=CARTESIAN_POINT('Ctrl Pts',(0.0113191440429158,-0.0340223579322365,
0.0791283938784772));
#92041=CARTESIAN_POINT('Ctrl Pts',(0.0112504790071358,-0.0339125849573551,
0.0791724662522392));
#92042=CARTESIAN_POINT('Ctrl Pts',(0.0111809500257546,-0.0338030433565216,
0.0792150864501694));
#92043=CARTESIAN_POINT('Ctrl Pts',(0.0111106508461742,-0.033693872113232,
0.0792562078502345));
#92044=CARTESIAN_POINT('Ctrl Pts',(0.0114285731056134,-0.0340223579322365,
0.0791578295722521));
#92045=CARTESIAN_POINT('Ctrl Pts',(0.0113595020748448,-0.0339125849573551,
0.0792034112581918));
#92046=CARTESIAN_POINT('Ctrl Pts',(0.011289536144508,-0.0338030433565216,
0.0792475313045704));
#92047=CARTESIAN_POINT('Ctrl Pts',(0.0112187697908164,-0.033693872113232,
0.0792901412208355));
#92048=CARTESIAN_POINT('Origin',(0.00184025653614732,-0.0345589643414859,
0.0652051429214359));
#92049=CARTESIAN_POINT('Ctrl Pts',(0.0109126308553257,-0.034193496108874,
0.0794624686483194));
#92050=CARTESIAN_POINT('Ctrl Pts',(0.0108393750585844,-0.0340836138581107,
0.0795009252198808));
#92051=CARTESIAN_POINT('Ctrl Pts',(0.0107653586332959,-0.03397388966435,
0.0795378474642542));
#92052=CARTESIAN_POINT('Ctrl Pts',(0.0106906794791397,-0.0338644633294062,
0.0795731944758687));
#92053=CARTESIAN_POINT('Ctrl Pts',(0.0109397083997648,-0.034193496108874,
0.0793524324459361));
#92054=CARTESIAN_POINT('Ctrl Pts',(0.0108679699370935,-0.0340836138581107,
0.0793912624008006));
#92055=CARTESIAN_POINT('Ctrl Pts',(0.0107954623914456,-0.03397388966435,
0.0794285892473656));
#92056=CARTESIAN_POINT('Ctrl Pts',(0.0107222817660344,-0.0338644633294062,
0.0794643714327629));
#92057=CARTESIAN_POINT('Ctrl Pts',(0.0109667859442039,-0.034193496108874,
0.0792423962435528));
#92058=CARTESIAN_POINT('Ctrl Pts',(0.0108965648156026,-0.0340836138581107,
0.0792815995817204));
#92059=CARTESIAN_POINT('Ctrl Pts',(0.0108255661495953,-0.03397388966435,
0.0793193310304769));
#92060=CARTESIAN_POINT('Ctrl Pts',(0.0107538840529292,-0.0338644633294062,
0.0793555483896571));
#92061=CARTESIAN_POINT('Ctrl Pts',(0.010993863488643,-0.034193496108874,
0.0791323600411695));
#92062=CARTESIAN_POINT('Ctrl Pts',(0.0109251596941117,-0.0340836138581107,
0.0791719367626402));
#92063=CARTESIAN_POINT('Ctrl Pts',(0.010855669907745,-0.03397388966435,
0.0792100728135884));
#92064=CARTESIAN_POINT('Ctrl Pts',(0.0107854863398239,-0.0338644633294062,
0.0792467253465512));
#92065=CARTESIAN_POINT('Origin',(0.00220592502735406,-0.0345610621863664,
0.0648923545487759));
#92066=CARTESIAN_POINT('Ctrl Pts',(0.0110246746444469,-0.0342436276873901,
0.0791161804221925));
#92067=CARTESIAN_POINT('Ctrl Pts',(0.0108373720621055,-0.0339430054201861,
0.0792255893846222));
#92068=CARTESIAN_POINT('Ctrl Pts',(0.0106423604554252,-0.0336441434784163,
0.0793205791297093));
#92069=CARTESIAN_POINT('Ctrl Pts',(0.0112377529694063,-0.0342436276873901,
0.0789854225259395));
#92070=CARTESIAN_POINT('Ctrl Pts',(0.0110553820024206,-0.0339430054201861,
0.0791028678698763));
#92071=CARTESIAN_POINT('Ctrl Pts',(0.0108646826677109,-0.0336441434784163,
0.0792062426354285));
#92072=CARTESIAN_POINT('Ctrl Pts',(0.00986777531919926,-0.0326943950436593,
0.0798909483516457));
#92073=CARTESIAN_POINT('Ctrl Pts',(0.00978865429122989,-0.0325844576448127,
0.0799149838455146));
#92074=CARTESIAN_POINT('Ctrl Pts',(0.0097090305703225,-0.0324744968375319,
0.0799373846878336));
#92075=CARTESIAN_POINT('Ctrl Pts',(0.00962900657090852,-0.0323646534831895,
0.0799581235844798));
#92076=CARTESIAN_POINT('Ctrl Pts',(0.00991499191592088,-0.0326943950436593,
0.0797879351458107));
#92077=CARTESIAN_POINT('Ctrl Pts',(0.00983729060299523,-0.0325844576448127,
0.0798126213728758));
#92078=CARTESIAN_POINT('Ctrl Pts',(0.00975907323937763,-0.0324744968375319,
0.0798357023564791));
#92079=CARTESIAN_POINT('Ctrl Pts',(0.00968044044961222,-0.0323646534831895,
0.0798571499062074));
#92080=CARTESIAN_POINT('Ctrl Pts',(0.0099622085126425,-0.0326943950436593,
0.0796849219399757));
#92081=CARTESIAN_POINT('Ctrl Pts',(0.00988592691476058,-0.0325844576448127,
0.0797102589002369));
#92082=CARTESIAN_POINT('Ctrl Pts',(0.00980911590843275,-0.0324744968375319,
0.0797340200251246));
#92083=CARTESIAN_POINT('Ctrl Pts',(0.00973187432831593,-0.0323646534831895,
0.079756176227935));
#92084=CARTESIAN_POINT('Ctrl Pts',(0.0100094251093641,-0.0326943950436593,
0.0795819087341407));
#92085=CARTESIAN_POINT('Ctrl Pts',(0.00993456322652593,-0.0325844576448127,
0.0796078964275981));
#92086=CARTESIAN_POINT('Ctrl Pts',(0.00985915857748787,-0.0324744968375319,
0.0796323376937701));
#92087=CARTESIAN_POINT('Ctrl Pts',(0.00978330820701964,-0.0323646534831895,
0.0796552025496625));
#92088=CARTESIAN_POINT('Origin',(0.00457127317689149,-0.0326395579068152,
0.0636764031143487));
#92089=CARTESIAN_POINT('Ctrl Pts',(0.0101257369732358,-0.0325229783203385,
0.0795401258895911));
#92090=CARTESIAN_POINT('Ctrl Pts',(0.0100514342070745,-0.032413025311208,
0.079567722791953));
#92091=CARTESIAN_POINT('Ctrl Pts',(0.00997657183301764,-0.0323031222247695,
0.0795937784605653));
#92092=CARTESIAN_POINT('Ctrl Pts',(0.00990124692215074,-0.0321934096636184,
0.0796182629037315));
#92093=CARTESIAN_POINT('Ctrl Pts',(0.0102277118930496,-0.0325229783203385,
0.0795895451002191));
#92094=CARTESIAN_POINT('Ctrl Pts',(0.0101527278841629,-0.032413025311208,
0.079618547724595));
#92095=CARTESIAN_POINT('Ctrl Pts',(0.0100771552915394,-0.0323031222247695,
0.0796459948096354));
#92096=CARTESIAN_POINT('Ctrl Pts',(0.0100010921588956,-0.0321934096636184,
0.07967185461344));
#92097=CARTESIAN_POINT('Ctrl Pts',(0.0103296868128634,-0.0325229783203385,
0.0796389643108472));
#92098=CARTESIAN_POINT('Ctrl Pts',(0.0102540215612513,-0.032413025311208,
0.0796693726572371));
#92099=CARTESIAN_POINT('Ctrl Pts',(0.0101777387500611,-0.0323031222247695,
0.0796982111587055));
#92100=CARTESIAN_POINT('Ctrl Pts',(0.0101009373956406,-0.0321934096636184,
0.0797254463231485));
#92101=CARTESIAN_POINT('Ctrl Pts',(0.0104316617326772,-0.0325229783203385,
0.0796883835214752));
#92102=CARTESIAN_POINT('Ctrl Pts',(0.0103553152383397,-0.032413025311208,
0.0797201975898791));
#92103=CARTESIAN_POINT('Ctrl Pts',(0.0102783222085829,-0.0323031222247695,
0.0797504275077756));
#92104=CARTESIAN_POINT('Ctrl Pts',(0.0102007826323855,-0.0321934096636184,
0.079779038032857));
#92105=CARTESIAN_POINT('Origin',(0.0041259267352345,-0.0326393375178154,
0.0638577421876095));
#92106=CARTESIAN_POINT('Ctrl Pts',(0.0100426911070143,-0.0327445246961877,
0.0795717998469266));
#92107=CARTESIAN_POINT('Ctrl Pts',(0.00983820458501583,-0.0324436878365475,
0.0796441726789962));
#92108=CARTESIAN_POINT('Ctrl Pts',(0.00962884757017125,-0.0321434074463188,
0.0797009371470741));
#92109=CARTESIAN_POINT('Ctrl Pts',(0.0102764973271794,-0.0327445246961877,
0.0794832862806662));
#92110=CARTESIAN_POINT('Ctrl Pts',(0.0100753491488722,-0.0324436878365475,
0.0795644772583946));
#92111=CARTESIAN_POINT('Ctrl Pts',(0.00986865677507285,-0.0321434074463188,
0.0796302862783996));
#92112=CARTESIAN_POINT('Ctrl Pts',(0.00950385681755172,-0.0321934096636184,
0.079989126135911));
#92113=CARTESIAN_POINT('Ctrl Pts',(0.00942333071739944,-0.0320835708272304,
0.0800081584405468));
#92114=CARTESIAN_POINT('Ctrl Pts',(0.00934245745310258,-0.0319739230346347,
0.0800255132222151));
#92115=CARTESIAN_POINT('Ctrl Pts',(0.00926134220050527,-0.0318646057455576,
0.0800411762178432));
#92116=CARTESIAN_POINT('Ctrl Pts',(0.00955744857340869,-0.0321934096636184,
0.0798892808131882));
#92117=CARTESIAN_POINT('Ctrl Pts',(0.00947829941807147,-0.0320835708272304,
0.0799090521899041));
#92118=CARTESIAN_POINT('Ctrl Pts',(0.00939878700484743,-0.0319739230346347,
0.0799271741107622));
#92119=CARTESIAN_POINT('Ctrl Pts',(0.00931901484379366,-0.0318646057455576,
0.0799436311975624));
#92120=CARTESIAN_POINT('Ctrl Pts',(0.00961104032926566,-0.0321934096636184,
0.0797894354904654));
#92121=CARTESIAN_POINT('Ctrl Pts',(0.0095332681187435,-0.0320835708272304,
0.0798099459392615));
#92122=CARTESIAN_POINT('Ctrl Pts',(0.00945511655659229,-0.0319739230346347,
0.0798288349993092));
#92123=CARTESIAN_POINT('Ctrl Pts',(0.00937668748708205,-0.0318646057455576,
0.0798460861772817));
#92124=CARTESIAN_POINT('Ctrl Pts',(0.00966463208512263,-0.0321934096636184,
0.0796895901677426));
#92125=CARTESIAN_POINT('Ctrl Pts',(0.00958823681941552,-0.0320835708272304,
0.0797108396886189));
#92126=CARTESIAN_POINT('Ctrl Pts',(0.00951144610833714,-0.0319739230346347,
0.0797304958878563));
#92127=CARTESIAN_POINT('Ctrl Pts',(0.00943436013037044,-0.0318646057455576,
0.0797485411570009));
#92128=CARTESIAN_POINT('Origin',(0.00460026649247057,-0.0326371942646895,
0.0637671874260098));
#92129=CARTESIAN_POINT('Ctrl Pts',(0.00978399678220021,-0.0320218834582328,
0.0796558591807856));
#92130=CARTESIAN_POINT('Ctrl Pts',(0.00972669409845655,-0.0319391099350611,
0.0796731380011153));
#92131=CARTESIAN_POINT('Ctrl Pts',(0.00966915632175085,-0.0318564869454879,
0.0796895115632053));
#92132=CARTESIAN_POINT('Ctrl Pts',(0.00961142647409324,-0.0317740741446459,
0.0797049718535495));
#92133=CARTESIAN_POINT('Ctrl Pts',(0.0098271544916287,-0.0320218834582328,
0.0796802362225375));
#92134=CARTESIAN_POINT('Ctrl Pts',(0.00976959810181152,-0.0319391099350611,
0.0796979642102892));
#92135=CARTESIAN_POINT('Ctrl Pts',(0.00971179975893409,-0.0318564869454879,
0.0797147827060062));
#92136=CARTESIAN_POINT('Ctrl Pts',(0.00965380270504909,-0.0317740741446459,
0.0797306833898253));
#92137=CARTESIAN_POINT('Ctrl Pts',(0.00987031220105719,-0.0320218834582328,
0.0797046132642893));
#92138=CARTESIAN_POINT('Ctrl Pts',(0.00981250210516649,-0.0319391099350611,
0.0797227904194631));
#92139=CARTESIAN_POINT('Ctrl Pts',(0.00975444319611733,-0.0318564869454879,
0.0797400538488072));
#92140=CARTESIAN_POINT('Ctrl Pts',(0.00969617893600494,-0.0317740741446459,
0.0797563949261011));
#92141=CARTESIAN_POINT('Ctrl Pts',(0.00991346991048568,-0.0320218834582328,
0.0797289903060412));
#92142=CARTESIAN_POINT('Ctrl Pts',(0.00985540610852146,-0.0319391099350611,
0.079747616628637));
#92143=CARTESIAN_POINT('Ctrl Pts',(0.00979708663330056,-0.0318564869454879,
0.0797653249916081));
#92144=CARTESIAN_POINT('Ctrl Pts',(0.00973855516696078,-0.0317740741446459,
0.0797821064623769));
#92145=CARTESIAN_POINT('Origin',(0.00416763752318638,-0.0326352985531528,
0.0639731718762183));
#92146=CARTESIAN_POINT('Ctrl Pts',(0.00969308699300744,-0.0322357242816073,
0.0796831191424922));
#92147=CARTESIAN_POINT('Ctrl Pts',(0.00951686432451163,-0.0319819883628706,
0.0797330994650554));
#92148=CARTESIAN_POINT('Ctrl Pts',(0.00933781840221456,-0.0317295851069886,
0.0797717649437681));
#92149=CARTESIAN_POINT('Ctrl Pts',(0.00993206117888817,-0.0322357242816073,
0.079609693408021));
#92150=CARTESIAN_POINT('Ctrl Pts',(0.00975817702480558,-0.0319819883628706,
0.0796672847484662));
#92151=CARTESIAN_POINT('Ctrl Pts',(0.00958098056679106,-0.0317295851069886,
0.079713694626751));
#92152=CARTESIAN_POINT('Ctrl Pts',(0.0107855108621147,-0.0335235895815127,
0.0792467123972283));
#92153=CARTESIAN_POINT('Ctrl Pts',(0.0107153445814646,-0.0334144449262719,
0.0792833563328182));
#92154=CARTESIAN_POINT('Ctrl Pts',(0.0106443406521271,-0.0333049234473133,
0.0793185927852983));
#92155=CARTESIAN_POINT('Ctrl Pts',(0.0105725857849066,-0.0331951640388588,
0.0793523684737116));
#92156=CARTESIAN_POINT('Ctrl Pts',(0.0108928756618168,-0.0335235895815127,
0.0792829611526807));
#92157=CARTESIAN_POINT('Ctrl Pts',(0.0108222103456806,-0.0334144449262719,
0.0793210831761204));
#92158=CARTESIAN_POINT('Ctrl Pts',(0.0107506762713432,-0.0333049234473133,
0.0793577891048965));
#92159=CARTESIAN_POINT('Ctrl Pts',(0.0106783606572928,-0.0331951640388588,
0.0793930237176365));
#92160=CARTESIAN_POINT('Ctrl Pts',(0.0110002404615188,-0.0335235895815127,
0.0793192099081332));
#92161=CARTESIAN_POINT('Ctrl Pts',(0.0109290761098966,-0.0334144449262719,
0.0793588100194225));
#92162=CARTESIAN_POINT('Ctrl Pts',(0.0108570118905593,-0.0333049234473133,
0.0793969854244946));
#92163=CARTESIAN_POINT('Ctrl Pts',(0.010784135529679,-0.0331951640388588,
0.0794336789615614));
#92164=CARTESIAN_POINT('Ctrl Pts',(0.0111076052612209,-0.0335235895815127,
0.0793554586635856));
#92165=CARTESIAN_POINT('Ctrl Pts',(0.0110359418741126,-0.0334144449262719,
0.0793965368627246));
#92166=CARTESIAN_POINT('Ctrl Pts',(0.0109633475097754,-0.0333049234473133,
0.0794361817440927));
#92167=CARTESIAN_POINT('Ctrl Pts',(0.0108899104020652,-0.0331951640388588,
0.0794743342054864));
#92168=CARTESIAN_POINT('Origin',(0.00417037681106416,-0.0326434571770334,
0.0639639780016505));
#92169=CARTESIAN_POINT('Ctrl Pts',(0.0105729478769377,-0.0336938721132457,
0.0796290334902976));
#92170=CARTESIAN_POINT('Ctrl Pts',(0.0105408772757806,-0.0336474569764991,
0.0796433692697655));
#92171=CARTESIAN_POINT('Ctrl Pts',(0.0105086410537226,-0.033601104548885,
0.0796573286400577));
#92172=CARTESIAN_POINT('Ctrl Pts',(0.0104270263545652,-0.0334837508643204,
0.0796926705546524));
#92173=CARTESIAN_POINT('Ctrl Pts',(0.0103444002404054,-0.033366026476049,
0.0797255785370371));
#92174=CARTESIAN_POINT('Ctrl Pts',(0.0106747477336468,-0.0336938721132457,
0.0793046774691523));
#92175=CARTESIAN_POINT('Ctrl Pts',(0.0106445756959143,-0.0336474569764991,
0.0793196091169623));
#92176=CARTESIAN_POINT('Ctrl Pts',(0.0106142309317989,-0.033601104548885,
0.0793341865398494));
#92177=CARTESIAN_POINT('Ctrl Pts',(0.0105374049690721,-0.0334837508643204,
0.0793710932214476));
#92178=CARTESIAN_POINT('Ctrl Pts',(0.0104595191211943,-0.033366026476049,
0.0794057071838885));
#92179=CARTESIAN_POINT('Ctrl Pts',(0.0106747477336484,-0.0336938721132426,
0.0793046774691665));
#92180=CARTESIAN_POINT('Ctrl Pts',(0.0106445756959201,-0.0336474569765026,
0.0793196091169743));
#92181=CARTESIAN_POINT('Ctrl Pts',(0.0106142309318089,-0.0336011045488949,
0.0793341865398594));
#92182=CARTESIAN_POINT('Ctrl Pts',(0.0105380448247086,-0.0334847282606778,
0.0793707858390697));
#92183=CARTESIAN_POINT('Ctrl Pts',(0.0104608161336227,-0.0333679869945434,
0.0794051305750701));
#92184=CARTESIAN_POINT('Ctrl Pts',(0.010674747733645,-0.0336938721132429,
0.0793046774691532));
#92185=CARTESIAN_POINT('Ctrl Pts',(0.0105668391742669,-0.0335278710435085,
0.0793580796496291));
#92186=CARTESIAN_POINT('Ctrl Pts',(0.0104572938983739,-0.0333620469224321,
0.0794080790589757));
#92187=CARTESIAN_POINT('Ctrl Pts',(0.0103460491095634,-0.0331951640388602,
0.0794546823422361));
#92188=CARTESIAN_POINT('Ctrl Pts',(0.0107490578005851,-0.0336938721132429,
0.0792658696893323));
#92189=CARTESIAN_POINT('Ctrl Pts',(0.0106419616473445,-0.0335278710435085,
0.079320827484552));
#92190=CARTESIAN_POINT('Ctrl Pts',(0.0105331797081127,-0.0333620469224321,
0.079372407438226));
#92191=CARTESIAN_POINT('Ctrl Pts',(0.0104226493032177,-0.0331951640388602,
0.0794206171084133));
#92192=CARTESIAN_POINT('Ctrl Pts',(0.0108233678675252,-0.0336938721132429,
0.0792270619095114));
#92193=CARTESIAN_POINT('Ctrl Pts',(0.0107170841204222,-0.0335278710435085,
0.0792835753194749));
#92194=CARTESIAN_POINT('Ctrl Pts',(0.0106090655178514,-0.0333620469224321,
0.0793367358174764));
#92195=CARTESIAN_POINT('Ctrl Pts',(0.010499249496872,-0.0331951640388602,
0.0793865518745905));
#92196=CARTESIAN_POINT('Ctrl Pts',(0.0108976779344653,-0.0336938721132429,
0.0791882541296904));
#92197=CARTESIAN_POINT('Ctrl Pts',(0.0107922065934999,-0.0335278710435085,
0.0792463231543978));
#92198=CARTESIAN_POINT('Ctrl Pts',(0.0106849513275902,-0.0333620469224321,
0.0793010641967267));
#92199=CARTESIAN_POINT('Ctrl Pts',(0.0105758496905263,-0.0331951640388602,
0.0793524866407678));
#92200=CARTESIAN_POINT('Ctrl Pts',(0.0103793061266113,-0.0332451089994433,
0.0794406272582177));
#92201=CARTESIAN_POINT('Ctrl Pts',(0.0101797668549345,-0.0329451141710259,
0.0795256957351628));
#92202=CARTESIAN_POINT('Ctrl Pts',(0.00997438674782287,-0.0326442513127503,
0.0795954924278775));
#92203=CARTESIAN_POINT('Ctrl Pts',(0.0106070938733704,-0.0332451089994433,
0.0793376090927011));
#92204=CARTESIAN_POINT('Ctrl Pts',(0.0104114399953744,-0.0329451141710259,
0.0794312687250738));
#92205=CARTESIAN_POINT('Ctrl Pts',(0.0102092871230025,-0.0326442513127503,
0.079509924830386));
#92206=CARTESIAN_POINT('Origin',(0.00458385954554729,-0.0326401908831853,
0.0637120898756703));
#92207=CARTESIAN_POINT('Origin',(0.00412306332237759,-0.0326396682857103,
0.0638497115031866));
#92208=CARTESIAN_POINT('Ctrl Pts',(0.010224811076733,-0.0331951640388588,
0.0797701136670258));
#92209=CARTESIAN_POINT('Ctrl Pts',(0.0101474053713548,-0.0330855618127431,
0.0797990510929201));
#92210=CARTESIAN_POINT('Ctrl Pts',(0.0100693457780804,-0.0329757224171935,
0.0798264095355998));
#92211=CARTESIAN_POINT('Ctrl Pts',(0.00999073053843142,-0.0328657861694599,
0.0798521490576809));
#92212=CARTESIAN_POINT('Ctrl Pts',(0.010265466288291,-0.0331951640388588,
0.0796643388788503));
#92213=CARTESIAN_POINT('Ctrl Pts',(0.0101895174168088,-0.0330855618127431,
0.0796938362481042));
#92214=CARTESIAN_POINT('Ctrl Pts',(0.0101129041345685,-0.0329757224171935,
0.0797217851480688));
#92215=CARTESIAN_POINT('Ctrl Pts',(0.0100357227939136,-0.0328657861694599,
0.0797481449760927));
#92216=CARTESIAN_POINT('Ctrl Pts',(0.010306121499849,-0.0331951640388588,
0.0795585640906749));
#92217=CARTESIAN_POINT('Ctrl Pts',(0.0102316294622629,-0.0330855618127431,
0.0795886214032884));
#92218=CARTESIAN_POINT('Ctrl Pts',(0.0101564624910565,-0.0329757224171935,
0.0796171607605378));
#92219=CARTESIAN_POINT('Ctrl Pts',(0.0100807150493959,-0.0328657861694599,
0.0796441408945044));
#92220=CARTESIAN_POINT('Ctrl Pts',(0.0103467767114071,-0.0331951640388588,
0.0794527893024995));
#92221=CARTESIAN_POINT('Ctrl Pts',(0.010273741507717,-0.0330855618127431,
0.0794834065584725));
#92222=CARTESIAN_POINT('Ctrl Pts',(0.0102000208475445,-0.0329757224171935,
0.0795125363730068));
#92223=CARTESIAN_POINT('Ctrl Pts',(0.0101257073048781,-0.0328657861694599,
0.0795401368129162));
#92224=CARTESIAN_POINT('Ctrl Pts',(0.0104602346180054,-0.0330240426238156,
0.0794037863342683));
#92225=CARTESIAN_POINT('Ctrl Pts',(0.0103878585927352,-0.0329142774063509,
0.0794359732427163));
#92226=CARTESIAN_POINT('Ctrl Pts',(0.0103147810920695,-0.0328043479726686,
0.0794666799828973));
#92227=CARTESIAN_POINT('Ctrl Pts',(0.0102410946503782,-0.0326943950436594,
0.0794958646389747));
#92228=CARTESIAN_POINT('Ctrl Pts',(0.010565111337429,-0.0330240426238156,
0.0794467049748362));
#92229=CARTESIAN_POINT('Ctrl Pts',(0.0104921440660714,-0.0329142774063509,
0.0794803366622707));
#92230=CARTESIAN_POINT('Ctrl Pts',(0.0104184451569431,-0.0328043479726686,
0.079512476679005));
#92231=CARTESIAN_POINT('Ctrl Pts',(0.0103441078899177,-0.0326943950436594,
0.0795430812511449));
#92232=CARTESIAN_POINT('Ctrl Pts',(0.0106699880568526,-0.0330240426238156,
0.0794896236154041));
#92233=CARTESIAN_POINT('Ctrl Pts',(0.0105964295394076,-0.0329142774063509,
0.0795247000818251));
#92234=CARTESIAN_POINT('Ctrl Pts',(0.0105221092218167,-0.0328043479726686,
0.0795582733751128));
#92235=CARTESIAN_POINT('Ctrl Pts',(0.0104471211294572,-0.0326943950436594,
0.0795902978633152));
#92236=CARTESIAN_POINT('Ctrl Pts',(0.0107748647762762,-0.0330240426238156,
0.079532542255972));
#92237=CARTESIAN_POINT('Ctrl Pts',(0.0107007150127437,-0.0329142774063509,
0.0795690635013796));
#92238=CARTESIAN_POINT('Ctrl Pts',(0.0106257732866902,-0.0328043479726686,
0.0796040700712205));
#92239=CARTESIAN_POINT('Ctrl Pts',(0.0105501343689966,-0.0326943950436594,
0.0796375144754854));
#92240=CARTESIAN_POINT('Origin',(0.0125018286955665,-0.0391228853390791,
0.0854067014330336));
#92241=CARTESIAN_POINT('Ctrl Pts',(0.0123565016694387,-0.0352722978779621,
0.0780446438062154));
#92242=CARTESIAN_POINT('Ctrl Pts',(0.0123434509783258,-0.0352466642097234,
0.0780583102666033));
#92243=CARTESIAN_POINT('Ctrl Pts',(0.0123304686144099,-0.0352210183808309,
0.0780720186975263));
#92244=CARTESIAN_POINT('Ctrl Pts',(0.0123175545062067,-0.0351953608940152,
0.0780857699489101));
#92245=CARTESIAN_POINT('Origin',(0.0157726898688784,-0.0352456003065063,
0.0815573922146694));
#92246=CARTESIAN_POINT('Ctrl Pts',(0.0122302082862127,-0.035024121149334,
0.0781747415919819));
#92247=CARTESIAN_POINT('Ctrl Pts',(0.0121747691234912,-0.0349144232867422,
0.0782313059251637));
#92248=CARTESIAN_POINT('Ctrl Pts',(0.0121181275526273,-0.0348045283677513,
0.0782867581477673));
#92249=CARTESIAN_POINT('Ctrl Pts',(0.0120603534811807,-0.0346945769586887,
0.0783410245327702));
#92250=CARTESIAN_POINT('Ctrl Pts',(0.0123435196248492,-0.035024121149334,
0.0781760386424488));
#92251=CARTESIAN_POINT('Ctrl Pts',(0.0122880625957901,-0.0349144232867422,
0.0782341637927904));
#92252=CARTESIAN_POINT('Ctrl Pts',(0.0122313708846903,-0.0348045283677513,
0.0782911773974682));
#92253=CARTESIAN_POINT('Ctrl Pts',(0.0121735143889105,-0.0346945769586887,
0.0783470037271379));
#92254=CARTESIAN_POINT('Ctrl Pts',(0.0124568309634857,-0.035024121149334,
0.0781773356929156));
#92255=CARTESIAN_POINT('Ctrl Pts',(0.0124013560680891,-0.0349144232867422,
0.0782370216604171));
#92256=CARTESIAN_POINT('Ctrl Pts',(0.0123446142167533,-0.0348045283677513,
0.0782955966471692));
#92257=CARTESIAN_POINT('Ctrl Pts',(0.0122866752966402,-0.0346945769586887,
0.0783529829215056));
#92258=CARTESIAN_POINT('Ctrl Pts',(0.0125701423021222,-0.035024121149334,
0.0781786327433825));
#92259=CARTESIAN_POINT('Ctrl Pts',(0.012514649540388,-0.0349144232867422,
0.0782398795280439));
#92260=CARTESIAN_POINT('Ctrl Pts',(0.0124578575488162,-0.0348045283677513,
0.0783000158968701));
#92261=CARTESIAN_POINT('Ctrl Pts',(0.01239983620437,-0.0346945769586887,
0.0783589621158733));
#92262=CARTESIAN_POINT('Origin',(0.000698110229997924,-0.0345629067942725,
0.0659813167131262));
#92263=CARTESIAN_POINT('Ctrl Pts',(0.0121463145442708,-0.0351970973651605,
0.0785082972892153));
#92264=CARTESIAN_POINT('Ctrl Pts',(0.0120859362418675,-0.0350869349321769,
0.0785640240234439));
#92265=CARTESIAN_POINT('Ctrl Pts',(0.0120243493948586,-0.0349764985129726,
0.0786185416896035));
#92266=CARTESIAN_POINT('Ctrl Pts',(0.011961629633163,-0.0348659306849652,
0.0786717749616932));
#92267=CARTESIAN_POINT('Ctrl Pts',(0.012145468537714,-0.0351970973651605,
0.0784260795604525));
#92268=CARTESIAN_POINT('Ctrl Pts',(0.012086229250518,-0.0350869349321769,
0.0784817945744068));
#92269=CARTESIAN_POINT('Ctrl Pts',(0.0120257826059213,-0.0349764985129726,
0.0785363241900781));
#92270=CARTESIAN_POINT('Ctrl Pts',(0.0119642027557658,-0.0348659306849652,
0.0785895931529392));
#92271=CARTESIAN_POINT('Ctrl Pts',(0.0121446225311572,-0.0351970973651605,
0.0783438618316897));
#92272=CARTESIAN_POINT('Ctrl Pts',(0.0120865222591685,-0.0350869349321769,
0.0783995651253697));
#92273=CARTESIAN_POINT('Ctrl Pts',(0.0120272158169839,-0.0349764985129726,
0.0784541066905527));
#92274=CARTESIAN_POINT('Ctrl Pts',(0.0119667758783686,-0.0348659306849652,
0.0785074113441852));
#92275=CARTESIAN_POINT('Ctrl Pts',(0.0121437765246004,-0.0351970973651605,
0.0782616441029269));
#92276=CARTESIAN_POINT('Ctrl Pts',(0.0120868152678189,-0.0350869349321769,
0.0783173356763326));
#92277=CARTESIAN_POINT('Ctrl Pts',(0.0120286490280466,-0.0349764985129726,
0.0783718891910273));
#92278=CARTESIAN_POINT('Ctrl Pts',(0.0119693490009714,-0.0348659306849652,
0.0784252295354313));
#92279=CARTESIAN_POINT('Origin',(0.00108299337951375,-0.0345637187966319,
0.0656928893953538));
#92280=CARTESIAN_POINT('Ctrl Pts',(0.0121685208140405,-0.0352450361861253,
0.0782387913236483));
#92281=CARTESIAN_POINT('Ctrl Pts',(0.0120143095227472,-0.0349452761023765,
0.0783913411400379));
#92282=CARTESIAN_POINT('Ctrl Pts',(0.0118490456534183,-0.0346444289983475,
0.0785318417533363));
#92283=CARTESIAN_POINT('Ctrl Pts',(0.0123423891770701,-0.0352450361861253,
0.0780591533757158));
#92284=CARTESIAN_POINT('Ctrl Pts',(0.012194953041984,-0.0349452761023765,
0.0782182607448527));
#92285=CARTESIAN_POINT('Ctrl Pts',(0.0120359511396659,-0.0346444289983475,
0.0783658106140565));
#92286=CARTESIAN_POINT('Ctrl Pts',(0.0119693903360891,-0.0345231616327822,
0.0784246437013716));
#92287=CARTESIAN_POINT('Ctrl Pts',(0.011910470390883,-0.0344132092796975,
0.0784776499954391));
#92288=CARTESIAN_POINT('Ctrl Pts',(0.0118504570922933,-0.0343032738558974,
0.0785294348420343));
#92289=CARTESIAN_POINT('Ctrl Pts',(0.0117894290236758,-0.0341934961088741,
0.0785799338681956));
#92290=CARTESIAN_POINT('Ctrl Pts',(0.0120823966146316,-0.0345231616327822,
0.0784330530502766));
#92291=CARTESIAN_POINT('Ctrl Pts',(0.0120233607583902,-0.0344132092796975,
0.0784876169767936));
#92292=CARTESIAN_POINT('Ctrl Pts',(0.0119631993363471,-0.0343032738558974,
0.0785409569779434));
#92293=CARTESIAN_POINT('Ctrl Pts',(0.0119019911726559,-0.0341934961088741,
0.0785930066932924));
#92294=CARTESIAN_POINT('Ctrl Pts',(0.012195402893174,-0.0345231616327822,
0.0784414623991816));
#92295=CARTESIAN_POINT('Ctrl Pts',(0.0121362511258975,-0.0344132092796975,
0.0784975839581482));
#92296=CARTESIAN_POINT('Ctrl Pts',(0.012075941580401,-0.0343032738558974,
0.0785524791138525));
#92297=CARTESIAN_POINT('Ctrl Pts',(0.0120145533216359,-0.0341934961088741,
0.0786060795183893));
#92298=CARTESIAN_POINT('Ctrl Pts',(0.0123084091717165,-0.0345231616327822,
0.0784498717480865));
#92299=CARTESIAN_POINT('Ctrl Pts',(0.0122491414934047,-0.0344132092796975,
0.0785075509395027));
#92300=CARTESIAN_POINT('Ctrl Pts',(0.0121886838244549,-0.0343032738558974,
0.0785640012497616));
#92301=CARTESIAN_POINT('Ctrl Pts',(0.012127115470616,-0.0341934961088741,
0.0786191523434861));
#92302=CARTESIAN_POINT('Origin',(0.000689785054019144,-0.0345625596229105,
0.0659725309447745));
#92303=CARTESIAN_POINT('Ctrl Pts',(0.0118586900372337,-0.0346945769586886,
0.0788457920946348));
#92304=CARTESIAN_POINT('Ctrl Pts',(0.0117939796488334,-0.0345846629178476,
0.0788972610124152));
#92305=CARTESIAN_POINT('Ctrl Pts',(0.0117281938516594,-0.0344746925055161,
0.0789474005369592));
#92306=CARTESIAN_POINT('Ctrl Pts',(0.0116614172033764,-0.0343648066260528,
0.0789961467718455));
#92307=CARTESIAN_POINT('Ctrl Pts',(0.0118646692268936,-0.0346945769586886,
0.078732631276002));
#92308=CARTESIAN_POINT('Ctrl Pts',(0.0118015182517676,-0.0345846629178476,
0.0787841825900379));
#92309=CARTESIAN_POINT('Ctrl Pts',(0.0117372904302988,-0.0344746925055161,
0.0788344367729368));
#92310=CARTESIAN_POINT('Ctrl Pts',(0.0116720683245006,-0.0343648066260528,
0.07888332977312));
#92311=CARTESIAN_POINT('Ctrl Pts',(0.0118706484165536,-0.0346945769586886,
0.0786194704573692));
#92312=CARTESIAN_POINT('Ctrl Pts',(0.0118090568547018,-0.0345846629178476,
0.0786711041676606));
#92313=CARTESIAN_POINT('Ctrl Pts',(0.0117463870089381,-0.0344746925055161,
0.0787214730089145));
#92314=CARTESIAN_POINT('Ctrl Pts',(0.0116827194456247,-0.0343648066260528,
0.0787705127743945));
#92315=CARTESIAN_POINT('Ctrl Pts',(0.0118766276062136,-0.0346945769586886,
0.0785063096387363));
#92316=CARTESIAN_POINT('Ctrl Pts',(0.011816595457636,-0.0345846629178476,
0.0785580257452832));
#92317=CARTESIAN_POINT('Ctrl Pts',(0.0117554835875775,-0.034474692505516,
0.0786085092448922));
#92318=CARTESIAN_POINT('Ctrl Pts',(0.0116933705667488,-0.0343648066260528,
0.0786576957756689));
#92319=CARTESIAN_POINT('Origin',(0.00104501336031176,-0.0345626446730462,
0.0656484861437726));
#92320=CARTESIAN_POINT('Ctrl Pts',(0.0118765206184609,-0.0346945769586885,
0.0785083344652383));
#92321=CARTESIAN_POINT('Ctrl Pts',(0.011785233558106,-0.0345275153362891,
0.0785869370740706));
#92322=CARTESIAN_POINT('Ctrl Pts',(0.0116914509065426,-0.0343603235965159,
0.0786626891195394));
#92323=CARTESIAN_POINT('Ctrl Pts',(0.0115954533610552,-0.034193496108874,
0.0787353706831235));
#92324=CARTESIAN_POINT('Ctrl Pts',(0.0119388449890012,-0.0346945769586885,
0.078452265746972));
#92325=CARTESIAN_POINT('Ctrl Pts',(0.0118487323103991,-0.0345275153362891,
0.0785321737646985));
#92326=CARTESIAN_POINT('Ctrl Pts',(0.0117560832904355,-0.0343603235965159,
0.0786092684899324));
#92327=CARTESIAN_POINT('Ctrl Pts',(0.0116611753326362,-0.034193496108874,
0.0786833259832705));
#92328=CARTESIAN_POINT('Ctrl Pts',(0.0120011693595415,-0.0346945769586885,
0.0783961970287057));
#92329=CARTESIAN_POINT('Ctrl Pts',(0.0119122310626921,-0.0345275153362891,
0.0784774104553265));
#92330=CARTESIAN_POINT('Ctrl Pts',(0.0118207156743284,-0.0343603235965159,
0.0785558478603254));
#92331=CARTESIAN_POINT('Ctrl Pts',(0.0117268973042172,-0.034193496108874,
0.0786312812834176));
#92332=CARTESIAN_POINT('Ctrl Pts',(0.0120634937300818,-0.0346945769586885,
0.0783401283104393));
#92333=CARTESIAN_POINT('Ctrl Pts',(0.0119757298149852,-0.0345275153362891,
0.0784226471459544));
#92334=CARTESIAN_POINT('Ctrl Pts',(0.0118853480582213,-0.0343603235965159,
0.0785024272307183));
#92335=CARTESIAN_POINT('Ctrl Pts',(0.0117926192757981,-0.034193496108874,
0.0785792365835646));
#92336=CARTESIAN_POINT('Ctrl Pts',(0.0116933949579953,-0.0340223579322365,
0.0786576757501994));
#92337=CARTESIAN_POINT('Ctrl Pts',(0.0116312223528886,-0.0339125849573552,
0.0787069100201677));
#92338=CARTESIAN_POINT('Ctrl Pts',(0.011568074400768,-0.0338030433565217,
0.0787548228653281));
#92339=CARTESIAN_POINT('Ctrl Pts',(0.0115040372887651,-0.033693872113232,
0.0788013601718708));
#92340=CARTESIAN_POINT('Ctrl Pts',(0.0118056504105315,-0.0340223579322365,
0.0786731642364631));
#92341=CARTESIAN_POINT('Ctrl Pts',(0.0117432641788035,-0.0339125849573552,
0.0787239468018964));
#92342=CARTESIAN_POINT('Ctrl Pts',(0.0116798707040562,-0.0338030433565217,
0.0787734024329777));
#92343=CARTESIAN_POINT('Ctrl Pts',(0.0116155566622982,-0.033693872113232,
0.0788214750707676));
#92344=CARTESIAN_POINT('Ctrl Pts',(0.0119179058630677,-0.0340223579322365,
0.0786886527227268));
#92345=CARTESIAN_POINT('Ctrl Pts',(0.0118553060047185,-0.0339125849573552,
0.078740983583625));
#92346=CARTESIAN_POINT('Ctrl Pts',(0.0117916670073445,-0.0338030433565217,
0.0787919820006274));
#92347=CARTESIAN_POINT('Ctrl Pts',(0.0117270760358313,-0.033693872113232,
0.0788415899696644));
#92348=CARTESIAN_POINT('Ctrl Pts',(0.0120301613156039,-0.0340223579322365,
0.0787041412089905));
#92349=CARTESIAN_POINT('Ctrl Pts',(0.0119673478306335,-0.0339125849573552,
0.0787580203653537));
#92350=CARTESIAN_POINT('Ctrl Pts',(0.0119034633106328,-0.0338030433565217,
0.0788105615682771));
#92351=CARTESIAN_POINT('Ctrl Pts',(0.0118385954093644,-0.033693872113232,
0.0788617048685612));
#92352=CARTESIAN_POINT('Origin',(0.000768716151143632,-0.0345589643415323,
0.0660632103798417));
#92353=CARTESIAN_POINT('Ctrl Pts',(0.0115564688245381,-0.034193496108874,
0.079071042825514));
#92354=CARTESIAN_POINT('Ctrl Pts',(0.0114886105581001,-0.0340836138581107,
0.079118377541405));
#92355=CARTESIAN_POINT('Ctrl Pts',(0.0114198053587104,-0.03397388966435,
0.0791642853607716));
#92356=CARTESIAN_POINT('Ctrl Pts',(0.0113501452272528,-0.0338644633294063,
0.0792087134305122));
#92357=CARTESIAN_POINT('Ctrl Pts',(0.0115695416613978,-0.034193496108874,
0.0789584805752507));
#92358=CARTESIAN_POINT('Ctrl Pts',(0.0115032355617342,-0.0340836138581107,
0.0790059955578207));
#92359=CARTESIAN_POINT('Ctrl Pts',(0.0114359780541195,-0.03397388966435,
0.0790521156762053));
#92360=CARTESIAN_POINT('Ctrl Pts',(0.0113678591767975,-0.0338644633294063,
0.0790967876728002));
#92361=CARTESIAN_POINT('Ctrl Pts',(0.0115826144982575,-0.034193496108874,
0.0788459183249875));
#92362=CARTESIAN_POINT('Ctrl Pts',(0.0115178605653684,-0.0340836138581107,
0.0788936135742363));
#92363=CARTESIAN_POINT('Ctrl Pts',(0.0114521507495286,-0.03397388966435,
0.078939945991639));
#92364=CARTESIAN_POINT('Ctrl Pts',(0.0113855731263423,-0.0338644633294063,
0.0789848619150882));
#92365=CARTESIAN_POINT('Ctrl Pts',(0.0115956873351173,-0.034193496108874,
0.0787333560747242));
#92366=CARTESIAN_POINT('Ctrl Pts',(0.0115324855690025,-0.0340836138581107,
0.078781231590652));
#92367=CARTESIAN_POINT('Ctrl Pts',(0.0114683234449377,-0.03397388966435,
0.0788277763070727));
#92368=CARTESIAN_POINT('Ctrl Pts',(0.011403287075887,-0.0338644633294063,
0.0788729361573761));
#92369=CARTESIAN_POINT('Origin',(0.00109229845921002,-0.0345610621864549,
0.0657070580230232));
#92370=CARTESIAN_POINT('Ctrl Pts',(0.0116242276917907,-0.0342436276873901,
0.0787134423750888));
#92371=CARTESIAN_POINT('Ctrl Pts',(0.0114521146252978,-0.0339430054201861,
0.0788454638534707));
#92372=CARTESIAN_POINT('Ctrl Pts',(0.0112705461152906,-0.0336441434784162,
0.0789641460112935));
#92373=CARTESIAN_POINT('Ctrl Pts',(0.0118192375205629,-0.0342436276873901,
0.0785570097484337));
#92374=CARTESIAN_POINT('Ctrl Pts',(0.0116530244078461,-0.0339430054201861,
0.0786963861437548));
#92375=CARTESIAN_POINT('Ctrl Pts',(0.0114767850879853,-0.0336441434784162,
0.0788228467326618));
#92376=CARTESIAN_POINT('Ctrl Pts',(0.0114033097818316,-0.0335235895815127,
0.0788729202367046));
#92377=CARTESIAN_POINT('Ctrl Pts',(0.0113382894862,-0.0334144449262718,
0.0789180693907584));
#92378=CARTESIAN_POINT('Ctrl Pts',(0.011272261742582,-0.0333049234473132,
0.0789619271453457));
#92379=CARTESIAN_POINT('Ctrl Pts',(0.0112053059001663,-0.0331951640388588,
0.0790044297719002));
#92380=CARTESIAN_POINT('Ctrl Pts',(0.0115143711517532,-0.0335235895815127,
0.0788954267823756));
#92381=CARTESIAN_POINT('Ctrl Pts',(0.0114490410092091,-0.0334144449262718,
0.0789421049148461));
#92382=CARTESIAN_POINT('Ctrl Pts',(0.0113826714751586,-0.0333049234473132,
0.078987487003257));
#92383=CARTESIAN_POINT('Ctrl Pts',(0.0113153421592727,-0.0331951640388588,
0.0790315073302976));
#92384=CARTESIAN_POINT('Ctrl Pts',(0.0116254325216747,-0.0335235895815127,
0.0789179333280467));
#92385=CARTESIAN_POINT('Ctrl Pts',(0.0115597925322182,-0.0334144449262718,
0.0789661404389338));
#92386=CARTESIAN_POINT('Ctrl Pts',(0.0114930812077352,-0.0333049234473132,
0.0790130468611683));
#92387=CARTESIAN_POINT('Ctrl Pts',(0.011425378418379,-0.0331951640388588,
0.079058584888695));
#92388=CARTESIAN_POINT('Ctrl Pts',(0.0117364938915962,-0.0335235895815127,
0.0789404398737177));
#92389=CARTESIAN_POINT('Ctrl Pts',(0.0116705440552272,-0.0334144449262718,
0.0789901759630215));
#92390=CARTESIAN_POINT('Ctrl Pts',(0.0116034909403119,-0.0333049234473132,
0.0790386067190796));
#92391=CARTESIAN_POINT('Ctrl Pts',(0.0115354146774854,-0.0331951640388588,
0.0790856624470924));
#92392=CARTESIAN_POINT('Origin',(0.00292490351896382,-0.032643457177084,
0.0645397909075513));
#92393=CARTESIAN_POINT('Ctrl Pts',(0.011240340458136,-0.0336938721132453,
0.0792788678200312));
#92394=CARTESIAN_POINT('Ctrl Pts',(0.0112103194928445,-0.0336474569764989,
0.0792971100697413));
#92395=CARTESIAN_POINT('Ctrl Pts',(0.0111800870360433,-0.033601104548885,
0.0793149996361777));
#92396=CARTESIAN_POINT('Ctrl Pts',(0.0111035454096023,-0.0334837508643202,
0.0793602919033715));
#92397=CARTESIAN_POINT('Ctrl Pts',(0.0110256952908741,-0.0333660264760487,
0.0794032961945505));
#92398=CARTESIAN_POINT('Ctrl Pts',(0.0113006850036129,-0.0336938721132453,
0.0789443105377739));
#92399=CARTESIAN_POINT('Ctrl Pts',(0.0112726223131125,-0.0336474569764989,
0.0789629060041331));
#92400=CARTESIAN_POINT('Ctrl Pts',(0.0112443438620732,-0.033601104548885,
0.078981171687095));
#92401=CARTESIAN_POINT('Ctrl Pts',(0.011172749328754,-0.0334837508643202,
0.0790274161948155));
#92402=CARTESIAN_POINT('Ctrl Pts',(0.0110998159138892,-0.0333660264760487,
0.0790715189009874));
#92403=CARTESIAN_POINT('Ctrl Pts',(0.0113006850036153,-0.0336938721132426,
0.0789443105377889));
#92404=CARTESIAN_POINT('Ctrl Pts',(0.0112726223131186,-0.0336474569765026,
0.0789629060041457));
#92405=CARTESIAN_POINT('Ctrl Pts',(0.0112443438620832,-0.0336011045488949,
0.078981171687105));
#92406=CARTESIAN_POINT('Ctrl Pts',(0.0111733456137093,-0.0334847282606778,
0.0790270310410649));
#92407=CARTESIAN_POINT('Ctrl Pts',(0.0111010304307386,-0.0333679869945434,
0.0790707842801414));
#92408=CARTESIAN_POINT('Ctrl Pts',(0.0113006850036114,-0.0336938721132429,
0.0789443105377748));
#92409=CARTESIAN_POINT('Ctrl Pts',(0.0112003204034131,-0.0335278710435085,
0.0790108161547833));
#92410=CARTESIAN_POINT('Ctrl Pts',(0.0110979055123899,-0.0333620469224321,
0.0790741509675024));
#92411=CARTESIAN_POINT('Ctrl Pts',(0.0109933788621521,-0.0331951640388602,
0.0791343294390534));
#92412=CARTESIAN_POINT('Ctrl Pts',(0.011369545208946,-0.0336938721132429,
0.0788964952479131));
#92413=CARTESIAN_POINT('Ctrl Pts',(0.0112701815790462,-0.0335278710435085,
0.0789644423916903));
#92414=CARTESIAN_POINT('Ctrl Pts',(0.0111687221002778,-0.0333620469224321,
0.0790292496142208));
#92415=CARTESIAN_POINT('Ctrl Pts',(0.0110651055344929,-0.0331951640388602,
0.0790909322698118));
#92416=CARTESIAN_POINT('Ctrl Pts',(0.0114384054142805,-0.0336938721132429,
0.0788486799580514));
#92417=CARTESIAN_POINT('Ctrl Pts',(0.0113400427546793,-0.0335278710435085,
0.0789180686285973));
#92418=CARTESIAN_POINT('Ctrl Pts',(0.0112395386881658,-0.0333620469224321,
0.0789843482609392));
#92419=CARTESIAN_POINT('Ctrl Pts',(0.0111368322068337,-0.0331951640388602,
0.0790475351005702));
#92420=CARTESIAN_POINT('Ctrl Pts',(0.011507265619615,-0.0336938721132429,
0.0788008646681897));
#92421=CARTESIAN_POINT('Ctrl Pts',(0.0114099039303124,-0.0335278710435085,
0.0788716948655044));
#92422=CARTESIAN_POINT('Ctrl Pts',(0.0113103552760537,-0.0333620469224321,
0.0789394469076575));
#92423=CARTESIAN_POINT('Ctrl Pts',(0.0112085588791746,-0.0331951640388602,
0.0790041379313286));
#92424=CARTESIAN_POINT('Ctrl Pts',(0.0102248110767327,-0.0321934096636183,
0.0797701136670266));
#92425=CARTESIAN_POINT('Ctrl Pts',(0.0101473053292143,-0.0320835708272304,
0.0797990884927741));
#92426=CARTESIAN_POINT('Ctrl Pts',(0.0100692449056664,-0.0319739230346346,
0.0798264425345285));
#92427=CARTESIAN_POINT('Ctrl Pts',(0.00999073236495321,-0.0318646057455576,
0.0798521484596572));
#92428=CARTESIAN_POINT('Ctrl Pts',(0.0102654663084347,-0.0321934096636183,
0.0796643388264415));
#92429=CARTESIAN_POINT('Ctrl Pts',(0.0101894192784039,-0.0320835708272304,
0.0796938743195189));
#92430=CARTESIAN_POINT('Ctrl Pts',(0.0101128051232469,-0.0319739230346346,
0.079721818891476));
#92431=CARTESIAN_POINT('Ctrl Pts',(0.0100357246094136,-0.0318646057455576,
0.0797481443121247));
#92432=CARTESIAN_POINT('Ctrl Pts',(0.0103061215401367,-0.0321934096636183,
0.0795585639858563));
#92433=CARTESIAN_POINT('Ctrl Pts',(0.0102315332275934,-0.0320835708272304,
0.0795886601462637));
#92434=CARTESIAN_POINT('Ctrl Pts',(0.0101563653408273,-0.0319739230346346,
0.0796171952484235));
#92435=CARTESIAN_POINT('Ctrl Pts',(0.0100807168538739,-0.0318646057455576,
0.0796441401645921));
#92436=CARTESIAN_POINT('Ctrl Pts',(0.0103467767718387,-0.0321934096636183,
0.0794527891452712));
#92437=CARTESIAN_POINT('Ctrl Pts',(0.010273647176783,-0.0320835708272304,
0.0794834459730085));
#92438=CARTESIAN_POINT('Ctrl Pts',(0.0101999255584078,-0.0319739230346346,
0.079512571605371));
#92439=CARTESIAN_POINT('Ctrl Pts',(0.0101257090983343,-0.0318646057455576,
0.0795401360170596));
#92440=CARTESIAN_POINT('Origin',(0.00332673899329973,-0.0326371942644191,
0.0642906726208783));
#92441=CARTESIAN_POINT('Ctrl Pts',(0.0103741962697567,-0.0322357242816073,
0.0794428028003719));
#92442=CARTESIAN_POINT('Ctrl Pts',(0.0102056273650785,-0.0319819883628705,
0.079514475570033));
#92443=CARTESIAN_POINT('Ctrl Pts',(0.0100328393428316,-0.0317295851069886,
0.0795752765642952));
#92444=CARTESIAN_POINT('Ctrl Pts',(0.0106020833880755,-0.0322357242816073,
0.0793400046422932));
#92445=CARTESIAN_POINT('Ctrl Pts',(0.0104367884714078,-0.0319819883628705,
0.0794189353211141));
#92446=CARTESIAN_POINT('Ctrl Pts',(0.0102668059605056,-0.0317295851069886,
0.0794871878487057));
#92447=CARTESIAN_POINT('Origin',(0.00292333812954877,-0.0326352985530547,
0.0645492556096483));
#92448=CARTESIAN_POINT('Ctrl Pts',(0.01046097262896,-0.032021883458232,
0.0794043637737633));
#92449=CARTESIAN_POINT('Ctrl Pts',(0.0104062874044174,-0.0319391099350606,
0.0794286882760792));
#92450=CARTESIAN_POINT('Ctrl Pts',(0.0103512554817486,-0.0318564869454878,
0.0794521441233481));
#92451=CARTESIAN_POINT('Ctrl Pts',(0.0102959185393638,-0.0317740741446461,
0.0794747179731653));
#92452=CARTESIAN_POINT('Ctrl Pts',(0.0105068452804265,-0.032021883458232,
0.079423139499984));
#92453=CARTESIAN_POINT('Ctrl Pts',(0.010451964645964,-0.0319391099350606,
0.0794479414257052));
#92454=CARTESIAN_POINT('Ctrl Pts',(0.0103967299767358,-0.0318564869454878,
0.0794718713557675));
#92455=CARTESIAN_POINT('Ctrl Pts',(0.0103411831310627,-0.0317740741446461,
0.0794949156162459));
#92456=CARTESIAN_POINT('Ctrl Pts',(0.0105527179318931,-0.032021883458232,
0.0794419152262047));
#92457=CARTESIAN_POINT('Ctrl Pts',(0.0104976418875106,-0.0319391099350606,
0.0794671945753313));
#92458=CARTESIAN_POINT('Ctrl Pts',(0.010442204471723,-0.0318564869454878,
0.0794915985881868));
#92459=CARTESIAN_POINT('Ctrl Pts',(0.0103864477227617,-0.0317740741446461,
0.0795151132593266));
#92460=CARTESIAN_POINT('Ctrl Pts',(0.0105985905833596,-0.032021883458232,
0.0794606909524254));
#92461=CARTESIAN_POINT('Ctrl Pts',(0.0105433191290573,-0.0319391099350606,
0.0794864477249573));
#92462=CARTESIAN_POINT('Ctrl Pts',(0.0104876789667102,-0.0318564869454878,
0.0795113258206062));
#92463=CARTESIAN_POINT('Ctrl Pts',(0.0104317123144606,-0.0317740741446461,
0.0795353109024072));
#92464=CARTESIAN_POINT('Ctrl Pts',(0.0111002850225003,-0.0330240426238156,
0.0790695235223111));
#92465=CARTESIAN_POINT('Ctrl Pts',(0.0110325137931213,-0.0329142774063509,
0.0791105277486519));
#92466=CARTESIAN_POINT('Ctrl Pts',(0.0109638611054147,-0.0328043479726686,
0.0791501513964742));
#92467=CARTESIAN_POINT('Ctrl Pts',(0.0108944135106418,-0.0326943950436594,
0.0791883412828284));
#92468=CARTESIAN_POINT('Ctrl Pts',(0.0112097138896685,-0.0330240426238156,
0.079098959198208));
#92469=CARTESIAN_POINT('Ctrl Pts',(0.0111415371551763,-0.0329142774063509,
0.0791414709138054));
#92470=CARTESIAN_POINT('Ctrl Pts',(0.0110724475961834,-0.0328043479726686,
0.0791825944194992));
#92471=CARTESIAN_POINT('Ctrl Pts',(0.0110025322707001,-0.0326943950436594,
0.0792222745954973));
#92472=CARTESIAN_POINT('Ctrl Pts',(0.0113191427568367,-0.0330240426238156,
0.0791283948741049));
#92473=CARTESIAN_POINT('Ctrl Pts',(0.0112505605172312,-0.0329142774063509,
0.0791724140789589));
#92474=CARTESIAN_POINT('Ctrl Pts',(0.0111810340869521,-0.0328043479726686,
0.0792150374425243));
#92475=CARTESIAN_POINT('Ctrl Pts',(0.0111106510307583,-0.0326943950436594,
0.0792562079081662));
#92476=CARTESIAN_POINT('Ctrl Pts',(0.0114285716240049,-0.0330240426238156,
0.0791578305500018));
#92477=CARTESIAN_POINT('Ctrl Pts',(0.0113595838792861,-0.0329142774063509,
0.0792033572441124));
#92478=CARTESIAN_POINT('Ctrl Pts',(0.0112896205777207,-0.0328043479726686,
0.0792474804655494));
#92479=CARTESIAN_POINT('Ctrl Pts',(0.0112187697908166,-0.0326943950436594,
0.0792901412208352));
#92480=CARTESIAN_POINT('Origin',(0.00286364172159143,-0.032639668285722,
0.0644323553870705));
#92481=CARTESIAN_POINT('Ctrl Pts',(0.0109126308553257,-0.0331951640388587,
0.0794624686483194));
#92482=CARTESIAN_POINT('Ctrl Pts',(0.0108394623467316,-0.0330855618255041,
0.0795008793968466));
#92483=CARTESIAN_POINT('Ctrl Pts',(0.0107654472074681,-0.0329757224427708,
0.0795378055671436));
#92484=CARTESIAN_POINT('Ctrl Pts',(0.0106906778988787,-0.0328657862078596,
0.0795731952238349));
#92485=CARTESIAN_POINT('Ctrl Pts',(0.0109397083921659,-0.0331951640388587,
0.079352432476816));
#92486=CARTESIAN_POINT('Ctrl Pts',(0.010868055409233,-0.0330855618255041,
0.0793912161636357));
#92487=CARTESIAN_POINT('Ctrl Pts',(0.0107955491801548,-0.0329757224427708,
0.0794285468643961));
#92488=CARTESIAN_POINT('Ctrl Pts',(0.0107222802086147,-0.0328657862078596,
0.079464372220477));
#92489=CARTESIAN_POINT('Ctrl Pts',(0.0109667859290061,-0.0331951640388587,
0.0792423963053125));
#92490=CARTESIAN_POINT('Ctrl Pts',(0.0108966484717343,-0.0330855618255041,
0.0792815529304248));
#92491=CARTESIAN_POINT('Ctrl Pts',(0.0108256511528415,-0.0329757224427708,
0.0793192881616486));
#92492=CARTESIAN_POINT('Ctrl Pts',(0.0107538825183506,-0.0328657862078596,
0.0793555492171192));
#92493=CARTESIAN_POINT('Ctrl Pts',(0.0109938634658464,-0.0331951640388587,
0.079132360133809));
#92494=CARTESIAN_POINT('Ctrl Pts',(0.0109252415342356,-0.0330855618255041,
0.0791718896972139));
#92495=CARTESIAN_POINT('Ctrl Pts',(0.0108557531255281,-0.0329757224427708,
0.0792100294589011));
#92496=CARTESIAN_POINT('Ctrl Pts',(0.0107854848280865,-0.0328657862078596,
0.0792467262137613));
#92497=CARTESIAN_POINT('Origin',(0.00330355586658263,-0.0326401908834077,
0.0642380658693673));
#92498=CARTESIAN_POINT('Ctrl Pts',(0.0110246120685592,-0.0332451089994432,
0.0791162169740853));
#92499=CARTESIAN_POINT('Ctrl Pts',(0.0108373081309289,-0.0329451141710258,
0.0792256235628233));
#92500=CARTESIAN_POINT('Ctrl Pts',(0.010642295352496,-0.0326442513127503,
0.0793206108407027));
#92501=CARTESIAN_POINT('Ctrl Pts',(0.0112376920410981,-0.0332451089994432,
0.0789854617627062));
#92502=CARTESIAN_POINT('Ctrl Pts',(0.0110553196169488,-0.0329451141710258,
0.0791029047940915));
#92503=CARTESIAN_POINT('Ctrl Pts',(0.0108646190043741,-0.0326442513127503,
0.0792062771456886));
#92504=CARTESIAN_POINT('Ctrl Pts',(0.0107070916436316,-0.0327445246961877,
0.0792885442766252));
#92505=CARTESIAN_POINT('Ctrl Pts',(0.0105132882800017,-0.0324436878365475,
0.0793859753843197));
#92506=CARTESIAN_POINT('Ctrl Pts',(0.0103126965820868,-0.0321434074463187,
0.079468531639252));
#92507=CARTESIAN_POINT('Ctrl Pts',(0.0109279605404424,-0.0327445246961877,
0.0791714249766719));
#92508=CARTESIAN_POINT('Ctrl Pts',(0.0107385744033761,-0.0324436878365475,
0.0792771862909031));
#92509=CARTESIAN_POINT('Ctrl Pts',(0.0105417599179551,-0.0321434074463187,
0.0793683818106906));
#92510=CARTESIAN_POINT('Origin',(0.00328659600653958,-0.0326395579069779,
0.0642042379962714));
#92511=CARTESIAN_POINT('Origin',(0.00286748906709375,-0.0326393375179411,
0.0644399638664167));
#92512=CARTESIAN_POINT('Ctrl Pts',(0.010573555033132,-0.0326943950436593,
0.0796270989613478));
#92513=CARTESIAN_POINT('Ctrl Pts',(0.0104980703442673,-0.0325844576448127,
0.0796608614224468));
#92514=CARTESIAN_POINT('Ctrl Pts',(0.0104218820501841,-0.0324744968375319,
0.0796930651258431));
#92515=CARTESIAN_POINT('Ctrl Pts',(0.0103450883368848,-0.0323646534831894,
0.0797236701567042));
#92516=CARTESIAN_POINT('Ctrl Pts',(0.0106074883346984,-0.0326943950436593,
0.0795189802366644));
#92517=CARTESIAN_POINT('Ctrl Pts',(0.010533493724496,-0.0325844576448127,
0.0795532103622568));
#92518=CARTESIAN_POINT('Ctrl Pts',(0.0104587859424617,-0.0324744968375319,
0.0795859125805135));
#92519=CARTESIAN_POINT('Ctrl Pts',(0.0103834612864896,-0.0323646534831894,
0.0796170463117117));
#92520=CARTESIAN_POINT('Ctrl Pts',(0.0106414216362648,-0.0326943950436593,
0.0794108615119809));
#92521=CARTESIAN_POINT('Ctrl Pts',(0.0105689171047246,-0.0325844576448127,
0.0794455593020667));
#92522=CARTESIAN_POINT('Ctrl Pts',(0.0104956898347393,-0.0324744968375319,
0.0794787600351839));
#92523=CARTESIAN_POINT('Ctrl Pts',(0.0104218342360944,-0.0323646534831894,
0.0795104224667191));
#92524=CARTESIAN_POINT('Ctrl Pts',(0.0106753549378313,-0.0326943950436593,
0.0793027427872974));
#92525=CARTESIAN_POINT('Ctrl Pts',(0.0106043404849533,-0.0325844576448127,
0.0793379082418766));
#92526=CARTESIAN_POINT('Ctrl Pts',(0.0105325937270169,-0.0324744968375319,
0.0793716074898543));
#92527=CARTESIAN_POINT('Ctrl Pts',(0.0104602071856992,-0.0323646534831894,
0.0794037986217265));
#92528=CARTESIAN_POINT('Ctrl Pts',(0.0107855128689007,-0.0325229783203385,
0.0792467116709563));
#92529=CARTESIAN_POINT('Ctrl Pts',(0.0107152548112531,-0.032413025311208,
0.079283403569446));
#92530=CARTESIAN_POINT('Ctrl Pts',(0.0106442483905759,-0.0323031222247695,
0.0793186365247416));
#92531=CARTESIAN_POINT('Ctrl Pts',(0.0105725861535637,-0.0321934096636184,
0.0793523686154071));
#92532=CARTESIAN_POINT('Ctrl Pts',(0.0108928775554811,-0.0325229783203385,
0.0792829603499048));
#92533=CARTESIAN_POINT('Ctrl Pts',(0.0108221198105961,-0.032413025311208,
0.0793211322682242));
#92534=CARTESIAN_POINT('Ctrl Pts',(0.0107505831623579,-0.0323031222247695,
0.0793578346822033));
#92535=CARTESIAN_POINT('Ctrl Pts',(0.0106783609030641,-0.0321934096636184,
0.0793930238121002));
#92536=CARTESIAN_POINT('Ctrl Pts',(0.0110002422420616,-0.0325229783203385,
0.0793192090288534));
#92537=CARTESIAN_POINT('Ctrl Pts',(0.010928984809939,-0.032413025311208,
0.0793588609670024));
#92538=CARTESIAN_POINT('Ctrl Pts',(0.0108569179341398,-0.0323031222247695,
0.079397032839665));
#92539=CARTESIAN_POINT('Ctrl Pts',(0.0107841356525646,-0.0321934096636184,
0.0794336790087933));
#92540=CARTESIAN_POINT('Ctrl Pts',(0.0111076069286421,-0.0325229783203385,
0.079355457707802));
#92541=CARTESIAN_POINT('Ctrl Pts',(0.011035849809282,-0.032413025311208,
0.0793965896657807));
#92542=CARTESIAN_POINT('Ctrl Pts',(0.0109632527059218,-0.0323031222247695,
0.0794362309971267));
#92543=CARTESIAN_POINT('Ctrl Pts',(0.0108899104020651,-0.0321934096636184,
0.0794743342054863));
#92544=CARTESIAN_POINT('Origin',(0.0138781452811081,-0.0391228853390915,
0.0847692242551965));
#92545=CARTESIAN_POINT('Ctrl Pts',(0.0128112537139296,-0.0352722978779613,
0.077483432957791));
#92546=CARTESIAN_POINT('Ctrl Pts',(0.0128000187930861,-0.0352466642097229,
0.0774986273393741));
#92547=CARTESIAN_POINT('Ctrl Pts',(0.0127888569209621,-0.0352210183808307,
0.0775138547968734));
#92548=CARTESIAN_POINT('Ctrl Pts',(0.012777768133161,-0.0351953608940152,
0.0775291161824723));
#92549=CARTESIAN_POINT('Origin',(0.0166407683657512,-0.0352456003065054,
0.0805403203823156));
#92550=CARTESIAN_POINT('Ctrl Pts',(0.0127022617679223,-0.035024121149334,
0.0776283336417555));
#92551=CARTESIAN_POINT('Ctrl Pts',(0.0126543491503399,-0.0349144232867421,
0.0776914003178052));
#92552=CARTESIAN_POINT('Ctrl Pts',(0.0126051042215475,-0.0348045283677512,
0.0777535143543013));
#92553=CARTESIAN_POINT('Ctrl Pts',(0.0125545870974168,-0.0346945769586886,
0.0778145938438405));
#92554=CARTESIAN_POINT('Ctrl Pts',(0.012814842176338,-0.035024121149334,
0.0776154187881212));
#92555=CARTESIAN_POINT('Ctrl Pts',(0.0127671074555611,-0.0349144232867421,
0.0776800362130671));
#92556=CARTESIAN_POINT('Ctrl Pts',(0.0127180084749677,-0.0348045283677512,
0.0777437056039114));
#92557=CARTESIAN_POINT('Ctrl Pts',(0.0126676050893535,-0.0346945769586886,
0.0778063430679958));
#92558=CARTESIAN_POINT('Ctrl Pts',(0.0129274225847537,-0.035024121149334,
0.0776025039344869));
#92559=CARTESIAN_POINT('Ctrl Pts',(0.0128798657607823,-0.0349144232867421,
0.077668672108329));
#92560=CARTESIAN_POINT('Ctrl Pts',(0.0128309127283878,-0.0348045283677512,
0.0777338968535214));
#92561=CARTESIAN_POINT('Ctrl Pts',(0.0127806230812902,-0.0346945769586886,
0.0777980922921512));
#92562=CARTESIAN_POINT('Ctrl Pts',(0.0130400029931695,-0.035024121149334,
0.0775895890808527));
#92563=CARTESIAN_POINT('Ctrl Pts',(0.0129926240660035,-0.0349144232867421,
0.077657308003591));
#92564=CARTESIAN_POINT('Ctrl Pts',(0.012943816981808,-0.0348045283677512,
0.0777240881031315));
#92565=CARTESIAN_POINT('Ctrl Pts',(0.0128936410732269,-0.0346945769586886,
0.0777898415163066));
#92566=CARTESIAN_POINT('Origin',(-0.000267143618523518,-0.0345629067940785,
0.0669764126992258));
#92567=CARTESIAN_POINT('Ctrl Pts',(0.0126608351673018,-0.0351970973651608,
0.0779697738266411));
#92568=CARTESIAN_POINT('Ctrl Pts',(0.0126079173776439,-0.0350869349321771,
0.078032628546803));
#92569=CARTESIAN_POINT('Ctrl Pts',(0.0125536490367048,-0.0349764985129727,
0.078094435203562));
#92570=CARTESIAN_POINT('Ctrl Pts',(0.0124980957371878,-0.0348659306849652,
0.078155109585943));
#92571=CARTESIAN_POINT('Ctrl Pts',(0.0126496912179573,-0.0351970973651608,
0.0778883104419646));
#92572=CARTESIAN_POINT('Ctrl Pts',(0.0125979019930916,-0.0350869349321771,
0.077951010777811));
#92573=CARTESIAN_POINT('Ctrl Pts',(0.0125447663613991,-0.0349764985129727,
0.0780126863846009));
#92574=CARTESIAN_POINT('Ctrl Pts',(0.0124903484581191,-0.0348659306849652,
0.0780732533075217));
#92575=CARTESIAN_POINT('Ctrl Pts',(0.0126385472686127,-0.0351970973651608,
0.077806847057288));
#92576=CARTESIAN_POINT('Ctrl Pts',(0.0125878866085394,-0.0350869349321771,
0.0778693930088189));
#92577=CARTESIAN_POINT('Ctrl Pts',(0.0125358836860934,-0.0349764985129727,
0.0779309375656399));
#92578=CARTESIAN_POINT('Ctrl Pts',(0.0124826011790504,-0.0348659306849652,
0.0779913970291004));
#92579=CARTESIAN_POINT('Ctrl Pts',(0.0126274033192682,-0.0351970973651608,
0.0777253836726114));
#92580=CARTESIAN_POINT('Ctrl Pts',(0.0125778712239871,-0.0350869349321771,
0.0777877752398269));
#92581=CARTESIAN_POINT('Ctrl Pts',(0.0125270010107877,-0.0349764985129727,
0.0778491887466789));
#92582=CARTESIAN_POINT('Ctrl Pts',(0.0124748538999816,-0.0348659306849652,
0.0779095407506791));
#92583=CARTESIAN_POINT('Origin',(7.85550839694687E-5,-0.0345637187964175,
0.0666420210672609));
#92584=CARTESIAN_POINT('Ctrl Pts',(0.0126490882798721,-0.0352450361861253,
0.0776996098125146));
#92585=CARTESIAN_POINT('Ctrl Pts',(0.0125152125524391,-0.0349452761023765,
0.0778702845278275));
#92586=CARTESIAN_POINT('Ctrl Pts',(0.0123688612342642,-0.0346444289983475,
0.0780303903069589));
#92587=CARTESIAN_POINT('Ctrl Pts',(0.0127990710340421,-0.0352450361861253,
0.0774995968793039));
#92588=CARTESIAN_POINT('Ctrl Pts',(0.0126727389179759,-0.0349452761023765,
0.0776759282868667));
#92589=CARTESIAN_POINT('Ctrl Pts',(0.0125334836953686,-0.0346444289983475,
0.0778422429038412));
#92590=CARTESIAN_POINT('Ctrl Pts',(0.0124748214846824,-0.0345231616327822,
0.0779089543554312));
#92591=CARTESIAN_POINT('Ctrl Pts',(0.0124230095910775,-0.0344132092796975,
0.0779689273062918));
#92592=CARTESIAN_POINT('Ctrl Pts',(0.0123699598775457,-0.0343032738558974,
0.0780278254746732));
#92593=CARTESIAN_POINT('Ctrl Pts',(0.0123157422397181,-0.0341934961088741,
0.078085575146108));
#92594=CARTESIAN_POINT('Ctrl Pts',(0.0125879906458554,-0.0345231616327822,
0.0779031339518055));
#92595=CARTESIAN_POINT('Ctrl Pts',(0.01253625897832,-0.0344132092796975,
0.0779646667802234));
#92596=CARTESIAN_POINT('Ctrl Pts',(0.0124832572218815,-0.0343032738558974,
0.0780251264050927));
#92597=CARTESIAN_POINT('Ctrl Pts',(0.0124290552619737,-0.0341934961088741,
0.0780844371099657));
#92598=CARTESIAN_POINT('Ctrl Pts',(0.0127011598070283,-0.0345231616327822,
0.0778973135481798));
#92599=CARTESIAN_POINT('Ctrl Pts',(0.0126495083655625,-0.0344132092796975,
0.077960406254155));
#92600=CARTESIAN_POINT('Ctrl Pts',(0.0125965545662173,-0.0343032738558974,
0.0780224273355121));
#92601=CARTESIAN_POINT('Ctrl Pts',(0.0125423682842293,-0.0341934961088741,
0.0780832990738234));
#92602=CARTESIAN_POINT('Ctrl Pts',(0.0128143289682013,-0.0345231616327822,
0.0778914931445541));
#92603=CARTESIAN_POINT('Ctrl Pts',(0.012762757752805,-0.0344132092796975,
0.0779561457280867));
#92604=CARTESIAN_POINT('Ctrl Pts',(0.0127098519105532,-0.0343032738558974,
0.0780197282659315));
#92605=CARTESIAN_POINT('Ctrl Pts',(0.0126556813064849,-0.0341934961088741,
0.078082161037681));
#92606=CARTESIAN_POINT('Origin',(-0.000276504297481307,-0.0345625596229775,
0.0669687396303667));
#92607=CARTESIAN_POINT('Ctrl Pts',(0.0124177779806862,-0.0346945769586885,
0.0783406562942356));
#92608=CARTESIAN_POINT('Ctrl Pts',(0.0123600286187926,-0.0345846629176052,
0.0783998297265801));
#92609=CARTESIAN_POINT('Ctrl Pts',(0.0123010457108863,-0.0344746925050311,
0.0784578190328047));
#92610=CARTESIAN_POINT('Ctrl Pts',(0.012240905139525,-0.034364806625326,
0.0785145502224446));
#92611=CARTESIAN_POINT('Ctrl Pts',(0.0124095272113377,-0.0346945769586885,
0.0782276383912827));
#92612=CARTESIAN_POINT('Ctrl Pts',(0.0123533352932715,-0.0345846629176052,
0.0782866981238552));
#92613=CARTESIAN_POINT('Ctrl Pts',(0.0122959124464725,-0.0344746925050311,
0.0783446059181864));
#92614=CARTESIAN_POINT('Ctrl Pts',(0.0122373325541367,-0.034364806625326,
0.0784012878799986));
#92615=CARTESIAN_POINT('Ctrl Pts',(0.0124012764419893,-0.0346945769586885,
0.0781146204883298));
#92616=CARTESIAN_POINT('Ctrl Pts',(0.0123466419677505,-0.0345846629176052,
0.0781735665211304));
#92617=CARTESIAN_POINT('Ctrl Pts',(0.0122907791820586,-0.0344746925050311,
0.0782313928035682));
#92618=CARTESIAN_POINT('Ctrl Pts',(0.0122337599687485,-0.034364806625326,
0.0782880255375526));
#92619=CARTESIAN_POINT('Ctrl Pts',(0.0123930256726408,-0.0346945769586885,
0.0780016025853769));
#92620=CARTESIAN_POINT('Ctrl Pts',(0.0123399486422294,-0.0345846629176052,
0.0780604349184056));
#92621=CARTESIAN_POINT('Ctrl Pts',(0.0122856459176447,-0.0344746925050311,
0.0781181796889499));
#92622=CARTESIAN_POINT('Ctrl Pts',(0.0122301873833602,-0.034364806625326,
0.0781747631951066));
#92623=CARTESIAN_POINT('Origin',(3.5309344467477E-5,-0.0345626446732227,
0.0666027281070317));
#92624=CARTESIAN_POINT('Ctrl Pts',(0.0123931733065714,-0.0346945769586886,
0.078003624854638));
#92625=CARTESIAN_POINT('Ctrl Pts',(0.0123124575910851,-0.0345275153362891,
0.078093048960879));
#92626=CARTESIAN_POINT('Ctrl Pts',(0.0122289086925484,-0.0343603235965159,
0.0781799577618159));
#92627=CARTESIAN_POINT('Ctrl Pts',(0.0121427775317648,-0.034193496108874,
0.0782640978923524));
#92628=CARTESIAN_POINT('Ctrl Pts',(0.0124479789570725,-0.0346945769586886,
0.0779401869400725));
#92629=CARTESIAN_POINT('Ctrl Pts',(0.0123685919741059,-0.0345275153362891,
0.0780307589726062));
#92630=CARTESIAN_POINT('Ctrl Pts',(0.0122863360505419,-0.0343603235965159,
0.0781188577841631));
#92631=CARTESIAN_POINT('Ctrl Pts',(0.0122014583354472,-0.034193496108874,
0.0782042264332884));
#92632=CARTESIAN_POINT('Ctrl Pts',(0.0125027846075736,-0.0346945769586886,
0.0778767490255069));
#92633=CARTESIAN_POINT('Ctrl Pts',(0.0124247263571267,-0.0345275153362891,
0.0779684689843333));
#92634=CARTESIAN_POINT('Ctrl Pts',(0.0123437634085354,-0.0343603235965159,
0.0780577578065103));
#92635=CARTESIAN_POINT('Ctrl Pts',(0.0122601391391296,-0.034193496108874,
0.0781443549742244));
#92636=CARTESIAN_POINT('Ctrl Pts',(0.0125575902580747,-0.0346945769586886,
0.0778133111109414));
#92637=CARTESIAN_POINT('Ctrl Pts',(0.0124808607401475,-0.0345275153362891,
0.0779061789960605));
#92638=CARTESIAN_POINT('Ctrl Pts',(0.0124011907665289,-0.0343603235965159,
0.0779966578288574));
#92639=CARTESIAN_POINT('Ctrl Pts',(0.012318819942812,-0.034193496108874,
0.0780844835151603));
#92640=CARTESIAN_POINT('Ctrl Pts',(0.0122302090727844,-0.0340223579322365,
0.0781747402701359));
#92641=CARTESIAN_POINT('Ctrl Pts',(0.0121746974074964,-0.0339125849573554,
0.078231378606817));
#92642=CARTESIAN_POINT('Ctrl Pts',(0.012118052467653,-0.0338030433565221,
0.0782868281819145));
#92643=CARTESIAN_POINT('Ctrl Pts',(0.0120603529785157,-0.0336938721132328,
0.0783410245062105));
#92644=CARTESIAN_POINT('Ctrl Pts',(0.0123435205796144,-0.0340223579322365,
0.0781760372862076));
#92645=CARTESIAN_POINT('Ctrl Pts',(0.0122879910250921,-0.0339125849573554,
0.0782342384840967));
#92646=CARTESIAN_POINT('Ctrl Pts',(0.0122312958609895,-0.0338030433565221,
0.0782912494519321));
#92647=CARTESIAN_POINT('Ctrl Pts',(0.0121735140538006,-0.0336938721132328,
0.0783470037094314));
#92648=CARTESIAN_POINT('Ctrl Pts',(0.0124568320864445,-0.0340223579322365,
0.0781773343022793));
#92649=CARTESIAN_POINT('Ctrl Pts',(0.0124012846426878,-0.0339125849573554,
0.0782370983613764));
#92650=CARTESIAN_POINT('Ctrl Pts',(0.0123445392543259,-0.0338030433565221,
0.0782956707219498));
#92651=CARTESIAN_POINT('Ctrl Pts',(0.0122866751290855,-0.0336938721132328,
0.0783529829126524));
#92652=CARTESIAN_POINT('Ctrl Pts',(0.0125701435932746,-0.0340223579322365,
0.0781786313183511));
#92653=CARTESIAN_POINT('Ctrl Pts',(0.0125145782602835,-0.0339125849573554,
0.0782399582386561));
#92654=CARTESIAN_POINT('Ctrl Pts',(0.0124577826476623,-0.0338030433565221,
0.0783000919919674));
#92655=CARTESIAN_POINT('Ctrl Pts',(0.0123998362043704,-0.0336938721132328,
0.0783589621158733));
#92656=CARTESIAN_POINT('Origin',(-0.00018683044819935,-0.0345589643413972,
0.0670488113415833));
#92657=CARTESIAN_POINT('Ctrl Pts',(0.0121461712749856,-0.034193496108874,
0.0786020092176615));
#92658=CARTESIAN_POINT('Ctrl Pts',(0.0120847807042492,-0.0340836138581107,
0.0786574755811364));
#92659=CARTESIAN_POINT('Ctrl Pts',(0.0120222718298549,-0.0339738896643499,
0.0787116449817608));
#92660=CARTESIAN_POINT('Ctrl Pts',(0.0119587293029819,-0.0338644633294062,
0.0787644534524276));
#92661=CARTESIAN_POINT('Ctrl Pts',(0.0121450332378193,-0.034193496108874,
0.0784886960934465));
#92662=CARTESIAN_POINT('Ctrl Pts',(0.0120852051879644,-0.0340836138581107,
0.0785441467640628));
#92663=CARTESIAN_POINT('Ctrl Pts',(0.0120242584094556,-0.0339738896643499,
0.0785983328124494));
#92664=CARTESIAN_POINT('Ctrl Pts',(0.0119622755556104,-0.0338644633294062,
0.0786511901161698));
#92665=CARTESIAN_POINT('Ctrl Pts',(0.0121438952006529,-0.034193496108874,
0.0783753829692315));
#92666=CARTESIAN_POINT('Ctrl Pts',(0.0120856296716796,-0.0340836138581107,
0.0784308179469892));
#92667=CARTESIAN_POINT('Ctrl Pts',(0.0120262449890562,-0.0339738896643499,
0.0784850206431379));
#92668=CARTESIAN_POINT('Ctrl Pts',(0.0119658218082389,-0.0338644633294062,
0.0785379267799119));
#92669=CARTESIAN_POINT('Ctrl Pts',(0.0121427571634866,-0.034193496108874,
0.0782620698450165));
#92670=CARTESIAN_POINT('Ctrl Pts',(0.0120860541553949,-0.0340836138581107,
0.0783174891299155));
#92671=CARTESIAN_POINT('Ctrl Pts',(0.0120282315686569,-0.0339738896643499,
0.0783717084738264));
#92672=CARTESIAN_POINT('Ctrl Pts',(0.0119693680608674,-0.0338644633294062,
0.0784246634436541));
#92673=CARTESIAN_POINT('Origin',(8.95625897499976E-5,-0.0345610621864118,
0.0666549117351775));
#92674=CARTESIAN_POINT('Ctrl Pts',(0.0121685766225554,-0.03424362768739,
0.0782387361156615));
#92675=CARTESIAN_POINT('Ctrl Pts',(0.012014367397785,-0.033943005420186,
0.0783912880524157));
#92676=CARTESIAN_POINT('Ctrl Pts',(0.0118491054283175,-0.0336441434784162,
0.0785317909344483));
#92677=CARTESIAN_POINT('Ctrl Pts',(0.0123424425336475,-0.03424362768739,
0.078059095794575));
#92678=CARTESIAN_POINT('Ctrl Pts',(0.0121950085552781,-0.033943005420186,
0.0782182051922669));
#92679=CARTESIAN_POINT('Ctrl Pts',(0.0120360086496206,-0.0336441434784162,
0.0783657572454977));
#92680=CARTESIAN_POINT('Ctrl Pts',(0.0119693885923796,-0.0335235895815127,
0.0784246448027122));
#92681=CARTESIAN_POINT('Ctrl Pts',(0.01191053969067,-0.0334144449262719,
0.0784775871460997));
#92682=CARTESIAN_POINT('Ctrl Pts',(0.0118505294297312,-0.0333049234473133,
0.078529374539805));
#92683=CARTESIAN_POINT('Ctrl Pts',(0.0117894285457527,-0.0331951640388588,
0.0785799338126902));
#92684=CARTESIAN_POINT('Ctrl Pts',(0.012082395028372,-0.0335235895815127,
0.0784330541969319));
#92685=CARTESIAN_POINT('Ctrl Pts',(0.0120234303547943,-0.0334144449262719,
0.0784875522964));
#92686=CARTESIAN_POINT('Ctrl Pts',(0.0119632720482299,-0.0333049234473133,
0.0785408948418015));
#92687=CARTESIAN_POINT('Ctrl Pts',(0.0119019908540405,-0.0331951640388588,
0.0785930066562889));
#92688=CARTESIAN_POINT('Ctrl Pts',(0.0121954014643643,-0.0335235895815127,
0.0784414635911516));
#92689=CARTESIAN_POINT('Ctrl Pts',(0.0121363210189186,-0.0334144449262719,
0.0784975174467003));
#92690=CARTESIAN_POINT('Ctrl Pts',(0.0120760146667286,-0.0333049234473133,
0.078552415143798));
#92691=CARTESIAN_POINT('Ctrl Pts',(0.0120145531623283,-0.0331951640388588,
0.0786060794998875));
#92692=CARTESIAN_POINT('Ctrl Pts',(0.0123084079003567,-0.0335235895815127,
0.0784498729853713));
#92693=CARTESIAN_POINT('Ctrl Pts',(0.012249211683043,-0.0334144449262719,
0.0785074825970005));
#92694=CARTESIAN_POINT('Ctrl Pts',(0.0121887572852272,-0.0333049234473133,
0.0785639354457945));
#92695=CARTESIAN_POINT('Ctrl Pts',(0.0121271154706161,-0.0331951640388588,
0.0786191523434861));
#92696=CARTESIAN_POINT('Origin',(0.0017614196500452,-0.0326434571768189,
0.065267162552053));
#92697=CARTESIAN_POINT('Ctrl Pts',(0.0118585830537535,-0.0336938721132448,
0.0788478168404056));
#92698=CARTESIAN_POINT('Ctrl Pts',(0.0118310851728839,-0.0336474569764987,
0.0788696778691827));
#92699=CARTESIAN_POINT('Ctrl Pts',(0.0118033332652433,-0.033601104548885,
0.0788912155026138));
#92700=CARTESIAN_POINT('Ctrl Pts',(0.0117330718186913,-0.03348375086432,
0.0789457438362969));
#92701=CARTESIAN_POINT('Ctrl Pts',(0.0116612254382725,-0.0333660264760483,
0.0789981662329088));
#92702=CARTESIAN_POINT('Ctrl Pts',(0.0118765206184675,-0.0336938721132448,
0.0785083344652326));
#92703=CARTESIAN_POINT('Ctrl Pts',(0.0118510098405922,-0.0336474569764987,
0.0785303004885282));
#92704=CARTESIAN_POINT('Ctrl Pts',(0.0118252436706948,-0.033601104548885,
0.0785519663708331));
#92705=CARTESIAN_POINT('Ctrl Pts',(0.0117600096553422,-0.03348375086432,
0.0786068194011643));
#92706=CARTESIAN_POINT('Ctrl Pts',(0.0116931788770111,-0.0333660264760483,
0.0786597153250451));
#92707=CARTESIAN_POINT('Ctrl Pts',(0.0118765206184709,-0.0336938721132426,
0.0785083344652483));
#92708=CARTESIAN_POINT('Ctrl Pts',(0.0118510098405988,-0.0336474569765026,
0.0785303004885411));
#92709=CARTESIAN_POINT('Ctrl Pts',(0.0118252436707048,-0.0336011045488949,
0.0785519663708431));
#92710=CARTESIAN_POINT('Ctrl Pts',(0.0117605529658464,-0.0334847282606778,
0.0786063625501455));
#92711=CARTESIAN_POINT('Ctrl Pts',(0.0116942917446253,-0.0333679869945434,
0.078658834277581));
#92712=CARTESIAN_POINT('Ctrl Pts',(0.0118765206184665,-0.0336938721132429,
0.0785083344652336));
#92713=CARTESIAN_POINT('Ctrl Pts',(0.0117852827871481,-0.0335278710435085,
0.0785868946854659));
#92714=CARTESIAN_POINT('Ctrl Pts',(0.0116916134250057,-0.0333620469224321,
0.0786625660737266));
#92715=CARTESIAN_POINT('Ctrl Pts',(0.011595453361056,-0.0331951640388601,
0.0787353706831229));
#92716=CARTESIAN_POINT('Ctrl Pts',(0.0119388449956222,-0.0336938721132429,
0.0784522657410156));
#92717=CARTESIAN_POINT('Ctrl Pts',(0.0118487809128638,-0.0335278710435085,
0.0785321306663034));
#92718=CARTESIAN_POINT('Ctrl Pts',(0.011756243971148,-0.0333620469224321,
0.078609143109077));
#92719=CARTESIAN_POINT('Ctrl Pts',(0.0116611753396131,-0.0331951640388601,
0.0786833259777455));
#92720=CARTESIAN_POINT('Ctrl Pts',(0.012001169372778,-0.0336938721132429,
0.0783961970167977));
#92721=CARTESIAN_POINT('Ctrl Pts',(0.0119122790385795,-0.0335278710435085,
0.0784773666471409));
#92722=CARTESIAN_POINT('Ctrl Pts',(0.0118208745172904,-0.0333620469224321,
0.0785557201444273));
#92723=CARTESIAN_POINT('Ctrl Pts',(0.0117268973181703,-0.0331951640388601,
0.0786312812723682));
#92724=CARTESIAN_POINT('Ctrl Pts',(0.0120634937499337,-0.0336938721132429,
0.0783401282925797));
#92725=CARTESIAN_POINT('Ctrl Pts',(0.0119757771642952,-0.0335278710435085,
0.0784226026279784));
#92726=CARTESIAN_POINT('Ctrl Pts',(0.0118855050634327,-0.0333620469224321,
0.0785022971797777));
#92727=CARTESIAN_POINT('Ctrl Pts',(0.0117926192967274,-0.0331951640388601,
0.0785792365669909));
#92728=CARTESIAN_POINT('Ctrl Pts',(0.0116933941992991,-0.0330240426238155,
0.0786576768856262));
#92729=CARTESIAN_POINT('Ctrl Pts',(0.0116312965585832,-0.0329142774063508,
0.0787068517687157));
#92730=CARTESIAN_POINT('Ctrl Pts',(0.0115681513777318,-0.0328043479726686,
0.078754767435583));
#92731=CARTESIAN_POINT('Ctrl Pts',(0.0115040378599329,-0.0326943950436594,
0.0788013602748927));
#92732=CARTESIAN_POINT('Ctrl Pts',(0.011805649455607,-0.0330240426238155,
0.0786731653786591));
#92733=CARTESIAN_POINT('Ctrl Pts',(0.0117433384458098,-0.0329142774063508,
0.0787238866872692));
#92734=CARTESIAN_POINT('Ctrl Pts',(0.0116799478205698,-0.0328043479726686,
0.0787733451396718));
#92735=CARTESIAN_POINT('Ctrl Pts',(0.0116155570430768,-0.0326943950436594,
0.0788214751394487));
#92736=CARTESIAN_POINT('Ctrl Pts',(0.0119179047119149,-0.0330240426238155,
0.078688653871692));
#92737=CARTESIAN_POINT('Ctrl Pts',(0.0118553803330365,-0.0329142774063509,
0.0787409216058228));
#92738=CARTESIAN_POINT('Ctrl Pts',(0.0117917442634077,-0.0328043479726686,
0.0787919228437605));
#92739=CARTESIAN_POINT('Ctrl Pts',(0.0117270762262207,-0.0326943950436594,
0.0788415900040047));
#92740=CARTESIAN_POINT('Ctrl Pts',(0.0120301599682228,-0.0330240426238155,
0.078704142364725));
#92741=CARTESIAN_POINT('Ctrl Pts',(0.0119674222202632,-0.0329142774063509,
0.0787579565243764));
#92742=CARTESIAN_POINT('Ctrl Pts',(0.0119035407062456,-0.0328043479726686,
0.0788105005478493));
#92743=CARTESIAN_POINT('Ctrl Pts',(0.0118385954093646,-0.0326943950436594,
0.0788617048685608));
#92744=CARTESIAN_POINT('Origin',(0.00168717567872209,-0.0326396682856143,
0.0651682523318792));
#92745=CARTESIAN_POINT('Ctrl Pts',(0.0115564688245381,-0.0331951640388587,
0.0790710428255139));
#92746=CARTESIAN_POINT('Ctrl Pts',(0.0114886914069139,-0.0330855618127431,
0.079118321145098));
#92747=CARTESIAN_POINT('Ctrl Pts',(0.0114198879673268,-0.0329757224171935,
0.0791642327034358));
#92748=CARTESIAN_POINT('Ctrl Pts',(0.0113501437288367,-0.0328657861694599,
0.0792087143861768));
#92749=CARTESIAN_POINT('Ctrl Pts',(0.0115695416577292,-0.0331951640388587,
0.0789584806068394));
#92750=CARTESIAN_POINT('Ctrl Pts',(0.0115033145571362,-0.0330855618127431,
0.0790059389782755));
#92751=CARTESIAN_POINT('Ctrl Pts',(0.0114360588308179,-0.0329757224171935,
0.0790520627606689));
#92752=CARTESIAN_POINT('Ctrl Pts',(0.0113678577065632,-0.0328657861694599,
0.0790967886651217));
#92753=CARTESIAN_POINT('Ctrl Pts',(0.0115826144909202,-0.0331951640388587,
0.0788459183881649));
#92754=CARTESIAN_POINT('Ctrl Pts',(0.0115179377073585,-0.0330855618127431,
0.078893556811453));
#92755=CARTESIAN_POINT('Ctrl Pts',(0.011452229694309,-0.0329757224171935,
0.078939892817902));
#92756=CARTESIAN_POINT('Ctrl Pts',(0.0113855716842898,-0.0328657861694599,
0.0789848629440667));
#92757=CARTESIAN_POINT('Ctrl Pts',(0.0115956873241113,-0.0331951640388587,
0.0787333561694903));
#92758=CARTESIAN_POINT('Ctrl Pts',(0.0115325608575808,-0.0330855618127431,
0.0787811746446305));
#92759=CARTESIAN_POINT('Ctrl Pts',(0.0114684005578001,-0.0329757224171935,
0.0788277228751352));
#92760=CARTESIAN_POINT('Ctrl Pts',(0.0114032856620164,-0.0328657861694599,
0.0788729372230117));
#92761=CARTESIAN_POINT('Origin',(0.00209927003337273,-0.0326401908833287,
0.0649203589795844));
#92762=CARTESIAN_POINT('Ctrl Pts',(0.0116241701904994,-0.0332451089994432,
0.0787134864815975));
#92763=CARTESIAN_POINT('Ctrl Pts',(0.0114520554819021,-0.0329451141710258,
0.0788455057748676));
#92764=CARTESIAN_POINT('Ctrl Pts',(0.0112704855001587,-0.0326442513127503,
0.0789641856317969));
#92765=CARTESIAN_POINT('Ctrl Pts',(0.0118191819903634,-0.0332451089994432,
0.0785570563121486));
#92766=CARTESIAN_POINT('Ctrl Pts',(0.0116529671421337,-0.0329451141710258,
0.0786964305957846));
#92767=CARTESIAN_POINT('Ctrl Pts',(0.0114767262519354,-0.0326442513127503,
0.07882288894993));
#92768=CARTESIAN_POINT('Ctrl Pts',(0.0114033116817675,-0.0325229783203385,
0.0788729192646424));
#92769=CARTESIAN_POINT('Ctrl Pts',(0.0113382063441729,-0.0324130253112079,
0.0789181275061021));
#92770=CARTESIAN_POINT('Ctrl Pts',(0.0112721756905466,-0.0323031222247695,
0.078961982103329));
#92771=CARTESIAN_POINT('Ctrl Pts',(0.0112053062836757,-0.0321934096636184,
0.0790044298662736));
#92772=CARTESIAN_POINT('Ctrl Pts',(0.0115143729298709,-0.0325229783203385,
0.0788954257485908));
#92773=CARTESIAN_POINT('Ctrl Pts',(0.0114489573408929,-0.0324130253112079,
0.0789421649668989));
#92774=CARTESIAN_POINT('Ctrl Pts',(0.0113825848127166,-0.0323031222247695,
0.0789875438908234));
#92775=CARTESIAN_POINT('Ctrl Pts',(0.0113153424149455,-0.0321934096636184,
0.0790315073932132));
#92776=CARTESIAN_POINT('Ctrl Pts',(0.0116254341779743,-0.0325229783203385,
0.0789179322325391));
#92777=CARTESIAN_POINT('Ctrl Pts',(0.0115597083376129,-0.0324130253112079,
0.0789662024276958));
#92778=CARTESIAN_POINT('Ctrl Pts',(0.0114929939348867,-0.0323031222247695,
0.0790131056783178));
#92779=CARTESIAN_POINT('Ctrl Pts',(0.0114253785462154,-0.0321934096636184,
0.0790585849201528));
#92780=CARTESIAN_POINT('Ctrl Pts',(0.0117364954260777,-0.0325229783203385,
0.0789404387164875));
#92781=CARTESIAN_POINT('Ctrl Pts',(0.0116704593343329,-0.0324130253112079,
0.0789902398884926));
#92782=CARTESIAN_POINT('Ctrl Pts',(0.0116034030570568,-0.0323031222247695,
0.0790386674658122));
#92783=CARTESIAN_POINT('Ctrl Pts',(0.0115354146774852,-0.0321934096636184,
0.0790856624470925));
#92784=CARTESIAN_POINT('Origin',(0.00169194628218417,-0.0326393375177923,
0.0651753186159354));
#92785=CARTESIAN_POINT('Ctrl Pts',(0.011240700365954,-0.0326943950436593,
0.0792768724485699));
#92786=CARTESIAN_POINT('Ctrl Pts',(0.0111700424548299,-0.0325844576448126,
0.0793198294227188));
#92787=CARTESIAN_POINT('Ctrl Pts',(0.0110984911224813,-0.0324744968375318,
0.0793613281155522));
#92788=CARTESIAN_POINT('Ctrl Pts',(0.0110261387780296,-0.0323646534831894,
0.0794013166210089));
#92789=CARTESIAN_POINT('Ctrl Pts',(0.0112608152239288,-0.0326943950436593,
0.0791653533019131));
#92790=CARTESIAN_POINT('Ctrl Pts',(0.0111916942556548,-0.0325844576448126,
0.0792085874965041));
#92791=CARTESIAN_POINT('Ctrl Pts',(0.0111216742415548,-0.0324744968375318,
0.079250395215897));
#92792=CARTESIAN_POINT('Ctrl Pts',(0.0110508456341974,-0.0323646534831894,
0.0792907241310255));
#92793=CARTESIAN_POINT('Ctrl Pts',(0.0112809300819036,-0.0326943950436593,
0.0790538341552562));
#92794=CARTESIAN_POINT('Ctrl Pts',(0.0112133460564797,-0.0325844576448126,
0.0790973455702894));
#92795=CARTESIAN_POINT('Ctrl Pts',(0.0111448573606284,-0.0324744968375318,
0.0791394623162418));
#92796=CARTESIAN_POINT('Ctrl Pts',(0.0110755524903652,-0.0323646534831894,
0.0791801316410422));
#92797=CARTESIAN_POINT('Ctrl Pts',(0.0113010449398784,-0.0326943950436593,
0.0789423150085994));
#92798=CARTESIAN_POINT('Ctrl Pts',(0.0112349978573045,-0.0325844576448126,
0.0789861036440747));
#92799=CARTESIAN_POINT('Ctrl Pts',(0.0111680404797019,-0.0324744968375318,
0.0790285294165866));
#92800=CARTESIAN_POINT('Ctrl Pts',(0.011100259346533,-0.0323646534831894,
0.0790695391510588));
#92801=CARTESIAN_POINT('Origin',(0.00207820415296465,-0.032639557906635,
0.0648889234867131));
#92802=CARTESIAN_POINT('Ctrl Pts',(0.0113307518470199,-0.0327445246961876,
0.078924250793464));
#92803=CARTESIAN_POINT('Ctrl Pts',(0.0111506880365756,-0.0324436878365475,
0.0790452036300124));
#92804=CARTESIAN_POINT('Ctrl Pts',(0.0109620251064942,-0.0321434074463187,
0.079152249710342));
#92805=CARTESIAN_POINT('Ctrl Pts',(0.0115352001860331,-0.0327445246961876,
0.0787803728011415));
#92806=CARTESIAN_POINT('Ctrl Pts',(0.011360562822723,-0.0324436878365475,
0.0789090365327715));
#92807=CARTESIAN_POINT('Ctrl Pts',(0.0111767301076868,-0.0321434074463187,
0.0790241803445167));
#92808=CARTESIAN_POINT('Ctrl Pts',(0.011019815172185,-0.0322357242816073,
0.0791190157963224));
#92809=CARTESIAN_POINT('Ctrl Pts',(0.0108615584636495,-0.0319819883628705,
0.0792112506906888));
#92810=CARTESIAN_POINT('Ctrl Pts',(0.0106977533117821,-0.0317295851069886,
0.0792932283325005));
#92811=CARTESIAN_POINT('Ctrl Pts',(0.0112330213069529,-0.0322357242816073,
0.078988466402998));
#92812=CARTESIAN_POINT('Ctrl Pts',(0.0110789224272784,-0.0319819883628705,
0.0790874916362385));
#92813=CARTESIAN_POINT('Ctrl Pts',(0.0109188345892279,-0.0317295851069886,
0.0791765104300049));
#92814=CARTESIAN_POINT('Origin',(0.00212886373024658,-0.032637194264519,
0.0649696452976313));
#92815=CARTESIAN_POINT('Origin',(0.00176105284582072,-0.0326352985527993,
0.065276748817572));
#92816=CARTESIAN_POINT('Ctrl Pts',(0.0109126308553257,-0.0321934096636183,
0.0794624686483194));
#92817=CARTESIAN_POINT('Ctrl Pts',(0.0108393677723792,-0.0320835708272304,
0.0795009290448678));
#92818=CARTESIAN_POINT('Ctrl Pts',(0.0107653512490906,-0.0319739230346346,
0.0795378509571295));
#92819=CARTESIAN_POINT('Ctrl Pts',(0.0106906796099296,-0.0318646057455575,
0.0795731944139634));
#92820=CARTESIAN_POINT('Ctrl Pts',(0.0109397084055824,-0.0321934096636183,
0.079352432422295));
#92821=CARTESIAN_POINT('Ctrl Pts',(0.0108679628079498,-0.0320835708272304,
0.0793912662393644));
#92822=CARTESIAN_POINT('Ctrl Pts',(0.0107954551618537,-0.0319739230346346,
0.0794285927598277));
#92823=CARTESIAN_POINT('Ctrl Pts',(0.0107222819009896,-0.0318646057455575,
0.079464371346715));
#92824=CARTESIAN_POINT('Ctrl Pts',(0.010966785955839,-0.0321934096636183,
0.0792423961962706));
#92825=CARTESIAN_POINT('Ctrl Pts',(0.0108965578435203,-0.0320835708272304,
0.079281603433861));
#92826=CARTESIAN_POINT('Ctrl Pts',(0.0108255590746167,-0.0319739230346346,
0.0793193345625259));
#92827=CARTESIAN_POINT('Ctrl Pts',(0.0107538841920495,-0.0318646057455575,
0.0793555482794666));
#92828=CARTESIAN_POINT('Ctrl Pts',(0.0109938635060957,-0.0321934096636183,
0.0791323599702462));
#92829=CARTESIAN_POINT('Ctrl Pts',(0.0109251528790909,-0.0320835708272304,
0.0791719406283576));
#92830=CARTESIAN_POINT('Ctrl Pts',(0.0108556629873797,-0.0319739230346346,
0.0792100763652241));
#92831=CARTESIAN_POINT('Ctrl Pts',(0.0107854864831095,-0.0318646057455575,
0.0792467252122182));
#92832=CARTESIAN_POINT('Ctrl Pts',(0.0111010895863765,-0.0320218834582313,
0.0790700039112242));
#92833=CARTESIAN_POINT('Ctrl Pts',(0.0110498842396934,-0.0319391099350602,
0.0791009904835938));
#92834=CARTESIAN_POINT('Ctrl Pts',(0.0109982260573564,-0.0318564869454876,
0.0791311587033183));
#92835=CARTESIAN_POINT('Ctrl Pts',(0.0109461547168824,-0.0317740741446462,
0.0791604901095118));
#92836=CARTESIAN_POINT('Ctrl Pts',(0.0111489537407645,-0.0320218834582313,
0.0790828822174951));
#92837=CARTESIAN_POINT('Ctrl Pts',(0.0110976143620462,-0.0319391099350602,
0.0791143669400011));
#92838=CARTESIAN_POINT('Ctrl Pts',(0.0110458144501965,-0.0318564869454876,
0.0791450309151164));
#92839=CARTESIAN_POINT('Ctrl Pts',(0.0109935938196735,-0.0317740741446462,
0.0791748553305004));
#92840=CARTESIAN_POINT('Ctrl Pts',(0.0111968178951524,-0.0320218834582313,
0.079095760523766));
#92841=CARTESIAN_POINT('Ctrl Pts',(0.011145344484399,-0.0319391099350602,
0.0791277433964083));
#92842=CARTESIAN_POINT('Ctrl Pts',(0.0110934028430365,-0.0318564869454876,
0.0791589031269145));
#92843=CARTESIAN_POINT('Ctrl Pts',(0.0110410329224647,-0.0317740741446462,
0.079189220551489));
#92844=CARTESIAN_POINT('Ctrl Pts',(0.0112446820495404,-0.0320218834582313,
0.0791086388300369));
#92845=CARTESIAN_POINT('Ctrl Pts',(0.0111930746067518,-0.0319391099350602,
0.0791411198528156));
#92846=CARTESIAN_POINT('Ctrl Pts',(0.0111409912358765,-0.0318564869454876,
0.0791727753387125));
#92847=CARTESIAN_POINT('Ctrl Pts',(0.0110884720252559,-0.0317740741446462,
0.0792035857724777));
#92848=CARTESIAN_POINT('Origin',(0.0151637121232632,-0.0391228853390932,
0.0839642755672192));
#92849=CARTESIAN_POINT('Ctrl Pts',(0.0131920815323775,-0.0352722978779604,
0.076869651880326));
#92850=CARTESIAN_POINT('Ctrl Pts',(0.0131828395632165,-0.0352466642097223,
0.07688613455863));
#92851=CARTESIAN_POINT('Ctrl Pts',(0.0131736742122756,-0.0352210183808304,
0.0769026408966044));
#92852=CARTESIAN_POINT('Ctrl Pts',(0.0131645856216842,-0.0351953608940152,
0.0769191717352508));
#92853=CARTESIAN_POINT('Origin',(0.0173745289028921,-0.0352456003065049,
0.0794224693801586));
#92854=CARTESIAN_POINT('Ctrl Pts',(0.0131021098916861,-0.035024121149334,
0.0770270702921428));
#92855=CARTESIAN_POINT('Ctrl Pts',(0.0130624794298435,-0.0349144232867422,
0.0770956447119049));
#92856=CARTESIAN_POINT('Ctrl Pts',(0.0130214077650672,-0.0348045283677513,
0.0771634409868329));
#92857=CARTESIAN_POINT('Ctrl Pts',(0.0129789442734774,-0.0346945769586886,
0.0772303703208712));
#92858=CARTESIAN_POINT('Ctrl Pts',(0.0132121839095879,-0.035024121149334,
0.0770001472093643));
#92859=CARTESIAN_POINT('Ctrl Pts',(0.013172924302155,-0.0349144232867422,
0.0770702378535225));
#92860=CARTESIAN_POINT('Ctrl Pts',(0.0131321923723223,-0.0348045283677513,
0.0771395589262053));
#92861=CARTESIAN_POINT('Ctrl Pts',(0.0130900369883744,-0.0346945769586886,
0.0772080196944782));
#92862=CARTESIAN_POINT('Ctrl Pts',(0.0133222579274898,-0.035024121149334,
0.0769732241265858));
#92863=CARTESIAN_POINT('Ctrl Pts',(0.0132833691744665,-0.0349144232867422,
0.0770448309951401));
#92864=CARTESIAN_POINT('Ctrl Pts',(0.0132429769795774,-0.0348045283677513,
0.0771156768655777));
#92865=CARTESIAN_POINT('Ctrl Pts',(0.0132011297032715,-0.0346945769586886,
0.0771856690680852));
#92866=CARTESIAN_POINT('Ctrl Pts',(0.0134323319453916,-0.035024121149334,
0.0769463010438072));
#92867=CARTESIAN_POINT('Ctrl Pts',(0.013393814046778,-0.0349144232867422,
0.0770194241367577));
#92868=CARTESIAN_POINT('Ctrl Pts',(0.0133537615868325,-0.0348045283677513,
0.0770917948049501));
#92869=CARTESIAN_POINT('Ctrl Pts',(0.0133122224181685,-0.0346945769586886,
0.0771633184416922));
#92870=CARTESIAN_POINT('Origin',(-0.00110006755546588,-0.0345629067944436,
0.0680846404425669));
#92871=CARTESIAN_POINT('Ctrl Pts',(0.0131038037546256,-0.0351970973651611,
0.0773710102489984));
#92872=CARTESIAN_POINT('Ctrl Pts',(0.0130591810228675,-0.0350869349321773,
0.077440001698609));
#92873=CARTESIAN_POINT('Ctrl Pts',(0.0130130870321533,-0.0349764985129728,
0.0775081226180688));
#92874=CARTESIAN_POINT('Ctrl Pts',(0.0129655763035342,-0.0348659306849652,
0.077575281239486));
#92875=CARTESIAN_POINT('Ctrl Pts',(0.0130825376092316,-0.0351970973651611,
0.0772915859346482));
#92876=CARTESIAN_POINT('Ctrl Pts',(0.0130390151937099,-0.0350869349321773,
0.0773602827706351));
#92877=CARTESIAN_POINT('Ctrl Pts',(0.0129940285555751,-0.0349764985129728,
0.0774281317073815));
#92878=CARTESIAN_POINT('Ctrl Pts',(0.0129476308020129,-0.0348659306849652,
0.0774950414138066));
#92879=CARTESIAN_POINT('Ctrl Pts',(0.0130612714638377,-0.0351970973651611,
0.077212161620298));
#92880=CARTESIAN_POINT('Ctrl Pts',(0.0130188493645523,-0.0350869349321773,
0.0772805638426612));
#92881=CARTESIAN_POINT('Ctrl Pts',(0.012974970078997,-0.0349764985129728,
0.0773481407966943));
#92882=CARTESIAN_POINT('Ctrl Pts',(0.0129296853004916,-0.0348659306849652,
0.0774148015881272));
#92883=CARTESIAN_POINT('Ctrl Pts',(0.0130400053184437,-0.0351970973651611,
0.0771327373059478));
#92884=CARTESIAN_POINT('Ctrl Pts',(0.0129986835353946,-0.0350869349321773,
0.0772008449146873));
#92885=CARTESIAN_POINT('Ctrl Pts',(0.0129559116024188,-0.0349764985129728,
0.077268149886007));
#92886=CARTESIAN_POINT('Ctrl Pts',(0.0129117397989703,-0.0348659306849652,
0.0773345617624478));
#92887=CARTESIAN_POINT('Origin',(-0.000799005175002816,-0.0345637187966945,
0.0677095580521295));
#92888=CARTESIAN_POINT('Ctrl Pts',(0.0130582889654286,-0.0352450361861252,
0.0771044488342036));
#92889=CARTESIAN_POINT('Ctrl Pts',(0.012946860102051,-0.0349452761023764,
0.0772905568062231));
#92890=CARTESIAN_POINT('Ctrl Pts',(0.0128217293827438,-0.0346444289983474,
0.077467742787408));
#92891=CARTESIAN_POINT('Ctrl Pts',(0.0131820207931102,-0.0352450361861252,
0.0768872152391532));
#92892=CARTESIAN_POINT('Ctrl Pts',(0.0130787850290016,-0.0349452761023764,
0.0770779898335093));
#92893=CARTESIAN_POINT('Ctrl Pts',(0.0129614726241525,-0.0346444289983474,
0.0772604463173933));
#92894=CARTESIAN_POINT('Ctrl Pts',(0.0129116341444627,-0.0345231616327822,
0.077333984053815));
#92895=CARTESIAN_POINT('Ctrl Pts',(0.0128677474069721,-0.0344132092796975,
0.0773999778522077));
#92896=CARTESIAN_POINT('Ctrl Pts',(0.0128224979041709,-0.0343032738558973,
0.0774650604830761));
#92897=CARTESIAN_POINT('Ctrl Pts',(0.0127759457416698,-0.034193496108874,
0.0775291500529677));
#92898=CARTESIAN_POINT('Ctrl Pts',(0.0130231814429904,-0.0345231616327822,
0.0773140256889009));
#92899=CARTESIAN_POINT('Ctrl Pts',(0.0129795698034611,-0.0344132092796975,
0.0773815570097577));
#92900=CARTESIAN_POINT('Ctrl Pts',(0.0129345635819879,-0.0343032738558973,
0.0774481827739455));
#92901=CARTESIAN_POINT('Ctrl Pts',(0.01288822262315,-0.034193496108874,
0.077513819103096));
#92902=CARTESIAN_POINT('Ctrl Pts',(0.0131347287415182,-0.0345231616327822,
0.0772940673239867));
#92903=CARTESIAN_POINT('Ctrl Pts',(0.01309139219995,-0.0344132092796975,
0.0773631361673077));
#92904=CARTESIAN_POINT('Ctrl Pts',(0.0130466292598048,-0.0343032738558973,
0.0774313050648149));
#92905=CARTESIAN_POINT('Ctrl Pts',(0.0130004995046302,-0.034193496108874,
0.0774984881532244));
#92906=CARTESIAN_POINT('Ctrl Pts',(0.0132462760400459,-0.0345231616327822,
0.0772741089590726));
#92907=CARTESIAN_POINT('Ctrl Pts',(0.0132032145964389,-0.0344132092796975,
0.0773447153248577));
#92908=CARTESIAN_POINT('Ctrl Pts',(0.0131586949376218,-0.0343032738558973,
0.0774144273556843));
#92909=CARTESIAN_POINT('Ctrl Pts',(0.0131127763861103,-0.034193496108874,
0.0774831572033528));
#92910=CARTESIAN_POINT('Origin',(-0.00111031611238196,-0.0345625596228078,
0.068078201081954));
#92911=CARTESIAN_POINT('Ctrl Pts',(0.0129091470454601,-0.0346945769586886,
0.0777694313406994));
#92912=CARTESIAN_POINT('Ctrl Pts',(0.0128592694522607,-0.0345846629178476,
0.0778353760869727));
#92913=CARTESIAN_POINT('Ctrl Pts',(0.0128080196295779,-0.034474692505516,
0.0779003006486292));
#92914=CARTESIAN_POINT('Ctrl Pts',(0.012755463588148,-0.0343648066260528,
0.0779641221080353));
#92915=CARTESIAN_POINT('Ctrl Pts',(0.0128867964366645,-0.0346945769586886,
0.0776583387132696));
#92916=CARTESIAN_POINT('Ctrl Pts',(0.0128384497560193,-0.0345846629178476,
0.0777239754568573));
#92917=CARTESIAN_POINT('Ctrl Pts',(0.0127887374767434,-0.034474692505516,
0.0777886236218635));
#92918=CARTESIAN_POINT('Ctrl Pts',(0.0127377236380325,-0.0343648066260528,
0.0778522006366695));
#92919=CARTESIAN_POINT('Ctrl Pts',(0.012864445827869,-0.0346945769586886,
0.0775472460858398));
#92920=CARTESIAN_POINT('Ctrl Pts',(0.012817630059778,-0.0345846629178476,
0.0776125748267419));
#92921=CARTESIAN_POINT('Ctrl Pts',(0.0127694553239088,-0.034474692505516,
0.0776769465950977));
#92922=CARTESIAN_POINT('Ctrl Pts',(0.0127199836879171,-0.0343648066260528,
0.0777402791653037));
#92923=CARTESIAN_POINT('Ctrl Pts',(0.0128420952190734,-0.0346945769586886,
0.07743615345841));
#92924=CARTESIAN_POINT('Ctrl Pts',(0.0127968103635366,-0.0345846629178476,
0.0775011741966266));
#92925=CARTESIAN_POINT('Ctrl Pts',(0.0127501731710742,-0.034474692505516,
0.0775652695683319));
#92926=CARTESIAN_POINT('Ctrl Pts',(0.0127022437378016,-0.0343648066260528,
0.0776283576939379));
#92927=CARTESIAN_POINT('Origin',(-0.000846834622031316,-0.0345626446732096,
0.0676759950569512));
#92928=CARTESIAN_POINT('Ctrl Pts',(0.012842495146412,-0.0346945769586885,
0.0774381412780363));
#92929=CARTESIAN_POINT('Ctrl Pts',(0.0127736237108447,-0.034527515336289,
0.0775369766101112));
#92930=CARTESIAN_POINT('Ctrl Pts',(0.0127016261813744,-0.0343603235965158,
0.0776336715628087));
#92931=CARTESIAN_POINT('Ctrl Pts',(0.0126267197451524,-0.0341934961088739,
0.0777279433201761));
#92932=CARTESIAN_POINT('Ctrl Pts',(0.0128889177590261,-0.0346945769586885,
0.0773683346209802));
#92933=CARTESIAN_POINT('Ctrl Pts',(0.0128215084518399,-0.034527515336289,
0.0774681422932629));
#92934=CARTESIAN_POINT('Ctrl Pts',(0.0127509428497275,-0.0343603235965158,
0.0775658558202569));
#92935=CARTESIAN_POINT('Ctrl Pts',(0.0126774339496079,-0.0341934961088739,
0.0776611893105759));
#92936=CARTESIAN_POINT('Ctrl Pts',(0.0129353403716402,-0.0346945769586885,
0.0772985279639242));
#92937=CARTESIAN_POINT('Ctrl Pts',(0.0128693931928351,-0.034527515336289,
0.0773993079764147));
#92938=CARTESIAN_POINT('Ctrl Pts',(0.0128002595180805,-0.0343603235965158,
0.0774980400777052));
#92939=CARTESIAN_POINT('Ctrl Pts',(0.0127281481540635,-0.0341934961088739,
0.0775944353009757));
#92940=CARTESIAN_POINT('Ctrl Pts',(0.0129817629842544,-0.0346945769586885,
0.0772287213068681));
#92941=CARTESIAN_POINT('Ctrl Pts',(0.0129172779338303,-0.034527515336289,
0.0773304736595664));
#92942=CARTESIAN_POINT('Ctrl Pts',(0.0128495761864335,-0.0343603235965158,
0.0774302243351535));
#92943=CARTESIAN_POINT('Ctrl Pts',(0.012778862358519,-0.0341934961088739,
0.0775276812913754));
#92944=CARTESIAN_POINT('Ctrl Pts',(0.0127022623826205,-0.0340223579322366,
0.0776283322317491));
#92945=CARTESIAN_POINT('Ctrl Pts',(0.0126542871092738,-0.0339125849573554,
0.0776914814147395));
#92946=CARTESIAN_POINT('Ctrl Pts',(0.0126050385062468,-0.0338030433565221,
0.077753593246851));
#92947=CARTESIAN_POINT('Ctrl Pts',(0.0125545865953867,-0.0336938721132328,
0.0778145938804907));
#92948=CARTESIAN_POINT('Ctrl Pts',(0.0128148429535926,-0.0340223579322366,
0.0776154173229107));
#92949=CARTESIAN_POINT('Ctrl Pts',(0.0127670458105223,-0.0339125849573554,
0.0776801192855972));
#92950=CARTESIAN_POINT('Ctrl Pts',(0.0127179430736701,-0.0338030433565221,
0.0777437864931673));
#92951=CARTESIAN_POINT('Ctrl Pts',(0.0126676047546669,-0.0336938721132328,
0.0778063430924294));
#92952=CARTESIAN_POINT('Ctrl Pts',(0.0129274235245647,-0.0340223579322366,
0.0776025024140722));
#92953=CARTESIAN_POINT('Ctrl Pts',(0.0128798045117708,-0.0339125849573554,
0.0776687571564549));
#92954=CARTESIAN_POINT('Ctrl Pts',(0.0128308476410933,-0.0338030433565221,
0.0777339797394836));
#92955=CARTESIAN_POINT('Ctrl Pts',(0.012780622913947,-0.0336938721132328,
0.077798092304368));
#92956=CARTESIAN_POINT('Ctrl Pts',(0.0130400040955369,-0.0340223579322366,
0.0775895875052338));
#92957=CARTESIAN_POINT('Ctrl Pts',(0.0129925632130193,-0.0339125849573554,
0.0776573950273126));
#92958=CARTESIAN_POINT('Ctrl Pts',(0.0129437522085166,-0.0338030433565221,
0.0777241729858));
#92959=CARTESIAN_POINT('Ctrl Pts',(0.0128936410732272,-0.0336938721132328,
0.0777898415163066));
#92960=CARTESIAN_POINT('Origin',(-0.00101131372167616,-0.0345589643412299,
0.0681464022903583));
#92961=CARTESIAN_POINT('Ctrl Pts',(0.0126724382467533,-0.0341934961088739,
0.0780627647649451));
#92962=CARTESIAN_POINT('Ctrl Pts',(0.012618483537692,-0.0340836138581106,
0.0781254880383177));
#92963=CARTESIAN_POINT('Ctrl Pts',(0.0125632567905833,-0.0339738896643499,
0.0781870647363929));
#92964=CARTESIAN_POINT('Ctrl Pts',(0.0125068339719022,-0.0338644633294062,
0.0782474207868571));
#92965=CARTESIAN_POINT('Ctrl Pts',(0.0126571072830868,-0.0341934961088739,
0.0779504877824372));
#92966=CARTESIAN_POINT('Ctrl Pts',(0.0126047008071265,-0.0340836138581106,
0.0780129996508995));
#92967=CARTESIAN_POINT('Ctrl Pts',(0.0125510259248284,-0.0339738896643499,
0.0780743970829358));
#92968=CARTESIAN_POINT('Ctrl Pts',(0.012496156601092,-0.0338644633294062,
0.0781346061025266));
#92969=CARTESIAN_POINT('Ctrl Pts',(0.0126417763194202,-0.0341934961088739,
0.0778382107999292));
#92970=CARTESIAN_POINT('Ctrl Pts',(0.0125909180765609,-0.0340836138581106,
0.0779005112634812));
#92971=CARTESIAN_POINT('Ctrl Pts',(0.0125387950590736,-0.0339738896643499,
0.0779617294294786));
#92972=CARTESIAN_POINT('Ctrl Pts',(0.0124854792302818,-0.0338644633294062,
0.078021791418196));
#92973=CARTESIAN_POINT('Ctrl Pts',(0.0126264453557537,-0.0341934961088739,
0.0777259338174213));
#92974=CARTESIAN_POINT('Ctrl Pts',(0.0125771353459954,-0.0340836138581106,
0.0777880228760629));
#92975=CARTESIAN_POINT('Ctrl Pts',(0.0125265641933187,-0.0339738896643499,
0.0778490617760215));
#92976=CARTESIAN_POINT('Ctrl Pts',(0.0124748018594716,-0.0338644633294062,
0.0779089767338654));
#92977=CARTESIAN_POINT('Origin',(-0.000786468836533358,-0.0345610621861424,
0.0677209674668325));
#92978=CARTESIAN_POINT('Ctrl Pts',(0.0126491367289247,-0.03424362768739,
0.0776995480451978));
#92979=CARTESIAN_POINT('Ctrl Pts',(0.0125152633174715,-0.033943005420186,
0.0778702246051515));
#92980=CARTESIAN_POINT('Ctrl Pts',(0.0123689141685249,-0.0336441434784162,
0.0780303323970116));
#92981=CARTESIAN_POINT('Ctrl Pts',(0.0127991167530562,-0.03424362768739,
0.0774995330648552));
#92982=CARTESIAN_POINT('Ctrl Pts',(0.0126727870309459,-0.033943005420186,
0.0776758662146689));
#92983=CARTESIAN_POINT('Ctrl Pts',(0.012533534062986,-0.0336441434784162,
0.0778421827482009));
#92984=CARTESIAN_POINT('Ctrl Pts',(0.0124748198927572,-0.0335235895815128,
0.0779089556666321));
#92985=CARTESIAN_POINT('Ctrl Pts',(0.012423070467304,-0.0334144449262719,
0.0779688562669718));
#92986=CARTESIAN_POINT('Ctrl Pts',(0.0123700240867079,-0.0333049234473133,
0.0780277565816601));
#92987=CARTESIAN_POINT('Ctrl Pts',(0.0123157417586069,-0.0331951640388588,
0.0780855751509399));
#92988=CARTESIAN_POINT('Ctrl Pts',(0.0125879892158179,-0.0335235895815128,
0.0779031352882301));
#92989=CARTESIAN_POINT('Ctrl Pts',(0.0125363199193327,-0.0334144449262719,
0.0779645938871116));
#92990=CARTESIAN_POINT('Ctrl Pts',(0.0124833215726857,-0.0333049234473133,
0.0780250556456975));
#92991=CARTESIAN_POINT('Ctrl Pts',(0.0124290549412329,-0.0331951640388588,
0.078084437113187));
#92992=CARTESIAN_POINT('Ctrl Pts',(0.0127011585388787,-0.0335235895815128,
0.0778973149098281));
#92993=CARTESIAN_POINT('Ctrl Pts',(0.0126495693713615,-0.0334144449262719,
0.0779603315072514));
#92994=CARTESIAN_POINT('Ctrl Pts',(0.0125966190586635,-0.0333049234473133,
0.0780223547097348));
#92995=CARTESIAN_POINT('Ctrl Pts',(0.0125423681238589,-0.0331951640388588,
0.078083299075434));
#92996=CARTESIAN_POINT('Ctrl Pts',(0.0128143278619394,-0.0335235895815128,
0.0778914945314261));
#92997=CARTESIAN_POINT('Ctrl Pts',(0.0127628188233902,-0.0334144449262719,
0.0779560691273912));
#92998=CARTESIAN_POINT('Ctrl Pts',(0.0127099165446413,-0.0333049234473133,
0.0780196537737722));
#92999=CARTESIAN_POINT('Ctrl Pts',(0.012655681306485,-0.0331951640388588,
0.0780821610376811));
#93000=CARTESIAN_POINT('Origin',(0.000698274037872084,-0.0326434571769895,
0.0661346218489206));
#93001=CARTESIAN_POINT('Ctrl Pts',(0.012417925608737,-0.0336938721132443,
0.0783426784828669));
#93002=CARTESIAN_POINT('Ctrl Pts',(0.0123933844702971,-0.0336474569764985,
0.0783678135292279));
#93003=CARTESIAN_POINT('Ctrl Pts',(0.0123685507759787,-0.033601104548885,
0.0783926595683084));
#93004=CARTESIAN_POINT('Ctrl Pts',(0.0123056775743001,-0.0334837508643197,
0.078455564024085));
#93005=CARTESIAN_POINT('Ctrl Pts',(0.0122409679925288,-0.0333660264760478,
0.0785165777936198));
#93006=CARTESIAN_POINT('Ctrl Pts',(0.0123931733065771,-0.0336938721132443,
0.0780036248546317));
#93007=CARTESIAN_POINT('Ctrl Pts',(0.0123706167615333,-0.0336474569764985,
0.0780286150175544));
#93008=CARTESIAN_POINT('Ctrl Pts',(0.0123477692206689,-0.033601104548885,
0.0780533394152957));
#93009=CARTESIAN_POINT('Ctrl Pts',(0.0122899245026739,-0.0334837508643197,
0.0781159359031816));
#93010=CARTESIAN_POINT('Ctrl Pts',(0.0122302503221735,-0.0333660264760478,
0.0781767908444534));
#93011=CARTESIAN_POINT('Ctrl Pts',(0.0123931733065814,-0.0336938721132426,
0.0780036248546481));
#93012=CARTESIAN_POINT('Ctrl Pts',(0.0123706167615404,-0.0336474569765026,
0.0780286150175676));
#93013=CARTESIAN_POINT('Ctrl Pts',(0.0123477692206789,-0.0336011045488949,
0.0780533394153058));
#93014=CARTESIAN_POINT('Ctrl Pts',(0.012290406270396,-0.0334847282606778,
0.0781154145597085));
#93015=CARTESIAN_POINT('Ctrl Pts',(0.0122312439899657,-0.0333679869945434,
0.0781757772650163));
#93016=CARTESIAN_POINT('Ctrl Pts',(0.0123931733065764,-0.0336938721132429,
0.0780036248546325));
#93017=CARTESIAN_POINT('Ctrl Pts',(0.0123125011192406,-0.0335278710435084,
0.0780930007364861));
#93018=CARTESIAN_POINT('Ctrl Pts',(0.0122290545077754,-0.0333620469224321,
0.0781798153172916));
#93019=CARTESIAN_POINT('Ctrl Pts',(0.0121427775317655,-0.0331951640388601,
0.0782640978923517));
#93020=CARTESIAN_POINT('Ctrl Pts',(0.0124479789628948,-0.0336938721132429,
0.0779401869333332));
#93021=CARTESIAN_POINT('Ctrl Pts',(0.0123686347916644,-0.0335278710435084,
0.0780307101225508));
#93022=CARTESIAN_POINT('Ctrl Pts',(0.012286479749851,-0.0333620469224321,
0.0781187132533399));
#93023=CARTESIAN_POINT('Ctrl Pts',(0.0122014583416767,-0.0331951640388601,
0.0782042264269325));
#93024=CARTESIAN_POINT('Ctrl Pts',(0.0125027846192132,-0.0336938721132429,
0.0778767490120339));
#93025=CARTESIAN_POINT('Ctrl Pts',(0.0124247684640883,-0.0335278710435084,
0.0779684195086153));
#93026=CARTESIAN_POINT('Ctrl Pts',(0.0123439049919267,-0.0333620469224321,
0.0780576111893881));
#93027=CARTESIAN_POINT('Ctrl Pts',(0.0122601391515879,-0.0331951640388601,
0.0781443549615133));
#93028=CARTESIAN_POINT('Ctrl Pts',(0.0125575902755317,-0.0336938721132429,
0.0778133110907345));
#93029=CARTESIAN_POINT('Ctrl Pts',(0.0124809021365122,-0.0335278710435084,
0.0779061288946799));
#93030=CARTESIAN_POINT('Ctrl Pts',(0.0124013302340024,-0.0333620469224321,
0.0779965091254364));
#93031=CARTESIAN_POINT('Ctrl Pts',(0.012318819961499,-0.0331951640388601,
0.0780844834960941));
#93032=CARTESIAN_POINT('Ctrl Pts',(0.0122302084623775,-0.0330240426238155,
0.0781747414916993));
#93033=CARTESIAN_POINT('Ctrl Pts',(0.0121747637272139,-0.0329142774063509,
0.0782313115142555));
#93034=CARTESIAN_POINT('Ctrl Pts',(0.0121181218904411,-0.0328043479726686,
0.0782867635414779));
#93035=CARTESIAN_POINT('Ctrl Pts',(0.0120603535580914,-0.0326943950436594,
0.078341024536834));
#93036=CARTESIAN_POINT('Ctrl Pts',(0.012343519775375,-0.0330240426238155,
0.0781760385390808));
#93037=CARTESIAN_POINT('Ctrl Pts',(0.0122880571721201,-0.0329142774063509,
0.0782341695353674));
#93038=CARTESIAN_POINT('Ctrl Pts',(0.0122313651886606,-0.0328043479726686,
0.0782911829451392));
#93039=CARTESIAN_POINT('Ctrl Pts',(0.0121735144401843,-0.0326943950436594,
0.0783470037298471));
#93040=CARTESIAN_POINT('Ctrl Pts',(0.0124568310883725,-0.0330240426238155,
0.0781773355864623));
#93041=CARTESIAN_POINT('Ctrl Pts',(0.0124013506170263,-0.0329142774063509,
0.0782370275564793));
#93042=CARTESIAN_POINT('Ctrl Pts',(0.0123446084868802,-0.0328043479726686,
0.0782956023488005));
#93043=CARTESIAN_POINT('Ctrl Pts',(0.0122866753222772,-0.0326943950436594,
0.0783529829228602));
#93044=CARTESIAN_POINT('Ctrl Pts',(0.01257014240137,-0.0330240426238155,
0.0781786326338438));
#93045=CARTESIAN_POINT('Ctrl Pts',(0.0125146440619325,-0.0329142774063509,
0.0782398855775912));
#93046=CARTESIAN_POINT('Ctrl Pts',(0.0124578517850998,-0.0328043479726686,
0.0783000217524617));
#93047=CARTESIAN_POINT('Ctrl Pts',(0.0123998362043701,-0.0326943950436594,
0.0783589621158732));
#93048=CARTESIAN_POINT('Origin',(0.000612218764699066,-0.0326396682859389,
0.0660457968026155));
#93049=CARTESIAN_POINT('Ctrl Pts',(0.0121461712749856,-0.0331951640388587,
0.0786020092176616));
#93050=CARTESIAN_POINT('Ctrl Pts',(0.0120848538543536,-0.0330855618255041,
0.0786574094900376));
#93051=CARTESIAN_POINT('Ctrl Pts',(0.0120223472019189,-0.0329757224427707,
0.0787115823734241));
#93052=CARTESIAN_POINT('Ctrl Pts',(0.0119587279583793,-0.0328657862078596,
0.07876445456989));
#93053=CARTESIAN_POINT('Ctrl Pts',(0.0121450332381386,-0.0331951640388587,
0.078488696125246));
#93054=CARTESIAN_POINT('Ctrl Pts',(0.0120852764761241,-0.0330855618255041,
0.0785440807234667));
#93055=CARTESIAN_POINT('Ctrl Pts',(0.012024331931322,-0.0329757224427708,
0.0785982701775445));
#93056=CARTESIAN_POINT('Ctrl Pts',(0.0119622742430163,-0.0328657862078596,
0.078651191266451));
#93057=CARTESIAN_POINT('Ctrl Pts',(0.0121438952012916,-0.0331951640388587,
0.0783753830328304));
#93058=CARTESIAN_POINT('Ctrl Pts',(0.0120856990978947,-0.0330855618255041,
0.0784307519568958));
#93059=CARTESIAN_POINT('Ctrl Pts',(0.012026316660725,-0.0329757224427708,
0.0784849579816649));
#93060=CARTESIAN_POINT('Ctrl Pts',(0.0119658205276534,-0.0328657862078596,
0.078537927963012));
#93061=CARTESIAN_POINT('Ctrl Pts',(0.0121427571644447,-0.0331951640388587,
0.0782620699404148));
#93062=CARTESIAN_POINT('Ctrl Pts',(0.0120861217196652,-0.0330855618255041,
0.0783174231903249));
#93063=CARTESIAN_POINT('Ctrl Pts',(0.012028301390128,-0.0329757224427708,
0.0783716457857853));
#93064=CARTESIAN_POINT('Ctrl Pts',(0.0119693668122904,-0.0328657862078596,
0.078424664659573));
#93065=CARTESIAN_POINT('Origin',(0.000989994360189074,-0.0326401908831897,
0.06574820904801));
#93066=CARTESIAN_POINT('Ctrl Pts',(0.0121685251026903,-0.0332451089994432,
0.0782387870811999));
#93067=CARTESIAN_POINT('Ctrl Pts',(0.0120143139748969,-0.0329451141710257,
0.0783913370558828));
#93068=CARTESIAN_POINT('Ctrl Pts',(0.0118490502569198,-0.0326442513127503,
0.0785318378396225));
#93069=CARTESIAN_POINT('Ctrl Pts',(0.0123423932773012,-0.0332451089994432,
0.0780591489509005));
#93070=CARTESIAN_POINT('Ctrl Pts',(0.0121949573124395,-0.0329451141710257,
0.0782182564710759));
#93071=CARTESIAN_POINT('Ctrl Pts',(0.0120359555687373,-0.0326442513127503,
0.0783658065039826));
#93072=CARTESIAN_POINT('Ctrl Pts',(0.0119693903555023,-0.0325229783203385,
0.0784246436001899));
#93073=CARTESIAN_POINT('Ctrl Pts',(0.0119104644880265,-0.0324130253112079,
0.0784776552236457));
#93074=CARTESIAN_POINT('Ctrl Pts',(0.0118504509443035,-0.0323031222247695,
0.0785294398496081));
#93075=CARTESIAN_POINT('Ctrl Pts',(0.0117894289380661,-0.0321934096636184,
0.078579933858253));
#93076=CARTESIAN_POINT('Ctrl Pts',(0.0120823966629012,-0.0325229783203385,
0.0784330529484414));
#93077=CARTESIAN_POINT('Ctrl Pts',(0.0120233548727458,-0.0324130253112079,
0.078487622361345));
#93078=CARTESIAN_POINT('Ctrl Pts',(0.0119631931990498,-0.0323031222247695,
0.0785409621424765));
#93079=CARTESIAN_POINT('Ctrl Pts',(0.0119019911155827,-0.0321934096636184,
0.078593006686664));
#93080=CARTESIAN_POINT('Ctrl Pts',(0.0121954029703001,-0.0325229783203385,
0.0784414622966929));
#93081=CARTESIAN_POINT('Ctrl Pts',(0.012136245257465,-0.0324130253112079,
0.0784975894990444));
#93082=CARTESIAN_POINT('Ctrl Pts',(0.0120759354537961,-0.0323031222247695,
0.078552484435345));
#93083=CARTESIAN_POINT('Ctrl Pts',(0.0120145532930994,-0.0321934096636184,
0.0786060795150751));
#93084=CARTESIAN_POINT('Ctrl Pts',(0.012308409277699,-0.0325229783203385,
0.0784498716449445));
#93085=CARTESIAN_POINT('Ctrl Pts',(0.0122491356421843,-0.0324130253112079,
0.0785075566367438));
#93086=CARTESIAN_POINT('Ctrl Pts',(0.0121886777085424,-0.0323031222247695,
0.0785640067282135));
#93087=CARTESIAN_POINT('Ctrl Pts',(0.012127115470616,-0.0321934096636184,
0.0786191523434861));
#93088=CARTESIAN_POINT('Origin',(0.000617837391061115,-0.0326393375179294,
0.0660522094516855));
#93089=CARTESIAN_POINT('Ctrl Pts',(0.0118586900372337,-0.0326943950436593,
0.0788457920946329));
#93090=CARTESIAN_POINT('Ctrl Pts',(0.0117939732213176,-0.0325844576448127,
0.0788972661246881));
#93091=CARTESIAN_POINT('Ctrl Pts',(0.0117281872579574,-0.0324744968375319,
0.0789474053477826));
#93092=CARTESIAN_POINT('Ctrl Pts',(0.0116614173220466,-0.0323646534831895,
0.0789961466852158));
#93093=CARTESIAN_POINT('Ctrl Pts',(0.0118646692282906,-0.0326943950436593,
0.0787326312495637));
#93094=CARTESIAN_POINT('Ctrl Pts',(0.0118015119809055,-0.0325844576448127,
0.0787841876840779));
#93095=CARTESIAN_POINT('Ctrl Pts',(0.0117372839921901,-0.0324744968375319,
0.0788344415718974));
#93096=CARTESIAN_POINT('Ctrl Pts',(0.0116720684428964,-0.0323646534831895,
0.0788833296598734));
#93097=CARTESIAN_POINT('Ctrl Pts',(0.0118706484193474,-0.0326943950436593,
0.0786194704044945));
#93098=CARTESIAN_POINT('Ctrl Pts',(0.0118090507404934,-0.0325844576448127,
0.0786711092434677));
#93099=CARTESIAN_POINT('Ctrl Pts',(0.0117463807264229,-0.0324744968375319,
0.0787214777960122));
#93100=CARTESIAN_POINT('Ctrl Pts',(0.0116827195637462,-0.0323646534831895,
0.078770512634531));
#93101=CARTESIAN_POINT('Ctrl Pts',(0.0118766276104042,-0.0326943950436593,
0.0785063095594253));
#93102=CARTESIAN_POINT('Ctrl Pts',(0.0118165895000813,-0.0325844576448127,
0.0785580308028574));
#93103=CARTESIAN_POINT('Ctrl Pts',(0.0117554774606557,-0.0324744968375319,
0.078608514020127));
#93104=CARTESIAN_POINT('Ctrl Pts',(0.011693370684596,-0.0323646534831895,
0.0786576956091886));
#93105=CARTESIAN_POINT('Origin',(0.000965154675876512,-0.0326395579066209,
0.0657196616857234));
#93106=CARTESIAN_POINT('Ctrl Pts',(0.0119038362232152,-0.0327445246961876,
0.0784846645232906));
#93107=CARTESIAN_POINT('Ctrl Pts',(0.011740351679812,-0.0324436878365474,
0.0786272315902069));
#93108=CARTESIAN_POINT('Ctrl Pts',(0.0115665928446733,-0.0321434074463186,
0.0787570793153007));
#93109=CARTESIAN_POINT('Ctrl Pts',(0.0120886397319929,-0.0327445246961876,
0.0783162968804865));
#93110=CARTESIAN_POINT('Ctrl Pts',(0.0119315052779819,-0.0324436878365474,
0.0784658339256074));
#93111=CARTESIAN_POINT('Ctrl Pts',(0.0117635534850628,-0.0321434074463186,
0.0786031101426155));
#93112=CARTESIAN_POINT('Ctrl Pts',(0.011619761904527,-0.0322357242816072,
0.0787168644448188));
#93113=CARTESIAN_POINT('Ctrl Pts',(0.0114743131949657,-0.0319819883628704,
0.0788282068645079));
#93114=CARTESIAN_POINT('Ctrl Pts',(0.0113220742185753,-0.0317295851069886,
0.0789300683174863));
#93115=CARTESIAN_POINT('Ctrl Pts',(0.0118149246676354,-0.0322357242816072,
0.0785606226581679));
#93116=CARTESIAN_POINT('Ctrl Pts',(0.0116744520563408,-0.0319819883628704,
0.0786781807587451));
#93117=CARTESIAN_POINT('Ctrl Pts',(0.01152678357198,-0.0317295851069886,
0.0787865619391311));
#93118=CARTESIAN_POINT('Origin',(0.00102553191220463,-0.0326371942646883,
0.0657933976519712));
#93119=CARTESIAN_POINT('Origin',(0.000699111604263792,-0.0326352985529171,
0.0661441784971164));
#93120=CARTESIAN_POINT('Ctrl Pts',(0.0115564688245381,-0.0321934096636184,
0.0790710428255141));
#93121=CARTESIAN_POINT('Ctrl Pts',(0.0114886038087468,-0.0320835708272304,
0.0791183822494348));
#93122=CARTESIAN_POINT('Ctrl Pts',(0.0114197984705051,-0.0319739230346346,
0.0791642897515911));
#93123=CARTESIAN_POINT('Ctrl Pts',(0.0113501453492525,-0.0318646057455575,
0.079208713352703));
#93124=CARTESIAN_POINT('Ctrl Pts',(0.0115695416642065,-0.0321934096636184,
0.0789584805510671));
#93125=CARTESIAN_POINT('Ctrl Pts',(0.0115032289699055,-0.0320835708272304,
0.079006000259635));
#93126=CARTESIAN_POINT('Ctrl Pts',(0.0114359713217632,-0.0319739230346346,
0.079052120067079));
#93127=CARTESIAN_POINT('Ctrl Pts',(0.0113678592999038,-0.0318646057455575,
0.0790967875705166));
#93128=CARTESIAN_POINT('Ctrl Pts',(0.0115826145038749,-0.0321934096636184,
0.0788459182766199));
#93129=CARTESIAN_POINT('Ctrl Pts',(0.0115178541310643,-0.0320835708272304,
0.0788936182698353));
#93130=CARTESIAN_POINT('Ctrl Pts',(0.0114521441730213,-0.0319739230346346,
0.0789399503825667));
#93131=CARTESIAN_POINT('Ctrl Pts',(0.011385573250555,-0.0318646057455575,
0.0789848617883303));
#93132=CARTESIAN_POINT('Ctrl Pts',(0.0115956873435434,-0.0321934096636184,
0.0787333560021728));
#93133=CARTESIAN_POINT('Ctrl Pts',(0.011532479292223,-0.0320835708272304,
0.0787812362800356));
#93134=CARTESIAN_POINT('Ctrl Pts',(0.0114683170242795,-0.0319739230346346,
0.0788277806980545));
#93135=CARTESIAN_POINT('Ctrl Pts',(0.0114032872012063,-0.0318646057455575,
0.078872936006144));
#93136=CARTESIAN_POINT('Ctrl Pts',(0.0116942526276437,-0.0320218834582307,
0.0786580526479372));
#93137=CARTESIAN_POINT('Ctrl Pts',(0.0116473346977258,-0.0319391099350599,
0.078695212613604));
#93138=CARTESIAN_POINT('Ctrl Pts',(0.0115998649361153,-0.0318564869454876,
0.0787316174349374));
#93139=CARTESIAN_POINT('Ctrl Pts',(0.0115518803936972,-0.0317740741446464,
0.0787672438237096));
#93140=CARTESIAN_POINT('Ctrl Pts',(0.0117433534386458,-0.0320218834582307,
0.0786648304356753));
#93141=CARTESIAN_POINT('Ctrl Pts',(0.0116963649683427,-0.0319391099350599,
0.0787025014220842));
#93142=CARTESIAN_POINT('Ctrl Pts',(0.0116488167294251,-0.0318564869454876,
0.0787394158530472));
#93143=CARTESIAN_POINT('Ctrl Pts',(0.0116007458645908,-0.0317740741446464,
0.0787755500744898));
#93144=CARTESIAN_POINT('Ctrl Pts',(0.0117924542496478,-0.0320218834582307,
0.0786716082234135));
#93145=CARTESIAN_POINT('Ctrl Pts',(0.0117453952389596,-0.0319391099350599,
0.0787097902305645));
#93146=CARTESIAN_POINT('Ctrl Pts',(0.0116977685227349,-0.0318564869454876,
0.078747214271157));
#93147=CARTESIAN_POINT('Ctrl Pts',(0.0116496113354845,-0.0317740741446464,
0.07878385632527));
#93148=CARTESIAN_POINT('Ctrl Pts',(0.0118415550606499,-0.0320218834582307,
0.0786783860111516));
#93149=CARTESIAN_POINT('Ctrl Pts',(0.0117944255095765,-0.0319391099350599,
0.0787170790390447));
#93150=CARTESIAN_POINT('Ctrl Pts',(0.0117467203160448,-0.0318564869454876,
0.0787550126892669));
#93151=CARTESIAN_POINT('Ctrl Pts',(0.0116984768063782,-0.0317740741446464,
0.0787921625760503));
#93152=CARTESIAN_POINT('Origin',(0.0163382550649517,-0.0391228853390709,
0.0830045498907383));
#93153=CARTESIAN_POINT('Ctrl Pts',(0.0134929792425902,-0.0352722978779597,
0.0762129802680671));
#93154=CARTESIAN_POINT('Ctrl Pts',(0.0134858759764861,-0.0352466642097219,
0.0762304913014088));
#93155=CARTESIAN_POINT('Ctrl Pts',(0.0134788516897875,-0.0352210183808301,
0.0762480162050482));
#93156=CARTESIAN_POINT('Ctrl Pts',(0.0134719066289087,-0.0351953608940152,
0.0762655557955414));
#93157=CARTESIAN_POINT('Origin',(0.0179623996382882,-0.0352456003065037,
0.0782214683862578));
#93158=CARTESIAN_POINT('Ctrl Pts',(0.0134234468137344,-0.035024121149334,
0.0763804338253446));
#93159=CARTESIAN_POINT('Ctrl Pts',(0.0133927235036891,-0.0349144232867422,
0.076453434529255));
#93160=CARTESIAN_POINT('Ctrl Pts',(0.0133604728276174,-0.0348045283677513,
0.0765258438548597));
#93161=CARTESIAN_POINT('Ctrl Pts',(0.0133267326431973,-0.0346945769586886,
0.0765975675178176));
#93162=CARTESIAN_POINT('Ctrl Pts',(0.013529278508105,-0.035024121149334,
0.0763399271065204));
#93163=CARTESIAN_POINT('Ctrl Pts',(0.0134991131614779,-0.0349144232867422,
0.0764143855985624));
#93164=CARTESIAN_POINT('Ctrl Pts',(0.0134673906492715,-0.0348045283677513,
0.0764882651183571));
#93165=CARTESIAN_POINT('Ctrl Pts',(0.0134341480825772,-0.0346945769586886,
0.0765614695236062));
#93166=CARTESIAN_POINT('Ctrl Pts',(0.0136351102024756,-0.035024121149334,
0.0762994203876963));
#93167=CARTESIAN_POINT('Ctrl Pts',(0.0136055028192668,-0.0349144232867422,
0.0763753366678697));
#93168=CARTESIAN_POINT('Ctrl Pts',(0.0135743084709256,-0.0348045283677513,
0.0764506863818545));
#93169=CARTESIAN_POINT('Ctrl Pts',(0.013541563521957,-0.0346945769586886,
0.0765253715293948));
#93170=CARTESIAN_POINT('Ctrl Pts',(0.0137409418968463,-0.035024121149334,
0.0762589136688721));
#93171=CARTESIAN_POINT('Ctrl Pts',(0.0137118924770557,-0.0349144232867422,
0.0763362877371771));
#93172=CARTESIAN_POINT('Ctrl Pts',(0.0136812262925797,-0.0348045283677513,
0.0764131076453519));
#93173=CARTESIAN_POINT('Ctrl Pts',(0.0136489789613369,-0.0346945769586886,
0.0764892735351834));
#93174=CARTESIAN_POINT('Origin',(-0.001787525871552,-0.0345629067946148,
0.0692885225293325));
#93175=CARTESIAN_POINT('Ctrl Pts',(0.0134682344270035,-0.0351970973651615,
0.0767214494155905));
#93176=CARTESIAN_POINT('Ctrl Pts',(0.0134326104802814,-0.0350869349321775,
0.076795489558276));
#93177=CARTESIAN_POINT('Ctrl Pts',(0.0133954177695608,-0.0349764985129729,
0.0768688504328433));
#93178=CARTESIAN_POINT('Ctrl Pts',(0.0133566988844116,-0.0348659306849652,
0.0769414341617182));
#93179=CARTESIAN_POINT('Ctrl Pts',(0.0134371814653768,-0.0351970973651615,
0.0766453167404497));
#93180=CARTESIAN_POINT('Ctrl Pts',(0.0134026122336908,-0.0350869349321775,
0.0767189266864361));
#93181=CARTESIAN_POINT('Ctrl Pts',(0.0133664840552708,-0.0349764985129729,
0.0767918789348754));
#93182=CARTESIAN_POINT('Ctrl Pts',(0.0133288381717169,-0.0348659306849652,
0.0768640762187645));
#93183=CARTESIAN_POINT('Ctrl Pts',(0.0134061285037501,-0.0351970973651615,
0.076569184065309));
#93184=CARTESIAN_POINT('Ctrl Pts',(0.0133726139871001,-0.0350869349321775,
0.0766423638145962));
#93185=CARTESIAN_POINT('Ctrl Pts',(0.0133375503409809,-0.0349764985129729,
0.0767149074369076));
#93186=CARTESIAN_POINT('Ctrl Pts',(0.0133009774590221,-0.0348659306849652,
0.0767867182758109));
#93187=CARTESIAN_POINT('Ctrl Pts',(0.0133750755421234,-0.0351970973651615,
0.0764930513901682));
#93188=CARTESIAN_POINT('Ctrl Pts',(0.0133426157405095,-0.0350869349321775,
0.0765658009427563));
#93189=CARTESIAN_POINT('Ctrl Pts',(0.0133086166266909,-0.0349764985129729,
0.0766379359389398));
#93190=CARTESIAN_POINT('Ctrl Pts',(0.0132731167463274,-0.0348659306849652,
0.0767093603328572));
#93191=CARTESIAN_POINT('Origin',(-0.00153584774646322,-0.0345637187967202,
0.0688786646538233));
#93192=CARTESIAN_POINT('Ctrl Pts',(0.0133896695314542,-0.0352450361861253,
0.076462694432875));
#93193=CARTESIAN_POINT('Ctrl Pts',(0.0133024448318717,-0.0349452761023765,
0.0766613006277069));
#93194=CARTESIAN_POINT('Ctrl Pts',(0.0132005080976252,-0.0346444289983475,
0.0768527724821762));
#93195=CARTESIAN_POINT('Ctrl Pts',(0.0134851991078111,-0.0352450361861253,
0.0762316660795478));
#93196=CARTESIAN_POINT('Ctrl Pts',(0.0134066877853302,-0.0349452761023765,
0.076433875231381));
#93197=CARTESIAN_POINT('Ctrl Pts',(0.0133131682849427,-0.0346444289983475,
0.0766295961344295));
#93198=CARTESIAN_POINT('Ctrl Pts',(0.0132729395188461,-0.0345231616327823,
0.0767088004216502));
#93199=CARTESIAN_POINT('Ctrl Pts',(0.0132376700575367,-0.0344132092796975,
0.0767797743059514));
#93200=CARTESIAN_POINT('Ctrl Pts',(0.013200934377156,-0.0343032738558974,
0.0768500150073395));
#93201=CARTESIAN_POINT('Ctrl Pts',(0.013162781845393,-0.034193496108874,
0.0769194337448856));
#93202=CARTESIAN_POINT('Ctrl Pts',(0.0133811057871956,-0.0345231616327823,
0.076675018850785));
#93203=CARTESIAN_POINT('Ctrl Pts',(0.0133463019572799,-0.0344132092796975,
0.0767474836548095));
#93204=CARTESIAN_POINT('Ctrl Pts',(0.0133100010457701,-0.0343032738558974,
0.0768192248302143));
#93205=CARTESIAN_POINT('Ctrl Pts',(0.0132722519126058,-0.034193496108874,
0.0768901516595225));
#93206=CARTESIAN_POINT('Ctrl Pts',(0.0134892720555451,-0.0345231616327823,
0.0766412372799198));
#93207=CARTESIAN_POINT('Ctrl Pts',(0.0134549338570232,-0.0344132092796976,
0.0767151930036676));
#93208=CARTESIAN_POINT('Ctrl Pts',(0.0134190677143842,-0.0343032738558974,
0.0767884346530891));
#93209=CARTESIAN_POINT('Ctrl Pts',(0.0133817219798186,-0.034193496108874,
0.0768608695741595));
#93210=CARTESIAN_POINT('Ctrl Pts',(0.0135974383238946,-0.0345231616327823,
0.0766074557090546));
#93211=CARTESIAN_POINT('Ctrl Pts',(0.0135635657567664,-0.0344132092796976,
0.0766829023525256));
#93212=CARTESIAN_POINT('Ctrl Pts',(0.0135281343829983,-0.0343032738558974,
0.0767576444759639));
#93213=CARTESIAN_POINT('Ctrl Pts',(0.0134911920470314,-0.034193496108874,
0.0768315874887964));
#93214=CARTESIAN_POINT('Origin',(-0.00179850068158374,-0.0345625596231899,
0.0692834184300123));
#93215=CARTESIAN_POINT('Ctrl Pts',(0.0133250480478741,-0.0346945769586886,
0.0771411257927765));
#93216=CARTESIAN_POINT('Ctrl Pts',(0.0132838288225909,-0.0345846629176053,
0.0772128018652248));
#93217=CARTESIAN_POINT('Ctrl Pts',(0.0132411203252203,-0.0344746925050311,
0.0772836377834714));
#93218=CARTESIAN_POINT('Ctrl Pts',(0.0131969776536493,-0.0343648066253259,
0.0773535430103733));
#93219=CARTESIAN_POINT('Ctrl Pts',(0.0132889500820837,-0.0346945769586886,
0.0770337104379681));
#93220=CARTESIAN_POINT('Ctrl Pts',(0.0132492110946827,-0.0345846629176053,
0.0771048890622021));
#93221=CARTESIAN_POINT('Ctrl Pts',(0.0132079933750472,-0.0344746925050311,
0.0771752580579806));
#93222=CARTESIAN_POINT('Ctrl Pts',(0.0131653501084374,-0.0343648066253259,
0.0772447274785468));
#93223=CARTESIAN_POINT('Ctrl Pts',(0.0132528521162933,-0.0346945769586886,
0.0769262950831597));
#93224=CARTESIAN_POINT('Ctrl Pts',(0.0132145933667745,-0.0345846629176053,
0.0769969762591795));
#93225=CARTESIAN_POINT('Ctrl Pts',(0.0131748664248742,-0.0344746925050311,
0.0770668783324899));
#93226=CARTESIAN_POINT('Ctrl Pts',(0.0131337225632256,-0.0343648066253259,
0.0771359119467202));
#93227=CARTESIAN_POINT('Ctrl Pts',(0.013216754150503,-0.0346945769586886,
0.0768188797283513));
#93228=CARTESIAN_POINT('Ctrl Pts',(0.0131799756388663,-0.0345846629176053,
0.0768890634561569));
#93229=CARTESIAN_POINT('Ctrl Pts',(0.0131417394747012,-0.0344746925050311,
0.0769584986069991));
#93230=CARTESIAN_POINT('Ctrl Pts',(0.0131020950180138,-0.0343648066253259,
0.0770270964148937));
#93231=CARTESIAN_POINT('Origin',(-0.00158750660273259,-0.0345626446733096,
0.0688513609322516));
#93232=CARTESIAN_POINT('Ctrl Pts',(0.0132174000641565,-0.0346945769586885,
0.0768208017492395));
#93233=CARTESIAN_POINT('Ctrl Pts',(0.0131614590521889,-0.034527515336289,
0.0769274896149203));
#93234=CARTESIAN_POINT('Ctrl Pts',(0.013102148335834,-0.0343603235965158,
0.0770324457822115));
#93235=CARTESIAN_POINT('Ctrl Pts',(0.0130396479434197,-0.0341934961088739,
0.077135362444481));
#93236=CARTESIAN_POINT('Ctrl Pts',(0.0132547075265512,-0.0346945769586885,
0.0767457272423751));
#93237=CARTESIAN_POINT('Ctrl Pts',(0.0132003389801881,-0.034527515336289,
0.0768531965277928));
#93238=CARTESIAN_POINT('Ctrl Pts',(0.0131425765612264,-0.0343603235965158,
0.076958983769532));
#93239=CARTESIAN_POINT('Ctrl Pts',(0.013081595755349,-0.0341934961088739,
0.0770627786349528));
#93240=CARTESIAN_POINT('Ctrl Pts',(0.013292014988946,-0.0346945769586885,
0.0766706527355107));
#93241=CARTESIAN_POINT('Ctrl Pts',(0.0132392189081873,-0.034527515336289,
0.0767789034406653));
#93242=CARTESIAN_POINT('Ctrl Pts',(0.0131830047866187,-0.0343603235965158,
0.0768855217568525));
#93243=CARTESIAN_POINT('Ctrl Pts',(0.0131235435672782,-0.0341934961088739,
0.0769901948254245));
#93244=CARTESIAN_POINT('Ctrl Pts',(0.0133293224513408,-0.0346945769586885,
0.0765955782286463));
#93245=CARTESIAN_POINT('Ctrl Pts',(0.0132780988361865,-0.034527515336289,
0.0767046103535378));
#93246=CARTESIAN_POINT('Ctrl Pts',(0.013223433012011,-0.0343603235965158,
0.076812059744173));
#93247=CARTESIAN_POINT('Ctrl Pts',(0.0131654913792074,-0.0341934961088739,
0.0769176110158964));
#93248=CARTESIAN_POINT('Ctrl Pts',(0.0131021103248165,-0.0340223579322365,
0.0770270688162126));
#93249=CARTESIAN_POINT('Ctrl Pts',(0.0130624280421308,-0.0339125849573554,
0.077095732945173));
#93250=CARTESIAN_POINT('Ctrl Pts',(0.0130213524558096,-0.0338030433565221,
0.0771635274936023));
#93251=CARTESIAN_POINT('Ctrl Pts',(0.0129789437799994,-0.0336938721132327,
0.0772303704201534));
#93252=CARTESIAN_POINT('Ctrl Pts',(0.013212184497074,-0.0340223579322365,
0.0770001456582915));
#93253=CARTESIAN_POINT('Ctrl Pts',(0.0131728735549546,-0.0339125849573554,
0.0770703279971728));
#93254=CARTESIAN_POINT('Ctrl Pts',(0.0131321376248455,-0.0338030433565221,
0.0771396473745813));
#93255=CARTESIAN_POINT('Ctrl Pts',(0.0130900366593892,-0.0336938721132327,
0.0772080197606663));
#93256=CARTESIAN_POINT('Ctrl Pts',(0.0133222586693315,-0.0340223579322365,
0.0769732225003704));
#93257=CARTESIAN_POINT('Ctrl Pts',(0.0132833190677784,-0.0339125849573554,
0.0770449230491726));
#93258=CARTESIAN_POINT('Ctrl Pts',(0.0132429227938813,-0.0338030433565221,
0.0771157672555604));
#93259=CARTESIAN_POINT('Ctrl Pts',(0.013201129538779,-0.0336938721132327,
0.0771856691011792));
#93260=CARTESIAN_POINT('Ctrl Pts',(0.0134323328415891,-0.0340223579322365,
0.0769462993424493));
#93261=CARTESIAN_POINT('Ctrl Pts',(0.0133937645806022,-0.0339125849573554,
0.0770195181011725));
#93262=CARTESIAN_POINT('Ctrl Pts',(0.0133537079629172,-0.0338030433565221,
0.0770918871365395));
#93263=CARTESIAN_POINT('Ctrl Pts',(0.0133122224181688,-0.0336938721132327,
0.0771633184416921));
#93264=CARTESIAN_POINT('Origin',(-0.00169173107631589,-0.0345589643414446,
0.0693386735614597));
#93265=CARTESIAN_POINT('Ctrl Pts',(0.0131269701953199,-0.034193496108874,
0.0774618136745128));
#93266=CARTESIAN_POINT('Ctrl Pts',(0.0130813022459265,-0.0340836138581107,
0.077530804674293));
#93267=CARTESIAN_POINT('Ctrl Pts',(0.0130342285848961,-0.03397388966435,
0.0775988175685062));
#93268=CARTESIAN_POINT('Ctrl Pts',(0.0129858152959628,-0.0338644633294062,
0.0776657693477972));
#93269=CARTESIAN_POINT('Ctrl Pts',(0.0130976880836083,-0.034193496108874,
0.0773523435087971));
#93270=CARTESIAN_POINT('Ctrl Pts',(0.0130535296629745,-0.0340836138581107,
0.0774209307255971));
#93271=CARTESIAN_POINT('Ctrl Pts',(0.013007973161845,-0.03397388966435,
0.0774885712671029));
#93272=CARTESIAN_POINT('Ctrl Pts',(0.0129610826902299,-0.0338644633294062,
0.077555182470358));
#93273=CARTESIAN_POINT('Ctrl Pts',(0.0130684059718968,-0.034193496108874,
0.0772428733430816));
#93274=CARTESIAN_POINT('Ctrl Pts',(0.0130257570800226,-0.0340836138581107,
0.0773110567769012));
#93275=CARTESIAN_POINT('Ctrl Pts',(0.0129817177387938,-0.03397388966435,
0.0773783249656995));
#93276=CARTESIAN_POINT('Ctrl Pts',(0.0129363500844969,-0.0338644633294062,
0.0774445955929188));
#93277=CARTESIAN_POINT('Ctrl Pts',(0.0130391238601852,-0.034193496108874,
0.077133403177366));
#93278=CARTESIAN_POINT('Ctrl Pts',(0.0129979844970706,-0.0340836138581107,
0.0772011828282052));
#93279=CARTESIAN_POINT('Ctrl Pts',(0.0129554623157426,-0.03397388966435,
0.0772680786642962));
#93280=CARTESIAN_POINT('Ctrl Pts',(0.012911617478764,-0.0338644633294062,
0.0773340087154796));
#93281=CARTESIAN_POINT('Origin',(-0.00152198028231409,-0.0345610621864561,
0.0688884128822638));
#93282=CARTESIAN_POINT('Ctrl Pts',(0.0130583292909483,-0.0342436276873899,
0.0771043814816642));
#93283=CARTESIAN_POINT('Ctrl Pts',(0.0129469029564832,-0.033943005420186,
0.0772904909935097));
#93284=CARTESIAN_POINT('Ctrl Pts',(0.012821774641561,-0.0336441434784162,
0.0774676786996759));
#93285=CARTESIAN_POINT('Ctrl Pts',(0.0131820581535451,-0.0342436276873899,
0.0768871461977886));
#93286=CARTESIAN_POINT('Ctrl Pts',(0.0130788249828772,-0.033943005420186,
0.0770779222206153));
#93287=CARTESIAN_POINT('Ctrl Pts',(0.0129615150551054,-0.0336441434784162,
0.0772603803233617));
#93288=CARTESIAN_POINT('Ctrl Pts',(0.0129116327294273,-0.0335235895815128,
0.0773339855541979));
#93289=CARTESIAN_POINT('Ctrl Pts',(0.0128677988995837,-0.0334144449262719,
0.0773998997432397));
#93290=CARTESIAN_POINT('Ctrl Pts',(0.0128225529724405,-0.0333049234473133,
0.077464984085763));
#93291=CARTESIAN_POINT('Ctrl Pts',(0.0127759452649579,-0.0331951640388588,
0.0775291501180608));
#93292=CARTESIAN_POINT('Ctrl Pts',(0.0130231801917276,-0.0335235895815128,
0.0773140271940187));
#93293=CARTESIAN_POINT('Ctrl Pts',(0.0129796211280063,-0.0334144449262719,
0.0773814770534957));
#93294=CARTESIAN_POINT('Ctrl Pts',(0.0129346185568629,-0.0333049234473133,
0.0774481045072149));
#93295=CARTESIAN_POINT('Ctrl Pts',(0.012888222305342,-0.0331951640388588,
0.0775138191464914));
#93296=CARTESIAN_POINT('Ctrl Pts',(0.013134727654028,-0.0335235895815128,
0.0772940688338394));
#93297=CARTESIAN_POINT('Ctrl Pts',(0.0130914433564288,-0.0334144449262719,
0.0773630543637517));
#93298=CARTESIAN_POINT('Ctrl Pts',(0.0130466841412852,-0.0333049234473133,
0.0774312249286668));
#93299=CARTESIAN_POINT('Ctrl Pts',(0.0130004993457262,-0.0331951640388588,
0.0774984881749221));
#93300=CARTESIAN_POINT('Ctrl Pts',(0.0132462751163283,-0.0335235895815128,
0.0772741104736601));
#93301=CARTESIAN_POINT('Ctrl Pts',(0.0132032655848514,-0.0334144449262719,
0.0773446316740077));
#93302=CARTESIAN_POINT('Ctrl Pts',(0.0131587497257076,-0.0333049234473133,
0.0774143453501187));
#93303=CARTESIAN_POINT('Ctrl Pts',(0.0131127763861104,-0.0331951640388588,
0.0774831572033528));
#93304=CARTESIAN_POINT('Origin',(-0.000247766874356772,-0.0326434571769543,
0.0671284884476075));
#93305=CARTESIAN_POINT('Ctrl Pts',(0.0129095469568594,-0.0336938721132437,
0.0777714190810689));
#93306=CARTESIAN_POINT('Ctrl Pts',(0.0128883495892626,-0.0336474569764982,
0.0777994317503177));
#93307=CARTESIAN_POINT('Ctrl Pts',(0.0128668257504606,-0.033601104548885,
0.0778271943581689));
#93308=CARTESIAN_POINT('Ctrl Pts',(0.0128123323439931,-0.0334837508694633,
0.0778974828921133));
#93309=CARTESIAN_POINT('Ctrl Pts',(0.0127557800721974,-0.0333660264863652,
0.0779661258080421));
#93310=CARTESIAN_POINT('Ctrl Pts',(0.0128424951464166,-0.0336938721132437,
0.0774381412780297));
#93311=CARTESIAN_POINT('Ctrl Pts',(0.0128232485643943,-0.0336474569764982,
0.0774657614707818));
#93312=CARTESIAN_POINT('Ctrl Pts',(0.0128036799719308,-0.033601104548885,
0.0774931544654374));
#93313=CARTESIAN_POINT('Ctrl Pts',(0.0127541367992225,-0.0334837508694633,
0.0775625072238309));
#93314=CARTESIAN_POINT('Ctrl Pts',(0.0127025603163759,-0.0333660264863652,
0.0776303614608095));
#93315=CARTESIAN_POINT('Ctrl Pts',(0.012842495146422,-0.0336938721132426,
0.0774381412780463));
#93316=CARTESIAN_POINT('Ctrl Pts',(0.012823248564402,-0.0336474569765026,
0.0774657614707951));
#93317=CARTESIAN_POINT('Ctrl Pts',(0.0128036799719408,-0.0336011045488949,
0.0774931544654473));
#93318=CARTESIAN_POINT('Ctrl Pts',(0.012754549426385,-0.033484728265791,
0.0775619296098196));
#93319=CARTESIAN_POINT('Ctrl Pts',(0.012703419113583,-0.0333679870047996,
0.0776292313341869));
#93320=CARTESIAN_POINT('Ctrl Pts',(0.0128424951464162,-0.0336938721132429,
0.0774381412780302));
#93321=CARTESIAN_POINT('Ctrl Pts',(0.0127736608516485,-0.0335278710435084,
0.0775369233104576));
#93322=CARTESIAN_POINT('Ctrl Pts',(0.0127017529937719,-0.033362046922432,
0.0776335119660081));
#93323=CARTESIAN_POINT('Ctrl Pts',(0.012626719745153,-0.0331951640388601,
0.0777279433201753));
#93324=CARTESIAN_POINT('Ctrl Pts',(0.0128889177639579,-0.0336938721132429,
0.0773683346135643));
#93325=CARTESIAN_POINT('Ctrl Pts',(0.0128215448092338,-0.0335278710435084,
0.0774680884619416));
#93326=CARTESIAN_POINT('Ctrl Pts',(0.0127510673014092,-0.033362046922432,
0.0775656944188034));
#93327=CARTESIAN_POINT('Ctrl Pts',(0.0126774339549917,-0.0331951640388601,
0.0776611893034893));
#93328=CARTESIAN_POINT('Ctrl Pts',(0.0129353403814995,-0.0336938721132429,
0.0772985279490984));
#93329=CARTESIAN_POINT('Ctrl Pts',(0.012869428766819,-0.0335278710435084,
0.0773992536134257));
#93330=CARTESIAN_POINT('Ctrl Pts',(0.0128003816090465,-0.033362046922432,
0.0774978768715986));
#93331=CARTESIAN_POINT('Ctrl Pts',(0.0127281481648304,-0.0331951640388601,
0.0775944352868034));
#93332=CARTESIAN_POINT('Ctrl Pts',(0.0129817629990412,-0.0336938721132429,
0.0772287212846325));
#93333=CARTESIAN_POINT('Ctrl Pts',(0.0129173127244043,-0.0335278710435084,
0.0773304187649098));
#93334=CARTESIAN_POINT('Ctrl Pts',(0.0128496959166838,-0.033362046922432,
0.0774300593243939));
#93335=CARTESIAN_POINT('Ctrl Pts',(0.0127788623746691,-0.0331951640388601,
0.0775276812701174));
#93336=CARTESIAN_POINT('Ctrl Pts',(0.0127022619301293,-0.0330240426238156,
0.0776283335201845));
#93337=CARTESIAN_POINT('Ctrl Pts',(0.0126543444971128,-0.0329142774063509,
0.0776914065391582));
#93338=CARTESIAN_POINT('Ctrl Pts',(0.0126050992800205,-0.0328043479726686,
0.0777535204151411));
#93339=CARTESIAN_POINT('Ctrl Pts',(0.0125545871742304,-0.0326943950436595,
0.0778145938382327));
#93340=CARTESIAN_POINT('Ctrl Pts',(0.0128148423127214,-0.0330240426238156,
0.0776154186667026));
#93341=CARTESIAN_POINT('Ctrl Pts',(0.012767102794394,-0.0329142774063509,
0.0776800425901283));
#93342=CARTESIAN_POINT('Ctrl Pts',(0.0127180035191604,-0.0328043479726686,
0.0777437118217391));
#93343=CARTESIAN_POINT('Ctrl Pts',(0.0126676051405626,-0.0326943950436595,
0.0778063430642574));
#93344=CARTESIAN_POINT('Ctrl Pts',(0.0129274226953136,-0.0330240426238156,
0.0776025038132207));
#93345=CARTESIAN_POINT('Ctrl Pts',(0.0128798610916752,-0.0329142774063509,
0.0776686786410984));
#93346=CARTESIAN_POINT('Ctrl Pts',(0.0128309077583004,-0.0328043479726686,
0.0777339032283372));
#93347=CARTESIAN_POINT('Ctrl Pts',(0.0127806231068947,-0.0326943950436595,
0.077798092290282));
#93348=CARTESIAN_POINT('Ctrl Pts',(0.0130400030779058,-0.0330240426238156,
0.0775895889597388));
#93349=CARTESIAN_POINT('Ctrl Pts',(0.0129926193889564,-0.0329142774063509,
0.0776573146920685));
#93350=CARTESIAN_POINT('Ctrl Pts',(0.0129438119974403,-0.0328043479726686,
0.0777240946349353));
#93351=CARTESIAN_POINT('Ctrl Pts',(0.0128936410732269,-0.0326943950436595,
0.0777898415163066));
#93352=CARTESIAN_POINT('Origin',(-0.000344276306308796,-0.0326396682859005,
0.0670511493989361));
#93353=CARTESIAN_POINT('Ctrl Pts',(0.0126724382467533,-0.0331951640388588,
0.0780627647649451));
#93354=CARTESIAN_POINT('Ctrl Pts',(0.0126185478275749,-0.0330855618255041,
0.0781254133002278));
#93355=CARTESIAN_POINT('Ctrl Pts',(0.0125633237214108,-0.0329757224427708,
0.078186993175117));
#93356=CARTESIAN_POINT('Ctrl Pts',(0.0125068327779574,-0.0328657862078596,
0.0782474220640313));
#93357=CARTESIAN_POINT('Ctrl Pts',(0.0126571072873892,-0.0331951640388588,
0.0779504878139458));
#93358=CARTESIAN_POINT('Ctrl Pts',(0.0126047632560763,-0.0330855618255041,
0.0780129251962775));
#93359=CARTESIAN_POINT('Ctrl Pts',(0.0125510910167178,-0.0329757224427708,
0.0780743257271925));
#93360=CARTESIAN_POINT('Ctrl Pts',(0.0124961554430166,-0.0328657862078596,
0.078134607408249));
#93361=CARTESIAN_POINT('Ctrl Pts',(0.012641776328025,-0.0331951640388588,
0.0778382108629465));
#93362=CARTESIAN_POINT('Ctrl Pts',(0.0125909786845777,-0.0330855618255041,
0.0779004370923273));
#93363=CARTESIAN_POINT('Ctrl Pts',(0.0125388583120248,-0.0329757224427708,
0.077961658279268));
#93364=CARTESIAN_POINT('Ctrl Pts',(0.0124854781080758,-0.0328657862078596,
0.0780217927524668));
#93365=CARTESIAN_POINT('Ctrl Pts',(0.0126264453686608,-0.0331951640388588,
0.0777259339119473));
#93366=CARTESIAN_POINT('Ctrl Pts',(0.0125771941130792,-0.0330855618255041,
0.0777879489883771));
#93367=CARTESIAN_POINT('Ctrl Pts',(0.0125266256073318,-0.0329757224427708,
0.0778489908313435));
#93368=CARTESIAN_POINT('Ctrl Pts',(0.012474800773135,-0.0328657862078596,
0.0779089780966845));
#93369=CARTESIAN_POINT('Origin',(-6.77721975676001E-6,-0.0326401908831744,
0.0667085603757756));
#93370=CARTESIAN_POINT('Ctrl Pts',(0.0126490920029848,-0.0332451089994431,
0.0776996050660091));
#93371=CARTESIAN_POINT('Ctrl Pts',(0.0125152164576019,-0.0329451141710257,
0.077870279917875));
#93372=CARTESIAN_POINT('Ctrl Pts',(0.0123688653109474,-0.0326442513127503,
0.0780303858471343));
#93373=CARTESIAN_POINT('Ctrl Pts',(0.0127990745473651,-0.0332451089994431,
0.0774995919754844));
#93374=CARTESIAN_POINT('Ctrl Pts',(0.0126727426191114,-0.0329451141710257,
0.0776759235115599));
#93375=CARTESIAN_POINT('Ctrl Pts',(0.0125334875743865,-0.0326442513127503,
0.0778422382710665));
#93376=CARTESIAN_POINT('Ctrl Pts',(0.012474821491261,-0.0325229783203385,
0.0779089542526142));
#93377=CARTESIAN_POINT('Ctrl Pts',(0.0124230043900348,-0.0324130253112079,
0.0779689332330966));
#93378=CARTESIAN_POINT('Ctrl Pts',(0.01236995440565,-0.0323031222247695,
0.0780278312133084));
#93379=CARTESIAN_POINT('Ctrl Pts',(0.0123157421535373,-0.0321934096636185,
0.0780855751469736));
#93380=CARTESIAN_POINT('Ctrl Pts',(0.012587990680981,-0.0325229783203385,
0.0779031338447236));
#93381=CARTESIAN_POINT('Ctrl Pts',(0.0125362538139488,-0.0324130253112079,
0.077964672859983));
#93382=CARTESIAN_POINT('Ctrl Pts',(0.0124832517802662,-0.0323031222247695,
0.0780251322981094));
#93383=CARTESIAN_POINT('Ctrl Pts',(0.0124290552045198,-0.0321934096636185,
0.0780844371105427));
#93384=CARTESIAN_POINT('Ctrl Pts',(0.0127011598707009,-0.0325229783203385,
0.077897313436833));
#93385=CARTESIAN_POINT('Ctrl Pts',(0.0126495032378628,-0.0324130253112079,
0.0779604124868694));
#93386=CARTESIAN_POINT('Ctrl Pts',(0.0125965491548823,-0.0323031222247695,
0.0780224333829103));
#93387=CARTESIAN_POINT('Ctrl Pts',(0.0125423682555023,-0.0321934096636185,
0.0780832990741119));
#93388=CARTESIAN_POINT('Ctrl Pts',(0.0128143290604209,-0.0325229783203385,
0.0778914930289423));
#93389=CARTESIAN_POINT('Ctrl Pts',(0.0127627526617768,-0.0324130253112079,
0.0779561521137558));
#93390=CARTESIAN_POINT('Ctrl Pts',(0.0127098465294984,-0.0323031222247695,
0.0780197344677113));
#93391=CARTESIAN_POINT('Ctrl Pts',(0.0126556813064848,-0.0321934096636185,
0.078082161037681));
#93392=CARTESIAN_POINT('Origin',(-0.000337898267003137,-0.0326393375182276,
0.0670568072818518));
#93393=CARTESIAN_POINT('Ctrl Pts',(0.012417777980686,-0.0326943950436593,
0.0783406562942332));
#93394=CARTESIAN_POINT('Ctrl Pts',(0.0123600228828247,-0.0325844576448127,
0.0783998356039916));
#93395=CARTESIAN_POINT('Ctrl Pts',(0.0123010397723938,-0.0324744968375319,
0.0784578246318473));
#93396=CARTESIAN_POINT('Ctrl Pts',(0.0122409052467996,-0.0323646534831895,
0.0785145501212491));
#93397=CARTESIAN_POINT('Ctrl Pts',(0.0124095272094101,-0.0326943950436593,
0.0782276383648774));
#93398=CARTESIAN_POINT('Ctrl Pts',(0.0123533297104334,-0.0325844576448127,
0.0782867039635441));
#93399=CARTESIAN_POINT('Ctrl Pts',(0.0122959066608527,-0.0324744968375319,
0.0783446114859591));
#93400=CARTESIAN_POINT('Ctrl Pts',(0.0122373326577929,-0.0323646534831895,
0.0784012877524309));
#93401=CARTESIAN_POINT('Ctrl Pts',(0.0124012764381341,-0.0326943950436593,
0.0781146204355217));
#93402=CARTESIAN_POINT('Ctrl Pts',(0.0123466365380422,-0.0325844576448127,
0.0781735723230966));
#93403=CARTESIAN_POINT('Ctrl Pts',(0.0122907735493116,-0.0324744968375319,
0.0782313983400709));
#93404=CARTESIAN_POINT('Ctrl Pts',(0.0122337600687862,-0.0323646534831895,
0.0782880253836128));
#93405=CARTESIAN_POINT('Ctrl Pts',(0.0123930256668581,-0.0326943950436593,
0.078001602506166));
#93406=CARTESIAN_POINT('Ctrl Pts',(0.0123399433656509,-0.0325844576448127,
0.0780604406826491));
#93407=CARTESIAN_POINT('Ctrl Pts',(0.0122856404377706,-0.0324744968375319,
0.0781181851941828));
#93408=CARTESIAN_POINT('Ctrl Pts',(0.0122301874797795,-0.0323646534831895,
0.0781747630147946));
#93409=CARTESIAN_POINT('Origin',(-3.49989696872885E-5,-0.032639557906955,
0.0666833513559041));
#93410=CARTESIAN_POINT('Ctrl Pts',(0.0124173068892609,-0.0327445246961876,
0.0779767180041819));
#93411=CARTESIAN_POINT('Ctrl Pts',(0.0122729798618093,-0.0324436878365475,
0.0781386509336553));
#93412=CARTESIAN_POINT('Ctrl Pts',(0.0121168654022419,-0.0321434074463187,
0.0782892525273214));
#93413=CARTESIAN_POINT('Ctrl Pts',(0.0125795511060735,-0.0327445246961876,
0.0777865159692011));
#93414=CARTESIAN_POINT('Ctrl Pts',(0.0124423976655688,-0.0324436878365475,
0.0779545680392822));
#93415=CARTESIAN_POINT('Ctrl Pts',(0.0122929754948708,-0.0321434074463187,
0.0781118117336063));
#93416=CARTESIAN_POINT('Ctrl Pts',(0.012164574948423,-0.0322357242816073,
0.0782426909129078));
#93417=CARTESIAN_POINT('Ctrl Pts',(0.0120342280508725,-0.0319819883628705,
0.0783713849214484));
#93418=CARTESIAN_POINT('Ctrl Pts',(0.0118959561495598,-0.0317295851069886,
0.078491523769631));
#93419=CARTESIAN_POINT('Ctrl Pts',(0.0123386165065131,-0.0322357242816073,
0.07806322075924));
#93420=CARTESIAN_POINT('Ctrl Pts',(0.0122139855005927,-0.0319819883628705,
0.0781974577656821));
#93421=CARTESIAN_POINT('Ctrl Pts',(0.0120810651901328,-0.0317295851069886,
0.0783234920967294));
#93422=CARTESIAN_POINT('Origin',(3.41437415837766E-5,-0.0326371942648999,
0.0667489386179022));
#93423=CARTESIAN_POINT('Origin',(-0.000245738147881846,-0.0326352985532511,
0.0671378647634999));
#93424=CARTESIAN_POINT('Ctrl Pts',(0.0121461712749856,-0.0321934096636183,
0.0786020092176618));
#93425=CARTESIAN_POINT('Ctrl Pts',(0.0120847745981891,-0.0320835708272304,
0.0786574810979602));
#93426=CARTESIAN_POINT('Ctrl Pts',(0.0120222655462808,-0.0319739230346346,
0.0787116502012785));
#93427=CARTESIAN_POINT('Ctrl Pts',(0.0119587294142675,-0.0318646057455575,
0.0787644533599413));
#93428=CARTESIAN_POINT('Ctrl Pts',(0.0121450332375747,-0.0321934096636183,
0.0784886960691015));
#93429=CARTESIAN_POINT('Ctrl Pts',(0.0120851992374078,-0.0320835708272304,
0.0785441522549771));
#93430=CARTESIAN_POINT('Ctrl Pts',(0.0120242522805083,-0.0319739230346346,
0.0785983380124876));
#93431=CARTESIAN_POINT('Ctrl Pts',(0.0119622756649264,-0.0318646057455575,
0.0786511899992634));
#93432=CARTESIAN_POINT('Ctrl Pts',(0.0121438952001639,-0.0321934096636183,
0.0783753829205412));
#93433=CARTESIAN_POINT('Ctrl Pts',(0.0120856238766265,-0.0320835708272304,
0.078430823411994));
#93434=CARTESIAN_POINT('Ctrl Pts',(0.0120262390147359,-0.0319739230346346,
0.0784850258236967));
#93435=CARTESIAN_POINT('Ctrl Pts',(0.0119658219155852,-0.0318646057455575,
0.0785379266385855));
#93436=CARTESIAN_POINT('Ctrl Pts',(0.012142757162753,-0.0321934096636183,
0.078262069771981));
#93437=CARTESIAN_POINT('Ctrl Pts',(0.0120860485158452,-0.0320835708272304,
0.0783174945690109));
#93438=CARTESIAN_POINT('Ctrl Pts',(0.0120282257489634,-0.0319739230346346,
0.0783717136349058));
#93439=CARTESIAN_POINT('Ctrl Pts',(0.0119693681662441,-0.0318646057455575,
0.0784246632779076));
#93440=CARTESIAN_POINT('Ctrl Pts',(0.0122311072172625,-0.0320218834582301,
0.0781750067014124));
#93441=CARTESIAN_POINT('Ctrl Pts',(0.012189216627892,-0.0319391099350596,
0.0782177540255193));
#93442=CARTESIAN_POINT('Ctrl Pts',(0.0121466839135055,-0.0318564869454876,
0.0782598213226819));
#93443=CARTESIAN_POINT('Ctrl Pts',(0.0121035429140419,-0.0317740741446466,
0.0783011808445998));
#93444=CARTESIAN_POINT('Ctrl Pts',(0.0122806703357578,-0.0320218834582301,
0.0781755770808563));
#93445=CARTESIAN_POINT('Ctrl Pts',(0.0122387738101161,-0.0319391099350596,
0.0782188402372087));
#93446=CARTESIAN_POINT('Ctrl Pts',(0.0121962271082623,-0.0318564869454876,
0.0782614229613914));
#93447=CARTESIAN_POINT('Ctrl Pts',(0.0121530641153712,-0.0317740741446466,
0.0783032971306349));
#93448=CARTESIAN_POINT('Ctrl Pts',(0.012330233454253,-0.0320218834582301,
0.0781761474603001));
#93449=CARTESIAN_POINT('Ctrl Pts',(0.0122883309923403,-0.0319391099350596,
0.078219926448898));
#93450=CARTESIAN_POINT('Ctrl Pts',(0.0122457703030191,-0.0318564869454876,
0.0782630246001008));
#93451=CARTESIAN_POINT('Ctrl Pts',(0.0122025853167005,-0.0317740741446466,
0.07830541341667));
#93452=CARTESIAN_POINT('Ctrl Pts',(0.0123797965727482,-0.0320218834582301,
0.078176717839744));
#93453=CARTESIAN_POINT('Ctrl Pts',(0.0123378881745644,-0.0319391099350596,
0.0782210126605874));
#93454=CARTESIAN_POINT('Ctrl Pts',(0.0122953134977759,-0.0318564869454876,
0.0782646262388103));
#93455=CARTESIAN_POINT('Ctrl Pts',(0.0122521065180299,-0.0317740741446466,
0.0783075297027051));
#93456=CARTESIAN_POINT('Origin',(0.0173832508623868,-0.0391228853390823,
0.0819051826730895));
#93457=CARTESIAN_POINT('Ctrl Pts',(0.0137092015079296,-0.035272297877959,
0.0755237742246161));
#93458=CARTESIAN_POINT('Ctrl Pts',(0.0137043489676322,-0.0352466642097214,
0.0755420374535391));
#93459=CARTESIAN_POINT('Ctrl Pts',(0.0136995765223734,-0.0352210183808299,
0.075560304544644));
#93460=CARTESIAN_POINT('Ctrl Pts',(0.013694884518966,-0.0351953608940152,
0.0755785762771645));
#93461=CARTESIAN_POINT('Origin',(0.0183951094992704,-0.0352456003065037,
0.0769562579037339));
#93462=CARTESIAN_POINT('Ctrl Pts',(0.0136612048588493,-0.035024121149334,
0.075698622084724));
#93463=CARTESIAN_POINT('Ctrl Pts',(0.0136398732255539,-0.0349144232867422,
0.0757748978080736));
#93464=CARTESIAN_POINT('Ctrl Pts',(0.0136169521506141,-0.0348045283677513,
0.0758507782460351));
#93465=CARTESIAN_POINT('Ctrl Pts',(0.0135924673762274,-0.0346945769586886,
0.0759261651129022));
#93466=CARTESIAN_POINT('Ctrl Pts',(0.0137611252006477,-0.035024121149334,
0.0756451705450078));
#93467=CARTESIAN_POINT('Ctrl Pts',(0.0137405298403627,-0.0349144232867422,
0.0757228226300346));
#93468=CARTESIAN_POINT('Ctrl Pts',(0.01371831702875,-0.0348045283677513,
0.0758000954727807));
#93469=CARTESIAN_POINT('Ctrl Pts',(0.0136945115344442,-0.0346945769586886,
0.0758768890378051));
#93470=CARTESIAN_POINT('Ctrl Pts',(0.013861045542446,-0.035024121149334,
0.0755917190052915));
#93471=CARTESIAN_POINT('Ctrl Pts',(0.0138411864551714,-0.0349144232867422,
0.0756707474519956));
#93472=CARTESIAN_POINT('Ctrl Pts',(0.013819681906886,-0.0348045283677513,
0.0757494126995263));
#93473=CARTESIAN_POINT('Ctrl Pts',(0.013796555692661,-0.0346945769586886,
0.075827612962708));
#93474=CARTESIAN_POINT('Ctrl Pts',(0.0139609658842444,-0.035024121149334,
0.0755382674655752));
#93475=CARTESIAN_POINT('Ctrl Pts',(0.0139418430699802,-0.0349144232867422,
0.0756186722739566));
#93476=CARTESIAN_POINT('Ctrl Pts',(0.013921046785022,-0.0348045283677513,
0.0756987299262718));
#93477=CARTESIAN_POINT('Ctrl Pts',(0.0138985998508777,-0.0346945769586886,
0.0757783368876108));
#93478=CARTESIAN_POINT('Origin',(-0.00231867693836035,-0.0345629067947109,
0.0705690730199885));
#93479=CARTESIAN_POINT('Ctrl Pts',(0.0137483798950316,-0.0351970973651619,
0.0760313352887893));
#93480=CARTESIAN_POINT('Ctrl Pts',(0.0137223165442662,-0.0350869349321778,
0.0761092564672701));
#93481=CARTESIAN_POINT('Ctrl Pts',(0.0136946116648051,-0.034976498512973,
0.0761867003521294));
#93482=CARTESIAN_POINT('Ctrl Pts',(0.0136652952430741,-0.0348659306849652,
0.0762635644996982));
#93483=CARTESIAN_POINT('Ctrl Pts',(0.0137080298409273,-0.0351970973651619,
0.0759596949106244));
#93484=CARTESIAN_POINT('Ctrl Pts',(0.0136829589705114,-0.0350869349321778,
0.0760370570937895));
#93485=CARTESIAN_POINT('Ctrl Pts',(0.0136562590147619,-0.034976498512973,
0.0761139621533845));
#93486=CARTESIAN_POINT('Ctrl Pts',(0.0136279586992884,-0.0348659306849652,
0.076190308420442));
#93487=CARTESIAN_POINT('Ctrl Pts',(0.0136676797868229,-0.0351970973651619,
0.0758880545324594));
#93488=CARTESIAN_POINT('Ctrl Pts',(0.0136436013967566,-0.0350869349321778,
0.0759648577203089));
#93489=CARTESIAN_POINT('Ctrl Pts',(0.0136179063647187,-0.034976498512973,
0.0760412239546396));
#93490=CARTESIAN_POINT('Ctrl Pts',(0.0135906221555027,-0.0348659306849652,
0.0761170523411859));
#93491=CARTESIAN_POINT('Ctrl Pts',(0.0136273297327185,-0.0351970973651619,
0.0758164141542945));
#93492=CARTESIAN_POINT('Ctrl Pts',(0.0136042438230018,-0.0350869349321778,
0.0758926583468284));
#93493=CARTESIAN_POINT('Ctrl Pts',(0.0135795537146755,-0.034976498512973,
0.0759684857558946));
#93494=CARTESIAN_POINT('Ctrl Pts',(0.013553285611717,-0.0348659306849652,
0.0760437962619298));
#93495=CARTESIAN_POINT('Origin',(-0.00212035218267538,-0.0345637187963098,
0.0701309033624755));
#93496=CARTESIAN_POINT('Ctrl Pts',(0.0136380039084654,-0.0352450361861252,
0.0757844674588033));
#93497=CARTESIAN_POINT('Ctrl Pts',(0.0135763589582961,-0.0349452761023765,
0.0759924397381133));
#93498=CARTESIAN_POINT('Ctrl Pts',(0.0134992238123034,-0.0346444289983475,
0.0761951778403425));
#93499=CARTESIAN_POINT('Ctrl Pts',(0.013703824675012,-0.0352450361861252,
0.0755432878023411));
#93500=CARTESIAN_POINT('Ctrl Pts',(0.0136512759646145,-0.0349452761023765,
0.075753742552533));
#93501=CARTESIAN_POINT('Ctrl Pts',(0.0135830242270757,-0.0346444289983475,
0.0759596412391868));
#93502=CARTESIAN_POINT('Ctrl Pts',(0.013553039606245,-0.0345231616327822,
0.0760432629782829));
#93503=CARTESIAN_POINT('Ctrl Pts',(0.0135269436415907,-0.0344132092796975,
0.0761180976479395));
#93504=CARTESIAN_POINT('Ctrl Pts',(0.013499301127255,-0.0343032738558974,
0.0761923886820265));
#93505=CARTESIAN_POINT('Ctrl Pts',(0.0134701499144472,-0.0341934961088741,
0.0762660418122672));
#93506=CARTESIAN_POINT('Ctrl Pts',(0.0136561189977491,-0.0345231616327822,
0.0759961909570195));
#93507=CARTESIAN_POINT('Ctrl Pts',(0.0136306718546357,-0.0344132092796975,
0.0760724464309637));
#93508=CARTESIAN_POINT('Ctrl Pts',(0.0136036487401489,-0.0343032738558974,
0.0761481716163932));
#93509=CARTESIAN_POINT('Ctrl Pts',(0.0135750867590384,-0.0341934961088741,
0.0762232703873912));
#93510=CARTESIAN_POINT('Ctrl Pts',(0.0137591983892531,-0.0345231616327822,
0.0759491189357559));
#93511=CARTESIAN_POINT('Ctrl Pts',(0.0137344000676807,-0.0344132092796975,
0.0760267952139879));
#93512=CARTESIAN_POINT('Ctrl Pts',(0.0137079963530427,-0.0343032738558974,
0.0761039545507599));
#93513=CARTESIAN_POINT('Ctrl Pts',(0.0136800236036295,-0.0341934961088741,
0.0761804989625153));
#93514=CARTESIAN_POINT('Ctrl Pts',(0.0138622777807571,-0.0345231616327822,
0.0759020469144925));
#93515=CARTESIAN_POINT('Ctrl Pts',(0.0138381282807258,-0.0344132092796975,
0.0759811439970121));
#93516=CARTESIAN_POINT('Ctrl Pts',(0.0138123439659366,-0.0343032738558974,
0.0760597374851266));
#93517=CARTESIAN_POINT('Ctrl Pts',(0.0137849604482207,-0.0341934961088741,
0.0761377275376394));
#93518=CARTESIAN_POINT('Origin',(-0.00233020492228257,-0.0345625596232513,
0.0705653846762973));
#93519=CARTESIAN_POINT('Ctrl Pts',(0.0136589219806728,-0.0346945769586885,
0.0764656484042893));
#93520=CARTESIAN_POINT('Ctrl Pts',(0.0136270111752922,-0.0345846629178476,
0.0765419254281193));
#93521=CARTESIAN_POINT('Ctrl Pts',(0.0135935175419434,-0.034474692505516,
0.0766175555779037));
#93522=CARTESIAN_POINT('Ctrl Pts',(0.0135584843967371,-0.0343648066260528,
0.0766924421248161));
#93523=CARTESIAN_POINT('Ctrl Pts',(0.013609645944372,-0.0346945769586885,
0.0763636043264145));
#93524=CARTESIAN_POINT('Ctrl Pts',(0.0135791413579593,-0.0345846629178476,
0.0764392023015593));
#93525=CARTESIAN_POINT('Ctrl Pts',(0.0135470682262121,-0.034474692505516,
0.076514182366706));
#93526=CARTESIAN_POINT('Ctrl Pts',(0.0135134680416907,-0.0343648066260528,
0.0765884486184748));
#93527=CARTESIAN_POINT('Ctrl Pts',(0.0135603699080712,-0.0346945769586885,
0.0762615602485397));
#93528=CARTESIAN_POINT('Ctrl Pts',(0.0135312715406265,-0.0345846629178476,
0.0763364791749993));
#93529=CARTESIAN_POINT('Ctrl Pts',(0.0135006189104809,-0.034474692505516,
0.0764108091555083));
#93530=CARTESIAN_POINT('Ctrl Pts',(0.0134684516866442,-0.0343648066260528,
0.0764844551121334));
#93531=CARTESIAN_POINT('Ctrl Pts',(0.0135110938717704,-0.0346945769586885,
0.0761595161706649));
#93532=CARTESIAN_POINT('Ctrl Pts',(0.0134834017232937,-0.0345846629178476,
0.0762337560484393));
#93533=CARTESIAN_POINT('Ctrl Pts',(0.0134541695947496,-0.034474692505516,
0.0763074359443106));
#93534=CARTESIAN_POINT('Ctrl Pts',(0.0134234353315977,-0.0343648066260528,
0.0763804616057921));
#93535=CARTESIAN_POINT('Origin',(-0.00217502575729261,-0.0345626446729475,
0.070110289510456));
#93536=CARTESIAN_POINT('Ctrl Pts',(0.0135119755852948,-0.0346945769586886,
0.0761613420813974));
#93537=CARTESIAN_POINT('Ctrl Pts',(0.0134698472201032,-0.0345275153362891,
0.0762741999493099));
#93538=CARTESIAN_POINT('Ctrl Pts',(0.0134241586822912,-0.0343603235965159,
0.0763857621097389));
#93539=CARTESIAN_POINT('Ctrl Pts',(0.0133750500022089,-0.034193496108874,
0.076495700619667));
#93540=CARTESIAN_POINT('Ctrl Pts',(0.0135395795365018,-0.0346945769586886,
0.0760821836945452));
#93541=CARTESIAN_POINT('Ctrl Pts',(0.0134991091754161,-0.0345275153362891,
0.0761956197382678));
#93542=CARTESIAN_POINT('Ctrl Pts',(0.0134550608874577,-0.0343603235965159,
0.0763078123667558));
#93543=CARTESIAN_POINT('Ctrl Pts',(0.0134075698795593,-0.034193496108874,
0.0764184317002467));
#93544=CARTESIAN_POINT('Ctrl Pts',(0.0135671834877089,-0.0346945769586886,
0.0760030253076931));
#93545=CARTESIAN_POINT('Ctrl Pts',(0.013528371130729,-0.0345275153362891,
0.0761170395272257));
#93546=CARTESIAN_POINT('Ctrl Pts',(0.0134859630926242,-0.0343603235965159,
0.0762298626237727));
#93547=CARTESIAN_POINT('Ctrl Pts',(0.0134400897569097,-0.034193496108874,
0.0763411627808263));
#93548=CARTESIAN_POINT('Ctrl Pts',(0.0135947874389159,-0.0346945769586886,
0.0759238669208409));
#93549=CARTESIAN_POINT('Ctrl Pts',(0.0135576330860419,-0.0345275153362891,
0.0760384593161836));
#93550=CARTESIAN_POINT('Ctrl Pts',(0.0135168652977908,-0.0343603235965159,
0.0761519128807895));
#93551=CARTESIAN_POINT('Ctrl Pts',(0.0134726096342601,-0.034193496108874,
0.076263893861406));
#93552=CARTESIAN_POINT('Ctrl Pts',(0.0134234470584664,-0.0340223579322365,
0.0763804323067669));
#93553=CARTESIAN_POINT('Ctrl Pts',(0.0133926835797447,-0.0339125849573554,
0.0764535285073657));
#93554=CARTESIAN_POINT('Ctrl Pts',(0.0133604287966631,-0.0338030433565221,
0.0765259366115855));
#93555=CARTESIAN_POINT('Ctrl Pts',(0.013326732166054,-0.0336938721132328,
0.0765975676781663));
#93556=CARTESIAN_POINT('Ctrl Pts',(0.0135292788965577,-0.0340223579322365,
0.0763399254940468));
#93557=CARTESIAN_POINT('Ctrl Pts',(0.0134990741124296,-0.0339125849573554,
0.0764144813917138));
#93558=CARTESIAN_POINT('Ctrl Pts',(0.0134673474190159,-0.0338030433565221,
0.0764883597309696));
#93559=CARTESIAN_POINT('Ctrl Pts',(0.0134341477644818,-0.0336938721132328,
0.0765614696305053));
#93560=CARTESIAN_POINT('Ctrl Pts',(0.013635110734649,-0.0340223579322365,
0.0762994186813266));
#93561=CARTESIAN_POINT('Ctrl Pts',(0.0136054646451145,-0.0339125849573554,
0.076375434276062));
#93562=CARTESIAN_POINT('Ctrl Pts',(0.0135742660413688,-0.0338030433565221,
0.0764507828503537));
#93563=CARTESIAN_POINT('Ctrl Pts',(0.0135415633629095,-0.0336938721132328,
0.0765253715828443));
#93564=CARTESIAN_POINT('Ctrl Pts',(0.0137409425727403,-0.0340223579322365,
0.0762589118686065));
#93565=CARTESIAN_POINT('Ctrl Pts',(0.0137118551777994,-0.0339125849573554,
0.0763363871604101));
#93566=CARTESIAN_POINT('Ctrl Pts',(0.0136811846637216,-0.0338030433565221,
0.0764132059697378));
#93567=CARTESIAN_POINT('Ctrl Pts',(0.0136489789613373,-0.0336938721132328,
0.0764892735351833));
#93568=CARTESIAN_POINT('Origin',(-0.00221735192247542,-0.0345589643412543,
0.0706068223244746));
#93569=CARTESIAN_POINT('Ctrl Pts',(0.013502598880332,-0.034193496108874,
0.0768086333040515));
#93570=CARTESIAN_POINT('Ctrl Pts',(0.0134659379014492,-0.0340836138581107,
0.0768828040009596));
#93571=CARTESIAN_POINT('Ctrl Pts',(0.0134277597062521,-0.0339738896643499,
0.0769561804873401));
#93572=CARTESIAN_POINT('Ctrl Pts',(0.0133881194535538,-0.0338644633294062,
0.0770286721259033));
#93573=CARTESIAN_POINT('Ctrl Pts',(0.0134598274169694,-0.034193496108874,
0.076703696365036));
#93574=CARTESIAN_POINT('Ctrl Pts',(0.0134246134563345,-0.0340836138581107,
0.0767772772687925));
#93575=CARTESIAN_POINT('Ctrl Pts',(0.0133878937896103,-0.0339738896643499,
0.0768500941880218));
#93576=CARTESIAN_POINT('Ctrl Pts',(0.013349721660865,-0.0338644633294062,
0.0769220570764743));
#93577=CARTESIAN_POINT('Ctrl Pts',(0.0134170559536069,-0.034193496108874,
0.0765987594260205));
#93578=CARTESIAN_POINT('Ctrl Pts',(0.0133832890112198,-0.0340836138581107,
0.0766717505366255));
#93579=CARTESIAN_POINT('Ctrl Pts',(0.0133480278729686,-0.0339738896643499,
0.0767440078887034));
#93580=CARTESIAN_POINT('Ctrl Pts',(0.0133113238681763,-0.0338644633294062,
0.0768154420270453));
#93581=CARTESIAN_POINT('Ctrl Pts',(0.0133742844902443,-0.034193496108874,
0.076493822487005));
#93582=CARTESIAN_POINT('Ctrl Pts',(0.0133419645661051,-0.0340836138581107,
0.0765662238044585));
#93583=CARTESIAN_POINT('Ctrl Pts',(0.0133081619563269,-0.0339738896643499,
0.0766379215893851));
#93584=CARTESIAN_POINT('Ctrl Pts',(0.0132729260754875,-0.0338644633294062,
0.0767088269776163));
#93585=CARTESIAN_POINT('Origin',(-0.0021053722911509,-0.0345610621863108,
0.0701388366693302));
#93586=CARTESIAN_POINT('Ctrl Pts',(0.0133897010974836,-0.03424362768739,
0.0764626225573025));
#93587=CARTESIAN_POINT('Ctrl Pts',(0.0133024790998638,-0.033943005420186,
0.0766612299628616));
#93588=CARTESIAN_POINT('Ctrl Pts',(0.0132005449672405,-0.0336441434784163,
0.076852703227361));
#93589=CARTESIAN_POINT('Ctrl Pts',(0.0134852275204704,-0.03424362768739,
0.0762315929000909));
#93590=CARTESIAN_POINT('Ctrl Pts',(0.0134067189500149,-0.033943005420186,
0.0764338031440864));
#93591=CARTESIAN_POINT('Ctrl Pts',(0.0133132021100695,-0.0336441434784163,
0.0766295253427721));
#93592=CARTESIAN_POINT('Ctrl Pts',(0.0132729383030164,-0.0335235895815127,
0.0767088020875533));
#93593=CARTESIAN_POINT('Ctrl Pts',(0.013237711354464,-0.0334144449262719,
0.0767796903591607));
#93594=CARTESIAN_POINT('Ctrl Pts',(0.0132009794360736,-0.0333049234473133,
0.0768499323105579));
#93595=CARTESIAN_POINT('Ctrl Pts',(0.0131627813805983,-0.0331951640388588,
0.0769194338692133));
#93596=CARTESIAN_POINT('Ctrl Pts',(0.0133811047344406,-0.0335235895815127,
0.0766750205008595));
#93597=CARTESIAN_POINT('Ctrl Pts',(0.0133463428559389,-0.0334144449262719,
0.0767473978963555));
#93598=CARTESIAN_POINT('Ctrl Pts',(0.0133100457777294,-0.0333049234473133,
0.0768191402904615));
#93599=CARTESIAN_POINT('Ctrl Pts',(0.0132722516027427,-0.0331951640388588,
0.0768901517424077));
#93600=CARTESIAN_POINT('Ctrl Pts',(0.0134892711658648,-0.0335235895815127,
0.0766412389141656));
#93601=CARTESIAN_POINT('Ctrl Pts',(0.0134549743574137,-0.0334144449262719,
0.0767151054335503));
#93602=CARTESIAN_POINT('Ctrl Pts',(0.0134191121193851,-0.0333049234473133,
0.0767883482703651));
#93603=CARTESIAN_POINT('Ctrl Pts',(0.013381721824887,-0.0331951640388588,
0.0768608696156021));
#93604=CARTESIAN_POINT('Ctrl Pts',(0.0135974375972889,-0.0335235895815127,
0.0766074573274718));
#93605=CARTESIAN_POINT('Ctrl Pts',(0.0135636058588885,-0.0334144449262719,
0.0766828129707451));
#93606=CARTESIAN_POINT('Ctrl Pts',(0.0135281784610409,-0.0333049234473133,
0.0767575562502687));
#93607=CARTESIAN_POINT('Ctrl Pts',(0.0134911920470314,-0.0331951640388588,
0.0768315874887965));
#93608=CARTESIAN_POINT('Origin',(-0.00106178345708809,-0.0326434571771455,
0.0682330884781778));
#93609=CARTESIAN_POINT('Ctrl Pts',(0.0133256939357804,-0.0336938721132431,
0.077143047737031));
#93610=CARTESIAN_POINT('Ctrl Pts',(0.0133081746341762,-0.0336474569764979,
0.0771734962526395));
#93611=CARTESIAN_POINT('Ctrl Pts',(0.0132903000946864,-0.033601104548885,
0.0772037375963512));
#93612=CARTESIAN_POINT('Ctrl Pts',(0.0132450458722633,-0.0334837508643191,
0.0772803017224079));
#93613=CARTESIAN_POINT('Ctrl Pts',(0.0131975427684567,-0.0333660264760466,
0.0773554912507659));
#93614=CARTESIAN_POINT('Ctrl Pts',(0.01321740006416,-0.0336938721132431,
0.0768208017492327));
#93615=CARTESIAN_POINT('Ctrl Pts',(0.0132017669752551,-0.0336474569764979,
0.0768506163848749));
#93616=CARTESIAN_POINT('Ctrl Pts',(0.0131857859395853,-0.033601104548885,
0.0768802459725553));
#93617=CARTESIAN_POINT('Ctrl Pts',(0.0131453256332841,-0.0334837508643191,
0.076955261273059));
#93618=CARTESIAN_POINT('Ctrl Pts',(0.0131026602353754,-0.0333660264760466,
0.0770290447096619));
#93619=CARTESIAN_POINT('Ctrl Pts',(0.0132174000641665,-0.0336938721132426,
0.0768208017492494));
#93620=CARTESIAN_POINT('Ctrl Pts',(0.0132017669752633,-0.0336474569765026,
0.0768506163848883));
#93621=CARTESIAN_POINT('Ctrl Pts',(0.0131857859395953,-0.0336011045488949,
0.0768802459725653));
#93622=CARTESIAN_POINT('Ctrl Pts',(0.0131456626125359,-0.0334847282606778,
0.0769546364977918));
#93623=CARTESIAN_POINT('Ctrl Pts',(0.0131033706183091,-0.0333679869945434,
0.0770278158585576));
#93624=CARTESIAN_POINT('Ctrl Pts',(0.0132174000641599,-0.0336938721132429,
0.0768208017492329));
#93625=CARTESIAN_POINT('Ctrl Pts',(0.0131614892199085,-0.0335278710435085,
0.0769274320805731));
#93626=CARTESIAN_POINT('Ctrl Pts',(0.0131022541454949,-0.0333620469224321,
0.0770322715500714));
#93627=CARTESIAN_POINT('Ctrl Pts',(0.0130396479434203,-0.0331951640388602,
0.07713536244448));
#93628=CARTESIAN_POINT('Ctrl Pts',(0.0132547075305147,-0.0336938721132429,
0.0767457272343995));
#93629=CARTESIAN_POINT('Ctrl Pts',(0.0132003683040395,-0.0335278710435085,
0.0768531385641577));
#93630=CARTESIAN_POINT('Ctrl Pts',(0.0131426798026034,-0.0333620469224321,
0.0769588080428453));
#93631=CARTESIAN_POINT('Ctrl Pts',(0.0130815957598022,-0.0331951640388602,
0.0770627786272473));
#93632=CARTESIAN_POINT('Ctrl Pts',(0.0132920149968694,-0.0336938721132429,
0.0766706527195662));
#93633=CARTESIAN_POINT('Ctrl Pts',(0.0132392473881706,-0.0335278710435085,
0.0767788450477423));
#93634=CARTESIAN_POINT('Ctrl Pts',(0.013183105459712,-0.0333620469224321,
0.0768853445356193));
#93635=CARTESIAN_POINT('Ctrl Pts',(0.013123543576184,-0.0331951640388602,
0.0769901948100146));
#93636=CARTESIAN_POINT('Ctrl Pts',(0.0133293224632242,-0.0336938721132429,
0.0765955782047328));
#93637=CARTESIAN_POINT('Ctrl Pts',(0.0132781264723017,-0.0335278710435085,
0.0767045515313269));
#93638=CARTESIAN_POINT('Ctrl Pts',(0.0132235311168205,-0.0333620469224321,
0.0768118810283932));
#93639=CARTESIAN_POINT('Ctrl Pts',(0.0131654913925659,-0.0331951640388602,
0.0769176109927819));
#93640=CARTESIAN_POINT('Ctrl Pts',(0.013102110037377,-0.0330240426238155,
0.0770270701512004));
#93641=CARTESIAN_POINT('Ctrl Pts',(0.0130624755930508,-0.0329142774063509,
0.0770956514674047));
#93642=CARTESIAN_POINT('Ctrl Pts',(0.0130214036221302,-0.0328043479726686,
0.0771634476192186));
#93643=CARTESIAN_POINT('Ctrl Pts',(0.0129789443489825,-0.0326943950436594,
0.0772303703056803));
#93644=CARTESIAN_POINT('Ctrl Pts',(0.0132121840296781,-0.0330240426238155,
0.0770001470718097));
#93645=CARTESIAN_POINT('Ctrl Pts',(0.0131729204770003,-0.0329142774063509,
0.0770702447644978));
#93646=CARTESIAN_POINT('Ctrl Pts',(0.0131321882348935,-0.0328043479726686,
0.0771395657161309));
#93647=CARTESIAN_POINT('Ctrl Pts',(0.0130900370387112,-0.0326943950436594,
0.0772080196843509));
#93648=CARTESIAN_POINT('Ctrl Pts',(0.0133222580219791,-0.0330240426238155,
0.0769732239924189));
#93649=CARTESIAN_POINT('Ctrl Pts',(0.0132833653609499,-0.0329142774063509,
0.0770448380615909));
#93650=CARTESIAN_POINT('Ctrl Pts',(0.0132429728476568,-0.0328043479726686,
0.0771156838130433));
#93651=CARTESIAN_POINT('Ctrl Pts',(0.0132011297284398,-0.0326943950436594,
0.0771856690630216));
#93652=CARTESIAN_POINT('Ctrl Pts',(0.0134323320142801,-0.0330240426238155,
0.0769463009130282));
#93653=CARTESIAN_POINT('Ctrl Pts',(0.0133938102448994,-0.0329142774063509,
0.0770194313586839));
#93654=CARTESIAN_POINT('Ctrl Pts',(0.0133537574604201,-0.0328043479726686,
0.0770918019099556));
#93655=CARTESIAN_POINT('Ctrl Pts',(0.0133122224181685,-0.0326943950436594,
0.0771633184416921));
#93656=CARTESIAN_POINT('Origin',(-0.00116722503613692,-0.0326396682859212,
0.0681684551100529));
#93657=CARTESIAN_POINT('Ctrl Pts',(0.0131269701953199,-0.0331951640388587,
0.0774618136745128));
#93658=CARTESIAN_POINT('Ctrl Pts',(0.013081356661698,-0.0330855618255041,
0.0775307224678763));
#93659=CARTESIAN_POINT('Ctrl Pts',(0.013034286018948,-0.0329757224427708,
0.0775987381828553));
#93660=CARTESIAN_POINT('Ctrl Pts',(0.0129858142715051,-0.0328657862078596,
0.0776657707645413));
#93661=CARTESIAN_POINT('Ctrl Pts',(0.0130976880918259,-0.0331951640388587,
0.0773523435395182));
#93662=CARTESIAN_POINT('Ctrl Pts',(0.0130535822878572,-0.0330855618255041,
0.0774208490311433));
#93663=CARTESIAN_POINT('Ctrl Pts',(0.0130080287972194,-0.0329757224427708,
0.077488492315844));
#93664=CARTESIAN_POINT('Ctrl Pts',(0.0129610817049368,-0.0328657862078596,
0.0775551839109298));
#93665=CARTESIAN_POINT('Ctrl Pts',(0.0130684059883319,-0.0331951640388587,
0.0772428734045236));
#93666=CARTESIAN_POINT('Ctrl Pts',(0.0130258079140165,-0.0330855618255041,
0.0773109755944103));
#93667=CARTESIAN_POINT('Ctrl Pts',(0.0129817715754907,-0.0329757224427708,
0.0773782464488327));
#93668=CARTESIAN_POINT('Ctrl Pts',(0.0129363491383684,-0.0328657862078596,
0.0774445970573182));
#93669=CARTESIAN_POINT('Ctrl Pts',(0.0130391238848379,-0.0331951640388587,
0.077133403269529));
#93670=CARTESIAN_POINT('Ctrl Pts',(0.0129980335401758,-0.0330855618255041,
0.0772011021576773));
#93671=CARTESIAN_POINT('Ctrl Pts',(0.012955514353762,-0.0329757224427708,
0.0772680005818214));
#93672=CARTESIAN_POINT('Ctrl Pts',(0.0129116165718001,-0.0328657862078596,
0.0773340102037066));
#93673=CARTESIAN_POINT('Origin',(-0.000875325020341547,-0.0326401908829857,
0.0677862676517416));
#93674=CARTESIAN_POINT('Ctrl Pts',(0.0130582920642887,-0.0332451089994433,
0.0771044436584957));
#93675=CARTESIAN_POINT('Ctrl Pts',(0.0129468633986402,-0.0329451141710258,
0.0772905517431748));
#93676=CARTESIAN_POINT('Ctrl Pts',(0.0128217328683168,-0.0326442513127503,
0.0774677378518065));
#93677=CARTESIAN_POINT('Ctrl Pts',(0.0131820236641183,-0.0332451089994433,
0.0768872099336655));
#93678=CARTESIAN_POINT('Ctrl Pts',(0.013078788102448,-0.0329451141710258,
0.0770779846319819));
#93679=CARTESIAN_POINT('Ctrl Pts',(0.0129614758919426,-0.0326442513127503,
0.0772604412349795));
#93680=CARTESIAN_POINT('Ctrl Pts',(0.0129116341381032,-0.0325229783203385,
0.0773339839509843));
#93681=CARTESIAN_POINT('Ctrl Pts',(0.0128677429897669,-0.032413025311208,
0.0773999843841413));
#93682=CARTESIAN_POINT('Ctrl Pts',(0.0128224931946646,-0.0323031222247695,
0.0774650668622706));
#93683=CARTESIAN_POINT('Ctrl Pts',(0.0127759456562771,-0.0321934096636184,
0.0775291500646277));
#93684=CARTESIAN_POINT('Ctrl Pts',(0.0130231814644182,-0.0325229783203385,
0.077314025578261));
#93685=CARTESIAN_POINT('Ctrl Pts',(0.0129795654418084,-0.032413025311208,
0.0773815636888438));
#93686=CARTESIAN_POINT('Ctrl Pts',(0.0129345589218722,-0.0323031222247695,
0.0774481893025091));
#93687=CARTESIAN_POINT('Ctrl Pts',(0.0128882225662215,-0.0321934096636184,
0.0775138191108694));
#93688=CARTESIAN_POINT('Ctrl Pts',(0.0131347287907332,-0.0325229783203385,
0.0772940672055376));
#93689=CARTESIAN_POINT('Ctrl Pts',(0.01309138789385,-0.032413025311208,
0.0773631429935464));
#93690=CARTESIAN_POINT('Ctrl Pts',(0.0130466246490798,-0.0323031222247695,
0.0774313117427476));
#93691=CARTESIAN_POINT('Ctrl Pts',(0.0130004994761659,-0.0321934096636184,
0.0774984881571111));
#93692=CARTESIAN_POINT('Ctrl Pts',(0.0132462761170482,-0.0325229783203385,
0.0772741088328143));
#93693=CARTESIAN_POINT('Ctrl Pts',(0.0132032103458915,-0.032413025311208,
0.0773447222982489));
#93694=CARTESIAN_POINT('Ctrl Pts',(0.0131586903762874,-0.0323031222247695,
0.0774144341829861));
#93695=CARTESIAN_POINT('Ctrl Pts',(0.0131127763861102,-0.0321934096636184,
0.0774831572033528));
#93696=CARTESIAN_POINT('Origin',(-0.00116018816837294,-0.0326393375179027,
0.0681732689983203));
#93697=CARTESIAN_POINT('Ctrl Pts',(0.0129091470454595,-0.0326943950436593,
0.0777694313406965));
#93698=CARTESIAN_POINT('Ctrl Pts',(0.0128592644980476,-0.0325844576448127,
0.0778353826370912));
#93699=CARTESIAN_POINT('Ctrl Pts',(0.0128080144394322,-0.0324744968375319,
0.0779003069480977));
#93700=CARTESIAN_POINT('Ctrl Pts',(0.0127554636815458,-0.0323646534831895,
0.0779641219946141));
#93701=CARTESIAN_POINT('Ctrl Pts',(0.0128867964314425,-0.0326943950436593,
0.0776583386873139));
#93702=CARTESIAN_POINT('Ctrl Pts',(0.012838444949004,-0.0325844576448127,
0.077723981950358));
#93703=CARTESIAN_POINT('Ctrl Pts',(0.0127887324343526,-0.0324744968375319,
0.0777886298711476));
#93704=CARTESIAN_POINT('Ctrl Pts',(0.0127377237245454,-0.0323646534831895,
0.0778522004975362));
#93705=CARTESIAN_POINT('Ctrl Pts',(0.0128644458174256,-0.0326943950436593,
0.0775472460339312));
#93706=CARTESIAN_POINT('Ctrl Pts',(0.0128176253999605,-0.0325844576448127,
0.0776125812636247));
#93707=CARTESIAN_POINT('Ctrl Pts',(0.0127694504292731,-0.0324744968375319,
0.0776769527941975));
#93708=CARTESIAN_POINT('Ctrl Pts',(0.0127199837675449,-0.0323646534831895,
0.0777402790004584));
#93709=CARTESIAN_POINT('Ctrl Pts',(0.0128420952034086,-0.0326943950436593,
0.0774361533805486));
#93710=CARTESIAN_POINT('Ctrl Pts',(0.012796805850917,-0.0325844576448127,
0.0775011805768914));
#93711=CARTESIAN_POINT('Ctrl Pts',(0.0127501684241935,-0.0324744968375319,
0.0775652757172474));
#93712=CARTESIAN_POINT('Ctrl Pts',(0.0127022438105445,-0.0323646534831895,
0.0776283575033805));
#93713=CARTESIAN_POINT('Origin',(-0.000906483761463371,-0.0326395579068527,
0.0677647945357601));
#93714=CARTESIAN_POINT('Ctrl Pts',(0.0128630661060209,-0.0327445246961876,
0.0774084218561767));
#93715=CARTESIAN_POINT('Ctrl Pts',(0.0127401727179607,-0.0324436878365475,
0.0775871668691753));
#93716=CARTESIAN_POINT('Ctrl Pts',(0.0126041646522502,-0.0321434074463188,
0.0777561472543167));
#93717=CARTESIAN_POINT('Ctrl Pts',(0.0130001923426494,-0.0327445246961876,
0.077199385028732));
#93718=CARTESIAN_POINT('Ctrl Pts',(0.0128851829073392,-0.0324436878365475,
0.0773833018422387));
#93719=CARTESIAN_POINT('Ctrl Pts',(0.0127566468357546,-0.0321434074463188,
0.0775580331868864));
#93720=CARTESIAN_POINT('Ctrl Pts',(0.0126456622767151,-0.0322357242816073,
0.0777039732004452));
#93721=CARTESIAN_POINT('Ctrl Pts',(0.0125324728396152,-0.0319819883628706,
0.0778479892164446));
#93722=CARTESIAN_POINT('Ctrl Pts',(0.0124103486438636,-0.0317295851069886,
0.0779845107984281));
#93723=CARTESIAN_POINT('Ctrl Pts',(0.0127958378904485,-0.0322357242816073,
0.0775041050312941));
#93724=CARTESIAN_POINT('Ctrl Pts',(0.0126890139953167,-0.0319819883628706,
0.0776529039458202));
#93725=CARTESIAN_POINT('Ctrl Pts',(0.0125729380914563,-0.0317295851069886,
0.0777946037908388));
#93726=CARTESIAN_POINT('Origin',(-0.000829665997267067,-0.0326371942646419,
0.0678211987429648));
#93727=CARTESIAN_POINT('Origin',(-0.00105859556252852,-0.0326352985529724,
0.0682421365922654));
#93728=CARTESIAN_POINT('Ctrl Pts',(0.0126724382467534,-0.0321934096636183,
0.0780627647649452));
#93729=CARTESIAN_POINT('Ctrl Pts',(0.0126184781712214,-0.0320835708272304,
0.0781254942769318));
#93730=CARTESIAN_POINT('Ctrl Pts',(0.0125632512107361,-0.0319739230346346,
0.0781870707022936));
#93731=CARTESIAN_POINT('Ctrl Pts',(0.0125068340707187,-0.0318646057455575,
0.0782474206811522));
#93732=CARTESIAN_POINT('Ctrl Pts',(0.012657107279793,-0.0321934096636183,
0.0779504877583147));
#93733=CARTESIAN_POINT('Ctrl Pts',(0.0126046955916858,-0.0320835708272304,
0.0780130058443187));
#93734=CARTESIAN_POINT('Ctrl Pts',(0.0125510204959474,-0.0319739230346346,
0.0780744030101308));
#93735=CARTESIAN_POINT('Ctrl Pts',(0.0124961566948937,-0.0318646057455575,
0.078134605972841));
#93736=CARTESIAN_POINT('Ctrl Pts',(0.0126417763128326,-0.0321934096636183,
0.0778382107516842));
#93737=CARTESIAN_POINT('Ctrl Pts',(0.0125909130121503,-0.0320835708272303,
0.0779005174117056));
#93738=CARTESIAN_POINT('Ctrl Pts',(0.0125387897811587,-0.0319739230346346,
0.077961735317968));
#93739=CARTESIAN_POINT('Ctrl Pts',(0.0124854793190688,-0.0318646057455575,
0.0780217912645298));
#93740=CARTESIAN_POINT('Ctrl Pts',(0.0126264453458722,-0.0321934096636183,
0.0777259337450536));
#93741=CARTESIAN_POINT('Ctrl Pts',(0.0125771304326147,-0.0320835708272303,
0.0777880289790925));
#93742=CARTESIAN_POINT('Ctrl Pts',(0.01252655906637,-0.0319739230346346,
0.0778490676258052));
#93743=CARTESIAN_POINT('Ctrl Pts',(0.0124748019432438,-0.0318646057455575,
0.0779089765562186));
#93744=CARTESIAN_POINT('Ctrl Pts',(0.0127031868376533,-0.0320218834582296,
0.077628483994784));
#93745=CARTESIAN_POINT('Ctrl Pts',(0.0126669842284488,-0.0319391099350593,
0.077676144526494));
#93746=CARTESIAN_POINT('Ctrl Pts',(0.0126300593276,-0.0318564869454876,
0.0777232108730797));
#93747=CARTESIAN_POINT('Ctrl Pts',(0.0125924422304235,-0.031774074144647,
0.0777696512637756));
#93748=CARTESIAN_POINT('Ctrl Pts',(0.0127524306236555,-0.0320218834582296,
0.0776228379707091));
#93749=CARTESIAN_POINT('Ctrl Pts',(0.0127162867759124,-0.0319391099350593,
0.0776710110111852));
#93750=CARTESIAN_POINT('Ctrl Pts',(0.0126794125980267,-0.0318564869454876,
0.0777185904735896));
#93751=CARTESIAN_POINT('Ctrl Pts',(0.012641838183261,-0.031774074144647,
0.0777655442099706));
#93752=CARTESIAN_POINT('Ctrl Pts',(0.0128016744096576,-0.0320218834582296,
0.0776171919466342));
#93753=CARTESIAN_POINT('Ctrl Pts',(0.012765589323376,-0.0319391099350593,
0.0776658774958765));
#93754=CARTESIAN_POINT('Ctrl Pts',(0.0127287658684534,-0.0318564869454876,
0.0777139700740995));
#93755=CARTESIAN_POINT('Ctrl Pts',(0.0126912341360985,-0.031774074144647,
0.0777614371561656));
#93756=CARTESIAN_POINT('Ctrl Pts',(0.0128509181956598,-0.0320218834582296,
0.0776115459225593));
#93757=CARTESIAN_POINT('Ctrl Pts',(0.0128148918708396,-0.0319391099350593,
0.0776607439805678));
#93758=CARTESIAN_POINT('Ctrl Pts',(0.0127781191388802,-0.0318564869454876,
0.0777093496746093));
#93759=CARTESIAN_POINT('Ctrl Pts',(0.012740630088936,-0.031774074144647,
0.0777573301023607));
#93760=CARTESIAN_POINT('Origin',(0.0182822193075388,-0.0391228853390615,
0.0806835115919135));
#93761=CARTESIAN_POINT('Ctrl Pts',(0.0138373383741067,-0.0352722978779582,
0.0748129029409901));
#93762=CARTESIAN_POINT('Ctrl Pts',(0.0138348130870752,-0.0352466642097209,
0.0748316303434644));
#93763=CARTESIAN_POINT('Ctrl Pts',(0.0138323677475688,-0.0352210183808297,
0.0748503515390959));
#93764=CARTESIAN_POINT('Ctrl Pts',(0.0138300027973293,-0.0351953608940152,
0.0748690672575067));
#93765=CARTESIAN_POINT('Origin',(0.0186658343928198,-0.0352456003065022,
0.0756467910576931));
#93766=CARTESIAN_POINT('Ctrl Pts',(0.0138116344406295,-0.035024121149334,
0.0749923876487254));
#93767=CARTESIAN_POINT('Ctrl Pts',(0.0138000308966839,-0.0349144232867422,
0.0750707354777921));
#93768=CARTESIAN_POINT('Ctrl Pts',(0.0137868009019202,-0.0348045283677513,
0.0751488903482748));
#93769=CARTESIAN_POINT('Ctrl Pts',(0.0137719576770855,-0.0346945769586886,
0.0752267515231267));
#93770=CARTESIAN_POINT('Ctrl Pts',(0.013904067626376,-0.035024121149334,
0.0749268342508288));
#93771=CARTESIAN_POINT('Ctrl Pts',(0.0138933670535677,-0.0349144232867422,
0.0750064553090727));
#93772=CARTESIAN_POINT('Ctrl Pts',(0.0138810142518574,-0.0348045283677513,
0.0750859028358794));
#93773=CARTESIAN_POINT('Ctrl Pts',(0.0138670212568059,-0.0346945769586886,
0.0751650744802844));
#93774=CARTESIAN_POINT('Ctrl Pts',(0.0139965008121224,-0.035024121149334,
0.0748612808529322));
#93775=CARTESIAN_POINT('Ctrl Pts',(0.0139867032104516,-0.0349144232867422,
0.0749421751403532));
#93776=CARTESIAN_POINT('Ctrl Pts',(0.0139752276017946,-0.0348045283677513,
0.0750229153234839));
#93777=CARTESIAN_POINT('Ctrl Pts',(0.0139620848365264,-0.0346945769586886,
0.0751033974374421));
#93778=CARTESIAN_POINT('Ctrl Pts',(0.0140889339978689,-0.035024121149334,
0.0747957274550357));
#93779=CARTESIAN_POINT('Ctrl Pts',(0.0140800393673354,-0.0349144232867422,
0.0748778949716338));
#93780=CARTESIAN_POINT('Ctrl Pts',(0.0140694409517319,-0.0348045283677513,
0.0749599278110884));
#93781=CARTESIAN_POINT('Ctrl Pts',(0.0140571484162468,-0.0346945769586886,
0.0750417203945998));
#93782=CARTESIAN_POINT('Origin',(-0.00268514418653433,-0.0345629067947195,
0.0719060968681436));
#93783=CARTESIAN_POINT('Ctrl Pts',(0.0139398220973284,-0.0351970973651623,
0.0753115513806286));
#93784=CARTESIAN_POINT('Ctrl Pts',(0.0139237303771306,-0.0350869349321781,
0.0753921247313721));
#93785=CARTESIAN_POINT('Ctrl Pts',(0.0139059502514284,-0.0349764985129732,
0.0754724302901964));
#93786=CARTESIAN_POINT('Ctrl Pts',(0.013886498630599,-0.0348659306849652,
0.0755523626629356));
#93787=CARTESIAN_POINT('Ctrl Pts',(0.0138908112952035,-0.0351970973651623,
0.0752455331109989));
#93788=CARTESIAN_POINT('Ctrl Pts',(0.0138756341686609,-0.0350869349321781,
0.0753254274835004));
#93789=CARTESIAN_POINT('Ctrl Pts',(0.0138587835098339,-0.0349764985129732,
0.0754050725155202));
#93790=CARTESIAN_POINT('Ctrl Pts',(0.0138402750753216,-0.0348659306849652,
0.0754843637395078));
#93791=CARTESIAN_POINT('Ctrl Pts',(0.0138418004930787,-0.0351970973651623,
0.0751795148413693));
#93792=CARTESIAN_POINT('Ctrl Pts',(0.0138275379601911,-0.0350869349321781,
0.0752587302356287));
#93793=CARTESIAN_POINT('Ctrl Pts',(0.0138116167682393,-0.0349764985129732,
0.075337714740844));
#93794=CARTESIAN_POINT('Ctrl Pts',(0.0137940515200442,-0.0348659306849652,
0.07541636481608));
#93795=CARTESIAN_POINT('Ctrl Pts',(0.0137927896909538,-0.0351970973651623,
0.0751134965717397));
#93796=CARTESIAN_POINT('Ctrl Pts',(0.0137794417517213,-0.0350869349321781,
0.075192032987757));
#93797=CARTESIAN_POINT('Ctrl Pts',(0.0137644500266448,-0.0349764985129732,
0.0752703569661678));
#93798=CARTESIAN_POINT('Ctrl Pts',(0.0137478279647668,-0.0348659306849652,
0.0753483658926522));
#93799=CARTESIAN_POINT('Origin',(-0.00254330050109684,-0.0345637187962885,
0.0714465256262351));
#93800=CARTESIAN_POINT('Ctrl Pts',(0.013799375714989,-0.0352450361861252,
0.0750804639565227));
#93801=CARTESIAN_POINT('Ctrl Pts',(0.013764282691922,-0.0349452761023764,
0.0752945224732297));
#93802=CARTESIAN_POINT('Ctrl Pts',(0.0137131656015136,-0.0346444289983475,
0.0755053295222366));
#93803=CARTESIAN_POINT('Ctrl Pts',(0.0138344496389174,-0.0352450361861252,
0.0748329365441815));
#93804=CARTESIAN_POINT('Ctrl Pts',(0.0138086922651574,-0.0349452761023764,
0.0750483178956022));
#93805=CARTESIAN_POINT('Ctrl Pts',(0.0137667846611399,-0.0346444289983475,
0.075261147220575));
#93806=CARTESIAN_POINT('Ctrl Pts',(0.0137475170609577,-0.0345231616327823,
0.0753478676467675));
#93807=CARTESIAN_POINT('Ctrl Pts',(0.0137310061419098,-0.0344132092796976,
0.0754253829143349));
#93808=CARTESIAN_POINT('Ctrl Pts',(0.0137128927325831,-0.0343032738558974,
0.075502552667134));
#93809=CARTESIAN_POINT('Ctrl Pts',(0.0136932025707705,-0.0341934961088741,
0.0755792786362073));
#93810=CARTESIAN_POINT('Ctrl Pts',(0.0138438839520356,-0.0345231616327823,
0.0752882475290006));
#93811=CARTESIAN_POINT('Ctrl Pts',(0.0138281948123727,-0.0344132092796976,
0.0753670910784878));
#93812=CARTESIAN_POINT('Ctrl Pts',(0.0138108756655672,-0.0343032738558974,
0.0754456060425318));
#93813=CARTESIAN_POINT('Ctrl Pts',(0.0137919512760146,-0.0341934961088741,
0.0755236924027393));
#93814=CARTESIAN_POINT('Ctrl Pts',(0.0139402508431135,-0.0345231616327823,
0.0752286274112337));
#93815=CARTESIAN_POINT('Ctrl Pts',(0.0139253834828356,-0.0344132092796976,
0.0753087992426407));
#93816=CARTESIAN_POINT('Ctrl Pts',(0.0139088585985512,-0.0343032738558974,
0.0753886594179296));
#93817=CARTESIAN_POINT('Ctrl Pts',(0.0138906999812588,-0.0341934961088741,
0.0754681061692713));
#93818=CARTESIAN_POINT('Ctrl Pts',(0.0140366177341914,-0.0345231616327823,
0.0751690072934668));
#93819=CARTESIAN_POINT('Ctrl Pts',(0.0140225721532985,-0.0344132092796976,
0.0752505074067936));
#93820=CARTESIAN_POINT('Ctrl Pts',(0.0140068415315353,-0.0343032738558974,
0.0753317127933274));
#93821=CARTESIAN_POINT('Ctrl Pts',(0.013989448686503,-0.0341934961088741,
0.0754125199358033));
#93822=CARTESIAN_POINT('Origin',(-0.0026970435407176,-0.0345625596231899,
0.0719038824475933));
#93823=CARTESIAN_POINT('Ctrl Pts',(0.0139055034524896,-0.0346945769586885,
0.0757536518571653));
#93824=CARTESIAN_POINT('Ctrl Pts',(0.0138834043193351,-0.0345846629176052,
0.0758333268984792));
#93825=CARTESIAN_POINT('Ctrl Pts',(0.0138596537644608,-0.0344746925050311,
0.075912558547488));
#93826=CARTESIAN_POINT('Ctrl Pts',(0.0138342826390803,-0.0343648066253259,
0.0759912454091523));
#93827=CARTESIAN_POINT('Ctrl Pts',(0.0138438264582068,-0.0346945769586885,
0.0756585883522903));
#93828=CARTESIAN_POINT('Ctrl Pts',(0.0138230373481992,-0.0345846629176052,
0.0757374134534485));
#93829=CARTESIAN_POINT('Ctrl Pts',(0.0138006146166402,-0.0344746925050311,
0.0758158221078704));
#93830=CARTESIAN_POINT('Ctrl Pts',(0.0137765874090285,-0.0343648066253259,
0.0758937139680057));
#93831=CARTESIAN_POINT('Ctrl Pts',(0.0137821494639241,-0.0346945769586885,
0.0755635248474153));
#93832=CARTESIAN_POINT('Ctrl Pts',(0.0137626703770633,-0.0345846629176052,
0.0756415000084178));
#93833=CARTESIAN_POINT('Ctrl Pts',(0.0137415754688197,-0.0344746925050311,
0.0757190856682528));
#93834=CARTESIAN_POINT('Ctrl Pts',(0.0137188921789766,-0.0343648066253259,
0.0757961825268591));
#93835=CARTESIAN_POINT('Ctrl Pts',(0.0137204724696414,-0.0346945769586885,
0.0754684613425404));
#93836=CARTESIAN_POINT('Ctrl Pts',(0.0137023034059274,-0.0345846629176052,
0.0755455865633871));
#93837=CARTESIAN_POINT('Ctrl Pts',(0.0136825363209992,-0.0344746925050311,
0.0756223492286352));
#93838=CARTESIAN_POINT('Ctrl Pts',(0.0136611969489248,-0.0343648066253259,
0.0756986510857125));
#93839=CARTESIAN_POINT('Origin',(-0.00260012655906958,-0.0345626446730747,
0.0714329267366677));
#93840=CARTESIAN_POINT('Ctrl Pts',(0.0137215760778875,-0.0346945769586885,
0.0754701623474144));
#93841=CARTESIAN_POINT('Ctrl Pts',(0.0136939247489572,-0.0345275153362891,
0.0755874103815636));
#93842=CARTESIAN_POINT('Ctrl Pts',(0.0136625789252224,-0.0343603235965159,
0.0757038191332164));
#93843=CARTESIAN_POINT('Ctrl Pts',(0.0136276364306931,-0.0341934961088741,
0.0758190456948274));
#93844=CARTESIAN_POINT('Ctrl Pts',(0.0137390411871065,-0.0346945769586885,
0.0753881684556221));
#93845=CARTESIAN_POINT('Ctrl Pts',(0.0137131072530683,-0.0345275153362891,
0.0755057823034765));
#93846=CARTESIAN_POINT('Ctrl Pts',(0.0136834677639275,-0.0343603235965159,
0.0756226109739413));
#93847=CARTESIAN_POINT('Ctrl Pts',(0.0136502155155724,-0.0341934961088741,
0.0757383102425323));
#93848=CARTESIAN_POINT('Ctrl Pts',(0.0137565062963254,-0.0346945769586885,
0.0753061745638298));
#93849=CARTESIAN_POINT('Ctrl Pts',(0.0137322897571793,-0.0345275153362891,
0.0754241542253895));
#93850=CARTESIAN_POINT('Ctrl Pts',(0.0137043566026327,-0.0343603235965159,
0.0755414028146662));
#93851=CARTESIAN_POINT('Ctrl Pts',(0.0136727946004517,-0.0341934961088741,
0.0756575747902372));
#93852=CARTESIAN_POINT('Ctrl Pts',(0.0137739714055443,-0.0346945769586885,
0.0752241806720375));
#93853=CARTESIAN_POINT('Ctrl Pts',(0.0137514722612904,-0.0345275153362891,
0.0753425261473024));
#93854=CARTESIAN_POINT('Ctrl Pts',(0.0137252454413379,-0.0343603235965159,
0.0754601946553911));
#93855=CARTESIAN_POINT('Ctrl Pts',(0.013695373685331,-0.0341934961088741,
0.0755768393379421));
#93856=CARTESIAN_POINT('Ctrl Pts',(0.0136612049113232,-0.0340223579322365,
0.0756986205474476));
#93857=CARTESIAN_POINT('Ctrl Pts',(0.0136398453950021,-0.0339125849573552,
0.075774996048936));
#93858=CARTESIAN_POINT('Ctrl Pts',(0.0136169200923572,-0.0338030433565217,
0.0758508757898885));
#93859=CARTESIAN_POINT('Ctrl Pts',(0.0135924669229434,-0.0336938721132321,
0.0759261653317888));
#93860=CARTESIAN_POINT('Ctrl Pts',(0.0137611253839407,-0.0340223579322365,
0.0756451688965628));
#93861=CARTESIAN_POINT('Ctrl Pts',(0.0137405031052931,-0.0339125849573552,
0.0757229225619721));
#93862=CARTESIAN_POINT('Ctrl Pts',(0.0137182859974825,-0.0338030433565217,
0.0758001947575325));
#93863=CARTESIAN_POINT('Ctrl Pts',(0.0136945112322549,-0.0336938721132321,
0.0758768891837296));
#93864=CARTESIAN_POINT('Ctrl Pts',(0.0138610458565582,-0.0340223579322365,
0.075591717245678));
#93865=CARTESIAN_POINT('Ctrl Pts',(0.013841160815584,-0.0339125849573552,
0.0756708490750082));
#93866=CARTESIAN_POINT('Ctrl Pts',(0.0138196519026078,-0.0338030433565217,
0.0757495137251764));
#93867=CARTESIAN_POINT('Ctrl Pts',(0.0137965555415665,-0.0336938721132321,
0.0758276130356704));
#93868=CARTESIAN_POINT('Ctrl Pts',(0.0139609663291757,-0.0340223579322365,
0.0755382655947932));
#93869=CARTESIAN_POINT('Ctrl Pts',(0.013941818525875,-0.0339125849573552,
0.0756187755880443));
#93870=CARTESIAN_POINT('Ctrl Pts',(0.0139210178077331,-0.0338030433565217,
0.0756988326928203));
#93871=CARTESIAN_POINT('Ctrl Pts',(0.013898599850878,-0.0336938721132321,
0.0757783368876112));
#93872=CARTESIAN_POINT('Origin',(-0.00257988690662493,-0.034558964341444,
0.0719308491163725));
#93873=CARTESIAN_POINT('Ctrl Pts',(0.0137934004130372,-0.034193496108874,
0.0761135246981947));
#93874=CARTESIAN_POINT('Ctrl Pts',(0.0137663245702022,-0.0340836138581107,
0.076191705376033));
#93875=CARTESIAN_POINT('Ctrl Pts',(0.0137376439337832,-0.03397388966435,
0.0762692882635576));
#93876=CARTESIAN_POINT('Ctrl Pts',(0.0137074018677849,-0.0338644633294062,
0.0763461765249485));
#93877=CARTESIAN_POINT('Ctrl Pts',(0.0137378141295513,-0.034193496108874,
0.0760147759040939));
#93878=CARTESIAN_POINT('Ctrl Pts',(0.0137120999741102,-0.0340836138581107,
0.0760921900799998));
#93879=CARTESIAN_POINT('Ctrl Pts',(0.0136847962328711,-0.03397388966435,
0.0761690350106375));
#93880=CARTESIAN_POINT('Ctrl Pts',(0.0136559444442687,-0.0338644633294062,
0.0762452146865479));
#93881=CARTESIAN_POINT('Ctrl Pts',(0.0136822278460653,-0.034193496108874,
0.0759160271099931));
#93882=CARTESIAN_POINT('Ctrl Pts',(0.0136578753780183,-0.0340836138581107,
0.0759926747839666));
#93883=CARTESIAN_POINT('Ctrl Pts',(0.0136319485319589,-0.03397388966435,
0.0760687817577173));
#93884=CARTESIAN_POINT('Ctrl Pts',(0.0136044870207526,-0.0338644633294062,
0.0761442528481473));
#93885=CARTESIAN_POINT('Ctrl Pts',(0.0136266415625794,-0.034193496108874,
0.0758172783158922));
#93886=CARTESIAN_POINT('Ctrl Pts',(0.0136036507819263,-0.0340836138581107,
0.0758931594879334));
#93887=CARTESIAN_POINT('Ctrl Pts',(0.0135791008310468,-0.03397388966435,
0.0759685285047972));
#93888=CARTESIAN_POINT('Ctrl Pts',(0.0135530295972365,-0.0338644633294062,
0.0760432910097467));
#93889=CARTESIAN_POINT('Origin',(-0.00252744442335263,-0.0345610621864089,
0.0714525188985465));
#93890=CARTESIAN_POINT('Ctrl Pts',(0.0136380262171894,-0.0342436276873901,
0.0757843921937186));
#93891=CARTESIAN_POINT('Ctrl Pts',(0.0135763840994213,-0.0339430054201861,
0.0759923653355634));
#93892=CARTESIAN_POINT('Ctrl Pts',(0.0134992517112607,-0.0336441434784162,
0.0761951045106342));
#93893=CARTESIAN_POINT('Ctrl Pts',(0.013703843691811,-0.0342436276873901,
0.0755432116388755));
#93894=CARTESIAN_POINT('Ctrl Pts',(0.0136512978486226,-0.0339430054201861,
0.0757536671276976));
#93895=CARTESIAN_POINT('Ctrl Pts',(0.0135830489129339,-0.0336441434784162,
0.0759595667663303));
#93896=CARTESIAN_POINT('Ctrl Pts',(0.0135530386087955,-0.0335235895815128,
0.0760432647834336));
#93897=CARTESIAN_POINT('Ctrl Pts',(0.0135269740915566,-0.0334144449262719,
0.0761180091872167));
#93898=CARTESIAN_POINT('Ctrl Pts',(0.0134993354662144,-0.0333049234473133,
0.0761923009899538));
#93899=CARTESIAN_POINT('Ctrl Pts',(0.0134701494688998,-0.0331951640388588,
0.0762660419938688));
#93900=CARTESIAN_POINT('Ctrl Pts',(0.0136561181601045,-0.0335235895815128,
0.0759961927260275));
#93901=CARTESIAN_POINT('Ctrl Pts',(0.0136307016824121,-0.0334144449262719,
0.0760723562227794));
#93902=CARTESIAN_POINT('Ctrl Pts',(0.0136036825237426,-0.0333049234473133,
0.0761480821368605));
#93903=CARTESIAN_POINT('Ctrl Pts',(0.0135750864620068,-0.0331951640388588,
0.076223270508459));
#93904=CARTESIAN_POINT('Ctrl Pts',(0.0137591977114134,-0.0335235895815128,
0.0759491206686215));
#93905=CARTESIAN_POINT('Ctrl Pts',(0.0137344292732676,-0.0334144449262719,
0.0760267032583421));
#93906=CARTESIAN_POINT('Ctrl Pts',(0.0137080295812708,-0.0333049234473133,
0.0761038632837671));
#93907=CARTESIAN_POINT('Ctrl Pts',(0.0136800234551138,-0.0331951640388588,
0.0761804990230492));
#93908=CARTESIAN_POINT('Ctrl Pts',(0.0138622772627224,-0.0335235895815128,
0.0759020486112155));
#93909=CARTESIAN_POINT('Ctrl Pts',(0.013838156864123,-0.0334144449262719,
0.0759810502939047));
#93910=CARTESIAN_POINT('Ctrl Pts',(0.013812376638799,-0.0333049234473133,
0.0760596444306737));
#93911=CARTESIAN_POINT('Ctrl Pts',(0.0137849604482207,-0.0331951640388588,
0.0761377275376394));
#93912=CARTESIAN_POINT('Origin',(-0.00173093818158889,-0.0326434571768067,
0.0694310017375691));
#93913=CARTESIAN_POINT('Ctrl Pts',(0.0136598036590481,-0.0336938721132425,
0.0764674742422201));
#93914=CARTESIAN_POINT('Ctrl Pts',(0.0136462387132884,-0.0336474569764975,
0.0764998784129082));
#93915=CARTESIAN_POINT('Ctrl Pts',(0.0136322953652761,-0.033601104548885,
0.0765321215684246));
#93916=CARTESIAN_POINT('Ctrl Pts',(0.0135969940169545,-0.0334837508694627,
0.0766137538179296));
#93917=CARTESIAN_POINT('Ctrl Pts',(0.0135592892377864,-0.0333660264863639,
0.0766943041685213));
#93918=CARTESIAN_POINT('Ctrl Pts',(0.0135119755852972,-0.0336938721132425,
0.0761613420813908));
#93919=CARTESIAN_POINT('Ctrl Pts',(0.0135002025326603,-0.0336474569764975,
0.0761928809653086));
#93920=CARTESIAN_POINT('Ctrl Pts',(0.0134880610842634,-0.033601104548885,
0.0762242798697162));
#93921=CARTESIAN_POINT('Ctrl Pts',(0.0134573217310885,-0.0334837508694627,
0.076303774669705));
#93922=CARTESIAN_POINT('Ctrl Pts',(0.0134242402808307,-0.0333660264863639,
0.0763823236907537));
#93923=CARTESIAN_POINT('Ctrl Pts',(0.0135119755853047,-0.0336938721132427,
0.0761613420814074));
#93924=CARTESIAN_POINT('Ctrl Pts',(0.0135002025326691,-0.0336474569765026,
0.076192880965322));
#93925=CARTESIAN_POINT('Ctrl Pts',(0.0134880610842734,-0.0336011045488949,
0.0762242798697262));
#93926=CARTESIAN_POINT('Ctrl Pts',(0.0134575777480446,-0.033484728265791,
0.0763031125863));
#93927=CARTESIAN_POINT('Ctrl Pts',(0.0134247910462803,-0.0333679870047996,
0.0763810154949585));
#93928=CARTESIAN_POINT('Ctrl Pts',(0.0135119755852973,-0.0336938721132429,
0.0761613420813906));
#93929=CARTESIAN_POINT('Ctrl Pts',(0.0134698699389755,-0.0335278710435085,
0.0762741390876206));
#93930=CARTESIAN_POINT('Ctrl Pts',(0.0134242418205336,-0.0333620469224321,
0.0763855759900045));
#93931=CARTESIAN_POINT('Ctrl Pts',(0.0133750500022093,-0.0331951640388601,
0.0764957006196661));
#93932=CARTESIAN_POINT('Ctrl Pts',(0.0135395795394343,-0.0336938721132429,
0.076082183686136));
#93933=CARTESIAN_POINT('Ctrl Pts',(0.0134991310032703,-0.0335278710435085,
0.0761955585564404));
#93934=CARTESIAN_POINT('Ctrl Pts',(0.0134551412903517,-0.0333620469224321,
0.076307625086151));
#93935=CARTESIAN_POINT('Ctrl Pts',(0.0134075698830115,-0.0331951640388601,
0.0764184316920439));
#93936=CARTESIAN_POINT('Ctrl Pts',(0.0135671834935713,-0.0336938721132429,
0.0760030252908814));
#93937=CARTESIAN_POINT('Ctrl Pts',(0.0135283920675652,-0.0335278710435085,
0.0761169780252601));
#93938=CARTESIAN_POINT('Ctrl Pts',(0.0134860407601697,-0.0333620469224321,
0.0762296741822976));
#93939=CARTESIAN_POINT('Ctrl Pts',(0.0134400897638137,-0.0331951640388601,
0.0763411627644218));
#93940=CARTESIAN_POINT('Ctrl Pts',(0.0135947874477083,-0.0336938721132429,
0.0759238668956268));
#93941=CARTESIAN_POINT('Ctrl Pts',(0.01355765313186,-0.0335278710435085,
0.0760383974940798));
#93942=CARTESIAN_POINT('Ctrl Pts',(0.0135169402299878,-0.0333620469224321,
0.0761517232784441));
#93943=CARTESIAN_POINT('Ctrl Pts',(0.013472609644616,-0.0331951640388601,
0.0762638938367996));
#93944=CARTESIAN_POINT('Ctrl Pts',(0.0134234469406118,-0.0330240426238156,
0.0763804336672536));
#93945=CARTESIAN_POINT('Ctrl Pts',(0.0133927205438393,-0.0329142774063509,
0.0764534417123633));
#93946=CARTESIAN_POINT('Ctrl Pts',(0.0133604695486071,-0.0328043479726686,
0.0765258509541948));
#93947=CARTESIAN_POINT('Ctrl Pts',(0.0133267327162031,-0.0326943950436594,
0.0765975674932834));
#93948=CARTESIAN_POINT('Ctrl Pts',(0.013529278610008,-0.0330240426238156,
0.0763399269549991));
#93949=CARTESIAN_POINT('Ctrl Pts',(0.0134991102326606,-0.0329142774063509,
0.0764143929344615));
#93950=CARTESIAN_POINT('Ctrl Pts',(0.0134673873954709,-0.0328043479726686,
0.0764882723732995));
#93951=CARTESIAN_POINT('Ctrl Pts',(0.0134341481312477,-0.0326943950436594,
0.07656146950725));
#93952=CARTESIAN_POINT('Ctrl Pts',(0.0136351102794043,-0.0330240426238156,
0.0762994202427447));
#93953=CARTESIAN_POINT('Ctrl Pts',(0.013605499921482,-0.0329142774063509,
0.0763753441565598));
#93954=CARTESIAN_POINT('Ctrl Pts',(0.0135743052423347,-0.0328043479726686,
0.0764506937924042));
#93955=CARTESIAN_POINT('Ctrl Pts',(0.0135415635462923,-0.0326943950436594,
0.0765253715212167));
#93956=CARTESIAN_POINT('Ctrl Pts',(0.0137409419488005,-0.0330240426238156,
0.0762589135304902));
#93957=CARTESIAN_POINT('Ctrl Pts',(0.0137118896103033,-0.0329142774063509,
0.076336295378658));
#93958=CARTESIAN_POINT('Ctrl Pts',(0.0136812230891986,-0.0328043479726686,
0.0764131152115089));
#93959=CARTESIAN_POINT('Ctrl Pts',(0.0136489789613369,-0.0326943950436594,
0.0764892735351834));
#93960=CARTESIAN_POINT('Origin',(-0.00184364903173004,-0.0326396682859487,
0.0693800933573045));
#93961=CARTESIAN_POINT('Ctrl Pts',(0.0135025988803319,-0.0331951640388588,
0.0768086333040516));
#93962=CARTESIAN_POINT('Ctrl Pts',(0.01346598158494,-0.0330855618255041,
0.0768827156226605));
#93963=CARTESIAN_POINT('Ctrl Pts',(0.013427806737759,-0.0329757224427708,
0.0769560945292735));
#93964=CARTESIAN_POINT('Ctrl Pts',(0.0133881186147393,-0.0328657862078596,
0.0770286736598748));
#93965=CARTESIAN_POINT('Ctrl Pts',(0.0134598274289725,-0.0331951640388588,
0.0767036963944849));
#93966=CARTESIAN_POINT('Ctrl Pts',(0.0134246554272242,-0.0330855618255041,
0.0767771896228773));
#93967=CARTESIAN_POINT('Ctrl Pts',(0.0133879390910666,-0.0329757224427708,
0.0768500088863559));
#93968=CARTESIAN_POINT('Ctrl Pts',(0.0133497208638927,-0.0328657862078596,
0.0769220586291769));
#93969=CARTESIAN_POINT('Ctrl Pts',(0.013417055977613,-0.0331951640388587,
0.0765987594849182));
#93970=CARTESIAN_POINT('Ctrl Pts',(0.0133833292695084,-0.0330855618255041,
0.0766716636230941));
#93971=CARTESIAN_POINT('Ctrl Pts',(0.0133480714443742,-0.0329757224427708,
0.0767439232434383));
#93972=CARTESIAN_POINT('Ctrl Pts',(0.0133113231130462,-0.0328657862078596,
0.0768154435984789));
#93973=CARTESIAN_POINT('Ctrl Pts',(0.0133742845262536,-0.0331951640388587,
0.0764938225753515));
#93974=CARTESIAN_POINT('Ctrl Pts',(0.0133420031117926,-0.0330855618255041,
0.0765661376233108));
#93975=CARTESIAN_POINT('Ctrl Pts',(0.0133082037976819,-0.0329757224427708,
0.0766378376005208));
#93976=CARTESIAN_POINT('Ctrl Pts',(0.0132729253621996,-0.0328657862078596,
0.0767088285677809));
#93977=CARTESIAN_POINT('Origin',(-0.00160195152521618,-0.032640190883275,
0.0689643347885643));
#93978=CARTESIAN_POINT('Ctrl Pts',(0.0133896719571905,-0.0332451089994432,
0.076462688909589));
#93979=CARTESIAN_POINT('Ctrl Pts',(0.0133024474678981,-0.0329451141710257,
0.07666129519141));
#93980=CARTESIAN_POINT('Ctrl Pts',(0.0132005109371185,-0.0326442513127503,
0.0768527671486353));
#93981=CARTESIAN_POINT('Ctrl Pts',(0.0134852012912264,-0.0332451089994432,
0.0762316604560629));
#93982=CARTESIAN_POINT('Ctrl Pts',(0.0134066901826171,-0.0329451141710257,
0.0764338696856644));
#93983=CARTESIAN_POINT('Ctrl Pts',(0.0133131708899699,-0.0326442513127503,
0.0766295906825294));
#93984=CARTESIAN_POINT('Ctrl Pts',(0.0132729394996485,-0.0325229783203385,
0.0767088003204275));
#93985=CARTESIAN_POINT('Ctrl Pts',(0.0132376664938307,-0.032413025311208,
0.0767797813400015));
#93986=CARTESIAN_POINT('Ctrl Pts',(0.0132009305043106,-0.0323031222247695,
0.0768500219264899));
#93987=CARTESIAN_POINT('Ctrl Pts',(0.013162781762135,-0.0321934096636185,
0.0769194337671563));
#93988=CARTESIAN_POINT('Ctrl Pts',(0.0133811057945875,-0.0325229783203385,
0.076675018738332));
#93989=CARTESIAN_POINT('Ctrl Pts',(0.0133462984671316,-0.032413025311208,
0.0767474908278892));
#93990=CARTESIAN_POINT('Ctrl Pts',(0.0133099972406468,-0.0323031222247695,
0.0768192318913657));
#93991=CARTESIAN_POINT('Ctrl Pts',(0.0132722518571004,-0.0321934096636185,
0.0768901516743697));
#93992=CARTESIAN_POINT('Ctrl Pts',(0.0134892720895264,-0.0325229783203385,
0.0766412371562365));
#93993=CARTESIAN_POINT('Ctrl Pts',(0.0134549304404326,-0.032413025311208,
0.0767152003157768));
#93994=CARTESIAN_POINT('Ctrl Pts',(0.0134190639769829,-0.0323031222247695,
0.0767884418562415));
#93995=CARTESIAN_POINT('Ctrl Pts',(0.0133817219520658,-0.0321934096636185,
0.0768608695815831));
#93996=CARTESIAN_POINT('Ctrl Pts',(0.0135974383844654,-0.0325229783203385,
0.076607455574141));
#93997=CARTESIAN_POINT('Ctrl Pts',(0.0135635624137335,-0.032413025311208,
0.0766829098036644));
#93998=CARTESIAN_POINT('Ctrl Pts',(0.0135281307133191,-0.0323031222247695,
0.0767576518211172));
#93999=CARTESIAN_POINT('Ctrl Pts',(0.0134911920470313,-0.0321934096636185,
0.0768315874887965));
#94000=CARTESIAN_POINT('Origin',(-0.00183606431180876,-0.0326393375181179,
0.0693839873334145));
#94001=CARTESIAN_POINT('Ctrl Pts',(0.0133250480478731,-0.0326943950436593,
0.0771411257927735));
#94002=CARTESIAN_POINT('Ctrl Pts',(0.0132838247284816,-0.0325844576448127,
0.0772128089844631));
#94003=CARTESIAN_POINT('Ctrl Pts',(0.0132411159657214,-0.0324744968375319,
0.077283644683452));
#94004=CARTESIAN_POINT('Ctrl Pts',(0.0131969777323871,-0.0323646534831895,
0.0773535428856782));
#94005=CARTESIAN_POINT('Ctrl Pts',(0.0132889500736497,-0.0326943950436593,
0.0770337104128714));
#94006=CARTESIAN_POINT('Ctrl Pts',(0.0132492071395111,-0.0325844576448127,
0.0771048961068213));
#94007=CARTESIAN_POINT('Ctrl Pts',(0.013207989155842,-0.0324744968375319,
0.0771752648896561));
#94008=CARTESIAN_POINT('Ctrl Pts',(0.0131653501771121,-0.0323646534831895,
0.0772447273292081));
#94009=CARTESIAN_POINT('Ctrl Pts',(0.0132528520994263,-0.0326943950436593,
0.0769262950329692));
#94010=CARTESIAN_POINT('Ctrl Pts',(0.0132145895505407,-0.0325844576448127,
0.0769969832291796));
#94011=CARTESIAN_POINT('Ctrl Pts',(0.0131748623459625,-0.0324744968375319,
0.0770668850958601));
#94012=CARTESIAN_POINT('Ctrl Pts',(0.0131337226218371,-0.0323646534831895,
0.077135911772738));
#94013=CARTESIAN_POINT('Ctrl Pts',(0.013216754125203,-0.0326943950436593,
0.076818879653067));
#94014=CARTESIAN_POINT('Ctrl Pts',(0.0131799719615702,-0.0325844576448127,
0.0768890703515378));
#94015=CARTESIAN_POINT('Ctrl Pts',(0.0131417355360831,-0.0324744968375319,
0.0769585053020642));
#94016=CARTESIAN_POINT('Ctrl Pts',(0.0131020950665621,-0.0323646534831895,
0.077027096216268));
#94017=CARTESIAN_POINT('Origin',(-0.00163555586517919,-0.0326395579070148,
0.0689469362202125));
#94018=CARTESIAN_POINT('Ctrl Pts',(0.0132340839843633,-0.0327445246961876,
0.0767887384490127));
#94019=CARTESIAN_POINT('Ctrl Pts',(0.013134562337837,-0.0324436878365474,
0.0769814766299047));
#94020=CARTESIAN_POINT('Ctrl Pts',(0.013020805594427,-0.0321434074463185,
0.0771661708849035));
#94021=CARTESIAN_POINT('Ctrl Pts',(0.0133439296781406,-0.0327445246961876,
0.0765641634647457));
#94022=CARTESIAN_POINT('Ctrl Pts',(0.0132528780155232,-0.0324436878365474,
0.0767610445436624));
#94023=CARTESIAN_POINT('Ctrl Pts',(0.0131472551336846,-0.0321434074463185,
0.0769505079209493));
#94024=CARTESIAN_POINT('Ctrl Pts',(0.0130554368548483,-0.0322357242816071,
0.077109207207571));
#94025=CARTESIAN_POINT('Ctrl Pts',(0.0129611899432383,-0.0319819883628704,
0.0772662740124256));
#94026=CARTESIAN_POINT('Ctrl Pts',(0.0128571394245683,-0.0317295851069886,
0.0774170253013081));
#94027=CARTESIAN_POINT('Ctrl Pts',(0.0131793781650859,-0.0322357242816071,
0.0768920930633598));
#94028=CARTESIAN_POINT('Ctrl Pts',(0.0130920460573823,-0.0319819883628704,
0.0770531072381995));
#94029=CARTESIAN_POINT('Ctrl Pts',(0.0129946451464659,-0.0317295851069886,
0.0772082379059861));
#94030=CARTESIAN_POINT('Origin',(-0.00155227451048989,-0.0326371942648798,
0.0689932678446254));
#94031=CARTESIAN_POINT('Origin',(-0.00172664139655714,-0.0326352985534453,
0.0694395789559609));
#94032=CARTESIAN_POINT('Ctrl Pts',(0.0131269701953199,-0.0321934096636184,
0.0774618136745129));
#94033=CARTESIAN_POINT('Ctrl Pts',(0.0130812977036778,-0.0320835708272304,
0.0775308115363109));
#94034=CARTESIAN_POINT('Ctrl Pts',(0.0130342237967733,-0.0319739230346346,
0.0775988241867043));
#94035=CARTESIAN_POINT('Ctrl Pts',(0.0129858153807518,-0.0318646057455575,
0.0776657692305408));
#94036=CARTESIAN_POINT('Ctrl Pts',(0.0130976880773171,-0.0321934096636184,
0.0773523434852778));
#94037=CARTESIAN_POINT('Ctrl Pts',(0.0130535252649005,-0.0320835708272304,
0.0774209375238474));
#94038=CARTESIAN_POINT('Ctrl Pts',(0.0130079685186468,-0.0319739230346346,
0.0774885778279795));
#94039=CARTESIAN_POINT('Ctrl Pts',(0.0129610827670381,-0.0318646057455575,
0.0775551823299387));
#94040=CARTESIAN_POINT('Ctrl Pts',(0.0130684059593144,-0.0321934096636184,
0.0772428732960427));
#94041=CARTESIAN_POINT('Ctrl Pts',(0.0130257528261232,-0.0320835708272304,
0.0773110635113839));
#94042=CARTESIAN_POINT('Ctrl Pts',(0.0129817132405203,-0.0319739230346346,
0.0773783314692546));
#94043=CARTESIAN_POINT('Ctrl Pts',(0.0129363501533244,-0.0318646057455575,
0.0774445954293365));
#94044=CARTESIAN_POINT('Ctrl Pts',(0.0130391238413116,-0.0321934096636184,
0.0771334031068076));
#94045=CARTESIAN_POINT('Ctrl Pts',(0.0129979803873458,-0.0320835708272304,
0.0772011894989205));
#94046=CARTESIAN_POINT('Ctrl Pts',(0.0129554579623938,-0.0319739230346346,
0.0772680851105298));
#94047=CARTESIAN_POINT('Ctrl Pts',(0.0129116175396107,-0.0318646057455575,
0.0773340085287344));
#94048=CARTESIAN_POINT('Ctrl Pts',(0.0131030465111959,-0.0320218834582293,
0.0770271035176127));
#94049=CARTESIAN_POINT('Ctrl Pts',(0.0130731028189308,-0.0319391099350593,
0.0770789256218695));
#94050=CARTESIAN_POINT('Ctrl Pts',(0.0130423680593638,-0.0318564869454878,
0.0771302487534767));
#94051=CARTESIAN_POINT('Ctrl Pts',(0.0130108681085682,-0.0317740741446474,
0.0771810376202471));
#94052=CARTESIAN_POINT('Ctrl Pts',(0.0131511943607829,-0.0320218834582293,
0.0770153301311914));
#94053=CARTESIAN_POINT('Ctrl Pts',(0.0131213732010085,-0.0319391099350593,
0.0770676533381657));
#94054=CARTESIAN_POINT('Ctrl Pts',(0.0130907530749037,-0.0318564869454878,
0.077119479182247));
#94055=CARTESIAN_POINT('Ctrl Pts',(0.0130593598092299,-0.0317740741446474,
0.077170771997294));
#94056=CARTESIAN_POINT('Ctrl Pts',(0.01319934221037,-0.0320218834582293,
0.0770035567447701));
#94057=CARTESIAN_POINT('Ctrl Pts',(0.0131696435830863,-0.0319391099350593,
0.0770563810544619));
#94058=CARTESIAN_POINT('Ctrl Pts',(0.0131391380904436,-0.0318564869454878,
0.0771087096110174));
#94059=CARTESIAN_POINT('Ctrl Pts',(0.0131078515098917,-0.0317740741446474,
0.0771605063743409));
#94060=CARTESIAN_POINT('Ctrl Pts',(0.013247490059957,-0.0320218834582293,
0.0769917833583488));
#94061=CARTESIAN_POINT('Ctrl Pts',(0.013217913965164,-0.0319391099350593,
0.0770451087707582));
#94062=CARTESIAN_POINT('Ctrl Pts',(0.0131875231059834,-0.0318564869454878,
0.0770979400397877));
#94063=CARTESIAN_POINT('Ctrl Pts',(0.0131563432105534,-0.0317740741446474,
0.0771502407513878));
#94064=CARTESIAN_POINT('Origin',(0.0190209831310754,-0.0391228853390752,
0.0793588031300553));
#94065=CARTESIAN_POINT('Ctrl Pts',(0.0138753690461966,-0.0352722978779574,
0.0740915772819855));
#94066=CARTESIAN_POINT('Ctrl Pts',(0.013875210837716,-0.0352466642097203,
0.0741104735156868));
#94067=CARTESIAN_POINT('Ctrl Pts',(0.0138751311684267,-0.0352210183808294,
0.0741293535714064));
#94068=CARTESIAN_POINT('Ctrl Pts',(0.0138751305680331,-0.0351953608940152,
0.074148218117648));
#94069=CARTESIAN_POINT('Origin',(0.0187703048256994,-0.0352456003065023,
0.0743137189225401));
#94070=CARTESIAN_POINT('Ctrl Pts',(0.013872363194708,-0.0350241211493339,
0.0742728682562885));
#94071=CARTESIAN_POINT('Ctrl Pts',(0.0138706707349319,-0.0349144232867421,
0.0743520525990051));
#94072=CARTESIAN_POINT('Ctrl Pts',(0.0138673404652649,-0.0348045283677512,
0.0744312493530141));
#94073=CARTESIAN_POINT('Ctrl Pts',(0.0138623728765049,-0.0346945769586886,
0.0745103569186112));
#94074=CARTESIAN_POINT('Ctrl Pts',(0.0139558514978465,-0.0350241211493339,
0.0741962468164563));
#94075=CARTESIAN_POINT('Ctrl Pts',(0.0139552144669405,-0.0349144232867421,
0.0742765811762652));
#94076=CARTESIAN_POINT('Ctrl Pts',(0.0139529164861946,-0.0348045283677512,
0.0743569504521751));
#94077=CARTESIAN_POINT('Ctrl Pts',(0.0139489566682885,-0.0346945769586886,
0.0744372515918336));
#94078=CARTESIAN_POINT('Ctrl Pts',(0.014039339800985,-0.0350241211493339,
0.0741196253766241));
#94079=CARTESIAN_POINT('Ctrl Pts',(0.0140397581989491,-0.0349144232867421,
0.0742011097535254));
#94080=CARTESIAN_POINT('Ctrl Pts',(0.0140384925071243,-0.0348045283677512,
0.0742826515513361));
#94081=CARTESIAN_POINT('Ctrl Pts',(0.0140355404600722,-0.0346945769586886,
0.0743641462650559));
#94082=CARTESIAN_POINT('Ctrl Pts',(0.0141228281041235,-0.0350241211493339,
0.0740430039367919));
#94083=CARTESIAN_POINT('Ctrl Pts',(0.0141243019309577,-0.0349144232867421,
0.0741256383307855));
#94084=CARTESIAN_POINT('Ctrl Pts',(0.014124068528054,-0.0348045283677512,
0.0742083526504972));
#94085=CARTESIAN_POINT('Ctrl Pts',(0.0141221242518559,-0.0346945769586886,
0.0742910409382783));
#94086=CARTESIAN_POINT('Origin',(-0.00288114820865989,-0.03456290679414,
0.073278508408283));
#94087=CARTESIAN_POINT('Ctrl Pts',(0.0140395418760017,-0.0351970973651627,
0.074573449113318));
#94088=CARTESIAN_POINT('Ctrl Pts',(0.0140336755624119,-0.0350869349321799,
0.0746554039464499));
#94089=CARTESIAN_POINT('Ctrl Pts',(0.0140261005936722,-0.0349764985129763,
0.0747373047126031));
#94090=CARTESIAN_POINT('Ctrl Pts',(0.014016820537425,-0.0348659306849698,
0.0748190447292442));
#94091=CARTESIAN_POINT('Ctrl Pts',(0.0139826432554834,-0.0351970973651627,
0.0745140940997731));
#94092=CARTESIAN_POINT('Ctrl Pts',(0.013977599225166,-0.0350869349321799,
0.074595260679629));
#94093=CARTESIAN_POINT('Ctrl Pts',(0.0139708636082174,-0.0349764985129763,
0.0746763896343399));
#94094=CARTESIAN_POINT('Ctrl Pts',(0.0139624389437352,-0.0348659306849698,
0.0747573753452878));
#94095=CARTESIAN_POINT('Ctrl Pts',(0.0139257446349652,-0.0351970973651627,
0.0744547390862282));
#94096=CARTESIAN_POINT('Ctrl Pts',(0.0139215228879201,-0.0350869349321799,
0.074535117412808));
#94097=CARTESIAN_POINT('Ctrl Pts',(0.0139156266227625,-0.0349764985129763,
0.0746154745560767));
#94098=CARTESIAN_POINT('Ctrl Pts',(0.0139080573500455,-0.0348659306849698,
0.0746957059613315));
#94099=CARTESIAN_POINT('Ctrl Pts',(0.0138688460144469,-0.0351970973651627,
0.0743953840726833));
#94100=CARTESIAN_POINT('Ctrl Pts',(0.0138654465506742,-0.0350869349321799,
0.0744749741459871));
#94101=CARTESIAN_POINT('Ctrl Pts',(0.0138603896373077,-0.0349764985129763,
0.0745545594778135));
#94102=CARTESIAN_POINT('Ctrl Pts',(0.0138536757563557,-0.0348659306849698,
0.0746340365773751));
#94103=CARTESIAN_POINT('Origin',(-0.00279802255310622,-0.034563718796424,
0.0728047832961103));
#94104=CARTESIAN_POINT('Ctrl Pts',(0.0138712400212374,-0.0352450361861253,
0.0743617864818154));
#94105=CARTESIAN_POINT('Ctrl Pts',(0.0138632523632099,-0.0349452761023764,
0.0745785554052386));
#94106=CARTESIAN_POINT('Ctrl Pts',(0.0138389594754375,-0.0346444289983475,
0.0747941068479304));
#94107=CARTESIAN_POINT('Ctrl Pts',(0.013875013965815,-0.0352450361861253,
0.0741118149687537));
#94108=CARTESIAN_POINT('Ctrl Pts',(0.0138764541378635,-0.0349452761023764,
0.0743287262288287));
#94109=CARTESIAN_POINT('Ctrl Pts',(0.013861551575317,-0.0346444289983475,
0.0745451297465273));
#94110=CARTESIAN_POINT('Ctrl Pts',(0.0138533048573479,-0.0345231616327822,
0.0746335812268912));
#94111=CARTESIAN_POINT('Ctrl Pts',(0.0138466393709632,-0.0344132092796975,
0.0747125546302946));
#94112=CARTESIAN_POINT('Ctrl Pts',(0.0138383407259309,-0.0343032738558973,
0.0747913860887051));
#94113=CARTESIAN_POINT('Ctrl Pts',(0.0138284221407276,-0.0341934961088741,
0.0748699748822446));
#94114=CARTESIAN_POINT('Ctrl Pts',(0.0139414394845606,-0.0345231616327822,
0.0745623532574936));
#94115=CARTESIAN_POINT('Ctrl Pts',(0.0139357557754531,-0.0344132092796975,
0.0746425414726495));
#94116=CARTESIAN_POINT('Ctrl Pts',(0.0139284137296199,-0.0343032738558973,
0.0747226079874224));
#94117=CARTESIAN_POINT('Ctrl Pts',(0.0139194253805535,-0.0341934961088741,
0.0748024504682921));
#94118=CARTESIAN_POINT('Ctrl Pts',(0.0140295741117733,-0.0345231616327822,
0.074491125288096));
#94119=CARTESIAN_POINT('Ctrl Pts',(0.014024872179943,-0.0344132092796975,
0.0745725283150044));
#94120=CARTESIAN_POINT('Ctrl Pts',(0.0140184867333089,-0.0343032738558973,
0.0746538298861396));
#94121=CARTESIAN_POINT('Ctrl Pts',(0.0140104286203793,-0.0341934961088741,
0.0747349260543396));
#94122=CARTESIAN_POINT('Ctrl Pts',(0.014117708738986,-0.0345231616327822,
0.0744198973186984));
#94123=CARTESIAN_POINT('Ctrl Pts',(0.0141139885844328,-0.0344132092796975,
0.0745025151573592));
#94124=CARTESIAN_POINT('Ctrl Pts',(0.0141085597369979,-0.0343032738558973,
0.0745850517848568));
#94125=CARTESIAN_POINT('Ctrl Pts',(0.0141014318602052,-0.0341934961088741,
0.0746674016403871));
#94126=CARTESIAN_POINT('Origin',(-0.00289323127354824,-0.034562559623145,
0.0732778028343769));
#94127=CARTESIAN_POINT('Ctrl Pts',(0.0140609037262127,-0.0346945769586885,
0.0750163647622781));
#94128=CARTESIAN_POINT('Ctrl Pts',(0.0140489647818862,-0.0345846629176052,
0.0750981812979107));
#94129=CARTESIAN_POINT('Ctrl Pts',(0.0140353318660018,-0.0344746925050311,
0.0751797649155431));
#94130=CARTESIAN_POINT('Ctrl Pts',(0.0140200228783344,-0.0343648066253259,
0.0752610111529836));
#94131=CARTESIAN_POINT('Ctrl Pts',(0.013987798456992,-0.0346945769586885,
0.0749297810386632));
#94132=CARTESIAN_POINT('Ctrl Pts',(0.0139770526801405,-0.0345846629176052,
0.075010590146735));
#94133=CARTESIAN_POINT('Ctrl Pts',(0.0139646339687153,-0.0344746925050311,
0.0750911908389489));
#94134=CARTESIAN_POINT('Ctrl Pts',(0.0139505586615112,-0.0343648066253259,
0.0751714799061253));
#94135=CARTESIAN_POINT('Ctrl Pts',(0.0139146931877713,-0.0346945769586885,
0.0748431973150483));
#94136=CARTESIAN_POINT('Ctrl Pts',(0.0139051405783948,-0.0345846629176052,
0.0749229989955593));
#94137=CARTESIAN_POINT('Ctrl Pts',(0.0138939360714287,-0.0344746925050311,
0.0750026167623547));
#94138=CARTESIAN_POINT('Ctrl Pts',(0.013881094444688,-0.0343648066253259,
0.0750819486592671));
#94139=CARTESIAN_POINT('Ctrl Pts',(0.0138415879185506,-0.0346945769586885,
0.0747566135914333));
#94140=CARTESIAN_POINT('Ctrl Pts',(0.013833228476649,-0.0345846629176052,
0.0748354078443836));
#94141=CARTESIAN_POINT('Ctrl Pts',(0.0138232381741422,-0.0344746925050311,
0.0749140426857605));
#94142=CARTESIAN_POINT('Ctrl Pts',(0.0138116302278648,-0.0343648066253259,
0.0749924174124088));
#94143=CARTESIAN_POINT('Origin',(-0.00285610491349698,-0.034562644673227,
0.0727984138314592));
#94144=CARTESIAN_POINT('Ctrl Pts',(0.0138428960169573,-0.0346945769586885,
0.0747581628645858));
#94145=CARTESIAN_POINT('Ctrl Pts',(0.0138301578022637,-0.034527515336289,
0.0748779519934327));
#94146=CARTESIAN_POINT('Ctrl Pts',(0.0138136490349714,-0.0343603235965158,
0.0749973715007565));
#94147=CARTESIAN_POINT('Ctrl Pts',(0.0137934237900075,-0.0341934961088739,
0.0751160689223409));
#94148=CARTESIAN_POINT('Ctrl Pts',(0.0138499468489827,-0.0346945769586885,
0.0746746265605078));
#94149=CARTESIAN_POINT('Ctrl Pts',(0.013838958335624,-0.034527515336289,
0.0747945633718544));
#94150=CARTESIAN_POINT('Ctrl Pts',(0.0138241950777504,-0.0343603235965158,
0.0749141856263728));
#94151=CARTESIAN_POINT('Ctrl Pts',(0.013805705996759,-0.0341934961088739,
0.0750331401834829));
#94152=CARTESIAN_POINT('Ctrl Pts',(0.013856997681008,-0.0346945769586885,
0.0745910902564298));
#94153=CARTESIAN_POINT('Ctrl Pts',(0.0138477588689843,-0.034527515336289,
0.0747111747502762));
#94154=CARTESIAN_POINT('Ctrl Pts',(0.0138347411205294,-0.0343603235965158,
0.074830999751989));
#94155=CARTESIAN_POINT('Ctrl Pts',(0.0138179882035106,-0.0341934961088739,
0.0749502114446248));
#94156=CARTESIAN_POINT('Ctrl Pts',(0.0138640485130333,-0.0346945769586885,
0.0745075539523517));
#94157=CARTESIAN_POINT('Ctrl Pts',(0.0138565594023446,-0.034527515336289,
0.0746277861286979));
#94158=CARTESIAN_POINT('Ctrl Pts',(0.0138452871633084,-0.0343603235965158,
0.0747478138776052));
#94159=CARTESIAN_POINT('Ctrl Pts',(0.0138302704102621,-0.0341934961088739,
0.0748672827057668));
#94160=CARTESIAN_POINT('Ctrl Pts',(0.0138116343000179,-0.0340223579322365,
0.0749923861169942));
#94161=CARTESIAN_POINT('Ctrl Pts',(0.0138000155984294,-0.0339125849573554,
0.0750708364320888));
#94162=CARTESIAN_POINT('Ctrl Pts',(0.0137867813219389,-0.0338030433565221,
0.0751489911409305));
#94163=CARTESIAN_POINT('Ctrl Pts',(0.0137719572548097,-0.0336938721132328,
0.0752267517970983));
#94164=CARTESIAN_POINT('Ctrl Pts',(0.0139040676016188,-0.0340223579322365,
0.0749268325924097));
#94165=CARTESIAN_POINT('Ctrl Pts',(0.0138933530541051,-0.0339125849573554,
0.0750065578038095));
#94166=CARTESIAN_POINT('Ctrl Pts',(0.0138809959089597,-0.0338030433565221,
0.07508600522699));
#94167=CARTESIAN_POINT('Ctrl Pts',(0.0138670209752888,-0.0336938721132328,
0.075165074662932));
#94168=CARTESIAN_POINT('Ctrl Pts',(0.0139965009032197,-0.0340223579322365,
0.0748612790678253));
#94169=CARTESIAN_POINT('Ctrl Pts',(0.0139866905097808,-0.0339125849573554,
0.0749422791755303));
#94170=CARTESIAN_POINT('Ctrl Pts',(0.0139752104959805,-0.0338030433565221,
0.0750230193130495));
#94171=CARTESIAN_POINT('Ctrl Pts',(0.013962084695768,-0.0336938721132328,
0.0751033975287658));
#94172=CARTESIAN_POINT('Ctrl Pts',(0.0140889342048206,-0.0340223579322365,
0.0747957255432408));
#94173=CARTESIAN_POINT('Ctrl Pts',(0.0140800279654565,-0.0339125849573554,
0.0748780005472511));
#94174=CARTESIAN_POINT('Ctrl Pts',(0.0140694250830013,-0.0338030433565221,
0.074960033399109));
#94175=CARTESIAN_POINT('Ctrl Pts',(0.0140571484162471,-0.0336938721132328,
0.0750417203945996));
#94176=CARTESIAN_POINT('Origin',(-0.00277361863472758,-0.0345589643412889,
0.0732898732429793));
#94177=CARTESIAN_POINT('Ctrl Pts',(0.0139947886795483,-0.034193496108874,
0.0753874501348942));
#94178=CARTESIAN_POINT('Ctrl Pts',(0.0139777249749769,-0.0340836138581107,
0.0754684078376702));
#94179=CARTESIAN_POINT('Ctrl Pts',(0.0139589942081052,-0.03397388966435,
0.075548973597857));
#94180=CARTESIAN_POINT('Ctrl Pts',(0.0139386272642535,-0.0338644633294062,
0.0756290459082627));
#94181=CARTESIAN_POINT('Ctrl Pts',(0.0139272642048352,-0.034193496108874,
0.0752964468131808));
#94182=CARTESIAN_POINT('Ctrl Pts',(0.0139114553821803,-0.0340836138581107,
0.075376473393437));
#94183=CARTESIAN_POINT('Ctrl Pts',(0.0138939981627359,-0.03397388966435,
0.0754561344450221));
#94184=CARTESIAN_POINT('Ctrl Pts',(0.013874921724218,-0.0338644633294062,
0.0755353295093939));
#94185=CARTESIAN_POINT('Ctrl Pts',(0.0138597397301222,-0.034193496108874,
0.0752054434914675));
#94186=CARTESIAN_POINT('Ctrl Pts',(0.0138451857893837,-0.0340836138581107,
0.0752845389492037));
#94187=CARTESIAN_POINT('Ctrl Pts',(0.0138290021173665,-0.03397388966435,
0.0753632952921872));
#94188=CARTESIAN_POINT('Ctrl Pts',(0.0138112161841826,-0.0338644633294062,
0.0754416131105251));
#94189=CARTESIAN_POINT('Ctrl Pts',(0.0137922152554091,-0.034193496108874,
0.0751144401697541));
#94190=CARTESIAN_POINT('Ctrl Pts',(0.013778916196587,-0.0340836138581107,
0.0751926045049705));
#94191=CARTESIAN_POINT('Ctrl Pts',(0.0137640060719971,-0.03397388966435,
0.0752704561393523));
#94192=CARTESIAN_POINT('Ctrl Pts',(0.0137475106441471,-0.0338644633294062,
0.0753478967116564));
#94193=CARTESIAN_POINT('Origin',(-0.00278154034885785,-0.0345610621863028,
0.072808742015884));
#94194=CARTESIAN_POINT('Ctrl Pts',(0.0137993884145856,-0.03424362768739,
0.0750803864889012));
#94195=CARTESIAN_POINT('Ctrl Pts',(0.0137642983096897,-0.033943005420186,
0.0752944455063475));
#94196=CARTESIAN_POINT('Ctrl Pts',(0.01371318408983,-0.0336441434784164,
0.0755052532740882));
#94197=CARTESIAN_POINT('Ctrl Pts',(0.0138344589599498,-0.03424362768739,
0.0748328585978508));
#94198=CARTESIAN_POINT('Ctrl Pts',(0.0138087045233651,-0.033943005420186,
0.0750482403227206));
#94199=CARTESIAN_POINT('Ctrl Pts',(0.0137667998184188,-0.0336441434784164,
0.0752610702410006));
#94200=CARTESIAN_POINT('Ctrl Pts',(0.0137475162976187,-0.0335235895815127,
0.0753478695626977));
#94201=CARTESIAN_POINT('Ctrl Pts',(0.0137310252647002,-0.0334144449262719,
0.0754252913347587));
#94202=CARTESIAN_POINT('Ctrl Pts',(0.0137129158100385,-0.0333049234473133,
0.0755024613627267));
#94203=CARTESIAN_POINT('Ctrl Pts',(0.0136932021514972,-0.0331951640388589,
0.0755792788722186));
#94204=CARTESIAN_POINT('Ctrl Pts',(0.0138438833427115,-0.0335235895815127,
0.0752882493890444));
#94205=CARTESIAN_POINT('Ctrl Pts',(0.0138282130988648,-0.0334144449262719,
0.0753669978432104));
#94206=CARTESIAN_POINT('Ctrl Pts',(0.013810897968008,-0.0333049234473133,
0.0754455130343649));
#94207=CARTESIAN_POINT('Ctrl Pts',(0.0137919509964991,-0.0331951640388589,
0.0755236925600801));
#94208=CARTESIAN_POINT('Ctrl Pts',(0.0139402503878044,-0.0335235895815127,
0.0752286292153912));
#94209=CARTESIAN_POINT('Ctrl Pts',(0.0139254009330293,-0.0334144449262719,
0.0753087043516621));
#94210=CARTESIAN_POINT('Ctrl Pts',(0.0139088801259775,-0.0333049234473133,
0.0753885647060031));
#94211=CARTESIAN_POINT('Ctrl Pts',(0.0138906998415011,-0.0331951640388589,
0.0754681062479417));
#94212=CARTESIAN_POINT('Ctrl Pts',(0.0140366174328973,-0.0335235895815127,
0.0751690090417379));
#94213=CARTESIAN_POINT('Ctrl Pts',(0.0140225887671938,-0.0334144449262719,
0.0752504108601138));
#94214=CARTESIAN_POINT('Ctrl Pts',(0.0140068622839471,-0.0333049234473133,
0.0753316163776412));
#94215=CARTESIAN_POINT('Ctrl Pts',(0.013989448686503,-0.0331951640388589,
0.0754125199358033));
#94216=CARTESIAN_POINT('Origin',(-0.00224467807951498,-0.0326434571769961,
0.07070333641904));
#94217=CARTESIAN_POINT('Ctrl Pts',(0.013906607016739,-0.0336938721132417,
0.0757553527942172));
#94218=CARTESIAN_POINT('Ctrl Pts',(0.0138972103541217,-0.0336474569764972,
0.0757892015868557));
#94219=CARTESIAN_POINT('Ctrl Pts',(0.0138874180925144,-0.033601104548885,
0.0758229380603531));
#94220=CARTESIAN_POINT('Ctrl Pts',(0.0138626263385752,-0.0334837508643185,
0.0759083510510667));
#94221=CARTESIAN_POINT('Ctrl Pts',(0.0138353145074499,-0.0333660264760452,
0.0759929919036535));
#94222=CARTESIAN_POINT('Ctrl Pts',(0.013721576077889,-0.0336938721132417,
0.0754701623474079));
#94223=CARTESIAN_POINT('Ctrl Pts',(0.0137138487295931,-0.0336474569764972,
0.0755029280925615));
#94224=CARTESIAN_POINT('Ctrl Pts',(0.0137057383463631,-0.033601104548885,
0.0755356011342169));
#94225=CARTESIAN_POINT('Ctrl Pts',(0.0136852047216034,-0.0334837508643185,
0.0756183217601209));
#94226=CARTESIAN_POINT('Ctrl Pts',(0.0136622289301495,-0.0333660264760452,
0.075700397607377));
#94227=CARTESIAN_POINT('Ctrl Pts',(0.0137215760778975,-0.0336938721132427,
0.0754701623474244));
#94228=CARTESIAN_POINT('Ctrl Pts',(0.0137138487296023,-0.0336474569765026,
0.0755029280925747));
#94229=CARTESIAN_POINT('Ctrl Pts',(0.0137057383463731,-0.0336011045488949,
0.0755356011342269));
#94230=CARTESIAN_POINT('Ctrl Pts',(0.0136853757387396,-0.0334847282606778,
0.0756176328099879));
#94231=CARTESIAN_POINT('Ctrl Pts',(0.0136626113922525,-0.0333679869945434,
0.07569903069784));
#94232=CARTESIAN_POINT('Ctrl Pts',(0.0137215760778892,-0.0336938721132429,
0.0754701623474071));
#94233=CARTESIAN_POINT('Ctrl Pts',(0.0136939396606921,-0.0335278710435085,
0.0755873471523571));
#94234=CARTESIAN_POINT('Ctrl Pts',(0.0136626380809068,-0.0333620469224321,
0.0757036240611069));
#94235=CARTESIAN_POINT('Ctrl Pts',(0.0136276364306934,-0.0331951640388602,
0.0758190456948265));
#94236=CARTESIAN_POINT('Ctrl Pts',(0.0137390411889619,-0.0336938721132429,
0.0753881684469115));
#94237=CARTESIAN_POINT('Ctrl Pts',(0.0137131212406871,-0.0335278710435085,
0.0755057188683304));
#94238=CARTESIAN_POINT('Ctrl Pts',(0.0136835240603369,-0.0333620469224321,
0.0756224150929454));
#94239=CARTESIAN_POINT('Ctrl Pts',(0.0136502155179694,-0.0331951640388602,
0.0757383102339616));
#94240=CARTESIAN_POINT('Ctrl Pts',(0.0137565063000346,-0.0336938721132429,
0.0753061745464158));
#94241=CARTESIAN_POINT('Ctrl Pts',(0.0137323028206821,-0.0335278710435085,
0.0754240905843038));
#94242=CARTESIAN_POINT('Ctrl Pts',(0.013704410039767,-0.0333620469224321,
0.0755412061247839));
#94243=CARTESIAN_POINT('Ctrl Pts',(0.0136727946052454,-0.0331951640388602,
0.0756575747730968));
#94244=CARTESIAN_POINT('Ctrl Pts',(0.0137739714111073,-0.0336938721132429,
0.0752241806459202));
#94245=CARTESIAN_POINT('Ctrl Pts',(0.0137514844006771,-0.0335278710435085,
0.0753424623002772));
#94246=CARTESIAN_POINT('Ctrl Pts',(0.0137252960191972,-0.0333620469224321,
0.0754599971566224));
#94247=CARTESIAN_POINT('Ctrl Pts',(0.0136953736925213,-0.0331951640388602,
0.0755768393122319));
#94248=CARTESIAN_POINT('Ctrl Pts',(0.0136612049649121,-0.0330240426238156,
0.0756986219119778));
#94249=CARTESIAN_POINT('Ctrl Pts',(0.0136398711893255,-0.0329142774063509,
0.0757749053055085));
#94250=CARTESIAN_POINT('Ctrl Pts',(0.0136169497872423,-0.0328043479726686,
0.0758507857003587));
#94251=CARTESIAN_POINT('Ctrl Pts',(0.0135924674455825,-0.0326943950436594,
0.0759261650794112));
#94252=CARTESIAN_POINT('Ctrl Pts',(0.0137611252827565,-0.0330240426238156,
0.0756451703819095));
#94253=CARTESIAN_POINT('Ctrl Pts',(0.0137405278540719,-0.0329142774063509,
0.0757228302751662));
#94254=CARTESIAN_POINT('Ctrl Pts',(0.013718314709892,-0.0328043479726686,
0.075800103078325));
#94255=CARTESIAN_POINT('Ctrl Pts',(0.0136945115806809,-0.0326943950436594,
0.0758768890154778));
#94256=CARTESIAN_POINT('Ctrl Pts',(0.0138610456006008,-0.0330240426238156,
0.0755917188518412));
#94257=CARTESIAN_POINT('Ctrl Pts',(0.0138411845188182,-0.0329142774063509,
0.0756707552448238));
#94258=CARTESIAN_POINT('Ctrl Pts',(0.0138196796325417,-0.0328043479726686,
0.0757494204562913));
#94259=CARTESIAN_POINT('Ctrl Pts',(0.0137965557157793,-0.0326943950436594,
0.0758276129515443));
#94260=CARTESIAN_POINT('Ctrl Pts',(0.0139609659184451,-0.0330240426238156,
0.0755382673217728));
#94261=CARTESIAN_POINT('Ctrl Pts',(0.0139418411835645,-0.0329142774063509,
0.0756186802144815));
#94262=CARTESIAN_POINT('Ctrl Pts',(0.0139210445551914,-0.0328043479726686,
0.0756987378342575));
#94263=CARTESIAN_POINT('Ctrl Pts',(0.0138985998508777,-0.0326943950436594,
0.0757783368876108));
#94264=CARTESIAN_POINT('Origin',(-0.00236288068206818,-0.0326396682854024,
0.0706669558810331));
#94265=CARTESIAN_POINT('Ctrl Pts',(0.0137934004130372,-0.0331951640388588,
0.0761135246981947));
#94266=CARTESIAN_POINT('Ctrl Pts',(0.0137663568324977,-0.0330855618255041,
0.0761916122196299));
#94267=CARTESIAN_POINT('Ctrl Pts',(0.0137376798210301,-0.0329757224427708,
0.0762691970886851));
#94268=CARTESIAN_POINT('Ctrl Pts',(0.0137074012278423,-0.0328657862078596,
0.0763461781519554));
#94269=CARTESIAN_POINT('Ctrl Pts',(0.0137378141451506,-0.0331951640388588,
0.0760147759318061));
#94270=CARTESIAN_POINT('Ctrl Pts',(0.013712130629101,-0.0330855618255041,
0.0760920978648513));
#94271=CARTESIAN_POINT('Ctrl Pts',(0.0136848304859782,-0.0329757224427708,
0.0761689447038226));
#94272=CARTESIAN_POINT('Ctrl Pts',(0.013655943848186,-0.0328657862078596,
0.076245216326894));
#94273=CARTESIAN_POINT('Ctrl Pts',(0.0136822278772641,-0.0331951640388588,
0.0759160271654175));
#94274=CARTESIAN_POINT('Ctrl Pts',(0.0136579044257043,-0.0330855618255041,
0.0759925835100727));
#94275=CARTESIAN_POINT('Ctrl Pts',(0.0136319811509262,-0.0329757224427708,
0.0760686923189602));
#94276=CARTESIAN_POINT('Ctrl Pts',(0.0136044864685298,-0.0328657862078596,
0.0761442545018326));
#94277=CARTESIAN_POINT('Ctrl Pts',(0.0136266416093775,-0.0331951640388588,
0.0758172783990289));
#94278=CARTESIAN_POINT('Ctrl Pts',(0.0136036782223076,-0.0330855618255041,
0.0758930691552941));
#94279=CARTESIAN_POINT('Ctrl Pts',(0.0135791318158743,-0.0329757224427708,
0.0759684399340977));
#94280=CARTESIAN_POINT('Ctrl Pts',(0.0135530290888735,-0.0328657862078596,
0.0760432926767712));
#94281=CARTESIAN_POINT('Origin',(-0.00217519739879767,-0.0326401908830531,
0.0702241829630992));
#94282=CARTESIAN_POINT('Ctrl Pts',(0.0136380056228228,-0.0332451089994433,
0.0757844616750446));
#94283=CARTESIAN_POINT('Ctrl Pts',(0.013576360892188,-0.0329451141710259,
0.0759924340143016));
#94284=CARTESIAN_POINT('Ctrl Pts',(0.0134992259609365,-0.0326442513127504,
0.0761951721929752));
#94285=CARTESIAN_POINT('Ctrl Pts',(0.0137038261364008,-0.0332451089994433,
0.0755432819495444));
#94286=CARTESIAN_POINT('Ctrl Pts',(0.0136512776479356,-0.0329451141710259,
0.0757537367500862));
#94287=CARTESIAN_POINT('Ctrl Pts',(0.0135830261282573,-0.0326442513127504,
0.07595963550378));
#94288=CARTESIAN_POINT('Ctrl Pts',(0.0135530395745123,-0.0325229783203384,
0.0760432628802644));
#94289=CARTESIAN_POINT('Ctrl Pts',(0.0135269409875858,-0.0324130253112079,
0.0761181050731748));
#94290=CARTESIAN_POINT('Ctrl Pts',(0.0134992981521476,-0.0323031222247694,
0.0761923960320136));
#94291=CARTESIAN_POINT('Ctrl Pts',(0.0134701498346369,-0.0321934096636184,
0.0762660418447972));
#94292=CARTESIAN_POINT('Ctrl Pts',(0.0136561189909885,-0.0325229783203384,
0.0759961908445267));
#94293=CARTESIAN_POINT('Ctrl Pts',(0.0136306692910335,-0.0324130253112079,
0.0760724539849131));
#94294=CARTESIAN_POINT('Ctrl Pts',(0.013603645850027,-0.0323031222247694,
0.0761481790987737));
#94295=CARTESIAN_POINT('Ctrl Pts',(0.0135750867058314,-0.0321934096636184,
0.0762232704090779));
#94296=CARTESIAN_POINT('Ctrl Pts',(0.0137591984074648,-0.0325229783203384,
0.0759491188087889));
#94297=CARTESIAN_POINT('Ctrl Pts',(0.0137343975944812,-0.0324130253112079,
0.0760268028966513));
#94298=CARTESIAN_POINT('Ctrl Pts',(0.0137079935479064,-0.0323031222247694,
0.0761039621655338));
#94299=CARTESIAN_POINT('Ctrl Pts',(0.013680023577026,-0.0321934096636184,
0.0761804989733586));
#94300=CARTESIAN_POINT('Ctrl Pts',(0.0138622778239411,-0.0325229783203384,
0.0759020467730511));
#94301=CARTESIAN_POINT('Ctrl Pts',(0.013838125897929,-0.0324130253112079,
0.0759811518083896));
#94302=CARTESIAN_POINT('Ctrl Pts',(0.0138123412457858,-0.0323031222247694,
0.076059745232294));
#94303=CARTESIAN_POINT('Ctrl Pts',(0.0137849604482206,-0.0321934096636184,
0.0761377275376394));
#94304=CARTESIAN_POINT('Origin',(-0.00235486772564658,-0.0326393375178655,
0.0706698685348405));
#94305=CARTESIAN_POINT('Ctrl Pts',(0.0136589219806714,-0.0326943950436593,
0.0764656484042864));
#94306=CARTESIAN_POINT('Ctrl Pts',(0.0136270080056728,-0.0325844576448127,
0.0765419330045164));
#94307=CARTESIAN_POINT('Ctrl Pts',(0.0135935140814695,-0.0324744968375319,
0.0766175629701994));
#94308=CARTESIAN_POINT('Ctrl Pts',(0.0135584844589939,-0.0323646534831895,
0.076692441991731));
#94309=CARTESIAN_POINT('Ctrl Pts',(0.0136096459328591,-0.0326943950436593,
0.0763636043025727));
#94310=CARTESIAN_POINT('Ctrl Pts',(0.0135791383168331,-0.0325844576448127,
0.0764392097865106));
#94311=CARTESIAN_POINT('Ctrl Pts',(0.013547064896371,-0.0324744968375319,
0.0765141896736488));
#94312=CARTESIAN_POINT('Ctrl Pts',(0.0135134680908844,-0.0323646534831894,
0.0765884484621976));
#94313=CARTESIAN_POINT('Ctrl Pts',(0.0135603698850467,-0.0326943950436593,
0.076261560200859));
#94314=CARTESIAN_POINT('Ctrl Pts',(0.0135312686279934,-0.0325844576448127,
0.0763364865685049));
#94315=CARTESIAN_POINT('Ctrl Pts',(0.0135006157112725,-0.0324744968375319,
0.0764108163770983));
#94316=CARTESIAN_POINT('Ctrl Pts',(0.0134684517227749,-0.0323646534831894,
0.0764844549326643));
#94317=CARTESIAN_POINT('Ctrl Pts',(0.0135110938372344,-0.0326943950436593,
0.0761595160991453));
#94318=CARTESIAN_POINT('Ctrl Pts',(0.0134833989391537,-0.0325844576448127,
0.0762337633504992));
#94319=CARTESIAN_POINT('Ctrl Pts',(0.013454166526174,-0.0324744968375319,
0.0763074430805478));
#94320=CARTESIAN_POINT('Ctrl Pts',(0.0134234353546655,-0.0323646534831894,
0.076380461403131));
#94321=CARTESIAN_POINT('Origin',(-0.00221071737745596,-0.0326395579069148,
0.07021113332839));
#94322=CARTESIAN_POINT('Ctrl Pts',(0.0135245093507114,-0.0327445246961878,
0.0761274405602016));
#94323=CARTESIAN_POINT('Ctrl Pts',(0.0134499289615361,-0.0324436878365476,
0.0763311323127379));
#94324=CARTESIAN_POINT('Ctrl Pts',(0.0133602175522251,-0.0321434074463188,
0.0765286276988619));
#94325=CARTESIAN_POINT('Ctrl Pts',(0.0136053421694281,-0.0327445246961878,
0.0758908691007685));
#94326=CARTESIAN_POINT('Ctrl Pts',(0.0135396842186145,-0.0324436878365476,
0.0760976095128697));
#94327=CARTESIAN_POINT('Ctrl Pts',(0.0134586402624646,-0.0321434074463188,
0.0762988169721559));
#94328=CARTESIAN_POINT('Ctrl Pts',(0.0133874362929384,-0.0322357242816073,
0.0764677727492884));
#94329=CARTESIAN_POINT('Ctrl Pts',(0.0133136182369147,-0.0319819883628706,
0.0766354133056589));
#94330=CARTESIAN_POINT('Ctrl Pts',(0.0132292823341623,-0.0317295851069885,
0.0767980168635604));
#94331=CARTESIAN_POINT('Ctrl Pts',(0.0134831886711788,-0.0322357242816073,
0.0762368366497688));
#94332=CARTESIAN_POINT('Ctrl Pts',(0.0134167256304116,-0.0319819883628706,
0.0764075267952));
#94333=CARTESIAN_POINT('Ctrl Pts',(0.0133395357829886,-0.0317295851069885,
0.0765736417824531));
#94334=CARTESIAN_POINT('Origin',(-0.00212228582860941,-0.0326371942647832,
0.0702466616927344));
#94335=CARTESIAN_POINT('Origin',(-0.00223934016449962,-0.0326352985530809,
0.0707113074730911));
#94336=CARTESIAN_POINT('Ctrl Pts',(0.013502598880332,-0.0321934096636183,
0.0768086333040518));
#94337=CARTESIAN_POINT('Ctrl Pts',(0.0134659342550564,-0.0320835708272303,
0.0768828113781633));
#94338=CARTESIAN_POINT('Ctrl Pts',(0.0134277557853652,-0.0319739230346346,
0.0769561876534628));
#94339=CARTESIAN_POINT('Ctrl Pts',(0.0133881195229781,-0.0318646057455575,
0.0770286719989447));
#94340=CARTESIAN_POINT('Ctrl Pts',(0.01345982740778,-0.0321934096636183,
0.0767036963424907));
#94341=CARTESIAN_POINT('Ctrl Pts',(0.0134246099449873,-0.0320835708272303,
0.0767772845646617));
#94342=CARTESIAN_POINT('Ctrl Pts',(0.0133878900053211,-0.0319739230346346,
0.076850101279111));
#94343=CARTESIAN_POINT('Ctrl Pts',(0.0133497217194684,-0.0318646057455575,
0.0769220569275356));
#94344=CARTESIAN_POINT('Ctrl Pts',(0.0134170559352281,-0.0321934096636183,
0.0765987593809296));
#94345=CARTESIAN_POINT('Ctrl Pts',(0.0133832856349181,-0.0320835708272303,
0.07667175775116));
#94346=CARTESIAN_POINT('Ctrl Pts',(0.013348024225277,-0.0319739230346346,
0.0767440149047593));
#94347=CARTESIAN_POINT('Ctrl Pts',(0.0133113239159587,-0.0318646057455575,
0.0768154418561265));
#94348=CARTESIAN_POINT('Ctrl Pts',(0.0133742844626761,-0.0321934096636183,
0.0764938224193685));
#94349=CARTESIAN_POINT('Ctrl Pts',(0.013341961324849,-0.0320835708272303,
0.0765662309376583));
#94350=CARTESIAN_POINT('Ctrl Pts',(0.0133081584452328,-0.0319739230346346,
0.0766379285304076));
#94351=CARTESIAN_POINT('Ctrl Pts',(0.013272926112449,-0.0318646057455575,
0.0767088267847174));
#94352=CARTESIAN_POINT('Ctrl Pts',(0.0134243802119738,-0.0320218834582289,
0.0763803493992706));
#94353=CARTESIAN_POINT('Ctrl Pts',(0.0134011676665627,-0.0319391099350591,
0.076435515810533));
#94354=CARTESIAN_POINT('Ctrl Pts',(0.013377107753796,-0.0318564869454879,
0.0764902863307171));
#94355=CARTESIAN_POINT('Ctrl Pts',(0.0133522217224225,-0.0317740741446479,
0.0765446227027933));
#94356=CARTESIAN_POINT('Ctrl Pts',(0.0134706728047956,-0.0320218834582289,
0.0763626343238399));
#94357=CARTESIAN_POINT('Ctrl Pts',(0.0134476446304938,-0.0319391099350591,
0.0764182825290819));
#94358=CARTESIAN_POINT('Ctrl Pts',(0.0134237614538501,-0.0318564869454879,
0.0764735374303196));
#94359=CARTESIAN_POINT('Ctrl Pts',(0.0133990444278215,-0.0317740741446479,
0.0765283604056984));
#94360=CARTESIAN_POINT('Ctrl Pts',(0.0135169653976174,-0.0320218834582289,
0.0763449192484091));
#94361=CARTESIAN_POINT('Ctrl Pts',(0.013494121594425,-0.0319391099350591,
0.0764010492476308));
#94362=CARTESIAN_POINT('Ctrl Pts',(0.0134704151539042,-0.0318564869454879,
0.0764567885299222));
#94363=CARTESIAN_POINT('Ctrl Pts',(0.0134458671332205,-0.0317740741446479,
0.0765120981086035));
#94364=CARTESIAN_POINT('Ctrl Pts',(0.0135632579904393,-0.0320218834582289,
0.0763272041729783));
#94365=CARTESIAN_POINT('Ctrl Pts',(0.0135405985583561,-0.0319391099350591,
0.0763838159661797));
#94366=CARTESIAN_POINT('Ctrl Pts',(0.0135170688539583,-0.0318564869454879,
0.0764400396295247));
#94367=CARTESIAN_POINT('Ctrl Pts',(0.0134926898386194,-0.0317740741446479,
0.0764958358115086));
#94368=CARTESIAN_POINT('Origin',(0.0195878915861359,-0.0391228853390771,
0.0779519487312299));
#94369=CARTESIAN_POINT('Ctrl Pts',(0.013822693757782,-0.0352722978779567,
0.0733711729841441));
#94370=CARTESIAN_POINT('Ctrl Pts',(0.0138249051228944,-0.0352466642097199,
0.0733899400441789));
#94371=CARTESIAN_POINT('Ctrl Pts',(0.0138271923802544,-0.0352210183808292,
0.0734086812102294));
#94372=CARTESIAN_POINT('Ctrl Pts',(0.0138295561391753,-0.0351953608940151,
0.0734273970791384));
#94373=CARTESIAN_POINT('Origin',(0.018706873236719,-0.0352456003065015,
0.0729780648421797));
#94374=CARTESIAN_POINT('Ctrl Pts',(0.0138424333923555,-0.0350241211493338,
0.0735514111580519));
#94375=CARTESIAN_POINT('Ctrl Pts',(0.0138506787078506,-0.0349144232867421,
0.0736301832300313));
#94376=CARTESIAN_POINT('Ctrl Pts',(0.0138573006836223,-0.0348045283677512,
0.0737091728874461));
#94377=CARTESIAN_POINT('Ctrl Pts',(0.0138622870727791,-0.0346945769586886,
0.0737882792702225));
#94378=CARTESIAN_POINT('Ctrl Pts',(0.0139156601524725,-0.0350241211493338,
0.0734649300421613));
#94379=CARTESIAN_POINT('Ctrl Pts',(0.0139250967098266,-0.0349144232867421,
0.0735447107826918));
#94380=CARTESIAN_POINT('Ctrl Pts',(0.0139328897905743,-0.0348045283677512,
0.0736247343362135));
#94381=CARTESIAN_POINT('Ctrl Pts',(0.0139390255985074,-0.0346945769586886,
0.0737048985741835));
#94382=CARTESIAN_POINT('Ctrl Pts',(0.0139888869125895,-0.0350241211493338,
0.0733784489262708));
#94383=CARTESIAN_POINT('Ctrl Pts',(0.0139995147118027,-0.0349144232867421,
0.0734592383353522));
#94384=CARTESIAN_POINT('Ctrl Pts',(0.0140084788975263,-0.0348045283677512,
0.073540295784981));
#94385=CARTESIAN_POINT('Ctrl Pts',(0.0140157641242358,-0.0346945769586886,
0.0736215178781444));
#94386=CARTESIAN_POINT('Ctrl Pts',(0.0140621136727065,-0.0350241211493338,
0.0732919678103802));
#94387=CARTESIAN_POINT('Ctrl Pts',(0.0140739327137787,-0.0349144232867421,
0.0733737658880126));
#94388=CARTESIAN_POINT('Ctrl Pts',(0.0140840680044782,-0.0348045283677512,
0.0734558572337484));
#94389=CARTESIAN_POINT('Ctrl Pts',(0.0140925026499641,-0.0346945769586886,
0.0735381371821054));
#94390=CARTESIAN_POINT('Origin',(-0.00290359790462051,-0.0345629067941849,
0.0746646638922539));
#94391=CARTESIAN_POINT('Ctrl Pts',(0.0140459665905722,-0.035197097365154,
0.0738286688005412));
#94392=CARTESIAN_POINT('Ctrl Pts',(0.014050418198839,-0.0350869349326852,
0.0739107126390035));
#94393=CARTESIAN_POINT('Ctrl Pts',(0.0140531678488388,-0.0349764985139983,
0.073992916988095));
#94394=CARTESIAN_POINT('Ctrl Pts',(0.0140542057092152,-0.0348659306865088,
0.0740751755593631));
#94395=CARTESIAN_POINT('Ctrl Pts',(0.0139820774768958,-0.035197097365154,
0.0737769131071014));
#94396=CARTESIAN_POINT('Ctrl Pts',(0.0139872460901505,-0.0350869349326852,
0.0738580718484829));
#94397=CARTESIAN_POINT('Ctrl Pts',(0.0139907317397745,-0.0349764985139983,
0.0739394052734259));
#94398=CARTESIAN_POINT('Ctrl Pts',(0.0139925237073211,-0.0348659306865088,
0.0740208082779145));
#94399=CARTESIAN_POINT('Ctrl Pts',(0.0139181883632194,-0.035197097365154,
0.0737251574136616));
#94400=CARTESIAN_POINT('Ctrl Pts',(0.013924073981462,-0.0350869349326852,
0.0738054310579624));
#94401=CARTESIAN_POINT('Ctrl Pts',(0.0139282956307102,-0.0349764985139983,
0.0738858935587567));
#94402=CARTESIAN_POINT('Ctrl Pts',(0.0139308417054269,-0.0348659306865088,
0.0739664409964658));
#94403=CARTESIAN_POINT('Ctrl Pts',(0.0138542992495431,-0.035197097365154,
0.0736734017202218));
#94404=CARTESIAN_POINT('Ctrl Pts',(0.0138609018727735,-0.0350869349326852,
0.0737527902674419));
#94405=CARTESIAN_POINT('Ctrl Pts',(0.0138658595216458,-0.0349764985139983,
0.0738323818440876));
#94406=CARTESIAN_POINT('Ctrl Pts',(0.0138691597035328,-0.0348659306865088,
0.0739120737150172));
#94407=CARTESIAN_POINT('Origin',(-0.00288050121975449,-0.0345637187969441,
0.0741842558375359));
#94408=CARTESIAN_POINT('Ctrl Pts',(0.0138524634841713,-0.0352450361861253,
0.0736397690077748));
#94409=CARTESIAN_POINT('Ctrl Pts',(0.013871707161322,-0.0349452761023764,
0.0738558297625003));
#94410=CARTESIAN_POINT('Ctrl Pts',(0.0138746215895376,-0.0346444289983475,
0.0740727262238615));
#94411=CARTESIAN_POINT('Ctrl Pts',(0.0138248779320376,-0.0352450361861253,
0.0733912955940793));
#94412=CARTESIAN_POINT('Ctrl Pts',(0.0138534929375211,-0.0349452761023764,
0.0736063159426606));
#94413=CARTESIAN_POINT('Ctrl Pts',(0.0138658304387593,-0.0346444289983475,
0.073822880840338));
#94414=CARTESIAN_POINT('Ctrl Pts',(0.0138687346586722,-0.0345231616327822,
0.0739116684421894));
#94415=CARTESIAN_POINT('Ctrl Pts',(0.0138720197236526,-0.0344132092796975,
0.0739908545236805));
#94416=CARTESIAN_POINT('Ctrl Pts',(0.0138736667175042,-0.0343032738558973,
0.0740701044685118));
#94417=CARTESIAN_POINT('Ctrl Pts',(0.013873676130924,-0.034193496108874,
0.0741493166942968));
#94418=CARTESIAN_POINT('Ctrl Pts',(0.0139472470862997,-0.0345231616327822,
0.0738299559287879));
#94419=CARTESIAN_POINT('Ctrl Pts',(0.0139516584432353,-0.0344132092796975,
0.0739102241935573));
#94420=CARTESIAN_POINT('Ctrl Pts',(0.0139544092868232,-0.0343032738558973,
0.0739905795622917));
#94421=CARTESIAN_POINT('Ctrl Pts',(0.0139554987298771,-0.034193496108874,
0.0740709190002049));
#94422=CARTESIAN_POINT('Ctrl Pts',(0.0140257595139273,-0.0345231616327822,
0.0737482434153864));
#94423=CARTESIAN_POINT('Ctrl Pts',(0.0140312971628181,-0.0344132092796975,
0.0738295938634339));
#94424=CARTESIAN_POINT('Ctrl Pts',(0.0140351518561422,-0.0343032738558973,
0.0739110546560716));
#94425=CARTESIAN_POINT('Ctrl Pts',(0.0140373213288301,-0.034193496108874,
0.073992521306113));
#94426=CARTESIAN_POINT('Ctrl Pts',(0.0141042719415548,-0.0345231616327822,
0.0736665309019849));
#94427=CARTESIAN_POINT('Ctrl Pts',(0.0141109358824009,-0.0344132092796975,
0.0737489635333106));
#94428=CARTESIAN_POINT('Ctrl Pts',(0.0141158944254612,-0.0343032738558973,
0.0738315297498515));
#94429=CARTESIAN_POINT('Ctrl Pts',(0.0141191439277832,-0.034193496108874,
0.0739141236120211));
#94430=CARTESIAN_POINT('Origin',(-0.00291567412291486,-0.0345625596233013,
0.0746654782917601));
#94431=CARTESIAN_POINT('Ctrl Pts',(0.0141226720466942,-0.0346945769586885,
0.0742654145775485));
#94432=CARTESIAN_POINT('Ctrl Pts',(0.0141210815754795,-0.0345846629176052,
0.074348082311858));
#94433=CARTESIAN_POINT('Ctrl Pts',(0.0141177812978126,-0.0344746925050311,
0.0744307312757282));
#94434=CARTESIAN_POINT('Ctrl Pts',(0.0141127758797389,-0.0343648066253259,
0.0745132555872463));
#94435=CARTESIAN_POINT('Ctrl Pts',(0.0140392914163022,-0.0346945769586885,
0.0741886761122377));
#94436=CARTESIAN_POINT('Ctrl Pts',(0.0140387584399268,-0.0345846629176052,
0.0742701948193158));
#94437=CARTESIAN_POINT('Ctrl Pts',(0.0140365395991332,-0.0344746925050311,
0.0743517164282569));
#94438=CARTESIAN_POINT('Ctrl Pts',(0.0140326381683396,-0.0343648066253259,
0.0744331364959228));
#94439=CARTESIAN_POINT('Ctrl Pts',(0.0139559107859102,-0.0346945769586885,
0.0741119376469268));
#94440=CARTESIAN_POINT('Ctrl Pts',(0.013956435304374,-0.0345846629176052,
0.0741923073267736));
#94441=CARTESIAN_POINT('Ctrl Pts',(0.0139552979004537,-0.0344746925050311,
0.0742727015807857));
#94442=CARTESIAN_POINT('Ctrl Pts',(0.0139525004569403,-0.0343648066253259,
0.0743530174045992));
#94443=CARTESIAN_POINT('Ctrl Pts',(0.0138725301555181,-0.0346945769586885,
0.074035199181616));
#94444=CARTESIAN_POINT('Ctrl Pts',(0.0138741121688213,-0.0345846629176052,
0.0741144198342314));
#94445=CARTESIAN_POINT('Ctrl Pts',(0.0138740562017742,-0.0344746925050311,
0.0741936867333144));
#94446=CARTESIAN_POINT('Ctrl Pts',(0.0138723627455409,-0.0343648066253259,
0.0742728983132757));
#94447=CARTESIAN_POINT('Origin',(-0.00293892388889004,-0.0345626446733475,
0.0741852162475095));
#94448=CARTESIAN_POINT('Ctrl Pts',(0.013874022114592,-0.0346945769586885,
0.0740365722900838));
#94449=CARTESIAN_POINT('Ctrl Pts',(0.0138763979033902,-0.034527515336289,
0.0741570133675078));
#94450=CARTESIAN_POINT('Ctrl Pts',(0.0138749865456624,-0.0343603235965158,
0.0742775603135345));
#94451=CARTESIAN_POINT('Ctrl Pts',(0.013869797514459,-0.0341934961088739,
0.0743978566658474));
#94452=CARTESIAN_POINT('Ctrl Pts',(0.0138705474735907,-0.0346945769586885,
0.0739528109911374));
#94453=CARTESIAN_POINT('Ctrl Pts',(0.0138746776763315,-0.034527515336289,
0.0740731792908145));
#94454=CARTESIAN_POINT('Ctrl Pts',(0.0138750234751208,-0.0343603235965158,
0.0741937086149738));
#94455=CARTESIAN_POINT('Ctrl Pts',(0.0138715891453453,-0.0341934961088739,
0.0743140424761774));
#94456=CARTESIAN_POINT('Ctrl Pts',(0.0138670728325894,-0.0346945769586885,
0.073869049692191));
#94457=CARTESIAN_POINT('Ctrl Pts',(0.0138729574492728,-0.034527515336289,
0.0739893452141212));
#94458=CARTESIAN_POINT('Ctrl Pts',(0.0138750604045792,-0.0343603235965158,
0.0741098569164131));
#94459=CARTESIAN_POINT('Ctrl Pts',(0.0138733807762316,-0.0341934961088739,
0.0742302282865074));
#94460=CARTESIAN_POINT('Ctrl Pts',(0.0138635981915882,-0.0346945769586885,
0.0737852883932446));
#94461=CARTESIAN_POINT('Ctrl Pts',(0.0138712372222141,-0.034527515336289,
0.0739055111374278));
#94462=CARTESIAN_POINT('Ctrl Pts',(0.0138750973340376,-0.0343603235965158,
0.0740260052178525));
#94463=CARTESIAN_POINT('Ctrl Pts',(0.013875172407118,-0.0341934961088739,
0.0741464140968374));
#94464=CARTESIAN_POINT('Ctrl Pts',(0.0138723628632283,-0.0340223579322365,
0.0742728667542586));
#94465=CARTESIAN_POINT('Ctrl Pts',(0.0138706682102372,-0.0339125849573554,
0.0743521546746266));
#94466=CARTESIAN_POINT('Ctrl Pts',(0.0138673336723471,-0.0338030433565221,
0.0744313518049119));
#94467=CARTESIAN_POINT('Ctrl Pts',(0.0138623724918966,-0.0336938721132327,
0.0745103572433477));
#94468=CARTESIAN_POINT('Ctrl Pts',(0.0139558512654297,-0.0340223579322365,
0.0741962451742169));
#94469=CARTESIAN_POINT('Ctrl Pts',(0.0139552134238648,-0.0339125849573554,
0.0742766846173982));
#94470=CARTESIAN_POINT('Ctrl Pts',(0.0139529111209454,-0.0338030433565221,
0.0743570543348758));
#94471=CARTESIAN_POINT('Ctrl Pts',(0.0139489564118833,-0.0336938721132327,
0.0744372518083244));
#94472=CARTESIAN_POINT('Ctrl Pts',(0.0140393396676311,-0.0340223579322365,
0.0741196235941752));
#94473=CARTESIAN_POINT('Ctrl Pts',(0.0140397586374924,-0.0339125849573554,
0.0742012145601697));
#94474=CARTESIAN_POINT('Ctrl Pts',(0.0140384885695436,-0.0338030433565221,
0.0742827568648396));
#94475=CARTESIAN_POINT('Ctrl Pts',(0.01403554033187,-0.0336938721132327,
0.074364146373301));
#94476=CARTESIAN_POINT('Ctrl Pts',(0.0141228280698325,-0.0340223579322365,
0.0740430020141335));
#94477=CARTESIAN_POINT('Ctrl Pts',(0.01412430385112,-0.0339125849573554,
0.0741257445029412));
#94478=CARTESIAN_POINT('Ctrl Pts',(0.0141240660181418,-0.0338030433565221,
0.0742084593948035));
#94479=CARTESIAN_POINT('Ctrl Pts',(0.0141221242518568,-0.0336938721132327,
0.0742910409382776));
#94480=CARTESIAN_POINT('Origin',(-0.00279549184214396,-0.0345589643412495,
0.0746624620825095));
#94481=CARTESIAN_POINT('Ctrl Pts',(0.0141035876665988,-0.034193496108874,
0.0746418602437495));
#94482=CARTESIAN_POINT('Ctrl Pts',(0.0140968052051056,-0.0340836138581107,
0.0747243182201288));
#94483=CARTESIAN_POINT('Ctrl Pts',(0.014088319703164,-0.03397388966435,
0.0748065962828118));
#94484=CARTESIAN_POINT('Ctrl Pts',(0.0140781490803299,-0.0338644633294063,
0.0748885898540643));
#94485=CARTESIAN_POINT('Ctrl Pts',(0.0140251899019621,-0.034193496108874,
0.0745600375711698));
#94486=CARTESIAN_POINT('Ctrl Pts',(0.0140195357266702,-0.0340836138581107,
0.0746414144888));
#94487=CARTESIAN_POINT('Ctrl Pts',(0.0140122003397996,-0.03397388966435,
0.0747226353589618));
#94488=CARTESIAN_POINT('Ctrl Pts',(0.0140032000981974,-0.0338644633294063,
0.074803596858321));
#94489=CARTESIAN_POINT('Ctrl Pts',(0.0139467921373253,-0.034193496108874,
0.0744782148985901));
#94490=CARTESIAN_POINT('Ctrl Pts',(0.0139422662482349,-0.0340836138581107,
0.0745585107574713));
#94491=CARTESIAN_POINT('Ctrl Pts',(0.0139360809764352,-0.0339738896643499,
0.0746386744351118));
#94492=CARTESIAN_POINT('Ctrl Pts',(0.0139282511160649,-0.0338644633294062,
0.0747186038625776));
#94493=CARTESIAN_POINT('Ctrl Pts',(0.0138683943726886,-0.034193496108874,
0.0743963922260104));
#94494=CARTESIAN_POINT('Ctrl Pts',(0.0138649967697996,-0.0340836138581107,
0.0744756070261426));
#94495=CARTESIAN_POINT('Ctrl Pts',(0.0138599616130708,-0.0339738896643499,
0.0745547135112618));
#94496=CARTESIAN_POINT('Ctrl Pts',(0.0138533021339323,-0.0338644633294062,
0.0746336108668343));
#94497=CARTESIAN_POINT('Origin',(-0.0028636528235915,-0.0345610621865684,
0.0741861175733144));
#94498=CARTESIAN_POINT('Ctrl Pts',(0.0138712429114264,-0.03424362768739,
0.0743617080333678));
#94499=CARTESIAN_POINT('Ctrl Pts',(0.0138632582113186,-0.0339430054201859,
0.074578477087838));
#94500=CARTESIAN_POINT('Ctrl Pts',(0.0138389682615409,-0.0336441434784161,
0.0747940288838211));
#94501=CARTESIAN_POINT('Ctrl Pts',(0.0138750134440826,-0.03424362768739,
0.0741117364688179));
#94502=CARTESIAN_POINT('Ctrl Pts',(0.0138764565769514,-0.0339430054201859,
0.0743286477312716));
#94503=CARTESIAN_POINT('Ctrl Pts',(0.0138615569649772,-0.0336441434784161,
0.0745450514742492));
#94504=CARTESIAN_POINT('Ctrl Pts',(0.0138533043401578,-0.0335235895815127,
0.0746335832233854));
#94505=CARTESIAN_POINT('Ctrl Pts',(0.0138466468650002,-0.0334144449262718,
0.0747124613761294));
#94506=CARTESIAN_POINT('Ctrl Pts',(0.013838352177937,-0.0333049234473133,
0.0747912926118882));
#94507=CARTESIAN_POINT('Ctrl Pts',(0.0138284217543404,-0.0331951640388588,
0.0748699751689439));
#94508=CARTESIAN_POINT('Ctrl Pts',(0.0139414391131666,-0.0335235895815127,
0.0745623551792388));
#94509=CARTESIAN_POINT('Ctrl Pts',(0.0139357622322718,-0.0334144449262718,
0.0746424466806548));
#94510=CARTESIAN_POINT('Ctrl Pts',(0.013928424199185,-0.0333049234473133,
0.0747225129174156));
#94511=CARTESIAN_POINT('Ctrl Pts',(0.013919425122962,-0.0331951640388588,
0.0748024506594249));
#94512=CARTESIAN_POINT('Ctrl Pts',(0.0140295738861754,-0.0335235895815127,
0.0744911271350923));
#94513=CARTESIAN_POINT('Ctrl Pts',(0.0140248775995434,-0.0334144449262718,
0.0745724319851801));
#94514=CARTESIAN_POINT('Ctrl Pts',(0.014018496220433,-0.0333049234473133,
0.0746537332229428));
#94515=CARTESIAN_POINT('Ctrl Pts',(0.0140104284915836,-0.0331951640388588,
0.074734926149906));
#94516=CARTESIAN_POINT('Ctrl Pts',(0.0141177086591842,-0.0335235895815127,
0.0744198990909458));
#94517=CARTESIAN_POINT('Ctrl Pts',(0.014113992966815,-0.0334144449262718,
0.0745024172897054));
#94518=CARTESIAN_POINT('Ctrl Pts',(0.0141085682416809,-0.0333049234473133,
0.0745849535284701));
#94519=CARTESIAN_POINT('Ctrl Pts',(0.0141014318602052,-0.0331951640388588,
0.074667401640387));
#94520=CARTESIAN_POINT('Origin',(-0.00259490116497956,-0.0326434571769064,
0.0720300270437704));
#94521=CARTESIAN_POINT('Ctrl Pts',(0.0140622117724693,-0.033693872113241,
0.0750179139736581));
#94522=CARTESIAN_POINT('Ctrl Pts',(0.014057131583977,-0.0336474569764968,
0.0750526735725668));
#94523=CARTESIAN_POINT('Ctrl Pts',(0.0140516448385898,-0.033601104548885,
0.0750873713197049));
#94524=CARTESIAN_POINT('Ctrl Pts',(0.0140377536613498,-0.0334837508643181,
0.0751752180341624));
#94525=CARTESIAN_POINT('Ctrl Pts',(0.0140212655039169,-0.0333660264760445,
0.0752626145484553));
#94526=CARTESIAN_POINT('Ctrl Pts',(0.013842896016958,-0.033693872113241,
0.0747581628645798));
#94527=CARTESIAN_POINT('Ctrl Pts',(0.0138393362379017,-0.0336474569764968,
0.0747916387355947));
#94528=CARTESIAN_POINT('Ctrl Pts',(0.0138353848254269,-0.033601104548885,
0.0748250706411131));
#94529=CARTESIAN_POINT('Ctrl Pts',(0.0138253807579586,-0.0334837508643181,
0.0749097125357627));
#94530=CARTESIAN_POINT('Ctrl Pts',(0.0138128729688169,-0.0333660264760445,
0.074994020820685));
#94531=CARTESIAN_POINT('Ctrl Pts',(0.0138428960169673,-0.0336938721132427,
0.0747581628645958));
#94532=CARTESIAN_POINT('Ctrl Pts',(0.0138393362379113,-0.0336474569765026,
0.0747916387356076));
#94533=CARTESIAN_POINT('Ctrl Pts',(0.0138353848254369,-0.0336011045488949,
0.0748250706411231));
#94534=CARTESIAN_POINT('Ctrl Pts',(0.0138254640782245,-0.0334847282606778,
0.0749090075840775));
#94535=CARTESIAN_POINT('Ctrl Pts',(0.0138130810958987,-0.0333679869945434,
0.0749926167544268));
#94536=CARTESIAN_POINT('Ctrl Pts',(0.0138428960169581,-0.0336938721132429,
0.0747581628645785));
#94537=CARTESIAN_POINT('Ctrl Pts',(0.0138301646716942,-0.0335278710435085,
0.0748778873938714));
#94538=CARTESIAN_POINT('Ctrl Pts',(0.0138136832751773,-0.0333620469224321,
0.0749971705526756));
#94539=CARTESIAN_POINT('Ctrl Pts',(0.0137934237900076,-0.0331951640388602,
0.0751160689223398));
#94540=CARTESIAN_POINT('Ctrl Pts',(0.0138499468497317,-0.0336938721132429,
0.0746746265516333));
#94541=CARTESIAN_POINT('Ctrl Pts',(0.0138389642624143,-0.0335278710435085,
0.0747944986837998));
#94542=CARTESIAN_POINT('Ctrl Pts',(0.0138242263798471,-0.0333620469224321,
0.0749139842341458));
#94543=CARTESIAN_POINT('Ctrl Pts',(0.0138057059980629,-0.0331951640388602,
0.0750331401746792));
#94544=CARTESIAN_POINT('Ctrl Pts',(0.0138569976825054,-0.0336938721132429,
0.0745910902386881));
#94545=CARTESIAN_POINT('Ctrl Pts',(0.0138477638531344,-0.0335278710435085,
0.0747111099737282));
#94546=CARTESIAN_POINT('Ctrl Pts',(0.013834769484517,-0.0333620469224321,
0.074830797915616));
#94547=CARTESIAN_POINT('Ctrl Pts',(0.0138179882061182,-0.0331951640388602,
0.0749502114270185));
#94548=CARTESIAN_POINT('Ctrl Pts',(0.013864048515279,-0.0336938721132429,
0.0745075539257429));
#94549=CARTESIAN_POINT('Ctrl Pts',(0.0138565634438545,-0.0335278710435085,
0.0746277212636567));
#94550=CARTESIAN_POINT('Ctrl Pts',(0.0138453125891868,-0.0333620469224321,
0.0747476115970862));
#94551=CARTESIAN_POINT('Ctrl Pts',(0.0138302704141734,-0.0331951640388602,
0.0748672826793579));
#94552=CARTESIAN_POINT('Ctrl Pts',(0.0138116345242051,-0.0330240426238155,
0.074992387464048));
#94553=CARTESIAN_POINT('Ctrl Pts',(0.0138000298161896,-0.0329142774063506,
0.0750707431713147));
#94554=CARTESIAN_POINT('Ctrl Pts',(0.0137867994914587,-0.0328043479726681,
0.0751488980400283));
#94555=CARTESIAN_POINT('Ctrl Pts',(0.0137719577416961,-0.0326943950436586,
0.0752267514812079));
#94556=CARTESIAN_POINT('Ctrl Pts',(0.0139040676873957,-0.0330240426238155,
0.0749268340787256));
#94557=CARTESIAN_POINT('Ctrl Pts',(0.0138933660411285,-0.0329142774063506,
0.0750064631428685));
#94558=CARTESIAN_POINT('Ctrl Pts',(0.0138810129045117,-0.0328043479726681,
0.075085910672082));
#94559=CARTESIAN_POINT('Ctrl Pts',(0.0138670212998796,-0.0326943950436586,
0.0751650744523387));
#94560=CARTESIAN_POINT('Ctrl Pts',(0.0139965008505862,-0.0330240426238155,
0.0748612806934032));
#94561=CARTESIAN_POINT('Ctrl Pts',(0.0139867022660674,-0.0329142774063506,
0.0749421831144223));
#94562=CARTESIAN_POINT('Ctrl Pts',(0.0139752263175646,-0.0328043479726681,
0.0750229233041358));
#94563=CARTESIAN_POINT('Ctrl Pts',(0.0139620848580632,-0.0326943950436586,
0.0751033974234695));
#94564=CARTESIAN_POINT('Ctrl Pts',(0.0140889340137767,-0.0330240426238155,
0.0747957273080808));
#94565=CARTESIAN_POINT('Ctrl Pts',(0.0140800384910063,-0.0329142774063506,
0.0748779030859761));
#94566=CARTESIAN_POINT('Ctrl Pts',(0.0140694397306175,-0.0328043479726681,
0.0749599359361896));
#94567=CARTESIAN_POINT('Ctrl Pts',(0.0140571484162467,-0.0326943950436586,
0.0750417203946003));
#94568=CARTESIAN_POINT('Origin',(-0.00271673139515919,-0.0326396682855295,
0.0720087480918698));
#94569=CARTESIAN_POINT('Ctrl Pts',(0.0139947886795482,-0.0331951640388588,
0.0753874501348943));
#94570=CARTESIAN_POINT('Ctrl Pts',(0.0139777453072813,-0.0330855618255041,
0.0754683113722955));
#94571=CARTESIAN_POINT('Ctrl Pts',(0.013959018385129,-0.0329757224427708,
0.0755488786440608));
#94572=CARTESIAN_POINT('Ctrl Pts',(0.0139386268332751,-0.0328657862078596,
0.0756290476026461));
#94573=CARTESIAN_POINT('Ctrl Pts',(0.0139272642237848,-0.0331951640388588,
0.0752964468387195));
#94574=CARTESIAN_POINT('Ctrl Pts',(0.0139114742378245,-0.0330855618255041,
0.0753763780633434));
#94575=CARTESIAN_POINT('Ctrl Pts',(0.0138940208273019,-0.0329757224427708,
0.0754560405572507));
#94576=CARTESIAN_POINT('Ctrl Pts',(0.0138749213384255,-0.0328657862078596,
0.0755353312115142));
#94577=CARTESIAN_POINT('Ctrl Pts',(0.0138597397680214,-0.0331951640388588,
0.0752054435425447));
#94578=CARTESIAN_POINT('Ctrl Pts',(0.0138452031683678,-0.0330855618255041,
0.0752844447543914));
#94579=CARTESIAN_POINT('Ctrl Pts',(0.0138290232694748,-0.0329757224427708,
0.0753632024704407));
#94580=CARTESIAN_POINT('Ctrl Pts',(0.0138112158435759,-0.0328657862078596,
0.0754416148203823));
#94581=CARTESIAN_POINT('Ctrl Pts',(0.013792215312258,-0.0331951640388588,
0.0751144402463699));
#94582=CARTESIAN_POINT('Ctrl Pts',(0.013778932098911,-0.0330855618255041,
0.0751925114454393));
#94583=CARTESIAN_POINT('Ctrl Pts',(0.0137640257116477,-0.0329757224427708,
0.0752703643836306));
#94584=CARTESIAN_POINT('Ctrl Pts',(0.0137475103487263,-0.0328657862078596,
0.0753478984292504));
#94585=CARTESIAN_POINT('Origin',(-0.00258602221238202,-0.0326401908833295,
0.0715459436180389));
#94586=CARTESIAN_POINT('Ctrl Pts',(0.0137993766909311,-0.0332451089994434,
0.0750804580035046));
#94587=CARTESIAN_POINT('Ctrl Pts',(0.0137642838931807,-0.0329451141710259,
0.0752945165521709));
#94588=CARTESIAN_POINT('Ctrl Pts',(0.0137131670254013,-0.0326442513127503,
0.0755053236501053));
#94589=CARTESIAN_POINT('Ctrl Pts',(0.0138344503552328,-0.0332451089994434,
0.0748329305543754));
#94590=CARTESIAN_POINT('Ctrl Pts',(0.0138086932079656,-0.0329451141710259,
0.0750483119279333));
#94591=CARTESIAN_POINT('Ctrl Pts',(0.013766785828493,-0.0326442513127503,
0.0752611412921123));
#94592=CARTESIAN_POINT('Ctrl Pts',(0.0137475170171901,-0.0325229783203385,
0.0753478675534991));
#94593=CARTESIAN_POINT('Ctrl Pts',(0.0137310044394613,-0.0324130253112079,
0.075425390613655));
#94594=CARTESIAN_POINT('Ctrl Pts',(0.0137128907021329,-0.0323031222247694,
0.0755025603320442));
#94595=CARTESIAN_POINT('Ctrl Pts',(0.0136932024956666,-0.0321934096636184,
0.0755792786784837));
#94596=CARTESIAN_POINT('Ctrl Pts',(0.0138438839312293,-0.0325229783203385,
0.0752882474182422));
#94597=CARTESIAN_POINT('Ctrl Pts',(0.0138281932157462,-0.0324130253112079,
0.0753670988941766));
#94598=CARTESIAN_POINT('Ctrl Pts',(0.0138108737360257,-0.0323031222247694,
0.0754456138281399));
#94599=CARTESIAN_POINT('Ctrl Pts',(0.0137919512259454,-0.0321934096636184,
0.0755236924309236));
#94600=CARTESIAN_POINT('Ctrl Pts',(0.0139402508452684,-0.0325229783203385,
0.0752286272829853));
#94601=CARTESIAN_POINT('Ctrl Pts',(0.0139253819920311,-0.0324130253112079,
0.0753088071746981));
#94602=CARTESIAN_POINT('Ctrl Pts',(0.0139088567699185,-0.0323031222247694,
0.0753886673242356));
#94603=CARTESIAN_POINT('Ctrl Pts',(0.0138906999562241,-0.0321934096636184,
0.0754681061833634));
#94604=CARTESIAN_POINT('Ctrl Pts',(0.0140366177593076,-0.0325229783203385,
0.0751690071477284));
#94605=CARTESIAN_POINT('Ctrl Pts',(0.014022570768316,-0.0324130253112079,
0.0752505154552196));
#94606=CARTESIAN_POINT('Ctrl Pts',(0.0140068398038113,-0.0323031222247694,
0.0753317208203313));
#94607=CARTESIAN_POINT('Ctrl Pts',(0.0139894486865029,-0.0321934096636184,
0.0754125199358033));
#94608=CARTESIAN_POINT('Origin',(-0.00270841657096725,-0.0326393375178475,
0.0720106334885954));
#94609=CARTESIAN_POINT('Ctrl Pts',(0.0139055034524876,-0.0326943950436594,
0.0757536518571623));
#94610=CARTESIAN_POINT('Ctrl Pts',(0.0138834021243321,-0.0325844576448127,
0.0758333348122168));
#94611=CARTESIAN_POINT('Ctrl Pts',(0.0138596512578787,-0.0324744968375319,
0.075912566314856));
#94612=CARTESIAN_POINT('Ctrl Pts',(0.0138342826843338,-0.0323646534831894,
0.0759912452687929));
#94613=CARTESIAN_POINT('Ctrl Pts',(0.0138438264437963,-0.0326943950436594,
0.0756585883300793));
#94614=CARTESIAN_POINT('Ctrl Pts',(0.013823035269212,-0.0325844576448127,
0.075737421260359));
#94615=CARTESIAN_POINT('Ctrl Pts',(0.0138006122289575,-0.0324744968375319,
0.0758158297741897));
#94616=CARTESIAN_POINT('Ctrl Pts',(0.0137765874384064,-0.0323646534831894,
0.0758937138062798));
#94617=CARTESIAN_POINT('Ctrl Pts',(0.0137821494351051,-0.0326943950436594,
0.0755635248029962));
#94618=CARTESIAN_POINT('Ctrl Pts',(0.013762668414092,-0.0325844576448127,
0.0756415077085012));
#94619=CARTESIAN_POINT('Ctrl Pts',(0.0137415732000363,-0.0324744968375319,
0.0757190932335233));
#94620=CARTESIAN_POINT('Ctrl Pts',(0.013718892192479,-0.0323646534831894,
0.0757961823437667));
#94621=CARTESIAN_POINT('Ctrl Pts',(0.0137204724264138,-0.0326943950436594,
0.0754684612759132));
#94622=CARTESIAN_POINT('Ctrl Pts',(0.013702301558972,-0.0325844576448127,
0.0755455941566433));
#94623=CARTESIAN_POINT('Ctrl Pts',(0.0136825341711151,-0.0324744968375319,
0.075622356692857));
#94624=CARTESIAN_POINT('Ctrl Pts',(0.0136611969465517,-0.0323646534831894,
0.0756986508812536));
#94625=CARTESIAN_POINT('Origin',(-0.00262289765796629,-0.0326395579068381,
0.0715374487169558));
#94626=CARTESIAN_POINT('Ctrl Pts',(0.0137297620235459,-0.0327445246961876,
0.0754349572524908));
#94627=CARTESIAN_POINT('Ctrl Pts',(0.0136812990690111,-0.0324436878365475,
0.0756463902360544));
#94628=CARTESIAN_POINT('Ctrl Pts',(0.013617047796315,-0.0321434074463186,
0.0758535721330864));
#94629=CARTESIAN_POINT('Ctrl Pts',(0.0137803071853637,-0.0327445246961876,
0.0751901201911279));
#94630=CARTESIAN_POINT('Ctrl Pts',(0.0137410784114604,-0.0324436878365475,
0.075403459516614));
#94631=CARTESIAN_POINT('Ctrl Pts',(0.013685891492601,-0.0321434074463186,
0.0756132378960711));
#94632=CARTESIAN_POINT('Ctrl Pts',(0.0136364247615194,-0.0322357242816072,
0.0757897856301795));
#94633=CARTESIAN_POINT('Ctrl Pts',(0.0135841997159223,-0.0319819883628705,
0.0759653561463479));
#94634=CARTESIAN_POINT('Ctrl Pts',(0.0135209084566539,-0.0317295851069886,
0.0761372476180256));
#94635=CARTESIAN_POINT('Ctrl Pts',(0.013702478135558,-0.0322357242816072,
0.0755486695755957));
#94636=CARTESIAN_POINT('Ctrl Pts',(0.0136579323235833,-0.0319819883628705,
0.075726343806059));
#94637=CARTESIAN_POINT('Ctrl Pts',(0.0136021708696587,-0.0317295851069886,
0.0759008233801974));
#94638=CARTESIAN_POINT('Origin',(-0.00253071053354238,-0.0326371942645646,
0.0715616135173585));
#94639=CARTESIAN_POINT('Origin',(-0.00258860630304265,-0.0326352985525967,
0.0720372662249546));
#94640=CARTESIAN_POINT('Ctrl Pts',(0.0137934004130372,-0.0321934096636183,
0.0761135246981948));
#94641=CARTESIAN_POINT('Ctrl Pts',(0.013766321877171,-0.0320835708272303,
0.0761917131520792));
#94642=CARTESIAN_POINT('Ctrl Pts',(0.0137376409419669,-0.0319739230346346,
0.0762692958645905));
#94643=CARTESIAN_POINT('Ctrl Pts',(0.0137074019207495,-0.0318646057455575,
0.0763461763902898));
#94644=CARTESIAN_POINT('Ctrl Pts',(0.0137378141176087,-0.0321934096636183,
0.076014775882878));
#94645=CARTESIAN_POINT('Ctrl Pts',(0.0137120974048659,-0.0320835708272303,
0.0760921977584271));
#94646=CARTESIAN_POINT('Ctrl Pts',(0.0136847933671711,-0.0319739230346346,
0.0761690425201084));
#94647=CARTESIAN_POINT('Ctrl Pts',(0.013655944483743,-0.0318646057455575,
0.0762452145314387));
#94648=CARTESIAN_POINT('Ctrl Pts',(0.0136822278221801,-0.0321934096636183,
0.0759160270675611));
#94649=CARTESIAN_POINT('Ctrl Pts',(0.0136578729325607,-0.0320835708272304,
0.075992682364775));
#94650=CARTESIAN_POINT('Ctrl Pts',(0.0136319457923753,-0.0319739230346346,
0.0760687891756264));
#94651=CARTESIAN_POINT('Ctrl Pts',(0.0136044870467364,-0.0318646057455575,
0.0761442526725876));
#94652=CARTESIAN_POINT('Ctrl Pts',(0.0136266415267516,-0.0321934096636183,
0.0758172782522443));
#94653=CARTESIAN_POINT('Ctrl Pts',(0.0136036484602555,-0.0320835708272304,
0.0758931669711228));
#94654=CARTESIAN_POINT('Ctrl Pts',(0.0135790982175796,-0.0319739230346346,
0.0759685358311443));
#94655=CARTESIAN_POINT('Ctrl Pts',(0.0135530296097299,-0.0318646057455575,
0.0760432908137365));
#94656=CARTESIAN_POINT('Ctrl Pts',(0.0136621203155706,-0.0320218834582286,
0.0756984213385563));
#94657=CARTESIAN_POINT('Ctrl Pts',(0.013646004992721,-0.0319391099350591,
0.0757560620495639));
#94658=CARTESIAN_POINT('Ctrl Pts',(0.0136289993659515,-0.0318564869454882,
0.0758134161945033));
#94659=CARTESIAN_POINT('Ctrl Pts',(0.0136111197215809,-0.0317740741446483,
0.0758704431548386));
#94660=CARTESIAN_POINT('Ctrl Pts',(0.0137058275897845,-0.0320218834582286,
0.0756750439514381));
#94661=CARTESIAN_POINT('Ctrl Pts',(0.0136899555690203,-0.0319391099350591,
0.0757331395495086));
#94662=CARTESIAN_POINT('Ctrl Pts',(0.0136731859938004,-0.0318564869454882,
0.0757909521051026));
#94663=CARTESIAN_POINT('Ctrl Pts',(0.0136555350096825,-0.0317740741446483,
0.0758484406497417));
#94664=CARTESIAN_POINT('Ctrl Pts',(0.0137495348639984,-0.0320218834582286,
0.0756516665643199));
#94665=CARTESIAN_POINT('Ctrl Pts',(0.0137339061453196,-0.0319391099350591,
0.0757102170494534));
#94666=CARTESIAN_POINT('Ctrl Pts',(0.0137173726216494,-0.0318564869454882,
0.0757684880157019));
#94667=CARTESIAN_POINT('Ctrl Pts',(0.0136999502977841,-0.0317740741446483,
0.0758264381446449));
#94668=CARTESIAN_POINT('Ctrl Pts',(0.0137932421382123,-0.0320218834582286,
0.0756282891772017));
#94669=CARTESIAN_POINT('Ctrl Pts',(0.013777856721619,-0.0319391099350591,
0.0756872945493981));
#94670=CARTESIAN_POINT('Ctrl Pts',(0.0137615592494983,-0.0318564869454882,
0.0757460239263013));
#94671=CARTESIAN_POINT('Ctrl Pts',(0.0137443655858856,-0.0317740741446483,
0.075804435639548));
#94672=CARTESIAN_POINT('Origin',(0.0199740041877478,-0.0391228853390816,
0.0764851353297408));
#94673=CARTESIAN_POINT('Ctrl Pts',(0.0136801432296278,-0.0352722978779561,
0.0726630512535914));
#94674=CARTESIAN_POINT('Ctrl Pts',(0.0136846892937845,-0.0352466642097194,
0.0726813931722122));
#94675=CARTESIAN_POINT('Ctrl Pts',(0.0136893074063788,-0.035221018380829,
0.0726996998892095));
#94676=CARTESIAN_POINT('Ctrl Pts',(0.0136939982467239,-0.0351953608940152,
0.0727179719203529));
#94677=CARTESIAN_POINT('Origin',(0.0184765399799541,-0.035245600306501,
0.0716608928793427));
#94678=CARTESIAN_POINT('Ctrl Pts',(0.0137223170444343,-0.0350241211493338,
0.0728393941634325));
#94679=CARTESIAN_POINT('Ctrl Pts',(0.0137403701016496,-0.034914423286742,
0.0729165116820436));
#94680=CARTESIAN_POINT('Ctrl Pts',(0.0137568398903465,-0.0348045283677512,
0.0729940485287804));
#94681=CARTESIAN_POINT('Ctrl Pts',(0.0137717016190843,-0.0346945769586886,
0.0730719061738239));
#94682=CARTESIAN_POINT('Ctrl Pts',(0.0137841274317792,-0.0350241211493338,
0.0727444172303425));
#94683=CARTESIAN_POINT('Ctrl Pts',(0.0138034887572468,-0.034914423286742,
0.0728223861616576));
#94684=CARTESIAN_POINT('Ctrl Pts',(0.0138212499979493,-0.0348045283677512,
0.0729008019735484));
#94685=CARTESIAN_POINT('Ctrl Pts',(0.0138373846663652,-0.0346945769586886,
0.0729795650719092));
#94686=CARTESIAN_POINT('Ctrl Pts',(0.0138459378191241,-0.0350241211493338,
0.0726494402972525));
#94687=CARTESIAN_POINT('Ctrl Pts',(0.013866607412844,-0.034914423286742,
0.0727282606412716));
#94688=CARTESIAN_POINT('Ctrl Pts',(0.0138856601055521,-0.0348045283677512,
0.0728075554183163));
#94689=CARTESIAN_POINT('Ctrl Pts',(0.0139030677136461,-0.0346945769586886,
0.0728872239699945));
#94690=CARTESIAN_POINT('Ctrl Pts',(0.013907748206469,-0.0350241211493338,
0.0725544633641624));
#94691=CARTESIAN_POINT('Ctrl Pts',(0.0139297260684412,-0.034914423286742,
0.0726341351208856));
#94692=CARTESIAN_POINT('Ctrl Pts',(0.013950070213155,-0.0348045283677512,
0.0727143088630843));
#94693=CARTESIAN_POINT('Ctrl Pts',(0.013968750760927,-0.0346945769586886,
0.0727948828680799));
#94694=CARTESIAN_POINT('Origin',(-0.00275213922892978,-0.0345629067943203,
0.0760427028193072));
#94695=CARTESIAN_POINT('Ctrl Pts',(0.0139589949194522,-0.0351970973651636,
0.0730889560727202));
#94696=CARTESIAN_POINT('Ctrl Pts',(0.0139736942450957,-0.0350869349321789,
0.0731697950369309));
#94697=CARTESIAN_POINT('Ctrl Pts',(0.0139867251502219,-0.0349764985129735,
0.0732510065580329));
#94698=CARTESIAN_POINT('Ctrl Pts',(0.0139980645595221,-0.0348659306849651,
0.0733324864178842));
#94699=CARTESIAN_POINT('Ctrl Pts',(0.0138891228821058,-0.0351970973651636,
0.0730456159175887));
#94700=CARTESIAN_POINT('Ctrl Pts',(0.0139044226268623,-0.0350869349321789,
0.0731254868994152));
#94701=CARTESIAN_POINT('Ctrl Pts',(0.0139180745722991,-0.0349764985129735,
0.0732057421186485));
#94702=CARTESIAN_POINT('Ctrl Pts',(0.0139300549114613,-0.0348659306849651,
0.0732862786434255));
#94703=CARTESIAN_POINT('Ctrl Pts',(0.0138192508447593,-0.0351970973651636,
0.073002275762457));
#94704=CARTESIAN_POINT('Ctrl Pts',(0.0138351510086288,-0.0350869349321789,
0.0730811787618996));
#94705=CARTESIAN_POINT('Ctrl Pts',(0.0138494239943763,-0.0349764985129735,
0.073160477679264));
#94706=CARTESIAN_POINT('Ctrl Pts',(0.0138620452634006,-0.0348659306849651,
0.0732400708689667));
#94707=CARTESIAN_POINT('Ctrl Pts',(0.0137493788074128,-0.0351970973651636,
0.0729589356073255));
#94708=CARTESIAN_POINT('Ctrl Pts',(0.0137658793903954,-0.0350869349321789,
0.0730368706243839));
#94709=CARTESIAN_POINT('Ctrl Pts',(0.0137807734164534,-0.0349764985129735,
0.0731152132398796));
#94710=CARTESIAN_POINT('Ctrl Pts',(0.0137940356153398,-0.0348659306849651,
0.073193863094508));
#94711=CARTESIAN_POINT('Origin',(-0.00278943576368031,-0.0345637187963003,
0.075563188142377));
#94712=CARTESIAN_POINT('Ctrl Pts',(0.0137433422209968,-0.0352450361861253,
0.0729257981812789));
#94713=CARTESIAN_POINT('Ctrl Pts',(0.0137895137490415,-0.0349452761023765,
0.0731377433601362));
#94714=CARTESIAN_POINT('Ctrl Pts',(0.0138195895309711,-0.0346444289983475,
0.0733525642534035));
#94715=CARTESIAN_POINT('Ctrl Pts',(0.0136848322127879,-0.0352450361861253,
0.0726827414411143));
#94716=CARTESIAN_POINT('Ctrl Pts',(0.0137401707759761,-0.0349452761023765,
0.0728924798788579));
#94717=CARTESIAN_POINT('Ctrl Pts',(0.0137795537712344,-0.0346444289983475,
0.073105790798708));
#94718=CARTESIAN_POINT('Ctrl Pts',(0.0137935631277463,-0.0345231616327822,
0.0731935142885265));
#94719=CARTESIAN_POINT('Ctrl Pts',(0.0138067469366547,-0.0344132092796975,
0.0732716642362969));
#94720=CARTESIAN_POINT('Ctrl Pts',(0.0138183135953134,-0.0343032738558974,
0.0733500828485773));
#94721=CARTESIAN_POINT('Ctrl Pts',(0.013828250858901,-0.0341934961088741,
0.0734286692824882));
#94722=CARTESIAN_POINT('Ctrl Pts',(0.0138612151679042,-0.0345231616327822,
0.07310260588627));
#94723=CARTESIAN_POINT('Ctrl Pts',(0.0138756520211489,-0.0344132092796975,
0.0731816883221675));
#94724=CARTESIAN_POINT('Ctrl Pts',(0.0138884523717112,-0.0343032738558974,
0.0732610652926967));
#94725=CARTESIAN_POINT('Ctrl Pts',(0.0138996024257176,-0.0341934961088741,
0.073340634686725));
#94726=CARTESIAN_POINT('Ctrl Pts',(0.0139288672080621,-0.0345231616327822,
0.0730116974840134));
#94727=CARTESIAN_POINT('Ctrl Pts',(0.0139445571056432,-0.0344132092796975,
0.0730917124080381));
#94728=CARTESIAN_POINT('Ctrl Pts',(0.013958591148109,-0.0343032738558974,
0.0731720477368159));
#94729=CARTESIAN_POINT('Ctrl Pts',(0.0139709539925342,-0.0341934961088741,
0.0732526000909618));
#94730=CARTESIAN_POINT('Ctrl Pts',(0.0139965192482201,-0.0345231616327822,
0.0729207890817569));
#94731=CARTESIAN_POINT('Ctrl Pts',(0.0140134621901374,-0.0344132092796975,
0.0730017364939087));
#94732=CARTESIAN_POINT('Ctrl Pts',(0.0140287299245069,-0.0343032738558974,
0.0730830301809353));
#94733=CARTESIAN_POINT('Ctrl Pts',(0.0140423055593507,-0.0341934961088741,
0.0731645654951986));
#94734=CARTESIAN_POINT('Origin',(-0.00276401815133821,-0.0345625596232808,
0.0760450243483039));
#94735=CARTESIAN_POINT('Ctrl Pts',(0.0140898342906213,-0.0346945769586885,
0.0735126442359855));
#94736=CARTESIAN_POINT('Ctrl Pts',(0.0140986173751996,-0.0345846629176052,
0.0735948594494186));
#94737=CARTESIAN_POINT('Ctrl Pts',(0.0141057017831005,-0.0344746925050311,
0.0736772703359942));
#94738=CARTESIAN_POINT('Ctrl Pts',(0.0141110788730535,-0.0343648066253259,
0.0737597712638998));
#94739=CARTESIAN_POINT('Ctrl Pts',(0.0139974932614085,-0.0346945769586885,
0.0734469612404181));
#94740=CARTESIAN_POINT('Ctrl Pts',(0.0140071814908651,-0.0345846629176052,
0.073527903947795));
#94741=CARTESIAN_POINT('Ctrl Pts',(0.0140151975131478,-0.0344746925050311,
0.0736090608289917));
#94742=CARTESIAN_POINT('Ctrl Pts',(0.0140215314866589,-0.0343648066253259,
0.073690327854042));
#94743=CARTESIAN_POINT('Ctrl Pts',(0.0139051522321957,-0.0346945769586885,
0.0733812782448507));
#94744=CARTESIAN_POINT('Ctrl Pts',(0.0139157456065305,-0.0345846629176052,
0.0734609484461715));
#94745=CARTESIAN_POINT('Ctrl Pts',(0.0139246932431951,-0.0344746925050311,
0.0735408513219892));
#94746=CARTESIAN_POINT('Ctrl Pts',(0.0139319841002643,-0.0343648066253259,
0.0736208844441842));
#94747=CARTESIAN_POINT('Ctrl Pts',(0.0138128112029828,-0.0346945769586885,
0.0733155952492833));
#94748=CARTESIAN_POINT('Ctrl Pts',(0.013824309722196,-0.0345846629176052,
0.0733939929445479));
#94749=CARTESIAN_POINT('Ctrl Pts',(0.0138341889732425,-0.0344746925050311,
0.0734726418149867));
#94750=CARTESIAN_POINT('Ctrl Pts',(0.0138424367138697,-0.0343648066253259,
0.0735514410343263));
#94751=CARTESIAN_POINT('Origin',(-0.00284727738114501,-0.0345626446731677,
0.0755714632818768));
#94752=CARTESIAN_POINT('Ctrl Pts',(0.0138144634936381,-0.0346945769586885,
0.0733167705383256));
#94753=CARTESIAN_POINT('Ctrl Pts',(0.0138319158183195,-0.0345275153362891,
0.0734359641365878));
#94754=CARTESIAN_POINT('Ctrl Pts',(0.0138456241281108,-0.0343603235965159,
0.0735557374239671));
#94755=CARTESIAN_POINT('Ctrl Pts',(0.0138555531447897,-0.034193496108874,
0.073675735561671));
#94756=CARTESIAN_POINT('Ctrl Pts',(0.0138005181767745,-0.0346945769586885,
0.0732341052102319));
#94757=CARTESIAN_POINT('Ctrl Pts',(0.0138197019598501,-0.0345275153362891,
0.0733530067182489));
#94758=CARTESIAN_POINT('Ctrl Pts',(0.0138351513618489,-0.0343603235965159,
0.0734725422926064));
#94759=CARTESIAN_POINT('Ctrl Pts',(0.0138468259447214,-0.034193496108874,
0.0735923577210283));
#94760=CARTESIAN_POINT('Ctrl Pts',(0.0137865728599108,-0.0346945769586885,
0.0731514398821381));
#94761=CARTESIAN_POINT('Ctrl Pts',(0.0138074881013808,-0.0345275153362891,
0.0732700492999101));
#94762=CARTESIAN_POINT('Ctrl Pts',(0.013824678595587,-0.0343603235965159,
0.0733893471612458));
#94763=CARTESIAN_POINT('Ctrl Pts',(0.0138380987446531,-0.034193496108874,
0.0735089798803856));
#94764=CARTESIAN_POINT('Ctrl Pts',(0.0137726275430471,-0.0346945769586885,
0.0730687745540444));
#94765=CARTESIAN_POINT('Ctrl Pts',(0.0137952742429114,-0.0345275153362891,
0.0731870918815713));
#94766=CARTESIAN_POINT('Ctrl Pts',(0.0138142058293251,-0.0343603235965159,
0.0733061520298852));
#94767=CARTESIAN_POINT('Ctrl Pts',(0.0138293715445849,-0.034193496108874,
0.0734256020397429));
#94768=CARTESIAN_POINT('Ctrl Pts',(0.0138424328752354,-0.0340223579322365,
0.0735514097094114));
#94769=CARTESIAN_POINT('Ctrl Pts',(0.0138506889965316,-0.0339125849573554,
0.0736302848171843));
#94770=CARTESIAN_POINT('Ctrl Pts',(0.0138573067848964,-0.0338030433565221,
0.0737092753828584));
#94771=CARTESIAN_POINT('Ctrl Pts',(0.0138622867319039,-0.0336938721132328,
0.0737882796406025));
#94772=CARTESIAN_POINT('Ctrl Pts',(0.0139156597160613,-0.0340223579322365,
0.073464928442001));
#94773=CARTESIAN_POINT('Ctrl Pts',(0.0139251086395876,-0.0339125849573554,
0.0735448135388925));
#94774=CARTESIAN_POINT('Ctrl Pts',(0.0139328974875865,-0.0338030433565221,
0.0736248380722121));
#94775=CARTESIAN_POINT('Ctrl Pts',(0.0139390253712576,-0.0336938721132328,
0.0737048988211032));
#94776=CARTESIAN_POINT('Ctrl Pts',(0.0139888865568871,-0.0340223579322365,
0.0733784471745906));
#94777=CARTESIAN_POINT('Ctrl Pts',(0.0139995282826436,-0.0339125849573554,
0.0734593422606007));
#94778=CARTESIAN_POINT('Ctrl Pts',(0.0140084881902765,-0.0338030433565221,
0.0735404007615657));
#94779=CARTESIAN_POINT('Ctrl Pts',(0.0140157640106112,-0.0336938721132328,
0.0736215180016039));
#94780=CARTESIAN_POINT('Ctrl Pts',(0.0140621133977129,-0.0340223579322365,
0.0732919659071803));
#94781=CARTESIAN_POINT('Ctrl Pts',(0.0140739479256997,-0.0339125849573554,
0.073373870982309));
#94782=CARTESIAN_POINT('Ctrl Pts',(0.0140840788929665,-0.0338030433565221,
0.0734559634509193));
#94783=CARTESIAN_POINT('Ctrl Pts',(0.0140925026499649,-0.0336938721132328,
0.0735381371821046));
#94784=CARTESIAN_POINT('Origin',(-0.00264516157481752,-0.0345589643414915,
0.076026969089253));
#94785=CARTESIAN_POINT('Ctrl Pts',(0.0141180815491695,-0.034193496108874,
0.0738885134227377));
#94786=CARTESIAN_POINT('Ctrl Pts',(0.0141216872942238,-0.0340836138581107,
0.0739711712611747));
#94787=CARTESIAN_POINT('Ctrl Pts',(0.014123580878647,-0.03397388966435,
0.0740538640521549));
#94788=CARTESIAN_POINT('Ctrl Pts',(0.0141237669736284,-0.0338644633294062,
0.0741364857966549));
#94789=CARTESIAN_POINT('Ctrl Pts',(0.0140300468741901,-0.034193496108874,
0.0738171617917167));
#94790=CARTESIAN_POINT('Ctrl Pts',(0.0140346365159833,-0.0340836138581107,
0.0738986056841178));
#94791=CARTESIAN_POINT('Ctrl Pts',(0.0140375386451194,-0.03397388966435,
0.0739801054712147));
#94792=CARTESIAN_POINT('Ctrl Pts',(0.0140387565396194,-0.0338644633294062,
0.0740615565943523));
#94793=CARTESIAN_POINT('Ctrl Pts',(0.0139420121992106,-0.034193496108874,
0.0737458101606958));
#94794=CARTESIAN_POINT('Ctrl Pts',(0.0139475857377429,-0.0340836138581107,
0.0738260401070609));
#94795=CARTESIAN_POINT('Ctrl Pts',(0.0139514964115919,-0.03397388966435,
0.0739063468902746));
#94796=CARTESIAN_POINT('Ctrl Pts',(0.0139537461056104,-0.0338644633294062,
0.0739866273920497));
#94797=CARTESIAN_POINT('Ctrl Pts',(0.0138539775242311,-0.034193496108874,
0.0736744585296748));
#94798=CARTESIAN_POINT('Ctrl Pts',(0.0138605349595024,-0.0340836138581107,
0.0737534745300041));
#94799=CARTESIAN_POINT('Ctrl Pts',(0.0138654541780643,-0.03397388966435,
0.0738325883093345));
#94800=CARTESIAN_POINT('Ctrl Pts',(0.0138687356716015,-0.0338644633294062,
0.0739116981897471));
#94801=CARTESIAN_POINT('Origin',(-0.00277248688440006,-0.0345610621863777,
0.075562923534416));
#94802=CARTESIAN_POINT('Ctrl Pts',(0.0138524565193727,-0.03424362768739,
0.0736396908156799));
#94803=CARTESIAN_POINT('Ctrl Pts',(0.0138717031475436,-0.033943005420186,
0.0738557513296935));
#94804=CARTESIAN_POINT('Ctrl Pts',(0.0138746205348661,-0.0336441434784161,
0.0740726477733318));
#94805=CARTESIAN_POINT('Ctrl Pts',(0.0138248675757685,-0.03424362768739,
0.0733912177785293));
#94806=CARTESIAN_POINT('Ctrl Pts',(0.0138534855190235,-0.033943005420186,
0.0736062377583814));
#94807=CARTESIAN_POINT('Ctrl Pts',(0.0138658259758028,-0.0336441434784161,
0.0738228025097566));
#94808=CARTESIAN_POINT('Ctrl Pts',(0.0138687343957871,-0.0335235895815127,
0.073911670487762));
#94809=CARTESIAN_POINT('Ctrl Pts',(0.0138720154707506,-0.0334144449262718,
0.0739907610656007));
#94810=CARTESIAN_POINT('Ctrl Pts',(0.013873666363456,-0.0333049234473132,
0.0740700102934708));
#94811=CARTESIAN_POINT('Ctrl Pts',(0.0138736757835164,-0.0331951640388588,
0.0741493170271627));
#94812=CARTESIAN_POINT('Ctrl Pts',(0.0139472469587047,-0.0335235895815127,
0.0738299578819154));
#94813=CARTESIAN_POINT('Ctrl Pts',(0.013951652968565,-0.0334144449262718,
0.0739101293397597));
#94814=CARTESIAN_POINT('Ctrl Pts',(0.0139544077584135,-0.0333049234473132,
0.0739904839297438));
#94815=CARTESIAN_POINT('Ctrl Pts',(0.0139554984982845,-0.0331951640388588,
0.0740709192221035));
#94816=CARTESIAN_POINT('Ctrl Pts',(0.0140257595216223,-0.0335235895815127,
0.0737482452760687));
#94817=CARTESIAN_POINT('Ctrl Pts',(0.0140312904663793,-0.0334144449262718,
0.0738294976139186));
#94818=CARTESIAN_POINT('Ctrl Pts',(0.0140351491533711,-0.0333049234473132,
0.0739109575660169));
#94819=CARTESIAN_POINT('Ctrl Pts',(0.0140373212130526,-0.0331951640388588,
0.0739925214170443));
#94820=CARTESIAN_POINT('Ctrl Pts',(0.0141042720845398,-0.0335235895815127,
0.0736665326702221));
#94821=CARTESIAN_POINT('Ctrl Pts',(0.0141109279641937,-0.0334144449262718,
0.0737488658880775));
#94822=CARTESIAN_POINT('Ctrl Pts',(0.0141158905483287,-0.0333049234473132,
0.0738314312022899));
#94823=CARTESIAN_POINT('Ctrl Pts',(0.0141191439278208,-0.0331951640388588,
0.0739141236119851));
#94824=CARTESIAN_POINT('Origin',(-0.00277608421101272,-0.0326434571770578,
0.0733901509087705));
#94825=CARTESIAN_POINT('Ctrl Pts',(0.0141241639462871,-0.0336938721132403,
0.0742667876312677));
#94826=CARTESIAN_POINT('Ctrl Pts',(0.014123480349527,-0.0336474569764965,
0.0743019098568073));
#94827=CARTESIAN_POINT('Ctrl Pts',(0.0141223856496123,-0.033601104548885,
0.0743370216733863));
#94828=CARTESIAN_POINT('Ctrl Pts',(0.0141196141212349,-0.0334837508643177,
0.0744259167164236));
#94829=CARTESIAN_POINT('Ctrl Pts',(0.0141142096655867,-0.0333660264760438,
0.0745146905971841));
#94830=CARTESIAN_POINT('Ctrl Pts',(0.0138740221145919,-0.0336938721132403,
0.0740365722900783));
#94831=CARTESIAN_POINT('Ctrl Pts',(0.0138746860446174,-0.0336474569764965,
0.0740702303524711));
#94832=CARTESIAN_POINT('Ctrl Pts',(0.0138749559190331,-0.033601104548885,
0.0741038938807312));
#94833=CARTESIAN_POINT('Ctrl Pts',(0.0138756391789763,-0.0334837508643177,
0.074189122190885));
#94834=CARTESIAN_POINT('Ctrl Pts',(0.0138737966474534,-0.0333660264760438,
0.0742743333214573));
#94835=CARTESIAN_POINT('Ctrl Pts',(0.0138740221146021,-0.0336938721132427,
0.0740365722900937));
#94836=CARTESIAN_POINT('Ctrl Pts',(0.0138746860446274,-0.0336474569765026,
0.0740702303524838));
#94837=CARTESIAN_POINT('Ctrl Pts',(0.0138749559190431,-0.0336011045488949,
0.0741038938807412));
#94838=CARTESIAN_POINT('Ctrl Pts',(0.0138756334883616,-0.0334847282606778,
0.0741884123551572));
#94839=CARTESIAN_POINT('Ctrl Pts',(0.0138738271572256,-0.0333679869945434,
0.0742729142414415));
#94840=CARTESIAN_POINT('Ctrl Pts',(0.0138740221145919,-0.0336938721132428,
0.0740365722900764));
#94841=CARTESIAN_POINT('Ctrl Pts',(0.0138763966221813,-0.0335278710435084,
0.0741569484163655));
#94842=CARTESIAN_POINT('Ctrl Pts',(0.0138749953304014,-0.033362046922432,
0.0742773566585535));
#94843=CARTESIAN_POINT('Ctrl Pts',(0.0138697975144591,-0.0331951640388601,
0.0743978566658464));
#94844=CARTESIAN_POINT('Ctrl Pts',(0.0138705474732217,-0.0336938721132428,
0.073952810982239));
#94845=CARTESIAN_POINT('Ctrl Pts',(0.0138746754488243,-0.0335278710435084,
0.0740731143700208));
#94846=CARTESIAN_POINT('Ctrl Pts',(0.0138750292892522,-0.033362046922432,
0.0741935048875918));
#94847=CARTESIAN_POINT('Ctrl Pts',(0.0138715891455355,-0.0331951640388601,
0.0743140424672798));
#94848=CARTESIAN_POINT('Ctrl Pts',(0.0138670728318515,-0.0336938721132428,
0.0738690496744017));
#94849=CARTESIAN_POINT('Ctrl Pts',(0.0138729542754672,-0.0335278710435084,
0.0739892803236762));
#94850=CARTESIAN_POINT('Ctrl Pts',(0.013875063248103,-0.033362046922432,
0.0741096531166301));
#94851=CARTESIAN_POINT('Ctrl Pts',(0.013873380776612,-0.0331951640388601,
0.0742302282687132));
#94852=CARTESIAN_POINT('Ctrl Pts',(0.0138635981904812,-0.0336938721132428,
0.0737852883665644));
#94853=CARTESIAN_POINT('Ctrl Pts',(0.0138712331021102,-0.0335278710435084,
0.0739054462773315));
#94854=CARTESIAN_POINT('Ctrl Pts',(0.0138750972069538,-0.033362046922432,
0.0740258013456685));
#94855=CARTESIAN_POINT('Ctrl Pts',(0.0138751724076885,-0.0331951640388601,
0.0741464140701466));
#94856=CARTESIAN_POINT('Ctrl Pts',(0.0138723632544785,-0.0330240426238155,
0.0742728680625924));
#94857=CARTESIAN_POINT('Ctrl Pts',(0.0138706706272117,-0.0329142774063509,
0.0743520603672835));
#94858=CARTESIAN_POINT('Ctrl Pts',(0.0138673400299578,-0.0328043479726686,
0.074431257160893));
#94859=CARTESIAN_POINT('Ctrl Pts',(0.0138623729353523,-0.0326943950436594,
0.0745103568689245));
#94860=CARTESIAN_POINT('Ctrl Pts',(0.0139558515368148,-0.0330240426238155,
0.0741962466380622));
#94861=CARTESIAN_POINT('Ctrl Pts',(0.0139552144443196,-0.0329142774063509,
0.0742765890751812));
#94862=CARTESIAN_POINT('Ctrl Pts',(0.0139529161316098,-0.0328043479726686,
0.0743569583954537));
#94863=CARTESIAN_POINT('Ctrl Pts',(0.0139489567075201,-0.0326943950436594,
0.074437251558709));
#94864=CARTESIAN_POINT('Ctrl Pts',(0.0140393398191512,-0.0330240426238155,
0.0741196252135321));
#94865=CARTESIAN_POINT('Ctrl Pts',(0.0140397582614275,-0.0329142774063509,
0.0742011177830789));
#94866=CARTESIAN_POINT('Ctrl Pts',(0.0140384922332618,-0.0328043479726686,
0.0742826596300145));
#94867=CARTESIAN_POINT('Ctrl Pts',(0.014035540479688,-0.0326943950436594,
0.0743641462484936));
#94868=CARTESIAN_POINT('Ctrl Pts',(0.0141228281014876,-0.0330240426238155,
0.0740430037890019));
#94869=CARTESIAN_POINT('Ctrl Pts',(0.0141243020785354,-0.0329142774063509,
0.0741256464909766));
#94870=CARTESIAN_POINT('Ctrl Pts',(0.0141240683349138,-0.0328043479726686,
0.0742083608645752));
#94871=CARTESIAN_POINT('Ctrl Pts',(0.0141221242518558,-0.0326943950436594,
0.0742910409382782));
#94872=CARTESIAN_POINT('Origin',(-0.00289962073335013,-0.0326396682857968,
0.0733843091246045));
#94873=CARTESIAN_POINT('Ctrl Pts',(0.0141035876665988,-0.0331951640388587,
0.0746418602437495));
#94874=CARTESIAN_POINT('Ctrl Pts',(0.0140968132867663,-0.0330855618255041,
0.0747242199670989));
#94875=CARTESIAN_POINT('Ctrl Pts',(0.0140883317886784,-0.0329757224427708,
0.0748064990475701));
#94876=CARTESIAN_POINT('Ctrl Pts',(0.0140781488651125,-0.0328657862078596,
0.074888591589103));
#94877=CARTESIAN_POINT('Ctrl Pts',(0.0140251899239631,-0.0331951640388587,
0.074560037594132));
#94878=CARTESIAN_POINT('Ctrl Pts',(0.0140195424856032,-0.0330855618255041,
0.0746413175471739));
#94879=CARTESIAN_POINT('Ctrl Pts',(0.0140122110583908,-0.0329757224427708,
0.0747225393709002));
#94880=CARTESIAN_POINT('Ctrl Pts',(0.0140031999287792,-0.0328657862078596,
0.0748035985953723));
#94881=CARTESIAN_POINT('Ctrl Pts',(0.0139467921813274,-0.0331951640388588,
0.0744782149445145));
#94882=CARTESIAN_POINT('Ctrl Pts',(0.0139422716844402,-0.0330855618255041,
0.0745584151272489));
#94883=CARTESIAN_POINT('Ctrl Pts',(0.0139360903281033,-0.0329757224427708,
0.0746385796942304));
#94884=CARTESIAN_POINT('Ctrl Pts',(0.013928250992446,-0.0328657862078596,
0.0747186056016415));
#94885=CARTESIAN_POINT('Ctrl Pts',(0.0138683944386917,-0.0331951640388588,
0.0743963922948969));
#94886=CARTESIAN_POINT('Ctrl Pts',(0.0138650008832771,-0.0330855618255041,
0.0744755127073239));
#94887=CARTESIAN_POINT('Ctrl Pts',(0.0138599695978157,-0.0329757224427708,
0.0745546200175605));
#94888=CARTESIAN_POINT('Ctrl Pts',(0.0138533020561127,-0.0328657862078596,
0.0746336126079108));
#94889=CARTESIAN_POINT('Origin',(-0.00282794701289518,-0.0326401908833756,
0.0729087717974273));
#94890=CARTESIAN_POINT('Ctrl Pts',(0.0138712402433729,-0.033245108999443,
0.074361780453421));
#94891=CARTESIAN_POINT('Ctrl Pts',(0.0138632528128909,-0.0329451141710257,
0.0745785493803117));
#94892=CARTESIAN_POINT('Ctrl Pts',(0.0138389601521242,-0.0326442513127504,
0.074794100843642));
#94893=CARTESIAN_POINT('Ctrl Pts',(0.0138750139257603,-0.033245108999443,
0.074111808936401));
#94894=CARTESIAN_POINT('Ctrl Pts',(0.0138764543252901,-0.0329451141710257,
0.0743287201900515));
#94895=CARTESIAN_POINT('Ctrl Pts',(0.0138615519904318,-0.0326442513127504,
0.0745451237185043));
#94896=CARTESIAN_POINT('Ctrl Pts',(0.0138533048022358,-0.0325229783203385,
0.0746335811398438));
#94897=CARTESIAN_POINT('Ctrl Pts',(0.0138466386469197,-0.0324130253112079,
0.0747125624822765));
#94898=CARTESIAN_POINT('Ctrl Pts',(0.0138383396721593,-0.0323031222247695,
0.074791393947658));
#94899=CARTESIAN_POINT('Ctrl Pts',(0.0138284220715146,-0.0321934096636184,
0.0748699749336006));
#94900=CARTESIAN_POINT('Ctrl Pts',(0.0139414394500367,-0.0325229783203385,
0.0745623531502163));
#94901=CARTESIAN_POINT('Ctrl Pts',(0.013935755170982,-0.0324130253112079,
0.0746425494268195));
#94902=CARTESIAN_POINT('Ctrl Pts',(0.0139284127910888,-0.0323031222247695,
0.0747226159534742));
#94903=CARTESIAN_POINT('Ctrl Pts',(0.0139194253344114,-0.0321934096636184,
0.0748024505025294));
#94904=CARTESIAN_POINT('Ctrl Pts',(0.0140295740978375,-0.0325229783203385,
0.0744911251605887));
#94905=CARTESIAN_POINT('Ctrl Pts',(0.0140248716950443,-0.0324130253112079,
0.0745725363713624));
#94906=CARTESIAN_POINT('Ctrl Pts',(0.0140184859100183,-0.0323031222247695,
0.0746538379592904));
#94907=CARTESIAN_POINT('Ctrl Pts',(0.0140104285973083,-0.0321934096636184,
0.0747349260714583));
#94908=CARTESIAN_POINT('Ctrl Pts',(0.0141177087456384,-0.0325229783203385,
0.0744198971709612));
#94909=CARTESIAN_POINT('Ctrl Pts',(0.0141139882191066,-0.0324130253112079,
0.0745025233159053));
#94910=CARTESIAN_POINT('Ctrl Pts',(0.0141085590289478,-0.0323031222247695,
0.0745850599651066));
#94911=CARTESIAN_POINT('Ctrl Pts',(0.0141014318602051,-0.0321934096636184,
0.0746674016403871));
#94912=CARTESIAN_POINT('Origin',(-0.00289113517097316,-0.0326393375180434,
0.0733851375305188));
#94913=CARTESIAN_POINT('Ctrl Pts',(0.0140609037262105,-0.0326943950436593,
0.0750163647622754));
#94914=CARTESIAN_POINT('Ctrl Pts',(0.0140489635960458,-0.0325844576448127,
0.075098189424353));
#94915=CARTESIAN_POINT('Ctrl Pts',(0.0140353303526944,-0.0324744968375319,
0.0751797729358211));
#94916=CARTESIAN_POINT('Ctrl Pts',(0.0140200229056394,-0.0323646534831894,
0.0752610110080593));
#94917=CARTESIAN_POINT('Ctrl Pts',(0.0139877984399115,-0.0326943950436593,
0.0749297810184334));
#94918=CARTESIAN_POINT('Ctrl Pts',(0.0139770515960121,-0.0325844576448127,
0.0750105981526519));
#94919=CARTESIAN_POINT('Ctrl Pts',(0.0139646325607048,-0.0324744968375319,
0.075091198744073));
#94920=CARTESIAN_POINT('Ctrl Pts',(0.0139505586703879,-0.0323646534831894,
0.0751714797419927));
#94921=CARTESIAN_POINT('Ctrl Pts',(0.0139146931536124,-0.0326943950436593,
0.0748431972745913));
#94922=CARTESIAN_POINT('Ctrl Pts',(0.0139051395959784,-0.0325844576448127,
0.0749230068809507));
#94923=CARTESIAN_POINT('Ctrl Pts',(0.0138939347687152,-0.0324744968375319,
0.0750026245523248));
#94924=CARTESIAN_POINT('Ctrl Pts',(0.0138810944351364,-0.0323646534831895,
0.0750819484759261));
#94925=CARTESIAN_POINT('Ctrl Pts',(0.0138415878673133,-0.0326943950436593,
0.0747566135307493));
#94926=CARTESIAN_POINT('Ctrl Pts',(0.0138332275959447,-0.0325844576448127,
0.0748354156092496));
#94927=CARTESIAN_POINT('Ctrl Pts',(0.0138232369767255,-0.0324744968375319,
0.0749140503605767));
#94928=CARTESIAN_POINT('Ctrl Pts',(0.0138116301998849,-0.0323646534831895,
0.0749924172098595));
#94929=CARTESIAN_POINT('Origin',(-0.00286559637766498,-0.0326395579068401,
0.0729049655999673));
#94930=CARTESIAN_POINT('Ctrl Pts',(0.0138466050456045,-0.0327445246961879,
0.0747222094013116));
#94931=CARTESIAN_POINT('Ctrl Pts',(0.0138250238154535,-0.0324436878365476,
0.0749380491914477));
#94932=CARTESIAN_POINT('Ctrl Pts',(0.0137872459603246,-0.0321434074463186,
0.0751516502171071));
#94933=CARTESIAN_POINT('Ctrl Pts',(0.0138660654231273,-0.0327445246961879,
0.0744729679647352));
#94934=CARTESIAN_POINT('Ctrl Pts',(0.0138538844873328,-0.0324436878365476,
0.0746895417150006));
#94935=CARTESIAN_POINT('Ctrl Pts',(0.0138254249364414,-0.0321434074463186,
0.0749045826842691));
#94936=CARTESIAN_POINT('Ctrl Pts',(0.0137984755637037,-0.0322357242816073,
0.0750859381121221));
#94937=CARTESIAN_POINT('Ctrl Pts',(0.0137686671486999,-0.0319819883628705,
0.0752666697361679));
#94938=CARTESIAN_POINT('Ctrl Pts',(0.0137274186738825,-0.0317295851069886,
0.0754451382904304));
#94939=CARTESIAN_POINT('Ctrl Pts',(0.0138337882323735,-0.0322357242816073,
0.0748384446466904));
#94940=CARTESIAN_POINT('Ctrl Pts',(0.0138118621632564,-0.0319819883628705,
0.0750203009334345));
#94941=CARTESIAN_POINT('Ctrl Pts',(0.0137784084942689,-0.0317295851069886,
0.0752003934473449));
#94942=CARTESIAN_POINT('Origin',(-0.00277110752374236,-0.0326371942649529,
0.0729173857438345));
#94943=CARTESIAN_POINT('Origin',(-0.00276893167612555,-0.0326352985533183,
0.0733965440521899));
#94944=CARTESIAN_POINT('Ctrl Pts',(0.0139947886795484,-0.0321934096636184,
0.0753874501348944));
#94945=CARTESIAN_POINT('Ctrl Pts',(0.0139777232777782,-0.0320835708272304,
0.0754684158899265));
#94946=CARTESIAN_POINT('Ctrl Pts',(0.0139589921925425,-0.0319739230346346,
0.0755489815139276));
#94947=CARTESIAN_POINT('Ctrl Pts',(0.0139386272999234,-0.0318646057455575,
0.0756290457680276));
#94948=CARTESIAN_POINT('Ctrl Pts',(0.0139272641903278,-0.0321934096636184,
0.0752964467936291));
#94949=CARTESIAN_POINT('Ctrl Pts',(0.0139114537955573,-0.0320835708272304,
0.0753764813333295));
#94950=CARTESIAN_POINT('Ctrl Pts',(0.0138939962608192,-0.0319739230346346,
0.0754561422544462));
#94951=CARTESIAN_POINT('Ctrl Pts',(0.0138749217439407,-0.0318646057455575,
0.0755353293505604));
#94952=CARTESIAN_POINT('Ctrl Pts',(0.0138597397011072,-0.0321934096636184,
0.0752054434523638));
#94953=CARTESIAN_POINT('Ctrl Pts',(0.0138451843133365,-0.0320835708272304,
0.0752845467767324));
#94954=CARTESIAN_POINT('Ctrl Pts',(0.0138290003290959,-0.0319739230346346,
0.0753633029949647));
#94955=CARTESIAN_POINT('Ctrl Pts',(0.013811216187958,-0.0318646057455575,
0.0754416129330931));
#94956=CARTESIAN_POINT('Ctrl Pts',(0.0137922152118866,-0.0321934096636184,
0.0751144401110984));
#94957=CARTESIAN_POINT('Ctrl Pts',(0.0137789148311156,-0.0320835708272304,
0.0751926122201353));
#94958=CARTESIAN_POINT('Ctrl Pts',(0.0137640043973725,-0.0319739230346346,
0.0752704637354833));
#94959=CARTESIAN_POINT('Ctrl Pts',(0.0137475106319754,-0.0318646057455575,
0.0753478965156258));
#94960=CARTESIAN_POINT('Ctrl Pts',(0.0138125175185335,-0.0320218834582285,
0.0749920737483511));
#94961=CARTESIAN_POINT('Ctrl Pts',(0.0138037535665135,-0.0319391099350593,
0.0750512797306585));
#94962=CARTESIAN_POINT('Ctrl Pts',(0.013794070414634,-0.0318564869454885,
0.0751103129912258));
#94963=CARTESIAN_POINT('Ctrl Pts',(0.0137834791299389,-0.0317740741446489,
0.0751691311905896));
#94964=CARTESIAN_POINT('Ctrl Pts',(0.0138529501843157,-0.0320218834582285,
0.0749634027249053));
#94965=CARTESIAN_POINT('Ctrl Pts',(0.013844484628338,-0.0319391099350593,
0.0750230295135182));
#94966=CARTESIAN_POINT('Ctrl Pts',(0.0138350931207608,-0.0318564869454885,
0.0750824879849312));
#94967=CARTESIAN_POINT('Ctrl Pts',(0.0138247865451173,-0.0317740741446489,
0.0751417354701397));
#94968=CARTESIAN_POINT('Ctrl Pts',(0.0138933828500979,-0.0320218834582285,
0.0749347317014596));
#94969=CARTESIAN_POINT('Ctrl Pts',(0.0138852156901625,-0.0319391099350593,
0.0749947792963779));
#94970=CARTESIAN_POINT('Ctrl Pts',(0.0138761158268876,-0.0318564869454885,
0.0750546629786365));
#94971=CARTESIAN_POINT('Ctrl Pts',(0.0138660939602956,-0.0317740741446489,
0.0751143397496899));
#94972=CARTESIAN_POINT('Ctrl Pts',(0.01393381551588,-0.0320218834582285,
0.0749060606780138));
#94973=CARTESIAN_POINT('Ctrl Pts',(0.013925946751987,-0.0319391099350593,
0.0749665290792376));
#94974=CARTESIAN_POINT('Ctrl Pts',(0.0139171385330143,-0.0318564869454885,
0.0750268379723418));
#94975=CARTESIAN_POINT('Ctrl Pts',(0.013907401375474,-0.0317740741446489,
0.0750869440292401));
#94976=CARTESIAN_POINT('Origin',(0.0201732317095217,-0.039122885339083,
0.0749814954491545));
#94977=CARTESIAN_POINT('Ctrl Pts',(0.0134499655687186,-0.0352722978779556,
0.0719783795930296));
#94978=CARTESIAN_POINT('Ctrl Pts',(0.013456774637772,-0.0352466642097192,
0.0719960071072227));
#94979=CARTESIAN_POINT('Ctrl Pts',(0.0134636507752063,-0.0352210183808287,
0.072013590667304));
#94980=CARTESIAN_POINT('Ctrl Pts',(0.0134705947196212,-0.0351953608940151,
0.0720311306998356));
#94981=CARTESIAN_POINT('Origin',(0.0180829375484461,-0.0352456003065004,
0.0703829756227244));
#94982=CARTESIAN_POINT('Ctrl Pts',(0.013513908457505,-0.0350241211493339,
0.0721480462057737));
#94983=CARTESIAN_POINT('Ctrl Pts',(0.013541484548944,-0.0349144232867421,
0.0722222929816801));
#94984=CARTESIAN_POINT('Ctrl Pts',(0.0135675424121596,-0.0348045283677512,
0.0722971542153479));
#94985=CARTESIAN_POINT('Ctrl Pts',(0.0135920451021384,-0.0346945769586886,
0.0723725352610863));
#94986=CARTESIAN_POINT('Ctrl Pts',(0.0135633276853456,-0.0350241211493339,
0.0720460712984555));
#94987=CARTESIAN_POINT('Ctrl Pts',(0.0135923084392583,-0.0349144232867421,
0.0721209988039321));
#94988=CARTESIAN_POINT('Ctrl Pts',(0.0136197577345397,-0.0348045283677512,
0.0721965702099951));
#94989=CARTESIAN_POINT('Ctrl Pts',(0.013645636810079,-0.0346945769586886,
0.072272690027635));
#94990=CARTESIAN_POINT('Ctrl Pts',(0.0136127469131863,-0.0350241211493339,
0.0719440963911372));
#94991=CARTESIAN_POINT('Ctrl Pts',(0.0136431323295726,-0.0349144232867421,
0.0720197046261839));
#94992=CARTESIAN_POINT('Ctrl Pts',(0.0136719730569197,-0.0348045283677512,
0.0720959862046423));
#94993=CARTESIAN_POINT('Ctrl Pts',(0.0136992285180197,-0.0346945769586886,
0.0721728447941837));
#94994=CARTESIAN_POINT('Ctrl Pts',(0.0136621661410269,-0.0350241211493339,
0.071842121483819));
#94995=CARTESIAN_POINT('Ctrl Pts',(0.0136939562198869,-0.0349144232867421,
0.0719184104484358));
#94996=CARTESIAN_POINT('Ctrl Pts',(0.0137241883792998,-0.0348045283677512,
0.0719954021992895));
#94997=CARTESIAN_POINT('Ctrl Pts',(0.0137528202259604,-0.0346945769586886,
0.0720729995607325));
#94998=CARTESIAN_POINT('Origin',(-0.00242916077554619,-0.0345629067942929,
0.0773908926920414));
#94999=CARTESIAN_POINT('Ctrl Pts',(0.0137799984578508,-0.035197097365164,
0.0723659766414764));
#95000=CARTESIAN_POINT('Ctrl Pts',(0.0138047136837033,-0.0350869349321807,
0.0724443358522937));
#95001=CARTESIAN_POINT('Ctrl Pts',(0.0138278203387926,-0.0349764985129768,
0.0725232737908184));
#95002=CARTESIAN_POINT('Ctrl Pts',(0.0138492824677688,-0.0348659306849698,
0.0726026899528025));
#95003=CARTESIAN_POINT('Ctrl Pts',(0.0137052454206028,-0.035197097365164,
0.0723317355247895));
#95004=CARTESIAN_POINT('Ctrl Pts',(0.013730435010722,-0.0350869349321807,
0.072409059133584));
#95005=CARTESIAN_POINT('Ctrl Pts',(0.0137540379526281,-0.0349764985129768,
0.0724869704739755));
#95006=CARTESIAN_POINT('Ctrl Pts',(0.0137760177263077,-0.0348659306849698,
0.072565370409552));
#95007=CARTESIAN_POINT('Ctrl Pts',(0.0136304923833547,-0.035197097365164,
0.0722974944081026));
#95008=CARTESIAN_POINT('Ctrl Pts',(0.0136561563377407,-0.0350869349321807,
0.0723737824148743));
#95009=CARTESIAN_POINT('Ctrl Pts',(0.0136802555664635,-0.0349764985129768,
0.0724506671571325));
#95010=CARTESIAN_POINT('Ctrl Pts',(0.0137027529848467,-0.0348659306849698,
0.0725280508663016));
#95011=CARTESIAN_POINT('Ctrl Pts',(0.0135557393461067,-0.035197097365164,
0.0722632532914156));
#95012=CARTESIAN_POINT('Ctrl Pts',(0.0135818776647594,-0.0350869349321807,
0.0723385056961646));
#95013=CARTESIAN_POINT('Ctrl Pts',(0.013606473180299,-0.0349764985129768,
0.0724143638402896));
#95014=CARTESIAN_POINT('Ctrl Pts',(0.0136294882433856,-0.0348659306849698,
0.0724907313230511));
#95015=CARTESIAN_POINT('Origin',(-0.00252626234102887,-0.034563718796407,
0.076919833627074));
#95016=CARTESIAN_POINT('Ctrl Pts',(0.01354559713922,-0.0352450361861253,
0.0722311337487669));
#95017=CARTESIAN_POINT('Ctrl Pts',(0.0136179683655798,-0.0349452761023765,
0.0724356208496755));
#95018=CARTESIAN_POINT('Ctrl Pts',(0.0136747311881761,-0.0346444289983475,
0.0726449783210342));
#95019=CARTESIAN_POINT('Ctrl Pts',(0.0134570854127176,-0.0352450361861253,
0.0719973268321208));
#95020=CARTESIAN_POINT('Ctrl Pts',(0.0135382748114113,-0.0349452761023765,
0.0721984756585717));
#95021=CARTESIAN_POINT('Ctrl Pts',(0.0136040822073283,-0.0346444289983475,
0.0724051685599627));
#95022=CARTESIAN_POINT('Ctrl Pts',(0.0136289757645181,-0.0345231616327822,
0.0724904444859104));
#95023=CARTESIAN_POINT('Ctrl Pts',(0.0136518504008124,-0.0344132092796975,
0.0725663258285993));
#95024=CARTESIAN_POINT('Ctrl Pts',(0.0136731543111615,-0.0343032738558974,
0.0726426763999681));
#95025=CARTESIAN_POINT('Ctrl Pts',(0.013692862708334,-0.0341934961088741,
0.0727193976869967));
#95026=CARTESIAN_POINT('Ctrl Pts',(0.0136847005041198,-0.0345231616327822,
0.0723917738746085));
#95027=CARTESIAN_POINT('Ctrl Pts',(0.0137089351758738,-0.0344132092796975,
0.0724684233043786));
#95028=CARTESIAN_POINT('Ctrl Pts',(0.0137315831642355,-0.0343032738558974,
0.0725455700544596));
#95029=CARTESIAN_POINT('Ctrl Pts',(0.013752617986182,-0.0341934961088741,
0.0726231145477268));
#95030=CARTESIAN_POINT('Ctrl Pts',(0.0137404252437214,-0.0345231616327822,
0.0722931032633066));
#95031=CARTESIAN_POINT('Ctrl Pts',(0.0137660199509351,-0.0344132092796975,
0.0723705207801579));
#95032=CARTESIAN_POINT('Ctrl Pts',(0.0137900120173095,-0.0343032738558974,
0.0724484637089511));
#95033=CARTESIAN_POINT('Ctrl Pts',(0.0138123732640301,-0.0341934961088741,
0.0725268314084568));
#95034=CARTESIAN_POINT('Ctrl Pts',(0.013796149983323,-0.0345231616327822,
0.0721944326520047));
#95035=CARTESIAN_POINT('Ctrl Pts',(0.0138231047259964,-0.0344132092796975,
0.0722726182559372));
#95036=CARTESIAN_POINT('Ctrl Pts',(0.0138484408703835,-0.0343032738558974,
0.0723513573634426));
#95037=CARTESIAN_POINT('Ctrl Pts',(0.0138721285418781,-0.0341934961088741,
0.0724305482691869));
#95038=CARTESIAN_POINT('Origin',(-0.00244065506430078,-0.0345625596231532,
0.0773946847386776));
#95039=CARTESIAN_POINT('Ctrl Pts',(0.0139629083290236,-0.0346945769586885,
0.072769925375559));
#95040=CARTESIAN_POINT('Ctrl Pts',(0.0139819264548934,-0.034584662917669,
0.0728503914850401));
#95041=CARTESIAN_POINT('Ctrl Pts',(0.0139992838230083,-0.0344746925051587,
0.0729312646253629));
#95042=CARTESIAN_POINT('Ctrl Pts',(0.0140149586210603,-0.0343648066255171,
0.0730124410806917));
#95043=CARTESIAN_POINT('Ctrl Pts',(0.0138630631741826,-0.0346945769586885,
0.0727163337098122));
#95044=CARTESIAN_POINT('Ctrl Pts',(0.0138828198202937,-0.034584662917669,
0.0727954239025938));
#95045=CARTESIAN_POINT('Ctrl Pts',(0.0139009442881833,-0.0344746925051587,
0.0728749361635026));
#95046=CARTESIAN_POINT('Ctrl Pts',(0.0139174137754455,-0.0343648066255171,
0.0729547685163588));
#95047=CARTESIAN_POINT('Ctrl Pts',(0.0137632180193416,-0.0346945769586885,
0.0726627420440654));
#95048=CARTESIAN_POINT('Ctrl Pts',(0.0137837131856941,-0.034584662917669,
0.0727404563201476));
#95049=CARTESIAN_POINT('Ctrl Pts',(0.0138026047533584,-0.0344746925051587,
0.0728186077016422));
#95050=CARTESIAN_POINT('Ctrl Pts',(0.0138198689298307,-0.0343648066255171,
0.072897095952026));
#95051=CARTESIAN_POINT('Ctrl Pts',(0.0136633728645006,-0.0346945769586885,
0.0726091503783186));
#95052=CARTESIAN_POINT('Ctrl Pts',(0.0136846065510945,-0.034584662917669,
0.0726854887377014));
#95053=CARTESIAN_POINT('Ctrl Pts',(0.0137042652185335,-0.0344746925051587,
0.0727622792397819));
#95054=CARTESIAN_POINT('Ctrl Pts',(0.0137223240842159,-0.0343648066255171,
0.0728394233876932));
#95055=CARTESIAN_POINT('Origin',(-0.00258261070982406,-0.0345626446731565,
0.0769352929913375));
#95056=CARTESIAN_POINT('Ctrl Pts',(0.0136651594291266,-0.0346945769586886,
0.0726101093129251));
#95057=CARTESIAN_POINT('Ctrl Pts',(0.0136974130561055,-0.0345275153362891,
0.0727261756777781));
#95058=CARTESIAN_POINT('Ctrl Pts',(0.0137260248451815,-0.0343603235965159,
0.072843286410219));
#95059=CARTESIAN_POINT('Ctrl Pts',(0.0137509153232183,-0.034193496108874,
0.072961093890999));
#95060=CARTESIAN_POINT('Ctrl Pts',(0.013640963362378,-0.0346945769586886,
0.07252984363729));
#95061=CARTESIAN_POINT('Ctrl Pts',(0.0136748981860697,-0.0345275153362891,
0.0726454032058373));
#95062=CARTESIAN_POINT('Ctrl Pts',(0.0137052075449794,-0.0343603235965159,
0.0727620598829783));
#95063=CARTESIAN_POINT('Ctrl Pts',(0.0137318069253539,-0.034193496108874,
0.072879467317738));
#95064=CARTESIAN_POINT('Ctrl Pts',(0.0136167672956295,-0.0346945769586886,
0.0724495779616548));
#95065=CARTESIAN_POINT('Ctrl Pts',(0.0136523833160339,-0.0345275153362891,
0.0725646307338965));
#95066=CARTESIAN_POINT('Ctrl Pts',(0.0136843902447773,-0.0343603235965159,
0.0726808333557376));
#95067=CARTESIAN_POINT('Ctrl Pts',(0.0137126985274895,-0.034193496108874,
0.0727978407444771));
#95068=CARTESIAN_POINT('Ctrl Pts',(0.0135925712288809,-0.0346945769586886,
0.0723693122860197));
#95069=CARTESIAN_POINT('Ctrl Pts',(0.0136298684459981,-0.0345275153362891,
0.0724838582619558));
#95070=CARTESIAN_POINT('Ctrl Pts',(0.0136635729445752,-0.0343603235965159,
0.0725996068284969));
#95071=CARTESIAN_POINT('Ctrl Pts',(0.0136935901296251,-0.034193496108874,
0.0727162141712161));
#95072=CARTESIAN_POINT('Ctrl Pts',(0.013722316349829,-0.0340223579322365,
0.0728393927910273));
#95073=CARTESIAN_POINT('Ctrl Pts',(0.0137403930414476,-0.0339125849573554,
0.0729166111786378));
#95074=CARTESIAN_POINT('Ctrl Pts',(0.0137568587895916,-0.0338030433565221,
0.0729941494512934));
#95075=CARTESIAN_POINT('Ctrl Pts',(0.0137717013273179,-0.0336938721132327,
0.0730719065840064));
#95076=CARTESIAN_POINT('Ctrl Pts',(0.0137841267982558,-0.0340223579322365,
0.0727444156974968));
#95077=CARTESIAN_POINT('Ctrl Pts',(0.0138035134717049,-0.0339125849573554,
0.0728224866123995));
#95078=CARTESIAN_POINT('Ctrl Pts',(0.0138212706358363,-0.0338030433565221,
0.0729009039268662));
#95079=CARTESIAN_POINT('Ctrl Pts',(0.0138373844718545,-0.0336938721132327,
0.0729795653453639));
#95080=CARTESIAN_POINT('Ctrl Pts',(0.0138459372466827,-0.0340223579322365,
0.0726494386039662));
#95081=CARTESIAN_POINT('Ctrl Pts',(0.0138666339019622,-0.0339125849573554,
0.0727283620461611));
#95082=CARTESIAN_POINT('Ctrl Pts',(0.013885682482081,-0.0338030433565221,
0.0728076584024389));
#95083=CARTESIAN_POINT('Ctrl Pts',(0.013903067616391,-0.0336938721132327,
0.0728872241067214));
#95084=CARTESIAN_POINT('Ctrl Pts',(0.0139077476951095,-0.0340223579322365,
0.0725544615104357));
#95085=CARTESIAN_POINT('Ctrl Pts',(0.0139297543322195,-0.0339125849573554,
0.0726342374799228));
#95086=CARTESIAN_POINT('Ctrl Pts',(0.0139500943283257,-0.0338030433565221,
0.0727144128780116));
#95087=CARTESIAN_POINT('Ctrl Pts',(0.0139687507609276,-0.0336938721132327,
0.0727948828680789));
#95088=CARTESIAN_POINT('Origin',(-0.00232499863165299,-0.0345589643413838,
0.0773618751717664));
#95089=CARTESIAN_POINT('Ctrl Pts',(0.0140380417500741,-0.034193496108874,
0.0731392904012537));
#95090=CARTESIAN_POINT('Ctrl Pts',(0.0140519788368658,-0.0340836138585568,
0.0732208445379278));
#95091=CARTESIAN_POINT('Ctrl Pts',(0.0140642216446534,-0.033973889665241,
0.07330264794216));
#95092=CARTESIAN_POINT('Ctrl Pts',(0.0140747615225922,-0.0338644633307392,
0.073384594865307));
#95093=CARTESIAN_POINT('Ctrl Pts',(0.0139417585241658,-0.034193496108874,
0.0730795350696361));
#95094=CARTESIAN_POINT('Ctrl Pts',(0.0139565196015914,-0.0340836138585568,
0.0731597615176469));
#95095=CARTESIAN_POINT('Ctrl Pts',(0.0139696134783777,-0.033973889665241,
0.0732402549210231));
#95096=CARTESIAN_POINT('Ctrl Pts',(0.0139810303020233,-0.0338644633307392,
0.0733209111347417));
#95097=CARTESIAN_POINT('Ctrl Pts',(0.0138454752982574,-0.034193496108874,
0.0730197797380186));
#95098=CARTESIAN_POINT('Ctrl Pts',(0.013861060366317,-0.0340836138585568,
0.0730986784973661));
#95099=CARTESIAN_POINT('Ctrl Pts',(0.013875005312102,-0.033973889665241,
0.0731778618998861));
#95100=CARTESIAN_POINT('Ctrl Pts',(0.0138872990814544,-0.0338644633307392,
0.0732572274041764));
#95101=CARTESIAN_POINT('Ctrl Pts',(0.0137491920723491,-0.034193496108874,
0.072960024406401));
#95102=CARTESIAN_POINT('Ctrl Pts',(0.0137656011310426,-0.0340836138585568,
0.0730375954770853));
#95103=CARTESIAN_POINT('Ctrl Pts',(0.0137803971458263,-0.033973889665241,
0.0731154688787492));
#95104=CARTESIAN_POINT('Ctrl Pts',(0.0137935678608855,-0.0338644633307392,
0.0731935436736112));
#95105=CARTESIAN_POINT('Origin',(-0.00250948027280974,-0.0345610621864204,
0.0769174468476583));
#95106=CARTESIAN_POINT('Ctrl Pts',(0.0137433255110496,-0.0342436276873901,
0.0729257214786727));
#95107=CARTESIAN_POINT('Ctrl Pts',(0.0137894999366756,-0.0339430054201861,
0.0731376660488551));
#95108=CARTESIAN_POINT('Ctrl Pts',(0.0138195786521574,-0.0336441434784163,
0.0733524865536648));
#95109=CARTESIAN_POINT('Ctrl Pts',(0.0136848121853066,-0.0342436276873901,
0.072682665537148));
#95110=CARTESIAN_POINT('Ctrl Pts',(0.013740153616887,-0.0339430054201861,
0.0728924032408694));
#95111=CARTESIAN_POINT('Ctrl Pts',(0.0137795395260446,-0.0336441434784163,
0.0731057136451434));
#95112=CARTESIAN_POINT('Ctrl Pts',(0.0137935631233125,-0.0335235895815127,
0.0731935163509172));
#95113=CARTESIAN_POINT('Ctrl Pts',(0.0138067310038849,-0.0334144449262719,
0.0732715720481918));
#95114=CARTESIAN_POINT('Ctrl Pts',(0.0138183014407946,-0.0333049234473133,
0.0733499894605085));
#95115=CARTESIAN_POINT('Ctrl Pts',(0.0138282505559521,-0.0331951640388588,
0.0734286696562709));
#95116=CARTESIAN_POINT('Ctrl Pts',(0.0138612152860968,-0.0335235895815127,
0.0731026078400021));
#95117=CARTESIAN_POINT('Ctrl Pts',(0.0138756347013044,-0.0334144449262719,
0.0731815949024922));
#95118=CARTESIAN_POINT('Ctrl Pts',(0.0138884388694064,-0.0333049234473133,
0.073260970605814));
#95119=CARTESIAN_POINT('Ctrl Pts',(0.0138996022237517,-0.0331951640388588,
0.0733406349359134));
#95120=CARTESIAN_POINT('Ctrl Pts',(0.0139288674488812,-0.0335235895815127,
0.0730116993290869));
#95121=CARTESIAN_POINT('Ctrl Pts',(0.0139445383987239,-0.0334144449262719,
0.0730916177567926));
#95122=CARTESIAN_POINT('Ctrl Pts',(0.0139585762980183,-0.0333049234473133,
0.0731719517511194));
#95123=CARTESIAN_POINT('Ctrl Pts',(0.0139709538915513,-0.0331951640388588,
0.0732526002155559));
#95124=CARTESIAN_POINT('Ctrl Pts',(0.0139965196116655,-0.0335235895815127,
0.0729207908181717));
#95125=CARTESIAN_POINT('Ctrl Pts',(0.0140134420961433,-0.0334144449262719,
0.073001640611093));
#95126=CARTESIAN_POINT('Ctrl Pts',(0.0140287137266301,-0.0333049234473133,
0.0730829328964249));
#95127=CARTESIAN_POINT('Ctrl Pts',(0.0140423055593509,-0.0331951640388588,
0.0731645654951985));
#95128=CARTESIAN_POINT('Origin',(-0.0027853698522513,-0.0326434571771509,
0.0747622580477667));
#95129=CARTESIAN_POINT('Ctrl Pts',(0.0140914865154029,-0.0336938721132395,
0.0735138194781665));
#95130=CARTESIAN_POINT('Ctrl Pts',(0.0140952102911043,-0.0336474569764961,
0.0735487504318593));
#95131=CARTESIAN_POINT('Ctrl Pts',(0.0140985249007336,-0.033601104548885,
0.0735837225835572));
#95132=CARTESIAN_POINT('Ctrl Pts',(0.0141069167297378,-0.0334837508662626,
0.0736722640257744));
#95133=CARTESIAN_POINT('Ctrl Pts',(0.0141126812073164,-0.0333660264799449,
0.073761015254398));
#95134=CARTESIAN_POINT('Ctrl Pts',(0.0138144634936374,-0.0336938721132395,
0.0733167705383206));
#95135=CARTESIAN_POINT('Ctrl Pts',(0.0138193406621715,-0.0336474569764961,
0.0733500799843411));
#95136=CARTESIAN_POINT('Ctrl Pts',(0.0138238275673968,-0.033601104548885,
0.0733834442413926));
#95137=CARTESIAN_POINT('Ctrl Pts',(0.0138351873791458,-0.0334837508662626,
0.0734679148642864));
#95138=CARTESIAN_POINT('Ctrl Pts',(0.0138440391629595,-0.0333660264799449,
0.0735526850086673));
#95139=CARTESIAN_POINT('Ctrl Pts',(0.0138144634936481,-0.0336938721132427,
0.0733167705383356));
#95140=CARTESIAN_POINT('Ctrl Pts',(0.0138193406621818,-0.0336474569765026,
0.0733500799843536));
#95141=CARTESIAN_POINT('Ctrl Pts',(0.0138238275674068,-0.0336011045488949,
0.0733834442414026));
#95142=CARTESIAN_POINT('Ctrl Pts',(0.0138350927673962,-0.0334847282626114,
0.0734672113390579));
#95143=CARTESIAN_POINT('Ctrl Pts',(0.0138438915742658,-0.0333679869984219,
0.0735512732946507));
#95144=CARTESIAN_POINT('Ctrl Pts',(0.0138144634936371,-0.0336938721132428,
0.0733167705383183));
#95145=CARTESIAN_POINT('Ctrl Pts',(0.0138319064066766,-0.0335278710435084,
0.0734358998581826));
#95146=CARTESIAN_POINT('Ctrl Pts',(0.0138456073188421,-0.0333620469224321,
0.0735555342738467));
#95147=CARTESIAN_POINT('Ctrl Pts',(0.0138555531447896,-0.0331951640388602,
0.07367573556167));
#95148=CARTESIAN_POINT('Ctrl Pts',(0.013800518175293,-0.0336938721132428,
0.07323410520145));
#95149=CARTESIAN_POINT('Ctrl Pts',(0.0138196916131744,-0.0335278710435084,
0.0733529425885558));
#95150=CARTESIAN_POINT('Ctrl Pts',(0.0138351315963226,-0.0333620469224321,
0.0734723394429718));
#95151=CARTESIAN_POINT('Ctrl Pts',(0.013846825943795,-0.0331951640388602,
0.073592357712177));
#95152=CARTESIAN_POINT('Ctrl Pts',(0.013786572856949,-0.0336938721132428,
0.0731514398645816));
#95153=CARTESIAN_POINT('Ctrl Pts',(0.0138074768196722,-0.0335278710435084,
0.0732699853189289));
#95154=CARTESIAN_POINT('Ctrl Pts',(0.013824655873803,-0.0333620469224321,
0.0733891446120969));
#95155=CARTESIAN_POINT('Ctrl Pts',(0.0138380987428003,-0.0331951640388602,
0.073508979862684));
#95156=CARTESIAN_POINT('Ctrl Pts',(0.013772627538605,-0.0336938721132428,
0.0730687745277132));
#95157=CARTESIAN_POINT('Ctrl Pts',(0.01379526202617,-0.0335278710435084,
0.0731870280493021));
#95158=CARTESIAN_POINT('Ctrl Pts',(0.0138141801512834,-0.0333620469224321,
0.073305949781222));
#95159=CARTESIAN_POINT('Ctrl Pts',(0.0138293715418057,-0.0331951640388602,
0.073425602013191));
#95160=CARTESIAN_POINT('Ctrl Pts',(0.0138424334273781,-0.0330240426238155,
0.073551410958392));
#95161=CARTESIAN_POINT('Ctrl Pts',(0.0138506795746033,-0.0329142774063509,
0.0736301909505556));
#95162=CARTESIAN_POINT('Ctrl Pts',(0.0138573012303345,-0.0328043479726686,
0.0737091806883161));
#95163=CARTESIAN_POINT('Ctrl Pts',(0.0138622871249351,-0.0326943950436594,
0.0737882792135521));
#95164=CARTESIAN_POINT('Ctrl Pts',(0.0139156601687748,-0.0330240426238155,
0.07346492986029));
#95165=CARTESIAN_POINT('Ctrl Pts',(0.0139250976773808,-0.0329142774063509,
0.0735447186221577));
#95166=CARTESIAN_POINT('Ctrl Pts',(0.0139328904343422,-0.0328043479726686,
0.0736247422612984));
#95167=CARTESIAN_POINT('Ctrl Pts',(0.0139390256332781,-0.0326943950436594,
0.0737048985364033));
#95168=CARTESIAN_POINT('Ctrl Pts',(0.0139888869101716,-0.0330240426238155,
0.0733784487621881));
#95169=CARTESIAN_POINT('Ctrl Pts',(0.0139995157801583,-0.0329142774063509,
0.0734592462937599));
#95170=CARTESIAN_POINT('Ctrl Pts',(0.01400847963835,-0.0328043479726686,
0.0735403038342808));
#95171=CARTESIAN_POINT('Ctrl Pts',(0.014015764141621,-0.0326943950436594,
0.0736215178592544));
#95172=CARTESIAN_POINT('Ctrl Pts',(0.0140621136515683,-0.0330240426238155,
0.0732919676640861));
#95173=CARTESIAN_POINT('Ctrl Pts',(0.0140739338829358,-0.0329142774063509,
0.073373773965362));
#95174=CARTESIAN_POINT('Ctrl Pts',(0.0140840688423578,-0.0328043479726686,
0.0734558654072631));
#95175=CARTESIAN_POINT('Ctrl Pts',(0.014092502649964,-0.0326943950436594,
0.0735381371821056));
#95176=CARTESIAN_POINT('Origin',(-0.00290866442199188,-0.03263966828572,
0.0747719455594014));
#95177=CARTESIAN_POINT('Ctrl Pts',(0.0141180815491696,-0.0331951640388587,
0.0738885134227377));
#95178=CARTESIAN_POINT('Ctrl Pts',(0.0141216829976228,-0.0330855618305429,
0.073971072766203));
#95179=CARTESIAN_POINT('Ctrl Pts',(0.0141235806818819,-0.0329757224528702,
0.0740537660613222));
#95180=CARTESIAN_POINT('Ctrl Pts',(0.0141237669775404,-0.0328657862230221,
0.0741364875335773));
#95181=CARTESIAN_POINT('Ctrl Pts',(0.0140300468988956,-0.0331951640388587,
0.0738171618117404));
#95182=CARTESIAN_POINT('Ctrl Pts',(0.0140346310714019,-0.0330855618305429,
0.0738985086560466));
#95183=CARTESIAN_POINT('Ctrl Pts',(0.0140375372484301,-0.0329757224528702,
0.0739800088891584));
#95184=CARTESIAN_POINT('Ctrl Pts',(0.0140387565890793,-0.0328657862230221,
0.0740615583276929));
#95185=CARTESIAN_POINT('Ctrl Pts',(0.0139420122486216,-0.0331951640388587,
0.0737458102007431));
#95186=CARTESIAN_POINT('Ctrl Pts',(0.0139475791451811,-0.0330855618305429,
0.0738259445458902));
#95187=CARTESIAN_POINT('Ctrl Pts',(0.0139514938149783,-0.0329757224528702,
0.0739062517169946));
#95188=CARTESIAN_POINT('Ctrl Pts',(0.0139537462006182,-0.0328657862230221,
0.0739866291218084));
#95189=CARTESIAN_POINT('Ctrl Pts',(0.0138539775983476,-0.0331951640388587,
0.0736744585897458));
#95190=CARTESIAN_POINT('Ctrl Pts',(0.0138605272189603,-0.0330855618305429,
0.0737533804357337));
#95191=CARTESIAN_POINT('Ctrl Pts',(0.0138654503815266,-0.0329757224528702,
0.0738324945448307));
#95192=CARTESIAN_POINT('Ctrl Pts',(0.0138687358121571,-0.0328657862230221,
0.073911699915924));
#95193=CARTESIAN_POINT('Origin',(-0.00289715649951292,-0.0326401908835659,
0.0742911748872013));
#95194=CARTESIAN_POINT('Ctrl Pts',(0.013852462948997,-0.0332451089994432,
0.0736397629990749));
#95195=CARTESIAN_POINT('Ctrl Pts',(0.0138717068523336,-0.0329451141710258,
0.0738558237287217));
#95196=CARTESIAN_POINT('Ctrl Pts',(0.0138746215083516,-0.0326442513127503,
0.0740727201821075));
#95197=CARTESIAN_POINT('Ctrl Pts',(0.0138248771362445,-0.0332451089994432,
0.0733912896143136));
#95198=CARTESIAN_POINT('Ctrl Pts',(0.0138534923666103,-0.0329451141710258,
0.0736063099280102));
#95199=CARTESIAN_POINT('Ctrl Pts',(0.0138658300950892,-0.0326442513127503,
0.0738228748078201));
#95200=CARTESIAN_POINT('Ctrl Pts',(0.0138687345930848,-0.0325229783203384,
0.0739116683627356));
#95201=CARTESIAN_POINT('Ctrl Pts',(0.0138720199894327,-0.0324130253112079,
0.073990862404494));
#95202=CARTESIAN_POINT('Ctrl Pts',(0.01387366665703,-0.0323031222247695,
0.0740701123975671));
#95203=CARTESIAN_POINT('Ctrl Pts',(0.0138736760686934,-0.0321934096636184,
0.0741493167539226));
#95204=CARTESIAN_POINT('Ctrl Pts',(0.0139472470386026,-0.0325229783203384,
0.0738299558266834));
#95205=CARTESIAN_POINT('Ctrl Pts',(0.0139516588404526,-0.0324130253112079,
0.0739102321607666));
#95206=CARTESIAN_POINT('Ctrl Pts',(0.0139544093541039,-0.0323031222247695,
0.073990587583158));
#95207=CARTESIAN_POINT('Ctrl Pts',(0.01395549868839,-0.0321934096636184,
0.0740709190399554));
#95208=CARTESIAN_POINT('Ctrl Pts',(0.0140257594841205,-0.0325229783203384,
0.0737482432906312));
#95209=CARTESIAN_POINT('Ctrl Pts',(0.0140312976914725,-0.0324130253112079,
0.0738296019170392));
#95210=CARTESIAN_POINT('Ctrl Pts',(0.0140351520511777,-0.0323031222247695,
0.0739110627687489));
#95211=CARTESIAN_POINT('Ctrl Pts',(0.0140373213080865,-0.0321934096636184,
0.0739925213259883));
#95212=CARTESIAN_POINT('Ctrl Pts',(0.0141042719296383,-0.0325229783203384,
0.073666530754579));
#95213=CARTESIAN_POINT('Ctrl Pts',(0.0141109365424923,-0.0324130253112079,
0.0737489716733118));
#95214=CARTESIAN_POINT('Ctrl Pts',(0.0141158947482515,-0.0323031222247695,
0.0738315379543398));
#95215=CARTESIAN_POINT('Ctrl Pts',(0.0141191439277831,-0.0321934096636184,
0.0739141236120212));
#95216=CARTESIAN_POINT('Origin',(-0.0029001419440751,-0.0326393375178958,
0.0747717039100236));
#95217=CARTESIAN_POINT('Ctrl Pts',(0.0141226720466918,-0.0326943950436593,
0.0742654145775462));
#95218=CARTESIAN_POINT('Ctrl Pts',(0.0141210814175033,-0.0325844576448127,
0.0743480905228462));
#95219=CARTESIAN_POINT('Ctrl Pts',(0.0141177808016456,-0.0324744968375319,
0.0744307394224318));
#95220=CARTESIAN_POINT('Ctrl Pts',(0.0141127758886649,-0.0323646534831895,
0.0745132554400428));
#95221=CARTESIAN_POINT('Ctrl Pts',(0.014039291396821,-0.0326943950436593,
0.0741886760943082));
#95222=CARTESIAN_POINT('Ctrl Pts',(0.0140387583677547,-0.0325844576448127,
0.074270202897981));
#95223=CARTESIAN_POINT('Ctrl Pts',(0.0140365391930001,-0.0324744968375319,
0.0743517244475174));
#95224=CARTESIAN_POINT('Ctrl Pts',(0.0140326381565751,-0.0323646534831895,
0.074433136331972));
#95225=CARTESIAN_POINT('Ctrl Pts',(0.0139559107469501,-0.0326943950436593,
0.0741119376110703));
#95226=CARTESIAN_POINT('Ctrl Pts',(0.0139564353180061,-0.0325844576448127,
0.0741923152731158));
#95227=CARTESIAN_POINT('Ctrl Pts',(0.0139552975843547,-0.0324744968375319,
0.0742727094726029));
#95228=CARTESIAN_POINT('Ctrl Pts',(0.0139525004244853,-0.0323646534831895,
0.0743530172239012));
#95229=CARTESIAN_POINT('Ctrl Pts',(0.0138725300970792,-0.0326943950436593,
0.0740351991278323));
#95230=CARTESIAN_POINT('Ctrl Pts',(0.0138741122682574,-0.0325844576448127,
0.0741144276482506));
#95231=CARTESIAN_POINT('Ctrl Pts',(0.0138740559757092,-0.0324744968375319,
0.0741936944976885));
#95232=CARTESIAN_POINT('Ctrl Pts',(0.0138723626923955,-0.0323646534831895,
0.0742728981158304));
#95233=CARTESIAN_POINT('Origin',(-0.00293498603248267,-0.0326395579068033,
0.0742921174191728));
#95234=CARTESIAN_POINT('Ctrl Pts',(0.0138731957326305,-0.0327445246961876,
0.0740004374660528));
#95235=CARTESIAN_POINT('Ctrl Pts',(0.0138788365757548,-0.0324436878365475,
0.0742172801403344));
#95236=CARTESIAN_POINT('Ctrl Pts',(0.0138681279175358,-0.0321434074463188,
0.0744339316788471));
#95237=CARTESIAN_POINT('Ctrl Pts',(0.0138612644240796,-0.0327445246961876,
0.0737507223406073));
#95238=CARTESIAN_POINT('Ctrl Pts',(0.0138763234270281,-0.0324436878365475,
0.0739671150182352));
#95239=CARTESIAN_POINT('Ctrl Pts',(0.0138750400682232,-0.0321434074463188,
0.0741840272527702));
#95240=CARTESIAN_POINT('Ctrl Pts',(0.0138710330615361,-0.0322357242816074,
0.0743673302909342));
#95241=CARTESIAN_POINT('Ctrl Pts',(0.0138641113736369,-0.0319819883628706,
0.0745503727771823));
#95242=CARTESIAN_POINT('Ctrl Pts',(0.013845556196359,-0.0317295851069885,
0.074732603858317));
#95243=CARTESIAN_POINT('Ctrl Pts',(0.0138750481229576,-0.0322357242816074,
0.0741173625344499));
#95244=CARTESIAN_POINT('Ctrl Pts',(0.0138760875839061,-0.0319819883628706,
0.074300532895197));
#95245=CARTESIAN_POINT('Ctrl Pts',(0.0138654692841997,-0.0317295851069885,
0.074483398182353));
#95246=CARTESIAN_POINT('Origin',(-0.00283968559452192,-0.0326371942645095,
0.0742925970323401));
#95247=CARTESIAN_POINT('Origin',(-0.00277747244381728,-0.0326352985532441,
0.0747677043288159));
#95248=CARTESIAN_POINT('Ctrl Pts',(0.0141035876665989,-0.0321934096636183,
0.0746418602437497));
#95249=CARTESIAN_POINT('Ctrl Pts',(0.0140968045305051,-0.0320835708272304,
0.074724326421606));
#95250=CARTESIAN_POINT('Ctrl Pts',(0.0140883186956413,-0.0319739230346346,
0.0748066043890788));
#95251=CARTESIAN_POINT('Ctrl Pts',(0.0140781490981425,-0.0318646057455575,
0.0748885897104643));
#95252=CARTESIAN_POINT('Ctrl Pts',(0.0140251898851185,-0.0321934096636183,
0.0745600375535904));
#95253=CARTESIAN_POINT('Ctrl Pts',(0.0140195351476907,-0.0320835708272304,
0.0746414225649406));
#95254=CARTESIAN_POINT('Ctrl Pts',(0.0140121994316605,-0.0319739230346346,
0.0747226433451796));
#95255=CARTESIAN_POINT('Ctrl Pts',(0.0140032000978575,-0.0318646057455575,
0.0748035966982679));
#95256=CARTESIAN_POINT('Ctrl Pts',(0.0139467921036381,-0.0321934096636183,
0.0744782148634312));
#95257=CARTESIAN_POINT('Ctrl Pts',(0.0139422657648763,-0.0320835708272304,
0.0745585187082753));
#95258=CARTESIAN_POINT('Ctrl Pts',(0.0139360801676797,-0.0319739230346346,
0.0746386823012803));
#95259=CARTESIAN_POINT('Ctrl Pts',(0.0139282510975725,-0.0318646057455575,
0.0747186036860715));
#95260=CARTESIAN_POINT('Ctrl Pts',(0.0138683943221577,-0.0321934096636183,
0.074396392173272));
#95261=CARTESIAN_POINT('Ctrl Pts',(0.0138649963820619,-0.0320835708272304,
0.0744756148516099));
#95262=CARTESIAN_POINT('Ctrl Pts',(0.0138599609036989,-0.0319739230346346,
0.0745547212573811));
#95263=CARTESIAN_POINT('Ctrl Pts',(0.0138533020972875,-0.0318646057455575,
0.0746336106738751));
#95264=CARTESIAN_POINT('Ctrl Pts',(0.0138731999671288,-0.0320218834582284,
0.0742724461521044));
#95265=CARTESIAN_POINT('Ctrl Pts',(0.0138719255986971,-0.0319391099350594,
0.0743322836920026));
#95266=CARTESIAN_POINT('Ctrl Pts',(0.0138697176307971,-0.0318564869454889,
0.0743920650784139));
#95267=CARTESIAN_POINT('Ctrl Pts',(0.013866581736664,-0.0317740741446495,
0.0744517469186658));
#95268=CARTESIAN_POINT('Ctrl Pts',(0.0139097203771866,-0.0320218834582284,
0.074238933651498));
#95269=CARTESIAN_POINT('Ctrl Pts',(0.0139087947928702,-0.0319391099350594,
0.0742991512805774));
#95270=CARTESIAN_POINT('Ctrl Pts',(0.0139069294626203,-0.0318564869454889,
0.0743593179721964));
#95271=CARTESIAN_POINT('Ctrl Pts',(0.013904129836306,-0.0317740741446495,
0.0744193900297399));
#95272=CARTESIAN_POINT('Ctrl Pts',(0.0139462407872444,-0.0320218834582284,
0.0742054211508916));
#95273=CARTESIAN_POINT('Ctrl Pts',(0.0139456639870434,-0.0319391099350594,
0.0742660188691522));
#95274=CARTESIAN_POINT('Ctrl Pts',(0.0139441412944436,-0.0318564869454889,
0.0743265708659789));
#95275=CARTESIAN_POINT('Ctrl Pts',(0.0139416779359479,-0.0317740741446495,
0.0743870331408141));
#95276=CARTESIAN_POINT('Ctrl Pts',(0.0139827611973022,-0.0320218834582284,
0.0741719086502852));
#95277=CARTESIAN_POINT('Ctrl Pts',(0.0139825331812165,-0.0319391099350594,
0.074232886457727));
#95278=CARTESIAN_POINT('Ctrl Pts',(0.0139813531262668,-0.0318564869454889,
0.0742938237597613));
#95279=CARTESIAN_POINT('Ctrl Pts',(0.0139792260355899,-0.0317740741446495,
0.0743546762518882));
#95280=CARTESIAN_POINT('Origin',(0.0201824322144088,-0.0391228853390779,
0.0734647423886097));
#95281=CARTESIAN_POINT('Ctrl Pts',(0.0131357908142684,-0.035272297877955,
0.0713279556835488));
#95282=CARTESIAN_POINT('Ctrl Pts',(0.0131447555051321,-0.0352466642097187,
0.0713445907968852));
#95283=CARTESIAN_POINT('Ctrl Pts',(0.0131537812266114,-0.0352210183808287,
0.0713611738968043));
#95284=CARTESIAN_POINT('Ctrl Pts',(0.0131628687649444,-0.0351953608940152,
0.071377705313933));
#95285=CARTESIAN_POINT('Origin',(0.0175322732876919,-0.0352456003065006,
0.0691644665908431));
#95286=CARTESIAN_POINT('Ctrl Pts',(0.0132204943594808,-0.035024121149334,
0.071488270255359));
#95287=CARTESIAN_POINT('Ctrl Pts',(0.0132571585937083,-0.0349144232867422,
0.0715584753725519));
#95288=CARTESIAN_POINT('Ctrl Pts',(0.0132923935833736,-0.0348045283677513,
0.0716294803867756));
#95289=CARTESIAN_POINT('Ctrl Pts',(0.0133261508125351,-0.0346945769586886,
0.071701196029087));
#95290=CARTESIAN_POINT('Ctrl Pts',(0.0132567430570725,-0.035024121149334,
0.0713809055790178));
#95291=CARTESIAN_POINT('Ctrl Pts',(0.0132948861956287,-0.0349144232867422,
0.071451610007135));
#95292=CARTESIAN_POINT('Ctrl Pts',(0.013331590653705,-0.0348045283677513,
0.0715231452011525));
#95293=CARTESIAN_POINT('Ctrl Pts',(0.0133668060078872,-0.0346945769586886,
0.0715954212830754));
#95294=CARTESIAN_POINT('Ctrl Pts',(0.0132929917546642,-0.035024121149334,
0.0712735409026767));
#95295=CARTESIAN_POINT('Ctrl Pts',(0.0133326137975491,-0.0349144232867422,
0.0713447446417181));
#95296=CARTESIAN_POINT('Ctrl Pts',(0.0133707877240365,-0.0348045283677513,
0.0714168100155294));
#95297=CARTESIAN_POINT('Ctrl Pts',(0.0134074612032392,-0.0346945769586886,
0.0714896465370638));
#95298=CARTESIAN_POINT('Ctrl Pts',(0.0133292404522559,-0.035024121149334,
0.0711661762263355));
#95299=CARTESIAN_POINT('Ctrl Pts',(0.0133703413994695,-0.0349144232867422,
0.0712378792763012));
#95300=CARTESIAN_POINT('Ctrl Pts',(0.0134099847943679,-0.0348045283677513,
0.0713104748299062));
#95301=CARTESIAN_POINT('Ctrl Pts',(0.0134481163985913,-0.0346945769586886,
0.0713838717910522));
#95302=CARTESIAN_POINT('Origin',(-0.00193975610763966,-0.0345629067941104,
0.0786879717508215));
#95303=CARTESIAN_POINT('Ctrl Pts',(0.0135118000868944,-0.0351970973651643,
0.0716711323243206));
#95304=CARTESIAN_POINT('Ctrl Pts',(0.0135461414390807,-0.0350869349321794,
0.0717457760101826));
#95305=CARTESIAN_POINT('Ctrl Pts',(0.0135789594383797,-0.0349764985129738,
0.0718211954676863));
#95306=CARTESIAN_POINT('Ctrl Pts',(0.0136102058164377,-0.0348659306849652,
0.0718972954914902));
#95307=CARTESIAN_POINT('Ctrl Pts',(0.0134333449497974,-0.0351970973651643,
0.0716465302489431));
#95308=CARTESIAN_POINT('Ctrl Pts',(0.0134680271303964,-0.0350869349321794,
0.0717200870452061));
#95309=CARTESIAN_POINT('Ctrl Pts',(0.0135012088362788,-0.0349764985129738,
0.071794425798378));
#95310=CARTESIAN_POINT('Ctrl Pts',(0.0135328414103154,-0.0348659306849652,
0.0718694527309385));
#95311=CARTESIAN_POINT('Ctrl Pts',(0.0133548898127005,-0.0351970973651643,
0.0716219281735656));
#95312=CARTESIAN_POINT('Ctrl Pts',(0.0133899128217121,-0.0350869349321794,
0.0716943980802297));
#95313=CARTESIAN_POINT('Ctrl Pts',(0.0134234582341778,-0.0349764985129738,
0.0717676561290697));
#95314=CARTESIAN_POINT('Ctrl Pts',(0.0134554770041932,-0.0348659306849652,
0.0718416099703869));
#95315=CARTESIAN_POINT('Ctrl Pts',(0.0132764346756035,-0.0351970973651643,
0.0715973260981881));
#95316=CARTESIAN_POINT('Ctrl Pts',(0.0133117985130278,-0.0350869349321794,
0.0716687091152532));
#95317=CARTESIAN_POINT('Ctrl Pts',(0.0133457076320769,-0.0349764985129738,
0.0717408864597614));
#95318=CARTESIAN_POINT('Ctrl Pts',(0.0133781125980709,-0.0348659306849652,
0.0718137672098353));
#95319=CARTESIAN_POINT('Origin',(-0.00209513135373274,-0.0345637187965986,
0.0782327971808723));
#95320=CARTESIAN_POINT('Ctrl Pts',(0.0132623467969079,-0.0352450361861252,
0.071566730983312));
#95321=CARTESIAN_POINT('Ctrl Pts',(0.0133597763841107,-0.0349452761023764,
0.071760535122536));
#95322=CARTESIAN_POINT('Ctrl Pts',(0.0134423310637528,-0.0346444289983474,
0.0719611274795987));
#95323=CARTESIAN_POINT('Ctrl Pts',(0.0131452292349131,-0.0352450361861252,
0.0713458611649293));
#95324=CARTESIAN_POINT('Ctrl Pts',(0.0132509890637948,-0.0349452761023764,
0.0715352481429339));
#95325=CARTESIAN_POINT('Ctrl Pts',(0.0133421830384254,-0.0346444289983474,
0.0717320633553387));
#95326=CARTESIAN_POINT('Ctrl Pts',(0.0133775682100256,-0.0345231616327823,
0.0718135468651221));
#95327=CARTESIAN_POINT('Ctrl Pts',(0.0134097729270268,-0.0344132092796976,
0.0718859629086258));
#95328=CARTESIAN_POINT('Ctrl Pts',(0.0134404781136738,-0.0343032738558974,
0.071959041344963));
#95329=CARTESIAN_POINT('Ctrl Pts',(0.0134696468312344,-0.0341934961088741,
0.0720326875445818));
#95330=CARTESIAN_POINT('Ctrl Pts',(0.0134204868366391,-0.0345231616327823,
0.0717086701392579));
#95331=CARTESIAN_POINT('Ctrl Pts',(0.0134541371316517,-0.0344132092796976,
0.0717816777556049));
#95332=CARTESIAN_POINT('Ctrl Pts',(0.0134862755855073,-0.0343032738558974,
0.0718553776349038));
#95333=CARTESIAN_POINT('Ctrl Pts',(0.0135168634436862,-0.0341934961088741,
0.0719296743044281));
#95334=CARTESIAN_POINT('Ctrl Pts',(0.0134634054632526,-0.0345231616327823,
0.0716037934133937));
#95335=CARTESIAN_POINT('Ctrl Pts',(0.0134985013362766,-0.0344132092796976,
0.0716773926025839));
#95336=CARTESIAN_POINT('Ctrl Pts',(0.0135320730573408,-0.0343032738558974,
0.0717517139248446));
#95337=CARTESIAN_POINT('Ctrl Pts',(0.013564080056138,-0.0341934961088741,
0.0718266610642744));
#95338=CARTESIAN_POINT('Ctrl Pts',(0.0135063240898661,-0.0345231616327823,
0.0714989166875295));
#95339=CARTESIAN_POINT('Ctrl Pts',(0.0135428655409015,-0.0344132092796976,
0.071573107449563));
#95340=CARTESIAN_POINT('Ctrl Pts',(0.0135778705291742,-0.0343032738558974,
0.0716480502147854));
#95341=CARTESIAN_POINT('Ctrl Pts',(0.0136112966685897,-0.0341934961088741,
0.0717236478241207));
#95342=CARTESIAN_POINT('Origin',(-0.00195068449090722,-0.0345625596231814,
0.0786931745126852));
#95343=CARTESIAN_POINT('Ctrl Pts',(0.0137438958601374,-0.0346945769586885,
0.0720489711163765));
#95344=CARTESIAN_POINT('Ctrl Pts',(0.0137728491000978,-0.034584662917669,
0.0721264191233387));
#95345=CARTESIAN_POINT('Ctrl Pts',(0.0138002056923659,-0.0344746925051587,
0.0722044790997225));
#95346=CARTESIAN_POINT('Ctrl Pts',(0.0138259309975891,-0.0343648066255171,
0.0722830508813294));
#95347=CARTESIAN_POINT('Ctrl Pts',(0.0136381211974047,-0.0346945769586885,
0.0720083159530333));
#95348=CARTESIAN_POINT('Ctrl Pts',(0.0136676346860648,-0.034584662917669,
0.0720843063316803));
#95349=CARTESIAN_POINT('Ctrl Pts',(0.0136955817658793,-0.0344746925051587,
0.0721609200164953));
#95350=CARTESIAN_POINT('Ctrl Pts',(0.0137219270332417,-0.0343648066255171,
0.0722380586933108));
#95351=CARTESIAN_POINT('Ctrl Pts',(0.0135323465346721,-0.0346945769586885,
0.07196766078969));
#95352=CARTESIAN_POINT('Ctrl Pts',(0.0135624202720318,-0.034584662917669,
0.0720421935400218));
#95353=CARTESIAN_POINT('Ctrl Pts',(0.0135909578393927,-0.0344746925051587,
0.0721173609332682));
#95354=CARTESIAN_POINT('Ctrl Pts',(0.0136179230688944,-0.0343648066255171,
0.0721930665052923));
#95355=CARTESIAN_POINT('Ctrl Pts',(0.0134265718719395,-0.0346945769586885,
0.0719270056263468));
#95356=CARTESIAN_POINT('Ctrl Pts',(0.0134572058579988,-0.034584662917669,
0.0720000807483634));
#95357=CARTESIAN_POINT('Ctrl Pts',(0.0134863339129061,-0.0344746925051587,
0.072073801850041));
#95358=CARTESIAN_POINT('Ctrl Pts',(0.013513919104547,-0.0343648066255171,
0.0721480743172738));
#95359=CARTESIAN_POINT('Origin',(-0.00214909782709286,-0.0345626446731185,
0.0782551969665255));
#95360=CARTESIAN_POINT('Ctrl Pts',(0.0134284645353448,-0.0346945769586885,
0.071927733083546));
#95361=CARTESIAN_POINT('Ctrl Pts',(0.0134750108056564,-0.034527515336289,
0.0720388417790813));
#95362=CARTESIAN_POINT('Ctrl Pts',(0.0135180748490115,-0.0343603235965158,
0.0721514430503747));
#95363=CARTESIAN_POINT('Ctrl Pts',(0.0135575342506988,-0.034193496108874,
0.072265201979884));
#95364=CARTESIAN_POINT('Ctrl Pts',(0.013394399305138,-0.0346945769586885,
0.0718511328980226));
#95365=CARTESIAN_POINT('Ctrl Pts',(0.0134425499970044,-0.034527515336289,
0.0719615280836723));
#95366=CARTESIAN_POINT('Ctrl Pts',(0.013487241316129,-0.0343603235965158,
0.0720734661181109));
#95367=CARTESIAN_POINT('Ctrl Pts',(0.0135283460058874,-0.034193496108874,
0.0721866139738265));
#95368=CARTESIAN_POINT('Ctrl Pts',(0.0133603340749312,-0.0346945769586885,
0.0717745327124992));
#95369=CARTESIAN_POINT('Ctrl Pts',(0.0134100891883523,-0.034527515336289,
0.0718842143882632));
#95370=CARTESIAN_POINT('Ctrl Pts',(0.0134564077832466,-0.0343603235965158,
0.0719954891858471));
#95371=CARTESIAN_POINT('Ctrl Pts',(0.013499157761076,-0.034193496108874,
0.0721080259677689));
#95372=CARTESIAN_POINT('Ctrl Pts',(0.0133262688447244,-0.0346945769586885,
0.0716979325269758));
#95373=CARTESIAN_POINT('Ctrl Pts',(0.0133776283797003,-0.034527515336289,
0.0718069006928541));
#95374=CARTESIAN_POINT('Ctrl Pts',(0.0134255742503641,-0.0343603235965158,
0.0719175122535833));
#95375=CARTESIAN_POINT('Ctrl Pts',(0.0134699695162646,-0.034193496108874,
0.0720294379617114));
#95376=CARTESIAN_POINT('Ctrl Pts',(0.0135139075963689,-0.0340223579322365,
0.0721480449312474));
#95377=CARTESIAN_POINT('Ctrl Pts',(0.0135415197780848,-0.0339125849573554,
0.0722223888185949));
#95378=CARTESIAN_POINT('Ctrl Pts',(0.0135675738113235,-0.0338030433565221,
0.0722972519733532));
#95379=CARTESIAN_POINT('Ctrl Pts',(0.0135920448640821,-0.0336938721132328,
0.0723725357046022));
#95380=CARTESIAN_POINT('Ctrl Pts',(0.0135633268647013,-0.0340223579322365,
0.0720460698570982));
#95381=CARTESIAN_POINT('Ctrl Pts',(0.0135923455486518,-0.0339125849573554,
0.0721210953650469));
#95382=CARTESIAN_POINT('Ctrl Pts',(0.0136197909878298,-0.0338030433565221,
0.0721966687727674));
#95383=CARTESIAN_POINT('Ctrl Pts',(0.013645636651375,-0.0336938721132328,
0.072272690323312));
#95384=CARTESIAN_POINT('Ctrl Pts',(0.0136127461330337,-0.0340223579322365,
0.0719440947829491));
#95385=CARTESIAN_POINT('Ctrl Pts',(0.0136431713192189,-0.0339125849573554,
0.0720198019114989));
#95386=CARTESIAN_POINT('Ctrl Pts',(0.0136720081643361,-0.0338030433565221,
0.0720960855721816));
#95387=CARTESIAN_POINT('Ctrl Pts',(0.013699228438668,-0.0336938721132328,
0.0721728449420217));
#95388=CARTESIAN_POINT('Ctrl Pts',(0.0136621654013662,-0.0340223579322365,
0.0718421197087999));
#95389=CARTESIAN_POINT('Ctrl Pts',(0.013693997089786,-0.0339125849573554,
0.0719185084579508));
#95390=CARTESIAN_POINT('Ctrl Pts',(0.0137242253408424,-0.0338030433565221,
0.0719955023715958));
#95391=CARTESIAN_POINT('Ctrl Pts',(0.0137528202259609,-0.0336938721132328,
0.0720729995607315));
#95392=CARTESIAN_POINT('Origin',(-0.00184005217284519,-0.0345589643414554,
0.0786461280643633));
#95393=CARTESIAN_POINT('Ctrl Pts',(0.0138647305447576,-0.034193496108874,
0.0724060068739107));
#95394=CARTESIAN_POINT('Ctrl Pts',(0.0138887791772146,-0.0340836138581107,
0.0724851711520253));
#95395=CARTESIAN_POINT('Ctrl Pts',(0.0139111781320594,-0.0339738896643499,
0.0725647950816189));
#95396=CARTESIAN_POINT('Ctrl Pts',(0.0139319055728418,-0.0338644633294062,
0.0726447748321448));
#95397=CARTESIAN_POINT('Ctrl Pts',(0.0137617172119098,-0.034193496108874,
0.0723587902189722));
#95398=CARTESIAN_POINT('Ctrl Pts',(0.0137864169340779,-0.0340836138581107,
0.0724365340042289));
#95399=CARTESIAN_POINT('Ctrl Pts',(0.0138094960603477,-0.0339738896643499,
0.0725147515954792));
#95400=CARTESIAN_POINT('Ctrl Pts',(0.0138309317630749,-0.0338644633294062,
0.0725933409037595));
#95401=CARTESIAN_POINT('Ctrl Pts',(0.0136587038790621,-0.034193496108874,
0.0723115735640337));
#95402=CARTESIAN_POINT('Ctrl Pts',(0.0136840546909412,-0.0340836138581107,
0.0723878968564325));
#95403=CARTESIAN_POINT('Ctrl Pts',(0.013707813988636,-0.0339738896643499,
0.0724647081093394));
#95404=CARTESIAN_POINT('Ctrl Pts',(0.0137299579533081,-0.0338644633294062,
0.0725419069753741));
#95405=CARTESIAN_POINT('Ctrl Pts',(0.0135556905462144,-0.034193496108874,
0.0722643569090952));
#95406=CARTESIAN_POINT('Ctrl Pts',(0.0135816924478045,-0.0340836138581107,
0.0723392597086361));
#95407=CARTESIAN_POINT('Ctrl Pts',(0.0136061319169243,-0.0339738896643499,
0.0724146646231997));
#95408=CARTESIAN_POINT('Ctrl Pts',(0.0136289841435412,-0.0338644633294062,
0.0724904730469888));
#95409=CARTESIAN_POINT('Origin',(-0.00207878075995784,-0.0345610621865069,
0.0782283258709278));
#95410=CARTESIAN_POINT('Ctrl Pts',(0.0135455709476501,-0.03424362768739,
0.0722310597452954));
#95411=CARTESIAN_POINT('Ctrl Pts',(0.0136179449724558,-0.033943005420186,
0.0724355458791655));
#95412=CARTESIAN_POINT('Ctrl Pts',(0.0136747106567857,-0.0336441434784162,
0.0726449025974582));
#95413=CARTESIAN_POINT('Ctrl Pts',(0.0134570560298694,-0.03424362768739,
0.0719972540367888));
#95414=CARTESIAN_POINT('Ctrl Pts',(0.0135382481823398,-0.033943005420186,
0.0721984017755008));
#95415=CARTESIAN_POINT('Ctrl Pts',(0.0136040584045603,-0.0336441434784162,
0.0724050938001729));
#95416=CARTESIAN_POINT('Ctrl Pts',(0.0136289760186054,-0.0335235895815127,
0.0724904465325943));
#95417=CARTESIAN_POINT('Ctrl Pts',(0.013651823039444,-0.0334144449262719,
0.0725662363643304));
#95418=CARTESIAN_POINT('Ctrl Pts',(0.0136731305478561,-0.0333049234473133,
0.0726425852716573));
#95419=CARTESIAN_POINT('Ctrl Pts',(0.0136928624546213,-0.0331951640388588,
0.0727193980958017));
#95420=CARTESIAN_POINT('Ctrl Pts',(0.013684700866248,-0.0335235895815127,
0.0723917757981214));
#95421=CARTESIAN_POINT('Ctrl Pts',(0.0137089062840114,-0.0334144449262719,
0.0724683327920974));
#95422=CARTESIAN_POINT('Ctrl Pts',(0.0137315579009873,-0.0333049234473133,
0.0725454778064989));
#95423=CARTESIAN_POINT('Ctrl Pts',(0.0137526178170403,-0.0331951640388588,
0.0726231148202633));
#95424=CARTESIAN_POINT('Ctrl Pts',(0.0137404257138906,-0.0335235895815127,
0.0722931050636484));
#95425=CARTESIAN_POINT('Ctrl Pts',(0.0137659895285788,-0.0334144449262719,
0.0723704292198644));
#95426=CARTESIAN_POINT('Ctrl Pts',(0.0137899852541185,-0.0333049234473133,
0.0724483703413403));
#95427=CARTESIAN_POINT('Ctrl Pts',(0.0138123731794593,-0.0331951640388588,
0.0725268315447249));
#95428=CARTESIAN_POINT('Ctrl Pts',(0.0137961505615332,-0.0335235895815127,
0.0721944343291755));
#95429=CARTESIAN_POINT('Ctrl Pts',(0.0138230727731462,-0.0334144449262719,
0.0722725256476314));
#95430=CARTESIAN_POINT('Ctrl Pts',(0.0138484126072496,-0.0333049234473133,
0.0723512628761819));
#95431=CARTESIAN_POINT('Ctrl Pts',(0.0138721285418783,-0.0331951640388588,
0.0724305482691866));
#95432=CARTESIAN_POINT('Origin',(-0.00262261164918678,-0.0326434571770125,
0.0761247095113126));
#95433=CARTESIAN_POINT('Ctrl Pts',(0.0139646948224223,-0.0336938721132388,
0.0727708842719304));
#95434=CARTESIAN_POINT('Ctrl Pts',(0.0139727672444178,-0.0336474569764957,
0.07280507307177));
#95435=CARTESIAN_POINT('Ctrl Pts',(0.013980438890217,-0.033601104548885,
0.0728393540268629));
#95436=CARTESIAN_POINT('Ctrl Pts',(0.0139998617318712,-0.0334837508694609,
0.0729261455159323));
#95437=CARTESIAN_POINT('Ctrl Pts',(0.0140167042329001,-0.0333660264863603,
0.073013474431601));
#95438=CARTESIAN_POINT('Ctrl Pts',(0.0136651594291254,-0.0336938721132388,
0.0726101093129208));
#95439=CARTESIAN_POINT('Ctrl Pts',(0.0136741729203068,-0.0336474569764957,
0.072642544832707));
#95440=CARTESIAN_POINT('Ctrl Pts',(0.0136828060951659,-0.033601104548885,
0.0726750836442855));
#95441=CARTESIAN_POINT('Ctrl Pts',(0.013704663307119,-0.0334837508694609,
0.0727574644269033));
#95442=CARTESIAN_POINT('Ctrl Pts',(0.0137240698078166,-0.0333660264863603,
0.0728404567084104));
#95443=CARTESIAN_POINT('Ctrl Pts',(0.0136651594291366,-0.0336938721132427,
0.0726101093129352));
#95444=CARTESIAN_POINT('Ctrl Pts',(0.0136741729203174,-0.0336474569765026,
0.0726425448327193));
#95445=CARTESIAN_POINT('Ctrl Pts',(0.0136828060951759,-0.0336011045488949,
0.0726750836442955));
#95446=CARTESIAN_POINT('Ctrl Pts',(0.0137044812663218,-0.033484728265791,
0.0727567783071924));
#95447=CARTESIAN_POINT('Ctrl Pts',(0.0137237464482251,-0.0333679870047996,
0.0728390746239767));
#95448=CARTESIAN_POINT('Ctrl Pts',(0.0136651594291247,-0.0336938721132428,
0.0726101093129181));
#95449=CARTESIAN_POINT('Ctrl Pts',(0.0136973956624559,-0.0335278710435084,
0.072726113085819));
#95450=CARTESIAN_POINT('Ctrl Pts',(0.0137259827069975,-0.033362046922432,
0.072843086968758));
#95451=CARTESIAN_POINT('Ctrl Pts',(0.0137509153232181,-0.0331951640388601,
0.072961093890998));
#95452=CARTESIAN_POINT('Ctrl Pts',(0.0136409633598077,-0.0336938721132428,
0.072529843628763));
#95453=CARTESIAN_POINT('Ctrl Pts',(0.0136748798833989,-0.0335278710435084,
0.0726453408786083));
#95454=CARTESIAN_POINT('Ctrl Pts',(0.0137051625115095,-0.033362046922432,
0.072761861110151));
#95455=CARTESIAN_POINT('Ctrl Pts',(0.0137318069233254,-0.0331951640388601,
0.0728794673090727));
#95456=CARTESIAN_POINT('Ctrl Pts',(0.0136167672904907,-0.0336938721132428,
0.0724495779446079));
#95457=CARTESIAN_POINT('Ctrl Pts',(0.0136523641043418,-0.0335278710435084,
0.0725645686713976));
#95458=CARTESIAN_POINT('Ctrl Pts',(0.0136843423160216,-0.033362046922432,
0.0726806352515439));
#95459=CARTESIAN_POINT('Ctrl Pts',(0.0137126985234327,-0.0331951640388601,
0.0727978407271474));
#95460=CARTESIAN_POINT('Ctrl Pts',(0.0135925712211737,-0.0336938721132428,
0.0723693122604529));
#95461=CARTESIAN_POINT('Ctrl Pts',(0.0136298483252848,-0.0335278710435084,
0.0724837964641869));
#95462=CARTESIAN_POINT('Ctrl Pts',(0.0136635221205336,-0.033362046922432,
0.0725994093929369));
#95463=CARTESIAN_POINT('Ctrl Pts',(0.01369359012354,-0.0331951640388601,
0.072716214145222));
#95464=CARTESIAN_POINT('Ctrl Pts',(0.0137223170541567,-0.0330240426238156,
0.0728393939609575));
#95465=CARTESIAN_POINT('Ctrl Pts',(0.013740371929206,-0.0329142774063509,
0.0729165192330562));
#95466=CARTESIAN_POINT('Ctrl Pts',(0.0137568414104559,-0.0328043479726686,
0.072994056199617));
#95467=CARTESIAN_POINT('Ctrl Pts',(0.0137717016637264,-0.0326943950436594,
0.0730719061110635));
#95468=CARTESIAN_POINT('Ctrl Pts',(0.0137841274251584,-0.0330240426238156,
0.072744417047862));
#95469=CARTESIAN_POINT('Ctrl Pts',(0.0138034906997171,-0.0329142774063509,
0.0728223938180403));
#95470=CARTESIAN_POINT('Ctrl Pts',(0.0138212516299175,-0.0328043479726686,
0.0729008097554561));
#95471=CARTESIAN_POINT('Ctrl Pts',(0.0138373846961265,-0.0326943950436594,
0.072979565030069));
#95472=CARTESIAN_POINT('Ctrl Pts',(0.0138459377961602,-0.0330240426238156,
0.0726494401347666));
#95473=CARTESIAN_POINT('Ctrl Pts',(0.0138666094702283,-0.0329142774063509,
0.0727282684030243));
#95474=CARTESIAN_POINT('Ctrl Pts',(0.0138856618493791,-0.0328043479726686,
0.0728075633112951));
#95475=CARTESIAN_POINT('Ctrl Pts',(0.0139030677285267,-0.0326943950436594,
0.0728872239490745));
#95476=CARTESIAN_POINT('Ctrl Pts',(0.0139077481671619,-0.0330240426238156,
0.0725544632216711));
#95477=CARTESIAN_POINT('Ctrl Pts',(0.0139297282407395,-0.0329142774063509,
0.0726341429880084));
#95478=CARTESIAN_POINT('Ctrl Pts',(0.0139500720688406,-0.0328043479726686,
0.0727143168671342));
#95479=CARTESIAN_POINT('Ctrl Pts',(0.0139687507609269,-0.0326943950436594,
0.07279488286808));
#95480=CARTESIAN_POINT('Origin',(-0.00274371983696767,-0.0326396682861129,
0.0761497735418175));
#95481=CARTESIAN_POINT('Ctrl Pts',(0.0140380417500741,-0.0331951640388588,
0.0731392904012537));
#95482=CARTESIAN_POINT('Ctrl Pts',(0.0140519622301479,-0.0330855618255041,
0.0732207473622013));
#95483=CARTESIAN_POINT('Ctrl Pts',(0.0140642091691572,-0.0329757224427708,
0.0733025507568613));
#95484=CARTESIAN_POINT('Ctrl Pts',(0.0140747617457512,-0.0328657862078596,
0.0733845966003569));
#95485=CARTESIAN_POINT('Ctrl Pts',(0.013941758551186,-0.0331951640388588,
0.0730795350864055));
#95486=CARTESIAN_POINT('Ctrl Pts',(0.0139565020398379,-0.0330855618255041,
0.0731596659410677));
#95487=CARTESIAN_POINT('Ctrl Pts',(0.0139695999890708,-0.0329757224427708,
0.0732401592836514));
#95488=CARTESIAN_POINT('Ctrl Pts',(0.0139810305700538,-0.0328657862078596,
0.0733209128603354));
#95489=CARTESIAN_POINT('Ctrl Pts',(0.013845475352298,-0.0331951640388588,
0.0730197797715573));
#95490=CARTESIAN_POINT('Ctrl Pts',(0.0138610418495279,-0.0330855618255041,
0.0730985845199341));
#95491=CARTESIAN_POINT('Ctrl Pts',(0.0138749908089843,-0.0329757224427708,
0.0731777678104415));
#95492=CARTESIAN_POINT('Ctrl Pts',(0.0138872993943565,-0.0328657862078596,
0.073257229120314));
#95493=CARTESIAN_POINT('Ctrl Pts',(0.0137491921534099,-0.0331951640388588,
0.072960024456709));
#95494=CARTESIAN_POINT('Ctrl Pts',(0.0137655816592178,-0.0330855618255041,
0.0730375030988005));
#95495=CARTESIAN_POINT('Ctrl Pts',(0.0137803816288978,-0.0329757224427708,
0.0731153763372315));
#95496=CARTESIAN_POINT('Ctrl Pts',(0.0137935682186592,-0.0328657862078596,
0.0731935453802926));
#95497=CARTESIAN_POINT('Origin',(-0.00279255920260905,-0.0326401908835072,
0.0756713515645391));
#95498=CARTESIAN_POINT('Ctrl Pts',(0.0137433409369527,-0.0332451089994432,
0.0729257922870346));
#95499=CARTESIAN_POINT('Ctrl Pts',(0.0137895126862565,-0.0329451141710257,
0.0731377374126622));
#95500=CARTESIAN_POINT('Ctrl Pts',(0.0138195886931928,-0.0326442513127503,
0.0733525582694659));
#95501=CARTESIAN_POINT('Ctrl Pts',(0.0136848306738065,-0.0332451089994432,
0.0726827356082403));
#95502=CARTESIAN_POINT('Ctrl Pts',(0.0137401694557315,-0.0329451141710257,
0.0728924739831889));
#95503=CARTESIAN_POINT('Ctrl Pts',(0.0137795526741993,-0.0326442513127503,
0.0731057848568316));
#95504=CARTESIAN_POINT('Ctrl Pts',(0.0137935630527179,-0.0325229783203385,
0.0731935142179197));
#95505=CARTESIAN_POINT('Ctrl Pts',(0.0138067481880669,-0.032413025311208,
0.0732716720216568));
#95506=CARTESIAN_POINT('Ctrl Pts',(0.0138183145290902,-0.0323031222247695,
0.0733500907226891));
#95507=CARTESIAN_POINT('Ctrl Pts',(0.0138282508046342,-0.0321934096636184,
0.0734286693494433));
#95508=CARTESIAN_POINT('Ctrl Pts',(0.0138612151077861,-0.0325229783203385,
0.0731026057909487));
#95509=CARTESIAN_POINT('Ctrl Pts',(0.0138756534137901,-0.032413025311208,
0.0731816961767686));
#95510=CARTESIAN_POINT('Ctrl Pts',(0.0138884534437424,-0.0323031222247695,
0.0732610732418835));
#95511=CARTESIAN_POINT('Ctrl Pts',(0.0138996023895397,-0.0321934096636184,
0.0733406347313618));
#95512=CARTESIAN_POINT('Ctrl Pts',(0.0139288671628544,-0.0325229783203385,
0.0730116973639778));
#95513=CARTESIAN_POINT('Ctrl Pts',(0.0139445586395133,-0.032413025311208,
0.0730917203318803));
#95514=CARTESIAN_POINT('Ctrl Pts',(0.0139585923583947,-0.0323031222247695,
0.073172055761078));
#95515=CARTESIAN_POINT('Ctrl Pts',(0.0139709539744452,-0.0321934096636184,
0.0732526001132802));
#95516=CARTESIAN_POINT('Ctrl Pts',(0.0139965192179226,-0.0325229783203385,
0.0729207889370068));
#95517=CARTESIAN_POINT('Ctrl Pts',(0.0140134638652365,-0.032413025311208,
0.0730017444869921));
#95518=CARTESIAN_POINT('Ctrl Pts',(0.0140287312730469,-0.0323031222247695,
0.0730830382802724));
#95519=CARTESIAN_POINT('Ctrl Pts',(0.0140423055593507,-0.0321934096636184,
0.0731645654951987));
#95520=CARTESIAN_POINT('Origin',(-0.00273529484821876,-0.0326393375179589,
0.076148465647772));
#95521=CARTESIAN_POINT('Ctrl Pts',(0.0140898342906189,-0.0326943950436593,
0.0735126442359838));
#95522=CARTESIAN_POINT('Ctrl Pts',(0.014098618247579,-0.0325844576448127,
0.0735948676154605));
#95523=CARTESIAN_POINT('Ctrl Pts',(0.0141057023118987,-0.0324744968375319,
0.0736772784806451));
#95524=CARTESIAN_POINT('Ctrl Pts',(0.0141110788634599,-0.0323646534831894,
0.0737597711167384));
#95525=CARTESIAN_POINT('Ctrl Pts',(0.0139974932398338,-0.0326943950436593,
0.0734469612250719));
#95526=CARTESIAN_POINT('Ctrl Pts',(0.0140071824317874,-0.0325844576448127,
0.0735279119718032));
#95527=CARTESIAN_POINT('Ctrl Pts',(0.0140151981152972,-0.0324744968375319,
0.07360906883592));
#95528=CARTESIAN_POINT('Ctrl Pts',(0.0140215314544389,-0.0323646534831894,
0.0736903276928586));
#95529=CARTESIAN_POINT('Ctrl Pts',(0.0139051521890488,-0.0326943950436593,
0.07338127821416));
#95530=CARTESIAN_POINT('Ctrl Pts',(0.0139157466159958,-0.0325844576448127,
0.0734609563281459));
#95531=CARTESIAN_POINT('Ctrl Pts',(0.0139246939186956,-0.0324744968375319,
0.0735408591911949));
#95532=CARTESIAN_POINT('Ctrl Pts',(0.0139319840454179,-0.0323646534831894,
0.0736208842689787));
#95533=CARTESIAN_POINT('Ctrl Pts',(0.0138128111382638,-0.0326943950436593,
0.0733155952032481));
#95534=CARTESIAN_POINT('Ctrl Pts',(0.0138243108002043,-0.0325844576448127,
0.0733940006844886));
#95535=CARTESIAN_POINT('Ctrl Pts',(0.0138341897220941,-0.0324744968375319,
0.0734726495464699));
#95536=CARTESIAN_POINT('Ctrl Pts',(0.0138424366363968,-0.0323646534831894,
0.0735514408450988));
#95537=CARTESIAN_POINT('Origin',(-0.00282997230623912,-0.0326395579068746,
0.075677027961926));
#95538=CARTESIAN_POINT('Ctrl Pts',(0.0138091147336051,-0.0327445246961876,
0.0732810242212984));
#95539=CARTESIAN_POINT('Ctrl Pts',(0.0138418886905391,-0.0324436878365474,
0.0734954500412169));
#95540=CARTESIAN_POINT('Ctrl Pts',(0.0138584181111671,-0.0321434074463185,
0.0737117353683997));
#95541=CARTESIAN_POINT('Ctrl Pts',(0.0137659799028439,-0.0327445246961876,
0.0730347735636847));
#95542=CARTESIAN_POINT('Ctrl Pts',(0.013808041355063,-0.0324436878365474,
0.0732475725268825));
#95543=CARTESIAN_POINT('Ctrl Pts',(0.0138339544276795,-0.0321434074463185,
0.0734629351911686));
#95544=CARTESIAN_POINT('Ctrl Pts',(0.0138529529799322,-0.0322357242816071,
0.0736452950412317));
#95545=CARTESIAN_POINT('Ctrl Pts',(0.0138690271782907,-0.0319819883628704,
0.0738277617003296));
#95546=CARTESIAN_POINT('Ctrl Pts',(0.0138734579247823,-0.0317295851069886,
0.0740108814153272));
#95547=CARTESIAN_POINT('Ctrl Pts',(0.0138256071141881,-0.0322357242816071,
0.0733967951345381));
#95548=CARTESIAN_POINT('Ctrl Pts',(0.0138495957122821,-0.0319819883628704,
0.0735783908632785));
#95549=CARTESIAN_POINT('Ctrl Pts',(0.0138619802387864,-0.0317295851069886,
0.0737611450288631));
#95550=CARTESIAN_POINT('Origin',(-0.00273536322915428,-0.0326371942643931,
0.0756655594808861));
#95551=CARTESIAN_POINT('Origin',(-0.00261409391399649,-0.0326352985534603,
0.0761291230395348));
#95552=CARTESIAN_POINT('Ctrl Pts',(0.0141180815491696,-0.0321934096636184,
0.0738885134227378));
#95553=CARTESIAN_POINT('Ctrl Pts',(0.0141216876528603,-0.0320835708272304,
0.0739711794825305));
#95554=CARTESIAN_POINT('Ctrl Pts',(0.0141235808950535,-0.0319739230346346,
0.0740538722207776));
#95555=CARTESIAN_POINT('Ctrl Pts',(0.0141237669733025,-0.0318646057455575,
0.0741364856519547));
#95556=CARTESIAN_POINT('Ctrl Pts',(0.014030046855276,-0.0321934096636184,
0.073817161776387));
#95557=CARTESIAN_POINT('Ctrl Pts',(0.0140346369537779,-0.0320835708272304,
0.0738986137691409));
#95558=CARTESIAN_POINT('Ctrl Pts',(0.0140375387450797,-0.0319739230346346,
0.0739801135082788));
#95559=CARTESIAN_POINT('Ctrl Pts',(0.0140387565192221,-0.0318646057455575,
0.0740615564356039));
#95560=CARTESIAN_POINT('Ctrl Pts',(0.0139420121613824,-0.0321934096636184,
0.0737458101300362));
#95561=CARTESIAN_POINT('Ctrl Pts',(0.0139475862546956,-0.0320835708272304,
0.0738260480557513));
#95562=CARTESIAN_POINT('Ctrl Pts',(0.0139514965951059,-0.0319739230346346,
0.07390635479578));
#95563=CARTESIAN_POINT('Ctrl Pts',(0.0139537460651417,-0.0318646057455575,
0.073986627219253));
#95564=CARTESIAN_POINT('Ctrl Pts',(0.0138539774674888,-0.0321934096636184,
0.0736744584836855));
#95565=CARTESIAN_POINT('Ctrl Pts',(0.0138605355556133,-0.0320835708272304,
0.0737534823423617));
#95566=CARTESIAN_POINT('Ctrl Pts',(0.0138654544451321,-0.0319739230346346,
0.0738325960832812));
#95567=CARTESIAN_POINT('Ctrl Pts',(0.0138687356110613,-0.0318646057455575,
0.0739116980029022));
#95568=CARTESIAN_POINT('Ctrl Pts',(0.0138432106628924,-0.0320218834582284,
0.0735508875068933));
#95569=CARTESIAN_POINT('Ctrl Pts',(0.0138494459756004,-0.0319391099350596,
0.0736104129306331));
#95570=CARTESIAN_POINT('Ctrl Pts',(0.0138547480126527,-0.0318564869454893,
0.0736699996547131));
#95571=CARTESIAN_POINT('Ctrl Pts',(0.0138591169640053,-0.0317740741446501,
0.0737296039175802));
#95572=CARTESIAN_POINT('Ctrl Pts',(0.013875242868543,-0.0320218834582284,
0.0735130620412803));
#95573=CARTESIAN_POINT('Ctrl Pts',(0.0138818718529055,-0.0319391099350596,
0.0735729208428435));
#95574=CARTESIAN_POINT('Ctrl Pts',(0.0138875621173552,-0.0318564869454893,
0.0736328468899999));
#95575=CARTESIAN_POINT('Ctrl Pts',(0.0138923135921493,-0.0317740741446501,
0.0736927961476457));
#95576=CARTESIAN_POINT('Ctrl Pts',(0.0139072750741935,-0.0320218834582284,
0.0734752365756672));
#95577=CARTESIAN_POINT('Ctrl Pts',(0.0139142977302106,-0.0319391099350596,
0.0735354287550539));
#95578=CARTESIAN_POINT('Ctrl Pts',(0.0139203762220577,-0.0318564869454893,
0.0735956941252867));
#95579=CARTESIAN_POINT('Ctrl Pts',(0.0139255102202933,-0.0317740741446501,
0.0736559883777112));
#95580=CARTESIAN_POINT('Ctrl Pts',(0.0139393072798441,-0.0320218834582284,
0.0734374111100542));
#95581=CARTESIAN_POINT('Ctrl Pts',(0.0139467236075157,-0.0319391099350596,
0.0734979366672643));
#95582=CARTESIAN_POINT('Ctrl Pts',(0.0139531903267603,-0.0318564869454893,
0.0735585413605735));
#95583=CARTESIAN_POINT('Ctrl Pts',(0.0139587068484374,-0.0317740741446501,
0.0736191806077768));
#95584=CARTESIAN_POINT('Origin',(0.0200014606049758,-0.0391228853390726,
0.0719587962499599));
#95585=CARTESIAN_POINT('Ctrl Pts',(0.0127425736898337,-0.0352722978779547,
0.0707220370987458));
#95586=CARTESIAN_POINT('Ctrl Pts',(0.0127535526239773,-0.0352466642097185,
0.070737417465551));
#95587=CARTESIAN_POINT('Ctrl Pts',(0.0127645855884823,-0.0352210183808286,
0.0707527385799157));
#95588=CARTESIAN_POINT('Ctrl Pts',(0.0127756734048254,-0.0351953608940152,
0.0707680006713182));
#95589=CARTESIAN_POINT('Origin',(0.0168332315020225,-0.0352456003065004,
0.0680245823990329));
#95590=CARTESIAN_POINT('Ctrl Pts',(0.0128467020659647,-0.035024121149334,
0.0708704713730577));
#95591=CARTESIAN_POINT('Ctrl Pts',(0.0128918762261048,-0.0349144232867421,
0.0709355276549003));
#95592=CARTESIAN_POINT('Ctrl Pts',(0.0129357326653843,-0.0348045283677512,
0.0710015566581894));
#95593=CARTESIAN_POINT('Ctrl Pts',(0.0129782120620591,-0.0346945769586886,
0.0710684758985538));
#95594=CARTESIAN_POINT('Ctrl Pts',(0.0128692085696925,-0.035024121149334,
0.070759410132776));
#95595=CARTESIAN_POINT('Ctrl Pts',(0.0129159125528116,-0.0349144232867421,
0.0708247764324656));
#95596=CARTESIAN_POINT('Ctrl Pts',(0.0129612933224528,-0.0348045283677512,
0.0708911472616948));
#95597=CARTESIAN_POINT('Ctrl Pts',(0.0130052895881056,-0.0346945769586886,
0.0709584397709131));
#95598=CARTESIAN_POINT('Ctrl Pts',(0.0128917150734203,-0.035024121149334,
0.0706483488924945));
#95599=CARTESIAN_POINT('Ctrl Pts',(0.0129399488795185,-0.0349144232867421,
0.0707140252100308));
#95600=CARTESIAN_POINT('Ctrl Pts',(0.0129868539795212,-0.0348045283677512,
0.0707807378652002));
#95601=CARTESIAN_POINT('Ctrl Pts',(0.0130323671141522,-0.0346945769586886,
0.0708484036432725));
#95602=CARTESIAN_POINT('Ctrl Pts',(0.0129142215771481,-0.035024121149334,
0.0705372876522129));
#95603=CARTESIAN_POINT('Ctrl Pts',(0.0129639852062253,-0.0349144232867421,
0.0706032739875961));
#95604=CARTESIAN_POINT('Ctrl Pts',(0.0130124146365897,-0.0348045283677512,
0.0706703284687056));
#95605=CARTESIAN_POINT('Ctrl Pts',(0.0130594446401987,-0.0346945769586886,
0.0707383675156319));
#95606=CARTESIAN_POINT('Origin',(-0.00129164342851129,-0.0345629067944392,
0.0799134842847298));
#95607=CARTESIAN_POINT('Ctrl Pts',(0.0131586294551069,-0.0351970973651647,
0.0710153812312143));
#95608=CARTESIAN_POINT('Ctrl Pts',(0.0132020553499877,-0.0350869349321812,
0.0710851322166028));
#95609=CARTESIAN_POINT('Ctrl Pts',(0.013244067134042,-0.034976498512977,
0.0711558437831852));
#95610=CARTESIAN_POINT('Ctrl Pts',(0.0132846049871334,-0.0348659306849697,
0.0712274275259713));
#95611=CARTESIAN_POINT('Ctrl Pts',(0.0130777095025398,-0.0351970973651647,
0.0710008061865715));
#95612=CARTESIAN_POINT('Ctrl Pts',(0.0131213373149115,-0.0350869349321812,
0.0710694361356832));
#95613=CARTESIAN_POINT('Ctrl Pts',(0.0131635744894457,-0.034976498512977,
0.0711390299350881));
#95614=CARTESIAN_POINT('Ctrl Pts',(0.0132043609992496,-0.0348659306849697,
0.071209500645085));
#95615=CARTESIAN_POINT('Ctrl Pts',(0.0129967895499728,-0.0351970973651647,
0.0709862311419287));
#95616=CARTESIAN_POINT('Ctrl Pts',(0.0130406192798352,-0.0350869349321812,
0.0710537400547635));
#95617=CARTESIAN_POINT('Ctrl Pts',(0.0130830818448493,-0.034976498512977,
0.0711222160869908));
#95618=CARTESIAN_POINT('Ctrl Pts',(0.0131241170113659,-0.0348659306849697,
0.0711915737641986));
#95619=CARTESIAN_POINT('Ctrl Pts',(0.0129158695974057,-0.0351970973651647,
0.0709716560972859));
#95620=CARTESIAN_POINT('Ctrl Pts',(0.0129599012447589,-0.0350869349321812,
0.0710380439738438));
#95621=CARTESIAN_POINT('Ctrl Pts',(0.013002589200253,-0.034976498512977,
0.0711054022388937));
#95622=CARTESIAN_POINT('Ctrl Pts',(0.0130438730234821,-0.0348659306849697,
0.0711736468833122));
#95623=CARTESIAN_POINT('Origin',(-0.00150284199576083,-0.0345637187964519,
0.0794813725838939));
#95624=CARTESIAN_POINT('Ctrl Pts',(0.0128980582211641,-0.0352450361861252,
0.0709430679134204));
#95625=CARTESIAN_POINT('Ctrl Pts',(0.0130190096464181,-0.0349452761023764,
0.0711231326839111));
#95626=CARTESIAN_POINT('Ctrl Pts',(0.0131260542464923,-0.0346444289983474,
0.0713117964653789));
#95627=CARTESIAN_POINT('Ctrl Pts',(0.0127541818375923,-0.0352450361861252,
0.0707386184422782));
#95628=CARTESIAN_POINT('Ctrl Pts',(0.0128828442009826,-0.0349452761023764,
0.0709132568260592));
#95629=CARTESIAN_POINT('Ctrl Pts',(0.0129979865708702,-0.0346444289983474,
0.0710970904560062));
#95630=CARTESIAN_POINT('Ctrl Pts',(0.0130433053115867,-0.0345231616327822,
0.0711734965060001));
#95631=CARTESIAN_POINT('Ctrl Pts',(0.0130843322216695,-0.0344132092796975,
0.0712413052060534));
#95632=CARTESIAN_POINT('Ctrl Pts',(0.0131239544454785,-0.0343032738558974,
0.0713099590167629));
#95633=CARTESIAN_POINT('Ctrl Pts',(0.0131621234753269,-0.0341934961088741,
0.0713793686844099));
#95634=CARTESIAN_POINT('Ctrl Pts',(0.013072740972832,-0.0345231616327822,
0.0710640676341909));
#95635=CARTESIAN_POINT('Ctrl Pts',(0.0131152762058492,-0.0344132092796975,
0.0711322820633924));
#95636=CARTESIAN_POINT('Ctrl Pts',(0.0131563982825826,-0.0343032738558974,
0.0712013727807864));
#95637=CARTESIAN_POINT('Ctrl Pts',(0.0131960567881982,-0.0341934961088741,
0.0712712499237069));
#95638=CARTESIAN_POINT('Ctrl Pts',(0.0131021766340773,-0.0345231616327822,
0.0709546387623816));
#95639=CARTESIAN_POINT('Ctrl Pts',(0.0131462201900288,-0.0344132092796975,
0.0710232589207312));
#95640=CARTESIAN_POINT('Ctrl Pts',(0.0131888421196867,-0.0343032738558974,
0.0710927865448099));
#95641=CARTESIAN_POINT('Ctrl Pts',(0.0132299901010695,-0.0341934961088741,
0.0711631311630038));
#95642=CARTESIAN_POINT('Ctrl Pts',(0.0131316122953226,-0.0345231616327822,
0.0708452098905724));
#95643=CARTESIAN_POINT('Ctrl Pts',(0.0131771641742084,-0.0344132092796975,
0.0709142357780702));
#95644=CARTESIAN_POINT('Ctrl Pts',(0.0132212859567907,-0.0343032738558974,
0.0709842003088334));
#95645=CARTESIAN_POINT('Ctrl Pts',(0.0132639234139408,-0.0341934961088741,
0.0710550124023007));
#95646=CARTESIAN_POINT('Origin',(-0.00130183356012355,-0.0345625596229081,
0.0799200157104307));
#95647=CARTESIAN_POINT('Ctrl Pts',(0.0134362508414286,-0.0346945769586885,
0.0713611513377829));
#95648=CARTESIAN_POINT('Ctrl Pts',(0.0134746825855898,-0.034584662917669,
0.0714343598408911));
#95649=CARTESIAN_POINT('Ctrl Pts',(0.0135116069722089,-0.0344746925051587,
0.0715083756008774));
#95650=CARTESIAN_POINT('Ctrl Pts',(0.0135469770811724,-0.0343648066255171,
0.0715831035848301));
#95651=CARTESIAN_POINT('Ctrl Pts',(0.0133262148004225,-0.0346945769586885,
0.0713340738330552));
#95652=CARTESIAN_POINT('Ctrl Pts',(0.0133650196862848,-0.034584662917669,
0.0714057659839018));
#95653=CARTESIAN_POINT('Ctrl Pts',(0.0134023486358807,-0.0344746925051587,
0.0714782728490469));
#95654=CARTESIAN_POINT('Ctrl Pts',(0.0134381542027392,-0.0343648066255171,
0.0715515013268078));
#95655=CARTESIAN_POINT('Ctrl Pts',(0.0132161787594164,-0.0346945769586885,
0.0713069963283276));
#95656=CARTESIAN_POINT('Ctrl Pts',(0.0132553567869799,-0.034584662917669,
0.0713771721269125));
#95657=CARTESIAN_POINT('Ctrl Pts',(0.0132930902995526,-0.0344746925051587,
0.0714481700972163));
#95658=CARTESIAN_POINT('Ctrl Pts',(0.0133293313243061,-0.0343648066255171,
0.0715198990687856));
#95659=CARTESIAN_POINT('Ctrl Pts',(0.0131061427184102,-0.0346945769586885,
0.0712799188235999));
#95660=CARTESIAN_POINT('Ctrl Pts',(0.013145693887675,-0.034584662917669,
0.0713485782699231));
#95661=CARTESIAN_POINT('Ctrl Pts',(0.0131838319632244,-0.0344746925051587,
0.0714180673453858));
#95662=CARTESIAN_POINT('Ctrl Pts',(0.0132205084458729,-0.0343648066255171,
0.0714882968107634));
#95663=CARTESIAN_POINT('Origin',(-0.00155357548898538,-0.0345626446734559,
0.079510359533461));
#95664=CARTESIAN_POINT('Ctrl Pts',(0.0131081116321624,-0.0346945769586884,
0.0712804033309573));
#95665=CARTESIAN_POINT('Ctrl Pts',(0.0131682164833183,-0.0345275153362889,
0.0713848021066732));
#95666=CARTESIAN_POINT('Ctrl Pts',(0.0132250536352637,-0.0343603235965158,
0.0714911181275061));
#95667=CARTESIAN_POINT('Ctrl Pts',(0.0132784596622649,-0.0341934961088739,
0.0715990344594701));
#95668=CARTESIAN_POINT('Ctrl Pts',(0.0130647144675272,-0.0346945769586884,
0.07120867666623));
#95669=CARTESIAN_POINT('Ctrl Pts',(0.0131263216623937,-0.0345275153362889,
0.0713121664709574));
#95670=CARTESIAN_POINT('Ctrl Pts',(0.0131846901329335,-0.0343603235965158,
0.0714176205330221));
#95671=CARTESIAN_POINT('Ctrl Pts',(0.0132396518865634,-0.0341934961088739,
0.0715247244004177));
#95672=CARTESIAN_POINT('Ctrl Pts',(0.0130213173028921,-0.0346945769586884,
0.0711369500015027));
#95673=CARTESIAN_POINT('Ctrl Pts',(0.0130844268414691,-0.0345275153362889,
0.0712395308352416));
#95674=CARTESIAN_POINT('Ctrl Pts',(0.0131443266306033,-0.0343603235965158,
0.0713441229385381));
#95675=CARTESIAN_POINT('Ctrl Pts',(0.0132008441108619,-0.0341934961088739,
0.0714504143413653));
#95676=CARTESIAN_POINT('Ctrl Pts',(0.012977920138257,-0.0346945769586884,
0.0710652233367754));
#95677=CARTESIAN_POINT('Ctrl Pts',(0.0130425320205444,-0.0345275153362889,
0.0711668951995257));
#95678=CARTESIAN_POINT('Ctrl Pts',(0.0131039631282731,-0.0343603235965158,
0.0712706253440542));
#95679=CARTESIAN_POINT('Ctrl Pts',(0.0131620363351604,-0.0341934961088739,
0.0713761042823129));
#95680=CARTESIAN_POINT('Ctrl Pts',(0.0132204933453946,-0.0340223579322365,
0.0714882690988118));
#95681=CARTESIAN_POINT('Ctrl Pts',(0.0132572055566073,-0.0339125849573552,
0.071558566038382));
#95682=CARTESIAN_POINT('Ctrl Pts',(0.0132924369872727,-0.0338030433565217,
0.0716295734385714));
#95683=CARTESIAN_POINT('Ctrl Pts',(0.0133261506319435,-0.033693872113232,
0.0717011964989426));
#95684=CARTESIAN_POINT('Ctrl Pts',(0.0132567420622493,-0.0340223579322365,
0.0713809042518803));
#95685=CARTESIAN_POINT('Ctrl Pts',(0.0132949351147205,-0.0339125849573552,
0.0714517011557965));
#95686=CARTESIAN_POINT('Ctrl Pts',(0.0133316359979741,-0.0338030433565217,
0.0715232388189858));
#95687=CARTESIAN_POINT('Ctrl Pts',(0.013366805887493,-0.033693872113232,
0.0715954215963123));
#95688=CARTESIAN_POINT('Ctrl Pts',(0.013292990779104,-0.0340223579322365,
0.0712735394049487));
#95689=CARTESIAN_POINT('Ctrl Pts',(0.0133326646728337,-0.0339125849573552,
0.071344836273211));
#95690=CARTESIAN_POINT('Ctrl Pts',(0.0133708350086756,-0.0338030433565217,
0.0714169041994003));
#95691=CARTESIAN_POINT('Ctrl Pts',(0.0134074611430425,-0.033693872113232,
0.071489646693682));
#95692=CARTESIAN_POINT('Ctrl Pts',(0.0133292394959588,-0.0340223579322365,
0.0711661745580171));
#95693=CARTESIAN_POINT('Ctrl Pts',(0.0133703942309469,-0.0339125849573552,
0.0712379713906255));
#95694=CARTESIAN_POINT('Ctrl Pts',(0.013410034019377,-0.0338030433565217,
0.0713105695798147));
#95695=CARTESIAN_POINT('Ctrl Pts',(0.013448116398592,-0.033693872113232,
0.0713838717910516));
#95696=CARTESIAN_POINT('Origin',(-0.00119797009390548,-0.0345589643415581,
0.0798594743315512));
#95697=CARTESIAN_POINT('Ctrl Pts',(0.0136008811544589,-0.034193496108874,
0.0717002271599773));
#95698=CARTESIAN_POINT('Ctrl Pts',(0.0136346620707946,-0.0340836138595105,
0.071775753110283));
#95699=CARTESIAN_POINT('Ctrl Pts',(0.0136668639273651,-0.0339738896671456,
0.0718519418469909));
#95700=CARTESIAN_POINT('Ctrl Pts',(0.0136974520464904,-0.0338644633335883,
0.0719286930951262));
#95701=CARTESIAN_POINT('Ctrl Pts',(0.0134927622964681,-0.034193496108874,
0.0716662938165721));
#95702=CARTESIAN_POINT('Ctrl Pts',(0.0135270111335089,-0.0340836138595105,
0.0717403288718705));
#95703=CARTESIAN_POINT('Ctrl Pts',(0.0135597115372108,-0.0339738896671456,
0.0718150371115677));
#95704=CARTESIAN_POINT('Ctrl Pts',(0.0135908280647937,-0.0338644633335883,
0.0718903201127684));
#95705=CARTESIAN_POINT('Ctrl Pts',(0.0133846434384773,-0.034193496108874,
0.0716323604731668));
#95706=CARTESIAN_POINT('Ctrl Pts',(0.0134193601962231,-0.0340836138595105,
0.071704904633458));
#95707=CARTESIAN_POINT('Ctrl Pts',(0.0134525591470564,-0.0339738896671456,
0.0717781323761444));
#95708=CARTESIAN_POINT('Ctrl Pts',(0.013484204083097,-0.0338644633335883,
0.0718519471304106));
#95709=CARTESIAN_POINT('Ctrl Pts',(0.0132765245804865,-0.034193496108874,
0.0715984271297616));
#95710=CARTESIAN_POINT('Ctrl Pts',(0.0133117092589374,-0.0340836138595105,
0.0716694803950455));
#95711=CARTESIAN_POINT('Ctrl Pts',(0.0133454067569021,-0.0339738896671456,
0.0717412276407211));
#95712=CARTESIAN_POINT('Ctrl Pts',(0.0133775801014003,-0.0338644633335883,
0.0718135741480528));
#95713=CARTESIAN_POINT('Origin',(-0.00148718073547668,-0.0345610621864637,
0.0794748872591137));
#95714=CARTESIAN_POINT('Ctrl Pts',(0.013262311536772,-0.0342436276873899,
0.0715666608460542));
#95715=CARTESIAN_POINT('Ctrl Pts',(0.0133597437791519,-0.033943005420186,
0.0717604636751267));
#95716=CARTESIAN_POINT('Ctrl Pts',(0.0134423012035778,-0.0336441434784164,
0.0719610549263912));
#95717=CARTESIAN_POINT('Ctrl Pts',(0.0131451909600831,-0.0342436276873899,
0.0713457926262577));
#95718=CARTESIAN_POINT('Ctrl Pts',(0.0132509533846973,-0.033943005420186,
0.0715351781799608));
#95719=CARTESIAN_POINT('Ctrl Pts',(0.0133421500534631,-0.0336441434784164,
0.0717319921683297));
#95720=CARTESIAN_POINT('Ctrl Pts',(0.0133775687186269,-0.0335235895815127,
0.0718135488638217));
#95721=CARTESIAN_POINT('Ctrl Pts',(0.0134097345685649,-0.0334144449262719,
0.0718858775790982));
#95722=CARTESIAN_POINT('Ctrl Pts',(0.0134404431163433,-0.0333049234473133,
0.071958953913558));
#95723=CARTESIAN_POINT('Ctrl Pts',(0.0134696466307592,-0.0331951640388588,
0.0720326879819619));
#95724=CARTESIAN_POINT('Ctrl Pts',(0.0134204874369919,-0.0335235895815127,
0.0717086720022167));
#95725=CARTESIAN_POINT('Ctrl Pts',(0.0134540971234135,-0.0334144449262719,
0.0717815915781507));
#95726=CARTESIAN_POINT('Ctrl Pts',(0.0134862389597321,-0.0333049234473133,
0.0718552892806703));
#95727=CARTESIAN_POINT('Ctrl Pts',(0.0135168633100361,-0.0331951640388588,
0.0719296745960148));
#95728=CARTESIAN_POINT('Ctrl Pts',(0.013463406155357,-0.0335235895815127,
0.0716037951406117));
#95729=CARTESIAN_POINT('Ctrl Pts',(0.013498459678262,-0.0334144449262719,
0.0716773055772031));
#95730=CARTESIAN_POINT('Ctrl Pts',(0.0135320348031209,-0.0333049234473133,
0.0717516246477827));
#95731=CARTESIAN_POINT('Ctrl Pts',(0.0135640799893129,-0.0331951640388588,
0.0718266612100676));
#95732=CARTESIAN_POINT('Ctrl Pts',(0.0135063248737221,-0.0335235895815127,
0.0714989182790066));
#95733=CARTESIAN_POINT('Ctrl Pts',(0.0135428222331106,-0.0334144449262719,
0.0715730195762555));
#95734=CARTESIAN_POINT('Ctrl Pts',(0.0135778306465096,-0.0333049234473133,
0.071647960014895));
#95735=CARTESIAN_POINT('Ctrl Pts',(0.0136112966685898,-0.0331951640388588,
0.0717236478241205));
#95736=CARTESIAN_POINT('Origin',(-0.00229037639583367,-0.0326434571767497,
0.0774560186261367));
#95737=CARTESIAN_POINT('Ctrl Pts',(0.013745788448085,-0.0336938721132382,
0.0720496985445698));
#95738=CARTESIAN_POINT('Ctrl Pts',(0.0137580822094575,-0.0336474569764954,
0.0720826060127594));
#95739=CARTESIAN_POINT('Ctrl Pts',(0.0137699899049895,-0.033601104548885,
0.0721156551401071));
#95740=CARTESIAN_POINT('Ctrl Pts',(0.0138001374510285,-0.0334837508643167,
0.07219932792848));
#95741=CARTESIAN_POINT('Ctrl Pts',(0.013827792360393,-0.0333660264760416,
0.0722838573081909));
#95742=CARTESIAN_POINT('Ctrl Pts',(0.0134284645353433,-0.0336938721132382,
0.0719277330835424));
#95743=CARTESIAN_POINT('Ctrl Pts',(0.0134414722010316,-0.0336474569764954,
0.0719587831495714));
#95744=CARTESIAN_POINT('Ctrl Pts',(0.0134541154951997,-0.033601104548885,
0.0719899833591804));
#95745=CARTESIAN_POINT('Ctrl Pts',(0.0134861254077803,-0.0334837508643167,
0.0720689751131332));
#95746=CARTESIAN_POINT('Ctrl Pts',(0.0135157805746217,-0.0333660264760416,
0.0721488806997686));
#95747=CARTESIAN_POINT('Ctrl Pts',(0.0134284645353548,-0.0336938721132426,
0.071927733083556));
#95748=CARTESIAN_POINT('Ctrl Pts',(0.0134414722010423,-0.0336474569765026,
0.0719587831495832));
#95749=CARTESIAN_POINT('Ctrl Pts',(0.0134541154952097,-0.0336011045488949,
0.0719899833591904));
#95750=CARTESIAN_POINT('Ctrl Pts',(0.0134858588088175,-0.0334847282606778,
0.0720683172194232));
#95751=CARTESIAN_POINT('Ctrl Pts',(0.013515286543691,-0.0333679869945434,
0.0721475500411451));
#95752=CARTESIAN_POINT('Ctrl Pts',(0.013428464535342,-0.0336938721132427,
0.0719277330835393));
#95753=CARTESIAN_POINT('Ctrl Pts',(0.0134749857043083,-0.0335278710435083,
0.0720387818606809));
#95754=CARTESIAN_POINT('Ctrl Pts',(0.0135180080464564,-0.033362046922432,
0.0721512504628841));
#95755=CARTESIAN_POINT('Ctrl Pts',(0.0135575342506985,-0.0331951640388601,
0.0722652019798831));
#95756=CARTESIAN_POINT('Ctrl Pts',(0.0133943993015192,-0.0336938721132427,
0.071851132889885));
#95757=CARTESIAN_POINT('Ctrl Pts',(0.0134425240269824,-0.0335278710435083,
0.0719614685418449));
#95758=CARTESIAN_POINT('Ctrl Pts',(0.0134871717249203,-0.033362046922432,
0.0720732745568571));
#95759=CARTESIAN_POINT('Ctrl Pts',(0.0135283460027888,-0.0331951640388601,
0.0721866139654837));
#95760=CARTESIAN_POINT('Ctrl Pts',(0.0133603340676964,-0.0336938721132427,
0.0717745326962308));
#95761=CARTESIAN_POINT('Ctrl Pts',(0.0134100623496565,-0.0335278710435083,
0.0718841552230089));
#95762=CARTESIAN_POINT('Ctrl Pts',(0.0134563354033842,-0.033362046922432,
0.0719952986508301));
#95763=CARTESIAN_POINT('Ctrl Pts',(0.0134991577548792,-0.0331951640388601,
0.0721080259510843));
#95764=CARTESIAN_POINT('Ctrl Pts',(0.0133262688338736,-0.0336938721132427,
0.0716979325025765));
#95765=CARTESIAN_POINT('Ctrl Pts',(0.0133776006723306,-0.0335278710435083,
0.0718068419041729));
#95766=CARTESIAN_POINT('Ctrl Pts',(0.0134254990818481,-0.033362046922432,
0.0719173227448031));
#95767=CARTESIAN_POINT('Ctrl Pts',(0.0134699695069695,-0.0331951640388601,
0.0720294379366849));
#95768=CARTESIAN_POINT('Ctrl Pts',(0.0135139084417739,-0.0330240426238156,
0.0721480460036767));
#95769=CARTESIAN_POINT('Ctrl Pts',(0.0135414873084824,-0.0329142774063509,
0.0722223002440972));
#95770=CARTESIAN_POINT('Ctrl Pts',(0.0135675448816933,-0.0328043479726686,
0.0722971616351774));
#95771=CARTESIAN_POINT('Ctrl Pts',(0.0135920451385624,-0.0326943950436594,
0.0723725351932255));
#95772=CARTESIAN_POINT('Ctrl Pts',(0.0135633276559063,-0.0330240426238156,
0.0720460711182437));
#95773=CARTESIAN_POINT('Ctrl Pts',(0.0135923113260109,-0.0329142774063509,
0.0721210061564858));
#95774=CARTESIAN_POINT('Ctrl Pts',(0.0136197603289709,-0.0328043479726686,
0.0721965777260002));
#95775=CARTESIAN_POINT('Ctrl Pts',(0.0136456368343617,-0.0326943950436594,
0.0722726899823945));
#95776=CARTESIAN_POINT('Ctrl Pts',(0.0136127468700386,-0.0330240426238156,
0.0719440962328108));
#95777=CARTESIAN_POINT('Ctrl Pts',(0.0136431353435394,-0.0329142774063509,
0.0720197120688743));
#95778=CARTESIAN_POINT('Ctrl Pts',(0.0136719757762486,-0.0328043479726686,
0.0720959938168231));
#95779=CARTESIAN_POINT('Ctrl Pts',(0.013699228530161,-0.0326943950436594,
0.0721728447715636));
#95780=CARTESIAN_POINT('Ctrl Pts',(0.0136621660841709,-0.0330240426238156,
0.0718421213473778));
#95781=CARTESIAN_POINT('Ctrl Pts',(0.0136939593610679,-0.0329142774063509,
0.0719184179812629));
#95782=CARTESIAN_POINT('Ctrl Pts',(0.0137241912235263,-0.0328043479726686,
0.071995409907646));
#95783=CARTESIAN_POINT('Ctrl Pts',(0.0137528202259603,-0.0326943950436594,
0.0720729995607326));
#95784=CARTESIAN_POINT('Origin',(-0.00240738825288042,-0.0326396682861535,
0.0774960639003165));
#95785=CARTESIAN_POINT('Ctrl Pts',(0.0138647305447576,-0.0331951640388587,
0.0724060068739108));
#95786=CARTESIAN_POINT('Ctrl Pts',(0.0138887505220001,-0.0330855618255041,
0.0724850768236108));
#95787=CARTESIAN_POINT('Ctrl Pts',(0.0139111535742066,-0.0329757224427708,
0.0725647002256031));
#95788=CARTESIAN_POINT('Ctrl Pts',(0.013931906011448,-0.0328657862078596,
0.0726447765245699));
#95789=CARTESIAN_POINT('Ctrl Pts',(0.0137617172408188,-0.0331951640388587,
0.0723587902322228));
#95790=CARTESIAN_POINT('Ctrl Pts',(0.0137863875317821,-0.0330855618255041,
0.0724364413820553));
#95791=CARTESIAN_POINT('Ctrl Pts',(0.0138094706906795,-0.0329757224427708,
0.0725146584022601));
#95792=CARTESIAN_POINT('Ctrl Pts',(0.0138309322450051,-0.0328657862078596,
0.072593342581196));
#95793=CARTESIAN_POINT('Ctrl Pts',(0.0136587039368801,-0.0331951640388587,
0.0723115735905349));
#95794=CARTESIAN_POINT('Ctrl Pts',(0.0136840245415641,-0.0330855618255041,
0.0723878059404998));
#95795=CARTESIAN_POINT('Ctrl Pts',(0.0137077878071524,-0.0329757224427708,
0.0724646165789171));
#95796=CARTESIAN_POINT('Ctrl Pts',(0.0137299584785622,-0.0328657862078596,
0.072541908637822));
#95797=CARTESIAN_POINT('Ctrl Pts',(0.0135556906329414,-0.0331951640388587,
0.072264356948847));
#95798=CARTESIAN_POINT('Ctrl Pts',(0.0135816615513462,-0.0330855618255041,
0.0723391704989444));
#95799=CARTESIAN_POINT('Ctrl Pts',(0.0136061049236253,-0.0329757224427708,
0.0724145747555741));
#95800=CARTESIAN_POINT('Ctrl Pts',(0.0136289847121193,-0.0328657862078596,
0.0724904746944481));
#95801=CARTESIAN_POINT('Origin',(-0.00251580467905608,-0.0326401908832323,
0.0770275356184265));
#95802=CARTESIAN_POINT('Ctrl Pts',(0.0135455951265563,-0.0332451089994432,
0.0722311280619339));
#95803=CARTESIAN_POINT('Ctrl Pts',(0.0136179665657591,-0.0329451141710257,
0.0724356150823013));
#95804=CARTESIAN_POINT('Ctrl Pts',(0.0136747296070177,-0.0326442513127503,
0.0726449724892832));
#95805=CARTESIAN_POINT('Ctrl Pts',(0.0134570831548185,-0.0332451089994432,
0.0719973212381261));
#95806=CARTESIAN_POINT('Ctrl Pts',(0.013538272762654,-0.0329451141710257,
0.0721984699748624));
#95807=CARTESIAN_POINT('Ctrl Pts',(0.013604080374229,-0.0326442513127503,
0.0724051628024348));
#95808=CARTESIAN_POINT('Ctrl Pts',(0.013628975681232,-0.0325229783203385,
0.072490444425264));
#95809=CARTESIAN_POINT('Ctrl Pts',(0.0136518526181212,-0.032413025311208,
0.0725663333957258));
#95810=CARTESIAN_POINT('Ctrl Pts',(0.0136731562244631,-0.0323031222247695,
0.0726426840949569));
#95811=CARTESIAN_POINT('Ctrl Pts',(0.0136928626628868,-0.0321934096636184,
0.0727193977602254));
#95812=CARTESIAN_POINT('Ctrl Pts',(0.0136847004325288,-0.0325229783203385,
0.0723917737875737));
#95813=CARTESIAN_POINT('Ctrl Pts',(0.0137089375419761,-0.032413025311208,
0.0724684309224996));
#95814=CARTESIAN_POINT('Ctrl Pts',(0.0137315852241107,-0.0323031222247695,
0.0725455778066037));
#95815=CARTESIAN_POINT('Ctrl Pts',(0.0137526179558839,-0.0321934096636184,
0.0726231145965459));
#95816=CARTESIAN_POINT('Ctrl Pts',(0.0137404251838257,-0.0325229783203385,
0.0722931031498835));
#95817=CARTESIAN_POINT('Ctrl Pts',(0.0137660224658309,-0.032413025311208,
0.0723705284492734));
#95818=CARTESIAN_POINT('Ctrl Pts',(0.0137900142237584,-0.0323031222247695,
0.0724484715182504));
#95819=CARTESIAN_POINT('Ctrl Pts',(0.013812373248881,-0.0321934096636184,
0.0725268314328665));
#95820=CARTESIAN_POINT('Ctrl Pts',(0.0137961499351225,-0.0325229783203385,
0.0721944325121933));
#95821=CARTESIAN_POINT('Ctrl Pts',(0.0138231073896858,-0.032413025311208,
0.0722726259760472));
#95822=CARTESIAN_POINT('Ctrl Pts',(0.013848443223406,-0.0323031222247695,
0.0723513652298972));
#95823=CARTESIAN_POINT('Ctrl Pts',(0.013872128541878,-0.0321934096636184,
0.072430548269187));
#95824=CARTESIAN_POINT('Origin',(-0.00239919362031183,-0.0326393375181522,
0.0774937103885663));
#95825=CARTESIAN_POINT('Ctrl Pts',(0.0139629083290213,-0.0326943950436593,
0.0727699253755577));
#95826=CARTESIAN_POINT('Ctrl Pts',(0.0139819283438816,-0.0325844576448127,
0.0728503994773991));
#95827=CARTESIAN_POINT('Ctrl Pts',(0.0139992853684527,-0.0324744968375319,
0.0729312726396087));
#95828=CARTESIAN_POINT('Ctrl Pts',(0.0140149585931257,-0.0323646534831894,
0.0730124409360345));
#95829=CARTESIAN_POINT('Ctrl Pts',(0.0138630631508549,-0.0326943950436593,
0.0727163336972911));
#95830=CARTESIAN_POINT('Ctrl Pts',(0.0138828217594832,-0.0325844576448127,
0.0727954317454475));
#95831=CARTESIAN_POINT('Ctrl Pts',(0.01390094588914,-0.0324744968375319,
0.0728749440319168));
#95832=CARTESIAN_POINT('Ctrl Pts',(0.0139174137233068,-0.0323646534831894,
0.0729547683606236));
#95833=CARTESIAN_POINT('Ctrl Pts',(0.0137632179726886,-0.0326943950436593,
0.0726627420190245));
#95834=CARTESIAN_POINT('Ctrl Pts',(0.0137837151750849,-0.0325844576448127,
0.0727404640134959));
#95835=CARTESIAN_POINT('Ctrl Pts',(0.0138026064098274,-0.0324744968375319,
0.0728186154242249));
#95836=CARTESIAN_POINT('Ctrl Pts',(0.0138198688534879,-0.0323646534831894,
0.0728970957852128));
#95837=CARTESIAN_POINT('Ctrl Pts',(0.0136633727945222,-0.0326943950436593,
0.0726091503407578));
#95838=CARTESIAN_POINT('Ctrl Pts',(0.0136846085906865,-0.0325844576448127,
0.0726854962815443));
#95839=CARTESIAN_POINT('Ctrl Pts',(0.0137042669305148,-0.0324744968375319,
0.072762286816533));
#95840=CARTESIAN_POINT('Ctrl Pts',(0.013722323983669,-0.0323646534831894,
0.0728394232098019));
#95841=CARTESIAN_POINT('Origin',(-0.00255221132791817,-0.0326395579070405,
0.0770378563616196));
#95842=CARTESIAN_POINT('Ctrl Pts',(0.0136553726441631,-0.0327445246961876,
0.0725753152436751));
#95843=CARTESIAN_POINT('Ctrl Pts',(0.0137147628500275,-0.0324436878365474,
0.0727839425859584));
#95844=CARTESIAN_POINT('Ctrl Pts',(0.0137582696706652,-0.0321434074463186,
0.0729964507529987));
#95845=CARTESIAN_POINT('Ctrl Pts',(0.0135817145532401,-0.0327445246961876,
0.0723364125738667));
#95846=CARTESIAN_POINT('Ctrl Pts',(0.013650115120502,-0.0324436878365474,
0.0725422618558647));
#95847=CARTESIAN_POINT('Ctrl Pts',(0.013702815959905,-0.0321434074463186,
0.0727526785520346));
#95848=CARTESIAN_POINT('Ctrl Pts',(0.0137445204525794,-0.0322357242816072,
0.0729312192902247));
#95849=CARTESIAN_POINT('Ctrl Pts',(0.013783337037485,-0.0319819883628705,
0.0731102325139584));
#95850=CARTESIAN_POINT('Ctrl Pts',(0.0138106838322272,-0.0317295851069886,
0.0732913529555231));
#95851=CARTESIAN_POINT('Ctrl Pts',(0.0136862449203081,-0.0322357242816072,
0.0726881062252971));
#95852=CARTESIAN_POINT('Ctrl Pts',(0.0137328043410256,-0.0319819883628705,
0.0728652634489086));
#95853=CARTESIAN_POINT('Ctrl Pts',(0.0137679963823594,-0.0317295851069886,
0.0730450243505586));
#95854=CARTESIAN_POINT('Origin',(-0.00245978565393022,-0.0326371942644254,
0.077014620651325));
#95855=CARTESIAN_POINT('Origin',(-0.00228137266389705,-0.0326352985527658,
0.0774593297964607));
#95856=CARTESIAN_POINT('Ctrl Pts',(0.0140380417500742,-0.0321934096636183,
0.0731392904012538));
#95857=CARTESIAN_POINT('Ctrl Pts',(0.0140519802231401,-0.0320835708272303,
0.0732208526498378));
#95858=CARTESIAN_POINT('Ctrl Pts',(0.0140642226848299,-0.0319739230346346,
0.0733026560449787));
#95859=CARTESIAN_POINT('Ctrl Pts',(0.0140747615042616,-0.0318646057455575,
0.073384594722787));
#95860=CARTESIAN_POINT('Ctrl Pts',(0.0139417585034795,-0.0321934096636183,
0.0730795350567979));
#95861=CARTESIAN_POINT('Ctrl Pts',(0.0139565210493159,-0.0320835708272303,
0.0731597694843727));
#95862=CARTESIAN_POINT('Ctrl Pts',(0.0139696145849673,-0.0319739230346346,
0.0732402628828378));
#95863=CARTESIAN_POINT('Ctrl Pts',(0.0139810302620295,-0.0318646057455575,
0.0733209109807841));
#95864=CARTESIAN_POINT('Ctrl Pts',(0.0138454752568849,-0.0321934096636183,
0.0730197797123419));
#95865=CARTESIAN_POINT('Ctrl Pts',(0.0138610618754918,-0.0320835708272303,
0.0730986863189077));
#95866=CARTESIAN_POINT('Ctrl Pts',(0.0138750064851048,-0.0319739230346346,
0.0731778697206968));
#95867=CARTESIAN_POINT('Ctrl Pts',(0.0138872990197974,-0.0318646057455575,
0.0732572272387812));
#95868=CARTESIAN_POINT('Ctrl Pts',(0.0137491920102902,-0.0321934096636183,
0.072960024367886));
#95869=CARTESIAN_POINT('Ctrl Pts',(0.0137656027016676,-0.0320835708272303,
0.0730376031534426));
#95870=CARTESIAN_POINT('Ctrl Pts',(0.0137803983852423,-0.0319739230346346,
0.0731154765585559));
#95871=CARTESIAN_POINT('Ctrl Pts',(0.0137935677775653,-0.0318646057455575,
0.0731935434967783));
#95872=CARTESIAN_POINT('Ctrl Pts',(0.0137230225550669,-0.0320218834582285,
0.0728387772235915));
#95873=CARTESIAN_POINT('Ctrl Pts',(0.0137366692143082,-0.0319391099350598,
0.0728970517796814));
#95874=CARTESIAN_POINT('Ctrl Pts',(0.0137493976400211,-0.0318564869454897,
0.072955504123196));
#95875=CARTESIAN_POINT('Ctrl Pts',(0.0137612025358867,-0.0317740741446507,
0.073014090813847));
#95876=CARTESIAN_POINT('Ctrl Pts',(0.0137500613892921,-0.0320218834582285,
0.0727972353231601));
#95877=CARTESIAN_POINT('Ctrl Pts',(0.01376414039929,-0.0319391099350598,
0.0728557912881484));
#95878=CARTESIAN_POINT('Ctrl Pts',(0.0137772965195698,-0.0318564869454897,
0.0729145316212805));
#95879=CARTESIAN_POINT('Ctrl Pts',(0.0137895241618764,-0.0317740741446507,
0.0729734126434235));
#95880=CARTESIAN_POINT('Ctrl Pts',(0.0137771002235173,-0.0320218834582285,
0.0727556934227288));
#95881=CARTESIAN_POINT('Ctrl Pts',(0.0137916115842718,-0.0319391099350598,
0.0728145307966154));
#95882=CARTESIAN_POINT('Ctrl Pts',(0.0138051953991184,-0.0318564869454897,
0.072873559119365));
#95883=CARTESIAN_POINT('Ctrl Pts',(0.0138178457878661,-0.0317740741446507,
0.072932734473));
#95884=CARTESIAN_POINT('Ctrl Pts',(0.0138041390577425,-0.0320218834582285,
0.0727141515222974));
#95885=CARTESIAN_POINT('Ctrl Pts',(0.0138190827692536,-0.0319391099350598,
0.0727732703050823));
#95886=CARTESIAN_POINT('Ctrl Pts',(0.013833094278667,-0.0318564869454897,
0.0728325866174495));
#95887=CARTESIAN_POINT('Ctrl Pts',(0.0138461674138558,-0.0317740741446507,
0.0728920563025765));
#95888=CARTESIAN_POINT('Origin',(0.0196331709116167,-0.039122885339073,
0.0704874067034132));
#95889=CARTESIAN_POINT('Ctrl Pts',(0.0122765154643634,-0.0352722978779544,
0.0701701795366615));
#95890=CARTESIAN_POINT('Ctrl Pts',(0.0122893354974371,-0.0352466642097183,
0.0701840625993632));
#95891=CARTESIAN_POINT('Ctrl Pts',(0.0123022017085266,-0.0352210183808285,
0.0701978801050475));
#95892=CARTESIAN_POINT('Ctrl Pts',(0.0123151149413924,-0.0351953608940152,
0.0702116321784253));
#95893=CARTESIAN_POINT('Origin',(0.0159968364979673,-0.0352456003065005,
0.0669812997019457));
#95894=CARTESIAN_POINT('Ctrl Pts',(0.012398426504718,-0.035024121149334,
0.0703043926162986));
#95895=CARTESIAN_POINT('Ctrl Pts',(0.0124513981672796,-0.0349144232867422,
0.0703632740863637));
#95896=CARTESIAN_POINT('Ctrl Pts',(0.0125031844139273,-0.0348045283677513,
0.0704232857618924));
#95897=CARTESIAN_POINT('Ctrl Pts',(0.0125537160526539,-0.0346945769586886,
0.0704843532439135));
#95898=CARTESIAN_POINT('Ctrl Pts',(0.0124068358735734,-0.035024121149334,
0.0701913863141805));
#95899=CARTESIAN_POINT('Ctrl Pts',(0.0124613641515421,-0.0349144232867422,
0.0702503836198484));
#95900=CARTESIAN_POINT('Ctrl Pts',(0.0125147055509017,-0.0348045283677513,
0.0703105433766643));
#95901=CARTESIAN_POINT('Ctrl Pts',(0.0125667888806338,-0.0346945769586886,
0.0703717910701092));
#95902=CARTESIAN_POINT('Ctrl Pts',(0.0124152452424289,-0.035024121149334,
0.0700783800120624));
#95903=CARTESIAN_POINT('Ctrl Pts',(0.0124713301358046,-0.0349144232867422,
0.070137493153333));
#95904=CARTESIAN_POINT('Ctrl Pts',(0.012526226687876,-0.0348045283677513,
0.0701978009914363));
#95905=CARTESIAN_POINT('Ctrl Pts',(0.0125798617086137,-0.0346945769586886,
0.0702592288963048));
#95906=CARTESIAN_POINT('Ctrl Pts',(0.0124236546112843,-0.035024121149334,
0.0699653737099443));
#95907=CARTESIAN_POINT('Ctrl Pts',(0.0124812961200671,-0.0349144232867422,
0.0700246026868177));
#95908=CARTESIAN_POINT('Ctrl Pts',(0.0125377478248504,-0.0348045283677513,
0.0700850586062083));
#95909=CARTESIAN_POINT('Ctrl Pts',(0.0125929345365936,-0.0346945769586886,
0.0701466667225005));
#95910=CARTESIAN_POINT('Origin',(-0.000495043863386638,-0.0345629067943128,
0.0810481032281225));
#95911=CARTESIAN_POINT('Ctrl Pts',(0.0127260562743256,-0.035197097365165,
0.0704090649486225));
#95912=CARTESIAN_POINT('Ctrl Pts',(0.0127778818595984,-0.0350869349321799,
0.0704728232188328));
#95913=CARTESIAN_POINT('Ctrl Pts',(0.0128284248774781,-0.034976498512974,
0.0705377117308498));
#95914=CARTESIAN_POINT('Ctrl Pts',(0.0128776148994444,-0.0348659306849651,
0.0706036502742342));
#95915=CARTESIAN_POINT('Ctrl Pts',(0.0126439476622796,-0.035197097365165,
0.0704047467918752));
#95916=CARTESIAN_POINT('Ctrl Pts',(0.012695833069762,-0.0350869349321799,
0.0704673675585424));
#95917=CARTESIAN_POINT('Ctrl Pts',(0.0127464596074756,-0.034976498512974,
0.0705311188683923));
#95918=CARTESIAN_POINT('Ctrl Pts',(0.0127957568254235,-0.0348659306849652,
0.0705959219906337));
#95919=CARTESIAN_POINT('Ctrl Pts',(0.0125618390502336,-0.035197097365165,
0.0704004286351279));
#95920=CARTESIAN_POINT('Ctrl Pts',(0.0126137842799256,-0.0350869349321799,
0.070461911898252));
#95921=CARTESIAN_POINT('Ctrl Pts',(0.0126644943374731,-0.0349764985129741,
0.0705245260059347));
#95922=CARTESIAN_POINT('Ctrl Pts',(0.0127138987514027,-0.0348659306849652,
0.0705881937070332));
#95923=CARTESIAN_POINT('Ctrl Pts',(0.0124797304381876,-0.035197097365165,
0.0703961104783805));
#95924=CARTESIAN_POINT('Ctrl Pts',(0.0125317354900891,-0.0350869349321799,
0.0704564562379617));
#95925=CARTESIAN_POINT('Ctrl Pts',(0.0125825290674705,-0.0349764985129741,
0.0705179331434772));
#95926=CARTESIAN_POINT('Ctrl Pts',(0.0126320406773818,-0.0348659306849652,
0.0705804654234326));
#95927=CARTESIAN_POINT('Origin',(-0.000758735023101335,-0.0345637187965591,
0.0806458690564938));
#95928=CARTESIAN_POINT('Ctrl Pts',(0.0124584764604435,-0.0352450361861253,
0.0703699800782624));
#95929=CARTESIAN_POINT('Ctrl Pts',(0.0126010422475195,-0.0349452761023765,
0.0705334657510238));
#95930=CARTESIAN_POINT('Ctrl Pts',(0.0127308886107374,-0.0346444289983474,
0.0707072256163607));
#95931=CARTESIAN_POINT('Ctrl Pts',(0.0122901102718113,-0.0352450361861253,
0.0701851752446529));
#95932=CARTESIAN_POINT('Ctrl Pts',(0.0124396460873804,-0.0349452761023765,
0.0703423108825742));
#95933=CARTESIAN_POINT('Ctrl Pts',(0.0125769209885692,-0.0346444289983474,
0.0705102637639023));
#95934=CARTESIAN_POINT('Ctrl Pts',(0.0126314585947887,-0.0345231616327823,
0.0705803873850557));
#95935=CARTESIAN_POINT('Ctrl Pts',(0.0126806606790728,-0.0344132092796976,
0.0706425193579517));
#95936=CARTESIAN_POINT('Ctrl Pts',(0.0127285750739053,-0.0343032738558974,
0.0707056658314269));
#95937=CARTESIAN_POINT('Ctrl Pts',(0.0127751424676396,-0.0341934961088741,
0.0707697443351799));
#95938=CARTESIAN_POINT('Ctrl Pts',(0.0126469470727039,-0.0345231616327823,
0.0704681321259795));
#95939=CARTESIAN_POINT('Ctrl Pts',(0.0126976964376916,-0.0344132092796976,
0.0705304775857376));
#95940=CARTESIAN_POINT('Ctrl Pts',(0.0127471536175878,-0.0343032738558974,
0.0705938695393407));
#95941=CARTESIAN_POINT('Ctrl Pts',(0.0127952573323156,-0.0341934961088741,
0.0706582251513707));
#95942=CARTESIAN_POINT('Ctrl Pts',(0.0126624355506191,-0.0345231616327823,
0.0703558768669033));
#95943=CARTESIAN_POINT('Ctrl Pts',(0.0127147321963105,-0.0344132092796976,
0.0704184358135234));
#95944=CARTESIAN_POINT('Ctrl Pts',(0.0127657321612702,-0.0343032738558974,
0.0704820732472545));
#95945=CARTESIAN_POINT('Ctrl Pts',(0.0128153721969916,-0.0341934961088741,
0.0705467059675616));
#95946=CARTESIAN_POINT('Ctrl Pts',(0.0126779240285344,-0.0345231616327823,
0.0702436216078271));
#95947=CARTESIAN_POINT('Ctrl Pts',(0.0127317679549293,-0.0344132092796976,
0.0703063940413092));
#95948=CARTESIAN_POINT('Ctrl Pts',(0.0127843107049527,-0.0343032738558974,
0.0703702769551683));
#95949=CARTESIAN_POINT('Ctrl Pts',(0.0128354870616676,-0.0341934961088741,
0.0704351867837524));
#95950=CARTESIAN_POINT('Origin',(-0.000504335037640546,-0.0345625596231234,
0.0810558603139963));
#95951=CARTESIAN_POINT('Ctrl Pts',(0.0130448250186207,-0.0346945769586885,
0.0707173133685701));
#95952=CARTESIAN_POINT('Ctrl Pts',(0.0130921291754465,-0.0345846629176052,
0.0707851278260371));
#95953=CARTESIAN_POINT('Ctrl Pts',(0.013138039036808,-0.0344746925050311,
0.0708539320969166));
#95954=CARTESIAN_POINT('Ctrl Pts',(0.0131824961417883,-0.0343648066253259,
0.0709236377783091));
#95955=CARTESIAN_POINT('Ctrl Pts',(0.0129322629334401,-0.0346945769586885,
0.0707042405508829));
#95956=CARTESIAN_POINT('Ctrl Pts',(0.0129797472403013,-0.0345846629176052,
0.0707705038459218));
#95957=CARTESIAN_POINT('Ctrl Pts',(0.0130258693598702,-0.0344746925050311,
0.0708377604148596));
#95958=CARTESIAN_POINT('Ctrl Pts',(0.0130705705510705,-0.0343648066253259,
0.0709059238367677));
#95959=CARTESIAN_POINT('Ctrl Pts',(0.0128197008482596,-0.0346945769586885,
0.0706911677331956));
#95960=CARTESIAN_POINT('Ctrl Pts',(0.0128673653051561,-0.0345846629176052,
0.0707558798658065));
#95961=CARTESIAN_POINT('Ctrl Pts',(0.0129136996829324,-0.0344746925050311,
0.0708215887328026));
#95962=CARTESIAN_POINT('Ctrl Pts',(0.0129586449603526,-0.0343648066253259,
0.0708882098952263));
#95963=CARTESIAN_POINT('Ctrl Pts',(0.012707138763079,-0.0346945769586885,
0.0706780949155084));
#95964=CARTESIAN_POINT('Ctrl Pts',(0.0127549833700109,-0.0345846629176052,
0.0707412558856912));
#95965=CARTESIAN_POINT('Ctrl Pts',(0.0128015300059947,-0.0344746925050311,
0.0708054170507456));
#95966=CARTESIAN_POINT('Ctrl Pts',(0.0128467193696347,-0.0343648066253259,
0.0708704959536849));
#95967=CARTESIAN_POINT('Origin',(-0.000805435439944113,-0.0345626446733757,
0.08068098602812));
#95968=CARTESIAN_POINT('Ctrl Pts',(0.0127091528762319,-0.0346945769586885,
0.0706783288320533));
#95969=CARTESIAN_POINT('Ctrl Pts',(0.0127818684188246,-0.034527515336289,
0.070774371256892));
#95970=CARTESIAN_POINT('Ctrl Pts',(0.0128515823235211,-0.0343603235965159,
0.0708727253601056));
#95971=CARTESIAN_POINT('Ctrl Pts',(0.0129180927308873,-0.034193496108874,
0.0709730971895031));
#95972=CARTESIAN_POINT('Ctrl Pts',(0.0126571081763789,-0.0346945769586885,
0.0706126068604723));
#95973=CARTESIAN_POINT('Ctrl Pts',(0.0127312002919801,-0.034527515336289,
0.0707075591882351));
#95974=CARTESIAN_POINT('Ctrl Pts',(0.0128023254082869,-0.0343603235965159,
0.0708048662043718));
#95975=CARTESIAN_POINT('Ctrl Pts',(0.0128702774461011,-0.034193496108874,
0.0709042369914778));
#95976=CARTESIAN_POINT('Ctrl Pts',(0.012605063476526,-0.0346945769586885,
0.0705468848888913));
#95977=CARTESIAN_POINT('Ctrl Pts',(0.0126805321651355,-0.034527515336289,
0.0706407471195782));
#95978=CARTESIAN_POINT('Ctrl Pts',(0.0127530684930527,-0.0343603235965159,
0.0707370070486381));
#95979=CARTESIAN_POINT('Ctrl Pts',(0.0128224621613149,-0.034193496108874,
0.0708353767934525));
#95980=CARTESIAN_POINT('Ctrl Pts',(0.0125530187766731,-0.0346945769586885,
0.0704811629173104));
#95981=CARTESIAN_POINT('Ctrl Pts',(0.012629864038291,-0.034527515336289,
0.0705739350509212));
#95982=CARTESIAN_POINT('Ctrl Pts',(0.0127038115778185,-0.0343603235965159,
0.0706691478929043));
#95983=CARTESIAN_POINT('Ctrl Pts',(0.0127746468765287,-0.034193496108874,
0.0707665165954272));
#95984=CARTESIAN_POINT('Ctrl Pts',(0.012846700914921,-0.0340223579322366,
0.0708704703527289));
#95985=CARTESIAN_POINT('Ctrl Pts',(0.0128919341821289,-0.0339125849573554,
0.0709356117197912));
#95986=CARTESIAN_POINT('Ctrl Pts',(0.012935787389513,-0.0338030433565221,
0.0710016435362927));
#95987=CARTESIAN_POINT('Ctrl Pts',(0.0129782119417798,-0.0336938721132327,
0.0710684763873381));
#95988=CARTESIAN_POINT('Ctrl Pts',(0.0128692074163793,-0.0340223579322366,
0.0707594089407877));
#95989=CARTESIAN_POINT('Ctrl Pts',(0.0129159725101181,-0.0339125849573554,
0.0708248607312046));
#95990=CARTESIAN_POINT('Ctrl Pts',(0.0129613500425943,-0.0338030433565221,
0.0708912344581794));
#95991=CARTESIAN_POINT('Ctrl Pts',(0.0130052895079195,-0.0336938721132327,
0.070958440096769));
#95992=CARTESIAN_POINT('Ctrl Pts',(0.0128917139178376,-0.0340223579322366,
0.0706483475288465));
#95993=CARTESIAN_POINT('Ctrl Pts',(0.0129400108381074,-0.0339125849573554,
0.0707141097426179));
#95994=CARTESIAN_POINT('Ctrl Pts',(0.0129869126956757,-0.0338030433565221,
0.0707808253800661));
#95995=CARTESIAN_POINT('Ctrl Pts',(0.0130323670740592,-0.0336938721132327,
0.0708484038061999));
#95996=CARTESIAN_POINT('Ctrl Pts',(0.0129142204192959,-0.0340223579322366,
0.0705372861169054));
#95997=CARTESIAN_POINT('Ctrl Pts',(0.0129640491660967,-0.0339125849573554,
0.0706033587540312));
#95998=CARTESIAN_POINT('Ctrl Pts',(0.0130124753487571,-0.0338030433565221,
0.0706704163019528));
#95999=CARTESIAN_POINT('Ctrl Pts',(0.013059444640199,-0.0336938721132327,
0.0707383675156308));
#96000=CARTESIAN_POINT('Origin',(-0.000408878412918008,-0.0345589643414788,
0.0809827787775909));
#96001=CARTESIAN_POINT('Ctrl Pts',(0.0132506546416793,-0.034193496108874,
0.0710330818271546));
#96002=CARTESIAN_POINT('Ctrl Pts',(0.0132936350975172,-0.0340836138581107,
0.0711037783622071));
#96003=CARTESIAN_POINT('Ctrl Pts',(0.0133351320140729,-0.03397388966435,
0.0711753303660813));
#96004=CARTESIAN_POINT('Ctrl Pts',(0.0133750984193218,-0.0338644633294062,
0.0712476427007624));
#96005=CARTESIAN_POINT('Ctrl Pts',(0.013139135357523,-0.034193496108874,
0.0710129669443788));
#96006=CARTESIAN_POINT('Ctrl Pts',(0.0131823931856828,-0.0340836138581107,
0.0710821256945419));
#96007=CARTESIAN_POINT('Ctrl Pts',(0.0132241991627036,-0.03397388966435,
0.071152146391023));
#96008=CARTESIAN_POINT('Ctrl Pts',(0.0132645057896207,-0.0338644633294062,
0.0712229358291754));
#96009=CARTESIAN_POINT('Ctrl Pts',(0.0130276160733668,-0.034193496108874,
0.070992852061603));
#96010=CARTESIAN_POINT('Ctrl Pts',(0.0130711512738485,-0.0340836138581107,
0.0710604730268767));
#96011=CARTESIAN_POINT('Ctrl Pts',(0.0131132663113343,-0.03397388966435,
0.0711289624159647));
#96012=CARTESIAN_POINT('Ctrl Pts',(0.0131539131599197,-0.0338644633294062,
0.0711982289575884));
#96013=CARTESIAN_POINT('Ctrl Pts',(0.0129160967892105,-0.034193496108874,
0.0709727371788273));
#96014=CARTESIAN_POINT('Ctrl Pts',(0.0129599093620141,-0.0340836138581107,
0.0710388203592115));
#96015=CARTESIAN_POINT('Ctrl Pts',(0.013002333459965,-0.03397388966435,
0.0711057784409064));
#96016=CARTESIAN_POINT('Ctrl Pts',(0.0130433205302187,-0.0338644633294062,
0.0711735220860013));
#96017=CARTESIAN_POINT('Origin',(-0.000744010083504203,-0.0345610621862648,
0.0806374719937393));
#96018=CARTESIAN_POINT('Ctrl Pts',(0.0128980144485355,-0.03424362768739,
0.0709430027484825));
#96019=CARTESIAN_POINT('Ctrl Pts',(0.0130189683438243,-0.033943005420186,
0.0711230658863709));
#96020=CARTESIAN_POINT('Ctrl Pts',(0.0131260155284456,-0.0336441434784162,
0.0713117282267475));
#96021=CARTESIAN_POINT('Ctrl Pts',(0.0127541352743974,-0.03424362768739,
0.0707385552411627));
#96022=CARTESIAN_POINT('Ctrl Pts',(0.0128828000345398,-0.033943005420186,
0.0709131918865416));
#96023=CARTESIAN_POINT('Ctrl Pts',(0.0129979449239063,-0.0336441434784162,
0.0710970239644403));
#96024=CARTESIAN_POINT('Ctrl Pts',(0.0130433060666809,-0.0335235895815128,
0.0711734984251947));
#96025=CARTESIAN_POINT('Ctrl Pts',(0.0130842834710499,-0.0334144449262719,
0.0712412253569647));
#96026=CARTESIAN_POINT('Ctrl Pts',(0.0131239087660518,-0.0333049234473133,
0.0713098766611093));
#96027=CARTESIAN_POINT('Ctrl Pts',(0.0131621233312507,-0.0331951640388588,
0.0713793691434673));
#96028=CARTESIAN_POINT('Ctrl Pts',(0.0130727418019415,-0.0335235895815128,
0.0710640694072154));
#96029=CARTESIAN_POINT('Ctrl Pts',(0.0131152257121888,-0.0334144449262719,
0.0711322015798349));
#96030=CARTESIAN_POINT('Ctrl Pts',(0.0131563508718908,-0.0333049234473133,
0.0712012897136793));
#96031=CARTESIAN_POINT('Ctrl Pts',(0.0131960566921474,-0.0331951640388588,
0.071271250229745));
#96032=CARTESIAN_POINT('Ctrl Pts',(0.013102177537202,-0.0335235895815128,
0.0709546403892362));
#96033=CARTESIAN_POINT('Ctrl Pts',(0.0131461679533277,-0.0334144449262719,
0.0710231778027052));
#96034=CARTESIAN_POINT('Ctrl Pts',(0.0131887929777299,-0.0333049234473133,
0.0710927027662494));
#96035=CARTESIAN_POINT('Ctrl Pts',(0.0132299900530441,-0.0331951640388588,
0.0711631313160227));
#96036=CARTESIAN_POINT('Ctrl Pts',(0.0131316132724625,-0.0335235895815128,
0.0708452113712569));
#96037=CARTESIAN_POINT('Ctrl Pts',(0.0131771101944666,-0.0334144449262719,
0.0709141540255754));
#96038=CARTESIAN_POINT('Ctrl Pts',(0.0132212350835689,-0.0333049234473133,
0.0709841158188194));
#96039=CARTESIAN_POINT('Ctrl Pts',(0.0132639234139408,-0.0331951640388588,
0.0710550124023004));
#96040=CARTESIAN_POINT('Origin',(-0.00179390363966221,-0.0326434571770524,
0.0787351898528119));
#96041=CARTESIAN_POINT('Ctrl Pts',(0.013438219676683,-0.0336938721132375,
0.0713616358258208));
#96042=CARTESIAN_POINT('Ctrl Pts',(0.0134545408974716,-0.033647456976495,
0.071392742991929));
#96043=CARTESIAN_POINT('Ctrl Pts',(0.0134704968512645,-0.033601104548885,
0.0714240390870506));
#96044=CARTESIAN_POINT('Ctrl Pts',(0.0135108936560266,-0.0334837508643164,
0.0715032736010666));
#96045=CARTESIAN_POINT('Ctrl Pts',(0.0135489248386611,-0.033366026476041,
0.0715836703621564));
#96046=CARTESIAN_POINT('Ctrl Pts',(0.0131081116321606,-0.0336938721132375,
0.0712804033309542));
#96047=CARTESIAN_POINT('Ctrl Pts',(0.0131249083336974,-0.0336474569764951,
0.0713095782651363));
#96048=CARTESIAN_POINT('Ctrl Pts',(0.0131413623548727,-0.033601104548885,
0.0713389478268323));
#96049=CARTESIAN_POINT('Ctrl Pts',(0.0131830201516796,-0.0334837508643164,
0.0714133048013619));
#96050=CARTESIAN_POINT('Ctrl Pts',(0.0132224563042259,-0.033366026476041,
0.0714888635306281));
#96051=CARTESIAN_POINT('Ctrl Pts',(0.0131081116321723,-0.0336938721132427,
0.0712804033309673));
#96052=CARTESIAN_POINT('Ctrl Pts',(0.0131249083337082,-0.0336474569765026,
0.0713095782651479));
#96053=CARTESIAN_POINT('Ctrl Pts',(0.0131413623548827,-0.0336011045488949,
0.0713389478268423));
#96054=CARTESIAN_POINT('Ctrl Pts',(0.013182673198982,-0.0334847282606778,
0.0714126855090515));
#96055=CARTESIAN_POINT('Ctrl Pts',(0.0132217993931271,-0.0333679869945434,
0.0714876052831402));
#96056=CARTESIAN_POINT('Ctrl Pts',(0.0131081116321587,-0.0336938721132427,
0.0712804033309509));
#96057=CARTESIAN_POINT('Ctrl Pts',(0.0131681840701349,-0.0335278710435084,
0.0713847458067803));
#96058=CARTESIAN_POINT('Ctrl Pts',(0.0132249632218537,-0.0333620469224321,
0.0714909354312055));
#96059=CARTESIAN_POINT('Ctrl Pts',(0.0132784596622644,-0.0331951640388602,
0.071599034459469));
#96060=CARTESIAN_POINT('Ctrl Pts',(0.013064714462917,-0.0336938721132427,
0.0712086766586101));
#96061=CARTESIAN_POINT('Ctrl Pts',(0.0131262884345833,-0.0335278710435084,
0.071312110653542));
#96062=CARTESIAN_POINT('Ctrl Pts',(0.0131845970814808,-0.0333620469224321,
0.0714174392043771));
#96063=CARTESIAN_POINT('Ctrl Pts',(0.0132396518824436,-0.0331951640388602,
0.0715247243925289));
#96064=CARTESIAN_POINT('Ctrl Pts',(0.0130213172936753,-0.0336938721132427,
0.0711369499862693));
#96065=CARTESIAN_POINT('Ctrl Pts',(0.0130843927990317,-0.0335278710435084,
0.0712394755003036));
#96066=CARTESIAN_POINT('Ctrl Pts',(0.0131442309411079,-0.0333620469224321,
0.0713439429775488));
#96067=CARTESIAN_POINT('Ctrl Pts',(0.0132008441026227,-0.0331951640388602,
0.0714504143255888));
#96068=CARTESIAN_POINT('Ctrl Pts',(0.0129779201244336,-0.0336938721132427,
0.0710652233139285));
#96069=CARTESIAN_POINT('Ctrl Pts',(0.01304249716348,-0.0335278710435084,
0.0711668403470652));
#96070=CARTESIAN_POINT('Ctrl Pts',(0.013103864800735,-0.0333620469224321,
0.0712704467507205));
#96071=CARTESIAN_POINT('Ctrl Pts',(0.0131620363228018,-0.0331951640388602,
0.0713761042586486));
#96072=CARTESIAN_POINT('Ctrl Pts',(0.0132204943185443,-0.0330240426238155,
0.0714882700568273));
#96073=CARTESIAN_POINT('Ctrl Pts',(0.0132571622417092,-0.0329142774063509,
0.0715584822318409));
#96074=CARTESIAN_POINT('Ctrl Pts',(0.0132923969633854,-0.0328043479726686,
0.071629487438583));
#96075=CARTESIAN_POINT('Ctrl Pts',(0.0133261508401667,-0.0326943950436594,
0.0717011959571964));
#96076=CARTESIAN_POINT('Ctrl Pts',(0.0132567430052788,-0.0330240426238156,
0.071380905403917));
#96077=CARTESIAN_POINT('Ctrl Pts',(0.0132948899811378,-0.0329142774063509,
0.0714516169399057));
#96078=CARTESIAN_POINT('Ctrl Pts',(0.0133315941696836,-0.0328043479726686,
0.0715231523327233));
#96079=CARTESIAN_POINT('Ctrl Pts',(0.0133668060263082,-0.0326943950436594,
0.0715954212351484));
#96080=CARTESIAN_POINT('Ctrl Pts',(0.0132929916920132,-0.0330240426238156,
0.0712735407510067));
#96081=CARTESIAN_POINT('Ctrl Pts',(0.0133326177205664,-0.0329142774063509,
0.0713447516479706));
#96082=CARTESIAN_POINT('Ctrl Pts',(0.0133707913759818,-0.0328043479726686,
0.0714168172268637));
#96083=CARTESIAN_POINT('Ctrl Pts',(0.0134074612124497,-0.0326943950436594,
0.0714896465131004));
#96084=CARTESIAN_POINT('Ctrl Pts',(0.0133292403787477,-0.0330240426238156,
0.0711661760980964));
#96085=CARTESIAN_POINT('Ctrl Pts',(0.013370345459995,-0.0329142774063509,
0.0712378863560354));
#96086=CARTESIAN_POINT('Ctrl Pts',(0.01340998858228,-0.0328043479726686,
0.071310482121004));
#96087=CARTESIAN_POINT('Ctrl Pts',(0.0134481163985912,-0.0326943950436594,
0.0713838717910524));
#96088=CARTESIAN_POINT('Origin',(-0.00190497382074644,-0.0326396682857095,
0.0787895848319035));
#96089=CARTESIAN_POINT('Ctrl Pts',(0.013600881154459,-0.0331951640388587,
0.0717002271599773));
#96090=CARTESIAN_POINT('Ctrl Pts',(0.0136346218194802,-0.0330855618255041,
0.0717756631180889));
#96091=CARTESIAN_POINT('Ctrl Pts',(0.0136668276753677,-0.0329757224427708,
0.0718518508187994));
#96092=CARTESIAN_POINT('Ctrl Pts',(0.0136974526949243,-0.0328657862078596,
0.0719286947221673));
#96093=CARTESIAN_POINT('Ctrl Pts',(0.0134927623268099,-0.0331951640388587,
0.0716662938260949));
#96094=CARTESIAN_POINT('Ctrl Pts',(0.0135269703548588,-0.0330855618255041,
0.0717402406660782));
#96095=CARTESIAN_POINT('Ctrl Pts',(0.0135596746882157,-0.0329757224427708,
0.0718149478347709));
#96096=CARTESIAN_POINT('Ctrl Pts',(0.0135908287543516,-0.0328657862078596,
0.0718903217194531));
#96097=CARTESIAN_POINT('Ctrl Pts',(0.0133846434991609,-0.0331951640388587,
0.0716323604922125));
#96098=CARTESIAN_POINT('Ctrl Pts',(0.0134193188902374,-0.0330855618255041,
0.0717048182140676));
#96099=CARTESIAN_POINT('Ctrl Pts',(0.0134525217010637,-0.0329757224427708,
0.0717780448507424));
#96100=CARTESIAN_POINT('Ctrl Pts',(0.0134842048137788,-0.0328657862078596,
0.0718519487167388));
#96101=CARTESIAN_POINT('Ctrl Pts',(0.0132765246715118,-0.0331951640388587,
0.0715984271583301));
#96102=CARTESIAN_POINT('Ctrl Pts',(0.013311667425616,-0.0330855618255041,
0.0716693957620569));
#96103=CARTESIAN_POINT('Ctrl Pts',(0.0133453687139117,-0.0329757224427708,
0.071741141866714));
#96104=CARTESIAN_POINT('Ctrl Pts',(0.013377580873206,-0.0328657862078596,
0.0718135757140245));
#96105=CARTESIAN_POINT('Origin',(-0.00207125751478917,-0.0326401908834337,
0.0783383392173187));
#96106=CARTESIAN_POINT('Ctrl Pts',(0.0132623440873654,-0.0332451089994434,
0.0715667255935749));
#96107=CARTESIAN_POINT('Ctrl Pts',(0.0133597738756384,-0.0329451141710259,
0.0717605296262166));
#96108=CARTESIAN_POINT('Ctrl Pts',(0.01344232876415,-0.0326442513127503,
0.0719611218920045));
#96109=CARTESIAN_POINT('Ctrl Pts',(0.0131452262937048,-0.0332451089994434,
0.0713458558980347));
#96110=CARTESIAN_POINT('Ctrl Pts',(0.0132509863188348,-0.0329451141710259,
0.0715352427608197));
#96111=CARTESIAN_POINT('Ctrl Pts',(0.013342180498171,-0.0326442513127503,
0.0717320578729588));
#96112=CARTESIAN_POINT('Ctrl Pts',(0.0133775681197952,-0.0325229783203385,
0.0718135468153923));
#96113=CARTESIAN_POINT('Ctrl Pts',(0.0134097760752639,-0.032413025311208,
0.0718859701381807));
#96114=CARTESIAN_POINT('Ctrl Pts',(0.0134404809763262,-0.0323031222247695,
0.0719590487394742));
#96115=CARTESIAN_POINT('Ctrl Pts',(0.0134696467953236,-0.0321934096636184,
0.0720326876229291));
#96116=CARTESIAN_POINT('Ctrl Pts',(0.0134204867547043,-0.0325229783203385,
0.0717086700618821));
#96117=CARTESIAN_POINT('Ctrl Pts',(0.0134541404339004,-0.032413025311208,
0.0717816850171034));
#96118=CARTESIAN_POINT('Ctrl Pts',(0.013486278600741,-0.0323031222247695,
0.0718553850677491));
#96119=CARTESIAN_POINT('Ctrl Pts',(0.0135168634197456,-0.0321934096636184,
0.0719296743566597));
#96120=CARTESIAN_POINT('Ctrl Pts',(0.0134634053896135,-0.0325229783203385,
0.071603793308372));
#96121=CARTESIAN_POINT('Ctrl Pts',(0.0134985047925368,-0.032413025311208,
0.0716773998960262));
#96122=CARTESIAN_POINT('Ctrl Pts',(0.0135320762251558,-0.0323031222247695,
0.0717517213960239));
#96123=CARTESIAN_POINT('Ctrl Pts',(0.0135640800441676,-0.0321934096636184,
0.0718266610903903));
#96124=CARTESIAN_POINT('Ctrl Pts',(0.0135063240245226,-0.0325229783203385,
0.0714989165548618));
#96125=CARTESIAN_POINT('Ctrl Pts',(0.0135428691511733,-0.032413025311208,
0.0715731147749489));
#96126=CARTESIAN_POINT('Ctrl Pts',(0.0135778738495706,-0.0323031222247695,
0.0716480577242988));
#96127=CARTESIAN_POINT('Ctrl Pts',(0.0136112966685897,-0.0321934096636184,
0.0717236478241209));
#96128=CARTESIAN_POINT('Origin',(-0.00189713877787275,-0.0326393375179539,
0.0787862228185586));
#96129=CARTESIAN_POINT('Ctrl Pts',(0.0137438958601353,-0.0326943950436594,
0.0720489711163758));
#96130=CARTESIAN_POINT('Ctrl Pts',(0.0137728519758994,-0.0325844576448127,
0.0721264268159228));
#96131=CARTESIAN_POINT('Ctrl Pts',(0.0138002082300757,-0.0324744968375319,
0.0722044868570782));
#96132=CARTESIAN_POINT('Ctrl Pts',(0.0138259309517448,-0.0323646534831894,
0.0722830507413142));
#96133=CARTESIAN_POINT('Ctrl Pts',(0.0136381211726919,-0.0326943950436594,
0.0720083159435348));
#96134=CARTESIAN_POINT('Ctrl Pts',(0.0136676375929337,-0.0325844576448127,
0.0720843138696459));
#96135=CARTESIAN_POINT('Ctrl Pts',(0.013695584340386,-0.0324744968375319,
0.0721609276222118));
#96136=CARTESIAN_POINT('Ctrl Pts',(0.0137219269619956,-0.0323646534831894,
0.0722380585453385));
#96137=CARTESIAN_POINT('Ctrl Pts',(0.0135323464852486,-0.0326943950436594,
0.0719676607706938));
#96138=CARTESIAN_POINT('Ctrl Pts',(0.013562423209968,-0.0325844576448127,
0.0720422009233691));
#96139=CARTESIAN_POINT('Ctrl Pts',(0.0135909604506963,-0.0324744968375319,
0.0721173683873454));
#96140=CARTESIAN_POINT('Ctrl Pts',(0.0136179229722464,-0.0323646534831894,
0.0721930663493628));
#96141=CARTESIAN_POINT('Ctrl Pts',(0.0134265717978053,-0.0326943950436594,
0.0719270055978528));
#96142=CARTESIAN_POINT('Ctrl Pts',(0.0134572088270023,-0.0325844576448127,
0.0720000879770922));
#96143=CARTESIAN_POINT('Ctrl Pts',(0.0134863365610066,-0.0324744968375319,
0.0720738091524791));
#96144=CARTESIAN_POINT('Ctrl Pts',(0.0135139189824972,-0.0323646534831894,
0.0721480741533871));
#96145=CARTESIAN_POINT('Origin',(-0.0021060835547087,-0.0326395579068067,
0.0783531415409322));
#96146=CARTESIAN_POINT('Ctrl Pts',(0.0134143940688959,-0.0327445246961877,
0.0718944399853301));
#96147=CARTESIAN_POINT('Ctrl Pts',(0.0134994639046664,-0.0324436878365475,
0.0720939786721626));
#96148=CARTESIAN_POINT('Ctrl Pts',(0.0135692619967624,-0.0321434074463186,
0.07229935829832));
#96149=CARTESIAN_POINT('Ctrl Pts',(0.0133113743499062,-0.0327445246961877,
0.0716666529411436));
#96150=CARTESIAN_POINT('Ctrl Pts',(0.0134050353144047,-0.0324436878365475,
0.0718623061757962));
#96151=CARTESIAN_POINT('Ctrl Pts',(0.0134836927968749,-0.0321434074463186,
0.0720644585068544));
#96152=CARTESIAN_POINT('Ctrl Pts',(0.0135474455252084,-0.0322357242816072,
0.0722363644390754));
#96153=CARTESIAN_POINT('Ctrl Pts',(0.0136083923359294,-0.0319819883628705,
0.0724091010819691));
#96154=CARTESIAN_POINT('Ctrl Pts',(0.0136582239036328,-0.0317295851069886,
0.0725853658725414));
#96155=CARTESIAN_POINT('Ctrl Pts',(0.013459159366366,-0.0322357242816072,
0.0720024722541764));
#96156=CARTESIAN_POINT('Ctrl Pts',(0.0135275553398291,-0.0319819883628705,
0.0721723970974139));
#96157=CARTESIAN_POINT('Ctrl Pts',(0.0135849998964778,-0.0317295851069886,
0.0723463297983264));
#96158=CARTESIAN_POINT('Origin',(-0.00201729889068405,-0.0326371942646779,
0.0783185050430045));
#96159=CARTESIAN_POINT('Origin',(-0.00178455590506462,-0.0326352985531359,
0.0787373464468648));
#96160=CARTESIAN_POINT('Ctrl Pts',(0.0138647305447577,-0.0321934096636183,
0.0724060068739108));
#96161=CARTESIAN_POINT('Ctrl Pts',(0.013888781569152,-0.0320835708272303,
0.072485179025903));
#96162=CARTESIAN_POINT('Ctrl Pts',(0.0139111801794043,-0.0319739230346346,
0.0725648029895292));
#96163=CARTESIAN_POINT('Ctrl Pts',(0.0139319055365407,-0.0318646057455575,
0.0726447746920718));
#96164=CARTESIAN_POINT('Ctrl Pts',(0.0137617171897777,-0.0321934096636183,
0.0723587902088279));
#96165=CARTESIAN_POINT('Ctrl Pts',(0.0137864193687819,-0.0320835708272303,
0.0724365417263711));
#96166=CARTESIAN_POINT('Ctrl Pts',(0.0138094981559041,-0.0319739230346346,
0.072514759355185));
#96167=CARTESIAN_POINT('Ctrl Pts',(0.0138309317038393,-0.0318646057455575,
0.0725933407550711));
#96168=CARTESIAN_POINT('Ctrl Pts',(0.0136587038347977,-0.0321934096636183,
0.0723115735437449));
#96169=CARTESIAN_POINT('Ctrl Pts',(0.0136840571684119,-0.0320835708272303,
0.0723879044268393));
#96170=CARTESIAN_POINT('Ctrl Pts',(0.0137078161324039,-0.0319739230346346,
0.0724647157208408));
#96171=CARTESIAN_POINT('Ctrl Pts',(0.013729957871138,-0.0318646057455575,
0.0725419068180704));
#96172=CARTESIAN_POINT('Ctrl Pts',(0.0135556904798177,-0.0321934096636183,
0.072264356878662));
#96173=CARTESIAN_POINT('Ctrl Pts',(0.0135816949680418,-0.0320835708272303,
0.0723392671273075));
#96174=CARTESIAN_POINT('Ctrl Pts',(0.0136061341089037,-0.0319739230346346,
0.0724146720864966));
#96175=CARTESIAN_POINT('Ctrl Pts',(0.0136289840384366,-0.0318646057455575,
0.0724904728810697));
#96176=CARTESIAN_POINT('Ctrl Pts',(0.0135145310819095,-0.0320218834582287,
0.0721473457067602));
#96177=CARTESIAN_POINT('Ctrl Pts',(0.0135353738717159,-0.0319391099350602,
0.0722034503706395));
#96178=CARTESIAN_POINT('Ctrl Pts',(0.0135553279512123,-0.0318564869454902,
0.0722598465052138));
#96179=CARTESIAN_POINT('Ctrl Pts',(0.0135743826213311,-0.0317740741446512,
0.0723164916765391));
#96180=CARTESIAN_POINT('Ctrl Pts',(0.0135361501261414,-0.0320218834582287,
0.0721027425120963));
#96181=CARTESIAN_POINT('Ctrl Pts',(0.0135574571273767,-0.0319391099350602,
0.0721590721779623));
#96182=CARTESIAN_POINT('Ctrl Pts',(0.0135778716236106,-0.0318564869454902,
0.0722157004269268));
#96183=CARTESIAN_POINT('Ctrl Pts',(0.0135973825962061,-0.0317740741446512,
0.072272584624674));
#96184=CARTESIAN_POINT('Ctrl Pts',(0.0135577691703733,-0.0320218834582287,
0.0720581393174323));
#96185=CARTESIAN_POINT('Ctrl Pts',(0.0135795403830375,-0.0319391099350602,
0.072114693985285));
#96186=CARTESIAN_POINT('Ctrl Pts',(0.0136004152960088,-0.0318564869454902,
0.0721715543486399));
#96187=CARTESIAN_POINT('Ctrl Pts',(0.0136203825710811,-0.0317740741446512,
0.0722286775728089));
#96188=CARTESIAN_POINT('Ctrl Pts',(0.0135793882146052,-0.0320218834582287,
0.0720135361227683));
#96189=CARTESIAN_POINT('Ctrl Pts',(0.0136016236386984,-0.0319391099350602,
0.0720703157926078));
#96190=CARTESIAN_POINT('Ctrl Pts',(0.013622958968407,-0.0318564869454902,
0.0721274082703529));
#96191=CARTESIAN_POINT('Ctrl Pts',(0.0136433825459561,-0.0317740741446512,
0.0721847705209438));
#96192=CARTESIAN_POINT('Origin',(0.0190833712827904,-0.0391228853390731,
0.0690737784410806));
#96193=CARTESIAN_POINT('Ctrl Pts',(0.0117449661544827,-0.0352722978779542,
0.0696810861207133));
#96194=CARTESIAN_POINT('Ctrl Pts',(0.0117594251069067,-0.0352466642097181,
0.0696932529351193));
#96195=CARTESIAN_POINT('Ctrl Pts',(0.011773921656746,-0.0352210183808283,
0.0697053489218047));
#96196=CARTESIAN_POINT('Ctrl Pts',(0.0117884566567382,-0.0351953608940152,
0.0697173740987455));
#96197=CARTESIAN_POINT('Origin',(0.0150362787244069,-0.0352456003065003,
0.0660510716909158));
#96198=CARTESIAN_POINT('Ctrl Pts',(0.0118827372491286,-0.035024121149334,
0.0697989613852351));
#96199=CARTESIAN_POINT('Ctrl Pts',(0.0119426710193492,-0.0349144232867421,
0.0698507394475655));
#96200=CARTESIAN_POINT('Ctrl Pts',(0.0120015703733199,-0.0348045283677512,
0.0699037873753614));
#96201=CARTESIAN_POINT('Ctrl Pts',(0.0120593573399695,-0.0346945769586886,
0.069958040028368));
#96202=CARTESIAN_POINT('Ctrl Pts',(0.0118769168623412,-0.035024121149334,
0.0696857921981716));
#96203=CARTESIAN_POINT('Ctrl Pts',(0.0119384094916422,-0.0349144232867421,
0.0697374900870641));
#96204=CARTESIAN_POINT('Ctrl Pts',(0.0119988702949877,-0.0348045283677512,
0.0697904900161641));
#96205=CARTESIAN_POINT('Ctrl Pts',(0.0120582193035762,-0.0346945769586886,
0.0698447269811222));
#96206=CARTESIAN_POINT('Ctrl Pts',(0.0118710964755538,-0.035024121149334,
0.0695726230111081));
#96207=CARTESIAN_POINT('Ctrl Pts',(0.0119341479639352,-0.0349144232867422,
0.0696242407265627));
#96208=CARTESIAN_POINT('Ctrl Pts',(0.0119961702166554,-0.0348045283677512,
0.0696771926569668));
#96209=CARTESIAN_POINT('Ctrl Pts',(0.0120570812671828,-0.0346945769586886,
0.0697314139338764));
#96210=CARTESIAN_POINT('Ctrl Pts',(0.0118652760887664,-0.035024121149334,
0.0694594538240447));
#96211=CARTESIAN_POINT('Ctrl Pts',(0.0119298864362281,-0.0349144232867422,
0.0695109913660613));
#96212=CARTESIAN_POINT('Ctrl Pts',(0.0119934701383231,-0.0348045283677512,
0.0695638952977694));
#96213=CARTESIAN_POINT('Ctrl Pts',(0.0120559432307895,-0.0346945769586886,
0.0696181008866307));
#96214=CARTESIAN_POINT('Origin',(0.000437479737908236,-0.0345629067945187,
0.0820739349628899));
#96215=CARTESIAN_POINT('Ctrl Pts',(0.0122209024820182,-0.0351970973651652,
0.0698617454465175));
#96216=CARTESIAN_POINT('Ctrl Pts',(0.0122803104372427,-0.0350869349321816,
0.0699185054955392));
#96217=CARTESIAN_POINT('Ctrl Pts',(0.0123385875953615,-0.0349764985129772,
0.0699765476223919));
#96218=CARTESIAN_POINT('Ctrl Pts',(0.0123956540301704,-0.0348659306849697,
0.070035801076154));
#96219=CARTESIAN_POINT('Ctrl Pts',(0.0121389001123545,-0.0351970973651652,
0.0698677522775772));
#96220=CARTESIAN_POINT('Ctrl Pts',(0.0121982248510754,-0.0350869349321816,
0.0699233762949));
#96221=CARTESIAN_POINT('Ctrl Pts',(0.0122564423412243,-0.0349764985129772,
0.0699802797189535));
#96222=CARTESIAN_POINT('Ctrl Pts',(0.0123134728207393,-0.0348659306849697,
0.0700383932694884));
#96223=CARTESIAN_POINT('Ctrl Pts',(0.0120568977426908,-0.0351970973651652,
0.0698737591086368));
#96224=CARTESIAN_POINT('Ctrl Pts',(0.012116139264908,-0.0350869349321816,
0.0699282470942608));
#96225=CARTESIAN_POINT('Ctrl Pts',(0.0121742970870872,-0.0349764985129772,
0.0699840118155151));
#96226=CARTESIAN_POINT('Ctrl Pts',(0.0122312916113082,-0.0348659306849698,
0.0700409854628228));
#96227=CARTESIAN_POINT('Ctrl Pts',(0.0119748953730271,-0.0351970973651652,
0.0698797659396964));
#96228=CARTESIAN_POINT('Ctrl Pts',(0.0120340536787406,-0.0350869349321816,
0.0699331178936216));
#96229=CARTESIAN_POINT('Ctrl Pts',(0.0120921518329501,-0.0349764985129772,
0.0699877439120767));
#96230=CARTESIAN_POINT('Ctrl Pts',(0.0121491104018771,-0.0348659306849698,
0.0700435776561572));
#96231=CARTESIAN_POINT('Origin',(0.000125454551840935,-0.0345637187966511,
0.0817079217938938));
#96232=CARTESIAN_POINT('Ctrl Pts',(0.0119505339817063,-0.0352450361861253,
0.0698565054153448));
#96233=CARTESIAN_POINT('Ctrl Pts',(0.0121124657829775,-0.0349452761023765,
0.0700008337236558));
#96234=CARTESIAN_POINT('Ctrl Pts',(0.0122630661546245,-0.0346444289983475,
0.0701569493759862));
#96235=CARTESIAN_POINT('Ctrl Pts',(0.0117603332233854,-0.0352450361861253,
0.0696942597018911));
#96236=CARTESIAN_POINT('Ctrl Pts',(0.0119283842219934,-0.0349452761023765,
0.0698314144710741));
#96237=CARTESIAN_POINT('Ctrl Pts',(0.0120856267472876,-0.0346444289983475,
0.0699808378865146));
#96238=CARTESIAN_POINT('Ctrl Pts',(0.0121485231283809,-0.0345231616327822,
0.0700435731874319));
#96239=CARTESIAN_POINT('Ctrl Pts',(0.0122051244406053,-0.0344132092796975,
0.0700990485748423));
#96240=CARTESIAN_POINT('Ctrl Pts',(0.0122605753678319,-0.0343032738558974,
0.0701556918534746));
#96241=CARTESIAN_POINT('Ctrl Pts',(0.012314806729835,-0.034193496108874,
0.0702134286370508));
#96242=CARTESIAN_POINT('Ctrl Pts',(0.012149820160417,-0.0345231616327822,
0.0699302618735825));
#96243=CARTESIAN_POINT('Ctrl Pts',(0.0122079833095732,-0.0344132092796975,
0.0699857551387534));
#96244=CARTESIAN_POINT('Ctrl Pts',(0.0122649956233607,-0.0343032738558974,
0.0700424485995888));
#96245=CARTESIAN_POINT('Ctrl Pts',(0.0123207859228837,-0.034193496108874,
0.0701002677542826));
#96246=CARTESIAN_POINT('Ctrl Pts',(0.012151117192453,-0.0345231616327822,
0.069816950559733));
#96247=CARTESIAN_POINT('Ctrl Pts',(0.0122108421785411,-0.0344132092796975,
0.0698724617026645));
#96248=CARTESIAN_POINT('Ctrl Pts',(0.0122694158788894,-0.0343032738558974,
0.069929205345703));
#96249=CARTESIAN_POINT('Ctrl Pts',(0.0123267651159325,-0.034193496108874,
0.0699871068715144));
#96250=CARTESIAN_POINT('Ctrl Pts',(0.0121524142244891,-0.0345231616327822,
0.0697036392458835));
#96251=CARTESIAN_POINT('Ctrl Pts',(0.012213701047509,-0.0344132092796975,
0.0697591682665756));
#96252=CARTESIAN_POINT('Ctrl Pts',(0.0122738361344182,-0.0343032738558974,
0.0698159620918172));
#96253=CARTESIAN_POINT('Ctrl Pts',(0.0123327443089813,-0.034193496108874,
0.0698739459887462));
#96254=CARTESIAN_POINT('Origin',(0.000429234047500226,-0.0345625596230095,
0.0820827953746281));
#96255=CARTESIAN_POINT('Ctrl Pts',(0.0125757914107657,-0.0346945769586885,
0.0701276109181229));
#96256=CARTESIAN_POINT('Ctrl Pts',(0.0126312219653004,-0.0345846629178476,
0.0701889618552662));
#96257=CARTESIAN_POINT('Ctrl Pts',(0.0126853932753282,-0.034474692505516,
0.0702514695524017));
#96258=CARTESIAN_POINT('Ctrl Pts',(0.0127382362610932,-0.0343648066260528,
0.0703150536308093));
#96259=CARTESIAN_POINT('Ctrl Pts',(0.0124624784527354,-0.0346945769586885,
0.0701287489536201));
#96260=CARTESIAN_POINT('Ctrl Pts',(0.0125178933245658,-0.0345846629178476,
0.0701885383809315));
#96261=CARTESIAN_POINT('Ctrl Pts',(0.0125720812405926,-0.034474692505516,
0.0702494839772133));
#96262=CARTESIAN_POINT('Ctrl Pts',(0.0126249730915163,-0.0343648066260528,
0.0703115073652014));
#96263=CARTESIAN_POINT('Ctrl Pts',(0.0123491654947052,-0.0346945769586885,
0.0701298869891174));
#96264=CARTESIAN_POINT('Ctrl Pts',(0.0124045646838312,-0.0345846629178476,
0.0701881149065968));
#96265=CARTESIAN_POINT('Ctrl Pts',(0.012458769205857,-0.034474692505516,
0.0702474984020249));
#96266=CARTESIAN_POINT('Ctrl Pts',(0.0125117099219394,-0.0343648066260528,
0.0703079610995936));
#96267=CARTESIAN_POINT('Ctrl Pts',(0.0122358525366749,-0.0346945769586885,
0.0701310250246147));
#96268=CARTESIAN_POINT('Ctrl Pts',(0.0122912360430966,-0.0345846629178476,
0.070187691432262));
#96269=CARTESIAN_POINT('Ctrl Pts',(0.0123454571711213,-0.034474692505516,
0.0702455128268366));
#96270=CARTESIAN_POINT('Ctrl Pts',(0.0123984467523625,-0.0343648066260528,
0.0703044148339857));
#96271=CARTESIAN_POINT('Origin',(8.35237049665021E-5,-0.0345626446730908,
0.0817486149715776));
#96272=CARTESIAN_POINT('Ctrl Pts',(0.0122378800854608,-0.0346945769586887,
0.0701310046613435));
#96273=CARTESIAN_POINT('Ctrl Pts',(0.0123220595519455,-0.0345275153362892,
0.0702171760888924));
#96274=CARTESIAN_POINT('Ctrl Pts',(0.012403550779471,-0.034360323596516,
0.0703060171715252));
#96275=CARTESIAN_POINT('Ctrl Pts',(0.0124821166583466,-0.0341934961088741,
0.0703972615746474));
#96276=CARTESIAN_POINT('Ctrl Pts',(0.0121780086263968,-0.0346945769586887,
0.0700723238576612));
#96277=CARTESIAN_POINT('Ctrl Pts',(0.0122634171858091,-0.0345275153362892,
0.0701572412535287));
#96278=CARTESIAN_POINT('Ctrl Pts',(0.0123461772623108,-0.034360323596516,
0.0702448666339647));
#96279=CARTESIAN_POINT('Ctrl Pts',(0.0124260479400804,-0.0341934961088741,
0.0703349372041072));
#96280=CARTESIAN_POINT('Ctrl Pts',(0.0121181371673327,-0.0346945769586887,
0.0700136430539788));
#96281=CARTESIAN_POINT('Ctrl Pts',(0.0122047748196728,-0.0345275153362892,
0.070097306418165));
#96282=CARTESIAN_POINT('Ctrl Pts',(0.0122888037451505,-0.034360323596516,
0.0701837160964042));
#96283=CARTESIAN_POINT('Ctrl Pts',(0.0123699792218141,-0.0341934961088741,
0.070272612833567));
#96284=CARTESIAN_POINT('Ctrl Pts',(0.0120582657082687,-0.0346945769586887,
0.0699549622502964));
#96285=CARTESIAN_POINT('Ctrl Pts',(0.0121461324535364,-0.0345275153362892,
0.0700373715828014));
#96286=CARTESIAN_POINT('Ctrl Pts',(0.0122314302279902,-0.034360323596516,
0.0701225655588437));
#96287=CARTESIAN_POINT('Ctrl Pts',(0.0123139105035478,-0.0341934961088741,
0.0702102884630267));
#96288=CARTESIAN_POINT('Ctrl Pts',(0.0123984252348696,-0.0340223579322365,
0.0703043917482794));
#96289=CARTESIAN_POINT('Ctrl Pts',(0.0124514662024277,-0.0339125849573554,
0.0703633502245619));
#96290=CARTESIAN_POINT('Ctrl Pts',(0.0125032495952535,-0.0338030433565221,
0.0704233650961839));
#96291=CARTESIAN_POINT('Ctrl Pts',(0.0125537159945839,-0.0336938721132327,
0.0704843537439186));
#96292=CARTESIAN_POINT('Ctrl Pts',(0.0124068345799588,-0.0340223579322365,
0.0701913852761399));
#96293=CARTESIAN_POINT('Ctrl Pts',(0.0124614342015009,-0.0339125849573554,
0.0702504597392235));
#96294=CARTESIAN_POINT('Ctrl Pts',(0.0125147727524054,-0.0338030433565221,
0.0703106227766599));
#96295=CARTESIAN_POINT('Ctrl Pts',(0.0125667888419205,-0.0336938721132327,
0.0703717914034456));
#96296=CARTESIAN_POINT('Ctrl Pts',(0.0124152439250479,-0.0340223579322365,
0.0700783788040003));
#96297=CARTESIAN_POINT('Ctrl Pts',(0.012471402200574,-0.0339125849573554,
0.0701375692538852));
#96298=CARTESIAN_POINT('Ctrl Pts',(0.0125262959095572,-0.0338030433565221,
0.0701978804571359));
#96299=CARTESIAN_POINT('Ctrl Pts',(0.0125798616892571,-0.0336938721132327,
0.0702592290629725));
#96300=CARTESIAN_POINT('Ctrl Pts',(0.012423653270137,-0.0340223579322365,
0.0699653723318607));
#96301=CARTESIAN_POINT('Ctrl Pts',(0.0124813701996472,-0.0339125849573554,
0.0700246787685469));
#96302=CARTESIAN_POINT('Ctrl Pts',(0.012537819066709,-0.0338030433565221,
0.0700851381376119));
#96303=CARTESIAN_POINT('Ctrl Pts',(0.0125929345365937,-0.0336938721132327,
0.0701466667224994));
#96304=CARTESIAN_POINT('Origin',(0.000514778422947674,-0.0345589643415595,
0.0819983262209085));
#96305=CARTESIAN_POINT('Ctrl Pts',(0.0128195742877403,-0.034193496108874,
0.0704150921558745));
#96306=CARTESIAN_POINT('Ctrl Pts',(0.0128710764551861,-0.0340836138581106,
0.0704798443481219));
#96307=CARTESIAN_POINT('Ctrl Pts',(0.0129212140001739,-0.0339738896643499,
0.0705456312003391));
#96308=CARTESIAN_POINT('Ctrl Pts',(0.0129699283971121,-0.0338644633294062,
0.0706123642118589));
#96309=CARTESIAN_POINT('Ctrl Pts',(0.0127064133031482,-0.034193496108874,
0.0704091129574456));
#96310=CARTESIAN_POINT('Ctrl Pts',(0.0127579979201997,-0.0340836138581106,
0.0704723047267267));
#96311=CARTESIAN_POINT('Ctrl Pts',(0.0128082501649112,-0.0339738896643499,
0.0705365336108195));
#96312=CARTESIAN_POINT('Ctrl Pts',(0.0128571112312219,-0.0338644633294062,
0.0706017130932228));
#96313=CARTESIAN_POINT('Ctrl Pts',(0.0125932523185562,-0.034193496108874,
0.0704031337590166));
#96314=CARTESIAN_POINT('Ctrl Pts',(0.0126449193852132,-0.0340836138581106,
0.0704647651053315));
#96315=CARTESIAN_POINT('Ctrl Pts',(0.0126952863296485,-0.0339738896643499,
0.0705274360212999));
#96316=CARTESIAN_POINT('Ctrl Pts',(0.0127442940653318,-0.0338644633294062,
0.0705910619745866));
#96317=CARTESIAN_POINT('Ctrl Pts',(0.0124800913339641,-0.034193496108874,
0.0703971545605877));
#96318=CARTESIAN_POINT('Ctrl Pts',(0.0125318408502268,-0.0340836138581106,
0.0704572254839363));
#96319=CARTESIAN_POINT('Ctrl Pts',(0.0125823224943859,-0.0339738896643499,
0.0705183384317803));
#96320=CARTESIAN_POINT('Ctrl Pts',(0.0126314768994416,-0.0338644633294062,
0.0705804108559505));
#96321=CARTESIAN_POINT('Origin',(0.000139010950174352,-0.0345610621862704,
0.081697745419754));
#96322=CARTESIAN_POINT('Ctrl Pts',(0.0124584248656429,-0.0342436276873901,
0.0703699209133347));
#96323=CARTESIAN_POINT('Ctrl Pts',(0.0126009928986574,-0.0339430054201861,
0.0705334046567898));
#96324=CARTESIAN_POINT('Ctrl Pts',(0.0127308416454257,-0.0336441434784164,
0.0707071627684692));
#96325=CARTESIAN_POINT('Ctrl Pts',(0.0122900561545809,-0.0342436276873901,
0.0701851183778129));
#96326=CARTESIAN_POINT('Ctrl Pts',(0.0124395941301235,-0.0339430054201861,
0.0703422519906471));
#96327=CARTESIAN_POINT('Ctrl Pts',(0.0125768713364009,-0.0336441434784164,
0.0705102030163908));
#96328=CARTESIAN_POINT('Ctrl Pts',(0.0126314595844677,-0.0335235895815127,
0.0705803891944784));
#96329=CARTESIAN_POINT('Ctrl Pts',(0.0126806023051219,-0.0334144449262719,
0.0706424462485696));
#96330=CARTESIAN_POINT('Ctrl Pts',(0.0127285194327741,-0.0333049234473133,
0.0707055898503223));
#96331=CARTESIAN_POINT('Ctrl Pts',(0.0127751423822346,-0.0331951640388588,
0.0707697448086749));
#96332=CARTESIAN_POINT('Ctrl Pts',(0.0126469481174946,-0.0335235895815127,
0.0704681337811082));
#96333=CARTESIAN_POINT('Ctrl Pts',(0.0126976362549244,-0.0334144449262719,
0.0705304040653507));
#96334=CARTESIAN_POINT('Ctrl Pts',(0.0127470961696743,-0.0333049234473133,
0.0705937930693777));
#96335=CARTESIAN_POINT('Ctrl Pts',(0.012795257275379,-0.0331951640388588,
0.0706582254670339));
#96336=CARTESIAN_POINT('Ctrl Pts',(0.0126624366505214,-0.0335235895815127,
0.070355878367738));
#96337=CARTESIAN_POINT('Ctrl Pts',(0.0127146702047269,-0.0334144449262719,
0.0704183618821317));
#96338=CARTESIAN_POINT('Ctrl Pts',(0.0127656729065746,-0.0333049234473133,
0.0704819962884332));
#96339=CARTESIAN_POINT('Ctrl Pts',(0.0128153721685233,-0.0331951640388588,
0.0705467061253931));
#96340=CARTESIAN_POINT('Ctrl Pts',(0.0126779251835483,-0.0335235895815127,
0.0702436229543678));
#96341=CARTESIAN_POINT('Ctrl Pts',(0.0127317041545293,-0.0334144449262719,
0.0703063196989127));
#96342=CARTESIAN_POINT('Ctrl Pts',(0.0127842496434748,-0.0333049234473133,
0.0703701995074886));
#96343=CARTESIAN_POINT('Ctrl Pts',(0.0128354870616677,-0.0331951640388588,
0.0704351867837521));
#96344=CARTESIAN_POINT('Origin',(-0.00114102305421436,-0.0326434571769475,
0.0799420498962871));
#96345=CARTESIAN_POINT('Ctrl Pts',(0.0130468390514737,-0.0336938721132369,
0.0707175472757866));
#96346=CARTESIAN_POINT('Ctrl Pts',(0.0130669303362767,-0.0336474569764948,
0.0707463635612215));
#96347=CARTESIAN_POINT('Ctrl Pts',(0.0130866829134076,-0.033601104548885,
0.0707754130660018));
#96348=CARTESIAN_POINT('Ctrl Pts',(0.0131366918951498,-0.033483750864316,
0.0708489597300422));
#96349=CARTESIAN_POINT('Ctrl Pts',(0.0131844995765855,-0.0333660264760404,
0.0709239559675618));
#96350=CARTESIAN_POINT('Ctrl Pts',(0.01270915287623,-0.0336938721132369,
0.0706783288320508));
#96351=CARTESIAN_POINT('Ctrl Pts',(0.0127294737195982,-0.0336474569764948,
0.0707051685282458));
#96352=CARTESIAN_POINT('Ctrl Pts',(0.0127494789780375,-0.033601104548885,
0.0707322442664963));
#96353=CARTESIAN_POINT('Ctrl Pts',(0.0128001276907301,-0.033483750864316,
0.0708007938076956));
#96354=CARTESIAN_POINT('Ctrl Pts',(0.0128487228972976,-0.0333660264760404,
0.0708708140732955));
#96355=CARTESIAN_POINT('Ctrl Pts',(0.0127091528762419,-0.0336938721132426,
0.0706783288320632));
#96356=CARTESIAN_POINT('Ctrl Pts',(0.0127294737196091,-0.0336474569765026,
0.070705168528257));
#96357=CARTESIAN_POINT('Ctrl Pts',(0.0127494789780475,-0.0336011045488949,
0.0707322442665063));
#96358=CARTESIAN_POINT('Ctrl Pts',(0.012799705855949,-0.0334847282606778,
0.0708002228833947));
#96359=CARTESIAN_POINT('Ctrl Pts',(0.0128479134659113,-0.0333679869945434,
0.070869648080258));
#96360=CARTESIAN_POINT('Ctrl Pts',(0.0127091528762275,-0.0336938721132427,
0.0706783288320474));
#96361=CARTESIAN_POINT('Ctrl Pts',(0.0127818292049813,-0.0335278710435083,
0.0707743194633896));
#96362=CARTESIAN_POINT('Ctrl Pts',(0.0128514697251298,-0.033362046922432,
0.070872555436225));
#96363=CARTESIAN_POINT('Ctrl Pts',(0.0129180927308868,-0.0331951640388602,
0.0709730971895022));
#96364=CARTESIAN_POINT('Ctrl Pts',(0.0126571081708501,-0.0336938721132427,
0.0706126068534904));
#96365=CARTESIAN_POINT('Ctrl Pts',(0.0127311603304038,-0.0335278710435083,
0.0707075079755056));
#96366=CARTESIAN_POINT('Ctrl Pts',(0.0128022103640674,-0.033362046922432,
0.0708046979679969));
#96367=CARTESIAN_POINT('Ctrl Pts',(0.0128702774410251,-0.0331951640388602,
0.0709042369841676));
#96368=CARTESIAN_POINT('Ctrl Pts',(0.0126050634654727,-0.0336938721132427,
0.0705468848749333));
#96369=CARTESIAN_POINT('Ctrl Pts',(0.0126804914558263,-0.0335278710435083,
0.0706406964876216));
#96370=CARTESIAN_POINT('Ctrl Pts',(0.0127529510030049,-0.033362046922432,
0.0707368404997688));
#96371=CARTESIAN_POINT('Ctrl Pts',(0.0128224621511635,-0.0331951640388602,
0.070835376778833));
#96372=CARTESIAN_POINT('Ctrl Pts',(0.0125530187600953,-0.0336938721132427,
0.0704811628963763));
#96373=CARTESIAN_POINT('Ctrl Pts',(0.0126298225812489,-0.0335278710435083,
0.0705738849997375));
#96374=CARTESIAN_POINT('Ctrl Pts',(0.0127036916419425,-0.033362046922432,
0.0706689830315406));
#96375=CARTESIAN_POINT('Ctrl Pts',(0.0127746468613019,-0.0331951640388602,
0.0707665165734984));
#96376=CARTESIAN_POINT('Ctrl Pts',(0.0128467020004684,-0.0330240426238155,
0.0708704711812222));
#96377=CARTESIAN_POINT('Ctrl Pts',(0.0128918807050369,-0.0329142774063509,
0.070935534002886));
#96378=CARTESIAN_POINT('Ctrl Pts',(0.0129357369025695,-0.0328043479726686,
0.0710015632307633));
#96379=CARTESIAN_POINT('Ctrl Pts',(0.0129782120804626,-0.0326943950436594,
0.0710684758237667));
#96380=CARTESIAN_POINT('Ctrl Pts',(0.0128692084963612,-0.0330240426238155,
0.0707594099655474));
#96381=CARTESIAN_POINT('Ctrl Pts',(0.0129159171773774,-0.0329142774063509,
0.0708247828361192));
#96382=CARTESIAN_POINT('Ctrl Pts',(0.0129612977045297,-0.0328043479726686,
0.070891153896362));
#96383=CARTESIAN_POINT('Ctrl Pts',(0.0130052896003746,-0.0326943950436594,
0.0709584397210552));
#96384=CARTESIAN_POINT('Ctrl Pts',(0.0128917149922541,-0.0330240426238155,
0.0706483487498726));
#96385=CARTESIAN_POINT('Ctrl Pts',(0.0129399536497178,-0.0329142774063509,
0.0707140316693524));
#96386=CARTESIAN_POINT('Ctrl Pts',(0.0129868585064898,-0.0328043479726686,
0.0707807445619608));
#96387=CARTESIAN_POINT('Ctrl Pts',(0.0130323671202866,-0.0326943950436594,
0.0708484036183436));
#96388=CARTESIAN_POINT('Ctrl Pts',(0.0129142214881469,-0.0330240426238155,
0.0705372875341979));
#96389=CARTESIAN_POINT('Ctrl Pts',(0.0129639901220583,-0.0329142774063509,
0.0706032805025856));
#96390=CARTESIAN_POINT('Ctrl Pts',(0.0130124193084499,-0.0328043479726686,
0.0706703352275596));
#96391=CARTESIAN_POINT('Ctrl Pts',(0.0130594446401986,-0.0326943950436594,
0.0707383675156321));
#96392=CARTESIAN_POINT('Origin',(-0.0012443999145456,-0.0326396682858909,
0.0800099367397309));
#96393=CARTESIAN_POINT('Ctrl Pts',(0.0132506546416792,-0.0331951640388587,
0.0710330818271546));
#96394=CARTESIAN_POINT('Ctrl Pts',(0.0132935838840361,-0.0330855618255041,
0.0711036941235551));
#96395=CARTESIAN_POINT('Ctrl Pts',(0.0133350846380184,-0.0329757224427708,
0.0711752445974313));
#96396=CARTESIAN_POINT('Ctrl Pts',(0.0133750992650374,-0.0328657862078596,
0.07124764423094));
#96397=CARTESIAN_POINT('Ctrl Pts',(0.0131391353888191,-0.0331951640388587,
0.0710129669500237));
#96398=CARTESIAN_POINT('Ctrl Pts',(0.0131823416729163,-0.0330855618255041,
0.0710820432943177));
#96399=CARTESIAN_POINT('Ctrl Pts',(0.0132241514138591,-0.0329757224427708,
0.0711520624348202));
#96400=CARTESIAN_POINT('Ctrl Pts',(0.0132645066735717,-0.0328657862078596,
0.071222937334061));
#96401=CARTESIAN_POINT('Ctrl Pts',(0.0130276161359589,-0.0331951640388587,
0.0709928520728929));
#96402=CARTESIAN_POINT('Ctrl Pts',(0.0130710994617965,-0.0330855618255041,
0.0710603924650804));
#96403=CARTESIAN_POINT('Ctrl Pts',(0.0131132181896998,-0.0329757224427708,
0.0711288802722091));
#96404=CARTESIAN_POINT('Ctrl Pts',(0.013153914082106,-0.0328657862078596,
0.0711982304371821));
#96405=CARTESIAN_POINT('Ctrl Pts',(0.0129160968830987,-0.0331951640388587,
0.070972737195762));
#96406=CARTESIAN_POINT('Ctrl Pts',(0.0129598572506768,-0.0330855618255041,
0.071038741635843));
#96407=CARTESIAN_POINT('Ctrl Pts',(0.0130022849655405,-0.0329757224427708,
0.071105698109598));
#96408=CARTESIAN_POINT('Ctrl Pts',(0.0130433214906403,-0.0328657862078596,
0.0711735235403031));
#96409=CARTESIAN_POINT('Origin',(-0.00146592848484389,-0.0326401908829356,
0.0795830902040864));
#96410=CARTESIAN_POINT('Ctrl Pts',(0.012898054857474,-0.0332451089994433,
0.0709430629057787));
#96411=CARTESIAN_POINT('Ctrl Pts',(0.0130190064688544,-0.0329451141710259,
0.0711231275453268));
#96412=CARTESIAN_POINT('Ctrl Pts',(0.0131260512647113,-0.0326442513127504,
0.0713117912100612));
#96413=CARTESIAN_POINT('Ctrl Pts',(0.0127541782594593,-0.0332451089994433,
0.0707386135855457));
#96414=CARTESIAN_POINT('Ctrl Pts',(0.0128828408031097,-0.0329451141710259,
0.0709132518304192));
#96415=CARTESIAN_POINT('Ctrl Pts',(0.0129979833635221,-0.0326442513127504,
0.0710970853352348));
#96416=CARTESIAN_POINT('Ctrl Pts',(0.013043305215835,-0.0325229783203385,
0.0711734964679713));
#96417=CARTESIAN_POINT('Ctrl Pts',(0.0130843362511853,-0.0324130253112079,
0.0712413119840224));
#96418=CARTESIAN_POINT('Ctrl Pts',(0.0131239582123361,-0.0323031222247695,
0.0713099659941807));
#96419=CARTESIAN_POINT('Ctrl Pts',(0.0131621234495188,-0.0321934096636184,
0.0713793687666401));
#96420=CARTESIAN_POINT('Ctrl Pts',(0.0130727408818455,-0.0325229783203385,
0.0710640675676944));
#96421=CARTESIAN_POINT('Ctrl Pts',(0.0131152803921657,-0.0324130253112079,
0.0711322888537504));
#96422=CARTESIAN_POINT('Ctrl Pts',(0.0131564022056229,-0.0323031222247695,
0.0712013797771125));
#96423=CARTESIAN_POINT('Ctrl Pts',(0.0131960567709927,-0.0321934096636184,
0.0712712499785271));
#96424=CARTESIAN_POINT('Ctrl Pts',(0.0131021765478561,-0.0325229783203385,
0.0709546386674175));
#96425=CARTESIAN_POINT('Ctrl Pts',(0.013146224533146,-0.0324130253112079,
0.0710232657234783));
#96426=CARTESIAN_POINT('Ctrl Pts',(0.0131888461989096,-0.0323031222247695,
0.0710927935600443));
#96427=CARTESIAN_POINT('Ctrl Pts',(0.0132299900924667,-0.0321934096636184,
0.071163131190414));
#96428=CARTESIAN_POINT('Ctrl Pts',(0.0131316122138666,-0.0325229783203385,
0.0708452097671406));
#96429=CARTESIAN_POINT('Ctrl Pts',(0.0131771686741264,-0.0324130253112079,
0.0709142425932062));
#96430=CARTESIAN_POINT('Ctrl Pts',(0.0132212901921964,-0.0323031222247695,
0.0709842073429761));
#96431=CARTESIAN_POINT('Ctrl Pts',(0.0132639234139407,-0.0321934096636184,
0.0710550124023009));
#96432=CARTESIAN_POINT('Origin',(-0.00123704802509541,-0.0326393375182704,
0.0800056192456978));
#96433=CARTESIAN_POINT('Ctrl Pts',(0.0134362508414271,-0.0326943950436593,
0.0713611513377825));
#96434=CARTESIAN_POINT('Ctrl Pts',(0.0134746864028517,-0.0325844576448127,
0.0714343671123835));
#96435=CARTESIAN_POINT('Ctrl Pts',(0.0135116104621632,-0.0324744968375319,
0.0715083829790049));
#96436=CARTESIAN_POINT('Ctrl Pts',(0.0135469770181415,-0.0323646534831895,
0.071583103451665));
#96437=CARTESIAN_POINT('Ctrl Pts',(0.0133262147747145,-0.0326943950436593,
0.0713340738267291));
#96438=CARTESIAN_POINT('Ctrl Pts',(0.0133650235149901,-0.0325844576448127,
0.0714057730981012));
#96439=CARTESIAN_POINT('Ctrl Pts',(0.0134023521433361,-0.0324744968375319,
0.0714782800721189));
#96440=CARTESIAN_POINT('Ctrl Pts',(0.0134381541135094,-0.0323646534831895,
0.071551501188932));
#96441=CARTESIAN_POINT('Ctrl Pts',(0.0132161787080019,-0.0326943950436593,
0.0713069963156756));
#96442=CARTESIAN_POINT('Ctrl Pts',(0.0132553606271285,-0.0325844576448127,
0.0713771790838189));
#96443=CARTESIAN_POINT('Ctrl Pts',(0.0132930938245091,-0.0324744968375319,
0.0714481771652329));
#96444=CARTESIAN_POINT('Ctrl Pts',(0.0133293312088772,-0.0323646534831895,
0.071519898926199));
#96445=CARTESIAN_POINT('Ctrl Pts',(0.0131061426412893,-0.0326943950436593,
0.0712799188046222));
#96446=CARTESIAN_POINT('Ctrl Pts',(0.0131456977392669,-0.0325844576448127,
0.0713485850695366));
#96447=CARTESIAN_POINT('Ctrl Pts',(0.013183835505682,-0.0324744968375319,
0.0714180742583469));
#96448=CARTESIAN_POINT('Ctrl Pts',(0.0132205083042451,-0.0323646534831895,
0.071488296663466));
#96449=CARTESIAN_POINT('Origin',(-0.00149862468699762,-0.0326395579068937,
0.0796021406675311));
#96450=CARTESIAN_POINT('Ctrl Pts',(0.0130899793838892,-0.0327445246961878,
0.0712491362558227));
#96451=CARTESIAN_POINT('Ctrl Pts',(0.0131993872474374,-0.0324436878365475,
0.0714364394429143));
#96452=CARTESIAN_POINT('Ctrl Pts',(0.0132943758533842,-0.0321434074463186,
0.0716314515687966));
#96453=CARTESIAN_POINT('Ctrl Pts',(0.0129592227193422,-0.0327445246961878,
0.0710360571750181));
#96454=CARTESIAN_POINT('Ctrl Pts',(0.0130766669917168,-0.0324436878365475,
0.0712184287939373));
#96455=CARTESIAN_POINT('Ctrl Pts',(0.0131800406417681,-0.0321434074463186,
0.0714091286968632));
#96456=CARTESIAN_POINT('Ctrl Pts',(0.0132648361871507,-0.0322357242816073,
0.0715716887638722));
#96457=CARTESIAN_POINT('Ctrl Pts',(0.0133469520560742,-0.0319819883628706,
0.0717354246658798));
#96458=CARTESIAN_POINT('Ctrl Pts',(0.0134184825231483,-0.0317295851069886,
0.0719040540044168));
#96459=CARTESIAN_POINT('Ctrl Pts',(0.0131479317272018,-0.0322357242816073,
0.0713507060784779));
#96460=CARTESIAN_POINT('Ctrl Pts',(0.0132370856080511,-0.0319819883628706,
0.0715107187250557));
#96461=CARTESIAN_POINT('Ctrl Pts',(0.0133158767450407,-0.0317295851069886,
0.0716760802026348));
#96462=CARTESIAN_POINT('Origin',(-0.00141488122122914,-0.0326371942647059,
0.0795566496198092));
#96463=CARTESIAN_POINT('Origin',(-0.00113147873671373,-0.0326352985528954,
0.0799430179030252));
#96464=CARTESIAN_POINT('Ctrl Pts',(0.0136008811544591,-0.0321934096636183,
0.0717002271599773));
#96465=CARTESIAN_POINT('Ctrl Pts',(0.0136346654311598,-0.0320835708272304,
0.0717757606232456));
#96466=CARTESIAN_POINT('Ctrl Pts',(0.0136668669505106,-0.0319739230346346,
0.0718519494378859));
#96467=CARTESIAN_POINT('Ctrl Pts',(0.0136974519940889,-0.0318646057455575,
0.0719286929636407));
#96468=CARTESIAN_POINT('Ctrl Pts',(0.013492762273239,-0.0321934096636183,
0.0716662938092816));
#96469=CARTESIAN_POINT('Ctrl Pts',(0.0135270145172919,-0.0320835708272304,
0.0717403362289151));
#96470=CARTESIAN_POINT('Ctrl Pts',(0.0135597145896253,-0.0319739230346346,
0.0718150445493465));
#96471=CARTESIAN_POINT('Ctrl Pts',(0.0135908279885789,-0.0318646057455575,
0.0718903199755538));
#96472=CARTESIAN_POINT('Ctrl Pts',(0.013384643392019,-0.0321934096636183,
0.0716323604585858));
#96473=CARTESIAN_POINT('Ctrl Pts',(0.013419363603424,-0.0320835708272304,
0.0717049118345846));
#96474=CARTESIAN_POINT('Ctrl Pts',(0.0134525622287399,-0.0319739230346346,
0.0717781396608072));
#96475=CARTESIAN_POINT('Ctrl Pts',(0.0134842039830689,-0.0318646057455575,
0.0718519469874669));
#96476=CARTESIAN_POINT('Ctrl Pts',(0.013276524510799,-0.0321934096636183,
0.07159842710789));
#96477=CARTESIAN_POINT('Ctrl Pts',(0.0133117126895561,-0.0320835708272304,
0.071669487440254));
#96478=CARTESIAN_POINT('Ctrl Pts',(0.0133454098678546,-0.0319739230346346,
0.0717412347722678));
#96479=CARTESIAN_POINT('Ctrl Pts',(0.0133775799775589,-0.0318646057455575,
0.07181357399938));
#96480=CARTESIAN_POINT('Ctrl Pts',(0.0132210242785011,-0.0320218834582289,
0.0714874972444543));
#96481=CARTESIAN_POINT('Ctrl Pts',(0.0132487344956265,-0.0319391099350605,
0.0715405472120583));
#96482=CARTESIAN_POINT('Ctrl Pts',(0.0132755995411529,-0.0318564869454907,
0.0715939977369605));
#96483=CARTESIAN_POINT('Ctrl Pts',(0.0133016034819944,-0.0317740741446519,
0.0716478080607704));
#96484=CARTESIAN_POINT('Ctrl Pts',(0.0132368825874967,-0.0320218834582289,
0.0714405361745845));
#96485=CARTESIAN_POINT('Ctrl Pts',(0.0132650815558318,-0.0319391099350605,
0.0714937511888478));
#96486=CARTESIAN_POINT('Ctrl Pts',(0.0132924324792191,-0.0318564869454907,
0.0715473742923306));
#96487=CARTESIAN_POINT('Ctrl Pts',(0.0133189190824105,-0.0317740741446519,
0.0716013645679027));
#96488=CARTESIAN_POINT('Ctrl Pts',(0.0132527408964923,-0.0320218834582289,
0.0713935751047146));
#96489=CARTESIAN_POINT('Ctrl Pts',(0.0132814286160371,-0.0319391099350606,
0.0714469551656374));
#96490=CARTESIAN_POINT('Ctrl Pts',(0.0133092654172854,-0.0318564869454907,
0.0715007508477007));
#96491=CARTESIAN_POINT('Ctrl Pts',(0.0133362346828265,-0.0317740741446519,
0.071554921075035));
#96492=CARTESIAN_POINT('Ctrl Pts',(0.0132685992054879,-0.0320218834582289,
0.0713466140348448));
#96493=CARTESIAN_POINT('Ctrl Pts',(0.0132977756762424,-0.0319391099350606,
0.071400159142427));
#96494=CARTESIAN_POINT('Ctrl Pts',(0.0133260983553517,-0.0318564869454907,
0.0714541274030708));
#96495=CARTESIAN_POINT('Ctrl Pts',(0.0133535502832426,-0.0317740741446519,
0.0715084775821673));
#96496=CARTESIAN_POINT('Origin',(0.0183607323870741,-0.0391228853390707,
0.067740205225121));
#96497=CARTESIAN_POINT('Ctrl Pts',(0.0111563086103407,-0.035272297877954,
0.0692624701462411));
#96498=CARTESIAN_POINT('Ctrl Pts',(0.0111721784557977,-0.0352466642097181,
0.0692727288344202));
#96499=CARTESIAN_POINT('Ctrl Pts',(0.0111880767251362,-0.0352210183808283,
0.0692829125411708));
#96500=CARTESIAN_POINT('Ctrl Pts',(0.0112040042666222,-0.0351953608940152,
0.0692930211774508));
#96501=CARTESIAN_POINT('Origin',(0.0139667067512102,-0.0352456003065003,
0.0652485686174006));
#96502=CARTESIAN_POINT('Ctrl Pts',(0.0113077670268148,-0.035024121149334,
0.0693621486323109));
#96503=CARTESIAN_POINT('Ctrl Pts',(0.0113737177133355,-0.0349144232867422,
0.069406006715933));
#96504=CARTESIAN_POINT('Ctrl Pts',(0.0114388012966323,-0.0348045283677512,
0.0694512542984857));
#96505=CARTESIAN_POINT('Ctrl Pts',(0.0115029322562204,-0.0346945769586886,
0.0694978365257308));
#96506=CARTESIAN_POINT('Ctrl Pts',(0.0112878086753612,-0.035024121149334,
0.069250601305986));
#96507=CARTESIAN_POINT('Ctrl Pts',(0.0113552958804965,-0.0349144232867422,
0.0692941844715125));
#96508=CARTESIAN_POINT('Ctrl Pts',(0.0114219225848416,-0.0348045283677512,
0.0693391887323541));
#96509=CARTESIAN_POINT('Ctrl Pts',(0.0114876013029676,-0.0346945769586886,
0.0693855596194885));
#96510=CARTESIAN_POINT('Ctrl Pts',(0.0112678503239075,-0.035024121149334,
0.0691390539796612));
#96511=CARTESIAN_POINT('Ctrl Pts',(0.0113368740476575,-0.0349144232867422,
0.069182362227092));
#96512=CARTESIAN_POINT('Ctrl Pts',(0.011405043873051,-0.0348045283677512,
0.0692271231662225));
#96513=CARTESIAN_POINT('Ctrl Pts',(0.0114722703497148,-0.0346945769586886,
0.0692732827132463));
#96514=CARTESIAN_POINT('Ctrl Pts',(0.0112478919724539,-0.035024121149334,
0.0690275066533363));
#96515=CARTESIAN_POINT('Ctrl Pts',(0.0113184522148186,-0.0349144232867422,
0.0690705399826715));
#96516=CARTESIAN_POINT('Ctrl Pts',(0.0113881651612603,-0.0348045283677512,
0.0691150576000909));
#96517=CARTESIAN_POINT('Ctrl Pts',(0.011456939396462,-0.0346945769586886,
0.069161005807004));
#96518=CARTESIAN_POINT('Origin',(0.00149122091931901,-0.0345629067941437,
0.0829748015098817));
#96519=CARTESIAN_POINT('Ctrl Pts',(0.0116511346552536,-0.0351970973651656,
0.0693820542804004));
#96520=CARTESIAN_POINT('Ctrl Pts',(0.011717188081489,-0.0350869349321803,
0.0694309209683551));
#96521=CARTESIAN_POINT('Ctrl Pts',(0.0117822803142518,-0.0349764985129742,
0.069481201351032));
#96522=CARTESIAN_POINT('Ctrl Pts',(0.0118463231901381,-0.0348659306849652,
0.0695328352528112));
#96523=CARTESIAN_POINT('Ctrl Pts',(0.0115705317543276,-0.0351970973651656,
0.0693982913679529));
#96524=CARTESIAN_POINT('Ctrl Pts',(0.0116363602377201,-0.0350869349321803,
0.0694460414119515));
#96525=CARTESIAN_POINT('Ctrl Pts',(0.011701250555709,-0.0349764985129742,
0.0694951995492205));
#96526=CARTESIAN_POINT('Ctrl Pts',(0.0117651148920621,-0.0348659306849652,
0.0695457070426431));
#96527=CARTESIAN_POINT('Ctrl Pts',(0.0114899288534016,-0.0351970973651656,
0.0694145284555054));
#96528=CARTESIAN_POINT('Ctrl Pts',(0.0115555323939512,-0.0350869349321803,
0.0694611618555479));
#96529=CARTESIAN_POINT('Ctrl Pts',(0.0116202207971662,-0.0349764985129742,
0.0695091977474089));
#96530=CARTESIAN_POINT('Ctrl Pts',(0.0116839065939862,-0.0348659306849652,
0.0695585788324751));
#96531=CARTESIAN_POINT('Ctrl Pts',(0.0114093259524756,-0.0351970973651656,
0.0694307655430578));
#96532=CARTESIAN_POINT('Ctrl Pts',(0.0114747045501823,-0.0350869349321803,
0.0694762822991443));
#96533=CARTESIAN_POINT('Ctrl Pts',(0.0115391910386234,-0.0349764985129742,
0.0695231959455974));
#96534=CARTESIAN_POINT('Ctrl Pts',(0.0116026982959102,-0.0348659306849652,
0.069571450622307));
#96535=CARTESIAN_POINT('Origin',(0.00113578253201136,-0.0345637187967305,
0.0826507815892884));
#96536=CARTESIAN_POINT('Ctrl Pts',(0.0113822413412722,-0.0352450361861253,
0.0694107417268366));
#96537=CARTESIAN_POINT('Ctrl Pts',(0.0115609853954992,-0.0349452761023765,
0.0695336365270574));
#96538=CARTESIAN_POINT('Ctrl Pts',(0.0117299647177502,-0.0346444289983475,
0.0696696459292855));
#96539=CARTESIAN_POINT('Ctrl Pts',(0.0111732055928418,-0.0352450361861253,
0.0692736138453606));
#96540=CARTESIAN_POINT('Ctrl Pts',(0.0113571215098518,-0.0349452761023765,
0.0693886247331633));
#96541=CARTESIAN_POINT('Ctrl Pts',(0.0115318518506954,-0.0346444289983475,
0.0695171621861935));
#96542=CARTESIAN_POINT('Ctrl Pts',(0.0116021150931601,-0.0345231616327823,
0.069571519793703));
#96543=CARTESIAN_POINT('Ctrl Pts',(0.011665222996819,-0.0344132092796976,
0.0696194637156289));
#96544=CARTESIAN_POINT('Ctrl Pts',(0.0117273359621928,-0.0343032738558974,
0.0696687105010772));
#96545=CARTESIAN_POINT('Ctrl Pts',(0.0117883760314895,-0.0341934961088741,
0.0697191950209093));
#96546=CARTESIAN_POINT('Ctrl Pts',(0.011589200224347,-0.0345231616327823,
0.0694589394121885));
#96547=CARTESIAN_POINT('Ctrl Pts',(0.0116538598900645,-0.0344132092796976,
0.0695067053208305));
#96548=CARTESIAN_POINT('Ctrl Pts',(0.0117175282194975,-0.0343032738558974,
0.0695558061991537));
#96549=CARTESIAN_POINT('Ctrl Pts',(0.0117801252574648,-0.0341934961088741,
0.0696061770539023));
#96550=CARTESIAN_POINT('Ctrl Pts',(0.0115762853555338,-0.0345231616327823,
0.069346359030674));
#96551=CARTESIAN_POINT('Ctrl Pts',(0.0116424967833101,-0.0344132092796976,
0.0693939469260321));
#96552=CARTESIAN_POINT('Ctrl Pts',(0.0117077204768023,-0.0343032738558974,
0.0694429018972302));
#96553=CARTESIAN_POINT('Ctrl Pts',(0.0117718744834402,-0.0341934961088741,
0.0694931590868952));
#96554=CARTESIAN_POINT('Ctrl Pts',(0.0115633704867207,-0.0345231616327823,
0.0692337786491595));
#96555=CARTESIAN_POINT('Ctrl Pts',(0.0116311336765556,-0.0344132092796976,
0.0692811885312336));
#96556=CARTESIAN_POINT('Ctrl Pts',(0.0116979127341071,-0.0343032738558974,
0.0693299975953067));
#96557=CARTESIAN_POINT('Ctrl Pts',(0.0117636237094155,-0.0341934961088741,
0.0693801411198881));
#96558=CARTESIAN_POINT('Origin',(0.00148415075349963,-0.0345625596230733,
0.082984625513595));
#96559=CARTESIAN_POINT('Ctrl Pts',(0.0120365469580469,-0.0346945769586885,
0.069601343946356));
#96560=CARTESIAN_POINT('Ctrl Pts',(0.0120992297375753,-0.0345846629176052,
0.0696552638225161));
#96561=CARTESIAN_POINT('Ctrl Pts',(0.0121608081825813,-0.0344746925050311,
0.0697104891624619));
#96562=CARTESIAN_POINT('Ctrl Pts',(0.0122212036838981,-0.0343648066253259,
0.0697669488792724));
#96563=CARTESIAN_POINT('Ctrl Pts',(0.0119242701402049,-0.0346945769586885,
0.0696166748875381));
#96564=CARTESIAN_POINT('Ctrl Pts',(0.0119867416516149,-0.0345846629176052,
0.0696690475323982));
#96565=CARTESIAN_POINT('Ctrl Pts',(0.0120481407885251,-0.0344746925050311,
0.0697227210078353));
#96566=CARTESIAN_POINT('Ctrl Pts',(0.0121083891633072,-0.0343648066253259,
0.0697776262163046));
#96567=CARTESIAN_POINT('Ctrl Pts',(0.0118119933223629,-0.0346945769586885,
0.0696320058287201));
#96568=CARTESIAN_POINT('Ctrl Pts',(0.0118742535656544,-0.0345846629176052,
0.0696828312422803));
#96569=CARTESIAN_POINT('Ctrl Pts',(0.0119354733944689,-0.0344746925050311,
0.0697349528532086));
#96570=CARTESIAN_POINT('Ctrl Pts',(0.0119955746427163,-0.0343648066253259,
0.0697883035533368));
#96571=CARTESIAN_POINT('Ctrl Pts',(0.0116997165045209,-0.0346945769586885,
0.0696473367699022));
#96572=CARTESIAN_POINT('Ctrl Pts',(0.011761765479694,-0.0345846629176052,
0.0696966149521625));
#96573=CARTESIAN_POINT('Ctrl Pts',(0.0118228060004128,-0.0344746925050311,
0.0697471846985819));
#96574=CARTESIAN_POINT('Ctrl Pts',(0.0118827601221254,-0.0343648066253259,
0.069798980890369));
#96575=CARTESIAN_POINT('Origin',(0.00109928252967554,-0.0345626446731628,
0.0826964092180731));
#96576=CARTESIAN_POINT('Ctrl Pts',(0.0117017255132845,-0.0346945769586885,
0.069647062447956));
#96577=CARTESIAN_POINT('Ctrl Pts',(0.0117960413431884,-0.0345275153362891,
0.0697220039033263));
#96578=CARTESIAN_POINT('Ctrl Pts',(0.0118880247282043,-0.0343603235965159,
0.0697999308884341));
#96579=CARTESIAN_POINT('Ctrl Pts',(0.0119774070477464,-0.034193496108874,
0.069880608886537));
#96580=CARTESIAN_POINT('Ctrl Pts',(0.0116349715036842,-0.0346945769586885,
0.0695963482435004));
#96581=CARTESIAN_POINT('Ctrl Pts',(0.0117303495629053,-0.0345275153362891,
0.0696698915094128));
#96582=CARTESIAN_POINT('Ctrl Pts',(0.0118234394237568,-0.0343603235965159,
0.0697464533495536));
#96583=CARTESIAN_POINT('Ctrl Pts',(0.0119139691331808,-0.034193496108874,
0.0698258032360359));
#96584=CARTESIAN_POINT('Ctrl Pts',(0.0115682174940839,-0.0346945769586885,
0.0695456340390449));
#96585=CARTESIAN_POINT('Ctrl Pts',(0.0116646577826221,-0.0345275153362891,
0.0696177791154993));
#96586=CARTESIAN_POINT('Ctrl Pts',(0.0117588541193092,-0.0343603235965159,
0.0696929758106731));
#96587=CARTESIAN_POINT('Ctrl Pts',(0.0118505312186153,-0.034193496108874,
0.0697709975855348));
#96588=CARTESIAN_POINT('Ctrl Pts',(0.0115014634844837,-0.0346945769586885,
0.0694949198345893));
#96589=CARTESIAN_POINT('Ctrl Pts',(0.011598966002339,-0.0345275153362891,
0.0695656667215859));
#96590=CARTESIAN_POINT('Ctrl Pts',(0.0116942688148617,-0.0343603235965159,
0.0696394982717926));
#96591=CARTESIAN_POINT('Ctrl Pts',(0.0117870933040497,-0.034193496108874,
0.0697161919350337));
#96592=CARTESIAN_POINT('Ctrl Pts',(0.0118827358805017,-0.0340223579322365,
0.0697989606832147));
#96593=CARTESIAN_POINT('Ctrl Pts',(0.0119427480606665,-0.0339125849573554,
0.0698508064583261));
#96594=CARTESIAN_POINT('Ctrl Pts',(0.0120016449838952,-0.0338030433565221,
0.069903857914692));
#96595=CARTESIAN_POINT('Ctrl Pts',(0.0120593573450247,-0.0336938721132328,
0.0699580405317086));
#96596=CARTESIAN_POINT('Ctrl Pts',(0.011876915448826,-0.0340223579322365,
0.0696857913304491));
#96597=CARTESIAN_POINT('Ctrl Pts',(0.0119384885295235,-0.0339125849573554,
0.0697375568266274));
#96598=CARTESIAN_POINT('Ctrl Pts',(0.0119989469180457,-0.0338030433565221,
0.0697905603674852));
#96599=CARTESIAN_POINT('Ctrl Pts',(0.0120582193069463,-0.0336938721132328,
0.0698447273166822));
#96600=CARTESIAN_POINT('Ctrl Pts',(0.0118710950171504,-0.0340223579322365,
0.0695726219776836));
#96601=CARTESIAN_POINT('Ctrl Pts',(0.0119342289983806,-0.0339125849573554,
0.0696243071949287));
#96602=CARTESIAN_POINT('Ctrl Pts',(0.0119962488521961,-0.0338030433565221,
0.0696772628202785));
#96603=CARTESIAN_POINT('Ctrl Pts',(0.0120570812688679,-0.0336938721132328,
0.0697314141016559));
#96604=CARTESIAN_POINT('Ctrl Pts',(0.0118652745854748,-0.0340223579322365,
0.069459452624918));
#96605=CARTESIAN_POINT('Ctrl Pts',(0.0119299694672377,-0.0339125849573554,
0.06951105756323));
#96606=CARTESIAN_POINT('Ctrl Pts',(0.0119935507863465,-0.0338030433565221,
0.0695639652730717));
#96607=CARTESIAN_POINT('Ctrl Pts',(0.0120559432307895,-0.0336938721132328,
0.0696181008866296));
#96608=CARTESIAN_POINT('Origin',(0.00155843379365339,-0.0345589643415022,
0.0828901008711272));
#96609=CARTESIAN_POINT('Ctrl Pts',(0.0123144384873385,-0.034193496108874,
0.0698560042124226));
#96610=CARTESIAN_POINT('Ctrl Pts',(0.0123736501464459,-0.0340836138581106,
0.0699137908811119));
#96611=CARTESIAN_POINT('Ctrl Pts',(0.0124316376208305,-0.0339738896643499,
0.0699727750837136));
#96612=CARTESIAN_POINT('Ctrl Pts',(0.0124883317543179,-0.0338644633294062,
0.0700328763526159));
#96613=CARTESIAN_POINT('Ctrl Pts',(0.0122014204186368,-0.034193496108874,
0.0698642549938713));
#96614=CARTESIAN_POINT('Ctrl Pts',(0.0122605183043539,-0.0340836138581106,
0.0699204832103199));
#96615=CARTESIAN_POINT('Ctrl Pts',(0.0123184243088379,-0.0339738896643499,
0.0699779073541539));
#96616=CARTESIAN_POINT('Ctrl Pts',(0.0123750692463383,-0.0338644633294062,
0.0700364489614341));
#96617=CARTESIAN_POINT('Ctrl Pts',(0.0120884023499351,-0.034193496108874,
0.0698725057753202));
#96618=CARTESIAN_POINT('Ctrl Pts',(0.0121473864622619,-0.0340836138581106,
0.069927175539528));
#96619=CARTESIAN_POINT('Ctrl Pts',(0.0122052109968453,-0.0339738896643499,
0.0699830396245943));
#96620=CARTESIAN_POINT('Ctrl Pts',(0.0122618067383588,-0.0338644633294062,
0.0700400215702524));
#96621=CARTESIAN_POINT('Ctrl Pts',(0.0119753842812334,-0.034193496108874,
0.069880756556769));
#96622=CARTESIAN_POINT('Ctrl Pts',(0.0120342546201699,-0.0340836138581106,
0.069933867868736));
#96623=CARTESIAN_POINT('Ctrl Pts',(0.0120919976848527,-0.0339738896643499,
0.0699881718950347));
#96624=CARTESIAN_POINT('Ctrl Pts',(0.0121485442303792,-0.0338644633294062,
0.0700435941790706));
#96625=CARTESIAN_POINT('Origin',(0.00114795659634253,-0.0345610621864789,
0.0826389863918568));
#96626=CARTESIAN_POINT('Ctrl Pts',(0.0119504753784144,-0.0342436276873901,
0.0698564531834935));
#96627=CARTESIAN_POINT('Ctrl Pts',(0.012112409166108,-0.0339430054201861,
0.0700007792962205));
#96628=CARTESIAN_POINT('Ctrl Pts',(0.012263011682719,-0.0336441434784162,
0.0701568929099836));
#96629=CARTESIAN_POINT('Ctrl Pts',(0.0117602724055806,-0.0342436276873901,
0.0696942100661505));
#96630=CARTESIAN_POINT('Ctrl Pts',(0.0119283252933194,-0.0339430054201861,
0.0698313625554986));
#96631=CARTESIAN_POINT('Ctrl Pts',(0.0120855698729596,-0.0336441434784162,
0.0699807838410823));
#96632=CARTESIAN_POINT('Ctrl Pts',(0.0121485243370367,-0.0335235895815128,
0.0700435748585472));
#96633=CARTESIAN_POINT('Ctrl Pts',(0.0122050573639151,-0.0334144449262719,
0.0700989833581458));
#96634=CARTESIAN_POINT('Ctrl Pts',(0.0122605106424901,-0.0333049234473133,
0.0701556234451868));
#96635=CARTESIAN_POINT('Ctrl Pts',(0.0123148067044481,-0.0331951640388588,
0.0702134291175165));
#96636=CARTESIAN_POINT('Ctrl Pts',(0.0121498214044117,-0.0335235895815128,
0.0699302633847131));
#96637=CARTESIAN_POINT('Ctrl Pts',(0.0122079143868172,-0.0334144449262719,
0.0699856897409977));
#96638=CARTESIAN_POINT('Ctrl Pts',(0.0122649290442134,-0.0333049234473133,
0.0700423799327472));
#96639=CARTESIAN_POINT('Ctrl Pts',(0.0123207859059592,-0.0331951640388588,
0.0701002680745929));
#96640=CARTESIAN_POINT('Ctrl Pts',(0.0121511184717866,-0.0335235895815128,
0.0698169519108789));
#96641=CARTESIAN_POINT('Ctrl Pts',(0.0122107714097192,-0.0334144449262719,
0.0698723961238496));
#96642=CARTESIAN_POINT('Ctrl Pts',(0.0122693474459368,-0.0333049234473133,
0.0699291364203076));
#96643=CARTESIAN_POINT('Ctrl Pts',(0.0123267651074702,-0.0331951640388588,
0.0699871070316694));
#96644=CARTESIAN_POINT('Ctrl Pts',(0.0121524155391616,-0.0335235895815128,
0.0697036404370447));
#96645=CARTESIAN_POINT('Ctrl Pts',(0.0122136284326212,-0.0334144449262719,
0.0697591025067015));
#96646=CARTESIAN_POINT('Ctrl Pts',(0.0122737658476601,-0.0333049234473133,
0.069815892907868));
#96647=CARTESIAN_POINT('Ctrl Pts',(0.0123327443089813,-0.0331951640388588,
0.0698739459887459));
#96648=CARTESIAN_POINT('Origin',(-0.00034203095527586,-0.0326434571768189,
0.0810575658527565));
#96649=CARTESIAN_POINT('Ctrl Pts',(0.0125778188787164,-0.0336938721132364,
0.0701275905556615));
#96650=CARTESIAN_POINT('Ctrl Pts',(0.0126013633759704,-0.0336474569764945,
0.0701536615103876));
#96651=CARTESIAN_POINT('Ctrl Pts',(0.0126246010664983,-0.033601104548885,
0.0701800062967829));
#96652=CARTESIAN_POINT('Ctrl Pts',(0.0126834335537046,-0.0334837508643158,
0.0702467052360211));
#96653=CARTESIAN_POINT('Ctrl Pts',(0.0127402637782464,-0.0333660264760398,
0.0703151182145042));
#96654=CARTESIAN_POINT('Ctrl Pts',(0.012237880085459,-0.0336938721132364,
0.0701310046613417));
#96655=CARTESIAN_POINT('Ctrl Pts',(0.0122614045988195,-0.0336474569764945,
0.0701550858415074));
#96656=CARTESIAN_POINT('Ctrl Pts',(0.0122846455996468,-0.033601104548885,
0.070179440755746));
#96657=CARTESIAN_POINT('Ctrl Pts',(0.0123434864677696,-0.0334837508643158,
0.0702411017964006));
#96658=CARTESIAN_POINT('Ctrl Pts',(0.0124004743529215,-0.0333660264760398,
0.0703044793369176));
#96659=CARTESIAN_POINT('Ctrl Pts',(0.0122378800854708,-0.0336938721132427,
0.0701310046613536));
#96660=CARTESIAN_POINT('Ctrl Pts',(0.0122614045988304,-0.0336474569765026,
0.0701550858415182));
#96661=CARTESIAN_POINT('Ctrl Pts',(0.0122846455996568,-0.0336011045488949,
0.070179440755756));
#96662=CARTESIAN_POINT('Ctrl Pts',(0.0123429964034918,-0.0334847282606778,
0.0702405882439267));
#96663=CARTESIAN_POINT('Ctrl Pts',(0.0123995251664643,-0.0333679869945434,
0.0703034239867374));
#96664=CARTESIAN_POINT('Ctrl Pts',(0.0122378800854558,-0.0336938721132427,
0.0701310046613385));
#96665=CARTESIAN_POINT('Ctrl Pts',(0.0123220141558681,-0.0335278710435083,
0.0702171296185953));
#96666=CARTESIAN_POINT('Ctrl Pts',(0.0124034177718423,-0.033362046922432,
0.0703058626998658));
#96667=CARTESIAN_POINT('Ctrl Pts',(0.012482116658346,-0.0331951640388602,
0.0703972615746468));
#96668=CARTESIAN_POINT('Ctrl Pts',(0.0121780086200365,-0.0336938721132427,
0.0700723238514274));
#96669=CARTESIAN_POINT('Ctrl Pts',(0.0122633711206849,-0.0335278710435083,
0.0701571954531406));
#96670=CARTESIAN_POINT('Ctrl Pts',(0.0123460420396404,-0.033362046922432,
0.0702447141430479));
#96671=CARTESIAN_POINT('Ctrl Pts',(0.0124260479341282,-0.0331951640388602,
0.070334937197491));
#96672=CARTESIAN_POINT('Ctrl Pts',(0.0121181371546173,-0.0336938721132427,
0.0700136430415162));
#96673=CARTESIAN_POINT('Ctrl Pts',(0.0122047280855018,-0.0335278710435083,
0.070097261287686));
#96674=CARTESIAN_POINT('Ctrl Pts',(0.0122886663074385,-0.033362046922432,
0.0701835655862302));
#96675=CARTESIAN_POINT('Ctrl Pts',(0.0123699792099104,-0.0331951640388602,
0.0702726128203351));
#96676=CARTESIAN_POINT('Ctrl Pts',(0.012058265689198,-0.0336938721132427,
0.0699549622316051));
#96677=CARTESIAN_POINT('Ctrl Pts',(0.0121460850503186,-0.0335278710435083,
0.0700373271222313));
#96678=CARTESIAN_POINT('Ctrl Pts',(0.0122312905752366,-0.033362046922432,
0.0701224170294123));
#96679=CARTESIAN_POINT('Ctrl Pts',(0.0123139104856925,-0.0331951640388602,
0.0702102884431793));
#96680=CARTESIAN_POINT('Ctrl Pts',(0.0123984264156948,-0.0330240426238156,
0.0703043924341847));
#96681=CARTESIAN_POINT('Ctrl Pts',(0.0124514034065075,-0.0329142774063509,
0.0703632798229346));
#96682=CARTESIAN_POINT('Ctrl Pts',(0.012503189441463,-0.0328043479726686,
0.0704232917515795));
#96683=CARTESIAN_POINT('Ctrl Pts',(0.0125537160615389,-0.0326943950436594,
0.0704843531674097));
#96684=CARTESIAN_POINT('Ctrl Pts',(0.012406835779861,-0.0330240426238156,
0.0701913861574614));
#96685=CARTESIAN_POINT('Ctrl Pts',(0.0124613695422323,-0.0329142774063509,
0.0702503893933956));
#96686=CARTESIAN_POINT('Ctrl Pts',(0.0125147107299688,-0.0328043479726686,
0.0703105494097955));
#96687=CARTESIAN_POINT('Ctrl Pts',(0.0125667888865571,-0.0326943950436594,
0.0703717910191067));
#96688=CARTESIAN_POINT('Ctrl Pts',(0.0124152451440273,-0.0330240426238156,
0.0700783798807381));
#96689=CARTESIAN_POINT('Ctrl Pts',(0.0124713356779571,-0.0329142774063509,
0.0701374989638565));
#96690=CARTESIAN_POINT('Ctrl Pts',(0.0125262320184747,-0.0328043479726686,
0.0701978070680114));
#96691=CARTESIAN_POINT('Ctrl Pts',(0.0125798617115753,-0.0326943950436594,
0.0702592288708037));
#96692=CARTESIAN_POINT('Ctrl Pts',(0.0124236545081936,-0.0330240426238156,
0.0699653736040149));
#96693=CARTESIAN_POINT('Ctrl Pts',(0.0124813018136819,-0.0329142774063509,
0.0700246085343175));
#96694=CARTESIAN_POINT('Ctrl Pts',(0.0125377533069805,-0.0328043479726686,
0.0700850647262274));
#96695=CARTESIAN_POINT('Ctrl Pts',(0.0125929345365935,-0.0326943950436594,
0.0701466667225008));
#96696=CARTESIAN_POINT('Origin',(-0.000436084180803091,-0.0326396682856425,
0.0811378739443185));
#96697=CARTESIAN_POINT('Ctrl Pts',(0.0128195742877403,-0.0331951640388587,
0.0704150921558746));
#96698=CARTESIAN_POINT('Ctrl Pts',(0.0128710150876361,-0.0330855618255041,
0.0704797671924681));
#96699=CARTESIAN_POINT('Ctrl Pts',(0.0129211562480315,-0.0329757224427708,
0.0705455520457946));
#96700=CARTESIAN_POINT('Ctrl Pts',(0.0129699294279412,-0.0328657862078596,
0.0706123656239742));
#96701=CARTESIAN_POINT('Ctrl Pts',(0.012706413334905,-0.0331951640388587,
0.0704091129591236));
#96702=CARTESIAN_POINT('Ctrl Pts',(0.0127579364861402,-0.0330855618255041,
0.0704722294325145));
#96703=CARTESIAN_POINT('Ctrl Pts',(0.0128081922700783,-0.0329757224427708,
0.0705364563011535));
#96704=CARTESIAN_POINT('Ctrl Pts',(0.0128571122968149,-0.0328657862078596,
0.0706017144754535));
#96705=CARTESIAN_POINT('Ctrl Pts',(0.0125932523820697,-0.0331951640388587,
0.0704031337623726));
#96706=CARTESIAN_POINT('Ctrl Pts',(0.0126448578846443,-0.0330855618255041,
0.070464691672561));
#96707=CARTESIAN_POINT('Ctrl Pts',(0.012695228292125,-0.0329757224427708,
0.0705273605565124));
#96708=CARTESIAN_POINT('Ctrl Pts',(0.0127442951656886,-0.0328657862078596,
0.0705910633269327));
#96709=CARTESIAN_POINT('Ctrl Pts',(0.0124800914292343,-0.0331951640388587,
0.0703971545656216));
#96710=CARTESIAN_POINT('Ctrl Pts',(0.0125317792831484,-0.0330855618255041,
0.0704571539126075));
#96711=CARTESIAN_POINT('Ctrl Pts',(0.0125822643141717,-0.0329757224427708,
0.0705182648118713));
#96712=CARTESIAN_POINT('Ctrl Pts',(0.0126314780345623,-0.0328657862078596,
0.0705804121784119));
#96713=CARTESIAN_POINT('Origin',(-0.000709363987007214,-0.0326401908837922,
0.0807421581137135));
#96714=CARTESIAN_POINT('Ctrl Pts',(0.0124584724956533,-0.0332451089994433,
0.0703699755316898));
#96715=CARTESIAN_POINT('Ctrl Pts',(0.0126010384509766,-0.0329451141710258,
0.0705334610512132));
#96716=CARTESIAN_POINT('Ctrl Pts',(0.0127308849938027,-0.0326442513127503,
0.0707072207761991));
#96717=CARTESIAN_POINT('Ctrl Pts',(0.012290106113183,-0.0332451089994433,
0.0701851708746763));
#96718=CARTESIAN_POINT('Ctrl Pts',(0.0124396420901811,-0.0329451141710258,
0.0703423063521926));
#96719=CARTESIAN_POINT('Ctrl Pts',(0.0125769171647092,-0.0326442513127503,
0.070510259085497));
#96720=CARTESIAN_POINT('Ctrl Pts',(0.0126314584950257,-0.0325229783203385,
0.0705803873593277));
#96721=CARTESIAN_POINT('Ctrl Pts',(0.0126806655263194,-0.0324130253112079,
0.0706425255774421));
#96722=CARTESIAN_POINT('Ctrl Pts',(0.0127285796855624,-0.0323031222247695,
0.0707056722817132));
#96723=CARTESIAN_POINT('Ctrl Pts',(0.0127751424523411,-0.0321934096636184,
0.0707697444199963));
#96724=CARTESIAN_POINT('Ctrl Pts',(0.0126469469741007,-0.0325229783203385,
0.070468132071411));
#96725=CARTESIAN_POINT('Ctrl Pts',(0.0126977014420553,-0.0324130253112079,
0.0705304837978669));
#96726=CARTESIAN_POINT('Ctrl Pts',(0.0127471583865658,-0.0323031222247695,
0.0705938759888112));
#96727=CARTESIAN_POINT('Ctrl Pts',(0.0127952573221166,-0.0321934096636184,
0.070658225207915));
#96728=CARTESIAN_POINT('Ctrl Pts',(0.0126624354531757,-0.0325229783203385,
0.0703558767834943));
#96729=CARTESIAN_POINT('Ctrl Pts',(0.0127147373577912,-0.0324130253112079,
0.0704184420182917));
#96730=CARTESIAN_POINT('Ctrl Pts',(0.0127657370875693,-0.0323031222247695,
0.0704820796959093));
#96731=CARTESIAN_POINT('Ctrl Pts',(0.0128153721918921,-0.0321934096636184,
0.0705467059958338));
#96732=CARTESIAN_POINT('Ctrl Pts',(0.0126779239322506,-0.0325229783203385,
0.0702436214955776));
#96733=CARTESIAN_POINT('Ctrl Pts',(0.0127317732735271,-0.0324130253112079,
0.0703064002387165));
#96734=CARTESIAN_POINT('Ctrl Pts',(0.0127843157885728,-0.0323031222247695,
0.0703702834030074));
#96735=CARTESIAN_POINT('Ctrl Pts',(0.0128354870616676,-0.0321934096636184,
0.0704351867837525));
#96736=CARTESIAN_POINT('Origin',(-0.000429331389440062,-0.0326393375175697,
0.081132669058702));
#96737=CARTESIAN_POINT('Ctrl Pts',(0.0130448250186197,-0.0326943950436594,
0.07071731336857));
#96738=CARTESIAN_POINT('Ctrl Pts',(0.0130921338739411,-0.0325844576448127,
0.0707851345617225));
#96739=CARTESIAN_POINT('Ctrl Pts',(0.0131380434239149,-0.0324744968375319,
0.0708539389793783));
#96740=CARTESIAN_POINT('Ctrl Pts',(0.0131824960624879,-0.0323646534831894,
0.0709236376539727));
#96741=CARTESIAN_POINT('Ctrl Pts',(0.0129322629071423,-0.0326943950436594,
0.0707042405478287));
#96742=CARTESIAN_POINT('Ctrl Pts',(0.0129797519304346,-0.0325844576448127,
0.0707705104241212));
#96743=CARTESIAN_POINT('Ctrl Pts',(0.0130258737449062,-0.0324744968375319,
0.0708377671412968));
#96744=CARTESIAN_POINT('Ctrl Pts',(0.0130705704451865,-0.0323646534831894,
0.0709059237110439));
#96745=CARTESIAN_POINT('Ctrl Pts',(0.012819700795665,-0.0326943950436594,
0.0706911677270873));
#96746=CARTESIAN_POINT('Ctrl Pts',(0.0128673699869281,-0.0325844576448127,
0.0707558862865198));
#96747=CARTESIAN_POINT('Ctrl Pts',(0.0129137040658974,-0.0324744968375319,
0.0708215953032153));
#96748=CARTESIAN_POINT('Ctrl Pts',(0.0129586448278851,-0.0323646534831894,
0.0708882097681151));
#96749=CARTESIAN_POINT('Ctrl Pts',(0.0127071386841876,-0.0326943950436594,
0.070678094906346));
#96750=CARTESIAN_POINT('Ctrl Pts',(0.0127549880434217,-0.0325844576448127,
0.0707412621489184));
#96751=CARTESIAN_POINT('Ctrl Pts',(0.0128015343868887,-0.0324744968375319,
0.0708054234651338));
#96752=CARTESIAN_POINT('Ctrl Pts',(0.0128467192105837,-0.0323646534831894,
0.0708704958251864));
#96753=CARTESIAN_POINT('Origin',(-0.000739414714879376,-0.0326395579070081,
0.0807651562789755));
#96754=CARTESIAN_POINT('Ctrl Pts',(0.0126872448025215,-0.0327445246961876,
0.0706495808804532));
#96755=CARTESIAN_POINT('Ctrl Pts',(0.0128192652664822,-0.0324436878365475,
0.0708216946846538));
#96756=CARTESIAN_POINT('Ctrl Pts',(0.0129379463592203,-0.0321434074463188,
0.071003263852541));
#96757=CARTESIAN_POINT('Ctrl Pts',(0.0125308133031275,-0.0327445246961876,
0.070454570147422));
#96758=CARTESIAN_POINT('Ctrl Pts',(0.012670188717045,-0.0324436878365475,
0.070620784041234));
#96759=CARTESIAN_POINT('Ctrl Pts',(0.0127966482704634,-0.0321434074463188,
0.0707970240646397));
#96760=CARTESIAN_POINT('Ctrl Pts',(0.0129011493564902,-0.0322357242816073,
0.0709476745970712));
#96761=CARTESIAN_POINT('Ctrl Pts',(0.0130031392673096,-0.0319819883628706,
0.0710998275452069));
#96762=CARTESIAN_POINT('Ctrl Pts',(0.0130952405555584,-0.0317295851069886,
0.0712581620463056));
#96763=CARTESIAN_POINT('Ctrl Pts',(0.0127574702486035,-0.0322357242816073,
0.0707430864401392));
#96764=CARTESIAN_POINT('Ctrl Pts',(0.01286597602688,-0.0319819883628706,
0.0708906633950335));
#96765=CARTESIAN_POINT('Ctrl Pts',(0.0129648711609127,-0.0317295851069886,
0.0710448457999957));
#96766=CARTESIAN_POINT('Origin',(-0.000662033131781533,-0.0326371942646385,
0.0807095281023099));
#96767=CARTESIAN_POINT('Origin',(-0.000332440573460987,-0.0326352985530457,
0.0810573300062842));
#96768=CARTESIAN_POINT('Ctrl Pts',(0.0132506546416794,-0.0321934096636184,
0.0710330818271546));
#96769=CARTESIAN_POINT('Ctrl Pts',(0.0132936393724612,-0.0320835708272304,
0.0711037853938617));
#96770=CARTESIAN_POINT('Ctrl Pts',(0.0133351359637141,-0.0319739230346346,
0.0711753375163961));
#96771=CARTESIAN_POINT('Ctrl Pts',(0.0133750983493265,-0.0318646057455575,
0.0712476425741178));
#96772=CARTESIAN_POINT('Ctrl Pts',(0.0131391353335633,-0.0321934096636184,
0.0710129669400572));
#96773=CARTESIAN_POINT('Ctrl Pts',(0.0131823974643148,-0.0320835708272304,
0.0710821325685925));
#96774=CARTESIAN_POINT('Ctrl Pts',(0.0132242031221846,-0.0319739230346346,
0.0711521533857997));
#96775=CARTESIAN_POINT('Ctrl Pts',(0.0132645056952689,-0.0318646057455575,
0.0712229356998896));
#96776=CARTESIAN_POINT('Ctrl Pts',(0.0130276160254473,-0.0321934096636184,
0.0709928520529598));
#96777=CARTESIAN_POINT('Ctrl Pts',(0.0130711555561684,-0.0320835708272304,
0.0710604797433233));
#96778=CARTESIAN_POINT('Ctrl Pts',(0.0131132702806552,-0.0319739230346346,
0.0711289692552033));
#96779=CARTESIAN_POINT('Ctrl Pts',(0.0131539130412113,-0.0318646057455575,
0.0711982288256615));
#96780=CARTESIAN_POINT('Ctrl Pts',(0.0129160967173313,-0.0321934096636184,
0.0709727371658623));
#96781=CARTESIAN_POINT('Ctrl Pts',(0.012959913648022,-0.0320835708272304,
0.0710388269180541));
#96782=CARTESIAN_POINT('Ctrl Pts',(0.0130023374391257,-0.0319739230346346,
0.0711057851246069));
#96783=CARTESIAN_POINT('Ctrl Pts',(0.0130433203871538,-0.0318646057455575,
0.0711735219514334));
#96784=CARTESIAN_POINT('Ctrl Pts',(0.0128471309224587,-0.0320218834582295,
0.0708696380411101));
#96785=CARTESIAN_POINT('Ctrl Pts',(0.0128812715602258,-0.0319391099350611,
0.0709187966827591));
#96786=CARTESIAN_POINT('Ctrl Pts',(0.0129146238939656,-0.0318564869454912,
0.070968458651282));
#96787=CARTESIAN_POINT('Ctrl Pts',(0.0129471670078489,-0.0317740741446524,
0.0710185855066251));
#96788=CARTESIAN_POINT('Ctrl Pts',(0.0128569784012128,-0.0320218834582295,
0.0708210597001579));
#96789=CARTESIAN_POINT('Ctrl Pts',(0.0128916246220717,-0.0319391099350611,
0.0708703208302546));
#96790=CARTESIAN_POINT('Ctrl Pts',(0.012925480632212,-0.0318564869454912,
0.0709200931198808));
#96791=CARTESIAN_POINT('Ctrl Pts',(0.0129585251564445,-0.0317740741446524,
0.0709703380143798));
#96792=CARTESIAN_POINT('Ctrl Pts',(0.0128668258799668,-0.0320218834582295,
0.0707724813592056));
#96793=CARTESIAN_POINT('Ctrl Pts',(0.0129019776839176,-0.0319391099350611,
0.07082184497775));
#96794=CARTESIAN_POINT('Ctrl Pts',(0.0129363373704585,-0.0318564869454912,
0.0708717275884797));
#96795=CARTESIAN_POINT('Ctrl Pts',(0.0129698833050402,-0.0317740741446524,
0.0709220905221345));
#96796=CARTESIAN_POINT('Ctrl Pts',(0.0128766733587208,-0.0320218834582295,
0.0707239030182534));
#96797=CARTESIAN_POINT('Ctrl Pts',(0.0129123307457636,-0.0319391099350611,
0.0707733691252455));
#96798=CARTESIAN_POINT('Ctrl Pts',(0.0129471941087049,-0.0318564869454912,
0.0708233620570786));
#96799=CARTESIAN_POINT('Ctrl Pts',(0.0129812414536358,-0.0317740741446524,
0.0708738430298891));
#96800=CARTESIAN_POINT('Origin',(0.0174766506715612,-0.0391228853390799,
0.0665077183017818));
#96801=CARTESIAN_POINT('Ctrl Pts',(0.0105198263130554,-0.0352722978779541,
0.0689209334372314));
#96802=CARTESIAN_POINT('Ctrl Pts',(0.0105368567746026,-0.0352466642097181,
0.0689291222135428));
#96803=CARTESIAN_POINT('Ctrl Pts',(0.0105539060382353,-0.0352210183808284,
0.0689372330372197));
#96804=CARTESIAN_POINT('Ctrl Pts',(0.0105709749343713,-0.0351953608940152,
0.0689452657136062));
#96805=CARTESIAN_POINT('Origin',(0.0128049883673411,-0.0352456003065,0.0645864464342393));
#96806=CARTESIAN_POINT('Ctrl Pts',(0.010682583461653,-0.035024121149334,
0.0690008431555788));
#96807=CARTESIAN_POINT('Ctrl Pts',(0.0107535109827503,-0.0349144232867422,
0.0690360895923144));
#96808=CARTESIAN_POINT('Ctrl Pts',(0.0108237523883856,-0.0348045283677512,
0.0690728232482173));
#96809=CARTESIAN_POINT('Ctrl Pts',(0.0108932159573696,-0.0346945769586886,
0.0691110004201504));
#96810=CARTESIAN_POINT('Ctrl Pts',(0.0106488019006581,-0.035024121149334,
0.0688926768579639));
#96811=CARTESIAN_POINT('Ctrl Pts',(0.0107212193680879,-0.0349144232867422,
0.0689274579675687));
#96812=CARTESIAN_POINT('Ctrl Pts',(0.0107929612305043,-0.0348045283677512,
0.0689637568160742));
#96813=CARTESIAN_POINT('Ctrl Pts',(0.0108639338655484,-0.0346945769586886,
0.0690015303287941));
#96814=CARTESIAN_POINT('Ctrl Pts',(0.0106150203396632,-0.035024121149334,
0.0687845105603489));
#96815=CARTESIAN_POINT('Ctrl Pts',(0.0106889277534256,-0.0349144232867422,
0.068818826342823));
#96816=CARTESIAN_POINT('Ctrl Pts',(0.0107621700726231,-0.0348045283677512,
0.068854690383931));
#96817=CARTESIAN_POINT('Ctrl Pts',(0.0108346517737272,-0.0346945769586886,
0.0688920602374378));
#96818=CARTESIAN_POINT('Ctrl Pts',(0.0105812387786684,-0.035024121149334,
0.0686763442627339));
#96819=CARTESIAN_POINT('Ctrl Pts',(0.0106566361387633,-0.0349144232867422,
0.0687101947180773));
#96820=CARTESIAN_POINT('Ctrl Pts',(0.0107313789147418,-0.0348045283677512,
0.0687456239517878));
#96821=CARTESIAN_POINT('Ctrl Pts',(0.010805369681906,-0.0346945769586886,
0.0687825901460815));
#96822=CARTESIAN_POINT('Origin',(0.00264956155499517,-0.0345629067942747,
0.083736495665415));
#96823=CARTESIAN_POINT('Ctrl Pts',(0.0110257383730229,-0.0351970973651658,
0.0689775564665144));
#96824=CARTESIAN_POINT('Ctrl Pts',(0.0110973955682782,-0.0350869349321804,
0.0690177591365407));
#96825=CARTESIAN_POINT('Ctrl Pts',(0.0111682763322893,-0.0349764985129743,
0.0690594848233701));
#96826=CARTESIAN_POINT('Ctrl Pts',(0.0112382856548422,-0.0348659306849651,
0.0691026848756899));
#96827=CARTESIAN_POINT('Ctrl Pts',(0.010947806096732,-0.0351970973651658,
0.0690037677419895));
#96828=CARTESIAN_POINT('Ctrl Pts',(0.0110191001702881,-0.0350869349321804,
0.0690428907659447));
#96829=CARTESIAN_POINT('Ctrl Pts',(0.0110896399570378,-0.0349764985129743,
0.069083528363238));
#96830=CARTESIAN_POINT('Ctrl Pts',(0.0111593309714934,-0.0348659306849651,
0.0691256332662046));
#96831=CARTESIAN_POINT('Ctrl Pts',(0.0108698738204411,-0.0351970973651658,
0.0690299790174647));
#96832=CARTESIAN_POINT('Ctrl Pts',(0.0109408047722981,-0.0350869349321804,
0.0690680223953488));
#96833=CARTESIAN_POINT('Ctrl Pts',(0.0110110035817863,-0.0349764985129743,
0.0691075719031058));
#96834=CARTESIAN_POINT('Ctrl Pts',(0.0110803762881446,-0.0348659306849651,
0.0691485816567192));
#96835=CARTESIAN_POINT('Ctrl Pts',(0.0107919415441502,-0.0351970973651658,
0.0690561902929398));
#96836=CARTESIAN_POINT('Ctrl Pts',(0.010862509374308,-0.0350869349321804,
0.0690931540247529));
#96837=CARTESIAN_POINT('Ctrl Pts',(0.0109323672065349,-0.0349764985129743,
0.0691316154429736));
#96838=CARTESIAN_POINT('Ctrl Pts',(0.0110014216047959,-0.0348659306849651,
0.0691715300472339));
#96839=CARTESIAN_POINT('Origin',(0.00225631544113613,-0.0345637187968448,
0.0834595789810976));
#96840=CARTESIAN_POINT('Ctrl Pts',(0.0107625608535624,-0.0352450361861253,
0.0690397189723917));
#96841=CARTESIAN_POINT('Ctrl Pts',(0.0109552982602334,-0.0349452761023765,
0.0691392421401093));
#96842=CARTESIAN_POINT('Ctrl Pts',(0.0111399916282332,-0.0346444289983475,
0.0692530003427135));
#96843=CARTESIAN_POINT('Ctrl Pts',(0.010537986733647,-0.0352450361861253,
0.0689298715115006));
#96844=CARTESIAN_POINT('Ctrl Pts',(0.0107348671051819,-0.0349452761023765,
0.0690209247275181));
#96845=CARTESIAN_POINT('Ctrl Pts',(0.0109243296597209,-0.0346444289983475,
0.0691265491057191));
#96846=CARTESIAN_POINT('Ctrl Pts',(0.0110008516702502,-0.0345231616327822,
0.0691716717678788));
#96847=CARTESIAN_POINT('Ctrl Pts',(0.011069470916004,-0.0344132092796975,
0.0692113281200311));
#96848=CARTESIAN_POINT('Ctrl Pts',(0.0111372663609564,-0.0343032738558973,
0.0692524017610703));
#96849=CARTESIAN_POINT('Ctrl Pts',(0.0112041524991905,-0.0341934961088741,
0.0692948378461226));
#96850=CARTESIAN_POINT('Ctrl Pts',(0.010973928575784,-0.0345231616327822,
0.0690615977785681));
#96851=CARTESIAN_POINT('Ctrl Pts',(0.0110440650365087,-0.0344132092796975,
0.0691008830337679));
#96852=CARTESIAN_POINT('Ctrl Pts',(0.0111133852939984,-0.0343032738558973,
0.0691416169793963));
#96853=CARTESIAN_POINT('Ctrl Pts',(0.0111818018777275,-0.0341934961088741,
0.0691837451557301));
#96854=CARTESIAN_POINT('Ctrl Pts',(0.0109470054813178,-0.0345231616327822,
0.0689515237892573));
#96855=CARTESIAN_POINT('Ctrl Pts',(0.0110186591570133,-0.0344132092796975,
0.0689904379475046));
#96856=CARTESIAN_POINT('Ctrl Pts',(0.0110895042270403,-0.0343032738558973,
0.0690308321977223));
#96857=CARTESIAN_POINT('Ctrl Pts',(0.0111594512562646,-0.0341934961088741,
0.0690726524653377));
#96858=CARTESIAN_POINT('Ctrl Pts',(0.0109200823868516,-0.0345231616327822,
0.0688414497999466));
#96859=CARTESIAN_POINT('Ctrl Pts',(0.010993253277518,-0.0344132092796975,
0.0688799928612413));
#96860=CARTESIAN_POINT('Ctrl Pts',(0.0110656231600823,-0.0343032738558973,
0.0689200474160483));
#96861=CARTESIAN_POINT('Ctrl Pts',(0.0111371006348017,-0.0341934961088741,
0.0689615597749452));
#96862=CARTESIAN_POINT('Origin',(0.00264377841353288,-0.0345625596230839,
0.083747128330629));
#96863=CARTESIAN_POINT('Ctrl Pts',(0.0114355958676125,-0.0346945769586885,
0.0691468119977909));
#96864=CARTESIAN_POINT('Ctrl Pts',(0.0115045423269825,-0.0345846629178476,
0.0691924504640746));
#96865=CARTESIAN_POINT('Ctrl Pts',(0.0115725567778391,-0.0344746925055161,
0.0692395225099826));
#96866=CARTESIAN_POINT('Ctrl Pts',(0.0116395523213195,-0.0343648066260528,
0.0692879674614766));
#96867=CARTESIAN_POINT('Ctrl Pts',(0.0113261258624471,-0.0346945769586885,
0.0691760940665569));
#96868=CARTESIAN_POINT('Ctrl Pts',(0.0113946688001098,-0.0345846629178476,
0.0692202239808414));
#96869=CARTESIAN_POINT('Ctrl Pts',(0.0114623108565725,-0.0344746925055161,
0.0692657788724225));
#96870=CARTESIAN_POINT('Ctrl Pts',(0.0115289656020984,-0.0343648066260528,
0.0693127000131858));
#96871=CARTESIAN_POINT('Ctrl Pts',(0.0112166558572818,-0.0346945769586885,
0.069205376135323));
#96872=CARTESIAN_POINT('Ctrl Pts',(0.0112847952732372,-0.0345846629178476,
0.0692479974976082));
#96873=CARTESIAN_POINT('Ctrl Pts',(0.0113520649353058,-0.0344746925055161,
0.0692920352348625));
#96874=CARTESIAN_POINT('Ctrl Pts',(0.0114183788828774,-0.0343648066260528,
0.0693374325648949));
#96875=CARTESIAN_POINT('Ctrl Pts',(0.0111071858521164,-0.0346945769586885,
0.069234658204089));
#96876=CARTESIAN_POINT('Ctrl Pts',(0.0111749217463646,-0.0345846629178476,
0.069275771014375));
#96877=CARTESIAN_POINT('Ctrl Pts',(0.0112418190140392,-0.0344746925055161,
0.0693182915973025));
#96878=CARTESIAN_POINT('Ctrl Pts',(0.0113077921636563,-0.0343648066260528,
0.069362165116604));
#96879=CARTESIAN_POINT('Origin',(0.00222582190978953,-0.0345626446729341,
0.0835094214858947));
#96880=CARTESIAN_POINT('Ctrl Pts',(0.0111091446375892,-0.0346945769586886,
0.0692341342496886));
#96881=CARTESIAN_POINT('Ctrl Pts',(0.0112121094139331,-0.0345275153362891,
0.0692966638613612));
#96882=CARTESIAN_POINT('Ctrl Pts',(0.0113131343235095,-0.0343603235965159,
0.0693624477938375));
#96883=CARTESIAN_POINT('Ctrl Pts',(0.0114119234711446,-0.034193496108874,
0.0694312870466963));
#96884=CARTESIAN_POINT('Ctrl Pts',(0.011036560828061,-0.0346945769586886,
0.0691921864377594));
#96885=CARTESIAN_POINT('Ctrl Pts',(0.0111404042181207,-0.0345275153362891,
0.0692531957524804));
#96886=CARTESIAN_POINT('Ctrl Pts',(0.0112423557806073,-0.0343603235965159,
0.0693174866263712));
#96887=CARTESIAN_POINT('Ctrl Pts',(0.0113421168140885,-0.034193496108874,
0.0693848644340822));
#96888=CARTESIAN_POINT('Ctrl Pts',(0.0109639770185329,-0.0346945769586886,
0.0691502386258302));
#96889=CARTESIAN_POINT('Ctrl Pts',(0.0110686990223084,-0.0345275153362891,
0.0692097276435997));
#96890=CARTESIAN_POINT('Ctrl Pts',(0.0111715772377051,-0.0343603235965159,
0.069272525458905));
#96891=CARTESIAN_POINT('Ctrl Pts',(0.0112723101570324,-0.034193496108874,
0.0693384418214681));
#96892=CARTESIAN_POINT('Ctrl Pts',(0.0108913932090047,-0.0346945769586886,
0.0691082908139009));
#96893=CARTESIAN_POINT('Ctrl Pts',(0.0109969938264961,-0.0345275153362891,
0.0691662595347189));
#96894=CARTESIAN_POINT('Ctrl Pts',(0.0111007986948029,-0.0343603235965159,
0.0692275642914387));
#96895=CARTESIAN_POINT('Ctrl Pts',(0.0112025034999763,-0.034193496108874,
0.0692920192088539));
#96896=CARTESIAN_POINT('Ctrl Pts',(0.0113077655809934,-0.0340223579322365,
0.0693621481073606));
#96897=CARTESIAN_POINT('Ctrl Pts',(0.0113738025458342,-0.0339125849573554,
0.0694060635424564));
#96898=CARTESIAN_POINT('Ctrl Pts',(0.0114388841598033,-0.0338030433565221,
0.0694513149304079));
#96899=CARTESIAN_POINT('Ctrl Pts',(0.011502932324321,-0.0336938721132328,
0.0694978370244687));
#96900=CARTESIAN_POINT('Ctrl Pts',(0.0112878071642375,-0.0340223579322365,
0.0692506006222662));
#96901=CARTESIAN_POINT('Ctrl Pts',(0.0113553826598258,-0.0339125849573554,
0.0692942407787412));
#96902=CARTESIAN_POINT('Ctrl Pts',(0.0114220074210625,-0.0338030433565221,
0.0693392489255184));
#96903=CARTESIAN_POINT('Ctrl Pts',(0.011487601348368,-0.0336938721132328,
0.0693855599519801));
#96904=CARTESIAN_POINT('Ctrl Pts',(0.0112678487474817,-0.0340223579322365,
0.0691390531371719));
#96905=CARTESIAN_POINT('Ctrl Pts',(0.0113369627738175,-0.0339125849573554,
0.069182418015026));
#96906=CARTESIAN_POINT('Ctrl Pts',(0.0114051306823216,-0.0338030433565221,
0.069227182920629));
#96907=CARTESIAN_POINT('Ctrl Pts',(0.0114722703724149,-0.0336938721132328,
0.0692732828794915));
#96908=CARTESIAN_POINT('Ctrl Pts',(0.0112478903307258,-0.0340223579322365,
0.0690275056520775));
#96909=CARTESIAN_POINT('Ctrl Pts',(0.0113185428878091,-0.0339125849573554,
0.0690705952513109));
#96910=CARTESIAN_POINT('Ctrl Pts',(0.0113882539435808,-0.0338030433565221,
0.0691151169157396));
#96911=CARTESIAN_POINT('Ctrl Pts',(0.0114569393964619,-0.0336938721132328,
0.0691610058070029));
#96912=CARTESIAN_POINT('Origin',(0.00270562863037882,-0.034558964341501,
0.0836440389099324));
#96913=CARTESIAN_POINT('Ctrl Pts',(0.0117432135338,-0.034193496108874,0.0693646351476499));
#96914=CARTESIAN_POINT('Ctrl Pts',(0.0118092008813334,-0.0340836138581107,
0.0694145449624959));
#96915=CARTESIAN_POINT('Ctrl Pts',(0.0118741237880036,-0.03397388966435,
0.0694657962993714));
#96916=CARTESIAN_POINT('Ctrl Pts',(0.0119379035576876,-0.0338644633294062,
0.069518317992743));
#96917=CARTESIAN_POINT('Ctrl Pts',(0.0116321207434458,-0.034193496108874,
0.069386985789224));
#96918=CARTESIAN_POINT('Ctrl Pts',(0.0116977998888674,-0.0340836138581107,
0.0694353637002776));
#96919=CARTESIAN_POINT('Ctrl Pts',(0.0117624464408417,-0.03397388966435,
0.0694850774908009));
#96920=CARTESIAN_POINT('Ctrl Pts',(0.0118259819250294,-0.0338644633294062,
0.0695360579868402));
#96921=CARTESIAN_POINT('Ctrl Pts',(0.0115210279530916,-0.034193496108874,
0.0694093364307981));
#96922=CARTESIAN_POINT('Ctrl Pts',(0.0115863988964014,-0.0340836138581107,
0.0694561824380593));
#96923=CARTESIAN_POINT('Ctrl Pts',(0.0116507690936797,-0.03397388966435,
0.0695043586822304));
#96924=CARTESIAN_POINT('Ctrl Pts',(0.0117140602923711,-0.0338644633294062,
0.0695537979809374));
#96925=CARTESIAN_POINT('Ctrl Pts',(0.0114099351627374,-0.034193496108874,
0.0694316870723723));
#96926=CARTESIAN_POINT('Ctrl Pts',(0.0114749979039354,-0.0340836138581107,
0.069477001175841));
#96927=CARTESIAN_POINT('Ctrl Pts',(0.0115390917465177,-0.03397388966435,
0.0695236398736599));
#96928=CARTESIAN_POINT('Ctrl Pts',(0.0116021386597128,-0.0338644633294062,
0.0695715379750346));
#96929=CARTESIAN_POINT('Origin',(0.00226691517884985,-0.0345610621863834,
0.0834463509773151));
#96930=CARTESIAN_POINT('Ctrl Pts',(0.0113821766536979,-0.0342436276873901,
0.069410697251789));
#96931=CARTESIAN_POINT('Ctrl Pts',(0.0115609224035041,-0.0339430054201861,
0.0695335896247741));
#96932=CARTESIAN_POINT('Ctrl Pts',(0.0117299035983051,-0.0336441434784164,
0.069669596735674));
#96933=CARTESIAN_POINT('Ctrl Pts',(0.0111731390335956,-0.0342436276873901,
0.0692735722235048));
#96934=CARTESIAN_POINT('Ctrl Pts',(0.0113570565391009,-0.0339430054201861,
0.0693885806126787));
#96935=CARTESIAN_POINT('Ctrl Pts',(0.0115317886511495,-0.0336441434784164,
0.0695171156951689));
#96936=CARTESIAN_POINT('Ctrl Pts',(0.0116021165017316,-0.0335235895815127,
0.0695715213001562));
#96937=CARTESIAN_POINT('Ctrl Pts',(0.0116651482752291,-0.0334144449262719,
0.0696194074201238));
#96938=CARTESIAN_POINT('Ctrl Pts',(0.0117272631733977,-0.0333049234473133,
0.0696686507444454));
#96939=CARTESIAN_POINT('Ctrl Pts',(0.0117883760665211,-0.0331951640388588,
0.069719195500768));
#96940=CARTESIAN_POINT('Ctrl Pts',(0.0115892016479273,-0.0335235895815127,
0.0694589407554894));
#96941=CARTESIAN_POINT('Ctrl Pts',(0.0116537833142729,-0.0334144449262719,
0.0695066490770674));
#96942=CARTESIAN_POINT('Ctrl Pts',(0.0117174535591095,-0.0333049234473133,
0.0695557464183504));
#96943=CARTESIAN_POINT('Ctrl Pts',(0.0117801252808193,-0.0331951640388588,
0.069606177373808));
#96944=CARTESIAN_POINT('Ctrl Pts',(0.0115762867941231,-0.0335235895815127,
0.0693463602108227));
#96945=CARTESIAN_POINT('Ctrl Pts',(0.0116424183533166,-0.0334144449262719,
0.069393890734011));
#96946=CARTESIAN_POINT('Ctrl Pts',(0.0117076439448212,-0.0333049234473133,
0.0694428420922554));
#96947=CARTESIAN_POINT('Ctrl Pts',(0.0117718744951174,-0.0331951640388588,
0.069493159246848));
#96948=CARTESIAN_POINT('Ctrl Pts',(0.0115633719403188,-0.0335235895815127,
0.0692337796661559));
#96949=CARTESIAN_POINT('Ctrl Pts',(0.0116310533923603,-0.0334144449262719,
0.0692811323909546));
#96950=CARTESIAN_POINT('Ctrl Pts',(0.011697834330533,-0.0333049234473133,
0.0693299377661604));
#96951=CARTESIAN_POINT('Ctrl Pts',(0.0117636237094155,-0.0331951640388588,
0.0693801411198879));
#96952=CARTESIAN_POINT('Origin',(0.00059047207459251,-0.0326434571769134,
0.0820641453694175));
#96953=CARTESIAN_POINT('Ctrl Pts',(0.0120385558867142,-0.0336938721132359,
0.0696010696353447));
#96954=CARTESIAN_POINT('Ctrl Pts',(0.0120651822856328,-0.0336474569764943,
0.0696239841048323));
#96955=CARTESIAN_POINT('Ctrl Pts',(0.0120915386172965,-0.033601104548885,
0.0696472086998235));
#96956=CARTESIAN_POINT('Ctrl Pts',(0.0121582667864989,-0.0334837508643155,
0.0697060080321436));
#96957=CARTESIAN_POINT('Ctrl Pts',(0.012223223307557,-0.0333660264760393,
0.0697667588380515));
#96958=CARTESIAN_POINT('Ctrl Pts',(0.0117017255132827,-0.0336938721132359,
0.0696470624479546));
#96959=CARTESIAN_POINT('Ctrl Pts',(0.011728082701007,-0.0336474569764943,
0.0696680053374943));
#96960=CARTESIAN_POINT('Ctrl Pts',(0.0117541929197555,-0.033601104548885,
0.0696892553361747));
#96961=CARTESIAN_POINT('Ctrl Pts',(0.0118202979876687,-0.0334837508643155,
0.069743055444839));
#96962=CARTESIAN_POINT('Ctrl Pts',(0.0118847798184132,-0.0333660264760393,
0.0697987907585992));
#96963=CARTESIAN_POINT('Ctrl Pts',(0.0117017255132945,-0.0336938721132427,
0.069647062447966));
#96964=CARTESIAN_POINT('Ctrl Pts',(0.0117280827010179,-0.0336474569765026,
0.069668005337505));
#96965=CARTESIAN_POINT('Ctrl Pts',(0.0117541929197655,-0.0336011045488949,
0.0696892553361847));
#96966=CARTESIAN_POINT('Ctrl Pts',(0.0118197474225006,-0.0334847282606778,
0.0697426073632216));
#96967=CARTESIAN_POINT('Ctrl Pts',(0.0118837058461226,-0.0333679869945434,
0.0697978626947793));
#96968=CARTESIAN_POINT('Ctrl Pts',(0.0117017255132788,-0.0336938721132427,
0.0696470624479515));
#96969=CARTESIAN_POINT('Ctrl Pts',(0.0117959904807998,-0.0335278710435083,
0.0697219634890984));
#96970=CARTESIAN_POINT('Ctrl Pts',(0.0118878734089479,-0.033362046922432,
0.069799794305106));
#96971=CARTESIAN_POINT('Ctrl Pts',(0.0119774070477457,-0.0331951640388602,
0.0698806088865364));
#96972=CARTESIAN_POINT('Ctrl Pts',(0.0116349714965928,-0.0336938721132427,
0.0695963482381129));
#96973=CARTESIAN_POINT('Ctrl Pts',(0.0117302981207075,-0.0335278710435083,
0.0696698518436653));
#96974=CARTESIAN_POINT('Ctrl Pts',(0.0118232861551779,-0.033362046922432,
0.0697463190089678));
#96975=CARTESIAN_POINT('Ctrl Pts',(0.0119139691264464,-0.0331951640388602,
0.0698258032302179));
#96976=CARTESIAN_POINT('Ctrl Pts',(0.0115682174799067,-0.0336938721132427,
0.0695456340282742));
#96977=CARTESIAN_POINT('Ctrl Pts',(0.0116646057606152,-0.0335278710435083,
0.0696177401982322));
#96978=CARTESIAN_POINT('Ctrl Pts',(0.0117586989014079,-0.033362046922432,
0.0696928437128296));
#96979=CARTESIAN_POINT('Ctrl Pts',(0.0118505312051471,-0.0331951640388602,
0.0697709975738993));
#96980=CARTESIAN_POINT('Ctrl Pts',(0.0115014634632207,-0.0336938721132427,
0.0694949198184356));
#96981=CARTESIAN_POINT('Ctrl Pts',(0.0115989134005229,-0.0335278710435083,
0.0695656285527992));
#96982=CARTESIAN_POINT('Ctrl Pts',(0.0116941116476378,-0.033362046922432,
0.0696393684166914));
#96983=CARTESIAN_POINT('Ctrl Pts',(0.0117870932838478,-0.0331951640388602,
0.0697161919175808));
#96984=CARTESIAN_POINT('Ctrl Pts',(0.0118827371379824,-0.0330240426238156,
0.0697989612157147));
#96985=CARTESIAN_POINT('Ctrl Pts',(0.0119426769362473,-0.0329142774063509,
0.0698507444822524));
#96986=CARTESIAN_POINT('Ctrl Pts',(0.0120015761119189,-0.0328043479726686,
0.0699037926877008));
#96987=CARTESIAN_POINT('Ctrl Pts',(0.0120593573391959,-0.0326943950436595,
0.0699580399513539));
#96988=CARTESIAN_POINT('Ctrl Pts',(0.0118769167497257,-0.0330240426238156,
0.0696857920544335));
#96989=CARTESIAN_POINT('Ctrl Pts',(0.0119384155634426,-0.0329142774063509,
0.0697374951394524));
#96990=CARTESIAN_POINT('Ctrl Pts',(0.0119988761893682,-0.0328043479726686,
0.0697904953526129));
#96991=CARTESIAN_POINT('Ctrl Pts',(0.0120582193030605,-0.0326943950436595,
0.0698447269297796));
#96992=CARTESIAN_POINT('Ctrl Pts',(0.0118710963614689,-0.0330240426238156,
0.0695726228931522));
#96993=CARTESIAN_POINT('Ctrl Pts',(0.0119341541906378,-0.0329142774063509,
0.0696242457966524));
#96994=CARTESIAN_POINT('Ctrl Pts',(0.0119961762668175,-0.0328043479726686,
0.069677198017525));
#96995=CARTESIAN_POINT('Ctrl Pts',(0.012057081266925,-0.0326943950436595,
0.0697314139082052));
#96996=CARTESIAN_POINT('Ctrl Pts',(0.0118652759732122,-0.0330240426238156,
0.069459453731871));
#96997=CARTESIAN_POINT('Ctrl Pts',(0.0119298928178331,-0.0329142774063509,
0.0695109964538524));
#96998=CARTESIAN_POINT('Ctrl Pts',(0.0119934763442668,-0.0328043479726686,
0.0695639006824371));
#96999=CARTESIAN_POINT('Ctrl Pts',(0.0120559432307895,-0.0326943950436595,
0.0696181008866309));
#97000=CARTESIAN_POINT('Origin',(0.000507225759736011,-0.0326396682857532,
0.0821556082025202));
#97001=CARTESIAN_POINT('Ctrl Pts',(0.0123144384873385,-0.0331951640388588,
0.0698560042124226));
#97002=CARTESIAN_POINT('Ctrl Pts',(0.0123735795995155,-0.0330855618127431,
0.0699137220319671));
#97003=CARTESIAN_POINT('Ctrl Pts',(0.0124315704168896,-0.0329757224171935,
0.0699727038053237));
#97004=CARTESIAN_POINT('Ctrl Pts',(0.0124883329738301,-0.0328657861694598,
0.0700328776454173));
#97005=CARTESIAN_POINT('Ctrl Pts',(0.0122014204503534,-0.0331951640388588,
0.0698642549915559));
#97006=CARTESIAN_POINT('Ctrl Pts',(0.0122604479247258,-0.0330855618127431,
0.0699204162160933));
#97007=CARTESIAN_POINT('Ctrl Pts',(0.0123183571945371,-0.0329757224171935,
0.0699778379236157));
#97008=CARTESIAN_POINT('Ctrl Pts',(0.0123750704965776,-0.0328657861694598,
0.070036450219684));
#97009=CARTESIAN_POINT('Ctrl Pts',(0.0120884024133683,-0.0331951640388588,
0.0698725057706893));
#97010=CARTESIAN_POINT('Ctrl Pts',(0.012147316249936,-0.0330855618127431,
0.0699271104002196));
#97011=CARTESIAN_POINT('Ctrl Pts',(0.0122051439721847,-0.0329757224171935,
0.0699829720419077));
#97012=CARTESIAN_POINT('Ctrl Pts',(0.012261808019325,-0.0328657861694598,
0.0700400227939507));
#97013=CARTESIAN_POINT('Ctrl Pts',(0.0119753843763832,-0.0331951640388588,
0.0698807565498226));
#97014=CARTESIAN_POINT('Ctrl Pts',(0.0120341845751463,-0.0330855618127431,
0.0699338045843459));
#97015=CARTESIAN_POINT('Ctrl Pts',(0.0120919307498322,-0.0329757224171935,
0.0699881061601998));
#97016=CARTESIAN_POINT('Ctrl Pts',(0.0121485455420724,-0.0328657861694598,
0.0700435953682174));
#97017=CARTESIAN_POINT('Origin',(0.000186504498140234,-0.0326401908833285,
0.0817972637539969));
#97018=CARTESIAN_POINT('Ctrl Pts',(0.011950529478343,-0.0332451089994433,
0.0698565014015431));
#97019=CARTESIAN_POINT('Ctrl Pts',(0.0121124614273289,-0.0329451141710259,
0.0700008295367375));
#97020=CARTESIAN_POINT('Ctrl Pts',(0.0122630619595774,-0.0326442513127503,
0.0701569450273128));
#97021=CARTESIAN_POINT('Ctrl Pts',(0.0117603285498458,-0.0332451089994433,
0.0696942558875872));
#97022=CARTESIAN_POINT('Ctrl Pts',(0.0119283796885058,-0.0329451141710259,
0.0698314104773981));
#97023=CARTESIAN_POINT('Ctrl Pts',(0.0120856223672202,-0.0326442513127503,
0.0699808337242568));
#97024=CARTESIAN_POINT('Ctrl Pts',(0.0121485230261799,-0.0325229783203385,
0.0700435731744104));
#97025=CARTESIAN_POINT('Ctrl Pts',(0.0122051300291387,-0.0324130253112079,
0.0700990541377692));
#97026=CARTESIAN_POINT('Ctrl Pts',(0.01226058075156,-0.0323031222247695,
0.0701556976749047));
#97027=CARTESIAN_POINT('Ctrl Pts',(0.0123148067252875,-0.0321934096636184,
0.070213428723116));
#97028=CARTESIAN_POINT('Ctrl Pts',(0.0121498200557519,-0.0325229783203385,
0.0699302618318026));
#97029=CARTESIAN_POINT('Ctrl Pts',(0.0122079890530622,-0.0324130253112079,
0.0699857606746853));
#97030=CARTESIAN_POINT('Ctrl Pts',(0.012265001163067,-0.0323031222247695,
0.070042454400492));
#97031=CARTESIAN_POINT('Ctrl Pts',(0.0123207859198521,-0.0321934096636184,
0.0701002678116594));
#97032=CARTESIAN_POINT('Ctrl Pts',(0.0121511170853239,-0.0325229783203385,
0.0698169504891947));
#97033=CARTESIAN_POINT('Ctrl Pts',(0.0122108480769856,-0.0324130253112079,
0.0698724672116013));
#97034=CARTESIAN_POINT('Ctrl Pts',(0.0122694215745739,-0.0323031222247695,
0.0699292111260794));
#97035=CARTESIAN_POINT('Ctrl Pts',(0.0123267651144167,-0.0321934096636184,
0.0699871069002029));
#97036=CARTESIAN_POINT('Ctrl Pts',(0.0121524141148959,-0.0325229783203385,
0.0697036391465868));
#97037=CARTESIAN_POINT('Ctrl Pts',(0.0122137071009091,-0.0324130253112079,
0.0697591737485174));
#97038=CARTESIAN_POINT('Ctrl Pts',(0.0122738419860809,-0.0323031222247695,
0.0698159678516667));
#97039=CARTESIAN_POINT('Ctrl Pts',(0.0123327443089813,-0.0321934096636184,
0.0698739459887464));
#97040=CARTESIAN_POINT('Origin',(0.000513272958069437,-0.0326393375177826,
0.0821495980101279));
#97041=CARTESIAN_POINT('Ctrl Pts',(0.0125757914107655,-0.0326943950436593,
0.0701276109181228));
#97042=CARTESIAN_POINT('Ctrl Pts',(0.0126312274710742,-0.0325844576448127,
0.0701889679490965));
#97043=CARTESIAN_POINT('Ctrl Pts',(0.0126853984906822,-0.0324744968375319,
0.0702514758310184));
#97044=CARTESIAN_POINT('Ctrl Pts',(0.0127382361671847,-0.0323646534831894,
0.0703150535178129));
#97045=CARTESIAN_POINT('Ctrl Pts',(0.0124624784262628,-0.0326943950436593,
0.070128748953886));
#97046=CARTESIAN_POINT('Ctrl Pts',(0.0125178988023057,-0.0325844576448127,
0.0701885443195621));
#97047=CARTESIAN_POINT('Ctrl Pts',(0.0125720864343368,-0.0324744968375319,
0.0702494901012886));
#97048=CARTESIAN_POINT('Ctrl Pts',(0.0126249729710602,-0.0323646534831894,
0.0703115072541501));
#97049=CARTESIAN_POINT('Ctrl Pts',(0.01234916544176,-0.0326943950436593,
0.0701298869896492));
#97050=CARTESIAN_POINT('Ctrl Pts',(0.0124045701335372,-0.0325844576448127,
0.0701881206900276));
#97051=CARTESIAN_POINT('Ctrl Pts',(0.0124587743779913,-0.0324744968375319,
0.0702475043715587));
#97052=CARTESIAN_POINT('Ctrl Pts',(0.0125117097749356,-0.0323646534831894,
0.0703079609904873));
#97053=CARTESIAN_POINT('Ctrl Pts',(0.0122358524572572,-0.0326943950436593,
0.0701310250254124));
#97054=CARTESIAN_POINT('Ctrl Pts',(0.0122912414647688,-0.0325844576448127,
0.0701876970604932));
#97055=CARTESIAN_POINT('Ctrl Pts',(0.0123454623216459,-0.0324744968375319,
0.0702455186418289));
#97056=CARTESIAN_POINT('Ctrl Pts',(0.012398446578811,-0.0323646534831894,
0.0703044147268244));
#97057=CARTESIAN_POINT('Origin',(0.000159573167040383,-0.0326395579069251,
0.081823846923887));
#97058=CARTESIAN_POINT('Ctrl Pts',(0.0122125416897229,-0.0327445246961877,
0.0701052292056477));
#97059=CARTESIAN_POINT('Ctrl Pts',(0.0123650927125142,-0.0324436878365474,
0.0702594392894495));
#97060=CARTESIAN_POINT('Ctrl Pts',(0.0125055946203147,-0.0321434074463186,
0.0704247020451001));
#97061=CARTESIAN_POINT('Ctrl Pts',(0.0120329023736749,-0.0327445246961877,
0.0699313622561437));
#97062=CARTESIAN_POINT('Ctrl Pts',(0.0121920108955991,-0.0324436878365474,
0.0700787971324517));
#97063=CARTESIAN_POINT('Ctrl Pts',(0.0123395620096841,-0.0321434074463186,
0.0702377978658875));
#97064=CARTESIAN_POINT('Ctrl Pts',(0.0124621205918024,-0.0322357242816072,
0.0703741630148512));
#97065=CARTESIAN_POINT('Ctrl Pts',(0.0125823761026982,-0.0319819883628705,
0.0705123334662308));
#97066=CARTESIAN_POINT('Ctrl Pts',(0.0126935957197873,-0.0317295851069886,
0.0706578761002245));
#97067=CARTESIAN_POINT('Ctrl Pts',(0.012293932741339,-0.0322357242816072,
0.0701891958638311));
#97068=CARTESIAN_POINT('Ctrl Pts',(0.0124200792161012,-0.0319819883628705,
0.070322009750305));
#97069=CARTESIAN_POINT('Ctrl Pts',(0.0125375187118361,-0.0317295851069886,
0.0704625815340199));
#97070=CARTESIAN_POINT('Origin',(0.000229372514003324,-0.0326371942646295,
0.0817589589081086));
#97071=CARTESIAN_POINT('Origin',(0.000599957274254053,-0.0326352985531905,
0.0820627093890013));
#97072=CARTESIAN_POINT('Ctrl Pts',(0.0128195742877404,-0.0321934096636183,
0.0704150921558745));
#97073=CARTESIAN_POINT('Ctrl Pts',(0.012871081577721,-0.0320835708272303,
0.0704798507885373));
#97074=CARTESIAN_POINT('Ctrl Pts',(0.0129212188148431,-0.0319739230346346,
0.0705456377992503));
#97075=CARTESIAN_POINT('Ctrl Pts',(0.0129699283117961,-0.0318646057455575,
0.0706123640949856));
#97076=CARTESIAN_POINT('Ctrl Pts',(0.0127064132788358,-0.0321934096636183,
0.070409112956161));
#97077=CARTESIAN_POINT('Ctrl Pts',(0.0127580030266404,-0.0320835708272303,
0.0704723110103186));
#97078=CARTESIAN_POINT('Ctrl Pts',(0.0128082549698485,-0.0319739230346346,
0.0705365400541858));
#97079=CARTESIAN_POINT('Ctrl Pts',(0.0128571111214103,-0.0318646057455575,
0.0706017129767819));
#97080=CARTESIAN_POINT('Ctrl Pts',(0.0125932522699313,-0.0321934096636183,
0.0704031337564475));
#97081=CARTESIAN_POINT('Ctrl Pts',(0.0126449244755597,-0.0320835708272303,
0.0704647712320999));
#97082=CARTESIAN_POINT('Ctrl Pts',(0.012695291124854,-0.0319739230346346,
0.0705274423091213));
#97083=CARTESIAN_POINT('Ctrl Pts',(0.0127442939310246,-0.0318646057455575,
0.0705910618585781));
#97084=CARTESIAN_POINT('Ctrl Pts',(0.0124800912610267,-0.0321934096636183,
0.0703971545567339));
#97085=CARTESIAN_POINT('Ctrl Pts',(0.0125318459244791,-0.0320835708272303,
0.0704572314538812));
#97086=CARTESIAN_POINT('Ctrl Pts',(0.0125823272798595,-0.0319739230346346,
0.0705183445640569));
#97087=CARTESIAN_POINT('Ctrl Pts',(0.0126314767406389,-0.0318646057455575,
0.0705804107403744));
#97088=CARTESIAN_POINT('Ctrl Pts',(0.0123987475353627,-0.03202188345823,
0.070303512105451));
#97089=CARTESIAN_POINT('Ctrl Pts',(0.0124387801755191,-0.0319391099350616,
0.0703480041600004));
#97090=CARTESIAN_POINT('Ctrl Pts',(0.0124780938112457,-0.0318564869454917,
0.0703930943732335));
#97091=CARTESIAN_POINT('Ctrl Pts',(0.0125166628738244,-0.0317740741446529,
0.0704387472296568));
#97092=CARTESIAN_POINT('Ctrl Pts',(0.0124024288832527,-0.03202188345823,
0.0702540826028725));
#97093=CARTESIAN_POINT('Ctrl Pts',(0.0124429759650359,-0.0319391099350616,
0.0702986129713538));
#97094=CARTESIAN_POINT('Ctrl Pts',(0.0124828031324247,-0.0318564869454917,
0.0703437495083835));
#97095=CARTESIAN_POINT('Ctrl Pts',(0.0125218844458113,-0.0317740741446529,
0.0703894566298082));
#97096=CARTESIAN_POINT('Ctrl Pts',(0.0124061102311427,-0.03202188345823,
0.070204653100294));
#97097=CARTESIAN_POINT('Ctrl Pts',(0.0124471717545526,-0.0319391099350616,
0.0702492217827072));
#97098=CARTESIAN_POINT('Ctrl Pts',(0.0124875124536037,-0.0318564869454917,
0.0702944046435336));
#97099=CARTESIAN_POINT('Ctrl Pts',(0.0125271060177983,-0.0317740741446529,
0.0703401660299596));
#97100=CARTESIAN_POINT('Ctrl Pts',(0.0124097915790327,-0.03202188345823,
0.0701552235977154));
#97101=CARTESIAN_POINT('Ctrl Pts',(0.0124513675440694,-0.0319391099350616,
0.0701998305940606));
#97102=CARTESIAN_POINT('Ctrl Pts',(0.0124922217747827,-0.0318564869454917,
0.0702450597786836));
#97103=CARTESIAN_POINT('Ctrl Pts',(0.0125323275897852,-0.0317740741446529,
0.0702908754301111));
#97104=CARTESIAN_POINT('Origin',(0.0164450686329765,-0.0391228853390699,
0.0653957547261134));
#97105=CARTESIAN_POINT('Ctrl Pts',(0.00984555696867123,-0.0352722978779542,
0.0686618622316097));
#97106=CARTESIAN_POINT('Ctrl Pts',(0.00986347946575636,-0.0352466642097182,
0.0686678519541593));
#97107=CARTESIAN_POINT('Ctrl Pts',(0.00988141084661135,-0.0352210183808283,
0.0686737619822279));
#97108=CARTESIAN_POINT('Ctrl Pts',(0.00989935191070874,-0.0351953608940152,
0.0686795920186157));
#97109=CARTESIAN_POINT('Origin',(0.0115694445656761,-0.0352456003065,0.064075147203832));
#97110=CARTESIAN_POINT('Ctrl Pts',(0.0100170460719326,-0.035024121149334,
0.0687207429582405));
#97111=CARTESIAN_POINT('Ctrl Pts',(0.0100918318582287,-0.0349144232867422,
0.0687468218907271));
#97112=CARTESIAN_POINT('Ctrl Pts',(0.0101661233372754,-0.0348045283677513,
0.068774462308283));
#97113=CARTESIAN_POINT('Ctrl Pts',(0.0102398240336769,-0.0346945769586886,
0.0688036323480967));
#97114=CARTESIAN_POINT('Ctrl Pts',(0.00996997405679344,-0.035024121149334,
0.0686176635364643));
#97115=CARTESIAN_POINT('Ctrl Pts',(0.0100461797197962,-0.0349144232867422,
0.0686430940712718));
#97116=CARTESIAN_POINT('Ctrl Pts',(0.0101219053282571,-0.0348045283677513,
0.0686701150529163));
#97117=CARTESIAN_POINT('Ctrl Pts',(0.0101970525993676,-0.0346945769586886,
0.0686986954803613));
#97118=CARTESIAN_POINT('Ctrl Pts',(0.0099229020416543,-0.035024121149334,
0.0685145841146881));
#97119=CARTESIAN_POINT('Ctrl Pts',(0.0100005275813638,-0.0349144232867422,
0.0685393662518166));
#97120=CARTESIAN_POINT('Ctrl Pts',(0.0100776873192388,-0.0348045283677513,
0.0685657677975495));
#97121=CARTESIAN_POINT('Ctrl Pts',(0.0101542811650583,-0.0346945769586886,
0.068593758612626));
#97122=CARTESIAN_POINT('Ctrl Pts',(0.00987583002651516,-0.035024121149334,
0.0684115046929119));
#97123=CARTESIAN_POINT('Ctrl Pts',(0.00995487544293143,-0.0349144232867422,
0.0684356384323613));
#97124=CARTESIAN_POINT('Ctrl Pts',(0.0100334693102204,-0.0348045283677513,
0.0684614205421828));
#97125=CARTESIAN_POINT('Ctrl Pts',(0.010111509730749,-0.0346945769586886,
0.0684888217448907));
#97126=CARTESIAN_POINT('Origin',(0.00389423392027531,-0.0345629067943679,
0.0843470050574501));
#97127=CARTESIAN_POINT('Ctrl Pts',(0.0103545765082903,-0.035197097365166,
0.0686546311770197));
#97128=CARTESIAN_POINT('Ctrl Pts',(0.0104307073957904,-0.0350869349321805,
0.0686855358089954));
#97129=CARTESIAN_POINT('Ctrl Pts',(0.0105062588590593,-0.0349764985129744,
0.0687180487609703));
#97130=CARTESIAN_POINT('Ctrl Pts',(0.0105811305394404,-0.0348659306849652,
0.0687521336731991));
#97131=CARTESIAN_POINT('Ctrl Pts',(0.0102805438951862,-0.035197097365166,
0.0686904032729455));
#97132=CARTESIAN_POINT('Ctrl Pts',(0.0103561792087769,-0.0350869349321805,
0.0687202822833985));
#97133=CARTESIAN_POINT('Ctrl Pts',(0.010431256009712,-0.0349764985129744,
0.068751758461531));
#97134=CARTESIAN_POINT('Ctrl Pts',(0.0105056746333406,-0.0348659306849652,
0.0687847967545695));
#97135=CARTESIAN_POINT('Ctrl Pts',(0.010206511282082,-0.0351970973651659,
0.0687261753688713));
#97136=CARTESIAN_POINT('Ctrl Pts',(0.0102816510217635,-0.0350869349321805,
0.0687550287578017));
#97137=CARTESIAN_POINT('Ctrl Pts',(0.0103562531603647,-0.0349764985129744,
0.0687854681620917));
#97138=CARTESIAN_POINT('Ctrl Pts',(0.0104302187272408,-0.0348659306849652,
0.0688174598359399));
#97139=CARTESIAN_POINT('Ctrl Pts',(0.0101324786689779,-0.0351970973651659,
0.0687619474647971));
#97140=CARTESIAN_POINT('Ctrl Pts',(0.0102071228347501,-0.0350869349321805,
0.0687897752322049));
#97141=CARTESIAN_POINT('Ctrl Pts',(0.0102812503110174,-0.0349764985129744,
0.0688191778626523));
#97142=CARTESIAN_POINT('Ctrl Pts',(0.010354762821141,-0.0348659306849652,
0.0688501229173102));
#97143=CARTESIAN_POINT('Origin',(0.00346938180570812,-0.0345637187967836,
0.0841215587510999));
#97144=CARTESIAN_POINT('Ctrl Pts',(0.0101012652500473,-0.0352450361861253,
0.0687492884024862));
#97145=CARTESIAN_POINT('Ctrl Pts',(0.0103049564251235,-0.0349452761023765,
0.0688238703978933));
#97146=CARTESIAN_POINT('Ctrl Pts',(0.0105024511141282,-0.0346444289983475,
0.0689135833660627));
#97147=CARTESIAN_POINT('Ctrl Pts',(0.0098646944266722,-0.0352450361861253,
0.0686684537222579));
#97148=CARTESIAN_POINT('Ctrl Pts',(0.010071434331662,-0.0349452761023765,
0.068734113302881));
#97149=CARTESIAN_POINT('Ctrl Pts',(0.010272641162232,-0.0346444289983475,
0.0688151588467118));
#97150=CARTESIAN_POINT('Ctrl Pts',(0.0103542151430076,-0.0345231616327823,
0.0688503349521842));
#97151=CARTESIAN_POINT('Ctrl Pts',(0.0104272635643597,-0.0344132092796976,
0.0688810783302));
#97152=CARTESIAN_POINT('Ctrl Pts',(0.0104996723142249,-0.0343032738558974,
0.0689133310709747));
#97153=CARTESIAN_POINT('Ctrl Pts',(0.0105713496870405,-0.0341934961088741,
0.0689470494788358));
#97154=CARTESIAN_POINT('Ctrl Pts',(0.0103137084161712,-0.0345231616327823,
0.0687445032876437));
#97155=CARTESIAN_POINT('Ctrl Pts',(0.0103882155780199,-0.0344132092796976,
0.068774688337459));
#97156=CARTESIAN_POINT('Ctrl Pts',(0.0104620945416958,-0.0343032738558974,
0.0688064129517368));
#97157=CARTESIAN_POINT('Ctrl Pts',(0.0105352517007913,-0.0341934961088741,
0.068839634063149));
#97158=CARTESIAN_POINT('Ctrl Pts',(0.0102732016893348,-0.0345231616327823,
0.0686386716231032));
#97159=CARTESIAN_POINT('Ctrl Pts',(0.0103491675916801,-0.0344132092796976,
0.0686682983447179));
#97160=CARTESIAN_POINT('Ctrl Pts',(0.0104245167691668,-0.0343032738558974,
0.0686994948324989));
#97161=CARTESIAN_POINT('Ctrl Pts',(0.0104991537145422,-0.0341934961088741,
0.0687322186474621));
#97162=CARTESIAN_POINT('Ctrl Pts',(0.0102326949624984,-0.0345231616327823,
0.0685328399585627));
#97163=CARTESIAN_POINT('Ctrl Pts',(0.0103101196053404,-0.0344132092796976,
0.0685619083519769));
#97164=CARTESIAN_POINT('Ctrl Pts',(0.0103869389966377,-0.0343032738558974,
0.0685925767132611));
#97165=CARTESIAN_POINT('Ctrl Pts',(0.010463055728293,-0.0341934961088741,
0.0686248032317753));
#97166=CARTESIAN_POINT('Origin',(0.00388982900676628,-0.0345625596231603,
0.084358278701058));
#97167=CARTESIAN_POINT('Ctrl Pts',(0.0107824154971496,-0.0346945769586886,
0.0687711833127807));
#97168=CARTESIAN_POINT('Ctrl Pts',(0.0108565383098119,-0.0345846629176053,
0.0688078206235114));
#97169=CARTESIAN_POINT('Ctrl Pts',(0.0109299161382929,-0.0344746925050311,
0.0688459970213101));
#97170=CARTESIAN_POINT('Ctrl Pts',(0.0110024551644792,-0.0343648066253259,
0.0688856632018872));
#97171=CARTESIAN_POINT('Ctrl Pts',(0.0106774787120365,-0.0346945769586886,
0.0688139547134139));
#97172=CARTESIAN_POINT('Ctrl Pts',(0.0107510121131793,-0.0345846629176053,
0.0688491459422056));
#97173=CARTESIAN_POINT('Ctrl Pts',(0.0108238303338486,-0.0344746925050311,
0.0688858638222829));
#97174=CARTESIAN_POINT('Ctrl Pts',(0.0108958402652469,-0.0343648066253259,
0.0689240609211381));
#97175=CARTESIAN_POINT('Ctrl Pts',(0.0105725419269234,-0.0346945769586886,
0.068856726114047));
#97176=CARTESIAN_POINT('Ctrl Pts',(0.0106454859165468,-0.0345846629176053,
0.0688904712608998));
#97177=CARTESIAN_POINT('Ctrl Pts',(0.0107177445294043,-0.0344746925050311,
0.0689257306232556));
#97178=CARTESIAN_POINT('Ctrl Pts',(0.0107892253660145,-0.0343648066253259,
0.0689624586403891));
#97179=CARTESIAN_POINT('Ctrl Pts',(0.0104676051418103,-0.0346945769586886,
0.0688994975146802));
#97180=CARTESIAN_POINT('Ctrl Pts',(0.0105399597199142,-0.0345846629176053,
0.068931796579594));
#97181=CARTESIAN_POINT('Ctrl Pts',(0.01061165872496,-0.0344746925050311,
0.0689655974242283));
#97182=CARTESIAN_POINT('Ctrl Pts',(0.0106826104667822,-0.0343648066253259,
0.06900085635964));
#97183=CARTESIAN_POINT('Origin',(0.00344537564772737,-0.0345626446730476,
0.084174830085337));
#97184=CARTESIAN_POINT('Ctrl Pts',(0.0104694828127754,-0.0346945769586885,
0.0688987321908996));
#97185=CARTESIAN_POINT('Ctrl Pts',(0.0105794727195282,-0.0345275153362891,
0.068947863829545));
#97186=CARTESIAN_POINT('Ctrl Pts',(0.0106879459304918,-0.0343603235965159,
0.0690004672574773));
#97187=CARTESIAN_POINT('Ctrl Pts',(0.0107945839423478,-0.034193496108874,
0.0690563821289519));
#97188=CARTESIAN_POINT('Ctrl Pts',(0.0103922138933551,-0.0346945769586885,
0.0688662123135492));
#97189=CARTESIAN_POINT('Ctrl Pts',(0.0105028849419592,-0.0345275153362891,
0.0689137255237406));
#97190=CARTESIAN_POINT('Ctrl Pts',(0.0106120903690375,-0.0343603235965159,
0.0689647315258947));
#97191=CARTESIAN_POINT('Ctrl Pts',(0.0107195094354834,-0.034193496108874,
0.0690190746665572));
#97192=CARTESIAN_POINT('Ctrl Pts',(0.0103149449739347,-0.0346945769586885,
0.0688336924361988));
#97193=CARTESIAN_POINT('Ctrl Pts',(0.0104262971643902,-0.0345275153362891,
0.0688795872179362));
#97194=CARTESIAN_POINT('Ctrl Pts',(0.0105362348075832,-0.0343603235965159,
0.068928995794312));
#97195=CARTESIAN_POINT('Ctrl Pts',(0.010644434928619,-0.034193496108874,
0.0689817672041624));
#97196=CARTESIAN_POINT('Ctrl Pts',(0.0102376760545144,-0.0346945769586885,
0.0688011725588484));
#97197=CARTESIAN_POINT('Ctrl Pts',(0.0103497093868212,-0.0345275153362891,
0.0688454489121318));
#97198=CARTESIAN_POINT('Ctrl Pts',(0.010460379246129,-0.0343603235965159,
0.0688932600627293));
#97199=CARTESIAN_POINT('Ctrl Pts',(0.0105693604217546,-0.034193496108874,
0.0689444597417676));
#97200=CARTESIAN_POINT('Ctrl Pts',(0.0106825819614387,-0.0340223579322365,
0.0690008428159775));
#97201=CARTESIAN_POINT('Ctrl Pts',(0.0107536022685714,-0.0339125849573554,
0.0690361353384123));
#97202=CARTESIAN_POINT('Ctrl Pts',(0.0108238421973506,-0.0338030433565221,
0.0690728730165295));
#97203=CARTESIAN_POINT('Ctrl Pts',(0.0108932160874417,-0.0336938721132328,
0.0691110009064204));
#97204=CARTESIAN_POINT('Ctrl Pts',(0.0106488003157574,-0.0340223579322365,
0.0688926763690295));
#97205=CARTESIAN_POINT('Ctrl Pts',(0.0107213125203034,-0.0339125849573554,
0.0689275029544642));
#97206=CARTESIAN_POINT('Ctrl Pts',(0.0107930529419702,-0.0338030433565221,
0.0689638059017995));
#97207=CARTESIAN_POINT('Ctrl Pts',(0.0108639339522631,-0.0336938721132328,
0.0690015306529737));
#97208=CARTESIAN_POINT('Ctrl Pts',(0.0106150186700761,-0.0340223579322365,
0.0687845099220815));
#97209=CARTESIAN_POINT('Ctrl Pts',(0.0106890227720354,-0.0339125849573554,
0.068818870570516));
#97210=CARTESIAN_POINT('Ctrl Pts',(0.0107622636865897,-0.0338030433565221,
0.0688547387870695));
#97211=CARTESIAN_POINT('Ctrl Pts',(0.0108346518170844,-0.0336938721132328,
0.0688920603995271));
#97212=CARTESIAN_POINT('Ctrl Pts',(0.0105812370243948,-0.0340223579322365,
0.0686763434751334));
#97213=CARTESIAN_POINT('Ctrl Pts',(0.0106567330237674,-0.0339125849573554,
0.0687102381865678));
#97214=CARTESIAN_POINT('Ctrl Pts',(0.0107314744312092,-0.0338030433565221,
0.0687456716723394));
#97215=CARTESIAN_POINT('Ctrl Pts',(0.0108053696819057,-0.0336938721132328,
0.0687825901460804));
#97216=CARTESIAN_POINT('Origin',(0.00393827098599277,-0.0345589643415482,
0.0842482502829731));
#97217=CARTESIAN_POINT('Ctrl Pts',(0.0111149079858753,-0.034193496108874,
0.0689487341452375));
#97218=CARTESIAN_POINT('Ctrl Pts',(0.0111866303619451,-0.0340836138581107,
0.0689899799986454));
#97219=CARTESIAN_POINT('Ctrl Pts',(0.0112574648278799,-0.03397388966435,
0.0690326902055963));
#97220=CARTESIAN_POINT('Ctrl Pts',(0.0113273243886923,-0.0338644633294062,
0.0690768040249576));
#97221=CARTESIAN_POINT('Ctrl Pts',(0.0110074924735361,-0.034193496108874,
0.0689848321639676));
#97222=CARTESIAN_POINT('Ctrl Pts',(0.011078717079304,-0.0340836138581107,
0.0690245968210693));
#97223=CARTESIAN_POINT('Ctrl Pts',(0.011149084664026,-0.03397388966435,
0.0690658162421078));
#97224=CARTESIAN_POINT('Ctrl Pts',(0.0112185087023611,-0.0338644633294062,
0.0691084316340294));
#97225=CARTESIAN_POINT('Ctrl Pts',(0.0109000769611969,-0.034193496108874,
0.0690209301826978));
#97226=CARTESIAN_POINT('Ctrl Pts',(0.010970803796663,-0.0340836138581107,
0.0690592136434932));
#97227=CARTESIAN_POINT('Ctrl Pts',(0.0110407045001722,-0.03397388966435,
0.0690989422786194));
#97228=CARTESIAN_POINT('Ctrl Pts',(0.0111096930160299,-0.0338644633294062,
0.0691400592431011));
#97229=CARTESIAN_POINT('Ctrl Pts',(0.0107926614488577,-0.034193496108874,
0.0690570282014279));
#97230=CARTESIAN_POINT('Ctrl Pts',(0.0108628905140219,-0.0340836138581107,
0.0690938304659171));
#97231=CARTESIAN_POINT('Ctrl Pts',(0.0109323243363184,-0.03397388966435,
0.069132068315131));
#97232=CARTESIAN_POINT('Ctrl Pts',(0.0110008773296986,-0.0338644633294062,
0.0691716868521729));
#97233=CARTESIAN_POINT('Origin',(0.00347824005280992,-0.0345610621863455,
0.0841071065547872));
#97234=CARTESIAN_POINT('Ctrl Pts',(0.0107624911018675,-0.03424362768739,
0.0690396829555461));
#97235=CARTESIAN_POINT('Ctrl Pts',(0.0109552298865343,-0.033943005420186,
0.0691392035026549));
#97236=CARTESIAN_POINT('Ctrl Pts',(0.0111399248251389,-0.0336441434784162,
0.0692529591973061));
#97237=CARTESIAN_POINT('Ctrl Pts',(0.0105379154826387,-0.03424362768739,
0.068929838559931));
#97238=CARTESIAN_POINT('Ctrl Pts',(0.0107347971169819,-0.033943005420186,
0.069020889097931));
#97239=CARTESIAN_POINT('Ctrl Pts',(0.010924261131652,-0.0336441434784162,
0.0691265109022937));
#97240=CARTESIAN_POINT('Ctrl Pts',(0.0110008532565233,-0.0335235895815128,
0.0691716730859124));
#97241=CARTESIAN_POINT('Ctrl Pts',(0.0110693897279185,-0.0334144449262719,
0.0692112816335314));
#97242=CARTESIAN_POINT('Ctrl Pts',(0.0111371866566308,-0.0333049234473133,
0.0692523515984925));
#97243=CARTESIAN_POINT('Ctrl Pts',(0.0112041525940881,-0.0331951640388588,
0.0692948383178068));
#97244=CARTESIAN_POINT('Ctrl Pts',(0.0109739301564992,-0.0335235895815128,
0.0690615989328548));
#97245=CARTESIAN_POINT('Ctrl Pts',(0.0110439820153273,-0.0334144449262719,
0.0691008368309952));
#97246=CARTESIAN_POINT('Ctrl Pts',(0.0111133037298084,-0.0333049234473133,
0.0691415670274103));
#97247=CARTESIAN_POINT('Ctrl Pts',(0.0111818019409926,-0.0331951640388588,
0.0691837454701862));
#97248=CARTESIAN_POINT('Ctrl Pts',(0.0109470070564751,-0.0335235895815128,
0.0689515247797971));
#97249=CARTESIAN_POINT('Ctrl Pts',(0.0110185743027361,-0.0334144449262719,
0.0689903920284591));
#97250=CARTESIAN_POINT('Ctrl Pts',(0.0110894208029859,-0.0333049234473133,
0.0690307824563282));
#97251=CARTESIAN_POINT('Ctrl Pts',(0.011159451287897,-0.0331951640388588,
0.0690726526225656));
#97252=CARTESIAN_POINT('Ctrl Pts',(0.0109200839564511,-0.0335235895815128,
0.0688414506267395));
#97253=CARTESIAN_POINT('Ctrl Pts',(0.0109931665901449,-0.0334144449262719,
0.0688799472259229));
#97254=CARTESIAN_POINT('Ctrl Pts',(0.0110655378761634,-0.0333049234473133,
0.0689199978852461));
#97255=CARTESIAN_POINT('Ctrl Pts',(0.0111371006348015,-0.0331951640388588,
0.0689615597749449));
#97256=CARTESIAN_POINT('Origin',(0.00164177990531128,-0.0326434571770353,
0.0829459140857844));
#97257=CARTESIAN_POINT('Ctrl Pts',(0.0114375545749916,-0.0336938721132355,
0.0691462880642782));
#97258=CARTESIAN_POINT('Ctrl Pts',(0.011466842961358,-0.0336474569764941,
0.0691656846736549));
#97259=CARTESIAN_POINT('Ctrl Pts',(0.0114959022790625,-0.033601104548885,
0.0691854228115053));
#97260=CARTESIAN_POINT('Ctrl Pts',(0.0115694737871713,-0.0334837508643153,
0.0692353952363117));
#97261=CARTESIAN_POINT('Ctrl Pts',(0.0116415322016055,-0.0333660264760389,
0.0692875257931444));
#97262=CARTESIAN_POINT('Ctrl Pts',(0.0111091446375875,-0.0336938721132355,
0.0692341342496876));
#97263=CARTESIAN_POINT('Ctrl Pts',(0.0111379188310802,-0.0336474569764941,
0.0692516085667228));
#97264=CARTESIAN_POINT('Ctrl Pts',(0.0111664864940029,-0.033601104548885,
0.0692694185246716));
#97265=CARTESIAN_POINT('Ctrl Pts',(0.011238813245296,-0.0334837508643153,
0.0693145092414934));
#97266=CARTESIAN_POINT('Ctrl Pts',(0.0113097721046427,-0.0333660264760389,
0.0693617233493038));
#97267=CARTESIAN_POINT('Ctrl Pts',(0.0111091446375992,-0.0336938721132427,
0.0692341342496987));
#97268=CARTESIAN_POINT('Ctrl Pts',(0.011137918831091,-0.0336474569765026,
0.0692516085667332));
#97269=CARTESIAN_POINT('Ctrl Pts',(0.0111664864940129,-0.0336011045488949,
0.0692694185246816));
#97270=CARTESIAN_POINT('Ctrl Pts',(0.0112382108619794,-0.0334847282606778,
0.0693141336972473));
#97271=CARTESIAN_POINT('Ctrl Pts',(0.0113085902837036,-0.0333679869945434,
0.0693609372079656));
#97272=CARTESIAN_POINT('Ctrl Pts',(0.0111091446375831,-0.0336938721132426,
0.0692341342496849));
#97273=CARTESIAN_POINT('Ctrl Pts',(0.0112120538873638,-0.0335278710435083,
0.0692966301405592));
#97274=CARTESIAN_POINT('Ctrl Pts',(0.0113129670790205,-0.033362046922432,
0.0693623312528415));
#97275=CARTESIAN_POINT('Ctrl Pts',(0.0114119234711438,-0.0331951640388602,
0.0694312870466959));
#97276=CARTESIAN_POINT('Ctrl Pts',(0.0110365608203503,-0.0336938721132426,
0.0691921864333031));
#97277=CARTESIAN_POINT('Ctrl Pts',(0.0111403482101237,-0.0335278710435083,
0.0692531628469262));
#97278=CARTESIAN_POINT('Ctrl Pts',(0.011242186883257,-0.033362046922432,
0.0693173725547477));
#97279=CARTESIAN_POINT('Ctrl Pts',(0.0113421168066779,-0.0331951640388602,
0.0693848644291541));
#97280=CARTESIAN_POINT('Ctrl Pts',(0.0109639770031176,-0.0336938721132426,
0.0691502386169214));
#97281=CARTESIAN_POINT('Ctrl Pts',(0.0110686425328836,-0.0335278710435083,
0.0692096955532933));
#97282=CARTESIAN_POINT('Ctrl Pts',(0.0111714066874934,-0.033362046922432,
0.0692724138566539));
#97283=CARTESIAN_POINT('Ctrl Pts',(0.0112723101422121,-0.0331951640388602,
0.0693384418116124));
#97284=CARTESIAN_POINT('Ctrl Pts',(0.0108913931858848,-0.0336938721132426,
0.0691082908005396));
#97285=CARTESIAN_POINT('Ctrl Pts',(0.0109969368556435,-0.0335278710435083,
0.0691662282596603));
#97286=CARTESIAN_POINT('Ctrl Pts',(0.0111006264917299,-0.033362046922432,
0.0692274551585602));
#97287=CARTESIAN_POINT('Ctrl Pts',(0.0112025034777462,-0.0331951640388602,
0.0692920191940707));
#97288=CARTESIAN_POINT('Ctrl Pts',(0.0113077668952985,-0.0330240426238156,
0.0693621484780575));
#97289=CARTESIAN_POINT('Ctrl Pts',(0.0113737242145906,-0.0329142774063509,
0.069406010969336));
#97290=CARTESIAN_POINT('Ctrl Pts',(0.0114388076557933,-0.0328043479726686,
0.0694512588496985));
#97291=CARTESIAN_POINT('Ctrl Pts',(0.0115029322458005,-0.0326943950436594,
0.0694978364494208));
#97292=CARTESIAN_POINT('Ctrl Pts',(0.0112878085456185,-0.0330240426238156,
0.0692506011774958));
#97293=CARTESIAN_POINT('Ctrl Pts',(0.0113553025376511,-0.0329142774063509,
0.069294188723063));
#97294=CARTESIAN_POINT('Ctrl Pts',(0.0114219291015776,-0.0328043479726686,
0.0693391932879617));
#97295=CARTESIAN_POINT('Ctrl Pts',(0.011487601296021,-0.0326943950436594,
0.0693855595686153));
#97296=CARTESIAN_POINT('Ctrl Pts',(0.0112678501959385,-0.0330240426238156,
0.0691390538769341));
#97297=CARTESIAN_POINT('Ctrl Pts',(0.0113368808607116,-0.0329142774063509,
0.0691823664767899));
#97298=CARTESIAN_POINT('Ctrl Pts',(0.0114050505473619,-0.0328043479726686,
0.0692271277262249));
#97299=CARTESIAN_POINT('Ctrl Pts',(0.0114722703462415,-0.0326943950436594,
0.0692732826878098));
#97300=CARTESIAN_POINT('Ctrl Pts',(0.0112478918462585,-0.0330240426238156,
0.0690275065763724));
#97301=CARTESIAN_POINT('Ctrl Pts',(0.0113184591837721,-0.0329142774063509,
0.0690705442305169));
#97302=CARTESIAN_POINT('Ctrl Pts',(0.0113881719931461,-0.0328043479726686,
0.0691150621644881));
#97303=CARTESIAN_POINT('Ctrl Pts',(0.011456939396462,-0.0326943950436594,
0.0691610058070043));
#97304=CARTESIAN_POINT('Origin',(0.00157065334461952,-0.0326396682857218,
0.0830470892373371));
#97305=CARTESIAN_POINT('Ctrl Pts',(0.0117432135338,-0.0331951640388588,
0.0693646351476499));
#97306=CARTESIAN_POINT('Ctrl Pts',(0.0118091222539269,-0.0330855618255041,
0.0694144854923179));
#97307=CARTESIAN_POINT('Ctrl Pts',(0.0118740481653163,-0.0329757224427708,
0.0694657339939863));
#97308=CARTESIAN_POINT('Ctrl Pts',(0.0119379049073101,-0.0328657862078597,
0.0695183191041373));
#97309=CARTESIAN_POINT('Ctrl Pts',(0.0116321207746222,-0.0331951640388588,
0.0693869857829517));
#97310=CARTESIAN_POINT('Ctrl Pts',(0.0116977216599627,-0.0330855618255041,
0.0694353060496009));
#97311=CARTESIAN_POINT('Ctrl Pts',(0.0117623711387492,-0.0329757224427708,
0.0694850170078197));
#97312=CARTESIAN_POINT('Ctrl Pts',(0.0118259833008915,-0.0328657862078597,
0.0695360590606433));
#97313=CARTESIAN_POINT('Ctrl Pts',(0.0115210280154443,-0.0331951640388588,
0.0694093364182535));
#97314=CARTESIAN_POINT('Ctrl Pts',(0.0115863210659985,-0.0330855618255041,
0.0694561266068838));
#97315=CARTESIAN_POINT('Ctrl Pts',(0.0116506941121821,-0.0329757224427708,
0.0695043000216531));
#97316=CARTESIAN_POINT('Ctrl Pts',(0.011714061694473,-0.0328657862078597,
0.0695537990171493));
#97317=CARTESIAN_POINT('Ctrl Pts',(0.0114099352562665,-0.0331951640388588,
0.0694316870535553));
#97318=CARTESIAN_POINT('Ctrl Pts',(0.0114749204720344,-0.0330855618255041,
0.0694769471641668));
#97319=CARTESIAN_POINT('Ctrl Pts',(0.011539017085615,-0.0329757224427708,
0.0695235830354865));
#97320=CARTESIAN_POINT('Ctrl Pts',(0.0116021400880544,-0.0328657862078597,
0.0695715389736553));
#97321=CARTESIAN_POINT('Origin',(0.0012075486003039,-0.0326401908836129,
0.0827317674714501));
#97322=CARTESIAN_POINT('Ctrl Pts',(0.0113822363703565,-0.0332451089994432,
0.0694107383091061));
#97323=CARTESIAN_POINT('Ctrl Pts',(0.0115609805494362,-0.0329451141710258,
0.0695336329190619));
#97324=CARTESIAN_POINT('Ctrl Pts',(0.0117299600107489,-0.0326442513127503,
0.0696696421406814));
#97325=CARTESIAN_POINT('Ctrl Pts',(0.0111732004780954,-0.0332451089994432,
0.0692736106468835));
#97326=CARTESIAN_POINT('Ctrl Pts',(0.0113571165115718,-0.0329451141710258,
0.0693886213391751));
#97327=CARTESIAN_POINT('Ctrl Pts',(0.0115318469834969,-0.0326442513127503,
0.0695171586057243));
#97328=CARTESIAN_POINT('Ctrl Pts',(0.011602114990133,-0.0325229783203385,
0.0695715197935932));
#97329=CARTESIAN_POINT('Ctrl Pts',(0.0116652292385048,-0.032413025311208,
0.0696194685342614));
#97330=CARTESIAN_POINT('Ctrl Pts',(0.0117273420330872,-0.0323031222247695,
0.0696687156018434));
#97331=CARTESIAN_POINT('Ctrl Pts',(0.0117883760377646,-0.0321934096636184,
0.0697191951068656));
#97332=CARTESIAN_POINT('Ctrl Pts',(0.0115892001152709,-0.0325229783203385,
0.069458939383856));
#97333=CARTESIAN_POINT('Ctrl Pts',(0.0116538662821006,-0.032413025311208,
0.0695067100932598));
#97334=CARTESIAN_POINT('Ctrl Pts',(0.0117175344425675,-0.0323031222247695,
0.0695558112600057));
#97335=CARTESIAN_POINT('Ctrl Pts',(0.0117801252616482,-0.0321934096636184,
0.0696061771112066));
#97336=CARTESIAN_POINT('Ctrl Pts',(0.0115762852404087,-0.0325229783203385,
0.0693463589741187));
#97337=CARTESIAN_POINT('Ctrl Pts',(0.0116425033256965,-0.032413025311208,
0.0693939516522582));
#97338=CARTESIAN_POINT('Ctrl Pts',(0.0117077268520479,-0.0323031222247695,
0.069442906918168));
#97339=CARTESIAN_POINT('Ctrl Pts',(0.0117718744855319,-0.0321934096636184,
0.0694931591155475));
#97340=CARTESIAN_POINT('Ctrl Pts',(0.0115633703655466,-0.0325229783203385,
0.0692337785643814));
#97341=CARTESIAN_POINT('Ctrl Pts',(0.0116311403692924,-0.032413025311208,
0.0692811932112566));
#97342=CARTESIAN_POINT('Ctrl Pts',(0.0116979192615282,-0.0323031222247695,
0.0693300025763304));
#97343=CARTESIAN_POINT('Ctrl Pts',(0.0117636237094155,-0.0321934096636184,
0.0693801411198884));
#97344=CARTESIAN_POINT('Origin',(0.00157589958277574,-0.0326393375179485,
0.0830403685218024));
#97345=CARTESIAN_POINT('Ctrl Pts',(0.0120365469580468,-0.0326943950436594,
0.0696013439463559));
#97346=CARTESIAN_POINT('Ctrl Pts',(0.0120992359635559,-0.0325844576448127,
0.0696552691781193));
#97347=CARTESIAN_POINT('Ctrl Pts',(0.0121608141434588,-0.0324744968375319,
0.0697104947376692));
#97348=CARTESIAN_POINT('Ctrl Pts',(0.0122212035761687,-0.0323646534831895,
0.0697669487785634));
#97349=CARTESIAN_POINT('Ctrl Pts',(0.0119242701139744,-0.0326943950436594,
0.0696166748911197));
#97350=CARTESIAN_POINT('Ctrl Pts',(0.0119867478303313,-0.0325844576448127,
0.0696690527375426));
#97351=CARTESIAN_POINT('Ctrl Pts',(0.0120481467085947,-0.0324744968375319,
0.0697227264324349));
#97352=CARTESIAN_POINT('Ctrl Pts',(0.0121083890294841,-0.0323646534831895,
0.0697776261208629));
#97353=CARTESIAN_POINT('Ctrl Pts',(0.0118119932699019,-0.0326943950436594,
0.0696320058358835));
#97354=CARTESIAN_POINT('Ctrl Pts',(0.0118742596971068,-0.0325844576448127,
0.0696828362969658));
#97355=CARTESIAN_POINT('Ctrl Pts',(0.0119354792737306,-0.0324744968375319,
0.0697349581272007));
#97356=CARTESIAN_POINT('Ctrl Pts',(0.0119955744827996,-0.0323646534831895,
0.0697883034631624));
#97357=CARTESIAN_POINT('Ctrl Pts',(0.0116997164258294,-0.0326943950436594,
0.0696473367806473));
#97358=CARTESIAN_POINT('Ctrl Pts',(0.0117617715638822,-0.0325844576448127,
0.0696966198563891));
#97359=CARTESIAN_POINT('Ctrl Pts',(0.0118228118388665,-0.0324744968375319,
0.0697471898219664));
#97360=CARTESIAN_POINT('Ctrl Pts',(0.011882759936115,-0.0323646534831895,
0.0697989808054619));
#97361=CARTESIAN_POINT('Origin',(0.00118416138267592,-0.0326395579069507,
0.0827615164191161));
#97362=CARTESIAN_POINT('Ctrl Pts',(0.0116733563971562,-0.0327445246961877,
0.0696246659824982));
#97363=CARTESIAN_POINT('Ctrl Pts',(0.0118440321580191,-0.0324436878365475,
0.069758540360759));
#97364=CARTESIAN_POINT('Ctrl Pts',(0.0120041390818642,-0.0321434074463186,
0.0699048904117932));
#97365=CARTESIAN_POINT('Ctrl Pts',(0.0114733422837796,-0.0327445246961877,
0.0694746848021782));
#97366=CARTESIAN_POINT('Ctrl Pts',(0.0116496746772728,-0.0324436878365475,
0.0696010155249095));
#97367=CARTESIAN_POINT('Ctrl Pts',(0.0118159903828125,-0.0321434074463186,
0.0697402694318267));
#97368=CARTESIAN_POINT('Ctrl Pts',(0.0119546736389694,-0.0322357242816072,
0.0698601986374625));
#97369=CARTESIAN_POINT('Ctrl Pts',(0.0120912982486977,-0.0319819883628705,
0.0699822075615288));
#97370=CARTESIAN_POINT('Ctrl Pts',(0.0122198821948262,-0.0317295851069886,
0.0701126630341365));
#97371=CARTESIAN_POINT('Ctrl Pts',(0.0117646294688016,-0.0322357242816072,
0.0696977695348199));
#97372=CARTESIAN_POINT('Ctrl Pts',(0.0119064272347863,-0.0319819883628705,
0.0698137257985448));
#97373=CARTESIAN_POINT('Ctrl Pts',(0.0120405590012207,-0.0317295851069886,
0.0699384700600097));
#97374=CARTESIAN_POINT('Origin',(0.00124527771626521,-0.0326371942645812,
0.0826883918865079));
#97375=CARTESIAN_POINT('Origin',(0.00165101033500555,-0.032635298553037,
0.0829433006175441));
#97376=CARTESIAN_POINT('Ctrl Pts',(0.0123144384873387,-0.0321934096636184,
0.0698560042124227));
#97377=CARTESIAN_POINT('Ctrl Pts',(0.0123736560357861,-0.0320835708272304,
0.0699137966287189));
#97378=CARTESIAN_POINT('Ctrl Pts',(0.0124316432245973,-0.0319739230346346,
0.0699727810271523));
#97379=CARTESIAN_POINT('Ctrl Pts',(0.0124883316550263,-0.0318646057455575,
0.0700328762473571));
#97380=CARTESIAN_POINT('Ctrl Pts',(0.0122014203943551,-0.0321934096636184,
0.0698642549956441));
#97381=CARTESIAN_POINT('Ctrl Pts',(0.0122605241580717,-0.0320835708272304,
0.0699204888043572));
#97382=CARTESIAN_POINT('Ctrl Pts',(0.0123184298834547,-0.0319739230346346,
0.069977913144494));
#97383=CARTESIAN_POINT('Ctrl Pts',(0.0123750691227986,-0.0318646057455575,
0.0700364488596744));
#97384=CARTESIAN_POINT('Ctrl Pts',(0.0120884023013716,-0.0321934096636184,
0.0698725057788655));
#97385=CARTESIAN_POINT('Ctrl Pts',(0.0121473922803572,-0.0320835708272304,
0.0699271809799954));
#97386=CARTESIAN_POINT('Ctrl Pts',(0.0122052165423121,-0.0319739230346346,
0.0699830452618357));
#97387=CARTESIAN_POINT('Ctrl Pts',(0.0122618065905709,-0.0318646057455575,
0.0700400214719917));
#97388=CARTESIAN_POINT('Ctrl Pts',(0.0119753842083881,-0.0321934096636184,
0.069880756562087));
#97389=CARTESIAN_POINT('Ctrl Pts',(0.0120342604026428,-0.0320835708272304,
0.0699338731556337));
#97390=CARTESIAN_POINT('Ctrl Pts',(0.0120920032011695,-0.0319739230346346,
0.0699881773791775));
#97391=CARTESIAN_POINT('Ctrl Pts',(0.0121485440583432,-0.0318646057455575,
0.070043594084309));
#97392=CARTESIAN_POINT('Ctrl Pts',(0.0118829453910787,-0.0320218834582305,
0.0697980475816695));
#97393=CARTESIAN_POINT('Ctrl Pts',(0.0119282386949749,-0.0319391099350621,
0.0698371713828407));
#97394=CARTESIAN_POINT('Ctrl Pts',(0.011972893633168,-0.0318564869454922,
0.0698769787411859));
#97395=CARTESIAN_POINT('Ctrl Pts',(0.0120168803872852,-0.0317740741446535,
0.069917437625872));
#97396=CARTESIAN_POINT('Ctrl Pts',(0.0118804025510494,-0.0320218834582305,
0.0697485464502481));
#97397=CARTESIAN_POINT('Ctrl Pts',(0.0119262110420555,-0.0319391099350621,
0.0697876437866018));
#97398=CARTESIAN_POINT('Ctrl Pts',(0.0119713812684715,-0.0318564869454922,
0.069827432740883));
#97399=CARTESIAN_POINT('Ctrl Pts',(0.0120158830353541,-0.0317740741446535,
0.0698678812606245));
#97400=CARTESIAN_POINT('Ctrl Pts',(0.0118778597110201,-0.0320218834582305,
0.0696990453188266));
#97401=CARTESIAN_POINT('Ctrl Pts',(0.011924183389136,-0.0319391099350621,
0.069738116190363));
#97402=CARTESIAN_POINT('Ctrl Pts',(0.011969868903775,-0.0318564869454922,
0.06977788674058));
#97403=CARTESIAN_POINT('Ctrl Pts',(0.012014885683423,-0.0317740741446535,
0.069818324895377));
#97404=CARTESIAN_POINT('Ctrl Pts',(0.0118753168709907,-0.0320218834582305,
0.0696495441874052));
#97405=CARTESIAN_POINT('Ctrl Pts',(0.0119221557362166,-0.0319391099350621,
0.0696885885941241));
#97406=CARTESIAN_POINT('Ctrl Pts',(0.0119683565390784,-0.0318564869454922,
0.069728340740277));
#97407=CARTESIAN_POINT('Ctrl Pts',(0.0120138883314918,-0.0317740741446535,
0.0697687685301295));
#97408=CARTESIAN_POINT('Origin',(0.0152822549363563,-0.0391228853390692,
0.0644218508279418));
#97409=CARTESIAN_POINT('Ctrl Pts',(0.00914413420753776,-0.0352722978779543,
0.06848934223705));
#97410=CARTESIAN_POINT('Ctrl Pts',(0.00916266609167554,-0.0352466642097183,
0.068493038444335));
#97411=CARTESIAN_POINT('Ctrl Pts',(0.00918119680116501,-0.0352210183808283,
0.0684966544721222));
#97412=CARTESIAN_POINT('Ctrl Pts',(0.00919972709192561,-0.0351953608940152,
0.0685001899253548));
#97413=CARTESIAN_POINT('Origin',(0.010279560610078,-0.0352456003065005,
0.0637227344203754));
#97414=CARTESIAN_POINT('Ctrl Pts',(0.0093216507798621,-0.0350241211493339,
0.0685262653877318));
#97415=CARTESIAN_POINT('Ctrl Pts',(0.00939911541483222,-0.0349144232867421,
0.0685427655356251));
#97416=CARTESIAN_POINT('Ctrl Pts',(0.00947628534628622,-0.0348045283677512,
0.0685608768089376));
#97417=CARTESIAN_POINT('Ctrl Pts',(0.00955306086609633,-0.0346945769586886,
0.0685805796876788));
#97418=CARTESIAN_POINT('Ctrl Pts',(0.0092620306643769,-0.0350241211493339,
0.0684298984658524));
#97419=CARTESIAN_POINT('Ctrl Pts',(0.00934082271412408,-0.0349144232867421,
0.0684455773711371));
#97420=CARTESIAN_POINT('Ctrl Pts',(0.00941933783054762,-0.0348045283677512,
0.0684628943488985));
#97421=CARTESIAN_POINT('Ctrl Pts',(0.00949747462036837,-0.0346945769586886,
0.0684818309606548));
#97422=CARTESIAN_POINT('Ctrl Pts',(0.00920241054889171,-0.0350241211493339,
0.068333531543973));
#97423=CARTESIAN_POINT('Ctrl Pts',(0.00928253001341594,-0.0349144232867421,
0.0683483892066491));
#97424=CARTESIAN_POINT('Ctrl Pts',(0.00936239031480901,-0.0348045283677512,
0.0683649118888594));
#97425=CARTESIAN_POINT('Ctrl Pts',(0.00944188837464041,-0.0346945769586886,
0.0683830822336308));
#97426=CARTESIAN_POINT('Ctrl Pts',(0.00914279043340651,-0.0350241211493339,
0.0682371646220936));
#97427=CARTESIAN_POINT('Ctrl Pts',(0.00922423731270781,-0.0349144232867421,
0.0682512010421611));
#97428=CARTESIAN_POINT('Ctrl Pts',(0.0093054427990704,-0.0348045283677512,
0.0682669294288202));
#97429=CARTESIAN_POINT('Ctrl Pts',(0.00938630212891245,-0.0346945769586886,
0.0682843335066068));
#97430=CARTESIAN_POINT('Origin',(0.0052056087878164,-0.0345629067941657,
0.0847967015889882));
#97431=CARTESIAN_POINT('Ctrl Pts',(0.00964823368459569,-0.035197097365166,
0.0684183711366379));
#97432=CARTESIAN_POINT('Ctrl Pts',(0.00972763763476626,-0.0350869349321805,
0.0684394903460552));
#97433=CARTESIAN_POINT('Ctrl Pts',(0.00980666830558493,-0.0349764985129744,
0.0684622778145007));
#97434=CARTESIAN_POINT('Ctrl Pts',(0.00988522157266863,-0.0348659306849651,
0.0684867100472114));
#97435=CARTESIAN_POINT('Ctrl Pts',(0.00957926827321185,-0.035197097365166,
0.0684631399056924));
#97436=CARTESIAN_POINT('Ctrl Pts',(0.00965805201275959,-0.0350869349321805,
0.0684833036927996));
#97437=CARTESIAN_POINT('Ctrl Pts',(0.00973648182188052,-0.0349764985129744,
0.0685051220536392));
#97438=CARTESIAN_POINT('Ctrl Pts',(0.00981445442853207,-0.0348659306849651,
0.0685285727031323));
#97439=CARTESIAN_POINT('Ctrl Pts',(0.009510302861828,-0.035197097365166,
0.0685079086747469));
#97440=CARTESIAN_POINT('Ctrl Pts',(0.00958846639075291,-0.0350869349321805,
0.0685271170395441));
#97441=CARTESIAN_POINT('Ctrl Pts',(0.00966629533817611,-0.0349764985129744,
0.0685479662927777));
#97442=CARTESIAN_POINT('Ctrl Pts',(0.0097436872843955,-0.0348659306849652,
0.0685704353590531));
#97443=CARTESIAN_POINT('Ctrl Pts',(0.00944133745044416,-0.035197097365166,
0.0685526774438014));
#97444=CARTESIAN_POINT('Ctrl Pts',(0.00951888076874623,-0.0350869349321805,
0.0685709303862885));
#97445=CARTESIAN_POINT('Ctrl Pts',(0.0095961088544717,-0.0349764985129744,
0.0685908105319162));
#97446=CARTESIAN_POINT('Ctrl Pts',(0.00967292014025894,-0.0348659306849652,
0.068612298014974));
#97447=CARTESIAN_POINT('Origin',(0.0047558508444338,-0.0345637187965071,
0.0846262810831878));
#97448=CARTESIAN_POINT('Ctrl Pts',(0.00940878355743313,-0.0352450361861253,
0.0685440302807021));
#97449=CARTESIAN_POINT('Ctrl Pts',(0.00962021616940426,-0.0349452761023765,
0.0685924949011781));
#97450=CARTESIAN_POINT('Ctrl Pts',(0.00982739757019066,-0.0346444289983475,
0.0686567478078128));
#97451=CARTESIAN_POINT('Ctrl Pts',(0.00916394689380343,-0.0352450361861253,
0.0684934831923322));
#97452=CARTESIAN_POINT('Ctrl Pts',(0.00937728592044621,-0.0349452761023765,
0.0685327136467514));
#97453=CARTESIAN_POINT('Ctrl Pts',(0.0095870638751338,-0.0346444289983475,
0.0685879022195713));
#97454=CARTESIAN_POINT('Ctrl Pts',(0.00967240335574919,-0.0345231616327822,
0.0686125770201603));
#97455=CARTESIAN_POINT('Ctrl Pts',(0.00974872893545784,-0.0344132092796975,
0.068633922582603));
#97456=CARTESIAN_POINT('Ctrl Pts',(0.00982460906099546,-0.0343032738558974,
0.0686568457781242));
#97457=CARTESIAN_POINT('Ctrl Pts',(0.00989994727340524,-0.034193496108874,
0.0686813147493598));
#97458=CARTESIAN_POINT('Ctrl Pts',(0.00961895181182228,-0.0345231616327822,
0.0685126567089605));
#97459=CARTESIAN_POINT('Ctrl Pts',(0.00969665465234427,-0.0344132092796975,
0.0685332655171239));
#97460=CARTESIAN_POINT('Ctrl Pts',(0.00977392720681601,-0.0343032738558974,
0.0685554804839326));
#97461=CARTESIAN_POINT('Ctrl Pts',(0.00985067120917691,-0.034193496108874,
0.0685792706136508));
#97462=CARTESIAN_POINT('Ctrl Pts',(0.00956550026789536,-0.0345231616327822,
0.0684127363977608));
#97463=CARTESIAN_POINT('Ctrl Pts',(0.00964458036923068,-0.0344132092796975,
0.0684326084516449));
#97464=CARTESIAN_POINT('Ctrl Pts',(0.00972324535263657,-0.0343032738558974,
0.068454115189741));
#97465=CARTESIAN_POINT('Ctrl Pts',(0.00980139514494859,-0.034193496108874,
0.0684772264779418));
#97466=CARTESIAN_POINT('Ctrl Pts',(0.00951204872396846,-0.0345231616327822,
0.068312816086561));
#97467=CARTESIAN_POINT('Ctrl Pts',(0.00959250608611711,-0.0344132092796975,
0.0683319513861659));
#97468=CARTESIAN_POINT('Ctrl Pts',(0.00967256349845712,-0.0343032738558974,
0.0683527498955494));
#97469=CARTESIAN_POINT('Ctrl Pts',(0.00975211908072027,-0.034193496108874,
0.0683751823422328));
#97470=CARTESIAN_POINT('Origin',(0.00520265157077387,-0.0345625596229807,
0.0848084384179098));
#97471=CARTESIAN_POINT('Ctrl Pts',(0.0100873068912915,-0.0346945769586886,
0.0684803817800777));
#97472=CARTESIAN_POINT('Ctrl Pts',(0.0101654370960595,-0.0345846629176053,
0.0685074401428784));
#97473=CARTESIAN_POINT('Ctrl Pts',(0.010243021089828,-0.0344746925050311,
0.0685361188278624));
#97474=CARTESIAN_POINT('Ctrl Pts',(0.0103199596148012,-0.034364806625326,
0.0685663806780462));
#97475=CARTESIAN_POINT('Ctrl Pts',(0.00998855824201811,-0.0346945769586886,
0.0685359679820395));
#97476=CARTESIAN_POINT('Ctrl Pts',(0.0100659224408271,-0.0345846629176053,
0.0685616655385408));
#97477=CARTESIAN_POINT('Ctrl Pts',(0.0101427684387163,-0.0344746925050311,
0.0685889673441078));
#97478=CARTESIAN_POINT('Ctrl Pts',(0.0102189979162095,-0.034364806625326,
0.0686178380098787));
#97479=CARTESIAN_POINT('Ctrl Pts',(0.00988980959274471,-0.0346945769586886,
0.0685915541840012));
#97480=CARTESIAN_POINT('Ctrl Pts',(0.00996640778559471,-0.0345846629176053,
0.0686158909342032));
#97481=CARTESIAN_POINT('Ctrl Pts',(0.0100425157876047,-0.0344746925050311,
0.0686418158603531));
#97482=CARTESIAN_POINT('Ctrl Pts',(0.0101180362176177,-0.034364806625326,
0.0686692953417112));
#97483=CARTESIAN_POINT('Ctrl Pts',(0.00979106094347131,-0.0346945769586886,
0.0686471403859629));
#97484=CARTESIAN_POINT('Ctrl Pts',(0.00986689313036234,-0.0345846629176053,
0.0686701163298657));
#97485=CARTESIAN_POINT('Ctrl Pts',(0.00994226313649308,-0.0344746925050311,
0.0686946643765985));
#97486=CARTESIAN_POINT('Ctrl Pts',(0.010017074519026,-0.034364806625326,
0.0687207526735436));
#97487=CARTESIAN_POINT('Origin',(0.00473871065156685,-0.0345626446731966,
0.0846821411257449));
#97488=CARTESIAN_POINT('Ctrl Pts',(0.00979282788793581,-0.0346945769586886,
0.0686461457624153));
#97489=CARTESIAN_POINT('Ctrl Pts',(0.00990810831856319,-0.0345275153362891,
0.0686811045927423));
#97490=CARTESIAN_POINT('Ctrl Pts',(0.0100223191435783,-0.0343603235965159,
0.0687196979286484));
#97491=CARTESIAN_POINT('Ctrl Pts',(0.0101351242745059,-0.034193496108874,
0.0687618066078137));
#97492=CARTESIAN_POINT('Ctrl Pts',(0.00971209243564077,-0.0346945769586886,
0.068623566677536));
#97493=CARTESIAN_POINT('Ctrl Pts',(0.00982784579424111,-0.0345275153362891,
0.0686568344714901));
#97494=CARTESIAN_POINT('Ctrl Pts',(0.00994258285109001,-0.0343603235965159,
0.0686937512067839));
#97495=CARTESIAN_POINT('Ctrl Pts',(0.0100559658876537,-0.034193496108874,
0.0687342026566066));
#97496=CARTESIAN_POINT('Ctrl Pts',(0.00963135698334572,-0.0346945769586886,
0.0686009875926567));
#97497=CARTESIAN_POINT('Ctrl Pts',(0.00974758326991903,-0.0345275153362891,
0.0686325643502378));
#97498=CARTESIAN_POINT('Ctrl Pts',(0.00986284655860173,-0.0343603235965159,
0.0686678044849194));
#97499=CARTESIAN_POINT('Ctrl Pts',(0.0099768075008016,-0.034193496108874,
0.0687065987053996));
#97500=CARTESIAN_POINT('Ctrl Pts',(0.00955062153105068,-0.0346945769586886,
0.0685784085077774));
#97501=CARTESIAN_POINT('Ctrl Pts',(0.00966732074559696,-0.0345275153362891,
0.0686082942289855));
#97502=CARTESIAN_POINT('Ctrl Pts',(0.00978311026611345,-0.0343603235965159,
0.068641857763055));
#97503=CARTESIAN_POINT('Ctrl Pts',(0.00989764911394947,-0.034193496108874,
0.0686789947541926));
#97504=CARTESIAN_POINT('Ctrl Pts',(0.0100170445409845,-0.0340223579322365,
0.0687207428093437));
#97505=CARTESIAN_POINT('Ctrl Pts',(0.0100919281577402,-0.0339125849573554,
0.0687468558349562));
#97506=CARTESIAN_POINT('Ctrl Pts',(0.0101662186756934,-0.0338030433565221,
0.0687745004281092));
#97507=CARTESIAN_POINT('Ctrl Pts',(0.0102398242236691,-0.0336938721132327,
0.06880363281423));
#97508=CARTESIAN_POINT('Ctrl Pts',(0.00996997242311036,-0.0340223579322365,
0.068617663250026));
#97509=CARTESIAN_POINT('Ctrl Pts',(0.0100462777758317,-0.0339125849573554,
0.0686431270283638));
#97510=CARTESIAN_POINT('Ctrl Pts',(0.0101220024686233,-0.0338030433565221,
0.0686701522570915));
#97511=CARTESIAN_POINT('Ctrl Pts',(0.0101970527260289,-0.0336938721132327,
0.0686986957911165));
#97512=CARTESIAN_POINT('Ctrl Pts',(0.00992290030523617,-0.0340223579322365,
0.0685145836907083));
#97513=CARTESIAN_POINT('Ctrl Pts',(0.0100006273939233,-0.0339125849573554,
0.0685393982217713));
#97514=CARTESIAN_POINT('Ctrl Pts',(0.0100777862615531,-0.0338030433565221,
0.0685658040860737));
#97515=CARTESIAN_POINT('Ctrl Pts',(0.0101542812283887,-0.0336938721132327,
0.0685937587680031));
#97516=CARTESIAN_POINT('Ctrl Pts',(0.00987582818736198,-0.0340223579322365,
0.0684115041313906));
#97517=CARTESIAN_POINT('Ctrl Pts',(0.00995497701201486,-0.0339125849573554,
0.0684356694151789));
#97518=CARTESIAN_POINT('Ctrl Pts',(0.010033570054483,-0.0338030433565221,
0.0684614559150559));
#97519=CARTESIAN_POINT('Ctrl Pts',(0.0101115097307485,-0.0336938721132327,
0.0684888217448896));
#97520=CARTESIAN_POINT('Origin',(0.0052369213529601,-0.0345589643414132,
0.0846932062174358));
#97521=CARTESIAN_POINT('Ctrl Pts',(0.0104394305973868,-0.034193496108874,
0.0686148602124408));
#97522=CARTESIAN_POINT('Ctrl Pts',(0.0105157568963052,-0.0340836138595105,
0.0686467916322565));
#97523=CARTESIAN_POINT('Ctrl Pts',(0.0105913858187076,-0.0339738896671456,
0.0686802871433586));
#97524=CARTESIAN_POINT('Ctrl Pts',(0.0106662234427092,-0.0338644633335883,
0.0687152973869414));
#97525=CARTESIAN_POINT('Ctrl Pts',(0.0103373863698591,-0.034193496108874,
0.0686641363210075));
#97526=CARTESIAN_POINT('Ctrl Pts',(0.0104130331804292,-0.0340836138595105,
0.0686946606113717));
#97527=CARTESIAN_POINT('Ctrl Pts',(0.0104880120581056,-0.0339738896671456,
0.068726735607604));
#97528=CARTESIAN_POINT('Ctrl Pts',(0.0105622297911055,-0.0338644633335883,
0.0687603138247538));
#97529=CARTESIAN_POINT('Ctrl Pts',(0.0102353421423314,-0.034193496108874,
0.0687134124295741));
#97530=CARTESIAN_POINT('Ctrl Pts',(0.0103103094645532,-0.0340836138595105,
0.0687425295904869));
#97531=CARTESIAN_POINT('Ctrl Pts',(0.0103846382975036,-0.0339738896671456,
0.0687731840718493));
#97532=CARTESIAN_POINT('Ctrl Pts',(0.0104582361395018,-0.0338644633335883,
0.0688053302625662));
#97533=CARTESIAN_POINT('Ctrl Pts',(0.0101332979148037,-0.034193496108874,
0.0687626885381408));
#97534=CARTESIAN_POINT('Ctrl Pts',(0.0102075857486772,-0.0340836138595105,
0.068790398569602));
#97535=CARTESIAN_POINT('Ctrl Pts',(0.0102812645369016,-0.0339738896671456,
0.0688196325360947));
#97536=CARTESIAN_POINT('Ctrl Pts',(0.010354242487898,-0.0338644633335883,
0.0688503467003786));
#97537=CARTESIAN_POINT('Origin',(0.00476282790100567,-0.0345610621862272,
0.0846108326147277));
#97538=CARTESIAN_POINT('Ctrl Pts',(0.0101011915342575,-0.03424362768739,
0.0687492614118496));
#97539=CARTESIAN_POINT('Ctrl Pts',(0.0103048837480143,-0.033943005420186,
0.0688238406346036));
#97540=CARTESIAN_POINT('Ctrl Pts',(0.0105023796809093,-0.0336441434784162,
0.068913550917747));
#97541=CARTESIAN_POINT('Ctrl Pts',(0.00986461960757254,-0.03424362768739,
0.0686684299606406));
#97542=CARTESIAN_POINT('Ctrl Pts',(0.0100713604297685,-0.033943005420186,
0.0687340867260913));
#97543=CARTESIAN_POINT('Ctrl Pts',(0.0102725683863685,-0.0336441434784162,
0.0688151295333762));
#97544=CARTESIAN_POINT('Ctrl Pts',(0.010354216881966,-0.0335235895815127,
0.0688503360610121));
#97545=CARTESIAN_POINT('Ctrl Pts',(0.0104271771901633,-0.0334144449262719,
0.0688810423858256));
#97546=CARTESIAN_POINT('Ctrl Pts',(0.0104995869513537,-0.0333049234473133,
0.0689132912935447));
#97547=CARTESIAN_POINT('Ctrl Pts',(0.0105713498403076,-0.0331951640388588,
0.068947049934907));
#97548=CARTESIAN_POINT('Ctrl Pts',(0.0103137101290925,-0.0335235895815127,
0.0687445042347124));
#97549=CARTESIAN_POINT('Ctrl Pts',(0.0103881274207425,-0.0334144449262719,
0.0687746529043221));
#97550=CARTESIAN_POINT('Ctrl Pts',(0.01046200736002,-0.0333049234473133,
0.0688063736163409));
#97551=CARTESIAN_POINT('Ctrl Pts',(0.0105352518029693,-0.0331951640388588,
0.0688396343671963));
#97552=CARTESIAN_POINT('Ctrl Pts',(0.0102732033762191,-0.0335235895815127,
0.0686386724084127));
#97553=CARTESIAN_POINT('Ctrl Pts',(0.0103490776513218,-0.0334144449262719,
0.0686682634228187));
#97554=CARTESIAN_POINT('Ctrl Pts',(0.0104244277686862,-0.0333049234473133,
0.0686994559391371));
#97555=CARTESIAN_POINT('Ctrl Pts',(0.0104991537656311,-0.0331951640388588,
0.0687322187994857));
#97556=CARTESIAN_POINT('Ctrl Pts',(0.0102326966233457,-0.0335235895815127,
0.068532840582113));
#97557=CARTESIAN_POINT('Ctrl Pts',(0.010310027881901,-0.0334144449262719,
0.0685618739413153));
#97558=CARTESIAN_POINT('Ctrl Pts',(0.0103868481773524,-0.0333049234473133,
0.0685925382619333));
#97559=CARTESIAN_POINT('Ctrl Pts',(0.0104630557282929,-0.0331951640388588,
0.068624803231775));
#97560=CARTESIAN_POINT('Origin',(0.00279531278370614,-0.0326434571769497,
0.0836889659829717));
#97561=CARTESIAN_POINT('Ctrl Pts',(0.010784293093255,-0.0336938721132351,
0.0687704180195108));
#97562=CARTESIAN_POINT('Ctrl Pts',(0.01081578157172,-0.0336474569764939,
0.0687859908726599));
#97563=CARTESIAN_POINT('Ctrl Pts',(0.0108470855926661,-0.033601104548885,
0.0688019312711447));
#97564=CARTESIAN_POINT('Ctrl Pts',(0.0109263401730489,-0.0334837508643151,
0.068842288693446));
#97565=CARTESIAN_POINT('Ctrl Pts',(0.0110043640766178,-0.0333660264760385,
0.068884976871181));
#97566=CARTESIAN_POINT('Ctrl Pts',(0.0104694828127738,-0.0336938721132351,
0.0688987321908988));
#97567=CARTESIAN_POINT('Ctrl Pts',(0.0105002202258146,-0.0336474569764939,
0.0689124623550111));
#97568=CARTESIAN_POINT('Ctrl Pts',(0.0105307948038016,-0.033601104548885,
0.0689265513985524));
#97569=CARTESIAN_POINT('Ctrl Pts',(0.010608202602401,-0.0334837508643151,
0.0689622216159913));
#97570=CARTESIAN_POINT('Ctrl Pts',(0.0106845194267492,-0.0333660264760385,
0.0690001699231677));
#97571=CARTESIAN_POINT('Ctrl Pts',(0.0104694828127854,-0.0336938721132426,
0.0688987321909096));
#97572=CARTESIAN_POINT('Ctrl Pts',(0.0105002202258254,-0.0336474569765026,
0.0689124623550215));
#97573=CARTESIAN_POINT('Ctrl Pts',(0.0105307948038116,-0.0336011045488949,
0.0689265513985624));
#97574=CARTESIAN_POINT('Ctrl Pts',(0.0106075579008808,-0.0334847282606778,
0.0689619245316742));
#97575=CARTESIAN_POINT('Ctrl Pts',(0.0106832483951838,-0.0333679869945434,
0.0689995381022298));
#97576=CARTESIAN_POINT('Ctrl Pts',(0.0104694828127689,-0.0336938721132426,
0.0688987321908966));
#97577=CARTESIAN_POINT('Ctrl Pts',(0.0105794134044654,-0.0335278710435082,
0.0689478373339662));
#97578=CARTESIAN_POINT('Ctrl Pts',(0.0106877653983156,-0.033362046922432,
0.0690003725967344));
#97579=CARTESIAN_POINT('Ctrl Pts',(0.0107945839423469,-0.0331951640388602,
0.0690563821289514));
#97580=CARTESIAN_POINT('Ctrl Pts',(0.0103922138851466,-0.0336938721132426,
0.0688662123100945));
#97581=CARTESIAN_POINT('Ctrl Pts',(0.0105028252514424,-0.0335278710435082,
0.0689136998973199));
#97582=CARTESIAN_POINT('Ctrl Pts',(0.0106119085065277,-0.033362046922432,
0.0689646395222109));
#97583=CARTESIAN_POINT('Ctrl Pts',(0.0107195094275136,-0.0331951640388602,
0.0690190746625966));
#97584=CARTESIAN_POINT('Ctrl Pts',(0.0103149449575244,-0.0336938721132426,
0.0688336924292923));
#97585=CARTESIAN_POINT('Ctrl Pts',(0.0104262370984195,-0.0335278710435082,
0.0688795624606737));
#97586=CARTESIAN_POINT('Ctrl Pts',(0.0105360516147399,-0.033362046922432,
0.0689289064476875));
#97587=CARTESIAN_POINT('Ctrl Pts',(0.0106444349126802,-0.0331951640388602,
0.0689817671962418));
#97588=CARTESIAN_POINT('Ctrl Pts',(0.0102376760299022,-0.0336938721132426,
0.0688011725484902));
#97589=CARTESIAN_POINT('Ctrl Pts',(0.0103496489453966,-0.0335278710435082,
0.0688454250240274));
#97590=CARTESIAN_POINT('Ctrl Pts',(0.010460194722952,-0.033362046922432,
0.0688931733731641));
#97591=CARTESIAN_POINT('Ctrl Pts',(0.0105693603978469,-0.0331951640388602,
0.068944459729887));
#97592=CARTESIAN_POINT('Ctrl Pts',(0.0106825833118407,-0.0330240426238155,
0.0690008430190253));
#97593=CARTESIAN_POINT('Ctrl Pts',(0.0107535179658339,-0.0329142774063509,
0.0690360929973547));
#97594=CARTESIAN_POINT('Ctrl Pts',(0.010823759267821,-0.0328043479726686,
0.0690728269665282));
#97595=CARTESIAN_POINT('Ctrl Pts',(0.0108932159374678,-0.0326943950436594,
0.069111000345748));
#97596=CARTESIAN_POINT('Ctrl Pts',(0.0106488017558345,-0.0330240426238155,
0.068892676746748));
#97597=CARTESIAN_POINT('Ctrl Pts',(0.0107212265056095,-0.0329142774063509,
0.0689274613512317));
#97598=CARTESIAN_POINT('Ctrl Pts',(0.0107929682668229,-0.0328043479726686,
0.0689637605189958));
#97599=CARTESIAN_POINT('Ctrl Pts',(0.0108639338522805,-0.0326943950436594,
0.0690015302791926));
#97600=CARTESIAN_POINT('Ctrl Pts',(0.0106150201998282,-0.0330240426238155,
0.0687845104744708));
#97601=CARTESIAN_POINT('Ctrl Pts',(0.0106889350453851,-0.0329142774063509,
0.0688188297051087));
#97602=CARTESIAN_POINT('Ctrl Pts',(0.0107621772658249,-0.0328043479726686,
0.0688546940714634));
#97603=CARTESIAN_POINT('Ctrl Pts',(0.0108346517670933,-0.0326943950436594,
0.0688920602126372));
#97604=CARTESIAN_POINT('Ctrl Pts',(0.0105812386438219,-0.0330240426238155,
0.0686763442021935));
#97605=CARTESIAN_POINT('Ctrl Pts',(0.0106566435851607,-0.0329142774063509,
0.0687101980589857));
#97606=CARTESIAN_POINT('Ctrl Pts',(0.0107313862648268,-0.0328043479726686,
0.068745627623931));
#97607=CARTESIAN_POINT('Ctrl Pts',(0.010805369681906,-0.0326943950436594,
0.0687825901460818));
#97608=CARTESIAN_POINT('Origin',(0.00273742768633797,-0.0326396682856775,
0.0837982578597));
#97609=CARTESIAN_POINT('Ctrl Pts',(0.0111149079858753,-0.0331951640388587,
0.0689487341452376));
#97610=CARTESIAN_POINT('Ctrl Pts',(0.0111865449009495,-0.0330855618255041,
0.0689899308520347));
#97611=CARTESIAN_POINT('Ctrl Pts',(0.0112573819925646,-0.0329757224427708,
0.0690326378695436));
#97612=CARTESIAN_POINT('Ctrl Pts',(0.0113273258669672,-0.0328657862078596,
0.0690768049584357));
#97613=CARTESIAN_POINT('Ctrl Pts',(0.0110074925036805,-0.0331951640388587,
0.0689848321538374));
#97614=CARTESIAN_POINT('Ctrl Pts',(0.0110786322417119,-0.0330855618255041,
0.069024549429667));
#97615=CARTESIAN_POINT('Ctrl Pts',(0.0111490023751854,-0.0329757224427708,
0.0690657656739077));
#97616=CARTESIAN_POINT('Ctrl Pts',(0.0112185102019574,-0.0328657862078596,
0.069108432526924));
#97617=CARTESIAN_POINT('Ctrl Pts',(0.0109000770214857,-0.0331951640388587,
0.0690209301624372));
#97618=CARTESIAN_POINT('Ctrl Pts',(0.0109707195824743,-0.0330855618255041,
0.0690591680072993));
#97619=CARTESIAN_POINT('Ctrl Pts',(0.0110406227578063,-0.0329757224427708,
0.0690988934782718));
#97620=CARTESIAN_POINT('Ctrl Pts',(0.0111096945369476,-0.0328657862078596,
0.0691400600954123));
#97621=CARTESIAN_POINT('Ctrl Pts',(0.0107926615392909,-0.0331951640388587,
0.069057028171037));
#97622=CARTESIAN_POINT('Ctrl Pts',(0.0108628069232368,-0.0330855618255041,
0.0690937865849316));
#97623=CARTESIAN_POINT('Ctrl Pts',(0.0109322431404272,-0.0329757224427708,
0.069132021282636));
#97624=CARTESIAN_POINT('Ctrl Pts',(0.0110008788719377,-0.0328657862078596,
0.0691716876639005));
#97625=CARTESIAN_POINT('Origin',(0.00233766583397968,-0.0326401908830995,
0.0835309315920745));
#97626=CARTESIAN_POINT('Ctrl Pts',(0.0107625554934886,-0.0332451089994432,
0.069039716204632));
#97627=CARTESIAN_POINT('Ctrl Pts',(0.0109552930001814,-0.0329451141710258,
0.0691392391679365));
#97628=CARTESIAN_POINT('Ctrl Pts',(0.0111399864835101,-0.0326442513127503,
0.0692529971739274));
#97629=CARTESIAN_POINT('Ctrl Pts',(0.0105379812583565,-0.0332451089994432,
0.0689298689792922));
#97630=CARTESIAN_POINT('Ctrl Pts',(0.0107348617209353,-0.0329451141710258,
0.0690209219867431));
#97631=CARTESIAN_POINT('Ctrl Pts',(0.0109243243821499,-0.0326442513127503,
0.0691265461635047));
#97632=CARTESIAN_POINT('Ctrl Pts',(0.0110008515680218,-0.0325229783203385,
0.0691716717806828));
#97633=CARTESIAN_POINT('Ctrl Pts',(0.011069477712407,-0.0324130253112079,
0.0692113321183767));
#97634=CARTESIAN_POINT('Ctrl Pts',(0.0111372730232755,-0.0323031222247694,
0.0692524060607307));
#97635=CARTESIAN_POINT('Ctrl Pts',(0.0112041525161893,-0.0321934096636184,
0.0692948379306147));
#97636=CARTESIAN_POINT('Ctrl Pts',(0.010973928464017,-0.0325229783203385,
0.0690615977641299));
#97637=CARTESIAN_POINT('Ctrl Pts',(0.0110440719762857,-0.0324130253112079,
0.0691008869674306));
#97638=CARTESIAN_POINT('Ctrl Pts',(0.0111133921022906,-0.0323031222247694,
0.0691416212203845));
#97639=CARTESIAN_POINT('Ctrl Pts',(0.0111818018890601,-0.0321934096636184,
0.0691837452120583));
#97640=CARTESIAN_POINT('Ctrl Pts',(0.0109470053600122,-0.0325229783203385,
0.068951523747577));
#97641=CARTESIAN_POINT('Ctrl Pts',(0.0110186662401643,-0.0324130253112079,
0.0689904418164846));
#97642=CARTESIAN_POINT('Ctrl Pts',(0.0110895111813056,-0.0323031222247694,
0.0690308363800384));
#97643=CARTESIAN_POINT('Ctrl Pts',(0.0111594512619309,-0.0321934096636184,
0.0690726524935018));
#97644=CARTESIAN_POINT('Ctrl Pts',(0.0109200822560075,-0.0325229783203385,
0.0688414497310241));
#97645=CARTESIAN_POINT('Ctrl Pts',(0.010993260504043,-0.0324130253112079,
0.0688799966655385));
#97646=CARTESIAN_POINT('Ctrl Pts',(0.0110656302603206,-0.0323031222247694,
0.0689200515396923));
#97647=CARTESIAN_POINT('Ctrl Pts',(0.0111371006348016,-0.0321934096636184,
0.0689615597749454));
#97648=CARTESIAN_POINT('Origin',(0.00274179022720111,-0.0326393375178865,
0.0837909326111887));
#97649=CARTESIAN_POINT('Ctrl Pts',(0.0114355958676124,-0.0326943950436593,
0.0691468119977909));
#97650=CARTESIAN_POINT('Ctrl Pts',(0.0115045491752563,-0.0325844576448126,
0.0691924549972257));
#97651=CARTESIAN_POINT('Ctrl Pts',(0.0115725633907719,-0.0324744968375318,
0.0692395272943391));
#97652=CARTESIAN_POINT('Ctrl Pts',(0.0116395522022605,-0.0323646534831894,
0.0692879673753842));
#97653=CARTESIAN_POINT('Ctrl Pts',(0.0113261258368723,-0.0326943950436593,
0.0691760940733979));
#97654=CARTESIAN_POINT('Ctrl Pts',(0.0113946755826339,-0.0325844576448126,
0.0692202283706404));
#97655=CARTESIAN_POINT('Ctrl Pts',(0.0114623174101414,-0.0324744968375318,
0.069265783512467));
#97656=CARTESIAN_POINT('Ctrl Pts',(0.0115289654578094,-0.0323646534831894,
0.0693126999355795));
#97657=CARTESIAN_POINT('Ctrl Pts',(0.0112166558061322,-0.0326943950436593,
0.0692053761490049));
#97658=CARTESIAN_POINT('Ctrl Pts',(0.0112848019900115,-0.0325844576448126,
0.0692480017440551));
#97659=CARTESIAN_POINT('Ctrl Pts',(0.0113520714295108,-0.0324744968375318,
0.0692920397305948));
#97660=CARTESIAN_POINT('Ctrl Pts',(0.0114183787133584,-0.0323646534831894,
0.0693374324957747));
#97661=CARTESIAN_POINT('Ctrl Pts',(0.0111071857753921,-0.0326943950436593,
0.0692346582246119));
#97662=CARTESIAN_POINT('Ctrl Pts',(0.0111749283973891,-0.0325844576448126,
0.0692757751174699));
#97663=CARTESIAN_POINT('Ctrl Pts',(0.0112418254488803,-0.0324744968375318,
0.0693182959487227));
#97664=CARTESIAN_POINT('Ctrl Pts',(0.0113077919689073,-0.0323646534831894,
0.0693621650559699));
#97665=CARTESIAN_POINT('Origin',(0.00231819156432896,-0.0326395579069474,
0.0835633771557399));
#97666=CARTESIAN_POINT('Ctrl Pts',(0.0110781921989789,-0.0327445246961876,
0.0692154699801082));
#97667=CARTESIAN_POINT('Ctrl Pts',(0.0112643010392078,-0.0324436878365474,
0.0693268973739101));
#97668=CARTESIAN_POINT('Ctrl Pts',(0.0114414879972651,-0.0321434074463186,
0.0694520266925976));
#97669=CARTESIAN_POINT('Ctrl Pts',(0.0108609576303243,-0.0327445246961876,
0.0690917398617802));
#97670=CARTESIAN_POINT('Ctrl Pts',(0.0110517330282052,-0.0324436878365474,
0.069194974119971));
#97671=CARTESIAN_POINT('Ctrl Pts',(0.011234190427171,-0.0321434074463186,
0.0693122850830711));
#97672=CARTESIAN_POINT('Ctrl Pts',(0.0113868112395716,-0.0322357242816072,
0.069413886990164));
#97673=CARTESIAN_POINT('Ctrl Pts',(0.0115376502964213,-0.0319819883628705,
0.0695178102333001));
#97674=CARTESIAN_POINT('Ctrl Pts',(0.0116815707259465,-0.0317295851069886,
0.0696311211837884));
#97675=CARTESIAN_POINT('Ctrl Pts',(0.0111779078597899,-0.0322357242816072,
0.0692765575398782));
#97676=CARTESIAN_POINT('Ctrl Pts',(0.0113331206815214,-0.0319819883628705,
0.0693738274813061));
#97677=CARTESIAN_POINT('Ctrl Pts',(0.0114818293805723,-0.0317295851069886,
0.0694807769289991));
#97678=CARTESIAN_POINT('Origin',(0.00236966104337161,-0.0326371942646938,
0.0834831693243248));
#97679=CARTESIAN_POINT('Origin',(0.00280414287347799,-0.0326352985528283,
0.083685216243867));
#97680=CARTESIAN_POINT('Ctrl Pts',(0.0117432135338001,-0.0321934096636183,
0.0693646351476498));
#97681=CARTESIAN_POINT('Ctrl Pts',(0.0118092074446005,-0.0320835708272304,
0.0694145499266512));
#97682=CARTESIAN_POINT('Ctrl Pts',(0.0118741300924936,-0.0319739230346346,
0.0694658014936061));
#97683=CARTESIAN_POINT('Ctrl Pts',(0.0119379034459866,-0.0318646057455575,
0.0695183179007587));
#97684=CARTESIAN_POINT('Ctrl Pts',(0.0116321207195778,-0.0321934096636183,
0.069386985794026));
#97685=CARTESIAN_POINT('Ctrl Pts',(0.0116978063975456,-0.0320835708272304,
0.0694353685165387));
#97686=CARTESIAN_POINT('Ctrl Pts',(0.0117624526972231,-0.0319739230346346,
0.0694850825367976));
#97687=CARTESIAN_POINT('Ctrl Pts',(0.01182598178971,-0.0318646057455575,
0.0695360579013665));
#97688=CARTESIAN_POINT('Ctrl Pts',(0.0115210279053554,-0.0321934096636183,
0.0694093364404021));
#97689=CARTESIAN_POINT('Ctrl Pts',(0.0115864053504907,-0.0320835708272304,
0.0694561871064263));
#97690=CARTESIAN_POINT('Ctrl Pts',(0.0116507753019525,-0.0319739230346346,
0.0695043635799891));
#97691=CARTESIAN_POINT('Ctrl Pts',(0.0117140601334333,-0.0318646057455575,
0.0695537979019742));
#97692=CARTESIAN_POINT('Ctrl Pts',(0.011409935091133,-0.0321934096636183,
0.0694316870867783));
#97693=CARTESIAN_POINT('Ctrl Pts',(0.0114750043034357,-0.0320835708272304,
0.0694770056963138));
#97694=CARTESIAN_POINT('Ctrl Pts',(0.011539097906682,-0.0319739230346346,
0.0695236446231807));
#97695=CARTESIAN_POINT('Ctrl Pts',(0.0116021384771566,-0.0318646057455575,
0.069571537902582));
#97696=CARTESIAN_POINT('Ctrl Pts',(0.0113078589975475,-0.0320218834582309,
0.0693612159472554));
#97697=CARTESIAN_POINT('Ctrl Pts',(0.0113576986627241,-0.0319391099350625,
0.0693943544893326));
#97698=CARTESIAN_POINT('Ctrl Pts',(0.0114069906683328,-0.0318564869454927,
0.069428251206969));
#97699=CARTESIAN_POINT('Ctrl Pts',(0.0114557014165997,-0.031774074144654,
0.0694628780591373));
#97700=CARTESIAN_POINT('Ctrl Pts',(0.0112991320717052,-0.0320218834582309,
0.0693124238494042));
#97701=CARTESIAN_POINT('Ctrl Pts',(0.0113494795446663,-0.0319391099350625,
0.0693454715652805));
#97702=CARTESIAN_POINT('Ctrl Pts',(0.0113992804686555,-0.0318564869454927,
0.0693792854412352));
#97703=CARTESIAN_POINT('Ctrl Pts',(0.0114485008695863,-0.031774074144654,
0.0694138374619745));
#97704=CARTESIAN_POINT('Ctrl Pts',(0.0112904051458629,-0.0320218834582309,
0.069263631751553));
#97705=CARTESIAN_POINT('Ctrl Pts',(0.0113412604266085,-0.0319391099350625,
0.0692965886412284));
#97706=CARTESIAN_POINT('Ctrl Pts',(0.0113915702689782,-0.0318564869454927,
0.0693303196755014));
#97707=CARTESIAN_POINT('Ctrl Pts',(0.0114413003225729,-0.031774074144654,
0.0693647968648116));
#97708=CARTESIAN_POINT('Ctrl Pts',(0.0112816782200206,-0.0320218834582309,
0.0692148396537017));
#97709=CARTESIAN_POINT('Ctrl Pts',(0.0113330413085507,-0.0319391099350625,
0.0692477057171764));
#97710=CARTESIAN_POINT('Ctrl Pts',(0.0113838600693009,-0.0318564869454927,
0.0692813539097676));
#97711=CARTESIAN_POINT('Ctrl Pts',(0.0114340997755596,-0.031774074144654,
0.0693157562676487));
#97712=CARTESIAN_POINT('Origin',(0.0140065478483093,-0.0391228853390673,
0.0636013656535299));
#97713=CARTESIAN_POINT('Ctrl Pts',(0.00842661988560802,-0.0352722978779546,
0.0684060941969251));
#97714=CARTESIAN_POINT('Ctrl Pts',(0.00844546889791518,-0.0352466642097184,
0.0684074385975486));
#97715=CARTESIAN_POINT('Ctrl Pts',(0.00846430669568076,-0.0352210183808285,
0.0684087035981362));
#97716=CARTESIAN_POINT('Ctrl Pts',(0.00848313397934979,-0.0351953608940152,
0.0684098887120041));
#97717=CARTESIAN_POINT('Origin',(0.00895567874103067,-0.0352456003065015,
0.0635347658441051));
#97718=CARTESIAN_POINT('Ctrl Pts',(0.00860736438460647,-0.035024121149334,
0.0684204774715147));
#97719=CARTESIAN_POINT('Ctrl Pts',(0.00868628620468203,-0.0349144232867422,
0.0684271386176258));
#97720=CARTESIAN_POINT('Ctrl Pts',(0.00876511757262519,-0.0348045283677512,
0.0684354351210956));
#97721=CARTESIAN_POINT('Ctrl Pts',(0.008843757120033,-0.0346945769586886,
0.0684453601125965));
#97722=CARTESIAN_POINT('Ctrl Pts',(0.00853613641361172,-0.035024121149334,
0.0683323428134569));
#97723=CARTESIAN_POINT('Ctrl Pts',(0.00861627225241067,-0.0349144232867422,
0.0683380228235164));
#97724=CARTESIAN_POINT('Ctrl Pts',(0.00869633864650826,-0.0348045283677512,
0.0683453626983107));
#97725=CARTESIAN_POINT('Ctrl Pts',(0.00877623269118711,-0.0346945769586886,
0.0683543568526987));
#97726=CARTESIAN_POINT('Ctrl Pts',(0.00846490844261696,-0.035024121149334,
0.0682442081553991));
#97727=CARTESIAN_POINT('Ctrl Pts',(0.0085462583001393,-0.0349144232867422,
0.068248907029407));
#97728=CARTESIAN_POINT('Ctrl Pts',(0.00862755972039133,-0.0348045283677512,
0.0682552902755259));
#97729=CARTESIAN_POINT('Ctrl Pts',(0.00870870826234121,-0.0346945769586886,
0.0682633535928009));
#97730=CARTESIAN_POINT('Ctrl Pts',(0.00839368047162221,-0.035024121149334,
0.0681560734973413));
#97731=CARTESIAN_POINT('Ctrl Pts',(0.00847624434786794,-0.0349144232867422,
0.0681597912352976));
#97732=CARTESIAN_POINT('Ctrl Pts',(0.0085587807942744,-0.0348045283677512,
0.0681652178527411));
#97733=CARTESIAN_POINT('Ctrl Pts',(0.00864118383349532,-0.0346945769586886,
0.0681723503329031));
#97734=CARTESIAN_POINT('Origin',(0.0065630049941059,-0.034562906794416,
0.0850784932751654));
#97735=CARTESIAN_POINT('Ctrl Pts',(0.00891784935021737,-0.0351970973651661,
0.0682725023073406));
#97736=CARTESIAN_POINT('Ctrl Pts',(0.00899927411533065,-0.0350869349321806,
0.068283503031651));
#97737=CARTESIAN_POINT('Ctrl Pts',(0.00908053763280962,-0.0349764985129744,
0.068296205644577));
#97738=CARTESIAN_POINT('Ctrl Pts',(0.00916153365464846,-0.0348659306849652,
0.0683105998868645));
#97739=CARTESIAN_POINT('Ctrl Pts',(0.00885503876628931,-0.0351970973651661,
0.0683255617192924));
#97740=CARTESIAN_POINT('Ctrl Pts',(0.00893572846515821,-0.0350869349321806,
0.0683356922880859));
#97741=CARTESIAN_POINT('Ctrl Pts',(0.00901627439752347,-0.0349764985129744,
0.0683475087430483));
#97742=CARTESIAN_POINT('Ctrl Pts',(0.00909657131261243,-0.0348659306849652,
0.0683610019182447));
#97743=CARTESIAN_POINT('Ctrl Pts',(0.00879222818236124,-0.0351970973651661,
0.0683786211312442));
#97744=CARTESIAN_POINT('Ctrl Pts',(0.00887218281498578,-0.0350869349321806,
0.0683878815445207));
#97745=CARTESIAN_POINT('Ctrl Pts',(0.00895201116223733,-0.0349764985129744,
0.0683988118415197));
#97746=CARTESIAN_POINT('Ctrl Pts',(0.0090316089705764,-0.0348659306849652,
0.0684114039496248));
#97747=CARTESIAN_POINT('Ctrl Pts',(0.00872941759843317,-0.0351970973651661,
0.0684316805431959));
#97748=CARTESIAN_POINT('Ctrl Pts',(0.00880863716481334,-0.0350869349321806,
0.0684400708009555));
#97749=CARTESIAN_POINT('Ctrl Pts',(0.00888774792695119,-0.0349764985129744,
0.068450114939991));
#97750=CARTESIAN_POINT('Ctrl Pts',(0.00896664662854037,-0.0348659306849652,
0.068461805981005));
#97751=CARTESIAN_POINT('Origin',(0.00609543417322961,-0.034563718796662,
0.084965786203636));
#97752=CARTESIAN_POINT('Ctrl Pts',(0.00869603662568097,-0.0352450361861253,
0.0684271816502354));
#97753=CARTESIAN_POINT('Ctrl Pts',(0.00891187625595256,-0.0349452761023765,
0.0684487645797641));
#97754=CARTESIAN_POINT('Ctrl Pts',(0.0091254769940661,-0.0346444289983475,
0.0684865441181435));
#97755=CARTESIAN_POINT('Ctrl Pts',(0.00844679534224049,-0.0352450361861253,
0.0684077193115027));
#97756=CARTESIAN_POINT('Ctrl Pts',(0.00866336900664345,-0.0349452761023765,
0.0684199019520167));
#97757=CARTESIAN_POINT('Ctrl Pts',(0.00887840976178802,-0.0346444289983475,
0.0684483631970645));
#97758=CARTESIAN_POINT('Ctrl Pts',(0.00896616888765449,-0.0345231616327822,
0.0684621475564246));
#97759=CARTESIAN_POINT('Ctrl Pts',(0.00904456792573297,-0.0344132092796975,
0.0684737586710232));
#97760=CARTESIAN_POINT('Ctrl Pts',(0.00912272275203471,-0.0343032738558974,
0.068486990808804));
#97761=CARTESIAN_POINT('Ctrl Pts',(0.00920053367542413,-0.0341934961088741,
0.0685018244531206));
#97762=CARTESIAN_POINT('Ctrl Pts',(0.0089006154894152,-0.0345231616327822,
0.0683697144015627));
#97763=CARTESIAN_POINT('Ctrl Pts',(0.00898028858839797,-0.0344132092796975,
0.0683804219548584));
#97764=CARTESIAN_POINT('Ctrl Pts',(0.00905973609932115,-0.0343032738558974,
0.0683927769309008));
#97765=CARTESIAN_POINT('Ctrl Pts',(0.00913885664618559,-0.0341934961088741,
0.0684067608943678));
#97766=CARTESIAN_POINT('Ctrl Pts',(0.00883506209117591,-0.0345231616327822,
0.0682772812467008));
#97767=CARTESIAN_POINT('Ctrl Pts',(0.00891600925106296,-0.0344132092796975,
0.0682870852386936));
#97768=CARTESIAN_POINT('Ctrl Pts',(0.00899674944660758,-0.0343032738558974,
0.0682985630529975));
#97769=CARTESIAN_POINT('Ctrl Pts',(0.00907717961694704,-0.0341934961088741,
0.068311697335615));
#97770=CARTESIAN_POINT('Ctrl Pts',(0.00876950869293662,-0.0345231616327822,
0.0681848480918389));
#97771=CARTESIAN_POINT('Ctrl Pts',(0.00885172991372796,-0.0344132092796975,
0.0681937485225288));
#97772=CARTESIAN_POINT('Ctrl Pts',(0.00893376279389401,-0.0343032738558974,
0.0682043491750943));
#97773=CARTESIAN_POINT('Ctrl Pts',(0.0090155025877085,-0.0341934961088741,
0.0682166337768622));
#97774=CARTESIAN_POINT('Origin',(0.00656154210998243,-0.0345625596230191,
0.0850905081937899));
#97775=CARTESIAN_POINT('Ctrl Pts',(0.00936123232799057,-0.0346945769586885,
0.0682789935135691));
#97776=CARTESIAN_POINT('Ctrl Pts',(0.0094421377648623,-0.0345846629176052,
0.0682960462018945));
#97777=CARTESIAN_POINT('Ctrl Pts',(0.0095227043779901,-0.0344746925050311,
0.0683147748940696));
#97778=CARTESIAN_POINT('Ctrl Pts',(0.00960282903525073,-0.034364806625326,
0.0683351551664054));
#97779=CARTESIAN_POINT('Ctrl Pts',(0.00927022913974539,-0.0346945769586885,
0.0683465178892488));
#97780=CARTESIAN_POINT('Ctrl Pts',(0.00935020405659018,-0.0345846629176052,
0.0683623165076428));
#97781=CARTESIAN_POINT('Ctrl Pts',(0.00942986592440711,-0.0344746925050311,
0.0683797716729162));
#97782=CARTESIAN_POINT('Ctrl Pts',(0.00950911276359782,-0.034364806625326,
0.0683988605979571));
#97783=CARTESIAN_POINT('Ctrl Pts',(0.00917922595150019,-0.0346945769586885,
0.0684140422649284));
#97784=CARTESIAN_POINT('Ctrl Pts',(0.00925827034831806,-0.0345846629176052,
0.068428586813391));
#97785=CARTESIAN_POINT('Ctrl Pts',(0.00933702747082412,-0.0344746925050311,
0.0684447684517628));
#97786=CARTESIAN_POINT('Ctrl Pts',(0.00941539649194491,-0.034364806625326,
0.0684625660295089));
#97787=CARTESIAN_POINT('Ctrl Pts',(0.00908822276325501,-0.0346945769586885,
0.068481566640608));
#97788=CARTESIAN_POINT('Ctrl Pts',(0.00916633664004595,-0.0345846629176052,
0.0684948571191392));
#97789=CARTESIAN_POINT('Ctrl Pts',(0.00924418901724114,-0.0344746925050311,
0.0685097652306094));
#97790=CARTESIAN_POINT('Ctrl Pts',(0.009321680220292,-0.034364806625326,
0.0685262714610606));
#97791=CARTESIAN_POINT('Origin',(0.00608543025515759,-0.0345626446730496,
0.0850233540094552));
#97792=CARTESIAN_POINT('Ctrl Pts',(0.00908985111544923,-0.0346945769586886,
0.068480358403101));
#97793=CARTESIAN_POINT('Ctrl Pts',(0.00920860402869501,-0.0345275153362891,
0.068500593103472));
#97794=CARTESIAN_POINT('Ctrl Pts',(0.00932675129482487,-0.0343603235965159,
0.0685245677073899));
#97795=CARTESIAN_POINT('Ctrl Pts',(0.0094439445405227,-0.034193496108874,
0.0685522061152209));
#97796=CARTESIAN_POINT('Ctrl Pts',(0.00900692237659121,-0.0346945769586886,
0.0684680761963494));
#97797=CARTESIAN_POINT('Ctrl Pts',(0.00912593254557493,-0.0345275153362891,
0.0684865739210822));
#97798=CARTESIAN_POINT('Ctrl Pts',(0.00924439176026727,-0.0343603235965159,
0.0685088191905472));
#97799=CARTESIAN_POINT('Ctrl Pts',(0.00936195064873045,-0.034193496108874,
0.068534741006002));
#97800=CARTESIAN_POINT('Ctrl Pts',(0.00892399363773319,-0.0346945769586886,
0.0684557939895979));
#97801=CARTESIAN_POINT('Ctrl Pts',(0.00904326106245485,-0.0345275153362891,
0.0684725547386924));
#97802=CARTESIAN_POINT('Ctrl Pts',(0.00916203222570968,-0.0343603235965159,
0.0684930706737045));
#97803=CARTESIAN_POINT('Ctrl Pts',(0.0092799567569382,-0.034193496108874,
0.068517275896783));
#97804=CARTESIAN_POINT('Ctrl Pts',(0.00884106489887517,-0.0346945769586886,
0.0684435117828463));
#97805=CARTESIAN_POINT('Ctrl Pts',(0.00896058957933477,-0.0345275153362891,
0.0684585355563027));
#97806=CARTESIAN_POINT('Ctrl Pts',(0.00907967269115209,-0.0343603235965159,
0.0684773221568619));
#97807=CARTESIAN_POINT('Ctrl Pts',(0.00919796286514594,-0.034193496108874,
0.0684998107875641));
#97808=CARTESIAN_POINT('Ctrl Pts',(0.00932164924232423,-0.0340223579322365,
0.0685262654318876));
#97809=CARTESIAN_POINT('Ctrl Pts',(0.00939921520933324,-0.0339125849573555,
0.0685427871426646));
#97810=CARTESIAN_POINT('Ctrl Pts',(0.00947638471061337,-0.0338030433565222,
0.0685609026791053));
#97811=CARTESIAN_POINT('Ctrl Pts',(0.00955306111301236,-0.0336938721132328,
0.068580580126324));
#97812=CARTESIAN_POINT('Ctrl Pts',(0.00926202900767557,-0.0340223579322365,
0.0684298983864274));
#97813=CARTESIAN_POINT('Ctrl Pts',(0.00934092412757726,-0.0339125849573555,
0.0684455977786725));
#97814=CARTESIAN_POINT('Ctrl Pts',(0.00941943886785254,-0.0338030433565222,
0.0684629190847914));
#97815=CARTESIAN_POINT('Ctrl Pts',(0.00949747478497886,-0.0336938721132328,
0.0684818312530846));
#97816=CARTESIAN_POINT('Ctrl Pts',(0.00920240877302691,-0.0340223579322365,
0.0683335313409672));
#97817=CARTESIAN_POINT('Ctrl Pts',(0.00928263304582129,-0.0339125849573555,
0.0683484084146803));
#97818=CARTESIAN_POINT('Ctrl Pts',(0.00936249302509171,-0.0338030433565222,
0.0683649354904774));
#97819=CARTESIAN_POINT('Ctrl Pts',(0.00944188845694536,-0.0336938721132328,
0.0683830823798452));
#97820=CARTESIAN_POINT('Ctrl Pts',(0.00914278853837825,-0.0340223579322365,
0.068237164295507));
#97821=CARTESIAN_POINT('Ctrl Pts',(0.00922434196406532,-0.0339125849573555,
0.0682512190506882));
#97822=CARTESIAN_POINT('Ctrl Pts',(0.00930554718233089,-0.0338030433565222,
0.0682669518961634));
#97823=CARTESIAN_POINT('Ctrl Pts',(0.00938630212891187,-0.0336938721132328,
0.0682843335066058));
#97824=CARTESIAN_POINT('Origin',(0.00658109924038061,-0.0345589643414756,
0.0849718894913104));
#97825=CARTESIAN_POINT('Ctrl Pts',(0.00972743405026164,-0.034193496108874,
0.0683682787406266));
#97826=CARTESIAN_POINT('Ctrl Pts',(0.00980716056262902,-0.0340836138581107,
0.0683903921500919));
#97827=CARTESIAN_POINT('Ctrl Pts',(0.00988639123010831,-0.03397388966435,
0.068414144722012));
#97828=CARTESIAN_POINT('Ctrl Pts',(0.00996502668511442,-0.0338644633294063,
0.0684394992583226));
#97829=CARTESIAN_POINT('Ctrl Pts',(0.00963237040597177,-0.034193496108874,
0.0684299558253615));
#97830=CARTESIAN_POINT('Ctrl Pts',(0.00971124642786439,-0.0340836138581107,
0.0684507583634664));
#97831=CARTESIAN_POINT('Ctrl Pts',(0.00978965413868244,-0.03397388966435,
0.0684731830938911));
#97832=CARTESIAN_POINT('Ctrl Pts',(0.00986749511019974,-0.0338644633294063,
0.0684971945886511));
#97833=CARTESIAN_POINT('Ctrl Pts',(0.00953730676168191,-0.034193496108874,
0.0684916329100963));
#97834=CARTESIAN_POINT('Ctrl Pts',(0.00961533229309976,-0.0340836138581107,
0.0685111245768409));
#97835=CARTESIAN_POINT('Ctrl Pts',(0.00969291704725657,-0.03397388966435,
0.0685322214657703));
#97836=CARTESIAN_POINT('Ctrl Pts',(0.00976996353528506,-0.0338644633294063,
0.0685548899189796));
#97837=CARTESIAN_POINT('Ctrl Pts',(0.00944224311739205,-0.034193496108874,
0.0685533099948311));
#97838=CARTESIAN_POINT('Ctrl Pts',(0.00951941815833512,-0.0340836138581107,
0.0685714907902154));
#97839=CARTESIAN_POINT('Ctrl Pts',(0.0095961799558307,-0.03397388966435,
0.0685912598376494));
#97840=CARTESIAN_POINT('Ctrl Pts',(0.00967243196037038,-0.0338644633294063,
0.0686125852493082));
#97841=CARTESIAN_POINT('Origin',(0.00610042000738715,-0.0345610621863924,
0.0849495850931085));
#97842=CARTESIAN_POINT('Ctrl Pts',(0.00940870704009062,-0.0342436276873901,
0.0685440127419332));
#97843=CARTESIAN_POINT('Ctrl Pts',(0.00962014033504646,-0.0339430054201861,
0.068592474481438));
#97844=CARTESIAN_POINT('Ctrl Pts',(0.0098273226333917,-0.0336441434784162,
0.0686567245683181));
#97845=CARTESIAN_POINT('Ctrl Pts',(0.00916386968655442,-0.0342436276873901,
0.068493468995402));
#97846=CARTESIAN_POINT('Ctrl Pts',(0.00937720927033622,-0.0339430054201861,
0.0685326965418909));
#97847=CARTESIAN_POINT('Ctrl Pts',(0.00958698799919459,-0.0336441434784162,
0.0685878822586144));
#97848=CARTESIAN_POINT('Ctrl Pts',(0.00967240521996829,-0.0335235895815128,
0.0686125779022954));
#97849=CARTESIAN_POINT('Ctrl Pts',(0.00974863873732299,-0.0334144449262719,
0.0686338977472179));
#97850=CARTESIAN_POINT('Ctrl Pts',(0.00982451938580206,-0.0333049234473133,
0.0686568170131558));
#97851=CARTESIAN_POINT('Ctrl Pts',(0.00989994748262462,-0.0331951640388588,
0.0686813151826251));
#97852=CARTESIAN_POINT('Ctrl Pts',(0.00961895362993591,-0.0335235895815128,
0.0685126574338753));
#97853=CARTESIAN_POINT('Ctrl Pts',(0.00969656274926369,-0.0334144449262719,
0.0685332414124246));
#97854=CARTESIAN_POINT('Ctrl Pts',(0.00977383578256132,-0.0333049234473133,
0.0685554523854694));
#97855=CARTESIAN_POINT('Ctrl Pts',(0.00985067134865647,-0.0331951640388588,
0.0685792709024943));
#97856=CARTESIAN_POINT('Ctrl Pts',(0.00956550203990353,-0.0335235895815128,
0.0684127369654553));
#97857=CARTESIAN_POINT('Ctrl Pts',(0.00964448676120439,-0.0334144449262719,
0.0684325850776313));
#97858=CARTESIAN_POINT('Ctrl Pts',(0.00972315217932059,-0.0333049234473133,
0.068454087757783));
#97859=CARTESIAN_POINT('Ctrl Pts',(0.00980139521468832,-0.0331951640388588,
0.0684772266223635));
#97860=CARTESIAN_POINT('Ctrl Pts',(0.00951205044987115,-0.0335235895815128,
0.0683128164970353));
#97861=CARTESIAN_POINT('Ctrl Pts',(0.0095924107731451,-0.0334144449262719,
0.068331928742838));
#97862=CARTESIAN_POINT('Ctrl Pts',(0.00967246857607985,-0.0333049234473133,
0.0683527231300966));
#97863=CARTESIAN_POINT('Ctrl Pts',(0.00975211908072016,-0.0331951640388588,
0.0683751823422326));
#97864=CARTESIAN_POINT('Origin',(0.00403287880815687,-0.0326434571769683,
0.0842815826877775));
#97865=CARTESIAN_POINT('Ctrl Pts',(0.0100890737653109,-0.033693872113235,
0.0684793871961827));
#97866=CARTESIAN_POINT('Ctrl Pts',(0.010122265743759,-0.0336474569764938,
0.0684908906999072));
#97867=CARTESIAN_POINT('Ctrl Pts',(0.0101553207848362,-0.033601104548885,
0.06850278196942));
#97868=CARTESIAN_POINT('Ctrl Pts',(0.010239008545416,-0.033483750864315,
0.0685328879285582));
#97869=CARTESIAN_POINT('Ctrl Pts',(0.0103217674545512,-0.0333660264760382,
0.0685654605091318));
#97870=CARTESIAN_POINT('Ctrl Pts',(0.00979282788793425,-0.033693872113235,
0.0686461457624149));
#97871=CARTESIAN_POINT('Ctrl Pts',(0.00982504377315792,-0.0336474569764938,
0.0686559152407143));
#97872=CARTESIAN_POINT('Ctrl Pts',(0.00985714308685013,-0.033601104548885,
0.0686660611772151));
#97873=CARTESIAN_POINT('Ctrl Pts',(0.00993841116553064,-0.033483750864315,
0.0686917483546339));
#97874=CARTESIAN_POINT('Ctrl Pts',(0.0100188823929709,-0.0333660264760383,
0.0687198323937026));
#97875=CARTESIAN_POINT('Ctrl Pts',(0.00979282788794581,-0.0336938721132427,
0.0686461457624253));
#97876=CARTESIAN_POINT('Ctrl Pts',(0.00982504377316868,-0.0336474569765026,
0.0686559152407246));
#97877=CARTESIAN_POINT('Ctrl Pts',(0.00985714308686013,-0.0336011045488949,
0.0686660611772251));
#97878=CARTESIAN_POINT('Ctrl Pts',(0.00993773431313503,-0.0334847282606778,
0.0686915344154427));
#97879=CARTESIAN_POINT('Ctrl Pts',(0.0100175421957065,-0.0333679869945434,
0.0687193648573588));
#97880=CARTESIAN_POINT('Ctrl Pts',(0.00979282788792897,-0.0336938721132426,
0.0686461457624133));
#97881=CARTESIAN_POINT('Ctrl Pts',(0.00990804615044084,-0.0335278710435082,
0.0686810857402377));
#97882=CARTESIAN_POINT('Ctrl Pts',(0.0100221281708153,-0.033362046922432,
0.0687196266410151));
#97883=CARTESIAN_POINT('Ctrl Pts',(0.0101351242745049,-0.0331951640388601,
0.0687618066078133));
#97884=CARTESIAN_POINT('Ctrl Pts',(0.0097120924270641,-0.0336938721132426,
0.0686235666751374));
#97885=CARTESIAN_POINT('Ctrl Pts',(0.00982778336255979,-0.0335278710435082,
0.0686568165283469));
#97886=CARTESIAN_POINT('Ctrl Pts',(0.00994239089150128,-0.033362046922432,
0.0686936827219932));
#97887=CARTESIAN_POINT('Ctrl Pts',(0.0100559658792504,-0.0331951640388601,
0.0687342026536762));
#97888=CARTESIAN_POINT('Ctrl Pts',(0.00963135696619923,-0.0336938721132426,
0.0686009875878615));
#97889=CARTESIAN_POINT('Ctrl Pts',(0.00974752057467875,-0.0335278710435082,
0.0686325473164561));
#97890=CARTESIAN_POINT('Ctrl Pts',(0.0098626536121873,-0.033362046922432,
0.0686677388029712));
#97891=CARTESIAN_POINT('Ctrl Pts',(0.00997680748399584,-0.0331951640388601,
0.0687065986995392));
#97892=CARTESIAN_POINT('Ctrl Pts',(0.00955062150533435,-0.0336938721132426,
0.0685784085005856));
#97893=CARTESIAN_POINT('Ctrl Pts',(0.00966725778679771,-0.0335278710435082,
0.0686082781045653));
#97894=CARTESIAN_POINT('Ctrl Pts',(0.00978291633287332,-0.033362046922432,
0.0686417948839492));
#97895=CARTESIAN_POINT('Ctrl Pts',(0.00989764908874131,-0.0331951640388601,
0.0686789947454021));
#97896=CARTESIAN_POINT('Ctrl Pts',(0.0100170459061869,-0.0330240426238155,
0.0687207428415402));
#97897=CARTESIAN_POINT('Ctrl Pts',(0.0100918392130133,-0.0329142774063509,
0.0687468243937052));
#97898=CARTESIAN_POINT('Ctrl Pts',(0.0101661306284923,-0.0328043479726686,
0.068774465135052));
#97899=CARTESIAN_POINT('Ctrl Pts',(0.0102398240046069,-0.0326943950436594,
0.0688036322767755));
#97900=CARTESIAN_POINT('Ctrl Pts',(0.00996997389917268,-0.0330240426238155,
0.0686176634442766));
#97901=CARTESIAN_POINT('Ctrl Pts',(0.0100461872251217,-0.0329142774063509,
0.0686430965336849));
#97902=CARTESIAN_POINT('Ctrl Pts',(0.0101219127731913,-0.0328043479726686,
0.0686701178447547));
#97903=CARTESIAN_POINT('Ctrl Pts',(0.0101970525799876,-0.0326943950436594,
0.068698695432814));
#97904=CARTESIAN_POINT('Ctrl Pts',(0.00992290189215845,-0.0330240426238155,
0.068514584047013));
#97905=CARTESIAN_POINT('Ctrl Pts',(0.0100005352372302,-0.0329142774063509,
0.0685393686736647));
#97906=CARTESIAN_POINT('Ctrl Pts',(0.0100776949178904,-0.0328043479726686,
0.0685657705544574));
#97907=CARTESIAN_POINT('Ctrl Pts',(0.0101542811553683,-0.0326943950436594,
0.0685937585888524));
#97908=CARTESIAN_POINT('Ctrl Pts',(0.00987582988514422,-0.0330240426238155,
0.0684115046497494));
#97909=CARTESIAN_POINT('Ctrl Pts',(0.00995488324933863,-0.0329142774063509,
0.0684356408136444));
#97910=CARTESIAN_POINT('Ctrl Pts',(0.0100334770625894,-0.0328043479726686,
0.06846142326416));
#97911=CARTESIAN_POINT('Ctrl Pts',(0.0101115097307491,-0.0326943950436594,
0.0684888217448909));
#97912=CARTESIAN_POINT('Origin',(0.00398914805644169,-0.032639668285777,
0.0843972676920441));
#97913=CARTESIAN_POINT('Ctrl Pts',(0.0104394305973869,-0.0331951640388587,
0.0686148602124409));
#97914=CARTESIAN_POINT('Ctrl Pts',(0.0105156659504639,-0.0330855618255041,
0.0686467535846912));
#97915=CARTESIAN_POINT('Ctrl Pts',(0.0105912970790538,-0.0329757224427708,
0.0686802456028626));
#97916=CARTESIAN_POINT('Ctrl Pts',(0.0106662250291835,-0.0328657862078596,
0.0687152981291199));
#97917=CARTESIAN_POINT('Ctrl Pts',(0.0103373863984962,-0.0331951640388587,
0.068664136307179));
#97918=CARTESIAN_POINT('Ctrl Pts',(0.0104129430730529,-0.0330855618255041,
0.0686946242270234));
#97919=CARTESIAN_POINT('Ctrl Pts',(0.0104879240821715,-0.0329757224427708,
0.0687266957524929));
#97920=CARTESIAN_POINT('Ctrl Pts',(0.0105622313936229,-0.0328657862078596,
0.0687603145239418));
#97921=CARTESIAN_POINT('Ctrl Pts',(0.0102353421996055,-0.0331951640388587,
0.0687134124019171));
#97922=CARTESIAN_POINT('Ctrl Pts',(0.0103102201956419,-0.0330855618255041,
0.0687424948693555));
#97923=CARTESIAN_POINT('Ctrl Pts',(0.0103845510852892,-0.0329757224427708,
0.0687731459021232));
#97924=CARTESIAN_POINT('Ctrl Pts',(0.0104582377580623,-0.0328657862078596,
0.0688053309187638));
#97925=CARTESIAN_POINT('Ctrl Pts',(0.0101332980007148,-0.0331951640388587,
0.0687626884966553));
#97926=CARTESIAN_POINT('Ctrl Pts',(0.010207497318231,-0.0330855618255041,
0.0687903655116877));
#97927=CARTESIAN_POINT('Ctrl Pts',(0.0102811780884069,-0.0329757224427708,
0.0688195960517534));
#97928=CARTESIAN_POINT('Ctrl Pts',(0.0103542441225017,-0.0328657862078596,
0.0688503473135857));
#97929=CARTESIAN_POINT('Origin',(0.00355903358096729,-0.0326401908835644,
0.0841821528168722));
#97930=CARTESIAN_POINT('Ctrl Pts',(0.010101259585347,-0.0332451089994432,
0.0687492863283464));
#97931=CARTESIAN_POINT('Ctrl Pts',(0.0103049508340365,-0.0329451141710258,
0.0688238681084164));
#97932=CARTESIAN_POINT('Ctrl Pts',(0.0105024456128185,-0.0326442513127503,
0.0689135808670683));
#97933=CARTESIAN_POINT('Ctrl Pts',(0.00986468867718615,-0.0332451089994432,
0.0686684518962526));
#97934=CARTESIAN_POINT('Ctrl Pts',(0.0100714286463617,-0.0329451141710258,
0.0687341112585429));
#97935=CARTESIAN_POINT('Ctrl Pts',(0.0102726355575189,-0.0326442513127503,
0.0688151565891526));
#97936=CARTESIAN_POINT('Ctrl Pts',(0.0103542150431901,-0.0325229783203385,
0.0688503349776998));
#97937=CARTESIAN_POINT('Ctrl Pts',(0.0104272708082967,-0.0324130253112079,
0.0688810814452022));
#97938=CARTESIAN_POINT('Ctrl Pts',(0.0104996794629,-0.0323031222247695,
0.0689133345017209));
#97939=CARTESIAN_POINT('Ctrl Pts',(0.010571349714495,-0.0321934096636184,
0.0689470495605312));
#97940=CARTESIAN_POINT('Ctrl Pts',(0.0103137083034759,-0.0325229783203385,
0.0687445032873275));
#97941=CARTESIAN_POINT('Ctrl Pts',(0.0103882229560934,-0.0324130253112079,
0.0687746913703189));
#97942=CARTESIAN_POINT('Ctrl Pts',(0.0104621018278394,-0.0323031222247695,
0.0688064163059783));
#97943=CARTESIAN_POINT('Ctrl Pts',(0.0105352517190943,-0.0321934096636184,
0.0688396341176126));
#97944=CARTESIAN_POINT('Ctrl Pts',(0.0102732015637618,-0.0325229783203385,
0.0686386715969551));
#97945=CARTESIAN_POINT('Ctrl Pts',(0.0103491751038901,-0.0324130253112079,
0.0686683012954356));
#97946=CARTESIAN_POINT('Ctrl Pts',(0.0104245241927788,-0.0323031222247695,
0.0686994981102356));
#97947=CARTESIAN_POINT('Ctrl Pts',(0.0104991537236937,-0.0321934096636184,
0.068732218674694));
#97948=CARTESIAN_POINT('Ctrl Pts',(0.0102326948240477,-0.0325229783203385,
0.0685328399065827));
#97949=CARTESIAN_POINT('Ctrl Pts',(0.0103101272516868,-0.0324130253112079,
0.0685619112205522));
#97950=CARTESIAN_POINT('Ctrl Pts',(0.0103869465577181,-0.0323031222247695,
0.0685925799144929));
#97951=CARTESIAN_POINT('Ctrl Pts',(0.0104630557282931,-0.0321934096636184,
0.0686248032317755));
#97952=CARTESIAN_POINT('Origin',(0.0039925581003947,-0.0326393375180069,
0.0843894534338173));
#97953=CARTESIAN_POINT('Ctrl Pts',(0.0107824154971495,-0.0326943950436593,
0.0687711833127807));
#97954=CARTESIAN_POINT('Ctrl Pts',(0.010856545672076,-0.0325844576448127,
0.0688078242625201));
#97955=CARTESIAN_POINT('Ctrl Pts',(0.0109299232983959,-0.0324744968375319,
0.0688460009389521));
#97956=CARTESIAN_POINT('Ctrl Pts',(0.0110024550350888,-0.0323646534831895,
0.0688856631311333));
#97957=CARTESIAN_POINT('Ctrl Pts',(0.0106774786875208,-0.0326943950436593,
0.0688139547234062));
#97958=CARTESIAN_POINT('Ctrl Pts',(0.0107510193922467,-0.0325844576448127,
0.0688491494472364));
#97959=CARTESIAN_POINT('Ctrl Pts',(0.0108238374169712,-0.0324744968375319,
0.0688858676041973));
#97960=CARTESIAN_POINT('Ctrl Pts',(0.0108958401118926,-0.0323646534831895,
0.0689240608619753));
#97961=CARTESIAN_POINT('Ctrl Pts',(0.010572541877892,-0.0326943950436593,
0.0688567261340318));
#97962=CARTESIAN_POINT('Ctrl Pts',(0.0106454931124174,-0.0325844576448127,
0.0688904746319527));
#97963=CARTESIAN_POINT('Ctrl Pts',(0.0107177515355465,-0.0324744968375319,
0.0689257342694425));
#97964=CARTESIAN_POINT('Ctrl Pts',(0.0107892251886963,-0.0323646534831895,
0.0689624585928173));
#97965=CARTESIAN_POINT('Ctrl Pts',(0.0104676050682633,-0.0326943950436593,
0.0688994975446573));
#97966=CARTESIAN_POINT('Ctrl Pts',(0.0105399668325881,-0.0325844576448127,
0.068931799816669));
#97967=CARTESIAN_POINT('Ctrl Pts',(0.0106116656541218,-0.0324744968375319,
0.0689656009346878));
#97968=CARTESIAN_POINT('Ctrl Pts',(0.0106826102655001,-0.0323646534831895,
0.0690008563236593));
#97969=CARTESIAN_POINT('Origin',(0.00354377937801091,-0.0326395579068536,
0.0842167833115162));
#97970=CARTESIAN_POINT('Ctrl Pts',(0.0104364351901299,-0.0327445246961876,
0.0688840944638773));
#97971=CARTESIAN_POINT('Ctrl Pts',(0.0106350420621385,-0.0324436878365475,
0.0689713175966564));
#97972=CARTESIAN_POINT('Ctrl Pts',(0.0108265147102331,-0.0321434074463186,
0.0690732528188931));
#97973=CARTESIAN_POINT('Ctrl Pts',(0.0102054060851146,-0.0327445246961876,
0.0687885667054201));
#97974=CARTESIAN_POINT('Ctrl Pts',(0.0104076158453951,-0.0324436878365475,
0.0688670764331495));
#97975=CARTESIAN_POINT('Ctrl Pts',(0.0106033374756105,-0.0321434074463186,
0.0689605943884664));
#97976=CARTESIAN_POINT('Ctrl Pts',(0.010767488922872,-0.0322357242816072,
0.0690422666742474));
#97977=CARTESIAN_POINT('Ctrl Pts',(0.0109301636048097,-0.0319819883628705,
0.0691264653048283));
#97978=CARTESIAN_POINT('Ctrl Pts',(0.0110871508065841,-0.0317295851069886,
0.0692208447518193));
#97979=CARTESIAN_POINT('Ctrl Pts',(0.0105430208645683,-0.0322357242816072,
0.0689322026437861));
#97980=CARTESIAN_POINT('Ctrl Pts',(0.0107092009431285,-0.0319819883628705,
0.0690092522578344));
#97981=CARTESIAN_POINT('Ctrl Pts',(0.0108701413497775,-0.0317295851069886,
0.069096720235077));
#97982=CARTESIAN_POINT('Origin',(0.00358479029800732,-0.0326371942645875,
0.0841307571064515));
#97983=CARTESIAN_POINT('Origin',(0.00404116930378793,-0.0326352985530836,
0.0842767558123109));
#97984=CARTESIAN_POINT('Ctrl Pts',(0.0111149079858754,-0.0321934096636184,
0.0689487341452376));
#97985=CARTESIAN_POINT('Ctrl Pts',(0.0111866374956326,-0.0320835708272304,
0.0689899841010614));
#97986=CARTESIAN_POINT('Ctrl Pts',(0.0112574717336673,-0.0319739230346346,
0.0690326945687108));
#97987=CARTESIAN_POINT('Ctrl Pts',(0.0113273242663435,-0.0318646057455575,
0.0690768039476986));
#97988=CARTESIAN_POINT('Ctrl Pts',(0.0110074924504581,-0.0321934096636184,
0.0689848321717232));
#97989=CARTESIAN_POINT('Ctrl Pts',(0.011078724140297,-0.0320835708272304,
0.0690246007835992));
#97990=CARTESIAN_POINT('Ctrl Pts',(0.0111490915035051,-0.0319739230346346,
0.0690658204641829));
#97991=CARTESIAN_POINT('Ctrl Pts',(0.0112185085573961,-0.0318646057455575,
0.0691084315661897));
#97992=CARTESIAN_POINT('Ctrl Pts',(0.0109000769150408,-0.0321934096636184,
0.0690209301982089));
#97993=CARTESIAN_POINT('Ctrl Pts',(0.0109708107849613,-0.0320835708272304,
0.0690592174661369));
#97994=CARTESIAN_POINT('Ctrl Pts',(0.0110407112733429,-0.0319739230346346,
0.069098946359655));
#97995=CARTESIAN_POINT('Ctrl Pts',(0.0111096928484487,-0.0318646057455575,
0.0691400591846809));
#97996=CARTESIAN_POINT('Ctrl Pts',(0.0107926613796235,-0.0321934096636184,
0.0690570282246946));
#97997=CARTESIAN_POINT('Ctrl Pts',(0.0108628974296257,-0.0320835708272304,
0.0690938341486746));
#97998=CARTESIAN_POINT('Ctrl Pts',(0.0109323310431808,-0.0319739230346346,
0.0691320722551271));
#97999=CARTESIAN_POINT('Ctrl Pts',(0.0110008771395012,-0.0318646057455575,
0.0691716868031721));
#98000=CARTESIAN_POINT('Ctrl Pts',(0.0106825578107348,-0.0320218834582315,
0.0689999062980342));
#98001=CARTESIAN_POINT('Ctrl Pts',(0.0107361578358993,-0.0319391099350631,
0.0690265369664127));
#98002=CARTESIAN_POINT('Ctrl Pts',(0.0107893095445496,-0.0318564869454932,
0.0690539884718543));
#98003=CARTESIAN_POINT('Ctrl Pts',(0.0108419760893676,-0.0317740741446544,
0.0690822372053611));
#98004=CARTESIAN_POINT('Ctrl Pts',(0.0106677844279134,-0.0320218834582315,
0.0689525927142832));
#98005=CARTESIAN_POINT('Ctrl Pts',(0.0107218768731049,-0.0319391099350631,
0.0689790696274609));
#98006=CARTESIAN_POINT('Ctrl Pts',(0.0107755231043464,-0.0318564869454932,
0.069006375160066));
#98007=CARTESIAN_POINT('Ctrl Pts',(0.0108286859041999,-0.0317740741446544,
0.0690344857757955));
#98008=CARTESIAN_POINT('Ctrl Pts',(0.010653011045092,-0.0320218834582315,
0.0689052791305322));
#98009=CARTESIAN_POINT('Ctrl Pts',(0.0107075959103105,-0.0319391099350631,
0.0689316022885092));
#98010=CARTESIAN_POINT('Ctrl Pts',(0.0107617366641432,-0.0318564869454932,
0.0689587618482776));
#98011=CARTESIAN_POINT('Ctrl Pts',(0.0108153957190322,-0.0317740741446544,
0.06898673434623));
#98012=CARTESIAN_POINT('Ctrl Pts',(0.0106382376622707,-0.0320218834582315,
0.0688579655467812));
#98013=CARTESIAN_POINT('Ctrl Pts',(0.0106933149475161,-0.0319391099350631,
0.0688841349495575));
#98014=CARTESIAN_POINT('Ctrl Pts',(0.0107479502239401,-0.0318564869454932,
0.0689111485364893));
#98015=CARTESIAN_POINT('Ctrl Pts',(0.0108021055338645,-0.0317740741446544,
0.0689389829166644));
#98016=CARTESIAN_POINT('Origin',(0.0126380660316932,-0.0391228853390702,
0.0629472387442048));
#98017=CARTESIAN_POINT('Ctrl Pts',(0.00770432963236102,-0.0352722978779549,
0.0684134309825576));
#98018=CARTESIAN_POINT('Ctrl Pts',(0.00772319851265365,-0.0352466642097187,
0.0684124023745188));
#98019=CARTESIAN_POINT('Ctrl Pts',(0.00774204631537146,-0.0352210183808286,
0.0684112963980917));
#98020=CARTESIAN_POINT('Ctrl Pts',(0.00776087367443863,-0.0351953608940152,
0.0684101124826413));
#98021=CARTESIAN_POINT('Origin',(0.00761867736647191,-0.0352456003065027,
0.0635142058516324));
#98022=CARTESIAN_POINT('Ctrl Pts',(0.007885451609313,-0.0350241211493338,
0.0684050475482226));
#98023=CARTESIAN_POINT('Ctrl Pts',(0.00796458597024578,-0.034914423286742,
0.0684017646422982));
#98024=CARTESIAN_POINT('Ctrl Pts',(0.00804383555691403,-0.0348045283677512,
0.0684001155351095));
#98025=CARTESIAN_POINT('Ctrl Pts',(0.00812309893927992,-0.0346945769586886,
0.0684001061163253));
#98026=CARTESIAN_POINT('Ctrl Pts',(0.00780373909046085,-0.0350241211493338,
0.0683265350901932));
#98027=CARTESIAN_POINT('Ctrl Pts',(0.00788395492826286,-0.034914423286742,
0.0683221266278758));
#98028=CARTESIAN_POINT('Ctrl Pts',(0.00796430990517022,-0.0348045283677512,
0.068319373645493));
#98029=CARTESIAN_POINT('Ctrl Pts',(0.00804470122789617,-0.0346945769586886,
0.068318283499325));
#98030=CARTESIAN_POINT('Ctrl Pts',(0.0077220265716087,-0.0350241211493338,
0.0682480226321637));
#98031=CARTESIAN_POINT('Ctrl Pts',(0.00780332388627993,-0.034914423286742,
0.0682424886134533));
#98032=CARTESIAN_POINT('Ctrl Pts',(0.0078847842534264,-0.0348045283677512,
0.0682386317558764));
#98033=CARTESIAN_POINT('Ctrl Pts',(0.00796630351651241,-0.0346945769586886,
0.0682364608823247));
#98034=CARTESIAN_POINT('Ctrl Pts',(0.00764031405275655,-0.0350241211493338,
0.0681695101741343));
#98035=CARTESIAN_POINT('Ctrl Pts',(0.00772269284429701,-0.034914423286742,
0.0681628505990308));
#98036=CARTESIAN_POINT('Ctrl Pts',(0.00780525860168259,-0.0348045283677512,
0.0681578898662599));
#98037=CARTESIAN_POINT('Ctrl Pts',(0.00788790580512866,-0.0346945769586886,
0.0681546382653243));
#98038=CARTESIAN_POINT('Origin',(0.00794501558844048,-0.0345629067942562,
0.0851879360948764));
#98039=CARTESIAN_POINT('Ctrl Pts',(0.00817494210242489,-0.0351970973651569,
0.0682193251277047));
#98040=CARTESIAN_POINT('Ctrl Pts',(0.00825710356490954,-0.0350869349326871,
0.068220033878911));
#98041=CARTESIAN_POINT('Ctrl Pts',(0.0083393183544485,-0.0349764985139992,
0.0682224513085043));
#98042=CARTESIAN_POINT('Ctrl Pts',(0.00842147977500923,-0.0348659306865088,
0.0682265805545339));
#98043=CARTESIAN_POINT('Ctrl Pts',(0.00811927690638267,-0.0351970973651569,
0.0682798384039308));
#98044=CARTESIAN_POINT('Ctrl Pts',(0.00820060003943912,-0.0350869349326871,
0.0682797759892892));
#98045=CARTESIAN_POINT('Ctrl Pts',(0.0082819918371981,-0.0349764985139992,
0.0682814041858056));
#98046=CARTESIAN_POINT('Ctrl Pts',(0.00836334673002591,-0.0348659306865088,
0.0682847270912407));
#98047=CARTESIAN_POINT('Ctrl Pts',(0.00806361171034044,-0.0351970973651569,
0.0683403516801568));
#98048=CARTESIAN_POINT('Ctrl Pts',(0.00814409651396871,-0.0350869349326871,
0.0683395180996673));
#98049=CARTESIAN_POINT('Ctrl Pts',(0.0082246653199477,-0.0349764985139992,
0.068340357063107));
#98050=CARTESIAN_POINT('Ctrl Pts',(0.00830521368504259,-0.0348659306865088,
0.0683428736279475));
#98051=CARTESIAN_POINT('Ctrl Pts',(0.00800794651429821,-0.0351970973651569,
0.0684008649563829));
#98052=CARTESIAN_POINT('Ctrl Pts',(0.00808759298849829,-0.0350869349326871,
0.0683992602100455));
#98053=CARTESIAN_POINT('Ctrl Pts',(0.00816733880269731,-0.0349764985139992,
0.0683993099404083));
#98054=CARTESIAN_POINT('Ctrl Pts',(0.00824708064005927,-0.0348659306865088,
0.0684010201646543));
#98055=CARTESIAN_POINT('Origin',(0.00746700576144667,-0.0345637187965205,
0.0851347199151462));
#98056=CARTESIAN_POINT('Ctrl Pts',(0.00797426489967894,-0.0352450361861252,
0.0684005852837905));
#98057=CARTESIAN_POINT('Ctrl Pts',(0.00819110762834526,-0.0349452761023764,
0.06839494614668));
#98058=CARTESIAN_POINT('Ctrl Pts',(0.00840775909254698,-0.0346444289983475,
0.0684056565109156));
#98059=CARTESIAN_POINT('Ctrl Pts',(0.00772454968035705,-0.0352450361861252,
0.0684125146274031));
#98060=CARTESIAN_POINT('Ctrl Pts',(0.00794094248645773,-0.0349452761023764,
0.0683974573264934));
#98061=CARTESIAN_POINT('Ctrl Pts',(0.0081578547208915,-0.0346444289983475,
0.0683987423929325));
#98062=CARTESIAN_POINT('Ctrl Pts',(0.00824664947816935,-0.0345231616327822,
0.0684014189234823));
#98063=CARTESIAN_POINT('Ctrl Pts',(0.00832588557495387,-0.0344132092796975,
0.0684031124760236));
#98064=CARTESIAN_POINT('Ctrl Pts',(0.00840508255372156,-0.0343032738558974,
0.0684064448773467));
#98065=CARTESIAN_POINT('Ctrl Pts',(0.00848413906334682,-0.034193496108874,
0.0684114092593122));
#98066=CARTESIAN_POINT('Ctrl Pts',(0.00817002804186763,-0.0345231616327822,
0.0683179306510274));
#98067=CARTESIAN_POINT('Ctrl Pts',(0.00825041490694585,-0.0344132092796975,
0.0683185680849436));
#98068=CARTESIAN_POINT('Ctrl Pts',(0.00833078443961359,-0.0343032738558974,
0.068320868224867));
#98069=CARTESIAN_POINT('Ctrl Pts',(0.00841103375269323,-0.034193496108874,
0.0683248254866254));
#98070=CARTESIAN_POINT('Ctrl Pts',(0.00809340660556591,-0.0345231616327822,
0.0682344423785725));
#98071=CARTESIAN_POINT('Ctrl Pts',(0.00817494423893782,-0.0344132092796975,
0.0682340236938637));
#98072=CARTESIAN_POINT('Ctrl Pts',(0.00825648632550562,-0.0343032738558974,
0.0682352915723873));
#98073=CARTESIAN_POINT('Ctrl Pts',(0.00833792844203965,-0.034193496108874,
0.0682382417139386));
#98074=CARTESIAN_POINT('Ctrl Pts',(0.00801678516926419,-0.0345231616327822,
0.0681509541061177));
#98075=CARTESIAN_POINT('Ctrl Pts',(0.0080994735709298,-0.0344132092796975,
0.0681494793027837));
#98076=CARTESIAN_POINT('Ctrl Pts',(0.00818218821139765,-0.0343032738558974,
0.0681497149199076));
#98077=CARTESIAN_POINT('Ctrl Pts',(0.00826482313138606,-0.034193496108874,
0.0681516579412518));
#98078=CARTESIAN_POINT('Origin',(0.00794507010844505,-0.0345625596230578,
0.0852000396209644));
#98079=CARTESIAN_POINT('Ctrl Pts',(0.00861564243684595,-0.0346945769586885,
0.0681701945265211));
#98080=CARTESIAN_POINT('Ctrl Pts',(0.00869804717875144,-0.0345846629176052,
0.0681769726092896));
#98081=CARTESIAN_POINT('Ctrl Pts',(0.00878032582762136,-0.0344746925050311,
0.0681854559459922));
#98082=CARTESIAN_POINT('Ctrl Pts',(0.00886237300346016,-0.034364806625326,
0.0681956332314106));
#98083=CARTESIAN_POINT('Ctrl Pts',(0.00853381988427018,-0.0346945769586885,
0.068248592176177));
#98084=CARTESIAN_POINT('Ctrl Pts',(0.00861514426693746,-0.0345846629176052,
0.0682542427028139));
#98085=CARTESIAN_POINT('Ctrl Pts',(0.00869636568943892,-0.0344746925050311,
0.0682615759494103));
#98086=CARTESIAN_POINT('Ctrl Pts',(0.00877738012033336,-0.034364806625326,
0.0682705820899701));
#98087=CARTESIAN_POINT('Ctrl Pts',(0.0084519973316944,-0.0346945769586885,
0.0683269898258329));
#98088=CARTESIAN_POINT('Ctrl Pts',(0.00853224135512349,-0.0345846629176052,
0.0683315127963383));
#98089=CARTESIAN_POINT('Ctrl Pts',(0.00861240555125647,-0.0344746925050311,
0.0683376959528283));
#98090=CARTESIAN_POINT('Ctrl Pts',(0.00869238723720655,-0.034364806625326,
0.0683455309485296));
#98091=CARTESIAN_POINT('Ctrl Pts',(0.00837017477911863,-0.0346945769586885,
0.0684053874754887));
#98092=CARTESIAN_POINT('Ctrl Pts',(0.00844933844330952,-0.0345846629176052,
0.0684087828898626));
#98093=CARTESIAN_POINT('Ctrl Pts',(0.00852844541307403,-0.0344746925050311,
0.0684138159562464));
#98094=CARTESIAN_POINT('Ctrl Pts',(0.00860739435407974,-0.034364806625326,
0.0684204798070892));
#98095=CARTESIAN_POINT('Origin',(0.00746429588693701,-0.0345626446732229,
0.0851930876050632));
#98096=CARTESIAN_POINT('Ctrl Pts',(0.00837163885895575,-0.0346945769586886,
0.0684039846786495));
#98097=CARTESIAN_POINT('Ctrl Pts',(0.00849199145043852,-0.0345275153362891,
0.068409176135752));
#98098=CARTESIAN_POINT('Ctrl Pts',(0.00861221190471851,-0.0343603235965159,
0.0684181539138563));
#98099=CARTESIAN_POINT('Ctrl Pts',(0.00873194505769413,-0.034193496108874,
0.0684308861761511));
#98100=CARTESIAN_POINT('Ctrl Pts',(0.00828782466928575,-0.0346945769586886,
0.0684021930477631));
#98101=CARTESIAN_POINT('Ctrl Pts',(0.00840821478719476,-0.0345275153362891,
0.0684056289831056));
#98102=CARTESIAN_POINT('Ctrl Pts',(0.00852852798715076,-0.0343603235965159,
0.0684128519655537));
#98103=CARTESIAN_POINT('Ctrl Pts',(0.00864840875361607,-0.034193496108874,
0.0684238353441258));
#98104=CARTESIAN_POINT('Ctrl Pts',(0.00820401047961575,-0.0346945769586886,
0.0684004014168768));
#98105=CARTESIAN_POINT('Ctrl Pts',(0.00832443812395101,-0.0345275153362891,
0.0684020818304593));
#98106=CARTESIAN_POINT('Ctrl Pts',(0.00844484406958301,-0.0343603235965159,
0.0684075500172511));
#98107=CARTESIAN_POINT('Ctrl Pts',(0.00856487244953801,-0.034193496108874,
0.0684167845121004));
#98108=CARTESIAN_POINT('Ctrl Pts',(0.00812019628994575,-0.0346945769586886,
0.0683986097859904));
#98109=CARTESIAN_POINT('Ctrl Pts',(0.00824066146070725,-0.0345275153362891,
0.068398534677813));
#98110=CARTESIAN_POINT('Ctrl Pts',(0.00836116015201525,-0.0343603235965159,
0.0684022480689486));
#98111=CARTESIAN_POINT('Ctrl Pts',(0.00848133614545995,-0.034193496108874,
0.0684097336800751));
#98112=CARTESIAN_POINT('Ctrl Pts',(0.00860736286472677,-0.0340223579322365,
0.0684204777080269));
#98113=CARTESIAN_POINT('Ctrl Pts',(0.00868638792035394,-0.0339125849573552,
0.0684271475467199));
#98114=CARTESIAN_POINT('Ctrl Pts',(0.00876521939582711,-0.0338030433565217,
0.0684354483336169));
#98115=CARTESIAN_POINT('Ctrl Pts',(0.00884375741997943,-0.0336938721132321,
0.0684453605168362));
#98116=CARTESIAN_POINT('Ctrl Pts',(0.0085361347600194,-0.0340223579322365,
0.0683323429422979));
#98117=CARTESIAN_POINT('Ctrl Pts',(0.00861637542393109,-0.0339125849573552,
0.0683380303596563));
#98118=CARTESIAN_POINT('Ctrl Pts',(0.0086964419873337,-0.0338030433565217,
0.0683453745758217));
#98119=CARTESIAN_POINT('Ctrl Pts',(0.00877623289115136,-0.0336938721132321,
0.0683543571221916));
#98120=CARTESIAN_POINT('Ctrl Pts',(0.00846490665531203,-0.0340223579322365,
0.0682442081765689));
#98121=CARTESIAN_POINT('Ctrl Pts',(0.00854636292750823,-0.0339125849573552,
0.0682489131725927));
#98122=CARTESIAN_POINT('Ctrl Pts',(0.00862766457884028,-0.0338030433565217,
0.0682553008180264));
#98123=CARTESIAN_POINT('Ctrl Pts',(0.00870870836232328,-0.0336938721132321,
0.0682633537275469));
#98124=CARTESIAN_POINT('Ctrl Pts',(0.00839367855060466,-0.0340223579322365,
0.0681560734108399));
#98125=CARTESIAN_POINT('Ctrl Pts',(0.00847635043108537,-0.0339125849573552,
0.0681597959855291));
#98126=CARTESIAN_POINT('Ctrl Pts',(0.00855888717034687,-0.0338030433565217,
0.0681652270602311));
#98127=CARTESIAN_POINT('Ctrl Pts',(0.00864118383349521,-0.0336938721132321,
0.0681723503329022));
#98128=CARTESIAN_POINT('Origin',(0.00794960615951678,-0.0345589643415262,
0.0850799051032651));
#98129=CARTESIAN_POINT('Ctrl Pts',(0.0089901469553743,-0.034193496108874,
0.0682128784669059));
#98130=CARTESIAN_POINT('Ctrl Pts',(0.00907201634549192,-0.0340836138581107,
0.0682248251239368));
#98131=CARTESIAN_POINT('Ctrl Pts',(0.00915359924213727,-0.03397388966435,
0.0682384601639801));
#98132=CARTESIAN_POINT('Ctrl Pts',(0.00923479239911469,-0.0338644633294063,
0.0682537591363501));
#98133=CARTESIAN_POINT('Ctrl Pts',(0.00890356310478089,-0.034193496108874,
0.0682859838433384));
#98134=CARTESIAN_POINT('Ctrl Pts',(0.00898442441504878,-0.0340836138581107,
0.0682967365603425));
#98135=CARTESIAN_POINT('Ctrl Pts',(0.00906502442162371,-0.03397388966435,
0.0683091573731367));
#98136=CARTESIAN_POINT('Ctrl Pts',(0.00914526103211158,-0.0338644633294063,
0.0683232234694246));
#98137=CARTESIAN_POINT('Ctrl Pts',(0.00881697925418748,-0.034193496108874,
0.0683590892197709));
#98138=CARTESIAN_POINT('Ctrl Pts',(0.00889683248460565,-0.0340836138581107,
0.0683686479967483));
#98139=CARTESIAN_POINT('Ctrl Pts',(0.00897644960111015,-0.03397388966435,
0.0683798545822933));
#98140=CARTESIAN_POINT('Ctrl Pts',(0.00905572966510848,-0.0338644633294063,
0.068392687802499));
#98141=CARTESIAN_POINT('Ctrl Pts',(0.00873039540359407,-0.034193496108874,
0.0684321945962035));
#98142=CARTESIAN_POINT('Ctrl Pts',(0.00880924055416252,-0.0340836138581107,
0.068440559433154));
#98143=CARTESIAN_POINT('Ctrl Pts',(0.00888787478059659,-0.03397388966435,
0.0684505517914499));
#98144=CARTESIAN_POINT('Ctrl Pts',(0.00896619829810537,-0.0338644633294063,
0.0684621521355734));
#98145=CARTESIAN_POINT('Origin',(0.00746992174341197,-0.034561062186391,
0.0851180216646338));
#98146=CARTESIAN_POINT('Ctrl Pts',(0.0086959585135099,-0.0342436276873901,
0.0684271738399308));
#98147=CARTESIAN_POINT('Ctrl Pts',(0.00891179846029925,-0.0339430054201861,
0.0684487538256049));
#98148=CARTESIAN_POINT('Ctrl Pts',(0.00912539973548516,-0.0336441434784162,
0.0684865304539705));
#98149=CARTESIAN_POINT('Ctrl Pts',(0.00844671696444653,-0.0342436276873901,
0.0684077149031538));
#98150=CARTESIAN_POINT('Ctrl Pts',(0.008663290817135,-0.0339430054201861,
0.0684198945888393));
#98151=CARTESIAN_POINT('Ctrl Pts',(0.00887833198238197,-0.0336441434784162,
0.0684483529032824));
#98152=CARTESIAN_POINT('Ctrl Pts',(0.00896617084773448,-0.0335235895815127,
0.068462148197955));
#98153=CARTESIAN_POINT('Ctrl Pts',(0.00904447532613822,-0.0334144449262719,
0.0684737453362964));
#98154=CARTESIAN_POINT('Ctrl Pts',(0.00912263017875049,-0.0333049234473133,
0.0684869735099379));
#98155=CARTESIAN_POINT('Ctrl Pts',(0.00920053393729631,-0.0331951640388588,
0.0685018248567473));
#98156=CARTESIAN_POINT('Ctrl Pts',(0.00890061738404836,-0.0335235895815127,
0.0683697148928912));
#98157=CARTESIAN_POINT('Ctrl Pts',(0.00898019438888071,-0.0334144449262719,
0.0683804095587421));
#98158=CARTESIAN_POINT('Ctrl Pts',(0.00905964187430276,-0.0333049234473133,
0.0683927605124998));
#98159=CARTESIAN_POINT('Ctrl Pts',(0.009138856820767,-0.0331951640388588,
0.0684067611634522));
#98160=CARTESIAN_POINT('Ctrl Pts',(0.00883506392036223,-0.0335235895815127,
0.0682772815878273));
#98161=CARTESIAN_POINT('Ctrl Pts',(0.00891591345162321,-0.0334144449262719,
0.0682870737811877));
#98162=CARTESIAN_POINT('Ctrl Pts',(0.00899665356985503,-0.0333049234473133,
0.0682985475150617));
#98163=CARTESIAN_POINT('Ctrl Pts',(0.00907717970423769,-0.0331951640388588,
0.0683116974701572));
#98164=CARTESIAN_POINT('Ctrl Pts',(0.00876951045667611,-0.0335235895815127,
0.0681848482827635));
#98165=CARTESIAN_POINT('Ctrl Pts',(0.0088516325143657,-0.0334144449262719,
0.0681937380036333));
#98166=CARTESIAN_POINT('Ctrl Pts',(0.0089336652654073,-0.0333049234473133,
0.0682043345176235));
#98167=CARTESIAN_POINT('Ctrl Pts',(0.00901550258770838,-0.0331951640388588,
0.0682166337768621));
#98168=CARTESIAN_POINT('Origin',(0.00533496082260069,-0.0326434571769664,
0.0847144182816732));
#98169=CARTESIAN_POINT('Ctrl Pts',(0.00936286061526512,-0.0336938721132348,
0.068277785324231));
#98170=CARTESIAN_POINT('Ctrl Pts',(0.00939723263636825,-0.0336474569764937,
0.0682850380614053));
#98171=CARTESIAN_POINT('Ctrl Pts',(0.00943151739983263,-0.033601104548885,
0.0682926926695225));
#98172=CARTESIAN_POINT('Ctrl Pts',(0.00951831853082757,-0.0334837508694588,
0.068312072375688));
#98173=CARTESIAN_POINT('Ctrl Pts',(0.00960450728434494,-0.0333660264863561,
0.0683340156689728));
#98174=CARTESIAN_POINT('Ctrl Pts',(0.00908985111544777,-0.0336938721132348,
0.0684803584031007));
#98175=CARTESIAN_POINT('Ctrl Pts',(0.00912303740909947,-0.0336474569764937,
0.0684860131250785));
#98176=CARTESIAN_POINT('Ctrl Pts',(0.00915615523314472,-0.033601104548885,
0.0684920559470593));
#98177=CARTESIAN_POINT('Ctrl Pts',(0.00924000194208312,-0.0334837508694588,
0.0685073549816545));
#98178=CARTESIAN_POINT('Ctrl Pts',(0.00932335848965693,-0.0333660264863561,
0.0685251318496555));
#98179=CARTESIAN_POINT('Ctrl Pts',(0.00908985111545924,-0.0336938721132427,
0.068480358403111));
#98180=CARTESIAN_POINT('Ctrl Pts',(0.0091230374091102,-0.0336474569765026,
0.0684860131250887));
#98181=CARTESIAN_POINT('Ctrl Pts',(0.00915615523315472,-0.0336011045488949,
0.0684920559470693));
#98182=CARTESIAN_POINT('Ctrl Pts',(0.00923930361320096,-0.033484728265791,
0.0685072275615425));
#98183=CARTESIAN_POINT('Ctrl Pts',(0.00932197026244842,-0.0333679870047996,
0.0685248359712446));
#98184=CARTESIAN_POINT('Ctrl Pts',(0.0090898511154422,-0.0336938721132426,
0.0684803584030998));
#98185=CARTESIAN_POINT('Ctrl Pts',(0.00920853998794152,-0.0335278710435082,
0.0685005821913567));
#98186=CARTESIAN_POINT('Ctrl Pts',(0.00932655289322954,-0.033362046922432,
0.0685245209171148));
#98187=CARTESIAN_POINT('Ctrl Pts',(0.00944394454052174,-0.0331951640388602,
0.0685522061152207));
#98188=CARTESIAN_POINT('Ctrl Pts',(0.00900692236778153,-0.0336938721132426,
0.0684680761950446));
#98189=CARTESIAN_POINT('Ctrl Pts',(0.00912586835731391,-0.0335278710435082,
0.0684865639441905));
#98190=CARTESIAN_POINT('Ctrl Pts',(0.00924419273091696,-0.033362046922432,
0.0685087753046955));
#98191=CARTESIAN_POINT('Ctrl Pts',(0.00936195064002609,-0.0331951640388602,
0.0685347410041479));
#98192=CARTESIAN_POINT('Ctrl Pts',(0.00892399362012087,-0.0336938721132426,
0.0684557939869894));
#98193=CARTESIAN_POINT('Ctrl Pts',(0.0090431967266863,-0.0335278710435082,
0.0684725456970244));
#98194=CARTESIAN_POINT('Ctrl Pts',(0.00916183256860439,-0.033362046922432,
0.0684930296922761));
#98195=CARTESIAN_POINT('Ctrl Pts',(0.00927995673953043,-0.0331951640388602,
0.0685172758930751));
#98196=CARTESIAN_POINT('Ctrl Pts',(0.00884106487246021,-0.0336938721132426,
0.0684435117789343));
#98197=CARTESIAN_POINT('Ctrl Pts',(0.0089605250960587,-0.0335278710435082,
0.0684585274498582));
#98198=CARTESIAN_POINT('Ctrl Pts',(0.00907947240629182,-0.033362046922432,
0.0684772840798568));
#98199=CARTESIAN_POINT('Ctrl Pts',(0.00919796283903478,-0.0331951640388602,
0.0684998107820023));
#98200=CARTESIAN_POINT('Ctrl Pts',(0.00932165060079693,-0.0330240426238155,
0.068526265292725));
#98201=CARTESIAN_POINT('Ctrl Pts',(0.00939912302532848,-0.0329142774063509,
0.0685427670970675));
#98202=CARTESIAN_POINT('Ctrl Pts',(0.00947629293429782,-0.0328043479726686,
0.0685608786995848));
#98203=CARTESIAN_POINT('Ctrl Pts',(0.00955306082831667,-0.0326943950436594,
0.0685805796205633));
#98204=CARTESIAN_POINT('Ctrl Pts',(0.0092620304964448,-0.0330240426238155,
0.0684298983941466));
#98205=CARTESIAN_POINT('Ctrl Pts',(0.00934083046888998,-0.0329142774063509,
0.0684455788734666));
#98206=CARTESIAN_POINT('Ctrl Pts',(0.00941934556668648,-0.0328043479726686,
0.0684628961856246));
#98207=CARTESIAN_POINT('Ctrl Pts',(0.00949747459518195,-0.0326943950436594,
0.0684818309159112));
#98208=CARTESIAN_POINT('Ctrl Pts',(0.00920241039209268,-0.0330240426238155,
0.0683335314955683));
#98209=CARTESIAN_POINT('Ctrl Pts',(0.00928253791245148,-0.0329142774063509,
0.0683483906498657));
#98210=CARTESIAN_POINT('Ctrl Pts',(0.00936239819907514,-0.0328043479726686,
0.0683649136716645));
#98211=CARTESIAN_POINT('Ctrl Pts',(0.00944188836204723,-0.0326943950436594,
0.0683830822112591));
#98212=CARTESIAN_POINT('Ctrl Pts',(0.00914279028774055,-0.0330240426238155,
0.0682371645969899));
#98213=CARTESIAN_POINT('Ctrl Pts',(0.00922424535601299,-0.0329142774063509,
0.0682512024262648));
#98214=CARTESIAN_POINT('Ctrl Pts',(0.0093054508314638,-0.0328043479726686,
0.0682669311577043));
#98215=CARTESIAN_POINT('Ctrl Pts',(0.00938630212891251,-0.0326943950436594,
0.068284333506607));
#98216=CARTESIAN_POINT('Origin',(0.00530607407682471,-0.0326396682858201,
0.0848346719908854));
#98217=CARTESIAN_POINT('Ctrl Pts',(0.00972743405026172,-0.0331951640388587,
0.0683682787406266));
#98218=CARTESIAN_POINT('Ctrl Pts',(0.00980706556428271,-0.0330855618255041,
0.0683903658007976));
#98219=CARTESIAN_POINT('Ctrl Pts',(0.00988629798176981,-0.0329757224427708,
0.0684141146304979));
#98220=CARTESIAN_POINT('Ctrl Pts',(0.00996502834909326,-0.0328657862078596,
0.0684394997948417));
#98221=CARTESIAN_POINT('Ctrl Pts',(0.00963237043264987,-0.0331951640388587,
0.0684299558080528));
#98222=CARTESIAN_POINT('Ctrl Pts',(0.00971115246983876,-0.0330855618255041,
0.0684507335592033));
#98223=CARTESIAN_POINT('Ctrl Pts',(0.00978956185929717,-0.0329757224427708,
0.0684731545787865));
#98224=CARTESIAN_POINT('Ctrl Pts',(0.00986749678473739,-0.0328657862078596,
0.0684971950805594));
#98225=CARTESIAN_POINT('Ctrl Pts',(0.00953730681503803,-0.0331951640388587,
0.0684916328754789));
#98226=CARTESIAN_POINT('Ctrl Pts',(0.00961523937539481,-0.0330855618255041,
0.068511101317609));
#98227=CARTESIAN_POINT('Ctrl Pts',(0.00969282573682452,-0.0329757224427708,
0.0685321945270751));
#98228=CARTESIAN_POINT('Ctrl Pts',(0.00976996522038151,-0.0328657862078596,
0.068554890366277));
#98229=CARTESIAN_POINT('Ctrl Pts',(0.00944224319742619,-0.0331951640388587,
0.0685533099429051));
#98230=CARTESIAN_POINT('Ctrl Pts',(0.00951932628095086,-0.0330855618255041,
0.0685714690760147));
#98231=CARTESIAN_POINT('Ctrl Pts',(0.00959608961435188,-0.0329757224427708,
0.0685912344753637));
#98232=CARTESIAN_POINT('Ctrl Pts',(0.00967243365602564,-0.0328657862078596,
0.0686125856519946));
#98233=CARTESIAN_POINT('Origin',(0.00485239013941621,-0.0326401908836119,
0.0846751609994067));
#98234=CARTESIAN_POINT('Ctrl Pts',(0.00940877767744207,-0.0332451089994432,
0.0685440289328928));
#98235=CARTESIAN_POINT('Ctrl Pts',(0.00962021033545713,-0.0329451141710258,
0.0685924933305034));
#98236=CARTESIAN_POINT('Ctrl Pts',(0.00982739179905341,-0.0326442513127503,
0.0686567460180206));
#98237=CARTESIAN_POINT('Ctrl Pts',(0.00916394096079468,-0.0332451089994432,
0.0684934821013271));
#98238=CARTESIAN_POINT('Ctrl Pts',(0.00937728002375266,-0.0329451141710258,
0.0685327123310906));
#98239=CARTESIAN_POINT('Ctrl Pts',(0.00958705803166844,-0.0326442513127503,
0.0685879006822705));
#98240=CARTESIAN_POINT('Ctrl Pts',(0.00967240325991672,-0.0325229783203384,
0.0686125770579851));
#98241=CARTESIAN_POINT('Ctrl Pts',(0.00974873651268751,-0.0324130253112079,
0.0686339247651364));
#98242=CARTESIAN_POINT('Ctrl Pts',(0.00982461658328766,-0.0323031222247694,
0.0686568482858514));
#98243=CARTESIAN_POINT('Ctrl Pts',(0.00989994731088243,-0.0321934096636184,
0.06868131482697));
#98244=CARTESIAN_POINT('Ctrl Pts',(0.00961895169997607,-0.0325229783203384,
0.0685126567227713));
#98245=CARTESIAN_POINT('Ctrl Pts',(0.0096966623523576,-0.0324130253112079,
0.0685332676013511));
#98246=CARTESIAN_POINT('Ctrl Pts',(0.00977393485590409,-0.0323031222247694,
0.068555482898529));
#98247=CARTESIAN_POINT('Ctrl Pts',(0.00985067123416174,-0.0321934096636184,
0.068579270665391));
#98248=CARTESIAN_POINT('Ctrl Pts',(0.00956550014003542,-0.0325229783203384,
0.0684127363875574));
#98249=CARTESIAN_POINT('Ctrl Pts',(0.00964458819202769,-0.0324130253112079,
0.0684326104375657));
#98250=CARTESIAN_POINT('Ctrl Pts',(0.00972325312852053,-0.0323031222247694,
0.0684541175112065));
#98251=CARTESIAN_POINT('Ctrl Pts',(0.00980139515744106,-0.0321934096636184,
0.068477226503812));
#98252=CARTESIAN_POINT('Ctrl Pts',(0.00951204858009477,-0.0325229783203384,
0.0683128160523436));
#98253=CARTESIAN_POINT('Ctrl Pts',(0.00959251403169778,-0.0324130253112079,
0.0683319532737804));
#98254=CARTESIAN_POINT('Ctrl Pts',(0.00967257140113696,-0.0323031222247694,
0.068352752123884));
#98255=CARTESIAN_POINT('Ctrl Pts',(0.00975211908072037,-0.0321934096636184,
0.068375182342233));
#98256=CARTESIAN_POINT('Origin',(0.00530847784489562,-0.0326393375179126,
0.0848264919594345));
#98257=CARTESIAN_POINT('Ctrl Pts',(0.0100873068912915,-0.0326943950436593,
0.0684803817800777));
#98258=CARTESIAN_POINT('Ctrl Pts',(0.0101654448563588,-0.0325844576448127,
0.0685074428304561));
#98259=CARTESIAN_POINT('Ctrl Pts',(0.0102430286844823,-0.0324744968375319,
0.0685361218172136));
#98260=CARTESIAN_POINT('Ctrl Pts',(0.0103199594775635,-0.0323646534831894,
0.0685663806240671));
#98261=CARTESIAN_POINT('Ctrl Pts',(0.00998855821894807,-0.0326943950436593,
0.0685359679950257));
#98262=CARTESIAN_POINT('Ctrl Pts',(0.0100659301017937,-0.0325844576448127,
0.0685616681036245));
#98263=CARTESIAN_POINT('Ctrl Pts',(0.0101427759399861,-0.0324744968375319,
0.06858897020845));
#98264=CARTESIAN_POINT('Ctrl Pts',(0.0102189977566495,-0.0323646534831894,
0.0686178379704027));
#98265=CARTESIAN_POINT('Ctrl Pts',(0.00988980954660469,-0.0326943950436593,
0.0685915542099737));
#98266=CARTESIAN_POINT('Ctrl Pts',(0.00996641534722872,-0.0325844576448127,
0.0686158933767928));
#98267=CARTESIAN_POINT('Ctrl Pts',(0.0100425231954899,-0.0324744968375319,
0.0686418185996864));
#98268=CARTESIAN_POINT('Ctrl Pts',(0.0101180360357355,-0.0323646534831894,
0.0686692953167383));
#98269=CARTESIAN_POINT('Ctrl Pts',(0.00979106087426132,-0.0326943950436593,
0.0686471404249216));
#98270=CARTESIAN_POINT('Ctrl Pts',(0.0098669005926637,-0.0325844576448127,
0.0686701186499611));
#98271=CARTESIAN_POINT('Ctrl Pts',(0.00994227045099364,-0.0324744968375319,
0.0686946669909228));
#98272=CARTESIAN_POINT('Ctrl Pts',(0.0100170743148215,-0.0323646534831894,
0.068720752663074));
#98273=CARTESIAN_POINT('Origin',(0.00484159657221721,-0.0326395579068595,
0.0847114302808474));
#98274=CARTESIAN_POINT('Ctrl Pts',(0.00975820626200597,-0.0327445246961877,
0.0686357654236504));
#98275=CARTESIAN_POINT('Ctrl Pts',(0.00996617901678053,-0.0324436878365475,
0.0686974087344984));
#98276=CARTESIAN_POINT('Ctrl Pts',(0.0101689177168719,-0.0321434074463188,
0.0687745422809362));
#98277=CARTESIAN_POINT('Ctrl Pts',(0.00951702608762621,-0.0327445246961877,
0.0685699465548805));
#98278=CARTESIAN_POINT('Ctrl Pts',(0.00972748124159231,-0.0324436878365475,
0.0686224936068429));
#98279=CARTESIAN_POINT('Ctrl Pts',(0.00993338045603041,-0.0321434074463188,
0.0686907437203563));
#98280=CARTESIAN_POINT('Ctrl Pts',(0.0101064737717701,-0.0322357242816073,
0.0687511983640899));
#98281=CARTESIAN_POINT('Ctrl Pts',(0.0102784186018846,-0.0319819883628706,
0.0688143445194136));
#98282=CARTESIAN_POINT('Ctrl Pts',(0.0104459967939566,-0.0317295851069886,
0.0688883040426486));
#98283=CARTESIAN_POINT('Ctrl Pts',(0.00986998103031469,-0.0322357242816073,
0.0686701355289624));
#98284=CARTESIAN_POINT('Ctrl Pts',(0.0100445076065934,-0.0319819883628706,
0.0687257496971906));
#98285=CARTESIAN_POINT('Ctrl Pts',(0.0102151415944866,-0.0317295851069886,
0.0687923567817306));
#98286=CARTESIAN_POINT('Origin',(0.00487150216666944,-0.0326371942646915,
0.0846209423866145));
#98287=CARTESIAN_POINT('Origin',(0.00534258097687683,-0.0326352985530559,
0.0847085903938754));
#98288=CARTESIAN_POINT('Ctrl Pts',(0.0104394305973869,-0.0321934096636184,
0.0686148602124408));
#98289=CARTESIAN_POINT('Ctrl Pts',(0.0105157644888829,-0.0320835708272304,
0.0686467948086424));
#98290=CARTESIAN_POINT('Ctrl Pts',(0.010591393218811,-0.0319739230346346,
0.0686802906073974));
#98291=CARTESIAN_POINT('Ctrl Pts',(0.0106662233145021,-0.0318646057455575,
0.068715297326964));
#98292=CARTESIAN_POINT('Ctrl Pts',(0.0103373863479351,-0.0321934096636184,
0.0686641363315943));
#98293=CARTESIAN_POINT('Ctrl Pts',(0.0104130406833445,-0.0320835708272304,
0.0686946636580675));
#98294=CARTESIAN_POINT('Ctrl Pts',(0.01048801937473,-0.0319739230346346,
0.0687267389399899));
#98295=CARTESIAN_POINT('Ctrl Pts',(0.0105622296416174,-0.0318646057455575,
0.0687603137769014));
#98296=CARTESIAN_POINT('Ctrl Pts',(0.0102353420984833,-0.0321934096636184,
0.0687134124507479));
#98297=CARTESIAN_POINT('Ctrl Pts',(0.0103103168778061,-0.0320835708272304,
0.0687425325074927));
#98298=CARTESIAN_POINT('Ctrl Pts',(0.0103846455306491,-0.0319739230346346,
0.0687731872725824));
#98299=CARTESIAN_POINT('Ctrl Pts',(0.0104582359687327,-0.0318646057455575,
0.0688053302268388));
#98300=CARTESIAN_POINT('Ctrl Pts',(0.0101332978490316,-0.0321934096636184,
0.0687626885699015));
#98301=CARTESIAN_POINT('Ctrl Pts',(0.0102075930722677,-0.0320835708272304,
0.0687904013569179));
#98302=CARTESIAN_POINT('Ctrl Pts',(0.0102812716865681,-0.0319739230346346,
0.0688196356051749));
#98303=CARTESIAN_POINT('Ctrl Pts',(0.0103542422958481,-0.0318646057455575,
0.0688503466767762));
#98304=CARTESIAN_POINT('Ctrl Pts',(0.0100169032038936,-0.0320218834582322,
0.0687198167030099));
#98305=CARTESIAN_POINT('Ctrl Pts',(0.01007341828463,-0.0319391099350637,
0.068739519516141));
#98306=CARTESIAN_POINT('Ctrl Pts',(0.0101295914621253,-0.0318564869454936,
0.0687600928827483));
#98307=CARTESIAN_POINT('Ctrl Pts',(0.0101853832206213,-0.0317740741446547,
0.0687815179981912));
#98308=CARTESIAN_POINT('Ctrl Pts',(0.00999631634916544,-0.0320218834582322,
0.0686747277968386));
#98309=CARTESIAN_POINT('Ctrl Pts',(0.0100533006964134,-0.0319391099350637,
0.0686942163505805));
#98310=CARTESIAN_POINT('Ctrl Pts',(0.0101099462017939,-0.0318564869454936,
0.0687145829152751));
#98311=CARTESIAN_POINT('Ctrl Pts',(0.0101662129914586,-0.0317740741446547,
0.0687358088047925));
#98312=CARTESIAN_POINT('Ctrl Pts',(0.0099757294944373,-0.0320218834582322,
0.0686296388906674));
#98313=CARTESIAN_POINT('Ctrl Pts',(0.0100331831081968,-0.0319391099350637,
0.0686489131850199));
#98314=CARTESIAN_POINT('Ctrl Pts',(0.0100903009414625,-0.0318564869454936,
0.0686690729478019));
#98315=CARTESIAN_POINT('Ctrl Pts',(0.0101470427622958,-0.0317740741446547,
0.0686900996113937));
#98316=CARTESIAN_POINT('Ctrl Pts',(0.00995514263970917,-0.0320218834582322,
0.0685845499844961));
#98317=CARTESIAN_POINT('Ctrl Pts',(0.0100130655199801,-0.0319391099350637,
0.0686036100194593));
#98318=CARTESIAN_POINT('Ctrl Pts',(0.0100706556811311,-0.0318564869454936,
0.0686235629803287));
#98319=CARTESIAN_POINT('Ctrl Pts',(0.0101278725331331,-0.0317740741446547,
0.068644390417995));
#98320=CARTESIAN_POINT('Origin',(0.0111983912622235,-0.0391228853390594,
0.0624697860721113));
#98321=CARTESIAN_POINT('Ctrl Pts',(0.0069886543965657,-0.0352722978779554,
0.0685112368884557));
#98322=CARTESIAN_POINT('Ctrl Pts',(0.0070072455713299,-0.035246664209719,
0.0685078514935177));
#98323=CARTESIAN_POINT('Ctrl Pts',(0.00702580613789197,-0.0352210183808288,
0.0685043919819847));
#98324=CARTESIAN_POINT('Ctrl Pts',(0.00704433665365789,-0.0351953608940152,
0.0685008577082699));
#98325=CARTESIAN_POINT('Origin',(0.00628964179675846,-0.0352456003065018,
0.0636613786864799));
#98326=CARTESIAN_POINT('Ctrl Pts',(0.0071672974496976,-0.0350241211493339,
0.0684802189569634));
#98327=CARTESIAN_POINT('Ctrl Pts',(0.00724539635534315,-0.0349144232867421,
0.068467043772391));
#98328=CARTESIAN_POINT('Ctrl Pts',(0.00732381434741339,-0.0348045283677512,
0.0684554750619493));
#98329=CARTESIAN_POINT('Ctrl Pts',(0.00740245153384783,-0.0346945769586886,
0.0684455313814199));
#98330=CARTESIAN_POINT('Ctrl Pts',(0.00707638903822302,-0.0350241211493339,
0.0684125668873264));
#98331=CARTESIAN_POINT('Ctrl Pts',(0.00715541982334738,-0.0349144232867421,
0.0683981394767163));
#98332=CARTESIAN_POINT('Ctrl Pts',(0.007234796137077,-0.0348045283677512,
0.0683853370533331));
#98333=CARTESIAN_POINT('Ctrl Pts',(0.00731441691866725,-0.0346945769586886,
0.0683741797988656));
#98334=CARTESIAN_POINT('Ctrl Pts',(0.00698548062674844,-0.0350241211493339,
0.0683449148176895));
#98335=CARTESIAN_POINT('Ctrl Pts',(0.0070654432913516,-0.0349144232867421,
0.0683292351810417));
#98336=CARTESIAN_POINT('Ctrl Pts',(0.00714577792674061,-0.0348045283677512,
0.068315199044717));
#98337=CARTESIAN_POINT('Ctrl Pts',(0.00722638230348667,-0.0346945769586886,
0.0683028282163112));
#98338=CARTESIAN_POINT('Ctrl Pts',(0.00689457221527386,-0.0350241211493339,
0.0682772627480525));
#98339=CARTESIAN_POINT('Ctrl Pts',(0.00697546675935583,-0.0349144232867421,
0.068260330885367));
#98340=CARTESIAN_POINT('Ctrl Pts',(0.00705675971640422,-0.0348045283677512,
0.0682450610361009));
#98341=CARTESIAN_POINT('Ctrl Pts',(0.0071383476883061,-0.0346945769586886,
0.0682314766337569));
#98342=CARTESIAN_POINT('Origin',(0.00932984543910564,-0.0345629067942411,
0.0851233040683128));
#98343=CARTESIAN_POINT('Ctrl Pts',(0.00743122803229611,-0.0351970973651569,
0.0682596782336155));
#98344=CARTESIAN_POINT('Ctrl Pts',(0.0075128304571892,-0.035086934932687,
0.0682500838343393));
#98345=CARTESIAN_POINT('Ctrl Pts',(0.00759469994282422,-0.034976498513999,
0.0682421779563585));
#98346=CARTESIAN_POINT('Ctrl Pts',(0.00767673102780055,-0.0348659306865085,
0.0682359770855367));
#98347=CARTESIAN_POINT('Ctrl Pts',(0.00738358609753361,-0.0351970973651569,
0.0683266910436016));
#98348=CARTESIAN_POINT('Ctrl Pts',(0.00746426015076711,-0.035086934932687,
0.0683164366298886));
#98349=CARTESIAN_POINT('Ctrl Pts',(0.00754521421702457,-0.034976498513999,
0.0683078508903905));
#98350=CARTESIAN_POINT('Ctrl Pts',(0.00762634407270598,-0.0348659306865085,
0.0683009511219393));
#98351=CARTESIAN_POINT('Ctrl Pts',(0.00733594416277111,-0.0351970973651569,
0.0683937038535878));
#98352=CARTESIAN_POINT('Ctrl Pts',(0.00741568984434501,-0.035086934932687,
0.068382789425438));
#98353=CARTESIAN_POINT('Ctrl Pts',(0.00749572849122493,-0.034976498513999,
0.0683735238244226));
#98354=CARTESIAN_POINT('Ctrl Pts',(0.00757595711761141,-0.0348659306865085,
0.0683659251583419));
#98355=CARTESIAN_POINT('Ctrl Pts',(0.0072883022280086,-0.0351970973651569,
0.068460716663574));
#98356=CARTESIAN_POINT('Ctrl Pts',(0.00736711953792292,-0.0350869349326871,
0.0684491422209874));
#98357=CARTESIAN_POINT('Ctrl Pts',(0.00744624276542529,-0.0349764985139991,
0.0684391967584546));
#98358=CARTESIAN_POINT('Ctrl Pts',(0.00752557016251684,-0.0348659306865085,
0.0684308991947446));
#98359=CARTESIAN_POINT('Origin',(0.0088489351065516,-0.0345637187965151,
0.085130418031708));
#98360=CARTESIAN_POINT('Ctrl Pts',(0.00725485115071148,-0.0352450361861253,
0.068464660621954));
#98361=CARTESIAN_POINT('Ctrl Pts',(0.00746927723840594,-0.0349452761023765,
0.0684318883507653));
#98362=CARTESIAN_POINT('Ctrl Pts',(0.00768556270568411,-0.0346444289983475,
0.068415360632015));
#98363=CARTESIAN_POINT('Ctrl Pts',(0.00700860015368956,-0.0352450361861253,
0.0685077935150371));
#98364=CARTESIAN_POINT('Ctrl Pts',(0.00722139945766898,-0.0349452761023765,
0.0684657337353337));
#98365=CARTESIAN_POINT('Ctrl Pts',(0.0074367623358779,-0.0346444289983475,
0.0684398223568989));
#98366=CARTESIAN_POINT('Ctrl Pts',(0.00752519237820144,-0.0345231616327822,
0.0684313488481526));
#98367=CARTESIAN_POINT('Ctrl Pts',(0.00760401593311234,-0.0344132092796975,
0.0684230981303012));
#98368=CARTESIAN_POINT('Ctrl Pts',(0.00768300608068082,-0.0343032738558973,
0.0684164782412072));
#98369=CARTESIAN_POINT('Ctrl Pts',(0.00776206140815902,-0.034193496108874,
0.0684114950695524));
#98370=CARTESIAN_POINT('Ctrl Pts',(0.00743871126965919,-0.0345231616327822,
0.0683581221180348));
#98371=CARTESIAN_POINT('Ctrl Pts',(0.00751854415194977,-0.0344132092796975,
0.0683486793798578));
#98372=CARTESIAN_POINT('Ctrl Pts',(0.00759856823082146,-0.0343032738558973,
0.0683408884090816));
#98373=CARTESIAN_POINT('Ctrl Pts',(0.00767868073051039,-0.034193496108874,
0.0683347565607495));
#98374=CARTESIAN_POINT('Ctrl Pts',(0.00735223016111695,-0.0345231616327822,
0.068284895387917));
#98375=CARTESIAN_POINT('Ctrl Pts',(0.0074330723707872,-0.0344132092796975,
0.0682742606294144));
#98376=CARTESIAN_POINT('Ctrl Pts',(0.0075141303809621,-0.0343032738558973,
0.0682652985769561));
#98377=CARTESIAN_POINT('Ctrl Pts',(0.00759530005286176,-0.034193496108874,
0.0682580180519466));
#98378=CARTESIAN_POINT('Ctrl Pts',(0.00726574905257471,-0.0345231616327822,
0.0682116686577992));
#98379=CARTESIAN_POINT('Ctrl Pts',(0.00734760058962464,-0.0344132092796975,
0.068199841878971));
#98380=CARTESIAN_POINT('Ctrl Pts',(0.00742969253110274,-0.0343032738558973,
0.0681897087448306));
#98381=CARTESIAN_POINT('Ctrl Pts',(0.00751191937521313,-0.034193496108874,
0.0681812795431436));
#98382=CARTESIAN_POINT('Origin',(0.0093314165033207,-0.0345625596231041,
0.0851353053208476));
#98383=CARTESIAN_POINT('Ctrl Pts',(0.00786229561583597,-0.0346945769586885,
0.0681557006439514));
#98384=CARTESIAN_POINT('Ctrl Pts',(0.00794490009058703,-0.0345846629178475,
0.0681520972267567));
#98385=CARTESIAN_POINT('Ctrl Pts',(0.00802759319157298,-0.034474692505516,
0.0681502014206997));
#98386=CARTESIAN_POINT('Ctrl Pts',(0.00811026895283217,-0.0343648066260528,
0.068150015217323));
#98387=CARTESIAN_POINT('Ctrl Pts',(0.00779094408946165,-0.0346945769586885,
0.0682437351898163));
#98388=CARTESIAN_POINT('Ctrl Pts',(0.00787233540367648,-0.0345846629178475,
0.0682391485125258));
#98389=CARTESIAN_POINT('Ctrl Pts',(0.00795383547033033,-0.034474692505516,
0.0682362441907683));
#98390=CARTESIAN_POINT('Ctrl Pts',(0.0080353398467779,-0.0343648066260528,
0.0682350255146257));
#98391=CARTESIAN_POINT('Ctrl Pts',(0.00771959256308734,-0.0346945769586885,
0.0683317697356813));
#98392=CARTESIAN_POINT('Ctrl Pts',(0.00779977071676592,-0.0345846629178475,
0.068326199798295));
#98393=CARTESIAN_POINT('Ctrl Pts',(0.00788007774908768,-0.034474692505516,
0.0683222869608369));
#98394=CARTESIAN_POINT('Ctrl Pts',(0.00796041074072362,-0.0343648066260528,
0.0683200358119284));
#98395=CARTESIAN_POINT('Ctrl Pts',(0.00764824103671302,-0.0346945769586885,
0.0684198042815462));
#98396=CARTESIAN_POINT('Ctrl Pts',(0.00772720602985537,-0.0345846629178475,
0.0684132510840642));
#98397=CARTESIAN_POINT('Ctrl Pts',(0.00780632002784502,-0.034474692505516,
0.0684083297309054));
#98398=CARTESIAN_POINT('Ctrl Pts',(0.00788548163466935,-0.0343648066260528,
0.0684050461092312));
#98399=CARTESIAN_POINT('Origin',(0.00885356201123892,-0.0345626446730313,
0.085188665111889));
#98400=CARTESIAN_POINT('Ctrl Pts',(0.00764951775477944,-0.0346945769586885,
0.0684182290483187));
#98401=CARTESIAN_POINT('Ctrl Pts',(0.00776957199223636,-0.034527515336289,
0.0684082953897729));
#98402=CARTESIAN_POINT('Ctrl Pts',(0.00788996968628629,-0.0343603235965159,
0.0684021347571399));
#98403=CARTESIAN_POINT('Ctrl Pts',(0.00801035448319214,-0.034193496108874,
0.0683997600785163));
#98404=CARTESIAN_POINT('Ctrl Pts',(0.00756613991413675,-0.0346945769586885,
0.068426956248387));
#98405=CARTESIAN_POINT('Ctrl Pts',(0.00768601135689406,-0.034527515336289,
0.0684152762075863));
#98406=CARTESIAN_POINT('Ctrl Pts',(0.00780628113107879,-0.0343603235965159,
0.0684073629922694));
#98407=CARTESIAN_POINT('Ctrl Pts',(0.00792659318424578,-0.034193496108874,
0.0684032347195176));
#98408=CARTESIAN_POINT('Ctrl Pts',(0.00748276207349405,-0.0346945769586885,
0.0684356834484552));
#98409=CARTESIAN_POINT('Ctrl Pts',(0.00760245072155176,-0.034527515336289,
0.0684222570253997));
#98410=CARTESIAN_POINT('Ctrl Pts',(0.0077225925758713,-0.0343603235965159,
0.068412591227399));
#98411=CARTESIAN_POINT('Ctrl Pts',(0.00784283188529941,-0.034193496108874,
0.0684067093605189));
#98412=CARTESIAN_POINT('Ctrl Pts',(0.00739938423285136,-0.0346945769586885,
0.0684444106485235));
#98413=CARTESIAN_POINT('Ctrl Pts',(0.00751889008620946,-0.034527515336289,
0.0684292378432131));
#98414=CARTESIAN_POINT('Ctrl Pts',(0.00763890402066379,-0.0343603235965159,
0.0684178194625285));
#98415=CARTESIAN_POINT('Ctrl Pts',(0.00775907058635305,-0.034193496108874,
0.0684101840015202));
#98416=CARTESIAN_POINT('Ctrl Pts',(0.00788545013106071,-0.0340223579322365,
0.0684050479733614));
#98417=CARTESIAN_POINT('Ctrl Pts',(0.00796468800297119,-0.0339125849573554,
0.0684017607526297));
#98418=CARTESIAN_POINT('Ctrl Pts',(0.0080439382331772,-0.0338030433565221,
0.0684001158816151));
#98419=CARTESIAN_POINT('Ctrl Pts',(0.0081230992875253,-0.0336938721132327,
0.0684001064797843));
#98420=CARTESIAN_POINT('Ctrl Pts',(0.00780373746605553,-0.0340223579322365,
0.0683265354252684));
#98421=CARTESIAN_POINT('Ctrl Pts',(0.00788405823077352,-0.0339125849573554,
0.0683221211737707));
#98422=CARTESIAN_POINT('Ctrl Pts',(0.00796441391976881,-0.0338030433565221,
0.0683193724773064));
#98423=CARTESIAN_POINT('Ctrl Pts',(0.00804470146005949,-0.0336938721132327,
0.0683182837416307));
#98424=CARTESIAN_POINT('Ctrl Pts',(0.00772202480105035,-0.0340223579322365,
0.0682480228771754));
#98425=CARTESIAN_POINT('Ctrl Pts',(0.00780342845857586,-0.0339125849573554,
0.0682424815949117));
#98426=CARTESIAN_POINT('Ctrl Pts',(0.00788488960636042,-0.0338030433565221,
0.0682386290729977));
#98427=CARTESIAN_POINT('Ctrl Pts',(0.00796630363259369,-0.0336938721132327,
0.0682364610034771));
#98428=CARTESIAN_POINT('Ctrl Pts',(0.00764031213604517,-0.0340223579322365,
0.0681695103290823));
#98429=CARTESIAN_POINT('Ctrl Pts',(0.0077227986863782,-0.0339125849573554,
0.0681628420160527));
#98430=CARTESIAN_POINT('Ctrl Pts',(0.00780536529295203,-0.0338030433565221,
0.068157885668689));
#98431=CARTESIAN_POINT('Ctrl Pts',(0.00788790580512789,-0.0336938721132327,
0.0681546382653236));
#98432=CARTESIAN_POINT('Origin',(0.00932085993867162,-0.0345589643415153,
0.0850155495813615));
#98433=CARTESIAN_POINT('Ctrl Pts',(0.0082391967706457,-0.034193496108874,
0.0681511101464263));
#98434=CARTESIAN_POINT('Ctrl Pts',(0.00832191790932497,-0.0340836138581106,
0.0681527016451047));
#98435=CARTESIAN_POINT('Ctrl Pts',(0.00840456642412107,-0.0339738896643499,
0.0681560041205447));
#98436=CARTESIAN_POINT('Ctrl Pts',(0.00848703681848185,-0.0338644633294062,
0.0681610062550407));
#98437=CARTESIAN_POINT('Ctrl Pts',(0.00816245819279496,-0.034193496108874,
0.0682344908990992));
#98438=CARTESIAN_POINT('Ctrl Pts',(0.008244029560271,-0.0340836138581106,
0.0682350242182319));
#98439=CARTESIAN_POINT('Ctrl Pts',(0.00832555075235104,-0.0339738896643499,
0.068237245229758));
#98440=CARTESIAN_POINT('Ctrl Pts',(0.00840691762253109,-0.0338644633294062,
0.0682411440968326));
#98441=CARTESIAN_POINT('Ctrl Pts',(0.00808571961494423,-0.034193496108874,
0.0683178716517722));
#98442=CARTESIAN_POINT('Ctrl Pts',(0.00816614121121704,-0.0340836138581106,
0.068317346791359));
#98443=CARTESIAN_POINT('Ctrl Pts',(0.00824653508058101,-0.0339738896643499,
0.0683184863389713));
#98444=CARTESIAN_POINT('Ctrl Pts',(0.00832679842658033,-0.0338644633294062,
0.0683212819386244));
#98445=CARTESIAN_POINT('Ctrl Pts',(0.0080089810370935,-0.034193496108874,
0.0684012524044451));
#98446=CARTESIAN_POINT('Ctrl Pts',(0.00808825286216307,-0.0340836138581106,
0.0683996693644862));
#98447=CARTESIAN_POINT('Ctrl Pts',(0.00816751940881098,-0.0339738896643499,
0.0683997274481846));
#98448=CARTESIAN_POINT('Ctrl Pts',(0.00824667923062957,-0.0338644633294062,
0.0684014197804163));
#98449=CARTESIAN_POINT('Origin',(0.00884973524919201,-0.0345610621862526,
0.0851134859820757));
#98450=CARTESIAN_POINT('Ctrl Pts',(0.0079741864245549,-0.03424362768739,
0.0684005873251233));
#98451=CARTESIAN_POINT('Ctrl Pts',(0.00819102909828033,-0.033943005420186,
0.0683949452277013));
#98452=CARTESIAN_POINT('Ctrl Pts',(0.00840768073059799,-0.0336441434784162,
0.0684056526375564));
#98453=CARTESIAN_POINT('Ctrl Pts',(0.00772447136808276,-0.03424362768739,
0.0684125200771577));
#98454=CARTESIAN_POINT('Ctrl Pts',(0.00794086399064604,-0.033943005420186,
0.0683974598211207));
#98455=CARTESIAN_POINT('Ctrl Pts',(0.00815777626464629,-0.0336441434784162,
0.0683987419286646));
#98456=CARTESIAN_POINT('Ctrl Pts',(0.0082466515031986,-0.0335235895815127,
0.068401419314291));
#98457=CARTESIAN_POINT('Ctrl Pts',(0.00832579203425014,-0.0334144449262719,
0.0684031108522518));
#98458=CARTESIAN_POINT('Ctrl Pts',(0.00840498854228248,-0.0333049234473133,
0.0684064393173964));
#98459=CARTESIAN_POINT('Ctrl Pts',(0.00848413937374187,-0.0331951640388588,
0.068411409626935));
#98460=CARTESIAN_POINT('Ctrl Pts',(0.00817002998314079,-0.0335235895815127,
0.0683179309010212));
#98461=CARTESIAN_POINT('Ctrl Pts',(0.00825031989657454,-0.0334144449262719,
0.0683185675929045));
#98462=CARTESIAN_POINT('Ctrl Pts',(0.00833068889981629,-0.0333049234473133,
0.0683208637454563));
#98463=CARTESIAN_POINT('Ctrl Pts',(0.00841103395962319,-0.0331951640388588,
0.0683248257317072));
#98464=CARTESIAN_POINT('Ctrl Pts',(0.00809340846308299,-0.0335235895815127,
0.0682344424877513));
#98465=CARTESIAN_POINT('Ctrl Pts',(0.00817484775889894,-0.0334144449262719,
0.0682340243335572));
#98466=CARTESIAN_POINT('Ctrl Pts',(0.00825638925735009,-0.0333049234473133,
0.0682352881735162));
#98467=CARTESIAN_POINT('Ctrl Pts',(0.00833792854550451,-0.0331951640388588,
0.0682382418364794));
#98468=CARTESIAN_POINT('Ctrl Pts',(0.00801678694302518,-0.0335235895815127,
0.0681509540744815));
#98469=CARTESIAN_POINT('Ctrl Pts',(0.00809937562122333,-0.0334144449262719,
0.0681494810742099));
#98470=CARTESIAN_POINT('Ctrl Pts',(0.0081820896148839,-0.0333049234473133,
0.068149712601576));
#98471=CARTESIAN_POINT('Ctrl Pts',(0.00826482313138583,-0.0331951640388588,
0.0681516579412516));
#98472=CARTESIAN_POINT('Origin',(0.00668102421589752,-0.03264345717686,
0.0849806466885375));
#98473=CARTESIAN_POINT('Ctrl Pts',(0.00861710645831259,-0.0336938721132347,
0.0681687917856074));
#98474=CARTESIAN_POINT('Ctrl Pts',(0.00865211645476513,-0.0336474569764937,
0.0681716793762339));
#98475=CARTESIAN_POINT('Ctrl Pts',(0.00868709024941617,-0.033601104548885,
0.0681749766052127));
#98476=CARTESIAN_POINT('Ctrl Pts',(0.0087756358526874,-0.0334837508643148,
0.0681833244305479));
#98477=CARTESIAN_POINT('Ctrl Pts',(0.00886389520989677,-0.033366026476038,
0.0681942923798312));
#98478=CARTESIAN_POINT('Ctrl Pts',(0.00837163885895429,-0.0336938721132347,
0.0684039846786493));
#98479=CARTESIAN_POINT('Ctrl Pts',(0.00840527219335863,-0.0336474569764937,
0.068405435465962));
#98480=CARTESIAN_POINT('Ctrl Pts',(0.00843888623988815,-0.033601104548885,
0.0684072798745103));
#98481=CARTESIAN_POINT('Ctrl Pts',(0.00852398927368931,-0.0334837508643148,
0.0684119494926978));
#98482=CARTESIAN_POINT('Ctrl Pts',(0.00860891656605055,-0.033366026476038,
0.0684191388395642));
#98483=CARTESIAN_POINT('Ctrl Pts',(0.00837163885896573,-0.0336938721132426,
0.0684039846786594));
#98484=CARTESIAN_POINT('Ctrl Pts',(0.00840527219336936,-0.0336474569765026,
0.0684054354659721));
#98485=CARTESIAN_POINT('Ctrl Pts',(0.00843888623989815,-0.0336011045488949,
0.0684072798745204));
#98486=CARTESIAN_POINT('Ctrl Pts',(0.00852328048134079,-0.0334847282606778,
0.0684119106011486));
#98487=CARTESIAN_POINT('Ctrl Pts',(0.00860750220198468,-0.0333679869945434,
0.0684190192852437));
#98488=CARTESIAN_POINT('Ctrl Pts',(0.00837163885894863,-0.0336938721132425,
0.068403984678649));
#98489=CARTESIAN_POINT('Ctrl Pts',(0.0084919265470148,-0.0335278710435082,
0.0684091733361166));
#98490=CARTESIAN_POINT('Ctrl Pts',(0.00861200920320254,-0.0333620469224319,
0.0684181323588499));
#98491=CARTESIAN_POINT('Ctrl Pts',(0.00873194505769313,-0.0331951640388602,
0.068430886176151));
#98492=CARTESIAN_POINT('Ctrl Pts',(0.00828782466038203,-0.0336938721132425,
0.0684021930475727));
#98493=CARTESIAN_POINT('Ctrl Pts',(0.00840814985464127,-0.0335278710435082,
0.068405627129807));
#98494=CARTESIAN_POINT('Ctrl Pts',(0.00852832502685063,-0.0333620469224319,
0.068412833370747));
#98495=CARTESIAN_POINT('Ctrl Pts',(0.00864840874474797,-0.0331951640388602,
0.0684238353433773));
#98496=CARTESIAN_POINT('Ctrl Pts',(0.00820401046181543,-0.0336938721132425,
0.0684004014164963));
#98497=CARTESIAN_POINT('Ctrl Pts',(0.00832437316226774,-0.0335278710435082,
0.0684020809234974));
#98498=CARTESIAN_POINT('Ctrl Pts',(0.00844464085049871,-0.0333620469224319,
0.0684075343826441));
#98499=CARTESIAN_POINT('Ctrl Pts',(0.0085648724318028,-0.0331951640388602,
0.0684167845106035));
#98500=CARTESIAN_POINT('Ctrl Pts',(0.00812019626324883,-0.0336938721132425,
0.0683986097854199));
#98501=CARTESIAN_POINT('Ctrl Pts',(0.00824059646989421,-0.0335278710435082,
0.0683985347171878));
#98502=CARTESIAN_POINT('Ctrl Pts',(0.0083609566741468,-0.0333620469224319,
0.0684022353945412));
#98503=CARTESIAN_POINT('Ctrl Pts',(0.00848133611885764,-0.0331951640388602,
0.0684097336778298));
#98504=CARTESIAN_POINT('Ctrl Pts',(0.00860736419504573,-0.0330240426238155,
0.0684204773996999));
#98505=CARTESIAN_POINT('Ctrl Pts',(0.00868629395086783,-0.0329142774063509,
0.0684271392129077));
#98506=CARTESIAN_POINT('Ctrl Pts',(0.00876512533776395,-0.0328043479726686,
0.0684354360458046));
#98507=CARTESIAN_POINT('Ctrl Pts',(0.00884375707413942,-0.0326943950436594,
0.0684453600507454));
#98508=CARTESIAN_POINT('Ctrl Pts',(0.00853613623801668,-0.0330240426238155,
0.0683323427633641));
#98509=CARTESIAN_POINT('Ctrl Pts',(0.00861628013431971,-0.0329142774063509,
0.0683380233420697));
#98510=CARTESIAN_POINT('Ctrl Pts',(0.00869634655184818,-0.0328043479726686,
0.0683453635509586));
#98511=CARTESIAN_POINT('Ctrl Pts',(0.00877623266059143,-0.0326943950436594,
0.0683543568114647));
#98512=CARTESIAN_POINT('Ctrl Pts',(0.00846490828098764,-0.0330240426238155,
0.0682442081270282));
#98513=CARTESIAN_POINT('Ctrl Pts',(0.00854626631777161,-0.0329142774063509,
0.0682489074712318));
#98514=CARTESIAN_POINT('Ctrl Pts',(0.00862756776593242,-0.0328043479726686,
0.0682552910561126));
#98515=CARTESIAN_POINT('Ctrl Pts',(0.00870870824704343,-0.0326943950436594,
0.068263353572184));
#98516=CARTESIAN_POINT('Ctrl Pts',(0.00839368032395859,-0.0330240426238155,
0.0681560734906924));
#98517=CARTESIAN_POINT('Ctrl Pts',(0.00847625250122349,-0.0329142774063509,
0.0681597916003938));
#98518=CARTESIAN_POINT('Ctrl Pts',(0.00855878898001665,-0.0328043479726686,
0.0681652185612667));
#98519=CARTESIAN_POINT('Ctrl Pts',(0.00864118383349544,-0.0326943950436594,
0.0681723503329033));
#98520=CARTESIAN_POINT('Origin',(0.00666743703714251,-0.0326396682858257,
0.0851035726301499));
#98521=CARTESIAN_POINT('Ctrl Pts',(0.00899014695537431,-0.0331951640388587,
0.0682128784669059));
#98522=CARTESIAN_POINT('Ctrl Pts',(0.00907191879379361,-0.0330855618255041,
0.0682248108888645));
#98523=CARTESIAN_POINT('Ctrl Pts',(0.00915350295762293,-0.0329757224427708,
0.0682384419968624));
#98524=CARTESIAN_POINT('Ctrl Pts',(0.00923479411721618,-0.0328657862078596,
0.0682537594600869));
#98525=CARTESIAN_POINT('Ctrl Pts',(0.00890356312907921,-0.0331951640388587,
0.0682859838228226));
#98526=CARTESIAN_POINT('Ctrl Pts',(0.00898432808911168,-0.0330855618255041,
0.0682967237277317));
#98527=CARTESIAN_POINT('Ctrl Pts',(0.00906492929599861,-0.0329757224427708,
0.0683091406485559));
#98528=CARTESIAN_POINT('Ctrl Pts',(0.0091452627550974,-0.0328657862078596,
0.0683232237475788));
#98529=CARTESIAN_POINT('Ctrl Pts',(0.0088169793027841,-0.0331951640388587,
0.0683590891787393));
#98530=CARTESIAN_POINT('Ctrl Pts',(0.00889673738442976,-0.0330855618255041,
0.0683686365665988));
#98531=CARTESIAN_POINT('Ctrl Pts',(0.0089763556343743,-0.0329757224427708,
0.0683798393002495));
#98532=CARTESIAN_POINT('Ctrl Pts',(0.00905573139297862,-0.0328657862078596,
0.0683926880350707));
#98533=CARTESIAN_POINT('Ctrl Pts',(0.008730395476489,-0.0331951640388587,
0.068432194534656));
#98534=CARTESIAN_POINT('Ctrl Pts',(0.00880914667974784,-0.0330855618255041,
0.0684405494054659));
#98535=CARTESIAN_POINT('Ctrl Pts',(0.00888778197274998,-0.0329757224427708,
0.0684505379519431));
#98536=CARTESIAN_POINT('Ctrl Pts',(0.00896620003085984,-0.0328657862078596,
0.0684621523225627));
#98537=CARTESIAN_POINT('Origin',(0.00619733850441799,-0.0326401908834255,
0.0850021811058405));
#98538=CARTESIAN_POINT('Ctrl Pts',(0.00869603062313004,-0.0332451089994432,
0.0684271810500122));
#98539=CARTESIAN_POINT('Ctrl Pts',(0.00891187027115007,-0.0329451141710258,
0.068448763752662));
#98540=CARTESIAN_POINT('Ctrl Pts',(0.00912547104411551,-0.0326442513127503,
0.0684865430657797));
#98541=CARTESIAN_POINT('Ctrl Pts',(0.00844678931927606,-0.0332451089994432,
0.0684077189727038));
#98542=CARTESIAN_POINT('Ctrl Pts',(0.00866336299155103,-0.0329451141710258,
0.0684199013857819));
#98543=CARTESIAN_POINT('Ctrl Pts',(0.00887840377172522,-0.0326442513127503,
0.0684483624042661));
#98544=CARTESIAN_POINT('Ctrl Pts',(0.00896616879731833,-0.0325229783203384,
0.0684621476059621));
#98545=CARTESIAN_POINT('Ctrl Pts',(0.00904457571675786,-0.0324130253112079,
0.068473759886668));
#98546=CARTESIAN_POINT('Ctrl Pts',(0.00912273052931295,-0.0323031222247694,
0.0684869923539639));
#98547=CARTESIAN_POINT('Ctrl Pts',(0.00920053372233297,-0.0321934096636184,
0.0685018245254217));
#98548=CARTESIAN_POINT('Ctrl Pts',(0.00890061538018178,-0.0325229783203384,
0.0683697144292825));
#98549=CARTESIAN_POINT('Ctrl Pts',(0.00898029648891727,-0.0324130253112079,
0.0683804230575832));
#98550=CARTESIAN_POINT('Ctrl Pts',(0.00905974399072303,-0.0323031222247694,
0.0683927783677724));
#98551=CARTESIAN_POINT('Ctrl Pts',(0.00913885667745818,-0.0321934096636184,
0.0684067609425686));
#98552=CARTESIAN_POINT('Ctrl Pts',(0.00883506196304524,-0.0325229783203384,
0.0682772812526029));
#98553=CARTESIAN_POINT('Ctrl Pts',(0.00891601726107668,-0.0324130253112079,
0.0682870862284984));
#98554=CARTESIAN_POINT('Ctrl Pts',(0.00899675745213311,-0.0323031222247694,
0.0682985643815809));
#98555=CARTESIAN_POINT('Ctrl Pts',(0.00907717963258339,-0.0321934096636184,
0.0683116973597155));
#98556=CARTESIAN_POINT('Ctrl Pts',(0.00876950854590869,-0.0325229783203384,
0.0681848480759233));
#98557=CARTESIAN_POINT('Ctrl Pts',(0.00885173803323609,-0.0324130253112079,
0.0681937493994136));
#98558=CARTESIAN_POINT('Ctrl Pts',(0.0089337709135432,-0.0323031222247694,
0.0682043503953893));
#98559=CARTESIAN_POINT('Ctrl Pts',(0.0090155025877086,-0.0321934096636184,
0.0682166337768624));
#98560=CARTESIAN_POINT('Origin',(0.00666879662080091,-0.0326393375178324,
0.0850951558291911));
#98561=CARTESIAN_POINT('Ctrl Pts',(0.00936123232799051,-0.0326943950436594,
0.0682789935135691));
#98562=CARTESIAN_POINT('Ctrl Pts',(0.00944214580081217,-0.0325844576448127,
0.0682960478956564));
#98563=CARTESIAN_POINT('Ctrl Pts',(0.0095227122874234,-0.0324744968375319,
0.0683147769079863));
#98564=CARTESIAN_POINT('Ctrl Pts',(0.00960282889232979,-0.0323646534831894,
0.0683351551300524));
#98565=CARTESIAN_POINT('Ctrl Pts',(0.00927022911848484,-0.0326943950436594,
0.0683465179050241));
#98566=CARTESIAN_POINT('Ctrl Pts',(0.00935021197863805,-0.0325844576448127,
0.0683623180923262));
#98567=CARTESIAN_POINT('Ctrl Pts',(0.00942987372552438,-0.0324744968375319,
0.0683797735745138));
#98568=CARTESIAN_POINT('Ctrl Pts',(0.00950911260034835,-0.0323646534831894,
0.0683988605787906));
#98569=CARTESIAN_POINT('Ctrl Pts',(0.00917922590897917,-0.0326943950436594,
0.0684140422964789));
#98570=CARTESIAN_POINT('Ctrl Pts',(0.00925827815646394,-0.0325844576448127,
0.0684285882889959));
#98571=CARTESIAN_POINT('Ctrl Pts',(0.00933703516362535,-0.0324744968375319,
0.0684447702410413));
#98572=CARTESIAN_POINT('Ctrl Pts',(0.0094153963083669,-0.0323646534831894,
0.0684625660275288));
#98573=CARTESIAN_POINT('Ctrl Pts',(0.00908822269947349,-0.0326943950436594,
0.0684815666879339));
#98574=CARTESIAN_POINT('Ctrl Pts',(0.00916634433428982,-0.0325844576448127,
0.0684948584856657));
#98575=CARTESIAN_POINT('Ctrl Pts',(0.00924419660172632,-0.0324744968375319,
0.0685097669075688));
#98576=CARTESIAN_POINT('Ctrl Pts',(0.00932168001638546,-0.0323646534831894,
0.0685262714762671));
#98577=CARTESIAN_POINT('Origin',(0.0061911757942771,-0.0326395579067402,
0.0850395171850295));
#98578=CARTESIAN_POINT('Ctrl Pts',(0.0090542014899579,-0.0327445246961877,
0.0684743991567367));
#98579=CARTESIAN_POINT('Ctrl Pts',(0.00926826027291881,-0.0324436878365475,
0.0685094904938175));
#98580=CARTESIAN_POINT('Ctrl Pts',(0.00947906771459618,-0.0321434074463187,
0.0685606059223521));
#98581=CARTESIAN_POINT('Ctrl Pts',(0.00880667380163768,-0.0327445246961877,
0.0684393271805328));
#98582=CARTESIAN_POINT('Ctrl Pts',(0.00902205534579157,-0.0324436878365475,
0.0684650828583286));
#98583=CARTESIAN_POINT('Ctrl Pts',(0.0092348849908425,-0.0321434074463187,
0.0685069887849776));
#98584=CARTESIAN_POINT('Ctrl Pts',(0.00941419039007019,-0.0322357242816072,
0.0685452723808186));
#98585=CARTESIAN_POINT('Ctrl Pts',(0.0095926936956757,-0.0319819883628706,
0.0685863702082937));
#98586=CARTESIAN_POINT('Ctrl Pts',(0.00976822006984993,-0.0317295851069886,
0.0686387434219101));
#98587=CARTESIAN_POINT('Ctrl Pts',(0.00916940259726973,-0.0322357242816072,
0.0684944891503594));
#98588=CARTESIAN_POINT('Ctrl Pts',(0.00934952328290193,-0.0319819883628706,
0.0685277908041121));
#98589=CARTESIAN_POINT('Ctrl Pts',(0.00952715985211837,-0.0317295851069886,
0.0685724865624373));
#98590=CARTESIAN_POINT('Origin',(0.00620950443384443,-0.032637194264687,
0.0849459946505887));
#98591=CARTESIAN_POINT('Origin',(0.00668785385502022,-0.0326352985529741,
0.0849739096964743));
#98592=CARTESIAN_POINT('Ctrl Pts',(0.00972743405026177,-0.0321934096636183,
0.0683682787406266));
#98593=CARTESIAN_POINT('Ctrl Pts',(0.00980716849242794,-0.0320835708272304,
0.0683903943495469));
#98594=CARTESIAN_POINT('Ctrl Pts',(0.00988639900400012,-0.0319739230346346,
0.0684141472306517));
#98595=CARTESIAN_POINT('Ctrl Pts',(0.00996502654739581,-0.0318646057455575,
0.0684394992139177));
#98596=CARTESIAN_POINT('Ctrl Pts',(0.00963237038554758,-0.0321934096636183,
0.0684299558386126));
#98597=CARTESIAN_POINT('Ctrl Pts',(0.00971125425246431,-0.0320835708272304,
0.0684507604455085));
#98598=CARTESIAN_POINT('Ctrl Pts',(0.00978966181327403,-0.0319739230346346,
0.0684731854824126));
#98599=CARTESIAN_POINT('Ctrl Pts',(0.009867494952918,-0.0318646057455575,
0.0684971945589941));
#98600=CARTESIAN_POINT('Ctrl Pts',(0.00953730672083339,-0.0321934096636183,
0.0684916329365987));
#98601=CARTESIAN_POINT('Ctrl Pts',(0.00961534001250069,-0.0320835708272304,
0.06851112654147));
#98602=CARTESIAN_POINT('Ctrl Pts',(0.00969292462254795,-0.0319739230346346,
0.0685322237341735));
#98603=CARTESIAN_POINT('Ctrl Pts',(0.00976996335844018,-0.0318646057455575,
0.0685548899040705));
#98604=CARTESIAN_POINT('Ctrl Pts',(0.0094422430561192,-0.0321934096636183,
0.0685533100345848));
#98605=CARTESIAN_POINT('Ctrl Pts',(0.00951942577253707,-0.0320835708272304,
0.0685714926374316));
#98606=CARTESIAN_POINT('Ctrl Pts',(0.00959618743182186,-0.0319739230346346,
0.0685912619859344));
#98607=CARTESIAN_POINT('Ctrl Pts',(0.00967243176396236,-0.0318646057455575,
0.068612585249147));
#98608=CARTESIAN_POINT('Ctrl Pts',(0.00932139294781656,-0.0320218834582328,
0.0685253643424135));
#98609=CARTESIAN_POINT('Ctrl Pts',(0.00937993180754131,-0.0319391099350642,
0.0685378285751643));
#98610=CARTESIAN_POINT('Ctrl Pts',(0.00943824056931616,-0.031856486945494,
0.0685511993486559));
#98611=CARTESIAN_POINT('Ctrl Pts',(0.00949627767213026,-0.031774074144655,
0.0685654629591656));
#98612=CARTESIAN_POINT('Ctrl Pts',(0.00929531728817879,-0.0320218834582328,
0.068483211192807));
#98613=CARTESIAN_POINT('Ctrl Pts',(0.00935429486028635,-0.0319391099350642,
0.0684954040409785));
#98614=CARTESIAN_POINT('Ctrl Pts',(0.00941304630634758,-0.031856486945494,
0.0685085104448712));
#98615=CARTESIAN_POINT('Ctrl Pts',(0.0094715297249382,-0.031774074144655,
0.0685225168632189));
#98616=CARTESIAN_POINT('Ctrl Pts',(0.00926924162854101,-0.0320218834582328,
0.0684410580432006));
#98617=CARTESIAN_POINT('Ctrl Pts',(0.00932865791303139,-0.0319391099350642,
0.0684529795067928));
#98618=CARTESIAN_POINT('Ctrl Pts',(0.009387852043379,-0.031856486945494,
0.0684658215410865));
#98619=CARTESIAN_POINT('Ctrl Pts',(0.00944678177774615,-0.031774074144655,
0.0684795707672721));
#98620=CARTESIAN_POINT('Ctrl Pts',(0.00924316596890324,-0.0320218834582328,
0.0683989048935941));
#98621=CARTESIAN_POINT('Ctrl Pts',(0.00930302096577642,-0.0319391099350642,
0.068410554972607));
#98622=CARTESIAN_POINT('Ctrl Pts',(0.00936265778041042,-0.031856486945494,
0.0684231326373018));
#98623=CARTESIAN_POINT('Ctrl Pts',(0.0094220338305541,-0.031774074144655,
0.0684366246713254));
#98624=CARTESIAN_POINT('Origin',(0.00971022807106882,-0.0391228853390632,
0.0621765373510591));
#98625=CARTESIAN_POINT('Ctrl Pts',(0.00629088080421439,-0.0352722978779559,
0.0686979694570567));
#98626=CARTESIAN_POINT('Ctrl Pts',(0.00630890107951828,-0.0352466642097193,
0.0686922806649198));
#98627=CARTESIAN_POINT('Ctrl Pts',(0.00632688169870236,-0.035221018380829,
0.0686865221768446));
#98628=CARTESIAN_POINT('Ctrl Pts',(0.00634482313386381,-0.0351953608940152,
0.0686806932824731));
#98629=CARTESIAN_POINT('Origin',(0.00498953171674852,-0.0352456003065034,
0.0639739633449897));
#98630=CARTESIAN_POINT('Ctrl Pts',(0.00646422762586219,-0.0350241211493339,
0.0686448061997158));
#98631=CARTESIAN_POINT('Ctrl Pts',(0.00654005940982445,-0.0349144232867421,
0.0686219465170266));
#98632=CARTESIAN_POINT('Ctrl Pts',(0.00661640910871704,-0.0348045283677512,
0.0686006406488063));
#98633=CARTESIAN_POINT('Ctrl Pts',(0.00669317994381437,-0.0346945769586886,
0.0685809195243136));
#98634=CARTESIAN_POINT('Ctrl Pts',(0.00636555700172017,-0.0350241211493339,
0.0685890814320229));
#98635=CARTESIAN_POINT('Ctrl Pts',(0.00644215637147474,-0.0349144232867421,
0.068564862602004));
#98636=CARTESIAN_POINT('Ctrl Pts',(0.00651930221014196,-0.0348045283677512,
0.0685422126394849));
#98637=CARTESIAN_POINT('Ctrl Pts',(0.00659689678330767,-0.0346945769586886,
0.0685211642332857));
#98638=CARTESIAN_POINT('Ctrl Pts',(0.00626688637757816,-0.0350241211493339,
0.06853335666433));
#98639=CARTESIAN_POINT('Ctrl Pts',(0.00634425333312504,-0.0349144232867421,
0.0685077786869814));
#98640=CARTESIAN_POINT('Ctrl Pts',(0.00642219531156688,-0.0348045283677512,
0.0684837846301635));
#98641=CARTESIAN_POINT('Ctrl Pts',(0.00650061362280097,-0.0346945769586886,
0.0684614089422577));
#98642=CARTESIAN_POINT('Ctrl Pts',(0.00616821575343614,-0.0350241211493339,
0.0684776318966372));
#98643=CARTESIAN_POINT('Ctrl Pts',(0.00624635029477534,-0.0349144232867421,
0.0684506947719588));
#98644=CARTESIAN_POINT('Ctrl Pts',(0.0063250884129918,-0.0348045283677512,
0.0684253566208421));
#98645=CARTESIAN_POINT('Ctrl Pts',(0.00640433046229427,-0.0346945769586886,
0.0684016536512297));
#98646=CARTESIAN_POINT('Origin',(0.0106956549522073,-0.0345629067943476,
0.0848856164820718));
#98647=CARTESIAN_POINT('Ctrl Pts',(0.0066984359549881,-0.035197097365166,
0.0683929252324924));
#98648=CARTESIAN_POINT('Ctrl Pts',(0.00677819242367436,-0.0350869349321818,
0.0683731789920494));
#98649=CARTESIAN_POINT('Ctrl Pts',(0.00685842547508718,-0.0349764985129769,
0.0683550744868359));
#98650=CARTESIAN_POINT('Ctrl Pts',(0.00693903254564575,-0.034865930684969,
0.0683386412905385));
#98651=CARTESIAN_POINT('Ctrl Pts',(0.00665956862327684,-0.035197097365166,
0.0684653807441935));
#98652=CARTESIAN_POINT('Ctrl Pts',(0.00673832131904309,-0.0350869349321818,
0.0684450960495441));
#98653=CARTESIAN_POINT('Ctrl Pts',(0.00681756096018664,-0.0349764985129769,
0.0684264317761925));
#98654=CARTESIAN_POINT('Ctrl Pts',(0.00689718631280816,-0.034865930684969,
0.0684094181472611));
#98655=CARTESIAN_POINT('Ctrl Pts',(0.00662070129156558,-0.035197097365166,
0.0685378362558945));
#98656=CARTESIAN_POINT('Ctrl Pts',(0.00669845021441181,-0.0350869349321818,
0.0685170131070389));
#98657=CARTESIAN_POINT('Ctrl Pts',(0.0067766964452861,-0.0349764985129769,
0.068497789065549));
#98658=CARTESIAN_POINT('Ctrl Pts',(0.00685534007997056,-0.034865930684969,
0.0684801950039836));
#98659=CARTESIAN_POINT('Ctrl Pts',(0.00658183395985432,-0.035197097365166,
0.0686102917675956));
#98660=CARTESIAN_POINT('Ctrl Pts',(0.00665857910978054,-0.0350869349321818,
0.0685889301645337));
#98661=CARTESIAN_POINT('Ctrl Pts',(0.00673583193038556,-0.0349764985129769,
0.0685691463549055));
#98662=CARTESIAN_POINT('Ctrl Pts',(0.00681349384713296,-0.034865930684969,
0.0685509718607061));
#98663=CARTESIAN_POINT('Origin',(0.0102194283572242,-0.0345637187966277,
0.0849529483964491));
#98664=CARTESIAN_POINT('Ctrl Pts',(0.00654914096335699,-0.0352450361861253,
0.0686183971583664));
#98665=CARTESIAN_POINT('Ctrl Pts',(0.00675776878258464,-0.0349452761023765,
0.0685590085913934));
#98666=CARTESIAN_POINT('Ctrl Pts',(0.00697027730191754,-0.0346444289983475,
0.0685155034416551));
#98667=CARTESIAN_POINT('Ctrl Pts',(0.00631023771396125,-0.0352450361861253,
0.0686920533694295));
#98668=CARTESIAN_POINT('Ctrl Pts',(0.00651608754367545,-0.0349452761023765,
0.0686236544187838));
#98669=CARTESIAN_POINT('Ctrl Pts',(0.00672650466441856,-0.0346444289983475,
0.0685709552333918));
#98670=CARTESIAN_POINT('Ctrl Pts',(0.00681317539719488,-0.0345231616327822,
0.0685514653176442));
#98671=CARTESIAN_POINT('Ctrl Pts',(0.00689034331568431,-0.0344132092796975,
0.0685334004481495));
#98672=CARTESIAN_POINT('Ctrl Pts',(0.00696788091024001,-0.0343032738558974,
0.0685169326682436));
#98673=CARTESIAN_POINT('Ctrl Pts',(0.00704568830583149,-0.0341934961088741,
0.0685020805305624));
#98674=CARTESIAN_POINT('Ctrl Pts',(0.00671819847515509,-0.0345231616327822,
0.068489654959141));
#98675=CARTESIAN_POINT('Ctrl Pts',(0.00679621836241447,-0.0344132092796975,
0.0684702809664927));
#98676=CARTESIAN_POINT('Ctrl Pts',(0.00687463495996224,-0.0343032738558974,
0.0684525217532801));
#98677=CARTESIAN_POINT('Ctrl Pts',(0.0069533472242835,-0.0341934961088741,
0.0684363974977686));
#98678=CARTESIAN_POINT('Ctrl Pts',(0.00662322155311531,-0.0345231616327822,
0.0684278446006377));
#98679=CARTESIAN_POINT('Ctrl Pts',(0.00670209340914463,-0.0344132092796975,
0.0684071614848359));
#98680=CARTESIAN_POINT('Ctrl Pts',(0.00678138900968448,-0.0343032738558974,
0.0683881108383165));
#98681=CARTESIAN_POINT('Ctrl Pts',(0.00686100614273552,-0.0341934961088741,
0.0683707144649747));
#98682=CARTESIAN_POINT('Ctrl Pts',(0.00652824463107553,-0.0345231616327822,
0.0683660342421344));
#98683=CARTESIAN_POINT('Ctrl Pts',(0.00660796845587478,-0.0344132092796975,
0.0683440420031791));
#98684=CARTESIAN_POINT('Ctrl Pts',(0.0066881430594067,-0.0343032738558974,
0.068323699923353));
#98685=CARTESIAN_POINT('Ctrl Pts',(0.00676866506118753,-0.0341934961088741,
0.0683050314321808));
#98686=CARTESIAN_POINT('Origin',(0.0106987177838239,-0.034562559623147,
0.0848973261947764));
#98687=CARTESIAN_POINT('Ctrl Pts',(0.00711307259435406,-0.0346945769586886,
0.0682357404430474));
#98688=CARTESIAN_POINT('Ctrl Pts',(0.00719457408035251,-0.034584662917669,
0.0682218123539234));
#98689=CARTESIAN_POINT('Ctrl Pts',(0.00727637751416807,-0.0344746925051587,
0.0682095673031063));
#98690=CARTESIAN_POINT('Ctrl Pts',(0.00735837801501828,-0.0343648066255171,
0.0681990205474912));
#98691=CARTESIAN_POINT('Ctrl Pts',(0.00705331735037547,-0.0346945769586886,
0.0683320235277438));
#98692=CARTESIAN_POINT('Ctrl Pts',(0.00713349200680147,-0.034584662917669,
0.0683172719811551));
#98693=CARTESIAN_POINT('Ctrl Pts',(0.00721398541318103,-0.0344746925051587,
0.0683041758939341));
#98694=CARTESIAN_POINT('Ctrl Pts',(0.00729469436278638,-0.0343648066255171,
0.068292751620354));
#98695=CARTESIAN_POINT('Ctrl Pts',(0.00699356210639688,-0.0346945769586886,
0.0684283066124402));
#98696=CARTESIAN_POINT('Ctrl Pts',(0.00707240993325044,-0.034584662917669,
0.0684127316083868));
#98697=CARTESIAN_POINT('Ctrl Pts',(0.00715159331219398,-0.0344746925051587,
0.0683987844847619));
#98698=CARTESIAN_POINT('Ctrl Pts',(0.00723101071055449,-0.0343648066255171,
0.0683864826932167));
#98699=CARTESIAN_POINT('Ctrl Pts',(0.00693380686241829,-0.0346945769586886,
0.0685245896971366));
#98700=CARTESIAN_POINT('Ctrl Pts',(0.0070113278596994,-0.034584662917669,
0.0685081912356185));
#98701=CARTESIAN_POINT('Ctrl Pts',(0.00708920121120694,-0.0344746925051587,
0.0684933930755897));
#98702=CARTESIAN_POINT('Ctrl Pts',(0.00716732705832259,-0.0343648066255171,
0.0684802137660795));
#98703=CARTESIAN_POINT('Origin',(0.0102313190724556,-0.0345626446731875,
0.0850101562767245));
#98704=CARTESIAN_POINT('Ctrl Pts',(0.0069348760841074,-0.0346945769586886,
0.0685228668698901));
#98705=CARTESIAN_POINT('Ctrl Pts',(0.00705273864049687,-0.0345275153362891,
0.0684979647554254));
#98706=CARTESIAN_POINT('Ctrl Pts',(0.0071714148307595,-0.0343603235965159,
0.0684767628689118));
#98707=CARTESIAN_POINT('Ctrl Pts',(0.00729055273143401,-0.034193496108874,
0.0684593186994703));
#98708=CARTESIAN_POINT('Ctrl Pts',(0.00685324951084643,-0.0346945769586886,
0.0685419752677544));
#98709=CARTESIAN_POINT('Ctrl Pts',(0.00697071183419206,-0.0345275153362891,
0.0685153634520314));
#98710=CARTESIAN_POINT('Ctrl Pts',(0.00708904145642097,-0.0343603235965159,
0.0684924388350822));
#98711=CARTESIAN_POINT('Ctrl Pts',(0.00720788740334028,-0.034193496108874,
0.0684732640163339));
#98712=CARTESIAN_POINT('Ctrl Pts',(0.00677162293758547,-0.0346945769586886,
0.0685610836656189));
#98713=CARTESIAN_POINT('Ctrl Pts',(0.00688868502788724,-0.0345275153362891,
0.0685327621486373));
#98714=CARTESIAN_POINT('Ctrl Pts',(0.00700666808208244,-0.0343603235965159,
0.0685081148012525));
#98715=CARTESIAN_POINT('Ctrl Pts',(0.00712522207524654,-0.034193496108874,
0.0684872093331976));
#98716=CARTESIAN_POINT('Ctrl Pts',(0.0066899963643245,-0.0346945769586886,
0.0685801920634833));
#98717=CARTESIAN_POINT('Ctrl Pts',(0.00680665822158242,-0.0345275153362891,
0.0685501608452433));
#98718=CARTESIAN_POINT('Ctrl Pts',(0.00692429470774392,-0.0343603235965159,
0.068523790767423));
#98719=CARTESIAN_POINT('Ctrl Pts',(0.00704255674715281,-0.034193496108874,
0.0685011546500612));
#98720=CARTESIAN_POINT('Ctrl Pts',(0.00716729603638599,-0.0340223579322365,
0.0684802195640239));
#98721=CARTESIAN_POINT('Ctrl Pts',(0.0072454970960055,-0.0339125849573554,
0.0684670271253022));
#98722=CARTESIAN_POINT('Ctrl Pts',(0.00732391625747238,-0.0338030433565221,
0.0684554625369745));
#98723=CARTESIAN_POINT('Ctrl Pts',(0.00740245192490082,-0.0336938721132328,
0.0684455316983661));
#98724=CARTESIAN_POINT('Ctrl Pts',(0.00707638746862284,-0.0340223579322365,
0.0684125674233514));
#98725=CARTESIAN_POINT('Ctrl Pts',(0.0071555216277064,-0.0339125849573554,
0.0683981211183808));
#98726=CARTESIAN_POINT('Ctrl Pts',(0.00723489918507691,-0.0338030433565221,
0.068385322857872));
#98727=CARTESIAN_POINT('Ctrl Pts',(0.00731441717936894,-0.0336938721132328,
0.0683741800101628));
#98728=CARTESIAN_POINT('Ctrl Pts',(0.00698547890085968,-0.0340223579322365,
0.0683449152826789));
#98729=CARTESIAN_POINT('Ctrl Pts',(0.00706554615940729,-0.0339125849573554,
0.0683292151114593));
#98730=CARTESIAN_POINT('Ctrl Pts',(0.00714588211268144,-0.0338030433565221,
0.0683151831787696));
#98731=CARTESIAN_POINT('Ctrl Pts',(0.00722638243383706,-0.0336938721132328,
0.0683028283219595));
#98732=CARTESIAN_POINT('Ctrl Pts',(0.00689457033309653,-0.0340223579322365,
0.0682772631420064));
#98733=CARTESIAN_POINT('Ctrl Pts',(0.00697557069110819,-0.0339125849573554,
0.0682603091045379));
#98734=CARTESIAN_POINT('Ctrl Pts',(0.00705686504028598,-0.0338030433565221,
0.0682450434996672));
#98735=CARTESIAN_POINT('Ctrl Pts',(0.00713834768830519,-0.0336938721132328,
0.0682314766337562));
#98736=CARTESIAN_POINT('Origin',(0.0106732350869064,-0.0345589643416464,
0.0847798378537598));
#98737=CARTESIAN_POINT('Ctrl Pts',(0.00748642642908477,-0.034193496108874,
0.0681839479025));
#98738=CARTESIAN_POINT('Ctrl Pts',(0.00756869475421948,-0.0340836138585569,
0.068175159143977));
#98739=CARTESIAN_POINT('Ctrl Pts',(0.00765110547038093,-0.033973889665241,
0.0681680769728248));
#98740=CARTESIAN_POINT('Ctrl Pts',(0.00773355249440548,-0.0338644633307392,
0.0681627033828056));
#98741=CARTESIAN_POINT('Ctrl Pts',(0.00742074333719059,-0.034193496108874,
0.0682762890671347));
#98742=CARTESIAN_POINT('Ctrl Pts',(0.00750173833235243,-0.0340836138585569,
0.068266594577674));
#98743=CARTESIAN_POINT('Ctrl Pts',(0.00758289507170985,-0.033973889665241,
0.0682585807612792));
#98744=CARTESIAN_POINT('Ctrl Pts',(0.00766410899710287,-0.0338644633307392,
0.0682522509116897));
#98745=CARTESIAN_POINT('Ctrl Pts',(0.00735506024529641,-0.034193496108874,
0.0683686302317693));
#98746=CARTESIAN_POINT('Ctrl Pts',(0.00743478191048538,-0.0340836138585569,
0.0683580300113712));
#98747=CARTESIAN_POINT('Ctrl Pts',(0.00751468467303877,-0.033973889665241,
0.0683490845497336));
#98748=CARTESIAN_POINT('Ctrl Pts',(0.00759466549980026,-0.0338644633307392,
0.0683417984405737));
#98749=CARTESIAN_POINT('Ctrl Pts',(0.00728937715340224,-0.034193496108874,
0.068460971396404));
#98750=CARTESIAN_POINT('Ctrl Pts',(0.00736782548861832,-0.0340836138585569,
0.0684494654450682));
#98751=CARTESIAN_POINT('Ctrl Pts',(0.0074464742743677,-0.033973889665241,
0.068439588338188));
#98752=CARTESIAN_POINT('Ctrl Pts',(0.00752522200249765,-0.0338644633307392,
0.0684313459694578));
#98753=CARTESIAN_POINT('Origin',(0.0102181000419078,-0.0345610621862964,
0.0849360495769488));
#98754=CARTESIAN_POINT('Ctrl Pts',(0.00725477355023421,-0.03424362768739,
0.0684646724827314));
#98755=CARTESIAN_POINT('Ctrl Pts',(0.00746919921239556,-0.033943005420186,
0.06843189728146));
#98756=CARTESIAN_POINT('Ctrl Pts',(0.00768548447618193,-0.0336441434784162,
0.068415366610555));
#98757=CARTESIAN_POINT('Ctrl Pts',(0.0070085231419664,-0.03424362768739,
0.0685078087369492));
#98758=CARTESIAN_POINT('Ctrl Pts',(0.00722132189348,-0.033943005420186,
0.0684657460484239));
#98759=CARTESIAN_POINT('Ctrl Pts',(0.00743668444009545,-0.0336441434784162,
0.0684398317294667));
#98760=CARTESIAN_POINT('Ctrl Pts',(0.0075251944362441,-0.0335235895815127,
0.0684313489820763));
#98761=CARTESIAN_POINT('Ctrl Pts',(0.00760392292649248,-0.0334144449262719,
0.0684231082430923));
#98762=CARTESIAN_POINT('Ctrl Pts',(0.0076829121137035,-0.0333049234473132,
0.0684164845078563));
#98763=CARTESIAN_POINT('Ctrl Pts',(0.0077620617621819,-0.0331951640388588,
0.0684114953953736));
#98764=CARTESIAN_POINT('Ctrl Pts',(0.00743871322695743,-0.0335235895815127,
0.0683581221227513));
#98765=CARTESIAN_POINT('Ctrl Pts',(0.00751844982909482,-0.0334144449262719,
0.0683486907996557));
#98766=CARTESIAN_POINT('Ctrl Pts',(0.00759847288296501,-0.0333049234473132,
0.0683408959393041));
#98767=CARTESIAN_POINT('Ctrl Pts',(0.00767868096652558,-0.0331951640388588,
0.0683347567779636));
#98768=CARTESIAN_POINT('Ctrl Pts',(0.00735223201767076,-0.0335235895815127,
0.0682848952634263));
#98769=CARTESIAN_POINT('Ctrl Pts',(0.00743297673169716,-0.0334144449262719,
0.068274273356219));
#98770=CARTESIAN_POINT('Ctrl Pts',(0.00751403365222652,-0.0333049234473132,
0.0682653073707518));
#98771=CARTESIAN_POINT('Ctrl Pts',(0.00759530017086926,-0.0331951640388588,
0.0682580181605535));
#98772=CARTESIAN_POINT('Ctrl Pts',(0.00726575080838409,-0.0335235895815127,
0.0682116684041013));
#98773=CARTESIAN_POINT('Ctrl Pts',(0.00734750363429951,-0.0334144449262719,
0.0681998559127824));
#98774=CARTESIAN_POINT('Ctrl Pts',(0.00742959442148803,-0.0333049234473132,
0.0681897188021996));
#98775=CARTESIAN_POINT('Ctrl Pts',(0.00751191937521294,-0.0331951640388588,
0.0681812795431434));
#98776=CARTESIAN_POINT('Origin',(0.00804984076466302,-0.0326434571769387,
0.0850760693271538));
#98777=CARTESIAN_POINT('Ctrl Pts',(0.00786357228300075,-0.0336938721132348,
0.0681541254735253));
#98778=CARTESIAN_POINT('Ctrl Pts',(0.00789866812624473,-0.0336474569764937,
0.0681526023785747));
#98779=CARTESIAN_POINT('Ctrl Pts',(0.00793377939444855,-0.033601104548885,
0.0681514902291446));
#98780=CARTESIAN_POINT('Ctrl Pts',(0.00802267304765969,-0.0334837508662601,
0.0681486745226544));
#98781=CARTESIAN_POINT('Ctrl Pts',(0.00811161110055061,-0.0333660264799399,
0.0681484941557096));
#98782=CARTESIAN_POINT('Ctrl Pts',(0.00764951775477796,-0.0336938721132348,
0.0684182290483189));
#98783=CARTESIAN_POINT('Ctrl Pts',(0.00768306771215988,-0.0336474569764937,
0.0684154530211838));
#98784=CARTESIAN_POINT('Ctrl Pts',(0.0077166478675799,-0.033601104548885,
0.0684130699288751));
#98785=CARTESIAN_POINT('Ctrl Pts',(0.00780166509547823,-0.0334837508662601,
0.0684070364874161));
#98786=CARTESIAN_POINT('Ctrl Pts',(0.00788682377344934,-0.0333660264799399,
0.0684035249319819));
#98787=CARTESIAN_POINT('Ctrl Pts',(0.00764951775478944,-0.0336938721132427,
0.0684182290483287));
#98788=CARTESIAN_POINT('Ctrl Pts',(0.00768306771217062,-0.0336474569765026,
0.0684154530211937));
#98789=CARTESIAN_POINT('Ctrl Pts',(0.0077166478675899,-0.0336011045488949,
0.0684130699288851));
#98790=CARTESIAN_POINT('Ctrl Pts',(0.0078009570177727,-0.0334847282626114,
0.0684070867377759));
#98791=CARTESIAN_POINT('Ctrl Pts',(0.00788540557795273,-0.0333679869984219,
0.068403583587206));
#98792=CARTESIAN_POINT('Ctrl Pts',(0.00764951775477237,-0.0336938721132425,
0.0684182290483193));
#98793=CARTESIAN_POINT('Ctrl Pts',(0.00776950724970819,-0.0335278710435082,
0.0684083007467696));
#98794=CARTESIAN_POINT('Ctrl Pts',(0.00788976588157369,-0.033362046922432,
0.0684021387773378));
#98795=CARTESIAN_POINT('Ctrl Pts',(0.00801035448319115,-0.0331951640388602,
0.0683997600785164));
#98796=CARTESIAN_POINT('Ctrl Pts',(0.0075661399052794,-0.0336938721132425,
0.068426956249314));
#98797=CARTESIAN_POINT('Ctrl Pts',(0.00768594670407325,-0.0335278710435082,
0.0684152825071084));
#98798=CARTESIAN_POINT('Ctrl Pts',(0.007806077440634,-0.033362046922432,
0.0684073699817591));
#98799=CARTESIAN_POINT('Ctrl Pts',(0.00792659317535379,-0.0331951640388602,
0.0684032347198865));
#98800=CARTESIAN_POINT('Ctrl Pts',(0.00748276205578642,-0.0336938721132425,
0.0684356834503088));
#98801=CARTESIAN_POINT('Ctrl Pts',(0.0076023861584383,-0.0335278710435082,
0.0684222642674473));
#98802=CARTESIAN_POINT('Ctrl Pts',(0.00772238899969432,-0.033362046922432,
0.0684126011861805));
#98803=CARTESIAN_POINT('Ctrl Pts',(0.00784283186751643,-0.0331951640388602,
0.0684067093612567));
#98804=CARTESIAN_POINT('Ctrl Pts',(0.00739938420629345,-0.0336938721132425,
0.0684444106513035));
#98805=CARTESIAN_POINT('Ctrl Pts',(0.00751882561280336,-0.0335278710435082,
0.0684292460277861));
#98806=CARTESIAN_POINT('Ctrl Pts',(0.00763870055875463,-0.033362046922432,
0.0684178323906018));
#98807=CARTESIAN_POINT('Ctrl Pts',(0.00775907055967907,-0.0331951640388602,
0.0684101840026268));
#98808=CARTESIAN_POINT('Ctrl Pts',(0.00788545141224616,-0.0330240426238155,
0.0684050475007324));
#98809=CARTESIAN_POINT('Ctrl Pts',(0.00796459372995917,-0.0329142774063509,
0.0684017642620316));
#98810=CARTESIAN_POINT('Ctrl Pts',(0.00804384337671913,-0.0328043479726686,
0.0684001154792969));
#98811=CARTESIAN_POINT('Ctrl Pts',(0.00812309888599626,-0.0326943950436594,
0.0684001060607139));
#98812=CARTESIAN_POINT('Ctrl Pts',(0.00780373890997204,-0.0330240426238155,
0.0683265350625032));
#98813=CARTESIAN_POINT('Ctrl Pts',(0.00788396281301261,-0.0329142774063509,
0.0683221261544749));
#98814=CARTESIAN_POINT('Ctrl Pts',(0.00796431785503927,-0.0328043479726686,
0.0683193735006156));
#98815=CARTESIAN_POINT('Ctrl Pts',(0.00804470119237377,-0.0326943950436594,
0.0683182834622508));
#98816=CARTESIAN_POINT('Ctrl Pts',(0.00772202640769792,-0.0330240426238155,
0.068248022624274));
#98817=CARTESIAN_POINT('Ctrl Pts',(0.00780333189606606,-0.0329142774063509,
0.0682424880469183));
#98818=CARTESIAN_POINT('Ctrl Pts',(0.00788479233335941,-0.0328043479726686,
0.0682386315219343));
#98819=CARTESIAN_POINT('Ctrl Pts',(0.00796630349875127,-0.0326943950436594,
0.0682364608637877));
#98820=CARTESIAN_POINT('Ctrl Pts',(0.0076403139054238,-0.0330240426238155,
0.0681695101860449));
#98821=CARTESIAN_POINT('Ctrl Pts',(0.0077227009791195,-0.0329142774063509,
0.0681628499393617));
#98822=CARTESIAN_POINT('Ctrl Pts',(0.00780526681167955,-0.0328043479726686,
0.0681578895432529));
#98823=CARTESIAN_POINT('Ctrl Pts',(0.00788790580512878,-0.0326943950436594,
0.0681546382653245));
#98824=CARTESIAN_POINT('Origin',(0.00805176743042016,-0.0326396682857536,
0.085199728886723));
#98825=CARTESIAN_POINT('Ctrl Pts',(0.00823919677064576,-0.0331951640388588,
0.0681511101464263));
#98826=CARTESIAN_POINT('Ctrl Pts',(0.00832181933892492,-0.033085561830543,
0.068152699748677));
#98827=CARTESIAN_POINT('Ctrl Pts',(0.00840446861429596,-0.0329757224528702,
0.0681559981640262));
#98828=CARTESIAN_POINT('Ctrl Pts',(0.0084870385522225,-0.0328657862230221,
0.0681610063601986));
#98829=CARTESIAN_POINT('Ctrl Pts',(0.00816245821433043,-0.0331951640388588,
0.0682344908756998));
#98830=CARTESIAN_POINT('Ctrl Pts',(0.00824393238179449,-0.033085561830543,
0.0682350235596266));
#98831=CARTESIAN_POINT('Ctrl Pts',(0.00832545427317847,-0.0329757224528702,
0.0682372405592537));
#98832=CARTESIAN_POINT('Ctrl Pts',(0.00840691935555694,-0.0328657862230221,
0.0682411441563076));
#98833=CARTESIAN_POINT('Ctrl Pts',(0.00808571965801511,-0.0331951640388588,
0.0683178716049733));
#98834=CARTESIAN_POINT('Ctrl Pts',(0.00816604542466406,-0.033085561830543,
0.0683173473705764));
#98835=CARTESIAN_POINT('Ctrl Pts',(0.00824643993206098,-0.0329757224528702,
0.0683184829544813));
#98836=CARTESIAN_POINT('Ctrl Pts',(0.00832680015889138,-0.0328657862230221,
0.0683212819524166));
#98837=CARTESIAN_POINT('Ctrl Pts',(0.00800898110169978,-0.0331951640388588,
0.0684012523342468));
#98838=CARTESIAN_POINT('Ctrl Pts',(0.00808815846753363,-0.033085561830543,
0.0683996711815261));
#98839=CARTESIAN_POINT('Ctrl Pts',(0.00816742559094349,-0.0329757224528702,
0.0683997253497088));
#98840=CARTESIAN_POINT('Ctrl Pts',(0.00824668096222582,-0.0328657862230221,
0.0684014197485256));
#98841=CARTESIAN_POINT('Origin',(0.0075726680375036,-0.0326401908834165,
0.0851580558324018));
#98842=CARTESIAN_POINT('Ctrl Pts',(0.00797425886923198,-0.0332451089994433,
0.0684005854406194));
#98843=CARTESIAN_POINT('Ctrl Pts',(0.00819110158707134,-0.0329451141710259,
0.0683949460761945));
#98844=CARTESIAN_POINT('Ctrl Pts',(0.00840775305761736,-0.0326442513127504,
0.0684056562125766));
#98845=CARTESIAN_POINT('Ctrl Pts',(0.0077245436624227,-0.0332451089994433,
0.0684125150461534));
#98846=CARTESIAN_POINT('Ctrl Pts',(0.00794093644782806,-0.0329451141710259,
0.0683974575186145));
#98847=CARTESIAN_POINT('Ctrl Pts',(0.00815784867869816,-0.0326442513127504,
0.0683987423571396));
#98848=CARTESIAN_POINT('Ctrl Pts',(0.00824664939475422,-0.0325229783203384,
0.0684014189839514));
#98849=CARTESIAN_POINT('Ctrl Pts',(0.00832589345690486,-0.0324130253112079,
0.0684031127056083));
#98850=CARTESIAN_POINT('Ctrl Pts',(0.00840509046333346,-0.0323031222247695,
0.068406445435571));
#98851=CARTESIAN_POINT('Ctrl Pts',(0.00848413911894741,-0.0321934096636184,
0.0684114093251639));
#98852=CARTESIAN_POINT('Ctrl Pts',(0.00817002793696981,-0.0325229783203384,
0.0683179306922193));
#98853=CARTESIAN_POINT('Ctrl Pts',(0.00825042288337526,-0.0324130253112079,
0.0683185681887754));
#98854=CARTESIAN_POINT('Ctrl Pts',(0.00833079244887716,-0.0323031222247695,
0.0683208686613535));
#98855=CARTESIAN_POINT('Ctrl Pts',(0.00841103378976034,-0.0321934096636184,
0.0683248255305266));
#98856=CARTESIAN_POINT('Ctrl Pts',(0.00809340647918541,-0.0325229783203384,
0.0682344424004872));
#98857=CARTESIAN_POINT('Ctrl Pts',(0.00817495230984567,-0.0324130253112079,
0.0682340236719426));
#98858=CARTESIAN_POINT('Ctrl Pts',(0.00825649443442085,-0.0323031222247695,
0.068235291887136));
#98859=CARTESIAN_POINT('Ctrl Pts',(0.00833792846057326,-0.0321934096636184,
0.0682382417358893));
#98860=CARTESIAN_POINT('Ctrl Pts',(0.008016785021401,-0.0325229783203384,
0.0681509541087551));
#98861=CARTESIAN_POINT('Ctrl Pts',(0.00809948173631607,-0.0324130253112079,
0.0681494791551098));
#98862=CARTESIAN_POINT('Ctrl Pts',(0.00818219641996455,-0.0323031222247695,
0.0681497151129185));
#98863=CARTESIAN_POINT('Ctrl Pts',(0.00826482313138619,-0.0321934096636184,
0.068151657941252));
#98864=CARTESIAN_POINT('Origin',(0.00805206138852261,-0.0326393375177959,
0.0851912080523513));
#98865=CARTESIAN_POINT('Ctrl Pts',(0.00861564243684593,-0.0326943950436593,
0.0681701945265211));
#98866=CARTESIAN_POINT('Ctrl Pts',(0.00869805536362011,-0.0325844576448127,
0.0681769732825241));
#98867=CARTESIAN_POINT('Ctrl Pts',(0.0087803339270971,-0.0324744968375319,
0.0681854569527138));
#98868=CARTESIAN_POINT('Ctrl Pts',(0.00886237285710993,-0.0323646534831895,
0.0681956332132571));
#98869=CARTESIAN_POINT('Ctrl Pts',(0.0085338198651545,-0.0326943950436593,
0.0682485921944925));
#98870=CARTESIAN_POINT('Ctrl Pts',(0.00861515232513115,-0.0325844576448127,
0.0682542432821058));
#98871=CARTESIAN_POINT('Ctrl Pts',(0.00869637366737543,-0.0324744968375319,
0.068261576858274));
#98872=CARTESIAN_POINT('Ctrl Pts',(0.00877737995596894,-0.0323646534831895,
0.0682705820914154));
#98873=CARTESIAN_POINT('Ctrl Pts',(0.00845199729346307,-0.0326943950436593,
0.0683269898624639));
#98874=CARTESIAN_POINT('Ctrl Pts',(0.00853224928664219,-0.0325844576448127,
0.0683315132816874));
#98875=CARTESIAN_POINT('Ctrl Pts',(0.00861241340765376,-0.0324744968375319,
0.0683376967638342));
#98876=CARTESIAN_POINT('Ctrl Pts',(0.00869238705482796,-0.0323646534831895,
0.0683455309695737));
#98877=CARTESIAN_POINT('Ctrl Pts',(0.00837017472177164,-0.0326943950436593,
0.0684053875304353));
#98878=CARTESIAN_POINT('Ctrl Pts',(0.00844934624815322,-0.0325844576448127,
0.0684087832812691));
#98879=CARTESIAN_POINT('Ctrl Pts',(0.00852845314793209,-0.0324744968375319,
0.0684138166693945));
#98880=CARTESIAN_POINT('Ctrl Pts',(0.00860739415368697,-0.0323646534831895,
0.068420479847732));
#98881=CARTESIAN_POINT('Origin',(0.00757123337387066,-0.0326395579068887,
0.0851958698995984));
#98882=CARTESIAN_POINT('Ctrl Pts',(0.00833552344979301,-0.0327445246961877,
0.0684025405055608));
#98883=CARTESIAN_POINT('Ctrl Pts',(0.00855229242606044,-0.0324436878365475,
0.0684105264575262));
#98884=CARTESIAN_POINT('Ctrl Pts',(0.00876784405003831,-0.0321434074463187,
0.0684348176473144));
#98885=CARTESIAN_POINT('Ctrl Pts',(0.008085551907043,-0.0327445246961877,
0.0683987685279387));
#98886=CARTESIAN_POINT('Ctrl Pts',(0.00830246314577066,-0.0324436878365475,
0.0683973266491432));
#98887=CARTESIAN_POINT('Ctrl Pts',(0.00851886677079367,-0.0321434074463187,
0.0684122275074315));
#98888=CARTESIAN_POINT('Ctrl Pts',(0.00870155650025176,-0.0322357242816073,
0.0684277363002037));
#98889=CARTESIAN_POINT('Ctrl Pts',(0.00888380317758615,-0.0319819883628706,
0.0684461376625405));
#98890=CARTESIAN_POINT('Ctrl Pts',(0.00906450957808754,-0.0317295851069886,
0.0684760986096733));
#98891=CARTESIAN_POINT('Ctrl Pts',(0.00845233410582779,-0.0322357242816073,
0.0684080335562937));
#98892=CARTESIAN_POINT('Ctrl Pts',(0.00863520829000221,-0.0319819883628706,
0.0684184975085977));
#98893=CARTESIAN_POINT('Ctrl Pts',(0.00881704600573044,-0.0317295851069886,
0.0684405770618994));
#98894=CARTESIAN_POINT('Origin',(0.00757769600471676,-0.0326371942646347,
0.0851007876301448));
#98895=CARTESIAN_POINT('Origin',(0.00805577218063784,-0.0326352985527098,
0.0850685294765079));
#98896=CARTESIAN_POINT('Ctrl Pts',(0.00899014695537443,-0.0321934096636184,
0.0682128784669059));
#98897=CARTESIAN_POINT('Ctrl Pts',(0.00907202448842683,-0.0320835708272304,
0.0682248263121812));
#98898=CARTESIAN_POINT('Ctrl Pts',(0.00915360726914559,-0.0319739230346346,
0.0682384616785115));
#98899=CARTESIAN_POINT('Ctrl Pts',(0.00923479225691667,-0.0318646057455575,
0.0682537591095561));
#98900=CARTESIAN_POINT('Ctrl Pts',(0.00890356308617857,-0.0321934096636184,
0.068285983859045));
#98901=CARTESIAN_POINT('Ctrl Pts',(0.00898443243889849,-0.0320835708272304,
0.0682967376452847));
#98902=CARTESIAN_POINT('Ctrl Pts',(0.00906503233506001,-0.0319739230346346,
0.0683091587809427));
#98903=CARTESIAN_POINT('Ctrl Pts',(0.00914526087235309,-0.0318646057455575,
0.0683232234597141));
#98904=CARTESIAN_POINT('Ctrl Pts',(0.0088169792169827,-0.0321934096636184,
0.0683590892511841));
#98905=CARTESIAN_POINT('Ctrl Pts',(0.00889684038937014,-0.0320835708272304,
0.0683686489783883));
#98906=CARTESIAN_POINT('Ctrl Pts',(0.00897645740097444,-0.0319739230346346,
0.0683798558833738));
#98907=CARTESIAN_POINT('Ctrl Pts',(0.00905572948778951,-0.0318646057455575,
0.068392687809872));
#98908=CARTESIAN_POINT('Ctrl Pts',(0.00873039534778683,-0.0321934096636184,
0.0684321946433232));
#98909=CARTESIAN_POINT('Ctrl Pts',(0.0088092483398418,-0.0320835708272304,
0.0684405603114918));
#98910=CARTESIAN_POINT('Ctrl Pts',(0.00888788246688886,-0.0319739230346346,
0.068450552985805));
#98911=CARTESIAN_POINT('Ctrl Pts',(0.00896619810322593,-0.0318646057455575,
0.06846215216003));
#98912=CARTESIAN_POINT('Ctrl Pts',(0.00860699565471972,-0.0320218834582337,
0.0684196158461317));
#98913=CARTESIAN_POINT('Ctrl Pts',(0.00866663510064553,-0.0319391099350648,
0.0684246449301059));
#98914=CARTESIAN_POINT('Ctrl Pts',(0.00872615988269489,-0.0318564869454945,
0.0684306022453965));
#98915=CARTESIAN_POINT('Ctrl Pts',(0.00878552705004609,-0.0317740741446553,
0.0684374794053147));
#98916=CARTESIAN_POINT('Ctrl Pts',(0.00857584241890168,-0.0320218834582337,
0.0683810632334404));
#98917=CARTESIAN_POINT('Ctrl Pts',(0.00863588310432525,-0.0319391099350648,
0.0683857680875422));
#98918=CARTESIAN_POINT('Ctrl Pts',(0.00869581394566648,-0.0318564869454945,
0.068391407634814));
#98919=CARTESIAN_POINT('Ctrl Pts',(0.00875559167473568,-0.0317740741446553,
0.0683979736924077));
#98920=CARTESIAN_POINT('Ctrl Pts',(0.00854468918308364,-0.0320218834582337,
0.0683425106207491));
#98921=CARTESIAN_POINT('Ctrl Pts',(0.00860513110800498,-0.0319391099350648,
0.0683468912449785));
#98922=CARTESIAN_POINT('Ctrl Pts',(0.00866546800863808,-0.0318564869454945,
0.0683522130242316));
#98923=CARTESIAN_POINT('Ctrl Pts',(0.00872565629942528,-0.0317740741446553,
0.0683584679795008));
#98924=CARTESIAN_POINT('Ctrl Pts',(0.00851353594726561,-0.0320218834582337,
0.0683039580080578));
#98925=CARTESIAN_POINT('Ctrl Pts',(0.00857437911168471,-0.0319391099350648,
0.0683080144024148));
#98926=CARTESIAN_POINT('Ctrl Pts',(0.00863512207160967,-0.0318564869454945,
0.0683130184136491));
#98927=CARTESIAN_POINT('Ctrl Pts',(0.00869572092411487,-0.0317740741446553,
0.0683189622665938));
#98928=CARTESIAN_POINT('Origin',(0.00819704568072141,-0.0391228853390677,
0.0620721172885788));
#98929=CARTESIAN_POINT('Ctrl Pts',(0.00562201316168811,-0.0352722978779565,
0.0689706838042051));
#98930=CARTESIAN_POINT('Ctrl Pts',(0.00563917834702537,-0.0352466642097198,
0.0689627813305198));
#98931=CARTESIAN_POINT('Ctrl Pts',(0.00565629545372585,-0.0352210183808291,
0.0689548146806992));
#98932=CARTESIAN_POINT('Ctrl Pts',(0.00567336486113266,-0.0351953608940152,
0.0689467830908172));
#98933=CARTESIAN_POINT('Origin',(0.00373885063905858,-0.0352456003065043,
0.0644470301804282));
#98934=CARTESIAN_POINT('Ctrl Pts',(0.00578732996892189,-0.035024121149334,
0.0688962136373421));
#98935=CARTESIAN_POINT('Ctrl Pts',(0.0058596987186681,-0.0349144232867421,
0.0688640299673878));
#98936=CARTESIAN_POINT('Ctrl Pts',(0.00593277604402248,-0.0348045283677512,
0.0688333229476583));
#98937=CARTESIAN_POINT('Ctrl Pts',(0.00600646980585258,-0.0346945769586886,
0.0688041353931166));
#98938=CARTESIAN_POINT('Ctrl Pts',(0.00568245322679813,-0.035024121149334,
0.0688532949844682));
#98939=CARTESIAN_POINT('Ctrl Pts',(0.00575541316336368,-0.0349144232867421,
0.0688196666804574));
#98940=CARTESIAN_POINT('Ctrl Pts',(0.00582911189100808,-0.0348045283677512,
0.0687875263822418));
#98941=CARTESIAN_POINT('Ctrl Pts',(0.00590345654297772,-0.0346945769586886,
0.0687569187702505));
#98942=CARTESIAN_POINT('Ctrl Pts',(0.00557757648467437,-0.035024121149334,
0.0688103763315943));
#98943=CARTESIAN_POINT('Ctrl Pts',(0.00565112760805927,-0.0349144232867421,
0.0687753033935271));
#98944=CARTESIAN_POINT('Ctrl Pts',(0.00572544773799369,-0.0348045283677512,
0.0687417298168253));
#98945=CARTESIAN_POINT('Ctrl Pts',(0.00580044328010287,-0.0346945769586886,
0.0687097021473843));
#98946=CARTESIAN_POINT('Ctrl Pts',(0.0054726997425506,-0.035024121149334,
0.0687674576787204));
#98947=CARTESIAN_POINT('Ctrl Pts',(0.00554684205275485,-0.0349144232867421,
0.0687309401065967));
#98948=CARTESIAN_POINT('Ctrl Pts',(0.00562178358497929,-0.0348045283677512,
0.0686959332514088));
#98949=CARTESIAN_POINT('Ctrl Pts',(0.00569743001722801,-0.0346945769586886,
0.0686624855245182));
#98950=CARTESIAN_POINT('Origin',(0.0120209044952922,-0.0345629067943303,
0.0844786218103012));
#98951=CARTESIAN_POINT('Ctrl Pts',(0.00598812243932284,-0.0351970973651659,
0.0686169647395614));
#98952=CARTESIAN_POINT('Ctrl Pts',(0.00606477514426711,-0.03508693493218,
0.0685873780680036));
#98953=CARTESIAN_POINT('Ctrl Pts',(0.0061421064379258,-0.0349764985129734,
0.0685593604544486));
#98954=CARTESIAN_POINT('Ctrl Pts',(0.0062200182720283,-0.0348659306849638,
0.0685329540940108));
#98955=CARTESIAN_POINT('Ctrl Pts',(0.00595864267170211,-0.0351970973651659,
0.0686937202862751));
#98956=CARTESIAN_POINT('Ctrl Pts',(0.00603423203256883,-0.03508693493218,
0.0686637252124891));
#98957=CARTESIAN_POINT('Ctrl Pts',(0.00611050759174411,-0.0349764985129734,
0.0686352767520561));
#98958=CARTESIAN_POINT('Ctrl Pts',(0.0061873727015498,-0.0348659306849638,
0.0686084175777525));
#98959=CARTESIAN_POINT('Ctrl Pts',(0.00592916290408138,-0.0351970973651659,
0.0687704758329889));
#98960=CARTESIAN_POINT('Ctrl Pts',(0.00600368892087055,-0.03508693493218,
0.0687400723569746));
#98961=CARTESIAN_POINT('Ctrl Pts',(0.00607890874556241,-0.0349764985129734,
0.0687111930496637));
#98962=CARTESIAN_POINT('Ctrl Pts',(0.00615472713107129,-0.0348659306849638,
0.0686838810614941));
#98963=CARTESIAN_POINT('Ctrl Pts',(0.00589968313646066,-0.0351970973651659,
0.0688472313797026));
#98964=CARTESIAN_POINT('Ctrl Pts',(0.00597314580917227,-0.03508693493218,
0.0688164195014601));
#98965=CARTESIAN_POINT('Ctrl Pts',(0.00604730989938071,-0.0349764985129734,
0.0687871093472712));
#98966=CARTESIAN_POINT('Ctrl Pts',(0.00612208156059279,-0.0348659306849638,
0.0687593445452358));
#98967=CARTESIAN_POINT('Origin',(0.0115568720158949,-0.034563718796663,
0.0846051098115322));
#98968=CARTESIAN_POINT('Ctrl Pts',(0.00586826380884067,-0.0352450361861252,
0.0688593703760109));
#98969=CARTESIAN_POINT('Ctrl Pts',(0.00606780317426413,-0.0349452761023764,
0.0687743021064317));
#98970=CARTESIAN_POINT('Ctrl Pts',(0.0062731833593555,-0.0346444289983475,
0.0687045056279055));
#98971=CARTESIAN_POINT('Ctrl Pts',(0.005640475954028,-0.0352450361861252,
0.0689623883026054));
#98972=CARTESIAN_POINT('Ctrl Pts',(0.00583612993469371,-0.0349452761023764,
0.0688687288733285));
#98973=CARTESIAN_POINT('Ctrl Pts',(0.00603828289427984,-0.0346444289983475,
0.0687900729786137));
#98974=CARTESIAN_POINT('Ctrl Pts',(0.00612182746827824,-0.0345231616327822,
0.068759874023479));
#98975=CARTESIAN_POINT('Ctrl Pts',(0.00619612276617375,-0.0344132092796975,
0.0687322798961242));
#98976=CARTESIAN_POINT('Ctrl Pts',(0.00627098499353181,-0.0343032738558974,
0.0687062239321332));
#98977=CARTESIAN_POINT('Ctrl Pts',(0.00634631738812818,-0.0341934961088741,
0.0686817370555091));
#98978=CARTESIAN_POINT('Ctrl Pts',(0.00601985257553799,-0.0345231616327822,
0.0687104548228676));
#98979=CARTESIAN_POINT('Ctrl Pts',(0.00609482904753725,-0.0344132092796975,
0.0686814551151856));
#98980=CARTESIAN_POINT('Ctrl Pts',(0.00617040148717397,-0.0343032738558974,
0.0686540077329378));
#98981=CARTESIAN_POINT('Ctrl Pts',(0.00624647217669877,-0.0341934961088741,
0.0686281453593886));
#98982=CARTESIAN_POINT('Ctrl Pts',(0.00591787768279773,-0.0345231616327822,
0.0686610356222562));
#98983=CARTESIAN_POINT('Ctrl Pts',(0.00599353532890075,-0.0344132092796975,
0.0686306303342469));
#98984=CARTESIAN_POINT('Ctrl Pts',(0.00606981798081613,-0.0343032738558974,
0.0686017915337425));
#98985=CARTESIAN_POINT('Ctrl Pts',(0.00614662696526936,-0.0341934961088741,
0.0685745536632681));
#98986=CARTESIAN_POINT('Ctrl Pts',(0.00581590279005748,-0.0345231616327822,
0.0686116164216449));
#98987=CARTESIAN_POINT('Ctrl Pts',(0.00589224161026425,-0.0344132092796975,
0.0685798055533083));
#98988=CARTESIAN_POINT('Ctrl Pts',(0.0059692344744583,-0.0343032738558974,
0.0685495753345471));
#98989=CARTESIAN_POINT('Ctrl Pts',(0.00604678175383996,-0.0341934961088741,
0.0685209619671476));
#98990=CARTESIAN_POINT('Origin',(0.0120254107912183,-0.0345625596229832,
0.0844898553130019));
#98991=CARTESIAN_POINT('Ctrl Pts',(0.00637978906701317,-0.0346945769586885,
0.0684090516483639));
#98992=CARTESIAN_POINT('Ctrl Pts',(0.00645890223700392,-0.0345846629176689,
0.0683850185416024));
#98993=CARTESIAN_POINT('Ctrl Pts',(0.00653852591449628,-0.0344746925051586,
0.0683626173577916));
#98994=CARTESIAN_POINT('Ctrl Pts',(0.00661855795792006,-0.0343648066255171,
0.0683418763785691));
#98995=CARTESIAN_POINT('Ctrl Pts',(0.0063325724813239,-0.0346945769586885,
0.0685120648301294));
#98996=CARTESIAN_POINT('Ctrl Pts',(0.00641026607760293,-0.0345846629176689,
0.0684873810549519));
#98997=CARTESIAN_POINT('Ctrl Pts',(0.00648848339447251,-0.0344746925051586,
0.0684642997353881));
#98998=CARTESIAN_POINT('Ctrl Pts',(0.00656712408875471,-0.0343648066255171,
0.0684428500319857));
#98999=CARTESIAN_POINT('Ctrl Pts',(0.00628535589563463,-0.0346945769586885,
0.068615078011895));
#99000=CARTESIAN_POINT('Ctrl Pts',(0.00636162991820194,-0.034584662917669,
0.0685897435683015));
#99001=CARTESIAN_POINT('Ctrl Pts',(0.00643844087444875,-0.0344746925051586,
0.0685659821129846));
#99002=CARTESIAN_POINT('Ctrl Pts',(0.00651569021958936,-0.0343648066255171,
0.0685438236854023));
#99003=CARTESIAN_POINT('Ctrl Pts',(0.00623813930994536,-0.0346945769586885,
0.0687180911936605));
#99004=CARTESIAN_POINT('Ctrl Pts',(0.00631299375880095,-0.034584662917669,
0.068692106081651));
#99005=CARTESIAN_POINT('Ctrl Pts',(0.00638839835442498,-0.0344746925051586,
0.0686676644905811));
#99006=CARTESIAN_POINT('Ctrl Pts',(0.00646425635042401,-0.0343648066255171,
0.0686447973388189));
#99007=CARTESIAN_POINT('Origin',(0.0115758390175073,-0.0345626446731051,
0.0846603762881038));
#99008=CARTESIAN_POINT('Ctrl Pts',(0.00623898417299243,-0.0346945769586885,
0.0687162479424096));
#99009=CARTESIAN_POINT('Ctrl Pts',(0.00635279628539246,-0.034527515336289,
0.068676770093247));
#99010=CARTESIAN_POINT('Ctrl Pts',(0.00646787937745356,-0.0343603235965159,
0.0686408613192686));
#99011=CARTESIAN_POINT('Ctrl Pts',(0.00658389150603351,-0.034193496108874,
0.0686086227639818));
#99012=CARTESIAN_POINT('Ctrl Pts',(0.00616039616693489,-0.0346945769586885,
0.0687454361872211));
#99013=CARTESIAN_POINT('Ctrl Pts',(0.00627359691986101,-0.034527515336289,
0.0687043122808066));
#99014=CARTESIAN_POINT('Ctrl Pts',(0.00638812026130482,-0.0343603235965159,
0.068666737797129));
#99015=CARTESIAN_POINT('Ctrl Pts',(0.00650362583039834,-0.034193496108874,
0.0686328188307304));
#99016=CARTESIAN_POINT('Ctrl Pts',(0.00608180816087734,-0.0346945769586885,
0.0687746244320324));
#99017=CARTESIAN_POINT('Ctrl Pts',(0.00619439755432957,-0.034527515336289,
0.0687318544683663));
#99018=CARTESIAN_POINT('Ctrl Pts',(0.00630836114515607,-0.0343603235965159,
0.0686926142749894));
#99019=CARTESIAN_POINT('Ctrl Pts',(0.00642336015476317,-0.034193496108874,
0.0686570148974789));
#99020=CARTESIAN_POINT('Ctrl Pts',(0.0060032201548198,-0.0346945769586885,
0.0688038126768439));
#99021=CARTESIAN_POINT('Ctrl Pts',(0.00611519818879812,-0.034527515336289,
0.0687593966559259));
#99022=CARTESIAN_POINT('Ctrl Pts',(0.00622860202900733,-0.0343603235965159,
0.0687184907528498));
#99023=CARTESIAN_POINT('Ctrl Pts',(0.006343094479128,-0.034193496108874,
0.0686812109642275));
#99024=CARTESIAN_POINT('Ctrl Pts',(0.00646422629977976,-0.0340223579322365,
0.0686448069791245));
#99025=CARTESIAN_POINT('Ctrl Pts',(0.00654015726968307,-0.0339125849573554,
0.0686219173750522));
#99026=CARTESIAN_POINT('Ctrl Pts',(0.00661650864538917,-0.0338030433565221,
0.0686006154498775));
#99027=CARTESIAN_POINT('Ctrl Pts',(0.0066931803715077,-0.0336938721132327,
0.0685809197897488));
#99028=CARTESIAN_POINT('Ctrl Pts',(0.00636555551167844,-0.0340223579322365,
0.0685890821605443));
#99029=CARTESIAN_POINT('Ctrl Pts',(0.00644225507216639,-0.0339125849573554,
0.0685648316289599));
#99030=CARTESIAN_POINT('Ctrl Pts',(0.00651940266641457,-0.0338030433565221,
0.0685421856406203));
#99031=CARTESIAN_POINT('Ctrl Pts',(0.00659689706843624,-0.0336938721132327,
0.0685211644102423));
#99032=CARTESIAN_POINT('Ctrl Pts',(0.00626688472357712,-0.0340223579322365,
0.0685333573419642));
#99033=CARTESIAN_POINT('Ctrl Pts',(0.00634435287464971,-0.0339125849573554,
0.0685077458828677));
#99034=CARTESIAN_POINT('Ctrl Pts',(0.00642229668743997,-0.0338030433565221,
0.068483755831363));
#99035=CARTESIAN_POINT('Ctrl Pts',(0.00650061376536478,-0.0336938721132327,
0.0684614090307357));
#99036=CARTESIAN_POINT('Ctrl Pts',(0.0061682139354758,-0.0340223579322365,
0.0684776325233841));
#99037=CARTESIAN_POINT('Ctrl Pts',(0.00624645067713303,-0.0339125849573554,
0.0684506601367754));
#99038=CARTESIAN_POINT('Ctrl Pts',(0.00632519070846537,-0.0338030433565221,
0.0684253260221058));
#99039=CARTESIAN_POINT('Ctrl Pts',(0.00640433046229332,-0.0336938721132327,
0.0684016536512291));
#99040=CARTESIAN_POINT('Origin',(0.0119854038397793,-0.0345589643416696,
0.0843764872320283));
#99041=CARTESIAN_POINT('Ctrl Pts',(0.00674370756866029,-0.0341934961088739,
0.0683108738640981));
#99042=CARTESIAN_POINT('Ctrl Pts',(0.00682422565995426,-0.0340836138585568,
0.0682918434523519));
#99043=CARTESIAN_POINT('Ctrl Pts',(0.00690509891159273,-0.033973889665241,
0.0682744883246977));
#99044=CARTESIAN_POINT('Ctrl Pts',(0.00698622232679418,-0.0338644633307392,
0.0682588237549221));
#99045=CARTESIAN_POINT('Ctrl Pts',(0.00669011582431903,-0.0341934961088739,
0.0684107191653662));
#99046=CARTESIAN_POINT('Ctrl Pts',(0.00676925710804014,-0.0340836138585568,
0.0683909497552044));
#99047=CARTESIAN_POINT('Ctrl Pts',(0.00684876950474543,-0.033973889665241,
0.0683728274935761));
#99048=CARTESIAN_POINT('Ctrl Pts',(0.00692854969356229,-0.0338644633307392,
0.0683563687528613));
#99049=CARTESIAN_POINT('Ctrl Pts',(0.00663652407997777,-0.0341934961088739,
0.0685105644666344));
#99050=CARTESIAN_POINT('Ctrl Pts',(0.00671428855612601,-0.0340836138585568,
0.0684900560580568));
#99051=CARTESIAN_POINT('Ctrl Pts',(0.00679244009789812,-0.033973889665241,
0.0684711666624546));
#99052=CARTESIAN_POINT('Ctrl Pts',(0.0068708770603304,-0.0338644633307392,
0.0684539137508006));
#99053=CARTESIAN_POINT('Ctrl Pts',(0.00658293233563651,-0.0341934961088739,
0.0686104097679026));
#99054=CARTESIAN_POINT('Ctrl Pts',(0.00665932000421189,-0.0340836138585568,
0.0685891623609093));
#99055=CARTESIAN_POINT('Ctrl Pts',(0.00673611069105082,-0.033973889665241,
0.068569505831333));
#99056=CARTESIAN_POINT('Ctrl Pts',(0.00681320442709851,-0.0338644633307392,
0.0685514587487399));
#99057=CARTESIAN_POINT('Origin',(0.0115534361909259,-0.0345610621862693,
0.0845885107262112));
#99058=CARTESIAN_POINT('Ctrl Pts',(0.00654906546133213,-0.03424362768739,
0.0686184186515369));
#99059=CARTESIAN_POINT('Ctrl Pts',(0.00675769249114546,-0.033943005420186,
0.0685590272309192));
#99060=CARTESIAN_POINT('Ctrl Pts',(0.00697020043858811,-0.0336441434784161,
0.068515519177809));
#99061=CARTESIAN_POINT('Ctrl Pts',(0.00631016321730991,-0.03424362768739,
0.0686920781234407));
#99062=CARTESIAN_POINT('Ctrl Pts',(0.00651601213434268,-0.033943005420186,
0.0686236763561524));
#99063=CARTESIAN_POINT('Ctrl Pts',(0.0067264285575619,-0.0336441434784161,
0.0685709742949843));
#99064=CARTESIAN_POINT('Ctrl Pts',(0.00681317745579414,-0.0335235895815127,
0.0685514651925706));
#99065=CARTESIAN_POINT('Ctrl Pts',(0.00689025230991804,-0.0334144449262719,
0.0685334221380184));
#99066=CARTESIAN_POINT('Ctrl Pts',(0.00696778846963959,-0.0333049234473133,
0.0685169506626634));
#99067=CARTESIAN_POINT('Ctrl Pts',(0.00704568869789882,-0.0331951640388588,
0.0685020808094435));
#99068=CARTESIAN_POINT('Ctrl Pts',(0.00671820041761043,-0.0335235895815127,
0.0684896547185057));
#99069=CARTESIAN_POINT('Ctrl Pts',(0.00679612621460344,-0.0334144449262719,
0.0684703041180303));
#99070=CARTESIAN_POINT('Ctrl Pts',(0.0068745413077391,-0.0333049234473133,
0.0684525411743796));
#99071=CARTESIAN_POINT('Ctrl Pts',(0.00695334748566163,-0.0331951640388588,
0.0684363976836892));
#99072=CARTESIAN_POINT('Ctrl Pts',(0.00662322337942671,-0.0335235895815127,
0.0684278442444407));
#99073=CARTESIAN_POINT('Ctrl Pts',(0.00670200011928885,-0.0334144449262719,
0.0684071860980422));
#99074=CARTESIAN_POINT('Ctrl Pts',(0.00678129414583862,-0.0333049234473133,
0.0683881316860958));
#99075=CARTESIAN_POINT('Ctrl Pts',(0.00686100627342445,-0.0331951640388588,
0.068370714557935));
#99076=CARTESIAN_POINT('Ctrl Pts',(0.006528246341243,-0.0335235895815127,
0.0683660337703758));
#99077=CARTESIAN_POINT('Ctrl Pts',(0.00660787402397425,-0.0334144449262719,
0.0683440680780541));
#99078=CARTESIAN_POINT('Ctrl Pts',(0.00668804698393813,-0.0333049234473133,
0.0683237221978119));
#99079=CARTESIAN_POINT('Ctrl Pts',(0.00676866506118727,-0.0331951640388588,
0.0683050314321807));
#99080=CARTESIAN_POINT('Origin',(0.00941982341379305,-0.0326434571770007,
0.0849991813247499));
#99081=CARTESIAN_POINT('Ctrl Pts',(0.00711414177341354,-0.0336938721132353,
0.0682340176844868));
#99082=CARTESIAN_POINT('Ctrl Pts',(0.00714876998103594,-0.033647456976494,
0.0682281079240763));
#99083=CARTESIAN_POINT('Ctrl Pts',(0.00718346499711866,-0.033601104548885,
0.068222603935498));
#99084=CARTESIAN_POINT('Ctrl Pts',(0.00727130479332956,-0.0334837508694588,
0.0682086691030741));
#99085=CARTESIAN_POINT('Ctrl Pts',(0.0073595189347229,-0.0333660264863561,
0.0681973432648582));
#99086=CARTESIAN_POINT('Ctrl Pts',(0.00693487608410553,-0.0336938721132353,
0.0685228668698905));
#99087=CARTESIAN_POINT('Ctrl Pts',(0.00696781356159551,-0.033647456976494,
0.0685159078079139));
#99088=CARTESIAN_POINT('Ctrl Pts',(0.00700083024679538,-0.033601104548885,
0.0685093347975374));
#99089=CARTESIAN_POINT('Ctrl Pts',(0.00708442089545231,-0.0334837508694588,
0.0684926934479388));
#99090=CARTESIAN_POINT('Ctrl Pts',(0.00716846795491225,-0.0333660264863561,
0.0684785363700099));
#99091=CARTESIAN_POINT('Ctrl Pts',(0.00693487608411741,-0.0336938721132426,
0.0685228668699001));
#99092=CARTESIAN_POINT('Ctrl Pts',(0.00696781356160645,-0.0336474569765026,
0.0685159078079236));
#99093=CARTESIAN_POINT('Ctrl Pts',(0.00700083024680538,-0.0336011045488949,
0.0685093347975474));
#99094=CARTESIAN_POINT('Ctrl Pts',(0.00708372469920354,-0.033484728265791,
0.0684928320477266));
#99095=CARTESIAN_POINT('Ctrl Pts',(0.00716706829378607,-0.0333679870047996,
0.0684787723097453));
#99096=CARTESIAN_POINT('Ctrl Pts',(0.00693487608410046,-0.0336938721132425,
0.0685228668698915));
#99097=CARTESIAN_POINT('Ctrl Pts',(0.00705267507989257,-0.0335278710435082,
0.068497978184571));
#99098=CARTESIAN_POINT('Ctrl Pts',(0.00717121313697226,-0.0333620469224319,
0.0684767924009128));
#99099=CARTESIAN_POINT('Ctrl Pts',(0.00729055273143295,-0.0331951640388601,
0.0684593186994704));
#99100=CARTESIAN_POINT('Ctrl Pts',(0.00685324950217514,-0.0336938721132425,
0.0685419752697843));
#99101=CARTESIAN_POINT('Ctrl Pts',(0.00697064848071752,-0.0335278710435082,
0.068515377805027));
#99102=CARTESIAN_POINT('Ctrl Pts',(0.00708884024815148,-0.0333620469224319,
0.0684924712986398));
#99103=CARTESIAN_POINT('Ctrl Pts',(0.00720788739456458,-0.0331951640388601,
0.0684732640178144));
#99104=CARTESIAN_POINT('Ctrl Pts',(0.00677162292024982,-0.0336938721132425,
0.0685610836696771));
#99105=CARTESIAN_POINT('Ctrl Pts',(0.00688862188154248,-0.0335278710435082,
0.068532777425483));
#99106=CARTESIAN_POINT('Ctrl Pts',(0.0070064673593307,-0.0333620469224319,
0.0685081501963667));
#99107=CARTESIAN_POINT('Ctrl Pts',(0.00712522205769621,-0.0331951640388601,
0.0684872093361583));
#99108=CARTESIAN_POINT('Ctrl Pts',(0.0066899963383245,-0.0336938721132425,
0.0685801920695698));
#99109=CARTESIAN_POINT('Ctrl Pts',(0.00680659528236743,-0.0335278710435082,
0.068550177045939));
#99110=CARTESIAN_POINT('Ctrl Pts',(0.00692409447050992,-0.0333620469224319,
0.0685238290940936));
#99111=CARTESIAN_POINT('Ctrl Pts',(0.00704255672082784,-0.0331951640388601,
0.0685011546545022));
#99112=CARTESIAN_POINT('Ctrl Pts',(0.0071672972482326,-0.0330240426238155,
0.0684802189345466));
#99113=CARTESIAN_POINT('Ctrl Pts',(0.00724540400620885,-0.0329142774063509,
0.0684670424225728));
#99114=CARTESIAN_POINT('Ctrl Pts',(0.00732382209856182,-0.0328043479726686,
0.0684554740264952));
#99115=CARTESIAN_POINT('Ctrl Pts',(0.00740245147401439,-0.0326943950436593,
0.0684455313329251));
#99116=CARTESIAN_POINT('Ctrl Pts',(0.00707638885568696,-0.0330240426238155,
0.068412566882476));
#99117=CARTESIAN_POINT('Ctrl Pts',(0.00715542758659068,-0.0329142774063509,
0.0683981380188272));
#99118=CARTESIAN_POINT('Ctrl Pts',(0.007234804006101,-0.0328043479726686,
0.0683853359132153));
#99119=CARTESIAN_POINT('Ctrl Pts',(0.00731441687877833,-0.0326943950436594,
0.0683741797665357));
#99120=CARTESIAN_POINT('Ctrl Pts',(0.00698548046314132,-0.0330240426238155,
0.0683449148304054));
#99121=CARTESIAN_POINT('Ctrl Pts',(0.0070654511669725,-0.0329142774063509,
0.0683292336150816));
#99122=CARTESIAN_POINT('Ctrl Pts',(0.00714578591364018,-0.0328043479726686,
0.0683151977999353));
#99123=CARTESIAN_POINT('Ctrl Pts',(0.00722638228354226,-0.0326943950436594,
0.0683028282001464));
#99124=CARTESIAN_POINT('Ctrl Pts',(0.00689457207059568,-0.0330240426238155,
0.0682772627783349));
#99125=CARTESIAN_POINT('Ctrl Pts',(0.00697547474735433,-0.0329142774063509,
0.0682603292113359));
#99126=CARTESIAN_POINT('Ctrl Pts',(0.00705676782117937,-0.0328043479726686,
0.0682450596866554));
#99127=CARTESIAN_POINT('Ctrl Pts',(0.0071383476883062,-0.0326943950436594,
0.068231476633757));
#99128=CARTESIAN_POINT('Origin',(0.00943723353963632,-0.0326396682857081,
0.0851216243169898));
#99129=CARTESIAN_POINT('Ctrl Pts',(0.00748642642908473,-0.0331951640388588,
0.0681839479025));
#99130=CARTESIAN_POINT('Ctrl Pts',(0.00756859672750268,-0.0330855618255041,
0.0681751696162108));
#99131=CARTESIAN_POINT('Ctrl Pts',(0.00765100769351245,-0.0329757224427708,
0.0681680833213879));
#99132=CARTESIAN_POINT('Ctrl Pts',(0.00773355424004404,-0.0328657862078596,
0.0681627032690316));
#99133=CARTESIAN_POINT('Ctrl Pts',(0.00742074335562341,-0.0331951640388588,
0.0682762890412207));
#99134=CARTESIAN_POINT('Ctrl Pts',(0.00750164184166008,-0.0330855618255041,
0.0682666061034703));
#99135=CARTESIAN_POINT('Ctrl Pts',(0.00758279877605615,-0.0329757224427708,
0.0682585882188477));
#99136=CARTESIAN_POINT('Ctrl Pts',(0.00766411073612138,-0.0328657862078596,
0.0682522507525389));
#99137=CARTESIAN_POINT('Ctrl Pts',(0.00735506028216208,-0.0331951640388588,
0.0683686301799413));
#99138=CARTESIAN_POINT('Ctrl Pts',(0.00743468695581749,-0.0330855618255041,
0.0683580425907298));
#99139=CARTESIAN_POINT('Ctrl Pts',(0.00751458985859985,-0.0329757224427708,
0.0683490931163075));
#99140=CARTESIAN_POINT('Ctrl Pts',(0.00759466723219872,-0.0328657862078596,
0.0683417982360462));
#99141=CARTESIAN_POINT('Ctrl Pts',(0.00728937720870076,-0.0331951640388588,
0.068460971318662));
#99142=CARTESIAN_POINT('Ctrl Pts',(0.00736773206997489,-0.0330855618255041,
0.0684494790779893));
#99143=CARTESIAN_POINT('Ctrl Pts',(0.00744638094114354,-0.0329757224427708,
0.0684395980137673));
#99144=CARTESIAN_POINT('Ctrl Pts',(0.00752522372827606,-0.0328657862078596,
0.0684313457195535));
#99145=CARTESIAN_POINT('Origin',(0.00895668896995906,-0.0326401908832491,
0.0851403269451843));
#99146=CARTESIAN_POINT('Ctrl Pts',(0.00725484518747234,-0.0332451089994432,
0.0684646615333617));
#99147=CARTESIAN_POINT('Ctrl Pts',(0.00746927123593514,-0.0329451141710258,
0.0684318890380081));
#99148=CARTESIAN_POINT('Ctrl Pts',(0.00768555668094991,-0.0326442513127503,
0.0684153610924057));
#99149=CARTESIAN_POINT('Ctrl Pts',(0.0070085942356918,-0.0332451089994432,
0.0685077946847324));
#99150=CARTESIAN_POINT('Ctrl Pts',(0.00722139349073491,-0.0329451141710258,
0.0684657346827808));
#99151=CARTESIAN_POINT('Ctrl Pts',(0.007436756336843,-0.0326442513127503,
0.0684398230786758));
#99152=CARTESIAN_POINT('Ctrl Pts',(0.00752519230302276,-0.0325229783203385,
0.0684313489185996));
#99153=CARTESIAN_POINT('Ctrl Pts',(0.00760402378168633,-0.0324130253112079,
0.0684230973702052));
#99154=CARTESIAN_POINT('Ctrl Pts',(0.00768301399788709,-0.0323031222247695,
0.0684164778036925));
#99155=CARTESIAN_POINT('Ctrl Pts',(0.00776206147157459,-0.0321934096636184,
0.0684114951279163));
#99156=CARTESIAN_POINT('Ctrl Pts',(0.00743871117075113,-0.0325229783203385,
0.068358122172049));
#99157=CARTESIAN_POINT('Ctrl Pts',(0.00751855207849617,-0.0324130253112079,
0.0683486784831592));
#99158=CARTESIAN_POINT('Ctrl Pts',(0.00759857623163581,-0.0323031222247695,
0.0683408878382994));
#99159=CARTESIAN_POINT('Ctrl Pts',(0.00767868077278747,-0.0321934096636184,
0.0683347565996588));
#99160=CARTESIAN_POINT('Ctrl Pts',(0.00735223003847951,-0.0325229783203385,
0.0682848954254985));
#99161=CARTESIAN_POINT('Ctrl Pts',(0.00743308037530601,-0.0324130253112079,
0.0682742595961133));
#99162=CARTESIAN_POINT('Ctrl Pts',(0.00751413846538452,-0.0323031222247695,
0.0682652978729063));
#99163=CARTESIAN_POINT('Ctrl Pts',(0.00759530007400035,-0.0321934096636184,
0.0682580180714012));
#99164=CARTESIAN_POINT('Ctrl Pts',(0.00726574890620788,-0.0325229783203385,
0.0682116686789479));
#99165=CARTESIAN_POINT('Ctrl Pts',(0.00734760867211584,-0.0324130253112079,
0.0681998407090673));
#99166=CARTESIAN_POINT('Ctrl Pts',(0.00742970069913324,-0.0323031222247695,
0.0681897079075132));
#99167=CARTESIAN_POINT('Ctrl Pts',(0.00751191937521324,-0.0321934096636184,
0.0681812795431437));
#99168=CARTESIAN_POINT('Origin',(0.00943645723634511,-0.0326393375179207,
0.0851131338295842));
#99169=CARTESIAN_POINT('Ctrl Pts',(0.00786229561583585,-0.0326943950436593,
0.0681557006439515));
#99170=CARTESIAN_POINT('Ctrl Pts',(0.00794490829547628,-0.0325844576448126,
0.0681520968688386));
#99171=CARTESIAN_POINT('Ctrl Pts',(0.00802760135372221,-0.0324744968375318,
0.0681502014043413));
#99172=CARTESIAN_POINT('Ctrl Pts',(0.00811026880590754,-0.0323646534831894,
0.068150015217654));
#99173=CARTESIAN_POINT('Ctrl Pts',(0.00779094407279218,-0.0326943950436593,
0.0682437352103833));
#99174=CARTESIAN_POINT('Ctrl Pts',(0.00787234347111283,-0.0325844576448126,
0.0682391480772802));
#99175=CARTESIAN_POINT('Ctrl Pts',(0.00795384349962864,-0.0324744968375318,
0.0682362440925521));
#99176=CARTESIAN_POINT('Ctrl Pts',(0.0080353396844298,-0.0323646534831894,
0.0682350255366519));
#99177=CARTESIAN_POINT('Ctrl Pts',(0.00771959252974852,-0.0326943950436593,
0.0683317697768151));
#99178=CARTESIAN_POINT('Ctrl Pts',(0.00779977864674937,-0.0325844576448126,
0.0683261992857219));
#99179=CARTESIAN_POINT('Ctrl Pts',(0.00788008564553506,-0.0324744968375318,
0.0683222867807628));
#99180=CARTESIAN_POINT('Ctrl Pts',(0.00796041056295206,-0.0323646534831894,
0.0683200358556498));
#99181=CARTESIAN_POINT('Ctrl Pts',(0.00764824098670485,-0.0326943950436593,
0.0684198043432469));
#99182=CARTESIAN_POINT('Ctrl Pts',(0.00772721382238591,-0.0325844576448126,
0.0684132504941635));
#99183=CARTESIAN_POINT('Ctrl Pts',(0.00780632779144149,-0.0324744968375318,
0.0684083294689736));
#99184=CARTESIAN_POINT('Ctrl Pts',(0.00788548144147433,-0.0323646534831894,
0.0684050461746477));
#99185=CARTESIAN_POINT('Origin',(0.00896000497826417,-0.0326395579068352,
0.0851780226454139));
#99186=CARTESIAN_POINT('Ctrl Pts',(0.00761350612352206,-0.0327445246961877,
0.0684213227239782));
#99187=CARTESIAN_POINT('Ctrl Pts',(0.00782956671684877,-0.0324436878365475,
0.0684020773475949));
#99188=CARTESIAN_POINT('Ctrl Pts',(0.00804646314525272,-0.0321434074463187,
0.0683991612120631));
#99189=CARTESIAN_POINT('Ctrl Pts',(0.00736503292689721,-0.0327445246961877,
0.0684489102312782));
#99190=CARTESIAN_POINT('Ctrl Pts',(0.0075800530403874,-0.0324436878365475,
0.0684202935351815));
#99191=CARTESIAN_POINT('Ctrl Pts',(0.00779661783094262,-0.0321434074463187,
0.0684079543296724));
#99192=CARTESIAN_POINT('Ctrl Pts',(0.00797981580823882,-0.0322357172926635,
0.0684004436101531));
#99193=CARTESIAN_POINT('Ctrl Pts',(0.00816290150188186,-0.0319820232604284,
0.06839585922422));
#99194=CARTESIAN_POINT('Ctrl Pts',(0.00834590794153078,-0.0317296613809579,
0.0684029324736967));
#99195=CARTESIAN_POINT('Ctrl Pts',(0.00773008918797611,-0.0322357172926635,
0.0684121318577619));
#99196=CARTESIAN_POINT('Ctrl Pts',(0.00791280268752697,-0.0319820232604284,
0.0683995953154551));
#99197=CARTESIAN_POINT('Ctrl Pts',(0.00809594362225033,-0.0317296613809579,
0.068398708839402));
#99198=CARTESIAN_POINT('Origin',(0.00895449968112472,-0.0326371942645948,
0.0850828801466654));
#99199=CARTESIAN_POINT('Origin',(0.00942476306524877,-0.0326352985529246,
0.0849909575247938));
#99200=CARTESIAN_POINT('Ctrl Pts',(0.00823919677064608,-0.0321934096636183,
0.0681511101464259));
#99201=CARTESIAN_POINT('Ctrl Pts',(0.00832192613697718,-0.0320835708272303,
0.0681527018033987));
#99202=CARTESIAN_POINT('Ctrl Pts',(0.00840457457765538,-0.0319739230346346,
0.0681560046170822));
#99203=CARTESIAN_POINT('Ctrl Pts',(0.00848703667404713,-0.0318646057455575,
0.0681610062462797));
#99204=CARTESIAN_POINT('Ctrl Pts',(0.00816245817630805,-0.0321934096636183,
0.0682344909170132));
#99205=CARTESIAN_POINT('Ctrl Pts',(0.00824403765682973,-0.0320835708272303,
0.0682350242889637));
#99206=CARTESIAN_POINT('Ctrl Pts',(0.00832555877983254,-0.0319739230346346,
0.0682372456346461));
#99207=CARTESIAN_POINT('Ctrl Pts',(0.00840691746281541,-0.0318646057455575,
0.0682411441072214));
#99208=CARTESIAN_POINT('Ctrl Pts',(0.00808571958197001,-0.0321934096636183,
0.0683178716876005));
#99209=CARTESIAN_POINT('Ctrl Pts',(0.00816614917668227,-0.0320835708272303,
0.0683173467745287));
#99210=CARTESIAN_POINT('Ctrl Pts',(0.0082465429820097,-0.0319739230346346,
0.06831848665221));
#99211=CARTESIAN_POINT('Ctrl Pts',(0.00832679825158368,-0.0318646057455575,
0.0683212819681631));
#99212=CARTESIAN_POINT('Ctrl Pts',(0.00800898098763197,-0.0321934096636183,
0.0684012524581878));
#99213=CARTESIAN_POINT('Ctrl Pts',(0.00808826069653482,-0.0320835708272303,
0.0683996692600936));
#99214=CARTESIAN_POINT('Ctrl Pts',(0.00816752718418686,-0.0319739230346346,
0.0683997276697739));
#99215=CARTESIAN_POINT('Ctrl Pts',(0.00824667904035195,-0.0318646057455575,
0.0684014198291049));
#99216=CARTESIAN_POINT('Ctrl Pts',(0.00788497779667553,-0.0320218834582343,
0.0684042389311222));
#99217=CARTESIAN_POINT('Ctrl Pts',(0.00794477727911326,-0.0319391099350653,
0.0684017535546613));
#99218=CARTESIAN_POINT('Ctrl Pts',(0.00800457934006583,-0.0318564869454948,
0.06840020346133));
#99219=CARTESIAN_POINT('Ctrl Pts',(0.00806434031626076,-0.0317740741446554,
0.0683995857137364));
#99220=CARTESIAN_POINT('Ctrl Pts',(0.00784923828981616,-0.0320218834582343,
0.0683698948530783));
#99221=CARTESIAN_POINT('Ctrl Pts',(0.00790939521108004,-0.0319391099350653,
0.0683670375147507));
#99222=CARTESIAN_POINT('Ctrl Pts',(0.00796956030253236,-0.0318564869454948,
0.0683651212663723));
#99223=CARTESIAN_POINT('Ctrl Pts',(0.00802968961158322,-0.0317740741446554,
0.0683641434125613));
#99224=CARTESIAN_POINT('Ctrl Pts',(0.00781349878295678,-0.0320218834582343,
0.0683355507750344));
#99225=CARTESIAN_POINT('Ctrl Pts',(0.00787401314304682,-0.0319391099350653,
0.0683323214748401));
#99226=CARTESIAN_POINT('Ctrl Pts',(0.00793454126499889,-0.0318564869454948,
0.0683300390714146));
#99227=CARTESIAN_POINT('Ctrl Pts',(0.00799503890690568,-0.0317740741446554,
0.0683287011113862));
#99228=CARTESIAN_POINT('Ctrl Pts',(0.00777775927609741,-0.0320218834582343,
0.0683012066969905));
#99229=CARTESIAN_POINT('Ctrl Pts',(0.0078386310750136,-0.0319391099350653,
0.0682976054349295));
#99230=CARTESIAN_POINT('Ctrl Pts',(0.00789952222746543,-0.0318564869454948,
0.068294956876457));
#99231=CARTESIAN_POINT('Ctrl Pts',(0.00796038820222814,-0.0317740741446554,
0.0682932588102111));
#99232=CARTESIAN_POINT('Origin',(0.00668270788140655,-0.0391228853390711,
0.0621581726514373));
#99233=CARTESIAN_POINT('Ctrl Pts',(0.00499259991127169,-0.0352722978779572,
0.0693250790617349));
#99234=CARTESIAN_POINT('Ctrl Pts',(0.00500863930141557,-0.0352466642097202,
0.0693150875332319));
#99235=CARTESIAN_POINT('Ctrl Pts',(0.00502462294863455,-0.0352210183808294,
0.0693050383604924));
#99236=CARTESIAN_POINT('Ctrl Pts',(0.00504055113353512,-0.0351953608940153,
0.0692949307380702));
#99237=CARTESIAN_POINT('Origin',(0.00255732255140221,-0.0352456003065054,
0.0650731186462026));
#99238=CARTESIAN_POINT('Ctrl Pts',(0.00514727955928602,-0.035024121149334,
0.0692304764243673));
#99239=CARTESIAN_POINT('Ctrl Pts',(0.00521504397640165,-0.0349144232867422,
0.0691894763228488));
#99240=CARTESIAN_POINT('Ctrl Pts',(0.00528369645514265,-0.0348045283677512,
0.0691498524196547));
#99241=CARTESIAN_POINT('Ctrl Pts',(0.00535315094905891,-0.0346945769586886,
0.0691116587402347));
#99242=CARTESIAN_POINT('Ctrl Pts',(0.00503785066805416,-0.035024121149334,
0.0692010407391066));
#99243=CARTESIAN_POINT('Ctrl Pts',(0.00510602054964687,-0.0349144232867422,
0.0691585332995469));
#99244=CARTESIAN_POINT('Ctrl Pts',(0.00517510989330797,-0.0348045283677512,
0.0691174095373373));
#99245=CARTESIAN_POINT('Ctrl Pts',(0.0052450321645086,-0.0346945769586886,
0.0690777254198789));
#99246=CARTESIAN_POINT('Ctrl Pts',(0.0049284217768223,-0.035024121149334,
0.0691716050538458));
#99247=CARTESIAN_POINT('Ctrl Pts',(0.0049969971228921,-0.0349144232867422,
0.0691275902762449));
#99248=CARTESIAN_POINT('Ctrl Pts',(0.00506652333147329,-0.0348045283677512,
0.0690849666550198));
#99249=CARTESIAN_POINT('Ctrl Pts',(0.00513691337995829,-0.0346945769586886,
0.0690437920995231));
#99250=CARTESIAN_POINT('Ctrl Pts',(0.00481899288559044,-0.035024121149334,
0.069142169368585));
#99251=CARTESIAN_POINT('Ctrl Pts',(0.00488797369613732,-0.0349144232867422,
0.069096647252943));
#99252=CARTESIAN_POINT('Ctrl Pts',(0.00495793676963861,-0.0348045283677512,
0.0690525237727024));
#99253=CARTESIAN_POINT('Ctrl Pts',(0.00502879459540797,-0.0346945769586886,
0.0690098587791673));
#99254=CARTESIAN_POINT('Origin',(0.0132846940916072,-0.0345629067942152,
0.0839087386028029));
#99255=CARTESIAN_POINT('Ctrl Pts',(0.00531148955375613,-0.0351970973651657,
0.0689282635179625));
#99256=CARTESIAN_POINT('Ctrl Pts',(0.0053838296360102,-0.0350869349321797,
0.0688893030147748));
#99257=CARTESIAN_POINT('Ctrl Pts',(0.00545703961121713,-0.0349764985129731,
0.0688518141473813));
#99258=CARTESIAN_POINT('Ctrl Pts',(0.00553102749269634,-0.0348659306849633,
0.0688158510668816));
#99259=CARTESIAN_POINT('Ctrl Pts',(0.00529186226377177,-0.0351970973651657,
0.0690081086188657));
#99260=CARTESIAN_POINT('Ctrl Pts',(0.00536309620036208,-0.0350869349321797,
0.0689688762061751));
#99261=CARTESIAN_POINT('Ctrl Pts',(0.00543520476643493,-0.0349764985129731,
0.0689310922078764));
#99262=CARTESIAN_POINT('Ctrl Pts',(0.00550809742472504,-0.0348659306849633,
0.0688948110734243));
#99263=CARTESIAN_POINT('Ctrl Pts',(0.00527223497378742,-0.0351970973651657,
0.069087953719769));
#99264=CARTESIAN_POINT('Ctrl Pts',(0.00534236276471396,-0.0350869349321797,
0.0690484493975753));
#99265=CARTESIAN_POINT('Ctrl Pts',(0.00541336992165274,-0.034976498512973,
0.0690103702683716));
#99266=CARTESIAN_POINT('Ctrl Pts',(0.00548516735675374,-0.0348659306849633,
0.068973771079967));
#99267=CARTESIAN_POINT('Ctrl Pts',(0.00525260768380306,-0.0351970973651657,
0.0691677988206723));
#99268=CARTESIAN_POINT('Ctrl Pts',(0.00532162932906583,-0.0350869349321797,
0.0691280225889755));
#99269=CARTESIAN_POINT('Ctrl Pts',(0.00539153507687054,-0.034976498512973,
0.0690896483288667));
#99270=CARTESIAN_POINT('Ctrl Pts',(0.00546223728878244,-0.0348659306849633,
0.0690527310865096));
#99271=CARTESIAN_POINT('Origin',(0.0128401737970739,-0.0345637187966152,
0.0840923878992216));
#99272=CARTESIAN_POINT('Ctrl Pts',(0.00522295752662561,-0.0352450361861253,
0.0691837799832946));
#99273=CARTESIAN_POINT('Ctrl Pts',(0.00541026158325311,-0.0349452761023765,
0.0690743735885377));
#99274=CARTESIAN_POINT('Ctrl Pts',(0.00560527446589586,-0.0346444289983475,
0.0689793865133844));
#99275=CARTESIAN_POINT('Ctrl Pts',(0.00500987741694025,-0.0352450361861253,
0.0693145349711782));
#99276=CARTESIAN_POINT('Ctrl Pts',(0.00519224996840435,-0.0349452761023765,
0.0691970921284193));
#99277=CARTESIAN_POINT('Ctrl Pts',(0.00538295069390048,-0.0346444289983475,
0.0690937199748283));
#99278=CARTESIAN_POINT('Ctrl Pts',(0.00546205156128212,-0.0345231616327823,
0.0690532882358687));
#99279=CARTESIAN_POINT('Ctrl Pts',(0.00553230255735404,-0.0344132092796976,
0.0690166000265262));
#99280=CARTESIAN_POINT('Ctrl Pts',(0.00560330879546848,-0.0343032738558974,
0.0689813667965672));
#99281=CARTESIAN_POINT('Ctrl Pts',(0.00567497815220558,-0.034193496108874,
0.0689476313536723));
#99282=CARTESIAN_POINT('Ctrl Pts',(0.00535468690281672,-0.0345231616327823,
0.0690170395634645));
#99283=CARTESIAN_POINT('Ctrl Pts',(0.00542543753580368,-0.0344132092796976,
0.0689788714834624));
#99284=CARTESIAN_POINT('Ctrl Pts',(0.00549697399501148,-0.0343032738558974,
0.0689421687937938));
#99285=CARTESIAN_POINT('Ctrl Pts',(0.0055692034295236,-0.034193496108874,
0.0689069761672871));
#99286=CARTESIAN_POINT('Ctrl Pts',(0.00524732224435132,-0.0345231616327823,
0.0689807908910602));
#99287=CARTESIAN_POINT('Ctrl Pts',(0.00531857251425332,-0.0344132092796976,
0.0689411429403985));
#99288=CARTESIAN_POINT('Ctrl Pts',(0.00539063919455449,-0.0343032738558974,
0.0689029707910203));
#99289=CARTESIAN_POINT('Ctrl Pts',(0.00546342870684162,-0.034193496108874,
0.0688663209809019));
#99290=CARTESIAN_POINT('Ctrl Pts',(0.00513995758588592,-0.0345231616327823,
0.0689445422186559));
#99291=CARTESIAN_POINT('Ctrl Pts',(0.00521170749270296,-0.0344132092796976,
0.0689034143973347));
#99292=CARTESIAN_POINT('Ctrl Pts',(0.00528430439409749,-0.0343032738558974,
0.0688637727882469));
#99293=CARTESIAN_POINT('Ctrl Pts',(0.00535765398415964,-0.034193496108874,
0.0688256657945168));
#99294=CARTESIAN_POINT('Origin',(0.0132905727852292,-0.0345625596229409,
0.0839193187370609));
#99295=CARTESIAN_POINT('Ctrl Pts',(0.00567400935308173,-0.0346945769586885,
0.0686729010386621));
#99296=CARTESIAN_POINT('Ctrl Pts',(0.00574948654511411,-0.0345846629176689,
0.0686391419307133));
#99297=CARTESIAN_POINT('Ctrl Pts',(0.00582567475332433,-0.0344746925051586,
0.0686069378939594));
#99298=CARTESIAN_POINT('Ctrl Pts',(0.00590247618618805,-0.0343648066255171,
0.0685763297887621));
#99299=CARTESIAN_POINT('Ctrl Pts',(0.00564007605944396,-0.0346945769586885,
0.0687810197380832));
#99300=CARTESIAN_POINT('Ctrl Pts',(0.0057140633211508,-0.0345846629176689,
0.0687467930121968));
#99301=CARTESIAN_POINT('Ctrl Pts',(0.00578877101469861,-0.0344746925051586,
0.0687140904664878));
#99302=CARTESIAN_POINT('Ctrl Pts',(0.00586410324293113,-0.0343648066255171,
0.0686829536078994));
#99303=CARTESIAN_POINT('Ctrl Pts',(0.00560614276580618,-0.0346945769586885,
0.0688891384375043));
#99304=CARTESIAN_POINT('Ctrl Pts',(0.00567864009718748,-0.0345846629176689,
0.0688544440936803));
#99305=CARTESIAN_POINT('Ctrl Pts',(0.00575186727607289,-0.0344746925051586,
0.0688212430390162));
#99306=CARTESIAN_POINT('Ctrl Pts',(0.00582573029967421,-0.0343648066255171,
0.0687895774270366));
#99307=CARTESIAN_POINT('Ctrl Pts',(0.0055722094721684,-0.0346945769586885,
0.0689972571369253));
#99308=CARTESIAN_POINT('Ctrl Pts',(0.00564321687322416,-0.0345846629176689,
0.0689620951751638));
#99309=CARTESIAN_POINT('Ctrl Pts',(0.00571496353744717,-0.0344746925051586,
0.0689283956115446));
#99310=CARTESIAN_POINT('Ctrl Pts',(0.00578735735641729,-0.0343648066255171,
0.0688962012461739));
#99311=CARTESIAN_POINT('Origin',(0.0128659179646129,-0.0345626446730797,
0.084144841387769));
#99312=CARTESIAN_POINT('Ctrl Pts',(0.00557281665257836,-0.0346945769586886,
0.0689953225308436));
#99313=CARTESIAN_POINT('Ctrl Pts',(0.00568078343598838,-0.0345275153362891,
0.0689418915362472));
#99314=CARTESIAN_POINT('Ctrl Pts',(0.00579045850073889,-0.0343603235965159,
0.0688918421776204));
#99315=CARTESIAN_POINT('Ctrl Pts',(0.00590151527665433,-0.0341934961088741,
0.0688453176577636));
#99316=CARTESIAN_POINT('Ctrl Pts',(0.00549850659352597,-0.0346945769586886,
0.0690341303065451));
#99317=CARTESIAN_POINT('Ctrl Pts',(0.00560566053253615,-0.0345275153362891,
0.0689791428580097));
#99318=CARTESIAN_POINT('Ctrl Pts',(0.00571457149168738,-0.0343603235965159,
0.068927511079657));
#99319=CARTESIAN_POINT('Ctrl Pts',(0.00582491509113088,-0.0341934961088741,
0.0688793828879704));
#99320=CARTESIAN_POINT('Ctrl Pts',(0.00542419653447358,-0.0346945769586886,
0.0690729380822466));
#99321=CARTESIAN_POINT('Ctrl Pts',(0.00553053762908392,-0.0345275153362891,
0.0690163941797723));
#99322=CARTESIAN_POINT('Ctrl Pts',(0.00563868448263588,-0.0343603235965159,
0.0689631799816938));
#99323=CARTESIAN_POINT('Ctrl Pts',(0.00574831490560744,-0.0341934961088741,
0.0689134481181772));
#99324=CARTESIAN_POINT('Ctrl Pts',(0.00534988647542119,-0.0346945769586886,
0.0691117458579481));
#99325=CARTESIAN_POINT('Ctrl Pts',(0.00545541472563169,-0.0345275153362891,
0.0690536455015349));
#99326=CARTESIAN_POINT('Ctrl Pts',(0.00556279747358437,-0.0343603235965159,
0.0689988488837304));
#99327=CARTESIAN_POINT('Ctrl Pts',(0.005671714720084,-0.0341934961088741,
0.068947513348384));
#99328=CARTESIAN_POINT('Ctrl Pts',(0.00578732875098196,-0.0340223579322365,
0.0688962145768071));
#99329=CARTESIAN_POINT('Ctrl Pts',(0.0058597921544147,-0.0339125849573554,
0.0688639887901141));
#99330=CARTESIAN_POINT('Ctrl Pts',(0.005932871637555,-0.0338030433565221,
0.0688332854721777));
#99331=CARTESIAN_POINT('Ctrl Pts',(0.00600647026344122,-0.0336938721132328,
0.0688041356028545));
#99332=CARTESIAN_POINT('Ctrl Pts',(0.00568245183981392,-0.0340223579322365,
0.0688532958939967));
#99333=CARTESIAN_POINT('Ctrl Pts',(0.00575550720381924,-0.0339125849573554,
0.0688196235811683));
#99334=CARTESIAN_POINT('Ctrl Pts',(0.00582920817129801,-0.0338030433565221,
0.0687874870057619));
#99335=CARTESIAN_POINT('Ctrl Pts',(0.00590345684803649,-0.0336938721132328,
0.0687569189100756));
#99336=CARTESIAN_POINT('Ctrl Pts',(0.00557757492864589,-0.0340223579322365,
0.0688103772111864));
#99337=CARTESIAN_POINT('Ctrl Pts',(0.00565122225322378,-0.0339125849573554,
0.0687752583722225));
#99338=CARTESIAN_POINT('Ctrl Pts',(0.00572554470504103,-0.0338030433565221,
0.068741688539346));
#99339=CARTESIAN_POINT('Ctrl Pts',(0.00580044343263177,-0.0336938721132328,
0.0687097022172967));
#99340=CARTESIAN_POINT('Ctrl Pts',(0.00547269801747785,-0.0340223579322365,
0.068767458528376));
#99341=CARTESIAN_POINT('Ctrl Pts',(0.00554693730262832,-0.0339125849573554,
0.0687308931632766));
#99342=CARTESIAN_POINT('Ctrl Pts',(0.00562188123878404,-0.0338030433565221,
0.0686958900729302));
#99343=CARTESIAN_POINT('Ctrl Pts',(0.00569743001722704,-0.0336938721132328,
0.0686624855245177));
#99344=CARTESIAN_POINT('Origin',(0.013236672512422,-0.03455896434161,0.0838118587980092));
#99345=CARTESIAN_POINT('Ctrl Pts',(0.00602275330947995,-0.0341934961088739,
0.0685298863329841));
#99346=CARTESIAN_POINT('Ctrl Pts',(0.00610025134884894,-0.0340836138581106,
0.0685009143888588));
#99347=CARTESIAN_POINT('Ctrl Pts',(0.006178311716794,-0.0339738896643499,
0.0684735600053287));
#99348=CARTESIAN_POINT('Ctrl Pts',(0.00625683215877638,-0.0338644633294062,
0.0684478514953285));
#99349=CARTESIAN_POINT('Ctrl Pts',(0.00598209808651405,-0.0341934961088739,
0.0686356611508401));
#99350=CARTESIAN_POINT('Ctrl Pts',(0.00605813755378216,-0.0340836138581106,
0.0686061285952651));
#99351=CARTESIAN_POINT('Ctrl Pts',(0.00613475165015428,-0.0339738896643499,
0.0685781836871882));
#99352=CARTESIAN_POINT('Ctrl Pts',(0.00621183992147581,-0.0338644633294062,
0.0685518556194274));
#99353=CARTESIAN_POINT('Ctrl Pts',(0.00594144286354814,-0.0341934961088739,
0.0687414359686961));
#99354=CARTESIAN_POINT('Ctrl Pts',(0.00601602375871537,-0.0340836138581106,
0.0687113428016715));
#99355=CARTESIAN_POINT('Ctrl Pts',(0.00609119158351456,-0.0339738896643499,
0.0686828073690477));
#99356=CARTESIAN_POINT('Ctrl Pts',(0.00616684768417524,-0.0338644633294062,
0.0686558597435262));
#99357=CARTESIAN_POINT('Ctrl Pts',(0.00590078764058223,-0.0341934961088739,
0.0688472107865521));
#99358=CARTESIAN_POINT('Ctrl Pts',(0.00597390996364859,-0.0340836138581106,
0.0688165570080778));
#99359=CARTESIAN_POINT('Ctrl Pts',(0.00604763151687485,-0.0339738896643499,
0.0687874310509072));
#99360=CARTESIAN_POINT('Ctrl Pts',(0.00612185544687467,-0.0338644633294062,
0.068759863867625));
#99361=CARTESIAN_POINT('Origin',(0.0128346846475394,-0.0345610621862508,
0.0840763503254826));
#99362=CARTESIAN_POINT('Ctrl Pts',(0.00586819159598038,-0.0342436276873901,
0.0688594011626142));
#99363=CARTESIAN_POINT('Ctrl Pts',(0.00606772982055773,-0.0339430054201861,
0.068774330160832));
#99364=CARTESIAN_POINT('Ctrl Pts',(0.00627310907437932,-0.0336441434784163,
0.0687045308735047));
#99365=CARTESIAN_POINT('Ctrl Pts',(0.00564040514730526,-0.0342436276873901,
0.06896242219833));
#99366=CARTESIAN_POINT('Ctrl Pts',(0.00583605786946734,-0.0339430054201861,
0.06886876008901));
#99367=CARTESIAN_POINT('Ctrl Pts',(0.00603820977659939,-0.0336441434784163,
0.0687901014286185));
#99368=CARTESIAN_POINT('Ctrl Pts',(0.00612182949496901,-0.0335235895815127,
0.0687598736413807));
#99369=CARTESIAN_POINT('Ctrl Pts',(0.00619603519647663,-0.0334144449262719,
0.0687323128210091));
#99370=CARTESIAN_POINT('Ctrl Pts',(0.00627089553715207,-0.0333049234473132,
0.068706253370541));
#99371=CARTESIAN_POINT('Ctrl Pts',(0.00634631781205715,-0.0331951640388588,
0.068681737283052));
#99372=CARTESIAN_POINT('Ctrl Pts',(0.0060198544725169,-0.0335235895815127,
0.0687104543406756));
#99373=CARTESIAN_POINT('Ctrl Pts',(0.00609474052799637,-0.0334144449262719,
0.0686814896333496));
#99374=CARTESIAN_POINT('Ctrl Pts',(0.00617031100753587,-0.0333049234473132,
0.0686540387386321));
#99375=CARTESIAN_POINT('Ctrl Pts',(0.00624647245931801,-0.0331951640388588,
0.0686281455110838));
#99376=CARTESIAN_POINT('Ctrl Pts',(0.00591787945006479,-0.0335235895815127,
0.0686610350399705));
#99377=CARTESIAN_POINT('Ctrl Pts',(0.00599344585951611,-0.0334144449262719,
0.06863066644569));
#99378=CARTESIAN_POINT('Ctrl Pts',(0.00606972647791968,-0.0333049234473132,
0.0686018241067232));
#99379=CARTESIAN_POINT('Ctrl Pts',(0.00614662710657887,-0.0331951640388588,
0.0685745537391156));
#99380=CARTESIAN_POINT('Ctrl Pts',(0.00581590442761268,-0.0335235895815127,
0.0686116157392653));
#99381=CARTESIAN_POINT('Ctrl Pts',(0.00589215119103584,-0.0334144449262719,
0.0685798432580305));
#99382=CARTESIAN_POINT('Ctrl Pts',(0.00596914194830348,-0.0333049234473132,
0.0685496094748143));
#99383=CARTESIAN_POINT('Ctrl Pts',(0.00604678175383973,-0.0331951640388588,
0.0685209619671475));
#99384=CARTESIAN_POINT('Origin',(0.0107693667188908,-0.032643457177125,
0.0847511952527698));
#99385=CARTESIAN_POINT('Ctrl Pts',(0.00638063389637515,-0.0336938721132356,
0.0684072084706003));
#99386=CARTESIAN_POINT('Ctrl Pts',(0.00641424836085578,-0.0336474569764941,
0.068397005245182));
#99387=CARTESIAN_POINT('Ctrl Pts',(0.00644797996368787,-0.033601104548885,
0.0683871962186434));
#99388=CARTESIAN_POINT('Ctrl Pts',(0.00653338061926225,-0.0334837508694588,
0.0683623620208405));
#99389=CARTESIAN_POINT('Ctrl Pts',(0.00661947966187594,-0.0333660264863562,
0.0683400693266549));
#99390=CARTESIAN_POINT('Ctrl Pts',(0.00623898417299042,-0.0336938721132356,
0.0687162479424104));
#99391=CARTESIAN_POINT('Ctrl Pts',(0.00627078972689244,-0.0336474569764941,
0.0687052155941567));
#99392=CARTESIAN_POINT('Ctrl Pts',(0.00630272224902327,-0.033601104548885,
0.0686945563260126));
#99393=CARTESIAN_POINT('Ctrl Pts',(0.00638356804629211,-0.0334837508694588,
0.0686675695121342));
#99394=CARTESIAN_POINT('Ctrl Pts',(0.00646517801722987,-0.0333660264863562,
0.0686429901772596));
#99395=CARTESIAN_POINT('Ctrl Pts',(0.00623898417300239,-0.0336938721132427,
0.0687162479424196));
#99396=CARTESIAN_POINT('Ctrl Pts',(0.00627078972690343,-0.0336474569765026,
0.0687052155941663));
#99397=CARTESIAN_POINT('Ctrl Pts',(0.00630272224903327,-0.0336011045488949,
0.0686945563260226));
#99398=CARTESIAN_POINT('Ctrl Pts',(0.00638289471091717,-0.033484728265791,
0.0686677942755497));
#99399=CARTESIAN_POINT('Ctrl Pts',(0.00646381896393862,-0.0333679870047995,
0.0686433996805959));
#99400=CARTESIAN_POINT('Ctrl Pts',(0.0062389841729857,-0.0336938721132425,
0.068716247942412));
#99401=CARTESIAN_POINT('Ctrl Pts',(0.00635273490910074,-0.0335278710435083,
0.0686767913827558));
#99402=CARTESIAN_POINT('Ctrl Pts',(0.00646768297542329,-0.033362046922432,
0.0686409158973354));
#99403=CARTESIAN_POINT('Ctrl Pts',(0.00658389150603253,-0.0331951640388601,
0.0686086227639821));
#99404=CARTESIAN_POINT('Ctrl Pts',(0.00616039615858634,-0.0336938721132425,
0.0687454361903217));
#99405=CARTESIAN_POINT('Ctrl Pts',(0.00627353586485489,-0.0335278710435083,
0.0687043344609204));
#99406=CARTESIAN_POINT('Ctrl Pts',(0.00638792470838529,-0.033362046922432,
0.0686667952227847));
#99407=CARTESIAN_POINT('Ctrl Pts',(0.00650362582187743,-0.0331951640388601,
0.068632818833299));
#99408=CARTESIAN_POINT('Ctrl Pts',(0.00608180814418698,-0.0336938721132425,
0.0687746244382315));
#99409=CARTESIAN_POINT('Ctrl Pts',(0.00619433682060903,-0.0335278710435083,
0.0687318775390851));
#99410=CARTESIAN_POINT('Ctrl Pts',(0.00630816644134729,-0.033362046922432,
0.0686926745482339));
#99411=CARTESIAN_POINT('Ctrl Pts',(0.00642336013772234,-0.0331951640388601,
0.0686570149026159));
#99412=CARTESIAN_POINT('Ctrl Pts',(0.00600322012978762,-0.0336938721132425,
0.0688038126861412));
#99413=CARTESIAN_POINT('Ctrl Pts',(0.00611513777636318,-0.0335278710435083,
0.0687594206172497));
#99414=CARTESIAN_POINT('Ctrl Pts',(0.00622840817430929,-0.033362046922432,
0.0687185538736831));
#99415=CARTESIAN_POINT('Ctrl Pts',(0.00634309445356724,-0.0331951640388601,
0.0686812109719328));
#99416=CARTESIAN_POINT('Ctrl Pts',(0.00646422742317616,-0.0330240426238155,
0.068644806202726));
#99417=CARTESIAN_POINT('Ctrl Pts',(0.00654006683118363,-0.0329142774063509,
0.0686219442189445));
#99418=CARTESIAN_POINT('Ctrl Pts',(0.00661641666896846,-0.0328043479726686,
0.0686006386500407));
#99419=CARTESIAN_POINT('Ctrl Pts',(0.00669317987837464,-0.0326943950436594,
0.0685809194837004));
#99420=CARTESIAN_POINT('Ctrl Pts',(0.00636555682001553,-0.0330240426238155,
0.0685890814500886));
#99421=CARTESIAN_POINT('Ctrl Pts',(0.00644216389078057,-0.0329142774063509,
0.0685648601826184));
#99422=CARTESIAN_POINT('Ctrl Pts',(0.00651930987422167,-0.0328043479726686,
0.068542210522107));
#99423=CARTESIAN_POINT('Ctrl Pts',(0.00659689673968124,-0.0326943950436594,
0.0685211642062102));
#99424=CARTESIAN_POINT('Ctrl Pts',(0.00626688621685489,-0.0330240426238155,
0.0685333566974512));
#99425=CARTESIAN_POINT('Ctrl Pts',(0.00634426095037751,-0.0329142774063509,
0.0685077761462924));
#99426=CARTESIAN_POINT('Ctrl Pts',(0.00642220307947488,-0.0328043479726686,
0.0684837823941734));
#99427=CARTESIAN_POINT('Ctrl Pts',(0.00650061360098785,-0.0326943950436594,
0.06846140892872));
#99428=CARTESIAN_POINT('Ctrl Pts',(0.00616821561369426,-0.0330240426238155,
0.0684776319448138));
#99429=CARTESIAN_POINT('Ctrl Pts',(0.00624635800997445,-0.0329142774063509,
0.0684506921099663));
#99430=CARTESIAN_POINT('Ctrl Pts',(0.00632509628472809,-0.0328043479726686,
0.0684253542662398));
#99431=CARTESIAN_POINT('Ctrl Pts',(0.00640433046229446,-0.0326943950436594,
0.0684016536512298));
#99432=CARTESIAN_POINT('Origin',(0.0108019857363915,-0.0326396682856121,
0.0848704906776846));
#99433=CARTESIAN_POINT('Ctrl Pts',(0.00674370756866024,-0.0331951640388587,
0.0683108738640981));
#99434=CARTESIAN_POINT('Ctrl Pts',(0.00682412971872628,-0.0330855618255041,
0.0682918661280146));
#99435=CARTESIAN_POINT('Ctrl Pts',(0.00690500270140994,-0.0329757224427708,
0.0682745068778918));
#99436=CARTESIAN_POINT('Ctrl Pts',(0.00698622404440808,-0.0328657862078596,
0.0682588234232589));
#99437=CARTESIAN_POINT('Ctrl Pts',(0.00669011583935863,-0.0331951640388587,
0.0684107191373463));
#99438=CARTESIAN_POINT('Ctrl Pts',(0.00676916282277103,-0.0330855618255041,
0.0683909732836069));
#99439=CARTESIAN_POINT('Ctrl Pts',(0.00684867490309286,-0.0329757224427708,
0.0683728469613853));
#99440=CARTESIAN_POINT('Ctrl Pts',(0.00692855139892115,-0.0328657862078596,
0.0683563683770089));
#99441=CARTESIAN_POINT('Ctrl Pts',(0.00663652411005703,-0.0331951640388587,
0.0685105644105946));
#99442=CARTESIAN_POINT('Ctrl Pts',(0.00671419592681577,-0.0330855618255041,
0.0684900804391991));
#99443=CARTESIAN_POINT('Ctrl Pts',(0.00679234710477578,-0.0329757224427708,
0.0684711870448789));
#99444=CARTESIAN_POINT('Ctrl Pts',(0.00687087875343423,-0.0328657862078596,
0.0684539133307588));
#99445=CARTESIAN_POINT('Ctrl Pts',(0.00658293238075542,-0.0331951640388587,
0.0686104096838428));
#99446=CARTESIAN_POINT('Ctrl Pts',(0.00665922903086051,-0.0330855618255041,
0.0685891875947914));
#99447=CARTESIAN_POINT('Ctrl Pts',(0.00673601930645869,-0.0329757224427708,
0.0685695271283724));
#99448=CARTESIAN_POINT('Ctrl Pts',(0.00681320610794731,-0.0328657862078596,
0.0685514582845088));
#99449=CARTESIAN_POINT('Origin',(0.0103275744650057,-0.0326401908832347,
0.0849492740342608));
#99450=CARTESIAN_POINT('Ctrl Pts',(0.00654913516136936,-0.0332451089994432,
0.0686183988099795));
#99451=CARTESIAN_POINT('Ctrl Pts',(0.00675776291357944,-0.0329451141710258,
0.0685590100255262));
#99452=CARTESIAN_POINT('Ctrl Pts',(0.00697027138239242,-0.0326442513127503,
0.0685155046535149));
#99453=CARTESIAN_POINT('Ctrl Pts',(0.0063102319892303,-0.0332451089994432,
0.0686920552716233));
#99454=CARTESIAN_POINT('Ctrl Pts',(0.00651608174253904,-0.0329451141710258,
0.0686236561066152));
#99455=CARTESIAN_POINT('Ctrl Pts',(0.00672649880315049,-0.0326442513127503,
0.0685709567013557));
#99456=CARTESIAN_POINT('Ctrl Pts',(0.00681317533143831,-0.0325229783203385,
0.068551465396958));
#99457=CARTESIAN_POINT('Ctrl Pts',(0.00689035100710463,-0.0324130253112079,
0.0685333987103598));
#99458=CARTESIAN_POINT('Ctrl Pts',(0.00696788871018158,-0.0323031222247695,
0.0685169312418898));
#99459=CARTESIAN_POINT('Ctrl Pts',(0.00704568837606189,-0.0321934096636184,
0.0685020805805181));
#99460=CARTESIAN_POINT('Ctrl Pts',(0.00671819838379667,-0.0325229783203385,
0.0684896550251256));
#99461=CARTESIAN_POINT('Ctrl Pts',(0.00679622611407149,-0.0324130253112079,
0.068470279083405));
#99462=CARTESIAN_POINT('Ctrl Pts',(0.00687464282614974,-0.0323031222247695,
0.0684525201842307));
#99463=CARTESIAN_POINT('Ctrl Pts',(0.00695334727110378,-0.0321934096636184,
0.0684363975310723));
#99464=CARTESIAN_POINT('Ctrl Pts',(0.00662322143615504,-0.0325229783203385,
0.0684278446532933));
#99465=CARTESIAN_POINT('Ctrl Pts',(0.00670210122103835,-0.0324130253112079,
0.0684071594564503));
#99466=CARTESIAN_POINT('Ctrl Pts',(0.0067813969421179,-0.0323031222247695,
0.0683881091265715));
#99467=CARTESIAN_POINT('Ctrl Pts',(0.00686100616614567,-0.0321934096636184,
0.0683707144816266));
#99468=CARTESIAN_POINT('Ctrl Pts',(0.00652824448851341,-0.0325229783203385,
0.068366034281461));
#99469=CARTESIAN_POINT('Ctrl Pts',(0.00660797632800521,-0.0324130253112079,
0.0683440398294956));
#99470=CARTESIAN_POINT('Ctrl Pts',(0.00668815105808605,-0.0323031222247695,
0.0683236980689124));
#99471=CARTESIAN_POINT('Ctrl Pts',(0.00676866506118755,-0.0321934096636184,
0.0683050314321809));
#99472=CARTESIAN_POINT('Origin',(0.0108001514141797,-0.0326393375178216,
0.0848621644365802));
#99473=CARTESIAN_POINT('Ctrl Pts',(0.00711307259435396,-0.0326943950436593,
0.0682357404430475));
#99474=CARTESIAN_POINT('Ctrl Pts',(0.00719458217555229,-0.0325844576448127,
0.068221810970505));
#99475=CARTESIAN_POINT('Ctrl Pts',(0.00727638560964018,-0.0324744968375319,
0.0682095662639281));
#99476=CARTESIAN_POINT('Ctrl Pts',(0.00735837786889389,-0.0323646534831894,
0.0681990205662855));
#99477=CARTESIAN_POINT('Ctrl Pts',(0.00705331733641517,-0.0326943950436593,
0.0683320235502378));
#99478=CARTESIAN_POINT('Ctrl Pts',(0.00713349995594264,-0.0325844576448127,
0.0683172705382477));
#99479=CARTESIAN_POINT('Ctrl Pts',(0.00721399336659453,-0.0324744968375319,
0.068304174790197));
#99480=CARTESIAN_POINT('Ctrl Pts',(0.00729469420408556,-0.0323646534831894,
0.0682927516626098));
#99481=CARTESIAN_POINT('Ctrl Pts',(0.00699356207847638,-0.0326943950436593,
0.0684283066574282));
#99482=CARTESIAN_POINT('Ctrl Pts',(0.007072417736333,-0.0325844576448127,
0.0684127301059904));
#99483=CARTESIAN_POINT('Ctrl Pts',(0.00715160112354887,-0.0324744968375319,
0.0683987833164659));
#99484=CARTESIAN_POINT('Ctrl Pts',(0.00723101053927724,-0.0323646534831894,
0.068386482758934));
#99485=CARTESIAN_POINT('Ctrl Pts',(0.00693380682053759,-0.0326943950436593,
0.0685245897646186));
#99486=CARTESIAN_POINT('Ctrl Pts',(0.00701133551672335,-0.0325844576448127,
0.0685081896737331));
#99487=CARTESIAN_POINT('Ctrl Pts',(0.00708920888050322,-0.0324744968375319,
0.0684933918427348));
#99488=CARTESIAN_POINT('Ctrl Pts',(0.00716732687446891,-0.0323646534831894,
0.0684802138552583));
#99489=CARTESIAN_POINT('Origin',(0.0103355888499022,-0.0326395579068055,
0.0849862568880412));
#99490=CARTESIAN_POINT('Ctrl Pts',(0.00689953615569267,-0.0327445246961877,
0.0685304496051844));
#99491=CARTESIAN_POINT('Ctrl Pts',(0.00711148096145355,-0.0324436878365475,
0.0684842764115347));
#99492=CARTESIAN_POINT('Ctrl Pts',(0.00732630160803998,-0.0321434074463187,
0.0684541989398822));
#99493=CARTESIAN_POINT('Ctrl Pts',(0.00665647987593443,-0.0327445246961877,
0.0685889615259362));
#99494=CARTESIAN_POINT('Ctrl Pts',(0.00686621786855063,-0.0324436878365475,
0.0685336213149307));
#99495=CARTESIAN_POINT('Ctrl Pts',(0.00707952846852147,-0.0321434074463187,
0.068494236642266));
#99496=CARTESIAN_POINT('Ctrl Pts',(0.00726033554411033,-0.0322357242816072,
0.0684638251095895));
#99497=CARTESIAN_POINT('Ctrl Pts',(0.00744143283967124,-0.0319819883628706,
0.0684363254536683));
#99498=CARTESIAN_POINT('Ctrl Pts',(0.00762391300086686,-0.0317295851069886,
0.0684204052682019));
#99499=CARTESIAN_POINT('Ctrl Pts',(0.00701404305633529,-0.0322357242816072,
0.0685067204527584));
#99500=CARTESIAN_POINT('Ctrl Pts',(0.00719377419084949,-0.0319819883628706,
0.0684713767005311));
#99501=CARTESIAN_POINT('Ctrl Pts',(0.00737539010198121,-0.0317295851069886,
0.0684475413830576));
#99502=CARTESIAN_POINT('Origin',(0.0103182024466775,-0.0326371942646543,
0.0848925546125099));
#99503=CARTESIAN_POINT('Origin',(0.0107732367041174,-0.0326352985529337,
0.0847424171978103));
#99504=CARTESIAN_POINT('Ctrl Pts',(0.00748642642908508,-0.0321934096636183,
0.0681839479024995));
#99505=CARTESIAN_POINT('Ctrl Pts',(0.00756870293716775,-0.0320835708272304,
0.0681751582697888));
#99506=CARTESIAN_POINT('Ctrl Pts',(0.00765111362252414,-0.0319739230346346,
0.0681680764434806));
#99507=CARTESIAN_POINT('Ctrl Pts',(0.00773355235101604,-0.0318646057455575,
0.0681627033921506));
#99508=CARTESIAN_POINT('Ctrl Pts',(0.00742074332307886,-0.0321934096636183,
0.0682762890869737));
#99509=CARTESIAN_POINT('Ctrl Pts',(0.00750174637426129,-0.0320835708272304,
0.0682665936330409));
#99510=CARTESIAN_POINT('Ctrl Pts',(0.00758290308729731,-0.0319739230346346,
0.0682585801567993));
#99511=CARTESIAN_POINT('Ctrl Pts',(0.00766410884093803,-0.0318646057455575,
0.0682522509419371));
#99512=CARTESIAN_POINT('Ctrl Pts',(0.00735506021707264,-0.0321934096636183,
0.0683686302714479));
#99513=CARTESIAN_POINT('Ctrl Pts',(0.00743478981135483,-0.0320835708272304,
0.0683580289962929));
#99514=CARTESIAN_POINT('Ctrl Pts',(0.00751469255207047,-0.0319739230346346,
0.0683490838701181));
#99515=CARTESIAN_POINT('Ctrl Pts',(0.00759466533086003,-0.0318646057455575,
0.0683417984917237));
#99516=CARTESIAN_POINT('Ctrl Pts',(0.00728937711106641,-0.0321934096636183,
0.0684609714559222));
#99517=CARTESIAN_POINT('Ctrl Pts',(0.00736783324844837,-0.0320835708272304,
0.068449464359545));
#99518=CARTESIAN_POINT('Ctrl Pts',(0.00744648201684363,-0.0319739230346346,
0.0684395875834368));
#99519=CARTESIAN_POINT('Ctrl Pts',(0.00752522182078202,-0.0318646057455575,
0.0684313460415102));
#99520=CARTESIAN_POINT('Ctrl Pts',(0.007166726026618,-0.032021883458235,
0.0684794761005202));
#99521=CARTESIAN_POINT('Ctrl Pts',(0.00722574247200713,-0.0319391099350658,
0.0684695154594957));
#99522=CARTESIAN_POINT('Ctrl Pts',(0.00728487869763767,-0.0318564869454951,
0.0684604824034403));
#99523=CARTESIAN_POINT('Ctrl Pts',(0.00734409101638228,-0.0317740741446555,
0.0684523794905836));
#99524=CARTESIAN_POINT('Ctrl Pts',(0.00712696388209023,-0.032021883458235,
0.0684498821837506));
#99525=CARTESIAN_POINT('Ctrl Pts',(0.00718628832861009,-0.0319391099350658,
0.0684395077149259));
#99526=CARTESIAN_POINT('Ctrl Pts',(0.00724573883074043,-0.0318564869454951,
0.0684300658912789));
#99527=CARTESIAN_POINT('Ctrl Pts',(0.00730527144464972,-0.0317740741446555,
0.068421559547402));
#99528=CARTESIAN_POINT('Ctrl Pts',(0.00708720173756246,-0.032021883458235,
0.068420288266981));
#99529=CARTESIAN_POINT('Ctrl Pts',(0.00714683418521306,-0.0319391099350658,
0.0684094999703561));
#99530=CARTESIAN_POINT('Ctrl Pts',(0.00720659896384319,-0.0318564869454951,
0.0683996493791175));
#99531=CARTESIAN_POINT('Ctrl Pts',(0.00726645187291716,-0.0317740741446555,
0.0683907396042204));
#99532=CARTESIAN_POINT('Ctrl Pts',(0.00704743959303469,-0.032021883458235,
0.0683906943502114));
#99533=CARTESIAN_POINT('Ctrl Pts',(0.00710738004181602,-0.0319391099350658,
0.0683794922257863));
#99534=CARTESIAN_POINT('Ctrl Pts',(0.00716745909694595,-0.0318564869454951,
0.0683692328669562));
#99535=CARTESIAN_POINT('Ctrl Pts',(0.0072276323011846,-0.0317740741446555,
0.0683599196610388));
#99536=CARTESIAN_POINT('Origin',(0.00519109668483847,-0.0391228853390555,
0.0624333462951897));
#99537=CARTESIAN_POINT('Ctrl Pts',(0.0044125672759175,-0.0352722978779579,
0.0697555662047294));
#99538=CARTESIAN_POINT('Ctrl Pts',(0.00442722792010397,-0.0352466642097207,
0.0697436431937817));
#99539=CARTESIAN_POINT('Ctrl Pts',(0.00444182603617658,-0.0352210183808296,
0.0697316699795806));
#99540=CARTESIAN_POINT('Ctrl Pts',(0.00445636180158001,-0.0351953608940152,
0.0697196457278616));
#99541=CARTESIAN_POINT('Origin',(0.0014635808575311,-0.0352456003065056,
0.0658423549531952));
#99542=CARTESIAN_POINT('Ctrl Pts',(0.00455417037426209,-0.035024121149334,
0.0696423230369613));
#99543=CARTESIAN_POINT('Ctrl Pts',(0.00461626177340869,-0.0349144232867422,
0.0695931530999717));
#99544=CARTESIAN_POINT('Ctrl Pts',(0.00467940671493554,-0.0348045283677513,
0.0695452372059366));
#99545=CARTESIAN_POINT('Ctrl Pts',(0.00474352660207877,-0.0346945769586887,
0.0694986397387786));
#99546=CARTESIAN_POINT('Ctrl Pts',(0.00444191509290649,-0.035024121149334,
0.0696268345376543));
#99547=CARTESIAN_POINT('Ctrl Pts',(0.00450421983977089,-0.0349144232867422,
0.0695761183302601));
#99548=CARTESIAN_POINT('Ctrl Pts',(0.00456761021922716,-0.0348045283677513,
0.0695266596503528));
#99549=CARTESIAN_POINT('Ctrl Pts',(0.00463200739367237,-0.0346945769586887,
0.0694785248696659));
#99550=CARTESIAN_POINT('Ctrl Pts',(0.00432965981155089,-0.035024121149334,
0.0696113460383472));
#99551=CARTESIAN_POINT('Ctrl Pts',(0.00439217790613309,-0.0349144232867422,
0.0695590835605486));
#99552=CARTESIAN_POINT('Ctrl Pts',(0.00445581372351877,-0.0348045283677513,
0.069508082094769));
#99553=CARTESIAN_POINT('Ctrl Pts',(0.00452048818526597,-0.0346945769586887,
0.0694584100005532));
#99554=CARTESIAN_POINT('Ctrl Pts',(0.00421740453019528,-0.035024121149334,
0.0695958575390402));
#99555=CARTESIAN_POINT('Ctrl Pts',(0.00428013597249529,-0.0349144232867422,
0.069542048790837));
#99556=CARTESIAN_POINT('Ctrl Pts',(0.00434401722781038,-0.0348045283677513,
0.0694895045391852));
#99557=CARTESIAN_POINT('Ctrl Pts',(0.00440896897685957,-0.0346945769586887,
0.0694382951314405));
#99558=CARTESIAN_POINT('Origin',(0.0144670930243381,-0.0345629067941596,
0.0831849542577961));
#99559=CARTESIAN_POINT('Ctrl Pts',(0.00467920820309421,-0.0351970973651654,
0.0693219121999994));
#99560=CARTESIAN_POINT('Ctrl Pts',(0.00474609481634698,-0.0350869349321794,
0.0692741922955912));
#99561=CARTESIAN_POINT('Ctrl Pts',(0.00481402890805956,-0.0349764985129727,
0.0692278233961926));
#99562=CARTESIAN_POINT('Ctrl Pts',(0.00488292600382625,-0.034865930684963,
0.069182870754894));
#99563=CARTESIAN_POINT('Ctrl Pts',(0.00466974292483447,-0.0351970973651654,
0.0694035876501514));
#99564=CARTESIAN_POINT('Ctrl Pts',(0.0047354980354152,-0.0350869349321794,
0.0693557366171406));
#99565=CARTESIAN_POINT('Ctrl Pts',(0.00480230241322307,-0.0349764985129727,
0.0693092129572004));
#99566=CARTESIAN_POINT('Ctrl Pts',(0.00487007305923235,-0.034865930684963,
0.0692640820377635));
#99567=CARTESIAN_POINT('Ctrl Pts',(0.00466027764657473,-0.0351970973651654,
0.0694852631003033));
#99568=CARTESIAN_POINT('Ctrl Pts',(0.00472490125448342,-0.0350869349321794,
0.06943728093869));
#99569=CARTESIAN_POINT('Ctrl Pts',(0.00479057591838658,-0.0349764985129727,
0.0693906025182083));
#99570=CARTESIAN_POINT('Ctrl Pts',(0.00485722011463844,-0.034865930684963,
0.0693452933206331));
#99571=CARTESIAN_POINT('Ctrl Pts',(0.00465081236831499,-0.0351970973651654,
0.0695669385504553));
#99572=CARTESIAN_POINT('Ctrl Pts',(0.00471430447355164,-0.0350869349321794,
0.0695188252602393));
#99573=CARTESIAN_POINT('Ctrl Pts',(0.0047788494235501,-0.0349764985129727,
0.0694719920792162));
#99574=CARTESIAN_POINT('Ctrl Pts',(0.00484436717004454,-0.034865930684963,
0.0694265046035027));
#99575=CARTESIAN_POINT('Origin',(0.0140490952653582,-0.0345637187966762,
0.0834228685904193));
#99576=CARTESIAN_POINT('Ctrl Pts',(0.00462339898226972,-0.0352450361861252,
0.0695865098469176));
#99577=CARTESIAN_POINT('Ctrl Pts',(0.0047955138332382,-0.0349452761023765,
0.0694544907311847));
#99578=CARTESIAN_POINT('Ctrl Pts',(0.00497708394377801,-0.0346444289983475,
0.069335811062322));
#99579=CARTESIAN_POINT('Ctrl Pts',(0.0044283870183293,-0.0352450361861252,
0.0697429398118224));
#99580=CARTESIAN_POINT('Ctrl Pts',(0.0045946020165111,-0.0349452761023765,
0.0696035656993688));
#99581=CARTESIAN_POINT('Ctrl Pts',(0.00477084304355708,-0.0346444289983475,
0.069477107527515));
#99582=CARTESIAN_POINT('Ctrl Pts',(0.00484425273639071,-0.0345231616327822,
0.0694270806374069));
#99583=CARTESIAN_POINT('Ctrl Pts',(0.00490935153046505,-0.0344132092796975,
0.0693818769410545));
#99584=CARTESIAN_POINT('Ctrl Pts',(0.00497538196854374,-0.0343032738558974,
0.0693380220942112));
#99585=CARTESIAN_POINT('Ctrl Pts',(0.00504225801885261,-0.0341934961088741,
0.0692955701131324));
#99586=CARTESIAN_POINT('Ctrl Pts',(0.00473319151700071,-0.0345231616327822,
0.0694045741564275));
#99587=CARTESIAN_POINT('Ctrl Pts',(0.00479860053122876,-0.0344132092796975,
0.0693578396375275));
#99588=CARTESIAN_POINT('Ctrl Pts',(0.00486497283731212,-0.0343032738558974,
0.0693124604637792));
#99589=CARTESIAN_POINT('Ctrl Pts',(0.00493222191548151,-0.0341934961088741,
0.0692684925930581));
#99590=CARTESIAN_POINT('Ctrl Pts',(0.00462213029761071,-0.0345231616327822,
0.0693820676754481));
#99591=CARTESIAN_POINT('Ctrl Pts',(0.00468784953199247,-0.0344132092796975,
0.0693338023340005));
#99592=CARTESIAN_POINT('Ctrl Pts',(0.00475456370608051,-0.0343032738558974,
0.0692868988333472));
#99593=CARTESIAN_POINT('Ctrl Pts',(0.00482218581211042,-0.0341934961088741,
0.0692414150729838));
#99594=CARTESIAN_POINT('Ctrl Pts',(0.00451106907822071,-0.0345231616327822,
0.0693595611944686));
#99595=CARTESIAN_POINT('Ctrl Pts',(0.00457709853275618,-0.0344132092796975,
0.0693097650304734));
#99596=CARTESIAN_POINT('Ctrl Pts',(0.00464415457484889,-0.0343032738558974,
0.0692613372029152));
#99597=CARTESIAN_POINT('Ctrl Pts',(0.00471214970873932,-0.0341934961088741,
0.0692143375529095));
#99598=CARTESIAN_POINT('Origin',(0.0144742514056604,-0.034562559623074,
0.0831947141691753));
#99599=CARTESIAN_POINT('Ctrl Pts',(0.00500686402026084,-0.0346945769586885,
0.0690231275514409));
#99600=CARTESIAN_POINT('Ctrl Pts',(0.00507751491392863,-0.034584662917669,
0.0689801748436039));
#99601=CARTESIAN_POINT('Ctrl Pts',(0.0051490661193006,-0.0344746925051586,
0.0689386758308042));
#99602=CARTESIAN_POINT('Ctrl Pts',(0.00522142573712908,-0.0343648066255171,
0.0688986833077355));
#99603=CARTESIAN_POINT('Ctrl Pts',(0.00498674916698599,-0.0346945769586885,
0.0691346466720407));
#99604=CARTESIAN_POINT('Ctrl Pts',(0.00505586327080568,-0.034584662917669,
0.0690914167713586));
#99605=CARTESIAN_POINT('Ctrl Pts',(0.00512588315607627,-0.0344746925051586,
0.0690496087381858));
#99606=CARTESIAN_POINT('Ctrl Pts',(0.00519671888401862,-0.0343648066255171,
0.0690092757712716));
#99607=CARTESIAN_POINT('Ctrl Pts',(0.00496663431371114,-0.0346945769586885,
0.0692461657926404));
#99608=CARTESIAN_POINT('Ctrl Pts',(0.00503421162768274,-0.034584662917669,
0.0692026586991134));
#99609=CARTESIAN_POINT('Ctrl Pts',(0.00510270019285194,-0.0344746925051586,
0.0691605416455675));
#99610=CARTESIAN_POINT('Ctrl Pts',(0.00517201203090817,-0.0343648066255171,
0.0691198682348077));
#99611=CARTESIAN_POINT('Ctrl Pts',(0.00494651946043629,-0.0346945769586885,
0.0693576849132402));
#99612=CARTESIAN_POINT('Ctrl Pts',(0.0050125599845598,-0.034584662917669,
0.0693139006268682));
#99613=CARTESIAN_POINT('Ctrl Pts',(0.00507951722962762,-0.0344746925051586,
0.0692714745529491));
#99614=CARTESIAN_POINT('Ctrl Pts',(0.00514730517779772,-0.0343648066255171,
0.0692304606983438));
#99615=CARTESIAN_POINT('Origin',(0.0140812105975753,-0.0345626446730884,
0.083471681867596));
#99616=CARTESIAN_POINT('Ctrl Pts',(0.00494687938261152,-0.0346945769586885,
0.069355689462221));
#99617=CARTESIAN_POINT('Ctrl Pts',(0.00504729813636091,-0.0345275153362891,
0.0692891479608938));
#99618=CARTESIAN_POINT('Ctrl Pts',(0.00514983553251299,-0.0343603235965159,
0.0692257473259022));
#99619=CARTESIAN_POINT('Ctrl Pts',(0.00525418552406562,-0.034193496108874,
0.0691656705609461));
#99620=CARTESIAN_POINT('Ctrl Pts',(0.0048780191845862,-0.0346945769586885,
0.0694035047470073));
#99621=CARTESIAN_POINT('Ctrl Pts',(0.00497743642805156,-0.0345275153362891,
0.0693355209412622));
#99622=CARTESIAN_POINT('Ctrl Pts',(0.00507901741402414,-0.0343603235965159,
0.0692706461322225));
#99623=CARTESIAN_POINT('Ctrl Pts',(0.00518245885933831,-0.034193496108874,
0.0692090677255812));
#99624=CARTESIAN_POINT('Ctrl Pts',(0.00480915898656087,-0.0346945769586885,
0.0694513200317935));
#99625=CARTESIAN_POINT('Ctrl Pts',(0.00490757471974221,-0.0345275153362891,
0.0693818939216307));
#99626=CARTESIAN_POINT('Ctrl Pts',(0.0050081992955353,-0.0343603235965159,
0.0693155449385429));
#99627=CARTESIAN_POINT('Ctrl Pts',(0.00511073219461101,-0.034193496108874,
0.0692524648902163));
#99628=CARTESIAN_POINT('Ctrl Pts',(0.00474029878853555,-0.0346945769586885,
0.0694991353165797));
#99629=CARTESIAN_POINT('Ctrl Pts',(0.00483771301143286,-0.0345275153362891,
0.0694282669019992));
#99630=CARTESIAN_POINT('Ctrl Pts',(0.00493738117704646,-0.0343603235965159,
0.0693604437448632));
#99631=CARTESIAN_POINT('Ctrl Pts',(0.00503900552988371,-0.034193496108874,
0.0692958620548515));
#99632=CARTESIAN_POINT('Ctrl Pts',(0.00514727846869623,-0.0340223579322365,
0.0692304775090728));
#99633=CARTESIAN_POINT('Ctrl Pts',(0.00521513151449874,-0.0339125849573554,
0.0691894237596659));
#99634=CARTESIAN_POINT('Ctrl Pts',(0.00528378659796856,-0.0338030433565221,
0.0691498032586328));
#99635=CARTESIAN_POINT('Ctrl Pts',(0.00535315142932657,-0.0336938721132328,
0.0691116588909678));
#99636=CARTESIAN_POINT('Ctrl Pts',(0.00503784940600099,-0.0340223579322365,
0.0692010418152985));
#99637=CARTESIAN_POINT('Ctrl Pts',(0.00510610844679215,-0.0339125849573554,
0.0691584787537141));
#99638=CARTESIAN_POINT('Ctrl Pts',(0.00517520047921756,-0.0338030433565221,
0.0691173584042325));
#99639=CARTESIAN_POINT('Ctrl Pts',(0.00524503248468668,-0.0336938721132328,
0.0690777255203675));
#99640=CARTESIAN_POINT('Ctrl Pts',(0.00492842034330574,-0.0340223579322365,
0.0691716061215241));
#99641=CARTESIAN_POINT('Ctrl Pts',(0.00499708537908556,-0.0339125849573554,
0.0691275337477622));
#99642=CARTESIAN_POINT('Ctrl Pts',(0.00506661436046656,-0.0338030433565221,
0.0690849135498322));
#99643=CARTESIAN_POINT('Ctrl Pts',(0.0051369135400468,-0.0336938721132328,
0.0690437921497672));
#99644=CARTESIAN_POINT('Ctrl Pts',(0.00481899128061049,-0.0340223579322365,
0.0691421704277498));
#99645=CARTESIAN_POINT('Ctrl Pts',(0.00488806231137896,-0.0339125849573554,
0.0690965887418104));
#99646=CARTESIAN_POINT('Ctrl Pts',(0.00495802824171557,-0.0338030433565221,
0.0690524686954319));
#99647=CARTESIAN_POINT('Ctrl Pts',(0.00502879459540692,-0.0336938721132328,
0.069009858779167));
#99648=CARTESIAN_POINT('Origin',(0.01440730785072,-0.0345589643417286,0.0830948570790016));
#99649=CARTESIAN_POINT('Ctrl Pts',(0.00533493353088826,-0.034193496108874,
0.0688375313516922));
#99650=CARTESIAN_POINT('Ctrl Pts',(0.00540818932669617,-0.0340836138595105,
0.0687990747806207));
#99651=CARTESIAN_POINT('Ctrl Pts',(0.00548220575103187,-0.0339738896671456,
0.0687621525366981));
#99652=CARTESIAN_POINT('Ctrl Pts',(0.00555688490421961,-0.0338644633335883,
0.0687268055254937));
#99653=CARTESIAN_POINT('Ctrl Pts',(0.00530785598645012,-0.034193496108874,
0.0689475675540716));
#99654=CARTESIAN_POINT('Ctrl Pts',(0.0053795944482074,-0.0340836138595105,
0.0689087375997018));
#99655=CARTESIAN_POINT('Ctrl Pts',(0.00545210199292166,-0.0339738896671456,
0.0688714107535931));
#99656=CARTESIAN_POINT('Ctrl Pts',(0.00552528261738328,-0.0338644633335883,
0.0688356285686123));
#99657=CARTESIAN_POINT('Ctrl Pts',(0.00528077844201199,-0.034193496108874,
0.069057603756451));
#99658=CARTESIAN_POINT('Ctrl Pts',(0.00535099956971864,-0.0340836138595105,
0.0690184004187828));
#99659=CARTESIAN_POINT('Ctrl Pts',(0.00542199823481146,-0.0339738896671456,
0.0689806689704882));
#99660=CARTESIAN_POINT('Ctrl Pts',(0.00549368033054695,-0.0338644633335883,
0.0689444516117309));
#99661=CARTESIAN_POINT('Ctrl Pts',(0.00525370089757385,-0.034193496108874,
0.0691676399588304));
#99662=CARTESIAN_POINT('Ctrl Pts',(0.00532240469122988,-0.0340836138595105,
0.0691280632378638));
#99663=CARTESIAN_POINT('Ctrl Pts',(0.00539189447670125,-0.0339738896671456,
0.0690899271873832));
#99664=CARTESIAN_POINT('Ctrl Pts',(0.00546207804371062,-0.0338644633335883,
0.0690532746548495));
#99665=CARTESIAN_POINT('Origin',(0.0140416393589376,-0.0345610621863313,
0.0834076454514424));
#99666=CARTESIAN_POINT('Ctrl Pts',(0.0052228897417699,-0.03424362768739,
0.0691838195778075));
#99667=CARTESIAN_POINT('Ctrl Pts',(0.00541019232411137,-0.033943005420186,
0.0690744106153777));
#99668=CARTESIAN_POINT('Ctrl Pts',(0.00560520393079155,-0.0336441434784162,
0.0689794208702906));
#99669=CARTESIAN_POINT('Ctrl Pts',(0.00500981141681051,-0.03424362768739,
0.0693145774740604));
#99670=CARTESIAN_POINT('Ctrl Pts',(0.00519218238379618,-0.033943005420186,
0.0691971321301237));
#99671=CARTESIAN_POINT('Ctrl Pts',(0.00538288171850594,-0.0336441434784162,
0.0690937573645715));
#99672=CARTESIAN_POINT('Ctrl Pts',(0.00546205352410219,-0.0335235895815127,
0.0690532876027717));
#99673=CARTESIAN_POINT('Ctrl Pts',(0.00553221980475236,-0.0334144449262719,
0.0690166436671819));
#99674=CARTESIAN_POINT('Ctrl Pts',(0.00560322373408977,-0.0333049234473132,
0.0689814072147018));
#99675=CARTESIAN_POINT('Ctrl Pts',(0.00567497860131031,-0.0331951640388588,
0.0689476315262886));
#99676=CARTESIAN_POINT('Ctrl Pts',(0.00535468872440273,-0.0335235895815127,
0.0690170388473202));
#99677=CARTESIAN_POINT('Ctrl Pts',(0.00542535404053891,-0.0334144449262719,
0.0689789168238806));
#99678=CARTESIAN_POINT('Ctrl Pts',(0.00549688811487624,-0.0333049234473132,
0.0689422108951045));
#99679=CARTESIAN_POINT('Ctrl Pts',(0.00556920372892668,-0.0331951640388588,
0.0689069762823646));
#99680=CARTESIAN_POINT('Ctrl Pts',(0.00524732392470326,-0.0335235895815127,
0.0689807900918687));
#99681=CARTESIAN_POINT('Ctrl Pts',(0.00531848827632547,-0.0334144449262719,
0.0689411899805794));
#99682=CARTESIAN_POINT('Ctrl Pts',(0.00539055249566271,-0.0333049234473132,
0.0689030145755074));
#99683=CARTESIAN_POINT('Ctrl Pts',(0.00546342885654305,-0.0331951640388588,
0.0688663210384406));
#99684=CARTESIAN_POINT('Ctrl Pts',(0.0051399591250038,-0.0335235895815127,
0.0689445413364172));
#99685=CARTESIAN_POINT('Ctrl Pts',(0.00521162251211202,-0.0334144449262719,
0.0689034631372782));
#99686=CARTESIAN_POINT('Ctrl Pts',(0.00528421687644918,-0.0333049234473132,
0.0688638182559102));
#99687=CARTESIAN_POINT('Ctrl Pts',(0.00535765398415942,-0.0331951640388588,
0.0688256657945166));
#99688=CARTESIAN_POINT('Origin',(0.0120771875754346,-0.0326434571770968,
0.0843360219986812));
#99689=CARTESIAN_POINT('Ctrl Pts',(0.00567461650928284,-0.0336938721132354,
0.0686709665097099));
#99690=CARTESIAN_POINT('Ctrl Pts',(0.00570668711043635,-0.033647456976494,
0.0686566307302437));
#99691=CARTESIAN_POINT('Ctrl Pts',(0.00573892333249069,-0.033601104548885,
0.0686426713599529));
#99692=CARTESIAN_POINT('Ctrl Pts',(0.00582053802807421,-0.033483750869459,
0.0686073294469058));
#99693=CARTESIAN_POINT('Ctrl Pts',(0.00590316413857309,-0.0333660264863565,
0.0685744214658548));
#99694=CARTESIAN_POINT('Ctrl Pts',(0.00557281665257666,-0.0336938721132354,
0.0689953225308444));
#99695=CARTESIAN_POINT('Ctrl Pts',(0.0056029886903058,-0.033647456976494,
0.0689803908830361));
#99696=CARTESIAN_POINT('Ctrl Pts',(0.00563333345441785,-0.033601104548885,
0.0689658134601506));
#99697=CARTESIAN_POINT('Ctrl Pts',(0.00571015941378067,-0.033483750869459,
0.0689289067801685));
#99698=CARTESIAN_POINT('Ctrl Pts',(0.00578804525820308,-0.0333660264863565,
0.0688942928191422));
#99699=CARTESIAN_POINT('Ctrl Pts',(0.00557281665258841,-0.0336938721132427,
0.0689953225308535));
#99700=CARTESIAN_POINT('Ctrl Pts',(0.00560298869031667,-0.0336474569765026,
0.0689803908830456));
#99701=CARTESIAN_POINT('Ctrl Pts',(0.00563333345442785,-0.0336011045488949,
0.0689658134601606));
#99702=CARTESIAN_POINT('Ctrl Pts',(0.00570951955818085,-0.033484728265791,
0.0689292141625584));
#99703=CARTESIAN_POINT('Ctrl Pts',(0.00578674824582927,-0.0333679870047996,
0.0688948694279671));
#99704=CARTESIAN_POINT('Ctrl Pts',(0.00557281665257206,-0.0336938721132425,
0.0689953225308467));
#99705=CARTESIAN_POINT('Ctrl Pts',(0.00568072521195011,-0.0335278710435082,
0.0689419203503709));
#99706=CARTESIAN_POINT('Ctrl Pts',(0.00579027048784295,-0.0333620469224319,
0.0688919209410244));
#99707=CARTESIAN_POINT('Ctrl Pts',(0.00590151527665343,-0.0331951640388602,
0.068845317657764));
#99708=CARTESIAN_POINT('Ctrl Pts',(0.00549850658563194,-0.0336938721132425,
0.0690341303106676));
#99709=CARTESIAN_POINT('Ctrl Pts',(0.00560560273887242,-0.0335278710435082,
0.068979172515448));
#99710=CARTESIAN_POINT('Ctrl Pts',(0.0057143846781042,-0.0333620469224319,
0.068927592561774));
#99711=CARTESIAN_POINT('Ctrl Pts',(0.00582491508299913,-0.0331951640388602,
0.0688793828915867));
#99712=CARTESIAN_POINT('Ctrl Pts',(0.00542419651869182,-0.0336938721132425,
0.0690729380904886));
#99713=CARTESIAN_POINT('Ctrl Pts',(0.00553048026579473,-0.0335278710435082,
0.069016424680525));
#99714=CARTESIAN_POINT('Ctrl Pts',(0.00563849886836544,-0.0333620469224319,
0.0689632641825236));
#99715=CARTESIAN_POINT('Ctrl Pts',(0.00574831488934483,-0.0331951640388602,
0.0689134481254095));
#99716=CARTESIAN_POINT('Ctrl Pts',(0.0053498864517517,-0.0336938721132425,
0.0691117458703095));
#99717=CARTESIAN_POINT('Ctrl Pts',(0.00545535779271704,-0.0335278710435082,
0.069053676845602));
#99718=CARTESIAN_POINT('Ctrl Pts',(0.00556261305862668,-0.0333620469224319,
0.0689989358032733));
#99719=CARTESIAN_POINT('Ctrl Pts',(0.00567171469569052,-0.0331951640388602,
0.0689475133592322));
#99720=CARTESIAN_POINT('Ctrl Pts',(0.00578732976821152,-0.0330240426238155,
0.0688962136657319));
#99721=CARTESIAN_POINT('Ctrl Pts',(0.00585970579348169,-0.0329142774063509,
0.0688640267572839));
#99722=CARTESIAN_POINT('Ctrl Pts',(0.00593278329414736,-0.0328043479726686,
0.0688333200171028));
#99723=CARTESIAN_POINT('Ctrl Pts',(0.00600646973583871,-0.0326943950436594,
0.0688041353610254));
#99724=CARTESIAN_POINT('Ctrl Pts',(0.00568245304879065,-0.0330240426238155,
0.0688532950251651));
#99725=CARTESIAN_POINT('Ctrl Pts',(0.00575542032014823,-0.0329142774063509,
0.0688196633377306));
#99726=CARTESIAN_POINT('Ctrl Pts',(0.00582911922927649,-0.0328043479726686,
0.0687875233209962));
#99727=CARTESIAN_POINT('Ctrl Pts',(0.00590345649630189,-0.0326943950436594,
0.0687569187488564));
#99728=CARTESIAN_POINT('Ctrl Pts',(0.00557757632936978,-0.0330240426238155,
0.0688103763845982));
#99729=CARTESIAN_POINT('Ctrl Pts',(0.00565113484681477,-0.0329142774063509,
0.0687752999181773));
#99730=CARTESIAN_POINT('Ctrl Pts',(0.00572545516440562,-0.0328043479726686,
0.0687417266248897));
#99731=CARTESIAN_POINT('Ctrl Pts',(0.00580044325676507,-0.0326943950436594,
0.0687097021366873));
#99732=CARTESIAN_POINT('Ctrl Pts',(0.0054726996099489,-0.0330240426238155,
0.0687674577440314));
#99733=CARTESIAN_POINT('Ctrl Pts',(0.00554684937348131,-0.0329142774063509,
0.068730936498624));
#99734=CARTESIAN_POINT('Ctrl Pts',(0.00562179109953475,-0.0328043479726686,
0.0686959299287831));
#99735=CARTESIAN_POINT('Ctrl Pts',(0.00569743001722824,-0.0326943950436594,
0.0686624855245183));
#99736=CARTESIAN_POINT('Origin',(0.0121245010631098,-0.0326396682854783,
0.0844502884958673));
#99737=CARTESIAN_POINT('Ctrl Pts',(0.00602275330947993,-0.0331951640388587,
0.0685298863329841));
#99738=CARTESIAN_POINT('Ctrl Pts',(0.00610015901485808,-0.0330855618127431,
0.0685009489070897));
#99739=CARTESIAN_POINT('Ctrl Pts',(0.00617821860813228,-0.0329757224171935,
0.0684735904644101));
#99740=CARTESIAN_POINT('Ctrl Pts',(0.00625683384778119,-0.0328657861694598,
0.0684478509423289));
#99741=CARTESIAN_POINT('Ctrl Pts',(0.00598209809792321,-0.0331951640388587,
0.0686356611211562));
#99742=CARTESIAN_POINT('Ctrl Pts',(0.00605804696940533,-0.0330855618127431,
0.0686061637519023));
#99743=CARTESIAN_POINT('Ctrl Pts',(0.00613466025164563,-0.0329757224171935,
0.0685782148519377));
#99744=CARTESIAN_POINT('Ctrl Pts',(0.00621184159230039,-0.0328657861694598,
0.0685518550239138));
#99745=CARTESIAN_POINT('Ctrl Pts',(0.00594144288636649,-0.0331951640388587,
0.0687414359093283));
#99746=CARTESIAN_POINT('Ctrl Pts',(0.00601593492395257,-0.0330855618127431,
0.0687113785967148));
#99747=CARTESIAN_POINT('Ctrl Pts',(0.00609110189515898,-0.0329757224171935,
0.0686828392394654));
#99748=CARTESIAN_POINT('Ctrl Pts',(0.00616684933681959,-0.0328657861694598,
0.0686558591054987));
#99749=CARTESIAN_POINT('Ctrl Pts',(0.00590078767480977,-0.0331951640388587,
0.0688472106975004));
#99750=CARTESIAN_POINT('Ctrl Pts',(0.00597382287849982,-0.0330855618127431,
0.0688165934415273));
#99751=CARTESIAN_POINT('Ctrl Pts',(0.00604754353867233,-0.0329757224171935,
0.0687874636269931));
#99752=CARTESIAN_POINT('Ctrl Pts',(0.0061218570813388,-0.0328657861694598,
0.0687598631870836));
#99753=CARTESIAN_POINT('Origin',(0.0116637048409317,-0.0326401908832987,
0.084587910124528));
#99754=CARTESIAN_POINT('Ctrl Pts',(0.00586825825960548,-0.0332451089994432,
0.0688593727417823));
#99755=CARTESIAN_POINT('Ctrl Pts',(0.00606779753128231,-0.0329451141710258,
0.0687743042648371));
#99756=CARTESIAN_POINT('Ctrl Pts',(0.00627317763839391,-0.0326442513127503,
0.0687045075721225));
#99757=CARTESIAN_POINT('Ctrl Pts',(0.00564047051284638,-0.0332451089994432,
0.0689623909072989));
#99758=CARTESIAN_POINT('Ctrl Pts',(0.00583612439084238,-0.0329451141710258,
0.0688687312749261));
#99759=CARTESIAN_POINT('Ctrl Pts',(0.00603827726321428,-0.0326442513127503,
0.068790075169614));
#99760=CARTESIAN_POINT('Ctrl Pts',(0.00612182741298092,-0.0325229783203384,
0.0687598741104088));
#99761=CARTESIAN_POINT('Ctrl Pts',(0.0061961301791422,-0.0324130253112079,
0.068732277208047));
#99762=CARTESIAN_POINT('Ctrl Pts',(0.00627099255319903,-0.0323031222247695,
0.0687062215394347));
#99763=CARTESIAN_POINT('Ctrl Pts',(0.00634631746406593,-0.0321934096636184,
0.0686817370962685));
#99764=CARTESIAN_POINT('Ctrl Pts',(0.00601985249317014,-0.0325229783203384,
0.0687104548997822));
#99765=CARTESIAN_POINT('Ctrl Pts',(0.00609483650205677,-0.0324130253112079,
0.0686814522754064));
#99766=CARTESIAN_POINT('Ctrl Pts',(0.00617040909468027,-0.0323031222247695,
0.0686540051903661));
#99767=CARTESIAN_POINT('Ctrl Pts',(0.00624647222732398,-0.0321934096636184,
0.0686281453865616));
#99768=CARTESIAN_POINT('Ctrl Pts',(0.00591787757335935,-0.0325229783203384,
0.0686610356891557));
#99769=CARTESIAN_POINT('Ctrl Pts',(0.00599354282497134,-0.0324130253112079,
0.0686306273427659));
#99770=CARTESIAN_POINT('Ctrl Pts',(0.0060698256361615,-0.0323031222247695,
0.0686017888412976));
#99771=CARTESIAN_POINT('Ctrl Pts',(0.00614662699058202,-0.0321934096636184,
0.0685745536768546));
#99772=CARTESIAN_POINT('Ctrl Pts',(0.00581590265354856,-0.0325229783203384,
0.0686116164785291));
#99773=CARTESIAN_POINT('Ctrl Pts',(0.00589224914788592,-0.0324130253112079,
0.0685798024101254));
#99774=CARTESIAN_POINT('Ctrl Pts',(0.00596924217764273,-0.0323031222247695,
0.068549572492229));
#99775=CARTESIAN_POINT('Ctrl Pts',(0.00604678175384007,-0.0321934096636184,
0.0685209619671477));
#99776=CARTESIAN_POINT('Origin',(0.0121216376506533,-0.0326393375177596,
0.0844422578116633));
#99777=CARTESIAN_POINT('Ctrl Pts',(0.00637978906701306,-0.0326943950436593,
0.0684090516483641));
#99778=CARTESIAN_POINT('Ctrl Pts',(0.00645891009498231,-0.0325844576448126,
0.0683850161544951));
#99779=CARTESIAN_POINT('Ctrl Pts',(0.00653853381588957,-0.0324744968375319,
0.068362615312176));
#99780=CARTESIAN_POINT('Ctrl Pts',(0.00661855781530343,-0.0323646534831894,
0.0683418764155297));
#99781=CARTESIAN_POINT('Ctrl Pts',(0.00633257247029293,-0.0326943950436593,
0.0685120648541959));
#99782=CARTESIAN_POINT('Ctrl Pts',(0.00641027378321849,-0.0325844576448126,
0.0684873786271307));
#99783=CARTESIAN_POINT('Ctrl Pts',(0.00648849114683602,-0.0324744968375319,
0.0684642976435273));
#99784=CARTESIAN_POINT('Ctrl Pts',(0.00656712393660134,-0.0323646534831894,
0.0684428500937989));
#99785=CARTESIAN_POINT('Ctrl Pts',(0.0062853558735728,-0.0326943950436593,
0.0686150780600276));
#99786=CARTESIAN_POINT('Ctrl Pts',(0.00636163747145468,-0.0325844576448126,
0.0685897410997663));
#99787=CARTESIAN_POINT('Ctrl Pts',(0.00643844847778248,-0.0324744968375319,
0.0685659799748785));
#99788=CARTESIAN_POINT('Ctrl Pts',(0.00651569005789925,-0.0323646534831894,
0.0685438237720681));
#99789=CARTESIAN_POINT('Ctrl Pts',(0.00623813927685267,-0.0326943950436593,
0.0687180912658593));
#99790=CARTESIAN_POINT('Ctrl Pts',(0.00631300115969087,-0.0325844576448126,
0.0686921035724019));
#99791=CARTESIAN_POINT('Ctrl Pts',(0.00638840580872893,-0.0324744968375319,
0.0686676623062299));
#99792=CARTESIAN_POINT('Ctrl Pts',(0.00646425617919717,-0.0323646534831894,
0.0686447974503374));
#99793=CARTESIAN_POINT('Origin',(0.0116762912092995,-0.032639557906863,
0.0846235968853021));
#99794=CARTESIAN_POINT('Ctrl Pts',(0.00620487327920245,-0.0327445246961877,
0.0687282001530734));
#99795=CARTESIAN_POINT('Ctrl Pts',(0.00640935980120099,-0.0324436878365475,
0.0686558273210038));
#99796=CARTESIAN_POINT('Ctrl Pts',(0.00661871681604563,-0.0321434074463186,
0.0685990628529258));
#99797=CARTESIAN_POINT('Ctrl Pts',(0.00597106705903739,-0.0327445246961877,
0.0688167137193337));
#99798=CARTESIAN_POINT('Ctrl Pts',(0.00617221523734467,-0.0324436878365475,
0.0687355227416054));
#99799=CARTESIAN_POINT('Ctrl Pts',(0.00637890761114403,-0.0321434074463186,
0.0686697137216004));
#99800=CARTESIAN_POINT('Ctrl Pts',(0.00655447739320943,-0.0322357242816072,
0.0686168808575076));
#99801=CARTESIAN_POINT('Ctrl Pts',(0.00673070006170515,-0.0319819883628706,
0.0685669005349447));
#99802=CARTESIAN_POINT('Ctrl Pts',(0.0069097459840021,-0.0317295851069887,
0.068528235056232));
#99803=CARTESIAN_POINT('Ctrl Pts',(0.00631550320732872,-0.0322357242816072,
0.0686903065919789));
#99804=CARTESIAN_POINT('Ctrl Pts',(0.00648938736141121,-0.0319819883628706,
0.0686327152515338));
#99805=CARTESIAN_POINT('Ctrl Pts',(0.00666658381942561,-0.0317295851069887,
0.0685863053732491));
#99806=CARTESIAN_POINT('Origin',(0.0116472978938751,-0.0326371942647044,
0.0845328125743387));
#99807=CARTESIAN_POINT('Origin',(0.0120799268622383,-0.032635298552708,
0.0843268281231969));
#99808=CARTESIAN_POINT('Ctrl Pts',(0.00674370756866054,-0.0321934096636183,
0.0683108738640975));
#99809=CARTESIAN_POINT('Ctrl Pts',(0.0068242336688127,-0.0320835708272303,
0.0682918415594616));
#99810=CARTESIAN_POINT('Ctrl Pts',(0.00690510693310943,-0.0319739230346346,
0.0682744867777932));
#99811=CARTESIAN_POINT('Ctrl Pts',(0.00698622218570662,-0.0318646057455575,
0.0682588237821651));
#99812=CARTESIAN_POINT('Ctrl Pts',(0.00669011581280508,-0.0321934096636183,
0.0684107191868175));
#99813=CARTESIAN_POINT('Ctrl Pts',(0.00676926496814222,-0.0320835708272303,
0.0683909478101015));
#99814=CARTESIAN_POINT('Ctrl Pts',(0.00684877738136617,-0.0319739230346346,
0.0683728258892434));
#99815=CARTESIAN_POINT('Ctrl Pts',(0.00692854954241986,-0.0318646057455575,
0.0683563688024431));
#99816=CARTESIAN_POINT('Ctrl Pts',(0.00663652405694963,-0.0321934096636183,
0.0685105645095375));
#99817=CARTESIAN_POINT('Ctrl Pts',(0.00671429626747175,-0.0320835708272303,
0.0684900540607413));
#99818=CARTESIAN_POINT('Ctrl Pts',(0.00679244782962291,-0.0319739230346346,
0.0684711650006936));
#99819=CARTESIAN_POINT('Ctrl Pts',(0.00687087689913309,-0.0318646057455575,
0.0684539138227211));
#99820=CARTESIAN_POINT('Ctrl Pts',(0.00658293230109417,-0.0321934096636183,
0.0686104098322574));
#99821=CARTESIAN_POINT('Ctrl Pts',(0.00665932756680127,-0.0320835708272303,
0.0685891603113812));
#99822=CARTESIAN_POINT('Ctrl Pts',(0.00673611827787965,-0.0319739230346346,
0.0685695041121437));
#99823=CARTESIAN_POINT('Ctrl Pts',(0.00681320425584633,-0.0318646057455575,
0.0685514588429991));
#99824=CARTESIAN_POINT('Ctrl Pts',(0.0064635676040236,-0.0320218834582358,
0.0686441408192202));
#99825=CARTESIAN_POINT('Ctrl Pts',(0.00652087028776568,-0.0319391099350663,
0.0686268619988911));
#99826=CARTESIAN_POINT('Ctrl Pts',(0.00657840806446979,-0.0318564869454954,
0.0686104884368015));
#99827=CARTESIAN_POINT('Ctrl Pts',(0.0066361379121258,-0.0317740741446555,
0.0685950281464577));
#99828=CARTESIAN_POINT('Ctrl Pts',(0.00642040989459936,-0.0320218834582358,
0.0686197637774708));
#99829=CARTESIAN_POINT('Ctrl Pts',(0.00647796628441493,-0.0319391099350663,
0.0686020357897196));
#99830=CARTESIAN_POINT('Ctrl Pts',(0.00653576462729074,-0.0318564869454954,
0.0685852172940031));
#99831=CARTESIAN_POINT('Ctrl Pts',(0.00659376168117411,-0.0317740741446555,
0.0685693166101845));
#99832=CARTESIAN_POINT('Ctrl Pts',(0.00637725218517513,-0.0320218834582358,
0.0685953867357213));
#99833=CARTESIAN_POINT('Ctrl Pts',(0.00643506228106419,-0.0319391099350663,
0.0685772095805482));
#99834=CARTESIAN_POINT('Ctrl Pts',(0.00649312119011169,-0.0318564869454954,
0.0685599461512047));
#99835=CARTESIAN_POINT('Ctrl Pts',(0.00655138545022241,-0.0317740741446555,
0.0685436050739113));
#99836=CARTESIAN_POINT('Ctrl Pts',(0.00633409447575089,-0.0320218834582358,
0.0685710096939719));
#99837=CARTESIAN_POINT('Ctrl Pts',(0.00639215827771344,-0.0319391099350663,
0.0685523833713767));
#99838=CARTESIAN_POINT('Ctrl Pts',(0.00645047775293264,-0.0318564869454954,
0.0685346750084063));
#99839=CARTESIAN_POINT('Ctrl Pts',(0.00650900921927072,-0.0317740741446555,
0.0685178935376381));
#99840=CARTESIAN_POINT('Origin',(0.00374573569064397,-0.0391228853390723,
0.0628932985669952));
#99841=CARTESIAN_POINT('Ctrl Pts',(0.00389106271677981,-0.0352722978779586,
0.0702553561937829));
#99842=CARTESIAN_POINT('Ctrl Pts',(0.00390411340789216,-0.0352466642097211,
0.0702416897333956));
#99843=CARTESIAN_POINT('Ctrl Pts',(0.00391709577180745,-0.0352210183808299,
0.0702279813024733));
#99844=CARTESIAN_POINT('Ctrl Pts',(0.00393000988001004,-0.0351953608940152,
0.0702142300510901));
#99845=CARTESIAN_POINT('Origin',(0.000474874517336402,-0.0352456003065064,
0.066742607785333));
#99846=CARTESIAN_POINT('Ctrl Pts',(0.00401735610000403,-0.035024121149334,
0.0701252584080182));
#99847=CARTESIAN_POINT('Ctrl Pts',(0.00407279526272551,-0.0349144232867422,
0.0700686940748364));
#99848=CARTESIAN_POINT('Ctrl Pts',(0.0041294368335894,-0.0348045283677512,
0.0700132418522327));
#99849=CARTESIAN_POINT('Ctrl Pts',(0.00418721090503603,-0.0346945769586886,
0.0699589754672298));
#99850=CARTESIAN_POINT('Ctrl Pts',(0.00390404476136973,-0.035024121149334,
0.0701239613575513));
#99851=CARTESIAN_POINT('Ctrl Pts',(0.00395950179042877,-0.0349144232867422,
0.0700658362072097));
#99852=CARTESIAN_POINT('Ctrl Pts',(0.00401619350152863,-0.0348045283677512,
0.0700088226025319));
#99853=CARTESIAN_POINT('Ctrl Pts',(0.00407404999730846,-0.0346945769586886,
0.0699529962728622));
#99854=CARTESIAN_POINT('Ctrl Pts',(0.00379073342273543,-0.035024121149334,
0.0701226643070845));
#99855=CARTESIAN_POINT('Ctrl Pts',(0.00384620831813203,-0.0349144232867422,
0.070062978339583));
#99856=CARTESIAN_POINT('Ctrl Pts',(0.00390295016946786,-0.0348045283677512,
0.070004403352831));
#99857=CARTESIAN_POINT('Ctrl Pts',(0.0039608890895809,-0.0346945769586886,
0.0699470170784946));
#99858=CARTESIAN_POINT('Ctrl Pts',(0.00367742208410113,-0.035024121149334,
0.0701213672566176));
#99859=CARTESIAN_POINT('Ctrl Pts',(0.00373291484583529,-0.0349144232867422,
0.0700601204719563));
#99860=CARTESIAN_POINT('Ctrl Pts',(0.00378970683740709,-0.0348045283677512,
0.0699999841031302));
#99861=CARTESIAN_POINT('Ctrl Pts',(0.00384772818185334,-0.0346945769586886,
0.0699410378841271));
#99862=CARTESIAN_POINT('Origin',(0.0155494541559422,-0.0345629067942227,
0.0823186832866856));
#99863=CARTESIAN_POINT('Ctrl Pts',(0.00410124984194354,-0.0351970973651652,
0.0697917027108022));
#99864=CARTESIAN_POINT('Ctrl Pts',(0.00416162814434792,-0.0350869349321791,
0.0697359759765723));
#99865=CARTESIAN_POINT('Ctrl Pts',(0.004223214991358,-0.0349764985129724,
0.0696814583104115));
#99866=CARTESIAN_POINT('Ctrl Pts',(0.00428593475305483,-0.0348659306849626,
0.0696282250383206));
#99867=CARTESIAN_POINT('Ctrl Pts',(0.00410209584850038,-0.0351970973651652,
0.0698739204395653));
#99868=CARTESIAN_POINT('Ctrl Pts',(0.00416133513569748,-0.0350869349321791,
0.0698182054256097));
#99869=CARTESIAN_POINT('Ctrl Pts',(0.00422178178029532,-0.0349764985129724,
0.0697636758099372));
#99870=CARTESIAN_POINT('Ctrl Pts',(0.00428336163045199,-0.0348659306849626,
0.0697104068470749));
#99871=CARTESIAN_POINT('Ctrl Pts',(0.00410294185505723,-0.0351970973651652,
0.0699561381683284));
#99872=CARTESIAN_POINT('Ctrl Pts',(0.00416104212704704,-0.0350869349321791,
0.0699004348746471));
#99873=CARTESIAN_POINT('Ctrl Pts',(0.00422034856923265,-0.0349764985129724,
0.0698458933094629));
#99874=CARTESIAN_POINT('Ctrl Pts',(0.00428078850784914,-0.0348659306849626,
0.0697925886558292));
#99875=CARTESIAN_POINT('Ctrl Pts',(0.00410378786161407,-0.0351970973651652,
0.0700383558970915));
#99876=CARTESIAN_POINT('Ctrl Pts',(0.0041607491183966,-0.0350869349321791,
0.0699826643236845));
#99877=CARTESIAN_POINT('Ctrl Pts',(0.00421891535816998,-0.0349764985129724,
0.0699281108089885));
#99878=CARTESIAN_POINT('Ctrl Pts',(0.00427821538524629,-0.0348659306849626,
0.0698747704645834));
#99879=CARTESIAN_POINT('Origin',(0.0151645710067182,-0.0345637187965536,
0.0826071106048243));
#99880=CARTESIAN_POINT('Ctrl Pts',(0.00407904357217628,-0.0352450361861253,
0.0700612086763518));
#99881=CARTESIAN_POINT('Ctrl Pts',(0.00423325486346955,-0.0349452761023765,
0.0699086588599623));
#99882=CARTESIAN_POINT('Ctrl Pts',(0.0043985187327985,-0.0346444289983475,
0.0697681582466638));
#99883=CARTESIAN_POINT('Ctrl Pts',(0.00390517520914662,-0.0352450361861253,
0.0702408466242843));
#99884=CARTESIAN_POINT('Ctrl Pts',(0.00405261134423279,-0.0349452761023765,
0.0700817392551474));
#99885=CARTESIAN_POINT('Ctrl Pts',(0.00421161324655083,-0.0346444289983475,
0.0699341893859435));
#99886=CARTESIAN_POINT('Ctrl Pts',(0.00427817405012767,-0.0345231616327821,
0.0698753562986284));
#99887=CARTESIAN_POINT('Ctrl Pts',(0.00433709399533374,-0.0344132092796975,
0.069822350004561));
#99888=CARTESIAN_POINT('Ctrl Pts',(0.00439710729392348,-0.0343032738558973,
0.0697705651579658));
#99889=CARTESIAN_POINT('Ctrl Pts',(0.00445813536254092,-0.034193496108874,
0.0697200661318044));
#99890=CARTESIAN_POINT('Ctrl Pts',(0.00416516777158763,-0.0345231616327821,
0.0698669469497236));
#99891=CARTESIAN_POINT('Ctrl Pts',(0.00422420362782893,-0.0344132092796975,
0.0698123830232066));
#99892=CARTESIAN_POINT('Ctrl Pts',(0.004284365049872,-0.0343032738558973,
0.0697590430220569));
#99893=CARTESIAN_POINT('Ctrl Pts',(0.00434557321356326,-0.034193496108874,
0.0697069933067079));
#99894=CARTESIAN_POINT('Ctrl Pts',(0.00405216149304758,-0.0345231616327821,
0.0698585376008188));
#99895=CARTESIAN_POINT('Ctrl Pts',(0.00411131326032411,-0.0344132092796975,
0.0698024160418523));
#99896=CARTESIAN_POINT('Ctrl Pts',(0.00417162280582052,-0.0343032738558973,
0.069747520886148));
#99897=CARTESIAN_POINT('Ctrl Pts',(0.0042330110645856,-0.034193496108874,
0.0696939204816113));
#99898=CARTESIAN_POINT('Ctrl Pts',(0.00393915521450753,-0.0345231616327821,
0.069850128251914));
#99899=CARTESIAN_POINT('Ctrl Pts',(0.0039984228928193,-0.0344132092796975,
0.0697924490604979));
#99900=CARTESIAN_POINT('Ctrl Pts',(0.00405888056176904,-0.0343032738558973,
0.0697359987502391));
#99901=CARTESIAN_POINT('Ctrl Pts',(0.00412044891560794,-0.034193496108874,
0.0696808476565147));
#99902=CARTESIAN_POINT('Origin',(0.0155577793327288,-0.0345625596230697,
0.0823274690555088));
#99903=CARTESIAN_POINT('Ctrl Pts',(0.00438887434898244,-0.0346945769586885,
0.0694542079053786));
#99904=CARTESIAN_POINT('Ctrl Pts',(0.00445358473752521,-0.0345846629176052,
0.0694027389874847));
#99905=CARTESIAN_POINT('Ctrl Pts',(0.00451937053484638,-0.0344746925050311,
0.0693525994628331));
#99906=CARTESIAN_POINT('Ctrl Pts',(0.00458614718328078,-0.0343648066253259,
0.0693038532278454));
#99907=CARTESIAN_POINT('Ctrl Pts',(0.00438289515932269,-0.0346945769586885,
0.0695673687240069));
#99908=CARTESIAN_POINT('Ctrl Pts',(0.00444604613458785,-0.0345846629176052,
0.0695158174098574));
#99909=CARTESIAN_POINT('Ctrl Pts',(0.00451027395620052,-0.0344746925050311,
0.0694655632268504));
#99910=CARTESIAN_POINT('Ctrl Pts',(0.0045754960621468,-0.0343648066253259,
0.0694166702265655));
#99911=CARTESIAN_POINT('Ctrl Pts',(0.00437691596966294,-0.0346945769586885,
0.0696805295426352));
#99912=CARTESIAN_POINT('Ctrl Pts',(0.00443850753165049,-0.0345846629176052,
0.0696288958322299));
#99913=CARTESIAN_POINT('Ctrl Pts',(0.00450117737755465,-0.0344746925050311,
0.0695785269908678));
#99914=CARTESIAN_POINT('Ctrl Pts',(0.00456484494101283,-0.0343648066253259,
0.0695294872252856));
#99915=CARTESIAN_POINT('Ctrl Pts',(0.00437093678000319,-0.0346945769586885,
0.0697936903612635));
#99916=CARTESIAN_POINT('Ctrl Pts',(0.00443096892871313,-0.0345846629176052,
0.0697419742546026));
#99917=CARTESIAN_POINT('Ctrl Pts',(0.00449208079890879,-0.0344746925050311,
0.0696914907548851));
#99918=CARTESIAN_POINT('Ctrl Pts',(0.00455419381987885,-0.0343648066253259,
0.0696423042240056));
#99919=CARTESIAN_POINT('Origin',(0.0152025510260162,-0.0345626446730064,
0.0826515138564479));
#99920=CARTESIAN_POINT('Ctrl Pts',(0.00437104376775593,-0.0346945769586885,
0.0697916655347617));
#99921=CARTESIAN_POINT('Ctrl Pts',(0.00446233082811079,-0.034527515336289,
0.0697130629259295));
#99922=CARTESIAN_POINT('Ctrl Pts',(0.00455611347967425,-0.0343603235965158,
0.0696373108804606));
#99923=CARTESIAN_POINT('Ctrl Pts',(0.0046521110251616,-0.034193496108874,
0.0695646293168765));
#99924=CARTESIAN_POINT('Ctrl Pts',(0.00430871939721564,-0.0346945769586885,
0.069847734253028));
#99925=CARTESIAN_POINT('Ctrl Pts',(0.00439883207581774,-0.034527515336289,
0.0697678262353015));
#99926=CARTESIAN_POINT('Ctrl Pts',(0.00449148109578134,-0.0343603235965158,
0.0696907315100676));
#99927=CARTESIAN_POINT('Ctrl Pts',(0.00458638905358064,-0.034193496108874,
0.0696166740167295));
#99928=CARTESIAN_POINT('Ctrl Pts',(0.00424639502667535,-0.0346945769586885,
0.0699038029712944));
#99929=CARTESIAN_POINT('Ctrl Pts',(0.00433533332352469,-0.034527515336289,
0.0698225895446736));
#99930=CARTESIAN_POINT('Ctrl Pts',(0.00442684871188844,-0.0343603235965158,
0.0697441521396747));
#99931=CARTESIAN_POINT('Ctrl Pts',(0.00452066708199968,-0.034193496108874,
0.0696687187165824));
#99932=CARTESIAN_POINT('Ctrl Pts',(0.00418407065613505,-0.0346945769586885,
0.0699598716895607));
#99933=CARTESIAN_POINT('Ctrl Pts',(0.00427183457123164,-0.034527515336289,
0.0698773528540456));
#99934=CARTESIAN_POINT('Ctrl Pts',(0.00436221632799553,-0.0343603235965158,
0.0697975727692817));
#99935=CARTESIAN_POINT('Ctrl Pts',(0.00445494511041871,-0.034193496108874,
0.0697207634164353));
#99936=CARTESIAN_POINT('Ctrl Pts',(0.0045541694282215,-0.0340223579322365,
0.0696423242498007));
#99937=CARTESIAN_POINT('Ctrl Pts',(0.00461634203332804,-0.0339125849573554,
0.0695930899798324));
#99938=CARTESIAN_POINT('Ctrl Pts',(0.00467948998544851,-0.0338030433565221,
0.0695451771346721));
#99939=CARTESIAN_POINT('Ctrl Pts',(0.00474352709745127,-0.0336938721132327,
0.0694986398281295));
#99940=CARTESIAN_POINT('Ctrl Pts',(0.00444191397568752,-0.0340223579322365,
0.0696268357635373));
#99941=CARTESIAN_POINT('Ctrl Pts',(0.0045043002074153,-0.0339125849573554,
0.0695760531981041));
#99942=CARTESIAN_POINT('Ctrl Pts',(0.00456769368216244,-0.0338030433565221,
0.0695265975670228));
#99943=CARTESIAN_POINT('Ctrl Pts',(0.00463200772392035,-0.0336938721132327,
0.0694785249292331));
#99944=CARTESIAN_POINT('Ctrl Pts',(0.00432965852315354,-0.0340223579322365,
0.0696113472772738));
#99945=CARTESIAN_POINT('Ctrl Pts',(0.00439225838150255,-0.0339125849573554,
0.0695590164163757));
#99946=CARTESIAN_POINT('Ctrl Pts',(0.00445589737887636,-0.0338030433565221,
0.0695080179993735));
#99947=CARTESIAN_POINT('Ctrl Pts',(0.00452048835038944,-0.0336938721132327,
0.0694584100303368));
#99948=CARTESIAN_POINT('Ctrl Pts',(0.00421740307061956,-0.0340223579322365,
0.0695958587910104));
#99949=CARTESIAN_POINT('Ctrl Pts',(0.00428021655558981,-0.0339125849573554,
0.0695419796346474));
#99950=CARTESIAN_POINT('Ctrl Pts',(0.00434410107559029,-0.0338030433565221,
0.0694894384317242));
#99951=CARTESIAN_POINT('Ctrl Pts',(0.00440896897685852,-0.0336938721132327,
0.0694382951314404));
#99952=CARTESIAN_POINT('Origin',(0.015478848235124,-0.0345589643415136,
0.0822367896202505));
#99953=CARTESIAN_POINT('Ctrl Pts',(0.00469109556167717,-0.034193496108874,
0.069228957174499));
#99954=CARTESIAN_POINT('Ctrl Pts',(0.00475895382725051,-0.0340836138595105,
0.0691816224592109));
#99955=CARTESIAN_POINT('Ctrl Pts',(0.00482775902575142,-0.0339738896671456,
0.0691357146404109));
#99956=CARTESIAN_POINT('Ctrl Pts',(0.00489741915629962,-0.0338644633335883,
0.0690912865711986));
#99957=CARTESIAN_POINT('Ctrl Pts',(0.00467802272481794,-0.034193496108874,
0.0693415194247579));
#99958=CARTESIAN_POINT('Ctrl Pts',(0.0047443288236367,-0.0340836138595105,
0.0692940044427933));
#99959=CARTESIAN_POINT('Ctrl Pts',(0.00481158633038239,-0.0339738896671456,
0.0692478843249783));
#99960=CARTESIAN_POINT('Ctrl Pts',(0.00487970520681449,-0.0338644633335883,
0.0692032123289156));
#99961=CARTESIAN_POINT('Ctrl Pts',(0.00466494988795871,-0.034193496108874,
0.0694540816750168));
#99962=CARTESIAN_POINT('Ctrl Pts',(0.00472970382002289,-0.0340836138595105,
0.0694063864263755));
#99963=CARTESIAN_POINT('Ctrl Pts',(0.00479541363501335,-0.0339738896671456,
0.0693600540095457));
#99964=CARTESIAN_POINT('Ctrl Pts',(0.00486199125732937,-0.0338644633335883,
0.0693151380866326));
#99965=CARTESIAN_POINT('Ctrl Pts',(0.00465187705109948,-0.034193496108874,
0.0695666439252757));
#99966=CARTESIAN_POINT('Ctrl Pts',(0.00471507881640908,-0.0340836138595105,
0.0695187684099579));
#99967=CARTESIAN_POINT('Ctrl Pts',(0.00477924093964432,-0.0339738896671456,
0.0694722236941131));
#99968=CARTESIAN_POINT('Ctrl Pts',(0.00484427730784424,-0.0338644633335883,
0.0694270638443497));
#99969=CARTESIAN_POINT('Origin',(0.0151552659273055,-0.0345610621863334,
0.0825929419776828));
#99970=CARTESIAN_POINT('Ctrl Pts',(0.00462333669442617,-0.03424362768739,
0.0695865576249111));
#99971=CARTESIAN_POINT('Ctrl Pts',(0.00479544976091908,-0.033943005420186,
0.0694545361465294));
#99972=CARTESIAN_POINT('Ctrl Pts',(0.00497701827092622,-0.0336441434784162,
0.0693358539887064));
#99973=CARTESIAN_POINT('Ctrl Pts',(0.00442832686565394,-0.03424362768739,
0.0697429902515664));
#99974=CARTESIAN_POINT('Ctrl Pts',(0.00459453997837069,-0.033943005420186,
0.0696036138562452));
#99975=CARTESIAN_POINT('Ctrl Pts',(0.00477077929823152,-0.0336441434784162,
0.0694771532673382));
#99976=CARTESIAN_POINT('Ctrl Pts',(0.00484425460438518,-0.0335235895815127,
0.0694270797632955));
#99977=CARTESIAN_POINT('Ctrl Pts',(0.00490927490001677,-0.0334144449262719,
0.0693819306092417));
#99978=CARTESIAN_POINT('Ctrl Pts',(0.00497530264363483,-0.0333049234473133,
0.0693380728546543));
#99979=CARTESIAN_POINT('Ctrl Pts',(0.00504225848605051,-0.0331951640388588,
0.0692955702280998));
#99980=CARTESIAN_POINT('Ctrl Pts',(0.00473319323446622,-0.0335235895815127,
0.069404573217625));
#99981=CARTESIAN_POINT('Ctrl Pts',(0.00479852337701027,-0.0334144449262719,
0.0693578950851545));
#99982=CARTESIAN_POINT('Ctrl Pts',(0.00486489291106075,-0.0333049234473133,
0.0693125129967436));
#99983=CARTESIAN_POINT('Ctrl Pts',(0.00493222222694669,-0.0331951640388588,
0.069268492669703));
#99984=CARTESIAN_POINT('Ctrl Pts',(0.00462213186454726,-0.0335235895815127,
0.0693820666719544));
#99985=CARTESIAN_POINT('Ctrl Pts',(0.00468777185400377,-0.0334144449262719,
0.0693338595610674));
#99986=CARTESIAN_POINT('Ctrl Pts',(0.00475448317848668,-0.0333049234473133,
0.0692869531388329));
#99987=CARTESIAN_POINT('Ctrl Pts',(0.00482218596784287,-0.0331951640388588,
0.0692414151113062));
#99988=CARTESIAN_POINT('Ctrl Pts',(0.0045110704946283,-0.0335235895815127,
0.0693595601262839));
#99989=CARTESIAN_POINT('Ctrl Pts',(0.00457702033099727,-0.0334144449262719,
0.0693098240369803));
#99990=CARTESIAN_POINT('Ctrl Pts',(0.00464407344591261,-0.0333049234473133,
0.0692613932809222));
#99991=CARTESIAN_POINT('Ctrl Pts',(0.00471214970873905,-0.0331951640388588,
0.0692143375529094));
#99992=CARTESIAN_POINT('Origin',(0.013322660867038,-0.032643457176965,0.0837602090924077));
#99993=CARTESIAN_POINT('Ctrl Pts',(0.00500722392808472,-0.0336938721132358,
0.0690211321799775));
#99994=CARTESIAN_POINT('Ctrl Pts',(0.00503724489337306,-0.0336474569764942,
0.0690028899302693));
#99995=CARTESIAN_POINT('Ctrl Pts',(0.00506747735017109,-0.033601104548885,
0.0689850003638347));
#99996=CARTESIAN_POINT('Ctrl Pts',(0.00514401897661511,-0.0334837508643153,
0.068939708096639));
#99997=CARTESIAN_POINT('Ctrl Pts',(0.00522186909534638,-0.0333660264760389,
0.0688967038054583));
#99998=CARTESIAN_POINT('Ctrl Pts',(0.00494687938260966,-0.0336938721132358,
0.0693556894622223));
#99999=CARTESIAN_POINT('Ctrl Pts',(0.00497494207310721,-0.0336474569764942,
0.0693370939958649));
#100000=CARTESIAN_POINT('Ctrl Pts',(0.00500322052414354,-0.033601104548885,
0.069318828312905));
#100001=CARTESIAN_POINT('Ctrl Pts',(0.00507481505746574,-0.0334837508643153,
0.0692725838051825));
#100002=CARTESIAN_POINT('Ctrl Pts',(0.00514774847233361,-0.0333660264760389,
0.0692284810990089));
#100003=CARTESIAN_POINT('Ctrl Pts',(0.00494687938262152,-0.0336938721132427,
0.0693556894622311));
#100004=CARTESIAN_POINT('Ctrl Pts',(0.00497494207311814,-0.0336474569765026,
0.0693370939958744));
#100005=CARTESIAN_POINT('Ctrl Pts',(0.00500322052415354,-0.0336011045488949,
0.069318828312915));
#100006=CARTESIAN_POINT('Ctrl Pts',(0.00507421877252747,-0.0334847282606778,
0.0692729689589552));
#100007=CARTESIAN_POINT('Ctrl Pts',(0.00514653395549822,-0.0333679869945434,
0.0692292157198786));
#100008=CARTESIAN_POINT('Ctrl Pts',(0.0049468793826056,-0.0336938721132425,
0.069355689462225));
#100009=CARTESIAN_POINT('Ctrl Pts',(0.00504724398280381,-0.0335278710435082,
0.0692891838452165));
#100010=CARTESIAN_POINT('Ctrl Pts',(0.00514965887382696,-0.0333620469224319,
0.0692258490324976));
#100011=CARTESIAN_POINT('Ctrl Pts',(0.00525418552406473,-0.0331951640388601,
0.0691656705609466));
#100012=CARTESIAN_POINT('Ctrl Pts',(0.00487801917727106,-0.0336938721132425,
0.0694035047520867));
#100013=CARTESIAN_POINT('Ctrl Pts',(0.00497738280717072,-0.0335278710435082,
0.0693355576083095));
#100014=CARTESIAN_POINT('Ctrl Pts',(0.00507884228593903,-0.0333620469224319,
0.0692707503857792));
#100015=CARTESIAN_POINT('Ctrl Pts',(0.00518245885172389,-0.0331951640388601,
0.0692090677301882));
#100016=CARTESIAN_POINT('Ctrl Pts',(0.00480915897193652,-0.0336938721132425,
0.0694513200419484));
#100017=CARTESIAN_POINT('Ctrl Pts',(0.00490752163153764,-0.0335278710435082,
0.0693819313714024));
#100018=CARTESIAN_POINT('Ctrl Pts',(0.00500802569805109,-0.0333620469224319,
0.0693156517390608));
#100019=CARTESIAN_POINT('Ctrl Pts',(0.00511073217938306,-0.0331951640388601,
0.0692524648994298));
#100020=CARTESIAN_POINT('Ctrl Pts',(0.00474029876660199,-0.0336938721132425,
0.0694991353318102));
#100021=CARTESIAN_POINT('Ctrl Pts',(0.00483766045590456,-0.0335278710435082,
0.0694283051344953));
#100022=CARTESIAN_POINT('Ctrl Pts',(0.00493720911016316,-0.0333620469224319,
0.0693605530923424));
#100023=CARTESIAN_POINT('Ctrl Pts',(0.00503900550704223,-0.0331951640388601,
0.0692958620686714));
#100024=CARTESIAN_POINT('Ctrl Pts',(0.00514727936371654,-0.0330240426238155,
0.069230476477689));
#100025=CARTESIAN_POINT('Ctrl Pts',(0.00521505059309556,-0.0329142774063509,
0.0691894722513481));
#100026=CARTESIAN_POINT('Ctrl Pts',(0.00528370328080219,-0.0328043479726686,
0.0691498486035259));
#100027=CARTESIAN_POINT('Ctrl Pts',(0.00535315087557508,-0.0326943950436594,
0.0691116587171717));
#100028=CARTESIAN_POINT('Ctrl Pts',(0.005037850496551,-0.0330240426238155,
0.0692010408017928));
#100029=CARTESIAN_POINT('Ctrl Pts',(0.00510602723104327,-0.0329142774063509,
0.0691585290861954));
#100030=CARTESIAN_POINT('Ctrl Pts',(0.00517511679003615,-0.0328043479726686,
0.0691174055805016));
#100031=CARTESIAN_POINT('Ctrl Pts',(0.00524503211551944,-0.0326943950436594,
0.0690777254045036));
#100032=CARTESIAN_POINT('Ctrl Pts',(0.00492842162938546,-0.0330240426238155,
0.0691716051258966));
#100033=CARTESIAN_POINT('Ctrl Pts',(0.00499700386899099,-0.0329142774063509,
0.0691275859210426));
#100034=CARTESIAN_POINT('Ctrl Pts',(0.00506653029927011,-0.0328043479726686,
0.0690849625574773));
#100035=CARTESIAN_POINT('Ctrl Pts',(0.00513691335546381,-0.0326943950436594,
0.0690437920918355));
#100036=CARTESIAN_POINT('Ctrl Pts',(0.00481899276221992,-0.0330240426238155,
0.0691421694500005));
#100037=CARTESIAN_POINT('Ctrl Pts',(0.00488798050693871,-0.0329142774063509,
0.0690966427558899));
#100038=CARTESIAN_POINT('Ctrl Pts',(0.00495794380850407,-0.0328043479726686,
0.069052519534453));
#100039=CARTESIAN_POINT('Ctrl Pts',(0.00502879459540817,-0.0326943950436594,
0.0690098587791674));
#100040=CARTESIAN_POINT('Origin',(0.0133839226643085,-0.0326396682856107,
0.0838676446126732));
#100041=CARTESIAN_POINT('Ctrl Pts',(0.00533493353088823,-0.0331951640388587,
0.0688375313516922));
#100042=CARTESIAN_POINT('Ctrl Pts',(0.00540810203948209,-0.0330855618255041,
0.0687991206031651));
#100043=CARTESIAN_POINT('Ctrl Pts',(0.00548211717874542,-0.0329757224427708,
0.068762194432868));
#100044=CARTESIAN_POINT('Ctrl Pts',(0.00555688648733464,-0.0328657862078596,
0.0687268047761767));
#100045=CARTESIAN_POINT('Ctrl Pts',(0.00530785599404896,-0.0331951640388587,
0.0689475675231918));
#100046=CARTESIAN_POINT('Ctrl Pts',(0.00537950897698177,-0.0330855618255041,
0.0689087838363721));
#100047=CARTESIAN_POINT('Ctrl Pts',(0.00545201520605982,-0.0329757224427708,
0.0688714531356117));
#100048=CARTESIAN_POINT('Ctrl Pts',(0.00552528417759984,-0.0328657862078596,
0.0688356277795307));
#100049=CARTESIAN_POINT('Ctrl Pts',(0.00528077845720969,-0.0331951640388587,
0.0690576036946913));
#100050=CARTESIAN_POINT('Ctrl Pts',(0.00535091591448146,-0.0330855618255041,
0.0690184470695791));
#100051=CARTESIAN_POINT('Ctrl Pts',(0.00542191323337422,-0.0329757224427708,
0.0689807118383553));
#100052=CARTESIAN_POINT('Ctrl Pts',(0.00549368186786503,-0.0328657862078596,
0.0689444507828847));
#100053=CARTESIAN_POINT('Ctrl Pts',(0.00525370092037042,-0.0331951640388587,
0.0691676398661909));
#100054=CARTESIAN_POINT('Ctrl Pts',(0.00532232285198114,-0.0330855618255041,
0.0691281103027861));
#100055=CARTESIAN_POINT('Ctrl Pts',(0.00539181126068862,-0.0329757224427708,
0.0690899705410989));
#100056=CARTESIAN_POINT('Ctrl Pts',(0.00546207955813023,-0.0328657862078596,
0.0690532737862387));
#100057=CARTESIAN_POINT('Origin',(0.0129440085191781,-0.0326401908833561,
0.0840619341299403));
#100058=CARTESIAN_POINT('Ctrl Pts',(0.00522295231765763,-0.0332451089994432,
0.0691837830259146));
#100059=CARTESIAN_POINT('Ctrl Pts',(0.00541025625528785,-0.0329451141710258,
0.0690743764371766));
#100060=CARTESIAN_POINT('Ctrl Pts',(0.00560526903372078,-0.0326442513127503,
0.0689793891592973));
#100061=CARTESIAN_POINT('Ctrl Pts',(0.00500987234511869,-0.0332451089994432,
0.0693145382372938));
#100062=CARTESIAN_POINT('Ctrl Pts',(0.00519224476926797,-0.0329451141710258,
0.0691970952059085));
#100063=CARTESIAN_POINT('Ctrl Pts',(0.00538294538184271,-0.0326442513127503,
0.0690937228543116));
#100064=CARTESIAN_POINT('Ctrl Pts',(0.00546205151731605,-0.0325229783203385,
0.0690532883290438));
#100065=CARTESIAN_POINT('Ctrl Pts',(0.00553230957496362,-0.0324130253112079,
0.0690165964305541));
#100066=CARTESIAN_POINT('Ctrl Pts',(0.00560331599564085,-0.0323031222247694,
0.0689813634752584));
#100067=CARTESIAN_POINT('Ctrl Pts',(0.00567497823265307,-0.0321934096636184,
0.0689476313845928));
#100068=CARTESIAN_POINT('Ctrl Pts',(0.00535468683073835,-0.0325229783203385,
0.0690170396500961));
#100069=CARTESIAN_POINT('Ctrl Pts',(0.0054254445756234,-0.0324130253112079,
0.0689788677317768));
#100070=CARTESIAN_POINT('Ctrl Pts',(0.00549698122386161,-0.0323031222247694,
0.0689421653177977));
#100071=CARTESIAN_POINT('Ctrl Pts',(0.00556920348315531,-0.0321934096636184,
0.0689069761879008));
#100072=CARTESIAN_POINT('Ctrl Pts',(0.00524732214416064,-0.0325229783203385,
0.0689807909711484));
#100073=CARTESIAN_POINT('Ctrl Pts',(0.00531857957628318,-0.0324130253112079,
0.0689411390329995));
#100074=CARTESIAN_POINT('Ctrl Pts',(0.00539064645208236,-0.0323031222247694,
0.068902967160337));
#100075=CARTESIAN_POINT('Ctrl Pts',(0.00546342873365755,-0.0321934096636184,
0.0688663209912088));
#100076=CARTESIAN_POINT('Ctrl Pts',(0.00513995745758293,-0.0325229783203385,
0.0689445422922008));
#100077=CARTESIAN_POINT('Ctrl Pts',(0.00521171457694297,-0.0324130253112079,
0.0689034103342222));
#100078=CARTESIAN_POINT('Ctrl Pts',(0.00528431168030312,-0.0323031222247694,
0.0688637690028764));
#100079=CARTESIAN_POINT('Ctrl Pts',(0.00535765398415979,-0.0321934096636184,
0.0688256657945168));
#100080=CARTESIAN_POINT('Origin',(0.0133800753187604,-0.0326393375177818,
0.0838600361333332));
#100081=CARTESIAN_POINT('Ctrl Pts',(0.00567400935308162,-0.0326943950436593,
0.0686729010386623));
#100082=CARTESIAN_POINT('Ctrl Pts',(0.00574949404194613,-0.0325844576448127,
0.0686391385775631));
#100083=CARTESIAN_POINT('Ctrl Pts',(0.00582568233602918,-0.0324744968375319,
0.0686069348741667));
#100084=CARTESIAN_POINT('Ctrl Pts',(0.00590247604932843,-0.0323646534831894,
0.0685763298433056));
#100085=CARTESIAN_POINT('Ctrl Pts',(0.00564007605151625,-0.0326943950436593,
0.0687810197633423));
#100086=CARTESIAN_POINT('Ctrl Pts',(0.00571407066171858,-0.0325844576448127,
0.0687467896377499));
#100087=CARTESIAN_POINT('Ctrl Pts',(0.00578877844375275,-0.0324744968375319,
0.068714087419493));
#100088=CARTESIAN_POINT('Ctrl Pts',(0.00586410309972482,-0.0323646534831894,
0.0686829536882949));
#100089=CARTESIAN_POINT('Ctrl Pts',(0.00560614274995088,-0.0326943950436593,
0.0688891384880224));
#100090=CARTESIAN_POINT('Ctrl Pts',(0.00567864728149104,-0.0325844576448127,
0.0688544406979365));
#100091=CARTESIAN_POINT('Ctrl Pts',(0.00575187455147631,-0.0324744968375319,
0.0688212399648193));
#100092=CARTESIAN_POINT('Ctrl Pts',(0.00582573015012121,-0.0323646534831894,
0.0687895775332841));
#100093=CARTESIAN_POINT('Ctrl Pts',(0.00557220944838551,-0.0326943950436593,
0.0689972572127024));
#100094=CARTESIAN_POINT('Ctrl Pts',(0.00564322390126349,-0.0325844576448127,
0.0689620917581233));
#100095=CARTESIAN_POINT('Ctrl Pts',(0.00571497065919988,-0.0324744968375319,
0.0689283925101456));
#100096=CARTESIAN_POINT('Ctrl Pts',(0.0057873572005176,-0.0323646534831894,
0.0688962013782734));
#100097=CARTESIAN_POINT('Origin',(0.0129609683792565,-0.0326395579068092,
0.0840957620033715));
#100098=CARTESIAN_POINT('Ctrl Pts',(0.00554047274258514,-0.0327445246961877,
0.0690114557233747));
#100099=CARTESIAN_POINT('Ctrl Pts',(0.00573427610621507,-0.0324436878365475,
0.0689140246156803));
#100100=CARTESIAN_POINT('Ctrl Pts',(0.00593486780412998,-0.0321434074463186,
0.068831468360748));
#100101=CARTESIAN_POINT('Ctrl Pts',(0.00531960384577433,-0.0327445246961877,
0.0691285750233282));
#100102=CARTESIAN_POINT('Ctrl Pts',(0.00550898998284065,-0.0324436878365475,
0.0690228137090968));
#100103=CARTESIAN_POINT('Ctrl Pts',(0.00570580446826165,-0.0321434074463186,
0.0689316181893094));
#100104=CARTESIAN_POINT('Ctrl Pts',(0.00587336811646014,-0.0322357242816072,
0.0688571971996282));
#100105=CARTESIAN_POINT('Ctrl Pts',(0.0060419370211382,-0.0319819883628705,
0.068785524429967));
#100106=CARTESIAN_POINT('Ctrl Pts',(0.00621472504338505,-0.0317295851069887,
0.0687247234357048));
#100107=CARTESIAN_POINT('Ctrl Pts',(0.00564548099814133,-0.0322357242816072,
0.0689599953577067));
#100108=CARTESIAN_POINT('Ctrl Pts',(0.00581077591480891,-0.0319819883628705,
0.0688810646788859));
#100109=CARTESIAN_POINT('Ctrl Pts',(0.0059807584257111,-0.0317295851069887,
0.0688128121512944));
#100110=CARTESIAN_POINT('Origin',(0.0129208253933554,-0.0326371942645984,
0.0840093273795378));
#100111=CARTESIAN_POINT('Origin',(0.0133242262562021,-0.0326352985528889,
0.0837507443898176));
#100112=CARTESIAN_POINT('Ctrl Pts',(0.00602275330948016,-0.0321934096636183,
0.0685298863329836));
#100113=CARTESIAN_POINT('Ctrl Pts',(0.00610025905699843,-0.0320835708272303,
0.068500911507236));
#100114=CARTESIAN_POINT('Ctrl Pts',(0.00617831948054618,-0.0319739230346346,
0.0684735574654815));
#100115=CARTESIAN_POINT('Ctrl Pts',(0.00625683202125929,-0.0318646057455576,
0.0684478515403528));
#100116=CARTESIAN_POINT('Ctrl Pts',(0.00598209807777947,-0.0321934096636183,
0.0686356611735653));
#100117=CARTESIAN_POINT('Ctrl Pts',(0.00605814510781022,-0.0320835708272303,
0.0686061256804878));
#100118=CARTESIAN_POINT('Ctrl Pts',(0.00613475926296713,-0.0319739230346346,
0.0685781811085306));
#100119=CARTESIAN_POINT('Ctrl Pts',(0.00621183977680037,-0.0318646057455576,
0.068551855687882));
#100120=CARTESIAN_POINT('Ctrl Pts',(0.00594144284607878,-0.0321934096636183,
0.068741436014147));
#100121=CARTESIAN_POINT('Ctrl Pts',(0.00601603115862201,-0.0320835708272303,
0.0687113398537396));
#100122=CARTESIAN_POINT('Ctrl Pts',(0.00609119904538808,-0.0319739230346346,
0.0686828047515797));
#100123=CARTESIAN_POINT('Ctrl Pts',(0.00616684753234146,-0.0318646057455576,
0.0686558598354111));
#100124=CARTESIAN_POINT('Ctrl Pts',(0.00590078761437809,-0.0321934096636183,
0.0688472108547287));
#100125=CARTESIAN_POINT('Ctrl Pts',(0.0059739172094338,-0.0320835708272303,
0.0688165540269914));
#100126=CARTESIAN_POINT('Ctrl Pts',(0.00604763882780903,-0.0319739230346346,
0.0687874283946289));
#100127=CARTESIAN_POINT('Ctrl Pts',(0.00612185528788254,-0.0318646057455576,
0.0687598639829403));
#100128=CARTESIAN_POINT('Ctrl Pts',(0.0057865917572633,-0.0320218834582364,
0.0688956362262419));
#100129=CARTESIAN_POINT('Ctrl Pts',(0.0058412769818047,-0.0319391099350667,
0.0688713117239265));
#100130=CARTESIAN_POINT('Ctrl Pts',(0.00589630890447229,-0.0318564869454955,
0.0688478558766581));
#100131=CARTESIAN_POINT('Ctrl Pts',(0.00595164584685598,-0.0317740741446555,
0.0688252820268415));
#100132=CARTESIAN_POINT('Ctrl Pts',(0.0057407191058014,-0.0320218834582364,
0.0688768605000231));
#100133=CARTESIAN_POINT('Ctrl Pts',(0.00579559974026271,-0.0319391099350667,
0.0688520585743025));
#100134=CARTESIAN_POINT('Ctrl Pts',(0.00585083440948972,-0.0318564869454955,
0.0688281286442408));
#100135=CARTESIAN_POINT('Ctrl Pts',(0.00590638125516161,-0.0317740741446555,
0.0688050843837629));
#100136=CARTESIAN_POINT('Ctrl Pts',(0.00569484645433949,-0.0320218834582364,
0.0688580847738044));
#100137=CARTESIAN_POINT('Ctrl Pts',(0.00574992249872072,-0.0319391099350667,
0.0688328054246785));
#100138=CARTESIAN_POINT('Ctrl Pts',(0.00580535991450715,-0.0318564869454955,
0.0688084014118235));
#100139=CARTESIAN_POINT('Ctrl Pts',(0.00586111666346724,-0.0317740741446555,
0.0687848867406844));
#100140=CARTESIAN_POINT('Ctrl Pts',(0.00564897380287759,-0.0320218834582364,
0.0688393090475856));
#100141=CARTESIAN_POINT('Ctrl Pts',(0.00570424525717873,-0.0319391099350667,
0.0688135522750544));
#100142=CARTESIAN_POINT('Ctrl Pts',(0.00575988541952458,-0.0318564869454955,
0.0687886741794062));
#100143=CARTESIAN_POINT('Ctrl Pts',(0.00581585207177287,-0.0317740741446555,
0.0687646890976059));
#100144=CARTESIAN_POINT('Origin',(0.00236941910510931,-0.0391228853390649,
0.0635307757448714));
#100145=CARTESIAN_POINT('Ctrl Pts',(0.00343631067228798,-0.0352722978779595,
0.070816567042208));
#100146=CARTESIAN_POINT('Ctrl Pts',(0.00344754559313125,-0.0352466642097217,
0.0708013726606252));
#100147=CARTESIAN_POINT('Ctrl Pts',(0.00345870746525495,-0.0352210183808301,
0.0707861452031262));
#100148=CARTESIAN_POINT('Ctrl Pts',(0.00346979625305581,-0.0351953608940152,
0.0707708838175277));
#100149=CARTESIAN_POINT('Origin',(-0.000393203979565928,-0.0352456003065074,
0.0677596796176656));
#100150=CARTESIAN_POINT('Ctrl Pts',(0.00354530261829435,-0.0350241211493339,
0.0706716663582445));
#100151=CARTESIAN_POINT('Ctrl Pts',(0.00359321523587681,-0.0349144232867421,
0.0706085996821949));
#100152=CARTESIAN_POINT('Ctrl Pts',(0.00364246016466918,-0.0348045283677512,
0.0705464856456987));
#100153=CARTESIAN_POINT('Ctrl Pts',(0.00369297728879991,-0.0346945769586886,
0.0704854061561595));
#100154=CARTESIAN_POINT('Ctrl Pts',(0.0034327222098805,-0.0350241211493339,
0.0706845812118786));
#100155=CARTESIAN_POINT('Ctrl Pts',(0.00348045693065747,-0.0349144232867421,
0.0706199637869327));
#100156=CARTESIAN_POINT('Ctrl Pts',(0.00352955591125088,-0.0348045283677512,
0.0705562943960884));
#100157=CARTESIAN_POINT('Ctrl Pts',(0.00357995929686508,-0.0346945769586886,
0.070493656932004));
#100158=CARTESIAN_POINT('Ctrl Pts',(0.00332014180146665,-0.0350241211493339,
0.0706974960655126));
#100159=CARTESIAN_POINT('Ctrl Pts',(0.00336769862543812,-0.0349144232867421,
0.0706313278916705));
#100160=CARTESIAN_POINT('Ctrl Pts',(0.00341665165783259,-0.0348045283677512,
0.0705661031464782));
#100161=CARTESIAN_POINT('Ctrl Pts',(0.00346694130493024,-0.0346945769586886,
0.0705019077078485));
#100162=CARTESIAN_POINT('Ctrl Pts',(0.00320756139305279,-0.0350241211493339,
0.0707104109191467));
#100163=CARTESIAN_POINT('Ctrl Pts',(0.00325494032021878,-0.0349144232867421,
0.0706426919964084));
#100164=CARTESIAN_POINT('Ctrl Pts',(0.00330374740441429,-0.0348045283677512,
0.070575911896868));
#100165=CARTESIAN_POINT('Ctrl Pts',(0.00335392331299541,-0.0346945769586886,
0.070510158483693));
#100166=CARTESIAN_POINT('Origin',(0.0165147080052373,-0.0345629067943449,
0.0813235873006996));
#100167=CARTESIAN_POINT('Ctrl Pts',(0.00358672921891514,-0.0351970973651648,
0.0703302261733762));
#100168=CARTESIAN_POINT('Ctrl Pts',(0.00363964700857392,-0.0350869349321788,
0.070267371453213));
#100169=CARTESIAN_POINT('Ctrl Pts',(0.00369391534951389,-0.0349764985129721,
0.0702055647964528));
#100170=CARTESIAN_POINT('Ctrl Pts',(0.00374946864903189,-0.0348659306849623,
0.0701448904140705));
#100171=CARTESIAN_POINT('Ctrl Pts',(0.00359787316825978,-0.0351970973651648,
0.0704116895580534));
#100172=CARTESIAN_POINT('Ctrl Pts',(0.00364966239312627,-0.0350869349321788,
0.0703489892222056));
#100173=CARTESIAN_POINT('Ctrl Pts',(0.00370279802481965,-0.0349764985129721,
0.0702873136154144));
#100174=CARTESIAN_POINT('Ctrl Pts',(0.00375721592810065,-0.0348659306849623,
0.0702267466924924));
#100175=CARTESIAN_POINT('Ctrl Pts',(0.00360901711760441,-0.0351970973651648,
0.0704931529427305));
#100176=CARTESIAN_POINT('Ctrl Pts',(0.00365967777767861,-0.0350869349321788,
0.0704306069911982));
#100177=CARTESIAN_POINT('Ctrl Pts',(0.0037116807001254,-0.0349764985129721,
0.0703690624343759));
#100178=CARTESIAN_POINT('Ctrl Pts',(0.00376496320716942,-0.0348659306849623,
0.0703086029709142));
#100179=CARTESIAN_POINT('Ctrl Pts',(0.00362016106694905,-0.0351970973651648,
0.0705746163274077));
#100180=CARTESIAN_POINT('Ctrl Pts',(0.00366969316223096,-0.0350869349321788,
0.0705122247601908));
#100181=CARTESIAN_POINT('Ctrl Pts',(0.00372056337543116,-0.0349764985129721,
0.0704508112533375));
#100182=CARTESIAN_POINT('Ctrl Pts',(0.00377271048623818,-0.0348659306849623,
0.0703904592493361));
#100183=CARTESIAN_POINT('Origin',(0.0161690093029537,-0.0345637187966485,
0.0816579789329045));
#100184=CARTESIAN_POINT('Ctrl Pts',(0.00359847610634473,-0.0352450361861253,
0.0706003901874853));
#100185=CARTESIAN_POINT('Ctrl Pts',(0.00373235183377771,-0.0349452761023764,
0.0704297154721725));
#100186=CARTESIAN_POINT('Ctrl Pts',(0.00387870315195259,-0.0346444289983475,
0.0702696096930411));
#100187=CARTESIAN_POINT('Ctrl Pts',(0.00344849335217477,-0.0352450361861253,
0.0708004031206961));
#100188=CARTESIAN_POINT('Ctrl Pts',(0.00357482546824089,-0.0349452761023764,
0.0706240717131334));
#100189=CARTESIAN_POINT('Ctrl Pts',(0.00371408069084825,-0.0346444289983475,
0.0704577570961589));
#100190=CARTESIAN_POINT('Ctrl Pts',(0.00377274290153435,-0.0345231616327822,
0.0703910456445689));
#100191=CARTESIAN_POINT('Ctrl Pts',(0.00382455479513922,-0.0344132092796975,
0.0703310726937082));
#100192=CARTESIAN_POINT('Ctrl Pts',(0.00387760450867109,-0.0343032738558974,
0.0702721745253267));
#100193=CARTESIAN_POINT('Ctrl Pts',(0.00393182214649865,-0.0341934961088741,
0.0702144248538919));
#100194=CARTESIAN_POINT('Ctrl Pts',(0.00365957374036347,-0.0345231616327822,
0.0703968660481945));
#100195=CARTESIAN_POINT('Ctrl Pts',(0.00371130540789883,-0.0344132092796975,
0.0703353332197765));
#100196=CARTESIAN_POINT('Ctrl Pts',(0.00376430716433736,-0.0343032738558974,
0.0702748735949072));
#100197=CARTESIAN_POINT('Ctrl Pts',(0.00381850912424515,-0.0341934961088741,
0.0702155628900342));
#100198=CARTESIAN_POINT('Ctrl Pts',(0.00354640457919259,-0.0345231616327822,
0.07040268645182));
#100199=CARTESIAN_POINT('Ctrl Pts',(0.00359805602065845,-0.0344132092796975,
0.0703395937458448));
#100200=CARTESIAN_POINT('Ctrl Pts',(0.00365100982000363,-0.0343032738558974,
0.0702775726644878));
#100201=CARTESIAN_POINT('Ctrl Pts',(0.00370519610199164,-0.0341934961088741,
0.0702167009261765));
#100202=CARTESIAN_POINT('Ctrl Pts',(0.00343323541802172,-0.0345231616327822,
0.0704085068554456));
#100203=CARTESIAN_POINT('Ctrl Pts',(0.00348480663341807,-0.0344132092796975,
0.0703438542719131));
#100204=CARTESIAN_POINT('Ctrl Pts',(0.00353771247566989,-0.0343032738558974,
0.0702802717340683));
#100205=CARTESIAN_POINT('Ctrl Pts',(0.00359188307973814,-0.0341934961088741,
0.0702178389623189));
#100206=CARTESIAN_POINT('Origin',(0.0165240686837907,-0.0345625596230435,
0.0813312603696003));
#100207=CARTESIAN_POINT('Ctrl Pts',(0.00382978640553166,-0.0346945769586885,
0.0699593437057787));
#100208=CARTESIAN_POINT('Ctrl Pts',(0.00388753576742504,-0.0345846629176052,
0.0699001702734341));
#100209=CARTESIAN_POINT('Ctrl Pts',(0.00394651867533112,-0.0344746925050311,
0.0698421809672095));
#100210=CARTESIAN_POINT('Ctrl Pts',(0.00400665924669232,-0.0343648066253259,
0.0697854497775696));
#100211=CARTESIAN_POINT('Ctrl Pts',(0.00383803717487975,-0.0346945769586885,
0.0700723616087268));
#100212=CARTESIAN_POINT('Ctrl Pts',(0.00389422909294583,-0.0345846629176052,
0.0700133018761542));
#100213=CARTESIAN_POINT('Ctrl Pts',(0.00395165193974478,-0.0344746925050311,
0.069955394081823));
#100214=CARTESIAN_POINT('Ctrl Pts',(0.00401023183208043,-0.0343648066253259,
0.0698987121200108));
#100215=CARTESIAN_POINT('Ctrl Pts',(0.00384628794422784,-0.0346945769586885,
0.070185379511675));
#100216=CARTESIAN_POINT('Ctrl Pts',(0.00390092241846661,-0.0345846629176052,
0.0701264334788743));
#100217=CARTESIAN_POINT('Ctrl Pts',(0.00395678520415844,-0.0344746925050311,
0.0700686071964365));
#100218=CARTESIAN_POINT('Ctrl Pts',(0.00401380441746853,-0.0343648066253259,
0.070011974462452));
#100219=CARTESIAN_POINT('Ctrl Pts',(0.00385453871357593,-0.0346945769586885,
0.0702983974146231));
#100220=CARTESIAN_POINT('Ctrl Pts',(0.0039076157439874,-0.0345846629176052,
0.0702395650815944));
#100221=CARTESIAN_POINT('Ctrl Pts',(0.0039619184685721,-0.0344746925050311,
0.07018182031105));
#100222=CARTESIAN_POINT('Ctrl Pts',(0.00401737700285664,-0.0343648066253259,
0.0701252368048932));
#100223=CARTESIAN_POINT('Origin',(0.0162122550414581,-0.0345626446731979,
0.0816972718927456));
#100224=CARTESIAN_POINT('Ctrl Pts',(0.00385439107964542,-0.0346945769586885,
0.070296375145362));
#100225=CARTESIAN_POINT('Ctrl Pts',(0.00393510679513173,-0.034527515336289,
0.070206951039121));
#100226=CARTESIAN_POINT('Ctrl Pts',(0.00401865569366838,-0.0343603235965158,
0.0701200422381841));
#100227=CARTESIAN_POINT('Ctrl Pts',(0.004104786854452,-0.0341934961088739,
0.0700359021076476));
#100228=CARTESIAN_POINT('Ctrl Pts',(0.00379958542914434,-0.0346945769586885,
0.0703598130599275));
#100229=CARTESIAN_POINT('Ctrl Pts',(0.00387897241211095,-0.034527515336289,
0.0702692410273938));
#100230=CARTESIAN_POINT('Ctrl Pts',(0.00396122833567491,-0.0343603235965158,
0.0701811422158369));
#100231=CARTESIAN_POINT('Ctrl Pts',(0.0040461060507696,-0.0341934961088739,
0.0700957735667116));
#100232=CARTESIAN_POINT('Ctrl Pts',(0.00374477977864326,-0.0346945769586885,
0.070423250974493));
#100233=CARTESIAN_POINT('Ctrl Pts',(0.00382283802909016,-0.034527515336289,
0.0703315310156666));
#100234=CARTESIAN_POINT('Ctrl Pts',(0.00390380097768144,-0.0343603235965158,
0.0702422421934897));
#100235=CARTESIAN_POINT('Ctrl Pts',(0.0039874252470872,-0.0341934961088739,
0.0701556450257756));
#100236=CARTESIAN_POINT('Ctrl Pts',(0.00368997412814219,-0.0346945769586885,
0.0704866888890586));
#100237=CARTESIAN_POINT('Ctrl Pts',(0.00376670364606938,-0.034527515336289,
0.0703938210039394));
#100238=CARTESIAN_POINT('Ctrl Pts',(0.00384637361968797,-0.0343603235965158,
0.0703033421711425));
#100239=CARTESIAN_POINT('Ctrl Pts',(0.0039287444434048,-0.0341934961088739,
0.0702155164848397));
#100240=CARTESIAN_POINT('Ctrl Pts',(0.00401735531343243,-0.0340223579322365,
0.0701252597298641));
#100241=CARTESIAN_POINT('Ctrl Pts',(0.00407286697872035,-0.0339125849573554,
0.0700686213931831));
#100242=CARTESIAN_POINT('Ctrl Pts',(0.00412951191856377,-0.0338030433565221,
0.0700131718180855));
#100243=CARTESIAN_POINT('Ctrl Pts',(0.00418721140770106,-0.0336938721132328,
0.0699589754937896));
#100244=CARTESIAN_POINT('Ctrl Pts',(0.00390404380660431,-0.0340223579322365,
0.0701239627137924));
#100245=CARTESIAN_POINT('Ctrl Pts',(0.00395957336112662,-0.0339125849573554,
0.0700657615159034));
#100246=CARTESIAN_POINT('Ctrl Pts',(0.00401626852522929,-0.0338030433565221,
0.070008750548068));
#100247=CARTESIAN_POINT('Ctrl Pts',(0.00407405033241811,-0.0336938721132328,
0.0699529962905688));
#100248=CARTESIAN_POINT('Ctrl Pts',(0.00379073229977619,-0.0340223579322365,
0.0701226656977207));
#100249=CARTESIAN_POINT('Ctrl Pts',(0.00384627974353289,-0.0339125849573554,
0.0700629016386237));
#100250=CARTESIAN_POINT('Ctrl Pts',(0.0039030251318948,-0.0338030433565221,
0.0700043292780504));
#100251=CARTESIAN_POINT('Ctrl Pts',(0.00396088925713516,-0.0336938721132328,
0.0699470170873479));
#100252=CARTESIAN_POINT('Ctrl Pts',(0.00367742079294807,-0.0340223579322365,
0.070121368681649));
#100253=CARTESIAN_POINT('Ctrl Pts',(0.00373298612593915,-0.0339125849573554,
0.0700600417613441));
#100254=CARTESIAN_POINT('Ctrl Pts',(0.00378978173856031,-0.0338030433565221,
0.0699999080080329));
#100255=CARTESIAN_POINT('Ctrl Pts',(0.00384772818185221,-0.0336938721132328,
0.069941037884127));
#100256=CARTESIAN_POINT('Origin',(0.0164343948347533,-0.0345589643415299,
0.0812511886584912));
#100257=CARTESIAN_POINT('Ctrl Pts',(0.00410139311123136,-0.034193496108874,
0.0696979907823524));
#100258=CARTESIAN_POINT('Ctrl Pts',(0.00416278368118548,-0.0340836138595105,
0.0696425244195842));
#100259=CARTESIAN_POINT('Ctrl Pts',(0.00422529255476902,-0.0339738896671456,
0.0695883550196333));
#100260=CARTESIAN_POINT('Ctrl Pts',(0.00428883508080599,-0.0338644633335883,
0.0695355465496046));
#100261=CARTESIAN_POINT('Ctrl Pts',(0.00410253114839765,-0.034193496108874,
0.0698113039065627));
#100262=CARTESIAN_POINT('Ctrl Pts',(0.00416235919749018,-0.0340836138595105,
0.0697558532366529));
#100263=CARTESIAN_POINT('Ctrl Pts',(0.00422330597520824,-0.0339738896671456,
0.0697016671889405));
#100264=CARTESIAN_POINT('Ctrl Pts',(0.00428528882823726,-0.0338644633335883,
0.0696488098858596));
#100265=CARTESIAN_POINT('Ctrl Pts',(0.00410366918556394,-0.034193496108874,
0.069924617030773));
#100266=CARTESIAN_POINT('Ctrl Pts',(0.00416193471379489,-0.0340836138595105,
0.0698691820537216));
#100267=CARTESIAN_POINT('Ctrl Pts',(0.00422131939564746,-0.0339738896671456,
0.0698149793582477));
#100268=CARTESIAN_POINT('Ctrl Pts',(0.00428174257566853,-0.0338644633335883,
0.0697620732221146));
#100269=CARTESIAN_POINT('Ctrl Pts',(0.00410480722273024,-0.034193496108874,
0.0700379301549834));
#100270=CARTESIAN_POINT('Ctrl Pts',(0.00416151023009959,-0.0340836138595105,
0.0699825108707904));
#100271=CARTESIAN_POINT('Ctrl Pts',(0.00421933281608668,-0.0339738896671456,
0.0699282915275549));
#100272=CARTESIAN_POINT('Ctrl Pts',(0.00427819632309979,-0.0338644633335883,
0.0698753365583697));
#100273=CARTESIAN_POINT('Origin',(0.0161580017964341,-0.0345610621862345,
0.0816450882651416));
#100274=CARTESIAN_POINT('Ctrl Pts',(0.00407898776366144,-0.03424362768739,
0.0700612638843384));
#100275=CARTESIAN_POINT('Ctrl Pts',(0.00423319698843185,-0.0339430054201859,
0.0699087119475842));
#100276=CARTESIAN_POINT('Ctrl Pts',(0.00439845895789937,-0.0336441434784161,
0.0697682090655518));
#100277=CARTESIAN_POINT('Ctrl Pts',(0.00390512185256935,-0.03424362768739,
0.0702409042054249));
#100278=CARTESIAN_POINT('Ctrl Pts',(0.00405255583093875,-0.0339430054201859,
0.070081794807733));
#100279=CARTESIAN_POINT('Ctrl Pts',(0.0042115557365962,-0.0336441434784161,
0.0699342427545023));
#100280=CARTESIAN_POINT('Ctrl Pts',(0.00427817579383718,-0.0335235895815127,
0.0698753551972878));
#100281=CARTESIAN_POINT('Ctrl Pts',(0.00433702469554684,-0.0334144449262719,
0.0698224128539003));
#100282=CARTESIAN_POINT('Ctrl Pts',(0.00439703495648564,-0.0333049234473133,
0.0697706254601949));
#100283=CARTESIAN_POINT('Ctrl Pts',(0.00445813584046408,-0.0331951640388588,
0.0697200661873098));
#100284=CARTESIAN_POINT('Ctrl Pts',(0.00416516935784719,-0.0335235895815127,
0.0698669458030683));
#100285=CARTESIAN_POINT('Ctrl Pts',(0.00422413403142485,-0.0334144449262719,
0.0698124477036002));
#100286=CARTESIAN_POINT('Ctrl Pts',(0.0042842923379893,-0.0333049234473133,
0.0697591051581987));
#100287=CARTESIAN_POINT('Ctrl Pts',(0.00434557353217863,-0.0331951640388588,
0.0697069933437114));
#100288=CARTESIAN_POINT('Ctrl Pts',(0.0040521629218572,-0.0335235895815127,
0.0698585364088488));
#100289=CARTESIAN_POINT('Ctrl Pts',(0.00411124336730287,-0.0334144449262719,
0.0698024825533001));
#100290=CARTESIAN_POINT('Ctrl Pts',(0.00417154971949296,-0.0333049234473133,
0.0697475848562025));
#100291=CARTESIAN_POINT('Ctrl Pts',(0.00423301122389317,-0.0331951640388588,
0.069693920500113));
#100292=CARTESIAN_POINT('Ctrl Pts',(0.00393915648586722,-0.0335235895815127,
0.0698501270146293));
#100293=CARTESIAN_POINT('Ctrl Pts',(0.00399835270318089,-0.0334144449262719,
0.0697925174030001));
#100294=CARTESIAN_POINT('Ctrl Pts',(0.00405880710099661,-0.0333049234473133,
0.0697360645542062));
#100295=CARTESIAN_POINT('Ctrl Pts',(0.00412044891560771,-0.0331951640388588,
0.0696808476565146));
#100296=CARTESIAN_POINT('Origin',(0.014486144736754,-0.0326434571770401,
0.0830328374481446));
#100297=CARTESIAN_POINT('Ctrl Pts',(0.0043889813324677,-0.0336938721132362,
0.0694521831596041));
#100298=CARTESIAN_POINT('Ctrl Pts',(0.00441647921333464,-0.0336474569764944,
0.069430322130829));
#100299=CARTESIAN_POINT('Ctrl Pts',(0.00444423112097265,-0.033601104548885,
0.0694087844974));
#100300=CARTESIAN_POINT('Ctrl Pts',(0.00451449256752707,-0.0334837508643155,
0.0693542561637148));
#100301=CARTESIAN_POINT('Ctrl Pts',(0.00458633894794849,-0.0333660264760393,
0.0693018337671009));
#100302=CARTESIAN_POINT('Ctrl Pts',(0.00437104376775398,-0.0336938721132362,
0.0697916655347634));
#100303=CARTESIAN_POINT('Ctrl Pts',(0.00439655454562698,-0.0336474569764944,
0.0697696995114698));
#100304=CARTESIAN_POINT('Ctrl Pts',(0.00442232071552202,-0.033601104548885,
0.069748033629167));
#100305=CARTESIAN_POINT('Ctrl Pts',(0.00448755473087715,-0.0334837508643155,
0.0696931805988338));
#100306=CARTESIAN_POINT('Ctrl Pts',(0.00455438550921085,-0.0333660264760393,
0.069640284674951));
#100307=CARTESIAN_POINT('Ctrl Pts',(0.00437104376776591,-0.0336938721132427,
0.0697916655347717));
#100308=CARTESIAN_POINT('Ctrl Pts',(0.00439655454563795,-0.0336474569765026,
0.0697696995114789));
#100309=CARTESIAN_POINT('Ctrl Pts',(0.00442232071553202,-0.0336011045488949,
0.069748033629177));
#100310=CARTESIAN_POINT('Ctrl Pts',(0.00448701142039042,-0.0334847282606778,
0.0696936374498745));
#100311=CARTESIAN_POINT('Ctrl Pts',(0.00455327264161155,-0.0333679869945434,
0.069641165722439));
#100312=CARTESIAN_POINT('Ctrl Pts',(0.00437104376775055,-0.0336938721132425,
0.0697916655347663));
#100313=CARTESIAN_POINT('Ctrl Pts',(0.0044622815990689,-0.0335278710435082,
0.0697131053145341));
#100314=CARTESIAN_POINT('Ctrl Pts',(0.00455595096121121,-0.0333620469224319,
0.0696374339262735));
#100315=CARTESIAN_POINT('Ctrl Pts',(0.00465211102516082,-0.0331951640388601,
0.0695646293168772));
#100316=CARTESIAN_POINT('Ctrl Pts',(0.0043087193905948,-0.0336938721132425,
0.0698477342589842));
#100317=CARTESIAN_POINT('Ctrl Pts',(0.00439878347335318,-0.0335278710435082,
0.0697678693336966));
#100318=CARTESIAN_POINT('Ctrl Pts',(0.00449132041506886,-0.0333620469224319,
0.0696908568909231));
#100319=CARTESIAN_POINT('Ctrl Pts',(0.0045863890466037,-0.0331951640388601,
0.0696166740222545));
#100320=CARTESIAN_POINT('Ctrl Pts',(0.00424639501343906,-0.0336938721132425,
0.0699038029832021));
#100321=CARTESIAN_POINT('Ctrl Pts',(0.00433528534763747,-0.0335278710435082,
0.0698226333528591));
#100322=CARTESIAN_POINT('Ctrl Pts',(0.00442668986892651,-0.0333620469224319,
0.0697442798555727));
#100323=CARTESIAN_POINT('Ctrl Pts',(0.00452066706804658,-0.0331951640388601,
0.0696687187276318));
#100324=CARTESIAN_POINT('Ctrl Pts',(0.00418407063628331,-0.0336938721132425,
0.0699598717074199));
#100325=CARTESIAN_POINT('Ctrl Pts',(0.00427178722192175,-0.0335278710435082,
0.0698773973720216));
#100326=CARTESIAN_POINT('Ctrl Pts',(0.00436205932278417,-0.0333620469224319,
0.0697977028202223));
#100327=CARTESIAN_POINT('Ctrl Pts',(0.00445494508948946,-0.0331951640388601,
0.0697207634330091));
#100328=CARTESIAN_POINT('Ctrl Pts',(0.00455417018691768,-0.0330240426238155,
0.0696423231143738));
#100329=CARTESIAN_POINT('Ctrl Pts',(0.00461626782763365,-0.0329142774063509,
0.0695931482312844));
#100330=CARTESIAN_POINT('Ctrl Pts',(0.00467941300848498,-0.0328043479726686,
0.069545232564417));
#100331=CARTESIAN_POINT('Ctrl Pts',(0.00474352652628386,-0.0326943950436594,
0.0694986397251073));
#100332=CARTESIAN_POINT('Ctrl Pts',(0.00444191493061234,-0.0330240426238155,
0.0696268346213412));
#100333=CARTESIAN_POINT('Ctrl Pts',(0.00450422594040955,-0.0329142774063509,
0.0695761133127312));
#100334=CARTESIAN_POINT('Ctrl Pts',(0.00456761656564961,-0.0328043479726686,
0.0695266548603287));
#100335=CARTESIAN_POINT('Ctrl Pts',(0.00463200734314253,-0.0326943950436594,
0.0694785248605517));
#100336=CARTESIAN_POINT('Ctrl Pts',(0.004329659674307,-0.0330240426238155,
0.0696113461283087));
#100337=CARTESIAN_POINT('Ctrl Pts',(0.00439218405318544,-0.0329142774063509,
0.069559078394178));
#100338=CARTESIAN_POINT('Ctrl Pts',(0.00445582012281424,-0.0328043479726686,
0.0695080771562403));
#100339=CARTESIAN_POINT('Ctrl Pts',(0.0045204881600012,-0.0326943950436594,
0.0694584099959962));
#100340=CARTESIAN_POINT('Ctrl Pts',(0.00421740441800167,-0.0330240426238155,
0.0695958576352761));
#100341=CARTESIAN_POINT('Ctrl Pts',(0.00428014216596133,-0.0329142774063509,
0.0695420434756248));
#100342=CARTESIAN_POINT('Ctrl Pts',(0.00434402367997886,-0.0328043479726686,
0.0694894994521519));
#100343=CARTESIAN_POINT('Ctrl Pts',(0.00440896897685988,-0.0326943950436594,
0.0694382951314406));
#100344=CARTESIAN_POINT('Origin',(0.0145603887075589,-0.0326396682856945,
0.0831317476680125));
#100345=CARTESIAN_POINT('Ctrl Pts',(0.00469109556167719,-0.0331951640388588,
0.069228957174499));
#100346=CARTESIAN_POINT('Ctrl Pts',(0.00475887297930124,-0.0330855618127431,
0.0691816788549149));
#100347=CARTESIAN_POINT('Ctrl Pts',(0.00482767641888813,-0.0329757224171935,
0.0691357672965771));
#100348=CARTESIAN_POINT('Ctrl Pts',(0.0048974206573781,-0.0328657861694599,
0.0690912856138361));
#100349=CARTESIAN_POINT('Ctrl Pts',(0.00467802272848662,-0.0331951640388588,
0.0693415193931692));
#100350=CARTESIAN_POINT('Ctrl Pts',(0.0047442498290795,-0.0330855618127431,
0.0692940610217331));
#100351=CARTESIAN_POINT('Ctrl Pts',(0.00481150555539766,-0.0329757224171935,
0.0692479372393397));
#100352=CARTESIAN_POINT('Ctrl Pts',(0.00487970667965222,-0.0328657861694599,
0.0692032113348868));
#100353=CARTESIAN_POINT('Ctrl Pts',(0.00466494989529606,-0.0331951640388588,
0.0694540816118394));
#100354=CARTESIAN_POINT('Ctrl Pts',(0.00472962667885776,-0.0330855618127431,
0.0694064431885513));
#100355=CARTESIAN_POINT('Ctrl Pts',(0.00479533469190719,-0.0329757224171935,
0.0693601071821022));
#100356=CARTESIAN_POINT('Ctrl Pts',(0.00486199270192635,-0.0328657861694599,
0.0693151370559375));
#100357=CARTESIAN_POINT('Ctrl Pts',(0.00465187706210549,-0.0331951640388588,
0.0695666438305097));
#100358=CARTESIAN_POINT('Ctrl Pts',(0.00471500352863602,-0.0330855618127431,
0.0695188253553695));
#100359=CARTESIAN_POINT('Ctrl Pts',(0.00477916382841672,-0.0329757224171935,
0.0694722771248648));
#100360=CARTESIAN_POINT('Ctrl Pts',(0.00484427872420048,-0.0328657861694599,
0.0694270627769882));
#100361=CARTESIAN_POINT('Origin',(0.0141482943526272,-0.0326401908832812,
0.0833796410202241));
#100362=CARTESIAN_POINT('Ctrl Pts',(0.00462339419571742,-0.0332451089994432,
0.0695865135184027));
#100363=CARTESIAN_POINT('Ctrl Pts',(0.0047955089043147,-0.0329451141710257,
0.0694544942251325));
#100364=CARTESIAN_POINT('Ctrl Pts',(0.00497707888605812,-0.0326442513127503,
0.0693358143682031));
#100365=CARTESIAN_POINT('Ctrl Pts',(0.00442838239585338,-0.0332451089994432,
0.0697429436878515));
#100366=CARTESIAN_POINT('Ctrl Pts',(0.00459459724408313,-0.0329451141710257,
0.0696035694042155));
#100367=CARTESIAN_POINT('Ctrl Pts',(0.00477083813428145,-0.0326442513127503,
0.06947711105007));
#100368=CARTESIAN_POINT('Ctrl Pts',(0.00484425270444921,-0.0325229783203385,
0.0694270807353576));
#100369=CARTESIAN_POINT('Ctrl Pts',(0.00490935804204383,-0.032413025311208,
0.0693818724938979));
#100370=CARTESIAN_POINT('Ctrl Pts',(0.00497538869567019,-0.0323031222247695,
0.069338017896671));
#100371=CARTESIAN_POINT('Ctrl Pts',(0.00504225810254109,-0.0321934096636185,
0.0692955701337264));
#100372=CARTESIAN_POINT('Ctrl Pts',(0.00473319145634849,-0.0325229783203385,
0.0694045742514098));
#100373=CARTESIAN_POINT('Ctrl Pts',(0.00479860704532649,-0.032413025311208,
0.0693578350331017));
#100374=CARTESIAN_POINT('Ctrl Pts',(0.00486497957350275,-0.0323031222247695,
0.0693124561091772));
#100375=CARTESIAN_POINT('Ctrl Pts',(0.00493222197127388,-0.0321934096636185,
0.0692684926067874));
#100376=CARTESIAN_POINT('Ctrl Pts',(0.00462213020824776,-0.0325229783203385,
0.069382067767462));
#100377=CARTESIAN_POINT('Ctrl Pts',(0.00468785604860915,-0.032413025311208,
0.0693337975723054));
#100378=CARTESIAN_POINT('Ctrl Pts',(0.00475457045133531,-0.0323031222247695,
0.0692868943216834));
#100379=CARTESIAN_POINT('Ctrl Pts',(0.00482218584000668,-0.0321934096636185,
0.0692414150798485));
#100380=CARTESIAN_POINT('Ctrl Pts',(0.00451106896014703,-0.0325229783203385,
0.0693595612835142));
#100381=CARTESIAN_POINT('Ctrl Pts',(0.00457710505189181,-0.032413025311208,
0.0693097601115091));
#100382=CARTESIAN_POINT('Ctrl Pts',(0.00464416132916788,-0.0323031222247695,
0.0692613325341897));
#100383=CARTESIAN_POINT('Ctrl Pts',(0.00471214970873947,-0.0321934096636185,
0.0692143375529095));
#100384=CARTESIAN_POINT('Origin',(0.0145556181039783,-0.0326393375177737,
0.0831246813840125));
#100385=CARTESIAN_POINT('Ctrl Pts',(0.00500686402026082,-0.0326943950436593,
0.069023127551441));
#100386=CARTESIAN_POINT('Ctrl Pts',(0.0050775219313848,-0.0325844576448127,
0.0689801705772921));
#100387=CARTESIAN_POINT('Ctrl Pts',(0.00514907326373325,-0.0324744968375319,
0.0689386718844586));
#100388=CARTESIAN_POINT('Ctrl Pts',(0.0052214256081848,-0.0323646534831894,
0.0688986833790018));
#100389=CARTESIAN_POINT('Ctrl Pts',(0.00498674916228668,-0.0326943950436593,
0.0691346466980942));
#100390=CARTESIAN_POINT('Ctrl Pts',(0.00505587013056062,-0.0325844576448127,
0.0690914125035031));
#100391=CARTESIAN_POINT('Ctrl Pts',(0.00512589014466045,-0.0324744968375319,
0.0690496047841102));
#100392=CARTESIAN_POINT('Ctrl Pts',(0.00519671875201782,-0.0323646534831894,
0.0690092758689816));
#100393=CARTESIAN_POINT('Ctrl Pts',(0.00496663430431253,-0.0326943950436593,
0.0692461658447474));
#100394=CARTESIAN_POINT('Ctrl Pts',(0.00503421832973644,-0.0325844576448127,
0.0692026544297142));
#100395=CARTESIAN_POINT('Ctrl Pts',(0.00510270702558766,-0.0324744968375319,
0.0691605376837617));
#100396=CARTESIAN_POINT('Ctrl Pts',(0.00517201189585083,-0.0323646534831894,
0.0691198683589613));
#100397=CARTESIAN_POINT('Ctrl Pts',(0.00494651944633839,-0.0326943950436593,
0.0693576849914006));
#100398=CARTESIAN_POINT('Ctrl Pts',(0.00501256652891226,-0.0325844576448127,
0.0693138963559252));
#100399=CARTESIAN_POINT('Ctrl Pts',(0.00507952390651487,-0.0324744968375319,
0.0692714705834133));
#100400=CARTESIAN_POINT('Ctrl Pts',(0.00514730503968384,-0.0323646534831894,
0.0692304608489411));
#100401=CARTESIAN_POINT('Origin',(0.0141693602333143,-0.0326395579067716,
0.083411076513016));
#100402=CARTESIAN_POINT('Ctrl Pts',(0.00491681253919695,-0.0327445246961876,
0.069375749206536));
#100403=CARTESIAN_POINT('Ctrl Pts',(0.00509687634964127,-0.0324436878365474,
0.0692547963699877));
#100404=CARTESIAN_POINT('Ctrl Pts',(0.00528553927972262,-0.0321434074463186,
0.069147750289658));
#100405=CARTESIAN_POINT('Ctrl Pts',(0.00471236420018378,-0.0327445246961876,
0.0695196271988585));
#100406=CARTESIAN_POINT('Ctrl Pts',(0.00488700156349379,-0.0324436878365474,
0.0693909634672285));
#100407=CARTESIAN_POINT('Ctrl Pts',(0.00507083427853004,-0.0321434074463186,
0.0692758196554833));
#100408=CARTESIAN_POINT('Ctrl Pts',(0.00522774921403184,-0.0322357242816072,
0.0691809842036775));
#100409=CARTESIAN_POINT('Ctrl Pts',(0.00538600592256728,-0.0319819883628705,
0.0690887493093111));
#100410=CARTESIAN_POINT('Ctrl Pts',(0.00554981107443461,-0.0317295851069887,
0.0690067716674996));
#100411=CARTESIAN_POINT('Ctrl Pts',(0.005014543079264,-0.0322357242816072,
0.069311533597002));
#100412=CARTESIAN_POINT('Ctrl Pts',(0.00516864195893842,-0.0319819883628705,
0.0692125083637614));
#100413=CARTESIAN_POINT('Ctrl Pts',(0.00532872979698884,-0.0317295851069887,
0.0691234895699953));
#100414=CARTESIAN_POINT('Origin',(0.0141187006564011,-0.0326371942646127,
0.0833303547028761));
#100415=CARTESIAN_POINT('Origin',(0.0144865115407432,-0.0326352985529064,
0.0830232511827497));
#100416=CARTESIAN_POINT('Ctrl Pts',(0.0053349335308884,-0.0321934096636184,
0.0688375313516916));
#100417=CARTESIAN_POINT('Ctrl Pts',(0.00540819661383477,-0.0320835708272304,
0.0687990709551432));
#100418=CARTESIAN_POINT('Ctrl Pts',(0.0054822131371232,-0.0319739230346346,
0.0687621490428815));
#100419=CARTESIAN_POINT('Ctrl Pts',(0.00555688477628411,-0.0318646057455575,
0.0687268055860474));
#100420=CARTESIAN_POINT('Ctrl Pts',(0.00530785598063264,-0.0321934096636184,
0.0689475675777124));
#100421=CARTESIAN_POINT('Ctrl Pts',(0.00537960157826516,-0.0320835708272304,
0.0689087337606429));
#100422=CARTESIAN_POINT('Ctrl Pts',(0.00545210922436118,-0.0319739230346346,
0.0688714072401796));
#100423=CARTESIAN_POINT('Ctrl Pts',(0.00552528248522519,-0.0318646057455575,
0.0688356286532922));
#100424=CARTESIAN_POINT('Ctrl Pts',(0.00528077843037688,-0.0321934096636184,
0.0690576038037331));
#100425=CARTESIAN_POINT('Ctrl Pts',(0.00535100654269556,-0.0320835708272304,
0.0690183965661427));
#100426=CARTESIAN_POINT('Ctrl Pts',(0.00542200531159916,-0.0319739230346346,
0.0689806654374777));
#100427=CARTESIAN_POINT('Ctrl Pts',(0.00549368019416628,-0.0318646057455575,
0.068944451720537));
#100428=CARTESIAN_POINT('Ctrl Pts',(0.00525370088012111,-0.0321934096636184,
0.0691676400297538));
#100429=CARTESIAN_POINT('Ctrl Pts',(0.00532241150712595,-0.0320835708272304,
0.0691280593716424));
#100430=CARTESIAN_POINT('Ctrl Pts',(0.00539190139883713,-0.0319739230346346,
0.0690899236347759));
#100431=CARTESIAN_POINT('Ctrl Pts',(0.00546207790310737,-0.0318646057455575,
0.0690532747877818));
#100432=CARTESIAN_POINT('Ctrl Pts',(0.00514647479984622,-0.0320218834582372,
0.0692299960887807));
#100433=CARTESIAN_POINT('Ctrl Pts',(0.00519768014652859,-0.0319391099350671,
0.0691990095164114));
#100434=CARTESIAN_POINT('Ctrl Pts',(0.00524933832886476,-0.0318564869454956,
0.0691688412966873));
#100435=CARTESIAN_POINT('Ctrl Pts',(0.00530140966933807,-0.0317740741446553,
0.0691395098904944));
#100436=CARTESIAN_POINT('Ctrl Pts',(0.00509861064546314,-0.0320218834582372,
0.0692171177825111));
#100437=CARTESIAN_POINT('Ctrl Pts',(0.00514995002418067,-0.0319391099350671,
0.0691856330600055));
#100438=CARTESIAN_POINT('Ctrl Pts',(0.00520174993602962,-0.0318564869454956,
0.0691549690848907));
#100439=CARTESIAN_POINT('Ctrl Pts',(0.00525397056655174,-0.0317740741446553,
0.0691251446695073));
#100440=CARTESIAN_POINT('Ctrl Pts',(0.00505074649108006,-0.0320218834582372,
0.0692042394762415));
#100441=CARTESIAN_POINT('Ctrl Pts',(0.00510221990183275,-0.0319391099350671,
0.0691722566035997));
#100442=CARTESIAN_POINT('Ctrl Pts',(0.00515416154319448,-0.0318564869454956,
0.0691410968730942));
#100443=CARTESIAN_POINT('Ctrl Pts',(0.0052065314637654,-0.0317740741446553,
0.0691107794485202));
#100444=CARTESIAN_POINT('Ctrl Pts',(0.00500288233669698,-0.0320218834582372,
0.0691913611699719));
#100445=CARTESIAN_POINT('Ctrl Pts',(0.00505448977948483,-0.0319391099350671,
0.0691588801471938));
#100446=CARTESIAN_POINT('Ctrl Pts',(0.00510657315035933,-0.0318564869454956,
0.0691272246612976));
#100447=CARTESIAN_POINT('Ctrl Pts',(0.00515909236097907,-0.0317740741446553,
0.0690964142275331));
#100448=CARTESIAN_POINT('Origin',(0.00108385226297125,-0.0391228853390487,
0.0643357244328841));
#100449=CARTESIAN_POINT('Ctrl Pts',(0.00305548285383934,-0.0352722978779602,
0.0714303481196738));
#100450=CARTESIAN_POINT('Ctrl Pts',(0.00306472482300037,-0.0352466642097222,
0.0714138654413699));
#100451=CARTESIAN_POINT('Ctrl Pts',(0.00307389017394128,-0.0352210183808304,
0.0713973591033955));
#100452=CARTESIAN_POINT('Ctrl Pts',(0.00308297876453264,-0.0351953608940152,
0.0713808282647492));
#100453=CARTESIAN_POINT('Origin',(-0.00112696451673218,-0.035245600306509,
0.0688775306198176));
#100454=CARTESIAN_POINT('Ctrl Pts',(0.00314545449453057,-0.0350241211493339,
0.0712729297078573));
#100455=CARTESIAN_POINT('Ctrl Pts',(0.00318508495637312,-0.0349144232867421,
0.0712043552880952));
#100456=CARTESIAN_POINT('Ctrl Pts',(0.00322615662114941,-0.0348045283677512,
0.0711365590131672));
#100457=CARTESIAN_POINT('Ctrl Pts',(0.00326862011273923,-0.0346945769586887,
0.071069629679129));
#100458=CARTESIAN_POINT('Ctrl Pts',(0.00303538047663015,-0.0350241211493339,
0.0712998527906354));
#100459=CARTESIAN_POINT('Ctrl Pts',(0.00307464008406305,-0.0349144232867421,
0.0712297621464773));
#100460=CARTESIAN_POINT('Ctrl Pts',(0.00311537201389575,-0.0348045283677512,
0.0711604410737945));
#100461=CARTESIAN_POINT('Ctrl Pts',(0.00315752739784363,-0.0346945769586887,
0.0710919803055216));
#100462=CARTESIAN_POINT('Ctrl Pts',(0.00292530645872974,-0.0350241211493339,
0.0713267758734136));
#100463=CARTESIAN_POINT('Ctrl Pts',(0.00296419521175299,-0.0349144232867421,
0.0712551690048593));
#100464=CARTESIAN_POINT('Ctrl Pts',(0.00300458740664209,-0.0348045283677512,
0.0711843231344218));
#100465=CARTESIAN_POINT('Ctrl Pts',(0.00304643468294803,-0.0346945769586887,
0.0711143309319143));
#100466=CARTESIAN_POINT('Ctrl Pts',(0.00281523244082933,-0.0350241211493339,
0.0713536989561917));
#100467=CARTESIAN_POINT('Ctrl Pts',(0.00285375033944292,-0.0349144232867421,
0.0712805758632414));
#100468=CARTESIAN_POINT('Ctrl Pts',(0.00289380279938843,-0.0348045283677512,
0.0712082051950491));
#100469=CARTESIAN_POINT('Ctrl Pts',(0.00293534196805244,-0.0346945769586887,
0.071136681558307));
#100470=CARTESIAN_POINT('Origin',(0.0173476319408053,-0.0345629067939361,
0.0802153595577315));
#100471=CARTESIAN_POINT('Ctrl Pts',(0.00314376063159375,-0.0351970973651645,
0.0709289897510182));
#100472=CARTESIAN_POINT('Ctrl Pts',(0.00318838336335184,-0.03508693493218,
0.0708599983014073));
#100473=CARTESIAN_POINT('Ctrl Pts',(0.00323447735406611,-0.0349764985129749,
0.0707918773819471));
#100474=CARTESIAN_POINT('Ctrl Pts',(0.00328198808268525,-0.0348659306849666,
0.0707247187605296));
#100475=CARTESIAN_POINT('Ctrl Pts',(0.00316502677698795,-0.0351970973651645,
0.0710084140653692));
#100476=CARTESIAN_POINT('Ctrl Pts',(0.00320854919250971,-0.03508693493218,
0.070939717229382));
#100477=CARTESIAN_POINT('Ctrl Pts',(0.0032535358306445,-0.0349764985129748,
0.0708718682926352));
#100478=CARTESIAN_POINT('Ctrl Pts',(0.00329993358420676,-0.0348659306849666,
0.0708049585862098));
#100479=CARTESIAN_POINT('Ctrl Pts',(0.00318629292238215,-0.0351970973651645,
0.0710878383797203));
#100480=CARTESIAN_POINT('Ctrl Pts',(0.00322871502166757,-0.03508693493218,
0.0710194361573567));
#100481=CARTESIAN_POINT('Ctrl Pts',(0.0032725943072229,-0.0349764985129748,
0.0709518592033234));
#100482=CARTESIAN_POINT('Ctrl Pts',(0.00331787908572827,-0.0348659306849666,
0.0708851984118901));
#100483=CARTESIAN_POINT('Ctrl Pts',(0.00320755906777635,-0.0351970973651645,
0.0711672626940713));
#100484=CARTESIAN_POINT('Ctrl Pts',(0.00324888085082544,-0.03508693493218,
0.0710991550853315));
#100485=CARTESIAN_POINT('Ctrl Pts',(0.00329165278380129,-0.0349764985129748,
0.0710318501140115));
#100486=CARTESIAN_POINT('Ctrl Pts',(0.00333582458724978,-0.0348659306849666,
0.0709654382375704));
#100487=CARTESIAN_POINT('Origin',(0.0170465695611525,-0.0345637187966549,
0.0805904419479017));
#100488=CARTESIAN_POINT('Ctrl Pts',(0.00318927542078819,-0.0352450361861253,
0.0711955511657964));
#100489=CARTESIAN_POINT('Ctrl Pts',(0.00330070428416582,-0.0349452761023765,
0.071009443193777));
#100490=CARTESIAN_POINT('Ctrl Pts',(0.00342583500347301,-0.0346444289983475,
0.070832257212592));
#100491=CARTESIAN_POINT('Ctrl Pts',(0.00306554359310653,-0.0352450361861253,
0.0714127847608469));
#100492=CARTESIAN_POINT('Ctrl Pts',(0.00316877935721512,-0.0349452761023765,
0.0712220101664909));
#100493=CARTESIAN_POINT('Ctrl Pts',(0.0032860917620643,-0.0346444289983475,
0.0710395536826068));
#100494=CARTESIAN_POINT('Ctrl Pts',(0.00333593024175403,-0.0345231616327822,
0.0709660159461851));
#100495=CARTESIAN_POINT('Ctrl Pts',(0.0033798169792446,-0.0344132092796975,
0.0709000221477925));
#100496=CARTESIAN_POINT('Ctrl Pts',(0.00342506648204582,-0.0343032738558974,
0.070834939516924));
#100497=CARTESIAN_POINT('Ctrl Pts',(0.00347161864454688,-0.0341934961088741,
0.0707708499470323));
#100498=CARTESIAN_POINT('Ctrl Pts',(0.003224382943228,-0.0345231616327822,
0.0709859743110989));
#100499=CARTESIAN_POINT('Ctrl Pts',(0.00326799458275737,-0.0344132092796975,
0.0709184429902421));
#100500=CARTESIAN_POINT('Ctrl Pts',(0.00331300080423056,-0.0343032738558974,
0.0708518172260543));
#100501=CARTESIAN_POINT('Ctrl Pts',(0.00335934176306841,-0.0341934961088741,
0.0707861808969037));
#100502=CARTESIAN_POINT('Ctrl Pts',(0.00311283564470197,-0.0345231616327822,
0.0710059326760127));
#100503=CARTESIAN_POINT('Ctrl Pts',(0.00315617218627013,-0.0344132092796975,
0.0709368638326918));
#100504=CARTESIAN_POINT('Ctrl Pts',(0.0032009351264153,-0.0343032738558974,
0.0708686949351846));
#100505=CARTESIAN_POINT('Ctrl Pts',(0.00324706488158994,-0.0341934961088741,
0.0708015118467751));
#100506=CARTESIAN_POINT('Ctrl Pts',(0.00300128834617593,-0.0345231616327822,
0.0710258910409265));
#100507=CARTESIAN_POINT('Ctrl Pts',(0.00304434978978289,-0.0344132092796975,
0.0709552846751415));
#100508=CARTESIAN_POINT('Ctrl Pts',(0.00308886944860003,-0.0343032738558974,
0.0708855726443149));
#100509=CARTESIAN_POINT('Ctrl Pts',(0.00313478800011147,-0.0341934961088741,
0.0708168427966465));
#100510=CARTESIAN_POINT('Origin',(0.0173578804990277,-0.0345625596230697,
0.0802217989179083));
#100511=CARTESIAN_POINT('Ctrl Pts',(0.00333841734075968,-0.0346945769586886,
0.0705305686593154));
#100512=CARTESIAN_POINT('Ctrl Pts',(0.00338829493406878,-0.0345846629176052,
0.0704646239128968));
#100513=CARTESIAN_POINT('Ctrl Pts',(0.0034395447568674,-0.0344746925050311,
0.0703996993510994));
#100514=CARTESIAN_POINT('Ctrl Pts',(0.00349210079841876,-0.0343648066253259,
0.0703358778915575));
#100515=CARTESIAN_POINT('Ctrl Pts',(0.00336076794955423,-0.0346945769586886,
0.0706416612867402));
#100516=CARTESIAN_POINT('Ctrl Pts',(0.00340911463030587,-0.0345846629176052,
0.0705760245430078));
#100517=CARTESIAN_POINT('Ctrl Pts',(0.00345882690969433,-0.0344746925050311,
0.0705113763778614));
#100518=CARTESIAN_POINT('Ctrl Pts',(0.00350984074852324,-0.0343648066253259,
0.0704477993629199));
#100519=CARTESIAN_POINT('Ctrl Pts',(0.00338311855834878,-0.0346945769586886,
0.0707527539141651));
#100520=CARTESIAN_POINT('Ctrl Pts',(0.00342993432654296,-0.0345846629176052,
0.070687425173119));
#100521=CARTESIAN_POINT('Ctrl Pts',(0.00347810906252126,-0.0344746925050311,
0.0706230534046234));
#100522=CARTESIAN_POINT('Ctrl Pts',(0.00352758069862772,-0.0343648066253259,
0.0705597208342823));
#100523=CARTESIAN_POINT('Ctrl Pts',(0.00340546916714334,-0.0346945769586886,
0.0708638465415899));
#100524=CARTESIAN_POINT('Ctrl Pts',(0.00345075402278005,-0.0345846629176052,
0.07079882580323));
#100525=CARTESIAN_POINT('Ctrl Pts',(0.00349739121534819,-0.0344746925050311,
0.0707347304313854));
#100526=CARTESIAN_POINT('Ctrl Pts',(0.0035453206487322,-0.0343648066253259,
0.0706716423056448));
#100527=CARTESIAN_POINT('Origin',(0.0170943990081613,-0.0345626446732366,
0.080624004942947));
#100528=CARTESIAN_POINT('Ctrl Pts',(0.00340506923980482,-0.0346945769586885,
0.0708618587219638));
#100529=CARTESIAN_POINT('Ctrl Pts',(0.00347394067537212,-0.034527515336289,
0.0707630233898889));
#100530=CARTESIAN_POINT('Ctrl Pts',(0.00354593820484234,-0.0343603235965158,
0.0706663284371914));
#100531=CARTESIAN_POINT('Ctrl Pts',(0.00362084464106438,-0.0341934961088739,
0.0705720566798239));
#100532=CARTESIAN_POINT('Ctrl Pts',(0.00335864662719066,-0.0346945769586885,
0.0709316653790199));
#100533=CARTESIAN_POINT('Ctrl Pts',(0.00342605593437689,-0.034527515336289,
0.0708318577067372));
#100534=CARTESIAN_POINT('Ctrl Pts',(0.00349662153648929,-0.0343603235965158,
0.0707341441797431));
#100535=CARTESIAN_POINT('Ctrl Pts',(0.00357013043660882,-0.0341934961088739,
0.0706388106894242));
#100536=CARTESIAN_POINT('Ctrl Pts',(0.0033122240145765,-0.0346945769586885,
0.071001472036076));
#100537=CARTESIAN_POINT('Ctrl Pts',(0.00337817119338165,-0.034527515336289,
0.0709006920235855));
#100538=CARTESIAN_POINT('Ctrl Pts',(0.00344730486813625,-0.0343603235965158,
0.0708019599222949));
#100539=CARTESIAN_POINT('Ctrl Pts',(0.00351941623215327,-0.0341934961088739,
0.0707055646990244));
#100540=CARTESIAN_POINT('Ctrl Pts',(0.00326580140196235,-0.0346945769586885,
0.0710712786931321));
#100541=CARTESIAN_POINT('Ctrl Pts',(0.00333028645238642,-0.034527515336289,
0.0709695263404338));
#100542=CARTESIAN_POINT('Ctrl Pts',(0.0033979881997832,-0.0343603235965158,
0.0708697756648466));
#100543=CARTESIAN_POINT('Ctrl Pts',(0.00346870202769771,-0.0341934961088739,
0.0707723187086247));
#100544=CARTESIAN_POINT('Ctrl Pts',(0.00354530200359632,-0.0340223579322366,
0.070671667768251));
#100545=CARTESIAN_POINT('Ctrl Pts',(0.00359327727694297,-0.0339125849573554,
0.0706085185852605));
#100546=CARTESIAN_POINT('Ctrl Pts',(0.00364252587996998,-0.0338030433565221,
0.070546406753149));
#100547=CARTESIAN_POINT('Ctrl Pts',(0.00369297779083012,-0.0336938721132328,
0.0704854061195093));
#100548=CARTESIAN_POINT('Ctrl Pts',(0.00343272143262576,-0.0340223579322366,
0.0706845826770892));
#100549=CARTESIAN_POINT('Ctrl Pts',(0.00348051857569604,-0.0339125849573554,
0.0706198807144027));
#100550=CARTESIAN_POINT('Ctrl Pts',(0.0035296213125483,-0.0338030433565221,
0.0705562135068326));
#100551=CARTESIAN_POINT('Ctrl Pts',(0.00357995963155151,-0.0336938721132328,
0.0704936569075705));
#100552=CARTESIAN_POINT('Ctrl Pts',(0.0033201408616552,-0.0340223579322366,
0.0706974975859275));
#100553=CARTESIAN_POINT('Ctrl Pts',(0.00336775987444911,-0.0339125849573554,
0.0706312428435448));
#100554=CARTESIAN_POINT('Ctrl Pts',(0.00341671674512663,-0.0338030433565221,
0.070566020260516));
#100555=CARTESIAN_POINT('Ctrl Pts',(0.0034669414722729,-0.0336938721132328,
0.0705019076956318));
#100556=CARTESIAN_POINT('Ctrl Pts',(0.00320756029068464,-0.0340223579322366,
0.0707104124947657));
#100557=CARTESIAN_POINT('Ctrl Pts',(0.00325500117320218,-0.0339125849573554,
0.0706426049726869));
#100558=CARTESIAN_POINT('Ctrl Pts',(0.00330381217770495,-0.0338030433565221,
0.0705758270141996));
#100559=CARTESIAN_POINT('Ctrl Pts',(0.0033539233129943,-0.0336938721132328,
0.0705101584836931));
#100560=CARTESIAN_POINT('Origin',(0.0172588781084155,-0.0345589643413925,
0.0801535977097717));
#100561=CARTESIAN_POINT('Ctrl Pts',(0.00357512613946545,-0.034193496108874,
0.0702372352350696));
#100562=CARTESIAN_POINT('Ctrl Pts',(0.00362908084852657,-0.0340836138581106,
0.0701745119616971));
#100563=CARTESIAN_POINT('Ctrl Pts',(0.00368430759563511,-0.0339738896643499,
0.0701129352636219));
#100564=CARTESIAN_POINT('Ctrl Pts',(0.00374073041431604,-0.0338644633294062,
0.0700525792131577));
#100565=CARTESIAN_POINT('Ctrl Pts',(0.00359045710313133,-0.034193496108874,
0.0703495122175726));
#100566=CARTESIAN_POINT('Ctrl Pts',(0.00364286357909152,-0.0340836138581106,
0.0702870003491104));
#100567=CARTESIAN_POINT('Ctrl Pts',(0.00369653846138944,-0.0339738896643499,
0.070225602917074));
#100568=CARTESIAN_POINT('Ctrl Pts',(0.00375140778512577,-0.0338644633294062,
0.0701653938974833));
#100569=CARTESIAN_POINT('Ctrl Pts',(0.0036057880667972,-0.034193496108874,
0.0704617892000756));
#100570=CARTESIAN_POINT('Ctrl Pts',(0.00365664630965646,-0.0340836138581106,
0.0703994887365236));
#100571=CARTESIAN_POINT('Ctrl Pts',(0.00370876932714378,-0.0339738896643499,
0.0703382705705262));
#100572=CARTESIAN_POINT('Ctrl Pts',(0.00376208515593551,-0.0338644633294062,
0.0702782085818089));
#100573=CARTESIAN_POINT('Ctrl Pts',(0.00362111903046307,-0.034193496108874,
0.0705740661825786));
#100574=CARTESIAN_POINT('Ctrl Pts',(0.00367042904022141,-0.0340836138581106,
0.0705119771239369));
#100575=CARTESIAN_POINT('Ctrl Pts',(0.00372100019289811,-0.0339738896643499,
0.0704509382239784));
#100576=CARTESIAN_POINT('Ctrl Pts',(0.00377276252674524,-0.0338644633294062,
0.0703910232661346));
#100577=CARTESIAN_POINT('Origin',(0.0170340332225967,-0.0345610621861625,
0.0805790325330161));
#100578=CARTESIAN_POINT('Ctrl Pts',(0.00359842765729212,-0.03424362768739,
0.0706004519548022));
#100579=CARTESIAN_POINT('Ctrl Pts',(0.00373230106874527,-0.0339430054201859,
0.0704297753948485));
#100580=CARTESIAN_POINT('Ctrl Pts',(0.00387865021769195,-0.0336441434784161,
0.0702696676029884));
#100581=CARTESIAN_POINT('Ctrl Pts',(0.00344844763316054,-0.03424362768739,
0.0708004669351448));
#100582=CARTESIAN_POINT('Ctrl Pts',(0.00357477735527091,-0.0339430054201859,
0.0706241337853311));
#100583=CARTESIAN_POINT('Ctrl Pts',(0.00371403032323082,-0.0336441434784161,
0.0704578172517991));
#100584=CARTESIAN_POINT('Ctrl Pts',(0.00377274449345952,-0.0335235895815127,
0.0703910443333679));
#100585=CARTESIAN_POINT('Ctrl Pts',(0.00382449391891267,-0.0334144449262719,
0.0703311437330281));
#100586=CARTESIAN_POINT('Ctrl Pts',(0.00387754029950884,-0.0333049234473133,
0.0702722434183398));
#100587=CARTESIAN_POINT('Ctrl Pts',(0.00393182262760982,-0.0331951640388588,
0.07021442484906));
#100588=CARTESIAN_POINT('Ctrl Pts',(0.00365957517040082,-0.0335235895815127,
0.0703968647117698));
#100589=CARTESIAN_POINT('Ctrl Pts',(0.003711244466886,-0.0334144449262719,
0.0703354061128883));
#100590=CARTESIAN_POINT('Ctrl Pts',(0.00376424281353307,-0.0333049234473133,
0.0702749443543024));
#100591=CARTESIAN_POINT('Ctrl Pts',(0.00381850944498583,-0.0331951640388588,
0.070215562886813));
#100592=CARTESIAN_POINT('Ctrl Pts',(0.00354640584734212,-0.0335235895815127,
0.0704026850901717));
#100593=CARTESIAN_POINT('Ctrl Pts',(0.00359799501485933,-0.0334144449262719,
0.0703396684927484));
#100594=CARTESIAN_POINT('Ctrl Pts',(0.0036509453275573,-0.0333049234473133,
0.070277645290265));
#100595=CARTESIAN_POINT('Ctrl Pts',(0.00370519626236183,-0.0331951640388588,
0.0702167009245659));
#100596=CARTESIAN_POINT('Ctrl Pts',(0.00343323652428342,-0.0335235895815127,
0.0704085054685736));
#100597=CARTESIAN_POINT('Ctrl Pts',(0.00348474556283266,-0.0334144449262719,
0.0703439308726085));
#100598=CARTESIAN_POINT('Ctrl Pts',(0.00353764784158153,-0.0333049234473133,
0.0702803462262276));
#100599=CARTESIAN_POINT('Ctrl Pts',(0.00359188307973784,-0.0331951640388588,
0.0702178389623189));
#100600=CARTESIAN_POINT('Origin',(0.0155492903479003,-0.0326434571768441,
0.0821653781509418));
#100601=CARTESIAN_POINT('Ctrl Pts',(0.00382963877748485,-0.0336938721132367,
0.0699573215171435));
#100602=CARTESIAN_POINT('Ctrl Pts',(0.00385417991592264,-0.0336474569764946,
0.0699321864707846));
#100603=CARTESIAN_POINT('Ctrl Pts',(0.00387901361023897,-0.033601104548885,
0.0699073404317061));
#100604=CARTESIAN_POINT('Ctrl Pts',(0.00394188680916358,-0.0334837508694597,
0.0698444359786847));
#100605=CARTESIAN_POINT('Ctrl Pts',(0.00400659638802133,-0.0333660264863578,
0.0697834222117383));
#100606=CARTESIAN_POINT('Ctrl Pts',(0.00385439107964342,-0.0336938721132367,
0.0702963751453641));
#100607=CARTESIAN_POINT('Ctrl Pts',(0.00387694762468536,-0.0336474569764946,
0.0702713849824435));
#100608=CARTESIAN_POINT('Ctrl Pts',(0.00389979516554788,-0.033601104548885,
0.0702466605847043));
#100609=CARTESIAN_POINT('Ctrl Pts',(0.00395763988100942,-0.0334837508694597,
0.0701840640995601));
#100610=CARTESIAN_POINT('Ctrl Pts',(0.00401731405881714,-0.0333660264863578,
0.0701232091608762));
#100611=CARTESIAN_POINT('Ctrl Pts',(0.00385439107965538,-0.0336938721132426,
0.070296375145372));
#100612=CARTESIAN_POINT('Ctrl Pts',(0.00387694762469635,-0.0336474569765026,
0.0702713849824524));
#100613=CARTESIAN_POINT('Ctrl Pts',(0.00389979516555788,-0.0336011045488949,
0.0702466605847143));
#100614=CARTESIAN_POINT('Ctrl Pts',(0.00395715811332046,-0.033484728265791,
0.0701845854430388));
#100615=CARTESIAN_POINT('Ctrl Pts',(0.00401632039107351,-0.0333679870047996,
0.0701242227403068));
#100616=CARTESIAN_POINT('Ctrl Pts',(0.00385439107964064,-0.0336938721132424,
0.0702963751453673));
#100617=CARTESIAN_POINT('Ctrl Pts',(0.00393506326697639,-0.0335278710435081,
0.0702069992635138));
#100618=CARTESIAN_POINT('Ctrl Pts',(0.00401850987844153,-0.0333620469224319,
0.0701201846827083));
#100619=CARTESIAN_POINT('Ctrl Pts',(0.00410478685445126,-0.0331951640388601,
0.0700359021076483));
#100620=CARTESIAN_POINT('Ctrl Pts',(0.0037995854233222,-0.0336938721132424,
0.0703598130666666));
#100621=CARTESIAN_POINT('Ctrl Pts',(0.00387892959455252,-0.0335278710435081,
0.0702692898774492));
#100622=CARTESIAN_POINT('Ctrl Pts',(0.00396108463636584,-0.0333620469224319,
0.07018128674666));
#100623=CARTESIAN_POINT('Ctrl Pts',(0.00404610604454009,-0.0331951640388601,
0.0700957735730675));
#100624=CARTESIAN_POINT('Ctrl Pts',(0.00374477976700376,-0.0336938721132424,
0.0704232509879659));
#100625=CARTESIAN_POINT('Ctrl Pts',(0.00382279592212864,-0.0335278710435081,
0.0703315804913845));
#100626=CARTESIAN_POINT('Ctrl Pts',(0.00390365939429015,-0.0333620469224319,
0.0702423888106118));
#100627=CARTESIAN_POINT('Ctrl Pts',(0.00398742523462892,-0.0331951640388601,
0.0701556450384867));
#100628=CARTESIAN_POINT('Ctrl Pts',(0.00368997411068532,-0.0336938721132424,
0.0704866889092652));
#100629=CARTESIAN_POINT('Ctrl Pts',(0.00376666224970477,-0.0335278710435081,
0.0703938711053199));
#100630=CARTESIAN_POINT('Ctrl Pts',(0.00384623415221446,-0.0333620469224319,
0.0703034908745635));
#100631=CARTESIAN_POINT('Ctrl Pts',(0.00392874442471776,-0.0331951640388601,
0.0702155165039059));
#100632=CARTESIAN_POINT('Ctrl Pts',(0.00401735592383927,-0.0330240426238156,
0.0701252585083006));
#100633=CARTESIAN_POINT('Ctrl Pts',(0.00407280065900278,-0.0329142774063509,
0.0700686884857445));
#100634=CARTESIAN_POINT('Ctrl Pts',(0.00412944249577568,-0.0328043479726686,
0.0700132364585221));
#100635=CARTESIAN_POINT('Ctrl Pts',(0.00418721082812532,-0.0326943950436594,
0.069958975463166));
#100636=CARTESIAN_POINT('Ctrl Pts',(0.00390404461084407,-0.0330240426238156,
0.0701239614609192));
#100637=CARTESIAN_POINT('Ctrl Pts',(0.00395950721409892,-0.0329142774063509,
0.0700658304646327));
#100638=CARTESIAN_POINT('Ctrl Pts',(0.00401619919755841,-0.0328043479726686,
0.0700088170548609));
#100639=CARTESIAN_POINT('Ctrl Pts',(0.00407404994603473,-0.0326943950436594,
0.069952996270153));
#100640=CARTESIAN_POINT('Ctrl Pts',(0.00379073329784888,-0.0330240426238156,
0.0701226644135377));
#100641=CARTESIAN_POINT('Ctrl Pts',(0.00384621376919505,-0.0329142774063509,
0.0700629724435208));
#100642=CARTESIAN_POINT('Ctrl Pts',(0.00390295589934115,-0.0328043479726686,
0.0700043976511997));
#100643=CARTESIAN_POINT('Ctrl Pts',(0.00396088906394415,-0.0326943950436594,
0.0699470170771401));
#100644=CARTESIAN_POINT('Ctrl Pts',(0.00367742198485368,-0.0330240426238156,
0.0701213673661562));
#100645=CARTESIAN_POINT('Ctrl Pts',(0.00373292032429119,-0.0329142774063509,
0.070060114422409));
#100646=CARTESIAN_POINT('Ctrl Pts',(0.00378971260112388,-0.0328043479726686,
0.0699999782475385));
#100647=CARTESIAN_POINT('Ctrl Pts',(0.00384772818185357,-0.0326943950436594,
0.0699410378841271));
#100648=CARTESIAN_POINT('Origin',(0.0156353456212262,-0.0326396682857831,
0.08225420319739));
#100649=CARTESIAN_POINT('Ctrl Pts',(0.00410139311123134,-0.0331951640388587,
0.0696979907823525));
#100650=CARTESIAN_POINT('Ctrl Pts',(0.00416271053186312,-0.0330855618255041,
0.0696425905099765));
#100651=CARTESIAN_POINT('Ctrl Pts',(0.00422521718429758,-0.0329757224427708,
0.0695884176265899));
#100652=CARTESIAN_POINT('Ctrl Pts',(0.00428883642783697,-0.0328657862078596,
0.0695355454301241));
#100653=CARTESIAN_POINT('Ctrl Pts',(0.00410253114807826,-0.0331951640388587,
0.0698113038747634));
#100654=CARTESIAN_POINT('Ctrl Pts',(0.0041622879100926,-0.0330855618255041,
0.0697559192765427));
#100655=CARTESIAN_POINT('Ctrl Pts',(0.00422323245489464,-0.0329757224427708,
0.0697017298224648));
#100656=CARTESIAN_POINT('Ctrl Pts',(0.00428529014320011,-0.0328657862078596,
0.0696488087335584));
#100657=CARTESIAN_POINT('Ctrl Pts',(0.00410366918492518,-0.0331951640388587,
0.0699246169671742));
#100658=CARTESIAN_POINT('Ctrl Pts',(0.00416186528832207,-0.0330855618255041,
0.0698692480431089));
#100659=CARTESIAN_POINT('Ctrl Pts',(0.0042212477254917,-0.0329757224427708,
0.0698150420183397));
#100660=CARTESIAN_POINT('Ctrl Pts',(0.00428174385856326,-0.0328657862078596,
0.0697620720369927));
#100661=CARTESIAN_POINT('Ctrl Pts',(0.00410480722177209,-0.0331951640388587,
0.0700379300595851));
#100662=CARTESIAN_POINT('Ctrl Pts',(0.00416144266655155,-0.0330855618255041,
0.0699825768096751));
#100663=CARTESIAN_POINT('Ctrl Pts',(0.00421926299608876,-0.0329757224427708,
0.0699283542142146));
#100664=CARTESIAN_POINT('Ctrl Pts',(0.0042781975739264,-0.0328657862078596,
0.0698753353404269));
#100665=CARTESIAN_POINT('Origin',(0.0152575700259859,-0.0326401908832753,
0.0825517909517735));
#100666=CARTESIAN_POINT('Ctrl Pts',(0.0040790392835265,-0.0332451089994432,
0.0700612129188001));
#100667=CARTESIAN_POINT('Ctrl Pts',(0.00423325041131986,-0.0329451141710257,
0.0699086629441171));
#100668=CARTESIAN_POINT('Ctrl Pts',(0.00439851412929696,-0.0326442513127503,
0.0697681621603776));
#100669=CARTESIAN_POINT('Ctrl Pts',(0.00390517110891562,-0.0332451089994432,
0.0702408510490995));
#100670=CARTESIAN_POINT('Ctrl Pts',(0.00405260707377728,-0.0329451141710257,
0.070081743528924));
#100671=CARTESIAN_POINT('Ctrl Pts',(0.00421160881747946,-0.0326442513127503,
0.0699341934960175));
#100672=CARTESIAN_POINT('Ctrl Pts',(0.00427817403071446,-0.0325229783203385,
0.0698753563998101));
#100673=CARTESIAN_POINT('Ctrl Pts',(0.00433709989819023,-0.0324130253112079,
0.0698223447763543));
#100674=CARTESIAN_POINT('Ctrl Pts',(0.00439711344191326,-0.0323031222247695,
0.0697705601503919));
#100675=CARTESIAN_POINT('Ctrl Pts',(0.00445813544815066,-0.0321934096636184,
0.069720066141747));
#100676=CARTESIAN_POINT('Ctrl Pts',(0.00416516772331802,-0.0325229783203385,
0.0698669470515587));
#100677=CARTESIAN_POINT('Ctrl Pts',(0.00422420951347343,-0.0324130253112079,
0.0698123776386551));
#100678=CARTESIAN_POINT('Ctrl Pts',(0.00428437118716941,-0.0323031222247695,
0.0697590378575237));
#100679=CARTESIAN_POINT('Ctrl Pts',(0.00434557327063648,-0.0321934096636184,
0.0697069933133363));
#100680=CARTESIAN_POINT('Ctrl Pts',(0.00405216141592158,-0.0325229783203385,
0.0698585377033074));
#100681=CARTESIAN_POINT('Ctrl Pts',(0.00411131912875662,-0.0324130253112079,
0.0698024105009559));
#100682=CARTESIAN_POINT('Ctrl Pts',(0.00417162893242555,-0.0323031222247695,
0.0697475155646555));
#100683=CARTESIAN_POINT('Ctrl Pts',(0.00423301109312229,-0.0321934096636184,
0.0696939204849255));
#100684=CARTESIAN_POINT('Ctrl Pts',(0.00393915510852514,-0.0325229783203385,
0.069850128355056));
#100685=CARTESIAN_POINT('Ctrl Pts',(0.00399842874403982,-0.0324130253112079,
0.0697924433632568));
#100686=CARTESIAN_POINT('Ctrl Pts',(0.0040588866776817,-0.0323031222247695,
0.0697359932717873));
#100687=CARTESIAN_POINT('Ctrl Pts',(0.00412044891560811,-0.0321934096636184,
0.0696808476565148));
#100688=CARTESIAN_POINT('Origin',(0.0156297269948085,-0.0326393375177989,
0.0822477905481969));
#100689=CARTESIAN_POINT('Ctrl Pts',(0.0043888743489824,-0.0326943950436593,
0.0694542079053788));
#100690=CARTESIAN_POINT('Ctrl Pts',(0.00445359116489844,-0.0325844576448127,
0.0694027338753235));
#100691=CARTESIAN_POINT('Ctrl Pts',(0.00451937712825846,-0.0324744968375319,
0.069352594652229));
#100692=CARTESIAN_POINT('Ctrl Pts',(0.00458614706416913,-0.0323646534831894,
0.0693038533147957));
#100693=CARTESIAN_POINT('Ctrl Pts',(0.00438289515792577,-0.0326943950436593,
0.0695673687504441));
#100694=CARTESIAN_POINT('Ctrl Pts',(0.00444605240531079,-0.0325844576448127,
0.0695158123159298));
#100695=CARTESIAN_POINT('Ctrl Pts',(0.00451028039402602,-0.0324744968375319,
0.0694655584281103));
#100696=CARTESIAN_POINT('Ctrl Pts',(0.00457549594331969,-0.0323646534831894,
0.0694166703401343));
#100697=CARTESIAN_POINT('Ctrl Pts',(0.00437691596686915,-0.0326943950436594,
0.0696805295955094));
#100698=CARTESIAN_POINT('Ctrl Pts',(0.00443851364572314,-0.0325844576448127,
0.0696288907565362));
#100699=CARTESIAN_POINT('Ctrl Pts',(0.00450118365979357,-0.0324744968375319,
0.0695785222039916));
#100700=CARTESIAN_POINT('Ctrl Pts',(0.00456484482247025,-0.0323646534831894,
0.0695294873654728));
#100701=CARTESIAN_POINT('Ctrl Pts',(0.00437093677581252,-0.0326943950436594,
0.0697936904405747));
#100702=CARTESIAN_POINT('Ctrl Pts',(0.0044309748861355,-0.0325844576448127,
0.0697419691971425));
#100703=CARTESIAN_POINT('Ctrl Pts',(0.00449208692556113,-0.0324744968375319,
0.0696914859798729));
#100704=CARTESIAN_POINT('Ctrl Pts',(0.00455419370162081,-0.0323646534831894,
0.0696423043908113));
#100705=CARTESIAN_POINT('Origin',(0.0152824097106913,-0.0326395579068753,
0.0825803383141517));
#100706=CARTESIAN_POINT('Ctrl Pts',(0.00434372816300158,-0.0327445246961877,
0.0698153354767094));
#100707=CARTESIAN_POINT('Ctrl Pts',(0.00450721270640475,-0.0324436878365475,
0.0696727684097933));
#100708=CARTESIAN_POINT('Ctrl Pts',(0.00468097154154346,-0.0321434074463186,
0.0695429206846993));
#100709=CARTESIAN_POINT('Ctrl Pts',(0.00415892465422382,-0.0327445246961877,
0.0699837031195135));
#100710=CARTESIAN_POINT('Ctrl Pts',(0.00431605910823487,-0.0324436878365475,
0.0698341660743927));
#100711=CARTESIAN_POINT('Ctrl Pts',(0.00448401090115397,-0.0321434074463186,
0.0696968898573845));
#100712=CARTESIAN_POINT('Ctrl Pts',(0.00462780248168976,-0.0322357242816072,
0.0695831355551812));
#100713=CARTESIAN_POINT('Ctrl Pts',(0.00477325119125102,-0.0319819883628705,
0.069471793135492));
#100714=CARTESIAN_POINT('Ctrl Pts',(0.00492549016764143,-0.0317295851069887,
0.0693699316825138));
#100715=CARTESIAN_POINT('Ctrl Pts',(0.00443263971858135,-0.0322357242816072,
0.0697393773418322));
#100716=CARTESIAN_POINT('Ctrl Pts',(0.00457311232987594,-0.0319819883628705,
0.069621819241255));
#100717=CARTESIAN_POINT('Ctrl Pts',(0.0047207808142367,-0.0317295851069887,
0.069513438060869));
#100718=CARTESIAN_POINT('Origin',(0.0152220324737634,-0.0326371942646248,
0.08250660234782));
#100719=CARTESIAN_POINT('Origin',(0.0155484527814898,-0.0326352985525135,
0.0821558215032046));
#100720=CARTESIAN_POINT('Ctrl Pts',(0.00469109556167726,-0.0321934096636183,
0.0692289571744985));
#100721=CARTESIAN_POINT('Ctrl Pts',(0.00475896057746837,-0.0320835708272304,
0.0691816177505778));
#100722=CARTESIAN_POINT('Ctrl Pts',(0.00482776591570985,-0.0319739230346346,
0.0691357102484214));
#100723=CARTESIAN_POINT('Ctrl Pts',(0.00489741903696226,-0.0318646057455575,
0.0690912866473095));
#100724=CARTESIAN_POINT('Ctrl Pts',(0.00467802272200933,-0.0321934096636183,
0.0693415194489414));
#100725=CARTESIAN_POINT('Ctrl Pts',(0.00474433541631017,-0.0320835708272304,
0.0692939997403734));
#100726=CARTESIAN_POINT('Ctrl Pts',(0.00481159306445234,-0.0319739230346346,
0.0692478799329295));
#100727=CARTESIAN_POINT('Ctrl Pts',(0.00487970508631167,-0.0318646057455575,
0.0692032124294917));
#100728=CARTESIAN_POINT('Ctrl Pts',(0.00466494988234139,-0.0321934096636183,
0.0694540817233843));
#100729=CARTESIAN_POINT('Ctrl Pts',(0.00472971025515197,-0.0320835708272304,
0.069406381730169));
#100730=CARTESIAN_POINT('Ctrl Pts',(0.00479542021319483,-0.0319739230346346,
0.0693600496174375));
#100731=CARTESIAN_POINT('Ctrl Pts',(0.00486199113566107,-0.0318646057455575,
0.0693151382116739));
#100732=CARTESIAN_POINT('Ctrl Pts',(0.00465187704267346,-0.0321934096636183,
0.0695666439978272));
#100733=CARTESIAN_POINT('Ctrl Pts',(0.00471508509399377,-0.0320835708272304,
0.0695187637199645));
#100734=CARTESIAN_POINT('Ctrl Pts',(0.00477924736193731,-0.0319739230346346,
0.0694722193019455));
#100735=CARTESIAN_POINT('Ctrl Pts',(0.00484427718501048,-0.0318646057455575,
0.069427063993856));
#100736=CARTESIAN_POINT('Ctrl Pts',(0.00455331175857821,-0.0320218834582377,
0.0696419473520672));
#100737=CARTESIAN_POINT('Ctrl Pts',(0.00460022968849572,-0.0319391099350675,
0.0696047873864008));
#100738=CARTESIAN_POINT('Ctrl Pts',(0.00464769945010586,-0.0318564869454957,
0.0695683825650677));
#100739=CARTESIAN_POINT('Ctrl Pts',(0.00469568399252358,-0.0317740741446551,
0.0695327561762958));
#100740=CARTESIAN_POINT('Ctrl Pts',(0.0045042109475812,-0.0320218834582377,
0.0696351695643298));
#100741=CARTESIAN_POINT('Ctrl Pts',(0.00455119941788386,-0.0319391099350675,
0.0695974985779213));
#100742=CARTESIAN_POINT('Ctrl Pts',(0.00459874765680106,-0.0318564869454957,
0.0695605841469588));
#100743=CARTESIAN_POINT('Ctrl Pts',(0.00464681852163494,-0.0317740741446551,
0.0695244499255165));
#100744=CARTESIAN_POINT('Ctrl Pts',(0.00445511013658419,-0.0320218834582377,
0.0696283917765924));
#100745=CARTESIAN_POINT('Ctrl Pts',(0.004502169147272,-0.0319391099350675,
0.0695902097694419));
#100746=CARTESIAN_POINT('Ctrl Pts',(0.00454979586349626,-0.0318564869454957,
0.0695527857288498));
#100747=CARTESIAN_POINT('Ctrl Pts',(0.00459795305074629,-0.0317740741446551,
0.0695161436747372));
#100748=CARTESIAN_POINT('Ctrl Pts',(0.00440600932558717,-0.0320218834582377,
0.069621613988855));
#100749=CARTESIAN_POINT('Ctrl Pts',(0.00445313887666013,-0.0319391099350675,
0.0695829209609625));
#100750=CARTESIAN_POINT('Ctrl Pts',(0.00450084407019146,-0.0318564869454957,
0.0695449873107408));
#100751=CARTESIAN_POINT('Ctrl Pts',(0.00454908757985765,-0.0317740741446551,
0.0695078374239579));
#100752=CARTESIAN_POINT('Origin',(-9.06906787348535E-5,-0.0391228853390656,
0.0652954501092941));
#100753=CARTESIAN_POINT('Ctrl Pts',(0.00275458514362636,-0.0352722978779612,
0.0720870197319338));
#100754=CARTESIAN_POINT('Ctrl Pts',(0.00276168840973056,-0.0352466642097229,
0.0720695086985918));
#100755=CARTESIAN_POINT('Ctrl Pts',(0.00276871269642917,-0.0352210183808307,
0.0720519837949522));
#100756=CARTESIAN_POINT('Ctrl Pts',(0.00277565775730809,-0.0351953608940152,
0.0720344442044586));
#100757=CARTESIAN_POINT('Origin',(-0.00171483525212223,-0.03524560030651,
0.0700785316137319));
#100758=CARTESIAN_POINT('Ctrl Pts',(0.00282411757248214,-0.035024121149334,
0.0719195661746556));
#100759=CARTESIAN_POINT('Ctrl Pts',(0.00285484088252747,-0.0349144232867422,
0.0718465654707452));
#100760=CARTESIAN_POINT('Ctrl Pts',(0.00288709155859916,-0.0348045283677512,
0.0717741561451404));
#100761=CARTESIAN_POINT('Ctrl Pts',(0.00292083174301926,-0.0346945769586886,
0.0717024324821825));
#100762=CARTESIAN_POINT('Ctrl Pts',(0.00271828587811248,-0.035024121149334,
0.0719600728934794));
#100763=CARTESIAN_POINT('Ctrl Pts',(0.00274845122473957,-0.0349144232867422,
0.0718856144014375));
#100764=CARTESIAN_POINT('Ctrl Pts',(0.00278017373694604,-0.0348045283677512,
0.0718117348816427));
#100765=CARTESIAN_POINT('Ctrl Pts',(0.00281341630364038,-0.0346945769586886,
0.0717385304763935));
#100766=CARTESIAN_POINT('Ctrl Pts',(0.00261245418374283,-0.035024121149334,
0.0720005796123032));
#100767=CARTESIAN_POINT('Ctrl Pts',(0.00264206156695168,-0.0349144232867422,
0.0719246633321297));
#100768=CARTESIAN_POINT('Ctrl Pts',(0.00267325591529292,-0.0348045283677512,
0.0718493136181449));
#100769=CARTESIAN_POINT('Ctrl Pts',(0.00270600086426149,-0.0346945769586886,
0.0717746284706046));
#100770=CARTESIAN_POINT('Ctrl Pts',(0.00250662248937317,-0.035024121149334,
0.072041086331127));
#100771=CARTESIAN_POINT('Ctrl Pts',(0.00253567190916378,-0.0349144232867422,
0.071963712262822));
#100772=CARTESIAN_POINT('Ctrl Pts',(0.00256633809363979,-0.0348045283677512,
0.0718868923546472));
#100773=CARTESIAN_POINT('Ctrl Pts',(0.0025985854248826,-0.0346945769586886,
0.0718107264648157));
#100774=CARTESIAN_POINT('Origin',(0.0180350902565986,-0.0345629067939025,
0.0790114774712389));
#100775=CARTESIAN_POINT('Ctrl Pts',(0.00277932995921813,-0.0351970973651641,
0.071578550584425));
#100776=CARTESIAN_POINT('Ctrl Pts',(0.00281495390594009,-0.0350869349321797,
0.0715045104417393));
#100777=CARTESIAN_POINT('Ctrl Pts',(0.00285214661666063,-0.0349764985129746,
0.0714311495671717));
#100778=CARTESIAN_POINT('Ctrl Pts',(0.00289086550180983,-0.0348659306849665,
0.0713585658382966));
#100779=CARTESIAN_POINT('Ctrl Pts',(0.00281038292084524,-0.0351970973651641,
0.0716546832595667));
#100780=CARTESIAN_POINT('Ctrl Pts',(0.00284495215253115,-0.0350869349321797,
0.0715810733135801));
#100781=CARTESIAN_POINT('Ctrl Pts',(0.002881080330951,-0.0349764985129746,
0.0715081210651405));
#100782=CARTESIAN_POINT('Ctrl Pts',(0.00291872621450492,-0.0348659306849665,
0.0714359237812513));
#100783=CARTESIAN_POINT('Ctrl Pts',(0.00284143588247235,-0.0351970973651641,
0.0717308159347085));
#100784=CARTESIAN_POINT('Ctrl Pts',(0.00287495039912221,-0.0350869349321797,
0.071657636185421));
#100785=CARTESIAN_POINT('Ctrl Pts',(0.00291001404524137,-0.0349764985129746,
0.0715850925631094));
#100786=CARTESIAN_POINT('Ctrl Pts',(0.00294658692720001,-0.0348659306849664,
0.0715132817242059));
#100787=CARTESIAN_POINT('Ctrl Pts',(0.00287248884409946,-0.0351970973651641,
0.0718069486098502));
#100788=CARTESIAN_POINT('Ctrl Pts',(0.00290494864571327,-0.0350869349321797,
0.0717341990572619));
#100789=CARTESIAN_POINT('Ctrl Pts',(0.00293894775953174,-0.0349764985129746,
0.0716620640610782));
#100790=CARTESIAN_POINT('Ctrl Pts',(0.0029744476398951,-0.0348659306849664,
0.0715906396671606));
#100791=CARTESIAN_POINT('Origin',(0.0177834121327603,-0.0345637187967461,
0.0794213353461847));
#100792=CARTESIAN_POINT('Ctrl Pts',(0.00285789485476266,-0.0352450361861253,
0.0718373055671251));
#100793=CARTESIAN_POINT('Ctrl Pts',(0.00294511955434506,-0.0349452761023765,
0.0716386993722933));
#100794=CARTESIAN_POINT('Ctrl Pts',(0.00304705628859159,-0.0346444289983475,
0.0714472275178238));
#100795=CARTESIAN_POINT('Ctrl Pts',(0.00276236527840564,-0.0352450361861253,
0.0720683339204522));
#100796=CARTESIAN_POINT('Ctrl Pts',(0.00284087660088663,-0.0349452761023765,
0.0718661247686191));
#100797=CARTESIAN_POINT('Ctrl Pts',(0.00293439610127408,-0.0346444289983475,
0.0716704038655705));
#100798=CARTESIAN_POINT('Ctrl Pts',(0.00297462486737071,-0.0345231616327822,
0.0715911995783497));
#100799=CARTESIAN_POINT('Ctrl Pts',(0.0030098943286801,-0.0344132092796975,
0.0715202256940485));
#100800=CARTESIAN_POINT('Ctrl Pts',(0.00304663000906076,-0.0343032738558974,
0.0714499849926605));
#100801=CARTESIAN_POINT('Ctrl Pts',(0.00308478254082378,-0.0341934961088741,
0.0713805662551144));
#100802=CARTESIAN_POINT('Ctrl Pts',(0.00286645859902239,-0.0345231616327822,
0.0716249811492146));
#100803=CARTESIAN_POINT('Ctrl Pts',(0.00290126242893806,-0.0344132092796975,
0.0715525163451901));
#100804=CARTESIAN_POINT('Ctrl Pts',(0.00293756334044789,-0.0343032738558974,
0.0714807751697854));
#100805=CARTESIAN_POINT('Ctrl Pts',(0.00297531247361221,-0.0341934961088741,
0.0714098483404771));
#100806=CARTESIAN_POINT('Ctrl Pts',(0.00275829233067407,-0.0345231616327822,
0.0716587627200794));
#100807=CARTESIAN_POINT('Ctrl Pts',(0.00279263052919602,-0.0344132092796975,
0.0715848069963317));
#100808=CARTESIAN_POINT('Ctrl Pts',(0.00282849667183502,-0.0343032738558974,
0.0715115653469102));
#100809=CARTESIAN_POINT('Ctrl Pts',(0.00286584240640064,-0.0341934961088741,
0.0714391304258398));
#100810=CARTESIAN_POINT('Ctrl Pts',(0.00265012606232575,-0.0345231616327822,
0.0716925442909443));
#100811=CARTESIAN_POINT('Ctrl Pts',(0.00268399862945398,-0.0344132092796975,
0.0716170976474733));
#100812=CARTESIAN_POINT('Ctrl Pts',(0.00271943000322216,-0.0343032738558974,
0.0715423555240351));
#100813=CARTESIAN_POINT('Ctrl Pts',(0.00275637233918907,-0.0341934961088741,
0.0714684125112026));
#100814=CARTESIAN_POINT('Origin',(0.0180460650678999,-0.0345625596232997,
0.0790165815698863));
#100815=CARTESIAN_POINT('Ctrl Pts',(0.00292251633834766,-0.0346945769586886,
0.0711588742072382));
#100816=CARTESIAN_POINT('Ctrl Pts',(0.00296373556363058,-0.0345846629176052,
0.07108719813479));
#100817=CARTESIAN_POINT('Ctrl Pts',(0.00300644406100104,-0.0344746925050311,
0.0710163622165435));
#100818=CARTESIAN_POINT('Ctrl Pts',(0.00305058673257186,-0.0343648066253259,
0.0709464569896416));
#100819=CARTESIAN_POINT('Ctrl Pts',(0.00295861430413636,-0.0346945769586886,
0.0712662895620416));
#100820=CARTESIAN_POINT('Ctrl Pts',(0.00299835329153721,-0.0345846629176052,
0.0711951109378076));
#100821=CARTESIAN_POINT('Ctrl Pts',(0.00303957101117255,-0.0344746925050311,
0.0711247419420293));
#100822=CARTESIAN_POINT('Ctrl Pts',(0.00308221427778222,-0.0343648066253259,
0.0710552725214632));
#100823=CARTESIAN_POINT('Ctrl Pts',(0.00299471226992506,-0.0346945769586886,
0.0713737049168451));
#100824=CARTESIAN_POINT('Ctrl Pts',(0.00303297101944384,-0.0345846629176052,
0.0713030237408253));
#100825=CARTESIAN_POINT('Ctrl Pts',(0.00307269796134406,-0.0344746925050311,
0.071233121667515));
#100826=CARTESIAN_POINT('Ctrl Pts',(0.00311384182299258,-0.0343648066253259,
0.0711640880532847));
#100827=CARTESIAN_POINT('Ctrl Pts',(0.00303081023571377,-0.0346945769586886,
0.0714811202716486));
#100828=CARTESIAN_POINT('Ctrl Pts',(0.00306758874735047,-0.0345846629176052,
0.071410936543843));
#100829=CARTESIAN_POINT('Ctrl Pts',(0.00310582491151557,-0.0344746925050311,
0.0713415013930008));
#100830=CARTESIAN_POINT('Ctrl Pts',(0.00314546936820293,-0.0343648066253259,
0.0712729035851062));
#100831=CARTESIAN_POINT('Origin',(0.0178350709883733,-0.0345626446729731,
0.0794486390679691));
#100832=CARTESIAN_POINT('Ctrl Pts',(0.00303016432206027,-0.0346945769586886,
0.0714791982507607));
#100833=CARTESIAN_POINT('Ctrl Pts',(0.00308610533402788,-0.0345275153362891,
0.0713725103850799));
#100834=CARTESIAN_POINT('Ctrl Pts',(0.00314541605038269,-0.0343603235965159,
0.0712675542177887));
#100835=CARTESIAN_POINT('Ctrl Pts',(0.003207916442797,-0.034193496108874,
0.0711646375555192));
#100836=CARTESIAN_POINT('Ctrl Pts',(0.0029928568596655,-0.0346945769586886,
0.0715542727576251));
#100837=CARTESIAN_POINT('Ctrl Pts',(0.00304722540602866,-0.0345275153362891,
0.0714468034722074));
#100838=CARTESIAN_POINT('Ctrl Pts',(0.00310498782499035,-0.0343603235965159,
0.0713410162304682));
#100839=CARTESIAN_POINT('Ctrl Pts',(0.00316596863086776,-0.034193496108874,
0.0712372213650474));
#100840=CARTESIAN_POINT('Ctrl Pts',(0.00295554939727072,-0.0346945769586886,
0.0716293472644895));
#100841=CARTESIAN_POINT('Ctrl Pts',(0.00300834547802944,-0.0345275153362891,
0.0715210965593349));
#100842=CARTESIAN_POINT('Ctrl Pts',(0.00306455959959802,-0.0343603235965159,
0.0714144782431476));
#100843=CARTESIAN_POINT('Ctrl Pts',(0.00312402081893851,-0.034193496108874,
0.0713098051745756));
#100844=CARTESIAN_POINT('Ctrl Pts',(0.00291824193487594,-0.0346945769586886,
0.071704421771354));
#100845=CARTESIAN_POINT('Ctrl Pts',(0.00296946555003022,-0.0345275153362891,
0.0715953896464624));
#100846=CARTESIAN_POINT('Ctrl Pts',(0.00302413137420568,-0.0343603235965159,
0.0714879402558271));
#100847=CARTESIAN_POINT('Ctrl Pts',(0.00308207300700927,-0.034193496108874,
0.0713823889841038));
#100848=CARTESIAN_POINT('Ctrl Pts',(0.00314545406140031,-0.0340223579322365,
0.0712729311837875));
#100849=CARTESIAN_POINT('Ctrl Pts',(0.00318513634408598,-0.0339125849573554,
0.071204267054827));
#100850=CARTESIAN_POINT('Ctrl Pts',(0.00322621193040712,-0.0338030433565221,
0.0711364725063977));
#100851=CARTESIAN_POINT('Ctrl Pts',(0.00326862060621732,-0.0336938721132328,
0.0710696295798466));
#100852=CARTESIAN_POINT('Ctrl Pts',(0.0030353798891439,-0.0340223579322365,
0.0712998543417083));
#100853=CARTESIAN_POINT('Ctrl Pts',(0.00307469083126329,-0.0339125849573554,
0.071229672002827));
#100854=CARTESIAN_POINT('Ctrl Pts',(0.00311542676137242,-0.0338030433565221,
0.0711603526254184));
#100855=CARTESIAN_POINT('Ctrl Pts',(0.00315752772682866,-0.0336938721132328,
0.0710919802393335));
#100856=CARTESIAN_POINT('Ctrl Pts',(0.00292530571688748,-0.0340223579322365,
0.0713267774996291));
#100857=CARTESIAN_POINT('Ctrl Pts',(0.00296424531844061,-0.0339125849573554,
0.0712550769508269));
#100858=CARTESIAN_POINT('Ctrl Pts',(0.00300464159233771,-0.0338030433565221,
0.0711842327444392));
#100859=CARTESIAN_POINT('Ctrl Pts',(0.00304643484743999,-0.0336938721132328,
0.0711143308988204));
#100860=CARTESIAN_POINT('Ctrl Pts',(0.00281523154463107,-0.0340223579322365,
0.0713537006575499));
#100861=CARTESIAN_POINT('Ctrl Pts',(0.00285379980561793,-0.0339125849573554,
0.0712804818988268));
#100862=CARTESIAN_POINT('Ctrl Pts',(0.00289385642330301,-0.0338030433565221,
0.0712081128634599));
#100863=CARTESIAN_POINT('Ctrl Pts',(0.00293534196805132,-0.0336938721132328,
0.0711366815583073));
#100864=CARTESIAN_POINT('Origin',(0.0179392954629266,-0.0345589643417464,
0.078961326438295));
#100865=CARTESIAN_POINT('Ctrl Pts',(0.00312059419090093,-0.034193496108874,
0.0708381863255022));
#100866=CARTESIAN_POINT('Ctrl Pts',(0.00316626214029408,-0.0340836138581107,
0.070769195325722));
#100867=CARTESIAN_POINT('Ctrl Pts',(0.00321333580132424,-0.0339738896643499,
0.0707011824315089));
#100868=CARTESIAN_POINT('Ctrl Pts',(0.00326174909025732,-0.0338644633294062,
0.070634230652218));
#100869=CARTESIAN_POINT('Ctrl Pts',(0.00314987630261111,-0.034193496108874,
0.0709476564912127));
#100870=CARTESIAN_POINT('Ctrl Pts',(0.00319403472324476,-0.0340836138581107,
0.0708790692744129));
#100871=CARTESIAN_POINT('Ctrl Pts',(0.00323959122437419,-0.0339738896643499,
0.0708114287329071));
#100872=CARTESIAN_POINT('Ctrl Pts',(0.00328648169598912,-0.0338644633294062,
0.070744817529652));
#100873=CARTESIAN_POINT('Ctrl Pts',(0.00317915841432129,-0.034193496108874,
0.0710571266569233));
#100874=CARTESIAN_POINT('Ctrl Pts',(0.00322180730619545,-0.0340836138581107,
0.0709889432231037));
#100875=CARTESIAN_POINT('Ctrl Pts',(0.00326584664742414,-0.0339738896643499,
0.0709216750343054));
#100876=CARTESIAN_POINT('Ctrl Pts',(0.00331121430172092,-0.0338644633294062,
0.0708554044070861));
#100877=CARTESIAN_POINT('Ctrl Pts',(0.00320844052603147,-0.034193496108874,
0.0711665968226338));
#100878=CARTESIAN_POINT('Ctrl Pts',(0.00324957988914614,-0.0340836138581107,
0.0710988171717946));
#100879=CARTESIAN_POINT('Ctrl Pts',(0.00329210207047409,-0.0339738896643499,
0.0710319213357036));
#100880=CARTESIAN_POINT('Ctrl Pts',(0.00333594690745272,-0.0338644633294062,
0.0709659912845202));
#100881=CARTESIAN_POINT('Origin',(0.0177695446677903,-0.0345610621860672,
0.0794115871179137));
#100882=CARTESIAN_POINT('Ctrl Pts',(0.00318923509526838,-0.0342436276873901,
0.0711956185183359));
#100883=CARTESIAN_POINT('Ctrl Pts',(0.00330066142973354,-0.0339430054201861,
0.0710095090064905));
#100884=CARTESIAN_POINT('Ctrl Pts',(0.00342578974465575,-0.0336441434784162,
0.0708323213003242));
#100885=CARTESIAN_POINT('Ctrl Pts',(0.0030655062326716,-0.0342436276873901,
0.0714128538022115));
#100886=CARTESIAN_POINT('Ctrl Pts',(0.00316873940333953,-0.0339430054201861,
0.0712220777793848));
#100887=CARTESIAN_POINT('Ctrl Pts',(0.00328604933111146,-0.0336441434784162,
0.0710396196766382));
#100888=CARTESIAN_POINT('Ctrl Pts',(0.00333593165678936,-0.0335235895815127,
0.0709660144458022));
#100889=CARTESIAN_POINT('Ctrl Pts',(0.00337976548663298,-0.0334144449262719,
0.0709001002567604));
#100890=CARTESIAN_POINT('Ctrl Pts',(0.0034250114137761,-0.0333049234473133,
0.070835015914237));
#100891=CARTESIAN_POINT('Ctrl Pts',(0.00347161912125876,-0.0331951640388588,
0.0707708498819393));
#100892=CARTESIAN_POINT('Ctrl Pts',(0.00322438419449067,-0.0335235895815127,
0.0709859728059811));
#100893=CARTESIAN_POINT('Ctrl Pts',(0.00326794325821204,-0.0334144449262719,
0.0709185229465041));
#100894=CARTESIAN_POINT('Ctrl Pts',(0.0033129458293554,-0.0333049234473133,
0.0708518954927849));
#100895=CARTESIAN_POINT('Ctrl Pts',(0.00335934208087624,-0.0331951640388588,
0.0707861808535084));
#100896=CARTESIAN_POINT('Ctrl Pts',(0.00311283673219199,-0.0335235895815127,
0.0710059311661601));
#100897=CARTESIAN_POINT('Ctrl Pts',(0.0031561210297911,-0.0334144449262719,
0.0709369456362478));
#100898=CARTESIAN_POINT('Ctrl Pts',(0.00320088024493469,-0.0333049234473133,
0.0708687750713328));
#100899=CARTESIAN_POINT('Ctrl Pts',(0.00324706504049372,-0.0331951640388588,
0.0708015118250775));
#100900=CARTESIAN_POINT('Ctrl Pts',(0.00300128926989331,-0.0335235895815127,
0.0710258895263391));
#100901=CARTESIAN_POINT('Ctrl Pts',(0.00304429880137016,-0.0334144449262719,
0.0709553683259915));
#100902=CARTESIAN_POINT('Ctrl Pts',(0.00308881466051398,-0.0333049234473133,
0.0708856546498806));
#100903=CARTESIAN_POINT('Ctrl Pts',(0.00313478800011121,-0.0331951640388588,
0.0708168427966466));
#100904=CARTESIAN_POINT('Origin',(0.0164953312605408,-0.0326434571770201,
0.0811715115522585));
#100905=CARTESIAN_POINT('Ctrl Pts',(0.00333801742936333,-0.0336938721132373,
0.0705285809189424));
#100906=CARTESIAN_POINT('Ctrl Pts',(0.00335921479695864,-0.033647456976495,
0.0705005682496956));
#100907=CARTESIAN_POINT('Ctrl Pts',(0.00338073863575899,-0.033601104548885,
0.0704728056418462));
#100908=CARTESIAN_POINT('Ctrl Pts',(0.00343523204461644,-0.033483750864316,
0.070402517104819));
#100909=CARTESIAN_POINT('Ctrl Pts',(0.0034917843189816,-0.0333660264760404,
0.0703338741859529));
#100910=CARTESIAN_POINT('Ctrl Pts',(0.00340506923980288,-0.0336938721132373,
0.0708618587219665));
#100911=CARTESIAN_POINT('Ctrl Pts',(0.00342431582182383,-0.033647456976495,
0.0708342385292164));
#100912=CARTESIAN_POINT('Ctrl Pts',(0.00344388441428595,-0.033601104548885,
0.0708068455345627));
#100913=CARTESIAN_POINT('Ctrl Pts',(0.00349342758916729,-0.033483750864316,
0.0707374927731274));
#100914=CARTESIAN_POINT('Ctrl Pts',(0.00354500407436432,-0.0333660264760404,
0.0706696385332396));
#100915=CARTESIAN_POINT('Ctrl Pts',(0.0034050692398148,-0.0336938721132427,
0.0708618587219738));
#100916=CARTESIAN_POINT('Ctrl Pts',(0.0034243158218348,-0.0336474569765026,
0.070834238529225));
#100917=CARTESIAN_POINT('Ctrl Pts',(0.00344388441429596,-0.0336011045488949,
0.0708068455345727));
#100918=CARTESIAN_POINT('Ctrl Pts',(0.00349301496201041,-0.0334847282606778,
0.0707380703871787));
#100919=CARTESIAN_POINT('Ctrl Pts',(0.00354414527714575,-0.0333679869945434,
0.0706707686599204));
#100920=CARTESIAN_POINT('Ctrl Pts',(0.00340506923980075,-0.0336938721132425,
0.0708618587219697));
#100921=CARTESIAN_POINT('Ctrl Pts',(0.00347390353456838,-0.0335278710435082,
0.0707630766895424));
#100922=CARTESIAN_POINT('Ctrl Pts',(0.00354581139244494,-0.0333620469224319,
0.0706664880339919));
#100923=CARTESIAN_POINT('Ctrl Pts',(0.00362084464106375,-0.0331951640388601,
0.0705720566798247));
#100924=CARTESIAN_POINT('Ctrl Pts',(0.00335864662225908,-0.0336938721132425,
0.0709316653864356));
#100925=CARTESIAN_POINT('Ctrl Pts',(0.00342601957698312,-0.0335278710435082,
0.0708319115380583));
#100926=CARTESIAN_POINT('Ctrl Pts',(0.00349649708480763,-0.0333620469224319,
0.0707343055811966));
#100927=CARTESIAN_POINT('Ctrl Pts',(0.00357013043122506,-0.0331951640388601,
0.0706388106965107));
#100928=CARTESIAN_POINT('Ctrl Pts',(0.00331222400471741,-0.0336938721132425,
0.0710014720509014));
#100929=CARTESIAN_POINT('Ctrl Pts',(0.00337813561939785,-0.0335278710435082,
0.0709007463865742));
#100930=CARTESIAN_POINT('Ctrl Pts',(0.00344718277717032,-0.0333620469224319,
0.0708021231284014));
#100931=CARTESIAN_POINT('Ctrl Pts',(0.00351941622138638,-0.0331951640388601,
0.0707055647131967));
#100932=CARTESIAN_POINT('Ctrl Pts',(0.00326580138717574,-0.0336938721132425,
0.0710712787153673));
#100933=CARTESIAN_POINT('Ctrl Pts',(0.00333025166181258,-0.0335278710435082,
0.0709695812350901));
#100934=CARTESIAN_POINT('Ctrl Pts',(0.00339786846953301,-0.0333620469224319,
0.0708699406756061));
#100935=CARTESIAN_POINT('Ctrl Pts',(0.00346870201154769,-0.0331951640388601,
0.0707723187298827));
#100936=CARTESIAN_POINT('Ctrl Pts',(0.0035453024560874,-0.0330240426238156,
0.0706716664798157));
#100937=CARTESIAN_POINT('Ctrl Pts',(0.00359321988910383,-0.0329142774063509,
0.0706085934608418));
#100938=CARTESIAN_POINT('Ctrl Pts',(0.00364246510619618,-0.0328043479726686,
0.070546479584859));
#100939=CARTESIAN_POINT('Ctrl Pts',(0.00369297721198627,-0.0326943950436594,
0.0704854061617673));
#100940=CARTESIAN_POINT('Ctrl Pts',(0.0034327220734972,-0.0330240426238156,
0.0706845813332973));
#100941=CARTESIAN_POINT('Ctrl Pts',(0.00348046159182459,-0.0329142774063509,
0.0706199574098715));
#100942=CARTESIAN_POINT('Ctrl Pts',(0.0035295608670582,-0.0328043479726686,
0.0705562881782607));
#100943=CARTESIAN_POINT('Ctrl Pts',(0.00357995924565606,-0.0326943950436594,
0.0704936569357425));
#100944=CARTESIAN_POINT('Ctrl Pts',(0.003320141690907,-0.0330240426238156,
0.0706974961867789));
#100945=CARTESIAN_POINT('Ctrl Pts',(0.00336770329454535,-0.0329142774063509,
0.0706313213589012));
#100946=CARTESIAN_POINT('Ctrl Pts',(0.00341665662792022,-0.0328043479726686,
0.0705660967716625));
#100947=CARTESIAN_POINT('Ctrl Pts',(0.00346694127932585,-0.0326943950436594,
0.0705019077097177));
#100948=CARTESIAN_POINT('Ctrl Pts',(0.0032075613083168,-0.0330240426238156,
0.0707104110402606));
#100949=CARTESIAN_POINT('Ctrl Pts',(0.00325494499726611,-0.0329142774063509,
0.0706426853079309));
#100950=CARTESIAN_POINT('Ctrl Pts',(0.00330375238878223,-0.0328043479726686,
0.0705759053650642));
#100951=CARTESIAN_POINT('Ctrl Pts',(0.00335392331299563,-0.0326943950436594,
0.070510158483693));
#100952=CARTESIAN_POINT('Origin',(0.0165918406917995,-0.0326396682856393,
0.0812488506009495));
#100953=CARTESIAN_POINT('Ctrl Pts',(0.00357512613946548,-0.0331951640388587,
0.0702372352350697));
#100954=CARTESIAN_POINT('Ctrl Pts',(0.00362901655864372,-0.0330855618255041,
0.070174586699787));
#100955=CARTESIAN_POINT('Ctrl Pts',(0.00368424066480755,-0.0329757224427708,
0.0701130068248977));
#100956=CARTESIAN_POINT('Ctrl Pts',(0.00374073160826077,-0.0328657862078596,
0.0700525779359834));
#100957=CARTESIAN_POINT('Ctrl Pts',(0.00359045709882897,-0.0331951640388587,
0.070349512186064));
#100958=CARTESIAN_POINT('Ctrl Pts',(0.00364280113014169,-0.0330855618255041,
0.0702870748037323));
#100959=CARTESIAN_POINT('Ctrl Pts',(0.00369647336950004,-0.0329757224427708,
0.0702256742728173));
#100960=CARTESIAN_POINT('Ctrl Pts',(0.0037514089432011,-0.0328657862078596,
0.0701653925917607));
#100961=CARTESIAN_POINT('Ctrl Pts',(0.00360578805819247,-0.0331951640388587,
0.0704617891370583));
#100962=CARTESIAN_POINT('Ctrl Pts',(0.00365658570163966,-0.0330855618255041,
0.0703995629076776));
#100963=CARTESIAN_POINT('Ctrl Pts',(0.00370870607419253,-0.0329757224427708,
0.0703383417207369));
#100964=CARTESIAN_POINT('Ctrl Pts',(0.00376208627814143,-0.0328657862078596,
0.0702782072475381));
#100965=CARTESIAN_POINT('Ctrl Pts',(0.00362111901755597,-0.0331951640388587,
0.0705740660880526));
#100966=CARTESIAN_POINT('Ctrl Pts',(0.00367037027313763,-0.0330855618255041,
0.0705120510116229));
#100967=CARTESIAN_POINT('Ctrl Pts',(0.00372093877888502,-0.0329757224427708,
0.0704510091686565));
#100968=CARTESIAN_POINT('Ctrl Pts',(0.00377276361308176,-0.0328657862078596,
0.0703910219033155));
#100969=CARTESIAN_POINT('Origin',(0.016254341606255,-0.032640190883445,
0.0815914396239748));
#100970=CARTESIAN_POINT('Ctrl Pts',(0.00359847238323193,-0.0332451089994432,
0.0706003949339911));
#100971=CARTESIAN_POINT('Ctrl Pts',(0.00373234792861486,-0.0329451141710257,
0.070429720082125));
#100972=CARTESIAN_POINT('Ctrl Pts',(0.00387869907526945,-0.0326442513127503,
0.0702696141528658));
#100973=CARTESIAN_POINT('Ctrl Pts',(0.00344848983885165,-0.0332451089994432,
0.0708004080245157));
#100974=CARTESIAN_POINT('Ctrl Pts',(0.00357482176710542,-0.0329451141710257,
0.0706240764884401));
#100975=CARTESIAN_POINT('Ctrl Pts',(0.00371407681183032,-0.0326442513127503,
0.0704577617289336));
#100976=CARTESIAN_POINT('Ctrl Pts',(0.00377274289495567,-0.0325229783203385,
0.0703910457473858));
#100977=CARTESIAN_POINT('Ctrl Pts',(0.00382455999618189,-0.032413025311208,
0.0703310667669035));
#100978=CARTESIAN_POINT('Ctrl Pts',(0.0038776099805667,-0.0323031222247695,
0.0702721687866917));
#100979=CARTESIAN_POINT('Ctrl Pts',(0.00393182223267944,-0.0321934096636184,
0.0702144248530265));
#100980=CARTESIAN_POINT('Ctrl Pts',(0.00365957370523785,-0.0325229783203385,
0.0703968661552763));
#100981=CARTESIAN_POINT('Ctrl Pts',(0.00371131057227004,-0.032413025311208,
0.070335327140017));
#100982=CARTESIAN_POINT('Ctrl Pts',(0.00376431260595269,-0.0323031222247695,
0.0702748677018907));
#100983=CARTESIAN_POINT('Ctrl Pts',(0.00381850918169905,-0.0321934096636184,
0.0702155628894573));
#100984=CARTESIAN_POINT('Ctrl Pts',(0.00354640451552002,-0.0325229783203385,
0.0704026865631669));
#100985=CARTESIAN_POINT('Ctrl Pts',(0.00359806114835818,-0.032413025311208,
0.0703395875131305));
#100986=CARTESIAN_POINT('Ctrl Pts',(0.00365101523133868,-0.0323031222247695,
0.0702775666170897));
#100987=CARTESIAN_POINT('Ctrl Pts',(0.00370519613071867,-0.0321934096636184,
0.0702167009258881));
#100988=CARTESIAN_POINT('Ctrl Pts',(0.00343323532580219,-0.0325229783203385,
0.0704085069710574));
#100989=CARTESIAN_POINT('Ctrl Pts',(0.00348481172444633,-0.032413025311208,
0.070343847886244));
#100990=CARTESIAN_POINT('Ctrl Pts',(0.00353771785672467,-0.0323031222247695,
0.0702802655322886));
#100991=CARTESIAN_POINT('Ctrl Pts',(0.00359188307973828,-0.0321934096636184,
0.070217838962319));
#100992=CARTESIAN_POINT('Origin',(0.0165854626521562,-0.0326393375177015,
0.0812431927181626));
#100993=CARTESIAN_POINT('Ctrl Pts',(0.00382978640553164,-0.0326943950436593,
0.0699593437057789));
#100994=CARTESIAN_POINT('Ctrl Pts',(0.0038875415033928,-0.0325844576448127,
0.0699001643960204));
#100995=CARTESIAN_POINT('Ctrl Pts',(0.00394652461382358,-0.0324744968375319,
0.0698421753681648));
#100996=CARTESIAN_POINT('Ctrl Pts',(0.00400665913941762,-0.0323646534831894,
0.069785449878763));
#100997=CARTESIAN_POINT('Ctrl Pts',(0.0038380371768073,-0.0326943950436593,
0.0700723616351306));
#100998=CARTESIAN_POINT('Ctrl Pts',(0.00389423467578382,-0.0325844576448127,
0.0700132960364639));
#100999=CARTESIAN_POINT('Ctrl Pts',(0.00395165772536446,-0.0324744968375319,
0.0699553885140489));
#101000=CARTESIAN_POINT('Ctrl Pts',(0.00401023172842419,-0.0323646534831894,
0.0698987122475771));
#101001=CARTESIAN_POINT('Ctrl Pts',(0.00384628794808296,-0.0326943950436593,
0.0701853795644822));
#101002=CARTESIAN_POINT('Ctrl Pts',(0.00390092784817484,-0.0325844576448127,
0.0701264276769074));
#101003=CARTESIAN_POINT('Ctrl Pts',(0.00395679083690534,-0.0324744968375319,
0.070068601659933));
#101004=CARTESIAN_POINT('Ctrl Pts',(0.00401380431743077,-0.0323646534831894,
0.0700119746163912));
#101005=CARTESIAN_POINT('Ctrl Pts',(0.00385453871935861,-0.0326943950436593,
0.0702983974938339));
#101006=CARTESIAN_POINT('Ctrl Pts',(0.00390762102056586,-0.0325844576448127,
0.0702395593173508));
#101007=CARTESIAN_POINT('Ctrl Pts',(0.00396192394844622,-0.0324744968375319,
0.0701818148058171));
#101008=CARTESIAN_POINT('Ctrl Pts',(0.00401737690643735,-0.0323646534831894,
0.0701252369852052));
#101009=CARTESIAN_POINT('Origin',(0.0162825633549792,-0.032639557906579,
0.0816166486439388));
#101010=CARTESIAN_POINT('Ctrl Pts',(0.00383025749695593,-0.0327445246961876,
0.0703232819958182));
#101011=CARTESIAN_POINT('Ctrl Pts',(0.00397458452440749,-0.0324436878365475,
0.0701613490663448));
#101012=CARTESIAN_POINT('Ctrl Pts',(0.00413069898397488,-0.0321434074463186,
0.0700107474726786));
#101013=CARTESIAN_POINT('Ctrl Pts',(0.00366801328014326,-0.0327445246961876,
0.070513484030799));
#101014=CARTESIAN_POINT('Ctrl Pts',(0.00380516672064799,-0.0324436878365475,
0.0703454319607179));
#101015=CARTESIAN_POINT('Ctrl Pts',(0.00395458889134602,-0.0321434074463186,
0.0701881882663937));
#101016=CARTESIAN_POINT('Ctrl Pts',(0.00408298943779383,-0.0322357242816072,
0.0700573090870923));
#101017=CARTESIAN_POINT('Ctrl Pts',(0.00421333633534426,-0.0319819883628705,
0.0699286150785516));
#101018=CARTESIAN_POINT('Ctrl Pts',(0.00435160823665694,-0.0317295851069887,
0.0698084762303691));
#101019=CARTESIAN_POINT('Ctrl Pts',(0.00390894787970366,-0.0322357242816072,
0.07023677924076));
#101020=CARTESIAN_POINT('Ctrl Pts',(0.00403357888562404,-0.0319819883628705,
0.0701025422343179));
#101021=CARTESIAN_POINT('Ctrl Pts',(0.00416649919608388,-0.0317295851069887,
0.0699765079032707));
#101022=CARTESIAN_POINT('Origin',(0.0162134206443787,-0.0326371942647745,
0.0815510613820758));
#101023=CARTESIAN_POINT('Origin',(0.0164933025329328,-0.0326352985527776,
0.0811621352362565));
#101024=CARTESIAN_POINT('Ctrl Pts',(0.00410139311123134,-0.0321934096636183,
0.0696979907823519));
#101025=CARTESIAN_POINT('Ctrl Pts',(0.0041627897880276,-0.0320835708272304,
0.0696425189020534));
#101026=CARTESIAN_POINT('Ctrl Pts',(0.00422529883993577,-0.0319739230346346,
0.0695883497987352));
#101027=CARTESIAN_POINT('Ctrl Pts',(0.00428883497194882,-0.0318646057455575,
0.0695355466400723));
#101028=CARTESIAN_POINT('Ctrl Pts',(0.00410253114864214,-0.0321934096636183,
0.0698113039309076));
#101029=CARTESIAN_POINT('Ctrl Pts',(0.00416236514880892,-0.0320835708272304,
0.069755847745032));
#101030=CARTESIAN_POINT('Ctrl Pts',(0.0042233121057083,-0.0319739230346346,
0.0697016619875215));
#101031=CARTESIAN_POINT('Ctrl Pts',(0.00428528872129011,-0.0318646057455575,
0.0696488100007457));
#101032=CARTESIAN_POINT('Ctrl Pts',(0.00410366918605294,-0.0321934096636184,
0.0699246170794633));
#101033=CARTESIAN_POINT('Ctrl Pts',(0.00416194050959024,-0.0320835708272304,
0.0698691765880105));
#101034=CARTESIAN_POINT('Ctrl Pts',(0.00422132537148083,-0.0319739230346346,
0.0698149741763078));
#101035=CARTESIAN_POINT('Ctrl Pts',(0.0042817424706314,-0.0318646057455575,
0.069762073361419));
#101036=CARTESIAN_POINT('Ctrl Pts',(0.00410480722346373,-0.0321934096636184,
0.0700379302280189));
#101037=CARTESIAN_POINT('Ctrl Pts',(0.00416151587037156,-0.0320835708272304,
0.0699825054309891));
#101038=CARTESIAN_POINT('Ctrl Pts',(0.00421933863725336,-0.0319739230346346,
0.0699282863650941));
#101039=CARTESIAN_POINT('Ctrl Pts',(0.00427819621997269,-0.0318646057455575,
0.0698753367220923));
#101040=CARTESIAN_POINT('Ctrl Pts',(0.00401645716895846,-0.0320218834582383,
0.070124993298592));
#101041=CARTESIAN_POINT('Ctrl Pts',(0.0040583477583289,-0.0319391099350678,
0.070082245974485));
#101042=CARTESIAN_POINT('Ctrl Pts',(0.00410088047271536,-0.0318564869454957,
0.0700401786773225));
#101043=CARTESIAN_POINT('Ctrl Pts',(0.00414402147217898,-0.0317740741446548,
0.0699988191554047));
#101044=CARTESIAN_POINT('Ctrl Pts',(0.00396689405046831,-0.0320218834582383,
0.0701244229191482));
#101045=CARTESIAN_POINT('Ctrl Pts',(0.00400879057610988,-0.0319391099350678,
0.0700811597627959));
#101046=CARTESIAN_POINT('Ctrl Pts',(0.00405133727796367,-0.0318564869454957,
0.0700385770386133));
#101047=CARTESIAN_POINT('Ctrl Pts',(0.00409450027085473,-0.0317740741446548,
0.0699967028693698));
#101048=CARTESIAN_POINT('Ctrl Pts',(0.00391733093197817,-0.0320218834582383,
0.0701238525397044));
#101049=CARTESIAN_POINT('Ctrl Pts',(0.00395923339389086,-0.0319391099350678,
0.0700800735511067));
#101050=CARTESIAN_POINT('Ctrl Pts',(0.00400179408321198,-0.0318564869454957,
0.0700369753999041));
#101051=CARTESIAN_POINT('Ctrl Pts',(0.00404497906953048,-0.0317740741446548,
0.069994586583335));
#101052=CARTESIAN_POINT('Ctrl Pts',(0.00386776781348802,-0.0320218834582383,
0.0701232821602607));
#101053=CARTESIAN_POINT('Ctrl Pts',(0.00390967621167184,-0.0319391099350678,
0.0700789873394175));
#101054=CARTESIAN_POINT('Ctrl Pts',(0.00395225088846029,-0.0318564869454957,
0.0700353737611948));
#101055=CARTESIAN_POINT('Ctrl Pts',(0.00399545786820623,-0.0317740741446548,
0.0699924702973002));
#101056=CARTESIAN_POINT('Origin',(-0.00113568647615043,-0.0391228853390614,
0.0663948173269696));
#101057=CARTESIAN_POINT('Ctrl Pts',(0.00253836287828677,-0.0352722978779618,
0.0727762257753859));
#101058=CARTESIAN_POINT('Ctrl Pts',(0.00254321541858433,-0.0352466642097233,
0.0727579625464622));
#101059=CARTESIAN_POINT('Ctrl Pts',(0.00254798786384325,-0.0352210183808309,
0.0727396954553567));
#101060=CARTESIAN_POINT('Ctrl Pts',(0.00255267986725082,-0.0351953608940152,
0.0727214237228355));
#101061=CARTESIAN_POINT('Origin',(-0.00214754511313579,-0.0352456003065105,
0.071343742096256));
#101062=CARTESIAN_POINT('Ctrl Pts',(0.00258635952736725,-0.035024121149334,
0.0726013779152761));
#101063=CARTESIAN_POINT('Ctrl Pts',(0.0026076911606627,-0.0349144232867421,
0.0725251021919265));
#101064=CARTESIAN_POINT('Ctrl Pts',(0.00263061223560249,-0.0348045283677512,
0.072449221753965));
#101065=CARTESIAN_POINT('Ctrl Pts',(0.00265509700998915,-0.0346945769586886,
0.072373834887098));
#101066=CARTESIAN_POINT('Ctrl Pts',(0.00248643918556934,-0.035024121149334,
0.0726548294549921));
#101067=CARTESIAN_POINT('Ctrl Pts',(0.00250703454585438,-0.0349144232867421,
0.0725771773699653));
#101068=CARTESIAN_POINT('Ctrl Pts',(0.00252924735746698,-0.0348045283677512,
0.0724999045272192));
#101069=CARTESIAN_POINT('Ctrl Pts',(0.00255305285177284,-0.0346945769586886,
0.0724231109621948));
#101070=CARTESIAN_POINT('Ctrl Pts',(0.00238651884377143,-0.035024121149334,
0.0727082809947082));
#101071=CARTESIAN_POINT('Ctrl Pts',(0.00240637793104606,-0.0349144232867421,
0.0726292525480041));
#101072=CARTESIAN_POINT('Ctrl Pts',(0.00242788247933147,-0.0348045283677512,
0.0725505873004734));
#101073=CARTESIAN_POINT('Ctrl Pts',(0.00245100869355653,-0.0346945769586886,
0.0724723870372917));
#101074=CARTESIAN_POINT('Ctrl Pts',(0.00228659850197351,-0.035024121149334,
0.0727617325344242));
#101075=CARTESIAN_POINT('Ctrl Pts',(0.00230572131623774,-0.0349144232867421,
0.0726813277260428));
#101076=CARTESIAN_POINT('Ctrl Pts',(0.00232651760119597,-0.0348045283677512,
0.0726012700737276));
#101077=CARTESIAN_POINT('Ctrl Pts',(0.00234896453534022,-0.0346945769586886,
0.0725216631123886));
#101078=CARTESIAN_POINT('Origin',(0.0185662413236461,-0.0345629067939343,
0.0777309269808658));
#101079=CARTESIAN_POINT('Ctrl Pts',(0.00249918449119187,-0.0351970973651637,
0.0722686647112246));
#101080=CARTESIAN_POINT('Ctrl Pts',(0.00252524784195756,-0.0350869349321779,
0.0721907435327427));
#101081=CARTESIAN_POINT('Ctrl Pts',(0.00255295272141885,-0.0349764985129713,
0.0721132996478823));
#101082=CARTESIAN_POINT('Ctrl Pts',(0.00258226914315024,-0.0348659306849617,
0.0720364355003123));
#101083=CARTESIAN_POINT('Ctrl Pts',(0.0025395345452969,-0.0351970973651637,
0.0723403050893907));
#101084=CARTESIAN_POINT('Ctrl Pts',(0.00256460541571298,-0.0350869349321779,
0.0722629429062244));
#101085=CARTESIAN_POINT('Ctrl Pts',(0.00259130537146266,-0.0349764985129713,
0.0721860378466283));
#101086=CARTESIAN_POINT('Ctrl Pts',(0.00261960568693649,-0.0348659306849617,
0.0721096915795697));
#101087=CARTESIAN_POINT('Ctrl Pts',(0.00257988459940193,-0.0351970973651637,
0.0724119454675567));
#101088=CARTESIAN_POINT('Ctrl Pts',(0.0026039629894684,-0.0350869349321779,
0.0723351422797061));
#101089=CARTESIAN_POINT('Ctrl Pts',(0.00262965802150647,-0.0349764985129713,
0.0722587760453744));
#101090=CARTESIAN_POINT('Ctrl Pts',(0.00265694223072274,-0.0348659306849617,
0.072182947658827));
#101091=CARTESIAN_POINT('Ctrl Pts',(0.00262023465350695,-0.0351970973651637,
0.0724835858457228));
#101092=CARTESIAN_POINT('Ctrl Pts',(0.00264332056322382,-0.0350869349321779,
0.0724073416531878));
#101093=CARTESIAN_POINT('Ctrl Pts',(0.00266801067155029,-0.0349764985129713,
0.0723315142441205));
#101094=CARTESIAN_POINT('Ctrl Pts',(0.00269427877450898,-0.0348659306849617,
0.0722562037380843));
#101095=CARTESIAN_POINT('Origin',(0.0183679165695076,-0.0345637187966988,
0.0781690966371691));
#101096=CARTESIAN_POINT('Ctrl Pts',(0.00260956047775145,-0.0352450361861253,
0.0725155325411968));
#101097=CARTESIAN_POINT('Ctrl Pts',(0.00267120542792072,-0.0349452761023765,
0.0723075602618868));
#101098=CARTESIAN_POINT('Ctrl Pts',(0.00274834057391347,-0.0346444289983475,
0.0721048221596576));
#101099=CARTESIAN_POINT('Ctrl Pts',(0.00254373971120484,-0.0352450361861253,
0.072756712197659));
#101100=CARTESIAN_POINT('Ctrl Pts',(0.00259628842160232,-0.0349452761023765,
0.0725462574474671));
#101101=CARTESIAN_POINT('Ctrl Pts',(0.0026645401591411,-0.0346444289983475,
0.0723403587608132));
#101102=CARTESIAN_POINT('Ctrl Pts',(0.00269452477997173,-0.0345231616327823,
0.0722567370217171));
#101103=CARTESIAN_POINT('Ctrl Pts',(0.00272062074462613,-0.0344132092796976,
0.0721819023520605));
#101104=CARTESIAN_POINT('Ctrl Pts',(0.00274826325896179,-0.0343032738558974,
0.0721076113179735));
#101105=CARTESIAN_POINT('Ctrl Pts',(0.00277741447176964,-0.0341934961088741,
0.0720339581877328));
#101106=CARTESIAN_POINT('Ctrl Pts',(0.00259144538846841,-0.0345231616327823,
0.0723038090429803));
#101107=CARTESIAN_POINT('Ctrl Pts',(0.0026168925315818,-0.0344132092796976,
0.072227553569036));
#101108=CARTESIAN_POINT('Ctrl Pts',(0.00264391564606864,-0.0343032738558974,
0.0721518283836065));
#101109=CARTESIAN_POINT('Ctrl Pts',(0.00267247762717917,-0.0341934961088741,
0.0720767296126085));
#101110=CARTESIAN_POINT('Ctrl Pts',(0.00248836599696508,-0.0345231616327823,
0.0723508810642435));
#101111=CARTESIAN_POINT('Ctrl Pts',(0.00251316431853747,-0.0344132092796976,
0.0722732047860115));
#101112=CARTESIAN_POINT('Ctrl Pts',(0.00253956803317549,-0.0343032738558974,
0.0721960454492395));
#101113=CARTESIAN_POINT('Ctrl Pts',(0.0025675407825887,-0.0341934961088741,
0.0721195010374841));
#101114=CARTESIAN_POINT('Ctrl Pts',(0.00238528660546176,-0.0345231616327823,
0.0723979530855067));
#101115=CARTESIAN_POINT('Ctrl Pts',(0.00240943610549314,-0.0344132092796976,
0.072318856002987));
#101116=CARTESIAN_POINT('Ctrl Pts',(0.00243522042028234,-0.0343032738558974,
0.0722402625148725));
#101117=CARTESIAN_POINT('Ctrl Pts',(0.00246260393799823,-0.0341934961088741,
0.0721622724623598));
#101118=CARTESIAN_POINT('Origin',(0.0185777693083837,-0.0345625596232488,
0.07773461532368));
#101119=CARTESIAN_POINT('Ctrl Pts',(0.00258864240555079,-0.0346945769586886,
0.0718343515957248));
#101120=CARTESIAN_POINT('Ctrl Pts',(0.00262055321100165,-0.0345846629176052,
0.0717580745717267));
#101121=CARTESIAN_POINT('Ctrl Pts',(0.0026540468444276,-0.0344746925050311,
0.0716824444217771));
#101122=CARTESIAN_POINT('Ctrl Pts',(0.00268907998971765,-0.0343648066253259,
0.0716075578747029));
#101123=CARTESIAN_POINT('Ctrl Pts',(0.00263791844184932,-0.0346945769586886,
0.0719363956735949));
#101124=CARTESIAN_POINT('Ctrl Pts',(0.00266842302832914,-0.0345846629176052,
0.0718607976982835));
#101125=CARTESIAN_POINT('Ctrl Pts',(0.00270049616015044,-0.0344746925050311,
0.0717858176329729));
#101126=CARTESIAN_POINT('Ctrl Pts',(0.00273409634475257,-0.0343648066253259,
0.0717115513810435));
#101127=CARTESIAN_POINT('Ctrl Pts',(0.00268719447814784,-0.0346945769586886,
0.072038439751465));
#101128=CARTESIAN_POINT('Ctrl Pts',(0.00271629284565663,-0.0345846629176052,
0.0719635208248402));
#101129=CARTESIAN_POINT('Ctrl Pts',(0.00274694547587327,-0.0344746925050311,
0.0718891908441687));
#101130=CARTESIAN_POINT('Ctrl Pts',(0.00277911269978749,-0.0343648066253259,
0.0718155448873842));
#101131=CARTESIAN_POINT('Ctrl Pts',(0.00273647051444636,-0.0346945769586886,
0.0721404838293351));
#101132=CARTESIAN_POINT('Ctrl Pts',(0.00276416266298413,-0.0345846629176052,
0.072066243951397));
#101133=CARTESIAN_POINT('Ctrl Pts',(0.00279339479159611,-0.0344746925050311,
0.0719925640553645));
#101134=CARTESIAN_POINT('Ctrl Pts',(0.00282412905482241,-0.0343648066253259,
0.0719195383937248));
#101135=CARTESIAN_POINT('Origin',(0.0184225901435341,-0.0345626446730962,
0.0781897104893465));
#101136=CARTESIAN_POINT('Ctrl Pts',(0.00273558880092203,-0.0346945769586887,
0.0721386579186026));
#101137=CARTESIAN_POINT('Ctrl Pts',(0.00277771716611366,-0.0345275153362892,
0.0720258000506902));
#101138=CARTESIAN_POINT('Ctrl Pts',(0.00282340570392564,-0.034360323596516,
0.0719142378902611));
#101139=CARTESIAN_POINT('Ctrl Pts',(0.00287251438400793,-0.0341934961088741,
0.071804299380333));
#101140=CARTESIAN_POINT('Ctrl Pts',(0.002707984849715,-0.0346945769586887,
0.0722178163054548));
#101141=CARTESIAN_POINT('Ctrl Pts',(0.00274845521080075,-0.0345275153362892,
0.0721043802617323));
#101142=CARTESIAN_POINT('Ctrl Pts',(0.00279250349875911,-0.034360323596516,
0.0719921876332443));
#101143=CARTESIAN_POINT('Ctrl Pts',(0.00283999450665753,-0.0341934961088741,
0.0718815682997534));
#101144=CARTESIAN_POINT('Ctrl Pts',(0.00268038089850797,-0.0346945769586887,
0.0722969746923069));
#101145=CARTESIAN_POINT('Ctrl Pts',(0.00271919325548784,-0.0345275153362892,
0.0721829604727744));
#101146=CARTESIAN_POINT('Ctrl Pts',(0.00276160129359259,-0.034360323596516,
0.0720701373762274));
#101147=CARTESIAN_POINT('Ctrl Pts',(0.00280747462930714,-0.0341934961088741,
0.0719588372191737));
#101148=CARTESIAN_POINT('Ctrl Pts',(0.00265277694730095,-0.0346945769586887,
0.0723761330791591));
#101149=CARTESIAN_POINT('Ctrl Pts',(0.00268993130017493,-0.0345275153362892,
0.0722615406838164));
#101150=CARTESIAN_POINT('Ctrl Pts',(0.00273069908842606,-0.034360323596516,
0.0721480871192105));
#101151=CARTESIAN_POINT('Ctrl Pts',(0.00277495475195675,-0.0341934961088741,
0.0720361061385941));
#101152=CARTESIAN_POINT('Ctrl Pts',(0.00282411732775041,-0.0340223579322365,
0.0719195676932332));
#101153=CARTESIAN_POINT('Ctrl Pts',(0.00285488080647209,-0.0339125849573554,
0.0718464714926344));
#101154=CARTESIAN_POINT('Ctrl Pts',(0.00288713558955374,-0.0338030433565221,
0.0717740633884145));
#101155=CARTESIAN_POINT('Ctrl Pts',(0.00292083222016277,-0.0336938721132328,
0.0717024323218338));
#101156=CARTESIAN_POINT('Ctrl Pts',(0.00271828548965978,-0.0340223579322365,
0.071960074505953));
#101157=CARTESIAN_POINT('Ctrl Pts',(0.00274849027378785,-0.0339125849573554,
0.071885518608286));
#101158=CARTESIAN_POINT('Ctrl Pts',(0.00278021696720156,-0.0338030433565221,
0.0718116402690302));
#101159=CARTESIAN_POINT('Ctrl Pts',(0.00281341662173569,-0.0336938721132328,
0.0717385303694945));
#101160=CARTESIAN_POINT('Ctrl Pts',(0.00261245365156914,-0.0340223579322365,
0.0720005813186729));
#101161=CARTESIAN_POINT('Ctrl Pts',(0.00264209974110361,-0.0339125849573554,
0.0719245657239375));
#101162=CARTESIAN_POINT('Ctrl Pts',(0.00267329834484938,-0.0338030433565221,
0.0718492171496458));
#101163=CARTESIAN_POINT('Ctrl Pts',(0.00270600102330862,-0.0336938721132328,
0.0717746284171553));
#101164=CARTESIAN_POINT('Ctrl Pts',(0.0025066218134785,-0.0340223579322365,
0.0720410881313928));
#101165=CARTESIAN_POINT('Ctrl Pts',(0.00253570920841937,-0.0339125849573554,
0.0719636128395891));
#101166=CARTESIAN_POINT('Ctrl Pts',(0.00256637972249721,-0.0338030433565221,
0.0718867940302615));
#101167=CARTESIAN_POINT('Ctrl Pts',(0.00259858542488155,-0.0336938721132328,
0.071810726464816));
#101168=CARTESIAN_POINT('Origin',(0.0184649163094403,-0.0345589643418681,
0.0776931776749366));
#101169=CARTESIAN_POINT('Ctrl Pts',(0.00274496550589085,-0.034193496108874,
0.0714913666959631));
#101170=CARTESIAN_POINT('Ctrl Pts',(0.0027816264847734,-0.0340836138581107,
0.0714171959990552));
#101171=CARTESIAN_POINT('Ctrl Pts',(0.00281980467997033,-0.03397388966435,
0.0713438195126748));
#101172=CARTESIAN_POINT('Ctrl Pts',(0.0028594449326684,-0.0338644633294062,
0.0712713278741116));
#101173=CARTESIAN_POINT('Ctrl Pts',(0.00278773696925139,-0.034193496108874,
0.0715963036349737));
#101174=CARTESIAN_POINT('Ctrl Pts',(0.00282295092988617,-0.0340836138581107,
0.0715227227312173));
#101175=CARTESIAN_POINT('Ctrl Pts',(0.00285967059661017,-0.03397388966435,
0.0714499058119881));
#101176=CARTESIAN_POINT('Ctrl Pts',(0.00289784272535534,-0.0338644633294062,
0.0713779429235356));
#101177=CARTESIAN_POINT('Ctrl Pts',(0.00283050843261193,-0.034193496108874,
0.0717012405739843));
#101178=CARTESIAN_POINT('Ctrl Pts',(0.00286427537499894,-0.0340836138581107,
0.0716282494633793));
#101179=CARTESIAN_POINT('Ctrl Pts',(0.00289953651325002,-0.03397388966435,
0.0715559921113014));
#101180=CARTESIAN_POINT('Ctrl Pts',(0.00293624051804228,-0.0338644633294062,
0.0714845579729596));
#101181=CARTESIAN_POINT('Ctrl Pts',(0.00287327989597247,-0.034193496108874,
0.0718061775129949));
#101182=CARTESIAN_POINT('Ctrl Pts',(0.00290559982011171,-0.0340836138581107,
0.0717337761955414));
#101183=CARTESIAN_POINT('Ctrl Pts',(0.00293940242988986,-0.03397388966435,
0.0716620784106148));
#101184=CARTESIAN_POINT('Ctrl Pts',(0.00297463831072922,-0.0338644633294062,
0.0715911730223836));
#101185=CARTESIAN_POINT('Origin',(0.0183529366772285,-0.0345610621863404,
0.0781611633305691));
#101186=CARTESIAN_POINT('Ctrl Pts',(0.00285786328873317,-0.0342436276873901,
0.0718373774426975));
#101187=CARTESIAN_POINT('Ctrl Pts',(0.00294508528635293,-0.0339430054201862,
0.0716387700371384));
#101188=CARTESIAN_POINT('Ctrl Pts',(0.00304701941897627,-0.0336441434784164,
0.0714472967726391));
#101189=CARTESIAN_POINT('Ctrl Pts',(0.00276233686574636,-0.0342436276873901,
0.0720684070999092));
#101190=CARTESIAN_POINT('Ctrl Pts',(0.00284084543620189,-0.0339430054201862,
0.0718661968559136));
#101191=CARTESIAN_POINT('Ctrl Pts',(0.0029343622761473,-0.0336441434784164,
0.071670474657228));
#101192=CARTESIAN_POINT('Ctrl Pts',(0.00297462608320018,-0.0335235895815127,
0.0715911979124468));
#101193=CARTESIAN_POINT('Ctrl Pts',(0.00300985303175257,-0.0334144449262719,
0.0715203096408395));
#101194=CARTESIAN_POINT('Ctrl Pts',(0.00304658495014301,-0.0333049234473133,
0.0714500676894422));
#101195=CARTESIAN_POINT('Ctrl Pts',(0.00308478300561825,-0.0331951640388588,
0.0713805661307868));
#101196=CARTESIAN_POINT('Ctrl Pts',(0.00286645965177719,-0.0335235895815127,
0.0716249794991403));
#101197=CARTESIAN_POINT('Ctrl Pts',(0.00290122153027892,-0.0334144449262719,
0.0715526021036443));
#101198=CARTESIAN_POINT('Ctrl Pts',(0.00293751860848841,-0.0333049234473133,
0.0714808597095383));
#101199=CARTESIAN_POINT('Ctrl Pts',(0.00297531278347509,-0.0331951640388588,
0.0714098482575921));
#101200=CARTESIAN_POINT('Ctrl Pts',(0.00275829322035419,-0.0335235895815127,
0.0716587610858338));
#101201=CARTESIAN_POINT('Ctrl Pts',(0.00279259002880527,-0.0334144449262719,
0.0715848945664492));
#101202=CARTESIAN_POINT('Ctrl Pts',(0.00282845226683381,-0.0333049234473133,
0.0715116517296343));
#101203=CARTESIAN_POINT('Ctrl Pts',(0.00286584256133193,-0.0331951640388588,
0.0714391303843974));
#101204=CARTESIAN_POINT('Ctrl Pts',(0.00265012678893119,-0.0335235895815127,
0.0716925426725273));
#101205=CARTESIAN_POINT('Ctrl Pts',(0.00268395852733162,-0.0334144449262719,
0.071617187029254));
#101206=CARTESIAN_POINT('Ctrl Pts',(0.00271938592517922,-0.0333049234473133,
0.0715424437497303));
#101207=CARTESIAN_POINT('Ctrl Pts',(0.00275637233918876,-0.0331951640388588,
0.0714684125112027));
#101208=CARTESIAN_POINT('Origin',(0.017309347843454,-0.0326434571772312,
0.0800669115217672));
#101209=CARTESIAN_POINT('Ctrl Pts',(0.00292187045044344,-0.0336938721132379,
0.0711569522629806));
#101210=CARTESIAN_POINT('Ctrl Pts',(0.00293938975204655,-0.0336474569764953,
0.0711265037473738));
#101211=CARTESIAN_POINT('Ctrl Pts',(0.00295726429153528,-0.033601104548885,
0.0710962624036639));
#101212=CARTESIAN_POINT('Ctrl Pts',(0.00300251851395925,-0.0334837508643164,
0.0710196982776055));
#101213=CARTESIAN_POINT('Ctrl Pts',(0.00305002161776679,-0.033366026476041,
0.0709445087492458));
#101214=CARTESIAN_POINT('Ctrl Pts',(0.00303016432205854,-0.0336938721132379,
0.0714791982507639));
#101215=CARTESIAN_POINT('Ctrl Pts',(0.00304579741096262,-0.0336474569764953,
0.0714493836151234));
#101216=CARTESIAN_POINT('Ctrl Pts',(0.00306177844663147,-0.033601104548885,
0.0714197540274447));
#101217=CARTESIAN_POINT('Ctrl Pts',(0.00310223875293364,-0.0334837508643164,
0.0713447387269392));
#101218=CARTESIAN_POINT('Ctrl Pts',(0.00314490415084343,-0.033366026476041,
0.0712709552903345));
#101219=CARTESIAN_POINT('Ctrl Pts',(0.00303016432207031,-0.0336938721132426,
0.0714791982507706));
#101220=CARTESIAN_POINT('Ctrl Pts',(0.00304579741097352,-0.0336474569765026,
0.0714493836151318));
#101221=CARTESIAN_POINT('Ctrl Pts',(0.00306177844664147,-0.0336011045488949,
0.0714197540274547));
#101222=CARTESIAN_POINT('Ctrl Pts',(0.00310190177370088,-0.0334847282606778,
0.0713453635022282));
#101223=CARTESIAN_POINT('Ctrl Pts',(0.00314419376792775,-0.0333679869945434,
0.0712721841414624));
#101224=CARTESIAN_POINT('Ctrl Pts',(0.00303016432205703,-0.0336938721132424,
0.0714791982507669));
#101225=CARTESIAN_POINT('Ctrl Pts',(0.00308607516630843,-0.0335278710435082,
0.0713725679194267));
#101226=CARTESIAN_POINT('Ctrl Pts',(0.00314531024072201,-0.033362046922432,
0.0712677284499286));
#101227=CARTESIAN_POINT('Ctrl Pts',(0.00320791644279647,-0.0331951640388603,
0.0711646375555202));
#101228=CARTESIAN_POINT('Ctrl Pts',(0.00299285685570229,-0.0336938721132424,
0.0715542727656003));
#101229=CARTESIAN_POINT('Ctrl Pts',(0.00304719608217738,-0.0335278710435082,
0.0714468614358421));
#101230=CARTESIAN_POINT('Ctrl Pts',(0.00310488458361347,-0.033362046922432,
0.0713411919571547));
#101231=CARTESIAN_POINT('Ctrl Pts',(0.00316596862641463,-0.0331951640388603,
0.0712372213727529));
#101232=CARTESIAN_POINT('Ctrl Pts',(0.00295554938934755,-0.0336938721132424,
0.0716293472804336));
#101233=CARTESIAN_POINT('Ctrl Pts',(0.00300831699804633,-0.0335278710435082,
0.0715211549522575));
#101234=CARTESIAN_POINT('Ctrl Pts',(0.00306445892650492,-0.033362046922432,
0.0714146554643807));
#101235=CARTESIAN_POINT('Ctrl Pts',(0.00312402081003279,-0.0331951640388603,
0.0713098051899855));
#101236=CARTESIAN_POINT('Ctrl Pts',(0.00291824192299281,-0.0336938721132424,
0.071704421795267));
#101237=CARTESIAN_POINT('Ctrl Pts',(0.00296943791391528,-0.0335278710435082,
0.0715954484686729));
#101238=CARTESIAN_POINT('Ctrl Pts',(0.00302403326939637,-0.033362046922432,
0.0714881189716068));
#101239=CARTESIAN_POINT('Ctrl Pts',(0.00308207299365095,-0.0331951640388603,
0.0713823890072182));
#101240=CARTESIAN_POINT('Ctrl Pts',(0.00314545434883956,-0.0330240426238156,
0.0712729298487996));
#101241=CARTESIAN_POINT('Ctrl Pts',(0.00318508879316578,-0.0329142774063509,
0.0712043485325954));
#101242=CARTESIAN_POINT('Ctrl Pts',(0.00322616076408639,-0.0328043479726686,
0.0711365523807815));
#101243=CARTESIAN_POINT('Ctrl Pts',(0.00326862003723418,-0.0326943950436594,
0.0710696296943197));
#101244=CARTESIAN_POINT('Ctrl Pts',(0.00303538035654005,-0.0330240426238156,
0.07129985292819));
#101245=CARTESIAN_POINT('Ctrl Pts',(0.00307464390921778,-0.0329142774063509,
0.071229755235502));
#101246=CARTESIAN_POINT('Ctrl Pts',(0.00311537615132461,-0.0328043479726686,
0.0711604342838688));
#101247=CARTESIAN_POINT('Ctrl Pts',(0.00315752734750701,-0.0326943950436594,
0.0710919803156488));
#101248=CARTESIAN_POINT('Ctrl Pts',(0.00292530636424054,-0.0330240426238156,
0.0713267760075804));
#101249=CARTESIAN_POINT('Ctrl Pts',(0.00296419902526979,-0.0329142774063509,
0.0712551619384086));
#101250=CARTESIAN_POINT('Ctrl Pts',(0.00300459153856282,-0.0328043479726686,
0.0711843161869562));
#101251=CARTESIAN_POINT('Ctrl Pts',(0.00304643465777984,-0.0326943950436594,
0.0711143309369779));
#101252=CARTESIAN_POINT('Ctrl Pts',(0.00281523237194103,-0.0330240426238156,
0.0713536990869708));
#101253=CARTESIAN_POINT('Ctrl Pts',(0.00285375414132179,-0.0329142774063509,
0.0712805686413151));
#101254=CARTESIAN_POINT('Ctrl Pts',(0.00289380692580104,-0.0328043479726686,
0.0712081980900436));
#101255=CARTESIAN_POINT('Ctrl Pts',(0.00293534196805267,-0.0326943950436594,
0.071136681558307));
#101256=CARTESIAN_POINT('Origin',(0.0174147894217676,-0.0326396682856539,
0.0801315448900268));
#101257=CARTESIAN_POINT('Ctrl Pts',(0.00312059419090093,-0.0331951640388587,
0.0708381863255022));
#101258=CARTESIAN_POINT('Ctrl Pts',(0.00316620772452263,-0.0330855618255041,
0.0707692775321387));
#101259=CARTESIAN_POINT('Ctrl Pts',(0.00321327836727237,-0.0329757224427708,
0.0707012618171597));
#101260=CARTESIAN_POINT('Ctrl Pts',(0.00326175011471513,-0.0328657862078596,
0.0706342292354737));
#101261=CARTESIAN_POINT('Ctrl Pts',(0.00314987629439357,-0.0331951640388587,
0.0709476564604918));
#101262=CARTESIAN_POINT('Ctrl Pts',(0.00319398209836207,-0.0330855618255041,
0.0708791509688667));
#101263=CARTESIAN_POINT('Ctrl Pts',(0.00323953558899983,-0.0329757224427708,
0.0708115076841659));
#101264=CARTESIAN_POINT('Ctrl Pts',(0.00328648268128231,-0.0328657862078596,
0.0707448160890802));
#101265=CARTESIAN_POINT('Ctrl Pts',(0.00317915839788622,-0.0331951640388588,
0.0710571265954814));
#101266=CARTESIAN_POINT('Ctrl Pts',(0.00322175647220151,-0.0330855618255041,
0.0709890244055947));
#101267=CARTESIAN_POINT('Ctrl Pts',(0.0032657928107273,-0.0329757224427708,
0.0709217535511722));
#101268=CARTESIAN_POINT('Ctrl Pts',(0.00331121524784949,-0.0328657862078596,
0.0708554029426867));
#101269=CARTESIAN_POINT('Ctrl Pts',(0.00320844050137886,-0.0331951640388588,
0.071166596730471));
#101270=CARTESIAN_POINT('Ctrl Pts',(0.00324953084604096,-0.0330855618255041,
0.0710988978423227));
#101271=CARTESIAN_POINT('Ctrl Pts',(0.00329205003245476,-0.0329757224427708,
0.0710319994181785));
#101272=CARTESIAN_POINT('Ctrl Pts',(0.00333594781441668,-0.0328657862078596,
0.0709659897962932));
#101273=CARTESIAN_POINT('Origin',(0.0171228894063379,-0.0326401908830065,
0.0805137323480971));
#101274=CARTESIAN_POINT('Ctrl Pts',(0.0031892723219281,-0.0332451089994434,
0.0711955563415044));
#101275=CARTESIAN_POINT('Ctrl Pts',(0.00330070098757655,-0.0329451141710259,
0.0710094482568253));
#101276=CARTESIAN_POINT('Ctrl Pts',(0.00342583151789996,-0.0326442513127504,
0.0708322621481936));
#101277=CARTESIAN_POINT('Ctrl Pts',(0.00306554072209852,-0.0332451089994434,
0.0714127900663346));
#101278=CARTESIAN_POINT('Ctrl Pts',(0.00316877628376881,-0.0329451141710259,
0.0712220153680182));
#101279=CARTESIAN_POINT('Ctrl Pts',(0.00328608849427418,-0.0326442513127504,
0.0710395587650206));
#101280=CARTESIAN_POINT('Ctrl Pts',(0.00333593024811363,-0.0325229783203385,
0.0709660160490157));
#101281=CARTESIAN_POINT('Ctrl Pts',(0.00337982139644991,-0.032413025311208,
0.0709000156158587));
#101282=CARTESIAN_POINT('Ctrl Pts',(0.00342507119155223,-0.0323031222247695,
0.0708349331377294));
#101283=CARTESIAN_POINT('Ctrl Pts',(0.00347161872993966,-0.0321934096636184,
0.0707708499353724));
#101284=CARTESIAN_POINT('Ctrl Pts',(0.00322438292180028,-0.0325229783203385,
0.0709859744217387));
#101285=CARTESIAN_POINT('Ctrl Pts',(0.00326799894441005,-0.032413025311208,
0.0709184363111559));
#101286=CARTESIAN_POINT('Ctrl Pts',(0.00331300546434632,-0.0323031222247695,
0.0708518106974906));
#101287=CARTESIAN_POINT('Ctrl Pts',(0.00335934181999699,-0.0321934096636184,
0.0707861808891304));
#101288=CARTESIAN_POINT('Ctrl Pts',(0.00311283559548694,-0.0325229783203385,
0.0710059327944618));
#101289=CARTESIAN_POINT('Ctrl Pts',(0.00315617649237019,-0.032413025311208,
0.0709368570064531));
#101290=CARTESIAN_POINT('Ctrl Pts',(0.0032009397371404,-0.0323031222247695,
0.0708686882572519));
#101291=CARTESIAN_POINT('Ctrl Pts',(0.00324706491005432,-0.0321934096636184,
0.0708015118428885));
#101292=CARTESIAN_POINT('Ctrl Pts',(0.00300128826917359,-0.0325229783203385,
0.0710258911671848));
#101293=CARTESIAN_POINT('Ctrl Pts',(0.00304435404033032,-0.032413025311208,
0.0709552777017503));
#101294=CARTESIAN_POINT('Ctrl Pts',(0.00308887400993449,-0.0323031222247695,
0.0708855658170131));
#101295=CARTESIAN_POINT('Ctrl Pts',(0.00313478800011164,-0.0321934096636184,
0.0708168427966465));
#101296=CARTESIAN_POINT('Origin',(0.0174077525540327,-0.0326393375176799,
0.0801267310016776));
#101297=CARTESIAN_POINT('Ctrl Pts',(0.00333841734075972,-0.0326943950436593,
0.0705305686593156));
#101298=CARTESIAN_POINT('Ctrl Pts',(0.0033882998881715,-0.0325844576448126,
0.0704646173629209));
#101299=CARTESIAN_POINT('Ctrl Pts',(0.00343954994678673,-0.0324744968375318,
0.0703996930519144));
#101300=CARTESIAN_POINT('Ctrl Pts',(0.0034921007046729,-0.0323646534831894,
0.070335878005398));
#101301=CARTESIAN_POINT('Ctrl Pts',(0.00336076795477588,-0.0326943950436593,
0.0706416613126942));
#101302=CARTESIAN_POINT('Ctrl Pts',(0.00340911943721428,-0.0325844576448126,
0.0705760180496501));
#101303=CARTESIAN_POINT('Ctrl Pts',(0.00345883195186557,-0.0324744968375318,
0.0705113701288604));
#101304=CARTESIAN_POINT('Ctrl Pts',(0.0035098406616727,-0.0323646534831894,
0.0704477995024718));
#101305=CARTESIAN_POINT('Ctrl Pts',(0.00338311856879204,-0.0326943950436593,
0.0707527539660728));
#101306=CARTESIAN_POINT('Ctrl Pts',(0.00342993898625707,-0.0325844576448126,
0.0706874187363793));
#101307=CARTESIAN_POINT('Ctrl Pts',(0.00347811395694441,-0.0324744968375318,
0.0706230472058065));
#101308=CARTESIAN_POINT('Ctrl Pts',(0.00352758061867251,-0.0323646534831894,
0.0705597209995456));
#101309=CARTESIAN_POINT('Ctrl Pts',(0.0034054691828082,-0.0326943950436593,
0.0708638466194514));
#101310=CARTESIAN_POINT('Ctrl Pts',(0.00345075853529985,-0.0325844576448126,
0.0707988194231086));
#101311=CARTESIAN_POINT('Ctrl Pts',(0.00349739596202326,-0.0324744968375318,
0.0707347242827525));
#101312=CARTESIAN_POINT('Ctrl Pts',(0.00354532057567232,-0.0323646534831894,
0.0706716424966194));
#101313=CARTESIAN_POINT('Origin',(0.0171540481476118,-0.0326395579068999,
0.0805352054641116));
#101314=CARTESIAN_POINT('Ctrl Pts',(0.00338449828019584,-0.0327445246961878,
0.0708915781438235));
#101315=CARTESIAN_POINT('Ctrl Pts',(0.00350739166825613,-0.0324436878365476,
0.0707128331308248));
#101316=CARTESIAN_POINT('Ctrl Pts',(0.0036433997339666,-0.0321434074463187,
0.0705438527456834));
#101317=CARTESIAN_POINT('Ctrl Pts',(0.00324737204356741,-0.0327445246961878,
0.0711006149712681));
#101318=CARTESIAN_POINT('Ctrl Pts',(0.00336238147887758,-0.0324436878365476,
0.0709166981577614));
#101319=CARTESIAN_POINT('Ctrl Pts',(0.0034909175504622,-0.0321434074463187,
0.0707419668131136));
#101320=CARTESIAN_POINT('Ctrl Pts',(0.00360190210950176,-0.0322357242816073,
0.0705960267995549));
#101321=CARTESIAN_POINT('Ctrl Pts',(0.00371509154660157,-0.0319819883628706,
0.0704520107835557));
#101322=CARTESIAN_POINT('Ctrl Pts',(0.0038372157423532,-0.0317295851069886,
0.070315489201572));
#101323=CARTESIAN_POINT('Ctrl Pts',(0.00345172649576831,-0.0322357242816073,
0.0707958949687059));
#101324=CARTESIAN_POINT('Ctrl Pts',(0.00355855039090018,-0.0319819883628706,
0.0706470960541798));
#101325=CARTESIAN_POINT('Ctrl Pts',(0.00367462629476046,-0.0317295851069886,
0.0705053962091613));
#101326=CARTESIAN_POINT('Origin',(0.0170772303833248,-0.0326371942646307,
0.0804788012569333));
#101327=CARTESIAN_POINT('Origin',(0.0173061599489961,-0.0326352985530895,
0.0800578634077293));
#101328=CARTESIAN_POINT('Ctrl Pts',(0.00357512613946539,-0.0321934096636183,
0.0702372352350691));
#101329=CARTESIAN_POINT('Ctrl Pts',(0.00362908621499712,-0.0320835708272304,
0.0701745057230825));
#101330=CARTESIAN_POINT('Ctrl Pts',(0.00368431317548228,-0.0319739230346346,
0.0701129292977206));
#101331=CARTESIAN_POINT('Ctrl Pts',(0.00374073031549945,-0.0318646057455575,
0.070052579318862));
#101332=CARTESIAN_POINT('Ctrl Pts',(0.00359045710642513,-0.0321934096636183,
0.0703495122416948));
#101333=CARTESIAN_POINT('Ctrl Pts',(0.00364286879453211,-0.0320835708272304,
0.0702869941556908));
#101334=CARTESIAN_POINT('Ctrl Pts',(0.00369654389027044,-0.0319739230346346,
0.0702255969898787));
#101335=CARTESIAN_POINT('Ctrl Pts',(0.00375140769132395,-0.0318646057455575,
0.0701653940271684));
#101336=CARTESIAN_POINT('Ctrl Pts',(0.00360578807338487,-0.0321934096636183,
0.0704617892483205));
#101337=CARTESIAN_POINT('Ctrl Pts',(0.00365665137406711,-0.0320835708272304,
0.0703994825882991));
#101338=CARTESIAN_POINT('Ctrl Pts',(0.00370877460505861,-0.0319739230346346,
0.0703382646820367));
#101339=CARTESIAN_POINT('Ctrl Pts',(0.00376208506714845,-0.0318646057455575,
0.0702782087354748));
#101340=CARTESIAN_POINT('Ctrl Pts',(0.00362111904034461,-0.0321934096636183,
0.0705740662549463));
#101341=CARTESIAN_POINT('Ctrl Pts',(0.00367043395360211,-0.0320835708272304,
0.0705119710209075));
#101342=CARTESIAN_POINT('Ctrl Pts',(0.00372100531984677,-0.0319739230346346,
0.0704509323741947));
#101343=CARTESIAN_POINT('Ctrl Pts',(0.00377276244297296,-0.0318646057455575,
0.0703910234437812));
#101344=CARTESIAN_POINT('Ctrl Pts',(0.00354437754856675,-0.0320218834582388,
0.0706715160052204));
#101345=CARTESIAN_POINT('Ctrl Pts',(0.00358058015777147,-0.031939109935068,
0.0706238554735102));
#101346=CARTESIAN_POINT('Ctrl Pts',(0.00361750505862053,-0.0318564869454956,
0.0705767891269242));
#101347=CARTESIAN_POINT('Ctrl Pts',(0.00365512215579729,-0.0317740741446545,
0.070530348736228));
#101348=CARTESIAN_POINT('Ctrl Pts',(0.00349513376256958,-0.0320218834582388,
0.0706771620292948));
#101349=CARTESIAN_POINT('Ctrl Pts',(0.00353127761031287,-0.031939109935068,
0.0706289889888185));
#101350=CARTESIAN_POINT('Ctrl Pts',(0.00356815178819881,-0.0318564869454956,
0.0705814095264139));
#101351=CARTESIAN_POINT('Ctrl Pts',(0.0036057262029648,-0.0317740741446545,
0.0705344557900326));
#101352=CARTESIAN_POINT('Ctrl Pts',(0.00344588997657241,-0.0320218834582388,
0.0706828080533692));
#101353=CARTESIAN_POINT('Ctrl Pts',(0.00348197506285426,-0.031939109935068,
0.0706341225041267));
#101354=CARTESIAN_POINT('Ctrl Pts',(0.00351879851777708,-0.0318564869454956,
0.0705860299259036));
#101355=CARTESIAN_POINT('Ctrl Pts',(0.0035563302501323,-0.0317740741446545,
0.0705385628438372));
#101356=CARTESIAN_POINT('Ctrl Pts',(0.00339664619057525,-0.0320218834582388,
0.0706884540774437));
#101357=CARTESIAN_POINT('Ctrl Pts',(0.00343267251539565,-0.031939109935068,
0.070639256019435));
#101358=CARTESIAN_POINT('Ctrl Pts',(0.00346944524735535,-0.0318564869454956,
0.0705906503253933));
#101359=CARTESIAN_POINT('Ctrl Pts',(0.00350693429729981,-0.0317740741446545,
0.0705426698976418));
#101360=CARTESIAN_POINT('Origin',(-0.00203465492131801,-0.0391228853390622,
0.067616488408112));
#101361=CARTESIAN_POINT('Ctrl Pts',(0.00241022601210972,-0.0352722978779625,
0.0734870970590132));
#101362=CARTESIAN_POINT('Ctrl Pts',(0.00241275129914135,-0.0352466642097238,
0.0734683696565378));
#101363=CARTESIAN_POINT('Ctrl Pts',(0.00241519663864789,-0.0352210183808312,
0.0734496484609053));
#101364=CARTESIAN_POINT('Ctrl Pts',(0.00241756158888749,-0.0351953608940153,
0.0734309327424934));
#101365=CARTESIAN_POINT('Origin',(-0.00241827000673056,-0.0352456003065117,
0.072653208942305));
#101366=CARTESIAN_POINT('Ctrl Pts',(0.002435929945587,-0.035024121149334,
0.0733076123512748));
#101367=CARTESIAN_POINT('Ctrl Pts',(0.00244753348953259,-0.0349144232867422,
0.0732292645222082));
#101368=CARTESIAN_POINT('Ctrl Pts',(0.00246076348429631,-0.0348045283677513,
0.0731511096517255));
#101369=CARTESIAN_POINT('Ctrl Pts',(0.00247560670913094,-0.0346945769586887,
0.0730732484768736));
#101370=CARTESIAN_POINT('Ctrl Pts',(0.00234349675984053,-0.035024121149334,
0.0733731657491714));
#101371=CARTESIAN_POINT('Ctrl Pts',(0.00235419733264876,-0.0349144232867422,
0.0732935446909276));
#101372=CARTESIAN_POINT('Ctrl Pts',(0.00236655013435908,-0.0348045283677513,
0.0732140971641209));
#101373=CARTESIAN_POINT('Ctrl Pts',(0.00238054312941053,-0.0346945769586887,
0.0731349255197159));
#101374=CARTESIAN_POINT('Ctrl Pts',(0.00225106357409406,-0.035024121149334,
0.073438719147068));
#101375=CARTESIAN_POINT('Ctrl Pts',(0.00226086117576492,-0.0349144232867422,
0.073357824859647));
#101376=CARTESIAN_POINT('Ctrl Pts',(0.00227233678442185,-0.0348045283677513,
0.0732770846765164));
#101377=CARTESIAN_POINT('Ctrl Pts',(0.00228547954969013,-0.0346945769586887,
0.0731966025625582));
#101378=CARTESIAN_POINT('Ctrl Pts',(0.0021586303883476,-0.035024121149334,
0.0735042725449646));
#101379=CARTESIAN_POINT('Ctrl Pts',(0.00216752501888108,-0.0349144232867422,
0.0734221050283664));
#101380=CARTESIAN_POINT('Ctrl Pts',(0.00217812343448462,-0.0348045283677513,
0.0733400721889119));
#101381=CARTESIAN_POINT('Ctrl Pts',(0.00219041596996972,-0.0346945769586887,
0.0732582796054005));
#101382=CARTESIAN_POINT('Origin',(0.0189327085722657,-0.0345629067940946,
0.0763939031326696));
#101383=CARTESIAN_POINT('Ctrl Pts',(0.00230774228889657,-0.0351970973651633,
0.0729884486193835));
#101384=CARTESIAN_POINT('Ctrl Pts',(0.00232383400909443,-0.0350869349321776,
0.072907875268639));
#101385=CARTESIAN_POINT('Ctrl Pts',(0.00234161413479677,-0.0349764985129712,
0.0728275697098138));
#101386=CARTESIAN_POINT('Ctrl Pts',(0.00236106575562629,-0.0348659306849618,
0.0727476373370736));
#101387=CARTESIAN_POINT('Ctrl Pts',(0.00235675309102232,-0.0351970973651633,
0.0730544668890143));
#101388=CARTESIAN_POINT('Ctrl Pts',(0.00237193021756503,-0.0350869349321776,
0.0729745725165119));
#101389=CARTESIAN_POINT('Ctrl Pts',(0.00238878087639209,-0.0349764985129712,
0.0728949274844911));
#101390=CARTESIAN_POINT('Ctrl Pts',(0.00240728931090446,-0.0348659306849618,
0.0728156362605026));
#101391=CARTESIAN_POINT('Ctrl Pts',(0.00240576389314807,-0.0351970973651633,
0.0731204851586451));
#101392=CARTESIAN_POINT('Ctrl Pts',(0.00242002642603563,-0.0350869349321776,
0.0730412697643848));
#101393=CARTESIAN_POINT('Ctrl Pts',(0.00243594761798742,-0.0349764985129712,
0.0729622852591685));
#101394=CARTESIAN_POINT('Ctrl Pts',(0.00245351286618263,-0.0348659306849618,
0.0728836351839316));
#101395=CARTESIAN_POINT('Ctrl Pts',(0.00245477469527383,-0.0351970973651633,
0.0731865034282759));
#101396=CARTESIAN_POINT('Ctrl Pts',(0.00246812263450623,-0.0350869349321776,
0.0731079670122576));
#101397=CARTESIAN_POINT('Ctrl Pts',(0.00248311435958274,-0.0349764985129712,
0.0730296430338458));
#101398=CARTESIAN_POINT('Ctrl Pts',(0.0024997364214608,-0.0348659306849618,
0.0729516341073605));
#101399=CARTESIAN_POINT('Origin',(0.0187908648875428,-0.0345637187965049,
0.0768534743735188));
#101400=CARTESIAN_POINT('Ctrl Pts',(0.00244818867122777,-0.0352450361861252,
0.0732195360434774));
#101401=CARTESIAN_POINT('Ctrl Pts',(0.00248328169429483,-0.0349452761023764,
0.0730054775267704));
#101402=CARTESIAN_POINT('Ctrl Pts',(0.00253439878470322,-0.0346444289983475,
0.0727946704777635));
#101403=CARTESIAN_POINT('Ctrl Pts',(0.00241311474729942,-0.0352450361861252,
0.0734670634558184));
#101404=CARTESIAN_POINT('Ctrl Pts',(0.00243887212105936,-0.0349452761023764,
0.0732516821043978));
#101405=CARTESIAN_POINT('Ctrl Pts',(0.00248077972507688,-0.0346444289983475,
0.0730388527794252));
#101406=CARTESIAN_POINT('Ctrl Pts',(0.00250004732525913,-0.0345231616327821,
0.0729521323532325));
#101407=CARTESIAN_POINT('Ctrl Pts',(0.00251655824430696,-0.0344132092796975,
0.072874617085665));
#101408=CARTESIAN_POINT('Ctrl Pts',(0.0025346716536337,-0.0343032738558973,
0.0727974473328659));
#101409=CARTESIAN_POINT('Ctrl Pts',(0.0025543618154463,-0.0341934961088741,
0.0727207213637928));
#101410=CARTESIAN_POINT('Ctrl Pts',(0.00240368043418143,-0.0345231616327821,
0.0730117524709993));
#101411=CARTESIAN_POINT('Ctrl Pts',(0.00241936957384426,-0.0344132092796975,
0.072932908921512));
#101412=CARTESIAN_POINT('Ctrl Pts',(0.00243668872064982,-0.0343032738558973,
0.0728543939574681));
#101413=CARTESIAN_POINT('Ctrl Pts',(0.00245561311020234,-0.0341934961088741,
0.0727763075972607));
#101414=CARTESIAN_POINT('Ctrl Pts',(0.00230731354310373,-0.0345231616327821,
0.073071372588766));
#101415=CARTESIAN_POINT('Ctrl Pts',(0.00232218090338157,-0.0344132092796975,
0.072991200757359));
#101416=CARTESIAN_POINT('Ctrl Pts',(0.00233870578766594,-0.0343032738558973,
0.0729113405820702));
#101417=CARTESIAN_POINT('Ctrl Pts',(0.00235686440495838,-0.0341934961088741,
0.0728318938307285));
#101418=CARTESIAN_POINT('Ctrl Pts',(0.00221094665202603,-0.0345231616327821,
0.0731309927065328));
#101419=CARTESIAN_POINT('Ctrl Pts',(0.00222499223291887,-0.0344132092796975,
0.073049492593206));
#101420=CARTESIAN_POINT('Ctrl Pts',(0.00224072285468207,-0.0343032738558973,
0.0729682872066723));
#101421=CARTESIAN_POINT('Ctrl Pts',(0.00225811569971443,-0.0341934961088741,
0.0728874800641964));
#101422=CARTESIAN_POINT('Origin',(0.0189446079269458,-0.0345625596231005,
0.0763961175525524));
#101423=CARTESIAN_POINT('Ctrl Pts',(0.0023420609337359,-0.0346945769586885,
0.0725463481428481));
#101424=CARTESIAN_POINT('Ctrl Pts',(0.00236416006689013,-0.0345846629176052,
0.0724666731015343));
#101425=CARTESIAN_POINT('Ctrl Pts',(0.00238791062176432,-0.0344746925050311,
0.0723874414525256));
#101426=CARTESIAN_POINT('Ctrl Pts',(0.00241328174714459,-0.0343648066253259,
0.0723087545908615));
#101427=CARTESIAN_POINT('Ctrl Pts',(0.00240373792801572,-0.0346945769586885,
0.0726414116477186));
#101428=CARTESIAN_POINT('Ctrl Pts',(0.00242452703802318,-0.0345846629176052,
0.0725625865465605));
#101429=CARTESIAN_POINT('Ctrl Pts',(0.00244694976958205,-0.0344746925050311,
0.0724841778921387));
#101430=CARTESIAN_POINT('Ctrl Pts',(0.0024709769771937,-0.0343648066253259,
0.0724062860320035));
#101431=CARTESIAN_POINT('Ctrl Pts',(0.00246541492229555,-0.0346945769586885,
0.0727364751525891));
#101432=CARTESIAN_POINT('Ctrl Pts',(0.00248489400915623,-0.0345846629176052,
0.0726584999915867));
#101433=CARTESIAN_POINT('Ctrl Pts',(0.00250598891739978,-0.0344746925050311,
0.0725809143317517));
#101434=CARTESIAN_POINT('Ctrl Pts',(0.00252867220724281,-0.0343648066253259,
0.0725038174731455));
#101435=CARTESIAN_POINT('Ctrl Pts',(0.00252709191657538,-0.0346945769586885,
0.0728315386574596));
#101436=CARTESIAN_POINT('Ctrl Pts',(0.00254526098028928,-0.0345846629176052,
0.0727544134366129));
#101437=CARTESIAN_POINT('Ctrl Pts',(0.00256502806521751,-0.0344746925050311,
0.0726776507713648));
#101438=CARTESIAN_POINT('Ctrl Pts',(0.00258636743729192,-0.0343648066253259,
0.0726013489142874));
#101439=CARTESIAN_POINT('Origin',(0.0188476909451964,-0.0345626446731571,
0.0768670732632059));
#101440=CARTESIAN_POINT('Ctrl Pts',(0.00252598830832928,-0.0346945769586886,
0.0728298376525857));
#101441=CARTESIAN_POINT('Ctrl Pts',(0.00255363963725959,-0.0345275153362891,
0.0727125896184365));
#101442=CARTESIAN_POINT('Ctrl Pts',(0.00258498546099442,-0.0343603235965159,
0.0725961808667837));
#101443=CARTESIAN_POINT('Ctrl Pts',(0.00261992795552367,-0.0341934961088741,
0.0724809543051727));
#101444=CARTESIAN_POINT('Ctrl Pts',(0.00250852319911034,-0.0346945769586886,
0.0729118315443779));
#101445=CARTESIAN_POINT('Ctrl Pts',(0.00253445713314853,-0.0345275153362891,
0.0727942176965235));
#101446=CARTESIAN_POINT('Ctrl Pts',(0.00256409662228927,-0.0343603235965159,
0.0726773890260587));
#101447=CARTESIAN_POINT('Ctrl Pts',(0.00259734887064439,-0.0341934961088741,
0.0725616897574677));
#101448=CARTESIAN_POINT('Ctrl Pts',(0.0024910580898914,-0.0346945769586886,
0.0729938254361702));
#101449=CARTESIAN_POINT('Ctrl Pts',(0.00251527462903747,-0.0345275153362891,
0.0728758457746105));
#101450=CARTESIAN_POINT('Ctrl Pts',(0.00254320778358412,-0.0343603235965159,
0.0727585971853337));
#101451=CARTESIAN_POINT('Ctrl Pts',(0.0025747697857651,-0.0341934961088741,
0.0726424252097627));
#101452=CARTESIAN_POINT('Ctrl Pts',(0.00247359298067246,-0.0346945769586886,
0.0730758193279624));
#101453=CARTESIAN_POINT('Ctrl Pts',(0.0024960921249264,-0.0345275153362891,
0.0729574738526975));
#101454=CARTESIAN_POINT('Ctrl Pts',(0.00252231894487896,-0.0343603235965159,
0.0728398053446087));
#101455=CARTESIAN_POINT('Ctrl Pts',(0.00255219070088582,-0.0341934961088741,
0.0727231606620577));
#101456=CARTESIAN_POINT('Ctrl Pts',(0.00258635947489357,-0.0340223579322365,
0.0726013794525524));
#101457=CARTESIAN_POINT('Ctrl Pts',(0.00260771899121465,-0.0339125849573551,
0.0725250039510641));
#101458=CARTESIAN_POINT('Ctrl Pts',(0.00263064429385958,-0.0338030433565216,
0.0724491242101115));
#101459=CARTESIAN_POINT('Ctrl Pts',(0.00265509746327339,-0.033693872113232,
0.0723738346682113));
#101460=CARTESIAN_POINT('Ctrl Pts',(0.00248643900227624,-0.0340223579322365,
0.0726548311034371));
#101461=CARTESIAN_POINT('Ctrl Pts',(0.00250706128092387,-0.0339125849573551,
0.0725770774380279));
#101462=CARTESIAN_POINT('Ctrl Pts',(0.00252927838873448,-0.0338030433565216,
0.0724998052424675));
#101463=CARTESIAN_POINT('Ctrl Pts',(0.00255305315396205,-0.033693872113232,
0.0724231108162704));
#101464=CARTESIAN_POINT('Ctrl Pts',(0.00238651852965892,-0.0340223579322365,
0.0727082827543218));
#101465=CARTESIAN_POINT('Ctrl Pts',(0.0024064035706331,-0.0339125849573551,
0.0726291509249917));
#101466=CARTESIAN_POINT('Ctrl Pts',(0.00242791248360938,-0.0338030433565216,
0.0725504862748235));
#101467=CARTESIAN_POINT('Ctrl Pts',(0.0024510088446507,-0.033693872113232,
0.0724723869643295));
#101468=CARTESIAN_POINT('Ctrl Pts',(0.00228659805704159,-0.0340223579322365,
0.0727617344052066));
#101469=CARTESIAN_POINT('Ctrl Pts',(0.00230574586034232,-0.0339125849573551,
0.0726812244119555));
#101470=CARTESIAN_POINT('Ctrl Pts',(0.00232654657848428,-0.0338030433565216,
0.0726011673071795));
#101471=CARTESIAN_POINT('Ctrl Pts',(0.00234896453533936,-0.033693872113232,
0.0725216631123886));
#101472=CARTESIAN_POINT('Origin',(0.0188274512928389,-0.0345589643414767,
0.0763691508835896));
#101473=CARTESIAN_POINT('Ctrl Pts',(0.0024541639731875,-0.034193496108874,
0.0721864753018193));
#101474=CARTESIAN_POINT('Ctrl Pts',(0.00248123981602225,-0.0340836138581107,
0.0721082946239812));
#101475=CARTESIAN_POINT('Ctrl Pts',(0.00250992045244113,-0.0339738896643499,
0.0720307117364567));
#101476=CARTESIAN_POINT('Ctrl Pts',(0.00254016251843922,-0.0338644633294062,
0.0719538234750659));
#101477=CARTESIAN_POINT('Ctrl Pts',(0.00250975025667077,-0.034193496108874,
0.0722852240959154));
#101478=CARTESIAN_POINT('Ctrl Pts',(0.00253546441211166,-0.0340836138581107,
0.0722078099200096));
#101479=CARTESIAN_POINT('Ctrl Pts',(0.00256276815335073,-0.0339738896643499,
0.072130964989372));
#101480=CARTESIAN_POINT('Ctrl Pts',(0.0025916199419529,-0.0338644633294062,
0.0720547853134616));
#101481=CARTESIAN_POINT('Ctrl Pts',(0.00256533654015405,-0.034193496108874,
0.0723839728900115));
#101482=CARTESIAN_POINT('Ctrl Pts',(0.00258968900820107,-0.0340836138581107,
0.0723073252160381));
#101483=CARTESIAN_POINT('Ctrl Pts',(0.00261561585426032,-0.0339738896643499,
0.0722312182422874));
#101484=CARTESIAN_POINT('Ctrl Pts',(0.00264307736546658,-0.0338644633294062,
0.0721557471518574));
#101485=CARTESIAN_POINT('Ctrl Pts',(0.00262092282363733,-0.034193496108874,
0.0724827216841076));
#101486=CARTESIAN_POINT('Ctrl Pts',(0.00264391360429047,-0.0340836138581107,
0.0724068405120665));
#101487=CARTESIAN_POINT('Ctrl Pts',(0.00266846355516991,-0.03397388966435,
0.0723314714952027));
#101488=CARTESIAN_POINT('Ctrl Pts',(0.00269453478898026,-0.0338644633294063,
0.0722567089902531));
#101489=CARTESIAN_POINT('Origin',(0.0187750088091898,-0.0345610621861796,
0.076847481101678));
#101490=CARTESIAN_POINT('Ctrl Pts',(0.00260953816902741,-0.0342436276873901,
0.0725156078062815));
#101491=CARTESIAN_POINT('Ctrl Pts',(0.00267118028679546,-0.0339430054201861,
0.0723076346644367));
#101492=CARTESIAN_POINT('Ctrl Pts',(0.00274831267495602,-0.0336441434784164,
0.072104895489366));
#101493=CARTESIAN_POINT('Ctrl Pts',(0.0025437206944058,-0.0342436276873901,
0.0727567883611246));
#101494=CARTESIAN_POINT('Ctrl Pts',(0.00259626653759414,-0.0339430054201861,
0.0725463328723026));
#101495=CARTESIAN_POINT('Ctrl Pts',(0.00266451547328288,-0.0336441434784164,
0.0723404332336699));
#101496=CARTESIAN_POINT('Ctrl Pts',(0.00269452577742099,-0.0335235895815127,
0.0722567352165666));
#101497=CARTESIAN_POINT('Ctrl Pts',(0.00272059029465993,-0.0334144449262719,
0.0721819908127834));
#101498=CARTESIAN_POINT('Ctrl Pts',(0.00274822892000209,-0.0333049234473133,
0.0721076990100463));
#101499=CARTESIAN_POINT('Ctrl Pts',(0.00277741491731665,-0.0331951640388588,
0.0720339580061314));
#101500=CARTESIAN_POINT('Ctrl Pts',(0.00259144622611276,-0.0335235895815127,
0.0723038072739723));
#101501=CARTESIAN_POINT('Ctrl Pts',(0.00261686270380516,-0.0334144449262719,
0.0722276437772204));
#101502=CARTESIAN_POINT('Ctrl Pts',(0.0026438818624746,-0.0333049234473133,
0.0721519178631394));
#101503=CARTESIAN_POINT('Ctrl Pts',(0.00267247792421042,-0.0331951640388588,
0.0720767294915409));
#101504=CARTESIAN_POINT('Ctrl Pts',(0.00248836667480452,-0.0335235895815127,
0.072350879331378));
#101505=CARTESIAN_POINT('Ctrl Pts',(0.00251313511295039,-0.0334144449262719,
0.0722732967416574));
#101506=CARTESIAN_POINT('Ctrl Pts',(0.00253953480494712,-0.0333049234473133,
0.0721961367162324));
#101507=CARTESIAN_POINT('Ctrl Pts',(0.00256754093110419,-0.0331951640388588,
0.0721195009769504));
#101508=CARTESIAN_POINT('Ctrl Pts',(0.00238528712349628,-0.0335235895815127,
0.0723979513887837));
#101509=CARTESIAN_POINT('Ctrl Pts',(0.00240940752209562,-0.0334144449262719,
0.0723189497060944));
#101510=CARTESIAN_POINT('Ctrl Pts',(0.00243518774741963,-0.0333049234473133,
0.0722403555693255));
#101511=CARTESIAN_POINT('Ctrl Pts',(0.00246260393799796,-0.0331951640388588,
0.0721622724623599));
#101512=CARTESIAN_POINT('Origin',(0.0179785025681745,-0.0326434571770922,
0.0788689982621595));
#101513=CARTESIAN_POINT('Ctrl Pts',(0.00258776072717685,-0.0336938721132386,
0.0718325257577917));
#101514=CARTESIAN_POINT('Ctrl Pts',(0.00260132567293593,-0.0336474569764956,
0.0718001215871051));
#101515=CARTESIAN_POINT('Ctrl Pts',(0.00261526902094752,-0.033601104548885,
0.0717678784315901));
#101516=CARTESIAN_POINT('Ctrl Pts',(0.00265057036926952,-0.0334837508694606,
0.0716862461820837));
#101517=CARTESIAN_POINT('Ctrl Pts',(0.00268827514843814,-0.0333660264863597,
0.0716056958314907));
#101518=CARTESIAN_POINT('Ctrl Pts',(0.00273558880092054,-0.0336938721132386,
0.0721386579186066));
#101519=CARTESIAN_POINT('Ctrl Pts',(0.00274736185355695,-0.0336474569764956,
0.0721071190346901));
#101520=CARTESIAN_POINT('Ctrl Pts',(0.00275950330195339,-0.033601104548885,
0.0720757201302838));
#101521=CARTESIAN_POINT('Ctrl Pts',(0.00279024265512883,-0.0334837508694606,
0.0719962253302936));
#101522=CARTESIAN_POINT('Ctrl Pts',(0.00282332410538725,-0.0333660264863597,
0.0719176763092435));
#101523=CARTESIAN_POINT('Ctrl Pts',(0.00273558880093204,-0.0336938721132426,
0.0721386579186126));
#101524=CARTESIAN_POINT('Ctrl Pts',(0.00274736185356772,-0.0336474569765026,
0.0721071190346981));
#101525=CARTESIAN_POINT('Ctrl Pts',(0.00275950330196339,-0.0336011045488949,
0.0720757201302938));
#101526=CARTESIAN_POINT('Ctrl Pts',(0.00278998663819216,-0.033484728265791,
0.07199688741372));
#101527=CARTESIAN_POINT('Ctrl Pts',(0.00282277333995648,-0.0333679870047996,
0.0719189845050616));
#101528=CARTESIAN_POINT('Ctrl Pts',(0.00273558880091956,-0.0336938721132425,
0.0721386579186092));
#101529=CARTESIAN_POINT('Ctrl Pts',(0.00277769444724139,-0.0335278710435082,
0.0720258609123792));
#101530=CARTESIAN_POINT('Ctrl Pts',(0.00282332256568321,-0.033362046922432,
0.0719144240099955));
#101531=CARTESIAN_POINT('Ctrl Pts',(0.0028725143840075,-0.0331951640388602,
0.071804299380334));
#101532=CARTESIAN_POINT('Ctrl Pts',(0.00270798484678257,-0.0336938721132425,
0.0722178163138638));
#101533=CARTESIAN_POINT('Ctrl Pts',(0.00274843338294655,-0.0335278710435082,
0.0721044414435594));
#101534=CARTESIAN_POINT('Ctrl Pts',(0.00279242309586514,-0.033362046922432,
0.071992374913849));
#101535=CARTESIAN_POINT('Ctrl Pts',(0.00283999450320525,-0.0331951640388602,
0.0718815683079562));
#101536=CARTESIAN_POINT('Ctrl Pts',(0.00268038089264557,-0.0336938721132425,
0.0722969747091183));
#101537=CARTESIAN_POINT('Ctrl Pts',(0.0027191723186517,-0.0335278710435082,
0.0721830219747397));
#101538=CARTESIAN_POINT('Ctrl Pts',(0.00276152362604707,-0.033362046922432,
0.0720703258177025));
#101539=CARTESIAN_POINT('Ctrl Pts',(0.00280747462240301,-0.0331951640388602,
0.0719588372355784));
#101540=CARTESIAN_POINT('Ctrl Pts',(0.00265277693850858,-0.0336938721132425,
0.0723761331043729));
#101541=CARTESIAN_POINT('Ctrl Pts',(0.00268991125435685,-0.0335278710435082,
0.07226160250592));
#101542=CARTESIAN_POINT('Ctrl Pts',(0.002730624156229,-0.033362046922432,
0.0721482767215559));
#101543=CARTESIAN_POINT('Ctrl Pts',(0.00277495474160076,-0.0331951640388602,
0.0720361061632006));
#101544=CARTESIAN_POINT('Ctrl Pts',(0.00282411744560475,-0.0330240426238155,
0.0719195663327465));
#101545=CARTESIAN_POINT('Ctrl Pts',(0.00285484384237725,-0.0329142774063509,
0.0718465582876369));
#101546=CARTESIAN_POINT('Ctrl Pts',(0.00288709483760948,-0.0328043479726686,
0.0717741490458054));
#101547=CARTESIAN_POINT('Ctrl Pts',(0.00292083167001347,-0.0326943950436594,
0.0717024325067168));
#101548=CARTESIAN_POINT('Ctrl Pts',(0.00271828577620953,-0.0330240426238155,
0.0719600730450006));
#101549=CARTESIAN_POINT('Ctrl Pts',(0.00274845415355695,-0.0329142774063509,
0.0718856070655383));
#101550=CARTESIAN_POINT('Ctrl Pts',(0.00278017699074669,-0.0328043479726686,
0.0718117276267003));
#101551=CARTESIAN_POINT('Ctrl Pts',(0.00281341625496992,-0.0326943950436594,
0.0717385304927498));
#101552=CARTESIAN_POINT('Ctrl Pts',(0.00261245410681431,-0.0330240426238155,
0.0720005797572547));
#101553=CARTESIAN_POINT('Ctrl Pts',(0.00264206446473666,-0.0329142774063509,
0.0719246558434397));
#101554=CARTESIAN_POINT('Ctrl Pts',(0.00267325914388389,-0.0328043479726686,
0.0718493062075953));
#101555=CARTESIAN_POINT('Ctrl Pts',(0.00270600083992636,-0.0326943950436594,
0.0717746284787828));
#101556=CARTESIAN_POINT('Ctrl Pts',(0.00250662243741909,-0.0330240426238155,
0.0720410864695089));
#101557=CARTESIAN_POINT('Ctrl Pts',(0.00253567477591636,-0.0329142774063509,
0.0719637046213411));
#101558=CARTESIAN_POINT('Ctrl Pts',(0.0025663412970211,-0.0328043479726686,
0.0718868847884903));
#101559=CARTESIAN_POINT('Ctrl Pts',(0.00259858542488281,-0.0326943950436594,
0.0718107264648157));
#101560=CARTESIAN_POINT('Origin',(0.0180912134173041,-0.0326396682855438,
0.0789199066430371));
#101561=CARTESIAN_POINT('Ctrl Pts',(0.00274496550589082,-0.0331951640388587,
0.0714913666959631));
#101562=CARTESIAN_POINT('Ctrl Pts',(0.00278158280128254,-0.0330855618255041,
0.0714172843773542));
#101563=CARTESIAN_POINT('Ctrl Pts',(0.00281975764846336,-0.0329757224427708,
0.0713439054707414));
#101564=CARTESIAN_POINT('Ctrl Pts',(0.00285944577148284,-0.0328657862078596,
0.0712713263401401));
#101565=CARTESIAN_POINT('Ctrl Pts',(0.00278773695724827,-0.0331951640388587,
0.0715963036055249));
#101566=CARTESIAN_POINT('Ctrl Pts',(0.00282290895899642,-0.0330855618255041,
0.0715228103771325));
#101567=CARTESIAN_POINT('Ctrl Pts',(0.00285962529515387,-0.0329757224427708,
0.071449991113654));
#101568=CARTESIAN_POINT('Ctrl Pts',(0.00289784352232761,-0.0328657862078596,
0.0713779413708331));
#101569=CARTESIAN_POINT('Ctrl Pts',(0.00283050840860572,-0.0331951640388587,
0.0717012405150867));
#101570=CARTESIAN_POINT('Ctrl Pts',(0.0028642351167103,-0.0330855618255041,
0.0716283363769108));
#101571=CARTESIAN_POINT('Ctrl Pts',(0.00289949294184438,-0.0329757224427708,
0.0715560767565666));
#101572=CARTESIAN_POINT('Ctrl Pts',(0.00293624127317238,-0.0328657862078596,
0.0714845564015261));
#101573=CARTESIAN_POINT('Ctrl Pts',(0.00287327985996318,-0.0331951640388587,
0.0718061774246485));
#101574=CARTESIAN_POINT('Ctrl Pts',(0.00290556127442418,-0.0330855618255041,
0.0717338623766891));
#101575=CARTESIAN_POINT('Ctrl Pts',(0.00293936058853489,-0.0329757224427708,
0.0716621623994793));
#101576=CARTESIAN_POINT('Ctrl Pts',(0.00297463902401715,-0.0328657862078596,
0.0715911714322191));
#101577=CARTESIAN_POINT('Origin',(0.0178495159115153,-0.0326401908833634,
0.079335665211352));
#101578=CARTESIAN_POINT('Ctrl Pts',(0.00285789242902623,-0.0332451089994433,
0.0718373110904111));
#101579=CARTESIAN_POINT('Ctrl Pts',(0.00294511691831862,-0.0329451141710259,
0.07163870480859));
#101580=CARTESIAN_POINT('Ctrl Pts',(0.00304705344909823,-0.0326442513127503,
0.0714472328513648));
#101581=CARTESIAN_POINT('Ctrl Pts',(0.00276236309499031,-0.0332451089994433,
0.0720683395439372));
#101582=CARTESIAN_POINT('Ctrl Pts',(0.00284087420359961,-0.0329451141710259,
0.0718661303143357));
#101583=CARTESIAN_POINT('Ctrl Pts',(0.00293439349624683,-0.0326442513127503,
0.0716704093174707));
#101584=CARTESIAN_POINT('Ctrl Pts',(0.00297462488656823,-0.0325229783203385,
0.0715911996795726));
#101585=CARTESIAN_POINT('Ctrl Pts',(0.00300989789238602,-0.0324130253112079,
0.0715202186599985));
#101586=CARTESIAN_POINT('Ctrl Pts',(0.00304663388190617,-0.0323031222247694,
0.0714499780735101));
#101587=CARTESIAN_POINT('Ctrl Pts',(0.00308478262408177,-0.0321934096636184,
0.0713805662328438));
#101588=CARTESIAN_POINT('Ctrl Pts',(0.00286645859163048,-0.0325229783203385,
0.0716249812616677));
#101589=CARTESIAN_POINT('Ctrl Pts',(0.00290126591908632,-0.0324130253112079,
0.0715525091721105));
#101590=CARTESIAN_POINT('Ctrl Pts',(0.00293756714557121,-0.0323031222247694,
0.071480768108634));
#101591=CARTESIAN_POINT('Ctrl Pts',(0.00297531252911759,-0.0321934096636184,
0.0714098483256301));
#101592=CARTESIAN_POINT('Ctrl Pts',(0.00275829229669273,-0.0325229783203385,
0.0716587628437628));
#101593=CARTESIAN_POINT('Ctrl Pts',(0.00279263394578661,-0.0324130253112079,
0.0715847996842225));
#101594=CARTESIAN_POINT('Ctrl Pts',(0.00282850040923626,-0.0323031222247694,
0.0715115581437579));
#101595=CARTESIAN_POINT('Ctrl Pts',(0.0028658424341534,-0.0321934096636184,
0.0714391304184163));
#101596=CARTESIAN_POINT('Ctrl Pts',(0.00265012600175497,-0.0325229783203385,
0.0716925444258579));
#101597=CARTESIAN_POINT('Ctrl Pts',(0.00268400197248691,-0.0324130253112079,
0.0716170901963345));
#101598=CARTESIAN_POINT('Ctrl Pts',(0.00271943367290131,-0.0323031222247694,
0.0715423481788817));
#101599=CARTESIAN_POINT('Ctrl Pts',(0.00275637233918922,-0.0321934096636184,
0.0714684125112026));
#101600=CARTESIAN_POINT('Origin',(0.0180836286971742,-0.0326393375175912,
0.0789160126669681));
#101601=CARTESIAN_POINT('Ctrl Pts',(0.0029225163383477,-0.0326943950436593,
0.0711588742072384));
#101602=CARTESIAN_POINT('Ctrl Pts',(0.00296373965773903,-0.0325844576448127,
0.0710871910155488));
#101603=CARTESIAN_POINT('Ctrl Pts',(0.00300644842049906,-0.0324744968375319,
0.07101635531656));
#101604=CARTESIAN_POINT('Ctrl Pts',(0.00305058665383319,-0.0323646534831894,
0.070946457114334));
#101605=CARTESIAN_POINT('Ctrl Pts',(0.00295861431256972,-0.0326943950436593,
0.0712662895871365));
#101606=CARTESIAN_POINT('Ctrl Pts',(0.00299835724670818,-0.0325844576448127,
0.0711951038931866));
#101607=CARTESIAN_POINT('Ctrl Pts',(0.00303957523037726,-0.0324744968375319,
0.0711247351103519));
#101608=CARTESIAN_POINT('Ctrl Pts',(0.003082214209107,-0.0323646534831894,
0.0710552726708));
#101609=CARTESIAN_POINT('Ctrl Pts',(0.00299471228679173,-0.0326943950436593,
0.0713737049670347));
#101610=CARTESIAN_POINT('Ctrl Pts',(0.00303297483567733,-0.0325844576448127,
0.0713030167708243));
#101611=CARTESIAN_POINT('Ctrl Pts',(0.00307270204025546,-0.0324744968375319,
0.0712331149041438));
#101612=CARTESIAN_POINT('Ctrl Pts',(0.00311384176438082,-0.0323646534831894,
0.0711640882272659));
#101613=CARTESIAN_POINT('Ctrl Pts',(0.00303081026101375,-0.0326943950436593,
0.0714811203469328));
#101614=CARTESIAN_POINT('Ctrl Pts',(0.00306759242464647,-0.0325844576448127,
0.0714109296484621));
#101615=CARTESIAN_POINT('Ctrl Pts',(0.00310582885013366,-0.0324744968375319,
0.0713414946979357));
#101616=CARTESIAN_POINT('Ctrl Pts',(0.00314546931965463,-0.0323646534831894,
0.0712729037837319));
#101617=CARTESIAN_POINT('Origin',(0.0178831202510714,-0.0326395579068478,
0.0793530637798792));
#101618=CARTESIAN_POINT('Ctrl Pts',(0.00301348040185345,-0.0327445246961877,
0.0715112615509875));
#101619=CARTESIAN_POINT('Ctrl Pts',(0.00311300204837979,-0.0324436878365475,
0.0713185233700955));
#101620=CARTESIAN_POINT('Ctrl Pts',(0.00322675879178978,-0.0321434074463186,
0.0711338291150967));
#101621=CARTESIAN_POINT('Ctrl Pts',(0.0029036347080761,-0.0327445246961877,
0.0717358365352546));
#101622=CARTESIAN_POINT('Ctrl Pts',(0.00299468637069356,-0.0324436878365475,
0.0715389554563378));
#101623=CARTESIAN_POINT('Ctrl Pts',(0.00310030925253212,-0.0321434074463186,
0.0713494920790509));
#101624=CARTESIAN_POINT('Ctrl Pts',(0.00319212753136846,-0.0322357242816072,
0.0711907927924291));
#101625=CARTESIAN_POINT('Ctrl Pts',(0.00328637444297842,-0.0319819883628705,
0.0710337259875744));
#101626=CARTESIAN_POINT('Ctrl Pts',(0.00339042496164847,-0.0317295851069887,
0.0708829746986919));
#101627=CARTESIAN_POINT('Ctrl Pts',(0.00306818622113084,-0.0322357242816072,
0.0714079069366403));
#101628=CARTESIAN_POINT('Ctrl Pts',(0.00315551832883441,-0.0319819883628705,
0.0712468927618007));
#101629=CARTESIAN_POINT('Ctrl Pts',(0.00325291923975078,-0.0317295851069887,
0.0710917620940142));
#101630=CARTESIAN_POINT('Origin',(0.0177998388959256,-0.0326371942644636,
0.0793067321555741));
#101631=CARTESIAN_POINT('Origin',(0.0179742057822713,-0.0326352985531313,
0.078860421044255));
#101632=CARTESIAN_POINT('Ctrl Pts',(0.00312059419090078,-0.0321934096636183,
0.0708381863255016));
#101633=CARTESIAN_POINT('Ctrl Pts',(0.00316626668254265,-0.0320835708272303,
0.0707691884637037));
#101634=CARTESIAN_POINT('Ctrl Pts',(0.00321334058944697,-0.0319739230346346,
0.0707011758133103));
#101635=CARTESIAN_POINT('Ctrl Pts',(0.00326174900546822,-0.0318646057455576,
0.0706342307694738));
#101636=CARTESIAN_POINT('Ctrl Pts',(0.00314987630890223,-0.0321934096636183,
0.0709476565147319));
#101637=CARTESIAN_POINT('Ctrl Pts',(0.00319403912131875,-0.0320835708272303,
0.0708790624761623));
#101638=CARTESIAN_POINT('Ctrl Pts',(0.00323959586757229,-0.0319739230346346,
0.0708114221720302));
#101639=CARTESIAN_POINT('Ctrl Pts',(0.00328648161918083,-0.0318646057455576,
0.070744817670071));
#101640=CARTESIAN_POINT('Ctrl Pts',(0.00317915842690369,-0.0321934096636183,
0.0710571267039621));
#101641=CARTESIAN_POINT('Ctrl Pts',(0.00322181156009484,-0.0320835708272303,
0.0709889364886208));
#101642=CARTESIAN_POINT('Ctrl Pts',(0.0032658511456976,-0.0319739230346346,
0.0709216685307502));
#101643=CARTESIAN_POINT('Ctrl Pts',(0.00331121423289344,-0.0318646057455576,
0.0708554045706683));
#101644=CARTESIAN_POINT('Ctrl Pts',(0.00320844054490514,-0.0321934096636183,
0.0711665968931924));
#101645=CARTESIAN_POINT('Ctrl Pts',(0.00324958399887094,-0.0320835708272303,
0.0710988105010794));
#101646=CARTESIAN_POINT('Ctrl Pts',(0.00329210642382292,-0.0319739230346346,
0.0710319148894701));
#101647=CARTESIAN_POINT('Ctrl Pts',(0.00333594684660605,-0.0318646057455575,
0.0709659914712655));
#101648=CARTESIAN_POINT('Ctrl Pts',(0.00314451787502327,-0.0320218834582391,
0.071272896482392));
#101649=CARTESIAN_POINT('Ctrl Pts',(0.00317446156728867,-0.0319391099350681,
0.0712210743781347));
#101650=CARTESIAN_POINT('Ctrl Pts',(0.003205196326856,-0.0318564869454955,
0.071169751246527));
#101651=CARTESIAN_POINT('Ctrl Pts',(0.00323669627765198,-0.0317740741446541,
0.0711189623797559));
#101652=CARTESIAN_POINT('Ctrl Pts',(0.00309637002544079,-0.0320218834582391,
0.0712846698688123));
#101653=CARTESIAN_POINT('Ctrl Pts',(0.00312619118521553,-0.0319391099350681,
0.0712323466618374));
#101654=CARTESIAN_POINT('Ctrl Pts',(0.00315681131132073,-0.0318564869454955,
0.0711805208177556));
#101655=CARTESIAN_POINT('Ctrl Pts',(0.00318820457699485,-0.0317740741446541,
0.0711292280027081));
#101656=CARTESIAN_POINT('Ctrl Pts',(0.00304822217585832,-0.0320218834582391,
0.0712964432552326));
#101657=CARTESIAN_POINT('Ctrl Pts',(0.0030779208031424,-0.0319391099350681,
0.0712436189455402));
#101658=CARTESIAN_POINT('Ctrl Pts',(0.00310842629578546,-0.0318564869454955,
0.0711912903889843));
#101659=CARTESIAN_POINT('Ctrl Pts',(0.00313971287633772,-0.0317740741446541,
0.0711394936256603));
#101660=CARTESIAN_POINT('Ctrl Pts',(0.00300007432627584,-0.0320218834582391,
0.0713082166416528));
#101661=CARTESIAN_POINT('Ctrl Pts',(0.00302965042106927,-0.0319391099350681,
0.071254891229243));
#101662=CARTESIAN_POINT('Ctrl Pts',(0.00306004128025019,-0.0318564869454955,
0.071202059960213));
#101663=CARTESIAN_POINT('Ctrl Pts',(0.00309122117568059,-0.0317740741446541,
0.0711497592486124));
#101664=CARTESIAN_POINT('Origin',(-0.00277341874484063,-0.0391228853390644,
0.068941196869976));
#101665=CARTESIAN_POINT('Ctrl Pts',(0.00237219534002025,-0.0352722978779633,
0.0742084227180186));
#101666=CARTESIAN_POINT('Ctrl Pts',(0.00237235354850088,-0.0352466642097243,
0.0741895264843159));
#101667=CARTESIAN_POINT('Ctrl Pts',(0.0023724332177902,-0.0352210183808314,
0.074170646428595));
#101668=CARTESIAN_POINT('Ctrl Pts',(0.00237243381818375,-0.0351953608940152,
0.074151781882352));
#101669=CARTESIAN_POINT('Origin',(-0.00252274043965582,-0.0352456003065124,
0.0739862810774749));
#101670=CARTESIAN_POINT('Ctrl Pts',(0.00237520119150846,-0.0350241211493339,
0.0740271317437118));
#101671=CARTESIAN_POINT('Ctrl Pts',(0.00237689365128457,-0.0349144232867421,
0.0739479474009952));
#101672=CARTESIAN_POINT('Ctrl Pts',(0.00238022392095156,-0.0348045283677512,
0.0738687506469863));
#101673=CARTESIAN_POINT('Ctrl Pts',(0.00238519150971162,-0.0346945769586886,
0.0737896430813891));
#101674=CARTESIAN_POINT('Ctrl Pts',(0.00229171288836954,-0.0350241211493339,
0.0741037531835444));
#101675=CARTESIAN_POINT('Ctrl Pts',(0.00229234991927556,-0.0349144232867421,
0.0740234188237355));
#101676=CARTESIAN_POINT('Ctrl Pts',(0.00229464790002142,-0.0348045283677512,
0.0739430495478256));
#101677=CARTESIAN_POINT('Ctrl Pts',(0.00229860771792751,-0.0346945769586886,
0.0738627484081671));
#101678=CARTESIAN_POINT('Ctrl Pts',(0.00220822458523062,-0.0350241211493339,
0.074180374623377));
#101679=CARTESIAN_POINT('Ctrl Pts',(0.00220780618726655,-0.0349144232867421,
0.0740988902464757));
#101680=CARTESIAN_POINT('Ctrl Pts',(0.00220907187909128,-0.0348045283677512,
0.0740173484486649));
#101681=CARTESIAN_POINT('Ctrl Pts',(0.0022120239261434,-0.0346945769586886,
0.0739358537349451));
#101682=CARTESIAN_POINT('Ctrl Pts',(0.0021247362820917,-0.0350241211493339,
0.0742569960632096));
#101683=CARTESIAN_POINT('Ctrl Pts',(0.00212326245525754,-0.0349144232867421,
0.074174361669216));
#101684=CARTESIAN_POINT('Ctrl Pts',(0.00212349585816114,-0.0348045283677512,
0.0740916473495043));
#101685=CARTESIAN_POINT('Ctrl Pts',(0.00212544013435929,-0.0346945769586886,
0.0740089590617232));
#101686=CARTESIAN_POINT('Origin',(0.0191287125947155,-0.0345629067942066,
0.0750214915916345));
#101687=CARTESIAN_POINT('Ctrl Pts',(0.00220802251022496,-0.0351970973651537,
0.073726550886685));
#101688=CARTESIAN_POINT('Ctrl Pts',(0.00221388882378741,-0.0350869349326839,
0.073644596053935));
#101689=CARTESIAN_POINT('Ctrl Pts',(0.00222146379248379,-0.0349764985139959,
0.073562695288163));
#101690=CARTESIAN_POINT('Ctrl Pts',(0.00223074384867184,-0.0348659306865055,
0.0734809552719012));
#101691=CARTESIAN_POINT('Ctrl Pts',(0.00226492113074422,-0.0351970973651537,
0.0737859059002311));
#101692=CARTESIAN_POINT('Ctrl Pts',(0.00226996516103811,-0.0350869349326839,
0.0737047393207534));
#101693=CARTESIAN_POINT('Ctrl Pts',(0.00227670077794741,-0.0349764985139959,
0.0736236103664203));
#101694=CARTESIAN_POINT('Ctrl Pts',(0.00228512544237453,-0.0348659306865055,
0.0735426246558483));
#101695=CARTESIAN_POINT('Ctrl Pts',(0.00232181975126347,-0.0351970973651537,
0.0738452609137773));
#101696=CARTESIAN_POINT('Ctrl Pts',(0.0023260414982888,-0.0350869349326839,
0.0737648825875719));
#101697=CARTESIAN_POINT('Ctrl Pts',(0.00233193776341103,-0.0349764985139959,
0.0736845254446775));
#101698=CARTESIAN_POINT('Ctrl Pts',(0.00233950703607721,-0.0348659306865055,
0.0736042940397953));
#101699=CARTESIAN_POINT('Ctrl Pts',(0.00237871837178273,-0.0351970973651537,
0.0739046159273234));
#101700=CARTESIAN_POINT('Ctrl Pts',(0.0023821178355395,-0.0350869349326839,
0.0738250258543903));
#101701=CARTESIAN_POINT('Ctrl Pts',(0.00238717474887465,-0.0349764985139959,
0.0737454405229347));
#101702=CARTESIAN_POINT('Ctrl Pts',(0.0023938886297799,-0.0348659306865055,
0.0736659634237424));
#101703=CARTESIAN_POINT('Origin',(0.0190455869393428,-0.0345637187965369,
0.0754952167037528));
#101704=CARTESIAN_POINT('Ctrl Pts',(0.00237632436497943,-0.0352450361861252,
0.0739382135181846));
#101705=CARTESIAN_POINT('Ctrl Pts',(0.00238431202300694,-0.0349452761023764,
0.0737214445947614));
#101706=CARTESIAN_POINT('Ctrl Pts',(0.00240860491077934,-0.0346444289983475,
0.0735058931520697));
#101707=CARTESIAN_POINT('Ctrl Pts',(0.00237255042040183,-0.0352450361861252,
0.0741881850312462));
#101708=CARTESIAN_POINT('Ctrl Pts',(0.00237111024835331,-0.0349452761023764,
0.0739712737711714));
#101709=CARTESIAN_POINT('Ctrl Pts',(0.00238601281089983,-0.0346444289983475,
0.0737548702534727));
#101710=CARTESIAN_POINT('Ctrl Pts',(0.00239425952886891,-0.0345231616327822,
0.0736664187731089));
#101711=CARTESIAN_POINT('Ctrl Pts',(0.00240092501525366,-0.0344132092796975,
0.0735874453697055));
#101712=CARTESIAN_POINT('Ctrl Pts',(0.00240922366028598,-0.0343032738558973,
0.0735086139112949));
#101713=CARTESIAN_POINT('Ctrl Pts',(0.00241914224548923,-0.034193496108874,
0.0734300251177555));
#101714=CARTESIAN_POINT('Ctrl Pts',(0.00230612490165591,-0.0345231616327822,
0.0737376467425067));
#101715=CARTESIAN_POINT('Ctrl Pts',(0.00231180861076347,-0.0344132092796975,
0.0736574585273509));
#101716=CARTESIAN_POINT('Ctrl Pts',(0.00231915065659668,-0.0343032738558973,
0.0735773920125779));
#101717=CARTESIAN_POINT('Ctrl Pts',(0.00232813900566308,-0.034193496108874,
0.0734975495317082));
#101718=CARTESIAN_POINT('Ctrl Pts',(0.00221799027444291,-0.0345231616327822,
0.0738088747119046));
#101719=CARTESIAN_POINT('Ctrl Pts',(0.00222269220627329,-0.0344132092796975,
0.0737274716849962));
#101720=CARTESIAN_POINT('Ctrl Pts',(0.00222907765290738,-0.0343032738558973,
0.0736461701138609));
#101721=CARTESIAN_POINT('Ctrl Pts',(0.00223713576583693,-0.034193496108874,
0.0735650739456609));
#101722=CARTESIAN_POINT('Ctrl Pts',(0.00212985564722991,-0.0345231616327822,
0.0738801026813024));
#101723=CARTESIAN_POINT('Ctrl Pts',(0.00213357580178311,-0.0344132092796975,
0.0737974848426416));
#101724=CARTESIAN_POINT('Ctrl Pts',(0.00213900464921807,-0.0343032738558973,
0.0737149482151439));
#101725=CARTESIAN_POINT('Ctrl Pts',(0.00214613252601077,-0.034193496108874,
0.0736325983596136));
#101726=CARTESIAN_POINT('Origin',(0.0191407956598087,-0.0345625596230709,
0.0750221971657493));
#101727=CARTESIAN_POINT('Ctrl Pts',(0.00218666066001417,-0.0346945769586885,
0.0732836352377339));
#101728=CARTESIAN_POINT('Ctrl Pts',(0.00219859960434057,-0.0345846629176052,
0.0732018187021015));
#101729=CARTESIAN_POINT('Ctrl Pts',(0.00221223252022474,-0.0344746925050311,
0.0731202350844692));
#101730=CARTESIAN_POINT('Ctrl Pts',(0.002227541507892,-0.0343648066253259,
0.0730389888470288));
#101731=CARTESIAN_POINT('Ctrl Pts',(0.00225976592923148,-0.0346945769586885,
0.0733702189613448));
#101732=CARTESIAN_POINT('Ctrl Pts',(0.00227051170608294,-0.0345846629176052,
0.0732894098532731));
#101733=CARTESIAN_POINT('Ctrl Pts',(0.00228293041750801,-0.0344746925050311,
0.0732088091610593));
#101734=CARTESIAN_POINT('Ctrl Pts',(0.00229700572471198,-0.0343648066253259,
0.0731285200938829));
#101735=CARTESIAN_POINT('Ctrl Pts',(0.00233287119844878,-0.0346945769586885,
0.0734568026849557));
#101736=CARTESIAN_POINT('Ctrl Pts',(0.00234242380782531,-0.0345846629176052,
0.0733770010044447));
#101737=CARTESIAN_POINT('Ctrl Pts',(0.00235362831479128,-0.0344746925050311,
0.0732973832376494));
#101738=CARTESIAN_POINT('Ctrl Pts',(0.00236646994153196,-0.0343648066253259,
0.073218051340737));
#101739=CARTESIAN_POINT('Ctrl Pts',(0.00240597646766608,-0.0346945769586885,
0.0735433864085666));
#101740=CARTESIAN_POINT('Ctrl Pts',(0.00241433590956768,-0.0345846629176052,
0.0734645921556163));
#101741=CARTESIAN_POINT('Ctrl Pts',(0.00242432621207455,-0.0344746925050311,
0.0733859573142394));
#101742=CARTESIAN_POINT('Ctrl Pts',(0.00243593415835193,-0.0343648066253259,
0.0733075825875911));
#101743=CARTESIAN_POINT('Origin',(0.0191036692995611,-0.0345626446731572,
0.0755015861686337));
#101744=CARTESIAN_POINT('Ctrl Pts',(0.0024046683692595,-0.0346945769586885,
0.0735418371354142));
#101745=CARTESIAN_POINT('Ctrl Pts',(0.00241740658395317,-0.034527515336289,
0.0734220480065674));
#101746=CARTESIAN_POINT('Ctrl Pts',(0.00243391535124547,-0.0343603235965158,
0.0733026284992435));
#101747=CARTESIAN_POINT('Ctrl Pts',(0.00245414059620935,-0.0341934961088739,
0.0731839310776591));
#101748=CARTESIAN_POINT('Ctrl Pts',(0.00239761753723417,-0.0346945769586885,
0.0736253734394922));
#101749=CARTESIAN_POINT('Ctrl Pts',(0.00240860605059284,-0.034527515336289,
0.0735054366281457));
#101750=CARTESIAN_POINT('Ctrl Pts',(0.00242336930846644,-0.0343603235965158,
0.0733858143736273));
#101751=CARTESIAN_POINT('Ctrl Pts',(0.00244185838945779,-0.0341934961088739,
0.0732668598165172));
#101752=CARTESIAN_POINT('Ctrl Pts',(0.00239056670520884,-0.0346945769586885,
0.0737089097435703));
#101753=CARTESIAN_POINT('Ctrl Pts',(0.00239980551723251,-0.034527515336289,
0.0735888252497239));
#101754=CARTESIAN_POINT('Ctrl Pts',(0.00241282326568742,-0.0343603235965158,
0.0734690002480111));
#101755=CARTESIAN_POINT('Ctrl Pts',(0.00242957618270623,-0.0341934961088739,
0.0733497885553752));
#101756=CARTESIAN_POINT('Ctrl Pts',(0.0023835158731835,-0.0346945769586885,
0.0737924460476483));
#101757=CARTESIAN_POINT('Ctrl Pts',(0.00239100498387218,-0.034527515336289,
0.0736722138713022));
#101758=CARTESIAN_POINT('Ctrl Pts',(0.00240227722290839,-0.0343603235965158,
0.0735521861223949));
#101759=CARTESIAN_POINT('Ctrl Pts',(0.00241729397595467,-0.0341934961088739,
0.0734327172942333));
#101760=CARTESIAN_POINT('Ctrl Pts',(0.00243593008619894,-0.0340223579322365,
0.0733076138830058));
#101761=CARTESIAN_POINT('Ctrl Pts',(0.00244754878778742,-0.0339125849573552,
0.0732291635679111));
#101762=CARTESIAN_POINT('Ctrl Pts',(0.00246078306427793,-0.0338030433565216,
0.0731510088590692));
#101763=CARTESIAN_POINT('Ctrl Pts',(0.00247560713140719,-0.033693872113232,
0.0730732482029013));
#101764=CARTESIAN_POINT('Ctrl Pts',(0.00234349678459771,-0.0340223579322365,
0.0733731674075905));
#101765=CARTESIAN_POINT('Ctrl Pts',(0.00235421133211141,-0.0339125849573552,
0.0732934421961905));
#101766=CARTESIAN_POINT('Ctrl Pts',(0.00236656847725681,-0.0338030433565216,
0.0732139947730099));
#101767=CARTESIAN_POINT('Ctrl Pts',(0.00238054341092774,-0.033693872113232,
0.0731349253370677));
#101768=CARTESIAN_POINT('Ctrl Pts',(0.00225106348299649,-0.0340223579322365,
0.0734387209321752));
#101769=CARTESIAN_POINT('Ctrl Pts',(0.0022608738764354,-0.0339125849573552,
0.07335772082447));
#101770=CARTESIAN_POINT('Ctrl Pts',(0.00227235389023568,-0.0338030433565216,
0.0732769806869506));
#101771=CARTESIAN_POINT('Ctrl Pts',(0.00228547969044829,-0.033693872113232,
0.0731966024712341));
#101772=CARTESIAN_POINT('Ctrl Pts',(0.00215863018139526,-0.0340223579322365,
0.0735042744567599));
#101773=CARTESIAN_POINT('Ctrl Pts',(0.00216753642075939,-0.0339125849573552,
0.0734219994527494));
#101774=CARTESIAN_POINT('Ctrl Pts',(0.00217813930321455,-0.0338030433565216,
0.0733399666008913));
#101775=CARTESIAN_POINT('Ctrl Pts',(0.00219041596996884,-0.033693872113232,
0.0732582796054005));
#101776=CARTESIAN_POINT('Origin',(0.0190211830209275,-0.0345589643412385,
0.0750101267571015));
#101777=CARTESIAN_POINT('Ctrl Pts',(0.00225277570667803,-0.034193496108874,
0.0729125498651185));
#101778=CARTESIAN_POINT('Ctrl Pts',(0.00226983941103179,-0.0340836138595105,
0.072831592163374));
#101779=CARTESIAN_POINT('Ctrl Pts',(0.00228857017764344,-0.0339738896671456,
0.0727510264042088));
#101780=CARTESIAN_POINT('Ctrl Pts',(0.00230893712119388,-0.0338644633335883,
0.0726709540948107));
#101781=CARTESIAN_POINT('Ctrl Pts',(0.00232030018138788,-0.034193496108874,
0.0730035531868276));
#101782=CARTESIAN_POINT('Ctrl Pts',(0.00233610900384129,-0.0340836138595105,
0.072923526607591));
#101783=CARTESIAN_POINT('Ctrl Pts',(0.0023535662230422,-0.0339738896671456,
0.0728438655570162));
#101784=CARTESIAN_POINT('Ctrl Pts',(0.00237264266127564,-0.0338644633335883,
0.0727646704936415));
#101785=CARTESIAN_POINT('Ctrl Pts',(0.00238782465609773,-0.0341934961088739,
0.0730945565085366));
#101786=CARTESIAN_POINT('Ctrl Pts',(0.00240237859665078,-0.0340836138595105,
0.0730154610518081));
#101787=CARTESIAN_POINT('Ctrl Pts',(0.00241856226844097,-0.0339738896671456,
0.0729367047098237));
#101788=CARTESIAN_POINT('Ctrl Pts',(0.0024363482013574,-0.0338644633335883,
0.0728583868924724));
#101789=CARTESIAN_POINT('Ctrl Pts',(0.00245534913080758,-0.0341934961088739,
0.0731855598302457));
#101790=CARTESIAN_POINT('Ctrl Pts',(0.00246864818946028,-0.0340836138595105,
0.0731073954960251));
#101791=CARTESIAN_POINT('Ctrl Pts',(0.00248355831383973,-0.0339738896671456,
0.0730295438626311));
#101792=CARTESIAN_POINT('Ctrl Pts',(0.00250005374143916,-0.0338644633335883,
0.0729521032913032));
#101793=CARTESIAN_POINT('Origin',(0.0190291047356391,-0.0345610621861485,
0.0754912579844561));
#101794=CARTESIAN_POINT('Ctrl Pts',(0.00244817597163118,-0.03424362768739,
0.0732196135110987));
#101795=CARTESIAN_POINT('Ctrl Pts',(0.00248326607652709,-0.033943005420186,
0.0730055544936525));
#101796=CARTESIAN_POINT('Ctrl Pts',(0.00253438029638688,-0.0336441434784164,
0.0727947467259119));
#101797=CARTESIAN_POINT('Ctrl Pts',(0.002413105426267,-0.03424362768739,
0.0734671414021492));
#101798=CARTESIAN_POINT('Ctrl Pts',(0.00243885986285169,-0.033943005420186,
0.0732517596772794));
#101799=CARTESIAN_POINT('Ctrl Pts',(0.002480764567798,-0.0336441434784164,
0.0730389297589995));
#101800=CARTESIAN_POINT('Ctrl Pts',(0.00250004808859784,-0.0335235895815127,
0.0729521304373025));
#101801=CARTESIAN_POINT('Ctrl Pts',(0.00251653912151628,-0.0334144449262719,
0.0728747086652415));
#101802=CARTESIAN_POINT('Ctrl Pts',(0.002534648576178,-0.0333049234473132,
0.0727975386372734));
#101803=CARTESIAN_POINT('Ctrl Pts',(0.00255436223471938,-0.0331951640388588,
0.0727207211277815));
#101804=CARTESIAN_POINT('Ctrl Pts',(0.0024036810435052,-0.0335235895815127,
0.0730117506109557));
#101805=CARTESIAN_POINT('Ctrl Pts',(0.002419351287352,-0.0334144449262719,
0.0729330021567897));
#101806=CARTESIAN_POINT('Ctrl Pts',(0.00243666641820872,-0.0333049234473132,
0.0728544869656352));
#101807=CARTESIAN_POINT('Ctrl Pts',(0.00245561338971766,-0.0331951640388588,
0.0727763074399199));
#101808=CARTESIAN_POINT('Ctrl Pts',(0.00230731399841256,-0.0335235895815127,
0.0730713707846088));
#101809=CARTESIAN_POINT('Ctrl Pts',(0.00232216345318771,-0.0334144449262719,
0.0729912956483379));
#101810=CARTESIAN_POINT('Ctrl Pts',(0.00233868426023943,-0.0333049234473132,
0.0729114352939969));
#101811=CARTESIAN_POINT('Ctrl Pts',(0.00235686454471594,-0.0331951640388588,
0.0728318937520582));
#101812=CARTESIAN_POINT('Ctrl Pts',(0.00221094695331992,-0.0335235895815127,
0.0731309909582619));
#101813=CARTESIAN_POINT('Ctrl Pts',(0.00222497561902343,-0.0334144449262719,
0.0730495891398861));
#101814=CARTESIAN_POINT('Ctrl Pts',(0.00224070210227015,-0.0333049234473132,
0.0729683836223587));
#101815=CARTESIAN_POINT('Ctrl Pts',(0.00225811569971422,-0.0331951640388588,
0.0728874800641966));
#101816=CARTESIAN_POINT('Origin',(0.0184922424657708,-0.0326434571769605,
0.0775966635810342));
#101817=CARTESIAN_POINT('Ctrl Pts',(0.00234095736948707,-0.0336938721132393,
0.0725446472057946));
#101818=CARTESIAN_POINT('Ctrl Pts',(0.00235035403210412,-0.033647456976496,
0.0725107984131571));
#101819=CARTESIAN_POINT('Ctrl Pts',(0.00236014629371103,-0.033601104548885,
0.0724770619396607));
#101820=CARTESIAN_POINT('Ctrl Pts',(0.00238493804765038,-0.033483750864317,
0.0723916489489461));
#101821=CARTESIAN_POINT('Ctrl Pts',(0.00241224987877581,-0.0333660264760423,
0.0723070080963583));
#101822=CARTESIAN_POINT('Ctrl Pts',(0.0025259883083282,-0.0336938721132393,
0.0728298376525904));
#101823=CARTESIAN_POINT('Ctrl Pts',(0.00253371565662393,-0.033647456976496,
0.0727970719074377));
#101824=CARTESIAN_POINT('Ctrl Pts',(0.00254182603985373,-0.033601104548885,
0.0727643988657831));
#101825=CARTESIAN_POINT('Ctrl Pts',(0.00256235966461365,-0.033483750864317,
0.0726816782398781));
#101826=CARTESIAN_POINT('Ctrl Pts',(0.00258533545606793,-0.0333660264760423,
0.072599602392621));
#101827=CARTESIAN_POINT('Ctrl Pts',(0.0025259883083393,-0.0336938721132427,
0.0728298376525957));
#101828=CARTESIAN_POINT('Ctrl Pts',(0.0025337156566345,-0.0336474569765026,
0.0727970719074453));
#101829=CARTESIAN_POINT('Ctrl Pts',(0.00254182603986373,-0.0336011045488949,
0.0727643988657931));
#101830=CARTESIAN_POINT('Ctrl Pts',(0.00256218864749723,-0.0334847282606778,
0.0726823671900321));
#101831=CARTESIAN_POINT('Ctrl Pts',(0.00258495299398426,-0.0333679869945434,
0.0726009693021799));
#101832=CARTESIAN_POINT('Ctrl Pts',(0.00252598830832766,-0.0336938721132425,
0.0728298376525926));
#101833=CARTESIAN_POINT('Ctrl Pts',(0.00255362472552474,-0.0335278710435082,
0.0727126528476428));
#101834=CARTESIAN_POINT('Ctrl Pts',(0.00258492630531003,-0.033362046922432,
0.0725963759388932));
#101835=CARTESIAN_POINT('Ctrl Pts',(0.00261992795552341,-0.0331951640388602,
0.0724809543051736));
#101836=CARTESIAN_POINT('Ctrl Pts',(0.00250852319725496,-0.0336938721132425,
0.0729118315530883));
#101837=CARTESIAN_POINT('Ctrl Pts',(0.00253444314552974,-0.0335278710435082,
0.0727942811316695));
#101838=CARTESIAN_POINT('Ctrl Pts',(0.00256404032587993,-0.033362046922432,
0.0726775849070547));
#101839=CARTESIAN_POINT('Ctrl Pts',(0.00259734886824744,-0.0331951640388602,
0.0725616897660385));
#101840=CARTESIAN_POINT('Ctrl Pts',(0.00249105808618226,-0.0336938721132425,
0.0729938254535839));
#101841=CARTESIAN_POINT('Ctrl Pts',(0.00251526156553474,-0.0335278710435082,
0.0728759094156961));
#101842=CARTESIAN_POINT('Ctrl Pts',(0.00254315434644982,-0.033362046922432,
0.0727587938752161));
#101843=CARTESIAN_POINT('Ctrl Pts',(0.00257476978097148,-0.0331951640388602,
0.0726424252269033));
#101844=CARTESIAN_POINT('Ctrl Pts',(0.00247359297510956,-0.0336938721132425,
0.0730758193540796));
#101845=CARTESIAN_POINT('Ctrl Pts',(0.00249607998553974,-0.0335278710435082,
0.0729575376997227));
#101846=CARTESIAN_POINT('Ctrl Pts',(0.00252226836701971,-0.033362046922432,
0.0728400028433776));
#101847=CARTESIAN_POINT('Ctrl Pts',(0.00255219069369551,-0.0331951640388602,
0.0727231606877681));
#101848=CARTESIAN_POINT('Ctrl Pts',(0.00258635942130437,-0.0330240426238155,
0.0726013780880225));
#101849=CARTESIAN_POINT('Ctrl Pts',(0.00260769319689097,-0.0329142774063509,
0.0725250946944917));
#101850=CARTESIAN_POINT('Ctrl Pts',(0.0026306145989742,-0.0328043479726686,
0.0724492142996415));
#101851=CARTESIAN_POINT('Ctrl Pts',(0.00265509694063396,-0.0326943950436594,
0.072373834920589));
#101852=CARTESIAN_POINT('Ctrl Pts',(0.00248643910346057,-0.0330240426238155,
0.0726548296180905));
#101853=CARTESIAN_POINT('Ctrl Pts',(0.00250703653214519,-0.0329142774063509,
0.0725771697248338));
#101854=CARTESIAN_POINT('Ctrl Pts',(0.00252924967632504,-0.0328043479726686,
0.072499896921675));
#101855=CARTESIAN_POINT('Ctrl Pts',(0.00255305280553612,-0.0326943950436594,
0.0724231109845222));
#101856=CARTESIAN_POINT('Ctrl Pts',(0.00238651878561677,-0.0330240426238155,
0.0727082811481585));
#101857=CARTESIAN_POINT('Ctrl Pts',(0.00240637986739941,-0.0329142774063509,
0.0726292447551759));
#101858=CARTESIAN_POINT('Ctrl Pts',(0.00242788475367589,-0.0328043479726686,
0.0725505795437084));
#101859=CARTESIAN_POINT('Ctrl Pts',(0.00245100867043827,-0.0326943950436594,
0.0724723870484554));
#101860=CARTESIAN_POINT('Ctrl Pts',(0.00228659846777298,-0.0330240426238155,
0.0727617326782265));
#101861=CARTESIAN_POINT('Ctrl Pts',(0.00230572320265362,-0.0329142774063509,
0.0726813197855179));
#101862=CARTESIAN_POINT('Ctrl Pts',(0.00232651983102673,-0.0328043479726686,
0.0726012621657419));
#101863=CARTESIAN_POINT('Ctrl Pts',(0.00234896453534043,-0.0326943950436594,
0.0725216631123886));
#101864=CARTESIAN_POINT('Origin',(0.0186104450682804,-0.0326396682854751,
0.0776330441188748));
#101865=CARTESIAN_POINT('Ctrl Pts',(0.00245416397318748,-0.0331951640388587,
0.0721864753018193));
#101866=CARTESIAN_POINT('Ctrl Pts',(0.00248120755687549,-0.0330855618127431,
0.0721083877712924));
#101867=CARTESIAN_POINT('Ctrl Pts',(0.00250988457187204,-0.0329757224171935,
0.0720308028932627));
#101868=CARTESIAN_POINT('Ctrl Pts',(0.00254016316895784,-0.0328657861694598,
0.07195382182117));
#101869=CARTESIAN_POINT('Ctrl Pts',(0.00250975024107142,-0.0331951640388587,
0.0722852240682033));
#101870=CARTESIAN_POINT('Ctrl Pts',(0.00253543376011127,-0.0330855618127431,
0.0722079021261555));
#101871=CARTESIAN_POINT('Ctrl Pts',(0.0025627339066009,-0.0329757224171935,
0.0721310552782923));
#101872=CARTESIAN_POINT('Ctrl Pts',(0.00259162054812548,-0.0328657861694598,
0.0720547836464745));
#101873=CARTESIAN_POINT('Ctrl Pts',(0.00256533650895536,-0.0331951640388587,
0.0723839728345872));
#101874=CARTESIAN_POINT('Ctrl Pts',(0.00258965996334704,-0.0330855618127431,
0.0723074164810186));
#101875=CARTESIAN_POINT('Ctrl Pts',(0.00261558324132976,-0.0329757224171935,
0.0722313076633219));
#101876=CARTESIAN_POINT('Ctrl Pts',(0.00264307792729312,-0.0328657861694598,
0.072155745471779));
#101877=CARTESIAN_POINT('Ctrl Pts',(0.00262092277683929,-0.0331951640388587,
0.0724827216009712));
#101878=CARTESIAN_POINT('Ctrl Pts',(0.00264388616658281,-0.0330855618127431,
0.0724069308358816));
#101879=CARTESIAN_POINT('Ctrl Pts',(0.00266843257605861,-0.0329757224171935,
0.0723315600483515));
#101880=CARTESIAN_POINT('Ctrl Pts',(0.00269453530646077,-0.0328657861694598,
0.0722567072970835));
#101881=CARTESIAN_POINT('Origin',(0.0184227617885679,-0.032640190883161,
0.0780758170378834));
#101882=CARTESIAN_POINT('Ctrl Pts',(0.00260955876339398,-0.0332451089994433,
0.0725155383249555));
#101883=CARTESIAN_POINT('Ctrl Pts',(0.0026712034940288,-0.0329451141710258,
0.0723075659856985));
#101884=CARTESIAN_POINT('Ctrl Pts',(0.00274833842528032,-0.0326442513127503,
0.0721048278070249));
#101885=CARTESIAN_POINT('Ctrl Pts',(0.00254373824981596,-0.0332451089994433,
0.0727567180504557));
#101886=CARTESIAN_POINT('Ctrl Pts',(0.00259628673828125,-0.0329451141710258,
0.0725462632499138));
#101887=CARTESIAN_POINT('Ctrl Pts',(0.00266453825795956,-0.0326442513127503,
0.07234036449622));
#101888=CARTESIAN_POINT('Ctrl Pts',(0.00269452481170455,-0.0325229783203384,
0.0722567371197357));
#101889=CARTESIAN_POINT('Ctrl Pts',(0.00272062339863101,-0.0324130253112079,
0.0721818949268253));
#101890=CARTESIAN_POINT('Ctrl Pts',(0.00274826623406922,-0.0323031222247695,
0.0721076039679865));
#101891=CARTESIAN_POINT('Ctrl Pts',(0.00277741455157991,-0.0321934096636185,
0.0720339581552029));
#101892=CARTESIAN_POINT('Ctrl Pts',(0.00259144539522894,-0.0325229783203384,
0.0723038091554731));
#101893=CARTESIAN_POINT('Ctrl Pts',(0.00261689509518397,-0.0324130253112079,
0.0722275460150867));
#101894=CARTESIAN_POINT('Ctrl Pts',(0.00264391853619052,-0.0323031222247695,
0.0721518209012261));
#101895=CARTESIAN_POINT('Ctrl Pts',(0.00267247768038604,-0.0321934096636185,
0.0720767295909218));
#101896=CARTESIAN_POINT('Ctrl Pts',(0.00248836597875334,-0.0325229783203384,
0.0723508811912106));
#101897=CARTESIAN_POINT('Ctrl Pts',(0.00251316679173693,-0.0324130253112079,
0.0722731971033481));
#101898=CARTESIAN_POINT('Ctrl Pts',(0.00253957083831181,-0.0323031222247695,
0.0721960378344656));
#101899=CARTESIAN_POINT('Ctrl Pts',(0.00256754080919217,-0.0321934096636184,
0.0721195010266408));
#101900=CARTESIAN_POINT('Ctrl Pts',(0.00238528656227773,-0.0325229783203384,
0.072397953226948));
#101901=CARTESIAN_POINT('Ctrl Pts',(0.0024094384882899,-0.0324130253112079,
0.0723188481916095));
#101902=CARTESIAN_POINT('Ctrl Pts',(0.0024352231404331,-0.0323031222247695,
0.0722402547677052));
#101903=CARTESIAN_POINT('Ctrl Pts',(0.0024626039379983,-0.0321934096636184,
0.0721622724623597));
#101904=CARTESIAN_POINT('Origin',(0.0186024321118089,-0.0326393375178981,
0.0776301314651015));
#101905=CARTESIAN_POINT('Ctrl Pts',(0.00258864240555086,-0.0326943950436594,
0.071834351595725));
#101906=CARTESIAN_POINT('Ctrl Pts',(0.00262055638054933,-0.0325844576448127,
0.0717580669954951));
#101907=CARTESIAN_POINT('Ctrl Pts',(0.00265405030475245,-0.0324744968375319,
0.0716824370298121));
#101908=CARTESIAN_POINT('Ctrl Pts',(0.00268907992722798,-0.0323646534831894,
0.0716075580082806));
#101909=CARTESIAN_POINT('Ctrl Pts',(0.00263791845336137,-0.0326943950436594,
0.0719363956974349));
#101910=CARTESIAN_POINT('Ctrl Pts',(0.00266842606938725,-0.0325844576448127,
0.0718607902134969));
#101911=CARTESIAN_POINT('Ctrl Pts',(0.00270049948984924,-0.0324744968375319,
0.0717858103263588));
#101912=CARTESIAN_POINT('Ctrl Pts',(0.00273409629533575,-0.0323646534831894,
0.0717115515378101));
#101913=CARTESIAN_POINT('Ctrl Pts',(0.00268719450117189,-0.0326943950436594,
0.0720384397991448));
#101914=CARTESIAN_POINT('Ctrl Pts',(0.00271629575822518,-0.0325844576448127,
0.0719635134314988));
#101915=CARTESIAN_POINT('Ctrl Pts',(0.00274694867494603,-0.0324744968375319,
0.0718891836229055));
#101916=CARTESIAN_POINT('Ctrl Pts',(0.00277911266344352,-0.0323646534831894,
0.0718155450673395));
#101917=CARTESIAN_POINT('Ctrl Pts',(0.00273647054898241,-0.0326943950436594,
0.0721404839008547));
#101918=CARTESIAN_POINT('Ctrl Pts',(0.00276416544706311,-0.0325844576448127,
0.0720662366495007));
#101919=CARTESIAN_POINT('Ctrl Pts',(0.00279339786004281,-0.0324744968375319,
0.0719925569194521));
#101920=CARTESIAN_POINT('Ctrl Pts',(0.0028241290315513,-0.0323646534831894,
0.0719195385968689));
#101921=CARTESIAN_POINT('Origin',(0.0184582817635514,-0.0326395579068394,
0.0780888666716867));
#101922=CARTESIAN_POINT('Ctrl Pts',(0.00272305503550547,-0.0327445246961876,
0.0721725594397983));
#101923=CARTESIAN_POINT('Ctrl Pts',(0.00279763542468079,-0.0324436878365475,
0.071968867687262));
#101924=CARTESIAN_POINT('Ctrl Pts',(0.00288734683399173,-0.0321434074463186,
0.0717713723011381));
#101925=CARTESIAN_POINT('Ctrl Pts',(0.00264222221678873,-0.0327445246961876,
0.0724091308992313));
#101926=CARTESIAN_POINT('Ctrl Pts',(0.00270788016760237,-0.0324436878365475,
0.0722023904871302));
#101927=CARTESIAN_POINT('Ctrl Pts',(0.00278892412375222,-0.0321434074463186,
0.072001183027844));
#101928=CARTESIAN_POINT('Ctrl Pts',(0.00286012809327848,-0.0322357242816072,
0.0718322272507116));
#101929=CARTESIAN_POINT('Ctrl Pts',(0.00293394614930217,-0.0319819883628705,
0.0716645866943412));
#101930=CARTESIAN_POINT('Ctrl Pts',(0.00301828205205449,-0.0317295851069887,
0.0715019831364399));
#101931=CARTESIAN_POINT('Ctrl Pts',(0.00276437571503811,-0.0322357242816072,
0.0720631633502311));
#101932=CARTESIAN_POINT('Ctrl Pts',(0.00283083875580525,-0.0319819883628705,
0.0718924732048001));
#101933=CARTESIAN_POINT('Ctrl Pts',(0.00290802860322813,-0.0317295851069887,
0.0717263582175471));
#101934=CARTESIAN_POINT('Origin',(0.0183698502145489,-0.0326371942646075,
0.078053338307413));
#101935=CARTESIAN_POINT('Origin',(0.0184869045507201,-0.032635298552719,
0.077588692527467));
#101936=CARTESIAN_POINT('Ctrl Pts',(0.00274496550589063,-0.0321934096636183,
0.0714913666959626));
#101937=CARTESIAN_POINT('Ctrl Pts',(0.00278163013116605,-0.0320835708272303,
0.0714171886218511));
#101938=CARTESIAN_POINT('Ctrl Pts',(0.00281980860085707,-0.0319739230346346,
0.0713438123465517));
#101939=CARTESIAN_POINT('Ctrl Pts',(0.00285944486324399,-0.0318646057455575,
0.0712713280010697));
#101940=CARTESIAN_POINT('Ctrl Pts',(0.00278773697844063,-0.0321934096636183,
0.0715963036575189));
#101941=CARTESIAN_POINT('Ctrl Pts',(0.0028229544412333,-0.0320835708272303,
0.071522715435348));
#101942=CARTESIAN_POINT('Ctrl Pts',(0.00285967438089936,-0.0319739230346346,
0.0714498987208986));
#101943=CARTESIAN_POINT('Ctrl Pts',(0.00289784266675191,-0.0318646057455575,
0.071377943072474));
#101944=CARTESIAN_POINT('Ctrl Pts',(0.00283050845099063,-0.0321934096636183,
0.0717012406190752));
#101945=CARTESIAN_POINT('Ctrl Pts',(0.00286427875130054,-0.0320835708272303,
0.0716282422488448));
#101946=CARTESIAN_POINT('Ctrl Pts',(0.00289954016094165,-0.0319739230346346,
0.0715559850952455));
#101947=CARTESIAN_POINT('Ctrl Pts',(0.00293624047025983,-0.0318646057455575,
0.0714845581438782));
#101948=CARTESIAN_POINT('Ctrl Pts',(0.00287327992354062,-0.0321934096636183,
0.0718061775806315));
#101949=CARTESIAN_POINT('Ctrl Pts',(0.00290560306136778,-0.0320835708272303,
0.0717337690623416));
#101950=CARTESIAN_POINT('Ctrl Pts',(0.00293940594098394,-0.0319739230346346,
0.0716620714695923));
#101951=CARTESIAN_POINT('Ctrl Pts',(0.00297463827376775,-0.0318646057455575,
0.0715911732152825));
#101952=CARTESIAN_POINT('Ctrl Pts',(0.00282318417424442,-0.0320218834582395,
0.0719196506007348));
#101953=CARTESIAN_POINT('Ctrl Pts',(0.00284639671965595,-0.0319391099350682,
0.0718644841894713));
#101954=CARTESIAN_POINT('Ctrl Pts',(0.00287045663242311,-0.0318564869454953,
0.0718097136692862));
#101955=CARTESIAN_POINT('Ctrl Pts',(0.00289534266379709,-0.0317740741446536,
0.0717553772972089));
#101956=CARTESIAN_POINT('Ctrl Pts',(0.00277689158142658,-0.0320218834582395,
0.0719373656761641));
#101957=CARTESIAN_POINT('Ctrl Pts',(0.00279991975572881,-0.0319391099350682,
0.071881717470921));
#101958=CARTESIAN_POINT('Ctrl Pts',(0.00282380293237298,-0.0318564869454953,
0.0718264625696823));
#101959=CARTESIAN_POINT('Ctrl Pts',(0.00284851995840211,-0.0317740741446536,
0.0717716395943025));
#101960=CARTESIAN_POINT('Ctrl Pts',(0.00273059898860874,-0.0320218834582395,
0.0719550807515934));
#101961=CARTESIAN_POINT('Ctrl Pts',(0.00275344279180167,-0.0319391099350682,
0.0718989507523707));
#101962=CARTESIAN_POINT('Ctrl Pts',(0.00277714923232285,-0.0318564869454953,
0.0718432114700783));
#101963=CARTESIAN_POINT('Ctrl Pts',(0.00280169725300713,-0.0317740741446536,
0.071787901891396));
#101964=CARTESIAN_POINT('Ctrl Pts',(0.0026843063957909,-0.0320218834582395,
0.0719727958270227));
#101965=CARTESIAN_POINT('Ctrl Pts',(0.00270696582787452,-0.0319391099350682,
0.0719161840338204));
#101966=CARTESIAN_POINT('Ctrl Pts',(0.00273049553227273,-0.0318564869454953,
0.0718599603704744));
#101967=CARTESIAN_POINT('Ctrl Pts',(0.00275487454761215,-0.0317740741446536,
0.0718041641884896));
#101968=CARTESIAN_POINT('Origin',(-0.00334032719988602,-0.0391228853390595,
0.0703480512688116));
#101969=CARTESIAN_POINT('Ctrl Pts',(0.00242487062843551,-0.035272297877964,
0.0749288270158611));
#101970=CARTESIAN_POINT('Ctrl Pts',(0.00242265926332284,-0.0352466642097247,
0.0749100599558245));
#101971=CARTESIAN_POINT('Ctrl Pts',(0.00242037200596261,-0.0352210183808316,
0.0748913187897723));
#101972=CARTESIAN_POINT('Ctrl Pts',(0.00241800824704151,-0.0351953608940153,
0.0748726029208616));
#101973=CARTESIAN_POINT('Origin',(-0.00245930885073002,-0.0352456003065141,
0.0753219351578665));
#101974=CARTESIAN_POINT('Ctrl Pts',(0.00240513099386094,-0.0350241211493338,
0.0747485888419485));
#101975=CARTESIAN_POINT('Ctrl Pts',(0.00239688567836588,-0.034914423286742,
0.074669816769969));
#101976=CARTESIAN_POINT('Ctrl Pts',(0.00239026370259411,-0.0348045283677512,
0.0745908271125543));
#101977=CARTESIAN_POINT('Ctrl Pts',(0.00238527731343735,-0.0346945769586886,
0.0745117207297779));
#101978=CARTESIAN_POINT('Ctrl Pts',(0.00233190423374359,-0.0350241211493338,
0.0748350699578395));
#101979=CARTESIAN_POINT('Ctrl Pts',(0.00232246767638947,-0.034914423286742,
0.074755289217309));
#101980=CARTESIAN_POINT('Ctrl Pts',(0.00231467459564178,-0.0348045283677512,
0.0746752656637873));
#101981=CARTESIAN_POINT('Ctrl Pts',(0.00230853878770864,-0.0346945769586886,
0.0745951014258173));
#101982=CARTESIAN_POINT('Ctrl Pts',(0.00225867747362623,-0.0350241211493338,
0.0749215510737304));
#101983=CARTESIAN_POINT('Ctrl Pts',(0.00224804967441307,-0.034914423286742,
0.074840761664649));
#101984=CARTESIAN_POINT('Ctrl Pts',(0.00223908548868946,-0.0348045283677512,
0.0747597042150202));
#101985=CARTESIAN_POINT('Ctrl Pts',(0.00223180026197993,-0.0346945769586886,
0.0746784821218568));
#101986=CARTESIAN_POINT('Ctrl Pts',(0.00218545071350887,-0.0350241211493338,
0.0750080321896214));
#101987=CARTESIAN_POINT('Ctrl Pts',(0.00217363167243667,-0.034914423286742,
0.074926234111989));
#101988=CARTESIAN_POINT('Ctrl Pts',(0.00216349638173713,-0.0348045283677512,
0.0748441427662532));
#101989=CARTESIAN_POINT('Ctrl Pts',(0.00215506173625123,-0.0346945769586886,
0.0747618628178962));
#101990=CARTESIAN_POINT('Origin',(0.0191511622908026,-0.0345629067940586,
0.0736353361079466));
#101991=CARTESIAN_POINT('Ctrl Pts',(0.00220159779565417,-0.0351970973651532,
0.0744713311994661));
#101992=CARTESIAN_POINT('Ctrl Pts',(0.00219714618738722,-0.0350869349326836,
0.0743892873610033));
#101993=CARTESIAN_POINT('Ctrl Pts',(0.00219439653738732,-0.0349764985139958,
0.0743070830119113));
#101994=CARTESIAN_POINT('Ctrl Pts',(0.00219335867701082,-0.0348659306865056,
0.0742248244406427));
#101995=CARTESIAN_POINT('Ctrl Pts',(0.00226548690933194,-0.0351970973651532,
0.074523086892907));
#101996=CARTESIAN_POINT('Ctrl Pts',(0.0022603182960771,-0.0350869349326836,
0.074441928151525));
#101997=CARTESIAN_POINT('Ctrl Pts',(0.00225683264645299,-0.0349764985139958,
0.0743605947265817));
#101998=CARTESIAN_POINT('Ctrl Pts',(0.00225504067890629,-0.0348659306865056,
0.0742791917220926));
#101999=CARTESIAN_POINT('Ctrl Pts',(0.00232937602300971,-0.0351970973651532,
0.0745748425863479));
#102000=CARTESIAN_POINT('Ctrl Pts',(0.00232349040476698,-0.0350869349326836,
0.0744945689420467));
#102001=CARTESIAN_POINT('Ctrl Pts',(0.00231926875551866,-0.0349764985139958,
0.074414106441252));
#102002=CARTESIAN_POINT('Ctrl Pts',(0.00231672268080175,-0.0348659306865056,
0.0743335590035424));
#102003=CARTESIAN_POINT('Ctrl Pts',(0.00239326513668748,-0.0351970973651532,
0.0746265982797888));
#102004=CARTESIAN_POINT('Ctrl Pts',(0.00238666251345686,-0.0350869349326836,
0.0745472097325684));
#102005=CARTESIAN_POINT('Ctrl Pts',(0.00238170486458433,-0.0349764985139958,
0.0744676181559223));
#102006=CARTESIAN_POINT('Ctrl Pts',(0.00237840468269722,-0.0348659306865056,
0.0743879262849923));
#102007=CARTESIAN_POINT('Origin',(0.0191280656060807,-0.0345637187964347,
0.0741157441631858));
#102008=CARTESIAN_POINT('Ctrl Pts',(0.00239510090204551,-0.0352450361861253,
0.0746602309922252));
#102009=CARTESIAN_POINT('Ctrl Pts',(0.0023758572248948,-0.0349452761023765,
0.0744441702374998));
#102010=CARTESIAN_POINT('Ctrl Pts',(0.00237294279667918,-0.0346444289983475,
0.0742272737761386));
#102011=CARTESIAN_POINT('Ctrl Pts',(0.00242268645417911,-0.0352450361861253,
0.0749087044059207));
#102012=CARTESIAN_POINT('Ctrl Pts',(0.00239407144869566,-0.0349452761023765,
0.0746936840573395));
#102013=CARTESIAN_POINT('Ctrl Pts',(0.00238173394745746,-0.0346444289983475,
0.0744771191596621));
#102014=CARTESIAN_POINT('Ctrl Pts',(0.0023788297275446,-0.0345231616327822,
0.0743883315578107));
#102015=CARTESIAN_POINT('Ctrl Pts',(0.0023755446625642,-0.0344132092796975,
0.0743091454763196));
#102016=CARTESIAN_POINT('Ctrl Pts',(0.00237389766871257,-0.0343032738558974,
0.0742298955314883));
#102017=CARTESIAN_POINT('Ctrl Pts',(0.00237388825529274,-0.0341934961088741,
0.0741506833057032));
#102018=CARTESIAN_POINT('Ctrl Pts',(0.00230031729991655,-0.0345231616327822,
0.0744700440712127));
#102019=CARTESIAN_POINT('Ctrl Pts',(0.00229590594298092,-0.0344132092796975,
0.0743897758064433));
#102020=CARTESIAN_POINT('Ctrl Pts',(0.00229315509939306,-0.0343032738558974,
0.0743094204377089));
#102021=CARTESIAN_POINT('Ctrl Pts',(0.00229206565633918,-0.0341934961088741,
0.0742290809997956));
#102022=CARTESIAN_POINT('Ctrl Pts',(0.0022218048722885,-0.0345231616327822,
0.0745517565846147));
#102023=CARTESIAN_POINT('Ctrl Pts',(0.00221626722339765,-0.0344132092796975,
0.0744704061365671));
#102024=CARTESIAN_POINT('Ctrl Pts',(0.00221241253007354,-0.0343032738558974,
0.0743889453439295));
#102025=CARTESIAN_POINT('Ctrl Pts',(0.00221024305738562,-0.0341934961088741,
0.074307478693888));
#102026=CARTESIAN_POINT('Ctrl Pts',(0.00214329244466045,-0.0345231616327822,
0.0746334690980167));
#102027=CARTESIAN_POINT('Ctrl Pts',(0.00213662850381438,-0.0344132092796975,
0.0745510364666909));
#102028=CARTESIAN_POINT('Ctrl Pts',(0.00213166996075403,-0.0343032738558974,
0.07446847025015));
#102029=CARTESIAN_POINT('Ctrl Pts',(0.00212842045843206,-0.0341934961088741,
0.0743858763879804));
#102030=CARTESIAN_POINT('Origin',(0.0191632385091167,-0.0345625596229836,
0.0736345217087045));
#102031=CARTESIAN_POINT('Ctrl Pts',(0.00212489233953381,-0.0346945769586885,
0.0740345854224619));
#102032=CARTESIAN_POINT('Ctrl Pts',(0.00212648281074835,-0.0345846629176052,
0.0739519176881526));
#102033=CARTESIAN_POINT('Ctrl Pts',(0.00212978308841509,-0.0344746925050311,
0.0738692687242825));
#102034=CARTESIAN_POINT('Ctrl Pts',(0.00213478850648869,-0.034364806625326,
0.0737867444127645));
#102035=CARTESIAN_POINT('Ctrl Pts',(0.00220827296992208,-0.0346945769586885,
0.0741113238877693));
#102036=CARTESIAN_POINT('Ctrl Pts',(0.00220880594629738,-0.0345846629176052,
0.0740298051806913));
#102037=CARTESIAN_POINT('Ctrl Pts',(0.0022110247870909,-0.0344746925050311,
0.0739482835717502));
#102038=CARTESIAN_POINT('Ctrl Pts',(0.0022149262178844,-0.034364806625326,
0.0738668635040844));
#102039=CARTESIAN_POINT('Ctrl Pts',(0.00229165360031035,-0.0346945769586885,
0.0741880623530767));
#102040=CARTESIAN_POINT('Ctrl Pts',(0.00229112908184641,-0.0345846629176052,
0.0741076926732299));
#102041=CARTESIAN_POINT('Ctrl Pts',(0.0022922664857667,-0.0344746925050311,
0.0740272984192179));
#102042=CARTESIAN_POINT('Ctrl Pts',(0.0022950639292801,-0.034364806625326,
0.0739469825954044));
#102043=CARTESIAN_POINT('Ctrl Pts',(0.00237503423069861,-0.0346945769586885,
0.074264800818384));
#102044=CARTESIAN_POINT('Ctrl Pts',(0.00237345221739543,-0.0345846629176052,
0.0741855801657686));
#102045=CARTESIAN_POINT('Ctrl Pts',(0.0023735081844425,-0.0344746925050311,
0.0741063132666856));
#102046=CARTESIAN_POINT('Ctrl Pts',(0.0023752016406758,-0.034364806625326,
0.0740271016867243));
#102047=CARTESIAN_POINT('Origin',(0.0191864882751684,-0.0345626446732421,
0.0741147837526571));
#102048=CARTESIAN_POINT('Ctrl Pts',(0.00237354227162475,-0.0346945769586885,
0.0742634277099163));
#102049=CARTESIAN_POINT('Ctrl Pts',(0.00237116648282662,-0.034527515336289,
0.0741429866324923));
#102050=CARTESIAN_POINT('Ctrl Pts',(0.00237257784055434,-0.0343603235965158,
0.0740224396864657));
#102051=CARTESIAN_POINT('Ctrl Pts',(0.00237776687175778,-0.0341934961088739,
0.0739021433341527));
#102052=CARTESIAN_POINT('Ctrl Pts',(0.00237701691262604,-0.0346945769586885,
0.0743471890088627));
#102053=CARTESIAN_POINT('Ctrl Pts',(0.0023728867098853,-0.034527515336289,
0.0742268207091856));
#102054=CARTESIAN_POINT('Ctrl Pts',(0.00237254091109597,-0.0343603235965158,
0.0741062913850263));
#102055=CARTESIAN_POINT('Ctrl Pts',(0.00237597524087146,-0.0341934961088739,
0.0739859575238226));
#102056=CARTESIAN_POINT('Ctrl Pts',(0.00238049155362732,-0.0346945769586885,
0.074430950307809));
#102057=CARTESIAN_POINT('Ctrl Pts',(0.00237460693694399,-0.034527515336289,
0.0743106547858789));
#102058=CARTESIAN_POINT('Ctrl Pts',(0.00237250398163759,-0.0343603235965158,
0.0741901430835869));
#102059=CARTESIAN_POINT('Ctrl Pts',(0.00237418360998514,-0.0341934961088739,
0.0740697717134926));
#102060=CARTESIAN_POINT('Ctrl Pts',(0.0023839661946286,-0.0346945769586885,
0.0745147116067554));
#102061=CARTESIAN_POINT('Ctrl Pts',(0.00237632716400267,-0.034527515336289,
0.0743944888625722));
#102062=CARTESIAN_POINT('Ctrl Pts',(0.00237246705217922,-0.0343603235965158,
0.0742739947821475));
#102063=CARTESIAN_POINT('Ctrl Pts',(0.00237239197909882,-0.0341934961088739,
0.0741535859031625));
#102064=CARTESIAN_POINT('Ctrl Pts',(0.00237520152298843,-0.0340223579322365,
0.0740271332457414));
#102065=CARTESIAN_POINT('Ctrl Pts',(0.00237689617597959,-0.0339125849573554,
0.0739478453253734));
#102066=CARTESIAN_POINT('Ctrl Pts',(0.00238023071386964,-0.0338030433565221,
0.0738686481950882));
#102067=CARTESIAN_POINT('Ctrl Pts',(0.00238519189432022,-0.0336938721132328,
0.0737896427566524));
#102068=CARTESIAN_POINT('Ctrl Pts',(0.00229171312078655,-0.0340223579322365,
0.0741037548257835));
#102069=CARTESIAN_POINT('Ctrl Pts',(0.00229235096235146,-0.0339125849573554,
0.0740233153826023));
#102070=CARTESIAN_POINT('Ctrl Pts',(0.00229465326527089,-0.0338030433565221,
0.0739429456651248));
#102071=CARTESIAN_POINT('Ctrl Pts',(0.00229860797433296,-0.0336938721132328,
0.0738627481916762));
#102072=CARTESIAN_POINT('Ctrl Pts',(0.00220822471858466,-0.0340223579322365,
0.0741803764058257));
#102073=CARTESIAN_POINT('Ctrl Pts',(0.00220780574872334,-0.0339125849573554,
0.0740987854398313));
#102074=CARTESIAN_POINT('Ctrl Pts',(0.00220907581667214,-0.0338030433565221,
0.0740172431351613));
#102075=CARTESIAN_POINT('Ctrl Pts',(0.0022120240543457,-0.0336938721132328,
0.0739358536267));
#102076=CARTESIAN_POINT('Ctrl Pts',(0.00212473631638278,-0.0340223579322365,
0.0742569979858679));
#102077=CARTESIAN_POINT('Ctrl Pts',(0.00212326053509521,-0.0339125849573554,
0.0741742554970602));
#102078=CARTESIAN_POINT('Ctrl Pts',(0.00212349836807339,-0.0338030433565221,
0.0740915406051979));
#102079=CARTESIAN_POINT('Ctrl Pts',(0.00212544013435845,-0.0336938721132328,
0.0740089590617238));
#102080=CARTESIAN_POINT('Origin',(0.019043056228323,-0.0345589643414795,
0.073637537917189));
#102081=CARTESIAN_POINT('Ctrl Pts',(0.00214397671962884,-0.034193496108874,
0.0736581397562618));
#102082=CARTESIAN_POINT('Ctrl Pts',(0.00215075918112192,-0.0340836138581107,
0.0735756817798827));
#102083=CARTESIAN_POINT('Ctrl Pts',(0.00215924468306331,-0.0339738896643499,
0.0734934037171999));
#102084=CARTESIAN_POINT('Ctrl Pts',(0.00216941530589721,-0.0338644633294062,
0.0734114101459476));
#102085=CARTESIAN_POINT('Ctrl Pts',(0.00222237448426191,-0.034193496108874,
0.0737399624288377));
#102086=CARTESIAN_POINT('Ctrl Pts',(0.00222802865955363,-0.0340836138581107,
0.0736585855112076));
#102087=CARTESIAN_POINT('Ctrl Pts',(0.00223536404642415,-0.0339738896643499,
0.073577364641046));
#102088=CARTESIAN_POINT('Ctrl Pts',(0.00224436428802624,-0.0338644633294062,
0.0734964031416869));
#102089=CARTESIAN_POINT('Ctrl Pts',(0.00230077224889499,-0.034193496108874,
0.0738217851014136));
#102090=CARTESIAN_POINT('Ctrl Pts',(0.00230529813798535,-0.0340836138581107,
0.0737414892425325));
#102091=CARTESIAN_POINT('Ctrl Pts',(0.002311483409785,-0.0339738896643499,
0.0736613255648921));
#102092=CARTESIAN_POINT('Ctrl Pts',(0.00231931327015528,-0.0338644633294062,
0.0735813961374263));
#102093=CARTESIAN_POINT('Ctrl Pts',(0.00237917001352806,-0.034193496108874,
0.0739036077739895));
#102094=CARTESIAN_POINT('Ctrl Pts',(0.00238256761641706,-0.0340836138581106,
0.0738243929738574));
#102095=CARTESIAN_POINT('Ctrl Pts',(0.00238760277314584,-0.0339738896643499,
0.0737452864887382));
#102096=CARTESIAN_POINT('Ctrl Pts',(0.00239426225228432,-0.0338644633294062,
0.0736663891331656));
#102097=CARTESIAN_POINT('Origin',(0.0191112172097644,-0.0345610621863715,
0.0741138824269738));
#102098=CARTESIAN_POINT('Ctrl Pts',(0.00237632147479038,-0.0342436276873899,
0.0739382919666322));
#102099=CARTESIAN_POINT('Ctrl Pts',(0.00238430617489815,-0.0339430054201859,
0.073721522912162));
#102100=CARTESIAN_POINT('Ctrl Pts',(0.00240859612467587,-0.0336441434784161,
0.073505971116179));
#102101=CARTESIAN_POINT('Ctrl Pts',(0.00237255094213417,-0.0342436276873899,
0.074188263531182));
#102102=CARTESIAN_POINT('Ctrl Pts',(0.00237110780926533,-0.0339430054201859,
0.0739713522687283));
#102103=CARTESIAN_POINT('Ctrl Pts',(0.00238600742123956,-0.0336441434784161,
0.0737549485257507));
#102104=CARTESIAN_POINT('Ctrl Pts',(0.0023942600460587,-0.0335235895815127,
0.0736664167766149));
#102105=CARTESIAN_POINT('Ctrl Pts',(0.00240091752121627,-0.0334144449262716,
0.0735875386238706));
#102106=CARTESIAN_POINT('Ctrl Pts',(0.00240921220827948,-0.0333049234473127,
0.0735087073881116));
#102107=CARTESIAN_POINT('Ctrl Pts',(0.00241914263187613,-0.033195164038858,
0.0734300248310558));
#102108=CARTESIAN_POINT('Ctrl Pts',(0.00230612527304964,-0.0335235895815127,
0.0737376448207616));
#102109=CARTESIAN_POINT('Ctrl Pts',(0.00231180215394443,-0.0334144449262716,
0.0736575533193455));
#102110=CARTESIAN_POINT('Ctrl Pts',(0.00231914018703127,-0.0333049234473127,
0.0735774870825845));
#102111=CARTESIAN_POINT('Ctrl Pts',(0.00232813926325428,-0.033195164038858,
0.0734975493405749));
#102112=CARTESIAN_POINT('Ctrl Pts',(0.00221799050004059,-0.0335235895815127,
0.0738088728649083));
#102113=CARTESIAN_POINT('Ctrl Pts',(0.0022226867866726,-0.0334144449262716,
0.0737275680148203));
#102114=CARTESIAN_POINT('Ctrl Pts',(0.00222906816578306,-0.0333049234473127,
0.0736462667770574));
#102115=CARTESIAN_POINT('Ctrl Pts',(0.00223713589463243,-0.033195164038858,
0.0735650738500941));
#102116=CARTESIAN_POINT('Ctrl Pts',(0.00212985572703154,-0.0335235895815127,
0.073880100909055));
#102117=CARTESIAN_POINT('Ctrl Pts',(0.00213357141940076,-0.0334144449262716,
0.0737975827102952));
#102118=CARTESIAN_POINT('Ctrl Pts',(0.00213899614453485,-0.0333049234473127,
0.0737150464715303));
#102119=CARTESIAN_POINT('Ctrl Pts',(0.00214613252601059,-0.033195164038858,
0.0736325983596132));
#102120=CARTESIAN_POINT('Origin',(0.0188424655511459,-0.0326434571768116,
0.0762699729563738));
#102121=CARTESIAN_POINT('Ctrl Pts',(0.00218535261375798,-0.03369387211324,
0.0732820860263534));
#102122=CARTESIAN_POINT('Ctrl Pts',(0.00219043280225018,-0.0336474569764963,
0.0732473264274453));
#102123=CARTESIAN_POINT('Ctrl Pts',(0.00219591954763718,-0.033601104548885,
0.0732126286803076));
#102124=CARTESIAN_POINT('Ctrl Pts',(0.00220981072487708,-0.0334837508643174,
0.0731247819658497));
#102125=CARTESIAN_POINT('Ctrl Pts',(0.00222629888230992,-0.0333660264760431,
0.0730373854515563));
#102126=CARTESIAN_POINT('Ctrl Pts',(0.00240466836925891,-0.03369387211324,
0.0735418371354195));
#102127=CARTESIAN_POINT('Ctrl Pts',(0.00240822814831518,-0.0336474569764963,
0.073508361264405));
#102128=CARTESIAN_POINT('Ctrl Pts',(0.00241217956078985,-0.033601104548885,
0.073474929358887));
#102129=CARTESIAN_POINT('Ctrl Pts',(0.00242218362825825,-0.0334837508643174,
0.073390287464237));
#102130=CARTESIAN_POINT('Ctrl Pts',(0.00243469141740008,-0.0333660264760431,
0.073305979179314));
#102131=CARTESIAN_POINT('Ctrl Pts',(0.00240466836926948,-0.0336938721132426,
0.0735418371354243));
#102132=CARTESIAN_POINT('Ctrl Pts',(0.00240822814832549,-0.0336474569765026,
0.0735083612644123));
#102133=CARTESIAN_POINT('Ctrl Pts',(0.00241217956079984,-0.0336011045488949,
0.073474929358897));
#102134=CARTESIAN_POINT('Ctrl Pts',(0.00242210030801232,-0.0334847282606778,
0.0733909924159425));
#102135=CARTESIAN_POINT('Ctrl Pts',(0.00243448329033809,-0.0333679869945434,
0.0733073832455932));
#102136=CARTESIAN_POINT('Ctrl Pts',(0.00240466836925872,-0.0336938721132425,
0.0735418371354214));
#102137=CARTESIAN_POINT('Ctrl Pts',(0.00241739971452264,-0.0335278710435082,
0.0734221126061285));
#102138=CARTESIAN_POINT('Ctrl Pts',(0.00243388111103953,-0.0333620469224319,
0.0733028294473244));
#102139=CARTESIAN_POINT('Ctrl Pts',(0.00245414059620915,-0.0331951640388601,
0.0731839310776603));
#102140=CARTESIAN_POINT('Ctrl Pts',(0.00239761753648507,-0.0336938721132425,
0.0736253734483665));
#102141=CARTESIAN_POINT('Ctrl Pts',(0.00240860012380252,-0.0335278710435082,
0.0735055013162));
#102142=CARTESIAN_POINT('Ctrl Pts',(0.00242333800636967,-0.0333620469224319,
0.0733860157658541));
#102143=CARTESIAN_POINT('Ctrl Pts',(0.00244185838815389,-0.0331951640388601,
0.0732668598253209));
#102144=CARTESIAN_POINT('Ctrl Pts',(0.00239056670371142,-0.0336938721132425,
0.0737089097613116));
#102145=CARTESIAN_POINT('Ctrl Pts',(0.0023998005330824,-0.0335278710435082,
0.0735888900262716));
#102146=CARTESIAN_POINT('Ctrl Pts',(0.00241279490169981,-0.0333620469224319,
0.0734692020843839));
#102147=CARTESIAN_POINT('Ctrl Pts',(0.00242957618009863,-0.0331951640388601,
0.0733497885729815));
#102148=CARTESIAN_POINT('Ctrl Pts',(0.00238351587093777,-0.0336938721132425,
0.0737924460742568));
#102149=CARTESIAN_POINT('Ctrl Pts',(0.00239100094236228,-0.0335278710435082,
0.0736722787363431));
#102150=CARTESIAN_POINT('Ctrl Pts',(0.00240225179702995,-0.0333620469224319,
0.0735523884029136));
#102151=CARTESIAN_POINT('Ctrl Pts',(0.00241729397204338,-0.0331951640388601,
0.0734327173206421));
#102152=CARTESIAN_POINT('Ctrl Pts',(0.00243592986201132,-0.0330240426238155,
0.0733076125359522));
#102153=CARTESIAN_POINT('Ctrl Pts',(0.00244753457002689,-0.0329142774063506,
0.0732292568286855));
#102154=CARTESIAN_POINT('Ctrl Pts',(0.00246076489475772,-0.032804347972668,
0.0731511019599719));
#102155=CARTESIAN_POINT('Ctrl Pts',(0.0024756066445203,-0.0326943950436586,
0.0730732485187923));
#102156=CARTESIAN_POINT('Ctrl Pts',(0.00234349669882086,-0.0330240426238155,
0.0733731659212745));
#102157=CARTESIAN_POINT('Ctrl Pts',(0.00235419834508804,-0.0329142774063506,
0.0732935368571316));
#102158=CARTESIAN_POINT('Ctrl Pts',(0.00236655148170485,-0.032804347972668,
0.0732140893279181));
#102159=CARTESIAN_POINT('Ctrl Pts',(0.00238054308633687,-0.0326943950436586,
0.0731349255476614));
#102160=CARTESIAN_POINT('Ctrl Pts',(0.0022510635356304,-0.0330240426238155,
0.0734387193065969));
#102161=CARTESIAN_POINT('Ctrl Pts',(0.0022608621201492,-0.0329142774063506,
0.0733578168855778));
#102162=CARTESIAN_POINT('Ctrl Pts',(0.00227233806865199,-0.032804347972668,
0.0732770766958643));
#102163=CARTESIAN_POINT('Ctrl Pts',(0.00228547952815344,-0.0326943950436586,
0.0731966025765306));
#102164=CARTESIAN_POINT('Ctrl Pts',(0.00215863037243994,-0.0330240426238155,
0.0735042726919192));
#102165=CARTESIAN_POINT('Ctrl Pts',(0.00216752589521035,-0.0329142774063506,
0.0734220969140239));
#102166=CARTESIAN_POINT('Ctrl Pts',(0.00217812465559913,-0.032804347972668,
0.0733400640638104));
#102167=CARTESIAN_POINT('Ctrl Pts',(0.00219041596997002,-0.0326943950436586,
0.0732582796053997));
#102168=CARTESIAN_POINT('Origin',(0.0189642957816681,-0.0326396682857656,
0.0762912519078639));
#102169=CARTESIAN_POINT('Ctrl Pts',(0.00225277570667803,-0.0331951640388587,
0.0729125498651186));
#102170=CARTESIAN_POINT('Ctrl Pts',(0.00226981907894478,-0.0330855618255041,
0.0728316886277174));
#102171=CARTESIAN_POINT('Ctrl Pts',(0.00228854600109696,-0.0329757224427708,
0.0727511213559523));
#102172=CARTESIAN_POINT('Ctrl Pts',(0.00230893755295068,-0.0328657862078596,
0.072670952397367));
#102173=CARTESIAN_POINT('Ctrl Pts',(0.00232030016243826,-0.0331951640388587,
0.0730035531612891));
#102174=CARTESIAN_POINT('Ctrl Pts',(0.00233609014839843,-0.0330855618255041,
0.0729236219366652));
#102175=CARTESIAN_POINT('Ctrl Pts',(0.00235354355892097,-0.0329757224427708,
0.072843959442758));
#102176=CARTESIAN_POINT('Ctrl Pts',(0.00237264304779727,-0.0328657862078596,
0.0727646687884945));
#102177=CARTESIAN_POINT('Ctrl Pts',(0.00238782461819848,-0.0331951640388587,
0.0730945564574596));
#102178=CARTESIAN_POINT('Ctrl Pts',(0.00240236121785207,-0.0330855618255041,
0.0730155552456129));
#102179=CARTESIAN_POINT('Ctrl Pts',(0.00241854111674499,-0.0329757224427708,
0.0729367975295637));
#102180=CARTESIAN_POINT('Ctrl Pts',(0.00243634854264385,-0.0328657862078596,
0.072858385179622));
#102181=CARTESIAN_POINT('Ctrl Pts',(0.0024553490739587,-0.0331951640388587,
0.0731855597536301));
#102182=CARTESIAN_POINT('Ctrl Pts',(0.00246863228730572,-0.0330855618255041,
0.0731074885545606));
#102183=CARTESIAN_POINT('Ctrl Pts',(0.002483538674569,-0.0329757224427708,
0.0730296356163694));
#102184=CARTESIAN_POINT('Ctrl Pts',(0.00250005403749043,-0.0328657862078596,
0.0729521015707495));
#102185=CARTESIAN_POINT('Origin',(0.0188335865984539,-0.0326401908830343,
0.0767540563823664));
#102186=CARTESIAN_POINT('Ctrl Pts',(0.00244818769528571,-0.0332451089994432,
0.0732195419964954));
#102187=CARTESIAN_POINT('Ctrl Pts',(0.00248328049303606,-0.0329451141710258,
0.073005483447829));
#102188=CARTESIAN_POINT('Ctrl Pts',(0.00253439736081545,-0.0326442513127503,
0.0727946763498947));
#102189=CARTESIAN_POINT('Ctrl Pts',(0.00241311403098397,-0.0332451089994432,
0.0734670694456246));
#102190=CARTESIAN_POINT('Ctrl Pts',(0.00243887117825119,-0.0329451141710258,
0.0732516880720666));
#102191=CARTESIAN_POINT('Ctrl Pts',(0.00248077855772377,-0.0326442513127503,
0.0730388587078877));
#102192=CARTESIAN_POINT('Ctrl Pts',(0.00250004736902662,-0.0325229783203384,
0.0729521324465009));
#102193=CARTESIAN_POINT('Ctrl Pts',(0.0025165599467554,-0.0324130253112079,
0.0728746093863449));
#102194=CARTESIAN_POINT('Ctrl Pts',(0.00253467368408381,-0.0323031222247695,
0.0727974396679559));
#102195=CARTESIAN_POINT('Ctrl Pts',(0.00255436189055012,-0.0321934096636184,
0.0727207213215165));
#102196=CARTESIAN_POINT('Ctrl Pts',(0.0024036804549877,-0.0325229783203384,
0.0730117525817576));
#102197=CARTESIAN_POINT('Ctrl Pts',(0.00241937117047073,-0.0324130253112079,
0.0729329011058233));
#102198=CARTESIAN_POINT('Ctrl Pts',(0.00243669065019125,-0.0323031222247695,
0.07285438617186));
#102199=CARTESIAN_POINT('Ctrl Pts',(0.0024556131602716,-0.0321934096636184,
0.0727763075690764));
#102200=CARTESIAN_POINT('Ctrl Pts',(0.00230731354094878,-0.0325229783203384,
0.0730713727170144));
#102201=CARTESIAN_POINT('Ctrl Pts',(0.00232218239418606,-0.0324130253112079,
0.0729911928253016));
#102202=CARTESIAN_POINT('Ctrl Pts',(0.00233870761629869,-0.0323031222247695,
0.0729113326757642));
#102203=CARTESIAN_POINT('Ctrl Pts',(0.00235686442999307,-0.0321934096636184,
0.0728318938166364));
#102204=CARTESIAN_POINT('Ctrl Pts',(0.00221094662690986,-0.0325229783203384,
0.0731309928522712));
#102205=CARTESIAN_POINT('Ctrl Pts',(0.0022249936179014,-0.0324130253112079,
0.07304948454478));
#102206=CARTESIAN_POINT('Ctrl Pts',(0.00224072458240613,-0.0323031222247695,
0.0729682791796684));
#102207=CARTESIAN_POINT('Ctrl Pts',(0.00225811569971455,-0.0321934096636184,
0.0728874800641964));
#102208=CARTESIAN_POINT('Origin',(0.0189559809570794,-0.0326393375178101,
0.0762893665114488));
#102209=CARTESIAN_POINT('Ctrl Pts',(0.00234206093373601,-0.0326943950436593,
0.0725463481428483));
#102210=CARTESIAN_POINT('Ctrl Pts',(0.0023641622618914,-0.0325844576448127,
0.0724666651877939));
#102211=CARTESIAN_POINT('Ctrl Pts',(0.00238791312834463,-0.0324744968375319,
0.0723874336851549));
#102212=CARTESIAN_POINT('Ctrl Pts',(0.0024132817018894,-0.0323646534831894,
0.072308754731218));
#102213=CARTESIAN_POINT('Ctrl Pts',(0.00240373794242499,-0.0326943950436593,
0.0726414116699278));
#102214=CARTESIAN_POINT('Ctrl Pts',(0.00242452911700918,-0.0325844576448127,
0.0725625787396482));
#102215=CARTESIAN_POINT('Ctrl Pts',(0.00244695215726364,-0.0324744968375319,
0.0724841702258176));
#102216=CARTESIAN_POINT('Ctrl Pts',(0.00247097694781462,-0.0323646534831894,
0.0724062861937275));
#102217=CARTESIAN_POINT('Ctrl Pts',(0.00246541495111396,-0.0326943950436593,
0.0727364751970073));
#102218=CARTESIAN_POINT('Ctrl Pts',(0.00248489597212697,-0.0325844576448127,
0.0726584922915024));
#102219=CARTESIAN_POINT('Ctrl Pts',(0.00250599118618266,-0.0324744968375319,
0.0725809067664803));
#102220=CARTESIAN_POINT('Ctrl Pts',(0.00252867219373984,-0.0323646534831894,
0.0725038176562369));
#102221=CARTESIAN_POINT('Ctrl Pts',(0.00252709195980294,-0.0326943950436593,
0.0728315387240867));
#102222=CARTESIAN_POINT('Ctrl Pts',(0.00254526282724476,-0.0325844576448127,
0.0727544058433566));
#102223=CARTESIAN_POINT('Ctrl Pts',(0.00256503021510168,-0.0324744968375319,
0.072677643307143));
#102224=CARTESIAN_POINT('Ctrl Pts',(0.00258636743966506,-0.0323646534831894,
0.0726013491187464));
#102225=CARTESIAN_POINT('Origin',(0.0188704620442487,-0.0326395579068987,
0.0767625512829897));
#102226=CARTESIAN_POINT('Ctrl Pts',(0.00251780236267085,-0.0327445246961877,
0.0728650427475093));
#102227=CARTESIAN_POINT('Ctrl Pts',(0.00256626531720569,-0.0324436878365475,
0.0726536097639458));
#102228=CARTESIAN_POINT('Ctrl Pts',(0.00263051658990176,-0.0321434074463187,
0.0724464278669139));
#102229=CARTESIAN_POINT('Ctrl Pts',(0.00246725720085306,-0.0327445246961877,
0.0731098798088722));
#102230=CARTESIAN_POINT('Ctrl Pts',(0.00250648597475639,-0.0324436878365475,
0.0728965404833861));
#102231=CARTESIAN_POINT('Ctrl Pts',(0.00256167289361573,-0.0321434074463187,
0.072686762103929));
#102232=CARTESIAN_POINT('Ctrl Pts',(0.0026111396246973,-0.0322357242816073,
0.0725102143698205));
#102233=CARTESIAN_POINT('Ctrl Pts',(0.00266336467029447,-0.0319819883628706,
0.0723346438536521));
#102234=CARTESIAN_POINT('Ctrl Pts',(0.00272665592956285,-0.0317295851069887,
0.0721627523819745));
#102235=CARTESIAN_POINT('Ctrl Pts',(0.00254508625065872,-0.0322357242816073,
0.0727513304244044));
#102236=CARTESIAN_POINT('Ctrl Pts',(0.00258963206263345,-0.0319819883628706,
0.072573656193941));
#102237=CARTESIAN_POINT('Ctrl Pts',(0.002645393516558,-0.0317295851069887,
0.0723991766198027));
#102238=CARTESIAN_POINT('Origin',(0.0187782749196005,-0.0326371942644775,
0.0767383864827326));
#102239=CARTESIAN_POINT('Origin',(0.0188361706893204,-0.0326352985529264,
0.0762627337746027));
#102240=CARTESIAN_POINT('Ctrl Pts',(0.00245416397318719,-0.0321934096636183,
0.0721864753018188));
#102241=CARTESIAN_POINT('Ctrl Pts',(0.00248124250905315,-0.0320835708272303,
0.0721082868479344));
#102242=CARTESIAN_POINT('Ctrl Pts',(0.00250992344425711,-0.0319739230346346,
0.0720307041354232));
#102243=CARTESIAN_POINT('Ctrl Pts',(0.00254016246547428,-0.0318646057455575,
0.071953823609724));
#102244=CARTESIAN_POINT('Ctrl Pts',(0.00250975026861318,-0.0321934096636183,
0.0722852241171311));
#102245=CARTESIAN_POINT('Ctrl Pts',(0.00253546698135585,-0.0320835708272303,
0.072207802241582));
#102246=CARTESIAN_POINT('Ctrl Pts',(0.00256277101905045,-0.0319739230346346,
0.0721309574799007));
#102247=CARTESIAN_POINT('Ctrl Pts',(0.00259161990247846,-0.0318646057455575,
0.0720547854685705));
#102248=CARTESIAN_POINT('Ctrl Pts',(0.00256533656403917,-0.0321934096636183,
0.0723839729324434));
#102249=CARTESIAN_POINT('Ctrl Pts',(0.00258969145365854,-0.0320835708272303,
0.0723073176352295));
#102250=CARTESIAN_POINT('Ctrl Pts',(0.00261561859384379,-0.0319739230346346,
0.0722312108243781));
#102251=CARTESIAN_POINT('Ctrl Pts',(0.00264307733948264,-0.0318646057455575,
0.0721557473274169));
#102252=CARTESIAN_POINT('Ctrl Pts',(0.00262092285946516,-0.0321934096636183,
0.0724827217477557));
#102253=CARTESIAN_POINT('Ctrl Pts',(0.00264391592596123,-0.0320835708272303,
0.0724068330288771));
#102254=CARTESIAN_POINT('Ctrl Pts',(0.00266846616863713,-0.0319739230346346,
0.0723314641688556));
#102255=CARTESIAN_POINT('Ctrl Pts',(0.00269453477648683,-0.0318646057455575,
0.0722567091862634));
#102256=CARTESIAN_POINT('Ctrl Pts',(0.00258544407064685,-0.0320218834582398,
0.07260157866145));
#102257=CARTESIAN_POINT('Ctrl Pts',(0.00260155939349681,-0.0319391099350682,
0.0725439379504409));
#102258=CARTESIAN_POINT('Ctrl Pts',(0.00261856502026669,-0.0318564869454951,
0.0724865838055));
#102259=CARTESIAN_POINT('Ctrl Pts',(0.00263644466463766,-0.0317740741446532,
0.0724295568451632));
#102260=CARTESIAN_POINT('Ctrl Pts',(0.00254173679643626,-0.0320218834582398,
0.0726249560485665));
#102261=CARTESIAN_POINT('Ctrl Pts',(0.00255760881720081,-0.0319391099350682,
0.0725668604504945));
#102262=CARTESIAN_POINT('Ctrl Pts',(0.0025743783924211,-0.0318564869454951,
0.0725090478948991));
#102263=CARTESIAN_POINT('Ctrl Pts',(0.00259202937653946,-0.0317740741446532,
0.0724515593502585));
#102264=CARTESIAN_POINT('Ctrl Pts',(0.00249802952222568,-0.0320218834582398,
0.0726483334356829));
#102265=CARTESIAN_POINT('Ctrl Pts',(0.00251365824090481,-0.0319391099350682,
0.0725897829505481));
#102266=CARTESIAN_POINT('Ctrl Pts',(0.0025301917645755,-0.0318564869454951,
0.0725315119842981));
#102267=CARTESIAN_POINT('Ctrl Pts',(0.00254761408844127,-0.0317740741446532,
0.0724735618553538));
#102268=CARTESIAN_POINT('Ctrl Pts',(0.00245432224801509,-0.0320218834582398,
0.0726717108227994));
#102269=CARTESIAN_POINT('Ctrl Pts',(0.00246970766460881,-0.0319391099350682,
0.0726127054506017));
#102270=CARTESIAN_POINT('Ctrl Pts',(0.00248600513672991,-0.0318564869454951,
0.0725539760736971));
#102271=CARTESIAN_POINT('Ctrl Pts',(0.00250319880034307,-0.0317740741446532,
0.072495564360449));
#102272=CARTESIAN_POINT('Origin',(-0.00372643980148012,-0.039122885339058,
0.071814864670307));
#102273=CARTESIAN_POINT('Ctrl Pts',(0.00256742115659057,-0.0352722978779646,
0.0756369487464146));
#102274=CARTESIAN_POINT('Ctrl Pts',(0.0025628750924334,-0.0352466642097251,
0.0756186068277919));
#102275=CARTESIAN_POINT('Ctrl Pts',(0.00255825697983851,-0.0352210183808318,
0.0756003001107925));
#102276=CARTESIAN_POINT('Ctrl Pts',(0.00255356613949293,-0.0351953608940152,
0.0755820280796471));
#102277=CARTESIAN_POINT('Origin',(-0.00222897559393711,-0.0352456003065129,
0.0766391071207262));
#102278=CARTESIAN_POINT('Ctrl Pts',(0.00252524734178226,-0.0350241211493339,
0.0754606058365681));
#102279=CARTESIAN_POINT('Ctrl Pts',(0.00250719428456688,-0.0349144232867421,
0.075383488317957));
#102280=CARTESIAN_POINT('Ctrl Pts',(0.00249072449587003,-0.0348045283677512,
0.0753059514712201));
#102281=CARTESIAN_POINT('Ctrl Pts',(0.00247586276713219,-0.0346945769586886,
0.0752280938261766));
#102282=CARTESIAN_POINT('Ctrl Pts',(0.00246343695443706,-0.0350241211493339,
0.0755555827696585));
#102283=CARTESIAN_POINT('Ctrl Pts',(0.0024440756289694,-0.0349144232867421,
0.0754776138383434));
#102284=CARTESIAN_POINT('Ctrl Pts',(0.0024263143882669,-0.0348045283677512,
0.0753991980264526));
#102285=CARTESIAN_POINT('Ctrl Pts',(0.00241017971985099,-0.0346945769586886,
0.0753204349280917));
#102286=CARTESIAN_POINT('Ctrl Pts',(0.00240162656709186,-0.0350241211493339,
0.075650559702749));
#102287=CARTESIAN_POINT('Ctrl Pts',(0.00238095697337193,-0.0349144232867421,
0.0755717393587299));
#102288=CARTESIAN_POINT('Ctrl Pts',(0.00236190428066376,-0.0348045283677512,
0.0754924445816851));
#102289=CARTESIAN_POINT('Ctrl Pts',(0.00234449667256979,-0.0346945769586886,
0.0754127760300068));
#102290=CARTESIAN_POINT('Ctrl Pts',(0.00233981617974666,-0.0350241211493339,
0.0757455366358395));
#102291=CARTESIAN_POINT('Ctrl Pts',(0.00231783831777446,-0.0349144232867421,
0.0756658648791163));
#102292=CARTESIAN_POINT('Ctrl Pts',(0.00229749417306063,-0.0348045283677512,
0.0755856911369176));
#102293=CARTESIAN_POINT('Ctrl Pts',(0.0022788136252886,-0.0346945769586886,
0.0755051171319219));
#102294=CARTESIAN_POINT('Origin',(0.0189997036149989,-0.0345629067943529,
0.0722572971807028));
#102295=CARTESIAN_POINT('Ctrl Pts',(0.00228856946677351,-0.035197097365162,
0.0752110439272844));
#102296=CARTESIAN_POINT('Ctrl Pts',(0.00227387014112994,-0.0350869349321768,
0.0751302049630735));
#102297=CARTESIAN_POINT('Ctrl Pts',(0.00226083923600357,-0.034976498512971,
0.0750489934419713));
#102298=CARTESIAN_POINT('Ctrl Pts',(0.00224949982670333,-0.034865930684962,
0.0749675135821197));
#102299=CARTESIAN_POINT('Ctrl Pts',(0.00235844150412178,-0.035197097365162,
0.0752543840824171));
#102300=CARTESIAN_POINT('Ctrl Pts',(0.00234314175936515,-0.0350869349321768,
0.0751745131005903));
#102301=CARTESIAN_POINT('Ctrl Pts',(0.00232948981392817,-0.034976498512971,
0.0750942578813569));
#102302=CARTESIAN_POINT('Ctrl Pts',(0.00231750947476583,-0.034865930684962,
0.0750137213565797));
#102303=CARTESIAN_POINT('Ctrl Pts',(0.00242831354147005,-0.035197097365162,
0.0752977242375498));
#102304=CARTESIAN_POINT('Ctrl Pts',(0.00241241337760036,-0.0350869349321768,
0.0752188212381071));
#102305=CARTESIAN_POINT('Ctrl Pts',(0.00239814039185277,-0.034976498512971,
0.0751395223207425));
#102306=CARTESIAN_POINT('Ctrl Pts',(0.00238551912282833,-0.034865930684962,
0.0750599291310396));
#102307=CARTESIAN_POINT('Ctrl Pts',(0.00249818557881832,-0.035197097365162,
0.0753410643926826));
#102308=CARTESIAN_POINT('Ctrl Pts',(0.00248168499583556,-0.0350869349321768,
0.075263129375624));
#102309=CARTESIAN_POINT('Ctrl Pts',(0.00246679096977737,-0.034976498512971,
0.0751847867601281));
#102310=CARTESIAN_POINT('Ctrl Pts',(0.00245352877089082,-0.034865930684962,
0.0751061369054996));
#102311=CARTESIAN_POINT('Origin',(0.019037000149744,-0.0345637187967391,
0.0727368118570569));
#102312=CARTESIAN_POINT('Ctrl Pts',(0.00250422216522004,-0.0352450361861252,
0.0753742018187211));
#102313=CARTESIAN_POINT('Ctrl Pts',(0.0024580506371754,-0.0349452761023765,
0.0751622566398639));
#102314=CARTESIAN_POINT('Ctrl Pts',(0.0024279748552457,-0.0346444289983475,
0.0749474357465967));
#102315=CARTESIAN_POINT('Ctrl Pts',(0.00256273217342888,-0.0352450361861252,
0.0756172585588856));
#102316=CARTESIAN_POINT('Ctrl Pts',(0.00250739361024074,-0.0349452761023765,
0.0754075201211421));
#102317=CARTESIAN_POINT('Ctrl Pts',(0.00246801061498241,-0.0346444289983475,
0.0751942092012921));
#102318=CARTESIAN_POINT('Ctrl Pts',(0.00245400125847058,-0.0345231616327822,
0.0751064857114735));
#102319=CARTESIAN_POINT('Ctrl Pts',(0.00244081744956218,-0.0344132092796975,
0.0750283357637031));
#102320=CARTESIAN_POINT('Ctrl Pts',(0.00242925079090351,-0.0343032738558974,
0.0749499171514227));
#102321=CARTESIAN_POINT('Ctrl Pts',(0.00241931352731584,-0.0341934961088741,
0.0748713307175119));
#102322=CARTESIAN_POINT('Ctrl Pts',(0.00238634921831221,-0.0345231616327822,
0.0751973941137306));
#102323=CARTESIAN_POINT('Ctrl Pts',(0.00237191236506749,-0.0344132092796975,
0.0751183116778331));
#102324=CARTESIAN_POINT('Ctrl Pts',(0.00235911201450521,-0.0343032738558974,
0.075038934707304));
#102325=CARTESIAN_POINT('Ctrl Pts',(0.00234796196049881,-0.0341934961088741,
0.0749593653132757));
#102326=CARTESIAN_POINT('Ctrl Pts',(0.00231869717815384,-0.0345231616327822,
0.0752883025159877));
#102327=CARTESIAN_POINT('Ctrl Pts',(0.0023030072805728,-0.0344132092796975,
0.0752082875919631));
#102328=CARTESIAN_POINT('Ctrl Pts',(0.00228897323810691,-0.0343032738558974,
0.0751279522631852));
#102329=CARTESIAN_POINT('Ctrl Pts',(0.00227661039368177,-0.0341934961088741,
0.0750473999090394));
#102330=CARTESIAN_POINT('Ctrl Pts',(0.00225104513799546,-0.0345231616327822,
0.0753792109182449));
#102331=CARTESIAN_POINT('Ctrl Pts',(0.00223410219607811,-0.0344132092796975,
0.0752982635060931));
#102332=CARTESIAN_POINT('Ctrl Pts',(0.00221883446170861,-0.0343032738558974,
0.0752169698190665));
#102333=CARTESIAN_POINT('Ctrl Pts',(0.00220525882686474,-0.0341934961088741,
0.0751354345048032));
#102334=CARTESIAN_POINT('Origin',(0.0190115825377258,-0.0345625596229667,
0.0722549756521341));
#102335=CARTESIAN_POINT('Ctrl Pts',(0.00215773009560743,-0.0346945769586885,
0.074787355764023));
#102336=CARTESIAN_POINT('Ctrl Pts',(0.00214894701102897,-0.0345846629176052,
0.0747051405505901));
#102337=CARTESIAN_POINT('Ctrl Pts',(0.002141862603128,-0.0344746925050311,
0.0746227296640146));
#102338=CARTESIAN_POINT('Ctrl Pts',(0.00213648551317482,-0.0343648066253259,
0.0745402287361092));
#102339=CARTESIAN_POINT('Ctrl Pts',(0.00225007112481624,-0.0346945769586885,
0.0748530387595875));
#102340=CARTESIAN_POINT('Ctrl Pts',(0.00224038289535956,-0.0345846629176052,
0.0747720960522108));
#102341=CARTESIAN_POINT('Ctrl Pts',(0.00223236687307674,-0.0344746925050311,
0.0746909391710142));
#102342=CARTESIAN_POINT('Ctrl Pts',(0.00222603289956556,-0.0343648066253259,
0.074609672145964));
#102343=CARTESIAN_POINT('Ctrl Pts',(0.00234241215402504,-0.0346945769586885,
0.0749187217551521));
#102344=CARTESIAN_POINT('Ctrl Pts',(0.00233181877969015,-0.0345846629176052,
0.0748390515538314));
#102345=CARTESIAN_POINT('Ctrl Pts',(0.00232287114302549,-0.0344746925050311,
0.0747591486780137));
#102346=CARTESIAN_POINT('Ctrl Pts',(0.0023155802859563,-0.0343648066253259,
0.0746791155558189));
#102347=CARTESIAN_POINT('Ctrl Pts',(0.00243475318323385,-0.0346945769586885,
0.0749844047507166));
#102348=CARTESIAN_POINT('Ctrl Pts',(0.00242325466402074,-0.0345846629176052,
0.074906007055452));
#102349=CARTESIAN_POINT('Ctrl Pts',(0.00241337541297424,-0.0344746925050311,
0.0748273581850132));
#102350=CARTESIAN_POINT('Ctrl Pts',(0.00240512767234704,-0.0343648066253259,
0.0747485589656737));
#102351=CARTESIAN_POINT('Origin',(0.0190948417673933,-0.0345626446727627,
0.0727285367187088));
#102352=CARTESIAN_POINT('Ctrl Pts',(0.0024331008925787,-0.0346945769586885,
0.0749832294616745));
#102353=CARTESIAN_POINT('Ctrl Pts',(0.00241564856789733,-0.034527515336289,
0.0748640358634123));
#102354=CARTESIAN_POINT('Ctrl Pts',(0.002401940258106,-0.0343603235965158,
0.0747442625760329));
#102355=CARTESIAN_POINT('Ctrl Pts',(0.00239201124142713,-0.0341934961088739,
0.074624264438329));
#102356=CARTESIAN_POINT('Ctrl Pts',(0.00244704620944235,-0.0346945769586885,
0.0750658947897682));
#102357=CARTESIAN_POINT('Ctrl Pts',(0.0024278624263667,-0.034527515336289,
0.0749469932817511));
#102358=CARTESIAN_POINT('Ctrl Pts',(0.00241241302436789,-0.0343603235965158,
0.0748274577073935));
#102359=CARTESIAN_POINT('Ctrl Pts',(0.00240073844149539,-0.0341934961088739,
0.0747076422789716));
#102360=CARTESIAN_POINT('Ctrl Pts',(0.002460991526306,-0.0346945769586885,
0.0751485601178619));
#102361=CARTESIAN_POINT('Ctrl Pts',(0.00244007628483606,-0.034527515336289,
0.0750299507000899));
#102362=CARTESIAN_POINT('Ctrl Pts',(0.00242288579062979,-0.0343603235965158,
0.0749106528387541));
#102363=CARTESIAN_POINT('Ctrl Pts',(0.00240946564156365,-0.0341934961088739,
0.0747910201196143));
#102364=CARTESIAN_POINT('Ctrl Pts',(0.00247493684316965,-0.0346945769586885,
0.0752312254459556));
#102365=CARTESIAN_POINT('Ctrl Pts',(0.00245229014330543,-0.034527515336289,
0.0751129081184287));
#102366=CARTESIAN_POINT('Ctrl Pts',(0.00243335855689168,-0.0343603235965158,
0.0749938479701148));
#102367=CARTESIAN_POINT('Ctrl Pts',(0.00241819284163192,-0.0341934961088739,
0.074874397960257));
#102368=CARTESIAN_POINT('Ctrl Pts',(0.00240513151098137,-0.0340223579322366,
0.0747485902905886));
#102369=CARTESIAN_POINT('Ctrl Pts',(0.00239687538968521,-0.0339125849573555,
0.0746697151828158));
#102370=CARTESIAN_POINT('Ctrl Pts',(0.00239025760132036,-0.0338030433565222,
0.0745907246171416));
#102371=CARTESIAN_POINT('Ctrl Pts',(0.00238527765431292,-0.0336938721132328,
0.0745117203593975));
#102372=CARTESIAN_POINT('Ctrl Pts',(0.0023319046701551,-0.0340223579322366,
0.0748350715579995));
#102373=CARTESIAN_POINT('Ctrl Pts',(0.00232245574662875,-0.0339125849573555,
0.0747551864611081));
#102374=CARTESIAN_POINT('Ctrl Pts',(0.00231466689862988,-0.0338030433565222,
0.0746751619277885));
#102375=CARTESIAN_POINT('Ctrl Pts',(0.00230853901495878,-0.0336938721132328,
0.0745951011788974));
#102376=CARTESIAN_POINT('Ctrl Pts',(0.00225867782932883,-0.0340223579322366,
0.0749215528254104));
#102377=CARTESIAN_POINT('Ctrl Pts',(0.00224803610357228,-0.0339125849573555,
0.0748406577394004));
#102378=CARTESIAN_POINT('Ctrl Pts',(0.00223907619593939,-0.0338030433565222,
0.0747595992384354));
#102379=CARTESIAN_POINT('Ctrl Pts',(0.00223180037560463,-0.0336938721132328,
0.0746784819983972));
#102380=CARTESIAN_POINT('Ctrl Pts',(0.00218545098850257,-0.0340223579322366,
0.0750080340928213));
#102381=CARTESIAN_POINT('Ctrl Pts',(0.00217361646051582,-0.0339125849573555,
0.0749261290176926));
#102382=CARTESIAN_POINT('Ctrl Pts',(0.00216348549324891,-0.0338030433565222,
0.0748440365490823));
#102383=CARTESIAN_POINT('Ctrl Pts',(0.00215506173625048,-0.0336938721132328,
0.074761862817897));
#102384=CARTESIAN_POINT('Origin',(0.018892725961209,-0.0345589643414346,
0.0722730309108332));
#102385=CARTESIAN_POINT('Ctrl Pts',(0.00212948283705902,-0.034193496108874,
0.0744114865772719));
#102386=CARTESIAN_POINT('Ctrl Pts',(0.00212587709205058,-0.0340836138595105,
0.0743288287398881));
#102387=CARTESIAN_POINT('Ctrl Pts',(0.00212398350762951,-0.0339738896671456,
0.074246135949962));
#102388=CARTESIAN_POINT('Ctrl Pts',(0.0021237974126069,-0.0338644633335883,
0.0741635142065129));
#102389=CARTESIAN_POINT('Ctrl Pts',(0.00221751751203453,-0.034193496108874,
0.0744828382082896));
#102390=CARTESIAN_POINT('Ctrl Pts',(0.00221292787029965,-0.0340836138595105,
0.0744013943169262));
#102391=CARTESIAN_POINT('Ctrl Pts',(0.00221002574117891,-0.0339738896671456,
0.0743198945308684));
#102392=CARTESIAN_POINT('Ctrl Pts',(0.00220880784665147,-0.0338644633335883,
0.0742384434087674));
#102393=CARTESIAN_POINT('Ctrl Pts',(0.00230555218701004,-0.034193496108874,
0.0745541898393074));
#102394=CARTESIAN_POINT('Ctrl Pts',(0.00229997864854872,-0.0340836138595105,
0.0744739598939644));
#102395=CARTESIAN_POINT('Ctrl Pts',(0.00229606797472831,-0.0339738896671456,
0.0743936531117748));
#102396=CARTESIAN_POINT('Ctrl Pts',(0.00229381828069604,-0.0338644633335883,
0.0743133726110218));
#102397=CARTESIAN_POINT('Ctrl Pts',(0.00239358686198556,-0.034193496108874,
0.0746255414703251));
#102398=CARTESIAN_POINT('Ctrl Pts',(0.00238702942679779,-0.0340836138595105,
0.0745465254710025));
#102399=CARTESIAN_POINT('Ctrl Pts',(0.00238211020827771,-0.0339738896671456,
0.0744674116926812));
#102400=CARTESIAN_POINT('Ctrl Pts',(0.00237882871474061,-0.0338644633335883,
0.0743883018132763));
#102401=CARTESIAN_POINT('Origin',(0.0190200512712865,-0.0345610621861553,
0.0727370764658675));
#102402=CARTESIAN_POINT('Ctrl Pts',(0.00239510786684413,-0.03424362768739,
0.07466030918432));
#102403=CARTESIAN_POINT('Ctrl Pts',(0.00237586123867319,-0.0339430054201859,
0.0744442486703066));
#102404=CARTESIAN_POINT('Ctrl Pts',(0.00237294385135072,-0.033644143478416,
0.0742273522266683));
#102405=CARTESIAN_POINT('Ctrl Pts',(0.00242269681044828,-0.03424362768739,
0.0749087822214706));
#102406=CARTESIAN_POINT('Ctrl Pts',(0.00239407886719331,-0.0339430054201859,
0.0746937622416185));
#102407=CARTESIAN_POINT('Ctrl Pts',(0.00238173841041401,-0.033644143478416,
0.0744771974902433));
#102408=CARTESIAN_POINT('Ctrl Pts',(0.00237882999042919,-0.0335235895815127,
0.0743883295122386));
#102409=CARTESIAN_POINT('Ctrl Pts',(0.00237554891546564,-0.0334144449262719,
0.0743092389343998));
#102410=CARTESIAN_POINT('Ctrl Pts',(0.00237389802276031,-0.0333049234473133,
0.0742299897065297));
#102411=CARTESIAN_POINT('Ctrl Pts',(0.0023738886026999,-0.0331951640388588,
0.0741506829728378));
#102412=CARTESIAN_POINT('Ctrl Pts',(0.00230031742752324,-0.0335235895815127,
0.0744700421180732));
#102413=CARTESIAN_POINT('Ctrl Pts',(0.00229591141766308,-0.0334144449262719,
0.074389870660229));
#102414=CARTESIAN_POINT('Ctrl Pts',(0.00229315662781468,-0.0333049234473133,
0.0743095160702449));
#102415=CARTESIAN_POINT('Ctrl Pts',(0.00229206588794388,-0.0331951640388588,
0.0742290807778854));
#102416=CARTESIAN_POINT('Ctrl Pts',(0.00222180486461729,-0.0335235895815127,
0.0745517547239077));
#102417=CARTESIAN_POINT('Ctrl Pts',(0.00221627391986051,-0.0334144449262719,
0.0744705023860581));
#102418=CARTESIAN_POINT('Ctrl Pts',(0.00221241523286906,-0.0333049234473133,
0.0743890424339601));
#102419=CARTESIAN_POINT('Ctrl Pts',(0.00221024317318787,-0.0331951640388588,
0.074307478582933));
#102420=CARTESIAN_POINT('Ctrl Pts',(0.00214329230171133,-0.0335235895815127,
0.0746334673297422));
#102421=CARTESIAN_POINT('Ctrl Pts',(0.00213663642205794,-0.0334144449262719,
0.0745511341118873));
#102422=CARTESIAN_POINT('Ctrl Pts',(0.00213167383792343,-0.0333049234473133,
0.0744685687976754));
#102423=CARTESIAN_POINT('Ctrl Pts',(0.00212842045843185,-0.0331951640388588,
0.0743858763879806));
#102424=CARTESIAN_POINT('Origin',(0.0190236485971153,-0.0326434571770372,
0.0749098490912811));
#102425=CARTESIAN_POINT('Ctrl Pts',(0.00212340043994126,-0.0336938721132408,
0.0740332123687434));
#102426=CARTESIAN_POINT('Ctrl Pts',(0.00212408403670126,-0.0336474569764967,
0.0739980901432037));
#102427=CARTESIAN_POINT('Ctrl Pts',(0.00212517873661592,-0.033601104548885,
0.0739629783266245));
#102428=CARTESIAN_POINT('Ctrl Pts',(0.00212795026487169,-0.0334837508694616,
0.0738740832874839));
#102429=CARTESIAN_POINT('Ctrl Pts',(0.00213335472016756,-0.0333660264863617,
0.0737853094106077));
#102430=CARTESIAN_POINT('Ctrl Pts',(0.00237354227162489,-0.0336938721132408,
0.0742634277099222));
#102431=CARTESIAN_POINT('Ctrl Pts',(0.0023728783415994,-0.0336474569764967,
0.0742297696475292));
#102432=CARTESIAN_POINT('Ctrl Pts',(0.00237260846718368,-0.033601104548885,
0.0741961061192689));
#102433=CARTESIAN_POINT('Ctrl Pts',(0.00237192520727048,-0.0334837508694616,
0.0741108778128509));
#102434=CARTESIAN_POINT('Ctrl Pts',(0.00237376773860192,-0.0333660264863617,
0.0740256666860111));
#102435=CARTESIAN_POINT('Ctrl Pts',(0.00237354227163478,-0.0336938721132427,
0.0742634277099263));
#102436=CARTESIAN_POINT('Ctrl Pts',(0.00237287834160937,-0.0336474569765026,
0.0742297696475362));
#102437=CARTESIAN_POINT('Ctrl Pts',(0.00237260846719368,-0.0336011045488949,
0.0741961061192789));
#102438=CARTESIAN_POINT('Ctrl Pts',(0.00237193089790498,-0.033484728265791,
0.0741115876485763));
#102439=CARTESIAN_POINT('Ctrl Pts',(0.00237373722885253,-0.0333679870047995,
0.0740270857660023));
#102440=CARTESIAN_POINT('Ctrl Pts',(0.00237354227162492,-0.0336938721132425,
0.0742634277099235));
#102441=CARTESIAN_POINT('Ctrl Pts',(0.00237116776403552,-0.0335278710435082,
0.0741430515836346));
#102442=CARTESIAN_POINT('Ctrl Pts',(0.00237256905581545,-0.0333620469224319,
0.0740226433414466));
#102443=CARTESIAN_POINT('Ctrl Pts',(0.00237776687175776,-0.0331951640388601,
0.0739021433341537));
#102444=CARTESIAN_POINT('Ctrl Pts',(0.00237701691299514,-0.0336938721132425,
0.0743471890177609));
#102445=CARTESIAN_POINT('Ctrl Pts',(0.00237288893739257,-0.0335278710435082,
0.0742268856299792));
#102446=CARTESIAN_POINT('Ctrl Pts',(0.00237253509696462,-0.0333620469224319,
0.0741064951124082));
#102447=CARTESIAN_POINT('Ctrl Pts',(0.00237597524068128,-0.0331951640388601,
0.0739859575327203));
#102448=CARTESIAN_POINT('Ctrl Pts',(0.00238049155436535,-0.0336938721132425,
0.0744309503255982));
#102449=CARTESIAN_POINT('Ctrl Pts',(0.00237461011074962,-0.0335278710435082,
0.0743107196763237));
#102450=CARTESIAN_POINT('Ctrl Pts',(0.0023725011381138,-0.0333620469224319,
0.0741903468833699));
#102451=CARTESIAN_POINT('Ctrl Pts',(0.0023741836096048,-0.0331951640388601,
0.0740697717312869));
#102452=CARTESIAN_POINT('Ctrl Pts',(0.00238396619573556,-0.0336938721132425,
0.0745147116334355));
#102453=CARTESIAN_POINT('Ctrl Pts',(0.00237633128410666,-0.0335278710435082,
0.0743945537226684));
#102454=CARTESIAN_POINT('Ctrl Pts',(0.00237246717926298,-0.0333620469224319,
0.0742741986543316));
#102455=CARTESIAN_POINT('Ctrl Pts',(0.00237239197852832,-0.0331951640388601,
0.0741535859298535));
#102456=CARTESIAN_POINT('Ctrl Pts',(0.00237520113173803,-0.0330240426238155,
0.0740271319374078));
#102457=CARTESIAN_POINT('Ctrl Pts',(0.00237689375900478,-0.0329142774063508,
0.0739479396327167));
#102458=CARTESIAN_POINT('Ctrl Pts',(0.00238022435625873,-0.0328043479726686,
0.0738687428391072));
#102459=CARTESIAN_POINT('Ctrl Pts',(0.00238519145086425,-0.0326943950436594,
0.0737896431310757));
#102460=CARTESIAN_POINT('Ctrl Pts',(0.00229171284940129,-0.0330240426238155,
0.0741037533619383));
#102461=CARTESIAN_POINT('Ctrl Pts',(0.0022923499418965,-0.0329142774063508,
0.0740234109248193));
#102462=CARTESIAN_POINT('Ctrl Pts',(0.00229464825460635,-0.0328043479726686,
0.0739430416045468));
#102463=CARTESIAN_POINT('Ctrl Pts',(0.00229860767869599,-0.0326943950436594,
0.0738627484412915));
#102464=CARTESIAN_POINT('Ctrl Pts',(0.00220822456706454,-0.0330240426238155,
0.0741803747864688));
#102465=CARTESIAN_POINT('Ctrl Pts',(0.00220780612478822,-0.0329142774063508,
0.074098882216922));
#102466=CARTESIAN_POINT('Ctrl Pts',(0.00220907215295397,-0.0328043479726686,
0.0740173403699864));
#102467=CARTESIAN_POINT('Ctrl Pts',(0.00221202390652774,-0.0326943950436594,
0.0739358537515073));
#102468=CARTESIAN_POINT('Ctrl Pts',(0.0021247362847278,-0.0330240426238155,
0.0742569962109993));
#102469=CARTESIAN_POINT('Ctrl Pts',(0.00212326230767993,-0.0329142774063508,
0.0741743535090246));
#102470=CARTESIAN_POINT('Ctrl Pts',(0.00212349605130159,-0.0328043479726686,
0.074091639135426));
#102471=CARTESIAN_POINT('Ctrl Pts',(0.00212544013435949,-0.0326943950436594,
0.0740089590617231));
#102472=CARTESIAN_POINT('Origin',(0.0191471851194885,-0.0326396682855343,
0.0749156908757754));
#102473=CARTESIAN_POINT('Ctrl Pts',(0.00214397671962881,-0.0331951640388587,
0.0736581397562618));
#102474=CARTESIAN_POINT('Ctrl Pts',(0.00215075109946113,-0.0330855618255041,
0.0735757800329126));
#102475=CARTESIAN_POINT('Ctrl Pts',(0.00215923259754889,-0.0329757224427708,
0.0734935009524415));
#102476=CARTESIAN_POINT('Ctrl Pts',(0.00216941552111462,-0.0328657862078596,
0.0734114084109088));
#102477=CARTESIAN_POINT('Ctrl Pts',(0.00222237446226089,-0.0331951640388587,
0.0737399624058756));
#102478=CARTESIAN_POINT('Ctrl Pts',(0.00222802190062066,-0.0330855618255041,
0.0736586824528338));
#102479=CARTESIAN_POINT('Ctrl Pts',(0.00223535332783296,-0.0329757224427708,
0.0735774606291075));
#102480=CARTESIAN_POINT('Ctrl Pts',(0.00224436445744446,-0.0328657862078596,
0.0734964014046356));
#102481=CARTESIAN_POINT('Ctrl Pts',(0.00230077220489298,-0.0331951640388587,
0.0738217850554894));
#102482=CARTESIAN_POINT('Ctrl Pts',(0.00230529270178019,-0.0330855618255041,
0.073741584872755));
#102483=CARTESIAN_POINT('Ctrl Pts',(0.00231147405811704,-0.0329757224427708,
0.0736614203057736));
#102484=CARTESIAN_POINT('Ctrl Pts',(0.0023193133937743,-0.0328657862078596,
0.0735813943983625));
#102485=CARTESIAN_POINT('Ctrl Pts',(0.00237916994752506,-0.0331951640388587,
0.0739036077051031));
#102486=CARTESIAN_POINT('Ctrl Pts',(0.00238256350293971,-0.0330855618255041,
0.0738244872926761));
#102487=CARTESIAN_POINT('Ctrl Pts',(0.00238759478840111,-0.0329757224427708,
0.0737453799824396));
#102488=CARTESIAN_POINT('Ctrl Pts',(0.00239426233010414,-0.0328657862078596,
0.0736663873920893));
#102489=CARTESIAN_POINT('Origin',(0.0190755113989164,-0.0326401908835166,
0.0753912282023842));
#102490=CARTESIAN_POINT('Ctrl Pts',(0.00237632414284395,-0.0332451089994431,
0.0739382195465792));
#102491=CARTESIAN_POINT('Ctrl Pts',(0.00238431157332591,-0.0329451141710257,
0.0737214506196884));
#102492=CARTESIAN_POINT('Ctrl Pts',(0.00240860423409257,-0.0326442513127503,
0.073505899156358));
#102493=CARTESIAN_POINT('Ctrl Pts',(0.00237255046045652,-0.0332451089994431,
0.0741881910635991));
#102494=CARTESIAN_POINT('Ctrl Pts',(0.00237111006092671,-0.0329451141710257,
0.0739712798099484));
#102495=CARTESIAN_POINT('Ctrl Pts',(0.00238601239578505,-0.0326442513127503,
0.0737548762814957));
#102496=CARTESIAN_POINT('Ctrl Pts',(0.00239425958398091,-0.0325229783203385,
0.0736664188601564));
#102497=CARTESIAN_POINT('Ctrl Pts',(0.0024009257392971,-0.0324130253112079,
0.0735874375177236));
#102498=CARTESIAN_POINT('Ctrl Pts',(0.00240922471405741,-0.0323031222247695,
0.0735086060523421));
#102499=CARTESIAN_POINT('Ctrl Pts',(0.00241914231470219,-0.0321934096636184,
0.0734300250663995));
#102500=CARTESIAN_POINT('Ctrl Pts',(0.00230612493617983,-0.0325229783203385,
0.0737376468497841));
#102501=CARTESIAN_POINT('Ctrl Pts',(0.00231180921523453,-0.0324130253112079,
0.0736574505731809));
#102502=CARTESIAN_POINT('Ctrl Pts',(0.00231915159512767,-0.0323031222247695,
0.0735773840465261));
#102503=CARTESIAN_POINT('Ctrl Pts',(0.0023281390518051,-0.0321934096636184,
0.0734975494974708));
#102504=CARTESIAN_POINT('Ctrl Pts',(0.00221799028837875,-0.0325229783203385,
0.0738088748394118));
#102505=CARTESIAN_POINT('Ctrl Pts',(0.00222269269117196,-0.0324130253112079,
0.0737274636286381));
#102506=CARTESIAN_POINT('Ctrl Pts',(0.00222907847619793,-0.0323031222247695,
0.0736461620407101));
#102507=CARTESIAN_POINT('Ctrl Pts',(0.002237135788908,-0.0321934096636184,
0.0735650739285422));
#102508=CARTESIAN_POINT('Ctrl Pts',(0.00212985564057767,-0.0325229783203385,
0.0738801028290395));
#102509=CARTESIAN_POINT('Ctrl Pts',(0.00213357616710938,-0.0324130253112079,
0.0737974766840954));
#102510=CARTESIAN_POINT('Ctrl Pts',(0.00213900535726818,-0.0323031222247695,
0.0737149400348941));
#102511=CARTESIAN_POINT('Ctrl Pts',(0.00214613252601091,-0.0321934096636184,
0.0736325983596135));
#102512=CARTESIAN_POINT('Origin',(0.0191386995571209,-0.0326393375178722,
0.0749148624697292));
#102513=CARTESIAN_POINT('Ctrl Pts',(0.00218666066001428,-0.0326943950436593,
0.0732836352377341));
#102514=CARTESIAN_POINT('Ctrl Pts',(0.00219860079017889,-0.0325844576448126,
0.0732018105756567));
#102515=CARTESIAN_POINT('Ctrl Pts',(0.00221223403353018,-0.0324744968375319,
0.0731202270641886));
#102516=CARTESIAN_POINT('Ctrl Pts',(0.00222754148058497,-0.0323646534831895,
0.0730389889919505));
#102517=CARTESIAN_POINT('Ctrl Pts',(0.00225976594631064,-0.0326943950436593,
0.0733702189815729));
#102518=CARTESIAN_POINT('Ctrl Pts',(0.00227051279020992,-0.0325844576448126,
0.0732894018473545));
#102519=CARTESIAN_POINT('Ctrl Pts',(0.00228293182551718,-0.0324744968375319,
0.0732088012559335));
#102520=CARTESIAN_POINT('Ctrl Pts',(0.00229700571583393,-0.0323646534831895,
0.0731285202580138));
#102521=CARTESIAN_POINT('Ctrl Pts',(0.002332871232607,-0.0326943950436593,
0.0734568027254117));
#102522=CARTESIAN_POINT('Ctrl Pts',(0.00234242479024096,-0.0325844576448126,
0.0733769931190524));
#102523=CARTESIAN_POINT('Ctrl Pts',(0.00235362961750417,-0.0324744968375319,
0.0732973754476784));
#102524=CARTESIAN_POINT('Ctrl Pts',(0.00236646995108289,-0.0323646534831894,
0.0732180515240771));
#102525=CARTESIAN_POINT('Ctrl Pts',(0.00240597651890337,-0.0326943950436593,
0.0735433864692505));
#102526=CARTESIAN_POINT('Ctrl Pts',(0.00241433679027199,-0.0325844576448126,
0.0734645843907503));
#102527=CARTESIAN_POINT('Ctrl Pts',(0.00242432740949117,-0.0324744968375319,
0.0733859496394233));
#102528=CARTESIAN_POINT('Ctrl Pts',(0.00243593418633185,-0.0323646534831894,
0.0733075827901404));
#102529=CARTESIAN_POINT('Origin',(0.0191131607638069,-0.0326395579068891,
0.0753950343999735));
#102530=CARTESIAN_POINT('Ctrl Pts',(0.00240095934061233,-0.0327445246961877,
0.0735777905986883));
#102531=CARTESIAN_POINT('Ctrl Pts',(0.00242254057076331,-0.0324436878365475,
0.0733619508085522));
#102532=CARTESIAN_POINT('Ctrl Pts',(0.00246031842589224,-0.0321434074463188,
0.073148349782893));
#102533=CARTESIAN_POINT('Ctrl Pts',(0.00238149896308957,-0.0327445246961877,
0.0738270320352647));
#102534=CARTESIAN_POINT('Ctrl Pts',(0.00239367989888399,-0.0324436878365475,
0.0736104582849994));
#102535=CARTESIAN_POINT('Ctrl Pts',(0.00242213944977537,-0.0321434074463188,
0.073395417315731));
#102536=CARTESIAN_POINT('Ctrl Pts',(0.0024490888225131,-0.0322357242816073,
0.0732140618878779));
#102537=CARTESIAN_POINT('Ctrl Pts',(0.00247889723751693,-0.0319819883628706,
0.0730333302638323));
#102538=CARTESIAN_POINT('Ctrl Pts',(0.00252014571233431,-0.0317295851069887,
0.0728548617095699));
#102539=CARTESIAN_POINT('Ctrl Pts',(0.00241377615384327,-0.0322357242816073,
0.0734615553533096));
#102540=CARTESIAN_POINT('Ctrl Pts',(0.00243570222296037,-0.0319819883628706,
0.0732796990665657));
#102541=CARTESIAN_POINT('Ctrl Pts',(0.00246915589194791,-0.0317295851069887,
0.0730996065526553));
#102542=CARTESIAN_POINT('Origin',(0.019018671909538,-0.032637194264179,
0.0753826142571921));
#102543=CARTESIAN_POINT('Origin',(0.0190164960621664,-0.0326352985532318,
0.0749034559479179));
#102544=CARTESIAN_POINT('Ctrl Pts',(0.00225277570667768,-0.0321934096636183,
0.0729125498651181));
#102545=CARTESIAN_POINT('Ctrl Pts',(0.00226984110844767,-0.0320835708272303,
0.0728315841100861));
#102546=CARTESIAN_POINT('Ctrl Pts',(0.00228857219368324,-0.0319739230346346,
0.0727510184860852));
#102547=CARTESIAN_POINT('Ctrl Pts',(0.00230893708630216,-0.0318646057455575,
0.0726709542319852));
#102548=CARTESIAN_POINT('Ctrl Pts',(0.00232030019589517,-0.0321934096636183,
0.0730035532063792));
#102549=CARTESIAN_POINT('Ctrl Pts',(0.00233611059066547,-0.0320835708272303,
0.072923518666679));
#102550=CARTESIAN_POINT('Ctrl Pts',(0.00235356812540354,-0.0319739230346346,
0.0728438577455623));
#102551=CARTESIAN_POINT('Ctrl Pts',(0.00237264264228187,-0.0318646057455575,
0.0727646706494482));
#102552=CARTESIAN_POINT('Ctrl Pts',(0.00238782468511265,-0.0321934096636183,
0.0730945565476404));
#102553=CARTESIAN_POINT('Ctrl Pts',(0.00240238007288327,-0.0320835708272303,
0.0730154532232718));
#102554=CARTESIAN_POINT('Ctrl Pts',(0.00241856405712383,-0.0319739230346346,
0.0729366970050395));
#102555=CARTESIAN_POINT('Ctrl Pts',(0.00243634819826157,-0.0318646057455575,
0.0728583870669111));
#102556=CARTESIAN_POINT('Ctrl Pts',(0.00245534917433013,-0.0321934096636183,
0.0731855598889015));
#102557=CARTESIAN_POINT('Ctrl Pts',(0.00246864955510107,-0.0320835708272303,
0.0731073877798646));
#102558=CARTESIAN_POINT('Ctrl Pts',(0.00248355998884413,-0.0319739230346346,
0.0730295362645166));
#102559=CARTESIAN_POINT('Ctrl Pts',(0.00250005375424128,-0.0318646057455575,
0.0729521034843741));
#102560=CARTESIAN_POINT('Ctrl Pts',(0.00243504686768346,-0.0320218834582399,
0.0733079262516562));
#102561=CARTESIAN_POINT('Ctrl Pts',(0.00244381081970364,-0.0319391099350681,
0.073248720269347));
#102562=CARTESIAN_POINT('Ctrl Pts',(0.00245349397158339,-0.0318564869454948,
0.0731896870087778));
#102563=CARTESIAN_POINT('Ctrl Pts',(0.00246408525627879,-0.0317740741446526,
0.0731308688094123));
#102564=CARTESIAN_POINT('Ctrl Pts',(0.00239461420190388,-0.0320218834582399,
0.0733365972751002));
#102565=CARTESIAN_POINT('Ctrl Pts',(0.00240307975788176,-0.0319391099350681,
0.0732769704864855));
#102566=CARTESIAN_POINT('Ctrl Pts',(0.00241247126545925,-0.0318564869454948,
0.0732175120150707));
#102567=CARTESIAN_POINT('Ctrl Pts',(0.00242277784110307,-0.0317740741446526,
0.0731582645298604));
#102568=CARTESIAN_POINT('Ctrl Pts',(0.00235418153612429,-0.0320218834582399,
0.0733652682985442));
#102569=CARTESIAN_POINT('Ctrl Pts',(0.00236234869605987,-0.0319391099350681,
0.0733052207036241));
#102570=CARTESIAN_POINT('Ctrl Pts',(0.0023714485593351,-0.0318564869454947,
0.0732453370213637));
#102571=CARTESIAN_POINT('Ctrl Pts',(0.00238147042592736,-0.0317740741446526,
0.0731856602503085));
#102572=CARTESIAN_POINT('Ctrl Pts',(0.00231374887034471,-0.0320218834582399,
0.0733939393219882));
#102573=CARTESIAN_POINT('Ctrl Pts',(0.00232161763423799,-0.0319391099350681,
0.0733334709207627));
#102574=CARTESIAN_POINT('Ctrl Pts',(0.00233042585321096,-0.0318564869454947,
0.0732731620276566));
#102575=CARTESIAN_POINT('Ctrl Pts',(0.00234016301075164,-0.0317740741446526,
0.0732130559707566));
#102576=CARTESIAN_POINT('Origin',(-0.00392566732324075,-0.039122885339057,
0.0733185045508921));
#102577=CARTESIAN_POINT('Ctrl Pts',(0.00279759881750081,-0.0352722978779652,
0.0763216204069769));
#102578=CARTESIAN_POINT('Ctrl Pts',(0.00279078974844655,-0.0352466642097256,
0.0763039928927817));
#102579=CARTESIAN_POINT('Ctrl Pts',(0.00278391361101129,-0.035221018380832,
0.0762864093326981));
#102580=CARTESIAN_POINT('Ctrl Pts',(0.00277696966659563,-0.0351953608940152,
0.0762688693001644));
#102581=CARTESIAN_POINT('Origin',(-0.00183537316245779,-0.0352456003065139,
0.0779170243773864));
#102582=CARTESIAN_POINT('Ctrl Pts',(0.00273365592871159,-0.0350241211493339,
0.0761519537942269));
#102583=CARTESIAN_POINT('Ctrl Pts',(0.00270607983727255,-0.0349144232867421,
0.0760777070183204));
#102584=CARTESIAN_POINT('Ctrl Pts',(0.00268002197405695,-0.0348045283677512,
0.0760028457846527));
#102585=CARTESIAN_POINT('Ctrl Pts',(0.00265551928407819,-0.0346945769586886,
0.0759274647389144));
#102586=CARTESIAN_POINT('Ctrl Pts',(0.00268423670087071,-0.0350241211493339,
0.0762539287015456));
#102587=CARTESIAN_POINT('Ctrl Pts',(0.00265525594695804,-0.0349144232867421,
0.076179001196069));
#102588=CARTESIAN_POINT('Ctrl Pts',(0.00262780665167665,-0.0348045283677512,
0.0761034297900059));
#102589=CARTESIAN_POINT('Ctrl Pts',(0.00260192757613728,-0.0346945769586886,
0.0760273099723661));
#102590=CARTESIAN_POINT('Ctrl Pts',(0.00263481747302984,-0.0350241211493339,
0.0763559036088642));
#102591=CARTESIAN_POINT('Ctrl Pts',(0.00260443205664353,-0.0349144232867421,
0.0762802953738175));
#102592=CARTESIAN_POINT('Ctrl Pts',(0.00257559132929634,-0.0348045283677512,
0.0762040137953592));
#102593=CARTESIAN_POINT('Ctrl Pts',(0.00254833586819637,-0.0346945769586886,
0.0761271552058178));
#102594=CARTESIAN_POINT('Ctrl Pts',(0.00258539824518897,-0.0350241211493339,
0.0764578785161829));
#102595=CARTESIAN_POINT('Ctrl Pts',(0.00255360816632902,-0.0349144232867421,
0.0763815895515661));
#102596=CARTESIAN_POINT('Ctrl Pts',(0.00252337600691604,-0.0348045283677512,
0.0763045978007125));
#102597=CARTESIAN_POINT('Ctrl Pts',(0.00249474416025546,-0.0346945769586886,
0.0762270004392695));
#102598=CARTESIAN_POINT('Origin',(0.018676725161843,-0.03456290679408,0.0709091073082728));
#102599=CARTESIAN_POINT('Ctrl Pts',(0.00246756592837366,-0.0351970973651616,
0.0759340233585258));
#102600=CARTESIAN_POINT('Ctrl Pts',(0.00244285070252079,-0.0350869349321767,
0.0758556641477074));
#102601=CARTESIAN_POINT('Ctrl Pts',(0.00241974404743112,-0.034976498512971,
0.0757767262091816));
#102602=CARTESIAN_POINT('Ctrl Pts',(0.00239828191845461,-0.0348659306849624,
0.0756973100471963));
#102603=CARTESIAN_POINT('Ctrl Pts',(0.0025423189656239,-0.0351970973651616,
0.0759682644752137));
#102604=CARTESIAN_POINT('Ctrl Pts',(0.00251712937550424,-0.0350869349321767,
0.0758909408664182));
#102605=CARTESIAN_POINT('Ctrl Pts',(0.00249352643359778,-0.034976498512971,
0.0758130295260256));
#102606=CARTESIAN_POINT('Ctrl Pts',(0.00247154665991777,-0.0348659306849624,
0.0757346295904479));
#102607=CARTESIAN_POINT('Ctrl Pts',(0.00261707200287414,-0.0351970973651616,
0.0760025055919017));
#102608=CARTESIAN_POINT('Ctrl Pts',(0.00259140804848769,-0.0350869349321767,
0.0759262175851289));
#102609=CARTESIAN_POINT('Ctrl Pts',(0.00256730881976445,-0.034976498512971,
0.0758493328428697));
#102610=CARTESIAN_POINT('Ctrl Pts',(0.00254481140138094,-0.0348659306849624,
0.0757719491336996));
#102611=CARTESIAN_POINT('Ctrl Pts',(0.00269182504012437,-0.0351970973651616,
0.0760367467085896));
#102612=CARTESIAN_POINT('Ctrl Pts',(0.00266568672147114,-0.0350869349321767,
0.0759614943038397));
#102613=CARTESIAN_POINT('Ctrl Pts',(0.00264109120593112,-0.034976498512971,
0.0758856361597137));
#102614=CARTESIAN_POINT('Ctrl Pts',(0.0026180761428441,-0.0348659306849624,
0.0758092686769512));
#102615=CARTESIAN_POINT('Origin',(0.0187738267269148,-0.0345637187967918,
0.0713801663725021));
#102616=CARTESIAN_POINT('Ctrl Pts',(0.00270196724699681,-0.0352450361861254,
0.0760688662512332));
#102617=CARTESIAN_POINT('Ctrl Pts',(0.002629596020637,-0.0349452761023765,
0.0758643791503246));
#102618=CARTESIAN_POINT('Ctrl Pts',(0.00257283319804065,-0.0346444289983475,
0.0756550216789658));
#102619=CARTESIAN_POINT('Ctrl Pts',(0.00279047897349925,-0.0352450361861254,
0.0763026731678793));
#102620=CARTESIAN_POINT('Ctrl Pts',(0.00270928957480554,-0.0349452761023765,
0.0761015243414284));
#102621=CARTESIAN_POINT('Ctrl Pts',(0.00264348217888855,-0.0346444289983475,
0.0758948314400373));
#102622=CARTESIAN_POINT('Ctrl Pts',(0.00261858862169873,-0.0345231616327822,
0.0758095555140895));
#102623=CARTESIAN_POINT('Ctrl Pts',(0.00259571398540442,-0.0344132092796975,
0.0757336741714007));
#102624=CARTESIAN_POINT('Ctrl Pts',(0.00257441007505534,-0.0343032738558974,
0.0756573236000318));
#102625=CARTESIAN_POINT('Ctrl Pts',(0.00255470167788285,-0.0341934961088741,
0.0755806023130033));
#102626=CARTESIAN_POINT('Ctrl Pts',(0.00256286388209672,-0.0345231616327822,
0.0759082261253921));
#102627=CARTESIAN_POINT('Ctrl Pts',(0.00253862921034272,-0.0344132092796975,
0.075831576695622));
#102628=CARTESIAN_POINT('Ctrl Pts',(0.00251598122198095,-0.0343032738558974,
0.075754429945541));
#102629=CARTESIAN_POINT('Ctrl Pts',(0.00249494640003443,-0.0341934961088741,
0.0756768854522739));
#102630=CARTESIAN_POINT('Ctrl Pts',(0.00250713914249471,-0.0345231616327822,
0.0760068967366947));
#102631=CARTESIAN_POINT('Ctrl Pts',(0.00248154443528103,-0.0344132092796975,
0.0759294792198434));
#102632=CARTESIAN_POINT('Ctrl Pts',(0.00245755236890656,-0.0343032738558974,
0.0758515362910501));
#102633=CARTESIAN_POINT('Ctrl Pts',(0.002435191122186,-0.0341934961088741,
0.0757731685915444));
#102634=CARTESIAN_POINT('Ctrl Pts',(0.0024514144028927,-0.0345231616327822,
0.0761055673479973));
#102635=CARTESIAN_POINT('Ctrl Pts',(0.00242445966021933,-0.0344132092796975,
0.0760273817440647));
#102636=CARTESIAN_POINT('Ctrl Pts',(0.00239912351583217,-0.0343032738558974,
0.0759486426365593));
#102637=CARTESIAN_POINT('Ctrl Pts',(0.00237543584433758,-0.0341934961088741,
0.075869451730815));
#102638=CARTESIAN_POINT('Origin',(0.018688219451002,-0.0345625596227404,
0.0709053152618022));
#102639=CARTESIAN_POINT('Ctrl Pts',(0.00228465605720541,-0.0346945769586885,
0.0755300746244476));
#102640=CARTESIAN_POINT('Ctrl Pts',(0.00226563793133554,-0.034584662917669,
0.0754496085149667));
#102641=CARTESIAN_POINT('Ctrl Pts',(0.00224828056322056,-0.0344746925051587,
0.075368735374644));
#102642=CARTESIAN_POINT('Ctrl Pts',(0.00223260576516843,-0.0343648066255171,
0.0752875589193154));
#102643=CARTESIAN_POINT('Ctrl Pts',(0.00238450121204229,-0.0346945769586885,
0.0755836662901922));
#102644=CARTESIAN_POINT('Ctrl Pts',(0.00236474456593109,-0.034584662917669,
0.0755045760974107));
#102645=CARTESIAN_POINT('Ctrl Pts',(0.00234662009804143,-0.0344746925051587,
0.075425063836502));
#102646=CARTESIAN_POINT('Ctrl Pts',(0.0023301506107792,-0.0343648066255171,
0.0753452314836459));
#102647=CARTESIAN_POINT('Ctrl Pts',(0.00248434636687917,-0.0346945769586885,
0.0756372579559368));
#102648=CARTESIAN_POINT('Ctrl Pts',(0.00246385120052663,-0.034584662917669,
0.0755595436798546));
#102649=CARTESIAN_POINT('Ctrl Pts',(0.0024449596328623,-0.0344746925051587,
0.07548139229836));
#102650=CARTESIAN_POINT('Ctrl Pts',(0.00242769545638997,-0.0343648066255171,
0.0754029040479763));
#102651=CARTESIAN_POINT('Ctrl Pts',(0.00258419152171605,-0.0346945769586885,
0.0756908496216814));
#102652=CARTESIAN_POINT('Ctrl Pts',(0.00256295783512218,-0.034584662917669,
0.0756145112622986));
#102653=CARTESIAN_POINT('Ctrl Pts',(0.00254329916768317,-0.0344746925051587,
0.0755377207602181));
#102654=CARTESIAN_POINT('Ctrl Pts',(0.00252524030200075,-0.0343648066255171,
0.0754605766123068));
#102655=CARTESIAN_POINT('Origin',(0.0188301750962575,-0.0345626446730578,
0.071364707008772));
#102656=CARTESIAN_POINT('Ctrl Pts',(0.00258240495709019,-0.0346945769586885,
0.0756898906870749));
#102657=CARTESIAN_POINT('Ctrl Pts',(0.00255015133011134,-0.0345275153362891,
0.075573824322222));
#102658=CARTESIAN_POINT('Ctrl Pts',(0.00252153954103531,-0.0343603235965159,
0.0754567135897811));
#102659=CARTESIAN_POINT('Ctrl Pts',(0.00249664906299847,-0.034193496108874,
0.0753389061090011));
#102660=CARTESIAN_POINT('Ctrl Pts',(0.00260660102383874,-0.0346945769586885,
0.07577015636271));
#102661=CARTESIAN_POINT('Ctrl Pts',(0.00257266620014711,-0.0345275153362891,
0.0756545967941627));
#102662=CARTESIAN_POINT('Ctrl Pts',(0.00254235684123739,-0.0343603235965159,
0.0755379401170217));
#102663=CARTESIAN_POINT('Ctrl Pts',(0.00251575746086286,-0.034193496108874,
0.075420532682262));
#102664=CARTESIAN_POINT('Ctrl Pts',(0.00263079709058728,-0.0346945769586885,
0.0758504220383451));
#102665=CARTESIAN_POINT('Ctrl Pts',(0.00259518107018288,-0.0345275153362891,
0.0757353692661034));
#102666=CARTESIAN_POINT('Ctrl Pts',(0.00256317414143947,-0.0343603235965159,
0.0756191666442624));
#102667=CARTESIAN_POINT('Ctrl Pts',(0.00253486585872724,-0.034193496108874,
0.0755021592555229));
#102668=CARTESIAN_POINT('Ctrl Pts',(0.00265499315733583,-0.0346945769586885,
0.0759306877139802));
#102669=CARTESIAN_POINT('Ctrl Pts',(0.00261769594021865,-0.0345275153362891,
0.0758161417380442));
#102670=CARTESIAN_POINT('Ctrl Pts',(0.00258399144164155,-0.0343603235965159,
0.075700393171503));
#102671=CARTESIAN_POINT('Ctrl Pts',(0.00255397425659163,-0.034193496108874,
0.0755837858287838));
#102672=CARTESIAN_POINT('Ctrl Pts',(0.00252524803638778,-0.0340223579322365,
0.0754606072089728));
#102673=CARTESIAN_POINT('Ctrl Pts',(0.00250717134476912,-0.0339125849573554,
0.0753833888213624));
#102674=CARTESIAN_POINT('Ctrl Pts',(0.00249070559662516,-0.0338030433565221,
0.0753058505487067));
#102675=CARTESIAN_POINT('Ctrl Pts',(0.0024758630588989,-0.0336938721132328,
0.0752280934159937));
#102676=CARTESIAN_POINT('Ctrl Pts',(0.00246343758796055,-0.0340223579322365,
0.0755555843025039));
#102677=CARTESIAN_POINT('Ctrl Pts',(0.00244405091451146,-0.0339125849573554,
0.0754775133876013));
#102678=CARTESIAN_POINT('Ctrl Pts',(0.00242629375038006,-0.0338030433565221,
0.0753990960731345));
#102679=CARTESIAN_POINT('Ctrl Pts',(0.00241017991436192,-0.0336938721132328,
0.0753204346546368));
#102680=CARTESIAN_POINT('Ctrl Pts',(0.00240162713953332,-0.0340223579322365,
0.075650561396035));
#102681=CARTESIAN_POINT('Ctrl Pts',(0.00238093048425379,-0.0339125849573554,
0.0755716379538401));
#102682=CARTESIAN_POINT('Ctrl Pts',(0.00236188190413497,-0.0338030433565221,
0.0754923415975624));
#102683=CARTESIAN_POINT('Ctrl Pts',(0.00234449676982493,-0.0336938721132328,
0.0754127758932798));
#102684=CARTESIAN_POINT('Ctrl Pts',(0.0023398166911061,-0.0340223579322365,
0.0757455384895661));
#102685=CARTESIAN_POINT('Ctrl Pts',(0.00231781005399612,-0.0339125849573554,
0.075665762520079));
#102686=CARTESIAN_POINT('Ctrl Pts',(0.00229747005788988,-0.0338030433565221,
0.0755855871219902));
#102687=CARTESIAN_POINT('Ctrl Pts',(0.00227881362528795,-0.0336938721132328,
0.0755051171319228));
#102688=CARTESIAN_POINT('Origin',(0.018572563017671,-0.0345589643416638,
0.0709381248279057));
#102689=CARTESIAN_POINT('Ctrl Pts',(0.00220952263615494,-0.034193496108874,
0.0751607095987538));
#102690=CARTESIAN_POINT('Ctrl Pts',(0.00219558554936318,-0.0340836138585569,
0.07507915546208));
#102691=CARTESIAN_POINT('Ctrl Pts',(0.00218334274157543,-0.033973889665241,
0.074997352057848));
#102692=CARTESIAN_POINT('Ctrl Pts',(0.00217280286363653,-0.0338644633307392,
0.0749154051347012));
#102693=CARTESIAN_POINT('Ctrl Pts',(0.00230580586205917,-0.034193496108874,
0.0752204649303689));
#102694=CARTESIAN_POINT('Ctrl Pts',(0.00229104478463349,-0.0340836138585569,
0.0751402384823583));
#102695=CARTESIAN_POINT('Ctrl Pts',(0.00227795090784711,-0.033973889665241,
0.0750597450789823));
#102696=CARTESIAN_POINT('Ctrl Pts',(0.00226653408420143,-0.0338644633307392,
0.0749790888652637));
#102697=CARTESIAN_POINT('Ctrl Pts',(0.0024020890879634,-0.034193496108874,
0.0752802202619839));
#102698=CARTESIAN_POINT('Ctrl Pts',(0.00238650401990379,-0.0340836138585569,
0.0752013215026364));
#102699=CARTESIAN_POINT('Ctrl Pts',(0.00237255907411878,-0.033973889665241,
0.0751221381001166));
#102700=CARTESIAN_POINT('Ctrl Pts',(0.00236026530476633,-0.0338644633307392,
0.0750427725958263));
#102701=CARTESIAN_POINT('Ctrl Pts',(0.00249837231386763,-0.034193496108874,
0.075339975593599));
#102702=CARTESIAN_POINT('Ctrl Pts',(0.0024819632551741,-0.0340836138585569,
0.0752624045229147));
#102703=CARTESIAN_POINT('Ctrl Pts',(0.00246716724039046,-0.033973889665241,
0.0751845311212508));
#102704=CARTESIAN_POINT('Ctrl Pts',(0.00245399652533122,-0.0338644633307392,
0.0751064563263888));
#102705=CARTESIAN_POINT('Origin',(0.0187570446595347,-0.0345610621860694,
0.0713825531527638));
#102706=CARTESIAN_POINT('Ctrl Pts',(0.00250423887516722,-0.0342436276873901,
0.0753742785213273));
#102707=CARTESIAN_POINT('Ctrl Pts',(0.00245806444954122,-0.0339430054201861,
0.0751623339511449));
#102708=CARTESIAN_POINT('Ctrl Pts',(0.00242798573405938,-0.0336441434784162,
0.0749475134463352));
#102709=CARTESIAN_POINT('Ctrl Pts',(0.00256275220091025,-0.0342436276873901,
0.0756173344628521));
#102710=CARTESIAN_POINT('Ctrl Pts',(0.00250741076932982,-0.0339430054201861,
0.0754075967591307));
#102711=CARTESIAN_POINT('Ctrl Pts',(0.00246802486017225,-0.0336441434784162,
0.0751942863548567));
#102712=CARTESIAN_POINT('Ctrl Pts',(0.00245400126290403,-0.0335235895815127,
0.0751064836490833));
#102713=CARTESIAN_POINT('Ctrl Pts',(0.00244083338233157,-0.0334144449262719,
0.0750284279518087));
#102714=CARTESIAN_POINT('Ctrl Pts',(0.00242926294542188,-0.0333049234473133,
0.074950010539492));
#102715=CARTESIAN_POINT('Ctrl Pts',(0.00241931383026442,-0.0331951640388588,
0.0748713303437296));
#102716=CARTESIAN_POINT('Ctrl Pts',(0.00238634910011936,-0.0335235895815127,
0.0751973921599989));
#102717=CARTESIAN_POINT('Ctrl Pts',(0.00237192968491178,-0.0334144449262719,
0.0751184050975087));
#102718=CARTESIAN_POINT('Ctrl Pts',(0.00235912551680972,-0.0333049234473133,
0.0750390293941869));
#102719=CARTESIAN_POINT('Ctrl Pts',(0.00234796216246448,-0.0331951640388588,
0.0749593650640875));
#102720=CARTESIAN_POINT('Ctrl Pts',(0.00231869693733469,-0.0335235895815127,
0.0752883006709144));
#102721=CARTESIAN_POINT('Ctrl Pts',(0.00230302598749199,-0.0334144449262719,
0.0752083822432087));
#102722=CARTESIAN_POINT('Ctrl Pts',(0.00228898808819756,-0.0333049234473133,
0.0751280482488818));
#102723=CARTESIAN_POINT('Ctrl Pts',(0.00227661049466454,-0.0331951640388588,
0.0750473997844454));
#102724=CARTESIAN_POINT('Ctrl Pts',(0.00225104477455003,-0.0335235895815127,
0.07537920918183));
#102725=CARTESIAN_POINT('Ctrl Pts',(0.0022341222900722,-0.0334144449262719,
0.0752983593889087));
#102726=CARTESIAN_POINT('Ctrl Pts',(0.00221885065958541,-0.0333049234473133,
0.0752170671035768));
#102727=CARTESIAN_POINT('Ctrl Pts',(0.0022052588268646,-0.0331951640388588,
0.0751354345048033));
#102728=CARTESIAN_POINT('Origin',(0.0190329342385817,-0.0326434571769145,
0.0735377419525711));
#102729=CARTESIAN_POINT('Ctrl Pts',(0.00215607787082645,-0.0336938721132415,
0.0747861805218438));
#102730=CARTESIAN_POINT('Ctrl Pts',(0.00215235409512492,-0.0336474569764971,
0.0747512495681503));
#102731=CARTESIAN_POINT('Ctrl Pts',(0.00214903948549557,-0.033601104548885,
0.0747162774164519));
#102732=CARTESIAN_POINT('Ctrl Pts',(0.00214064765649121,-0.0334837508662633,
0.0746277359742353));
#102733=CARTESIAN_POINT('Ctrl Pts',(0.00213488317891247,-0.0333660264799464,
0.0745389847456124));
#102734=CARTESIAN_POINT('Ctrl Pts',(0.00243310089257962,-0.0336938721132415,
0.0749832294616808));
#102735=CARTESIAN_POINT('Ctrl Pts',(0.00242822372404542,-0.0336474569764971,
0.0749499200156596));
#102736=CARTESIAN_POINT('Ctrl Pts',(0.00242373681882,-0.033601104548885,
0.0749165557586074));
#102737=CARTESIAN_POINT('Ctrl Pts',(0.00241237700707111,-0.0334837508662633,
0.0748320851357141));
#102738=CARTESIAN_POINT('Ctrl Pts',(0.00240352522325742,-0.0333660264799464,
0.0747473149913337));
#102739=CARTESIAN_POINT('Ctrl Pts',(0.0024331008925887,-0.0336938721132427,
0.0749832294616845));
#102740=CARTESIAN_POINT('Ctrl Pts',(0.00242822372405499,-0.0336474569765026,
0.0749499200156664));
#102741=CARTESIAN_POINT('Ctrl Pts',(0.00242373681883,-0.0336011045488949,
0.0749165557586174));
#102742=CARTESIAN_POINT('Ctrl Pts',(0.00241247161884069,-0.0334847282626114,
0.0748327886609622));
#102743=CARTESIAN_POINT('Ctrl Pts',(0.00240367281197103,-0.0333679869984219,
0.0747487267053694));
#102744=CARTESIAN_POINT('Ctrl Pts',(0.00243310089257973,-0.0336938721132426,
0.0749832294616816));
#102745=CARTESIAN_POINT('Ctrl Pts',(0.00241565797954017,-0.0335278710435082,
0.0748641001418174));
#102746=CARTESIAN_POINT('Ctrl Pts',(0.00240195706737466,-0.033362046922432,
0.0747444657261533));
#102747=CARTESIAN_POINT('Ctrl Pts',(0.00239201124142721,-0.0331951640388601,
0.07462426443833));
#102748=CARTESIAN_POINT('Ctrl Pts',(0.00244704621092374,-0.0336938721132426,
0.0750658947985499));
#102749=CARTESIAN_POINT('Ctrl Pts',(0.00242787277304235,-0.0335278710435082,
0.0749470574114441));
#102750=CARTESIAN_POINT('Ctrl Pts',(0.00241243278989423,-0.033362046922432,
0.0748276605570282));
#102751=CARTESIAN_POINT('Ctrl Pts',(0.00240073844242185,-0.0331951640388601,
0.074707642287823));
#102752=CARTESIAN_POINT('Ctrl Pts',(0.00246099152926775,-0.0336938721132426,
0.0751485601354182));
#102753=CARTESIAN_POINT('Ctrl Pts',(0.00244008756654453,-0.0335278710435082,
0.0750300146810709));
#102754=CARTESIAN_POINT('Ctrl Pts',(0.0024229085124138,-0.033362046922432,
0.0749108553879031));
#102755=CARTESIAN_POINT('Ctrl Pts',(0.0024094656434165,-0.0331951640388601,
0.074791020137316));
#102756=CARTESIAN_POINT('Ctrl Pts',(0.00247493684761175,-0.0336938721132426,
0.0752312254722866));
#102757=CARTESIAN_POINT('Ctrl Pts',(0.00245230236004672,-0.0335278710435082,
0.0751129719506977));
#102758=CARTESIAN_POINT('Ctrl Pts',(0.00243338423493337,-0.033362046922432,
0.074994050218778));
#102759=CARTESIAN_POINT('Ctrl Pts',(0.00241819284441114,-0.0331951640388601,
0.0748743979868089));
#102760=CARTESIAN_POINT('Ctrl Pts',(0.00240513095883838,-0.0330240426238155,
0.0747485890416084));
#102761=CARTESIAN_POINT('Ctrl Pts',(0.00239688481161322,-0.0329142774063509,
0.0746698090494448));
#102762=CARTESIAN_POINT('Ctrl Pts',(0.00239026315588202,-0.0328043479726686,
0.0745908193116843));
#102763=CARTESIAN_POINT('Ctrl Pts',(0.00238527726128139,-0.0326943950436594,
0.0745117207864483));
#102764=CARTESIAN_POINT('Ctrl Pts',(0.00233190421744132,-0.0330240426238155,
0.0748350701397107));
#102765=CARTESIAN_POINT('Ctrl Pts',(0.00232246670883535,-0.0329142774063509,
0.0747552813778431));
#102766=CARTESIAN_POINT('Ctrl Pts',(0.00231467395187389,-0.0328043479726686,
0.0746752577387024));
#102767=CARTESIAN_POINT('Ctrl Pts',(0.00230853875293807,-0.0326943950436594,
0.0745951014635975));
#102768=CARTESIAN_POINT('Ctrl Pts',(0.00225867747604425,-0.0330240426238155,
0.0749215512378131));
#102769=CARTESIAN_POINT('Ctrl Pts',(0.00224804860605748,-0.0329142774063509,
0.0748407537062414));
#102770=CARTESIAN_POINT('Ctrl Pts',(0.00223908474786576,-0.0328043479726686,
0.0747596961657204));
#102771=CARTESIAN_POINT('Ctrl Pts',(0.00223180024459474,-0.0326943950436594,
0.0746784821407468));
#102772=CARTESIAN_POINT('Ctrl Pts',(0.00218545073464719,-0.0330240426238155,
0.0750080323359155));
#102773=CARTESIAN_POINT('Ctrl Pts',(0.00217363050327962,-0.0329142774063509,
0.0749262260346396));
#102774=CARTESIAN_POINT('Ctrl Pts',(0.00216349554385763,-0.0328043479726686,
0.0748441345927385));
#102775=CARTESIAN_POINT('Ctrl Pts',(0.00215506173625141,-0.0326943950436594,
0.074761862817896));
#102776=CARTESIAN_POINT('Origin',(0.0191562288082617,-0.0326396682858259,
0.0735280544404682));
#102777=CARTESIAN_POINT('Ctrl Pts',(0.00212948283705904,-0.0331951640388587,
0.0744114865772719));
#102778=CARTESIAN_POINT('Ctrl Pts',(0.00212588138860573,-0.0330855618305429,
0.0743289272338067));
#102779=CARTESIAN_POINT('Ctrl Pts',(0.00212398370434648,-0.0329757224528702,
0.0742462339386878));
#102780=CARTESIAN_POINT('Ctrl Pts',(0.00212379740868786,-0.0328657862230221,
0.0741635124664328));
#102781=CARTESIAN_POINT('Ctrl Pts',(0.00221751748732908,-0.0331951640388587,
0.074482838188266));
#102782=CARTESIAN_POINT('Ctrl Pts',(0.00221293331482264,-0.0330855618305429,
0.0744014913439599));
#102783=CARTESIAN_POINT('Ctrl Pts',(0.00221002713779438,-0.0329757224528702,
0.0743199911108482));
#102784=CARTESIAN_POINT('Ctrl Pts',(0.00220880779714513,-0.0328657862230221,
0.0742384416723138));
#102785=CARTESIAN_POINT('Ctrl Pts',(0.00230555213759912,-0.0331951640388587,
0.0745541897992601));
#102786=CARTESIAN_POINT('Ctrl Pts',(0.00229998524103954,-0.0330855618305429,
0.0744740554541131));
#102787=CARTESIAN_POINT('Ctrl Pts',(0.00229607057124228,-0.0329757224528702,
0.0743937482830087));
#102788=CARTESIAN_POINT('Ctrl Pts',(0.00229381818560241,-0.0328657862230221,
0.0743133708781948));
#102789=CARTESIAN_POINT('Ctrl Pts',(0.00239358678786915,-0.0331951640388587,
0.0746255414102542));
#102790=CARTESIAN_POINT('Ctrl Pts',(0.00238703716725645,-0.0330855618305429,
0.0745466195642662));
#102791=CARTESIAN_POINT('Ctrl Pts',(0.00238211400469018,-0.0329757224528702,
0.0744675054551692));
#102792=CARTESIAN_POINT('Ctrl Pts',(0.00237882857405968,-0.0328657862230221,
0.0743883000840759));
#102793=CARTESIAN_POINT('Origin',(0.0191447208858007,-0.0326401908832289,
0.0740088251132834));
#102794=CARTESIAN_POINT('Ctrl Pts',(0.00239510143721985,-0.0332451089994432,
0.0746602370009251));
#102795=CARTESIAN_POINT('Ctrl Pts',(0.00237585753388324,-0.0329451141710258,
0.0744441762712784));
#102796=CARTESIAN_POINT('Ctrl Pts',(0.00237294287786516,-0.0326442513127503,
0.0742272798178925));
#102797=CARTESIAN_POINT('Ctrl Pts',(0.00242268724997227,-0.0332451089994432,
0.0749087103856865));
#102798=CARTESIAN_POINT('Ctrl Pts',(0.00239407201960647,-0.0329451141710258,
0.0746936900719898));
#102799=CARTESIAN_POINT('Ctrl Pts',(0.00238173429112761,-0.0326442513127503,
0.07447712519218));
#102800=CARTESIAN_POINT('Ctrl Pts',(0.00237882979313201,-0.0325229783203384,
0.0743883316372644));
#102801=CARTESIAN_POINT('Ctrl Pts',(0.00237554439678409,-0.0324130253112079,
0.0743091375955061));
#102802=CARTESIAN_POINT('Ctrl Pts',(0.00237389772918677,-0.0323031222247694,
0.074229887602433));
#102803=CARTESIAN_POINT('Ctrl Pts',(0.00237388831752336,-0.0321934096636184,
0.0741506832460775));
#102804=CARTESIAN_POINT('Ctrl Pts',(0.00230031734761368,-0.0325229783203384,
0.0744700441733171));
#102805=CARTESIAN_POINT('Ctrl Pts',(0.00229590554576372,-0.0324130253112079,
0.074389767839234));
#102806=CARTESIAN_POINT('Ctrl Pts',(0.00229315503211244,-0.0323031222247694,
0.0743094124168426));
#102807=CARTESIAN_POINT('Ctrl Pts',(0.0022920656978263,-0.0321934096636184,
0.0742290809600451));
#102808=CARTESIAN_POINT('Ctrl Pts',(0.00222180490209536,-0.0325229783203384,
0.0745517567093699));
#102809=CARTESIAN_POINT('Ctrl Pts',(0.00221626669474334,-0.0324130253112079,
0.0744703980829619));
#102810=CARTESIAN_POINT('Ctrl Pts',(0.00221241233503811,-0.0323031222247694,
0.0743889372312521));
#102811=CARTESIAN_POINT('Ctrl Pts',(0.00221024307812924,-0.0321934096636184,
0.0743074786740127));
#102812=CARTESIAN_POINT('Ctrl Pts',(0.00214329245657703,-0.0325229783203384,
0.0746334692454226));
#102813=CARTESIAN_POINT('Ctrl Pts',(0.00213662784372297,-0.0324130253112079,
0.0745510283266898));
#102814=CARTESIAN_POINT('Ctrl Pts',(0.00213166963796378,-0.0323031222247694,
0.0744684620456617));
#102815=CARTESIAN_POINT('Ctrl Pts',(0.00212842045843218,-0.0321934096636184,
0.0743858763879803));
#102816=CARTESIAN_POINT('Origin',(0.0191477063303145,-0.0326393375175144,
0.0735282960905243));
#102817=CARTESIAN_POINT('Ctrl Pts',(0.00212489233953397,-0.0326943950436593,
0.074034585422462));
#102818=CARTESIAN_POINT('Ctrl Pts',(0.00212648296872241,-0.0325844576448127,
0.0739519094771622));
#102819=CARTESIAN_POINT('Ctrl Pts',(0.00212978358458001,-0.0324744968375319,
0.0738692605775767));
#102820=CARTESIAN_POINT('Ctrl Pts',(0.00213478849756053,-0.0323646534831895,
0.0737867445599659));
#102821=CARTESIAN_POINT('Ctrl Pts',(0.00220827298940184,-0.0326943950436593,
0.0741113239056972));
#102822=CARTESIAN_POINT('Ctrl Pts',(0.00220880601846805,-0.0325844576448127,
0.0740297971020245));
#102823=CARTESIAN_POINT('Ctrl Pts',(0.00221102519322253,-0.0324744968375319,
0.0739482755524883));
#102824=CARTESIAN_POINT('Ctrl Pts',(0.00221492622964742,-0.0323646534831895,
0.0738668636680338));
#102825=CARTESIAN_POINT('Ctrl Pts',(0.0022916536392697,-0.0326943950436593,
0.0741880623889324));
#102826=CARTESIAN_POINT('Ctrl Pts',(0.00229112906821369,-0.0325844576448127,
0.0741076847268869));
#102827=CARTESIAN_POINT('Ctrl Pts',(0.00229226680186505,-0.0324744968375319,
0.0740272905273999));
#102828=CARTESIAN_POINT('Ctrl Pts',(0.00229506396173432,-0.0323646534831895,
0.0739469827761017));
#102829=CARTESIAN_POINT('Ctrl Pts',(0.00237503428913756,-0.0326943950436593,
0.0742648008721676));
#102830=CARTESIAN_POINT('Ctrl Pts',(0.00237345211795933,-0.0325844576448127,
0.0741855723517493));
#102831=CARTESIAN_POINT('Ctrl Pts',(0.00237350841050757,-0.0324744968375319,
0.0741063055023115));
#102832=CARTESIAN_POINT('Ctrl Pts',(0.00237520169382122,-0.0323646534831895,
0.0740271018841696));
#102833=CARTESIAN_POINT('Origin',(0.0191825504187299,-0.032639557906713,
0.0740078825809728));
#102834=CARTESIAN_POINT('Ctrl Pts',(0.0023743686535863,-0.0327445246961876,
0.0742995625339472));
#102835=CARTESIAN_POINT('Ctrl Pts',(0.00236872781046194,-0.0324436878365474,
0.0740827198596655));
#102836=CARTESIAN_POINT('Ctrl Pts',(0.00237943646868096,-0.0321434074463187,
0.0738660683211528));
#102837=CARTESIAN_POINT('Ctrl Pts',(0.00238629996213717,-0.0327445246961876,
0.0745492776593927));
#102838=CARTESIAN_POINT('Ctrl Pts',(0.00237124095918869,-0.0324436878365474,
0.0743328849817647));
#102839=CARTESIAN_POINT('Ctrl Pts',(0.00237252431799363,-0.0321434074463187,
0.0741159727472298));
#102840=CARTESIAN_POINT('Ctrl Pts',(0.00237653132468067,-0.0322357242816072,
0.0739326697090658));
#102841=CARTESIAN_POINT('Ctrl Pts',(0.00238345301257987,-0.0319819883628706,
0.0737496272228177));
#102842=CARTESIAN_POINT('Ctrl Pts',(0.00240200818985774,-0.0317295851069886,
0.0735673961416831));
#102843=CARTESIAN_POINT('Ctrl Pts',(0.00237251626325928,-0.0322357242816072,
0.07418263746555));
#102844=CARTESIAN_POINT('Ctrl Pts',(0.00237147680231076,-0.0319819883628706,
0.073999467104803));
#102845=CARTESIAN_POINT('Ctrl Pts',(0.0023820951020171,-0.0317295851069886,
0.0738166018176471));
#102846=CARTESIAN_POINT('Origin',(0.0190872499807766,-0.0326371942644308,
0.0740074029677877));
#102847=CARTESIAN_POINT('Origin',(0.0190250368299907,-0.0326352985529686,
0.0735322956715836));
#102848=CARTESIAN_POINT('Ctrl Pts',(0.00214397671962844,-0.0321934096636184,
0.0736581397562614));
#102849=CARTESIAN_POINT('Ctrl Pts',(0.00215075985572215,-0.0320835708272304,
0.0735756735784052));
#102850=CARTESIAN_POINT('Ctrl Pts',(0.00215924569058578,-0.0319739230346346,
0.0734933956109326));
#102851=CARTESIAN_POINT('Ctrl Pts',(0.00216941528808444,-0.0318646057455575,
0.0734114102895471));
#102852=CARTESIAN_POINT('Ctrl Pts',(0.0022223745011053,-0.0321934096636184,
0.0737399624464169));
#102853=CARTESIAN_POINT('Ctrl Pts',(0.00222802923853304,-0.0320835708272304,
0.0736585774350668));
#102854=CARTESIAN_POINT('Ctrl Pts',(0.00223536495456313,-0.0319739230346346,
0.073577356654828));
#102855=CARTESIAN_POINT('Ctrl Pts',(0.00224436428836604,-0.0318646057455575,
0.0734964033017397));
#102856=CARTESIAN_POINT('Ctrl Pts',(0.00230077228258216,-0.0321934096636184,
0.0738217851365724));
#102857=CARTESIAN_POINT('Ctrl Pts',(0.00230529862134393,-0.0320835708272304,
0.0737414812917285));
#102858=CARTESIAN_POINT('Ctrl Pts',(0.00231148421854049,-0.0319739230346346,
0.0736613176987234));
#102859=CARTESIAN_POINT('Ctrl Pts',(0.00231931328864765,-0.0318646057455575,
0.0735813963139323));
#102860=CARTESIAN_POINT('Ctrl Pts',(0.00237917006405902,-0.0321934096636184,
0.073903607826728));
#102861=CARTESIAN_POINT('Ctrl Pts',(0.00238256800415482,-0.0320835708272304,
0.0738243851483901));
#102862=CARTESIAN_POINT('Ctrl Pts',(0.00238760348251784,-0.0319739230346346,
0.0737452787426189));
#102863=CARTESIAN_POINT('Ctrl Pts',(0.00239426228892925,-0.0318646057455575,
0.0736663893261249));
#102864=CARTESIAN_POINT('Ctrl Pts',(0.00237436441908778,-0.03202188345824,
0.0740275538479042));
#102865=CARTESIAN_POINT('Ctrl Pts',(0.00237563878751945,-0.031939109935068,
0.0739677163080037));
#102866=CARTESIAN_POINT('Ctrl Pts',(0.00237784675541944,-0.0318564869454944,
0.0739079349215902));
#102867=CARTESIAN_POINT('Ctrl Pts',(0.00238098264955265,-0.031774074144652,
0.0738482530813361));
#102868=CARTESIAN_POINT('Ctrl Pts',(0.00233784400903193,-0.03202188345824,
0.0740610663485089));
#102869=CARTESIAN_POINT('Ctrl Pts',(0.00233876959334825,-0.031939109935068,
0.0740008487194273));
#102870=CARTESIAN_POINT('Ctrl Pts',(0.00234063492359818,-0.0318564869454944,
0.0739406820278061));
#102871=CARTESIAN_POINT('Ctrl Pts',(0.00234343454991267,-0.031774074144652,
0.0738806099702603));
#102872=CARTESIAN_POINT('Ctrl Pts',(0.00230132359897608,-0.03202188345824,
0.0740945788491135));
#102873=CARTESIAN_POINT('Ctrl Pts',(0.00230190039917705,-0.031939109935068,
0.0740339811308508));
#102874=CARTESIAN_POINT('Ctrl Pts',(0.00230342309177692,-0.0318564869454944,
0.0739734291340219));
#102875=CARTESIAN_POINT('Ctrl Pts',(0.00230588645027268,-0.031774074144652,
0.0739129668591845));
#102876=CARTESIAN_POINT('Ctrl Pts',(0.00226480318892024,-0.03202188345824,
0.0741280913497182));
#102877=CARTESIAN_POINT('Ctrl Pts',(0.00226503120500585,-0.031939109935068,
0.0740671135422743));
#102878=CARTESIAN_POINT('Ctrl Pts',(0.00226621125995567,-0.0318564869454944,
0.0740061762402378));
#102879=CARTESIAN_POINT('Ctrl Pts',(0.0022683383506327,-0.031774074144652,
0.0739453237481087));
#102880=CARTESIAN_POINT('Origin',(-0.00393486782814988,-0.039122885339064,
0.0748352576114155));
#102881=CARTESIAN_POINT('Ctrl Pts',(0.00311177357195213,-0.0352722978779657,
0.076972044316458));
#102882=CARTESIAN_POINT('Ctrl Pts',(0.00310280888108729,-0.0352466642097258,
0.0769554092031193));
#102883=CARTESIAN_POINT('Ctrl Pts',(0.00309378315960661,-0.0352210183808322,
0.076938826103198));
#102884=CARTESIAN_POINT('Ctrl Pts',(0.00308469562127239,-0.0351953608940152,
0.076922294686067));
#102885=CARTESIAN_POINT('Origin',(-0.00128470890169918,-0.0352456003065134,
0.0791355334093028));
#102886=CARTESIAN_POINT('Ctrl Pts',(0.00302707002673582,-0.035024121149334,
0.0768117297446416));
#102887=CARTESIAN_POINT('Ctrl Pts',(0.00299040579250827,-0.0349144232867421,
0.0767415246274487));
#102888=CARTESIAN_POINT('Ctrl Pts',(0.00295517080284304,-0.0348045283677512,
0.076670519613225));
#102889=CARTESIAN_POINT('Ctrl Pts',(0.0029214135736815,-0.0346945769586886,
0.0765988039709136));
#102890=CARTESIAN_POINT('Ctrl Pts',(0.00299082132914393,-0.0350241211493339,
0.0769190944209832));
#102891=CARTESIAN_POINT('Ctrl Pts',(0.00295267819058769,-0.0349144232867421,
0.0768483899928661));
#102892=CARTESIAN_POINT('Ctrl Pts',(0.00291597373251141,-0.0348045283677512,
0.0767768547988486));
#102893=CARTESIAN_POINT('Ctrl Pts',(0.00288075837832923,-0.0346945769586886,
0.0767045787169257));
#102894=CARTESIAN_POINT('Ctrl Pts',(0.00295457263155204,-0.0350241211493339,
0.0770264590973249));
#102895=CARTESIAN_POINT('Ctrl Pts',(0.00291495058866711,-0.0349144232867421,
0.0769552553582835));
#102896=CARTESIAN_POINT('Ctrl Pts',(0.00287677666217978,-0.0348045283677512,
0.0768831899844722));
#102897=CARTESIAN_POINT('Ctrl Pts',(0.00284010318297697,-0.0346945769586886,
0.0768103534629378));
#102898=CARTESIAN_POINT('Ctrl Pts',(0.00291832393396015,-0.0350241211493339,
0.0771338237736666));
#102899=CARTESIAN_POINT('Ctrl Pts',(0.00287722298674654,-0.0349144232867421,
0.0770621207237008));
#102900=CARTESIAN_POINT('Ctrl Pts',(0.00283757959184816,-0.0348045283677512,
0.0769895251700958));
#102901=CARTESIAN_POINT('Ctrl Pts',(0.0027994479876247,-0.0346945769586886,
0.0769161282089499));
#102902=CARTESIAN_POINT('Origin',(0.0181873204939195,-0.0345629067940851,
0.0696120282492125));
#102903=CARTESIAN_POINT('Ctrl Pts',(0.0027357642993283,-0.0351970973651613,
0.0766288676756795));
#102904=CARTESIAN_POINT('Ctrl Pts',(0.00270142294714201,-0.0350869349321765,
0.0765542239898177));
#102905=CARTESIAN_POINT('Ctrl Pts',(0.00266860494784307,-0.0349764985129711,
0.0764788045323143));
#102906=CARTESIAN_POINT('Ctrl Pts',(0.00263735856978515,-0.0348659306849626,
0.0764027045085106));
#102907=CARTESIAN_POINT('Ctrl Pts',(0.00281421943642782,-0.0351970973651613,
0.0766534697510578));
#102908=CARTESIAN_POINT('Ctrl Pts',(0.00277953725582888,-0.0350869349321765,
0.0765799129547951));
#102909=CARTESIAN_POINT('Ctrl Pts',(0.00274635554994655,-0.0349764985129711,
0.0765055742016235));
#102910=CARTESIAN_POINT('Ctrl Pts',(0.00271472297590992,-0.0348659306849626,
0.0764305472690632));
#102911=CARTESIAN_POINT('Ctrl Pts',(0.00289267457352733,-0.0351970973651613,
0.0766780718264362));
#102912=CARTESIAN_POINT('Ctrl Pts',(0.00285765156451574,-0.0350869349321765,
0.0766056019197724));
#102913=CARTESIAN_POINT('Ctrl Pts',(0.00282410615205003,-0.0349764985129711,
0.0765323438709326));
#102914=CARTESIAN_POINT('Ctrl Pts',(0.00279208738203469,-0.0348659306849626,
0.0764583900296157));
#102915=CARTESIAN_POINT('Ctrl Pts',(0.00297112971062685,-0.0351970973651613,
0.0767026739018145));
#102916=CARTESIAN_POINT('Ctrl Pts',(0.00293576587320261,-0.0350869349321765,
0.0766312908847497));
#102917=CARTESIAN_POINT('Ctrl Pts',(0.00290185675415351,-0.0349764985129711,
0.0765591135402418));
#102918=CARTESIAN_POINT('Ctrl Pts',(0.00286945178815946,-0.0348659306849626,
0.0764862327901682));
#102919=CARTESIAN_POINT('Origin',(0.0183426957394639,-0.0345637187969653,
0.070067202818824));
#102920=CARTESIAN_POINT('Ctrl Pts',(0.00298521758930896,-0.0352450361861253,
0.076733269016688));
#102921=CARTESIAN_POINT('Ctrl Pts',(0.00288778800210619,-0.0349452761023765,
0.0765394648774642));
#102922=CARTESIAN_POINT('Ctrl Pts',(0.00280523332246403,-0.0346444289983475,
0.0763388725204015));
#102923=CARTESIAN_POINT('Ctrl Pts',(0.00310233515130371,-0.0352450361861253,
0.0769541388350707));
#102924=CARTESIAN_POINT('Ctrl Pts',(0.00299657532242206,-0.0349452761023765,
0.0767647518570661));
#102925=CARTESIAN_POINT('Ctrl Pts',(0.00290538134779148,-0.0346444289983475,
0.0765679366446615));
#102926=CARTESIAN_POINT('Ctrl Pts',(0.00286999617619118,-0.0345231616327822,
0.0764864531348779));
#102927=CARTESIAN_POINT('Ctrl Pts',(0.00283779145918998,-0.0344132092796975,
0.0764140370913742));
#102928=CARTESIAN_POINT('Ctrl Pts',(0.00280708627254303,-0.0343032738558974,
0.0763409586550371));
#102929=CARTESIAN_POINT('Ctrl Pts',(0.00277791755498236,-0.0341934961088741,
0.0762673124554182));
#102930=CARTESIAN_POINT('Ctrl Pts',(0.00282707754957742,-0.0345231616327822,
0.0765913298607428));
#102931=CARTESIAN_POINT('Ctrl Pts',(0.00279342725456481,-0.0344132092796975,
0.0765183222443958));
#102932=CARTESIAN_POINT('Ctrl Pts',(0.00276128880070926,-0.0343032738558974,
0.0764446223650969));
#102933=CARTESIAN_POINT('Ctrl Pts',(0.0027307009425303,-0.0341934961088741,
0.0763703256955726));
#102934=CARTESIAN_POINT('Ctrl Pts',(0.00278415892296366,-0.0345231616327822,
0.0766962065866076));
#102935=CARTESIAN_POINT('Ctrl Pts',(0.00274906304993963,-0.0344132092796975,
0.0766226073974174));
#102936=CARTESIAN_POINT('Ctrl Pts',(0.00271549132887548,-0.0343032738558974,
0.0765482860751567));
#102937=CARTESIAN_POINT('Ctrl Pts',(0.00268348433007824,-0.0341934961088741,
0.0764733389357269));
#102938=CARTESIAN_POINT('Ctrl Pts',(0.00274124029634991,-0.0345231616327822,
0.0768010833124725));
#102939=CARTESIAN_POINT('Ctrl Pts',(0.00270469884531446,-0.0344132092796975,
0.076726892550439));
#102940=CARTESIAN_POINT('Ctrl Pts',(0.0026696938570417,-0.0343032738558974,
0.0766519497852166));
#102941=CARTESIAN_POINT('Ctrl Pts',(0.00263626771762619,-0.0341934961088741,
0.0765763521758813));
#102942=CARTESIAN_POINT('Origin',(0.0181982488773147,-0.0345625596229882,
0.0696068254875496));
#102943=CARTESIAN_POINT('Ctrl Pts',(0.00250366852609144,-0.0346945769586886,
0.0762510288836281));
#102944=CARTESIAN_POINT('Ctrl Pts',(0.00247471528617795,-0.0345846629178476,
0.0761735808767919));
#102945=CARTESIAN_POINT('Ctrl Pts',(0.00244735869395167,-0.034474692505516,
0.0760955209005362));
#102946=CARTESIAN_POINT('Ctrl Pts',(0.00242163338876489,-0.0343648066260528,
0.0760169491190588));
#102947=CARTESIAN_POINT('Ctrl Pts',(0.00260944318882002,-0.0346945769586886,
0.0762916840469698));
#102948=CARTESIAN_POINT('Ctrl Pts',(0.00257992970020784,-0.0345846629178476,
0.0762156936684464));
#102949=CARTESIAN_POINT('Ctrl Pts',(0.00255198262043619,-0.034474692505516,
0.076139079983757));
#102950=CARTESIAN_POINT('Ctrl Pts',(0.00252563735311132,-0.0343648066260528,
0.0760619413070686));
#102951=CARTESIAN_POINT('Ctrl Pts',(0.00271521785154859,-0.0346945769586886,
0.0763323392103115));
#102952=CARTESIAN_POINT('Ctrl Pts',(0.00268514411423773,-0.0345846629178476,
0.0762578064601009));
#102953=CARTESIAN_POINT('Ctrl Pts',(0.00265660654692071,-0.034474692505516,
0.0761826390669778));
#102954=CARTESIAN_POINT('Ctrl Pts',(0.00262964131745774,-0.0343648066260528,
0.0761069334950785));
#102955=CARTESIAN_POINT('Ctrl Pts',(0.00282099251427717,-0.0346945769586886,
0.0763729943736532));
#102956=CARTESIAN_POINT('Ctrl Pts',(0.00279035852826763,-0.0345846629178476,
0.0762999192517554));
#102957=CARTESIAN_POINT('Ctrl Pts',(0.00276123047340524,-0.034474692505516,
0.0762261981501985));
#102958=CARTESIAN_POINT('Ctrl Pts',(0.00273364528180416,-0.0343648066260528,
0.0761519256830883));
#102959=CARTESIAN_POINT('Origin',(0.0183966622133401,-0.0345626446730873,
0.070044803033538));
#102960=CARTESIAN_POINT('Ctrl Pts',(0.00281909985087201,-0.0346945769586886,
0.0763722669164541));
#102961=CARTESIAN_POINT('Ctrl Pts',(0.00277255358056049,-0.0345275153362891,
0.0762611582209188));
#102962=CARTESIAN_POINT('Ctrl Pts',(0.00272948953720534,-0.0343603235965159,
0.0761485569496254));
#102963=CARTESIAN_POINT('Ctrl Pts',(0.00269003013551802,-0.034193496108874,
0.076034798020116));
#102964=CARTESIAN_POINT('Ctrl Pts',(0.00285316508107882,-0.0346945769586886,
0.0764488671019775));
#102965=CARTESIAN_POINT('Ctrl Pts',(0.00280501438921249,-0.0345275153362891,
0.0763384719163279));
#102966=CARTESIAN_POINT('Ctrl Pts',(0.00276032307008778,-0.0343603235965159,
0.0762265338818892));
#102967=CARTESIAN_POINT('Ctrl Pts',(0.00271921838032941,-0.034193496108874,
0.0761133860261735));
#102968=CARTESIAN_POINT('Ctrl Pts',(0.00288723031128562,-0.0346945769586886,
0.0765254672875009));
#102969=CARTESIAN_POINT('Ctrl Pts',(0.00283747519786449,-0.0345275153362891,
0.0764157856117369));
#102970=CARTESIAN_POINT('Ctrl Pts',(0.00279115660297022,-0.0343603235965159,
0.0763045108141529));
#102971=CARTESIAN_POINT('Ctrl Pts',(0.00274840662514081,-0.034193496108874,
0.076191974032231));
#102972=CARTESIAN_POINT('Ctrl Pts',(0.00292129554149242,-0.0346945769586886,
0.0766020674730243));
#102973=CARTESIAN_POINT('Ctrl Pts',(0.00286993600651649,-0.0345275153362891,
0.076493099307146));
#102974=CARTESIAN_POINT('Ctrl Pts',(0.00282199013585266,-0.0343603235965159,
0.0763824877464167));
#102975=CARTESIAN_POINT('Ctrl Pts',(0.0027775948699522,-0.034193496108874,
0.0762705620382886));
#102976=CARTESIAN_POINT('Ctrl Pts',(0.00273365678984782,-0.0340223579322365,
0.0761519550687527));
#102977=CARTESIAN_POINT('Ctrl Pts',(0.00270604460813198,-0.0339125849573554,
0.0760776111814053));
#102978=CARTESIAN_POINT('Ctrl Pts',(0.00267999057489329,-0.0338030433565222,
0.076002748026647));
#102979=CARTESIAN_POINT('Ctrl Pts',(0.00265551952213465,-0.0336938721132328,
0.075927464295398));
#102980=CARTESIAN_POINT('Ctrl Pts',(0.00268423752151511,-0.0340223579322365,
0.0762539301429025));
#102981=CARTESIAN_POINT('Ctrl Pts',(0.00265521883756461,-0.0339125849573554,
0.0761789046349539));
#102982=CARTESIAN_POINT('Ctrl Pts',(0.00262777339838666,-0.0338030433565222,
0.0761033312272334));
#102983=CARTESIAN_POINT('Ctrl Pts',(0.0026019277348414,-0.0336938721132328,
0.0760273096766888));
#102984=CARTESIAN_POINT('Ctrl Pts',(0.00263481825318241,-0.0340223579322365,
0.0763559052170523));
#102985=CARTESIAN_POINT('Ctrl Pts',(0.00260439306699723,-0.0339125849573554,
0.0762801980885026));
#102986=CARTESIAN_POINT('Ctrl Pts',(0.00257555622188002,-0.0338030433565222,
0.0762039144278198));
#102987=CARTESIAN_POINT('Ctrl Pts',(0.00254833594754816,-0.0336938721132328,
0.0761271550579797));
#102988=CARTESIAN_POINT('Ctrl Pts',(0.00258539898484971,-0.0340223579322365,
0.0764578802912021));
#102989=CARTESIAN_POINT('Ctrl Pts',(0.00255356729642986,-0.0339125849573554,
0.0763814915420512));
#102990=CARTESIAN_POINT('Ctrl Pts',(0.00252333904537339,-0.0338030433565222,
0.0763044976284062));
#102991=CARTESIAN_POINT('Ctrl Pts',(0.00249474416025491,-0.0336938721132328,
0.0762270004392705));
#102992=CARTESIAN_POINT('Origin',(0.0180876165588606,-0.0345589643416277,
0.0696538719354821));
#102993=CARTESIAN_POINT('Ctrl Pts',(0.00238283384147149,-0.034193496108874,
0.0758939931260948));
#102994=CARTESIAN_POINT('Ctrl Pts',(0.00235878520901436,-0.0340836138581107,
0.0758148288479804));
#102995=CARTESIAN_POINT('Ctrl Pts',(0.00233638625416955,-0.03397388966435,
0.075735204918387));
#102996=CARTESIAN_POINT('Ctrl Pts',(0.00231565881338707,-0.0338644633294063,
0.0756552251678614));
#102997=CARTESIAN_POINT('Ctrl Pts',(0.0024858471743151,-0.034193496108874,
0.0759412097810315));
#102998=CARTESIAN_POINT('Ctrl Pts',(0.00246114745214699,-0.0340836138581107,
0.0758634659957749));
#102999=CARTESIAN_POINT('Ctrl Pts',(0.00243806832587719,-0.03397388966435,
0.0757852484045248));
#103000=CARTESIAN_POINT('Ctrl Pts',(0.0024166326231499,-0.0338644633294063,
0.0757066590962446));
#103001=CARTESIAN_POINT('Ctrl Pts',(0.00258886050715872,-0.034193496108874,
0.0759884264359681));
#103002=CARTESIAN_POINT('Ctrl Pts',(0.00256350969527962,-0.0340836138581107,
0.0759121031435693));
#103003=CARTESIAN_POINT('Ctrl Pts',(0.00253975039758483,-0.03397388966435,
0.0758352918906625));
#103004=CARTESIAN_POINT('Ctrl Pts',(0.00251760643291272,-0.0338644633294063,
0.0757580930246279));
#103005=CARTESIAN_POINT('Ctrl Pts',(0.00269187384000233,-0.034193496108874,
0.0760356430909048));
#103006=CARTESIAN_POINT('Ctrl Pts',(0.00266587193841225,-0.0340836138581107,
0.0759607402913638));
#103007=CARTESIAN_POINT('Ctrl Pts',(0.00264143246929247,-0.03397388966435,
0.0758853353768002));
#103008=CARTESIAN_POINT('Ctrl Pts',(0.00261858024267554,-0.0338644633294063,
0.0758095269530112));
#103009=CARTESIAN_POINT('Origin',(0.0183263451466634,-0.0345610621861401,
0.0700716741294723));
#103010=CARTESIAN_POINT('Ctrl Pts',(0.00270199343856667,-0.03424362768739,
0.0760689402547046));
#103011=CARTESIAN_POINT('Ctrl Pts',(0.00262961941376101,-0.033943005420186,
0.0758644541208345));
#103012=CARTESIAN_POINT('Ctrl Pts',(0.00257285372943111,-0.0336441434784162,
0.0756550974025419));
#103013=CARTESIAN_POINT('Ctrl Pts',(0.00279050835634744,-0.03424362768739,
0.0763027459632112));
#103014=CARTESIAN_POINT('Ctrl Pts',(0.00270931620387696,-0.033943005420186,
0.0761015982244992));
#103015=CARTESIAN_POINT('Ctrl Pts',(0.00264350598165653,-0.0336441434784162,
0.0758949061998273));
#103016=CARTESIAN_POINT('Ctrl Pts',(0.00261858836761115,-0.0335235895815127,
0.0758095534674062));
#103017=CARTESIAN_POINT('Ctrl Pts',(0.00259574134677251,-0.0334144449262719,
0.0757337636356701));
#103018=CARTESIAN_POINT('Ctrl Pts',(0.00257443383836038,-0.0333049234473133,
0.0756574147283433));
#103019=CARTESIAN_POINT('Ctrl Pts',(0.00255470193159522,-0.0331951640388589,
0.0755806019041989));
#103020=CARTESIAN_POINT('Ctrl Pts',(0.0025628635199683,-0.0335235895815127,
0.0759082242018796));
#103021=CARTESIAN_POINT('Ctrl Pts',(0.00253865810220486,-0.0334144449262719,
0.0758316672079036));
#103022=CARTESIAN_POINT('Ctrl Pts',(0.00251600648522894,-0.0333049234473133,
0.0757545221935022));
#103023=CARTESIAN_POINT('Ctrl Pts',(0.00249494656917595,-0.0331951640388589,
0.0756768851797377));
#103024=CARTESIAN_POINT('Ctrl Pts',(0.00250713867232545,-0.0335235895815127,
0.076006894936353));
#103025=CARTESIAN_POINT('Ctrl Pts',(0.0024815748576372,-0.0334144449262719,
0.0759295707801371));
#103026=CARTESIAN_POINT('Ctrl Pts',(0.00245757913209751,-0.0333049234473133,
0.0758516296586612));
#103027=CARTESIAN_POINT('Ctrl Pts',(0.00243519120675668,-0.0331951640388589,
0.0757731684552765));
#103028=CARTESIAN_POINT('Ctrl Pts',(0.0024514138246826,-0.0335235895815127,
0.0761055656708264));
#103029=CARTESIAN_POINT('Ctrl Pts',(0.00242449161306955,-0.0334144449262719,
0.0760274743523705));
#103030=CARTESIAN_POINT('Ctrl Pts',(0.00239915177896608,-0.0333049234473133,
0.0759487371238201));
#103031=CARTESIAN_POINT('Ctrl Pts',(0.00237543584433741,-0.0331951640388589,
0.0758694517308153));
#103032=CARTESIAN_POINT('Origin',(0.0188701760354181,-0.0326434571770769,
0.0721752904886176));
#103033=CARTESIAN_POINT('Ctrl Pts',(0.00228286956380782,-0.0336938721132422,
0.0755291157280789));
#103034=CARTESIAN_POINT('Ctrl Pts',(0.00227479714181198,-0.0336474569764974,
0.0754949269282381));
#103035=CARTESIAN_POINT('Ctrl Pts',(0.00226712549601245,-0.033601104548885,
0.0754606459731441));
#103036=CARTESIAN_POINT('Ctrl Pts',(0.00224770265350699,-0.0334837508643185,
0.0753738544802717));
#103037=CARTESIAN_POINT('Ctrl Pts',(0.00223086015185338,-0.0333660264760453,
0.0752865255607544));
#103038=CARTESIAN_POINT('Ctrl Pts',(0.00258240495709203,-0.0336938721132422,
0.0756898906870816));
#103039=CARTESIAN_POINT('Ctrl Pts',(0.00257339146591032,-0.0336474569764974,
0.0756574551672941));
#103040=CARTESIAN_POINT('Ctrl Pts',(0.00256475829105089,-0.033601104548885,
0.0756249163557145));
#103041=CARTESIAN_POINT('Ctrl Pts',(0.00254290107814002,-0.0334837508643185,
0.0755425355694867));
#103042=CARTESIAN_POINT('Ctrl Pts',(0.00252349457669983,-0.0333660264760453,
0.0754595432843177));
#103043=CARTESIAN_POINT('Ctrl Pts',(0.00258240495710018,-0.0336938721132426,
0.0756898906870849));
#103044=CARTESIAN_POINT('Ctrl Pts',(0.00257339146591944,-0.0336474569765026,
0.0756574551673007));
#103045=CARTESIAN_POINT('Ctrl Pts',(0.00256475829106089,-0.0336011045488949,
0.0756249163557245));
#103046=CARTESIAN_POINT('Ctrl Pts',(0.00254308311896268,-0.0334847282606778,
0.0755432216892383));
#103047=CARTESIAN_POINT('Ctrl Pts',(0.00252381793631918,-0.0333679869945435,
0.0754609253688133));
#103048=CARTESIAN_POINT('Ctrl Pts',(0.00258240495709209,-0.0336938721132425,
0.0756898906870818));
#103049=CARTESIAN_POINT('Ctrl Pts',(0.00255016872376089,-0.0335278710435082,
0.0755738869141809));
#103050=CARTESIAN_POINT('Ctrl Pts',(0.00252158167921933,-0.033362046922432,
0.075456913031242));
#103051=CARTESIAN_POINT('Ctrl Pts',(0.00249664906299867,-0.0331951640388602,
0.0753389061090021));
#103052=CARTESIAN_POINT('Ctrl Pts',(0.00260660102640909,-0.0336938721132425,
0.0757701563712369));
#103053=CARTESIAN_POINT('Ctrl Pts',(0.00257268450281793,-0.0335278710435082,
0.0756546591213917));
#103054=CARTESIAN_POINT('Ctrl Pts',(0.00254240187470728,-0.033362046922432,
0.0755381388898491));
#103055=CARTESIAN_POINT('Ctrl Pts',(0.00251575746289138,-0.0331951640388602,
0.0754205326909275));
#103056=CARTESIAN_POINT('Ctrl Pts',(0.00263079709572609,-0.0336938721132425,
0.075850422055392));
#103057=CARTESIAN_POINT('Ctrl Pts',(0.00259520028187497,-0.0335278710435082,
0.0757354313286024));
#103058=CARTESIAN_POINT('Ctrl Pts',(0.00256322207019523,-0.033362046922432,
0.0756193647484562));
#103059=CARTESIAN_POINT('Ctrl Pts',(0.00253486586278409,-0.0331951640388602,
0.0755021592728528));
#103060=CARTESIAN_POINT('Ctrl Pts',(0.00265499316504309,-0.0336938721132425,
0.075930687739547));
#103061=CARTESIAN_POINT('Ctrl Pts',(0.00261771606093201,-0.0335278710435082,
0.0758162035358132));
#103062=CARTESIAN_POINT('Ctrl Pts',(0.00258404226568318,-0.033362046922432,
0.0757005906070632));
#103063=CARTESIAN_POINT('Ctrl Pts',(0.0025539742626768,-0.0331951640388602,
0.0755837858547782));
#103064=CARTESIAN_POINT('Ctrl Pts',(0.00252524733205986,-0.0330240426238155,
0.075460606039043));
#103065=CARTESIAN_POINT('Ctrl Pts',(0.00250719245701054,-0.0329142774063509,
0.0753834807669443));
#103066=CARTESIAN_POINT('Ctrl Pts',(0.00249072297576066,-0.0328043479726686,
0.0753059438003835));
#103067=CARTESIAN_POINT('Ctrl Pts',(0.00247586272249016,-0.0326943950436594,
0.075228093888937));
#103068=CARTESIAN_POINT('Ctrl Pts',(0.00246343696105782,-0.0330240426238155,
0.0755555829521389));
#103069=CARTESIAN_POINT('Ctrl Pts',(0.00244407368649909,-0.0329142774063509,
0.0754776061819607));
#103070=CARTESIAN_POINT('Ctrl Pts',(0.00242631275629876,-0.0328043479726686,
0.0753991902445449));
#103071=CARTESIAN_POINT('Ctrl Pts',(0.00241017969008967,-0.0326943950436594,
0.0753204349699319));
#103072=CARTESIAN_POINT('Ctrl Pts',(0.00240162659005577,-0.0330240426238155,
0.0756505598652348));
#103073=CARTESIAN_POINT('Ctrl Pts',(0.00238095491598763,-0.0329142774063509,
0.0755717315969771));
#103074=CARTESIAN_POINT('Ctrl Pts',(0.00236190253683687,-0.0328043479726686,
0.0754924366887063));
#103075=CARTESIAN_POINT('Ctrl Pts',(0.00234449665768919,-0.0326943950436594,
0.0754127760509268));
#103076=CARTESIAN_POINT('Ctrl Pts',(0.00233981621905373,-0.0330240426238155,
0.0757455367783307));
#103077=CARTESIAN_POINT('Ctrl Pts',(0.00231783614547617,-0.0329142774063509,
0.0756658570119935));
#103078=CARTESIAN_POINT('Ctrl Pts',(0.00229749231737497,-0.0328043479726686,
0.0755856831328677));
#103079=CARTESIAN_POINT('Ctrl Pts',(0.0022788136252887,-0.0326943950436594,
0.0755051171319217));
#103080=CARTESIAN_POINT('Origin',(0.0189912842235296,-0.0326396682855742,
0.0721502264588975));
#103081=CARTESIAN_POINT('Ctrl Pts',(0.00220952263615499,-0.0331951640388587,
0.0751607095987539));
#103082=CARTESIAN_POINT('Ctrl Pts',(0.00219560215608103,-0.0330855618255041,
0.0750792526378066));
#103083=CARTESIAN_POINT('Ctrl Pts',(0.0021833552170716,-0.0329757224427708,
0.0749974492431467));
#103084=CARTESIAN_POINT('Ctrl Pts',(0.00217280264047757,-0.0328657862078596,
0.0749154033996513));
#103085=CARTESIAN_POINT('Ctrl Pts',(0.00230580583503894,-0.0331951640388587,
0.0752204649135996));
#103086=CARTESIAN_POINT('Ctrl Pts',(0.00229106234638699,-0.0330855618255041,
0.0751403340589375));
#103087=CARTESIAN_POINT('Ctrl Pts',(0.00227796439715407,-0.0329757224427708,
0.075059840716354));
#103088=CARTESIAN_POINT('Ctrl Pts',(0.00226653381617092,-0.0328657862078596,
0.07497908713967));
#103089=CARTESIAN_POINT('Ctrl Pts',(0.00240208903392289,-0.0331951640388587,
0.0752802202284453));
#103090=CARTESIAN_POINT('Ctrl Pts',(0.00238652253669296,-0.0330855618255041,
0.0752014154800685));
#103091=CARTESIAN_POINT('Ctrl Pts',(0.00237257357723654,-0.0329757224427708,
0.0751222321895612));
#103092=CARTESIAN_POINT('Ctrl Pts',(0.00236026499186427,-0.0328657862078596,
0.0750427708796888));
#103093=CARTESIAN_POINT('Ctrl Pts',(0.00249837223280683,-0.0331951640388587,
0.075339975543291));
#103094=CARTESIAN_POINT('Ctrl Pts',(0.00248198272699892,-0.0330855618255041,
0.0752624969011995));
#103095=CARTESIAN_POINT('Ctrl Pts',(0.00246718275731901,-0.0329757224427708,
0.0751846236627685));
#103096=CARTESIAN_POINT('Ctrl Pts',(0.00245399616755762,-0.0328657862078596,
0.0751064546197075));
#103097=CARTESIAN_POINT('Origin',(0.0190401235886673,-0.0326401908834989,
0.0726286484355253));
#103098=CARTESIAN_POINT('Ctrl Pts',(0.00250422344926411,-0.0332451089994432,
0.0753742077129654));
#103099=CARTESIAN_POINT('Ctrl Pts',(0.00245805169996031,-0.0329451141710258,
0.0751622625873378));
#103100=CARTESIAN_POINT('Ctrl Pts',(0.00242797569302402,-0.0326442513127503,
0.0749474417305342));
#103101=CARTESIAN_POINT('Ctrl Pts',(0.00256273371241031,-0.0332451089994432,
0.0756172643917598));
#103102=CARTESIAN_POINT('Ctrl Pts',(0.00250739493048529,-0.0329451141710258,
0.0754075260168111));
#103103=CARTESIAN_POINT('Ctrl Pts',(0.00246801171201756,-0.0326442513127503,
0.0751942151431685));
#103104=CARTESIAN_POINT('Ctrl Pts',(0.00245400133349894,-0.0325229783203385,
0.0751064857820804));
#103105=CARTESIAN_POINT('Ctrl Pts',(0.00244081619814992,-0.032413025311208,
0.0750283279783433));
#103106=CARTESIAN_POINT('Ctrl Pts',(0.00242924985712664,-0.0323031222247695,
0.074949909277311));
#103107=CARTESIAN_POINT('Ctrl Pts',(0.00241931358158259,-0.0321934096636184,
0.0748713306505568));
#103108=CARTESIAN_POINT('Ctrl Pts',(0.00238634927843028,-0.0325229783203385,
0.0751973942090519));
#103109=CARTESIAN_POINT('Ctrl Pts',(0.0023719109724263,-0.032413025311208,
0.0751183038232321));
#103110=CARTESIAN_POINT('Ctrl Pts',(0.00235911094247396,-0.0323031222247695,
0.0750389267581171));
#103111=CARTESIAN_POINT('Ctrl Pts',(0.00234796199667667,-0.0321934096636184,
0.0749593652686388));
#103112=CARTESIAN_POINT('Ctrl Pts',(0.00231869722336161,-0.0325229783203385,
0.0752883026360234));
#103113=CARTESIAN_POINT('Ctrl Pts',(0.00230300574670268,-0.032413025311208,
0.0752082796681209));
#103114=CARTESIAN_POINT('Ctrl Pts',(0.00228897202782127,-0.0323031222247695,
0.0751279442389232));
#103115=CARTESIAN_POINT('Ctrl Pts',(0.00227661041177075,-0.0321934096636184,
0.0750473998867209));
#103116=CARTESIAN_POINT('Ctrl Pts',(0.00225104516829294,-0.0325229783203385,
0.0753792110629949));
#103117=CARTESIAN_POINT('Ctrl Pts',(0.00223410052097905,-0.032413025311208,
0.0752982555130097));
#103118=CARTESIAN_POINT('Ctrl Pts',(0.00221883311316859,-0.0323031222247695,
0.0752169617197293));
#103119=CARTESIAN_POINT('Ctrl Pts',(0.00220525882686484,-0.0321934096636184,
0.075135434504803));
#103120=CARTESIAN_POINT('Origin',(0.0189828592343901,-0.032639337517782,
0.0721515343525047));
#103121=CARTESIAN_POINT('Ctrl Pts',(0.00215773009560759,-0.0326943950436594,
0.0747873557640232));
#103122=CARTESIAN_POINT('Ctrl Pts',(0.00214894613864736,-0.0325844576448127,
0.0747051323845465));
#103123=CARTESIAN_POINT('Ctrl Pts',(0.00214186207432751,-0.0324744968375319,
0.0746227215193621));
#103124=CARTESIAN_POINT('Ctrl Pts',(0.00213648552276626,-0.0323646534831895,
0.0745402288832689));
#103125=CARTESIAN_POINT('Ctrl Pts',(0.00225007114638938,-0.0326943950436594,
0.0748530387749328));
#103126=CARTESIAN_POINT('Ctrl Pts',(0.00224038195443574,-0.0325844576448127,
0.0747720880282014));
#103127=CARTESIAN_POINT('Ctrl Pts',(0.00223236627092589,-0.0324744968375319,
0.0746909311640848));
#103128=CARTESIAN_POINT('Ctrl Pts',(0.00222603293178415,-0.0323646534831895,
0.0746096723071463));
#103129=CARTESIAN_POINT('Ctrl Pts',(0.00234241219717117,-0.0326943950436594,
0.0749187217858424));
#103130=CARTESIAN_POINT('Ctrl Pts',(0.00233181777022411,-0.0325844576448127,
0.0748390436718564));
#103131=CARTESIAN_POINT('Ctrl Pts',(0.00232287046752428,-0.0324744968375319,
0.0747591408088074));
#103132=CARTESIAN_POINT('Ctrl Pts',(0.00231558034080203,-0.0323646534831895,
0.0746791157310237));
#103133=CARTESIAN_POINT('Ctrl Pts',(0.00243475324795296,-0.0326943950436594,
0.074984404796752));
#103134=CARTESIAN_POINT('Ctrl Pts',(0.00242325358601249,-0.0325844576448127,
0.0749059993155113));
#103135=CARTESIAN_POINT('Ctrl Pts',(0.00241337466412267,-0.0324744968375319,
0.0748273504535301));
#103136=CARTESIAN_POINT('Ctrl Pts',(0.00240512774981991,-0.0323646534831895,
0.0747485591549012));
#103137=CARTESIAN_POINT('Origin',(0.0190775366925626,-0.0326395579068863,
0.0726229720380674));
#103138=CARTESIAN_POINT('Ctrl Pts',(0.0024384496526117,-0.0327445246961877,
0.0750189757787017));
#103139=CARTESIAN_POINT('Ctrl Pts',(0.00240567569567775,-0.0324436878365475,
0.0748045499587832));
#103140=CARTESIAN_POINT('Ctrl Pts',(0.0023891462750497,-0.0321434074463187,
0.0745882646316005));
#103141=CARTESIAN_POINT('Ctrl Pts',(0.00248158448337294,-0.0327445246961877,
0.0752652264363154));
#103142=CARTESIAN_POINT('Ctrl Pts',(0.00243952303115385,-0.0324436878365475,
0.0750524274731176));
#103143=CARTESIAN_POINT('Ctrl Pts',(0.00241360995853735,-0.0321434074463187,
0.0748370648088316));
#103144=CARTESIAN_POINT('Ctrl Pts',(0.00239461140628459,-0.0322357242816073,
0.0746547049587685));
#103145=CARTESIAN_POINT('Ctrl Pts',(0.00237853720792616,-0.0319819883628706,
0.0744722382996705));
#103146=CARTESIAN_POINT('Ctrl Pts',(0.00237410646143453,-0.0317295851069886,
0.0742891185846729));
#103147=CARTESIAN_POINT('Ctrl Pts',(0.00242195727202873,-0.0322357242816073,
0.074903204865462));
#103148=CARTESIAN_POINT('Ctrl Pts',(0.00239796867393468,-0.0319819883628706,
0.0747216091367218));
#103149=CARTESIAN_POINT('Ctrl Pts',(0.00238558414743039,-0.0317295851069886,
0.074538854971137));
#103150=CARTESIAN_POINT('Origin',(0.0189829276155652,-0.0326371942643099,
0.0726344405192385));
#103151=CARTESIAN_POINT('Origin',(0.0188616583006038,-0.0326352985525182,
0.0721708769617584));
#103152=CARTESIAN_POINT('Ctrl Pts',(0.00212948283705859,-0.0321934096636183,
0.0744114865772715));
#103153=CARTESIAN_POINT('Ctrl Pts',(0.00212587673336777,-0.0320835708272303,
0.0743288205174788));
#103154=CARTESIAN_POINT('Ctrl Pts',(0.00212398349117446,-0.0319739230346346,
0.0742461277792319));
#103155=CARTESIAN_POINT('Ctrl Pts',(0.00212379741292528,-0.0318646057455575,
0.0741635143480549));
#103156=CARTESIAN_POINT('Ctrl Pts',(0.00221751753094838,-0.0321934096636183,
0.0744828382236192));
#103157=CARTESIAN_POINT('Ctrl Pts',(0.00221292743244634,-0.0320835708272303,
0.0744013862308653));
#103158=CARTESIAN_POINT('Ctrl Pts',(0.00221002564114451,-0.0319739230346346,
0.0743198864917275));
#103159=CARTESIAN_POINT('Ctrl Pts',(0.00220880786700199,-0.0318646057455575,
0.0742384435644025));
#103160=CARTESIAN_POINT('Ctrl Pts',(0.00230555222483818,-0.0321934096636183,
0.0745541898699668));
#103161=CARTESIAN_POINT('Ctrl Pts',(0.00229997813152491,-0.0320835708272303,
0.0744739519442518));
#103162=CARTESIAN_POINT('Ctrl Pts',(0.00229606779111457,-0.0319739230346346,
0.0743936452042231));
#103163=CARTESIAN_POINT('Ctrl Pts',(0.0022938183210787,-0.0318646057455575,
0.0743133727807501));
#103164=CARTESIAN_POINT('Ctrl Pts',(0.00239358691872797,-0.0321934096636183,
0.0746255415163145));
#103165=CARTESIAN_POINT('Ctrl Pts',(0.00238702883060348,-0.0320835708272303,
0.0745465176576383));
#103166=CARTESIAN_POINT('Ctrl Pts',(0.00238210994108463,-0.0319739230346346,
0.0744674039167187));
#103167=CARTESIAN_POINT('Ctrl Pts',(0.00237882877515541,-0.0318646057455575,
0.0743883019970977));
#103168=CARTESIAN_POINT('Ctrl Pts',(0.00240435372332806,-0.03202188345824,
0.0747491124931118));
#103169=CARTESIAN_POINT('Ctrl Pts',(0.00239811841061979,-0.0319391099350678,
0.0746895870693697));
#103170=CARTESIAN_POINT('Ctrl Pts',(0.00239281637356727,-0.031856486945494,
0.0746300003452872));
#103171=CARTESIAN_POINT('Ctrl Pts',(0.00238844742221453,-0.0317740741446515,
0.0745703960824178));
#103172=CARTESIAN_POINT('Ctrl Pts',(0.00237232151767753,-0.03202188345824,
0.0747869379587249));
#103173=CARTESIAN_POINT('Ctrl Pts',(0.0023656925333147,-0.0319391099350678,
0.0747270791571593));
#103174=CARTESIAN_POINT('Ctrl Pts',(0.00236000226886473,-0.031856486945494,
0.0746671531100005));
#103175=CARTESIAN_POINT('Ctrl Pts',(0.00235525079407047,-0.0317740741446515,
0.0746072038523523));
#103176=CARTESIAN_POINT('Ctrl Pts',(0.002340289312027,-0.03202188345824,
0.074824763424338));
#103177=CARTESIAN_POINT('Ctrl Pts',(0.00233326665600961,-0.0319391099350678,
0.074764571244949));
#103178=CARTESIAN_POINT('Ctrl Pts',(0.00232718816416218,-0.031856486945494,
0.0747043058747137));
#103179=CARTESIAN_POINT('Ctrl Pts',(0.00232205416592641,-0.0317740741446515,
0.0746440116222868));
#103180=CARTESIAN_POINT('Ctrl Pts',(0.00230825710637647,-0.03202188345824,
0.0748625888899511));
#103181=CARTESIAN_POINT('Ctrl Pts',(0.00230084077870451,-0.0319391099350678,
0.0748020633327386));
#103182=CARTESIAN_POINT('Ctrl Pts',(0.00229437405945963,-0.031856486945494,
0.074741458639427));
#103183=CARTESIAN_POINT('Ctrl Pts',(0.00228885753778234,-0.0317740741446515,
0.0746808193922213));
#103184=CARTESIAN_POINT('Origin',(-0.00375389621872825,-0.0391228853390656,
0.0763412037500568));
#103185=CARTESIAN_POINT('Ctrl Pts',(0.00350499069638799,-0.0352722978779661,
0.0775779629012608));
#103186=CARTESIAN_POINT('Ctrl Pts',(0.00349401176224274,-0.0352466642097261,
0.0775625825344534));
#103187=CARTESIAN_POINT('Ctrl Pts',(0.00348297879773608,-0.0352210183808323,
0.0775472614200865));
#103188=CARTESIAN_POINT('Ctrl Pts',(0.00347189098139146,-0.0351953608940152,
0.0775319993286817));
#103189=CARTESIAN_POINT('Origin',(-0.000585667115997817,-0.0352456003065141,
0.0802754176011314));
#103190=CARTESIAN_POINT('Ctrl Pts',(0.00340086232025206,-0.035024121149334,
0.0774295286269429));
#103191=CARTESIAN_POINT('Ctrl Pts',(0.00335568816011192,-0.0349144232867422,
0.0773644723451003));
#103192=CARTESIAN_POINT('Ctrl Pts',(0.00331183172083244,-0.0348045283677513,
0.0772984433418113));
#103193=CARTESIAN_POINT('Ctrl Pts',(0.0032693523241576,-0.0346945769586886,
0.0772315241014469));
#103194=CARTESIAN_POINT('Ctrl Pts',(0.00337835581652413,-0.035024121149334,
0.0775405898672251));
#103195=CARTESIAN_POINT('Ctrl Pts',(0.00333165183340497,-0.0349144232867422,
0.0774752235675356));
#103196=CARTESIAN_POINT('Ctrl Pts',(0.00328627106376384,-0.0348045283677513,
0.0774088527383064));
#103197=CARTESIAN_POINT('Ctrl Pts',(0.00324227479811095,-0.0346945769586886,
0.077341560229088));
#103198=CARTESIAN_POINT('Ctrl Pts',(0.0033558493127962,-0.035024121149334,
0.0776516511075072));
#103199=CARTESIAN_POINT('Ctrl Pts',(0.00330761550669801,-0.0349144232867422,
0.0775859747899709));
#103200=CARTESIAN_POINT('Ctrl Pts',(0.00326071040669524,-0.0348045283677513,
0.0775192621348016));
#103201=CARTESIAN_POINT('Ctrl Pts',(0.00321519727206429,-0.0346945769586886,
0.0774515963567292));
#103202=CARTESIAN_POINT('Ctrl Pts',(0.00333334280906827,-0.035024121149334,
0.0777627123477894));
#103203=CARTESIAN_POINT('Ctrl Pts',(0.00328357917999106,-0.0349144232867422,
0.0776967260124062));
#103204=CARTESIAN_POINT('Ctrl Pts',(0.00323514974962664,-0.0348045283677513,
0.0776296715312967));
#103205=CARTESIAN_POINT('Ctrl Pts',(0.00318811974601763,-0.0346945769586886,
0.0775616324843703));
#103206=CARTESIAN_POINT('Origin',(0.0175392078150369,-0.0345629067942413,
0.0683865157154276));
#103207=CARTESIAN_POINT('Ctrl Pts',(0.00308893493111351,-0.0351970973651609,
0.0772846187687842));
#103208=CARTESIAN_POINT('Ctrl Pts',(0.00304550903623238,-0.0350869349321765,
0.0772148677833951));
#103209=CARTESIAN_POINT('Ctrl Pts',(0.00300349725217769,-0.0349764985129713,
0.0771441562168122));
#103210=CARTESIAN_POINT('Ctrl Pts',(0.00296295939908606,-0.034865930684963,
0.0770725724740255));
#103211=CARTESIAN_POINT('Ctrl Pts',(0.00316985488368547,-0.0351970973651609,
0.0772991938134279));
#103212=CARTESIAN_POINT('Ctrl Pts',(0.00312622707131348,-0.0350869349321765,
0.0772305638643158));
#103213=CARTESIAN_POINT('Ctrl Pts',(0.00308398989677888,-0.0349764985129713,
0.0771609700649104));
#103214=CARTESIAN_POINT('Ctrl Pts',(0.00304320338697462,-0.034865930684963,
0.077090499354913));
#103215=CARTESIAN_POINT('Ctrl Pts',(0.00325077483625743,-0.0351970973651609,
0.0773137688580717));
#103216=CARTESIAN_POINT('Ctrl Pts',(0.00320694510639458,-0.0350869349321765,
0.0772462599452364));
#103217=CARTESIAN_POINT('Ctrl Pts',(0.00316448254138008,-0.0349764985129713,
0.0771777839130087));
#103218=CARTESIAN_POINT('Ctrl Pts',(0.00312344737486319,-0.034865930684963,
0.0771084262358005));
#103219=CARTESIAN_POINT('Ctrl Pts',(0.00333169478882939,-0.0351970973651609,
0.0773283439027154));
#103220=CARTESIAN_POINT('Ctrl Pts',(0.00328766314147569,-0.0350869349321765,
0.0772619560261571));
#103221=CARTESIAN_POINT('Ctrl Pts',(0.00324497518598127,-0.0349764985129713,
0.0771945977611069));
#103222=CARTESIAN_POINT('Ctrl Pts',(0.00320369136275175,-0.034865930684963,
0.077126353116688));
#103223=CARTESIAN_POINT('Origin',(0.0177504063812929,-0.0345637187967915,
0.0688186274160212));
#103224=CARTESIAN_POINT('Ctrl Pts',(0.0033495061650528,-0.0352450361861253,
0.0773569320865797));
#103225=CARTESIAN_POINT('Ctrl Pts',(0.00322855473979882,-0.0349452761023765,
0.077176867316089));
#103226=CARTESIAN_POINT('Ctrl Pts',(0.00312151013972454,-0.0346444289983474,
0.0769882035346211));
#103227=CARTESIAN_POINT('Ctrl Pts',(0.00349338254862458,-0.0352450361861253,
0.0775613815577218));
#103228=CARTESIAN_POINT('Ctrl Pts',(0.00336472018523426,-0.0349452761023765,
0.0773867431739409));
#103229=CARTESIAN_POINT('Ctrl Pts',(0.00324957781534661,-0.0346444289983474,
0.0772029095439938));
#103230=CARTESIAN_POINT('Ctrl Pts',(0.0032042590746301,-0.0345231616327822,
0.0771265034939999));
#103231=CARTESIAN_POINT('Ctrl Pts',(0.0031632321645473,-0.0344132092796975,
0.0770586947939467));
#103232=CARTESIAN_POINT('Ctrl Pts',(0.00312360994073829,-0.0343032738558974,
0.0769900409832371));
#103233=CARTESIAN_POINT('Ctrl Pts',(0.00308544091088991,-0.0341934961088741,
0.0769206313155901));
#103234=CARTESIAN_POINT('Ctrl Pts',(0.00317482341338464,-0.0345231616327822,
0.0772359323658098));
#103235=CARTESIAN_POINT('Ctrl Pts',(0.00313228818036747,-0.0344132092796975,
0.0771677179366084));
#103236=CARTESIAN_POINT('Ctrl Pts',(0.00309116610363403,-0.0343032738558974,
0.0770986272192143));
#103237=CARTESIAN_POINT('Ctrl Pts',(0.00305150759801842,-0.0341934961088741,
0.0770287500762939));
#103238=CARTESIAN_POINT('Ctrl Pts',(0.00314538775213918,-0.0345231616327822,
0.0773453612376198));
#103239=CARTESIAN_POINT('Ctrl Pts',(0.00310134419618765,-0.0344132092796975,
0.0772767410792702));
#103240=CARTESIAN_POINT('Ctrl Pts',(0.00305872226652977,-0.0343032738558974,
0.0772072134551915));
#103241=CARTESIAN_POINT('Ctrl Pts',(0.00301757428514694,-0.034193496108874,
0.0771368688369976));
#103242=CARTESIAN_POINT('Ctrl Pts',(0.00311595209089371,-0.0345231616327822,
0.0774547901094297));
#103243=CARTESIAN_POINT('Ctrl Pts',(0.00307040021200782,-0.0344132092796975,
0.0773857642219319));
#103244=CARTESIAN_POINT('Ctrl Pts',(0.0030262784294255,-0.0343032738558974,
0.0773157996911687));
#103245=CARTESIAN_POINT('Ctrl Pts',(0.00298364097227546,-0.034193496108874,
0.0772449875977014));
#103246=CARTESIAN_POINT('Origin',(0.0175493979460578,-0.0345625596230862,
0.0683799842894739));
#103247=CARTESIAN_POINT('Ctrl Pts',(0.00281131354479945,-0.0346945769586885,
0.0769388486622199));
#103248=CARTESIAN_POINT('Ctrl Pts',(0.00277288180063825,-0.0345846629176689,
0.0768656401591118));
#103249=CARTESIAN_POINT('Ctrl Pts',(0.00273595741401905,-0.0344746925051586,
0.0767916243991256));
#103250=CARTESIAN_POINT('Ctrl Pts',(0.00270058730505555,-0.034364806625517,
0.0767168964151731));
#103251=CARTESIAN_POINT('Ctrl Pts',(0.00292134958580179,-0.0346945769586885,
0.0769659261669466));
#103252=CARTESIAN_POINT('Ctrl Pts',(0.00288254469993941,-0.0345846629176689,
0.0768942340161001));
#103253=CARTESIAN_POINT('Ctrl Pts',(0.00284521575034348,-0.0344746925051586,
0.0768217271509552));
#103254=CARTESIAN_POINT('Ctrl Pts',(0.00280941018348495,-0.034364806625517,
0.0767484986731943));
#103255=CARTESIAN_POINT('Ctrl Pts',(0.00303138562680414,-0.0346945769586885,
0.0769930036716733));
#103256=CARTESIAN_POINT('Ctrl Pts',(0.00299220759924057,-0.0345846629176689,
0.0769228278730884));
#103257=CARTESIAN_POINT('Ctrl Pts',(0.0029544740866679,-0.0344746925051586,
0.0768518299027847));
#103258=CARTESIAN_POINT('Ctrl Pts',(0.00291823306191435,-0.034364806625517,
0.0767801009312154));
#103259=CARTESIAN_POINT('Ctrl Pts',(0.00314142166780648,-0.0346945769586885,
0.0770200811764));
#103260=CARTESIAN_POINT('Ctrl Pts',(0.00310187049854172,-0.0345846629176689,
0.0769514217300768));
#103261=CARTESIAN_POINT('Ctrl Pts',(0.00306373242299233,-0.0344746925051586,
0.0768819326546142));
#103262=CARTESIAN_POINT('Ctrl Pts',(0.00302705594034375,-0.034364806625517,
0.0768117031892366));
#103263=CARTESIAN_POINT('Origin',(0.0178011398758306,-0.0345626446730454,
0.0687896404668735));
#103264=CARTESIAN_POINT('Ctrl Pts',(0.00313945275405448,-0.0346945769586885,
0.0770195966690427));
#103265=CARTESIAN_POINT('Ctrl Pts',(0.00307934790289853,-0.034527515336289,
0.0769151978933269));
#103266=CARTESIAN_POINT('Ctrl Pts',(0.00302251075095321,-0.0343603235965158,
0.0768088818724941));
#103267=CARTESIAN_POINT('Ctrl Pts',(0.00296910472395195,-0.034193496108874,
0.0767009655405301));
#103268=CARTESIAN_POINT('Ctrl Pts',(0.00318284991868958,-0.0346945769586885,
0.07709132333377));
#103269=CARTESIAN_POINT('Ctrl Pts',(0.00312124272382316,-0.034527515336289,
0.0769878335290427));
#103270=CARTESIAN_POINT('Ctrl Pts',(0.00306287425328339,-0.0343603235965158,
0.076882379466978));
#103271=CARTESIAN_POINT('Ctrl Pts',(0.00300791249965346,-0.034193496108874,
0.0767752755995824));
#103272=CARTESIAN_POINT('Ctrl Pts',(0.00322624708332469,-0.0346945769586885,
0.0771630499984973));
#103273=CARTESIAN_POINT('Ctrl Pts',(0.00316313754474779,-0.034527515336289,
0.0770604691647585));
#103274=CARTESIAN_POINT('Ctrl Pts',(0.00310323775561356,-0.0343603235965158,
0.0769558770614619));
#103275=CARTESIAN_POINT('Ctrl Pts',(0.00304672027535497,-0.034193496108874,
0.0768495856586347));
#103276=CARTESIAN_POINT('Ctrl Pts',(0.0032696442479598,-0.0346945769586885,
0.0772347766632246));
#103277=CARTESIAN_POINT('Ctrl Pts',(0.00320503236567241,-0.034527515336289,
0.0771331048004743));
#103278=CARTESIAN_POINT('Ctrl Pts',(0.00314360125794374,-0.0343603235965158,
0.0770293746559459));
#103279=CARTESIAN_POINT('Ctrl Pts',(0.00308552805105648,-0.034193496108874,
0.0769238957176871));
#103280=CARTESIAN_POINT('Ctrl Pts',(0.00302707104082222,-0.0340223579322365,
0.0768117309011883));
#103281=CARTESIAN_POINT('Ctrl Pts',(0.00299035882960958,-0.0339125849573554,
0.0767414339616182));
#103282=CARTESIAN_POINT('Ctrl Pts',(0.00295512739894426,-0.0338030433565221,
0.076670426561429));
#103283=CARTESIAN_POINT('Ctrl Pts',(0.00292141375427354,-0.0336938721132328,
0.0765988035010579));
#103284=CARTESIAN_POINT('Ctrl Pts',(0.00299082232396728,-0.0340223579322365,
0.0769190957481205));
#103285=CARTESIAN_POINT('Ctrl Pts',(0.00295262927149617,-0.0339125849573554,
0.0768482988442044));
#103286=CARTESIAN_POINT('Ctrl Pts',(0.00291592838824261,-0.0338030433565221,
0.0767767611810152));
#103287=CARTESIAN_POINT('Ctrl Pts',(0.0028807584987238,-0.0336938721132328,
0.0767045784036889));
#103288=CARTESIAN_POINT('Ctrl Pts',(0.00295457360711233,-0.0340223579322365,
0.0770264605950527));
#103289=CARTESIAN_POINT('Ctrl Pts',(0.00291489971338277,-0.0339125849573554,
0.0769551637267906));
#103290=CARTESIAN_POINT('Ctrl Pts',(0.00287672937754096,-0.0338030433565221,
0.0768830958006015));
#103291=CARTESIAN_POINT('Ctrl Pts',(0.00284010324317407,-0.0336938721132328,
0.0768103533063199));
#103292=CARTESIAN_POINT('Ctrl Pts',(0.00291832489025738,-0.0340223579322365,
0.077133825441985));
#103293=CARTESIAN_POINT('Ctrl Pts',(0.00287717015526936,-0.0339125849573554,
0.0770620286093768));
#103294=CARTESIAN_POINT('Ctrl Pts',(0.00283753036683931,-0.0338030433565221,
0.0769894304201877));
#103295=CARTESIAN_POINT('Ctrl Pts',(0.00279944798762434,-0.0336938721132328,
0.0769161282089509));
#103296=CARTESIAN_POINT('Origin',(0.0174455344802189,-0.0345589643414732,
0.0684405256685634));
#103297=CARTESIAN_POINT('Ctrl Pts',(0.00264668323176961,-0.034193496108874,
0.0765997728400264));
#103298=CARTESIAN_POINT('Ctrl Pts',(0.00261290231500352,-0.0340836138581107,
0.0765242468887588));
#103299=CARTESIAN_POINT('Ctrl Pts',(0.00258070045804288,-0.03397388966435,
0.0764480581510719));
#103300=CARTESIAN_POINT('Ctrl Pts',(0.00255011233856891,-0.0338644633294062,
0.0763713069019447));
#103301=CARTESIAN_POINT('Ctrl Pts',(0.00275480208975648,-0.034193496108874,
0.0766337061834304));
#103302=CARTESIAN_POINT('Ctrl Pts',(0.00272055325227938,-0.0340836138581107,
0.0765596711271889));
#103303=CARTESIAN_POINT('Ctrl Pts',(0.00268785284818063,-0.03397388966435,
0.0764849628865316));
#103304=CARTESIAN_POINT('Ctrl Pts',(0.00265673632024154,-0.0338644633294062,
0.0764096798843573));
#103305=CARTESIAN_POINT('Ctrl Pts',(0.00286292094774335,-0.034193496108874,
0.0766676395268344));
#103306=CARTESIAN_POINT('Ctrl Pts',(0.00282820418955523,-0.0340836138581107,
0.0765950953656192));
#103307=CARTESIAN_POINT('Ctrl Pts',(0.00279500523831838,-0.03397388966435,
0.0765218676219912));
#103308=CARTESIAN_POINT('Ctrl Pts',(0.00276336030191417,-0.0338644633294062,
0.0764480528667698));
#103309=CARTESIAN_POINT('Ctrl Pts',(0.00297103980573021,-0.034193496108874,
0.0767015728702384));
#103310=CARTESIAN_POINT('Ctrl Pts',(0.00293585512683108,-0.0340836138581107,
0.0766305196040494));
#103311=CARTESIAN_POINT('Ctrl Pts',(0.00290215762845613,-0.03397388966435,
0.0765587723574509));
#103312=CARTESIAN_POINT('Ctrl Pts',(0.00286998428358681,-0.0338644633294062,
0.0764864258491823));
#103313=CARTESIAN_POINT('Origin',(0.0177347451211335,-0.0345610621863674,
0.0688251127413223));
#103314=CARTESIAN_POINT('Ctrl Pts',(0.00298525284944489,-0.03424362768739,
0.0767333391539459));
#103315=CARTESIAN_POINT('Ctrl Pts',(0.00288782060706489,-0.033943005420186,
0.0765395363248733));
#103316=CARTESIAN_POINT('Ctrl Pts',(0.00280526318263899,-0.0336441434784162,
0.0763389450736088));
#103317=CARTESIAN_POINT('Ctrl Pts',(0.00310237342613376,-0.03424362768739,
0.0769542073737423));
#103318=CARTESIAN_POINT('Ctrl Pts',(0.00299661100151951,-0.033943005420186,
0.0767648218200392));
#103319=CARTESIAN_POINT('Ctrl Pts',(0.00290541433275375,-0.0336441434784162,
0.0765680078316702));
#103320=CARTESIAN_POINT('Ctrl Pts',(0.00286999566758987,-0.0335235895815127,
0.0764864511361787));
#103321=CARTESIAN_POINT('Ctrl Pts',(0.00283782981765183,-0.0334144449262719,
0.0764141224209021));
#103322=CARTESIAN_POINT('Ctrl Pts',(0.00280712126987339,-0.0333049234473133,
0.0763410460864424));
#103323=CARTESIAN_POINT('Ctrl Pts',(0.0027779177554575,-0.0331951640388588,
0.0762673120180385));
#103324=CARTESIAN_POINT('Ctrl Pts',(0.00282707694921841,-0.0335235895815127,
0.0765913279977993));
#103325=CARTESIAN_POINT('Ctrl Pts',(0.00279346726279665,-0.0334144449262719,
0.0765184084218652));
#103326=CARTESIAN_POINT('Ctrl Pts',(0.0027613254264778,-0.0333049234473133,
0.0764447107193454));
#103327=CARTESIAN_POINT('Ctrl Pts',(0.0027307010761736,-0.0331951640388588,
0.0763703254040009));
#103328=CARTESIAN_POINT('Ctrl Pts',(0.00278415823084696,-0.0335235895815127,
0.0766962048594199));
#103329=CARTESIAN_POINT('Ctrl Pts',(0.00274910470794147,-0.0334144449262719,
0.0766226944228283));
#103330=CARTESIAN_POINT('Ctrl Pts',(0.00271552958308222,-0.0333049234473133,
0.0765483753522485));
#103331=CARTESIAN_POINT('Ctrl Pts',(0.00268348439688969,-0.0331951640388588,
0.0764733387899634));
#103332=CARTESIAN_POINT('Ctrl Pts',(0.00274123951247551,-0.0335235895815127,
0.0768010817210406));
#103333=CARTESIAN_POINT('Ctrl Pts',(0.00270474215308629,-0.0334144449262719,
0.0767269804237914));
#103334=CARTESIAN_POINT('Ctrl Pts',(0.00266973373968662,-0.0333049234473133,
0.0766520399851516));
#103335=CARTESIAN_POINT('Ctrl Pts',(0.00263626771760579,-0.0331951640388588,
0.0765763521759258));
#103336=CARTESIAN_POINT('Origin',(0.0185379407817257,-0.032643457177078,
0.0708439813735357));
#103337=CARTESIAN_POINT('Ctrl Pts',(0.00250177593814554,-0.0336938721132429,
0.0762503014554384));
#103338=CARTESIAN_POINT('Ctrl Pts',(0.00248948217677242,-0.0336474569764978,
0.0762173939872473));
#103339=CARTESIAN_POINT('Ctrl Pts',(0.00247757448123973,-0.033601104548885,
0.0761843448598979));
#103340=CARTESIAN_POINT('Ctrl Pts',(0.00244742693520127,-0.0334837508643188,
0.0761006720715267));
#103341=CARTESIAN_POINT('Ctrl Pts',(0.0024197720258371,-0.033366026476046,
0.0760161426918175));
#103342=CARTESIAN_POINT('Ctrl Pts',(0.00281909985087487,-0.0336938721132429,
0.0763722669164609));
#103343=CARTESIAN_POINT('Ctrl Pts',(0.00280609218518593,-0.0336474569764978,
0.0763412168504303));
#103344=CARTESIAN_POINT('Ctrl Pts',(0.00279344889101716,-0.033601104548885,
0.0763100166408197));
#103345=CARTESIAN_POINT('Ctrl Pts',(0.00276143897843713,-0.0334837508643188,
0.0762310248868684));
#103346=CARTESIAN_POINT('Ctrl Pts',(0.00273178381159619,-0.033366026476046,
0.0761511193002344));
#103347=CARTESIAN_POINT('Ctrl Pts',(0.00281909985088202,-0.0336938721132427,
0.0763722669164641));
#103348=CARTESIAN_POINT('Ctrl Pts',(0.00280609218519454,-0.0336474569765026,
0.0763412168504368));
#103349=CARTESIAN_POINT('Ctrl Pts',(0.00279344889102716,-0.0336011045488949,
0.0763100166408297));
#103350=CARTESIAN_POINT('Ctrl Pts',(0.00276170557741933,-0.0334847282606778,
0.0762316827805968));
#103351=CARTESIAN_POINT('Ctrl Pts',(0.00273227784254589,-0.0333679869945435,
0.076152449958875));
#103352=CARTESIAN_POINT('Ctrl Pts',(0.00281909985087479,-0.0336938721132426,
0.0763722669164607));
#103353=CARTESIAN_POINT('Ctrl Pts',(0.00277257868190858,-0.0335278710435083,
0.0762612181393193));
#103354=CARTESIAN_POINT('Ctrl Pts',(0.00272955633976043,-0.033362046922432,
0.076148749537116));
#103355=CARTESIAN_POINT('Ctrl Pts',(0.00269003013551838,-0.0331951640388602,
0.076034798020117));
#103356=CARTESIAN_POINT('Ctrl Pts',(0.00285316508469761,-0.0336938721132426,
0.076448867110115));
#103357=CARTESIAN_POINT('Ctrl Pts',(0.00280504035923445,-0.0335278710435083,
0.0763385314581551));
#103358=CARTESIAN_POINT('Ctrl Pts',(0.00276039266129652,-0.033362046922432,
0.076226725443143));
#103359=CARTESIAN_POINT('Ctrl Pts',(0.00271921838342804,-0.0331951640388602,
0.0761133860345164));
#103360=CARTESIAN_POINT('Ctrl Pts',(0.00288723031852043,-0.0336938721132426,
0.0765254673037692));
#103361=CARTESIAN_POINT('Ctrl Pts',(0.00283750203656033,-0.0335278710435083,
0.076415844776991));
#103362=CARTESIAN_POINT('Ctrl Pts',(0.00279122898283262,-0.033362046922432,
0.07630470134917));
#103363=CARTESIAN_POINT('Ctrl Pts',(0.00274840663133769,-0.0331951640388602,
0.0761919740489158));
#103364=CARTESIAN_POINT('Ctrl Pts',(0.00292129555234325,-0.0336938721132426,
0.0766020674974234));
#103365=CARTESIAN_POINT('Ctrl Pts',(0.0028699637138862,-0.0335278710435083,
0.0764931580958269));
#103366=CARTESIAN_POINT('Ctrl Pts',(0.00282206530436872,-0.033362046922432,
0.076382677255197));
#103367=CARTESIAN_POINT('Ctrl Pts',(0.00277759487924734,-0.0331951640388602,
0.0762705620633152));
#103368=CARTESIAN_POINT('Ctrl Pts',(0.00273365594444268,-0.0330240426238155,
0.0761519539963238));
#103369=CARTESIAN_POINT('Ctrl Pts',(0.0027060770777342,-0.0329142774063509,
0.0760776997559033));
#103370=CARTESIAN_POINT('Ctrl Pts',(0.00268001950452334,-0.0328043479726686,
0.0760028383648232));
#103371=CARTESIAN_POINT('Ctrl Pts',(0.00265551924765414,-0.0326943950436594,
0.0759274648067751));
#103372=CARTESIAN_POINT('Ctrl Pts',(0.00268423673031011,-0.0330240426238155,
0.0762539288817572));
#103373=CARTESIAN_POINT('Ctrl Pts',(0.00265525306020547,-0.0329142774063509,
0.0761789938435152));
#103374=CARTESIAN_POINT('Ctrl Pts',(0.00262780405724542,-0.0328043479726686,
0.0761034222740008));
#103375=CARTESIAN_POINT('Ctrl Pts',(0.00260192755185462,-0.0326943950436594,
0.0760273100176065));
#103376=CARTESIAN_POINT('Ctrl Pts',(0.00263481751617755,-0.0330240426238155,
0.0763559037671906));
#103377=CARTESIAN_POINT('Ctrl Pts',(0.00260442904267675,-0.0329142774063509,
0.0762802879311271));
#103378=CARTESIAN_POINT('Ctrl Pts',(0.0025755886099675,-0.0328043479726686,
0.0762040061831784));
#103379=CARTESIAN_POINT('Ctrl Pts',(0.00254833585605509,-0.0326943950436594,
0.0761271552284379));
#103380=CARTESIAN_POINT('Ctrl Pts',(0.00258539830204498,-0.0330240426238155,
0.076457878652624));
#103381=CARTESIAN_POINT('Ctrl Pts',(0.00255360502514803,-0.0329142774063509,
0.076381582018739));
#103382=CARTESIAN_POINT('Ctrl Pts',(0.00252337316268958,-0.0328043479726686,
0.0763045900923559));
#103383=CARTESIAN_POINT('Ctrl Pts',(0.00249474416025557,-0.0326943950436594,
0.0762270004392693));
#103384=CARTESIAN_POINT('Origin',(0.0186549526395914,-0.0326396682857451,
0.0708039361001382));
#103385=CARTESIAN_POINT('Ctrl Pts',(0.00238283384147148,-0.0331951640388587,
0.0758939931260949));
#103386=CARTESIAN_POINT('Ctrl Pts',(0.00235881386422889,-0.0330855618255041,
0.0758149231763951));
#103387=CARTESIAN_POINT('Ctrl Pts',(0.00233641081202227,-0.0329757224427708,
0.0757352997744029));
#103388=CARTESIAN_POINT('Ctrl Pts',(0.0023156583747808,-0.0328657862078596,
0.0756552234754363));
#103389=CARTESIAN_POINT('Ctrl Pts',(0.00248584714540612,-0.0331951640388587,
0.075941209767781));
#103390=CARTESIAN_POINT('Ctrl Pts',(0.00246117685444279,-0.0330855618255041,
0.0758635586179486));
#103391=CARTESIAN_POINT('Ctrl Pts',(0.00243809369554534,-0.0329757224427708,
0.0757853415977439));
#103392=CARTESIAN_POINT('Ctrl Pts',(0.00241663214121971,-0.0328657862078596,
0.0757066574188082));
#103393=CARTESIAN_POINT('Ctrl Pts',(0.00258886044934076,-0.0331951640388587,
0.075988426409467));
#103394=CARTESIAN_POINT('Ctrl Pts',(0.0025635398446567,-0.0330855618255041,
0.0759121940595022));
#103395=CARTESIAN_POINT('Ctrl Pts',(0.00253977657906841,-0.0329757224427708,
0.075835383421085));
#103396=CARTESIAN_POINT('Ctrl Pts',(0.00251760590765862,-0.0328657862078596,
0.0757580913621801));
#103397=CARTESIAN_POINT('Ctrl Pts',(0.0026918737532754,-0.0331951640388587,
0.0760356430511531));
#103398=CARTESIAN_POINT('Ctrl Pts',(0.0026659028348706,-0.0330855618255041,
0.0759608295010557));
#103399=CARTESIAN_POINT('Ctrl Pts',(0.00264145946259147,-0.0329757224427708,
0.075885425244426));
#103400=CARTESIAN_POINT('Ctrl Pts',(0.00261857967409753,-0.0328657862078596,
0.075809525305552));
#103401=CARTESIAN_POINT('Origin',(0.0187633690656965,-0.0326401908828985,
0.0712724643819485));
#103402=CARTESIAN_POINT('Ctrl Pts',(0.00270196925966051,-0.0332451089994433,
0.0760688719380663));
#103403=CARTESIAN_POINT('Ctrl Pts',(0.00262959782045771,-0.0329451141710259,
0.0758643849176987));
#103404=CARTESIAN_POINT('Ctrl Pts',(0.00257283477919912,-0.0326442513127504,
0.0756550275107169));
#103405=CARTESIAN_POINT('Ctrl Pts',(0.00279048123139834,-0.0332451089994433,
0.076302678761874));
#103406=CARTESIAN_POINT('Ctrl Pts',(0.00270929162356284,-0.0329451141710259,
0.0761015300251378));
#103407=CARTESIAN_POINT('Ctrl Pts',(0.00264348401198786,-0.0326442513127504,
0.0758948371975654));
#103408=CARTESIAN_POINT('Ctrl Pts',(0.00261858870498485,-0.0325229783203385,
0.0758095555747362));
#103409=CARTESIAN_POINT('Ctrl Pts',(0.0025957117680956,-0.032413025311208,
0.0757336666042744));
#103410=CARTESIAN_POINT('Ctrl Pts',(0.0025744081617537,-0.0323031222247695,
0.0756573159050432));
#103411=CARTESIAN_POINT('Ctrl Pts',(0.00255470172332999,-0.0321934096636184,
0.0755806022397748));
#103412=CARTESIAN_POINT('Ctrl Pts',(0.00256286395368766,-0.0325229783203385,
0.075908226212427));
#103413=CARTESIAN_POINT('Ctrl Pts',(0.00253862684424039,-0.032413025311208,
0.0758315690775011));
#103414=CARTESIAN_POINT('Ctrl Pts',(0.0025159791621057,-0.0323031222247695,
0.075754422193397));
#103415=CARTESIAN_POINT('Ctrl Pts',(0.00249494643033256,-0.0321934096636184,
0.0756768854034548));
#103416=CARTESIAN_POINT('Ctrl Pts',(0.00250713920239047,-0.0325229783203385,
0.0760068968501178));
#103417=CARTESIAN_POINT('Ctrl Pts',(0.00248154192038518,-0.032413025311208,
0.0759294715507279));
#103418=CARTESIAN_POINT('Ctrl Pts',(0.0024575501624577,-0.0323031222247695,
0.0758515284817508));
#103419=CARTESIAN_POINT('Ctrl Pts',(0.00243519113733513,-0.0321934096636184,
0.0757731685671348));
#103420=CARTESIAN_POINT('Ctrl Pts',(0.00245141445109328,-0.0325229783203385,
0.0761055674878086));
#103421=CARTESIAN_POINT('Ctrl Pts',(0.00242445699652996,-0.032413025311208,
0.0760273740239547));
#103422=CARTESIAN_POINT('Ctrl Pts',(0.00239912116280971,-0.0323031222247695,
0.0759486347701046));
#103423=CARTESIAN_POINT('Ctrl Pts',(0.00237543584433769,-0.0321934096636184,
0.0758694517308149));
#103424=CARTESIAN_POINT('Origin',(0.0186467580066177,-0.0326393375179189,
0.070806289611769));
#103425=CARTESIAN_POINT('Ctrl Pts',(0.0022846560572056,-0.0326943950436593,
0.0755300746244477));
#103426=CARTESIAN_POINT('Ctrl Pts',(0.00226563604234525,-0.0325844576448127,
0.0754496005226064));
#103427=CARTESIAN_POINT('Ctrl Pts',(0.00224827901777408,-0.0324744968375319,
0.0753687273603969));
#103428=CARTESIAN_POINT('Ctrl Pts',(0.00223260579310099,-0.0323646534831894,
0.0752875590639713));
#103429=CARTESIAN_POINT('Ctrl Pts',(0.00238450123536857,-0.0326943950436593,
0.0755836663027125));
#103430=CARTESIAN_POINT('Ctrl Pts',(0.00236474262674023,-0.0325844576448127,
0.0755045682545562));
#103431=CARTESIAN_POINT('Ctrl Pts',(0.00234661849708335,-0.0324744968375319,
0.0754250559680869));
#103432=CARTESIAN_POINT('Ctrl Pts',(0.00233015066291658,-0.0323646534831894,
0.0753452316393802));
#103433=CARTESIAN_POINT('Ctrl Pts',(0.00248434641353155,-0.0326943950436593,
0.0756372579809774));
#103434=CARTESIAN_POINT('Ctrl Pts',(0.00246384921113521,-0.0325844576448127,
0.0755595359865059));
#103435=CARTESIAN_POINT('Ctrl Pts',(0.00244495797639263,-0.0324744968375319,
0.075481384575777));
#103436=CARTESIAN_POINT('Ctrl Pts',(0.00242769553273217,-0.0323646534831894,
0.0754029042147891));
#103437=CARTESIAN_POINT('Ctrl Pts',(0.00258419159169452,-0.0326943950436593,
0.0756908496592422));
#103438=CARTESIAN_POINT('Ctrl Pts',(0.00256295579553019,-0.0325844576448127,
0.0756145037184556));
#103439=CARTESIAN_POINT('Ctrl Pts',(0.00254329745570191,-0.0324744968375319,
0.075537713183467));
#103440=CARTESIAN_POINT('Ctrl Pts',(0.00252524040254776,-0.0323646534831894,
0.075460576790198));
#103441=CARTESIAN_POINT('Origin',(0.0187997757146061,-0.0326395579065083,
0.0712621436390492));
#103442=CARTESIAN_POINT('Ctrl Pts',(0.0025921917420538,-0.0327445246961877,
0.075724684756325));
#103443=CARTESIAN_POINT('Ctrl Pts',(0.00253280153618932,-0.0324436878365475,
0.0755160574140417));
#103444=CARTESIAN_POINT('Ctrl Pts',(0.0024892947155517,-0.0321434074463187,
0.0753035492470014));
#103445=CARTESIAN_POINT('Ctrl Pts',(0.0026658498329768,-0.0327445246961877,
0.0759635874261334));
#103446=CARTESIAN_POINT('Ctrl Pts',(0.0025974492657149,-0.0324436878365475,
0.0757577381441354));
#103447=CARTESIAN_POINT('Ctrl Pts',(0.00254474842631184,-0.0321434074463187,
0.0755473214479656));
#103448=CARTESIAN_POINT('Ctrl Pts',(0.00250304393363748,-0.0322357242816073,
0.0753687807097753));
#103449=CARTESIAN_POINT('Ctrl Pts',(0.0024642273487318,-0.0319819883628706,
0.0751897674860417));
#103450=CARTESIAN_POINT('Ctrl Pts',(0.00243688055398963,-0.0317295851069886,
0.0750086470444769));
#103451=CARTESIAN_POINT('Ctrl Pts',(0.00256131946590874,-0.0322357242816073,
0.0756118937747029));
#103452=CARTESIAN_POINT('Ctrl Pts',(0.00251476004519121,-0.0319819883628706,
0.0754347365510916));
#103453=CARTESIAN_POINT('Ctrl Pts',(0.00247956800385742,-0.0317295851069886,
0.0752549756494414));
#103454=CARTESIAN_POINT('Origin',(0.0187073500398116,-0.0326371942646192,
0.0712853793484881));
#103455=CARTESIAN_POINT('Origin',(0.0185289370504553,-0.0326352985523298,
0.0708406702041081));
#103456=CARTESIAN_POINT('Ctrl Pts',(0.00220952263615451,-0.0321934096636184,
0.0751607095987536));
#103457=CARTESIAN_POINT('Ctrl Pts',(0.00219558416308856,-0.0320835708272304,
0.0750791473501697));
#103458=CARTESIAN_POINT('Ctrl Pts',(0.00218334170139865,-0.0319739230346346,
0.074997343955029));
#103459=CARTESIAN_POINT('Ctrl Pts',(0.0021728028819668,-0.0318646057455576,
0.0749154052772209));
#103460=CARTESIAN_POINT('Ctrl Pts',(0.0023058058827452,-0.0321934096636184,
0.0752204649432071));
#103461=CARTESIAN_POINT('Ctrl Pts',(0.00229104333690875,-0.0320835708272304,
0.0751402305156323));
#103462=CARTESIAN_POINT('Ctrl Pts',(0.00227794980125727,-0.0319739230346346,
0.0750597371171674));
#103463=CARTESIAN_POINT('Ctrl Pts',(0.00226653412419501,-0.0318646057455576,
0.0749790890192212));
#103464=CARTESIAN_POINT('Ctrl Pts',(0.00240208912933588,-0.0321934096636184,
0.0752802202876605));
#103465=CARTESIAN_POINT('Ctrl Pts',(0.00238650251072894,-0.0320835708272304,
0.0752013136810948));
#103466=CARTESIAN_POINT('Ctrl Pts',(0.0023725579011159,-0.0319739230346346,
0.0751221302793057));
#103467=CARTESIAN_POINT('Ctrl Pts',(0.00236026536642323,-0.0318646057455576,
0.0750427727612214));
#103468=CARTESIAN_POINT('Ctrl Pts',(0.00249837237592657,-0.0321934096636184,
0.075339975632114));
#103469=CARTESIAN_POINT('Ctrl Pts',(0.00248196168454913,-0.0320835708272304,
0.0752623968465574));
#103470=CARTESIAN_POINT('Ctrl Pts',(0.00246716600097452,-0.0319739230346346,
0.0751845234414441));
#103471=CARTESIAN_POINT('Ctrl Pts',(0.00245399660865145,-0.0318646057455576,
0.0751064565032216));
#103472=CARTESIAN_POINT('Ctrl Pts',(0.00252454183115225,-0.03202188345824,
0.0754612227764161));
#103473=CARTESIAN_POINT('Ctrl Pts',(0.00251089517191015,-0.0319391099350675,
0.0754029482203234));
#103474=CARTESIAN_POINT('Ctrl Pts',(0.00249816674619664,-0.0318564869454936,
0.0753444958768062));
#103475=CARTESIAN_POINT('Ctrl Pts',(0.00248636185033058,-0.0317740741446509,
0.0752859091861526));
#103476=CARTESIAN_POINT('Ctrl Pts',(0.00249750299692719,-0.03202188345824,
0.0755027646768473));
#103477=CARTESIAN_POINT('Ctrl Pts',(0.0024834239869285,-0.0319391099350675,
0.0754442087118564));
#103478=CARTESIAN_POINT('Ctrl Pts',(0.00247026786664812,-0.0318564869454936,
0.0753854683787216));
#103479=CARTESIAN_POINT('Ctrl Pts',(0.00245804022434095,-0.0317740741446509,
0.075326587356576));
#103480=CARTESIAN_POINT('Ctrl Pts',(0.00247046416270213,-0.03202188345824,
0.0755443065772786));
#103481=CARTESIAN_POINT('Ctrl Pts',(0.00245595280194684,-0.0319391099350675,
0.0754854692033893));
#103482=CARTESIAN_POINT('Ctrl Pts',(0.00244236898709961,-0.0318564869454936,
0.075426440880637));
#103483=CARTESIAN_POINT('Ctrl Pts',(0.00242971859835133,-0.0317740741446509,
0.0753672655269994));
#103484=CARTESIAN_POINT('Ctrl Pts',(0.00244342532847707,-0.03202188345824,
0.0755858484777098));
#103485=CARTESIAN_POINT('Ctrl Pts',(0.00242848161696518,-0.0319391099350675,
0.0755267296949222));
#103486=CARTESIAN_POINT('Ctrl Pts',(0.0024144701075511,-0.0318564869454936,
0.0754674133825524));
#103487=CARTESIAN_POINT('Ctrl Pts',(0.00240139697236171,-0.0317740741446509,
0.0754079436974228));
#103488=CARTESIAN_POINT('Origin',(-0.00338560652537836,-0.0391228853390713,
0.0778125932965984));
#103489=CARTESIAN_POINT('Ctrl Pts',(0.0039710489218594,-0.0352722978779663,
0.078129820463345));
#103490=CARTESIAN_POINT('Ctrl Pts',(0.00395822888878371,-0.0352466642097263,
0.0781159374006412));
#103491=CARTESIAN_POINT('Ctrl Pts',(0.00394536267769211,-0.0352210183808324,
0.0781021198949546));
#103492=CARTESIAN_POINT('Ctrl Pts',(0.00393244944482438,-0.0351953608940153,
0.0780883678215747));
#103493=CARTESIAN_POINT('Origin',(0.000250727888052832,-0.0352456003065144,
0.0813187002982664));
#103494=CARTESIAN_POINT('Ctrl Pts',(0.00384913788149874,-0.035024121149334,
0.077995607383702));
#103495=CARTESIAN_POINT('Ctrl Pts',(0.00379616621893717,-0.0349144232867421,
0.0779367259136369));
#103496=CARTESIAN_POINT('Ctrl Pts',(0.00374437997228945,-0.0348045283677512,
0.0778767142381083));
#103497=CARTESIAN_POINT('Ctrl Pts',(0.00369384833356284,-0.0346945769586886,
0.0778156467560871));
#103498=CARTESIAN_POINT('Ctrl Pts',(0.00384072851264329,-0.035024121149334,
0.0781086136858207));
#103499=CARTESIAN_POINT('Ctrl Pts',(0.00378620023467461,-0.0349144232867421,
0.0780496163801528));
#103500=CARTESIAN_POINT('Ctrl Pts',(0.00373285883531504,-0.0348045283677512,
0.0779894566233369));
#103501=CARTESIAN_POINT('Ctrl Pts',(0.00368077550558287,-0.0346945769586886,
0.077928208929892));
#103502=CARTESIAN_POINT('Ctrl Pts',(0.00383231914378784,-0.035024121149334,
0.0782216199879394));
#103503=CARTESIAN_POINT('Ctrl Pts',(0.00377623425041205,-0.0349144232867421,
0.0781625068466687));
#103504=CARTESIAN_POINT('Ctrl Pts',(0.00372133769834064,-0.0348045283677512,
0.0781021990085655));
#103505=CARTESIAN_POINT('Ctrl Pts',(0.0036677026776029,-0.0346945769586886,
0.0780407711036969));
#103506=CARTESIAN_POINT('Ctrl Pts',(0.00382390977493239,-0.035024121149334,
0.078334626290058));
#103507=CARTESIAN_POINT('Ctrl Pts',(0.00376626826614949,-0.0349144232867421,
0.0782753973131846));
#103508=CARTESIAN_POINT('Ctrl Pts',(0.00370981656136623,-0.0348045283677512,
0.0782149413937941));
#103509=CARTESIAN_POINT('Ctrl Pts',(0.00365462984962294,-0.0346945769586886,
0.0781533332775019));
#103510=CARTESIAN_POINT('Origin',(0.0167426082500215,-0.0345629067941904,
0.0672518967717792));
#103511=CARTESIAN_POINT('Ctrl Pts',(0.00352150811189216,-0.0351970973651605,
0.0778909350513752));
#103512=CARTESIAN_POINT('Ctrl Pts',(0.00346968252661987,-0.0350869349321763,
0.0778271767811655));
#103513=CARTESIAN_POINT('Ctrl Pts',(0.00341913950874065,-0.0349764985129714,
0.077762288269149));
#103514=CARTESIAN_POINT('Ctrl Pts',(0.00336994948677475,-0.0348659306849635,
0.0776963497257651));
#103515=CARTESIAN_POINT('Ctrl Pts',(0.00360361672394291,-0.0351970973651605,
0.0778952532081228));
#103516=CARTESIAN_POINT('Ctrl Pts',(0.00355173131646102,-0.0350869349321763,
0.0778326324414562));
#103517=CARTESIAN_POINT('Ctrl Pts',(0.00350110477874789,-0.0349764985129714,
0.077768881131607));
#103518=CARTESIAN_POINT('Ctrl Pts',(0.00345180756080035,-0.0348659306849635,
0.0777040780093661));
#103519=CARTESIAN_POINT('Ctrl Pts',(0.00368572533599366,-0.0351970973651605,
0.0778995713648704));
#103520=CARTESIAN_POINT('Ctrl Pts',(0.00363378010630217,-0.0350869349321763,
0.0778380881017469));
#103521=CARTESIAN_POINT('Ctrl Pts',(0.00358307004875512,-0.0349764985129715,
0.0777754739940649));
#103522=CARTESIAN_POINT('Ctrl Pts',(0.00353366563482594,-0.0348659306849635,
0.0777118062929671));
#103523=CARTESIAN_POINT('Ctrl Pts',(0.00376783394804441,-0.0351970973651605,
0.077903889521618));
#103524=CARTESIAN_POINT('Ctrl Pts',(0.00371582889614332,-0.0350869349321763,
0.0778435437620376));
#103525=CARTESIAN_POINT('Ctrl Pts',(0.00366503531876236,-0.0349764985129715,
0.0777820668565228));
#103526=CARTESIAN_POINT('Ctrl Pts',(0.00361552370885153,-0.0348659306849635,
0.0777195345765681));
#103527=CARTESIAN_POINT('Origin',(0.0170062994093576,-0.0345637187965744,
0.0676541309434874));
#103528=CARTESIAN_POINT('Ctrl Pts',(0.00378908792577322,-0.0352450361861252,
0.0779300199217376));
#103529=CARTESIAN_POINT('Ctrl Pts',(0.00364652213869726,-0.0349452761023764,
0.0777665342489764));
#103530=CARTESIAN_POINT('Ctrl Pts',(0.00351667577547945,-0.0346444289983475,
0.0775927743836394));
#103531=CARTESIAN_POINT('Ctrl Pts',(0.00395745411440549,-0.0352450361861252,
0.0781148247553471));
#103532=CARTESIAN_POINT('Ctrl Pts',(0.00380791829883643,-0.0349452761023764,
0.077957689117426));
#103533=CARTESIAN_POINT('Ctrl Pts',(0.00367064339764764,-0.0346444289983475,
0.0777897362360978));
#103534=CARTESIAN_POINT('Ctrl Pts',(0.00361610579142808,-0.0345231616327822,
0.0777196126149445));
#103535=CARTESIAN_POINT('Ctrl Pts',(0.00356690370714396,-0.0344132092796975,
0.0776574806420485));
#103536=CARTESIAN_POINT('Ctrl Pts',(0.00351898931231153,-0.0343032738558974,
0.0775943341685733));
#103537=CARTESIAN_POINT('Ctrl Pts',(0.00347242191857722,-0.0341934961088741,
0.0775302556648203));
#103538=CARTESIAN_POINT('Ctrl Pts',(0.00360061731351277,-0.0345231616327822,
0.0778318678740214));
#103539=CARTESIAN_POINT('Ctrl Pts',(0.00354986794852505,-0.0344132092796975,
0.0777695224142633));
#103540=CARTESIAN_POINT('Ctrl Pts',(0.00350041076862894,-0.0343032738558974,
0.0777061304606602));
#103541=CARTESIAN_POINT('Ctrl Pts',(0.00345230705390109,-0.0341934961088741,
0.0776417748486301));
#103542=CARTESIAN_POINT('Ctrl Pts',(0.00358512883559746,-0.0345231616327822,
0.0779441231330983));
#103543=CARTESIAN_POINT('Ctrl Pts',(0.00353283218990613,-0.0344132092796975,
0.0778815641864782));
#103544=CARTESIAN_POINT('Ctrl Pts',(0.00348183222494634,-0.0343032738558974,
0.0778179267527471));
#103545=CARTESIAN_POINT('Ctrl Pts',(0.00343219218922495,-0.0341934961088741,
0.07775329403244));
#103546=CARTESIAN_POINT('Ctrl Pts',(0.00356964035768215,-0.0345231616327822,
0.0780563783921752));
#103547=CARTESIAN_POINT('Ctrl Pts',(0.00351579643128722,-0.0344132092796975,
0.077993605958693));
#103548=CARTESIAN_POINT('Ctrl Pts',(0.00346325368126374,-0.0343032738558974,
0.077929723044834));
#103549=CARTESIAN_POINT('Ctrl Pts',(0.00341207732454881,-0.0341934961088741,
0.0778648132162498));
#103550=CARTESIAN_POINT('Origin',(0.0167518994234811,-0.0345625596231696,
0.0672441396862457));
#103551=CARTESIAN_POINT('Ctrl Pts',(0.00320273936760623,-0.0346945769586885,
0.0775826866314311));
#103552=CARTESIAN_POINT('Ctrl Pts',(0.0031554352107804,-0.0345846629176052,
0.0775148721739643));
#103553=CARTESIAN_POINT('Ctrl Pts',(0.00310952534941888,-0.0344746925050311,
0.0774460679030849));
#103554=CARTESIAN_POINT('Ctrl Pts',(0.00306506824443851,-0.0343648066253259,
0.0773763622216925));
#103555=CARTESIAN_POINT('Ctrl Pts',(0.00331530145278338,-0.0346945769586885,
0.077595759449118));
#103556=CARTESIAN_POINT('Ctrl Pts',(0.00326781714592219,-0.0345846629176052,
0.0775294961540791));
#103557=CARTESIAN_POINT('Ctrl Pts',(0.00322169502635326,-0.0344746925050311,
0.0774622395851415));
#103558=CARTESIAN_POINT('Ctrl Pts',(0.00317699383515299,-0.0343648066253259,
0.0773940761632334));
#103559=CARTESIAN_POINT('Ctrl Pts',(0.00342786353796052,-0.0346945769586885,
0.0776088322668048));
#103560=CARTESIAN_POINT('Ctrl Pts',(0.00338019908106397,-0.0345846629176052,
0.077544120134194));
#103561=CARTESIAN_POINT('Ctrl Pts',(0.00333386470328764,-0.0344746925050311,
0.077478411267198));
#103562=CARTESIAN_POINT('Ctrl Pts',(0.00328891942586748,-0.0343648066253259,
0.0774117901047743));
#103563=CARTESIAN_POINT('Ctrl Pts',(0.00354042562313766,-0.0346945769586885,
0.0776219050844916));
#103564=CARTESIAN_POINT('Ctrl Pts',(0.00349258101620576,-0.0345846629176052,
0.0775587441143089));
#103565=CARTESIAN_POINT('Ctrl Pts',(0.00344603438022202,-0.0344746925050311,
0.0774945829492545));
#103566=CARTESIAN_POINT('Ctrl Pts',(0.00340084501658196,-0.0343648066253259,
0.0774295040463152));
#103567=CARTESIAN_POINT('Origin',(0.0170529998266576,-0.0345626446730515,
0.0676190139721156));
#103568=CARTESIAN_POINT('Ctrl Pts',(0.00353841150998499,-0.0346945769586886,
0.0776216711679469));
#103569=CARTESIAN_POINT('Ctrl Pts',(0.00346569596739218,-0.034527515336289,
0.0775256287431082));
#103570=CARTESIAN_POINT('Ctrl Pts',(0.00339598206269568,-0.0343603235965158,
0.0774272746398945));
#103571=CARTESIAN_POINT('Ctrl Pts',(0.00332947165532945,-0.0341934961088738,
0.0773269028104969));
#103572=CARTESIAN_POINT('Ctrl Pts',(0.00359045620983789,-0.0346945769586886,
0.0776873931395278));
#103573=CARTESIAN_POINT('Ctrl Pts',(0.0035163640942367,-0.034527515336289,
0.077592440811765));
#103574=CARTESIAN_POINT('Ctrl Pts',(0.00344523897792986,-0.0343603235965158,
0.0774951337956282));
#103575=CARTESIAN_POINT('Ctrl Pts',(0.00337728694011562,-0.0341934961088738,
0.0773957630085222));
#103576=CARTESIAN_POINT('Ctrl Pts',(0.0036425009096908,-0.0346945769586886,
0.0777531151111088));
#103577=CARTESIAN_POINT('Ctrl Pts',(0.00356703222108122,-0.034527515336289,
0.0776592528804219));
#103578=CARTESIAN_POINT('Ctrl Pts',(0.00349449589316403,-0.0343603235965158,
0.0775629929513619));
#103579=CARTESIAN_POINT('Ctrl Pts',(0.00342510222490178,-0.0341934961088738,
0.0774646232065475));
#103580=CARTESIAN_POINT('Ctrl Pts',(0.0036945456095437,-0.0346945769586886,
0.0778188370826897));
#103581=CARTESIAN_POINT('Ctrl Pts',(0.00361770034792574,-0.034527515336289,
0.0777260649490788));
#103582=CARTESIAN_POINT('Ctrl Pts',(0.00354375280839821,-0.0343603235965158,
0.0776308521070957));
#103583=CARTESIAN_POINT('Ctrl Pts',(0.00347291750968795,-0.0341934961088738,
0.0775334834045728));
#103584=CARTESIAN_POINT('Ctrl Pts',(0.00340086347129577,-0.0340223579322365,
0.0774295296472712));
#103585=CARTESIAN_POINT('Ctrl Pts',(0.00335563020408784,-0.0339125849573552,
0.0773643882802087));
#103586=CARTESIAN_POINT('Ctrl Pts',(0.00331177699670363,-0.0338030433565216,
0.0772983564637071));
#103587=CARTESIAN_POINT('Ctrl Pts',(0.00326935244443675,-0.033693872113232,
0.0772315236126616));
#103588=CARTESIAN_POINT('Ctrl Pts',(0.00337835696983735,-0.0340223579322365,
0.0775405910592131));
#103589=CARTESIAN_POINT('Ctrl Pts',(0.00333159187609843,-0.0339125849573552,
0.0774751392687961));
#103590=CARTESIAN_POINT('Ctrl Pts',(0.00328621434362211,-0.0338030433565216,
0.0774087655418211));
#103591=CARTESIAN_POINT('Ctrl Pts',(0.00324227487829685,-0.033693872113232,
0.0773415599032314));
#103592=CARTESIAN_POINT('Ctrl Pts',(0.00335585046837892,-0.0340223579322365,
0.0776516524711549));
#103593=CARTESIAN_POINT('Ctrl Pts',(0.00330755354810902,-0.0339125849573552,
0.0775858902573834));
#103594=CARTESIAN_POINT('Ctrl Pts',(0.00326065169054059,-0.0338030433565216,
0.077519174619935));
#103595=CARTESIAN_POINT('Ctrl Pts',(0.00321519731215695,-0.033693872113232,
0.0774515961938011));
#103596=CARTESIAN_POINT('Ctrl Pts',(0.0033333439669205,-0.0340223579322365,
0.0777627138830968));
#103597=CARTESIAN_POINT('Ctrl Pts',(0.00328351522011961,-0.0339125849573552,
0.0776966412459707));
#103598=CARTESIAN_POINT('Ctrl Pts',(0.00323508903745907,-0.0338030433565216,
0.077629583698049));
#103599=CARTESIAN_POINT('Ctrl Pts',(0.00318811974601705,-0.033693872113232,
0.0775616324843709));
#103600=CARTESIAN_POINT('Origin',(0.0166564427992684,-0.0345589643414914,
0.0673172212223324));
#103601=CARTESIAN_POINT('Ctrl Pts',(0.00299690974454832,-0.0341934961088739,
0.0772669181728474));
#103602=CARTESIAN_POINT('Ctrl Pts',(0.0029539292887104,-0.0340836138581106,
0.0771962216377951));
#103603=CARTESIAN_POINT('Ctrl Pts',(0.00291243237215464,-0.0339738896643499,
0.077124669633921));
#103604=CARTESIAN_POINT('Ctrl Pts',(0.00287246596690574,-0.0338644633294062,
0.07705235729924));
#103605=CARTESIAN_POINT('Ctrl Pts',(0.00310842902870093,-0.0341934961088739,
0.0772870330556225));
#103606=CARTESIAN_POINT('Ctrl Pts',(0.0030651712005411,-0.0340836138581106,
0.0772178743054596));
#103607=CARTESIAN_POINT('Ctrl Pts',(0.00302336522352032,-0.0339738896643499,
0.0771478536089786));
#103608=CARTESIAN_POINT('Ctrl Pts',(0.00298305859660315,-0.0338644633294062,
0.0770770641708263));
#103609=CARTESIAN_POINT('Ctrl Pts',(0.00321994831285354,-0.0341934961088739,
0.0773071479383976));
#103610=CARTESIAN_POINT('Ctrl Pts',(0.00317641311237181,-0.0340836138581106,
0.077239526973124));
#103611=CARTESIAN_POINT('Ctrl Pts',(0.003134298074886,-0.0339738896643499,
0.0771710375840361));
#103612=CARTESIAN_POINT('Ctrl Pts',(0.00309365122630057,-0.0338644633294062,
0.0771017710424124));
#103613=CARTESIAN_POINT('Ctrl Pts',(0.00333146759700616,-0.0341934961088739,
0.0773272628211727));
#103614=CARTESIAN_POINT('Ctrl Pts',(0.00328765502420252,-0.0340836138581106,
0.0772611796407885));
#103615=CARTESIAN_POINT('Ctrl Pts',(0.00324523092625167,-0.0339738896643499,
0.0771942215590936));
#103616=CARTESIAN_POINT('Ctrl Pts',(0.00320424385599798,-0.0338644633294062,
0.0771264779139987));
#103617=CARTESIAN_POINT('Origin',(0.0169915744700192,-0.0345610621860186,
0.0676625280065053));
#103618=CARTESIAN_POINT('Ctrl Pts',(0.00334954993768123,-0.0342436276873899,
0.0773569972515174));
#103619=CARTESIAN_POINT('Ctrl Pts',(0.00322859604239246,-0.0339430054201859,
0.0771769341136292));
#103620=CARTESIAN_POINT('Ctrl Pts',(0.00312154885777119,-0.0336441434784162,
0.0769882717732526));
#103621=CARTESIAN_POINT('Ctrl Pts',(0.00349342911181937,-0.0342436276873899,
0.0775614447588372));
#103622=CARTESIAN_POINT('Ctrl Pts',(0.00336476435167696,-0.0339430054201859,
0.0773868081134584));
#103623=CARTESIAN_POINT('Ctrl Pts',(0.00324961946231059,-0.0336441434784162,
0.0772029760355599));
#103624=CARTESIAN_POINT('Ctrl Pts',(0.00320425831953572,-0.0335235895815127,
0.0771265015748059));
#103625=CARTESIAN_POINT('Ctrl Pts',(0.00316328091516676,-0.0334144449262719,
0.0770587746430359));
#103626=CARTESIAN_POINT('Ctrl Pts',(0.00312365562016488,-0.0333049234473133,
0.0769901233388914));
#103627=CARTESIAN_POINT('Ctrl Pts',(0.00308544105496591,-0.0331951640388588,
0.0769206308565334));
#103628=CARTESIAN_POINT('Ctrl Pts',(0.00317482258427507,-0.0335235895815127,
0.0772359305927856));
#103629=CARTESIAN_POINT('Ctrl Pts',(0.00313233867402772,-0.0334144449262719,
0.0771677984201661));
#103630=CARTESIAN_POINT('Ctrl Pts',(0.0030912135143257,-0.0333049234473133,
0.0770987102863218));
#103631=CARTESIAN_POINT('Ctrl Pts',(0.00305150769406908,-0.0331951640388588,
0.0770287497702561));
#103632=CARTESIAN_POINT('Ctrl Pts',(0.00314538684901441,-0.0335235895815127,
0.0773453596107654));
#103633=CARTESIAN_POINT('Ctrl Pts',(0.00310139643288869,-0.0334144449262719,
0.0772768221972964));
#103634=CARTESIAN_POINT('Ctrl Pts',(0.00305877140848652,-0.0333049234473133,
0.0772072972337522));
#103635=CARTESIAN_POINT('Ctrl Pts',(0.00301757433317225,-0.0331951640388588,
0.0771368686839789));
#103636=CARTESIAN_POINT('Ctrl Pts',(0.00311595111375375,-0.0335235895815127,
0.0774547886287451));
#103637=CARTESIAN_POINT('Ctrl Pts',(0.00307045419174965,-0.0334144449262719,
0.0773858459744266));
#103638=CARTESIAN_POINT('Ctrl Pts',(0.00302632930264734,-0.0333049234473133,
0.0773158841811827));
#103639=CARTESIAN_POINT('Ctrl Pts',(0.00298364097227541,-0.0331951640388588,
0.0772449875977016));
#103640=CARTESIAN_POINT('Origin',(0.0180414680259711,-0.0326434571770575,
0.0695648101471628));
#103641=CARTESIAN_POINT('Ctrl Pts',(0.00280934470954787,-0.0336938721132435,
0.0769383641741863));
#103642=CARTESIAN_POINT('Ctrl Pts',(0.00279302348875822,-0.0336474569764981,
0.0769072570080762));
#103643=CARTESIAN_POINT('Ctrl Pts',(0.00277706753496419,-0.033601104548885,
0.0768759609129525));
#103644=CARTESIAN_POINT('Ctrl Pts',(0.00273667073020307,-0.0334837508643192,
0.0767967263989386));
#103645=CARTESIAN_POINT('Ctrl Pts',(0.00269863954756933,-0.0333660264760466,
0.0767163296378509));
#103646=CARTESIAN_POINT('Ctrl Pts',(0.00313945275405843,-0.0336938721132435,
0.0770195966690497));
#103647=CARTESIAN_POINT('Ctrl Pts',(0.00312265605252052,-0.0336474569764981,
0.0769904217348656));
#103648=CARTESIAN_POINT('Ctrl Pts',(0.00310620203134415,-0.033601104548885,
0.0769610521731677));
#103649=CARTESIAN_POINT('Ctrl Pts',(0.00306454423453818,-0.0334837508643192,
0.0768866951986399));
#103650=CARTESIAN_POINT('Ctrl Pts',(0.00302510808199276,-0.0333660264760466,
0.0768111364693754));
#103651=CARTESIAN_POINT('Ctrl Pts',(0.00313945275406449,-0.0336938721132426,
0.0770195966690529));
#103652=CARTESIAN_POINT('Ctrl Pts',(0.00312265605252859,-0.0336474569765026,
0.0769904217348721));
#103653=CARTESIAN_POINT('Ctrl Pts',(0.00310620203135415,-0.0336011045488949,
0.0769610521731777));
#103654=CARTESIAN_POINT('Ctrl Pts',(0.00306489118725482,-0.0334847282606778,
0.0768873144909686));
#103655=CARTESIAN_POINT('Ctrl Pts',(0.00302576499310969,-0.0333679869945434,
0.0768123947168798));
#103656=CARTESIAN_POINT('Ctrl Pts',(0.00313945275405809,-0.0336938721132426,
0.077019596669049));
#103657=CARTESIAN_POINT('Ctrl Pts',(0.00307938031608184,-0.0335278710435082,
0.0769152541932195));
#103658=CARTESIAN_POINT('Ctrl Pts',(0.00302260116436309,-0.033362046922432,
0.0768090645687945));
#103659=CARTESIAN_POINT('Ctrl Pts',(0.00296910472395236,-0.0331951640388601,
0.0767009655405309));
#103660=CARTESIAN_POINT('Ctrl Pts',(0.00318284992329977,-0.0336938721132426,
0.0770913233413898));
#103661=CARTESIAN_POINT('Ctrl Pts',(0.00312127595163347,-0.0335278710435082,
0.0769878893464579));
#103662=CARTESIAN_POINT('Ctrl Pts',(0.00306296730473599,-0.033362046922432,
0.0768825607956229));
#103663=CARTESIAN_POINT('Ctrl Pts',(0.00300791250377322,-0.0331951640388601,
0.0767752756074711));
#103664=CARTESIAN_POINT('Ctrl Pts',(0.00322624709254146,-0.0336938721132426,
0.0771630500137307));
#103665=CARTESIAN_POINT('Ctrl Pts',(0.0031631715871851,-0.0335278710435082,
0.0770605244996964));
#103666=CARTESIAN_POINT('Ctrl Pts',(0.00310333344510889,-0.033362046922432,
0.0769560570224513));
#103667=CARTESIAN_POINT('Ctrl Pts',(0.00304672028359408,-0.0331951640388601,
0.0768495856744113));
#103668=CARTESIAN_POINT('Ctrl Pts',(0.00326964426178314,-0.0336938721132426,
0.0772347766860715));
#103669=CARTESIAN_POINT('Ctrl Pts',(0.00320506722273674,-0.0335278710435082,
0.0771331596529348));
#103670=CARTESIAN_POINT('Ctrl Pts',(0.00314369958548179,-0.033362046922432,
0.0770295532492797));
#103671=CARTESIAN_POINT('Ctrl Pts',(0.00308552806341493,-0.0331951640388601,
0.0769238957413515));
#103672=CARTESIAN_POINT('Ctrl Pts',(0.00302707006767231,-0.0330240426238155,
0.0768117299431733));
#103673=CARTESIAN_POINT('Ctrl Pts',(0.00299040214450746,-0.0329142774063509,
0.0767415177681598));
#103674=CARTESIAN_POINT('Ctrl Pts',(0.0029551674228312,-0.0328043479726686,
0.0766705125614177));
#103675=CARTESIAN_POINT('Ctrl Pts',(0.00292141354604987,-0.0326943950436594,
0.0765988040428044));
#103676=CARTESIAN_POINT('Ctrl Pts',(0.0029908213809377,-0.0330240426238155,
0.0769190945960841));
#103677=CARTESIAN_POINT('Ctrl Pts',(0.0029526744050787,-0.0329142774063509,
0.0768483830600954));
#103678=CARTESIAN_POINT('Ctrl Pts',(0.00291597021653283,-0.0328043479726686,
0.0767768476672778));
#103679=CARTESIAN_POINT('Ctrl Pts',(0.0028807583599082,-0.0326943950436594,
0.0767045787648528));
#103680=CARTESIAN_POINT('Ctrl Pts',(0.00295457269420309,-0.0330240426238155,
0.0770264592489949));
#103681=CARTESIAN_POINT('Ctrl Pts',(0.00291494666564993,-0.0329142774063509,
0.076955248352031));
#103682=CARTESIAN_POINT('Ctrl Pts',(0.00287677301023446,-0.0328043479726686,
0.0768831827731379));
#103683=CARTESIAN_POINT('Ctrl Pts',(0.00284010317376653,-0.0326943950436594,
0.0768103534869012));
#103684=CARTESIAN_POINT('Ctrl Pts',(0.00291832400746847,-0.0330240426238155,
0.0771338239019057));
#103685=CARTESIAN_POINT('Ctrl Pts',(0.00287721892622117,-0.0329142774063509,
0.0770621136439667));
#103686=CARTESIAN_POINT('Ctrl Pts',(0.00283757580393609,-0.0328043479726686,
0.076989517878998));
#103687=CARTESIAN_POINT('Ctrl Pts',(0.00279944798762485,-0.0326943950436594,
0.0769161282089497));
#103688=CARTESIAN_POINT('Origin',(0.0181525382067224,-0.0326396682858048,
0.069510415168098));
#103689=CARTESIAN_POINT('Ctrl Pts',(0.00264668323176962,-0.0331951640388587,
0.0765997728400265));
#103690=CARTESIAN_POINT('Ctrl Pts',(0.00261294256674836,-0.0330855618255041,
0.076524336881915));
#103691=CARTESIAN_POINT('Ctrl Pts',(0.00258073671086079,-0.0329757224427708,
0.0764481491812047));
#103692=CARTESIAN_POINT('Ctrl Pts',(0.00255011169130408,-0.0328657862078596,
0.0763713052778369));
#103693=CARTESIAN_POINT('Ctrl Pts',(0.00275480205941473,-0.0331951640388587,
0.0766337061739077));
#103694=CARTESIAN_POINT('Ctrl Pts',(0.00272059403136584,-0.0330855618255041,
0.0765597593339244));
#103695=CARTESIAN_POINT('Ctrl Pts',(0.00268788969800888,-0.0329757224427708,
0.0764850521652318));
#103696=CARTESIAN_POINT('Ctrl Pts',(0.002656735631873,-0.0328657862078596,
0.0764096782805498));
#103697=CARTESIAN_POINT('Ctrl Pts',(0.00286292088705985,-0.0331951640388587,
0.0766676395077888));
#103698=CARTESIAN_POINT('Ctrl Pts',(0.00282824549598332,-0.0330855618255041,
0.0765951817859338));
#103699=CARTESIAN_POINT('Ctrl Pts',(0.00279504268515697,-0.0329757224427708,
0.076521955149259));
#103700=CARTESIAN_POINT('Ctrl Pts',(0.00276335957244192,-0.0328657862078596,
0.0764480512832627));
#103701=CARTESIAN_POINT('Ctrl Pts',(0.00297103971470497,-0.0331951640388587,
0.07670157284167));
#103702=CARTESIAN_POINT('Ctrl Pts',(0.0029358969606008,-0.0330855618255041,
0.0766306042379432));
#103703=CARTESIAN_POINT('Ctrl Pts',(0.00290219567230506,-0.0329757224427708,
0.0765588581332861));
#103704=CARTESIAN_POINT('Ctrl Pts',(0.00286998351301083,-0.0328657862078596,
0.0764864242859755));
#103705=CARTESIAN_POINT('Origin',(0.0183188219012972,-0.0326401908832583,
0.0699616607828441));
#103706=CARTESIAN_POINT('Ctrl Pts',(0.00298522029885135,-0.0332451089994432,
0.076733274406425));
#103707=CARTESIAN_POINT('Ctrl Pts',(0.00288779051057838,-0.0329451141710257,
0.0765394703737833));
#103708=CARTESIAN_POINT('Ctrl Pts',(0.00280523562206676,-0.0326442513127503,
0.0763388781079957));
#103709=CARTESIAN_POINT('Ctrl Pts',(0.00310233809251201,-0.0332451089994432,
0.0769541441019654));
#103710=CARTESIAN_POINT('Ctrl Pts',(0.00299657806738194,-0.0329451141710257,
0.0767647572391802));
#103711=CARTESIAN_POINT('Ctrl Pts',(0.00290538388804582,-0.0326442513127503,
0.0765679421270413));
#103712=CARTESIAN_POINT('Ctrl Pts',(0.00286999626642163,-0.0325229783203385,
0.0764864531846078));
#103713=CARTESIAN_POINT('Ctrl Pts',(0.00283778831095292,-0.032413025311208,
0.0764140298618194));
#103714=CARTESIAN_POINT('Ctrl Pts',(0.00280708340989057,-0.0323031222247695,
0.076340951260526));
#103715=CARTESIAN_POINT('Ctrl Pts',(0.00277791759089321,-0.0321934096636184,
0.0762673123770711));
#103716=CARTESIAN_POINT('Ctrl Pts',(0.00282707763151222,-0.0325229783203385,
0.0765913299381186));
#103717=CARTESIAN_POINT('Ctrl Pts',(0.00279342395231619,-0.032413025311208,
0.0765183149828973));
#103718=CARTESIAN_POINT('Ctrl Pts',(0.0027612857854755,-0.0323031222247695,
0.0764446149322517));
#103719=CARTESIAN_POINT('Ctrl Pts',(0.00273070096647091,-0.0321934096636184,
0.0763703256433411));
#103720=CARTESIAN_POINT('Ctrl Pts',(0.00278415899660282,-0.0325229783203385,
0.0766962066916294));
#103721=CARTESIAN_POINT('Ctrl Pts',(0.00274905959367946,-0.032413025311208,
0.0766226001039753));
#103722=CARTESIAN_POINT('Ctrl Pts',(0.00271548816106042,-0.0323031222247695,
0.0765482786039775));
#103723=CARTESIAN_POINT('Ctrl Pts',(0.00268348434204861,-0.0321934096636184,
0.0764733389096111));
#103724=CARTESIAN_POINT('Ctrl Pts',(0.00274124036169342,-0.0325229783203385,
0.0768010834451402));
#103725=CARTESIAN_POINT('Ctrl Pts',(0.00270469523504273,-0.032413025311208,
0.0767268852250532));
#103726=CARTESIAN_POINT('Ctrl Pts',(0.00266969053664535,-0.0323031222247695,
0.0766519422757033));
#103727=CARTESIAN_POINT('Ctrl Pts',(0.00263626771762631,-0.0321934096636184,
0.0765763521758811));
#103728=CARTESIAN_POINT('Origin',(0.0181447031648636,-0.0326393375174202,
0.069513777181946));
#103729=CARTESIAN_POINT('Ctrl Pts',(0.00250366852609156,-0.0326943950436593,
0.0762510288836282));
#103730=CARTESIAN_POINT('Ctrl Pts',(0.00247471241032746,-0.0325844576448126,
0.0761735731840813));
#103731=CARTESIAN_POINT('Ctrl Pts',(0.00244735615615104,-0.0324744968375319,
0.0760955131429261));
#103732=CARTESIAN_POINT('Ctrl Pts',(0.00242163343448193,-0.0323646534831895,
0.0760169492586902));
#103733=CARTESIAN_POINT('Ctrl Pts',(0.00260944321353152,-0.0326943950436593,
0.0762916840564678));
#103734=CARTESIAN_POINT('Ctrl Pts',(0.00257992679328977,-0.0325844576448126,
0.0762156861303568));
#103735=CARTESIAN_POINT('Ctrl Pts',(0.00255198004583739,-0.0324744968375319,
0.076139072377791));
#103736=CARTESIAN_POINT('Ctrl Pts',(0.00252563742422781,-0.0323646534831895,
0.0760619414546645));
#103737=CARTESIAN_POINT('Ctrl Pts',(0.00271521790097148,-0.0326943950436593,
0.0763323392293075));
#103738=CARTESIAN_POINT('Ctrl Pts',(0.00268514117625209,-0.0325844576448126,
0.0762577990766323));
#103739=CARTESIAN_POINT('Ctrl Pts',(0.00265660393552373,-0.0324744968375319,
0.076182631612656));
#103740=CARTESIAN_POINT('Ctrl Pts',(0.00262964141397369,-0.0323646534831895,
0.0761069336506387));
#103741=CARTESIAN_POINT('Ctrl Pts',(0.00282099258841144,-0.0326943950436593,
0.0763729944021472));
#103742=CARTESIAN_POINT('Ctrl Pts',(0.0027903555592144,-0.0325844576448126,
0.0762999120229078));
#103743=CARTESIAN_POINT('Ctrl Pts',(0.00276122782521008,-0.0324744968375319,
0.0762261908475209));
#103744=CARTESIAN_POINT('Ctrl Pts',(0.00273364540371956,-0.0323646534831895,
0.0761519258466129));
#103745=CARTESIAN_POINT('Origin',(0.0183536479408555,-0.0326395579067962,
0.0699468584591393));
#103746=CARTESIAN_POINT('Ctrl Pts',(0.0028331703173209,-0.0327445246961875,
0.0764055600146698));
#103747=CARTESIAN_POINT('Ctrl Pts',(0.00274810048155036,-0.0324436878365473,
0.0762060213278374));
#103748=CARTESIAN_POINT('Ctrl Pts',(0.00267830238945435,-0.0321434074463185,
0.07600064170168));
#103749=CARTESIAN_POINT('Ctrl Pts',(0.0029361900363106,-0.0327445246961875,
0.0766333470588565));
#103750=CARTESIAN_POINT('Ctrl Pts',(0.00284252907181213,-0.0324436878365473,
0.0764376938242037));
#103751=CARTESIAN_POINT('Ctrl Pts',(0.00276387158934186,-0.0321434074463185,
0.0762355414931456));
#103752=CARTESIAN_POINT('Ctrl Pts',(0.00270011886100842,-0.0322357242816071,
0.0760636355609245));
#103753=CARTESIAN_POINT('Ctrl Pts',(0.00263917205028739,-0.0319819883628705,
0.0758908989180309));
#103754=CARTESIAN_POINT('Ctrl Pts',(0.00258934048258397,-0.0317295851069886,
0.0757146341274587));
#103755=CARTESIAN_POINT('Ctrl Pts',(0.00278840501985078,-0.0322357242816071,
0.0762975277458236));
#103756=CARTESIAN_POINT('Ctrl Pts',(0.00272000904638777,-0.0319819883628705,
0.0761276029025862));
#103757=CARTESIAN_POINT('Ctrl Pts',(0.00266256448973903,-0.0317295851069886,
0.0759536702016737));
#103758=CARTESIAN_POINT('Origin',(0.0182648632769585,-0.0326371942646736,
0.0699814949570038));
#103759=CARTESIAN_POINT('Origin',(0.0180321202916383,-0.0326352985529878,
0.0695626535532545));
#103760=CARTESIAN_POINT('Ctrl Pts',(0.00238283384147098,-0.0321934096636183,
0.0758939931260947));
#103761=CARTESIAN_POINT('Ctrl Pts',(0.00235878281707659,-0.0320835708272304,
0.0758148209741027));
#103762=CARTESIAN_POINT('Ctrl Pts',(0.00233638420682424,-0.0319739230346346,
0.0757351970104766));
#103763=CARTESIAN_POINT('Ctrl Pts',(0.00231565884968773,-0.0318646057455575,
0.0756552253079342));
#103764=CARTESIAN_POINT('Ctrl Pts',(0.002485847196447,-0.0321934096636183,
0.0759412097911758));
#103765=CARTESIAN_POINT('Ctrl Pts',(0.00246114501744271,-0.0320835708272304,
0.0758634582736327));
#103766=CARTESIAN_POINT('Ctrl Pts',(0.00243806623032052,-0.0319739230346346,
0.0757852406448189));
#103767=CARTESIAN_POINT('Ctrl Pts',(0.00241663268238519,-0.0318646057455575,
0.0757066592449329));
#103768=CARTESIAN_POINT('Ctrl Pts',(0.00258886055142302,-0.0321934096636183,
0.075988426456257));
#103769=CARTESIAN_POINT('Ctrl Pts',(0.00256350721780883,-0.0320835708272304,
0.0759120955731626));
#103770=CARTESIAN_POINT('Ctrl Pts',(0.0025397482538168,-0.0319739230346346,
0.0758352842791612));
#103771=CARTESIAN_POINT('Ctrl Pts',(0.00251760651508264,-0.0318646057455575,
0.0757580931819316));
#103772=CARTESIAN_POINT('Ctrl Pts',(0.00269187390639904,-0.0321934096636183,
0.0760356431213381));
#103773=CARTESIAN_POINT('Ctrl Pts',(0.00266586941817495,-0.0320835708272304,
0.0759607328726926));
#103774=CARTESIAN_POINT('Ctrl Pts',(0.00264143027731307,-0.0319739230346346,
0.0758853279135035));
#103775=CARTESIAN_POINT('Ctrl Pts',(0.00261858034778009,-0.0318646057455575,
0.0758095271189303));
#103776=CARTESIAN_POINT('Ctrl Pts',(0.00273303330430885,-0.0320218834582397,
0.07615265429325));
#103777=CARTESIAN_POINT('Ctrl Pts',(0.00271219051450128,-0.0319391099350671,
0.0760965496293679));
#103778=CARTESIAN_POINT('Ctrl Pts',(0.00269223643500384,-0.0318564869454931,
0.076040153494791));
#103779=CARTESIAN_POINT('Ctrl Pts',(0.00267318176488415,-0.0317740741446503,
0.0759835083234629));
#103780=CARTESIAN_POINT('Ctrl Pts',(0.00271141426007721,-0.0320218834582397,
0.0761972574879136));
#103781=CARTESIAN_POINT('Ctrl Pts',(0.00269010725884071,-0.0319391099350671,
0.0761409278220448));
#103782=CARTESIAN_POINT('Ctrl Pts',(0.00266969276260582,-0.0318564869454931,
0.0760842995730776));
#103783=CARTESIAN_POINT('Ctrl Pts',(0.00265018179000934,-0.0317740741446503,
0.0760274153753276));
#103784=CARTESIAN_POINT('Ctrl Pts',(0.00268979521584557,-0.0320218834582397,
0.0762418606825772));
#103785=CARTESIAN_POINT('Ctrl Pts',(0.00266802400318014,-0.0319391099350671,
0.0761853060147217));
#103786=CARTESIAN_POINT('Ctrl Pts',(0.00264714909020781,-0.0318564869454931,
0.0761284456513641));
#103787=CARTESIAN_POINT('Ctrl Pts',(0.00262718181513453,-0.0317740741446503,
0.0760713224271923));
#103788=CARTESIAN_POINT('Ctrl Pts',(0.00266817617161393,-0.0320218834582397,
0.0762864638772409));
#103789=CARTESIAN_POINT('Ctrl Pts',(0.00264594074751957,-0.0319391099350671,
0.0762296842073986));
#103790=CARTESIAN_POINT('Ctrl Pts',(0.00262460541780979,-0.0318564869454931,
0.0761725917296507));
#103791=CARTESIAN_POINT('Ctrl Pts',(0.00260418184025973,-0.0317740741446503,
0.076115229479057));
#103792=CARTESIAN_POINT('Origin',(-0.00283580689655155,-0.0391228853390708,
0.0792262215589275));
#103793=CARTESIAN_POINT('Ctrl Pts',(0.00450259823174105,-0.0352722978779665,
0.0786189138792926));
#103794=CARTESIAN_POINT('Ctrl Pts',(0.00448813927931483,-0.0352466642097264,
0.0786067470648846));
#103795=CARTESIAN_POINT('Ctrl Pts',(0.00447364272947313,-0.0352210183808325,
0.0785946510781973));
#103796=CARTESIAN_POINT('Ctrl Pts',(0.00445910772947859,-0.0351953608940152,
0.0785826259012546));
#103797=CARTESIAN_POINT('Origin',(0.00121128566165112,-0.0352456003065142,
0.082248928309305));
#103798=CARTESIAN_POINT('Ctrl Pts',(0.00436482713708829,-0.035024121149334,
0.0785010386147655));
#103799=CARTESIAN_POINT('Ctrl Pts',(0.00430489336686762,-0.0349144232867421,
0.0784492605524351));
#103800=CARTESIAN_POINT('Ctrl Pts',(0.0042459940128969,-0.0348045283677512,
0.0783962126246391));
#103801=CARTESIAN_POINT('Ctrl Pts',(0.00418820704624738,-0.0346945769586886,
0.0783419599716325));
#103802=CARTESIAN_POINT('Ctrl Pts',(0.00437064752387573,-0.035024121149334,
0.0786142078018301));
#103803=CARTESIAN_POINT('Ctrl Pts',(0.00430915489457471,-0.0349144232867421,
0.0785625099129376));
#103804=CARTESIAN_POINT('Ctrl Pts',(0.0042486940912292,-0.0348045283677512,
0.0785095099838376));
#103805=CARTESIAN_POINT('Ctrl Pts',(0.0041893450826407,-0.0346945769586886,
0.0784552730188794));
#103806=CARTESIAN_POINT('Ctrl Pts',(0.00437646791066317,-0.035024121149334,
0.0787273769888946));
#103807=CARTESIAN_POINT('Ctrl Pts',(0.00431341642228179,-0.0349144232867421,
0.0786757592734401));
#103808=CARTESIAN_POINT('Ctrl Pts',(0.0042513941695615,-0.0348045283677512,
0.078622807343036));
#103809=CARTESIAN_POINT('Ctrl Pts',(0.00419048311903402,-0.0346945769586886,
0.0785685860661263));
#103810=CARTESIAN_POINT('Ctrl Pts',(0.00438228829745061,-0.035024121149334,
0.0788405461759592));
#103811=CARTESIAN_POINT('Ctrl Pts',(0.00431767794998888,-0.0349144232867421,
0.0787890086339426));
#103812=CARTESIAN_POINT('Ctrl Pts',(0.00425409424789381,-0.0348045283677512,
0.0787361047022345));
#103813=CARTESIAN_POINT('Ctrl Pts',(0.00419162115542735,-0.0346945769586886,
0.0786818991133732));
#103814=CARTESIAN_POINT('Origin',(0.0158100846488341,-0.0345629067942937,
0.0662260650370403));
#103815=CARTESIAN_POINT('Ctrl Pts',(0.00402666190419685,-0.0351970973651602,
0.0784382545534798));
#103816=CARTESIAN_POINT('Ctrl Pts',(0.00396725394897228,-0.0350869349321763,
0.078381494504458));
#103817=CARTESIAN_POINT('Ctrl Pts',(0.00390897679085345,-0.0349764985129717,
0.0783234523776052));
#103818=CARTESIAN_POINT('Ctrl Pts',(0.0038519103560444,-0.034865930684964,
0.078264198923843));
#103819=CARTESIAN_POINT('Ctrl Pts',(0.00410866427386499,-0.0351970973651602,
0.0784322477224199));
#103820=CARTESIAN_POINT('Ctrl Pts',(0.00404933953514405,-0.0350869349321763,
0.078376623705097));
#103821=CARTESIAN_POINT('Ctrl Pts',(0.00399112204499497,-0.0349764985129717,
0.0783197202810434));
#103822=CARTESIAN_POINT('Ctrl Pts',(0.00393409156547994,-0.034865930684964,
0.0782616067305085));
#103823=CARTESIAN_POINT('Ctrl Pts',(0.00419066664353313,-0.0351970973651602,
0.07842624089136));
#103824=CARTESIAN_POINT('Ctrl Pts',(0.00413142512131583,-0.0350869349321763,
0.078371752905736));
#103825=CARTESIAN_POINT('Ctrl Pts',(0.0040732672991365,-0.0349764985129717,
0.0783159881844817));
#103826=CARTESIAN_POINT('Ctrl Pts',(0.00401627277491548,-0.034865930684964,
0.078259014537174));
#103827=CARTESIAN_POINT('Ctrl Pts',(0.00427266901320127,-0.0351970973651602,
0.0784202340603001));
#103828=CARTESIAN_POINT('Ctrl Pts',(0.0042135107074876,-0.0350869349321763,
0.0783668821063749));
#103829=CARTESIAN_POINT('Ctrl Pts',(0.00415541255327803,-0.0349764985129717,
0.07831225608792));
#103830=CARTESIAN_POINT('Ctrl Pts',(0.00409845398435102,-0.034865930684964,
0.0782564223438395));
#103831=CARTESIAN_POINT('Origin',(0.0161221098346002,-0.0345637187964946,
0.0665920782062245));
#103832=CARTESIAN_POINT('Ctrl Pts',(0.00429703040451049,-0.0352450361861253,
0.0784434945846552));
#103833=CARTESIAN_POINT('Ctrl Pts',(0.00413509860323931,-0.0349452761023764,
0.0782991662763443));
#103834=CARTESIAN_POINT('Ctrl Pts',(0.00398449823159228,-0.0346444289983474,
0.0781430506240137));
#103835=CARTESIAN_POINT('Ctrl Pts',(0.00448723116283145,-0.0352450361861253,
0.078605740298109));
#103836=CARTESIAN_POINT('Ctrl Pts',(0.00431918016422343,-0.0349452761023764,
0.0784685855289259));
#103837=CARTESIAN_POINT('Ctrl Pts',(0.00416193763892921,-0.0346444289983474,
0.0783191621134853));
#103838=CARTESIAN_POINT('Ctrl Pts',(0.00409904125783595,-0.0345231616327822,
0.0782564268125681));
#103839=CARTESIAN_POINT('Ctrl Pts',(0.00404243994561156,-0.0344132092796975,
0.0782009514251577));
#103840=CARTESIAN_POINT('Ctrl Pts',(0.0039869890183849,-0.0343032738558974,
0.0781443081465254));
#103841=CARTESIAN_POINT('Ctrl Pts',(0.00393275765638187,-0.034193496108874,
0.0780865713629492));
#103842=CARTESIAN_POINT('Ctrl Pts',(0.00409774422579989,-0.0345231616327822,
0.0783697381264187));
#103843=CARTESIAN_POINT('Ctrl Pts',(0.00403958107664365,-0.0344132092796975,
0.0783142448612478));
#103844=CARTESIAN_POINT('Ctrl Pts',(0.00398256876285612,-0.0343032738558974,
0.0782575514004124));
#103845=CARTESIAN_POINT('Ctrl Pts',(0.00392677846333303,-0.034193496108874,
0.0781997322457186));
#103846=CARTESIAN_POINT('Ctrl Pts',(0.00409644719376382,-0.0345231616327822,
0.0784830494402693));
#103847=CARTESIAN_POINT('Ctrl Pts',(0.00403672220767573,-0.0344132092796975,
0.0784275382973378));
#103848=CARTESIAN_POINT('Ctrl Pts',(0.00397814850732733,-0.0343032738558974,
0.0783707946542993));
#103849=CARTESIAN_POINT('Ctrl Pts',(0.0039207992702842,-0.034193496108874,
0.0783128931284879));
#103850=CARTESIAN_POINT('Ctrl Pts',(0.00409515016172776,-0.0345231616327822,
0.0785963607541199));
#103851=CARTESIAN_POINT('Ctrl Pts',(0.00403386333870782,-0.0344132092796975,
0.0785408317334278));
#103852=CARTESIAN_POINT('Ctrl Pts',(0.00397372825179854,-0.0343032738558974,
0.0784840379081863));
#103853=CARTESIAN_POINT('Ctrl Pts',(0.00391482007723537,-0.034193496108874,
0.0784260540112573));
#103854=CARTESIAN_POINT('Origin',(0.0158183303387263,-0.0345625596230808,
0.0662172046252609));
#103855=CARTESIAN_POINT('Ctrl Pts',(0.00367177297545972,-0.0346945769586886,
0.0781723890818771));
#103856=CARTESIAN_POINT('Ctrl Pts',(0.0036163424208028,-0.0345846629176053,
0.0781110381445986));
#103857=CARTESIAN_POINT('Ctrl Pts',(0.00356217111065839,-0.0344746925050312,
0.0780485304473229));
#103858=CARTESIAN_POINT('Ctrl Pts',(0.00350932812478276,-0.034364806625326,
0.0779849463687704));
#103859=CARTESIAN_POINT('Ctrl Pts',(0.0037850859334871,-0.0346945769586886,
0.0781712510463798));
#103860=CARTESIAN_POINT('Ctrl Pts',(0.00372967106153454,-0.0345846629176053,
0.0781114616189367));
#103861=CARTESIAN_POINT('Ctrl Pts',(0.00367548314539103,-0.0344746925050311,
0.0780505160225181));
#103862=CARTESIAN_POINT('Ctrl Pts',(0.00362259129435643,-0.034364806625326,
0.0779884926343885));
#103863=CARTESIAN_POINT('Ctrl Pts',(0.00389839889151448,-0.0346945769586885,
0.0781701130108826));
#103864=CARTESIAN_POINT('Ctrl Pts',(0.00384299970226629,-0.0345846629176052,
0.0781118850932749));
#103865=CARTESIAN_POINT('Ctrl Pts',(0.00378879518012367,-0.0344746925050311,
0.0780525015977133));
#103866=CARTESIAN_POINT('Ctrl Pts',(0.0037358544639301,-0.034364806625326,
0.0779920389000066));
#103867=CARTESIAN_POINT('Ctrl Pts',(0.00401171184954186,-0.0346945769586885,
0.0781689749753853));
#103868=CARTESIAN_POINT('Ctrl Pts',(0.00395632834299804,-0.0345846629176052,
0.078112308567613));
#103869=CARTESIAN_POINT('Ctrl Pts',(0.00390210721485631,-0.0344746925050311,
0.0780544871729085));
#103870=CARTESIAN_POINT('Ctrl Pts',(0.00384911763350376,-0.034364806625326,
0.0779955851656247));
#103871=CARTESIAN_POINT('Origin',(0.0161640406813811,-0.0345626446730904,
0.0665513850283427));
#103872=CARTESIAN_POINT('Ctrl Pts',(0.00400968430075594,-0.0346945769586885,
0.0781689953386564));
#103873=CARTESIAN_POINT('Ctrl Pts',(0.00392550483427121,-0.034527515336289,
0.0780828239111076));
#103874=CARTESIAN_POINT('Ctrl Pts',(0.00384401360674573,-0.0343603235965158,
0.0779939828284748));
#103875=CARTESIAN_POINT('Ctrl Pts',(0.00376544772787016,-0.034193496108874,
0.0779027384253525));
#103876=CARTESIAN_POINT('Ctrl Pts',(0.00406955575982,-0.0346945769586885,
0.0782276761423388));
#103877=CARTESIAN_POINT('Ctrl Pts',(0.00398414720040764,-0.034527515336289,
0.0781427587464713));
#103878=CARTESIAN_POINT('Ctrl Pts',(0.00390138712390605,-0.0343603235965158,
0.0780551333660354));
#103879=CARTESIAN_POINT('Ctrl Pts',(0.00382151644613647,-0.034193496108874,
0.0779650627958928));
#103880=CARTESIAN_POINT('Ctrl Pts',(0.00412942721888406,-0.0346945769586885,
0.0782863569460212));
#103881=CARTESIAN_POINT('Ctrl Pts',(0.00404278956654408,-0.034527515336289,
0.078202693581835));
#103882=CARTESIAN_POINT('Ctrl Pts',(0.00395876064106636,-0.0343603235965158,
0.0781162839035959));
#103883=CARTESIAN_POINT('Ctrl Pts',(0.00387758516440278,-0.034193496108874,
0.0780273871664331));
#103884=CARTESIAN_POINT('Ctrl Pts',(0.00418929867794812,-0.0346945769586885,
0.0783450377497036));
#103885=CARTESIAN_POINT('Ctrl Pts',(0.00410143193268052,-0.034527515336289,
0.0782626284171987));
#103886=CARTESIAN_POINT('Ctrl Pts',(0.00401613415822667,-0.0343603235965158,
0.0781774344411565));
#103887=CARTESIAN_POINT('Ctrl Pts',(0.0039336538826691,-0.034193496108874,
0.0780897115369734));
#103888=CARTESIAN_POINT('Ctrl Pts',(0.00384913915134722,-0.0340223579322365,
0.0779956082517206));
#103889=CARTESIAN_POINT('Ctrl Pts',(0.00379609818378914,-0.0339125849573554,
0.0779366497754382));
#103890=CARTESIAN_POINT('Ctrl Pts',(0.00374431479096331,-0.0338030433565221,
0.0778766349038162));
#103891=CARTESIAN_POINT('Ctrl Pts',(0.0036938483916329,-0.0336938721132328,
0.0778156462560814));
#103892=CARTESIAN_POINT('Ctrl Pts',(0.00384072980625804,-0.0340223579322365,
0.0781086147238609));
#103893=CARTESIAN_POINT('Ctrl Pts',(0.00378613018471591,-0.0339125849573554,
0.0780495402607772));
#103894=CARTESIAN_POINT('Ctrl Pts',(0.0037327916338114,-0.0338030433565221,
0.0779893772233409));
#103895=CARTESIAN_POINT('Ctrl Pts',(0.00368077554429622,-0.0336938721132328,
0.0779282085965552));
#103896=CARTESIAN_POINT('Ctrl Pts',(0.00383232046116886,-0.0340223579322365,
0.0782216211960012));
#103897=CARTESIAN_POINT('Ctrl Pts',(0.00377616218564268,-0.0339125849573554,
0.0781624307461163));
#103898=CARTESIAN_POINT('Ctrl Pts',(0.0037212684766595,-0.0338030433565221,
0.0781021195428656));
#103899=CARTESIAN_POINT('Ctrl Pts',(0.00366770269695954,-0.0336938721132328,
0.078040770937029));
#103900=CARTESIAN_POINT('Ctrl Pts',(0.00382391111607968,-0.0340223579322365,
0.0783346276681416));
#103901=CARTESIAN_POINT('Ctrl Pts',(0.00376619418656945,-0.0339125849573554,
0.0782753212314553));
#103902=CARTESIAN_POINT('Ctrl Pts',(0.0037097453195076,-0.0338030433565221,
0.0782148618623903));
#103903=CARTESIAN_POINT('Ctrl Pts',(0.00365462984962285,-0.0336938721132328,
0.0781533332775029));
#103904=CARTESIAN_POINT('Origin',(0.0157327859634578,-0.0345589643414735,
0.0663016737791342));
#103905=CARTESIAN_POINT('Ctrl Pts',(0.00342799009848604,-0.034193496108874,
0.0778849078441259));
#103906=CARTESIAN_POINT('Ctrl Pts',(0.00337648793104013,-0.0340836138581107,
0.0778201556518787));
#103907=CARTESIAN_POINT('Ctrl Pts',(0.00332635038605239,-0.0339738896643499,
0.0777543687996616));
#103908=CARTESIAN_POINT('Ctrl Pts',(0.0032776359891141,-0.0338644633294062,
0.077687635788142));
#103909=CARTESIAN_POINT('Ctrl Pts',(0.00354115108307491,-0.034193496108874,
0.0778908870425547));
#103910=CARTESIAN_POINT('Ctrl Pts',(0.00348956646602342,-0.0340836138581107,
0.0778276952732737));
#103911=CARTESIAN_POINT('Ctrl Pts',(0.00343931422131188,-0.0339738896643499,
0.077763466389181));
#103912=CARTESIAN_POINT('Ctrl Pts',(0.00339045315500113,-0.0338644633294062,
0.0776982869067778));
#103913=CARTESIAN_POINT('Ctrl Pts',(0.00365431206766379,-0.034193496108874,
0.0778968662409835));
#103914=CARTESIAN_POINT('Ctrl Pts',(0.0036026450010067,-0.0340836138581107,
0.0778352348946687));
#103915=CARTESIAN_POINT('Ctrl Pts',(0.00355227805657137,-0.0339738896643499,
0.0777725639787003));
#103916=CARTESIAN_POINT('Ctrl Pts',(0.00350327032088815,-0.0338644633294062,
0.0777089380254137));
#103917=CARTESIAN_POINT('Ctrl Pts',(0.00376747305225267,-0.034193496108874,
0.0779028454394122));
#103918=CARTESIAN_POINT('Ctrl Pts',(0.00371572353598999,-0.0340836138581107,
0.0778427745160637));
#103919=CARTESIAN_POINT('Ctrl Pts',(0.00366524189183086,-0.0339738896643499,
0.0777816615682196));
#103920=CARTESIAN_POINT('Ctrl Pts',(0.00361608748677517,-0.0338644633294062,
0.0777195891440495));
#103921=CARTESIAN_POINT('Origin',(0.0161085534363768,-0.0345610621861926,
0.0666022545801441));
#103922=CARTESIAN_POINT('Ctrl Pts',(0.00378913952057393,-0.03424362768739,
0.0779300790866652));
#103923=CARTESIAN_POINT('Ctrl Pts',(0.00364657148755933,-0.0339430054201859,
0.0777665953432102));
#103924=CARTESIAN_POINT('Ctrl Pts',(0.00351672274079097,-0.033644143478416,
0.0775928372315306));
#103925=CARTESIAN_POINT('Ctrl Pts',(0.00395750823163594,-0.03424362768739,
0.0781148816221871));
#103926=CARTESIAN_POINT('Ctrl Pts',(0.0038079702560933,-0.0339430054201859,
0.0779577480093528));
#103927=CARTESIAN_POINT('Ctrl Pts',(0.00367069304981574,-0.033644143478416,
0.0777897969836091));
#103928=CARTESIAN_POINT('Ctrl Pts',(0.00361610480174909,-0.0335235895815128,
0.0777196108055224));
#103929=CARTESIAN_POINT('Ctrl Pts',(0.00356696208109481,-0.0334144449262719,
0.077657553751431));
#103930=CARTESIAN_POINT('Ctrl Pts',(0.00351904495344267,-0.0333049234473133,
0.0775944101496783));
#103931=CARTESIAN_POINT('Ctrl Pts',(0.0034724220039821,-0.0331951640388588,
0.0775302551913258));
#103932=CARTESIAN_POINT('Ctrl Pts',(0.00360061626872215,-0.0335235895815128,
0.0778318662188931));
#103933=CARTESIAN_POINT('Ctrl Pts',(0.00354992813129227,-0.0334144449262719,
0.0777695959346505));
#103934=CARTESIAN_POINT('Ctrl Pts',(0.00350046821654235,-0.0333049234473133,
0.0777062069306234));
#103935=CARTESIAN_POINT('Ctrl Pts',(0.00345230711083766,-0.0331951640388588,
0.0776417745329672));
#103936=CARTESIAN_POINT('Ctrl Pts',(0.00358512773569521,-0.0335235895815128,
0.0779441216322637));
#103937=CARTESIAN_POINT('Ctrl Pts',(0.00353289418148973,-0.0334144449262719,
0.07788163811787));
#103938=CARTESIAN_POINT('Ctrl Pts',(0.00348189147964202,-0.0333049234473133,
0.0778180037115685));
#103939=CARTESIAN_POINT('Ctrl Pts',(0.00343219221769322,-0.0331951640388588,
0.0777532938746086));
#103940=CARTESIAN_POINT('Ctrl Pts',(0.00356963920266827,-0.0335235895815128,
0.0780563770456345));
#103941=CARTESIAN_POINT('Ctrl Pts',(0.00351586023168719,-0.0334144449262719,
0.0779936803010894));
#103942=CARTESIAN_POINT('Ctrl Pts',(0.00346331474274169,-0.0333049234473133,
0.0779298004925136));
#103943=CARTESIAN_POINT('Ctrl Pts',(0.00341207732454878,-0.0331951640388588,
0.07786481321625));
#103944=CARTESIAN_POINT('Origin',(0.0173885874402498,-0.0326434571769693,
0.0683579501038521));
#103945=CARTESIAN_POINT('Ctrl Pts',(0.00320072533475701,-0.0336938721132442,
0.0775824527242192));
#103946=CARTESIAN_POINT('Ctrl Pts',(0.00318063404995246,-0.0336474569764984,
0.0775536364387821));
#103947=CARTESIAN_POINT('Ctrl Pts',(0.00316088147281998,-0.033601104548885,
0.0775245869339996));
#103948=CARTESIAN_POINT('Ctrl Pts',(0.00311087249107923,-0.0334837508643194,
0.0774510402699615));
#103949=CARTESIAN_POINT('Ctrl Pts',(0.00306306480964481,-0.0333660264760472,
0.0773760440324443));
#103950=CARTESIAN_POINT('Ctrl Pts',(0.00353841150999001,-0.0336938721132442,
0.0776216711679534));
#103951=CARTESIAN_POINT('Ctrl Pts',(0.00351809066662021,-0.0336474569764984,
0.0775948314717563));
#103952=CARTESIAN_POINT('Ctrl Pts',(0.0034980854081793,-0.033601104548885,
0.0775677557335037));
#103953=CARTESIAN_POINT('Ctrl Pts',(0.00344743669548824,-0.0334837508643194,
0.0774992061923065));
#103954=CARTESIAN_POINT('Ctrl Pts',(0.00339884148892204,-0.0333660264760472,
0.0774291859267086));
#103955=CARTESIAN_POINT('Ctrl Pts',(0.003538411509995,-0.0336938721132427,
0.0776216711679568));
#103956=CARTESIAN_POINT('Ctrl Pts',(0.00351809066662774,-0.0336474569765026,
0.0775948314717629));
#103957=CARTESIAN_POINT('Ctrl Pts',(0.0034980854081893,-0.0336011045488949,
0.0775677557335137));
#103958=CARTESIAN_POINT('Ctrl Pts',(0.00344785853028782,-0.0334847282606778,
0.0774997771166254));
#103959=CARTESIAN_POINT('Ctrl Pts',(0.0033996509203255,-0.0333679869945434,
0.0774303519197621));
#103960=CARTESIAN_POINT('Ctrl Pts',(0.00353841150998937,-0.0336938721132427,
0.0776216711679526));
#103961=CARTESIAN_POINT('Ctrl Pts',(0.00346573518123552,-0.0335278710435083,
0.0775256805366102));
#103962=CARTESIAN_POINT('Ctrl Pts',(0.003396094661087,-0.033362046922432,
0.0774274445637751));
#103963=CARTESIAN_POINT('Ctrl Pts',(0.00332947165533008,-0.0331951640388601,
0.0773269028104978));
#103964=CARTESIAN_POINT('Ctrl Pts',(0.00359045621536674,-0.0336938721132427,
0.0776873931465096));
#103965=CARTESIAN_POINT('Ctrl Pts',(0.003516404055813,-0.0335278710435083,
0.0775924920244943));
#103966=CARTESIAN_POINT('Ctrl Pts',(0.00344535402214944,-0.033362046922432,
0.0774953020320032));
#103967=CARTESIAN_POINT('Ctrl Pts',(0.00337728694519171,-0.0331951640388601,
0.0773957630158324));
#103968=CARTESIAN_POINT('Ctrl Pts',(0.00364250092074412,-0.0336938721132427,
0.0777531151250667));
#103969=CARTESIAN_POINT('Ctrl Pts',(0.00356707293039049,-0.0335278710435083,
0.0776593035123785));
#103970=CARTESIAN_POINT('Ctrl Pts',(0.00349461338321189,-0.033362046922432,
0.0775631595002313));
#103971=CARTESIAN_POINT('Ctrl Pts',(0.00342510223505334,-0.0331951640388601,
0.0774646232211669));
#103972=CARTESIAN_POINT('Ctrl Pts',(0.0036945456261215,-0.0336938721132427,
0.0778188371036238));
#103973=CARTESIAN_POINT('Ctrl Pts',(0.00361774180496797,-0.0335278710435083,
0.0777261150002626));
#103974=CARTESIAN_POINT('Ctrl Pts',(0.00354387274427434,-0.033362046922432,
0.0776310169684594));
#103975=CARTESIAN_POINT('Ctrl Pts',(0.00347291752491498,-0.0331951640388601,
0.0775334834265015));
#103976=CARTESIAN_POINT('Ctrl Pts',(0.00340086238574835,-0.0330240426238156,
0.0774295288187784));
#103977=CARTESIAN_POINT('Ctrl Pts',(0.00335568368117981,-0.0329142774063509,
0.0773644659971146));
#103978=CARTESIAN_POINT('Ctrl Pts',(0.00331182748364718,-0.0328043479726686,
0.0772984367692373));
#103979=CARTESIAN_POINT('Ctrl Pts',(0.00326935230575415,-0.0326943950436594,
0.0772315241762339));
#103980=CARTESIAN_POINT('Ctrl Pts',(0.0033783558898554,-0.0330240426238156,
0.0775405900344537));
#103981=CARTESIAN_POINT('Ctrl Pts',(0.00333164720883924,-0.0329142774063509,
0.0774752171638819));
#103982=CARTESIAN_POINT('Ctrl Pts',(0.00328626668168694,-0.0328043479726686,
0.0774088461036391));
#103983=CARTESIAN_POINT('Ctrl Pts',(0.003242274785842,-0.0326943950436594,
0.0773415602789459));
#103984=CARTESIAN_POINT('Ctrl Pts',(0.00335584939396246,-0.0330240426238156,
0.077651651250129));
#103985=CARTESIAN_POINT('Ctrl Pts',(0.00330761073649868,-0.0329142774063509,
0.0775859683306493));
#103986=CARTESIAN_POINT('Ctrl Pts',(0.00326070587972671,-0.0328043479726686,
0.0775192554380409));
#103987=CARTESIAN_POINT('Ctrl Pts',(0.00321519726592985,-0.0326943950436594,
0.077451596381658));
#103988=CARTESIAN_POINT('Ctrl Pts',(0.00333334289806951,-0.0330240426238156,
0.0777627124658043));
#103989=CARTESIAN_POINT('Ctrl Pts',(0.00328357426415811,-0.0329142774063509,
0.0776967194974166));
#103990=CARTESIAN_POINT('Ctrl Pts',(0.00323514507776647,-0.0328043479726686,
0.0776296647724427));
#103991=CARTESIAN_POINT('Ctrl Pts',(0.0031881197460177,-0.0326943950436594,
0.0775616324843701));
#103992=CARTESIAN_POINT('Origin',(0.0174919643009571,-0.032639668285648,
0.0682900632605691));
#103993=CARTESIAN_POINT('Ctrl Pts',(0.00299690974454837,-0.0331951640388587,
0.0772669181728474));
#103994=CARTESIAN_POINT('Ctrl Pts',(0.00295398050219153,-0.0330855618255041,
0.077196305876447));
#103995=CARTESIAN_POINT('Ctrl Pts',(0.0029124797482092,-0.0329757224427708,
0.077124755402571));
#103996=CARTESIAN_POINT('Ctrl Pts',(0.00287246512119015,-0.0328657862078597,
0.0770523557690625));
#103997=CARTESIAN_POINT('Ctrl Pts',(0.00310842899740496,-0.0331951640388587,
0.0772870330499777));
#103998=CARTESIAN_POINT('Ctrl Pts',(0.00306522271330771,-0.0330855618255041,
0.0772179567056837));
#103999=CARTESIAN_POINT('Ctrl Pts',(0.00302341297236491,-0.0329757224427708,
0.0771479375651814));
#104000=CARTESIAN_POINT('Ctrl Pts',(0.00298305771265227,-0.0328657862078597,
0.0770770626659407));
#104001=CARTESIAN_POINT('Ctrl Pts',(0.00321994825026155,-0.0331951640388587,
0.0773071479271078));
#104002=CARTESIAN_POINT('Ctrl Pts',(0.0031764649244239,-0.0330855618255041,
0.0772396075349204));
#104003=CARTESIAN_POINT('Ctrl Pts',(0.00313434619652062,-0.0329757224427708,
0.0771711197277918));
#104004=CARTESIAN_POINT('Ctrl Pts',(0.00309365030411439,-0.0328657862078597,
0.0771017695628188));
#104005=CARTESIAN_POINT('Ctrl Pts',(0.00333146750311814,-0.0331951640388587,
0.077327262804238));
#104006=CARTESIAN_POINT('Ctrl Pts',(0.00328770713554008,-0.0330855618255041,
0.0772612583641571));
#104007=CARTESIAN_POINT('Ctrl Pts',(0.00324527942067632,-0.0329757224427708,
0.0771943018904021));
#104008=CARTESIAN_POINT('Ctrl Pts',(0.0032042428955765,-0.0328657862078597,
0.077126476459697));
#104009=CARTESIAN_POINT('Origin',(0.0177134928710351,-0.0326401908830748,
0.0687169097957367));
#104010=CARTESIAN_POINT('Ctrl Pts',(0.0033495095287428,-0.0332451089994432,
0.0773569370942212));
#104011=CARTESIAN_POINT('Ctrl Pts',(0.00322855791736245,-0.0329451141710257,
0.0771768724546732));
#104012=CARTESIAN_POINT('Ctrl Pts',(0.00312151312150551,-0.0326442513127503,
0.0769882087899389));
#104013=CARTESIAN_POINT('Ctrl Pts',(0.00349338612675748,-0.0332451089994432,
0.0775613864144542));
#104014=CARTESIAN_POINT('Ctrl Pts',(0.0033647235831071,-0.0329451141710257,
0.0773867481695808));
#104015=CARTESIAN_POINT('Ctrl Pts',(0.00324958102269472,-0.0326442513127503,
0.0772029146647653));
#104016=CARTESIAN_POINT('Ctrl Pts',(0.0032042591703819,-0.0325229783203385,
0.0771265035320287));
#104017=CARTESIAN_POINT('Ctrl Pts',(0.00316322813503157,-0.0324130253112079,
0.0770586880159776));
#104018=CARTESIAN_POINT('Ctrl Pts',(0.00312360617388073,-0.0323031222247694,
0.0769900340058193));
#104019=CARTESIAN_POINT('Ctrl Pts',(0.0030854409366981,-0.0321934096636184,
0.0769206312333599));
#104020=CARTESIAN_POINT('Ctrl Pts',(0.00317482350437116,-0.0325229783203385,
0.0772359324323063));
#104021=CARTESIAN_POINT('Ctrl Pts',(0.00313228399405101,-0.0324130253112079,
0.0771677111462504));
#104022=CARTESIAN_POINT('Ctrl Pts',(0.00309116218059378,-0.0323031222247694,
0.0770986202228882));
#104023=CARTESIAN_POINT('Ctrl Pts',(0.00305150761522392,-0.0321934096636184,
0.0770287500214736));
#104024=CARTESIAN_POINT('Ctrl Pts',(0.00314538783836041,-0.0325229783203385,
0.0773453613325839));
#104025=CARTESIAN_POINT('Ctrl Pts',(0.00310133985307044,-0.0324130253112079,
0.0772767342765231));
#104026=CARTESIAN_POINT('Ctrl Pts',(0.00305871818730682,-0.0323031222247694,
0.0772072064399572));
#104027=CARTESIAN_POINT('Ctrl Pts',(0.00301757429374974,-0.0321934096636184,
0.0771368688095874));
#104028=CARTESIAN_POINT('Ctrl Pts',(0.00311595217234966,-0.0325229783203385,
0.0774547902328616));
#104029=CARTESIAN_POINT('Ctrl Pts',(0.00307039571208988,-0.0324130253112079,
0.0773857574067959));
#104030=CARTESIAN_POINT('Ctrl Pts',(0.00302627419401987,-0.0323031222247694,
0.0773157926570261));
#104031=CARTESIAN_POINT('Ctrl Pts',(0.00298364097227555,-0.0321934096636184,
0.0772449875977012));
#104032=CARTESIAN_POINT('Origin',(0.0174846124122548,-0.0326393375177375,
0.0682943807546413));
#104033=CARTESIAN_POINT('Ctrl Pts',(0.00281131354479966,-0.0326943950436594,
0.07693884866222));
#104034=CARTESIAN_POINT('Ctrl Pts',(0.00277287798337493,-0.0325844576448127,
0.0768656328876191));
#104035=CARTESIAN_POINT('Ctrl Pts',(0.00273595392406345,-0.0324744968375319,
0.0767916170209979));
#104036=CARTESIAN_POINT('Ctrl Pts',(0.00270058736808504,-0.0323646534831895,
0.076716896548338));
#104037=CARTESIAN_POINT('Ctrl Pts',(0.00292134961150893,-0.0326943950436594,
0.0769659261732727));
#104038=CARTESIAN_POINT('Ctrl Pts',(0.00288254087123323,-0.0325844576448127,
0.0768942269019006));
#104039=CARTESIAN_POINT('Ctrl Pts',(0.00284521224288721,-0.0324744968375319,
0.076821719927883));
#104040=CARTESIAN_POINT('Ctrl Pts',(0.00280941027271392,-0.0323646534831895,
0.07674849881107));
#104041=CARTESIAN_POINT('Ctrl Pts',(0.00303138567821819,-0.0326943950436594,
0.0769930036843253));
#104042=CARTESIAN_POINT('Ctrl Pts',(0.00299220375909152,-0.0325844576448127,
0.0769228209161821));
#104043=CARTESIAN_POINT('Ctrl Pts',(0.00295447056171098,-0.0324744968375319,
0.0768518228347681));
#104044=CARTESIAN_POINT('Ctrl Pts',(0.0029182331773428,-0.0323646534831895,
0.0767801010738021));
#104045=CARTESIAN_POINT('Ctrl Pts',(0.00314142174492745,-0.0326943950436594,
0.077020081195378));
#104046=CARTESIAN_POINT('Ctrl Pts',(0.00310186664694981,-0.0325844576448127,
0.0769514149304635));
#104047=CARTESIAN_POINT('Ctrl Pts',(0.00306372888053474,-0.0324744968375319,
0.0768819257416532));
#104048=CARTESIAN_POINT('Ctrl Pts',(0.00302705608197167,-0.0323646534831895,
0.0768117033365341));
#104049=CARTESIAN_POINT('Origin',(0.0177461890740257,-0.0326395579065289,
0.0686978593326361));
#104050=CARTESIAN_POINT('Ctrl Pts',(0.00315758500232762,-0.0327445246961876,
0.0770508637441773));
#104051=CARTESIAN_POINT('Ctrl Pts',(0.0030481771387794,-0.0324436878365475,
0.0768635605570858));
#104052=CARTESIAN_POINT('Ctrl Pts',(0.00295318853283271,-0.0321434074463186,
0.0766685484312035));
#104053=CARTESIAN_POINT('Ctrl Pts',(0.00328834166687456,-0.0327445246961876,
0.0772639428249819));
#104054=CARTESIAN_POINT('Ctrl Pts',(0.00317089739450002,-0.0324436878365475,
0.0770815712060626));
#104055=CARTESIAN_POINT('Ctrl Pts',(0.0030675237444488,-0.0321434074463186,
0.0768908713031368));
#104056=CARTESIAN_POINT('Ctrl Pts',(0.00298272819906614,-0.0322357242816072,
0.0767283112361278));
#104057=CARTESIAN_POINT('Ctrl Pts',(0.00290061233014264,-0.0319819883628705,
0.0765645753341203));
#104058=CARTESIAN_POINT('Ctrl Pts',(0.00282908186306855,-0.0317295851069886,
0.0763959459955833));
#104059=CARTESIAN_POINT('Ctrl Pts',(0.00309963265901505,-0.0322357242816072,
0.076949293921522));
#104060=CARTESIAN_POINT('Ctrl Pts',(0.00301047877816578,-0.0319819883628705,
0.0767892812749444));
#104061=CARTESIAN_POINT('Ctrl Pts',(0.00293168764117612,-0.0317295851069886,
0.0766239197973653));
#104062=CARTESIAN_POINT('Origin',(0.0176624456079492,-0.0326371942643908,
0.0687433503804637));
#104063=CARTESIAN_POINT('Origin',(0.0173790431228128,-0.0326352985527103,
0.0683569820973483));
#104064=CARTESIAN_POINT('Ctrl Pts',(0.00264668323176902,-0.0321934096636183,
0.0765997728400263));
#104065=CARTESIAN_POINT('Ctrl Pts',(0.00261289895506826,-0.0320835708272303,
0.0765242393767581));
#104066=CARTESIAN_POINT('Ctrl Pts',(0.00258069743571743,-0.0319739230346346,
0.076448050562118));
#104067=CARTESIAN_POINT('Ctrl Pts',(0.00255011239213904,-0.0318646057455575,
0.0763713070363633));
#104068=CARTESIAN_POINT('Ctrl Pts',(0.00275480211298525,-0.0321934096636183,
0.0766337061907208));
#104069=CARTESIAN_POINT('Ctrl Pts',(0.00272054986893237,-0.0320835708272303,
0.0765596637710874));
#104070=CARTESIAN_POINT('Ctrl Pts',(0.00268784979659898,-0.0319739230346346,
0.0764849554506561));
#104071=CARTESIAN_POINT('Ctrl Pts',(0.00265673639764529,-0.0318646057455575,
0.0764096800244489));
#104072=CARTESIAN_POINT('Ctrl Pts',(0.00286292099420148,-0.0321934096636183,
0.0766676395414154));
#104073=CARTESIAN_POINT('Ctrl Pts',(0.00282820078279648,-0.0320835708272303,
0.0765950881654167));
#104074=CARTESIAN_POINT('Ctrl Pts',(0.00279500215748052,-0.0319739230346346,
0.0765218603391941));
#104075=CARTESIAN_POINT('Ctrl Pts',(0.00276336040315155,-0.0318646057455575,
0.0764480530125344));
#104076=CARTESIAN_POINT('Ctrl Pts',(0.00297103987541771,-0.0321934096636183,
0.07670157289211));
#104077=CARTESIAN_POINT('Ctrl Pts',(0.00293585169666059,-0.0320835708272303,
0.076630512559746));
#104078=CARTESIAN_POINT('Ctrl Pts',(0.00290215451836207,-0.0319739230346346,
0.0765587652277322));
#104079=CARTESIAN_POINT('Ctrl Pts',(0.00286998440865781,-0.0318646057455575,
0.07648642600062));
#104080=CARTESIAN_POINT('Ctrl Pts',(0.00302654010771948,-0.0320218834582394,
0.0768125027555518));
#104081=CARTESIAN_POINT('Ctrl Pts',(0.00299882989059256,-0.0319391099350668,
0.0767594527879451));
#104082=CARTESIAN_POINT('Ctrl Pts',(0.00297196484506484,-0.0318564869454926,
0.0767060022630402));
#104083=CARTESIAN_POINT('Ctrl Pts',(0.00294596090422198,-0.0317740741446496,
0.0766521919392276));
#104084=CARTESIAN_POINT('Ctrl Pts',(0.0030106817987234,-0.0320218834582394,
0.0768594638254233));
#104085=CARTESIAN_POINT('Ctrl Pts',(0.00298248283038676,-0.0319391099350668,
0.0768062488111572));
#104086=CARTESIAN_POINT('Ctrl Pts',(0.00295513190699799,-0.0318564869454926,
0.0767526257076716));
#104087=CARTESIAN_POINT('Ctrl Pts',(0.00292864530380531,-0.0317740741446496,
0.0766986354320969));
#104088=CARTESIAN_POINT('Ctrl Pts',(0.00299482348972731,-0.0320218834582394,
0.0769064248952948));
#104089=CARTESIAN_POINT('Ctrl Pts',(0.00296613577018095,-0.0319391099350668,
0.0768530448343692));
#104090=CARTESIAN_POINT('Ctrl Pts',(0.00293829896893114,-0.0318564869454926,
0.0767992491523032));
#104091=CARTESIAN_POINT('Ctrl Pts',(0.00291132970338863,-0.0317740741446496,
0.0767450789249662));
#104092=CARTESIAN_POINT('Ctrl Pts',(0.00297896518073123,-0.0320218834582394,
0.0769533859651663));
#104093=CARTESIAN_POINT('Ctrl Pts',(0.00294978870997515,-0.0319391099350668,
0.0768998408575813));
#104094=CARTESIAN_POINT('Ctrl Pts',(0.00292146603086429,-0.0318564869454926,
0.0768458725969347));
#104095=CARTESIAN_POINT('Ctrl Pts',(0.00289401410297195,-0.0317740741446496,
0.0767915224178355));
#104096=CARTESIAN_POINT('Ctrl Pts',(0.00493979735941889,-0.0350241211493618,
0.0789378513677008));
#104097=CARTESIAN_POINT('Ctrl Pts',(0.00487384667289248,-0.0349144232867607,
0.0788939932840753));
#104098=CARTESIAN_POINT('Ctrl Pts',(0.00480876308959006,-0.0348045283677605,
0.0788487457015188));
#104099=CARTESIAN_POINT('Ctrl Pts',(0.00474463212999654,-0.0346945769586886,
0.0788021634742698));
#104100=CARTESIAN_POINT('Ctrl Pts',(0.00495975571087317,-0.0350241211493618,
0.0790493986940272));
#104101=CARTESIAN_POINT('Ctrl Pts',(0.00489226850573195,-0.0349144232867607,
0.0790058155284973));
#104102=CARTESIAN_POINT('Ctrl Pts',(0.00482564180138109,-0.0348045283677605,
0.0789608112676519));
#104103=CARTESIAN_POINT('Ctrl Pts',(0.00475996308324953,-0.0346945769586886,
0.0789144403805136));
#104104=CARTESIAN_POINT('Ctrl Pts',(0.00497971406232745,-0.0350241211493618,
0.0791609460203535));
#104105=CARTESIAN_POINT('Ctrl Pts',(0.00491069033857141,-0.0349144232867607,
0.0791176377729192));
#104106=CARTESIAN_POINT('Ctrl Pts',(0.00484252051317211,-0.0348045283677605,
0.079072876833785));
#104107=CARTESIAN_POINT('Ctrl Pts',(0.00477529403650252,-0.0346945769586886,
0.0790267172867574));
#104108=CARTESIAN_POINT('Ctrl Pts',(0.00499967241378172,-0.0350241211493618,
0.0792724933466798));
#104109=CARTESIAN_POINT('Ctrl Pts',(0.00492911217141088,-0.0349144232867607,
0.0792294600173412));
#104110=CARTESIAN_POINT('Ctrl Pts',(0.00485939922496313,-0.0348045283677605,
0.0791849423999181));
#104111=CARTESIAN_POINT('Ctrl Pts',(0.00479062498975552,-0.0346945769586886,
0.0791389941930012));
#104112=CARTESIAN_POINT('Origin',(0.014756343467682,-0.034562906794184,
0.0653251984889228));
#104113=CARTESIAN_POINT('Ctrl Pts',(0.00459642973095872,-0.03519709736516,
0.0789179457195974));
#104114=CARTESIAN_POINT('Ctrl Pts',(0.00453037630472438,-0.0350869349321763,
0.0788690790316434));
#104115=CARTESIAN_POINT('Ctrl Pts',(0.00446528407196257,-0.034976498512972,
0.0788187986489671));
#104116=CARTESIAN_POINT('Ctrl Pts',(0.00440124119607719,-0.0348659306849645,
0.0787671647471887));
#104117=CARTESIAN_POINT('Ctrl Pts',(0.00467703263188872,-0.03519709736516,
0.0789017086320442));
#104118=CARTESIAN_POINT('Ctrl Pts',(0.00461120414849727,-0.0350869349321763,
0.0788539585880463));
#104119=CARTESIAN_POINT('Ctrl Pts',(0.00454631383050936,-0.034976498512972,
0.078804800450778));
#104120=CARTESIAN_POINT('Ctrl Pts',(0.00448244949415718,-0.0348659306849645,
0.0787542929573562));
#104121=CARTESIAN_POINT('Ctrl Pts',(0.00475763553281871,-0.03519709736516,
0.078885471544491));
#104122=CARTESIAN_POINT('Ctrl Pts',(0.00469203199227016,-0.0350869349321763,
0.0788388381444492));
#104123=CARTESIAN_POINT('Ctrl Pts',(0.00462734358905615,-0.034976498512972,
0.0787908022525889));
#104124=CARTESIAN_POINT('Ctrl Pts',(0.00456365779223717,-0.0348659306849645,
0.0787414211675236));
#104125=CARTESIAN_POINT('Ctrl Pts',(0.0048382384337487,-0.03519709736516,
0.0788692344569377));
#104126=CARTESIAN_POINT('Ctrl Pts',(0.00477285983604305,-0.0350869349321763,
0.078823717700852));
#104127=CARTESIAN_POINT('Ctrl Pts',(0.00470837334760294,-0.034976498512972,
0.0787768040543999));
#104128=CARTESIAN_POINT('Ctrl Pts',(0.00464486609031715,-0.0348659306849645,
0.0787285493776911));
#104129=CARTESIAN_POINT('Origin',(0.0151117818539896,-0.0345637187967143,
0.0656492184110888));
#104130=CARTESIAN_POINT('Ctrl Pts',(0.00486532304494461,-0.0352450361861253,
0.0788892582731634));
#104131=CARTESIAN_POINT('Ctrl Pts',(0.00468657899071769,-0.0349452761023765,
0.0787663634729426));
#104132=CARTESIAN_POINT('Ctrl Pts',(0.00451759966846667,-0.0346444289983475,
0.0786303540707146));
#104133=CARTESIAN_POINT('Ctrl Pts',(0.00507435879337509,-0.0352450361861253,
0.0790263861546395));
#104134=CARTESIAN_POINT('Ctrl Pts',(0.00489044287636505,-0.0349452761023765,
0.0789113752668368));
#104135=CARTESIAN_POINT('Ctrl Pts',(0.00471571253552146,-0.0346444289983475,
0.0787828378138066));
#104136=CARTESIAN_POINT('Origin',(-0.00211316800085609,-0.0391228853390801,
0.0805597947748885));
#104137=CARTESIAN_POINT('Ctrl Pts',(0.00509125577588388,-0.0352722978779667,
0.0790375298537638));
#104138=CARTESIAN_POINT('Ctrl Pts',(0.00507538593042427,-0.0352466642097266,
0.0790272711655831));
#104139=CARTESIAN_POINT('Ctrl Pts',(0.00505948766108327,-0.0352210183808325,
0.0790170874588308));
#104140=CARTESIAN_POINT('Ctrl Pts',(0.00504356011959463,-0.0351953608940153,
0.0790069788225492));
#104141=CARTESIAN_POINT('Origin',(0.00228085763488299,-0.0352456003065148,
0.0830514313828313));
#104142=CARTESIAN_POINT('Ctrl Pts',(0.00464544929305672,-0.0345231616327822,
0.0787284802062971));
#104143=CARTESIAN_POINT('Ctrl Pts',(0.00458234138939785,-0.0344132092796975,
0.0786805362843711));
#104144=CARTESIAN_POINT('Ctrl Pts',(0.00452022842402409,-0.0343032738558974,
0.0786312894989229));
#104145=CARTESIAN_POINT('Ctrl Pts',(0.00445918835472738,-0.0341934961088741,
0.0785808049790908));
#104146=CARTESIAN_POINT('Ctrl Pts',(0.00465836416187004,-0.0345231616327822,
0.0788410605878131));
#104147=CARTESIAN_POINT('Ctrl Pts',(0.00459370449615248,-0.0344132092796975,
0.0787932946791711));
#104148=CARTESIAN_POINT('Ctrl Pts',(0.00453003616671946,-0.0343032738558974,
0.0787441938008479));
#104149=CARTESIAN_POINT('Ctrl Pts',(0.00446743912875214,-0.0341934961088741,
0.0786938229460994));
#104150=CARTESIAN_POINT('Ctrl Pts',(0.00467127903068336,-0.0345231616327822,
0.0789536409693292));
#104151=CARTESIAN_POINT('Ctrl Pts',(0.0046050676029071,-0.0344132092796975,
0.0789060530739711));
#104152=CARTESIAN_POINT('Ctrl Pts',(0.00453984390941482,-0.0343032738558974,
0.078857098102773));
#104153=CARTESIAN_POINT('Ctrl Pts',(0.00447568990277691,-0.0341934961088741,
0.078806840913108));
#104154=CARTESIAN_POINT('Ctrl Pts',(0.00468419389949668,-0.0345231616327822,
0.0790662213508453));
#104155=CARTESIAN_POINT('Ctrl Pts',(0.00461643070966173,-0.0344132092796975,
0.0790188114687711));
#104156=CARTESIAN_POINT('Ctrl Pts',(0.00454965165211019,-0.0343032738558974,
0.078970002404698));
#104157=CARTESIAN_POINT('Ctrl Pts',(0.00448394067680167,-0.0341934961088741,
0.0789198588801166));
#104158=CARTESIAN_POINT('Origin',(0.0147634136330329,-0.0345625596229466,
0.0653153744863288));
#104159=CARTESIAN_POINT('Ctrl Pts',(0.0042110174281769,-0.0346945769586885,
0.0786986560536431));
#104160=CARTESIAN_POINT('Ctrl Pts',(0.00414833464864841,-0.0345846629176052,
0.0786447361774831));
#104161=CARTESIAN_POINT('Ctrl Pts',(0.00408675620364244,-0.034474692505031,
0.0785895108375374));
#104162=CARTESIAN_POINT('Ctrl Pts',(0.00402636070232569,-0.0343648066253259,
0.0785330511207269));
#104163=CARTESIAN_POINT('Ctrl Pts',(0.00432329424601654,-0.0346945769586885,
0.0786833251124613));
#104164=CARTESIAN_POINT('Ctrl Pts',(0.00426082273460653,-0.0345846629176052,
0.0786309524676012));
#104165=CARTESIAN_POINT('Ctrl Pts',(0.00419942359769629,-0.034474692505031,
0.0785772789921643));
#104166=CARTESIAN_POINT('Ctrl Pts',(0.00413917522291422,-0.0343648066253259,
0.078522373783695));
#104167=CARTESIAN_POINT('Ctrl Pts',(0.00443557106385618,-0.0346945769586885,
0.0786679941712795));
#104168=CARTESIAN_POINT('Ctrl Pts',(0.00437331082056465,-0.0345846629176052,
0.0786171687577194));
#104169=CARTESIAN_POINT('Ctrl Pts',(0.00431209099175013,-0.034474692505031,
0.0785650471467912));
#104170=CARTESIAN_POINT('Ctrl Pts',(0.00425198974350276,-0.0343648066253259,
0.078511696446663));
#104171=CARTESIAN_POINT('Ctrl Pts',(0.00454784788169582,-0.0346945769586885,
0.0786526632300978));
#104172=CARTESIAN_POINT('Ctrl Pts',(0.00448579890652278,-0.0345846629176052,
0.0786033850478375));
#104173=CARTESIAN_POINT('Ctrl Pts',(0.00442475838580397,-0.034474692505031,
0.0785528153014181));
#104174=CARTESIAN_POINT('Ctrl Pts',(0.0043648042640913,-0.0343648066253259,
0.0785010191096311));
#104175=CARTESIAN_POINT('Origin',(0.0151482818569298,-0.0345626446729742,
0.0656035907819192));
#104176=CARTESIAN_POINT('Ctrl Pts',(0.0045458388729324,-0.0346945769586886,
0.0786529375520441));
#104177=CARTESIAN_POINT('Ctrl Pts',(0.00445152304302849,-0.0345275153362891,
0.0785779960966738));
#104178=CARTESIAN_POINT('Ctrl Pts',(0.00435953965801255,-0.0343603235965159,
0.078500069111566));
#104179=CARTESIAN_POINT('Ctrl Pts',(0.00427015733847041,-0.034193496108874,
0.078419391113463));
#104180=CARTESIAN_POINT('Ctrl Pts',(0.00461259288253264,-0.0346945769586886,
0.0787036517564996));
#104181=CARTESIAN_POINT('Ctrl Pts',(0.00451721482331157,-0.0345275153362891,
0.0786301084905873));
#104182=CARTESIAN_POINT('Ctrl Pts',(0.00442412496246005,-0.0343603235965159,
0.0785535466504464));
#104183=CARTESIAN_POINT('Ctrl Pts',(0.00433359525303593,-0.034193496108874,
0.0784741967639641));
#104184=CARTESIAN_POINT('Ctrl Pts',(0.00467934689213288,-0.0346945769586886,
0.0787543659609552));
#104185=CARTESIAN_POINT('Ctrl Pts',(0.00458290660359465,-0.0345275153362891,
0.0786822208845007));
#104186=CARTESIAN_POINT('Ctrl Pts',(0.00448871026690755,-0.0343603235965159,
0.0786070241893269));
#104187=CARTESIAN_POINT('Ctrl Pts',(0.00439703316760146,-0.034193496108874,
0.0785290024144652));
#104188=CARTESIAN_POINT('Ctrl Pts',(0.00474610090173312,-0.0346945769586886,
0.0788050801654107));
#104189=CARTESIAN_POINT('Ctrl Pts',(0.00464859838387773,-0.0345275153362891,
0.0787343332784142));
#104190=CARTESIAN_POINT('Ctrl Pts',(0.00455329557135505,-0.0343603235965159,
0.0786605017282073));
#104191=CARTESIAN_POINT('Ctrl Pts',(0.00446047108216698,-0.034193496108874,
0.0785838080649662));
#104192=CARTESIAN_POINT('Ctrl Pts',(0.0043648285057152,-0.0340223579322365,
0.0785010393167854));
#104193=CARTESIAN_POINT('Ctrl Pts',(0.00430481632555026,-0.0339125849573552,
0.0784491935416738));
#104194=CARTESIAN_POINT('Ctrl Pts',(0.00424591940232135,-0.0338030433565217,
0.0783961420853078));
#104195=CARTESIAN_POINT('Ctrl Pts',(0.00418820704119181,-0.0336938721132321,
0.0783419594682911));
#104196=CARTESIAN_POINT('Ctrl Pts',(0.00437064893739086,-0.0340223579322365,
0.078614208669552));
#104197=CARTESIAN_POINT('Ctrl Pts',(0.00430907585669322,-0.0339125849573552,
0.0785624431733736));
#104198=CARTESIAN_POINT('Ctrl Pts',(0.00424861746817096,-0.0338030433565217,
0.0785094396325156));
#104199=CARTESIAN_POINT('Ctrl Pts',(0.00418934507927019,-0.0336938721132321,
0.0784552726833185));
#104200=CARTESIAN_POINT('Ctrl Pts',(0.00437646936906652,-0.0340223579322365,
0.0787273780223186));
#104201=CARTESIAN_POINT('Ctrl Pts',(0.00431333538783617,-0.0339125849573552,
0.0786756928050733));
#104202=CARTESIAN_POINT('Ctrl Pts',(0.00425131553402058,-0.0338030433565217,
0.0786227371797234));
#104203=CARTESIAN_POINT('Ctrl Pts',(0.00419048311734857,-0.0336938721132321,
0.0785685858983459));
#104204=CARTESIAN_POINT('Ctrl Pts',(0.00438228980074218,-0.0340223579322365,
0.0788405473750853));
#104205=CARTESIAN_POINT('Ctrl Pts',(0.00431759491897913,-0.0339125849573552,
0.0787889424367731));
#104206=CARTESIAN_POINT('Ctrl Pts',(0.00425401359987019,-0.0338030433565217,
0.0787360347269312));
#104207=CARTESIAN_POINT('Ctrl Pts',(0.00419162115542696,-0.0336938721132321,
0.0786818991133732));
#104208=CARTESIAN_POINT('Origin',(0.0146891305925633,-0.0345589643415143,
0.0654098991288901));
#104209=CARTESIAN_POINT('Ctrl Pts',(0.00393312589888617,-0.034193496108874,
0.0784439957875769));
#104210=CARTESIAN_POINT('Ctrl Pts',(0.00387391423977879,-0.0340836138581107,
0.0783862091188876));
#104211=CARTESIAN_POINT('Ctrl Pts',(0.00381592676539424,-0.0339738896643499,
0.0783272249162861));
#104212=CARTESIAN_POINT('Ctrl Pts',(0.00375923263190683,-0.0338644633294062,
0.0782671236473839));
#104213=CARTESIAN_POINT('Ctrl Pts',(0.00404614396758526,-0.034193496108874,
0.0784357450061283));
#104214=CARTESIAN_POINT('Ctrl Pts',(0.00398704608186814,-0.0340836138581107,
0.0783795167896797));
#104215=CARTESIAN_POINT('Ctrl Pts',(0.00392914007738418,-0.0339738896643499,
0.0783220926458458));
#104216=CARTESIAN_POINT('Ctrl Pts',(0.00387249513988373,-0.0338644633294062,
0.0782635510385658));
#104217=CARTESIAN_POINT('Ctrl Pts',(0.00415916203628435,-0.034193496108874,
0.0784274942246797));
#104218=CARTESIAN_POINT('Ctrl Pts',(0.00410017792395748,-0.0340836138581107,
0.0783728244604719));
#104219=CARTESIAN_POINT('Ctrl Pts',(0.00404235338937413,-0.0339738896643499,
0.0783169603754056));
#104220=CARTESIAN_POINT('Ctrl Pts',(0.00398575764786062,-0.0338644633294062,
0.0782599784297477));
#104221=CARTESIAN_POINT('Ctrl Pts',(0.00427218010498344,-0.034193496108874,
0.0784192434432311));
#104222=CARTESIAN_POINT('Ctrl Pts',(0.00421330976604683,-0.0340836138581107,
0.078366132131264));
#104223=CARTESIAN_POINT('Ctrl Pts',(0.00415556670136407,-0.0339738896643499,
0.0783118281049653));
#104224=CARTESIAN_POINT('Ctrl Pts',(0.00409902015583752,-0.0338644633294062,
0.0782564058209295));
#104225=CARTESIAN_POINT('Origin',(0.0150996077902769,-0.0345610621862833,
0.0656610136081441));
#104226=CARTESIAN_POINT('Ctrl Pts',(0.00429708900780242,-0.03424362768739,
0.0784435468165065));
#104227=CARTESIAN_POINT('Ctrl Pts',(0.00413515522010882,-0.0339430054201861,
0.0782992207037796));
#104228=CARTESIAN_POINT('Ctrl Pts',(0.00398455270349793,-0.0336441434784164,
0.0781431070900165));
#104229=CARTESIAN_POINT('Ctrl Pts',(0.00448729198063623,-0.03424362768739,
0.0786057899338495));
#104230=CARTESIAN_POINT('Ctrl Pts',(0.00431923909289752,-0.0339430054201861,
0.0784686374445015));
#104231=CARTESIAN_POINT('Ctrl Pts',(0.00416199451325736,-0.0336441434784164,
0.0783192161589178));
#104232=CARTESIAN_POINT('Ctrl Pts',(0.00409904004918011,-0.0335235895815127,
0.0782564251414534));
#104233=CARTESIAN_POINT('Ctrl Pts',(0.00404250702230167,-0.0334144449262719,
0.0782010166418549));
#104234=CARTESIAN_POINT('Ctrl Pts',(0.00398705374372666,-0.0333049234473133,
0.0781443765548139));
#104235=CARTESIAN_POINT('Ctrl Pts',(0.00393275768176867,-0.0331951640388588,
0.0780865708824843));
#104236=CARTESIAN_POINT('Ctrl Pts',(0.00409774298180513,-0.0335235895815127,
0.0783697366152884));
#104237=CARTESIAN_POINT('Ctrl Pts',(0.00403964999939961,-0.0334144449262719,
0.0783143102590038));
#104238=CARTESIAN_POINT('Ctrl Pts',(0.00398263534200331,-0.0333049234473133,
0.0782576200672543));
#104239=CARTESIAN_POINT('Ctrl Pts',(0.00392677848025757,-0.0331951640388588,
0.0781997319254086));
#104240=CARTESIAN_POINT('Ctrl Pts',(0.00409644591443015,-0.0335235895815127,
0.0784830480891234));
#104241=CARTESIAN_POINT('Ctrl Pts',(0.00403679297649755,-0.0334144449262719,
0.0784276038761527));
#104242=CARTESIAN_POINT('Ctrl Pts',(0.00397821694027996,-0.0333049234473133,
0.0783708635796947));
#104243=CARTESIAN_POINT('Ctrl Pts',(0.00392079927874647,-0.0331951640388588,
0.0783128929683329));
#104244=CARTESIAN_POINT('Ctrl Pts',(0.00409514884705517,-0.0335235895815127,
0.0785963595629584));
#104245=CARTESIAN_POINT('Ctrl Pts',(0.0040339359535955,-0.0334144449262719,
0.0785408974933015));
#104246=CARTESIAN_POINT('Ctrl Pts',(0.00397379853855662,-0.0333049234473133,
0.0784841070921351));
#104247=CARTESIAN_POINT('Ctrl Pts',(0.00391482007723537,-0.0331951640388588,
0.0784260540112573));
#104248=CARTESIAN_POINT('Origin',(0.0165895953408375,-0.0326434571771486,
0.0672424341472882));
#104249=CARTESIAN_POINT('Ctrl Pts',(0.00366974550751436,-0.0336938721132452,
0.0781724094443434));
#104250=CARTESIAN_POINT('Ctrl Pts',(0.00364620101025808,-0.0336474569764989,
0.0781463384896148));
#104251=CARTESIAN_POINT('Ctrl Pts',(0.00362296331972801,-0.033601104548885,
0.0781199937032171));
#104252=CARTESIAN_POINT('Ctrl Pts',(0.00356413083252362,-0.0334837508643197,
0.0780532947639813));
#104253=CARTESIAN_POINT('Ctrl Pts',(0.00350730060798373,-0.0333660264760478,
0.0779848817855008));
#104254=CARTESIAN_POINT('Ctrl Pts',(0.00400968430076233,-0.0336938721132452,
0.078168995338663));
#104255=CARTESIAN_POINT('Ctrl Pts',(0.00398615978739951,-0.0336474569764989,
0.0781449141584951));
#104256=CARTESIAN_POINT('Ctrl Pts',(0.00396291878657009,-0.033601104548885,
0.0781205592442541));
#104257=CARTESIAN_POINT('Ctrl Pts',(0.00390407791844918,-0.0334837508643197,
0.0780588982036015));
#104258=CARTESIAN_POINT('Ctrl Pts',(0.00384709003329916,-0.0333660264760478,
0.0779955206630868));
#104259=CARTESIAN_POINT('Ctrl Pts',(0.00400968430076601,-0.0336938721132427,
0.0781689953386665));
#104260=CARTESIAN_POINT('Ctrl Pts',(0.00398615978740639,-0.0336474569765026,
0.0781449141585017));
#104261=CARTESIAN_POINT('Ctrl Pts',(0.00396291878658009,-0.0336011045488949,
0.0781205592442641));
#104262=CARTESIAN_POINT('Ctrl Pts',(0.00390456798274507,-0.0334847282606778,
0.0780594117560933));
#104263=CARTESIAN_POINT('Ctrl Pts',(0.00384803921977251,-0.0333679869945434,
0.0779965760132826));
#104264=CARTESIAN_POINT('Ctrl Pts',(0.00400968430076107,-0.0336938721132427,
0.0781689953386617));
#104265=CARTESIAN_POINT('Ctrl Pts',(0.00392555023034879,-0.0335278710435083,
0.0780828703814048));
#104266=CARTESIAN_POINT('Ctrl Pts',(0.00384414661437448,-0.033362046922432,
0.0779941373001344));
#104267=CARTESIAN_POINT('Ctrl Pts',(0.00376544772787081,-0.0331951640388601,
0.0779027384253533));
#104268=CARTESIAN_POINT('Ctrl Pts',(0.00406955576618036,-0.0336938721132427,
0.0782276761485728));
#104269=CARTESIAN_POINT('Ctrl Pts',(0.00398419326553195,-0.0335278710435083,
0.0781428045468594));
#104270=CARTESIAN_POINT('Ctrl Pts',(0.00390152234657642,-0.033362046922432,
0.0780552858569522));
#104271=CARTESIAN_POINT('Ctrl Pts',(0.00382151645208865,-0.0331951640388601,
0.0779650628025091));
#104272=CARTESIAN_POINT('Ctrl Pts',(0.00412942723159965,-0.0336938721132427,
0.0782863569584839));
#104273=CARTESIAN_POINT('Ctrl Pts',(0.0040428363007151,-0.0335278710435083,
0.0782027387123141));
#104274=CARTESIAN_POINT('Ctrl Pts',(0.00395889807877836,-0.033362046922432,
0.07811643441377));
#104275=CARTESIAN_POINT('Ctrl Pts',(0.00387758517630648,-0.0331951640388601,
0.078027387179665));
#104276=CARTESIAN_POINT('Ctrl Pts',(0.00418929869701894,-0.0336938721132427,
0.078345037768395));
#104277=CARTESIAN_POINT('Ctrl Pts',(0.00410147933589826,-0.0335278710435083,
0.0782626728777687));
#104278=CARTESIAN_POINT('Ctrl Pts',(0.0040162738109803,-0.033362046922432,
0.0781775829705879));
#104279=CARTESIAN_POINT('Ctrl Pts',(0.00393365390052432,-0.0331951640388601,
0.0780897115568208));
#104280=CARTESIAN_POINT('Ctrl Pts',(0.00384913797052196,-0.0330240426238156,
0.0779956075658159));
#104281=CARTESIAN_POINT('Ctrl Pts',(0.00379616097970921,-0.0329142774063509,
0.077936720177066));
#104282=CARTESIAN_POINT('Ctrl Pts',(0.00374437494475373,-0.0328043479726686,
0.0778767082484212));
#104283=CARTESIAN_POINT('Ctrl Pts',(0.00369384832467781,-0.0326943950436594,
0.077815646832591));
#104284=CARTESIAN_POINT('Ctrl Pts',(0.00384072860635565,-0.0330240426238156,
0.0781086138425399));
#104285=CARTESIAN_POINT('Ctrl Pts',(0.00378619484398436,-0.0329142774063509,
0.0780496106066058));
#104286=CARTESIAN_POINT('Ctrl Pts',(0.00373285365624783,-0.0328043479726686,
0.0779894505902059));
#104287=CARTESIAN_POINT('Ctrl Pts',(0.00368077549965953,-0.0326943950436594,
0.0779282089808946));
#104288=CARTESIAN_POINT('Ctrl Pts',(0.00383231924218934,-0.0330240426238156,
0.0782216201192638));
#104289=CARTESIAN_POINT('Ctrl Pts',(0.0037762287082595,-0.0329142774063509,
0.0781625010361455));
#104290=CARTESIAN_POINT('Ctrl Pts',(0.00372133236774193,-0.0328043479726686,
0.0781021929319906));
#104291=CARTESIAN_POINT('Ctrl Pts',(0.00366770267464125,-0.0326943950436594,
0.0780407711291983));
#104292=CARTESIAN_POINT('Ctrl Pts',(0.00382390987802303,-0.0330240426238156,
0.0783346263959878));
#104293=CARTESIAN_POINT('Ctrl Pts',(0.00376626257253464,-0.0329142774063509,
0.0782753914656852));
#104294=CARTESIAN_POINT('Ctrl Pts',(0.00370981107923603,-0.0328043479726686,
0.0782149352737753));
#104295=CARTESIAN_POINT('Ctrl Pts',(0.00365462984962296,-0.0326943950436594,
0.078153333277502));
#104296=CARTESIAN_POINT('Origin',(0.0166836485668985,-0.0326396682856619,
0.0671621260557949));
#104297=CARTESIAN_POINT('Ctrl Pts',(0.00342799009848604,-0.0331951640388587,
0.077884907844126));
#104298=CARTESIAN_POINT('Ctrl Pts',(0.00337654929859024,-0.0330855618255041,
0.0778202328075326));
#104299=CARTESIAN_POINT('Ctrl Pts',(0.00332640813819479,-0.0329757224427707,
0.0777544479542062));
#104300=CARTESIAN_POINT('Ctrl Pts',(0.00327763495828507,-0.0328657862078596,
0.0776876343760267));
#104301=CARTESIAN_POINT('Ctrl Pts',(0.0035411510513182,-0.0331951640388587,
0.0778908870408769));
#104302=CARTESIAN_POINT('Ctrl Pts',(0.00348962790008298,-0.0330855618255041,
0.077827770567486));
#104303=CARTESIAN_POINT('Ctrl Pts',(0.00343937211614491,-0.0329757224427707,
0.077763543698847));
#104304=CARTESIAN_POINT('Ctrl Pts',(0.00339045208940823,-0.0328657862078596,
0.0776982855245472));
#104305=CARTESIAN_POINT('Ctrl Pts',(0.00365431200415035,-0.0331951640388587,
0.0778968662376277));
#104306=CARTESIAN_POINT('Ctrl Pts',(0.0036027065015757,-0.0330855618255041,
0.0778353083274393));
#104307=CARTESIAN_POINT('Ctrl Pts',(0.00355233609409502,-0.0329757224427707,
0.0777726394434879));
#104308=CARTESIAN_POINT('Ctrl Pts',(0.0035032692205314,-0.0328657862078596,
0.0777089366730677));
#104309=CARTESIAN_POINT('Ctrl Pts',(0.00376747295698251,-0.0331951640388587,
0.0779028454343785));
#104310=CARTESIAN_POINT('Ctrl Pts',(0.00371578510306843,-0.0330855618255041,
0.0778428460873926));
#104311=CARTESIAN_POINT('Ctrl Pts',(0.00366530007204514,-0.0329757224427707,
0.0777817351881287));
#104312=CARTESIAN_POINT('Ctrl Pts',(0.00361608635165456,-0.0328657862078596,
0.0777195878215882));
#104313=CARTESIAN_POINT('Origin',(0.0169569283738614,-0.0326401908834453,
0.0675578418864235));
#104314=CARTESIAN_POINT('Ctrl Pts',(0.00378909189056348,-0.0332451089994431,
0.0779300244683103));
#104315=CARTESIAN_POINT('Ctrl Pts',(0.00364652593524024,-0.0329451141710258,
0.0777665389487869));
#104316=CARTESIAN_POINT('Ctrl Pts',(0.00351667939241414,-0.0326442513127504,
0.077592779223801));
#104317=CARTESIAN_POINT('Ctrl Pts',(0.00395745827303377,-0.0332451089994431,
0.0781148291253237));
#104318=CARTESIAN_POINT('Ctrl Pts',(0.00380792229603575,-0.0329451141710258,
0.0779576936478073));
#104319=CARTESIAN_POINT('Ctrl Pts',(0.00367064722150769,-0.0326442513127504,
0.0777897409145031));
#104320=CARTESIAN_POINT('Ctrl Pts',(0.00361610589119112,-0.0325229783203385,
0.0777196126406724));
#104321=CARTESIAN_POINT('Ctrl Pts',(0.00356689885989739,-0.0324130253112079,
0.077657474422558));
#104322=CARTESIAN_POINT('Ctrl Pts',(0.00351898470065442,-0.0323031222247694,
0.0775943277182869));
#104323=CARTESIAN_POINT('Ctrl Pts',(0.00347242193387571,-0.0321934096636184,
0.0775302555800038));
#104324=CARTESIAN_POINT('Ctrl Pts',(0.00360061741211605,-0.0325229783203385,
0.0778318679285898));
#104325=CARTESIAN_POINT('Ctrl Pts',(0.0035498629441614,-0.0324130253112079,
0.0777695162021339));
#104326=CARTESIAN_POINT('Ctrl Pts',(0.00350040599965085,-0.0323031222247694,
0.0777061240111895));
#104327=CARTESIAN_POINT('Ctrl Pts',(0.00345230706410009,-0.0321934096636184,
0.0776417747920857));
#104328=CARTESIAN_POINT('Ctrl Pts',(0.00358512893304098,-0.0325229783203385,
0.0779441232165072));
#104329=CARTESIAN_POINT('Ctrl Pts',(0.00353282702842542,-0.0324130253112079,
0.0778815579817098));
#104330=CARTESIAN_POINT('Ctrl Pts',(0.00348182729864727,-0.0323031222247694,
0.0778179203040921));
#104331=CARTESIAN_POINT('Ctrl Pts',(0.00343219219432447,-0.0321934096636184,
0.0777532940041677));
#104332=CARTESIAN_POINT('Ctrl Pts',(0.00356964045396591,-0.0325229783203385,
0.0780563785044246));
#104333=CARTESIAN_POINT('Ctrl Pts',(0.00351579111268944,-0.0324130253112079,
0.0779935997612857));
#104334=CARTESIAN_POINT('Ctrl Pts',(0.00346324859764369,-0.0323031222247694,
0.0779297165969947));
#104335=CARTESIAN_POINT('Ctrl Pts',(0.00341207732454886,-0.0321934096636184,
0.0778648132162496));
#104336=CARTESIAN_POINT('Origin',(0.016676895775367,-0.0326393375177862,
0.0671673309411812));
#104337=CARTESIAN_POINT('Ctrl Pts',(0.00320273936760646,-0.0326943950436593,
0.0775826866314311));
#104338=CARTESIAN_POINT('Ctrl Pts',(0.00315543051228508,-0.0325844576448126,
0.0775148654382787));
#104339=CARTESIAN_POINT('Ctrl Pts',(0.00310952096231126,-0.0324744968375318,
0.0774460610206231));
#104340=CARTESIAN_POINT('Ctrl Pts',(0.00306506832373831,-0.0323646534831894,
0.0773763623460288));
#104341=CARTESIAN_POINT('Ctrl Pts',(0.00331530147908066,-0.0326943950436593,
0.0775957594521721));
#104342=CARTESIAN_POINT('Ctrl Pts',(0.00326781245578839,-0.0325844576448126,
0.0775294895758797));
#104343=CARTESIAN_POINT('Ctrl Pts',(0.00322169064131683,-0.0324744968375318,
0.0774622328587041));
#104344=CARTESIAN_POINT('Ctrl Pts',(0.00317699394103653,-0.0323646534831894,
0.0773940762889571));
#104345=CARTESIAN_POINT('Ctrl Pts',(0.00342786359055486,-0.0326943950436593,
0.0776088322729131));
#104346=CARTESIAN_POINT('Ctrl Pts',(0.0033801943992917,-0.0325844576448126,
0.0775441137134806));
#104347=CARTESIAN_POINT('Ctrl Pts',(0.0033338603203224,-0.0324744968375318,
0.0774784046967851));
#104348=CARTESIAN_POINT('Ctrl Pts',(0.00328891955833475,-0.0323646534831894,
0.0774117902318853));
#104349=CARTESIAN_POINT('Ctrl Pts',(0.00354042570202905,-0.0326943950436593,
0.077621905093654));
#104350=CARTESIAN_POINT('Ctrl Pts',(0.00349257634279501,-0.0325844576448126,
0.0775587378510816));
#104351=CARTESIAN_POINT('Ctrl Pts',(0.00344602999932797,-0.0324744968375318,
0.0774945765348661));
#104352=CARTESIAN_POINT('Ctrl Pts',(0.00340084517563298,-0.0323646534831894,
0.0774295041748136));
#104353=CARTESIAN_POINT('Origin',(0.0169869791008811,-0.0326395579070497,
0.0675348437211409));
#104354=CARTESIAN_POINT('Ctrl Pts',(0.00356031958369538,-0.0327445246961878,
0.0776504191195471));
#104355=CARTESIAN_POINT('Ctrl Pts',(0.00342829911973467,-0.0324436878365476,
0.0774783053153463));
#104356=CARTESIAN_POINT('Ctrl Pts',(0.0033096180269965,-0.0321434074463187,
0.077296736147459));
#104357=CARTESIAN_POINT('Ctrl Pts',(0.0037167510830894,-0.0327445246961878,
0.0778454298525781));
#104358=CARTESIAN_POINT('Ctrl Pts',(0.00357737566917189,-0.0324436878365476,
0.0776792159587661));
#104359=CARTESIAN_POINT('Ctrl Pts',(0.00345091611575342,-0.0321434074463187,
0.0775029759353604));
#104360=CARTESIAN_POINT('Ctrl Pts',(0.00334641502972665,-0.0322357242816073,
0.0773523254029287));
#104361=CARTESIAN_POINT('Ctrl Pts',(0.00324442511890726,-0.0319819883628706,
0.0772001724547932));
#104362=CARTESIAN_POINT('Ctrl Pts',(0.0031523238306585,-0.0317295851069886,
0.0770418379536945));
#104363=CARTESIAN_POINT('Ctrl Pts',(0.00349009413761337,-0.0322357242816073,
0.0775569135598608));
#104364=CARTESIAN_POINT('Ctrl Pts',(0.0033815883593368,-0.0319819883628706,
0.0774093366049665));
#104365=CARTESIAN_POINT('Ctrl Pts',(0.00328269322530411,-0.0317295851069886,
0.0772551542000042));
#104366=CARTESIAN_POINT('Origin',(0.0169095975179532,-0.0326371942645834,
0.0675904718978414));
#104367=CARTESIAN_POINT('Origin',(0.0165800049600085,-0.0326352985529742,
0.0672426699936465));
#104368=CARTESIAN_POINT('Ctrl Pts',(0.00299690974454782,-0.0321934096636183,
0.0772669181728473));
#104369=CARTESIAN_POINT('Ctrl Pts',(0.00295392501376602,-0.0320835708272303,
0.0771962146061403));
#104370=CARTESIAN_POINT('Ctrl Pts',(0.00291242842251313,-0.0319739230346346,
0.0771246624836061));
#104371=CARTESIAN_POINT('Ctrl Pts',(0.00287246603690069,-0.0318646057455575,
0.0770523574258845));
#104372=CARTESIAN_POINT('Ctrl Pts',(0.00310842905266035,-0.0321934096636183,
0.0772870330599441));
#104373=CARTESIAN_POINT('Ctrl Pts',(0.0030651669219089,-0.0320835708272303,
0.0772178674314088));
#104374=CARTESIAN_POINT('Ctrl Pts',(0.00302336126403907,-0.0319739230346346,
0.0771478466142018));
#104375=CARTESIAN_POINT('Ctrl Pts',(0.00298305869095478,-0.0318646057455575,
0.0770770643001119));
#104376=CARTESIAN_POINT('Ctrl Pts',(0.00321994836077288,-0.0321934096636183,
0.0773071479470409));
#104377=CARTESIAN_POINT('Ctrl Pts',(0.00317640883005177,-0.0320835708272303,
0.0772395202566774));
#104378=CARTESIAN_POINT('Ctrl Pts',(0.00313429410556502,-0.0319739230346346,
0.0771710307447974));
#104379=CARTESIAN_POINT('Ctrl Pts',(0.00309365134500887,-0.0318646057455575,
0.0771017711743393));
#104380=CARTESIAN_POINT('Ctrl Pts',(0.0033314676688854,-0.0321934096636183,
0.0773272628341376));
#104381=CARTESIAN_POINT('Ctrl Pts',(0.00328765073819465,-0.0320835708272303,
0.0772611730819459));
#104382=CARTESIAN_POINT('Ctrl Pts',(0.00324522694709097,-0.0319739230346346,
0.077194214875393));
#104383=CARTESIAN_POINT('Ctrl Pts',(0.00320424399906295,-0.0318646057455575,
0.0771264780485666));
#104384=CARTESIAN_POINT('Ctrl Pts',(0.00340043346376184,-0.0320218834582391,
0.0774303619588967));
#104385=CARTESIAN_POINT('Ctrl Pts',(0.00336629282599294,-0.0319391099350663,
0.0773812033172451));
#104386=CARTESIAN_POINT('Ctrl Pts',(0.00333294049225132,-0.0318564869454921,
0.0773315413487196));
#104387=CARTESIAN_POINT('Ctrl Pts',(0.0033003973783664,-0.0317740741446491,
0.0772814144933739));
#104388=CARTESIAN_POINT('Ctrl Pts',(0.00339058598500747,-0.0320218834582391,
0.077478940299851));
#104389=CARTESIAN_POINT('Ctrl Pts',(0.00335593976414661,-0.0319391099350663,
0.0774296791697517));
#104390=CARTESIAN_POINT('Ctrl Pts',(0.00332208375400445,-0.0318564869454921,
0.0773799068801228));
#104391=CARTESIAN_POINT('Ctrl Pts',(0.00328903922977025,-0.0317740741446491,
0.0773296619856212));
#104392=CARTESIAN_POINT('Ctrl Pts',(0.00338073850625309,-0.0320218834582391,
0.0775275186408052));
#104393=CARTESIAN_POINT('Ctrl Pts',(0.00334558670230027,-0.0319391099350663,
0.0774781550222582));
#104394=CARTESIAN_POINT('Ctrl Pts',(0.00331122701575758,-0.0318564869454921,
0.077428272411526));
#104395=CARTESIAN_POINT('Ctrl Pts',(0.0032776810811741,-0.0317740741446491,
0.0773779094778686));
#104396=CARTESIAN_POINT('Ctrl Pts',(0.00337089102749872,-0.0320218834582391,
0.0775760969817595));
#104397=CARTESIAN_POINT('Ctrl Pts',(0.00333523364045393,-0.0319391099350663,
0.0775266308747648));
#104398=CARTESIAN_POINT('Ctrl Pts',(0.00330037027751072,-0.0318564869454921,
0.0774766379429291));
#104399=CARTESIAN_POINT('Ctrl Pts',(0.00326632293257795,-0.0317740741446491,
0.0774261569701159));
#104400=CARTESIAN_POINT('Origin',(-0.00122908628533505,-0.039122885339083,
0.0817922816982227));
#104401=CARTESIAN_POINT('Ctrl Pts',(0.00572773807316979,-0.0352722978779668,
0.0793790665627724));
#104402=CARTESIAN_POINT('Ctrl Pts',(0.00571070761161987,-0.0352466642097266,
0.0793708777864596));
#104403=CARTESIAN_POINT('Ctrl Pts',(0.00569365834798426,-0.0352210183808326,
0.0793627669627815));
#104404=CARTESIAN_POINT('Ctrl Pts',(0.00567658945184547,-0.0351953608940152,
0.0793547342863937));
#104405=CARTESIAN_POINT('Origin',(0.00344257601878882,-0.035245600306513,
0.0837135535659921));
#104406=CARTESIAN_POINT('Ctrl Pts',(0.00556498092456399,-0.035024121149334,
0.0792991568444217));
#104407=CARTESIAN_POINT('Ctrl Pts',(0.00549405340346672,-0.0349144232867422,
0.0792639104076861));
#104408=CARTESIAN_POINT('Ctrl Pts',(0.00542381199783139,-0.0348045283677512,
0.0792271767517832));
#104409=CARTESIAN_POINT('Ctrl Pts',(0.00535434842884735,-0.0346945769586886,
0.0791889995798501));
#104410=CARTESIAN_POINT('Ctrl Pts',(0.00559876248555947,-0.035024121149334,
0.0794073231420385));
#104411=CARTESIAN_POINT('Ctrl Pts',(0.00552634501812962,-0.0349144232867422,
0.0793725420324337));
#104412=CARTESIAN_POINT('Ctrl Pts',(0.00545460315571319,-0.0348045283677512,
0.0793362431839283));
#104413=CARTESIAN_POINT('Ctrl Pts',(0.00538363052066906,-0.0346945769586886,
0.0792984696712083));
#104414=CARTESIAN_POINT('Ctrl Pts',(0.00563254404655495,-0.035024121149334,
0.0795154894396554));
#104415=CARTESIAN_POINT('Ctrl Pts',(0.00555863663279252,-0.0349144232867422,
0.0794811736571813));
#104416=CARTESIAN_POINT('Ctrl Pts',(0.00548539431359499,-0.0348045283677512,
0.0794453096160734));
#104417=CARTESIAN_POINT('Ctrl Pts',(0.00541291261249077,-0.0346945769586886,
0.0794079397625665));
#104418=CARTESIAN_POINT('Ctrl Pts',(0.00566632560755044,-0.035024121149334,
0.0796236557372722));
#104419=CARTESIAN_POINT('Ctrl Pts',(0.00559092824745542,-0.0349144232867422,
0.0795898052819289));
#104420=CARTESIAN_POINT('Ctrl Pts',(0.00551618547147678,-0.0348045283677512,
0.0795543760482185));
#104421=CARTESIAN_POINT('Ctrl Pts',(0.00544219470431248,-0.0346945769586886,
0.0795174098539247));
#104422=CARTESIAN_POINT('Origin',(0.0135980028313961,-0.0345629067942075,
0.0645635043344994));
#104423=CARTESIAN_POINT('Ctrl Pts',(0.00522182601318706,-0.0351970973651599,
0.0793224435334846));
#104424=CARTESIAN_POINT('Ctrl Pts',(0.00515016881793308,-0.0350869349321764,
0.0792822408634588));
#104425=CARTESIAN_POINT('Ctrl Pts',(0.0050792880539232,-0.0349764985129723,
0.07924051517663));
#104426=CARTESIAN_POINT('Ctrl Pts',(0.00500927873137156,-0.0348659306849651,
0.079197315124311));
#104427=CARTESIAN_POINT('Ctrl Pts',(0.00529975828948135,-0.0351970973651599,
0.0792962322580083));
#104428=CARTESIAN_POINT('Ctrl Pts',(0.00522846421592652,-0.0350869349321764,
0.0792571092340537));
#104429=CARTESIAN_POINT('Ctrl Pts',(0.00515792442917808,-0.0349764985129723,
0.0792164716367612));
#104430=CARTESIAN_POINT('Ctrl Pts',(0.00508823341472374,-0.0348659306849651,
0.0791743667337953));
#104431=CARTESIAN_POINT('Ctrl Pts',(0.00537769056577565,-0.0351970973651599,
0.0792700209825321));
#104432=CARTESIAN_POINT('Ctrl Pts',(0.00530675961391997,-0.0350869349321764,
0.0792319776046486));
#104433=CARTESIAN_POINT('Ctrl Pts',(0.00523656080443296,-0.0349764985129723,
0.0791924280968924));
#104434=CARTESIAN_POINT('Ctrl Pts',(0.00516718809807591,-0.0348659306849651,
0.0791514183432797));
#104435=CARTESIAN_POINT('Ctrl Pts',(0.00545562284206994,-0.0351970973651599,
0.0792438097070558));
#104436=CARTESIAN_POINT('Ctrl Pts',(0.00538505501191342,-0.0350869349321764,
0.0792068459752435));
#104437=CARTESIAN_POINT('Ctrl Pts',(0.00531519717968783,-0.0349764985129723,
0.0791683845570235));
#104438=CARTESIAN_POINT('Ctrl Pts',(0.00524614278142808,-0.0348659306849651,
0.079128469952764));
#104439=CARTESIAN_POINT('Origin',(0.0139912489451564,-0.0345637187967834,
0.0648404210190056));
#104440=CARTESIAN_POINT('Ctrl Pts',(0.00548500353265436,-0.0352450361861252,
0.0792602810276083));
#104441=CARTESIAN_POINT('Ctrl Pts',(0.00529226612598336,-0.0349452761023764,
0.0791607578598907));
#104442=CARTESIAN_POINT('Ctrl Pts',(0.00510757275798361,-0.0346444289983475,
0.0790469996572866));
#104443=CARTESIAN_POINT('Ctrl Pts',(0.00570957765256976,-0.0352450361861252,
0.0793701284884993));
#104444=CARTESIAN_POINT('Ctrl Pts',(0.00551269728103495,-0.0349452761023764,
0.079279075272482));
#104445=CARTESIAN_POINT('Ctrl Pts',(0.00532323472649595,-0.0346444289983475,
0.0791734508942809));
#104446=CARTESIAN_POINT('Ctrl Pts',(0.0052467127159667,-0.0345231616327822,
0.0791283282321213));
#104447=CARTESIAN_POINT('Ctrl Pts',(0.00517809347021286,-0.0344132092796975,
0.079088671879969));
#104448=CARTESIAN_POINT('Ctrl Pts',(0.00511029802526044,-0.0343032738558974,
0.0790475982389298));
#104449=CARTESIAN_POINT('Ctrl Pts',(0.00504341188702641,-0.0341934961088741,
0.0790051621538775));
#104450=CARTESIAN_POINT('Ctrl Pts',(0.00527363581043336,-0.0345231616327822,
0.079238402221434));
#104451=CARTESIAN_POINT('Ctrl Pts',(0.00520349934970864,-0.0344132092796975,
0.0791991169662342));
#104452=CARTESIAN_POINT('Ctrl Pts',(0.0051341790922189,-0.0343032738558974,
0.0791583830206058));
#104453=CARTESIAN_POINT('Ctrl Pts',(0.00506576250848974,-0.0341934961088741,
0.079116254844272));
#104454=CARTESIAN_POINT('Ctrl Pts',(0.00530055890490002,-0.0345231616327822,
0.0793484762107467));
#104455=CARTESIAN_POINT('Ctrl Pts',(0.00522890522920441,-0.0344132092796975,
0.0793095620524994));
#104456=CARTESIAN_POINT('Ctrl Pts',(0.00515806015917737,-0.0343032738558974,
0.0792691678022817));
#104457=CARTESIAN_POINT('Ctrl Pts',(0.00508811312995308,-0.0341934961088741,
0.0792273475346664));
#104458=CARTESIAN_POINT('Ctrl Pts',(0.00532748199936668,-0.0345231616327822,
0.0794585502000594));
#104459=CARTESIAN_POINT('Ctrl Pts',(0.00525431110870019,-0.0344132092796975,
0.0794200071387646));
#104460=CARTESIAN_POINT('Ctrl Pts',(0.00518194122613583,-0.0343032738558974,
0.0793799525839576));
#104461=CARTESIAN_POINT('Ctrl Pts',(0.00511046375141642,-0.0341934961088741,
0.0793384402250608));
#104462=CARTESIAN_POINT('Origin',(0.0136037859726627,-0.0345625596230417,
0.0645528716695589));
#104463=CARTESIAN_POINT('Ctrl Pts',(0.00481196851860944,-0.0346945769586886,
0.0791531880022078));
#104464=CARTESIAN_POINT('Ctrl Pts',(0.00474302205908745,-0.0345846629176052,
0.0791075495358235));
#104465=CARTESIAN_POINT('Ctrl Pts',(0.00467500760808286,-0.0344746925050311,
0.0790604774898087));
#104466=CARTESIAN_POINT('Ctrl Pts',(0.00460801206445927,-0.0343648066253259,
0.0790120325382018));
#104467=CARTESIAN_POINT('Ctrl Pts',(0.00492143852377309,-0.0346945769586886,
0.0791239059334422));
#104468=CARTESIAN_POINT('Ctrl Pts',(0.00485289558595925,-0.0345846629176052,
0.0790797760190604));
#104469=CARTESIAN_POINT('Ctrl Pts',(0.00478525352934943,-0.0344746925050311,
0.0790342211273758));
#104470=CARTESIAN_POINT('Ctrl Pts',(0.00471859878368086,-0.0343648066253259,
0.0789872999865031));
#104471=CARTESIAN_POINT('Ctrl Pts',(0.00503090852893673,-0.0346945769586886,
0.0790946238646766));
#104472=CARTESIAN_POINT('Ctrl Pts',(0.00496276911283105,-0.0345846629176052,
0.0790520025022974));
#104473=CARTESIAN_POINT('Ctrl Pts',(0.004895499450616,-0.0344746925050311,
0.0790079647649429));
#104474=CARTESIAN_POINT('Ctrl Pts',(0.00482918550290245,-0.0343648066253259,
0.0789625674348044));
#104475=CARTESIAN_POINT('Ctrl Pts',(0.00514037853410038,-0.0346945769586886,
0.079065341795911));
#104476=CARTESIAN_POINT('Ctrl Pts',(0.00507264263970285,-0.0345846629176052,
0.0790242289855344));
#104477=CARTESIAN_POINT('Ctrl Pts',(0.00500574537188257,-0.0344746925050311,
0.0789817084025101));
#104478=CARTESIAN_POINT('Ctrl Pts',(0.00493977222212403,-0.0343648066253259,
0.0789378348831058));
#104479=CARTESIAN_POINT('Origin',(0.0140217424761463,-0.0345626446730268,
0.06479057851436));
#104480=CARTESIAN_POINT('Ctrl Pts',(0.00513841974862758,-0.0346945769586885,
0.0790658657503114));
#104481=CARTESIAN_POINT('Ctrl Pts',(0.0050354549722837,-0.034527515336289,
0.0790033361386388));
#104482=CARTESIAN_POINT('Ctrl Pts',(0.00493443006270726,-0.0343603235965159,
0.0789375522061625));
#104483=CARTESIAN_POINT('Ctrl Pts',(0.00483564091507221,-0.034193496108874,
0.0788687129533036));
#104484=CARTESIAN_POINT('Ctrl Pts',(0.00521100355815576,-0.0346945769586885,
0.0791078135622406));
#104485=CARTESIAN_POINT('Ctrl Pts',(0.00510716016809604,-0.034527515336289,
0.0790468042475196));
#104486=CARTESIAN_POINT('Ctrl Pts',(0.00500520860560947,-0.0343603235965159,
0.0789825133736288));
#104487=CARTESIAN_POINT('Ctrl Pts',(0.00490544757212831,-0.034193496108874,
0.0789151355659178));
#104488=CARTESIAN_POINT('Ctrl Pts',(0.00528358736768393,-0.0346945769586885,
0.0791497613741698));
#104489=CARTESIAN_POINT('Ctrl Pts',(0.00517886536390838,-0.034527515336289,
0.0790902723564003));
#104490=CARTESIAN_POINT('Ctrl Pts',(0.00507598714851168,-0.0343603235965159,
0.079027474541095));
#104491=CARTESIAN_POINT('Ctrl Pts',(0.00497525422918442,-0.034193496108874,
0.0789615581785319));
#104492=CARTESIAN_POINT('Ctrl Pts',(0.0053561711772121,-0.0346945769586885,
0.079191709186099));
#104493=CARTESIAN_POINT('Ctrl Pts',(0.00525057055972072,-0.034527515336289,
0.0791337404652811));
#104494=CARTESIAN_POINT('Ctrl Pts',(0.00514676569141389,-0.0343603235965159,
0.0790724357085613));
#104495=CARTESIAN_POINT('Ctrl Pts',(0.00504506088624052,-0.034193496108874,
0.0790079807911461));
#104496=CARTESIAN_POINT('Ctrl Pts',(0.00493979880522349,-0.0340223579322365,
0.0789378518926395));
#104497=CARTESIAN_POINT('Ctrl Pts',(0.00487376184038252,-0.0339125849573552,
0.0788939364575437));
#104498=CARTESIAN_POINT('Ctrl Pts',(0.00480868022641328,-0.0338030433565216,
0.078848685069592));
#104499=CARTESIAN_POINT('Ctrl Pts',(0.0047446320618954,-0.033693872113232,
0.0788021629755311));
#104500=CARTESIAN_POINT('Ctrl Pts',(0.00495975722197961,-0.0340223579322365,
0.0790493993777354));
#104501=CARTESIAN_POINT('Ctrl Pts',(0.00489218172639113,-0.0339125849573552,
0.0790057592212603));
#104502=CARTESIAN_POINT('Ctrl Pts',(0.00482555696515432,-0.0338030433565216,
0.0789607510744829));
#104503=CARTESIAN_POINT('Ctrl Pts',(0.00475996303784863,-0.033693872113232,
0.0789144400480211));
#104504=CARTESIAN_POINT('Ctrl Pts',(0.00497971563873574,-0.0340223579322365,
0.0791609468628312));
#104505=CARTESIAN_POINT('Ctrl Pts',(0.00491060161239974,-0.0339125849573552,
0.0791175819849769));
#104506=CARTESIAN_POINT('Ctrl Pts',(0.00484243370389537,-0.0338030433565216,
0.0790728170793739));
#104507=CARTESIAN_POINT('Ctrl Pts',(0.00477529401380186,-0.033693872113232,
0.0790267171205112));
#104508=CARTESIAN_POINT('Ctrl Pts',(0.00499967405549186,-0.0340223579322365,
0.0792724943479271));
#104509=CARTESIAN_POINT('Ctrl Pts',(0.00492902149840835,-0.0339125849573552,
0.0792294047486935));
#104510=CARTESIAN_POINT('Ctrl Pts',(0.00485931044263641,-0.0338030433565216,
0.0791848830842648));
#104511=CARTESIAN_POINT('Ctrl Pts',(0.00479062498975509,-0.033693872113232,
0.0791389941930013));
#104512=CARTESIAN_POINT('Origin',(0.0135419357555965,-0.0345589643414837,
0.0646559610905117));
#104513=CARTESIAN_POINT('Ctrl Pts',(0.00450435085242287,-0.034193496108874,
0.0789353648523489));
#104514=CARTESIAN_POINT('Ctrl Pts',(0.0044383635048895,-0.0340836138581106,
0.078885455037503));
#104515=CARTESIAN_POINT('Ctrl Pts',(0.00437344059821924,-0.0339738896643499,
0.0788342037006276));
#104516=CARTESIAN_POINT('Ctrl Pts',(0.00430966082853527,-0.0338644633294062,
0.0787816820072562));
#104517=CARTESIAN_POINT('Ctrl Pts',(0.00461544364277505,-0.034193496108874,
0.0789130142107752));
#104518=CARTESIAN_POINT('Ctrl Pts',(0.00454976449735345,-0.0340836138581106,
0.0788646362997217));
#104519=CARTESIAN_POINT('Ctrl Pts',(0.00448511794537918,-0.0339738896643499,
0.0788149225091984));
#104520=CARTESIAN_POINT('Ctrl Pts',(0.00442158246119149,-0.0338644633294062,
0.0787639420131593));
#104521=CARTESIAN_POINT('Ctrl Pts',(0.00472653643312723,-0.034193496108874,
0.0788906635692014));
#104522=CARTESIAN_POINT('Ctrl Pts',(0.00466116548981741,-0.0340836138581106,
0.0788438175619403));
#104523=CARTESIAN_POINT('Ctrl Pts',(0.00459679529253913,-0.0339738896643499,
0.0787956413177693));
#104524=CARTESIAN_POINT('Ctrl Pts',(0.0045335040938477,-0.0338644633294062,
0.0787462020190624));
#104525=CARTESIAN_POINT('Ctrl Pts',(0.0048376292234794,-0.034193496108874,
0.0788683129276277));
#104526=CARTESIAN_POINT('Ctrl Pts',(0.00477256648228136,-0.0340836138581106,
0.078822998824159));
#104527=CARTESIAN_POINT('Ctrl Pts',(0.00470847263969908,-0.0339738896643499,
0.0787763601263402));
#104528=CARTESIAN_POINT('Ctrl Pts',(0.00464542572650392,-0.0338644633294062,
0.0787284620249655));
#104529=CARTESIAN_POINT('Origin',(0.013980649207717,-0.0345610621862729,
0.064853649022503));
#104530=CARTESIAN_POINT('Ctrl Pts',(0.00486538773251886,-0.03424362768739,
0.0788893027482109));
#104531=CARTESIAN_POINT('Ctrl Pts',(0.00468664198271262,-0.033943005420186,
0.0787664103752259));
#104532=CARTESIAN_POINT('Ctrl Pts',(0.00451766078791165,-0.0336441434784162,
0.0786304032643261));
#104533=CARTESIAN_POINT('Ctrl Pts',(0.00507442535262118,-0.03424362768739,
0.0790264277764952));
#104534=CARTESIAN_POINT('Ctrl Pts',(0.00489050784711583,-0.033943005420186,
0.0789114193873213));
#104535=CARTESIAN_POINT('Ctrl Pts',(0.00471577573506724,-0.0336441434784162,
0.0787828843048311));
#104536=CARTESIAN_POINT('Ctrl Pts',(0.00464544788448532,-0.0335235895815127,
0.0787284786998444));
#104537=CARTESIAN_POINT('Ctrl Pts',(0.00458241611098779,-0.0334144449262719,
0.0786805925798768));
#104538=CARTESIAN_POINT('Ctrl Pts',(0.00452030121281923,-0.0333049234473133,
0.0786313492555552));
#104539=CARTESIAN_POINT('Ctrl Pts',(0.0044591883196958,-0.0331951640388588,
0.0785808044992326));
#104540=CARTESIAN_POINT('Ctrl Pts',(0.00465836273828975,-0.0335235895815127,
0.0788410592445124));
#104541=CARTESIAN_POINT('Ctrl Pts',(0.00459378107194419,-0.0334144449262719,
0.0787933509229345));
#104542=CARTESIAN_POINT('Ctrl Pts',(0.00453011082710756,-0.0333049234473133,
0.0787442535816515));
#104543=CARTESIAN_POINT('Ctrl Pts',(0.00446743910539777,-0.0331951640388588,
0.078693822626194));
#104544=CARTESIAN_POINT('Ctrl Pts',(0.00467127759209418,-0.0335235895815127,
0.0789536397891805));
#104545=CARTESIAN_POINT('Ctrl Pts',(0.00460514603290059,-0.0334144449262719,
0.0789061092659922));
#104546=CARTESIAN_POINT('Ctrl Pts',(0.00453992044139589,-0.0333049234473133,
0.0788571579077478));
#104547=CARTESIAN_POINT('Ctrl Pts',(0.00447568989109973,-0.0331951640388588,
0.0788068407531553));
#104548=CARTESIAN_POINT('Ctrl Pts',(0.0046841924458986,-0.0335235895815127,
0.0790662203338486));
#104549=CARTESIAN_POINT('Ctrl Pts',(0.00461651099385698,-0.0334144449262719,
0.0790188676090499));
#104550=CARTESIAN_POINT('Ctrl Pts',(0.00454973005568423,-0.0333049234473133,
0.0789700622338442));
#104551=CARTESIAN_POINT('Ctrl Pts',(0.0044839406768017,-0.0331951640388588,
0.0789198588801167));
#104552=CARTESIAN_POINT('Origin',(0.0156570923110334,-0.0326434571772002,
0.066235854630734));
#104553=CARTESIAN_POINT('Ctrl Pts',(0.00420900849951589,-0.0336938721132456,
0.0786989303646591));
#104554=CARTESIAN_POINT('Ctrl Pts',(0.0041823821005945,-0.0336474569764991,
0.0786760158951693));
#104555=CARTESIAN_POINT('Ctrl Pts',(0.00415602576892811,-0.033601104548885,
0.0786527913001756));
#104556=CARTESIAN_POINT('Ctrl Pts',(0.00408929759972816,-0.03348375086432,
0.0785939919678578));
#104557=CARTESIAN_POINT('Ctrl Pts',(0.00402434107867253,-0.0333660264760483,
0.0785332411619524));
#104558=CARTESIAN_POINT('Ctrl Pts',(0.00454583887293969,-0.0336938721132456,
0.0786529375520499));
#104559=CARTESIAN_POINT('Ctrl Pts',(0.00451948168521255,-0.0336474569764991,
0.078631994662508));
#104560=CARTESIAN_POINT('Ctrl Pts',(0.00449337146646129,-0.033601104548885,
0.0786107446638254));
#104561=CARTESIAN_POINT('Ctrl Pts',(0.00442726639855065,-0.03348375086432,
0.0785569445551631));
#104562=CARTESIAN_POINT('Ctrl Pts',(0.00436278456780856,-0.0333660264760482,
0.0785012092414052));
#104563=CARTESIAN_POINT('Ctrl Pts',(0.00454583887294235,-0.0336938721132427,
0.078652937552054));
#104564=CARTESIAN_POINT('Ctrl Pts',(0.00451948168521891,-0.0336474569765026,
0.0786319946625149));
#104565=CARTESIAN_POINT('Ctrl Pts',(0.00449337146647129,-0.0336011045488949,
0.0786107446638354));
#104566=CARTESIAN_POINT('Ctrl Pts',(0.00442781696373628,-0.0334847282606778,
0.0785573926367984));
#104567=CARTESIAN_POINT('Ctrl Pts',(0.00436385854011419,-0.0333679869945434,
0.0785021373052407));
#104568=CARTESIAN_POINT('Ctrl Pts',(0.00454583887293804,-0.0336938721132427,
0.0786529375520486));
#104569=CARTESIAN_POINT('Ctrl Pts',(0.004451573905417,-0.0335278710435084,
0.0785780365109017));
#104570=CARTESIAN_POINT('Ctrl Pts',(0.00435969097726898,-0.033362046922432,
0.0785002056948942));
#104571=CARTESIAN_POINT('Ctrl Pts',(0.00427015733847117,-0.0331951640388602,
0.0784193911134637));
#104572=CARTESIAN_POINT('Ctrl Pts',(0.00461259288962409,-0.0336938721132427,
0.0787036517618872));
#104573=CARTESIAN_POINT('Ctrl Pts',(0.00451726626550933,-0.0335278710435084,
0.0786301481563348));
#104574=CARTESIAN_POINT('Ctrl Pts',(0.00442427823103898,-0.033362046922432,
0.0785536809910323));
#104575=CARTESIAN_POINT('Ctrl Pts',(0.00433359525977046,-0.0331951640388602,
0.0784741967697822));
#104576=CARTESIAN_POINT('Ctrl Pts',(0.00467934690631015,-0.0336938721132427,
0.0787543659717258));
#104577=CARTESIAN_POINT('Ctrl Pts',(0.00458295862560166,-0.0335278710435084,
0.0786822598017678));
#104578=CARTESIAN_POINT('Ctrl Pts',(0.00448886548480899,-0.033362046922432,
0.0786071562871705));
#104579=CARTESIAN_POINT('Ctrl Pts',(0.00439703318106975,-0.0331951640388602,
0.0785290024261008));
#104580=CARTESIAN_POINT('Ctrl Pts',(0.0047461009229962,-0.0336938721132427,
0.0788050801815644));
#104581=CARTESIAN_POINT('Ctrl Pts',(0.00464865098569399,-0.0335278710435084,
0.0787343714472009));
#104582=CARTESIAN_POINT('Ctrl Pts',(0.004553452738579,-0.033362046922432,
0.0786606315833087));
#104583=CARTESIAN_POINT('Ctrl Pts',(0.00446047110236904,-0.0331951640388602,
0.0785838080824193));
#104584=CARTESIAN_POINT('Ctrl Pts',(0.0043648272482345,-0.0330240426238156,
0.0785010387842859));
#104585=CARTESIAN_POINT('Ctrl Pts',(0.00430488744996958,-0.0329142774063509,
0.0784492555177482));
#104586=CARTESIAN_POINT('Ctrl Pts',(0.00424598827429796,-0.0328043479726686,
0.0783962073122998));
#104587=CARTESIAN_POINT('Ctrl Pts',(0.00418820704702087,-0.0326943950436594,
0.0783419600486467));
#104588=CARTESIAN_POINT('Ctrl Pts',(0.0043706476364913,-0.0330240426238156,
0.0786142079455682));
#104589=CARTESIAN_POINT('Ctrl Pts',(0.00430914882277435,-0.0329142774063509,
0.0785625048605493));
#104590=CARTESIAN_POINT('Ctrl Pts',(0.00424868819684867,-0.0328043479726686,
0.0785095046473889));
#104591=CARTESIAN_POINT('Ctrl Pts',(0.00418934508315637,-0.0326943950436594,
0.0784552730702223));
#104592=CARTESIAN_POINT('Ctrl Pts',(0.0043764680247481,-0.0330240426238156,
0.0787273771068507));
#104593=CARTESIAN_POINT('Ctrl Pts',(0.00431341019557912,-0.0329142774063509,
0.0786757542033505));
#104594=CARTESIAN_POINT('Ctrl Pts',(0.00425138811939938,-0.0328043479726686,
0.0786228019824779));
#104595=CARTESIAN_POINT('Ctrl Pts',(0.00419048311929187,-0.0326943950436594,
0.0785685860917978));
#104596=CARTESIAN_POINT('Ctrl Pts',(0.0043822884130049,-0.0330240426238156,
0.078840546268133));
#104597=CARTESIAN_POINT('Ctrl Pts',(0.00431767156838389,-0.0329142774063509,
0.0787890035461516));
#104598=CARTESIAN_POINT('Ctrl Pts',(0.00425408804195009,-0.0328043479726686,
0.0787360993175669));
#104599=CARTESIAN_POINT('Ctrl Pts',(0.00419162115542737,-0.0326943950436594,
0.0786818991133733));
#104600=CARTESIAN_POINT('Origin',(0.0157403386267391,-0.0326396682855912,
0.0661443917975717));
#104601=CARTESIAN_POINT('Ctrl Pts',(0.00393312589888615,-0.0331951640388588,
0.0784439957875769));
#104602=CARTESIAN_POINT('Ctrl Pts',(0.00387398479359502,-0.0330855618255041,
0.0783862779747526));
#104603=CARTESIAN_POINT('Ctrl Pts',(0.00381599398283876,-0.0329757224427708,
0.0783272962084107));
#104604=CARTESIAN_POINT('Ctrl Pts',(0.00375923143222123,-0.0328657862078596,
0.0782671223756007));
#104605=CARTESIAN_POINT('Ctrl Pts',(0.00404614393586861,-0.0331951640388588,
0.0784357450084437));
#104606=CARTESIAN_POINT('Ctrl Pts',(0.00398711646836885,-0.0330855618255041,
0.0783795837904453));
#104607=CARTESIAN_POINT('Ctrl Pts',(0.00392920720516958,-0.0329757224427708,
0.0783221620897555));
#104608=CARTESIAN_POINT('Ctrl Pts',(0.00387249390945392,-0.0328657862078596,
0.0782635498007886));
#104609=CARTESIAN_POINT('Ctrl Pts',(0.00415916197285108,-0.0331951640388588,
0.0784274942293106));
#104610=CARTESIAN_POINT('Ctrl Pts',(0.00410024814314268,-0.0330855618255042,
0.0783728896061379));
#104611=CARTESIAN_POINT('Ctrl Pts',(0.0040424204275004,-0.0329757224427708,
0.0783170279711003));
#104612=CARTESIAN_POINT('Ctrl Pts',(0.00398575638668661,-0.0328657862078596,
0.0782599772259765));
#104613=CARTESIAN_POINT('Ctrl Pts',(0.00427218000983354,-0.0331951640388588,
0.0784192434501774));
#104614=CARTESIAN_POINT('Ctrl Pts',(0.00421337981791651,-0.0330855618255042,
0.0783661954218306));
#104615=CARTESIAN_POINT('Ctrl Pts',(0.00415563364983122,-0.0329757224427708,
0.0783118938524451));
#104616=CARTESIAN_POINT('Ctrl Pts',(0.0040990188639193,-0.0328657862078596,
0.0782564046511645));
#104617=CARTESIAN_POINT('Origin',(0.0160610598854413,-0.032640190883307,
0.0665027362489383));
#104618=CARTESIAN_POINT('Ctrl Pts',(0.00429703490787385,-0.0332451089994433,
0.0784434985984568));
#104619=CARTESIAN_POINT('Ctrl Pts',(0.00413510295888785,-0.0329451141710258,
0.0782991704632625));
#104620=CARTESIAN_POINT('Ctrl Pts',(0.00398450242663942,-0.0326442513127502,
0.0781430549726871));
#104621=CARTESIAN_POINT('Ctrl Pts',(0.00448723583637103,-0.0332451089994433,
0.0786057441124127));
#104622=CARTESIAN_POINT('Ctrl Pts',(0.004319184697711,-0.0329451141710258,
0.078468589522602));
#104623=CARTESIAN_POINT('Ctrl Pts',(0.00416194201899661,-0.0326442513127502,
0.0783191662757433));
#104624=CARTESIAN_POINT('Ctrl Pts',(0.00409904136003693,-0.0325229783203385,
0.0782564268255897));
#104625=CARTESIAN_POINT('Ctrl Pts',(0.00404243435707815,-0.032413025311208,
0.0782009458622309));
#104626=CARTESIAN_POINT('Ctrl Pts',(0.00398698363465686,-0.0323031222247695,
0.0781443023250954));
#104627=CARTESIAN_POINT('Ctrl Pts',(0.0039327576609294,-0.0321934096636184,
0.0780865712768841));
#104628=CARTESIAN_POINT('Ctrl Pts',(0.00409774433046492,-0.0325229783203385,
0.0783697381681987));
#104629=CARTESIAN_POINT('Ctrl Pts',(0.00403957533315467,-0.032413025311208,
0.078314239325316));
#104630=CARTESIAN_POINT('Ctrl Pts',(0.00398256322314985,-0.0323031222247695,
0.0782575455995092));
#104631=CARTESIAN_POINT('Ctrl Pts',(0.00392677846636474,-0.0321934096636184,
0.0781997321883418));
#104632=CARTESIAN_POINT('Ctrl Pts',(0.00409644730089292,-0.0325229783203385,
0.0784830495108077));
#104633=CARTESIAN_POINT('Ctrl Pts',(0.00403671630923118,-0.032413025311208,
0.078427532788401));
#104634=CARTESIAN_POINT('Ctrl Pts',(0.00397814281164285,-0.0323031222247695,
0.078370788873923));
#104635=CARTESIAN_POINT('Ctrl Pts',(0.00392079927180007,-0.0321934096636184,
0.0783128930997994));
#104636=CARTESIAN_POINT('Ctrl Pts',(0.00409515027132091,-0.0325229783203385,
0.0785963608534167));
#104637=CARTESIAN_POINT('Ctrl Pts',(0.0040338572853077,-0.032413025311208,
0.078540826251486));
#104638=CARTESIAN_POINT('Ctrl Pts',(0.00397372240013584,-0.0323031222247695,
0.0784840321483367));
#104639=CARTESIAN_POINT('Ctrl Pts',(0.0039148200772354,-0.0321934096636184,
0.0784260540112571));
#104640=CARTESIAN_POINT('Origin',(0.0157342914279694,-0.0326393375177525,
0.0661504019901444));
#104641=CARTESIAN_POINT('Ctrl Pts',(0.00367177297545991,-0.0326943950436594,
0.0781723890818772));
#104642=CARTESIAN_POINT('Ctrl Pts',(0.00361633691515119,-0.0325844576448127,
0.0781110320509036));
#104643=CARTESIAN_POINT('Ctrl Pts',(0.00356216589554312,-0.0324744968375319,
0.0780485241689818));
#104644=CARTESIAN_POINT('Ctrl Pts',(0.00350932821904061,-0.0323646534831894,
0.0779849464821874));
#104645=CARTESIAN_POINT('Ctrl Pts',(0.00378508595995979,-0.0326943950436594,
0.078171251046114));
#104646=CARTESIAN_POINT('Ctrl Pts',(0.0037296655839168,-0.0325844576448127,
0.078111455680438));
#104647=CARTESIAN_POINT('Ctrl Pts',(0.00367547795188571,-0.0324744968375319,
0.0780505098987116));
#104648=CARTESIAN_POINT('Ctrl Pts',(0.00362259141516232,-0.0323646534831894,
0.0779884927458501));
#104649=CARTESIAN_POINT('Ctrl Pts',(0.00389839894445967,-0.0326943950436594,
0.0781701130103508));
#104650=CARTESIAN_POINT('Ctrl Pts',(0.0038429942526824,-0.0325844576448127,
0.0781118793099724));
#104651=CARTESIAN_POINT('Ctrl Pts',(0.0037887900082283,-0.0324744968375319,
0.0780524956284414));
#104652=CARTESIAN_POINT('Ctrl Pts',(0.00373585461128402,-0.0323646534831894,
0.0779920390095128));
#104653=CARTESIAN_POINT('Ctrl Pts',(0.00401171192895955,-0.0326943950436594,
0.0781689749745877));
#104654=CARTESIAN_POINT('Ctrl Pts',(0.00395632292144801,-0.0325844576448127,
0.0781123029395069));
#104655=CARTESIAN_POINT('Ctrl Pts',(0.00390210206457089,-0.0324744968375319,
0.0780544813581712));
#104656=CARTESIAN_POINT('Ctrl Pts',(0.00384911780740573,-0.0323646534831894,
0.0779955852731756));
#104657=CARTESIAN_POINT('Origin',(0.0160879912199795,-0.032639557906681,
0.0664761530758608));
#104658=CARTESIAN_POINT('Ctrl Pts',(0.00403502269649379,-0.0327445246961875,
0.0781947707943522));
#104659=CARTESIAN_POINT('Ctrl Pts',(0.00388247167370257,-0.0324436878365474,
0.0780405607105505));
#104660=CARTESIAN_POINT('Ctrl Pts',(0.00374196976590213,-0.0321434074463187,
0.0778752979548999));
#104661=CARTESIAN_POINT('Ctrl Pts',(0.00421466201254181,-0.0327445246961875,
0.0783686377438561));
#104662=CARTESIAN_POINT('Ctrl Pts',(0.00405555349061777,-0.0324436878365474,
0.0782212028675482));
#104663=CARTESIAN_POINT('Ctrl Pts',(0.00390800237653284,-0.0321434074463187,
0.0780622021341126));
#104664=CARTESIAN_POINT('Ctrl Pts',(0.00378544379441447,-0.0322357242816073,
0.0779258369851489));
#104665=CARTESIAN_POINT('Ctrl Pts',(0.00366518828351864,-0.0319819883628706,
0.0777876665337693));
#104666=CARTESIAN_POINT('Ctrl Pts',(0.00355396866642955,-0.0317295851069886,
0.0776421238997756));
#104667=CARTESIAN_POINT('Ctrl Pts',(0.00395363164487792,-0.0322357242816073,
0.078110804136169));
#104668=CARTESIAN_POINT('Ctrl Pts',(0.0038274851701157,-0.0319819883628706,
0.077977990249695));
#104669=CARTESIAN_POINT('Ctrl Pts',(0.00371004567438076,-0.0317295851069886,
0.07783741846598));
#104670=CARTESIAN_POINT('Origin',(0.0160181918719063,-0.0326371942646663,
0.0665410410921116));
#104671=CARTESIAN_POINT('Origin',(0.015647607112183,-0.0326352985530941,
0.0662372906110294));
#104672=CARTESIAN_POINT('Ctrl Pts',(0.00342799009848551,-0.0321934096636183,
0.0778849078441259));
#104673=CARTESIAN_POINT('Ctrl Pts',(0.00337648280850493,-0.0320835708272304,
0.0778201492114634));
#104674=CARTESIAN_POINT('Ctrl Pts',(0.00332634557138288,-0.0319739230346346,
0.0777543622007505));
#104675=CARTESIAN_POINT('Ctrl Pts',(0.00327763607442989,-0.0318646057455576,
0.0776876359050153));
#104676=CARTESIAN_POINT('Ctrl Pts',(0.00354115110738701,-0.0321934096636183,
0.0778908870438393));
#104677=CARTESIAN_POINT('Ctrl Pts',(0.00348956135958248,-0.0320835708272304,
0.0778276889896818));
#104678=CARTESIAN_POINT('Ctrl Pts',(0.00343930941637432,-0.0319739230346346,
0.0777634599458147));
#104679=CARTESIAN_POINT('Ctrl Pts',(0.00339045326481254,-0.0318646057455576,
0.0776982870232187));
#104680=CARTESIAN_POINT('Ctrl Pts',(0.00365431211628852,-0.0321934096636183,
0.0778968662435527));
#104681=CARTESIAN_POINT('Ctrl Pts',(0.00360263991066004,-0.0320835708272304,
0.0778352287679003));
#104682=CARTESIAN_POINT('Ctrl Pts',(0.00355227326136576,-0.0319739230346346,
0.0777725576908789));
#104683=CARTESIAN_POINT('Ctrl Pts',(0.0035032704551952,-0.0318646057455576,
0.0777089381414222));
#104684=CARTESIAN_POINT('Ctrl Pts',(0.00376747312519003,-0.0321934096636183,
0.0779028454432661));
#104685=CARTESIAN_POINT('Ctrl Pts',(0.00371571846173759,-0.0320835708272304,
0.0778427685461188));
#104686=CARTESIAN_POINT('Ctrl Pts',(0.0036652371063572,-0.0319739230346346,
0.0777816554359431));
#104687=CARTESIAN_POINT('Ctrl Pts',(0.00361608764557785,-0.0318646057455576,
0.0777195892596256));
#104688=CARTESIAN_POINT('Ctrl Pts',(0.00384881685085818,-0.0320218834582387,
0.0779964878945564));
#104689=CARTESIAN_POINT('Ctrl Pts',(0.00380878421069954,-0.0319391099350659,
0.0779519958400047));
#104690=CARTESIAN_POINT('Ctrl Pts',(0.00376947057497083,-0.0318564869454916,
0.0779069056267691));
#104691=CARTESIAN_POINT('Ctrl Pts',(0.00373090151239011,-0.0317740741446485,
0.0778612527703433));
#104692=CARTESIAN_POINT('Ctrl Pts',(0.00384513550296807,-0.0320218834582387,
0.0780459173971374));
#104693=CARTESIAN_POINT('Ctrl Pts',(0.0038045884211826,-0.0319391099350659,
0.0780013870286538));
#104694=CARTESIAN_POINT('Ctrl Pts',(0.00376476125379159,-0.0318564869454916,
0.0779562504916215));
#104695=CARTESIAN_POINT('Ctrl Pts',(0.00372567994040288,-0.0317740741446485,
0.0779105433701943));
#104696=CARTESIAN_POINT('Ctrl Pts',(0.00384145415507796,-0.0320218834582387,
0.0780953468997184));
#104697=CARTESIAN_POINT('Ctrl Pts',(0.00380039263166567,-0.0319391099350659,
0.0780507782173028));
#104698=CARTESIAN_POINT('Ctrl Pts',(0.00376005193261236,-0.0318564869454916,
0.078005595356474));
#104699=CARTESIAN_POINT('Ctrl Pts',(0.00372045836841565,-0.0317740741446485,
0.0779598339700454));
#104700=CARTESIAN_POINT('Ctrl Pts',(0.00383777280718785,-0.0320218834582387,
0.0781447764022994));
#104701=CARTESIAN_POINT('Ctrl Pts',(0.00379619684214873,-0.0319391099350659,
0.0781001694059519));
#104702=CARTESIAN_POINT('Ctrl Pts',(0.00375534261143313,-0.0318564869454916,
0.0780549402213264));
#104703=CARTESIAN_POINT('Ctrl Pts',(0.00371523679642842,-0.0317740741446485,
0.0780091245698964));
#104704=CARTESIAN_POINT('Origin',(-0.00019750424675882,-0.0391228853390767,
0.0829042452738927));
#104705=CARTESIAN_POINT('Ctrl Pts',(0.00640200741755438,-0.0352722978779667,
0.0796381377683931));
#104706=CARTESIAN_POINT('Ctrl Pts',(0.00638408492046634,-0.0352466642097265,
0.0796321480458426));
#104707=CARTESIAN_POINT('Ctrl Pts',(0.00636615353960843,-0.0352210183808325,
0.079626238017773));
#104708=CARTESIAN_POINT('Ctrl Pts',(0.00634821247550811,-0.0351953608940152,
0.0796204079813843));
#104709=CARTESIAN_POINT('Origin',(0.00467811982047751,-0.0352456003065129,
0.0842248527964227));
#104710=CARTESIAN_POINT('Ctrl Pts',(0.00623051831428444,-0.035024121149334,
0.0795792570417599));
#104711=CARTESIAN_POINT('Ctrl Pts',(0.00615573252798837,-0.0349144232867421,
0.0795531781092734));
#104712=CARTESIAN_POINT('Ctrl Pts',(0.00608144104894163,-0.0348045283677512,
0.0795255376917175));
#104713=CARTESIAN_POINT('Ctrl Pts',(0.00600774035254011,-0.0346945769586886,
0.0794963676519038));
#104714=CARTESIAN_POINT('Ctrl Pts',(0.00627759032942455,-0.035024121149334,
0.0796823364635382));
#104715=CARTESIAN_POINT('Ctrl Pts',(0.00620138466642172,-0.0349144232867421,
0.0796569059287308));
#104716=CARTESIAN_POINT('Ctrl Pts',(0.00612565905796086,-0.0348045283677512,
0.0796298849470864));
#104717=CARTESIAN_POINT('Ctrl Pts',(0.0060505117868503,-0.0346945769586886,
0.0796013045196413));
#104718=CARTESIAN_POINT('Ctrl Pts',(0.00632466234456467,-0.035024121149334,
0.0797854158853166));
#104719=CARTESIAN_POINT('Ctrl Pts',(0.00624703680485506,-0.0349144232867421,
0.0797606337481882));
#104720=CARTESIAN_POINT('Ctrl Pts',(0.00616987706698009,-0.0348045283677512,
0.0797342322024552));
#104721=CARTESIAN_POINT('Ctrl Pts',(0.0060932832211605,-0.0346945769586886,
0.0797062413873788));
#104722=CARTESIAN_POINT('Ctrl Pts',(0.00637173435970478,-0.035024121149334,
0.0798884953070949));
#104723=CARTESIAN_POINT('Ctrl Pts',(0.00629268894328841,-0.0349144232867421,
0.0798643615676456));
#104724=CARTESIAN_POINT('Ctrl Pts',(0.00621409507599933,-0.0348045283677512,
0.0798385794578241));
#104725=CARTESIAN_POINT('Ctrl Pts',(0.00613605465547069,-0.0346945769586886,
0.0798111782551163));
#104726=CARTESIAN_POINT('Origin',(0.0123533304663821,-0.0345629067941944,
0.0639529949421231));
#104727=CARTESIAN_POINT('Ctrl Pts',(0.00589298787791728,-0.0351970973651596,
0.0796453688229808));
#104728=CARTESIAN_POINT('Ctrl Pts',(0.00581685699041973,-0.0350869349321778,
0.079614464191006));
#104729=CARTESIAN_POINT('Ctrl Pts',(0.00574130552715329,-0.0349764985129753,
0.0795819512390321));
#104730=CARTESIAN_POINT('Ctrl Pts',(0.00566643384677454,-0.0348659306849698,
0.0795478663268045));
#104731=CARTESIAN_POINT('Ctrl Pts',(0.00596702049102428,-0.0351970973651596,
0.0796095967270538));
#104732=CARTESIAN_POINT('Ctrl Pts',(0.00589138517743602,-0.0350869349321778,
0.0795797177166016));
#104733=CARTESIAN_POINT('Ctrl Pts',(0.00581630837650343,-0.0349764985129753,
0.0795482415384702));
#104734=CARTESIAN_POINT('Ctrl Pts',(0.00574188975287722,-0.0348659306849698,
0.0795152032454328));
#104735=CARTESIAN_POINT('Ctrl Pts',(0.00604105310413129,-0.0351970973651596,
0.0795738246311267));
#104736=CARTESIAN_POINT('Ctrl Pts',(0.0059659133644523,-0.0350869349321778,
0.0795449712421971));
#104737=CARTESIAN_POINT('Ctrl Pts',(0.00589131122585358,-0.0349764985129753,
0.0795145318379082));
#104738=CARTESIAN_POINT('Ctrl Pts',(0.0058173456589799,-0.0348659306849698,
0.0794825401640612));
#104739=CARTESIAN_POINT('Ctrl Pts',(0.00611508571723829,-0.0351970973651596,
0.0795380525351997));
#104740=CARTESIAN_POINT('Ctrl Pts',(0.00604044155146859,-0.0350869349321778,
0.0795102247677927));
#104741=CARTESIAN_POINT('Ctrl Pts',(0.00596631407520372,-0.0349764985129753,
0.0794808221373463));
#104742=CARTESIAN_POINT('Ctrl Pts',(0.00589280156508258,-0.0348659306849698,
0.0794498770826896));
#104743=CARTESIAN_POINT('Origin',(0.0127781825806878,-0.0345637187966566,
0.0641784412489904));
#104744=CARTESIAN_POINT('Ctrl Pts',(0.00614629913616949,-0.0352450361861252,
0.0795507115975138));
#104745=CARTESIAN_POINT('Ctrl Pts',(0.00594260796109335,-0.0349452761023764,
0.0794761296021067));
#104746=CARTESIAN_POINT('Ctrl Pts',(0.00574511327208869,-0.0346444289983475,
0.0793864166339374));
#104747=CARTESIAN_POINT('Ctrl Pts',(0.00638286995954464,-0.0352450361861252,
0.079631546277742));
#104748=CARTESIAN_POINT('Ctrl Pts',(0.00617613005455479,-0.0349452761023764,
0.079565886697119));
#104749=CARTESIAN_POINT('Ctrl Pts',(0.0059749232239849,-0.0346444289983475,
0.0794848411532883));
#104750=CARTESIAN_POINT('Ctrl Pts',(0.00589334924320917,-0.0345231616327822,
0.0794496650478157));
#104751=CARTESIAN_POINT('Ctrl Pts',(0.00582030082185705,-0.0344132092796975,
0.0794189216698));
#104752=CARTESIAN_POINT('Ctrl Pts',(0.0057478920719919,-0.0343032738558974,
0.0793866689290254));
#104753=CARTESIAN_POINT('Ctrl Pts',(0.00567621469917636,-0.0341934961088741,
0.0793529505211642));
#104754=CARTESIAN_POINT('Ctrl Pts',(0.00593385597004646,-0.0345231616327822,
0.0795554967123585));
#104755=CARTESIAN_POINT('Ctrl Pts',(0.0058593488081977,-0.0344132092796975,
0.0795253116625433));
#104756=CARTESIAN_POINT('Ctrl Pts',(0.00578546984452178,-0.0343032738558974,
0.0794935870482655));
#104757=CARTESIAN_POINT('Ctrl Pts',(0.00571231268542628,-0.0341934961088741,
0.0794603659368534));
#104758=CARTESIAN_POINT('Ctrl Pts',(0.00597436269688375,-0.0345231616327822,
0.0796613283769013));
#104759=CARTESIAN_POINT('Ctrl Pts',(0.00589839679453834,-0.0344132092796975,
0.0796317016552866));
#104760=CARTESIAN_POINT('Ctrl Pts',(0.00582304761705166,-0.0343032738558974,
0.0796005051675057));
#104761=CARTESIAN_POINT('Ctrl Pts',(0.0057484106716762,-0.0341934961088741,
0.0795677813525425));
#104762=CARTESIAN_POINT('Ctrl Pts',(0.00601486942372104,-0.0345231616327822,
0.0797671600414441));
#104763=CARTESIAN_POINT('Ctrl Pts',(0.00593744478087899,-0.0344132092796975,
0.07973809164803));
#104764=CARTESIAN_POINT('Ctrl Pts',(0.00586062538958153,-0.0343032738558974,
0.0797074232867459));
#104765=CARTESIAN_POINT('Ctrl Pts',(0.00578450865792613,-0.0341934961088741,
0.0796751967682317));
#104766=CARTESIAN_POINT('Origin',(0.0123577353792793,-0.0345625596231457,
0.0639417212994246));
#104767=CARTESIAN_POINT('Ctrl Pts',(0.00546514888907037,-0.0346945769586886,
0.079528816687218));
#104768=CARTESIAN_POINT('Ctrl Pts',(0.00539102607640815,-0.0345846629176052,
0.0794921793764874));
#104769=CARTESIAN_POINT('Ctrl Pts',(0.00531764824792714,-0.0344746925050311,
0.0794540029786887));
#104770=CARTESIAN_POINT('Ctrl Pts',(0.00524510922174087,-0.0343648066253259,
0.0794143367981118));
#104771=CARTESIAN_POINT('Ctrl Pts',(0.0055700856741824,-0.0346945769586886,
0.0794860452865853));
#104772=CARTESIAN_POINT('Ctrl Pts',(0.00549655227303962,-0.0345846629176052,
0.0794508540577936));
#104773=CARTESIAN_POINT('Ctrl Pts',(0.00542373405237037,-0.0344746925050311,
0.0794141361777164));
#104774=CARTESIAN_POINT('Ctrl Pts',(0.0053517241209721,-0.0343648066253259,
0.0793759390788612));
#104775=CARTESIAN_POINT('Ctrl Pts',(0.00567502245929443,-0.0346945769586886,
0.0794432738859526));
#104776=CARTESIAN_POINT('Ctrl Pts',(0.00560207846967109,-0.0345846629176052,
0.0794095287390998));
#104777=CARTESIAN_POINT('Ctrl Pts',(0.00552981985681359,-0.0344746925050311,
0.079374269376744));
#104778=CARTESIAN_POINT('Ctrl Pts',(0.00545833902020333,-0.0343648066253259,
0.0793375413596106));
#104779=CARTESIAN_POINT('Ctrl Pts',(0.00577995924440646,-0.0346945769586886,
0.0794005024853199));
#104780=CARTESIAN_POINT('Ctrl Pts',(0.00570760466630256,-0.0345846629176052,
0.0793682034204061));
#104781=CARTESIAN_POINT('Ctrl Pts',(0.00563590566125681,-0.0344746925050311,
0.0793344025757717));
#104782=CARTESIAN_POINT('Ctrl Pts',(0.00556495391943456,-0.0343648066253259,
0.07929914364036));
#104783=CARTESIAN_POINT('Origin',(0.0128021887384452,-0.0345626446730568,
0.0641251699148011));
#104784=CARTESIAN_POINT('Ctrl Pts',(0.00577808157344143,-0.0346945769586885,
0.0794012678091005));
#104785=CARTESIAN_POINT('Ctrl Pts',(0.00566809166668867,-0.0345275153362891,
0.0793521361704551));
#104786=CARTESIAN_POINT('Ctrl Pts',(0.00555961845572507,-0.0343603235965159,
0.0792995327425228));
#104787=CARTESIAN_POINT('Ctrl Pts',(0.00545298044386904,-0.034193496108874,
0.0792436178710481));
#104788=CARTESIAN_POINT('Ctrl Pts',(0.00585535049286178,-0.0346945769586885,
0.0794337876864509));
#104789=CARTESIAN_POINT('Ctrl Pts',(0.00574467944425767,-0.0345275153362891,
0.0793862744762595));
#104790=CARTESIAN_POINT('Ctrl Pts',(0.00563547401717934,-0.0343603235965159,
0.0793352684741054));
#104791=CARTESIAN_POINT('Ctrl Pts',(0.00552805495073345,-0.034193496108874,
0.0792809253334429));
#104792=CARTESIAN_POINT('Ctrl Pts',(0.00593261941228212,-0.0346945769586885,
0.0794663075638013));
#104793=CARTESIAN_POINT('Ctrl Pts',(0.00582126722182666,-0.0345275153362891,
0.0794204127820639));
#104794=CARTESIAN_POINT('Ctrl Pts',(0.00571132957863361,-0.0343603235965159,
0.079371004205688));
#104795=CARTESIAN_POINT('Ctrl Pts',(0.00560312945759786,-0.034193496108874,
0.0793182327958377));
#104796=CARTESIAN_POINT('Ctrl Pts',(0.00600988833170246,-0.0346945769586885,
0.0794988274411517));
#104797=CARTESIAN_POINT('Ctrl Pts',(0.00589785499939566,-0.0345275153362891,
0.0794545510878683));
#104798=CARTESIAN_POINT('Ctrl Pts',(0.00578718514008788,-0.0343603235965159,
0.0794067399372707));
#104799=CARTESIAN_POINT('Ctrl Pts',(0.00567820396446227,-0.034193496108874,
0.0793555402582325));
#104800=CARTESIAN_POINT('Ctrl Pts',(0.0055649824247782,-0.0340223579322365,
0.0792991571840227));
#104801=CARTESIAN_POINT('Ctrl Pts',(0.00549396211764549,-0.0339125849573554,
0.0792638646615878));
#104802=CARTESIAN_POINT('Ctrl Pts',(0.00542372218886624,-0.0338030433565221,
0.0792271269834706));
#104803=CARTESIAN_POINT('Ctrl Pts',(0.00535434829877516,-0.0336938721132328,
0.0791889990935798));
#104804=CARTESIAN_POINT('Ctrl Pts',(0.00559876407046006,-0.0340223579322365,
0.0794073236309725));
#104805=CARTESIAN_POINT('Ctrl Pts',(0.005526251865914,-0.0339125849573554,
0.0793724970455378));
#104806=CARTESIAN_POINT('Ctrl Pts',(0.00545451144424721,-0.0338030433565221,
0.0793361940982024));
#104807=CARTESIAN_POINT('Ctrl Pts',(0.00538363043395429,-0.0336938721132328,
0.0792984693470282));
#104808=CARTESIAN_POINT('Ctrl Pts',(0.00563254571614192,-0.0340223579322365,
0.0795154900779222));
#104809=CARTESIAN_POINT('Ctrl Pts',(0.0055585416141825,-0.0339125849573554,
0.0794811294294877));
#104810=CARTESIAN_POINT('Ctrl Pts',(0.00548530069962818,-0.0338030433565221,
0.0794452612129342));
#104811=CARTESIAN_POINT('Ctrl Pts',(0.00541291256913342,-0.0336938721132328,
0.0794079396004766));
#104812=CARTESIAN_POINT('Ctrl Pts',(0.00566632736182378,-0.0340223579322365,
0.079623656524872));
#104813=CARTESIAN_POINT('Ctrl Pts',(0.00559083136245101,-0.0339125849573554,
0.0795897618134376));
#104814=CARTESIAN_POINT('Ctrl Pts',(0.00551608995500914,-0.0338030433565221,
0.079554328327666));
#104815=CARTESIAN_POINT('Ctrl Pts',(0.00544219470431255,-0.0336938721132328,
0.079517409853925));
#104816=CARTESIAN_POINT('Origin',(0.0123092934001533,-0.0345589643415753,
0.0640517497171613));
#104817=CARTESIAN_POINT('Ctrl Pts',(0.00513265640034567,-0.034193496108874,
0.079351265854761));
#104818=CARTESIAN_POINT('Ctrl Pts',(0.00506093402518955,-0.0340836138595105,
0.0793100200018787));
#104819=CARTESIAN_POINT('Ctrl Pts',(0.0049900995601459,-0.0339738896671456,
0.0792673097954907));
#104820=CARTESIAN_POINT('Ctrl Pts',(0.00492024000019863,-0.0338644633335883,
0.0792231959767272));
#104821=CARTESIAN_POINT('Ctrl Pts',(0.00524007191268345,-0.034193496108874,
0.0793151678360314));
#104822=CARTESIAN_POINT('Ctrl Pts',(0.00516884730782287,-0.0340836138595105,
0.0792754031794364));
#104823=CARTESIAN_POINT('Ctrl Pts',(0.00509847972398642,-0.0339738896671456,
0.0792341837589416));
#104824=CARTESIAN_POINT('Ctrl Pts',(0.00502905568651178,-0.0338644633335883,
0.0791915683675986));
#104825=CARTESIAN_POINT('Ctrl Pts',(0.00534748742502123,-0.034193496108874,
0.0792790698173018));
#104826=CARTESIAN_POINT('Ctrl Pts',(0.00527676059045619,-0.0340836138595105,
0.0792407863569941));
#104827=CARTESIAN_POINT('Ctrl Pts',(0.00520685988782694,-0.0339738896671456,
0.0792010577223924));
#104828=CARTESIAN_POINT('Ctrl Pts',(0.00513787137282492,-0.0338644633335883,
0.07915994075847));
#104829=CARTESIAN_POINT('Ctrl Pts',(0.00545490293735901,-0.034193496108874,
0.0792429717985722));
#104830=CARTESIAN_POINT('Ctrl Pts',(0.00538467387308951,-0.0340836138595105,
0.0792061695345518));
#104831=CARTESIAN_POINT('Ctrl Pts',(0.00531524005166745,-0.0339738896671456,
0.0791679316858433));
#104832=CARTESIAN_POINT('Ctrl Pts',(0.00524668705913807,-0.0338644633335883,
0.0791283131493414));
#104833=CARTESIAN_POINT('Origin',(0.0127693243339131,-0.0345610621862859,
0.0641928934445164));
#104834=CARTESIAN_POINT('Ctrl Pts',(0.00548507328434942,-0.0342436276873901,
0.079260317044454));
#104835=CARTESIAN_POINT('Ctrl Pts',(0.00529233449968253,-0.0339430054201861,
0.0791607964973451));
#104836=CARTESIAN_POINT('Ctrl Pts',(0.00510763956107794,-0.0336441434784162,
0.079047040802694));
#104837=CARTESIAN_POINT('Ctrl Pts',(0.00570964890357818,-0.0342436276873901,
0.0793701614400689));
#104838=CARTESIAN_POINT('Ctrl Pts',(0.00551276726923501,-0.0339430054201861,
0.079279110902069));
#104839=CARTESIAN_POINT('Ctrl Pts',(0.0053233032545649,-0.0336441434784162,
0.0791734890977064));
#104840=CARTESIAN_POINT('Ctrl Pts',(0.00524671112969369,-0.0335235895815127,
0.0791283269140882));
#104841=CARTESIAN_POINT('Ctrl Pts',(0.00517817465829848,-0.0334144449262719,
0.0790887183664692));
#104842=CARTESIAN_POINT('Ctrl Pts',(0.00511037772958611,-0.0333049234473133,
0.0790476484015081));
#104843=CARTESIAN_POINT('Ctrl Pts',(0.00504341179212886,-0.0331951640388588,
0.0790051616821937));
#104844=CARTESIAN_POINT('Ctrl Pts',(0.00527363422971817,-0.0335235895815127,
0.0792384010671475));
#104845=CARTESIAN_POINT('Ctrl Pts',(0.00520358237089006,-0.0334144449262719,
0.079199163169007));
#104846=CARTESIAN_POINT('Ctrl Pts',(0.00513426065640893,-0.0333049234473133,
0.0791584329725919));
#104847=CARTESIAN_POINT('Ctrl Pts',(0.00506576244522471,-0.0331951640388588,
0.0791162545298161));
#104848=CARTESIAN_POINT('Ctrl Pts',(0.00530055732974265,-0.0335235895815127,
0.0793484752202068));
#104849=CARTESIAN_POINT('Ctrl Pts',(0.00522899008348163,-0.0334144449262719,
0.0793096079715449));
#104850=CARTESIAN_POINT('Ctrl Pts',(0.00515814358323175,-0.0333049234473133,
0.0792692175436757));
#104851=CARTESIAN_POINT('Ctrl Pts',(0.00508811309832056,-0.0331951640388588,
0.0792273473774384));
#104852=CARTESIAN_POINT('Ctrl Pts',(0.00532748042976713,-0.0335235895815127,
0.0794585493732661));
#104853=CARTESIAN_POINT('Ctrl Pts',(0.0052543977960732,-0.0334144449262719,
0.0794200527740827));
#104854=CARTESIAN_POINT('Ctrl Pts',(0.00518202651005457,-0.0333049234473133,
0.0793800021147596));
#104855=CARTESIAN_POINT('Ctrl Pts',(0.00511046375141641,-0.0331951640388588,
0.0793384402250607));
#104856=CARTESIAN_POINT('Origin',(0.0146057844810557,-0.0326434571769772,
0.0653540859141867));
#104857=CARTESIAN_POINT('Ctrl Pts',(0.00481000981123756,-0.0336938721132456,
0.0791537119357245));
#104858=CARTESIAN_POINT('Ctrl Pts',(0.004780721424868,-0.0336474569764991,
0.0791343153263458));
#104859=CARTESIAN_POINT('Ctrl Pts',(0.00475166210716029,-0.033601104548885,
0.0791145771884932));
#104860=CARTESIAN_POINT('Ctrl Pts',(0.00467809059905453,-0.0334837508643202,
0.0790646047636889));
#104861=CARTESIAN_POINT('Ctrl Pts',(0.00460603218462337,-0.0333660264760487,
0.0790124742068587));
#104862=CARTESIAN_POINT('Ctrl Pts',(0.00513841974863563,-0.0336938721132456,
0.0790658657503163));
#104863=CARTESIAN_POINT('Ctrl Pts',(0.00510964555513977,-0.0336474569764991,
0.0790483914332793));
#104864=CARTESIAN_POINT('Ctrl Pts',(0.00508107789221398,-0.033601104548885,
0.0790305814753285));
#104865=CARTESIAN_POINT('Ctrl Pts',(0.00500875114092382,-0.0334837508643202,
0.0789854907585086));
#104866=CARTESIAN_POINT('Ctrl Pts',(0.00493779228158005,-0.0333660264760487,
0.0789382766507001));
#104867=CARTESIAN_POINT('Ctrl Pts',(0.00513841974863763,-0.0336938721132427,
0.0790658657503215));
#104868=CARTESIAN_POINT('Ctrl Pts',(0.00510964555514579,-0.0336474569765026,
0.0790483914332867));
#104869=CARTESIAN_POINT('Ctrl Pts',(0.00508107789222398,-0.0336011045488949,
0.0790305814753385));
#104870=CARTESIAN_POINT('Ctrl Pts',(0.00500935352425746,-0.0334847282606778,
0.0789858663027726));
#104871=CARTESIAN_POINT('Ctrl Pts',(0.00493897410253327,-0.0333679869945434,
0.0789390627920544));
#104872=CARTESIAN_POINT('Ctrl Pts',(0.00513841974863386,-0.0336938721132428,
0.0790658657503152));
#104873=CARTESIAN_POINT('Ctrl Pts',(0.00503551049885303,-0.0335278710435084,
0.0790033698594408));
#104874=CARTESIAN_POINT('Ctrl Pts',(0.00493459730719635,-0.033362046922432,
0.0789376687471586));
#104875=CARTESIAN_POINT('Ctrl Pts',(0.00483564091507303,-0.0331951640388601,
0.0788687129533042));
#104876=CARTESIAN_POINT('Ctrl Pts',(0.0052110035658666,-0.0336938721132428,
0.079107813566697));
#104877=CARTESIAN_POINT('Ctrl Pts',(0.00510721617609314,-0.0335278710435084,
0.0790468371530738));
#104878=CARTESIAN_POINT('Ctrl Pts',(0.00500537750295989,-0.033362046922432,
0.0789826274452524));
#104879=CARTESIAN_POINT('Ctrl Pts',(0.00490544757953888,-0.0331951640388601,
0.078915135570846));
#104880=CARTESIAN_POINT('Ctrl Pts',(0.00528358738309935,-0.0336938721132428,
0.0791497613830787));
#104881=CARTESIAN_POINT('Ctrl Pts',(0.00517892185333324,-0.0335278710435084,
0.0790903044467068));
#104882=CARTESIAN_POINT('Ctrl Pts',(0.00507615769872343,-0.033362046922432,
0.0790275861433462));
#104883=CARTESIAN_POINT('Ctrl Pts',(0.00497525424400473,-0.0331951640388601,
0.0789615581883877));
#104884=CARTESIAN_POINT('Ctrl Pts',(0.0053561712003321,-0.0336938721132428,
0.0791917091994605));
#104885=CARTESIAN_POINT('Ctrl Pts',(0.00525062753057335,-0.0335278710435084,
0.0791337717403398));
#104886=CARTESIAN_POINT('Ctrl Pts',(0.00514693789448697,-0.033362046922432,
0.07907254484144));
#104887=CARTESIAN_POINT('Ctrl Pts',(0.00504506090847058,-0.0331951640388601,
0.0790079808059295));
#104888=CARTESIAN_POINT('Ctrl Pts',(0.00493979749091848,-0.0330240426238156,
0.0789378515219431));
#104889=CARTESIAN_POINT('Ctrl Pts',(0.00487384017162634,-0.0329142774063509,
0.0788939890306646));
#104890=CARTESIAN_POINT('Ctrl Pts',(0.00480875673042359,-0.0328043479726686,
0.0788487411503022));
#104891=CARTESIAN_POINT('Ctrl Pts',(0.00474463214041636,-0.0326943950436594,
0.0788021635505798));
#104892=CARTESIAN_POINT('Ctrl Pts',(0.00495975584059877,-0.0330240426238156,
0.0790493988225064));
#104893=CARTESIAN_POINT('Ctrl Pts',(0.00489226184856611,-0.0329142774063509,
0.0790058112769393));
#104894=CARTESIAN_POINT('Ctrl Pts',(0.00482563528463957,-0.0328043479726686,
0.0789608067120406));
#104895=CARTESIAN_POINT('Ctrl Pts',(0.00475996309019608,-0.0326943950436594,
0.0789144404313869));
#104896=CARTESIAN_POINT('Ctrl Pts',(0.00497971419027906,-0.0330240426238156,
0.0791609461230697));
#104897=CARTESIAN_POINT('Ctrl Pts',(0.00491068352550588,-0.0329142774063509,
0.079117633523214));
#104898=CARTESIAN_POINT('Ctrl Pts',(0.00484251383885554,-0.0328043479726686,
0.079072872273779));
#104899=CARTESIAN_POINT('Ctrl Pts',(0.0047752940399758,-0.0326943950436594,
0.0790267173121941));
#104900=CARTESIAN_POINT('Ctrl Pts',(0.00499967253995936,-0.0330240426238156,
0.079272493423633));
#104901=CARTESIAN_POINT('Ctrl Pts',(0.00492910520244565,-0.0329142774063509,
0.0792294557694886));
#104902=CARTESIAN_POINT('Ctrl Pts',(0.00485939239307151,-0.0328043479726686,
0.0791849378355174));
#104903=CARTESIAN_POINT('Ctrl Pts',(0.00479062498975551,-0.0326943950436594,
0.0791389941930012));
#104904=CARTESIAN_POINT('Origin',(0.014676911042144,-0.0326396682854563,
0.0652529107625777));
#104905=CARTESIAN_POINT('Ctrl Pts',(0.00450435085242291,-0.0331951640388587,
0.0789353648523489));
#104906=CARTESIAN_POINT('Ctrl Pts',(0.00443844213229608,-0.033085561825504,
0.0788855145076809));
#104907=CARTESIAN_POINT('Ctrl Pts',(0.00437351622090669,-0.0329757224427707,
0.0788342660060127));
#104908=CARTESIAN_POINT('Ctrl Pts',(0.00430965947891291,-0.0328657862078596,
0.0787816808958618));
#104909=CARTESIAN_POINT('Ctrl Pts',(0.00461544361159874,-0.0331951640388587,
0.0789130142170475));
#104910=CARTESIAN_POINT('Ctrl Pts',(0.00454984272625821,-0.033085561825504,
0.0788646939503983));
#104911=CARTESIAN_POINT('Ctrl Pts',(0.00448519324747173,-0.0329757224427707,
0.0788149829921797));
#104912=CARTESIAN_POINT('Ctrl Pts',(0.00442158108532942,-0.0328657862078596,
0.0787639409393561));
#104913=CARTESIAN_POINT('Ctrl Pts',(0.00472653637077457,-0.0331951640388587,
0.0788906635817461));
#104914=CARTESIAN_POINT('Ctrl Pts',(0.00466124332022035,-0.0330855618255041,
0.0788438733931158));
#104915=CARTESIAN_POINT('Ctrl Pts',(0.00459687027403676,-0.0329757224427707,
0.0787956999783466));
#104916=CARTESIAN_POINT('Ctrl Pts',(0.00453350269174592,-0.0328657862078596,
0.0787462009828505));
#104917=CARTESIAN_POINT('Ctrl Pts',(0.00483762912995039,-0.0331951640388587,
0.0788683129464448));
#104918=CARTESIAN_POINT('Ctrl Pts',(0.00477264391418249,-0.0330855618255041,
0.0788230528358333));
#104919=CARTESIAN_POINT('Ctrl Pts',(0.0047085473006018,-0.0329757224427707,
0.0787764169645136));
#104920=CARTESIAN_POINT('Ctrl Pts',(0.00464542429816242,-0.0328657862078596,
0.0787284610263448));
#104921=CARTESIAN_POINT('Origin',(0.0150400157860922,-0.0326401908834433,
0.0655682325287461));
#104922=CARTESIAN_POINT('Ctrl Pts',(0.0048653280158603,-0.0332451089994432,
0.0788892616908939));
#104923=CARTESIAN_POINT('Ctrl Pts',(0.00468658383678061,-0.0329451141710258,
0.0787663670809381));
#104924=CARTESIAN_POINT('Ctrl Pts',(0.00451760437546793,-0.0326442513127503,
0.0786303578593187));
#104925=CARTESIAN_POINT('Ctrl Pts',(0.00507436390812141,-0.0332451089994432,
0.0790263893531165));
#104926=CARTESIAN_POINT('Ctrl Pts',(0.00489044787464504,-0.0329451141710258,
0.0789113786608249));
#104927=CARTESIAN_POINT('Ctrl Pts',(0.00471571740271998,-0.0326442513127503,
0.0787828413942759));
#104928=CARTESIAN_POINT('Ctrl Pts',(0.00464544939608382,-0.0325229783203385,
0.0787284802064067));
#104929=CARTESIAN_POINT('Ctrl Pts',(0.00458233514771206,-0.0324130253112079,
0.0786805314657386));
#104930=CARTESIAN_POINT('Ctrl Pts',(0.00452022235312969,-0.0323031222247695,
0.0786312843981566));
#104931=CARTESIAN_POINT('Ctrl Pts',(0.00445918834845222,-0.0321934096636184,
0.0785808048931343));
#104932=CARTESIAN_POINT('Ctrl Pts',(0.00465836427094616,-0.0325229783203385,
0.0788410606161457));
#104933=CARTESIAN_POINT('Ctrl Pts',(0.00459369810411637,-0.0324130253112079,
0.0787932899067419));
#104934=CARTESIAN_POINT('Ctrl Pts',(0.00453002994364946,-0.0323031222247695,
0.0787441887399959));
#104935=CARTESIAN_POINT('Ctrl Pts',(0.00446743912456871,-0.0321934096636184,
0.078693822888795));
#104936=CARTESIAN_POINT('Ctrl Pts',(0.0046712791458085,-0.0325229783203385,
0.0789536410258846));
#104937=CARTESIAN_POINT('Ctrl Pts',(0.00460506106052067,-0.0324130253112079,
0.0789060483477451));
#104938=CARTESIAN_POINT('Ctrl Pts',(0.00453983753416924,-0.0323031222247695,
0.0788570930818352));
#104939=CARTESIAN_POINT('Ctrl Pts',(0.0044756899006852,-0.0321934096636184,
0.0788068408844558));
#104940=CARTESIAN_POINT('Ctrl Pts',(0.00468419402067084,-0.0325229783203385,
0.0790662214356236));
#104941=CARTESIAN_POINT('Ctrl Pts',(0.00461642401692498,-0.0324130253112079,
0.0790188067887484));
#104942=CARTESIAN_POINT('Ctrl Pts',(0.00454964512468902,-0.0323031222247695,
0.0789699974236745));
#104943=CARTESIAN_POINT('Ctrl Pts',(0.00448394067680168,-0.0321934096636184,
0.0789198588801165));
#104944=CARTESIAN_POINT('Origin',(0.0146716648041683,-0.0326393375176332,
0.065259631478032));
#104945=CARTESIAN_POINT('Ctrl Pts',(0.00421101742817708,-0.0326943950436594,
0.0786986560536431));
#104946=CARTESIAN_POINT('Ctrl Pts',(0.00414832842266803,-0.0325844576448127,
0.0786447308218798));
#104947=CARTESIAN_POINT('Ctrl Pts',(0.00408675024276515,-0.0324744968375318,
0.0785895052623301));
#104948=CARTESIAN_POINT('Ctrl Pts',(0.00402636081005524,-0.0323646534831894,
0.078533051221436));
#104949=CARTESIAN_POINT('Ctrl Pts',(0.00432329427224715,-0.0326943950436594,
0.0786833251088797));
#104950=CARTESIAN_POINT('Ctrl Pts',(0.0042608165558902,-0.0325844576448127,
0.0786309472624569));
#104951=CARTESIAN_POINT('Ctrl Pts',(0.00419941767762686,-0.0324744968375318,
0.0785772735675646));
#104952=CARTESIAN_POINT('Ctrl Pts',(0.0041391753567374,-0.0323646534831894,
0.0785223738791367));
#104953=CARTESIAN_POINT('Ctrl Pts',(0.00443557111631723,-0.0326943950436593,
0.0786679941641163));
#104954=CARTESIAN_POINT('Ctrl Pts',(0.00437330468911236,-0.0325844576448126,
0.078617163703034));
#104955=CARTESIAN_POINT('Ctrl Pts',(0.00431208511248856,-0.0324744968375318,
0.0785650418727991));
#104956=CARTESIAN_POINT('Ctrl Pts',(0.00425198990341955,-0.0323646534831894,
0.0785116965368374));
#104957=CARTESIAN_POINT('Ctrl Pts',(0.0045478479603873,-0.0326943950436593,
0.0786526632193529));
#104958=CARTESIAN_POINT('Ctrl Pts',(0.00448579282233453,-0.0325844576448126,
0.0786033801436111));
#104959=CARTESIAN_POINT('Ctrl Pts',(0.00442475254735027,-0.0324744968375318,
0.0785528101780337));
#104960=CARTESIAN_POINT('Ctrl Pts',(0.00436480445010171,-0.0323646534831894,
0.0785010191945382));
#104961=CARTESIAN_POINT('Origin',(0.0150634030036769,-0.0326395579067523,
0.0655384835811933));
#104962=CARTESIAN_POINT('Ctrl Pts',(0.00457420798906062,-0.0327445246961877,
0.0786753340175019));
#104963=CARTESIAN_POINT('Ctrl Pts',(0.00440353222819769,-0.0324436878365475,
0.0785414596392411));
#104964=CARTESIAN_POINT('Ctrl Pts',(0.00424342530435261,-0.0321434074463186,
0.0783951095882069));
#104965=CARTESIAN_POINT('Ctrl Pts',(0.00477422210243722,-0.0327445246961877,
0.0788253151978218));
#104966=CARTESIAN_POINT('Ctrl Pts',(0.00459788970894404,-0.0324436878365475,
0.0786989844750906));
#104967=CARTESIAN_POINT('Ctrl Pts',(0.00443157400340436,-0.0321434074463186,
0.0785597305681734));
#104968=CARTESIAN_POINT('Ctrl Pts',(0.0042928907472474,-0.0322357242816072,
0.0784398013625377));
#104969=CARTESIAN_POINT('Ctrl Pts',(0.00415626613751914,-0.0319819883628705,
0.0783177924384711));
#104970=CARTESIAN_POINT('Ctrl Pts',(0.00402768219139062,-0.0317295851069886,
0.0781873369658635));
#104971=CARTESIAN_POINT('Ctrl Pts',(0.00448293491741518,-0.0322357242816072,
0.0786022304651801));
#104972=CARTESIAN_POINT('Ctrl Pts',(0.00434113715143059,-0.0319819883628705,
0.0784862742014552));
#104973=CARTESIAN_POINT('Ctrl Pts',(0.00420700538499615,-0.0317295851069886,
0.0783615299399902));
#104974=CARTESIAN_POINT('Origin',(0.015002286670181,-0.032637194264492,
0.0656116081134578));
#104975=CARTESIAN_POINT('Origin',(0.0145965540519013,-0.0326352985529824,
0.0653566993818225));
#104976=CARTESIAN_POINT('Ctrl Pts',(0.00393312589888557,-0.0321934096636183,
0.0784439957875769));
#104977=CARTESIAN_POINT('Ctrl Pts',(0.00387390835043815,-0.0320835708272303,
0.0783862033712807));
#104978=CARTESIAN_POINT('Ctrl Pts',(0.00381592116162688,-0.0319739230346346,
0.0783272189728474));
#104979=CARTESIAN_POINT('Ctrl Pts',(0.00375923273119791,-0.0318646057455575,
0.0782671237526427));
#104980=CARTESIAN_POINT('Ctrl Pts',(0.0040461439918666,-0.0321934096636183,
0.0784357450043557));
#104981=CARTESIAN_POINT('Ctrl Pts',(0.00398704022815007,-0.0320835708272303,
0.0783795111956426));
#104982=CARTESIAN_POINT('Ctrl Pts',(0.00392913450276701,-0.0319739230346346,
0.0783220868555058));
#104983=CARTESIAN_POINT('Ctrl Pts',(0.00387249526342312,-0.0318646057455575,
0.0782635511403255));
#104984=CARTESIAN_POINT('Ctrl Pts',(0.00415916208484763,-0.0321934096636183,
0.0784274942211344));
#104985=CARTESIAN_POINT('Ctrl Pts',(0.00410017210586199,-0.0320835708272303,
0.0783728190200045));
#104986=CARTESIAN_POINT('Ctrl Pts',(0.00404234784390713,-0.0319739230346346,
0.0783169547381642));
#104987=CARTESIAN_POINT('Ctrl Pts',(0.00398575779564832,-0.0318646057455575,
0.0782599785280082));
#104988=CARTESIAN_POINT('Ctrl Pts',(0.00427218017782866,-0.0321934096636183,
0.0784192434379131));
#104989=CARTESIAN_POINT('Ctrl Pts',(0.00421330398357392,-0.0320835708272303,
0.0783661268443664));
#104990=CARTESIAN_POINT('Ctrl Pts',(0.00415556118504725,-0.0319739230346346,
0.0783118226208226));
#104991=CARTESIAN_POINT('Ctrl Pts',(0.00409902032787352,-0.0318646057455575,
0.078256405915691));
#104992=CARTESIAN_POINT('Ctrl Pts',(0.00436461899514258,-0.0320218834582382,
0.0785019524183383));
#104993=CARTESIAN_POINT('Ctrl Pts',(0.00431932569124386,-0.0319391099350654,
0.0784628286171652));
#104994=CARTESIAN_POINT('Ctrl Pts',(0.00427467075304835,-0.0318564869454911,
0.0784230212588178));
#104995=CARTESIAN_POINT('Ctrl Pts',(0.0042306839989288,-0.031774074144648,
0.0783825623741296));
#104996=CARTESIAN_POINT('Ctrl Pts',(0.0043671618351721,-0.0320218834582382,
0.0785514535497625));
#104997=CARTESIAN_POINT('Ctrl Pts',(0.00432135334416346,-0.0319391099350654,
0.0785123562134068));
#104998=CARTESIAN_POINT('Ctrl Pts',(0.00427618311774497,-0.0318564869454911,
0.0784725672591235));
#104999=CARTESIAN_POINT('Ctrl Pts',(0.00423168135085995,-0.031774074144648,
0.0784321187393798));
#105000=CARTESIAN_POINT('Ctrl Pts',(0.00436970467520161,-0.0320218834582382,
0.0786009546811868));
#105001=CARTESIAN_POINT('Ctrl Pts',(0.00432338099708305,-0.0319391099350654,
0.0785618838096484));
#105002=CARTESIAN_POINT('Ctrl Pts',(0.00427769548244158,-0.0318564869454911,
0.0785221132594293));
#105003=CARTESIAN_POINT('Ctrl Pts',(0.0042326787027911,-0.031774074144648,
0.0784816751046301));
#105004=CARTESIAN_POINT('Ctrl Pts',(0.00437224751523113,-0.0320218834582382,
0.078650455812611));
#105005=CARTESIAN_POINT('Ctrl Pts',(0.00432540865000264,-0.0319391099350654,
0.07861141140589));
#105006=CARTESIAN_POINT('Ctrl Pts',(0.0042792078471382,-0.0318564869454911,
0.078571659259735));
#105007=CARTESIAN_POINT('Ctrl Pts',(0.00423367605472224,-0.031774074144648,
0.0785312314698804));
#105008=CARTESIAN_POINT('Origin',(0.000965309449836182,-0.0391228853390901,
0.0838781491720797));
#105009=CARTESIAN_POINT('Ctrl Pts',(0.00710343017868775,-0.0352722978779664,
0.0798106577629517));
#105010=CARTESIAN_POINT('Ctrl Pts',(0.0070848982945471,-0.0352466642097263,
0.0798069615556662));
#105011=CARTESIAN_POINT('Ctrl Pts',(0.00706636758505475,-0.0352210183808324,
0.0798033455278783));
#105012=CARTESIAN_POINT('Ctrl Pts',(0.00704783729429126,-0.0351953608940152,
0.0797998100746452));
#105013=CARTESIAN_POINT('Origin',(0.00596800377611451,-0.0352456003065123,
0.0845772655798465));
#105014=CARTESIAN_POINT('Ctrl Pts',(0.00692591360635499,-0.0350241211493339,
0.0797737346122686));
#105015=CARTESIAN_POINT('Ctrl Pts',(0.00684844897138487,-0.0349144232867421,
0.0797572344643753));
#105016=CARTESIAN_POINT('Ctrl Pts',(0.00677127903993087,-0.0348045283677512,
0.0797391231910628));
#105017=CARTESIAN_POINT('Ctrl Pts',(0.00669450352012076,-0.0346945769586886,
0.0797194203123216));
#105018=CARTESIAN_POINT('Ctrl Pts',(0.00698553372184158,-0.0350241211493339,
0.0798701015341502));
#105019=CARTESIAN_POINT('Ctrl Pts',(0.00690674167209437,-0.0349144232867421,
0.0798544226288656));
#105020=CARTESIAN_POINT('Ctrl Pts',(0.0068282265556708,-0.0348045283677512,
0.0798371056511042));
#105021=CARTESIAN_POINT('Ctrl Pts',(0.00675008976585002,-0.0346945769586886,
0.0798181690393479));
#105022=CARTESIAN_POINT('Ctrl Pts',(0.00704515383732817,-0.0350241211493339,
0.0799664684560319));
#105023=CARTESIAN_POINT('Ctrl Pts',(0.00696503437280388,-0.0349144232867421,
0.0799516107933558));
#105024=CARTESIAN_POINT('Ctrl Pts',(0.00688517407141074,-0.0348045283677512,
0.0799350881111456));
#105025=CARTESIAN_POINT('Ctrl Pts',(0.00680567601157928,-0.0346945769586886,
0.0799169177663742));
#105026=CARTESIAN_POINT('Ctrl Pts',(0.00710477395281477,-0.0350241211493339,
0.0800628353779136));
#105027=CARTESIAN_POINT('Ctrl Pts',(0.00702332707351338,-0.0349144232867421,
0.0800487989578461));
#105028=CARTESIAN_POINT('Ctrl Pts',(0.00694212158715068,-0.0348045283677512,
0.0800330705711871));
#105029=CARTESIAN_POINT('Ctrl Pts',(0.00686126225730854,-0.0346945769586886,
0.0800156664934005));
#105030=CARTESIAN_POINT('Origin',(0.0110419555985394,-0.034562906794156,
0.0635032984105877));
#105031=CARTESIAN_POINT('Ctrl Pts',(0.00659933070161038,-0.0351970973651595,
0.0798816288633648));
#105032=CARTESIAN_POINT('Ctrl Pts',(0.00651992675144133,-0.0350869349321762,
0.0798605096539478));
#105033=CARTESIAN_POINT('Ctrl Pts',(0.00644089608062417,-0.0349764985129722,
0.0798377221855027));
#105034=CARTESIAN_POINT('Ctrl Pts',(0.00636234281354197,-0.0348659306849651,
0.0798132899527924));
#105035=CARTESIAN_POINT('Ctrl Pts',(0.00666829611299639,-0.0351970973651595,
0.079836860094309));
#105036=CARTESIAN_POINT('Ctrl Pts',(0.00658951237345017,-0.0350869349321762,
0.079816696307202));
#105037=CARTESIAN_POINT('Ctrl Pts',(0.00651108256433076,-0.0349764985129722,
0.0797948779463629));
#105038=CARTESIAN_POINT('Ctrl Pts',(0.00643310995768071,-0.0348659306849651,
0.0797714272968703));
#105039=CARTESIAN_POINT('Ctrl Pts',(0.00673726152438239,-0.0351970973651595,
0.0797920913252531));
#105040=CARTESIAN_POINT('Ctrl Pts',(0.00665909799545902,-0.0350869349321762,
0.0797728829604563));
#105041=CARTESIAN_POINT('Ctrl Pts',(0.00658126904803734,-0.0349764985129722,
0.0797520337072231));
#105042=CARTESIAN_POINT('Ctrl Pts',(0.00650387710181946,-0.0348659306849651,
0.0797295646409481));
#105043=CARTESIAN_POINT('Ctrl Pts',(0.00680622693576839,-0.0351970973651595,
0.0797473225561973));
#105044=CARTESIAN_POINT('Ctrl Pts',(0.00672868361746786,-0.0350869349321762,
0.0797290696137105));
#105045=CARTESIAN_POINT('Ctrl Pts',(0.00665145553174393,-0.0349764985129722,
0.0797091894680833));
#105046=CARTESIAN_POINT('Ctrl Pts',(0.0065746442459582,-0.0348659306849651,
0.0796877019850259));
#105047=CARTESIAN_POINT('Origin',(0.0114917135417066,-0.0345637187965474,
0.0636737189169973));
#105048=CARTESIAN_POINT('Ctrl Pts',(0.00683878082878371,-0.0352450361861253,
0.0797559697192978));
#105049=CARTESIAN_POINT('Ctrl Pts',(0.00662734821681258,-0.0349452761023765,
0.0797075050988219));
#105050=CARTESIAN_POINT('Ctrl Pts',(0.00642016681602617,-0.0346444289983475,
0.0796432521921873));
#105051=CARTESIAN_POINT('Ctrl Pts',(0.0070836174924134,-0.0352450361861253,
0.0798065168076678));
#105052=CARTESIAN_POINT('Ctrl Pts',(0.00687027846577064,-0.0349452761023765,
0.0797672863532487));
#105053=CARTESIAN_POINT('Ctrl Pts',(0.00666050051108305,-0.0346444289983475,
0.0797120977804287));
#105054=CARTESIAN_POINT('Ctrl Pts',(0.00657516103046764,-0.0345231616327822,
0.0796874229798397));
#105055=CARTESIAN_POINT('Ctrl Pts',(0.00649883545075899,-0.0344132092796975,
0.079666077417397));
#105056=CARTESIAN_POINT('Ctrl Pts',(0.00642295532522138,-0.0343032738558974,
0.0796431542218758));
#105057=CARTESIAN_POINT('Ctrl Pts',(0.00634761711281161,-0.034193496108874,
0.0796186852506402));
#105058=CARTESIAN_POINT('Ctrl Pts',(0.00662861257439584,-0.0345231616327822,
0.0797873432910419));
#105059=CARTESIAN_POINT('Ctrl Pts',(0.00655090973387383,-0.0344132092796975,
0.0797667344828785));
#105060=CARTESIAN_POINT('Ctrl Pts',(0.00647363717940205,-0.0343032738558974,
0.0797445195160698));
#105061=CARTESIAN_POINT('Ctrl Pts',(0.00639689317704112,-0.034193496108874,
0.0797207293863516));
#105062=CARTESIAN_POINT('Ctrl Pts',(0.00668206411832403,-0.0345231616327822,
0.079887263602244));
#105063=CARTESIAN_POINT('Ctrl Pts',(0.00660298401698866,-0.0344132092796975,
0.07986739154836));
#105064=CARTESIAN_POINT('Ctrl Pts',(0.00652431903358272,-0.0343032738558974,
0.0798458848102639));
#105065=CARTESIAN_POINT('Ctrl Pts',(0.00644616924127063,-0.034193496108874,
0.0798227735220631));
#105066=CARTESIAN_POINT('Ctrl Pts',(0.00673551566225223,-0.0345231616327822,
0.0799871839134462));
#105067=CARTESIAN_POINT('Ctrl Pts',(0.00665505830010349,-0.0344132092796975,
0.0799680486138414));
#105068=CARTESIAN_POINT('Ctrl Pts',(0.00657500088776339,-0.0343032738558974,
0.079947250104458));
#105069=CARTESIAN_POINT('Ctrl Pts',(0.00649544530550014,-0.034193496108874,
0.0799248176577745));
#105070=CARTESIAN_POINT('Origin',(0.0110449128153173,-0.0345625596230184,
0.0634915615823885));
#105071=CARTESIAN_POINT('Ctrl Pts',(0.00616025749492642,-0.0346945769586885,
0.0798196182199217));
#105072=CARTESIAN_POINT('Ctrl Pts',(0.00608212729015849,-0.0345846629176052,
0.079792559857121));
#105073=CARTESIAN_POINT('Ctrl Pts',(0.00600454329639,-0.0344746925050311,
0.0797638811721372));
#105074=CARTESIAN_POINT('Ctrl Pts',(0.00592760477141671,-0.0343648066253259,
0.0797336193219533));
#105075=CARTESIAN_POINT('Ctrl Pts',(0.00625900614419945,-0.0346945769586885,
0.0797640320179602));
#105076=CARTESIAN_POINT('Ctrl Pts',(0.00618164194539049,-0.0345846629176052,
0.0797383344614588));
#105077=CARTESIAN_POINT('Ctrl Pts',(0.00610479594750125,-0.0344746925050311,
0.0797110326558919));
#105078=CARTESIAN_POINT('Ctrl Pts',(0.00602856647000809,-0.0343648066253259,
0.079682161990121));
#105079=CARTESIAN_POINT('Ctrl Pts',(0.00635775479347248,-0.0346945769586885,
0.0797084458159986));
#105080=CARTESIAN_POINT('Ctrl Pts',(0.00628115660062249,-0.0345846629176052,
0.0796841090657966));
#105081=CARTESIAN_POINT('Ctrl Pts',(0.0062050485986125,-0.0344746925050311,
0.0796581841396467));
#105082=CARTESIAN_POINT('Ctrl Pts',(0.00612952816859947,-0.0343648066253259,
0.0796307046582887));
#105083=CARTESIAN_POINT('Ctrl Pts',(0.00645650344274552,-0.0346945769586885,
0.0796528596140371));
#105084=CARTESIAN_POINT('Ctrl Pts',(0.00638067125585449,-0.0345846629176052,
0.0796298836701343));
#105085=CARTESIAN_POINT('Ctrl Pts',(0.00630530124972375,-0.0344746925050311,
0.0796053356234015));
#105086=CARTESIAN_POINT('Ctrl Pts',(0.00623048986719085,-0.0343648066253259,
0.0795792473264565));
#105087=CARTESIAN_POINT('Origin',(0.0115088537350995,-0.0345626446730671,
0.0636178588735325));
#105088=CARTESIAN_POINT('Ctrl Pts',(0.00645473649828103,-0.0346945769586886,
0.0796538542375848));
#105089=CARTESIAN_POINT('Ctrl Pts',(0.00633945606765366,-0.0345275153362891,
0.0796188954072578));
#105090=CARTESIAN_POINT('Ctrl Pts',(0.00622524524263857,-0.0343603235965159,
0.0795803020713518));
#105091=CARTESIAN_POINT('Ctrl Pts',(0.00611244011171103,-0.034193496108874,
0.0795381933921864));
#105092=CARTESIAN_POINT('Ctrl Pts',(0.00653547195057605,-0.0346945769586886,
0.079676433322464));
#105093=CARTESIAN_POINT('Ctrl Pts',(0.00641971859197572,-0.0345275153362891,
0.07964316552851));
#105094=CARTESIAN_POINT('Ctrl Pts',(0.00630498153512684,-0.0343603235965159,
0.0796062487932162));
#105095=CARTESIAN_POINT('Ctrl Pts',(0.00619159849856314,-0.034193496108874,
0.0795657973433934));
#105096=CARTESIAN_POINT('Ctrl Pts',(0.00661620740287108,-0.0346945769586886,
0.0796990124073433));
#105097=CARTESIAN_POINT('Ctrl Pts',(0.00649998111629779,-0.0345275153362891,
0.0796674356497623));
#105098=CARTESIAN_POINT('Ctrl Pts',(0.00638471782761511,-0.0343603235965159,
0.0796321955150806));
#105099=CARTESIAN_POINT('Ctrl Pts',(0.00627075688541525,-0.034193496108874,
0.0795934012946004));
#105100=CARTESIAN_POINT('Ctrl Pts',(0.0066969428551661,-0.0346945769586886,
0.0797215914922225));
#105101=CARTESIAN_POINT('Ctrl Pts',(0.00658024364061985,-0.0345275153362891,
0.0796917057710145));
#105102=CARTESIAN_POINT('Ctrl Pts',(0.00646445412010338,-0.0343603235965159,
0.0796581422369451));
#105103=CARTESIAN_POINT('Ctrl Pts',(0.00634991527226737,-0.034193496108874,
0.0796210052458074));
#105104=CARTESIAN_POINT('Ctrl Pts',(0.00623051984523234,-0.0340223579322365,
0.0795792571906563));
#105105=CARTESIAN_POINT('Ctrl Pts',(0.00615563622847656,-0.0339125849573552,
0.0795531441650439));
#105106=CARTESIAN_POINT('Ctrl Pts',(0.00608134571052315,-0.0338030433565217,
0.0795254995718907));
#105107=CARTESIAN_POINT('Ctrl Pts',(0.00600774016254726,-0.0336938721132321,
0.0794963671857699));
#105108=CARTESIAN_POINT('Ctrl Pts',(0.00627759196310741,-0.0340223579322365,
0.079682336749976));
#105109=CARTESIAN_POINT('Ctrl Pts',(0.00620128661038585,-0.0339125849573552,
0.0796568729716383));
#105110=CARTESIAN_POINT('Ctrl Pts',(0.00612556191759411,-0.0338030433565217,
0.0796298477429105));
#105111=CARTESIAN_POINT('Ctrl Pts',(0.00605051166018825,-0.0336938721132321,
0.0796013042088853));
#105112=CARTESIAN_POINT('Ctrl Pts',(0.00632466408098248,-0.0340223579322365,
0.0797854163092957));
#105113=CARTESIAN_POINT('Ctrl Pts',(0.00624693699229514,-0.0339125849573552,
0.0797606017782327));
#105114=CARTESIAN_POINT('Ctrl Pts',(0.00616977812466508,-0.0338030433565217,
0.0797341959139303));
#105115=CARTESIAN_POINT('Ctrl Pts',(0.00609328315782925,-0.0336938721132321,
0.0797062412320008));
#105116=CARTESIAN_POINT('Ctrl Pts',(0.00637173619885756,-0.0340223579322365,
0.0798884958686154));
#105117=CARTESIAN_POINT('Ctrl Pts',(0.00629258737420443,-0.0339125849573552,
0.0798643305848271));
#105118=CARTESIAN_POINT('Ctrl Pts',(0.00621399433173604,-0.0338030433565217,
0.07983854408495));
#105119=CARTESIAN_POINT('Ctrl Pts',(0.00613605465547024,-0.0336938721132321,
0.0798111782551162));
#105120=CARTESIAN_POINT('Origin',(0.0110106430328453,-0.0345589643415453,
0.0636067937832463));
#105121=CARTESIAN_POINT('Ctrl Pts',(0.00580813378883228,-0.034193496108874,
0.0796851397875581));
#105122=CARTESIAN_POINT('Ctrl Pts',(0.00573180748894145,-0.0340836138581107,
0.0796532083673356));
#105123=CARTESIAN_POINT('Ctrl Pts',(0.0056561785655845,-0.0339738896643499,
0.079619712855787));
#105124=CARTESIAN_POINT('Ctrl Pts',(0.0055813409406497,-0.0338644633294062,
0.0795847026117196));
#105125=CARTESIAN_POINT('Ctrl Pts',(0.00591017801635925,-0.034193496108874,
0.0796358636789918));
#105126=CARTESIAN_POINT('Ctrl Pts',(0.0058345312048254,-0.0340836138581107,
0.0796053393882387));
#105127=CARTESIAN_POINT('Ctrl Pts',(0.00575955232620233,-0.0339738896643499,
0.0795732643915782));
#105128=CARTESIAN_POINT('Ctrl Pts',(0.00568533459227637,-0.0338644633294062,
0.0795396861739623));
#105129=CARTESIAN_POINT('Ctrl Pts',(0.00601222224388621,-0.034193496108874,
0.0795865875704255));
#105130=CARTESIAN_POINT('Ctrl Pts',(0.00593725492070934,-0.0340836138581107,
0.0795574704091419));
#105131=CARTESIAN_POINT('Ctrl Pts',(0.00586292608682015,-0.0339738896643499,
0.0795268159273693));
#105132=CARTESIAN_POINT('Ctrl Pts',(0.00578932824390305,-0.0338644633294062,
0.0794946697362049));
#105133=CARTESIAN_POINT('Ctrl Pts',(0.00611426647141318,-0.034193496108874,
0.0795373114618592));
#105134=CARTESIAN_POINT('Ctrl Pts',(0.00603997863659329,-0.0340836138581107,
0.079509601430045));
#105135=CARTESIAN_POINT('Ctrl Pts',(0.00596629984743797,-0.0339738896643499,
0.0794803674631605));
#105136=CARTESIAN_POINT('Ctrl Pts',(0.00589332189552972,-0.0338644633294062,
0.0794496532984475));
#105137=CARTESIAN_POINT('Origin',(0.011484736484883,-0.0345610621862571,
0.0636891673860762));
#105138=CARTESIAN_POINT('Ctrl Pts',(0.00614637285195932,-0.0342436276873901,
0.0795507385881505));
#105139=CARTESIAN_POINT('Ctrl Pts',(0.00594268063820261,-0.0339430054201861,
0.0794761593653965));
#105140=CARTESIAN_POINT('Ctrl Pts',(0.00574518470530769,-0.0336441434784164,
0.0793864490822531));
#105141=CARTESIAN_POINT('Ctrl Pts',(0.00638294477864433,-0.0342436276873901,
0.0796315700393595));
#105142=CARTESIAN_POINT('Ctrl Pts',(0.00617620395644838,-0.0339430054201861,
0.0795659132739087));
#105143=CARTESIAN_POINT('Ctrl Pts',(0.00597499599984848,-0.0336441434784164,
0.0794848704666239));
#105144=CARTESIAN_POINT('Ctrl Pts',(0.00589334750425107,-0.0335235895815127,
0.0794496639389884));
#105145=CARTESIAN_POINT('Ctrl Pts',(0.00582038719605378,-0.0334144449262719,
0.079418957614175));
#105146=CARTESIAN_POINT('Ctrl Pts',(0.00574797743486331,-0.0333049234473133,
0.0793867087064559));
#105147=CARTESIAN_POINT('Ctrl Pts',(0.00567621454590946,-0.0331951640388588,
0.0793529500650937));
#105148=CARTESIAN_POINT('Ctrl Pts',(0.00593385425712526,-0.0335235895815127,
0.0795554957652901));
#105149=CARTESIAN_POINT('Ctrl Pts',(0.00585943696547526,-0.0334144449262719,
0.0795253470956804));
#105150=CARTESIAN_POINT('Ctrl Pts',(0.00578555702619778,-0.0333049234473133,
0.0794936263836617));
#105151=CARTESIAN_POINT('Ctrl Pts',(0.00571231258324836,-0.0331951640388588,
0.0794603656328063));
#105152=CARTESIAN_POINT('Ctrl Pts',(0.00597436100999945,-0.0335235895815127,
0.0796613275915918));
#105153=CARTESIAN_POINT('Ctrl Pts',(0.00589848673489674,-0.0334144449262719,
0.0796317365771858));
#105154=CARTESIAN_POINT('Ctrl Pts',(0.00582313661753225,-0.0333049234473133,
0.0796005440608675));
#105155=CARTESIAN_POINT('Ctrl Pts',(0.00574841062058726,-0.0331951640388588,
0.079567781200519));
#105156=CARTESIAN_POINT('Ctrl Pts',(0.00601486776287364,-0.0335235895815127,
0.0797671594178934));
#105157=CARTESIAN_POINT('Ctrl Pts',(0.00593753650431821,-0.0334144449262719,
0.0797381260586913));
#105158=CARTESIAN_POINT('Ctrl Pts',(0.00586071620886671,-0.0333049234473133,
0.0797074617380733));
#105159=CARTESIAN_POINT('Ctrl Pts',(0.00578450865792616,-0.0331951640388588,
0.0796751967682316));
#105160=CARTESIAN_POINT('Origin',(0.0134522516024782,-0.0326434571769783,
0.0646110340170667));
#105161=CARTESIAN_POINT('Ctrl Pts',(0.00546327129297219,-0.0336938721132459,
0.0795295819804915));
#105162=CARTESIAN_POINT('Ctrl Pts',(0.00543178281450347,-0.0336474569764992,
0.0795140091273407));
#105163=CARTESIAN_POINT('Ctrl Pts',(0.0054004787935538,-0.033601104548885,
0.0794980687288541));
#105164=CARTESIAN_POINT('Ctrl Pts',(0.00532122421317455,-0.0334837508643204,
0.0794577113065546));
#105165=CARTESIAN_POINT('Ctrl Pts',(0.00524320030960904,-0.0333660264760491,
0.0794150231288218));
#105166=CARTESIAN_POINT('Ctrl Pts',(0.00577808157345017,-0.0336938721132459,
0.0794012678091044));
#105167=CARTESIAN_POINT('Ctrl Pts',(0.00574734416040578,-0.0336474569764992,
0.0793875376449905));
#105168=CARTESIAN_POINT('Ctrl Pts',(0.00571676958241522,-0.033601104548885,
0.0793734486014476));
#105169=CARTESIAN_POINT('Ctrl Pts',(0.00563936178381929,-0.0334837508643204,
0.0793377783840103));
#105170=CARTESIAN_POINT('Ctrl Pts',(0.00556304495947447,-0.0333660264760491,
0.0792998300768357));
#105171=CARTESIAN_POINT('Ctrl Pts',(0.00577808157345143,-0.0336938721132426,
0.0794012678091105));
#105172=CARTESIAN_POINT('Ctrl Pts',(0.00574734416041144,-0.0336474569765026,
0.0793875376449985));
#105173=CARTESIAN_POINT('Ctrl Pts',(0.00571676958242522,-0.0336011045488949,
0.0793734486014576));
#105174=CARTESIAN_POINT('Ctrl Pts',(0.00564000648535609,-0.0334847282606778,
0.0793380754683458));
#105175=CARTESIAN_POINT('Ctrl Pts',(0.00556431599105305,-0.0333679869945434,
0.0793004618977903));
#105176=CARTESIAN_POINT('Ctrl Pts',(0.00577808157344808,-0.0336938721132427,
0.0794012678091035));
#105177=CARTESIAN_POINT('Ctrl Pts',(0.00566815098175153,-0.0335278710435083,
0.0793521626660339));
#105178=CARTESIAN_POINT('Ctrl Pts',(0.0055597989879013,-0.033362046922432,
0.0792996274032657));
#105179=CARTESIAN_POINT('Ctrl Pts',(0.00545298044386996,-0.0331951640388602,
0.0792436178710486));
#105180=CARTESIAN_POINT('Ctrl Pts',(0.0058553505010703,-0.0336938721132427,
0.0794337876899056));
#105181=CARTESIAN_POINT('Ctrl Pts',(0.00574473913477446,-0.0335278710435083,
0.0793863001026801));
#105182=CARTESIAN_POINT('Ctrl Pts',(0.00563565587968916,-0.033362046922432,
0.0793353604777891));
#105183=CARTESIAN_POINT('Ctrl Pts',(0.00552805495870329,-0.0331951640388602,
0.0792809253374034));
#105184=CARTESIAN_POINT('Ctrl Pts',(0.00593261942869252,-0.0336938721132427,
0.0794663075707078));
#105185=CARTESIAN_POINT('Ctrl Pts',(0.0058213272877974,-0.0335278710435083,
0.0794204375393264));
#105186=CARTESIAN_POINT('Ctrl Pts',(0.00571151277147702,-0.033362046922432,
0.0793710935523126));
#105187=CARTESIAN_POINT('Ctrl Pts',(0.00560312947353661,-0.0331951640388602,
0.0793182328037582));
#105188=CARTESIAN_POINT('Ctrl Pts',(0.00600988835631474,-0.0336938721132427,
0.0794988274515099));
#105189=CARTESIAN_POINT('Ctrl Pts',(0.00589791544082033,-0.0335278710435083,
0.0794545749759726));
#105190=CARTESIAN_POINT('Ctrl Pts',(0.00578736966326488,-0.033362046922432,
0.079406826626836));
#105191=CARTESIAN_POINT('Ctrl Pts',(0.00567820398836994,-0.0331951640388602,
0.0793555402701131));
#105192=CARTESIAN_POINT('Ctrl Pts',(0.00556498107437625,-0.0330240426238155,
0.0792991569809753));
#105193=CARTESIAN_POINT('Ctrl Pts',(0.00549404642038312,-0.0329142774063509,
0.0792639070026458));
#105194=CARTESIAN_POINT('Ctrl Pts',(0.00542380511839599,-0.0328043479726686,
0.0792271730334723));
#105195=CARTESIAN_POINT('Ctrl Pts',(0.0053543484487492,-0.0326943950436594,
0.0791889996542524));
#105196=CARTESIAN_POINT('Ctrl Pts',(0.00559876263038315,-0.0330240426238155,
0.0794073232532546));
#105197=CARTESIAN_POINT('Ctrl Pts',(0.00552633788060809,-0.0329142774063509,
0.0793725386487708));
#105198=CARTESIAN_POINT('Ctrl Pts',(0.00545459611939459,-0.0328043479726686,
0.0793362394810067));
#105199=CARTESIAN_POINT('Ctrl Pts',(0.00538363053393696,-0.0326943950436594,
0.0792984697208099));
#105200=CARTESIAN_POINT('Ctrl Pts',(0.00563254418639006,-0.0330240426238155,
0.0795154895255338));
#105201=CARTESIAN_POINT('Ctrl Pts',(0.00555862934083307,-0.0329142774063509,
0.0794811702948958));
#105202=CARTESIAN_POINT('Ctrl Pts',(0.00548538712039319,-0.0328043479726686,
0.0794453059285411));
#105203=CARTESIAN_POINT('Ctrl Pts',(0.00541291261912473,-0.0326943950436594,
0.0794079397873673));
#105204=CARTESIAN_POINT('Ctrl Pts',(0.00566632574239696,-0.0330240426238155,
0.079623655797813));
#105205=CARTESIAN_POINT('Ctrl Pts',(0.00559092080105804,-0.0329142774063509,
0.0795898019410208));
#105206=CARTESIAN_POINT('Ctrl Pts',(0.00551617812139179,-0.0328043479726686,
0.0795543723760755));
#105207=CARTESIAN_POINT('Ctrl Pts',(0.0054421947043125,-0.0326943950436594,
0.0795174098539247));
#105208=CARTESIAN_POINT('Origin',(0.0135101367001887,-0.0326396682855018,
0.0645017421403));
#105209=CARTESIAN_POINT('Ctrl Pts',(0.00513265640034573,-0.0331951640388587,
0.0793512658547611));
#105210=CARTESIAN_POINT('Ctrl Pts',(0.00506101948527155,-0.0330855618255041,
0.079310069147964));
#105211=CARTESIAN_POINT('Ctrl Pts',(0.0049901823936565,-0.0329757224427708,
0.0792673621304551));
#105212=CARTESIAN_POINT('Ctrl Pts',(0.00492023851925387,-0.0328657862078596,
0.079223195041563));
#105213=CARTESIAN_POINT('Ctrl Pts',(0.00524007188253915,-0.0331951640388587,
0.0793151678461617));
#105214=CARTESIAN_POINT('Ctrl Pts',(0.00516893214450775,-0.0330855618255041,
0.0792754505703321));
#105215=CARTESIAN_POINT('Ctrl Pts',(0.00509856201103423,-0.0329757224427708,
0.0792342343260914));
#105216=CARTESIAN_POINT('Ctrl Pts',(0.0050290541842623,-0.0328657862078596,
0.0791915674730752));
#105217=CARTESIAN_POINT('Ctrl Pts',(0.00534748736473257,-0.0331951640388587,
0.0792790698375624));
#105218=CARTESIAN_POINT('Ctrl Pts',(0.00527684480374394,-0.0330855618255041,
0.0792408319927003));
#105219=CARTESIAN_POINT('Ctrl Pts',(0.00520694162841195,-0.0329757224427708,
0.0792011065217278));
#105220=CARTESIAN_POINT('Ctrl Pts',(0.00513786984927074,-0.0328657862078596,
0.0791599399045873));
#105221=CARTESIAN_POINT('Ctrl Pts',(0.00545490284692598,-0.0331951640388587,
0.0792429718289631));
#105222=CARTESIAN_POINT('Ctrl Pts',(0.00538475746298014,-0.0330855618255041,
0.0792062134150684));
#105223=CARTESIAN_POINT('Ctrl Pts',(0.00531532124578968,-0.0329757224427708,
0.0791679787173641));
#105224=CARTESIAN_POINT('Ctrl Pts',(0.00524668551427917,-0.0328657862078596,
0.0791283123360995));
#105225=CARTESIAN_POINT('Origin',(0.0139098985521678,-0.0326401908831938,
0.0647690684078328));
#105226=CARTESIAN_POINT('Ctrl Pts',(0.00548500889272825,-0.0332451089994433,
0.0792602837953681));
#105227=CARTESIAN_POINT('Ctrl Pts',(0.00529227138603548,-0.0329451141710259,
0.0791607608320634));
#105228=CARTESIAN_POINT('Ctrl Pts',(0.00510757790270678,-0.0326442513127503,
0.0790470028260727));
#105229=CARTESIAN_POINT('Ctrl Pts',(0.00570958312786032,-0.0332451089994433,
0.0793701310207078));
#105230=CARTESIAN_POINT('Ctrl Pts',(0.00551270266528155,-0.0329451141710259,
0.0792790780132568));
#105231=CARTESIAN_POINT('Ctrl Pts',(0.00532324000406695,-0.0326442513127503,
0.0791734538364954));
#105232=CARTESIAN_POINT('Ctrl Pts',(0.00524671281819513,-0.0325229783203385,
0.0791283282193173));
#105233=CARTESIAN_POINT('Ctrl Pts',(0.00517808667380982,-0.0324130253112079,
0.0790886678816234));
#105234=CARTESIAN_POINT('Ctrl Pts',(0.00511029136294131,-0.0323031222247694,
0.0790475939392694));
#105235=CARTESIAN_POINT('Ctrl Pts',(0.00504341187002752,-0.0321934096636184,
0.0790051620693853));
#105236=CARTESIAN_POINT('Ctrl Pts',(0.00527363592220037,-0.0325229783203385,
0.0792384022358722));
#105237=CARTESIAN_POINT('Ctrl Pts',(0.00520349240993164,-0.0324130253112079,
0.0791991130325715));
#105238=CARTESIAN_POINT('Ctrl Pts',(0.00513417228392672,-0.0323031222247694,
0.0791583787796175));
#105239=CARTESIAN_POINT('Ctrl Pts',(0.00506576249715715,-0.0321934096636184,
0.0791162547879437));
#105240=CARTESIAN_POINT('Ctrl Pts',(0.00530055902620562,-0.0325229783203385,
0.0793484762524271));
#105241=CARTESIAN_POINT('Ctrl Pts',(0.00522889814605345,-0.0324130253112079,
0.0793095581835195));
#105242=CARTESIAN_POINT('Ctrl Pts',(0.00515805320491213,-0.0323031222247694,
0.0792691636199657));
#105243=CARTESIAN_POINT('Ctrl Pts',(0.00508811312428678,-0.0321934096636184,
0.0792273475065022));
#105244=CARTESIAN_POINT('Ctrl Pts',(0.00532748213021086,-0.0325229783203385,
0.0794585502689819));
#105245=CARTESIAN_POINT('Ctrl Pts',(0.00525430388217526,-0.0324130253112079,
0.0794200033344676));
#105246=CARTESIAN_POINT('Ctrl Pts',(0.00518193412589754,-0.0323031222247694,
0.0793799484603138));
#105247=CARTESIAN_POINT('Ctrl Pts',(0.00511046375141641,-0.0321934096636184,
0.0793384402250607));
#105248=CARTESIAN_POINT('Origin',(0.0135057741594412,-0.0326393375177481,
0.0645090673885528));
#105249=CARTESIAN_POINT('Ctrl Pts',(0.00481196851860963,-0.0326943950436593,
0.0791531880022078));
#105250=CARTESIAN_POINT('Ctrl Pts',(0.00474301521096575,-0.0325844576448127,
0.0791075450027729));
#105251=CARTESIAN_POINT('Ctrl Pts',(0.00467500099545019,-0.0324744968375319,
0.0790604727056596));
#105252=CARTESIAN_POINT('Ctrl Pts',(0.00460801218396164,-0.0323646534831895,
0.0790120326246146));
#105253=CARTESIAN_POINT('Ctrl Pts',(0.00492143854934795,-0.0326943950436593,
0.0791239059266012));
#105254=CARTESIAN_POINT('Ctrl Pts',(0.00485288880358638,-0.0325844576448127,
0.0790797716293587));
#105255=CARTESIAN_POINT('Ctrl Pts',(0.00478524697607894,-0.0324744968375319,
0.0790342164875322));
#105256=CARTESIAN_POINT('Ctrl Pts',(0.00471859892841089,-0.0323646534831895,
0.0789873000644197));
#105257=CARTESIAN_POINT('Ctrl Pts',(0.00503090858008626,-0.0326943950436593,
0.0790946238509947));
#105258=CARTESIAN_POINT('Ctrl Pts',(0.00496276239620701,-0.0325844576448127,
0.0790519982559444));
#105259=CARTESIAN_POINT('Ctrl Pts',(0.0048954929567077,-0.0324744968375319,
0.0790079602694048));
#105260=CARTESIAN_POINT('Ctrl Pts',(0.00482918567286014,-0.0323646534831895,
0.0789625675042249));
#105261=CARTESIAN_POINT('Ctrl Pts',(0.00514037861082458,-0.0326943950436593,
0.0790653417753881));
#105262=CARTESIAN_POINT('Ctrl Pts',(0.00507263598882764,-0.0325844576448127,
0.0790242248825302));
#105263=CARTESIAN_POINT('Ctrl Pts',(0.00500573893733646,-0.0324744968375319,
0.0789817040512773));
#105264=CARTESIAN_POINT('Ctrl Pts',(0.00493977241730939,-0.0323646534831895,
0.0789378349440301));
#105265=CARTESIAN_POINT('Origin',(0.0139293728226059,-0.0326395579066818,
0.0647366228438751));
#105266=CARTESIAN_POINT('Ctrl Pts',(0.00516937218723801,-0.0327445246961877,
0.0790845300198918));
#105267=CARTESIAN_POINT('Ctrl Pts',(0.00498326334700908,-0.0324436878365475,
0.0789731026260901));
#105268=CARTESIAN_POINT('Ctrl Pts',(0.00480607638895177,-0.0321434074463188,
0.0788479733074025));
#105269=CARTESIAN_POINT('Ctrl Pts',(0.00538660675589261,-0.0327445246961877,
0.0792082601382198));
#105270=CARTESIAN_POINT('Ctrl Pts',(0.00519583135801167,-0.0324436878365475,
0.0791050258800291));
#105271=CARTESIAN_POINT('Ctrl Pts',(0.00501337395904593,-0.0321434074463188,
0.0789877149169289));
#105272=CARTESIAN_POINT('Ctrl Pts',(0.00486075314664532,-0.0322357242816073,
0.0788861130098361));
#105273=CARTESIAN_POINT('Ctrl Pts',(0.00470991408979555,-0.0319819883628706,
0.0787821897666999));
#105274=CARTESIAN_POINT('Ctrl Pts',(0.0045659936602703,-0.0317295851069886,
0.0786688788162117));
#105275=CARTESIAN_POINT('Ctrl Pts',(0.00506965652642701,-0.0322357242816073,
0.0790234424601218));
#105276=CARTESIAN_POINT('Ctrl Pts',(0.00491444370469541,-0.0319819883628706,
0.078926172518694));
#105277=CARTESIAN_POINT('Ctrl Pts',(0.00476573500564448,-0.0317295851069886,
0.0788192230710009));
#105278=CARTESIAN_POINT('Origin',(0.0138779033429583,-0.032637194264591,
0.0648168306758043));
#105279=CARTESIAN_POINT('Origin',(0.0134434215129649,-0.032635298552763,
0.0646147837559969));
#105280=CARTESIAN_POINT('Ctrl Pts',(0.00450435085242233,-0.0321934096636183,
0.0789353648523491));
#105281=CARTESIAN_POINT('Ctrl Pts',(0.00443835694162196,-0.0320835708272304,
0.0788854500733479));
#105282=CARTESIAN_POINT('Ctrl Pts',(0.00437343429372893,-0.0319739230346346,
0.078834198506393));
#105283=CARTESIAN_POINT('Ctrl Pts',(0.00430966094023589,-0.0318646057455576,
0.0787816820992405));
#105284=CARTESIAN_POINT('Ctrl Pts',(0.00461544366664279,-0.0321934096636183,
0.0789130142059733));
#105285=CARTESIAN_POINT('Ctrl Pts',(0.00454975798867498,-0.0320835708272304,
0.0788646314834606));
#105286=CARTESIAN_POINT('Ctrl Pts',(0.00448511168899753,-0.0319739230346346,
0.0788149174632018));
#105287=CARTESIAN_POINT('Ctrl Pts',(0.00442158259651064,-0.0318646057455576,
0.078763942098633));
#105288=CARTESIAN_POINT('Ctrl Pts',(0.00472653648086325,-0.0321934096636183,
0.0788906635595975));
#105289=CARTESIAN_POINT('Ctrl Pts',(0.004661159035728,-0.0320835708272304,
0.0788438128935734));
#105290=CARTESIAN_POINT('Ctrl Pts',(0.00459678908426614,-0.0319739230346346,
0.0787956364200106));
#105291=CARTESIAN_POINT('Ctrl Pts',(0.00453350425278539,-0.0318646057455576,
0.0787462020980255));
#105292=CARTESIAN_POINT('Ctrl Pts',(0.00483762929508372,-0.0321934096636183,
0.0788683129132217));
#105293=CARTESIAN_POINT('Ctrl Pts',(0.00477256008278102,-0.0320835708272304,
0.0788229943036862));
#105294=CARTESIAN_POINT('Ctrl Pts',(0.00470846647953474,-0.0319739230346346,
0.0787763553768194));
#105295=CARTESIAN_POINT('Ctrl Pts',(0.00464542590906015,-0.0318646057455576,
0.078728462097418));
#105296=CARTESIAN_POINT('Ctrl Pts',(0.0049397053886744,-0.0320218834582375,
0.0789387840527528));
#105297=CARTESIAN_POINT('Ctrl Pts',(0.00488986572349503,-0.0319391099350648,
0.0789056455106741));
#105298=CARTESIAN_POINT('Ctrl Pts',(0.00484057371788366,-0.0318564869454906,
0.0788717487930358));
#105299=CARTESIAN_POINT('Ctrl Pts',(0.00479186296961419,-0.0317740741446476,
0.0788371219408657));
#105300=CARTESIAN_POINT('Ctrl Pts',(0.00494843231451724,-0.0320218834582375,
0.0789875761506071));
#105301=CARTESIAN_POINT('Ctrl Pts',(0.00489808484155334,-0.0319391099350648,
0.0789545284347292));
#105302=CARTESIAN_POINT('Ctrl Pts',(0.00484828391756141,-0.0318564869454906,
0.0789207145587727));
#105303=CARTESIAN_POINT('Ctrl Pts',(0.00479906351662797,-0.0317740741446476,
0.0788861625380316));
#105304=CARTESIAN_POINT('Ctrl Pts',(0.00495715924036009,-0.0320218834582375,
0.0790363682484614));
#105305=CARTESIAN_POINT('Ctrl Pts',(0.00490630395961165,-0.0319391099350648,
0.0790034113587843));
#105306=CARTESIAN_POINT('Ctrl Pts',(0.00485599411723916,-0.0318564869454906,
0.0789696803245095));
#105307=CARTESIAN_POINT('Ctrl Pts',(0.00480626406364174,-0.0317740741446476,
0.0789352031351975));
#105308=CARTESIAN_POINT('Ctrl Pts',(0.00496588616620294,-0.0320218834582375,
0.0790851603463157));
#105309=CARTESIAN_POINT('Ctrl Pts',(0.00491452307766996,-0.0319391099350648,
0.0790522942828394));
#105310=CARTESIAN_POINT('Ctrl Pts',(0.00486370431691691,-0.0318564869454906,
0.0790186460902464));
#105311=CARTESIAN_POINT('Ctrl Pts',(0.00481346461065551,-0.0317740741446476,
0.0789842437323634));
#105312=CARTESIAN_POINT('Origin',(0.00224101653788164,-0.0391228853390896,
0.0846986343464964));
#105313=CARTESIAN_POINT('Ctrl Pts',(0.00782094450061722,-0.0352722978779661,
0.0798939058030755));
#105314=CARTESIAN_POINT('Ctrl Pts',(0.00780209548830728,-0.0352466642097262,
0.0798925614024518));
#105315=CARTESIAN_POINT('Ctrl Pts',(0.0077832576905389,-0.0352210183808323,
0.0798912964018642));
#105316=CARTESIAN_POINT('Ctrl Pts',(0.00776443040686705,-0.0351953608940152,
0.079890111287996));
#105317=CARTESIAN_POINT('Origin',(0.00729188564518976,-0.0352456003065119,
0.0847652341560871));
#105318=CARTESIAN_POINT('Ctrl Pts',(0.00764020000161069,-0.035024121149334,
0.0798795225284857));
#105319=CARTESIAN_POINT('Ctrl Pts',(0.00756127818153511,-0.0349144232867422,
0.0798728613823746));
#105320=CARTESIAN_POINT('Ctrl Pts',(0.00748244681359192,-0.0348045283677512,
0.0798645648789048));
#105321=CARTESIAN_POINT('Ctrl Pts',(0.00740380726618409,-0.0346945769586886,
0.0798546398874039));
#105322=CARTESIAN_POINT('Ctrl Pts',(0.00771142797260723,-0.035024121149334,
0.0799676571865457));
#105323=CARTESIAN_POINT('Ctrl Pts',(0.00763129213380823,-0.0349144232867422,
0.0799619771764862));
#105324=CARTESIAN_POINT('Ctrl Pts',(0.00755122573971058,-0.0348045283677512,
0.0799546373016919));
#105325=CARTESIAN_POINT('Ctrl Pts',(0.00747133169503169,-0.0346945769586886,
0.079945643147304));
#105326=CARTESIAN_POINT('Ctrl Pts',(0.00778265594360378,-0.035024121149334,
0.0800557918446057));
#105327=CARTESIAN_POINT('Ctrl Pts',(0.00770130608608136,-0.0349144232867422,
0.0800510929705979));
#105328=CARTESIAN_POINT('Ctrl Pts',(0.00762000466582925,-0.0348045283677512,
0.080044709724479));
#105329=CARTESIAN_POINT('Ctrl Pts',(0.00753885612387928,-0.0346945769586886,
0.0800366464072041));
#105330=CARTESIAN_POINT('Ctrl Pts',(0.00785388391460032,-0.035024121149334,
0.0801439265026657));
#105331=CARTESIAN_POINT('Ctrl Pts',(0.00777132003835448,-0.0349144232867422,
0.0801402087647095));
#105332=CARTESIAN_POINT('Ctrl Pts',(0.00768878359194791,-0.0348045283677512,
0.0801347821472661));
#105333=CARTESIAN_POINT('Ctrl Pts',(0.00760638055272687,-0.0346945769586886,
0.0801276496671042));
#105334=CARTESIAN_POINT('Origin',(0.00968455939246014,-0.0345629067942544,
0.0632215067238589));
#105335=CARTESIAN_POINT('Ctrl Pts',(0.0073297150359876,-0.0351970973651594,
0.0800274976926647));
#105336=CARTESIAN_POINT('Ctrl Pts',(0.00724829027087589,-0.0350869349321761,
0.0800164969683543));
#105337=CARTESIAN_POINT('Ctrl Pts',(0.00716702675339849,-0.0349764985129721,
0.0800037943554284));
#105338=CARTESIAN_POINT('Ctrl Pts',(0.00708603073156119,-0.0348659306849651,
0.0799894001131411));
#105339=CARTESIAN_POINT('Ctrl Pts',(0.0073925256199172,-0.0351970973651594,
0.0799744382807117));
#105340=CARTESIAN_POINT('Ctrl Pts',(0.00731183592104986,-0.0350869349321761,
0.0799643077119182));
#105341=CARTESIAN_POINT('Ctrl Pts',(0.00723128998868617,-0.0349764985129722,
0.0799524912569559));
#105342=CARTESIAN_POINT('Ctrl Pts',(0.00715099307359876,-0.0348659306849651,
0.0799389980817598));
#105343=CARTESIAN_POINT('Ctrl Pts',(0.00745533620384681,-0.0351970973651595,
0.0799213788687587));
#105344=CARTESIAN_POINT('Ctrl Pts',(0.00737538157122384,-0.0350869349321761,
0.0799121184554822));
#105345=CARTESIAN_POINT('Ctrl Pts',(0.00729555322397385,-0.0349764985129722,
0.0799011881584834));
#105346=CARTESIAN_POINT('Ctrl Pts',(0.00721595541563633,-0.0348659306849651,
0.0798885960503785));
#105347=CARTESIAN_POINT('Ctrl Pts',(0.00751814678777641,-0.0351970973651595,
0.0798683194568057));
#105348=CARTESIAN_POINT('Ctrl Pts',(0.00743892722139781,-0.0350869349321762,
0.0798599291990462));
#105349=CARTESIAN_POINT('Ctrl Pts',(0.00735981645926153,-0.0349764985129722,
0.0798498850600108));
#105350=CARTESIAN_POINT('Ctrl Pts',(0.0072809177576739,-0.0348659306849651,
0.0798381940189971));
#105351=CARTESIAN_POINT('Origin',(0.0101521302129177,-0.0345637187967259,
0.0633342137964626));
#105352=CARTESIAN_POINT('Ctrl Pts',(0.00755152776053585,-0.0352450361861252,
0.0798728183497645));
#105353=CARTESIAN_POINT('Ctrl Pts',(0.00733568813026428,-0.0349452761023764,
0.079851235420236));
#105354=CARTESIAN_POINT('Ctrl Pts',(0.00712208739215075,-0.0346444289983475,
0.0798134558818566));
#105355=CARTESIAN_POINT('Ctrl Pts',(0.00780076904397632,-0.0352450361861252,
0.0798922806884972));
#105356=CARTESIAN_POINT('Ctrl Pts',(0.0075841953795734,-0.0349452761023764,
0.0798800980479834));
#105357=CARTESIAN_POINT('Ctrl Pts',(0.00736915462442884,-0.0346444289983475,
0.0798516368029356));
#105358=CARTESIAN_POINT('Ctrl Pts',(0.00728139549856233,-0.0345231616327822,
0.0798378524435754));
#105359=CARTESIAN_POINT('Ctrl Pts',(0.00720299646048385,-0.0344132092796975,
0.0798262413289768));
#105360=CARTESIAN_POINT('Ctrl Pts',(0.00712484163418209,-0.0343032738558974,
0.0798130091911959));
#105361=CARTESIAN_POINT('Ctrl Pts',(0.00704703071079267,-0.0341934961088741,
0.0797981755468794));
#105362=CARTESIAN_POINT('Ctrl Pts',(0.00734694889680335,-0.0345231616327822,
0.0799302855984397));
#105363=CARTESIAN_POINT('Ctrl Pts',(0.00726727579782055,-0.0344132092796975,
0.079919578045144));
#105364=CARTESIAN_POINT('Ctrl Pts',(0.00718782828689733,-0.0343032738558974,
0.0799072230691017));
#105365=CARTESIAN_POINT('Ctrl Pts',(0.00710870774003284,-0.0341934961088741,
0.0798932391056347));
#105366=CARTESIAN_POINT('Ctrl Pts',(0.00741250229504438,-0.0345231616327822,
0.080022718753304));
#105367=CARTESIAN_POINT('Ctrl Pts',(0.00733155513515725,-0.0344132092796975,
0.0800129147613113));
#105368=CARTESIAN_POINT('Ctrl Pts',(0.00725081493961256,-0.0343032738558974,
0.0800014369470074));
#105369=CARTESIAN_POINT('Ctrl Pts',(0.00717038476927302,-0.0341934961088741,
0.07998830266439));
#105370=CARTESIAN_POINT('Ctrl Pts',(0.0074780556932854,-0.0345231616327822,
0.0801151519081683));
#105371=CARTESIAN_POINT('Ctrl Pts',(0.00739583447249395,-0.0344132092796975,
0.0801062514774786));
#105372=CARTESIAN_POINT('Ctrl Pts',(0.00731380159232779,-0.0343032738558974,
0.0800956508249132));
#105373=CARTESIAN_POINT('Ctrl Pts',(0.0072320617985132,-0.0341934961088741,
0.0800833662231453));
#105374=CARTESIAN_POINT('Origin',(0.00968602227619365,-0.0345625596230275,
0.0632094918065127));
#105375=CARTESIAN_POINT('Ctrl Pts',(0.00688633205822454,-0.0346945769586889,
0.0800210064864324));
#105376=CARTESIAN_POINT('Ctrl Pts',(0.00680542662135271,-0.0345846629176054,
0.080003953798107));
#105377=CARTESIAN_POINT('Ctrl Pts',(0.0067248600082248,-0.0344746925050312,
0.0799852251059319));
#105378=CARTESIAN_POINT('Ctrl Pts',(0.00664473535096407,-0.0343648066253259,
0.0799648448335961));
#105379=CARTESIAN_POINT('Ctrl Pts',(0.00697733524647039,-0.0346945769586889,
0.0799534821107523));
#105380=CARTESIAN_POINT('Ctrl Pts',(0.00689736032962549,-0.0345846629176054,
0.0799376834923582));
#105381=CARTESIAN_POINT('Ctrl Pts',(0.00681769846180846,-0.0344746925050312,
0.0799202283270848));
#105382=CARTESIAN_POINT('Ctrl Pts',(0.00673845162261766,-0.0343648066253259,
0.0799011394020439));
#105383=CARTESIAN_POINT('Ctrl Pts',(0.00706833843471624,-0.0346945769586889,
0.0798859577350721));
#105384=CARTESIAN_POINT('Ctrl Pts',(0.00698929403789827,-0.0345846629176054,
0.0798714131866095));
#105385=CARTESIAN_POINT('Ctrl Pts',(0.00691053691539213,-0.0344746925050312,
0.0798552315482378));
#105386=CARTESIAN_POINT('Ctrl Pts',(0.00683216789427126,-0.0343648066253259,
0.0798374339704917));
#105387=CARTESIAN_POINT('Ctrl Pts',(0.00715934162296208,-0.0346945769586889,
0.079818433359392));
#105388=CARTESIAN_POINT('Ctrl Pts',(0.00708122774617106,-0.0345846629176054,
0.0798051428808608));
#105389=CARTESIAN_POINT('Ctrl Pts',(0.0070033753689758,-0.0344746925050312,
0.0797902347693907));
#105390=CARTESIAN_POINT('Ctrl Pts',(0.00692588416592485,-0.0343648066253259,
0.0797737285389395));
#105391=CARTESIAN_POINT('Origin',(0.0101621341310956,-0.0345626446731115,
0.0632766459900518));
#105392=CARTESIAN_POINT('Ctrl Pts',(0.00715771327076763,-0.0346945769586885,
0.0798196415968991));
#105393=CARTESIAN_POINT('Ctrl Pts',(0.00703896035752182,-0.0345275153362891,
0.0797994068965281));
#105394=CARTESIAN_POINT('Ctrl Pts',(0.00692081309139195,-0.0343603235965159,
0.0797754322926102));
#105395=CARTESIAN_POINT('Ctrl Pts',(0.0068036198456941,-0.034193496108874,
0.0797477938847791));
#105396=CARTESIAN_POINT('Ctrl Pts',(0.00724064200962563,-0.0346945769586885,
0.0798319238036506));
#105397=CARTESIAN_POINT('Ctrl Pts',(0.00712163184064189,-0.0345275153362891,
0.0798134260789179));
#105398=CARTESIAN_POINT('Ctrl Pts',(0.00700317262594953,-0.0343603235965159,
0.0797911808094528));
#105399=CARTESIAN_POINT('Ctrl Pts',(0.00688561373748634,-0.034193496108874,
0.079765258993998));
#105400=CARTESIAN_POINT('Ctrl Pts',(0.00732357074848363,-0.0346945769586885,
0.0798442060104022));
#105401=CARTESIAN_POINT('Ctrl Pts',(0.00720430332376196,-0.0345275153362891,
0.0798274452613076));
#105402=CARTESIAN_POINT('Ctrl Pts',(0.00708553216050711,-0.0343603235965159,
0.0798069293262955));
#105403=CARTESIAN_POINT('Ctrl Pts',(0.00696760762927858,-0.034193496108874,
0.079782724103217));
#105404=CARTESIAN_POINT('Ctrl Pts',(0.00740649948734163,-0.0346945769586885,
0.0798564882171538));
#105405=CARTESIAN_POINT('Ctrl Pts',(0.00728697480688202,-0.0345275153362891,
0.0798414644436974));
#105406=CARTESIAN_POINT('Ctrl Pts',(0.00716789169506468,-0.0343603235965159,
0.0798226778431382));
#105407=CARTESIAN_POINT('Ctrl Pts',(0.00704960152107082,-0.034193496108874,
0.0798001892124359));
#105408=CARTESIAN_POINT('Ctrl Pts',(0.00692591514389262,-0.0340223579322365,
0.0797737345681123));
#105409=CARTESIAN_POINT('Ctrl Pts',(0.00684834917688344,-0.0339125849573552,
0.0797572128573353));
#105410=CARTESIAN_POINT('Ctrl Pts',(0.00677117967560313,-0.0338030433565217,
0.0797390973208946));
#105411=CARTESIAN_POINT('Ctrl Pts',(0.00669450327320398,-0.0336938721132321,
0.0797194198736759));
#105412=CARTESIAN_POINT('Ctrl Pts',(0.00698553537854258,-0.0340223579322365,
0.0798701016135747));
#105413=CARTESIAN_POINT('Ctrl Pts',(0.00690664025864068,-0.0339125849573552,
0.0798544022213296));
#105414=CARTESIAN_POINT('Ctrl Pts',(0.0068281255183652,-0.0338030433565217,
0.0798370809152107));
#105415=CARTESIAN_POINT('Ctrl Pts',(0.00675008960123868,-0.0336938721132321,
0.0798181687469174));
#105416=CARTESIAN_POINT('Ctrl Pts',(0.00704515561319254,-0.0340223579322365,
0.079966468659037));
#105417=CARTESIAN_POINT('Ctrl Pts',(0.00696493134039792,-0.0339125849573552,
0.0799515915853239));
#105418=CARTESIAN_POINT('Ctrl Pts',(0.00688507136112726,-0.0338030433565217,
0.0799350645095268));
#105419=CARTESIAN_POINT('Ctrl Pts',(0.00680567592927338,-0.0336938721132321,
0.079916917620159));
#105420=CARTESIAN_POINT('Ctrl Pts',(0.0071047758478425,-0.0340223579322365,
0.0800628357044994));
#105421=CARTESIAN_POINT('Ctrl Pts',(0.00702322242215516,-0.0339125849573552,
0.0800487809493182));
#105422=CARTESIAN_POINT('Ctrl Pts',(0.00694201720388932,-0.0338030433565217,
0.0800330481038429));
#105423=CARTESIAN_POINT('Ctrl Pts',(0.00686126225730807,-0.0336938721132321,
0.0800156664934005));
#105424=CARTESIAN_POINT('Origin',(0.00966646514550984,-0.0345589643415296,
0.0633281105098358));
#105425=CARTESIAN_POINT('Ctrl Pts',(0.0065201303359547,-0.034193496108874,
0.0799317212593736));
#105426=CARTESIAN_POINT('Ctrl Pts',(0.00644040382358729,-0.0340836138581107,
0.0799096078499084));
#105427=CARTESIAN_POINT('Ctrl Pts',(0.00636117315610799,-0.0339738896643499,
0.0798858552779883));
#105428=CARTESIAN_POINT('Ctrl Pts',(0.00628253770110186,-0.0338644633294062,
0.0798605007416777));
#105429=CARTESIAN_POINT('Ctrl Pts',(0.00661519398024474,-0.034193496108874,
0.0798700441746387));
#105430=CARTESIAN_POINT('Ctrl Pts',(0.00653631795835211,-0.0340836138581107,
0.0798492416365338));
#105431=CARTESIAN_POINT('Ctrl Pts',(0.00645791024753404,-0.0339738896643499,
0.079826816906109));
#105432=CARTESIAN_POINT('Ctrl Pts',(0.00638006927601672,-0.0338644633294062,
0.0798028054113491));
#105433=CARTESIAN_POINT('Ctrl Pts',(0.00671025762453478,-0.034193496108874,
0.0798083670899038));
#105434=CARTESIAN_POINT('Ctrl Pts',(0.00663223209311692,-0.0340836138581107,
0.0797888754231592));
#105435=CARTESIAN_POINT('Ctrl Pts',(0.00655464733896009,-0.0339738896643499,
0.0797677785342298));
#105436=CARTESIAN_POINT('Ctrl Pts',(0.00647760085093159,-0.0338644633294062,
0.0797451100810205));
#105437=CARTESIAN_POINT('Ctrl Pts',(0.00680532126882482,-0.034193496108874,
0.0797466900051689));
#105438=CARTESIAN_POINT('Ctrl Pts',(0.00672814622788174,-0.0340836138581107,
0.0797285092097846));
#105439=CARTESIAN_POINT('Ctrl Pts',(0.00665138443038615,-0.0339738896643499,
0.0797087401623506));
#105440=CARTESIAN_POINT('Ctrl Pts',(0.00657513242584646,-0.0338644633294062,
0.0796874147506919));
#105441=CARTESIAN_POINT('Origin',(0.0101471443791771,-0.0345610621862551,
0.0633504149063426));
#105442=CARTESIAN_POINT('Ctrl Pts',(0.00683885734612616,-0.03424362768739,
0.0797559872580669));
#105443=CARTESIAN_POINT('Ctrl Pts',(0.00662742405117035,-0.033943005420186,
0.079707525518562));
#105444=CARTESIAN_POINT('Ctrl Pts',(0.00642024175282514,-0.0336441434784162,
0.0796432754316819));
#105445=CARTESIAN_POINT('Ctrl Pts',(0.00708369469966236,-0.03424362768739,
0.079806531004598));
#105446=CARTESIAN_POINT('Ctrl Pts',(0.00687035511588059,-0.033943005420186,
0.0797673034581091));
#105447=CARTESIAN_POINT('Ctrl Pts',(0.00666057638702226,-0.0336441434784162,
0.0797121177413856));
#105448=CARTESIAN_POINT('Ctrl Pts',(0.00657515916624883,-0.0335235895815127,
0.0796874220977052));
#105449=CARTESIAN_POINT('Ctrl Pts',(0.00649892564889411,-0.0334144449262719,
0.0796661022527825));
#105450=CARTESIAN_POINT('Ctrl Pts',(0.00642304500041502,-0.0333049234473133,
0.0796431829868447));
#105451=CARTESIAN_POINT('Ctrl Pts',(0.00634761690359244,-0.0331951640388588,
0.0796186848173753));
#105452=CARTESIAN_POINT('Ctrl Pts',(0.00662861075628238,-0.0335235895815127,
0.0797873425661274));
#105453=CARTESIAN_POINT('Ctrl Pts',(0.00655100163695455,-0.0334144449262719,
0.079766758587578));
#105454=CARTESIAN_POINT('Ctrl Pts',(0.00647372860365686,-0.0333049234473133,
0.0797445476145333));
#105455=CARTESIAN_POINT('Ctrl Pts',(0.00639689303756167,-0.0331951640388588,
0.0797207290975084));
#105456=CARTESIAN_POINT('Ctrl Pts',(0.00668206234631593,-0.0335235895815127,
0.0798872630345496));
#105457=CARTESIAN_POINT('Ctrl Pts',(0.00660307762501498,-0.0334144449262719,
0.0798674149223736));
#105458=CARTESIAN_POINT('Ctrl Pts',(0.0065244122068987,-0.0333049234473133,
0.0798459122422219));
#105459=CARTESIAN_POINT('Ctrl Pts',(0.0064461691715309,-0.0331951640388588,
0.0798227733776415));
#105460=CARTESIAN_POINT('Ctrl Pts',(0.00673551393634947,-0.0335235895815127,
0.0799871835029718));
#105461=CARTESIAN_POINT('Ctrl Pts',(0.00665515361307542,-0.0334144449262719,
0.0799680712571691));
#105462=CARTESIAN_POINT('Ctrl Pts',(0.00657509581014055,-0.0333049234473133,
0.0799472768699105));
#105463=CARTESIAN_POINT('Ctrl Pts',(0.00649544530550012,-0.0331951640388588,
0.0799248176577745));
#105464=CARTESIAN_POINT('Origin',(0.0122146855780136,-0.0326434571770428,
0.0640184173121102));
#105465=CARTESIAN_POINT('Ctrl Pts',(0.00615849062091358,-0.0336938721132461,
0.0798206128038202));
#105466=CARTESIAN_POINT('Ctrl Pts',(0.00612529864246142,-0.0336474569764994,
0.0798091093000944));
#105467=CARTESIAN_POINT('Ctrl Pts',(0.00609224360138026,-0.033601104548885,
0.0797972180305801));
#105468=CARTESIAN_POINT('Ctrl Pts',(0.00600855584080445,-0.0334837508643205,
0.0797671120714434));
#105469=CARTESIAN_POINT('Ctrl Pts',(0.00592579693167301,-0.0333660264760493,
0.0797345394908715));
#105470=CARTESIAN_POINT('Ctrl Pts',(0.00645473649829036,-0.0336938721132461,
0.0796538542375875));
#105471=CARTESIAN_POINT('Ctrl Pts',(0.0064225206130628,-0.0336474569764994,
0.0796440847592869));
#105472=CARTESIAN_POINT('Ctrl Pts',(0.00639042129936673,-0.033601104548885,
0.0796339388227849));
#105473=CARTESIAN_POINT('Ctrl Pts',(0.00630915322069004,-0.0334837508643205,
0.0796082516453673));
#105474=CARTESIAN_POINT('Ctrl Pts',(0.00622868199325349,-0.0333660264760493,
0.0795801676063));
#105475=CARTESIAN_POINT('Ctrl Pts',(0.00645473649829103,-0.0336938721132426,
0.0796538542375947));
#105476=CARTESIAN_POINT('Ctrl Pts',(0.00642252061306816,-0.0336474569765026,
0.0796440847592955));
#105477=CARTESIAN_POINT('Ctrl Pts',(0.00639042129937673,-0.0336011045488949,
0.0796339388227949));
#105478=CARTESIAN_POINT('Ctrl Pts',(0.00630983007310182,-0.0334847282606778,
0.0796084655845773));
#105479=CARTESIAN_POINT('Ctrl Pts',(0.00623002219053035,-0.0333679869945434,
0.0795806351426612));
#105480=CARTESIAN_POINT('Ctrl Pts',(0.00645473649828801,-0.0336938721132428,
0.0796538542375868));
#105481=CARTESIAN_POINT('Ctrl Pts',(0.00633951823577612,-0.0335278710435084,
0.0796189142597623));
#105482=CARTESIAN_POINT('Ctrl Pts',(0.00622543621540167,-0.033362046922432,
0.0795803733589849));
#105483=CARTESIAN_POINT('Ctrl Pts',(0.00611244011171198,-0.0331951640388602,
0.0795381933921867));
#105484=CARTESIAN_POINT('Ctrl Pts',(0.00653547195915288,-0.0336938721132428,
0.0796764333248627));
#105485=CARTESIAN_POINT('Ctrl Pts',(0.00641978102365716,-0.0335278710435084,
0.0796431834716532));
#105486=CARTESIAN_POINT('Ctrl Pts',(0.00630517349471564,-0.033362046922432,
0.0796063172780069));
#105487=CARTESIAN_POINT('Ctrl Pts',(0.00619159850696651,-0.0331951640388602,
0.0795657973463238));
#105488=CARTESIAN_POINT('Ctrl Pts',(0.00661620742001775,-0.0336938721132428,
0.0796990124121386));
#105489=CARTESIAN_POINT('Ctrl Pts',(0.0065000438115382,-0.0335278710435084,
0.079667452683544));
#105490=CARTESIAN_POINT('Ctrl Pts',(0.00638491077402962,-0.033362046922432,
0.0796322611970289));
#105491=CARTESIAN_POINT('Ctrl Pts',(0.00627075690222105,-0.0331951640388602,
0.0795934013004609));
#105492=CARTESIAN_POINT('Ctrl Pts',(0.00669694288088262,-0.0336938721132428,
0.0797215914994144));
#105493=CARTESIAN_POINT('Ctrl Pts',(0.00658030659941925,-0.0335278710435084,
0.0796917218954349));
#105494=CARTESIAN_POINT('Ctrl Pts',(0.00646464805334359,-0.033362046922432,
0.0796582051160508));
#105495=CARTESIAN_POINT('Ctrl Pts',(0.00634991529747558,-0.0331951640388602,
0.079621005254598));
#105496=CARTESIAN_POINT('Ctrl Pts',(0.00623051848003017,-0.0330240426238156,
0.0795792571584604));
#105497=CARTESIAN_POINT('Ctrl Pts',(0.00615572517320382,-0.0329142774063509,
0.0795531756062954));
#105498=CARTESIAN_POINT('Ctrl Pts',(0.00608143375772474,-0.0328043479726686,
0.0795255348649484));
#105499=CARTESIAN_POINT('Ctrl Pts',(0.0060077403816101,-0.0326943950436594,
0.079496367723225));
#105500=CARTESIAN_POINT('Ctrl Pts',(0.00627759048704541,-0.0330240426238156,
0.0796823365557261));
#105501=CARTESIAN_POINT('Ctrl Pts',(0.00620137716109633,-0.0329142774063509,
0.0796569034663178));
#105502=CARTESIAN_POINT('Ctrl Pts',(0.00612565161302665,-0.0328043479726686,
0.079629882155248));
#105503=CARTESIAN_POINT('Ctrl Pts',(0.0060505118062303,-0.0326943950436594,
0.0796013045671887));
#105504=CARTESIAN_POINT('Ctrl Pts',(0.00632466249406064,-0.0330240426238156,
0.0797854159529919));
#105505=CARTESIAN_POINT('Ctrl Pts',(0.00624702914898885,-0.0329142774063509,
0.0797606313263402));
#105506=CARTESIAN_POINT('Ctrl Pts',(0.00616986946832855,-0.0328043479726686,
0.0797342294455475));
#105507=CARTESIAN_POINT('Ctrl Pts',(0.00609328323085051,-0.0326943950436594,
0.0797062414111525));
#105508=CARTESIAN_POINT('Ctrl Pts',(0.00637173450107587,-0.0330240426238156,
0.0798884953502576));
#105509=CARTESIAN_POINT('Ctrl Pts',(0.00629268113688136,-0.0329142774063509,
0.0798643591863626));
#105510=CARTESIAN_POINT('Ctrl Pts',(0.00621408732363045,-0.0328043479726686,
0.0798385767358471));
#105511=CARTESIAN_POINT('Ctrl Pts',(0.00613605465547072,-0.0326943950436594,
0.0798111782551163));
#105512=CARTESIAN_POINT('Origin',(0.0122584163300697,-0.03263966828561,
0.0639027323079114));
#105513=CARTESIAN_POINT('Ctrl Pts',(0.00580813378883238,-0.0331951640388587,
0.079685139787558));
#105514=CARTESIAN_POINT('Ctrl Pts',(0.0057318984357554,-0.0330855618255041,
0.0796532464153077));
#105515=CARTESIAN_POINT('Ctrl Pts',(0.00565626730716548,-0.0329757224427707,
0.0796197543971362));
#105516=CARTESIAN_POINT('Ctrl Pts',(0.00558133935703579,-0.0328657862078596,
0.0795847018708791));
#105517=CARTESIAN_POINT('Ctrl Pts',(0.00591017798772229,-0.0331951640388587,
0.0796358636928203));
#105518=CARTESIAN_POINT('Ctrl Pts',(0.00583462131316559,-0.0330855618255041,
0.0796053757729759));
#105519=CARTESIAN_POINT('Ctrl Pts',(0.005759640304047,-0.0329757224427707,
0.0795733042475063));
#105520=CARTESIAN_POINT('Ctrl Pts',(0.00568533299259563,-0.0328657862078596,
0.0795396854760575));
#105521=CARTESIAN_POINT('Ctrl Pts',(0.0060122221866122,-0.0331951640388587,
0.0795865875980825));
#105522=CARTESIAN_POINT('Ctrl Pts',(0.00593734419057578,-0.0330855618255041,
0.0795575051306441));
#105523=CARTESIAN_POINT('Ctrl Pts',(0.00586301330092851,-0.0329757224427707,
0.0795268540978765));
#105524=CARTESIAN_POINT('Ctrl Pts',(0.00578932662815546,-0.0328657862078596,
0.0794946690812359));
#105525=CARTESIAN_POINT('Ctrl Pts',(0.00611426638550211,-0.0331951640388587,
0.0795373115033448));
#105526=CARTESIAN_POINT('Ctrl Pts',(0.00604006706798597,-0.0330855618255041,
0.0795096344883123));
#105527=CARTESIAN_POINT('Ctrl Pts',(0.00596638629781003,-0.0329757224427707,
0.0794804039482466));
#105528=CARTESIAN_POINT('Ctrl Pts',(0.0058933202637153,-0.0328657862078596,
0.0794496526864143));
#105529=CARTESIAN_POINT('Origin',(0.0126885308057799,-0.0326401908832882,
0.0641178471829243));
#105530=CARTESIAN_POINT('Ctrl Pts',(0.00614630480086988,-0.0332451089994433,
0.0795507136716536));
#105531=CARTESIAN_POINT('Ctrl Pts',(0.0059426135521804,-0.0329451141710259,
0.0794761318915836));
#105532=CARTESIAN_POINT('Ctrl Pts',(0.00574511877339838,-0.0326442513127503,
0.0793864191329318));
#105533=CARTESIAN_POINT('Ctrl Pts',(0.00638287570903076,-0.0332451089994433,
0.0796315481037475));
#105534=CARTESIAN_POINT('Ctrl Pts',(0.00617613573985519,-0.0329451141710259,
0.0795658887414571));
#105535=CARTESIAN_POINT('Ctrl Pts',(0.00597492882869792,-0.0326442513127503,
0.0794848434108475));
#105536=CARTESIAN_POINT('Ctrl Pts',(0.00589334934302681,-0.0325229783203385,
0.0794496650223003));
#105537=CARTESIAN_POINT('Ctrl Pts',(0.00582029357792018,-0.032413025311208,
0.0794189185547979));
#105538=CARTESIAN_POINT('Ctrl Pts',(0.00574788492331688,-0.0323031222247695,
0.0793866654982792));
#105539=CARTESIAN_POINT('Ctrl Pts',(0.0056762146717219,-0.0321934096636184,
0.0793529504394689));
#105540=CARTESIAN_POINT('Ctrl Pts',(0.00593385608274179,-0.0325229783203385,
0.0795554967126749));
#105541=CARTESIAN_POINT('Ctrl Pts',(0.0058593414301243,-0.032413025311208,
0.0795253086296835));
#105542=CARTESIAN_POINT('Ctrl Pts',(0.0057854625583783,-0.0323031222247695,
0.0794935836940241));
#105543=CARTESIAN_POINT('Ctrl Pts',(0.0057123126671233,-0.0321934096636184,
0.0794603658823897));
#105544=CARTESIAN_POINT('Ctrl Pts',(0.00597436282245677,-0.0325229783203385,
0.0796613284030495));
#105545=CARTESIAN_POINT('Ctrl Pts',(0.00589838928232841,-0.032413025311208,
0.0796316987045691));
#105546=CARTESIAN_POINT('Ctrl Pts',(0.00582304019343971,-0.0323031222247695,
0.079600501889769));
#105547=CARTESIAN_POINT('Ctrl Pts',(0.00574841066252471,-0.0321934096636184,
0.0795677813253106));
#105548=CARTESIAN_POINT('Ctrl Pts',(0.00601486956217176,-0.0325229783203385,
0.0797671600934241));
#105549=CARTESIAN_POINT('Ctrl Pts',(0.00593743713453252,-0.032413025311208,
0.0797380887794547));
#105550=CARTESIAN_POINT('Ctrl Pts',(0.00586061782850113,-0.0323031222247695,
0.079707420085514));
#105551=CARTESIAN_POINT('Ctrl Pts',(0.00578450865792611,-0.0321934096636184,
0.0796751967682314));
#105552=CARTESIAN_POINT('Origin',(0.0122550062864071,-0.0326393375177815,
0.0639105465657135));
#105553=CARTESIAN_POINT('Ctrl Pts',(0.00546514888907057,-0.0326943950436593,
0.079528816687218));
#105554=CARTESIAN_POINT('Ctrl Pts',(0.00539101871414405,-0.0325844576448126,
0.0794921757374785));
#105555=CARTESIAN_POINT('Ctrl Pts',(0.00531764108782414,-0.0324744968375319,
0.0794539990610467));
#105556=CARTESIAN_POINT('Ctrl Pts',(0.00524510935113126,-0.0323646534831894,
0.0794143368688656));
#105557=CARTESIAN_POINT('Ctrl Pts',(0.00557008569869822,-0.0326943950436593,
0.0794860452765929));
#105558=CARTESIAN_POINT('Ctrl Pts',(0.00549654499397228,-0.0325844576448127,
0.0794508505527627));
#105559=CARTESIAN_POINT('Ctrl Pts',(0.00542372696924775,-0.0324744968375319,
0.0794141323958019));
#105560=CARTESIAN_POINT('Ctrl Pts',(0.00535172427432639,-0.0323646534831894,
0.079375939138024));
#105561=CARTESIAN_POINT('Ctrl Pts',(0.00567502250832588,-0.0326943950436593,
0.0794432738659678));
#105562=CARTESIAN_POINT('Ctrl Pts',(0.00560207127380052,-0.0325844576448127,
0.0794095253680468));
#105563=CARTESIAN_POINT('Ctrl Pts',(0.00552981285067137,-0.0324744968375319,
0.079374265730557));
#105564=CARTESIAN_POINT('Ctrl Pts',(0.00545833919752153,-0.0323646534831894,
0.0793375414071823));
#105565=CARTESIAN_POINT('Ctrl Pts',(0.00577995931795353,-0.0326943950436594,
0.0794005024553427));
#105566=CARTESIAN_POINT('Ctrl Pts',(0.00570759755362875,-0.0325844576448127,
0.0793682001833309));
#105567=CARTESIAN_POINT('Ctrl Pts',(0.00563589873209498,-0.0324744968375319,
0.0793343990653122));
#105568=CARTESIAN_POINT('Ctrl Pts',(0.00556495412071667,-0.0323646534831894,
0.0792991436763407));
#105569=CARTESIAN_POINT('Origin',(0.0127037850083422,-0.0326395579068186,
0.0640832166883785));
#105570=CARTESIAN_POINT('Ctrl Pts',(0.00581112919608697,-0.0327445246961877,
0.0794159055361228));
#105571=CARTESIAN_POINT('Ctrl Pts',(0.00561252232407842,-0.0324436878365475,
0.0793286824033436));
#105572=CARTESIAN_POINT('Ctrl Pts',(0.00542104967598372,-0.0321434074463186,
0.0792267471811069));
#105573=CARTESIAN_POINT('Ctrl Pts',(0.00604215830110225,-0.0327445246961877,
0.0795114332945799));
#105574=CARTESIAN_POINT('Ctrl Pts',(0.00583994854082175,-0.0324436878365475,
0.0794329235668505));
#105575=CARTESIAN_POINT('Ctrl Pts',(0.00564422691060632,-0.0321434074463186,
0.0793394056115336));
#105576=CARTESIAN_POINT('Ctrl Pts',(0.0054800754633449,-0.0322357242816072,
0.0792577333257527));
#105577=CARTESIAN_POINT('Ctrl Pts',(0.00531740078140711,-0.0319819883628705,
0.0791735346951717));
#105578=CARTESIAN_POINT('Ctrl Pts',(0.00516041357963271,-0.0317295851069886,
0.0790791552481808));
#105579=CARTESIAN_POINT('Ctrl Pts',(0.0057045435216485,-0.0322357242816072,
0.079367797356214));
#105580=CARTESIAN_POINT('Ctrl Pts',(0.00553836344308834,-0.0319819883628705,
0.0792907477421656));
#105581=CARTESIAN_POINT('Ctrl Pts',(0.0053774230364393,-0.0317295851069886,
0.079203279764923));
#105582=CARTESIAN_POINT('Origin',(0.0126627740881763,-0.0326371942646596,
0.0641692428934363));
#105583=CARTESIAN_POINT('Origin',(0.0122063950829564,-0.0326352985529098,
0.0640232441872437));
#105584=CARTESIAN_POINT('Ctrl Pts',(0.00513265640034522,-0.0321934096636183,
0.0793512658547612));
#105585=CARTESIAN_POINT('Ctrl Pts',(0.00506092689058805,-0.0320835708272303,
0.0793100158989374));
#105586=CARTESIAN_POINT('Ctrl Pts',(0.00499009265255341,-0.0319739230346346,
0.0792673054312881));
#105587=CARTESIAN_POINT('Ctrl Pts',(0.00492024011987723,-0.0318646057455575,
0.0792231960523004));
#105588=CARTESIAN_POINT('Ctrl Pts',(0.00524007193576123,-0.0321934096636183,
0.0793151678282759));
#105589=CARTESIAN_POINT('Ctrl Pts',(0.00516884024592239,-0.0320835708272303,
0.0792753992164001));
#105590=CARTESIAN_POINT('Ctrl Pts',(0.00509847288271428,-0.0319739230346346,
0.0792341795358164));
#105591=CARTESIAN_POINT('Ctrl Pts',(0.00502905582882334,-0.0318646057455575,
0.0791915684338096));
#105592=CARTESIAN_POINT('Ctrl Pts',(0.00534748747117725,-0.0321934096636183,
0.0792790698017906));
#105593=CARTESIAN_POINT('Ctrl Pts',(0.00527675360125673,-0.0320835708272303,
0.0792407825338627));
#105594=CARTESIAN_POINT('Ctrl Pts',(0.00520685311287515,-0.0319739230346346,
0.0792010536403447));
#105595=CARTESIAN_POINT('Ctrl Pts',(0.00513787153776944,-0.0318646057455575,
0.0791599408153188));
#105596=CARTESIAN_POINT('Ctrl Pts',(0.00545490300659327,-0.0321934096636183,
0.0792429717753053));
#105597=CARTESIAN_POINT('Ctrl Pts',(0.00538466695659108,-0.0320835708272303,
0.0792061658513254));
#105598=CARTESIAN_POINT('Ctrl Pts',(0.00531523334303603,-0.0319739230346346,
0.0791679277448729));
#105599=CARTESIAN_POINT('Ctrl Pts',(0.00524668724671554,-0.0318646057455575,
0.079128313196828));
#105600=CARTESIAN_POINT('Ctrl Pts',(0.00556500657548765,-0.032021883458237,
0.0793000937019742));
#105601=CARTESIAN_POINT('Ctrl Pts',(0.0055114065503203,-0.0319391099350643,
0.0792734630335944));
#105602=CARTESIAN_POINT('Ctrl Pts',(0.0054582548416672,-0.0318564869454901,
0.0792460115281513));
#105603=CARTESIAN_POINT('Ctrl Pts',(0.00540558829684642,-0.0317740741446471,
0.0792177627946431));
#105604=CARTESIAN_POINT('Ctrl Pts',(0.00557977995831009,-0.032021883458237,
0.0793474072857285));
#105605=CARTESIAN_POINT('Ctrl Pts',(0.0055256875131157,-0.0319391099350643,
0.0793209303725494));
#105606=CARTESIAN_POINT('Ctrl Pts',(0.00547204128187133,-0.0318564869454901,
0.079293624839943));
#105607=CARTESIAN_POINT('Ctrl Pts',(0.00541887848201503,-0.0317740741446471,
0.0792655142242119));
#105608=CARTESIAN_POINT('Ctrl Pts',(0.00559455334113253,-0.032021883458237,
0.0793947208694827));
#105609=CARTESIAN_POINT('Ctrl Pts',(0.0055399684759111,-0.0319391099350643,
0.0793683977115044));
#105610=CARTESIAN_POINT('Ctrl Pts',(0.00548582772207545,-0.0318564869454901,
0.0793412381517346));
#105611=CARTESIAN_POINT('Ctrl Pts',(0.00543216866718363,-0.0317740741446471,
0.0793132656537809));
#105612=CARTESIAN_POINT('Ctrl Pts',(0.00560932672395496,-0.032021883458237,
0.079442034453237));
#105613=CARTESIAN_POINT('Ctrl Pts',(0.00555424943870649,-0.0319391099350643,
0.0794158650504595));
#105614=CARTESIAN_POINT('Ctrl Pts',(0.00549961416227957,-0.0318564869454901,
0.0793888514635263));
#105615=CARTESIAN_POINT('Ctrl Pts',(0.00544545885235224,-0.0317740741446471,
0.0793610170833498));
#105616=CARTESIAN_POINT('Origin',(0.00360949835450093,-0.0391228853390903,
0.0853527612558224));
#105617=CARTESIAN_POINT('Ctrl Pts',(0.00854323475386372,-0.0352722978779658,
0.0798865690174418));
#105618=CARTESIAN_POINT('Ctrl Pts',(0.00852436587356845,-0.0352466642097259,
0.0798875976254809));
#105619=CARTESIAN_POINT('Ctrl Pts',(0.008505518070848,-0.0352210183808322,
0.0798887036019082));
#105620=CARTESIAN_POINT('Ctrl Pts',(0.00848669071177818,-0.0351953608940152,
0.0798898875173587));
#105621=CARTESIAN_POINT('Origin',(0.00862888701976859,-0.0352456003065125,
0.084785794148498));
#105622=CARTESIAN_POINT('Ctrl Pts',(0.00836211277690418,-0.0350241211493338,
0.0798949524517777));
#105623=CARTESIAN_POINT('Ctrl Pts',(0.00828297841597139,-0.034914423286742,
0.0798982353577021));
#105624=CARTESIAN_POINT('Ctrl Pts',(0.00820372882930312,-0.0348045283677512,
0.0798998844648908));
#105625=CARTESIAN_POINT('Ctrl Pts',(0.00812446544693723,-0.0346945769586886,
0.079899893883675));
#105626=CARTESIAN_POINT('Ctrl Pts',(0.00844382529575833,-0.0350241211493338,
0.0799734649098091));
#105627=CARTESIAN_POINT('Ctrl Pts',(0.00836360945795629,-0.034914423286742,
0.0799778733721265));
#105628=CARTESIAN_POINT('Ctrl Pts',(0.00828325448104889,-0.0348045283677512,
0.0799806263545093));
#105629=CARTESIAN_POINT('Ctrl Pts',(0.00820286315832291,-0.0346945769586886,
0.0799817165006773));
#105630=CARTESIAN_POINT('Ctrl Pts',(0.00852553781461249,-0.0350241211493338,
0.0800519773678404));
#105631=CARTESIAN_POINT('Ctrl Pts',(0.00844424049994119,-0.034914423286742,
0.0800575113865509));
#105632=CARTESIAN_POINT('Ctrl Pts',(0.00836278013279466,-0.0348045283677512,
0.0800613682441279));
#105633=CARTESIAN_POINT('Ctrl Pts',(0.00828126086970859,-0.0346945769586886,
0.0800635391176797));
#105634=CARTESIAN_POINT('Ctrl Pts',(0.00860725033346665,-0.0350241211493338,
0.0801304898258718));
#105635=CARTESIAN_POINT('Ctrl Pts',(0.0085248715419261,-0.034914423286742,
0.0801371494009753));
#105636=CARTESIAN_POINT('Ctrl Pts',(0.00844230578454043,-0.0348045283677512,
0.0801421101337464));
#105637=CARTESIAN_POINT('Ctrl Pts',(0.00835965858109427,-0.0346945769586886,
0.080145361734682));
#105638=CARTESIAN_POINT('Origin',(0.00830254879793467,-0.0345629067941517,
0.0631120639048819));
#105639=CARTESIAN_POINT('Ctrl Pts',(0.00807262228378706,-0.0351970973651502,
0.0800806748722953));
#105640=CARTESIAN_POINT('Ctrl Pts',(0.00799046082130408,-0.0350869349326827,
0.0800799661210889));
#105641=CARTESIAN_POINT('Ctrl Pts',(0.00790824603176679,-0.034976498513997,
0.0800775486914956));
#105642=CARTESIAN_POINT('Ctrl Pts',(0.00782608461120774,-0.0348659306865088,
0.0800734194454661));
#105643=CARTESIAN_POINT('Ctrl Pts',(0.00812828747982777,-0.0351970973651502,
0.080020161596071));
#105644=CARTESIAN_POINT('Ctrl Pts',(0.00804696434677294,-0.0350869349326827,
0.0800202240107124));
#105645=CARTESIAN_POINT('Ctrl Pts',(0.00796557254901559,-0.034976498513997,
0.0800185958141959));
#105646=CARTESIAN_POINT('Ctrl Pts',(0.00788421765618942,-0.0348659306865088,
0.0800152729087609));
#105647=CARTESIAN_POINT('Ctrl Pts',(0.00818395267586848,-0.0351970973651502,
0.0799596483198466));
#105648=CARTESIAN_POINT('Ctrl Pts',(0.0081034678722418,-0.0350869349326827,
0.0799604819003359));
#105649=CARTESIAN_POINT('Ctrl Pts',(0.00802289906626439,-0.034976498513997,
0.0799596429368962));
#105650=CARTESIAN_POINT('Ctrl Pts',(0.00794235070117111,-0.0348659306865088,
0.0799571263720558));
#105651=CARTESIAN_POINT('Ctrl Pts',(0.00823961787190918,-0.0351970973651502,
0.0798991350436223));
#105652=CARTESIAN_POINT('Ctrl Pts',(0.00815997139771065,-0.0350869349326827,
0.0799007397899595));
#105653=CARTESIAN_POINT('Ctrl Pts',(0.00808022558351319,-0.034976498513997,
0.0799006900595965));
#105654=CARTESIAN_POINT('Ctrl Pts',(0.00800048374615279,-0.0348659306865088,
0.0798989798353506));
#105655=CARTESIAN_POINT('Origin',(0.00878055862465359,-0.0345637187966198,
0.0631652800849412));
#105656=CARTESIAN_POINT('Ctrl Pts',(0.00827329948653789,-0.0352450361861252,
0.0798994147162095));
#105657=CARTESIAN_POINT('Ctrl Pts',(0.00805645675787159,-0.0349452761023764,
0.07990505385332));
#105658=CARTESIAN_POINT('Ctrl Pts',(0.00783980529366988,-0.0346444289983475,
0.0798943434890843));
#105659=CARTESIAN_POINT('Ctrl Pts',(0.00852301470585977,-0.0352450361861252,
0.0798874853725969));
#105660=CARTESIAN_POINT('Ctrl Pts',(0.00830662189975912,-0.0349452761023764,
0.0799025426735067));
#105661=CARTESIAN_POINT('Ctrl Pts',(0.00808970966532535,-0.0346444289983475,
0.0799012576070674));
#105662=CARTESIAN_POINT('Ctrl Pts',(0.00800091490804747,-0.0345231616327821,
0.0798985810765177));
#105663=CARTESIAN_POINT('Ctrl Pts',(0.00792167881126297,-0.0344132092796975,
0.0798968875239764));
#105664=CARTESIAN_POINT('Ctrl Pts',(0.00784248183249529,-0.0343032738558973,
0.0798935551226533));
#105665=CARTESIAN_POINT('Ctrl Pts',(0.00776342532287004,-0.034193496108874,
0.0798885907406878));
#105666=CARTESIAN_POINT('Ctrl Pts',(0.00807753634435134,-0.0345231616327821,
0.0799820693489749));
#105667=CARTESIAN_POINT('Ctrl Pts',(0.00799714947927311,-0.0344132092796975,
0.0799814319150588));
#105668=CARTESIAN_POINT('Ctrl Pts',(0.00791677994660534,-0.0343032738558973,
0.0799791317751354));
#105669=CARTESIAN_POINT('Ctrl Pts',(0.00783653063352568,-0.034193496108874,
0.079975174513377));
#105670=CARTESIAN_POINT('Ctrl Pts',(0.00815415778065521,-0.0345231616327821,
0.0800655576214321));
#105671=CARTESIAN_POINT('Ctrl Pts',(0.00807262014728325,-0.0344132092796975,
0.0800659763061411));
#105672=CARTESIAN_POINT('Ctrl Pts',(0.0079910780607154,-0.0343032738558973,
0.0800647084276175));
#105673=CARTESIAN_POINT('Ctrl Pts',(0.00790963594418132,-0.034193496108874,
0.0800617582860662));
#105674=CARTESIAN_POINT('Ctrl Pts',(0.00823077921695908,-0.0345231616327821,
0.0801490458938894));
#105675=CARTESIAN_POINT('Ctrl Pts',(0.00814809081529339,-0.0344132092796975,
0.0801505206972234));
#105676=CARTESIAN_POINT('Ctrl Pts',(0.00806537617482546,-0.0343032738558973,
0.0801502850800996));
#105677=CARTESIAN_POINT('Ctrl Pts',(0.00798274125483696,-0.034193496108874,
0.0801483420587555));
#105678=CARTESIAN_POINT('Origin',(0.00830249427756325,-0.034562559623222,
0.0630999603790713));
#105679=CARTESIAN_POINT('Ctrl Pts',(0.00763192194936664,-0.0346945769586885,
0.080129805473483));
#105680=CARTESIAN_POINT('Ctrl Pts',(0.00754951720746111,-0.0345846629176052,
0.0801230273907144));
#105681=CARTESIAN_POINT('Ctrl Pts',(0.00746723855859114,-0.0344746925050311,
0.0801145440540118));
#105682=CARTESIAN_POINT('Ctrl Pts',(0.00738519138275229,-0.0343648066253259,
0.0801043667685933));
#105683=CARTESIAN_POINT('Ctrl Pts',(0.00771374450194384,-0.0346945769586885,
0.0800514078238258));
#105684=CARTESIAN_POINT('Ctrl Pts',(0.00763242011927652,-0.0345846629176052,
0.0800457572971887));
#105685=CARTESIAN_POINT('Ctrl Pts',(0.00755119869677504,-0.0344746925050311,
0.0800384240505924));
#105686=CARTESIAN_POINT('Ctrl Pts',(0.00747018426588057,-0.0343648066253259,
0.0800294179100325));
#105687=CARTESIAN_POINT('Ctrl Pts',(0.00779556705452104,-0.0346945769586885,
0.0799730101741685));
#105688=CARTESIAN_POINT('Ctrl Pts',(0.00771532303109194,-0.0345846629176052,
0.0799684872036631));
#105689=CARTESIAN_POINT('Ctrl Pts',(0.00763515883495895,-0.0344746925050311,
0.079962304047173));
#105690=CARTESIAN_POINT('Ctrl Pts',(0.00755517714900886,-0.0343648066253259,
0.0799544690514716));
#105691=CARTESIAN_POINT('Ctrl Pts',(0.00787738960709824,-0.0346945769586885,
0.0798946125245113));
#105692=CARTESIAN_POINT('Ctrl Pts',(0.00779822594290735,-0.0345846629176052,
0.0798912171101374));
#105693=CARTESIAN_POINT('Ctrl Pts',(0.00771911897314285,-0.0344746925050311,
0.0798861840437536));
#105694=CARTESIAN_POINT('Ctrl Pts',(0.00764017003213714,-0.0343648066253259,
0.0798795201929108));
#105695=CARTESIAN_POINT('Origin',(0.0087832684994177,-0.0345626446731317,
0.0631069123950791));
#105696=CARTESIAN_POINT('Ctrl Pts',(0.00787592552726108,-0.0346945769586885,
0.0798960153213506));
#105697=CARTESIAN_POINT('Ctrl Pts',(0.00775557293577831,-0.034527515336289,
0.0798908238642481));
#105698=CARTESIAN_POINT('Ctrl Pts',(0.00763535248149831,-0.0343603235965159,
0.0798818460861438));
#105699=CARTESIAN_POINT('Ctrl Pts',(0.0075156193285227,-0.034193496108874,
0.0798691138238489));
#105700=CARTESIAN_POINT('Ctrl Pts',(0.00795973971693108,-0.0346945769586885,
0.0798978069522369));
#105701=CARTESIAN_POINT('Ctrl Pts',(0.00783934959902206,-0.034527515336289,
0.0798943710168944));
#105702=CARTESIAN_POINT('Ctrl Pts',(0.00771903639906606,-0.0343603235965159,
0.0798871480344464));
#105703=CARTESIAN_POINT('Ctrl Pts',(0.00759915563260076,-0.034193496108874,
0.0798761646558743));
#105704=CARTESIAN_POINT('Ctrl Pts',(0.00804355390660107,-0.0346945769586885,
0.0798995985831233));
#105705=CARTESIAN_POINT('Ctrl Pts',(0.00792312626226581,-0.034527515336289,
0.0798979181695408));
#105706=CARTESIAN_POINT('Ctrl Pts',(0.00780272031663381,-0.0343603235965159,
0.0798924499827489));
#105707=CARTESIAN_POINT('Ctrl Pts',(0.00768269193667881,-0.034193496108874,
0.0798832154878996));
#105708=CARTESIAN_POINT('Ctrl Pts',(0.00812736809627107,-0.0346945769586885,
0.0799013902140096));
#105709=CARTESIAN_POINT('Ctrl Pts',(0.00800690292550956,-0.034527515336289,
0.0799014653221871));
#105710=CARTESIAN_POINT('Ctrl Pts',(0.00788640423420156,-0.0343603235965159,
0.0798977519310515));
#105711=CARTESIAN_POINT('Ctrl Pts',(0.00776622824075686,-0.034193496108874,
0.0798902663199249));
#105712=CARTESIAN_POINT('Ctrl Pts',(0.00764020152149013,-0.0340223579322366,
0.0798795222919731));
#105713=CARTESIAN_POINT('Ctrl Pts',(0.00756117646586297,-0.0339125849573552,
0.0798728524532801));
#105714=CARTESIAN_POINT('Ctrl Pts',(0.0074823449903898,-0.0338030433565217,
0.0798645516663831));
#105715=CARTESIAN_POINT('Ctrl Pts',(0.00740380696623747,-0.0336938721132321,
0.0798546394831638));
#105716=CARTESIAN_POINT('Ctrl Pts',(0.00771142962619917,-0.0340223579322366,
0.0799676570577041));
#105717=CARTESIAN_POINT('Ctrl Pts',(0.00763118896228746,-0.0339125849573552,
0.0799619696403458));
#105718=CARTESIAN_POINT('Ctrl Pts',(0.00755112239888483,-0.0338030433565217,
0.0799546254241805));
#105719=CARTESIAN_POINT('Ctrl Pts',(0.00747133149506713,-0.0336938721132321,
0.0799456428778106));
#105720=CARTESIAN_POINT('Ctrl Pts',(0.0077826577309082,-0.0340223579322366,
0.0800557918234352));
#105721=CARTESIAN_POINT('Ctrl Pts',(0.00770120145871196,-0.0339125849573552,
0.0800510868274115));
#105722=CARTESIAN_POINT('Ctrl Pts',(0.00761989980737985,-0.0338030433565217,
0.0800446991819779));
#105723=CARTESIAN_POINT('Ctrl Pts',(0.00753885602389679,-0.0336938721132321,
0.0800366462724574));
#105724=CARTESIAN_POINT('Ctrl Pts',(0.00785388583561724,-0.0340223579322366,
0.0801439265891663));
#105725=CARTESIAN_POINT('Ctrl Pts',(0.00777121395513645,-0.0339125849573552,
0.0801402040144772));
#105726=CARTESIAN_POINT('Ctrl Pts',(0.00768867721587487,-0.0338030433565217,
0.0801347729397753));
#105727=CARTESIAN_POINT('Ctrl Pts',(0.00760638055272644,-0.0336938721132321,
0.0801276496671042));
#105728=CARTESIAN_POINT('Origin',(0.00829795822678823,-0.0345589643414324,
0.0632200948973638));
#105729=CARTESIAN_POINT('Ctrl Pts',(0.00725741743083934,-0.034193496108874,
0.0800871215330967));
#105730=CARTESIAN_POINT('Ctrl Pts',(0.00717554804072168,-0.0340836138581107,
0.0800751748760659));
#105731=CARTESIAN_POINT('Ctrl Pts',(0.00709396514407627,-0.03397388966435,
0.0800615398360225));
#105732=CARTESIAN_POINT('Ctrl Pts',(0.00701277198709879,-0.0338644633294062,
0.0800462408636525));
#105733=CARTESIAN_POINT('Ctrl Pts',(0.00734400128143384,-0.034193496108874,
0.0800140161566633));
#105734=CARTESIAN_POINT('Ctrl Pts',(0.00726313997116592,-0.0340836138581107,
0.0800032634396592));
#105735=CARTESIAN_POINT('Ctrl Pts',(0.00718253996459094,-0.03397388966435,
0.079990842626865));
#105736=CARTESIAN_POINT('Ctrl Pts',(0.00710230335410302,-0.0338644633294062,
0.0799767765305772));
#105737=CARTESIAN_POINT('Ctrl Pts',(0.00743058513202835,-0.034193496108874,
0.0799409107802299));
#105738=CARTESIAN_POINT('Ctrl Pts',(0.00735073190161015,-0.0340836138581107,
0.0799313520032526));
#105739=CARTESIAN_POINT('Ctrl Pts',(0.00727111478510562,-0.03397388966435,
0.0799201454177075));
#105740=CARTESIAN_POINT('Ctrl Pts',(0.00719183472110726,-0.0338644633294062,
0.0799073121975019));
#105741=CARTESIAN_POINT('Ctrl Pts',(0.00751716898262285,-0.034193496108874,
0.0798678054037965));
#105742=CARTESIAN_POINT('Ctrl Pts',(0.00743832383205439,-0.0340836138581107,
0.0798594405668459));
#105743=CARTESIAN_POINT('Ctrl Pts',(0.00735968960562029,-0.03397388966435,
0.07984944820855));
#105744=CARTESIAN_POINT('Ctrl Pts',(0.00728136608811149,-0.0338644633294062,
0.0798378478644266));
#105745=CARTESIAN_POINT('Origin',(0.00877764264291297,-0.0345610621863865,
0.0631819783347345));
#105746=CARTESIAN_POINT('Ctrl Pts',(0.00755160587270691,-0.03424362768739,
0.0798728261600692));
#105747=CARTESIAN_POINT('Ctrl Pts',(0.00733576592591758,-0.033943005420186,
0.0798512461743951));
#105748=CARTESIAN_POINT('Ctrl Pts',(0.00712216465073168,-0.0336441434784162,
0.0798134695460296));
#105749=CARTESIAN_POINT('Ctrl Pts',(0.00780084742177028,-0.03424362768739,
0.0798922850968461));
#105750=CARTESIAN_POINT('Ctrl Pts',(0.00758427356908182,-0.033943005420186,
0.0798801054111607));
#105751=CARTESIAN_POINT('Ctrl Pts',(0.00736923240383486,-0.0336441434784162,
0.0798516470967176));
#105752=CARTESIAN_POINT('Ctrl Pts',(0.00728139353848262,-0.0335235895815127,
0.0798378518020453));
#105753=CARTESIAN_POINT('Ctrl Pts',(0.00720308906007888,-0.0334144449262719,
0.0798262546637039));
#105754=CARTESIAN_POINT('Ctrl Pts',(0.00712493420746662,-0.0333049234473133,
0.0798130264900625));
#105755=CARTESIAN_POINT('Ctrl Pts',(0.0070470304489208,-0.0331951640388588,
0.0797981751432531));
#105756=CARTESIAN_POINT('Ctrl Pts',(0.00734694700217044,-0.0335235895815127,
0.0799302851071116));
#105757=CARTESIAN_POINT('Ctrl Pts',(0.00726736999733805,-0.0334144449262719,
0.0799195904412607));
#105758=CARTESIAN_POINT('Ctrl Pts',(0.00718792251191598,-0.0333049234473133,
0.0799072394875031));
#105759=CARTESIAN_POINT('Ctrl Pts',(0.00710870756545171,-0.0331951640388588,
0.0798932388365506));
#105760=CARTESIAN_POINT('Ctrl Pts',(0.00741250046585826,-0.0335235895815127,
0.0800227184121778));
#105761=CARTESIAN_POINT('Ctrl Pts',(0.00733165093459722,-0.0334144449262719,
0.0800129262188175));
#105762=CARTESIAN_POINT('Ctrl Pts',(0.00725091081636533,-0.0333049234473133,
0.0800014524849436));
#105763=CARTESIAN_POINT('Ctrl Pts',(0.00717038468198261,-0.0331951640388588,
0.0799883025298482));
#105764=CARTESIAN_POINT('Ctrl Pts',(0.00747805392954608,-0.0335235895815127,
0.0801151517172441));
#105765=CARTESIAN_POINT('Ctrl Pts',(0.00739593187185639,-0.0334144449262719,
0.0801062619963743));
#105766=CARTESIAN_POINT('Ctrl Pts',(0.00731389912081469,-0.0333049234473133,
0.0800956654823841));
#105767=CARTESIAN_POINT('Ctrl Pts',(0.00723206179851352,-0.0331951640388588,
0.0800833662231457));
#105768=CARTESIAN_POINT('Origin',(0.0109126035636551,-0.0326434571769533,
0.0635855817183451));
#105769=CARTESIAN_POINT('Ctrl Pts',(0.00688470377095714,-0.0336938721132463,
0.0800222146757731));
#105770=CARTESIAN_POINT('Ctrl Pts',(0.00685033174984972,-0.0336474569764994,
0.0800149619385979));
#105771=CARTESIAN_POINT('Ctrl Pts',(0.00681604698638109,-0.033601104548885,
0.0800073073304798));
#105772=CARTESIAN_POINT('Ctrl Pts',(0.0067292458553903,-0.0334837508694645,
0.0799879276243151));
#105773=CARTESIAN_POINT('Ctrl Pts',(0.00664305710187704,-0.0333660264863674,
0.0799659843310315));
#105774=CARTESIAN_POINT('Ctrl Pts',(0.00715771327077731,-0.0336938721132463,
0.0798196415969008));
#105775=CARTESIAN_POINT('Ctrl Pts',(0.00712452697712149,-0.0336474569764994,
0.0798139868749222));
#105776=CARTESIAN_POINT('Ctrl Pts',(0.00709140915307214,-0.033601104548885,
0.0798079440529407));
#105777=CARTESIAN_POINT('Ctrl Pts',(0.00700756244413778,-0.0334837508694645,
0.0797926450183462));
#105778=CARTESIAN_POINT('Ctrl Pts',(0.00692420589656798,-0.0333660264863674,
0.0797748681503462));
#105779=CARTESIAN_POINT('Ctrl Pts',(0.00715771327077761,-0.0336938721132426,
0.079819641596909));
#105780=CARTESIAN_POINT('Ctrl Pts',(0.00712452697712665,-0.0336474569765026,
0.0798139868749313));
#105781=CARTESIAN_POINT('Ctrl Pts',(0.00709140915308214,-0.0336011045488949,
0.0798079440529507));
#105782=CARTESIAN_POINT('Ctrl Pts',(0.0070082607730359,-0.033484728265791,
0.0797927724384774));
#105783=CARTESIAN_POINT('Ctrl Pts',(0.00692559412378843,-0.0333679870047995,
0.0797751640287754));
#105784=CARTESIAN_POINT('Ctrl Pts',(0.00715771327077482,-0.0336938721132428,
0.0798196415969002));
#105785=CARTESIAN_POINT('Ctrl Pts',(0.00703902439827544,-0.0335278710435084,
0.0797994178086434));
#105786=CARTESIAN_POINT('Ctrl Pts',(0.00692101149298736,-0.033362046922432,
0.0797754790828853));
#105787=CARTESIAN_POINT('Ctrl Pts',(0.00680361984569509,-0.0331951640388602,
0.0797477938847794));
#105788=CARTESIAN_POINT('Ctrl Pts',(0.00724064201843547,-0.0336938721132428,
0.0798319238049554));
#105789=CARTESIAN_POINT('Ctrl Pts',(0.00712169602890304,-0.0335278710435084,
0.0798134360558096));
#105790=CARTESIAN_POINT('Ctrl Pts',(0.00700337165529993,-0.033362046922432,
0.0797912246953047));
#105791=CARTESIAN_POINT('Ctrl Pts',(0.00688561374619074,-0.0331951640388602,
0.0797652589958522));
#105792=CARTESIAN_POINT('Ctrl Pts',(0.00732357076609612,-0.0336938721132428,
0.0798442060130106));
#105793=CARTESIAN_POINT('Ctrl Pts',(0.00720436765953065,-0.0335278710435084,
0.0798274543029757));
#105794=CARTESIAN_POINT('Ctrl Pts',(0.00708573181761249,-0.033362046922432,
0.079806970307724));
#105795=CARTESIAN_POINT('Ctrl Pts',(0.00696760764668638,-0.0331951640388602,
0.079782724106925));
#105796=CARTESIAN_POINT('Ctrl Pts',(0.00740649951375678,-0.0336938721132428,
0.0798564882210658));
#105797=CARTESIAN_POINT('Ctrl Pts',(0.00728703929015824,-0.0335278710435084,
0.0798414725501419));
#105798=CARTESIAN_POINT('Ctrl Pts',(0.00716809197992505,-0.033362046922432,
0.0798227159201434));
#105799=CARTESIAN_POINT('Ctrl Pts',(0.00704960154718203,-0.0331951640388602,
0.0798001892179978));
#105800=CARTESIAN_POINT('Ctrl Pts',(0.00692591378542022,-0.0330240426238155,
0.0797737347072755));
#105801=CARTESIAN_POINT('Ctrl Pts',(0.00684844136088866,-0.0329142774063509,
0.0797572329029329));
#105802=CARTESIAN_POINT('Ctrl Pts',(0.0067712714519193,-0.0328043479726686,
0.0797391213004156));
#105803=CARTESIAN_POINT('Ctrl Pts',(0.00669450355790043,-0.0326943950436594,
0.0797194203794371));
#105804=CARTESIAN_POINT('Ctrl Pts',(0.00698553388977376,-0.0330240426238155,
0.0798701016058561));
#105805=CARTESIAN_POINT('Ctrl Pts',(0.00690673391732854,-0.0329142774063509,
0.0798544211265362));
#105806=CARTESIAN_POINT('Ctrl Pts',(0.00682821881953199,-0.0328043479726686,
0.0798371038143781));
#105807=CARTESIAN_POINT('Ctrl Pts',(0.00675008979103648,-0.0326943950436594,
0.0798181690840916));
#105808=CARTESIAN_POINT('Ctrl Pts',(0.00704515399412731,-0.0330240426238155,
0.0799664685044368));
#105809=CARTESIAN_POINT('Ctrl Pts',(0.00696502647376842,-0.0329142774063509,
0.0799516093501394));
#105810=CARTESIAN_POINT('Ctrl Pts',(0.00688516618714469,-0.0328043479726686,
0.0799350863283406));
#105811=CARTESIAN_POINT('Ctrl Pts',(0.00680567602417252,-0.0326943950436594,
0.079916917788746));
#105812=CARTESIAN_POINT('Ctrl Pts',(0.00710477409848085,-0.0330240426238155,
0.0800628354030175));
#105813=CARTESIAN_POINT('Ctrl Pts',(0.00702331903020831,-0.0329142774063509,
0.0800487975737426));
#105814=CARTESIAN_POINT('Ctrl Pts',(0.00694211355475738,-0.0328043479726686,
0.0800330688423031));
#105815=CARTESIAN_POINT('Ctrl Pts',(0.00686126225730857,-0.0326943950436594,
0.0800156664934005));
#105816=CARTESIAN_POINT('Origin',(0.01094149030982,-0.0326396682856681,
0.0634653280083133));
#105817=CARTESIAN_POINT('Ctrl Pts',(0.00652013033595481,-0.0331951640388589,
0.0799317212593737));
#105818=CARTESIAN_POINT('Ctrl Pts',(0.00644049882193376,-0.0330855618255042,
0.0799096341992027));
#105819=CARTESIAN_POINT('Ctrl Pts',(0.00636126640444661,-0.0329757224427709,
0.0798858853695025));
#105820=CARTESIAN_POINT('Ctrl Pts',(0.00628253603712311,-0.0328657862078596,
0.0798605002051586));
#105821=CARTESIAN_POINT('Ctrl Pts',(0.00661519395356684,-0.0331951640388589,
0.0798700441919475));
#105822=CARTESIAN_POINT('Ctrl Pts',(0.0065364119163779,-0.0330855618255042,
0.0798492664407969));
#105823=CARTESIAN_POINT('Ctrl Pts',(0.00645800252691944,-0.0329757224427709,
0.0798268454212137));
#105824=CARTESIAN_POINT('Ctrl Pts',(0.00638006760147917,-0.0328657862078596,
0.0798028049194409));
#105825=CARTESIAN_POINT('Ctrl Pts',(0.00671025757117887,-0.0331951640388589,
0.0798083671245212));
#105826=CARTESIAN_POINT('Ctrl Pts',(0.00663232501082203,-0.0330855618255042,
0.0797888986823911));
#105827=CARTESIAN_POINT('Ctrl Pts',(0.00655473864939227,-0.0329757224427709,
0.079767805472925));
#105828=CARTESIAN_POINT('Ctrl Pts',(0.00647759916583523,-0.0328657862078596,
0.0797451096337231));
#105829=CARTESIAN_POINT('Ctrl Pts',(0.0068053211887909,-0.0331951640388589,
0.0797466900570949));
#105830=CARTESIAN_POINT('Ctrl Pts',(0.00672823810526616,-0.0330855618255042,
0.0797285309239853));
#105831=CARTESIAN_POINT('Ctrl Pts',(0.00665147477186511,-0.0329757224427709,
0.0797087655246363));
#105832=CARTESIAN_POINT('Ctrl Pts',(0.0065751307301913,-0.0328657862078596,
0.0796874143480053));
#105833=CARTESIAN_POINT('Origin',(0.0113951742473582,-0.0326401908833327,
0.0636248390000959));
#105834=CARTESIAN_POINT('Ctrl Pts',(0.00683878670877478,-0.0332451089994432,
0.0797559710671071));
#105835=CARTESIAN_POINT('Ctrl Pts',(0.00662735405075975,-0.0329451141710259,
0.0797075066694966));
#105836=CARTESIAN_POINT('Ctrl Pts',(0.00642017258716349,-0.0326442513127504,
0.0796432539819795));
#105837=CARTESIAN_POINT('Ctrl Pts',(0.00708362342542217,-0.0332451089994432,
0.0798065178986729));
#105838=CARTESIAN_POINT('Ctrl Pts',(0.00687028436246422,-0.0329451141710259,
0.0797672876689095));
#105839=CARTESIAN_POINT('Ctrl Pts',(0.00666050635454846,-0.0326442513127504,
0.0797120993177296));
#105840=CARTESIAN_POINT('Ctrl Pts',(0.00657516112630008,-0.0325229783203384,
0.0796874229420149));
#105841=CARTESIAN_POINT('Ctrl Pts',(0.0064988278735293,-0.0324130253112079,
0.0796660752348636));
#105842=CARTESIAN_POINT('Ctrl Pts',(0.00642294780292916,-0.0323031222247694,
0.0796431517141486));
#105843=CARTESIAN_POINT('Ctrl Pts',(0.00634761707533441,-0.0321934096636184,
0.0796186851730301));
#105844=CARTESIAN_POINT('Ctrl Pts',(0.00662861268624204,-0.0325229783203384,
0.0797873432772312));
#105845=CARTESIAN_POINT('Ctrl Pts',(0.00655090203386048,-0.0324130253112079,
0.0797667323986514));
#105846=CARTESIAN_POINT('Ctrl Pts',(0.00647362953031397,-0.0323031222247694,
0.0797445171014735));
#105847=CARTESIAN_POINT('Ctrl Pts',(0.0063968931520563,-0.0321934096636184,
0.0797207293346115));
#105848=CARTESIAN_POINT('Ctrl Pts',(0.00668206424618399,-0.0325229783203384,
0.0798872636124475));
#105849=CARTESIAN_POINT('Ctrl Pts',(0.00660297619419166,-0.0324130253112079,
0.0798673895624392));
#105850=CARTESIAN_POINT('Ctrl Pts',(0.00652431125769877,-0.0323031222247694,
0.0798458824887985));
#105851=CARTESIAN_POINT('Ctrl Pts',(0.00644616922877819,-0.0321934096636184,
0.079822773496193));
#105852=CARTESIAN_POINT('Ctrl Pts',(0.00673551580612595,-0.0325229783203384,
0.0799871839476638));
#105853=CARTESIAN_POINT('Ctrl Pts',(0.00665505035452285,-0.0324130253112079,
0.079968046726227));
#105854=CARTESIAN_POINT('Ctrl Pts',(0.00657499298508357,-0.0323031222247694,
0.0799472478761234));
#105855=CARTESIAN_POINT('Ctrl Pts',(0.00649544530550007,-0.0321934096636184,
0.0799248176577744));
#105856=CARTESIAN_POINT('Origin',(0.0109390865415934,-0.0326393375177802,
0.0634735080404004));
#105857=CARTESIAN_POINT('Ctrl Pts',(0.00616025749492643,-0.0326943950436593,
0.0798196182199216));
#105858=CARTESIAN_POINT('Ctrl Pts',(0.00608211952985911,-0.0325844576448127,
0.0797925571695433));
#105859=CARTESIAN_POINT('Ctrl Pts',(0.00600453570173563,-0.0324744968375319,
0.0797638781827858));
#105860=CARTESIAN_POINT('Ctrl Pts',(0.00592760490865445,-0.0323646534831894,
0.0797336193759323));
#105861=CARTESIAN_POINT('Ctrl Pts',(0.00625900616726944,-0.0326943950436593,
0.0797640320049739));
#105862=CARTESIAN_POINT('Ctrl Pts',(0.00618163428442377,-0.0325844576448127,
0.0797383318963751));
#105863=CARTESIAN_POINT('Ctrl Pts',(0.00610478844623147,-0.0324744968375319,
0.0797110297915496));
#105864=CARTESIAN_POINT('Ctrl Pts',(0.00602856662956808,-0.0323646534831894,
0.0796821620295969));
#105865=CARTESIAN_POINT('Ctrl Pts',(0.00635775483961245,-0.0326943950436593,
0.0797084457900262));
#105866=CARTESIAN_POINT('Ctrl Pts',(0.00628114903898843,-0.0325844576448127,
0.079684106623207));
#105867=CARTESIAN_POINT('Ctrl Pts',(0.00620504119072732,-0.0324744968375319,
0.0796581814003134));
#105868=CARTESIAN_POINT('Ctrl Pts',(0.00612952835048171,-0.0323646534831894,
0.0796307046832615));
#105869=CARTESIAN_POINT('Ctrl Pts',(0.00645650351195547,-0.0326943950436593,
0.0796528595750784));
#105870=CARTESIAN_POINT('Ctrl Pts',(0.00638066379355309,-0.0325844576448127,
0.0796298813500389));
#105871=CARTESIAN_POINT('Ctrl Pts',(0.00630529393522316,-0.0324744968375319,
0.0796053330090773));
#105872=CARTESIAN_POINT('Ctrl Pts',(0.00623049007139533,-0.0323646534831894,
0.0795792473369261));
#105873=CARTESIAN_POINT('Origin',(0.0114059678144438,-0.0326395579066531,
0.063588569718786));
#105874=CARTESIAN_POINT('Ctrl Pts',(0.00648935812421096,-0.0327445246961878,
0.0796642345763496));
#105875=CARTESIAN_POINT('Ctrl Pts',(0.00628138536943636,-0.0324436878365476,
0.0796025912655016));
#105876=CARTESIAN_POINT('Ctrl Pts',(0.00607864666934498,-0.0321434074463187,
0.0795254577190637));
#105877=CARTESIAN_POINT('Ctrl Pts',(0.00673053829859072,-0.0327445246961878,
0.0797300534451195));
#105878=CARTESIAN_POINT('Ctrl Pts',(0.00652008314462459,-0.0324436878365476,
0.0796775063931573));
#105879=CARTESIAN_POINT('Ctrl Pts',(0.00631418393018645,-0.0321434074463187,
0.0796092562796439));
#105880=CARTESIAN_POINT('Ctrl Pts',(0.00614109061444679,-0.0322357242816073,
0.07954880163591));
#105881=CARTESIAN_POINT('Ctrl Pts',(0.00596914578433222,-0.0319819883628706,
0.0794856554805864));
#105882=CARTESIAN_POINT('Ctrl Pts',(0.0058015675922602,-0.0317295851069886,
0.0794116959573514));
#105883=CARTESIAN_POINT('Ctrl Pts',(0.00637758335590217,-0.0322357242816073,
0.0796298644710376));
#105884=CARTESIAN_POINT('Ctrl Pts',(0.00620305677962344,-0.0319819883628706,
0.0795742503028096));
#105885=CARTESIAN_POINT('Ctrl Pts',(0.00603242279173021,-0.0317295851069886,
0.0795076432182694));
#105886=CARTESIAN_POINT('Origin',(0.0113760622196953,-0.0326371942645951,
0.0636790576134149));
#105887=CARTESIAN_POINT('Origin',(0.0109049834096659,-0.0326352985528477,
0.0635914096061122));
#105888=CARTESIAN_POINT('Ctrl Pts',(0.00580813378883181,-0.0321934096636183,
0.0796851397875583));
#105889=CARTESIAN_POINT('Ctrl Pts',(0.00573179989733588,-0.0320835708272303,
0.0796532051913567));
#105890=CARTESIAN_POINT('Ctrl Pts',(0.00565617116740778,-0.0319739230346346,
0.0796197093926018));
#105891=CARTESIAN_POINT('Ctrl Pts',(0.00558134107171666,-0.0318646057455575,
0.0795847026730352));
#105892=CARTESIAN_POINT('Ctrl Pts',(0.00591017803828295,-0.0321934096636183,
0.079635863668405));
#105893=CARTESIAN_POINT('Ctrl Pts',(0.00583452370287361,-0.0320835708272303,
0.0796053363419319));
#105894=CARTESIAN_POINT('Ctrl Pts',(0.00575954501148807,-0.0319739230346346,
0.0795732610600095));
#105895=CARTESIAN_POINT('Ctrl Pts',(0.00568533474460069,-0.0318646057455575,
0.0795396862230981));
#105896=CARTESIAN_POINT('Ctrl Pts',(0.00601222228773408,-0.0321934096636183,
0.0795865875492518));
#105897=CARTESIAN_POINT('Ctrl Pts',(0.00593724750841134,-0.0320835708272303,
0.079557467492507));
#105898=CARTESIAN_POINT('Ctrl Pts',(0.00586291885556837,-0.0319739230346346,
0.0795268127274173));
#105899=CARTESIAN_POINT('Ctrl Pts',(0.00578932841748471,-0.0318646057455575,
0.079494669773161));
#105900=CARTESIAN_POINT('Ctrl Pts',(0.00611426653718522,-0.0321934096636183,
0.0795373114300986));
#105901=CARTESIAN_POINT('Ctrl Pts',(0.00603997131394907,-0.0320835708272303,
0.0795095986430821));
#105902=CARTESIAN_POINT('Ctrl Pts',(0.00596629269964866,-0.0319739230346346,
0.0794803643948251));
#105903=CARTESIAN_POINT('Ctrl Pts',(0.00589332209036874,-0.0318646057455575,
0.0794496533232239));
#105904=CARTESIAN_POINT('Ctrl Pts',(0.00623066118232943,-0.0320218834582362,
0.0795801832969985));
#105905=CARTESIAN_POINT('Ctrl Pts',(0.00617414610159012,-0.0319391099350637,
0.0795604804838664));
#105906=CARTESIAN_POINT('Ctrl Pts',(0.00611797292409208,-0.0318564869454897,
0.0795399071172582));
#105907=CARTESIAN_POINT('Ctrl Pts',(0.00606218116559332,-0.0317740741446468,
0.0795184820018143));
#105908=CARTESIAN_POINT('Ctrl Pts',(0.00625124803705913,-0.0320218834582362,
0.0796252722031731));
#105909=CARTESIAN_POINT('Ctrl Pts',(0.00619426368980827,-0.0319391099350637,
0.0796057836494304));
#105910=CARTESIAN_POINT('Ctrl Pts',(0.00613761818442492,-0.0318564869454897,
0.0795854170847348));
#105911=CARTESIAN_POINT('Ctrl Pts',(0.00608135139475746,-0.0317740741446468,
0.0795641911952165));
#105912=CARTESIAN_POINT('Ctrl Pts',(0.00627183489178884,-0.0320218834582362,
0.0796703611093477));
#105913=CARTESIAN_POINT('Ctrl Pts',(0.00621438127802641,-0.0319391099350637,
0.0796510868149944));
#105914=CARTESIAN_POINT('Ctrl Pts',(0.00615726344475776,-0.0318564869454897,
0.0796309270522114));
#105915=CARTESIAN_POINT('Ctrl Pts',(0.00610052162392159,-0.0317740741446468,
0.0796099003886187));
#105916=CARTESIAN_POINT('Ctrl Pts',(0.00629242174651854,-0.0320218834582362,
0.0797154500155224));
#105917=CARTESIAN_POINT('Ctrl Pts',(0.00623449886624456,-0.0319391099350637,
0.0796963899805584));
#105918=CARTESIAN_POINT('Ctrl Pts',(0.00617690870509059,-0.0318564869454897,
0.079676437019688));
#105919=CARTESIAN_POINT('Ctrl Pts',(0.00611969185308573,-0.0317740741446468,
0.0796556095820209));
#105920=CARTESIAN_POINT('Origin',(0.00504917312395027,-0.0391228853391003,
0.0858302139279516));
#105921=CARTESIAN_POINT('Ctrl Pts',(0.00925890998965823,-0.0352722978779654,
0.0797887631115429));
#105922=CARTESIAN_POINT('Ctrl Pts',(0.00924031881489165,-0.0352466642097257,
0.0797921485064815));
#105923=CARTESIAN_POINT('Ctrl Pts',(0.00922175824832721,-0.0352210183808321,
0.0797956080180148));
#105924=CARTESIAN_POINT('Ctrl Pts',(0.00920322773255888,-0.0351953608940152,
0.0797991422917301));
#105925=CARTESIAN_POINT('Origin',(0.00995792258949127,-0.0352456003065099,
0.0846386213136292));
#105926=CARTESIAN_POINT('Ctrl Pts',(0.00908026693651953,-0.0350241211493339,
0.0798197810430369));
#105927=CARTESIAN_POINT('Ctrl Pts',(0.00900216803087394,-0.0349144232867421,
0.0798329562276092));
#105928=CARTESIAN_POINT('Ctrl Pts',(0.00892375003880367,-0.0348045283677512,
0.079844524938051));
#105929=CARTESIAN_POINT('Ctrl Pts',(0.00884511285236919,-0.0346945769586885,
0.0798544686185804));
#105930=CARTESIAN_POINT('Ctrl Pts',(0.00917117534799638,-0.0350241211493339,
0.0798874331126755));
#105931=CARTESIAN_POINT('Ctrl Pts',(0.00909214456287197,-0.0349144232867421,
0.0799018605232856));
#105932=CARTESIAN_POINT('Ctrl Pts',(0.00901276824914229,-0.0348045283677512,
0.0799146629466688));
#105933=CARTESIAN_POINT('Ctrl Pts',(0.00893314746755198,-0.0346945769586885,
0.0799258202011364));
#105934=CARTESIAN_POINT('Ctrl Pts',(0.00926208375947324,-0.0350241211493339,
0.0799550851823141));
#105935=CARTESIAN_POINT('Ctrl Pts',(0.00918212109487,-0.034914423286742,
0.079970764818962));
#105936=CARTESIAN_POINT('Ctrl Pts',(0.00910178645948091,-0.0348045283677512,
0.0799848009552867));
#105937=CARTESIAN_POINT('Ctrl Pts',(0.00902118208273476,-0.0346945769586885,
0.0799971717836925));
#105938=CARTESIAN_POINT('Ctrl Pts',(0.0093529921709501,-0.0350241211493339,
0.0800227372519528));
#105939=CARTESIAN_POINT('Ctrl Pts',(0.00927209762686803,-0.034914423286742,
0.0800396691146383));
#105940=CARTESIAN_POINT('Ctrl Pts',(0.00919080466981953,-0.0348045283677512,
0.0800549389639046));
#105941=CARTESIAN_POINT('Ctrl Pts',(0.00910921669791754,-0.0346945769586885,
0.0800685233662486));
#105942=CARTESIAN_POINT('Origin',(0.00691771894704748,-0.0345629067942052,
0.0631766959308064));
#105943=CARTESIAN_POINT('Ctrl Pts',(0.00881633635390863,-0.0351970973651503,
0.0800403217663952));
#105944=CARTESIAN_POINT('Ctrl Pts',(0.00873473392901711,-0.0350869349326827,
0.080049916165671));
#105945=CARTESIAN_POINT('Ctrl Pts',(0.00865286444338367,-0.034976498513997,
0.0800578220436516));
#105946=CARTESIAN_POINT('Ctrl Pts',(0.00857083335840892,-0.0348659306865088,
0.0800640229144731));
#105947=CARTESIAN_POINT('Ctrl Pts',(0.00886397828867158,-0.0351970973651503,
0.0799733089564085));
#105948=CARTESIAN_POINT('Ctrl Pts',(0.00878330423543964,-0.0350869349326827,
0.0799835633701211));
#105949=CARTESIAN_POINT('Ctrl Pts',(0.00870235016918374,-0.034976498513997,
0.079992149109619));
#105950=CARTESIAN_POINT('Ctrl Pts',(0.00862122031350391,-0.0348659306865088,
0.07999904887807));
#105951=CARTESIAN_POINT('Ctrl Pts',(0.00891162022343454,-0.0351970973651503,
0.0799062961464218));
#105952=CARTESIAN_POINT('Ctrl Pts',(0.00883187454186217,-0.0350869349326827,
0.0799172105745713));
#105953=CARTESIAN_POINT('Ctrl Pts',(0.00875183589498381,-0.034976498513997,
0.0799264761755864));
#105954=CARTESIAN_POINT('Ctrl Pts',(0.0086716072685989,-0.0348659306865088,
0.0799340748416668));
#105955=CARTESIAN_POINT('Ctrl Pts',(0.00895926215819749,-0.0351970973651503,
0.0798392833364352));
#105956=CARTESIAN_POINT('Ctrl Pts',(0.0088804448482847,-0.0350869349326827,
0.0798508577790214));
#105957=CARTESIAN_POINT('Ctrl Pts',(0.00880132162078388,-0.034976498513997,
0.0798608032415538));
#105958=CARTESIAN_POINT('Ctrl Pts',(0.00872199422369388,-0.0348659306865088,
0.0798691008052636));
#105959=CARTESIAN_POINT('Origin',(0.00739862927952232,-0.0345637187966112,
0.0631695819681397));
#105960=CARTESIAN_POINT('Ctrl Pts',(0.00899271323550525,-0.0352450361861251,
0.0798353393780459));
#105961=CARTESIAN_POINT('Ctrl Pts',(0.00877828714781084,-0.0349452761023764,
0.0798681116492347));
#105962=CARTESIAN_POINT('Ctrl Pts',(0.00856200168053271,-0.0346444289983474,
0.0798846393679849));
#105963=CARTESIAN_POINT('Ctrl Pts',(0.00923896423252717,-0.0352450361861251,
0.079792206484963));
#105964=CARTESIAN_POINT('Ctrl Pts',(0.0090261649285478,-0.0349452761023764,
0.0798342662646664));
#105965=CARTESIAN_POINT('Ctrl Pts',(0.00881080205033893,-0.0346444289983474,
0.0798601776431011));
#105966=CARTESIAN_POINT('Ctrl Pts',(0.00872237200801529,-0.0345231616327821,
0.0798686511518472));
#105967=CARTESIAN_POINT('Ctrl Pts',(0.00864354845310441,-0.0344132092796975,
0.0798769018696987));
#105968=CARTESIAN_POINT('Ctrl Pts',(0.00856455830553595,-0.0343032738558973,
0.0798835217587928));
#105969=CARTESIAN_POINT('Ctrl Pts',(0.00848550297805775,-0.034193496108874,
0.0798885049304476));
#105970=CARTESIAN_POINT('Ctrl Pts',(0.00880885311655982,-0.0345231616327821,
0.079941877881967));
#105971=CARTESIAN_POINT('Ctrl Pts',(0.00872902023426923,-0.0344132092796975,
0.079951320620144));
#105972=CARTESIAN_POINT('Ctrl Pts',(0.00864899615539753,-0.0343032738558973,
0.0799591115909203));
#105973=CARTESIAN_POINT('Ctrl Pts',(0.00856888365570858,-0.034193496108874,
0.0799652434392525));
#105974=CARTESIAN_POINT('Ctrl Pts',(0.00889533422510434,-0.0345231616327821,
0.0800151046120867));
#105975=CARTESIAN_POINT('Ctrl Pts',(0.00881449201543405,-0.0344132092796975,
0.0800257393705894));
#105976=CARTESIAN_POINT('Ctrl Pts',(0.00873343400525911,-0.0343032738558973,
0.0800347014230478));
#105977=CARTESIAN_POINT('Ctrl Pts',(0.00865226433335941,-0.034193496108874,
0.0800419819480574));
#105978=CARTESIAN_POINT('Ctrl Pts',(0.00898181533364887,-0.0345231616327821,
0.0800883313422065));
#105979=CARTESIAN_POINT('Ctrl Pts',(0.00889996379659887,-0.0344132092796975,
0.0801001581210348));
#105980=CARTESIAN_POINT('Ctrl Pts',(0.0088178718551207,-0.0343032738558973,
0.0801102912551753));
#105981=CARTESIAN_POINT('Ctrl Pts',(0.00873564501101023,-0.034193496108874,
0.0801187204568624));
#105982=CARTESIAN_POINT('Origin',(0.00691614788271578,-0.0345625596231992,
0.0631646946784457));
#105983=CARTESIAN_POINT('Ctrl Pts',(0.0083852687703767,-0.0346945769586885,
0.0801442993560538));
#105984=CARTESIAN_POINT('Ctrl Pts',(0.00830266429544345,-0.0345846629176052,
0.0801479027732564));
#105985=CARTESIAN_POINT('Ctrl Pts',(0.00821997119427492,-0.0344746925050311,
0.0801497985793136));
#105986=CARTESIAN_POINT('Ctrl Pts',(0.00813729543283345,-0.0343648066253259,
0.0801499847826831));
#105987=CARTESIAN_POINT('Ctrl Pts',(0.0084566202967524,-0.0346945769586885,
0.0800562648101871));
#105988=CARTESIAN_POINT('Ctrl Pts',(0.00837522898235808,-0.0345846629176052,
0.0800608514874877));
#105989=CARTESIAN_POINT('Ctrl Pts',(0.00829372891552425,-0.0344746925050311,
0.0800637558092479));
#105990=CARTESIAN_POINT('Ctrl Pts',(0.00821222453889692,-0.0343648066253259,
0.0800649744853856));
#105991=CARTESIAN_POINT('Ctrl Pts',(0.0085279718231281,-0.0346945769586885,
0.0799682302643205));
#105992=CARTESIAN_POINT('Ctrl Pts',(0.00844779366927271,-0.0345846629176052,
0.079973800201719));
#105993=CARTESIAN_POINT('Ctrl Pts',(0.00836748663677359,-0.0344746925050311,
0.0799777130391821));
#105994=CARTESIAN_POINT('Ctrl Pts',(0.00828715364496039,-0.0343648066253259,
0.0799799641880881));
#105995=CARTESIAN_POINT('Ctrl Pts',(0.00859932334950379,-0.0346945769586885,
0.0798801957184538));
#105996=CARTESIAN_POINT('Ctrl Pts',(0.00852035835618734,-0.0345846629176052,
0.0798867489159503));
#105997=CARTESIAN_POINT('Ctrl Pts',(0.00844124435802293,-0.0344746925050311,
0.0798916702691163));
#105998=CARTESIAN_POINT('Ctrl Pts',(0.00836208275102385,-0.0343648066253259,
0.0798949538907905));
#105999=CARTESIAN_POINT('Origin',(0.00739400237491167,-0.0345626446730793,
0.063111334887826));
#106000=CARTESIAN_POINT('Ctrl Pts',(0.00859804663143735,-0.0346945769586885,
0.0798817709516812));
#106001=CARTESIAN_POINT('Ctrl Pts',(0.00847799239398044,-0.034527515336289,
0.079891704610227));
#106002=CARTESIAN_POINT('Ctrl Pts',(0.00835759469993052,-0.0343603235965158,
0.0798978652428601));
#106003=CARTESIAN_POINT('Ctrl Pts',(0.00823720990302468,-0.0341934961088739,
0.0799002399214836));
#106004=CARTESIAN_POINT('Ctrl Pts',(0.00868142447208004,-0.0346945769586885,
0.079873043751613));
#106005=CARTESIAN_POINT('Ctrl Pts',(0.00856155302932274,-0.034527515336289,
0.0798847237924136));
#106006=CARTESIAN_POINT('Ctrl Pts',(0.00844128325513802,-0.0343603235965158,
0.0798926370077305));
#106007=CARTESIAN_POINT('Ctrl Pts',(0.00832097120197104,-0.0341934961088739,
0.0798967652804823));
#106008=CARTESIAN_POINT('Ctrl Pts',(0.00876480231272273,-0.0346945769586885,
0.0798643165515447));
#106009=CARTESIAN_POINT('Ctrl Pts',(0.00864511366466504,-0.034527515336289,
0.0798777429746003));
#106010=CARTESIAN_POINT('Ctrl Pts',(0.00852497181034551,-0.0343603235965158,
0.079887408772601));
#106011=CARTESIAN_POINT('Ctrl Pts',(0.0084047325009174,-0.0341934961088739,
0.079893290639481));
#106012=CARTESIAN_POINT('Ctrl Pts',(0.00884818015336542,-0.0346945769586885,
0.0798555893514764));
#106013=CARTESIAN_POINT('Ctrl Pts',(0.00872867430000733,-0.034527515336289,
0.0798707621567869));
#106014=CARTESIAN_POINT('Ctrl Pts',(0.00860866036555301,-0.0343603235965158,
0.0798821805374715));
#106015=CARTESIAN_POINT('Ctrl Pts',(0.00848849379986377,-0.0341934961088739,
0.0798898159984798));
#106016=CARTESIAN_POINT('Ctrl Pts',(0.00836211425515608,-0.0340223579322365,
0.0798949520266385));
#106017=CARTESIAN_POINT('Ctrl Pts',(0.00828287638324561,-0.0339125849573554,
0.0798982392473703));
#106018=CARTESIAN_POINT('Ctrl Pts',(0.0082036261530396,-0.0338030433565221,
0.0798998841183849));
#106019=CARTESIAN_POINT('Ctrl Pts',(0.0081244650986915,-0.0336938721132327,
0.0798998935202157));
#106020=CARTESIAN_POINT('Ctrl Pts',(0.00844382692016333,-0.0340223579322365,
0.0799734645747335));
#106021=CARTESIAN_POINT('Ctrl Pts',(0.00836350615544531,-0.0339125849573554,
0.0799778788262313));
#106022=CARTESIAN_POINT('Ctrl Pts',(0.00828315046645,-0.0338030433565221,
0.0799806275226956));
#106023=CARTESIAN_POINT('Ctrl Pts',(0.00820286292615929,-0.0336938721132327,
0.0799817162583713));
#106024=CARTESIAN_POINT('Ctrl Pts',(0.00852553958517058,-0.0340223579322365,
0.0800519771228286));
#106025=CARTESIAN_POINT('Ctrl Pts',(0.00844413592764502,-0.0339125849573554,
0.0800575184050923));
#106026=CARTESIAN_POINT('Ctrl Pts',(0.00836267477986041,-0.0338030433565221,
0.0800613709270064));
#106027=CARTESIAN_POINT('Ctrl Pts',(0.00828126075362708,-0.0336938721132327,
0.080063538996527));
#106028=CARTESIAN_POINT('Ctrl Pts',(0.00860725225017783,-0.0340223579322365,
0.0801304896709236));
#106029=CARTESIAN_POINT('Ctrl Pts',(0.00852476569984473,-0.0339125849573554,
0.0801371579839533));
#106030=CARTESIAN_POINT('Ctrl Pts',(0.00844219909327081,-0.0338030433565221,
0.0801421143313171));
#106031=CARTESIAN_POINT('Ctrl Pts',(0.00835965858109488,-0.0336938721132327,
0.0801453617346826));
#106032=CARTESIAN_POINT('Origin',(0.00692670444745188,-0.0345589643415875,
0.0632844504180948));
#106033=CARTESIAN_POINT('Ctrl Pts',(0.00800836761556648,-0.034193496108874,
0.0801488898535788));
#106034=CARTESIAN_POINT('Ctrl Pts',(0.00792564647794095,-0.0340836138595105,
0.0801472983549206));
#106035=CARTESIAN_POINT('Ctrl Pts',(0.00784299796419675,-0.0339738896671456,
0.0801439958795444));
#106036=CARTESIAN_POINT('Ctrl Pts',(0.00776052757088199,-0.0338644633335883,
0.0801389937451553));
#106037=CARTESIAN_POINT('Ctrl Pts',(0.00808510619341875,-0.034193496108874,
0.0800655091009042));
#106038=CARTESIAN_POINT('Ctrl Pts',(0.00800353482698184,-0.0340836138595105,
0.0800649757817782));
#106039=CARTESIAN_POINT('Ctrl Pts',(0.00792201363593965,-0.0339738896671456,
0.0800627547703019));
#106040=CARTESIAN_POINT('Ctrl Pts',(0.00784064676679219,-0.0338644633335883,
0.0800588559033197));
#106041=CARTESIAN_POINT('Ctrl Pts',(0.00816184477127103,-0.034193496108874,
0.0799821283482295));
#106042=CARTESIAN_POINT('Ctrl Pts',(0.00808142317602273,-0.0340836138595105,
0.0799826532086359));
#106043=CARTESIAN_POINT('Ctrl Pts',(0.00800102930768255,-0.0339738896671456,
0.0799815136610594));
#106044=CARTESIAN_POINT('Ctrl Pts',(0.00792076596270239,-0.0338644633335883,
0.079978718061484));
#106045=CARTESIAN_POINT('Ctrl Pts',(0.0082385833491233,-0.034193496108874,
0.0798987475955549));
#106046=CARTESIAN_POINT('Ctrl Pts',(0.00815931152506361,-0.0340836138595105,
0.0799003306354936));
#106047=CARTESIAN_POINT('Ctrl Pts',(0.00808004497942545,-0.0339738896671456,
0.0799002725518169));
#106048=CARTESIAN_POINT('Ctrl Pts',(0.00800088515861259,-0.0338644633335883,
0.0798985802196484));
#106049=CARTESIAN_POINT('Origin',(0.00739782913690974,-0.034561062186344,
0.0631865140171341));
#106050=CARTESIAN_POINT('Ctrl Pts',(0.0082733779616619,-0.03424362768739,
0.0798994126748766));
#106051=CARTESIAN_POINT('Ctrl Pts',(0.00805653528793645,-0.0339430054201859,
0.0799050547722985));
#106052=CARTESIAN_POINT('Ctrl Pts',(0.00783988365561877,-0.0336441434784161,
0.0798943473624435));
#106053=CARTESIAN_POINT('Ctrl Pts',(0.00852309301813404,-0.03424362768739,
0.0798874799228422));
#106054=CARTESIAN_POINT('Ctrl Pts',(0.00830670039557075,-0.0339430054201859,
0.0799025401788792));
#106055=CARTESIAN_POINT('Ctrl Pts',(0.00808978812157049,-0.0336441434784161,
0.0799012580713354));
#106056=CARTESIAN_POINT('Ctrl Pts',(0.00800091288301854,-0.0335235895815127,
0.0798985806857093));
#106057=CARTESIAN_POINT('Ctrl Pts',(0.007921772351967,-0.0334144449262719,
0.0798968891477485));
#106058=CARTESIAN_POINT('Ctrl Pts',(0.00784257584393467,-0.0333049234473133,
0.0798935606826039));
#106059=CARTESIAN_POINT('Ctrl Pts',(0.00776342501247529,-0.0331951640388588,
0.0798885903730654));
#106060=CARTESIAN_POINT('Ctrl Pts',(0.00807753440307829,-0.0335235895815127,
0.0799820690989813));
#106061=CARTESIAN_POINT('Ctrl Pts',(0.00799724448964452,-0.0334144449262719,
0.079981432407098));
#106062=CARTESIAN_POINT('Ctrl Pts',(0.00791687548640275,-0.0333049234473133,
0.0799791362545462));
#106063=CARTESIAN_POINT('Ctrl Pts',(0.00783653042659583,-0.0331951640388588,
0.0799751742682954));
#106064=CARTESIAN_POINT('Ctrl Pts',(0.00815415592313804,-0.0335235895815127,
0.0800655575122532));
#106065=CARTESIAN_POINT('Ctrl Pts',(0.00807271662732204,-0.0334144449262719,
0.0800659756664474));
#106066=CARTESIAN_POINT('Ctrl Pts',(0.00799117512887083,-0.0333049234473133,
0.0800647118264885));
#106067=CARTESIAN_POINT('Ctrl Pts',(0.00790963584071636,-0.0331951640388588,
0.0800617581635254));
#106068=CARTESIAN_POINT('Ctrl Pts',(0.00823077744319779,-0.0335235895815127,
0.0801490459255251));
#106069=CARTESIAN_POINT('Ctrl Pts',(0.00814818876499955,-0.0334144449262719,
0.0801505189257969));
#106070=CARTESIAN_POINT('Ctrl Pts',(0.00806547477133891,-0.0333049234473133,
0.0801502873984308));
#106071=CARTESIAN_POINT('Ctrl Pts',(0.0079827412548369,-0.0331951640388588,
0.0801483420587554));
#106072=CARTESIAN_POINT('Origin',(0.00956654017020789,-0.0326434571769428,
0.063319353312045));
#106073=CARTESIAN_POINT('Ctrl Pts',(0.00763045792790763,-0.0336938721132464,
0.0801312082143985));
#106074=CARTESIAN_POINT('Ctrl Pts',(0.00759544793145065,-0.0336474569764995,
0.0801283206237717));
#106075=CARTESIAN_POINT('Ctrl Pts',(0.00756047413679517,-0.033601104548885,
0.0801250233947924));
#106076=CARTESIAN_POINT('Ctrl Pts',(0.0074719285374094,-0.0334837508694645,
0.0801166755698235));
#106077=CARTESIAN_POINT('Ctrl Pts',(0.00738366918405866,-0.0333660264863676,
0.0801057076211362));
#106078=CARTESIAN_POINT('Ctrl Pts',(0.00787592552727102,-0.0336938721132464,
0.0798960153213509));
#106079=CARTESIAN_POINT('Ctrl Pts',(0.00784229219286244,-0.0336474569764995,
0.0798945645340381));
#106080=CARTESIAN_POINT('Ctrl Pts',(0.00780867814632869,-0.033601104548885,
0.0798927201254896));
#106081=CARTESIAN_POINT('Ctrl Pts',(0.007723575116262,-0.0334837508694645,
0.079888050507507));
#106082=CARTESIAN_POINT('Ctrl Pts',(0.00763864782761815,-0.0333660264863676,
0.0798808611610665));
#106083=CARTESIAN_POINT('Ctrl Pts',(0.00787592552727113,-0.0336938721132427,
0.0798960153213606));
#106084=CARTESIAN_POINT('Ctrl Pts',(0.00784229219286749,-0.0336474569765026,
0.0798945645340479));
#106085=CARTESIAN_POINT('Ctrl Pts',(0.00780867814633869,-0.0336011045488949,
0.0798927201254996));
#106086=CARTESIAN_POINT('Ctrl Pts',(0.00772428390860401,-0.033484728265791,
0.0798880893990749));
#106087=CARTESIAN_POINT('Ctrl Pts',(0.00764006219165131,-0.0333679870047996,
0.0798809807154008));
#106088=CARTESIAN_POINT('Ctrl Pts',(0.00787592552726848,-0.0336938721132429,
0.0798960153213509));
#106089=CARTESIAN_POINT('Ctrl Pts',(0.00775563783920221,-0.0335278710435085,
0.0798908266638833));
#106090=CARTESIAN_POINT('Ctrl Pts',(0.00763555518301437,-0.033362046922432,
0.07988186764115));
#106091=CARTESIAN_POINT('Ctrl Pts',(0.00751561932852367,-0.0331951640388601,
0.0798691138238489));
#106092=CARTESIAN_POINT('Ctrl Pts',(0.00795973972583508,-0.0336938721132429,
0.0798978069524273));
#106093=CARTESIAN_POINT('Ctrl Pts',(0.00783941453157574,-0.0335278710435085,
0.079894372870193));
#106094=CARTESIAN_POINT('Ctrl Pts',(0.00771923935936628,-0.033362046922432,
0.0798871666292529));
#106095=CARTESIAN_POINT('Ctrl Pts',(0.00759915564146883,-0.0331951640388601,
0.0798761646566227));
#106096=CARTESIAN_POINT('Ctrl Pts',(0.00804355392440168,-0.0336938721132429,
0.0798995985835036));
#106097=CARTESIAN_POINT('Ctrl Pts',(0.00792319122394927,-0.0335278710435085,
0.0798979190765027));
#106098=CARTESIAN_POINT('Ctrl Pts',(0.0078029235357182,-0.033362046922432,
0.0798924656173559));
#106099=CARTESIAN_POINT('Ctrl Pts',(0.007682691954414,-0.0331951640388601,
0.0798832154893964));
#106100=CARTESIAN_POINT('Ctrl Pts',(0.00812736812296829,-0.0336938721132429,
0.07990139021458));
#106101=CARTESIAN_POINT('Ctrl Pts',(0.0080069679163228,-0.0335278710435085,
0.0799014652828123));
#106102=CARTESIAN_POINT('Ctrl Pts',(0.00788660771207011,-0.033362046922432,
0.0798977646054588));
#106103=CARTESIAN_POINT('Ctrl Pts',(0.00776622826735916,-0.0331951640388601,
0.0798902663221702));
#106104=CARTESIAN_POINT('Ctrl Pts',(0.00764020019117138,-0.0330240426238155,
0.0798795226003004));
#106105=CARTESIAN_POINT('Ctrl Pts',(0.00756127043534926,-0.0329142774063509,
0.0798728607870927));
#106106=CARTESIAN_POINT('Ctrl Pts',(0.00748243904845313,-0.0328043479726686,
0.0798645639541958));
#106107=CARTESIAN_POINT('Ctrl Pts',(0.00740380731207764,-0.0326943950436594,
0.079854639949255));
#106108=CARTESIAN_POINT('Ctrl Pts',(0.00771142814820226,-0.0330240426238155,
0.0799676572366385));
#106109=CARTESIAN_POINT('Ctrl Pts',(0.00763128425189917,-0.0329142774063509,
0.0799619766579329));
#106110=CARTESIAN_POINT('Ctrl Pts',(0.00755121783437066,-0.0328043479726686,
0.0799546364490441));
#106111=CARTESIAN_POINT('Ctrl Pts',(0.00747133172562738,-0.0326943950436594,
0.0799456431885381));
#106112=CARTESIAN_POINT('Ctrl Pts',(0.00778265610523314,-0.0330240426238155,
0.0800557918729766));
#106113=CARTESIAN_POINT('Ctrl Pts',(0.00770129806844909,-0.0329142774063509,
0.0800510925287732));
#106114=CARTESIAN_POINT('Ctrl Pts',(0.0076199966202882,-0.0328043479726686,
0.0800447089438924));
#106115=CARTESIAN_POINT('Ctrl Pts',(0.00753885613917711,-0.0326943950436594,
0.0800366464278211));
#106116=CARTESIAN_POINT('Ctrl Pts',(0.00785388406226402,-0.0330240426238155,
0.0801439265093147));
#106117=CARTESIAN_POINT('Ctrl Pts',(0.007771311884999,-0.0329142774063509,
0.0801402083996134));
#106118=CARTESIAN_POINT('Ctrl Pts',(0.00768877540620573,-0.0328043479726686,
0.0801347814387407));
#106119=CARTESIAN_POINT('Ctrl Pts',(0.00760638055272684,-0.0326943950436594,
0.0801276496671042));
#106120=CARTESIAN_POINT('Origin',(0.00958012734946644,-0.0326396682856541,
0.0631964273685868));
#106121=CARTESIAN_POINT('Ctrl Pts',(0.00725741743083936,-0.0331951640388587,
0.0800871215330967));
#106122=CARTESIAN_POINT('Ctrl Pts',(0.00717564559242002,-0.0330855618255041,
0.0800751891111381));
#106123=CARTESIAN_POINT('Ctrl Pts',(0.00709406142859066,-0.0329757224427708,
0.0800615580031402));
#106124=CARTESIAN_POINT('Ctrl Pts',(0.00701277026899738,-0.0328657862078596,
0.0800462405399157));
#106125=CARTESIAN_POINT('Ctrl Pts',(0.00734400125713554,-0.0331951640388587,
0.0800140161771792));
#106126=CARTESIAN_POINT('Ctrl Pts',(0.00726323629710303,-0.0330855618255041,
0.0800032762722701));
#106127=CARTESIAN_POINT('Ctrl Pts',(0.00718263509021607,-0.0329757224427708,
0.0799908593514458));
#106128=CARTESIAN_POINT('Ctrl Pts',(0.00710230163111726,-0.0328657862078596,
0.0799767762524229));
#106129=CARTESIAN_POINT('Ctrl Pts',(0.00743058508343171,-0.0331951640388587,
0.0799409108212615));
#106130=CARTESIAN_POINT('Ctrl Pts',(0.00735082700178604,-0.0330855618255041,
0.079931363433402));
#106131=CARTESIAN_POINT('Ctrl Pts',(0.00727120875184148,-0.0329757224427708,
0.0799201606997513));
#106132=CARTESIAN_POINT('Ctrl Pts',(0.00719183299323715,-0.0328657862078596,
0.0799073119649301));
#106133=CARTESIAN_POINT('Ctrl Pts',(0.00751716890972788,-0.0331951640388587,
0.0798678054653439));
#106134=CARTESIAN_POINT('Ctrl Pts',(0.00743841770646904,-0.0330855618255041,
0.079859450594534));
#106135=CARTESIAN_POINT('Ctrl Pts',(0.0073597824134669,-0.0329757224427708,
0.0798494620480569));
#106136=CARTESIAN_POINT('Ctrl Pts',(0.00728136435535703,-0.0328657862078596,
0.0798378476774373));
#106137=CARTESIAN_POINT('Origin',(0.010050225882153,-0.0326401908832541,
0.0632978188934094));
#106138=CARTESIAN_POINT('Ctrl Pts',(0.00755153376308668,-0.0332451089994431,
0.0798728189499877));
#106139=CARTESIAN_POINT('Ctrl Pts',(0.00733569411506671,-0.0329451141710257,
0.0798512362473379));
#106140=CARTESIAN_POINT('Ctrl Pts',(0.00712209334210132,-0.0326442513127503,
0.0798134569342203));
#106141=CARTESIAN_POINT('Ctrl Pts',(0.00780077506694068,-0.0332451089994431,
0.0798922810272961));
#106142=CARTESIAN_POINT('Ctrl Pts',(0.00758420139466576,-0.0329451141710257,
0.079880098614218));
#106143=CARTESIAN_POINT('Ctrl Pts',(0.00736916061449163,-0.0326442513127503,
0.0798516375957339));
#106144=CARTESIAN_POINT('Ctrl Pts',(0.00728139558889851,-0.0325229783203384,
0.0798378523940379));
#106145=CARTESIAN_POINT('Ctrl Pts',(0.00720298866945899,-0.0324130253112079,
0.079826240113332));
#106146=CARTESIAN_POINT('Ctrl Pts',(0.00712483385690391,-0.0323031222247694,
0.0798130076460361));
#106147=CARTESIAN_POINT('Ctrl Pts',(0.00704703066388391,-0.0321934096636184,
0.0797981754745783));
#106148=CARTESIAN_POINT('Ctrl Pts',(0.00734694900603678,-0.0325229783203384,
0.0799302855707199));
#106149=CARTESIAN_POINT('Ctrl Pts',(0.00726726789730127,-0.0324130253112079,
0.0799195769424193));
#106150=CARTESIAN_POINT('Ctrl Pts',(0.00718782039549549,-0.0323031222247694,
0.0799072216322301));
#106151=CARTESIAN_POINT('Ctrl Pts',(0.00710870770876032,-0.0321934096636184,
0.0798932390574339));
#106152=CARTESIAN_POINT('Ctrl Pts',(0.00741250242317505,-0.0325229783203384,
0.080022718747402));
#106153=CARTESIAN_POINT('Ctrl Pts',(0.00733154712514356,-0.0324130253112079,
0.0800129137715066));
#106154=CARTESIAN_POINT('Ctrl Pts',(0.00725080693408707,-0.0323031222247694,
0.0800014356184241));
#106155=CARTESIAN_POINT('Ctrl Pts',(0.00717038475363674,-0.0321934096636184,
0.0799883026402895));
#106156=CARTESIAN_POINT('Ctrl Pts',(0.00747805584031332,-0.0325229783203384,
0.0801151519240841));
#106157=CARTESIAN_POINT('Ctrl Pts',(0.00739582635298584,-0.0324130253112079,
0.0801062506005939));
#106158=CARTESIAN_POINT('Ctrl Pts',(0.00731379347267864,-0.0323031222247694,
0.0800956496046182));
#106159=CARTESIAN_POINT('Ctrl Pts',(0.00723206179851315,-0.0321934096636184,
0.0800833662231452));
#106160=CARTESIAN_POINT('Origin',(0.00957876776548617,-0.0326393375177939,
0.0632048441708871));
#106161=CARTESIAN_POINT('Ctrl Pts',(0.0068863320582244,-0.0326943950436594,
0.0800210064864323));
#106162=CARTESIAN_POINT('Ctrl Pts',(0.00680541858540274,-0.0325844576448127,
0.0800039521043449));
#106163=CARTESIAN_POINT('Ctrl Pts',(0.00672485209879151,-0.0324744968375319,
0.079985223092015));
#106164=CARTESIAN_POINT('Ctrl Pts',(0.00664473549388511,-0.0323646534831895,
0.0799648448699489));
#106165=CARTESIAN_POINT('Ctrl Pts',(0.00697733526773067,-0.0326943950436594,
0.0799534820949769));
#106166=CARTESIAN_POINT('Ctrl Pts',(0.00689735240757747,-0.0325844576448127,
0.0799376819076747));
#106167=CARTESIAN_POINT('Ctrl Pts',(0.00681769066069115,-0.0324744968375319,
0.0799202264254871));
#106168=CARTESIAN_POINT('Ctrl Pts',(0.00673845178586718,-0.0323646534831895,
0.0799011394212102));
#106169=CARTESIAN_POINT('Ctrl Pts',(0.00706833847723695,-0.0326943950436594,
0.0798859577035216));
#106170=CARTESIAN_POINT('Ctrl Pts',(0.00698928622975219,-0.0325844576448127,
0.0798714117110046));
#106171=CARTESIAN_POINT('Ctrl Pts',(0.00691052922259079,-0.0324744968375319,
0.0798552297589591));
#106172=CARTESIAN_POINT('Ctrl Pts',(0.00683216807784924,-0.0323646534831895,
0.0798374339724716));
#106173=CARTESIAN_POINT('Ctrl Pts',(0.00715934168674322,-0.0326943950436594,
0.0798184333120662));
#106174=CARTESIAN_POINT('Ctrl Pts',(0.00708122005192691,-0.0325844576448127,
0.0798051415143344));
#106175=CARTESIAN_POINT('Ctrl Pts',(0.00700336778449043,-0.0324744968375319,
0.0797902330924312));
#106176=CARTESIAN_POINT('Ctrl Pts',(0.0069258843698313,-0.0323646534831895,
0.0797737285237329));
#106177=CARTESIAN_POINT('Origin',(0.0100563885920909,-0.032639557906725,
0.063260482814387));
#106178=CARTESIAN_POINT('Ctrl Pts',(0.0071933628962589,-0.0327445246961876,
0.0798256008432632));
#106179=CARTESIAN_POINT('Ctrl Pts',(0.006979304113298,-0.0324436878365474,
0.0797905095061824));
#106180=CARTESIAN_POINT('Ctrl Pts',(0.00676849667162067,-0.0321434074463187,
0.079739394077648));
#106181=CARTESIAN_POINT('Ctrl Pts',(0.00744089058457912,-0.0327445246961876,
0.0798606728194671));
#106182=CARTESIAN_POINT('Ctrl Pts',(0.00722550904042526,-0.0324436878365474,
0.0798349171416714));
#106183=CARTESIAN_POINT('Ctrl Pts',(0.00701267939537438,-0.0321434074463187,
0.0797930112150224));
#106184=CARTESIAN_POINT('Ctrl Pts',(0.00683337399614665,-0.0322357242816073,
0.0797547276191814));
#106185=CARTESIAN_POINT('Ctrl Pts',(0.00665487069054111,-0.0319819883628705,
0.0797136297917062));
#106186=CARTESIAN_POINT('Ctrl Pts',(0.00647934431636683,-0.0317295851069886,
0.0796612565780899));
#106187=CARTESIAN_POINT('Ctrl Pts',(0.00707816178894713,-0.0322357242816073,
0.0798055108496405));
#106188=CARTESIAN_POINT('Ctrl Pts',(0.00689804110331489,-0.0319819883628705,
0.079772209195888));
#106189=CARTESIAN_POINT('Ctrl Pts',(0.00672040453409841,-0.0317295851069886,
0.0797275134375627));
#106190=CARTESIAN_POINT('Origin',(0.0100380599527638,-0.0326371942645376,
0.0633540053487781));
#106191=CARTESIAN_POINT('Origin',(0.00955971053113989,-0.0326352985529813,
0.0633260903038244));
#106192=CARTESIAN_POINT('Ctrl Pts',(0.00652013033595464,-0.0321934096636183,
0.0799317212593738));
#106193=CARTESIAN_POINT('Ctrl Pts',(0.00644039589378846,-0.0320835708272304,
0.0799096056504534));
#106194=CARTESIAN_POINT('Ctrl Pts',(0.00636116538221627,-0.0319739230346346,
0.0798858527693486));
#106195=CARTESIAN_POINT('Ctrl Pts',(0.00628253783882057,-0.0318646057455576,
0.0798605007860826));
#106196=CARTESIAN_POINT('Ctrl Pts',(0.00661519400066897,-0.0321934096636183,
0.0798700441613876));
#106197=CARTESIAN_POINT('Ctrl Pts',(0.00653631013375223,-0.0320835708272304,
0.0798492395544918));
#106198=CARTESIAN_POINT('Ctrl Pts',(0.0064579025729425,-0.0319739230346346,
0.0798268145175876));
#106199=CARTESIAN_POINT('Ctrl Pts',(0.00638006943329853,-0.0318646057455576,
0.0798028054410061));
#106200=CARTESIAN_POINT('Ctrl Pts',(0.0067102576653833,-0.0321934096636183,
0.0798083670634014));
#106201=CARTESIAN_POINT('Ctrl Pts',(0.00663222437371599,-0.0320835708272304,
0.0797888734585301));
#106202=CARTESIAN_POINT('Ctrl Pts',(0.00655463976366873,-0.0319739230346346,
0.0797677762658266));
#106203=CARTESIAN_POINT('Ctrl Pts',(0.0064776010277765,-0.0318646057455576,
0.0797451100959295));
#106204=CARTESIAN_POINT('Ctrl Pts',(0.00680532133009763,-0.0321934096636183,
0.0797466899654153));
#106205=CARTESIAN_POINT('Ctrl Pts',(0.00672813861367976,-0.0320835708272304,
0.0797285073625685));
#106206=CARTESIAN_POINT('Ctrl Pts',(0.00665137695439496,-0.0319739230346346,
0.0797087380140656));
#106207=CARTESIAN_POINT('Ctrl Pts',(0.00657513262225446,-0.0318646057455576,
0.079687414750853));
#106208=CARTESIAN_POINT('Ctrl Pts',(0.00692617143840692,-0.0320218834582356,
0.0797746356575945));
#106209=CARTESIAN_POINT('Ctrl Pts',(0.00686763257867941,-0.0319391099350632,
0.0797621714248432));
#106210=CARTESIAN_POINT('Ctrl Pts',(0.00680932381690182,-0.0318564869454893,
0.0797488006513511));
#106211=CARTESIAN_POINT('Ctrl Pts',(0.00675128671408501,-0.0317740741446465,
0.0797345370408407));
#106212=CARTESIAN_POINT('Ctrl Pts',(0.00695224709804686,-0.0320218834582356,
0.0798167888072044));
#106213=CARTESIAN_POINT('Ctrl Pts',(0.00689326952593648,-0.0319391099350632,
0.0798045959590324));
#106214=CARTESIAN_POINT('Ctrl Pts',(0.00683451807987246,-0.0318564869454893,
0.0797914895551393));
#106215=CARTESIAN_POINT('Ctrl Pts',(0.00677603466127906,-0.0317740741446465,
0.079777483136791));
#106216=CARTESIAN_POINT('Ctrl Pts',(0.0069783227576868,-0.0320218834582356,
0.0798589419568143));
#106217=CARTESIAN_POINT('Ctrl Pts',(0.00691890647319356,-0.0319391099350632,
0.0798470204932217));
#106218=CARTESIAN_POINT('Ctrl Pts',(0.0068597123428431,-0.0318564869454893,
0.0798341784589275));
#106219=CARTESIAN_POINT('Ctrl Pts',(0.00680078260847311,-0.0317740741446465,
0.0798204292327412));
#106220=CARTESIAN_POINT('Ctrl Pts',(0.00700439841732674,-0.0320218834582356,
0.0799010951064242));
#106221=CARTESIAN_POINT('Ctrl Pts',(0.00694454342045063,-0.0319391099350632,
0.079889445027411));
#106222=CARTESIAN_POINT('Ctrl Pts',(0.00688490660581373,-0.0318564869454893,
0.0798768673627157));
#106223=CARTESIAN_POINT('Ctrl Pts',(0.00682553055566716,-0.0317740741446465,
0.0798633753286915));
#106224=CARTESIAN_POINT('',(0.,0.,0.));
#106225=CARTESIAN_POINT('Origin',(-0.0411262178068916,-0.00152418147196182,
0.079));
#106226=CARTESIAN_POINT('',(0.0136237821931184,-0.00152418147196182,0.081));
#106227=CARTESIAN_POINT('Origin',(0.0136237821931184,-0.00152418147197183,
0.07900000000001));
#106228=CARTESIAN_POINT('',(0.0161237821931184,-0.00152418147196182,0.081));
#106229=CARTESIAN_POINT('',(-0.0411262178068916,-0.00152418147196182,0.081));
#106230=CARTESIAN_POINT('Origin',(0.0161237821931184,-0.00152418147197183,
0.07900000000001));
#106231=CARTESIAN_POINT('Origin',(0.0161237821931084,-0.00152418147196182,
0.079));
#106232=CARTESIAN_POINT('',(0.0151237821931184,-0.00152418147197183,0.07375));
#106233=CARTESIAN_POINT('Origin',(0.0151237821931184,-0.00152418147197183,
0.07900000000001));
#106234=CARTESIAN_POINT('',(0.0161237821931184,-0.00152418147197183,0.07375));
#106235=CARTESIAN_POINT('',(0.0161237821931084,-0.00152418147196182,0.07375));
#106236=CARTESIAN_POINT('Origin',(0.0161237821931184,-0.00152418147197183,
0.07900000000001));
#106237=CARTESIAN_POINT('Origin',(0.0151237821931084,-0.00152418147196182,
0.079));
#106238=CARTESIAN_POINT('',(0.0136237821931184,-0.00152418147197183,0.0746047698558177));
#106239=CARTESIAN_POINT('Origin',(0.0136237821931184,-0.00152418147197183,
0.07900000000001));
#106240=CARTESIAN_POINT('',(0.0151237821931184,-0.00152418147197183,0.0746047698558177));
#106241=CARTESIAN_POINT('',(0.0151237821931084,-0.00152418147196182,0.0746047698558177));
#106242=CARTESIAN_POINT('Origin',(0.0151237821931184,-0.00152418147197183,
0.07900000000001));
#106243=CARTESIAN_POINT('Origin',(0.0136237821931084,-0.00152418147196182,
0.079));
#106244=CARTESIAN_POINT('Origin',(0.0161237821931084,-0.00152418147196182,
0.079));
#106245=CARTESIAN_POINT('Origin',(0.0151237821931084,-0.00152418147196182,
0.079));
#106246=CARTESIAN_POINT('',(0.,0.,0.));
#106247=CARTESIAN_POINT('Origin',(-0.0411262178068916,-0.00152418147196182,
0.079));
#106248=CARTESIAN_POINT('',(0.0121237821931184,-0.00152418147196182,0.081));
#106249=CARTESIAN_POINT('Origin',(0.0121237821931184,-0.00152418147197183,
0.07900000000001));
#106250=CARTESIAN_POINT('',(0.0136237821931184,-0.00152418147196182,0.081));
#106251=CARTESIAN_POINT('',(-0.0411262178068916,-0.00152418147196182,0.081));
#106252=CARTESIAN_POINT('Origin',(0.0136237821931184,-0.00152418147197183,
0.07900000000001));
#106253=CARTESIAN_POINT('Origin',(0.0136237821931084,-0.00152418147196182,
0.079));
#106254=CARTESIAN_POINT('',(0.0121237821931184,-0.00152418147197183,0.07375));
#106255=CARTESIAN_POINT('Origin',(0.0121237821931184,-0.00152418147197183,
0.07900000000001));
#106256=CARTESIAN_POINT('',(0.0136237821931184,-0.00152418147197183,0.07375));
#106257=CARTESIAN_POINT('',(0.0136237821931084,-0.00152418147196182,0.07375));
#106258=CARTESIAN_POINT('Origin',(0.0136237821931184,-0.00152418147197183,
0.07900000000001));
#106259=CARTESIAN_POINT('Origin',(0.0136237821931084,-0.00152418147196182,
0.079));
#106260=CARTESIAN_POINT('Origin',(0.0121237821931084,-0.00152418147196182,
0.079));
#106261=CARTESIAN_POINT('',(0.,0.,0.));
#106262=CARTESIAN_POINT('Origin',(-0.00312621780689159,0.00227581852803817,
0.0479362915010152));
#106263=CARTESIAN_POINT('',(-0.0071262178069116,0.00227581852804816,0.05991000000001));
#106264=CARTESIAN_POINT('Origin',(-0.0031262178069016,0.00227581852804816,
0.05991000000001));
#106265=CARTESIAN_POINT('',(-0.0071262178069116,0.00227581852804816,0.05925000000001));
#106266=CARTESIAN_POINT('',(-0.00712621780689159,0.00227581852803817,0.0479362915010152));
#106267=CARTESIAN_POINT('Origin',(-0.0031262178069016,0.00227581852804816,
0.05925000000001));
#106268=CARTESIAN_POINT('Origin',(-0.00312621780689159,0.00227581852803817,
0.06603));
#106269=CARTESIAN_POINT('',(0.0026987821931084,0.00227581852804816,0.06169000000001));
#106270=CARTESIAN_POINT('Origin',(-0.0031262178069016,0.00227581852804816,
0.06169000000001));
#106271=CARTESIAN_POINT('',(0.0026987821931084,0.00227581852804816,0.06603000000001));
#106272=CARTESIAN_POINT('',(0.00269878219310841,0.00227581852803817,0.06603));
#106273=CARTESIAN_POINT('Origin',(-0.0031262178069016,0.00227581852804816,
0.06603000000001));
#106274=CARTESIAN_POINT('Origin',(-0.00312621780689159,0.00227581852803817,
0.06169));
#106275=CARTESIAN_POINT('',(-0.0140012178068916,0.00227581852803817,0.06169000000001));
#106276=CARTESIAN_POINT('Origin',(-0.0031262178069016,0.00227581852804816,
0.06169000000001));
#106277=CARTESIAN_POINT('',(-0.0140012178068916,0.00227581852803817,0.06235000000001));
#106278=CARTESIAN_POINT('',(-0.0140012178068916,0.00227581852803817,0.06169));
#106279=CARTESIAN_POINT('Origin',(-0.0031262178069016,0.00227581852804816,
0.06235000000001));
#106280=CARTESIAN_POINT('Origin',(-0.00312621780689159,0.00227581852803817,
0.05991));
#106281=CARTESIAN_POINT('',(0.00774878219310841,0.00227581852803817,0.05991000000001));
#106282=CARTESIAN_POINT('Origin',(-0.0031262178069016,0.00227581852804816,
0.05991000000001));
#106283=CARTESIAN_POINT('',(0.00774878219310841,0.00227581852803817,0.05925000000001));
#106284=CARTESIAN_POINT('',(0.00774878219310841,0.00227581852803817,0.05991));
#106285=CARTESIAN_POINT('Origin',(-0.0031262178069016,0.00227581852804816,
0.05925000000001));
#106286=CARTESIAN_POINT('Origin',(-0.00312621780689159,0.00227581852803817,
0.06235));
#106287=CARTESIAN_POINT('',(-0.00141627505618096,0.0156670879148174,0.06235));
#106288=CARTESIAN_POINT('',(-0.00141627505618096,0.0156670879148174,0.05925));
#106289=CARTESIAN_POINT('',(-0.00141627505619096,0.0156670879148274,0.0640570798288245));
#106290=CARTESIAN_POINT('',(-0.00173858848307247,0.0157043137847554,0.05925));
#106291=CARTESIAN_POINT('Origin',(-0.0031262178069016,0.00227581852804816,
0.05925000000001));
#106292=CARTESIAN_POINT('',(-0.00173858848307247,0.0157043137847554,0.06235));
#106293=CARTESIAN_POINT('',(-0.00173858848308247,0.0157043137847654,0.0640296944304424));
#106294=CARTESIAN_POINT('Origin',(-0.0031262178069016,0.00227581852804816,
0.06235000000001));
#106295=CARTESIAN_POINT('Origin',(-0.00312621780689159,0.00227581852803817,
0.06235));
#106296=CARTESIAN_POINT('',(-9.89011778140814E-5,0.0154320092391563,0.06235));
#106297=CARTESIAN_POINT('',(-9.89011778140883E-5,0.0154320092391563,0.05925));
#106298=CARTESIAN_POINT('',(-9.89011778240814E-5,0.0154320092391663,0.0640570798288245));
#106299=CARTESIAN_POINT('',(0.000216394654050496,0.0153554569762505,0.06235));
#106300=CARTESIAN_POINT('Origin',(-0.0031262178069016,0.00227581852804816,
0.06235000000001));
#106301=CARTESIAN_POINT('',(0.000216394654050503,0.0153554569762505,0.05925));
#106302=CARTESIAN_POINT('',(0.000216394654060503,0.0153554569762605,0.0640610392221439));
#106303=CARTESIAN_POINT('Origin',(-0.0031262178069016,0.00227581852804816,
0.05925000000001));
#106304=CARTESIAN_POINT('Origin',(-0.00312621780689159,0.00227581852803817,
0.06235));
#106305=CARTESIAN_POINT('',(0.00149489509322412,0.014960270253059,0.06235));
#106306=CARTESIAN_POINT('',(0.00149489509322413,0.014960270253059,0.05925));
#106307=CARTESIAN_POINT('',(0.00149489509323412,0.014960270253069,0.0640610392221439));
#106308=CARTESIAN_POINT('',(0.00179839376664563,0.014845552051458,0.06235));
#106309=CARTESIAN_POINT('Origin',(-0.0031262178069016,0.00227581852804816,
0.06235000000001));
#106310=CARTESIAN_POINT('',(0.00179839376664562,0.014845552051458,0.05925));
#106311=CARTESIAN_POINT('',(0.00179839376665562,0.0148455520514679,0.0640414954613587));
#106312=CARTESIAN_POINT('Origin',(-0.0031262178069016,0.00227581852804816,
0.05925000000001));
#106313=CARTESIAN_POINT('Origin',(-0.00312621780689159,0.00227581852803817,
0.06235));
#106314=CARTESIAN_POINT('',(0.00301864000319971,0.0142962479086285,0.06235));
#106315=CARTESIAN_POINT('',(0.0030186400031997,0.0142962479086285,0.05925));
#106316=CARTESIAN_POINT('',(0.00301864000320971,0.0142962479086385,0.0640414954613587));
#106317=CARTESIAN_POINT('',(0.00330574078765853,0.0141451027793312,0.06235));
#106318=CARTESIAN_POINT('Origin',(-0.0031262178069016,0.00227581852804816,
0.06235000000001));
#106319=CARTESIAN_POINT('',(0.00330574078765853,0.0141451027793312,0.05925));
#106320=CARTESIAN_POINT('',(0.00330574078766853,0.0141451027793412,0.0639988309423612));
#106321=CARTESIAN_POINT('Origin',(-0.0031262178069016,0.00227581852804816,
0.05925000000001));
#106322=CARTESIAN_POINT('Origin',(-0.00312621780689159,0.00227581852803817,
0.06235));
#106323=CARTESIAN_POINT('',(0.00444923513249744,0.0134500081077393,0.06235));
#106324=CARTESIAN_POINT('',(0.00444923513249746,0.0134500081077393,0.05925));
#106325=CARTESIAN_POINT('',(0.00444923513250745,0.0134500081077493,0.0639988309423612));
#106326=CARTESIAN_POINT('',(0.00471558587275565,0.013264727256837,0.06235));
#106327=CARTESIAN_POINT('Origin',(-0.0031262178069016,0.00227581852804816,
0.06235000000001));
#106328=CARTESIAN_POINT('',(0.00471558587275565,0.013264727256837,0.05925));
#106329=CARTESIAN_POINT('',(0.00471558587276565,0.013264727256847,0.0639917959462876));
#106330=CARTESIAN_POINT('Origin',(-0.0031262178069016,0.00227581852804816,
0.05925000000001));
#106331=CARTESIAN_POINT('Origin',(-0.00312621780689159,0.00227581852803817,
0.06235));
#106332=CARTESIAN_POINT('',(0.00576499411722559,0.0124343789831635,0.06235));
#106333=CARTESIAN_POINT('',(0.00576499411722558,0.0124343789831635,0.05925));
#106334=CARTESIAN_POINT('',(0.00576499411723559,0.0124343789831735,0.0639917959462876));
#106335=CARTESIAN_POINT('',(0.00600655720756383,0.012217771079491,0.06235));
#106336=CARTESIAN_POINT('Origin',(-0.0031262178069016,0.00227581852804816,
0.06235000000001));
#106337=CARTESIAN_POINT('',(0.00600655720756383,0.012217771079491,0.05925));
#106338=CARTESIAN_POINT('',(0.00600655720757383,0.012217771079501,0.0640024596936978));
#106339=CARTESIAN_POINT('Origin',(-0.0031262178069016,0.00227581852804816,
0.05925000000001));
#106340=CARTESIAN_POINT('Origin',(-0.00312621780689159,0.00227581852803817,
0.06235));
#106341=CARTESIAN_POINT('',(0.00694597139238648,0.0112647564371543,0.06235));
#106342=CARTESIAN_POINT('',(0.00694597139238648,0.0112647564371543,0.05925));
#106343=CARTESIAN_POINT('',(0.00694597139239648,0.0112647564371643,0.0640024596936978));
#106344=CARTESIAN_POINT('',(0.0071590849825911,0.0110201050357333,0.06235));
#106345=CARTESIAN_POINT('Origin',(-0.0031262178069016,0.00227581852804816,
0.06235000000001));
#106346=CARTESIAN_POINT('',(0.0071590849825911,0.0110201050357333,0.05925));
#106347=CARTESIAN_POINT('',(0.0071590849826011,0.0110201050357433,0.0639889835233611));
#106348=CARTESIAN_POINT('Origin',(-0.0031262178069016,0.00227581852804816,
0.05925000000001));
#106349=CARTESIAN_POINT('Origin',(-0.00312621780689159,0.00227581852803817,
0.06235));
#106350=CARTESIAN_POINT('',(0.00797426454631066,0.00995887075526175,0.06235));
#106351=CARTESIAN_POINT('',(0.00797426454631067,0.00995887075526175,0.05925));
#106352=CARTESIAN_POINT('',(0.00797426454632066,0.00995887075527175,0.0639889835233611));
#106353=CARTESIAN_POINT('',(0.00815569805159019,0.00968988452195386,0.06235));
#106354=CARTESIAN_POINT('Origin',(-0.0031262178069016,0.00227581852804816,
0.06235000000001));
#106355=CARTESIAN_POINT('',(0.00815569805159019,0.00968988452195386,0.05925));
#106356=CARTESIAN_POINT('',(0.00815569805160019,0.00968988452196386,0.0640049766461123));
#106357=CARTESIAN_POINT('Origin',(-0.0031262178069016,0.00227581852804816,
0.05925000000001));
#106358=CARTESIAN_POINT('Origin',(-0.00312621780689159,0.00227581852803817,
0.06235));
#106359=CARTESIAN_POINT('',(0.00883428570296894,0.00853651783327664,0.06235));
#106360=CARTESIAN_POINT('',(0.00883428570296894,0.00853651783327664,0.05925));
#106361=CARTESIAN_POINT('',(0.00883428570297895,0.00853651783328664,0.0640049766461123));
#106362=CARTESIAN_POINT('',(0.00898128877632649,0.00824727432518939,0.06235));
#106363=CARTESIAN_POINT('Origin',(-0.0031262178069016,0.00227581852804816,
0.06235000000001));
#106364=CARTESIAN_POINT('',(0.00898128877632649,0.00824727432518939,0.05925));
#106365=CARTESIAN_POINT('',(0.00898128877633649,0.00824727432519939,0.064044978432889));
#106366=CARTESIAN_POINT('Origin',(-0.0031262178069016,0.00227581852804816,
0.05925000000001));
#106367=CARTESIAN_POINT('Origin',(-0.00312621780689159,0.00227581852803817,
0.06235));
#106368=CARTESIAN_POINT('',(0.00951299781828371,0.00701925909162959,0.06235));
#106369=CARTESIAN_POINT('',(0.0095129978182837,0.00701925909162959,0.05925));
#106370=CARTESIAN_POINT('',(0.00951299781829371,0.00701925909163959,0.064044978432889));
#106371=CARTESIAN_POINT('',(0.00962334204297382,0.00671414294550698,0.06235));
#106372=CARTESIAN_POINT('Origin',(-0.0031262178069016,0.00227581852804816,
0.06235000000001));
#106373=CARTESIAN_POINT('',(0.00962334204297382,0.00671414294550698,0.05925));
#106374=CARTESIAN_POINT('',(0.00962334204298382,0.00671414294551698,0.0640617910186538));
#106375=CARTESIAN_POINT('Origin',(-0.0031262178069016,0.00227581852804816,
0.05925000000001));
#106376=CARTESIAN_POINT('Origin',(-0.00312621780689159,0.00227581852803817,
0.06235));
#106377=CARTESIAN_POINT('',(0.0100001123084278,0.00543009462623556,0.06235));
#106378=CARTESIAN_POINT('',(0.0100001123084278,0.00543009462623556,0.05925));
#106379=CARTESIAN_POINT('',(0.0100001123084378,0.00543009462624556,0.0640617910186538));
#106380=CARTESIAN_POINT('',(0.0100721249784829,0.00511373109183454,0.06235));
#106381=CARTESIAN_POINT('Origin',(-0.0031262178069016,0.00227581852804816,
0.06235000000001));
#106382=CARTESIAN_POINT('',(0.0100721249784829,0.00511373109183452,0.05925));
#106383=CARTESIAN_POINT('',(0.0100721249784929,0.00511373109184452,0.0640550858195668));
#106384=CARTESIAN_POINT('Origin',(-0.0031262178069016,0.00227581852804816,
0.05925000000001));
#106385=CARTESIAN_POINT('Origin',(-0.00312621780689159,0.00227581852803817,
0.06235));
#106386=CARTESIAN_POINT('',(0.0102882450142678,0.00379311455048486,0.06235));
#106387=CARTESIAN_POINT('',(0.0102882450142678,0.00379311455048487,0.05925));
#106388=CARTESIAN_POINT('',(0.0102882450142778,0.00379311455049486,0.0640550858195668));
#106389=CARTESIAN_POINT('',(0.0103208344910155,0.0034702993765037,0.06235));
#106390=CARTESIAN_POINT('Origin',(-0.0031262178069016,0.00227581852804816,
0.06235000000001));
#106391=CARTESIAN_POINT('',(0.0103208344910155,0.0034702993765037,0.05925));
#106392=CARTESIAN_POINT('',(0.0103208344910255,0.0034702993765137,0.0640254477644275));
#106393=CARTESIAN_POINT('Origin',(-0.0031262178069016,0.00227581852804816,
0.05925000000001));
#106394=CARTESIAN_POINT('Origin',(-0.00312621780689159,0.00227581852803817,
0.06235));
#106395=CARTESIAN_POINT('',(0.0103730281376895,0.00213313381368028,0.06235));
#106396=CARTESIAN_POINT('',(0.0103730281376895,0.00213313381368028,0.05925));
#106397=CARTESIAN_POINT('',(0.0103730281376995,0.00213313381369029,0.0640254477644275));
#106398=CARTESIAN_POINT('',(0.0103657003978822,0.00180876054909688,0.06235));
#106399=CARTESIAN_POINT('Origin',(-0.0031262178069016,0.00227581852804816,
0.06235000000001));
#106400=CARTESIAN_POINT('',(0.0103657003978822,0.00180876054909688,0.05925));
#106401=CARTESIAN_POINT('',(0.0103657003978922,0.00180876054910688,0.0640387154811168));
#106402=CARTESIAN_POINT('Origin',(-0.0031262178069016,0.00227581852804816,
0.05925000000001));
#106403=CARTESIAN_POINT('Origin',(-0.00312621780689159,0.00227581852803817,
0.06235));
#106404=CARTESIAN_POINT('',(0.0102531764529649,0.000475316031700583,0.06235));
#106405=CARTESIAN_POINT('',(0.0102531764529649,0.000475316031700583,0.05925));
#106406=CARTESIAN_POINT('',(0.0102531764529749,0.000475316031710583,0.0640387154811168));
#106407=CARTESIAN_POINT('',(0.0102060425776687,0.000154301844558103,0.06235));
#106408=CARTESIAN_POINT('Origin',(-0.0031262178069016,0.00227581852804816,
0.06235000000001));
#106409=CARTESIAN_POINT('',(0.0102060425776687,0.000154301844558114,0.05925));
#106410=CARTESIAN_POINT('',(0.0102060425776787,0.000154301844568114,0.0640602767163006));
#106411=CARTESIAN_POINT('Origin',(-0.0031262178069016,0.00227581852804816,
0.05925000000001));
#106412=CARTESIAN_POINT('Origin',(-0.00312621780689159,0.00227581852803817,
0.06235));
#106413=CARTESIAN_POINT('',(0.00993050678946452,-0.00115520796776584,0.06235));
#106414=CARTESIAN_POINT('',(0.00993050678946452,-0.00115520796776584,0.05925));
#106415=CARTESIAN_POINT('',(0.00993050678947452,-0.00115520796777584,0.0640602767163006));
#106416=CARTESIAN_POINT('',(0.00984428128018315,-0.00146799682961414,0.06235));
#106417=CARTESIAN_POINT('Origin',(-0.0031262178069016,0.00227581852804816,
0.06235000000001));
#106418=CARTESIAN_POINT('',(0.00984428128018315,-0.00146799682961413,0.05925));
#106419=CARTESIAN_POINT('',(0.00984428128019315,-0.00146799682962413,0.06405834964241));
#106420=CARTESIAN_POINT('Origin',(-0.0031262178069016,0.00227581852804816,
0.05925000000001));
#106421=CARTESIAN_POINT('Origin',(-0.00312621780689159,0.00227581852803817,
0.06235));
#106422=CARTESIAN_POINT('',(0.00940991049037555,-0.00273372110295171,0.06235));
#106423=CARTESIAN_POINT('',(0.00940991049037555,-0.0027337211029517,0.05925));
#106424=CARTESIAN_POINT('',(0.00940991049038555,-0.00273372110296171,0.06405834964241));
#106425=CARTESIAN_POINT('',(0.0092859004379363,-0.00303354307919961,0.06235));
#106426=CARTESIAN_POINT('Origin',(-0.0031262178069016,0.00227581852804816,
0.06235000000001));
#106427=CARTESIAN_POINT('',(0.0092859004379363,-0.0030335430791996,0.05925));
#106428=CARTESIAN_POINT('',(0.0092859004379463,-0.0030335430792096,0.064032971803583));
#106429=CARTESIAN_POINT('Origin',(-0.0031262178069016,0.00227581852804816,
0.05925000000001));
#106430=CARTESIAN_POINT('Origin',(-0.00312621780689159,0.00227581852803817,
0.06235));
#106431=CARTESIAN_POINT('',(0.00529718495642217,-0.00827388696012587,0.06235));
#106432=CARTESIAN_POINT('',(0.00529718495642217,-0.00827388696012587,0.05925));
#106433=CARTESIAN_POINT('',(0.00529718495643217,-0.00827388696013587,0.0639818602956537));
#106434=CARTESIAN_POINT('',(0.00554828316999589,-0.00806840849972849,0.05925));
#106435=CARTESIAN_POINT('Origin',(-0.0031262178069016,0.00227581852804816,
0.05925000000001));
#106436=CARTESIAN_POINT('',(0.00554828316999589,-0.00806840849972849,0.06235));
#106437=CARTESIAN_POINT('',(0.00554828317000589,-0.00806840849973849,0.064001351848484));
#106438=CARTESIAN_POINT('Origin',(-0.0031262178069016,0.00227581852804816,
0.06235000000001));
#106439=CARTESIAN_POINT('Origin',(-0.00312621780689159,0.00227581852803817,
0.06235));
#106440=CARTESIAN_POINT('',(0.00652977513110488,-0.00715878800225032,0.06235));
#106441=CARTESIAN_POINT('',(0.00652977513110488,-0.00715878800225032,0.05925));
#106442=CARTESIAN_POINT('',(0.00652977513111488,-0.00715878800226032,0.064001351848484));
#106443=CARTESIAN_POINT('',(0.00675371925143076,-0.00692400993360114,0.05925));
#106444=CARTESIAN_POINT('Origin',(-0.0031262178069016,0.00227581852804816,
0.05925000000001));
#106445=CARTESIAN_POINT('',(0.00675371925143076,-0.00692400993360114,0.06235));
#106446=CARTESIAN_POINT('',(0.00675371925144076,-0.00692400993361114,0.0639967221271783));
#106447=CARTESIAN_POINT('Origin',(-0.0031262178069016,0.00227581852804816,
0.06235000000001));
#106448=CARTESIAN_POINT('Origin',(-0.00312621780689159,0.00227581852803817,
0.06235));
#106449=CARTESIAN_POINT('',(0.00761599029562478,-0.00590067002648398,0.06235));
#106450=CARTESIAN_POINT('',(0.00761599029562478,-0.00590067002648399,0.05925));
#106451=CARTESIAN_POINT('',(0.00761599029563478,-0.00590067002649399,0.0639967221271783));
#106452=CARTESIAN_POINT('',(0.00780938555811477,-0.00564015134578409,0.05925));
#106453=CARTESIAN_POINT('Origin',(-0.0031262178069016,0.00227581852804816,
0.05925000000001));
#106454=CARTESIAN_POINT('',(0.00780938555811477,-0.00564015134578409,0.06235));
#106455=CARTESIAN_POINT('',(0.00780938555812477,-0.00564015134579409,0.0639846412563078));
#106456=CARTESIAN_POINT('Origin',(-0.0031262178069016,0.00227581852804816,
0.06235000000001));
#106457=CARTESIAN_POINT('Origin',(-0.00312621780689159,0.00227581852803817,
0.06235));
#106458=CARTESIAN_POINT('',(0.00869927926492554,-0.00423629472377529,0.06235));
#106459=CARTESIAN_POINT('',(0.00869927926492554,-0.00423629472377528,0.05925));
#106460=CARTESIAN_POINT('',(0.00869927926493554,-0.00423629472378529,0.064032971803583));
#106461=CARTESIAN_POINT('',(0.00853936453531453,-0.00451860481888456,0.06235));
#106462=CARTESIAN_POINT('Origin',(-0.0031262178069016,0.00227581852804816,
0.06235000000001));
#106463=CARTESIAN_POINT('',(0.00853936453531453,-0.00451860481888456,0.05925));
#106464=CARTESIAN_POINT('',(0.00853936453532453,-0.00451860481889456,0.0639846412563078));
#106465=CARTESIAN_POINT('Origin',(-0.0031262178069016,0.00227581852804816,
0.05925000000001));
#106466=CARTESIAN_POINT('Origin',(-0.00312621780689159,0.00227581852803817,
0.06235));
#106467=CARTESIAN_POINT('',(0.0042113504960508,-0.00905599912843934,0.06235));
#106468=CARTESIAN_POINT('',(0.0042113504960508,-0.00905599912843933,0.05925));
#106469=CARTESIAN_POINT('',(0.00421135049606079,-0.00905599912844934,0.0639818602956537));
#106470=CARTESIAN_POINT('',(0.00393690458219163,-0.00922906313657846,0.06235));
#106471=CARTESIAN_POINT('Origin',(-0.0031262178069016,0.00227581852804816,
0.06235000000001));
#106472=CARTESIAN_POINT('',(0.00393690458219163,-0.00922906313657845,0.05925));
#106473=CARTESIAN_POINT('',(0.00393690458220163,-0.00922906313658845,0.0640171157235625));
#106474=CARTESIAN_POINT('Origin',(-0.0031262178069016,0.00227581852804816,
0.05925000000001));
#106475=CARTESIAN_POINT('Origin',(-0.00312621780689159,0.00227581852803817,
0.06235));
#106476=CARTESIAN_POINT('',(0.00276318776613839,-0.00987181095249685,0.06235));
#106477=CARTESIAN_POINT('',(0.00276318776613839,-0.00987181095249684,0.05925));
#106478=CARTESIAN_POINT('',(0.0027631877661484,-0.00987181095250685,0.0640171157235625));
#106479=CARTESIAN_POINT('',(0.00246955447229308,-0.0100098370344261,0.06235));
#106480=CARTESIAN_POINT('Origin',(-0.0031262178069016,0.00227581852804816,
0.06235000000001));
#106481=CARTESIAN_POINT('',(0.00246955447229308,-0.0100098370344261,0.05925));
#106482=CARTESIAN_POINT('',(0.00246955447230308,-0.0100098370344361,0.0640513762773574));
#106483=CARTESIAN_POINT('Origin',(-0.0031262178069016,0.00227581852804816,
0.05925000000001));
#106484=CARTESIAN_POINT('Origin',(-0.00312621780689159,0.00227581852803817,
0.06235));
#106485=CARTESIAN_POINT('',(0.00122574765106832,-0.0105034770962411,0.06235));
#106486=CARTESIAN_POINT('',(0.00122574765106833,-0.0105034770962411,0.05925));
#106487=CARTESIAN_POINT('',(0.00122574765107832,-0.0105034770962511,0.0640513762773574));
#106488=CARTESIAN_POINT('',(0.00091737815865827,-0.0106043729172544,0.06235));
#106489=CARTESIAN_POINT('Origin',(-0.0031262178069016,0.00227581852804816,
0.06235000000001));
#106490=CARTESIAN_POINT('',(0.00091737815865827,-0.0106043729172544,0.05925));
#106491=CARTESIAN_POINT('',(0.00091737815866827,-0.0106043729172644,0.0640623222440636));
#106492=CARTESIAN_POINT('Origin',(-0.0031262178069016,0.00227581852804816,
0.05925000000001));
#106493=CARTESIAN_POINT('Origin',(-0.00312621780689159,0.00227581852803817,
0.06235));
#106494=CARTESIAN_POINT('',(-0.000377663824195094,-0.010941422144818,0.06235));
#106495=CARTESIAN_POINT('',(-0.000377663824195087,-0.010941422144818,0.05925));
#106496=CARTESIAN_POINT('',(-0.000377663824205095,-0.010941422144828,0.0640623222440636));
#106497=CARTESIAN_POINT('',(-0.000696094947999507,-0.0110036582271164,0.06235));
#106498=CARTESIAN_POINT('Origin',(-0.0031262178069016,0.00227581852804816,
0.06235000000001));
#106499=CARTESIAN_POINT('',(-0.000696094947999507,-0.0110036582271164,0.05925));
#106500=CARTESIAN_POINT('',(-0.000696094948009507,-0.0110036582271264,0.0640497400911727));
#106501=CARTESIAN_POINT('Origin',(-0.0031262178069016,0.00227581852804816,
0.05925000000001));
#106502=CARTESIAN_POINT('Origin',(-0.00312621780689159,0.00227581852803817,
0.06235));
#106503=CARTESIAN_POINT('',(-0.00202274057611456,-0.0111790072977077,0.06235));
#106504=CARTESIAN_POINT('',(-0.00202274057611456,-0.0111790072977077,0.05925));
#106505=CARTESIAN_POINT('',(-0.00202274057612456,-0.0111790072977176,0.0640497400911727));
#106506=CARTESIAN_POINT('',(-0.00234640624006724,-0.0112016402057234,0.06235));
#106507=CARTESIAN_POINT('Origin',(-0.0031262178069016,0.00227581852804816,
0.06235000000001));
#106508=CARTESIAN_POINT('',(-0.00234640624006724,-0.0112016402057234,0.05925));
#106509=CARTESIAN_POINT('',(-0.00234640624007724,-0.0112016402057334,0.0640207658501784));
#106510=CARTESIAN_POINT('Origin',(-0.0031262178069016,0.00227581852804816,
0.05925000000001));
#106511=CARTESIAN_POINT('Origin',(-0.00312621780689159,0.00227581852803817,
0.06235));
#106512=CARTESIAN_POINT('',(-0.00368454491802983,-0.0112126310061732,0.06235));
#106513=CARTESIAN_POINT('',(-0.00368454491802983,-0.0112126310061732,0.05925));
#106514=CARTESIAN_POINT('',(-0.00368454491803983,-0.0112126310061832,0.0640207658501784));
#106515=CARTESIAN_POINT('',(-0.00400853868059187,-0.0111953176480916,0.06235));
#106516=CARTESIAN_POINT('Origin',(-0.0031262178069016,0.00227581852804816,
0.06235000000001));
#106517=CARTESIAN_POINT('',(-0.00400853868059187,-0.0111953176480916,0.05925));
#106518=CARTESIAN_POINT('',(-0.00400853868060188,-0.0111953176481016,0.0640462926264831));
#106519=CARTESIAN_POINT('Origin',(-0.0031262178069016,0.00227581852804816,
0.05925000000001));
#106520=CARTESIAN_POINT('Origin',(-0.00312621780689159,0.00227581852803817,
0.06235));
#106521=CARTESIAN_POINT('',(-0.00533788559006755,-0.0110417835690686,0.06235));
#106522=CARTESIAN_POINT('',(-0.00533788559006755,-0.0110417835690686,0.05925));
#106523=CARTESIAN_POINT('',(-0.00533788559007755,-0.0110417835690786,0.0640462926264831));
#106524=CARTESIAN_POINT('',(-0.00565729603605961,-0.0109847863977498,0.06235));
#106525=CARTESIAN_POINT('Origin',(-0.0031262178069016,0.00227581852804816,
0.06235000000001));
#106526=CARTESIAN_POINT('',(-0.00565729603605961,-0.0109847863977498,0.05925));
#106527=CARTESIAN_POINT('',(-0.00565729603606961,-0.0109847863977598,0.0640620033446139));
#106528=CARTESIAN_POINT('Origin',(-0.0031262178069016,0.00227581852804816,
0.05925000000001));
#106529=CARTESIAN_POINT('Origin',(-0.00312621780689159,0.00227581852803817,
0.06235));
#106530=CARTESIAN_POINT('',(-0.00695769963296234,-0.0106690548593878,0.06235));
#106531=CARTESIAN_POINT('',(-0.00695769963296234,-0.0106690548593878,0.05925));
#106532=CARTESIAN_POINT('',(-0.00695769963297234,-0.0106690548593978,0.0640620033446139));
#106533=CARTESIAN_POINT('',(-0.00726768482561223,-0.0105732378938494,0.06235));
#106534=CARTESIAN_POINT('Origin',(-0.0031262178069016,0.00227581852804816,
0.06235000000001));
#106535=CARTESIAN_POINT('',(-0.00726768482561223,-0.0105732378938494,0.05925));
#106536=CARTESIAN_POINT('',(-0.00726768482562223,-0.0105732378938594,0.0640541921468464));
#106537=CARTESIAN_POINT('Origin',(-0.0031262178069016,0.00227581852804816,
0.05925000000001));
#106538=CARTESIAN_POINT('Origin',(-0.00312621780689159,0.00227581852803817,
0.06235));
#106539=CARTESIAN_POINT('',(-0.00851943231697142,-0.0101000950644311,0.06235));
#106540=CARTESIAN_POINT('',(-0.00851943231697142,-0.010100095064431,0.05925));
#106541=CARTESIAN_POINT('',(-0.00851943231698142,-0.0101000950644411,0.0640541921468464));
#106542=CARTESIAN_POINT('',(-0.00881529319674008,-0.00996691079220006,0.06235));
#106543=CARTESIAN_POINT('Origin',(-0.0031262178069016,0.00227581852804816,
0.06235000000001));
#106544=CARTESIAN_POINT('',(-0.00881529319674006,-0.00996691079220006,0.05925));
#106545=CARTESIAN_POINT('',(-0.00881529319675006,-0.00996691079221006,0.064023011312257));
#106546=CARTESIAN_POINT('Origin',(-0.0031262178069016,0.00227581852804816,
0.05925000000001));
#106547=CARTESIAN_POINT('Origin',(-0.00312621780689159,0.00227581852803817,
0.06235));
#106548=CARTESIAN_POINT('',(-0.00999940936654784,-0.00934352903472414,0.06235));
#106549=CARTESIAN_POINT('',(-0.00999940936654784,-0.00934352903472414,0.05925));
#106550=CARTESIAN_POINT('',(-0.00999940936655784,-0.00934352903473414,0.064023011312257));
#106551=CARTESIAN_POINT('',(-0.0102766609840819,-0.00917499639360702,0.06235));
#106552=CARTESIAN_POINT('Origin',(-0.0031262178069016,0.00227581852804816,
0.06235000000001));
#106553=CARTESIAN_POINT('',(-0.0102766609840819,-0.00917499639360702,0.05925));
#106554=CARTESIAN_POINT('',(-0.0102766609840919,-0.00917499639361702,0.0639774518569539));
#106555=CARTESIAN_POINT('Origin',(-0.0031262178069016,0.00227581852804816,
0.05925000000001));
#106556=CARTESIAN_POINT('Origin',(-0.00312621780689159,0.00227581852803817,
0.06235));
#106557=CARTESIAN_POINT('',(-0.0128537065572342,-0.00708505550230524,0.06235));
#106558=CARTESIAN_POINT('',(-0.0128537065572342,-0.00708505550230524,0.05925));
#106559=CARTESIAN_POINT('',(-0.0128537065572442,-0.00708505550231524,0.0639987344374706));
#106560=CARTESIAN_POINT('',(-0.0126259362114935,-0.00731612341472131,0.05925));
#106561=CARTESIAN_POINT('Origin',(-0.0031262178069016,0.00227581852804816,
0.05925000000001));
#106562=CARTESIAN_POINT('',(-0.0126259362114935,-0.00731612341472131,0.06235));
#106563=CARTESIAN_POINT('',(-0.0126259362115035,-0.00731612341473131,0.0640001436149048));
#106564=CARTESIAN_POINT('Origin',(-0.0031262178069016,0.00227581852804816,
0.06235000000001));
#106565=CARTESIAN_POINT('Origin',(-0.00312621780689159,0.00227581852803817,
0.06235));
#106566=CARTESIAN_POINT('',(-0.0113751958382256,-0.00841082554007646,0.06235));
#106567=CARTESIAN_POINT('',(-0.0113751958382256,-0.00841082554007647,0.05925));
#106568=CARTESIAN_POINT('',(-0.0113751958382356,-0.00841082554008646,0.0639774518569539));
#106569=CARTESIAN_POINT('',(-0.011629635341618,-0.00820949931311987,0.06235));
#106570=CARTESIAN_POINT('Origin',(-0.0031262178069016,0.00227581852804816,
0.06235000000001));
#106571=CARTESIAN_POINT('',(-0.011629635341618,-0.00820949931311987,0.05925));
#106572=CARTESIAN_POINT('',(-0.011629635341628,-0.00820949931312987,0.0640001436149048));
#106573=CARTESIAN_POINT('Origin',(-0.0031262178069016,0.00227581852804816,
0.05925000000001));
#106574=CARTESIAN_POINT('Origin',(-0.00312621780689159,0.00227581852803817,
0.06235));
#106575=CARTESIAN_POINT('',(-0.0137326705372273,-0.00607601722700116,0.06235));
#106576=CARTESIAN_POINT('',(-0.0137326705372273,-0.00607601722700116,0.05925));
#106577=CARTESIAN_POINT('',(-0.0137326705372373,-0.00607601722701116,0.0639987344374706));
#106578=CARTESIAN_POINT('',(-0.0139303189590513,-0.00581871038314018,0.06235));
#106579=CARTESIAN_POINT('Origin',(-0.0031262178069016,0.00227581852804816,
0.06235000000001));
#106580=CARTESIAN_POINT('',(-0.0139303189590513,-0.00581871038314018,0.05925));
#106581=CARTESIAN_POINT('',(-0.0139303189590613,-0.00581871038315018,0.06397650941056));
#106582=CARTESIAN_POINT('Origin',(-0.0031262178069016,0.00227581852804816,
0.05925000000001));
#106583=CARTESIAN_POINT('Origin',(-0.00312621780689159,0.00227581852803817,
0.06235));
#106584=CARTESIAN_POINT('',(-0.0146786218511919,-0.00470930572262721,0.06235));
#106585=CARTESIAN_POINT('',(-0.0146786218511919,-0.00470930572262721,0.05925));
#106586=CARTESIAN_POINT('',(-0.0146786218512019,-0.00470930572263721,0.06397650941056));
#106587=CARTESIAN_POINT('',(-0.0148431522004959,-0.00442966045679009,0.06235));
#106588=CARTESIAN_POINT('Origin',(-0.0031262178069016,0.00227581852804816,
0.06235000000001));
#106589=CARTESIAN_POINT('',(-0.0148431522004959,-0.00442966045679009,0.05925));
#106590=CARTESIAN_POINT('',(-0.0148431522005059,-0.00442966045680008,0.0640278376069454));
#106591=CARTESIAN_POINT('Origin',(-0.0031262178069016,0.00227581852804816,
0.05925000000001));
#106592=CARTESIAN_POINT('Origin',(-0.00312621780689159,0.00227581852803817,
0.06235));
#106593=CARTESIAN_POINT('',(-0.0154494504957172,-0.00323670685485675,0.06235));
#106594=CARTESIAN_POINT('',(-0.0154494504957172,-0.00323670685485676,0.05925));
#106595=CARTESIAN_POINT('',(-0.0154494504957272,-0.00323670685486675,0.0640278376069454));
#106596=CARTESIAN_POINT('',(-0.0155783686601187,-0.00293896230421893,0.06235));
#106597=CARTESIAN_POINT('Origin',(-0.0031262178069016,0.00227581852804816,
0.06235000000001));
#106598=CARTESIAN_POINT('',(-0.0155783686601187,-0.00293896230421893,0.05925));
#106599=CARTESIAN_POINT('',(-0.0155783686601287,-0.00293896230422892,0.0640563147052341));
#106600=CARTESIAN_POINT('Origin',(-0.0031262178069016,0.00227581852804816,
0.05925000000001));
#106601=CARTESIAN_POINT('Origin',(-0.00312621780689159,0.00227581852803817,
0.06235));
#106602=CARTESIAN_POINT('',(-0.0160334714942915,-0.00168054372144059,0.06235));
#106603=CARTESIAN_POINT('',(-0.0160334714942915,-0.00168054372144059,0.05925));
#106604=CARTESIAN_POINT('',(-0.0160334714943015,-0.00168054372145059,0.0640563147052341));
#106605=CARTESIAN_POINT('',(-0.0161248232058302,-0.00136921338988561,0.06235));
#106606=CARTESIAN_POINT('Origin',(-0.0031262178069016,0.00227581852804816,
0.06235000000001));
#106607=CARTESIAN_POINT('',(-0.0161248232058302,-0.00136921338988561,0.05925));
#106608=CARTESIAN_POINT('',(-0.0161248232058402,-0.00136921338989561,0.064061380725474));
#106609=CARTESIAN_POINT('Origin',(-0.0031262178069016,0.00227581852804816,
0.05925000000001));
#106610=CARTESIAN_POINT('Origin',(-0.00312621780689159,0.00227581852803817,
0.06235));
#106611=CARTESIAN_POINT('',(-0.0164218316838949,-6.44061692159324E-5,0.06235));
#106612=CARTESIAN_POINT('',(-0.0164218316838948,-6.44061692159359E-5,0.05925));
#106613=CARTESIAN_POINT('',(-0.0164218316839049,-6.44061692259324E-5,0.064061380725474));
#106614=CARTESIAN_POINT('',(-0.0164742321437426,0.000255790492782481,0.06235));
#106615=CARTESIAN_POINT('Origin',(-0.0031262178069016,0.00227581852804816,
0.06235000000001));
#106616=CARTESIAN_POINT('',(-0.0164742321437426,0.000255790492782477,0.05925));
#106617=CARTESIAN_POINT('',(-0.0164742321437527,0.000255790492792477,0.0640429369448856));
#106618=CARTESIAN_POINT('Origin',(-0.0031262178069016,0.00227581852804816,
0.05925000000001));
#106619=CARTESIAN_POINT('Origin',(-0.00312621780689159,0.00227581852803817,
0.06235));
#106620=CARTESIAN_POINT('',(-0.0166086439199253,0.00158720680392539,0.06235));
#106621=CARTESIAN_POINT('',(-0.0166086439199253,0.00158720680392539,0.05925));
#106622=CARTESIAN_POINT('',(-0.0166086439199353,0.00158720680393539,0.0640429369448856));
#106623=CARTESIAN_POINT('',(-0.016621298790525,0.00191141594136183,0.06235));
#106624=CARTESIAN_POINT('Origin',(-0.0031262178069016,0.00227581852804816,
0.06235000000001));
#106625=CARTESIAN_POINT('',(-0.016621298790525,0.00191141594136184,0.05925));
#106626=CARTESIAN_POINT('',(-0.016621298790535,0.00191141594137184,0.0640221869975759));
#106627=CARTESIAN_POINT('Origin',(-0.0031262178069016,0.00227581852804816,
0.05925000000001));
#106628=CARTESIAN_POINT('Origin',(-0.00312621780689159,0.00227581852803817,
0.06235));
#106629=CARTESIAN_POINT('',(-0.0165910763193107,0.00324925842887212,0.06235));
#106630=CARTESIAN_POINT('',(-0.0165910763193107,0.00324925842887211,0.05925));
#106631=CARTESIAN_POINT('',(-0.0165910763193207,0.00324925842888212,0.0640221869975759));
#106632=CARTESIAN_POINT('',(-0.0165637937657236,0.00357256536170368,0.06235));
#106633=CARTESIAN_POINT('Origin',(-0.0031262178069016,0.00227581852804816,
0.06235000000001));
#106634=CARTESIAN_POINT('',(-0.0165637937657236,0.00357256536170368,0.05925));
#106635=CARTESIAN_POINT('',(-0.0165637937657335,0.00357256536171368,0.0640524165708933));
#106636=CARTESIAN_POINT('Origin',(-0.0031262178069016,0.00227581852804816,
0.05925000000001));
#106637=CARTESIAN_POINT('Origin',(-0.00312621780689159,0.00227581852803817,
0.06235));
#106638=CARTESIAN_POINT('',(-0.0163693951889687,0.00489655369719221,0.06235));
#106639=CARTESIAN_POINT('',(-0.0163693951889687,0.00489655369719221,0.05925));
#106640=CARTESIAN_POINT('',(-0.0163693951889787,0.00489655369720221,0.0640524165708933));
#106641=CARTESIAN_POINT('',(-0.0163025887868969,0.00521405742187809,0.06235));
#106642=CARTESIAN_POINT('Origin',(-0.0031262178069016,0.00227581852804816,
0.06235000000001));
#106643=CARTESIAN_POINT('',(-0.0163025887868969,0.00521405742187809,0.05925));
#106644=CARTESIAN_POINT('',(-0.0163025887869069,0.00521405742188809,0.0640622576161447));
#106645=CARTESIAN_POINT('Origin',(-0.0031262178069016,0.00227581852804816,
0.05925000000001));
#106646=CARTESIAN_POINT('Origin',(-0.00312621780689159,0.00227581852803817,
0.06235));
#106647=CARTESIAN_POINT('',(-0.00795506065672538,0.0148826530526763,0.06235));
#106648=CARTESIAN_POINT('',(-0.00795506065672538,0.0148826530526763,0.05925));
#106649=CARTESIAN_POINT('',(-0.00795506065673538,0.0148826530526863,0.0640597876943085));
#106650=CARTESIAN_POINT('',(-0.0082566340354141,0.0147629650924905,0.05925));
#106651=CARTESIAN_POINT('Origin',(-0.0031262178069016,0.00227581852804816,
0.05925000000001));
#106652=CARTESIAN_POINT('',(-0.0082566340354141,0.0147629650924905,0.06235));
#106653=CARTESIAN_POINT('',(-0.0082566340354241,0.0147629650925005,0.0640371289970171));
#106654=CARTESIAN_POINT('Origin',(-0.0031262178069016,0.00227581852804816,
0.06235000000001));
#106655=CARTESIAN_POINT('Origin',(-0.00312621780689159,0.00227581852803817,
0.06235));
#106656=CARTESIAN_POINT('',(-0.00946769283447502,0.0141936914286247,0.06235));
#106657=CARTESIAN_POINT('',(-0.00946769283447502,0.0141936914286247,0.05925));
#106658=CARTESIAN_POINT('',(-0.00946769283448502,0.0141936914286347,0.0640371289970171));
#106659=CARTESIAN_POINT('',(-0.00975227219181637,0.0140378508051584,0.05925));
#106660=CARTESIAN_POINT('Origin',(-0.0031262178069016,0.00227581852804816,
0.05925000000001));
#106661=CARTESIAN_POINT('',(-0.00975227219181637,0.0140378508051584,0.06235));
#106662=CARTESIAN_POINT('',(-0.00975227219182637,0.0140378508051684,0.0639914355303226));
#106663=CARTESIAN_POINT('Origin',(-0.0031262178069016,0.00227581852804816,
0.06235000000001));
#106664=CARTESIAN_POINT('Origin',(-0.00312621780689159,0.00227581852803817,
0.06235));
#106665=CARTESIAN_POINT('',(-0.0108841947149502,0.0133240669998109,0.06235));
#106666=CARTESIAN_POINT('',(-0.0108841947149502,0.0133240669998109,0.05925));
#106667=CARTESIAN_POINT('',(-0.0108841947149602,0.0133240669998209,0.0639914355303226));
#106668=CARTESIAN_POINT('',(-0.0111474661179711,0.0131344360980608,0.05925));
#106669=CARTESIAN_POINT('Origin',(-0.0031262178069016,0.00227581852804816,
0.05925000000001));
#106670=CARTESIAN_POINT('',(-0.0111474661179711,0.0131344360980608,0.06235));
#106671=CARTESIAN_POINT('',(-0.0111474661179811,0.0131344360980708,0.0639946102147355));
#106672=CARTESIAN_POINT('Origin',(-0.0031262178069016,0.00227581852804816,
0.06235000000001));
#106673=CARTESIAN_POINT('Origin',(-0.00312621780689159,0.00227581852803817,
0.06235));
#106674=CARTESIAN_POINT('',(-0.0121830935735454,0.0122869623861294,0.06235));
#106675=CARTESIAN_POINT('',(-0.0121830935735454,0.0122869623861294,0.05925));
#106676=CARTESIAN_POINT('',(-0.0121830935735554,0.0122869623861394,0.0639946102147355));
#106677=CARTESIAN_POINT('',(-0.0124210660961402,0.0120664158172669,0.05925));
#106678=CARTESIAN_POINT('Origin',(-0.0031262178069016,0.00227581852804816,
0.05925000000001));
#106679=CARTESIAN_POINT('',(-0.0124210660961402,0.0120664158172669,0.06235));
#106680=CARTESIAN_POINT('',(-0.0124210660961502,0.0120664158172769,0.0640020568079385));
#106681=CARTESIAN_POINT('Origin',(-0.0031262178069016,0.00227581852804816,
0.06235000000001));
#106682=CARTESIAN_POINT('Origin',(-0.00312621780689159,0.00227581852803817,
0.06235));
#106683=CARTESIAN_POINT('',(-0.013344699427589,0.0110980990363574,0.06235));
#106684=CARTESIAN_POINT('',(-0.013344699427589,0.0110980990363574,0.05925));
#106685=CARTESIAN_POINT('',(-0.013344699427599,0.0110980990363674,0.0640020568079385));
#106686=CARTESIAN_POINT('',(-0.0135537656488909,0.0108499800615536,0.05925));
#106687=CARTESIAN_POINT('Origin',(-0.0031262178069016,0.00227581852804816,
0.05925000000001));
#106688=CARTESIAN_POINT('',(-0.0135537656488909,0.0108499800615536,0.06235));
#106689=CARTESIAN_POINT('',(-0.0135537656489009,0.0108499800615636,0.0639853702628634));
#106690=CARTESIAN_POINT('Origin',(-0.0031262178069016,0.00227581852804816,
0.06235000000001));
#106691=CARTESIAN_POINT('Origin',(-0.00312621780689159,0.00227581852803817,
0.06235));
#106692=CARTESIAN_POINT('',(-0.0143514035164094,0.00977549890701684,0.06235));
#106693=CARTESIAN_POINT('',(-0.0143514035164094,0.00977549890701684,0.05925));
#106694=CARTESIAN_POINT('',(-0.0143514035164194,0.00977549890702684,0.0639853702628634));
#106695=CARTESIAN_POINT('',(-0.0145283942056139,0.0095035687570112,0.05925));
#106696=CARTESIAN_POINT('Origin',(-0.0031262178069016,0.00227581852804816,
0.05925000000001));
#106697=CARTESIAN_POINT('',(-0.0145283942056139,0.00950356875701119,0.06235));
#106698=CARTESIAN_POINT('',(-0.0145283942056239,0.00950356875702119,0.0640116263041442));
#106699=CARTESIAN_POINT('Origin',(-0.0031262178069016,0.00227581852804816,
0.06235000000001));
#106700=CARTESIAN_POINT('Origin',(-0.00312621780689159,0.00227581852803817,
0.06235));
#106701=CARTESIAN_POINT('',(-0.0151879452321978,0.00833921126788417,0.06235));
#106702=CARTESIAN_POINT('',(-0.0151879452321978,0.00833921126788417,0.05925));
#106703=CARTESIAN_POINT('',(-0.0151879452322077,0.00833921126789417,0.0640116263041442));
#106704=CARTESIAN_POINT('',(-0.0153301773908709,0.0080475921265605,0.05925));
#106705=CARTESIAN_POINT('Origin',(-0.0031262178069016,0.00227581852804816,
0.05925000000001));
#106706=CARTESIAN_POINT('',(-0.0153301773908709,0.0080475921265605,0.06235));
#106707=CARTESIAN_POINT('',(-0.0153301773908809,0.0080475921265705,0.0640485717989525));
#106708=CARTESIAN_POINT('Origin',(-0.0031262178069016,0.00227581852804816,
0.06235000000001));
#106709=CARTESIAN_POINT('Origin',(-0.00312621780689159,0.00227581852803817,
0.06235));
#106710=CARTESIAN_POINT('',(-0.0159469609888662,0.00650412129177826,0.06235));
#106711=CARTESIAN_POINT('',(-0.0159469609888662,0.00650412129177825,0.05925));
#106712=CARTESIAN_POINT('',(-0.0159469609888762,0.00650412129178826,0.0640622576161447));
#106713=CARTESIAN_POINT('',(-0.0158416434552664,0.00681100877549768,0.06235));
#106714=CARTESIAN_POINT('Origin',(-0.0031262178069016,0.00227581852804816,
0.06235000000001));
#106715=CARTESIAN_POINT('',(-0.0158416434552664,0.00681100877549768,0.05925));
#106716=CARTESIAN_POINT('',(-0.0158416434552764,0.00681100877550768,0.0640485717989525));
#106717=CARTESIAN_POINT('Origin',(-0.0031262178069016,0.00227581852804816,
0.05925000000001));
#106718=CARTESIAN_POINT('Origin',(-0.00312621780689159,0.00227581852803817,
0.06235));
#106719=CARTESIAN_POINT('',(-0.00668322399864577,0.0152987869666017,0.06235));
#106720=CARTESIAN_POINT('',(-0.00668322399864577,0.0152987869666017,0.05925));
#106721=CARTESIAN_POINT('',(-0.00668322399865577,0.0152987869666117,0.0640597876943085));
#106722=CARTESIAN_POINT('',(-0.00636922814362363,0.0153805079160339,0.06235));
#106723=CARTESIAN_POINT('Origin',(-0.0031262178069016,0.00227581852804816,
0.06235000000001));
#106724=CARTESIAN_POINT('',(-0.00636922814362363,0.0153805079160339,0.05925));
#106725=CARTESIAN_POINT('',(-0.00636922814363363,0.015380507916044,0.0640589676062857));
#106726=CARTESIAN_POINT('Origin',(-0.0031262178069016,0.00227581852804816,
0.05925000000001));
#106727=CARTESIAN_POINT('Origin',(-0.00312621780689159,0.00227581852803817,
0.06235));
#106728=CARTESIAN_POINT('',(-0.00307486575549354,0.0157757208597892,0.06235));
#106729=CARTESIAN_POINT('',(-0.00307486575549354,0.0157757208597892,0.05925));
#106730=CARTESIAN_POINT('',(-0.00307486575550355,0.0157757208597992,0.0640296944304424));
#106731=CARTESIAN_POINT('',(-0.0033993108344085,0.015773056030517,0.05925));
#106732=CARTESIAN_POINT('Origin',(-0.0031262178069016,0.00227581852804816,
0.05925000000001));
#106733=CARTESIAN_POINT('',(-0.0033993108344085,0.015773056030517,0.06235));
#106734=CARTESIAN_POINT('',(-0.00339931083441851,0.015773056030527,0.0640346847097368));
#106735=CARTESIAN_POINT('Origin',(-0.0031262178069016,0.00227581852804816,
0.06235000000001));
#106736=CARTESIAN_POINT('Origin',(-0.00312621780689159,0.00227581852803817,
0.06235));
#106737=CARTESIAN_POINT('',(-0.0050558933738229,0.0156371939140674,0.06235));
#106738=CARTESIAN_POINT('',(-0.0050558933738229,0.0156371939140674,0.05925));
#106739=CARTESIAN_POINT('',(-0.0050558933738329,0.0156371939140774,0.0640589676062857));
#106740=CARTESIAN_POINT('',(-0.00473423489955992,0.0156797090464543,0.06235));
#106741=CARTESIAN_POINT('Origin',(-0.0031262178069016,0.00227581852804816,
0.06235000000001));
#106742=CARTESIAN_POINT('',(-0.00473423489955992,0.0156797090464543,0.05925));
#106743=CARTESIAN_POINT('',(-0.00473423489956992,0.0156797090464643,0.0640346847097368));
#106744=CARTESIAN_POINT('Origin',(-0.0031262178069016,0.00227581852804816,
0.05925000000001));
#106745=CARTESIAN_POINT('Origin',(-0.00312621780689159,0.00227581852803817,
0.06235));
#106746=CARTESIAN_POINT('',(-0.000930343506396564,0.0145814325337034,0.06235));
#106747=CARTESIAN_POINT('',(-9.89011778240814E-5,0.0154320092391663,0.06235000000001));
#106748=CARTESIAN_POINT('',(-0.000930343506406564,0.0145814325337134,0.06235000000001));
#106749=CARTESIAN_POINT('',(-0.00245920298515479,0.014758009490669,0.06235));
#106750=CARTESIAN_POINT('',(-0.00173858848308247,0.0157043137847654,0.06235000000001));
#106751=CARTESIAN_POINT('',(-0.00245920298516479,0.014758009490679,0.06235000000001));
#106752=CARTESIAN_POINT('',(-0.00399817372869307,0.014745369156286,0.06235));
#106753=CARTESIAN_POINT('',(-0.00339931083441851,0.015773056030527,0.06235000000001));
#106754=CARTESIAN_POINT('',(-0.00399817372870308,0.014745369156296,0.06235000000001));
#106755=CARTESIAN_POINT('',(-0.0055239265092796,0.0145437031451387,0.06235));
#106756=CARTESIAN_POINT('',(-0.0050558933738329,0.0156371939140774,0.06235000000001));
#106757=CARTESIAN_POINT('',(-0.0055239265092896,0.0145437031451487,0.06235000000001));
#106758=CARTESIAN_POINT('',(-0.00701333247002777,0.0141560685083892,0.06235));
#106759=CARTESIAN_POINT('',(-0.00668322399865577,0.0152987869666117,0.06235000000001));
#106760=CARTESIAN_POINT('',(-0.00701333247003777,0.0141560685083992,0.06235000000001));
#106761=CARTESIAN_POINT('',(-0.0084438137347893,0.0135883413919976,0.06235));
#106762=CARTESIAN_POINT('',(-0.0082566340354241,0.0147629650925005,0.06235000000001));
#106763=CARTESIAN_POINT('',(-0.0084438137347993,0.0135883413920076,0.06235000000001));
#106764=CARTESIAN_POINT('',(-0.00979368566574272,0.0128491279603392,0.06235));
#106765=CARTESIAN_POINT('',(-0.00975227219182637,0.0140378508051684,0.06235000000001));
#106766=CARTESIAN_POINT('',(-0.00979368566575272,0.0128491279603492,0.06235000000001));
#106767=CARTESIAN_POINT('',(-0.0110424855803985,0.0119496339355254,0.06235));
#106768=CARTESIAN_POINT('',(-0.0111474661179811,0.0131344360980708,0.06235000000001));
#106769=CARTESIAN_POINT('',(-0.0110424855804085,0.0119496339355354,0.06235000000001));
#106770=CARTESIAN_POINT('',(-0.0121712829450069,0.0109034947300784,0.06235));
#106771=CARTESIAN_POINT('',(-0.0124210660961502,0.0120664158172769,0.06235000000001));
#106772=CARTESIAN_POINT('',(-0.0121712829450169,0.0109034947300884,0.06235000000001));
#106773=CARTESIAN_POINT('',(-0.0131629663421532,0.00972656874797738,0.06235));
#106774=CARTESIAN_POINT('',(-0.0135537656489009,0.0108499800615636,0.06235000000001));
#106775=CARTESIAN_POINT('',(-0.0131629663421632,0.00972656874798738,0.06235000000001));
#106776=CARTESIAN_POINT('',(-0.014002502862403,0.00843669698741865,0.06235));
#106777=CARTESIAN_POINT('',(-0.0145283942056239,0.00950356875702119,0.06235000000001));
#106778=CARTESIAN_POINT('',(-0.014002502862413,0.00843669698742865,0.06235000000001));
#106779=CARTESIAN_POINT('',(-0.0146771659878858,0.00705343258946943,0.06235));
#106780=CARTESIAN_POINT('',(-0.0153301773908809,0.0080475921265705,0.06235000000001));
#106781=CARTESIAN_POINT('',(-0.0146771659878958,0.00705343258947943,0.06235000000001));
#106782=CARTESIAN_POINT('',(-0.015176728513333,0.00559774443238052,0.06235));
#106783=CARTESIAN_POINT('',(-0.0159469609888762,0.00650412129178826,0.06235000000001));
#106784=CARTESIAN_POINT('',(-0.015176728513343,0.00559774443239052,0.06235000000001));
#106785=CARTESIAN_POINT('',(-0.0154936175800848,0.00409169926476658,0.06235));
#106786=CARTESIAN_POINT('',(-0.0163693951889787,0.00489655369720221,0.06235000000001));
#106787=CARTESIAN_POINT('',(-0.0154936175800948,0.00409169926477658,0.06235000000001));
#106788=CARTESIAN_POINT('',(-0.0156230294729081,0.00255812719619073,0.06235));
#106789=CARTESIAN_POINT('',(-0.0165910763193207,0.00324925842888212,0.06235000000001));
#106790=CARTESIAN_POINT('',(-0.0156230294729181,0.00255812719620073,0.06235000000001));
#106791=CARTESIAN_POINT('',(-0.015563002439423,0.00102027561597532,0.06235));
#106792=CARTESIAN_POINT('',(-0.0166086439199353,0.00158720680393539,0.06235000000001));
#106793=CARTESIAN_POINT('',(-0.015563002439433,0.00102027561598532,0.06235000000001));
#106794=CARTESIAN_POINT('',(-0.0153144464282689,-0.0004985432135232,0.06235));
#106795=CARTESIAN_POINT('',(-0.0164218316839049,-6.44061692259324E-5,0.06235000000001));
#106796=CARTESIAN_POINT('',(-0.0153144464282789,-0.0004985432135332,0.06235000000001));
#106797=CARTESIAN_POINT('',(-0.0148811292952109,-0.00197530554704829,0.06235));
#106798=CARTESIAN_POINT('',(-0.0160334714943015,-0.00168054372145059,0.06235000000001));
#106799=CARTESIAN_POINT('',(-0.0148811292952209,-0.00197530554705829,0.06235000000001));
#106800=CARTESIAN_POINT('',(-0.0142696196862869,-0.00338762517295234,0.06235));
#106801=CARTESIAN_POINT('',(-0.0154494504957272,-0.00323670685486675,0.06235000000001));
#106802=CARTESIAN_POINT('',(-0.0142696196862969,-0.00338762517296234,0.06235000000001));
#106803=CARTESIAN_POINT('',(-0.0134891874638297,-0.004714092765346,0.06235));
#106804=CARTESIAN_POINT('',(-0.0146786218512019,-0.00470930572263721,0.06235000000001));
#106805=CARTESIAN_POINT('',(-0.0134891874638397,-0.004714092765356,0.06235000000001));
#106806=CARTESIAN_POINT('',(-0.012551663184803,-0.0059346004276552,0.06235));
#106807=CARTESIAN_POINT('',(-0.0137326705372373,-0.00607601722701116,0.06235000000001));
#106808=CARTESIAN_POINT('',(-0.012551663184813,-0.0059346004276652,0.06235000000001));
#106809=CARTESIAN_POINT('',(-0.0114712587616171,-0.00703064650783633,0.06235));
#106810=CARTESIAN_POINT('',(-0.0126259362115035,-0.00731612341473131,0.06235000000001));
#106811=CARTESIAN_POINT('',(-0.0114712587616271,-0.00703064650784633,0.06235000000001));
#106812=CARTESIAN_POINT('',(-0.0102643520240239,-0.0079856160645617,0.06235));
#106813=CARTESIAN_POINT('',(-0.0113751958382356,-0.00841082554008646,0.06235000000001));
#106814=CARTESIAN_POINT('',(-0.0102643520240339,-0.0079856160645717,0.06235000000001));
#106815=CARTESIAN_POINT('',(-0.00894923844791235,-0.00878503273279372,0.06235));
#106816=CARTESIAN_POINT('',(-0.00999940936655784,-0.00934352903473414,0.06235000000001));
#106817=CARTESIAN_POINT('',(-0.00894923844792235,-0.00878503273280372,0.06235000000001));
#106818=CARTESIAN_POINT('',(-0.00754585381454333,-0.00941677817072247,0.06235));
#106819=CARTESIAN_POINT('',(-0.00851943231698142,-0.0101000950644411,0.06235000000001));
#106820=CARTESIAN_POINT('',(-0.00754585381455333,-0.00941677817073247,0.06235000000001));
#106821=CARTESIAN_POINT('',(-0.00607547200442719,-0.00987127576147481,0.06235));
#106822=CARTESIAN_POINT('',(-0.00695769963297234,-0.0106690548593978,0.06235000000001));
#106823=CARTESIAN_POINT('',(-0.00607547200443719,-0.00987127576148481,0.06235000000001));
#106824=CARTESIAN_POINT('',(-0.0045603825069806,-0.0101416357848642,0.06235));
#106825=CARTESIAN_POINT('',(-0.00533788559007755,-0.0110417835690786,0.06235000000001));
#106826=CARTESIAN_POINT('',(-0.0045603825069906,-0.0101416357848742,0.06235000000001));
#106827=CARTESIAN_POINT('',(-0.00302355253458767,-0.010223759858526,0.06235));
#106828=CARTESIAN_POINT('',(-0.00368454491803983,-0.0112126310061832,0.06235000000001));
#106829=CARTESIAN_POINT('',(-0.00302355253459767,-0.010223759858536,0.06235000000001));
#106830=CARTESIAN_POINT('',(-0.00148827886307164,-0.0101164030652161,0.06235));
#106831=CARTESIAN_POINT('',(-0.00202274057612456,-0.0111790072977176,0.06235000000001));
#106832=CARTESIAN_POINT('',(-0.00148827886308164,-0.0101164030652261,0.06235000000001));
#106833=CARTESIAN_POINT('',(2.21653236791089E-5,-0.00982119282448763,0.06235));
#106834=CARTESIAN_POINT('',(-0.000377663824205095,-0.010941422144828,0.06235000000001));
#106835=CARTESIAN_POINT('',(2.21653236891089E-5,-0.00982119282449763,0.06235000000001));
#106836=CARTESIAN_POINT('',(0.00148488323145545,-0.00934260422266922,0.06235));
#106837=CARTESIAN_POINT('',(0.00122574765107832,-0.0105034770962511,0.06235000000001));
#106838=CARTESIAN_POINT('',(0.00148488323146545,-0.00934260422267922,0.06235000000001));
#106839=CARTESIAN_POINT('',(0.00287770154778802,-0.00868789217511811,0.06235));
#106840=CARTESIAN_POINT('',(0.0027631877661484,-0.00987181095250685,0.06235000000001));
#106841=CARTESIAN_POINT('',(0.00287770154779802,-0.00868789217512811,0.06235000000001));
#106842=CARTESIAN_POINT('',(0.00417950656676206,-0.00786698144909848,0.06235));
#106843=CARTESIAN_POINT('',(0.00421135049606079,-0.00905599912844934,0.06235000000001));
#106844=CARTESIAN_POINT('',(0.00417950656677206,-0.00786698144910848,0.06235000000001));
#106845=CARTESIAN_POINT('',(0.00537056425127688,-0.00689231621442642,0.06235));
#106846=CARTESIAN_POINT('',(0.00554828317000589,-0.00806840849973849,0.06235000000001));
#106847=CARTESIAN_POINT('',(0.00537056425128688,-0.00689231621443642,0.06235000000001));
#106848=CARTESIAN_POINT('',(0.00643281938093257,-0.00577867140254061,0.06235));
#106849=CARTESIAN_POINT('',(0.00675371925144076,-0.00692400993361114,0.06235000000001));
#106850=CARTESIAN_POINT('',(0.00643281938094257,-0.00577867140255061,0.06235000000001));
#106851=CARTESIAN_POINT('',(0.00735016925076682,-0.00454292873360213,0.06235));
#106852=CARTESIAN_POINT('',(0.00780938555812477,-0.00564015134579409,0.06235000000001));
#106853=CARTESIAN_POINT('',(0.00735016925077682,-0.00454292873361213,0.06235000000001));
#106854=CARTESIAN_POINT('',(0.00810870777184792,-0.00320382080682545,0.06235));
#106855=CARTESIAN_POINT('',(0.00869927926493554,-0.00423629472378529,0.06235000000001));
#106856=CARTESIAN_POINT('',(0.00810870777185792,-0.00320382080683544,0.06235000000001));
#106857=CARTESIAN_POINT('',(0.00869693627340787,-0.00178164713336899,0.06235));
#106858=CARTESIAN_POINT('',(0.00940991049038555,-0.00273372110296171,0.06235000000001));
#106859=CARTESIAN_POINT('',(0.00869693627341787,-0.00178164713337899,0.06235000000001));
#106860=CARTESIAN_POINT('',(0.00910593781097012,-0.000297966416438346,0.06235));
#106861=CARTESIAN_POINT('',(0.00993050678947452,-0.00115520796777584,0.06235000000001));
#106862=CARTESIAN_POINT('',(0.00910593781098012,-0.000297966416448346,0.06235000000001));
#106863=CARTESIAN_POINT('',(0.00932951233813846,0.00122473025667865,0.06235));
#106864=CARTESIAN_POINT('',(0.0102531764529749,0.000475316031710583,0.06235000000001));
#106865=CARTESIAN_POINT('',(0.00932951233814846,0.00122473025668865,0.06235000000001));
#106866=CARTESIAN_POINT('',(0.00936427069298033,0.00276336035656906,0.06235));
#106867=CARTESIAN_POINT('',(0.0103730281376995,0.00213313381369029,0.06235000000001));
#106868=CARTESIAN_POINT('',(0.00936427069299033,0.00276336035657905,0.06235000000001));
#106869=CARTESIAN_POINT('',(0.00920968597426703,0.0042945998193117,0.06235));
#106870=CARTESIAN_POINT('',(0.0102882450142778,0.00379311455049486,0.06235000000001));
#106871=CARTESIAN_POINT('',(0.00920968597427703,0.0042945998193217,0.06235000000001));
#106872=CARTESIAN_POINT('',(0.0088681015287593,0.005795236615511,0.06235));
#106873=CARTESIAN_POINT('',(0.0100001123084378,0.00543009462624556,0.06235000000001));
#106874=CARTESIAN_POINT('',(0.0088681015287693,0.005795236615521,0.06235000000001));
#106875=CARTESIAN_POINT('',(0.00834469542845901,0.00724252262100145,0.06235));
#106876=CARTESIAN_POINT('',(0.00951299781829371,0.00701925909163959,0.06235000000001));
#106877=CARTESIAN_POINT('',(0.00834469542846901,0.00724252262101145,0.06235000000001));
#106878=CARTESIAN_POINT('',(0.0076474019763159,0.00861451845522197,0.06235));
#106879=CARTESIAN_POINT('',(0.00883428570297895,0.00853651783328664,0.06235000000001));
#106880=CARTESIAN_POINT('',(0.0076474019763259,0.00861451845523197,0.06235000000001));
#106881=CARTESIAN_POINT('',(0.00678679143028267,0.00989042605986129,0.06235));
#106882=CARTESIAN_POINT('',(0.00797426454632066,0.00995887075527175,0.06235000000001));
#106883=CARTESIAN_POINT('',(0.00678679143029267,0.00989042605987129,0.06235000000001));
#106884=CARTESIAN_POINT('',(0.0057759097689791,0.0110509039762217,0.06235));
#106885=CARTESIAN_POINT('',(0.00694597139239648,0.0112647564371643,0.06235000000001));
#106886=CARTESIAN_POINT('',(0.0057759097689891,0.0110509039762317,0.06235000000001));
#106887=CARTESIAN_POINT('',(0.00463008092795451,0.0120783605420172,0.06235));
#106888=CARTESIAN_POINT('',(0.00576499411723559,0.0124343789831735,0.06235000000001));
#106889=CARTESIAN_POINT('',(0.00463008092796451,0.0120783605420272,0.06235000000001));
#106890=CARTESIAN_POINT('',(0.00336667450444523,0.0129572205630419,0.06235));
#106891=CARTESIAN_POINT('',(0.00444923513250745,0.0134500081077493,0.06235000000001));
#106892=CARTESIAN_POINT('',(0.00336667450445523,0.0129572205630519,0.06235000000001));
#106893=CARTESIAN_POINT('',(0.00200484245198608,0.0136741614172377,0.06235));
#106894=CARTESIAN_POINT('',(0.00301864000320971,0.0142962479086385,0.06235000000001));
#106895=CARTESIAN_POINT('',(0.00200484245199608,0.0136741614172477,0.06235000000001));
#106896=CARTESIAN_POINT('',(0.000565228756317156,0.0142183150120642,0.06235));
#106897=CARTESIAN_POINT('',(0.00149489509323412,0.014960270253069,0.06235000000001));
#106898=CARTESIAN_POINT('',(0.000565228756327156,0.0142183150120742,0.06235000000001));
#106899=CARTESIAN_POINT('Origin',(-0.00312621780689159,0.00227581852803817,
0.05925));
#106900=CARTESIAN_POINT('',(-0.000930343506396564,0.0145814325337034,0.05925));
#106901=CARTESIAN_POINT('',(-0.000930343506406564,0.0145814325337134,0.05925000000001));
#106902=CARTESIAN_POINT('',(-9.89011778240814E-5,0.0154320092391663,0.05925000000001));
#106903=CARTESIAN_POINT('',(0.000565228756317156,0.0142183150120642,0.05925));
#106904=CARTESIAN_POINT('',(0.000565228756327156,0.0142183150120742,0.05925000000001));
#106905=CARTESIAN_POINT('',(0.00149489509323412,0.014960270253069,0.05925000000001));
#106906=CARTESIAN_POINT('',(0.00200484245198608,0.0136741614172377,0.05925));
#106907=CARTESIAN_POINT('',(0.00200484245199608,0.0136741614172477,0.05925000000001));
#106908=CARTESIAN_POINT('',(0.00301864000320971,0.0142962479086385,0.05925000000001));
#106909=CARTESIAN_POINT('',(0.00336667450444523,0.0129572205630419,0.05925));
#106910=CARTESIAN_POINT('',(0.00336667450445523,0.0129572205630519,0.05925000000001));
#106911=CARTESIAN_POINT('',(0.00444923513250745,0.0134500081077493,0.05925000000001));
#106912=CARTESIAN_POINT('',(0.00463008092795451,0.0120783605420172,0.05925));
#106913=CARTESIAN_POINT('',(0.00463008092796451,0.0120783605420272,0.05925000000001));
#106914=CARTESIAN_POINT('',(0.00576499411723559,0.0124343789831735,0.05925000000001));
#106915=CARTESIAN_POINT('',(0.0057759097689791,0.0110509039762217,0.05925));
#106916=CARTESIAN_POINT('',(0.0057759097689891,0.0110509039762317,0.05925000000001));
#106917=CARTESIAN_POINT('',(0.00694597139239648,0.0112647564371643,0.05925000000001));
#106918=CARTESIAN_POINT('',(0.00678679143028267,0.00989042605986129,0.05925));
#106919=CARTESIAN_POINT('',(0.00678679143029267,0.00989042605987129,0.05925000000001));
#106920=CARTESIAN_POINT('',(0.00797426454632066,0.00995887075527175,0.05925000000001));
#106921=CARTESIAN_POINT('',(0.0076474019763159,0.00861451845522197,0.05925));
#106922=CARTESIAN_POINT('',(0.0076474019763259,0.00861451845523197,0.05925000000001));
#106923=CARTESIAN_POINT('',(0.00883428570297895,0.00853651783328664,0.05925000000001));
#106924=CARTESIAN_POINT('',(0.00834469542845901,0.00724252262100145,0.05925));
#106925=CARTESIAN_POINT('',(0.00834469542846901,0.00724252262101145,0.05925000000001));
#106926=CARTESIAN_POINT('',(0.00951299781829371,0.00701925909163959,0.05925000000001));
#106927=CARTESIAN_POINT('',(0.0088681015287593,0.005795236615511,0.05925));
#106928=CARTESIAN_POINT('',(0.0088681015287693,0.005795236615521,0.05925000000001));
#106929=CARTESIAN_POINT('',(0.0100001123084378,0.00543009462624556,0.05925000000001));
#106930=CARTESIAN_POINT('',(0.00920968597426703,0.0042945998193117,0.05925));
#106931=CARTESIAN_POINT('',(0.00920968597427703,0.0042945998193217,0.05925000000001));
#106932=CARTESIAN_POINT('',(0.0102882450142778,0.00379311455049486,0.05925000000001));
#106933=CARTESIAN_POINT('',(0.00936427069298033,0.00276336035656906,0.05925));
#106934=CARTESIAN_POINT('',(0.00936427069299033,0.00276336035657905,0.05925000000001));
#106935=CARTESIAN_POINT('',(0.0103730281376995,0.00213313381369029,0.05925000000001));
#106936=CARTESIAN_POINT('',(0.00932951233813846,0.00122473025667865,0.05925));
#106937=CARTESIAN_POINT('',(0.00932951233814846,0.00122473025668865,0.05925000000001));
#106938=CARTESIAN_POINT('',(0.0102531764529749,0.000475316031710583,0.05925000000001));
#106939=CARTESIAN_POINT('',(0.00910593781097012,-0.000297966416438346,0.05925));
#106940=CARTESIAN_POINT('',(0.00910593781098012,-0.000297966416448346,0.05925000000001));
#106941=CARTESIAN_POINT('',(0.00993050678947452,-0.00115520796777584,0.05925000000001));
#106942=CARTESIAN_POINT('',(0.00869693627340787,-0.00178164713336899,0.05925));
#106943=CARTESIAN_POINT('',(0.00869693627341787,-0.00178164713337899,0.05925000000001));
#106944=CARTESIAN_POINT('',(0.00940991049038555,-0.00273372110296171,0.05925000000001));
#106945=CARTESIAN_POINT('',(0.00810870777184792,-0.00320382080682545,0.05925));
#106946=CARTESIAN_POINT('',(0.00810870777185792,-0.00320382080683544,0.05925000000001));
#106947=CARTESIAN_POINT('',(0.00869927926493554,-0.00423629472378529,0.05925000000001));
#106948=CARTESIAN_POINT('',(0.00735016925076682,-0.00454292873360213,0.05925));
#106949=CARTESIAN_POINT('',(0.00735016925077682,-0.00454292873361213,0.05925000000001));
#106950=CARTESIAN_POINT('',(0.00780938555812477,-0.00564015134579409,0.05925000000001));
#106951=CARTESIAN_POINT('',(0.00643281938093257,-0.00577867140254061,0.05925));
#106952=CARTESIAN_POINT('',(0.00643281938094257,-0.00577867140255061,0.05925000000001));
#106953=CARTESIAN_POINT('',(0.00675371925144076,-0.00692400993361114,0.05925000000001));
#106954=CARTESIAN_POINT('',(0.00537056425127688,-0.00689231621442642,0.05925));
#106955=CARTESIAN_POINT('',(0.00537056425128688,-0.00689231621443642,0.05925000000001));
#106956=CARTESIAN_POINT('',(0.00554828317000589,-0.00806840849973849,0.05925000000001));
#106957=CARTESIAN_POINT('',(0.00417950656676206,-0.00786698144909848,0.05925));
#106958=CARTESIAN_POINT('',(0.00417950656677206,-0.00786698144910848,0.05925000000001));
#106959=CARTESIAN_POINT('',(0.00421135049606079,-0.00905599912844934,0.05925000000001));
#106960=CARTESIAN_POINT('',(0.00287770154778802,-0.00868789217511811,0.05925));
#106961=CARTESIAN_POINT('',(0.00287770154779802,-0.00868789217512811,0.05925000000001));
#106962=CARTESIAN_POINT('',(0.0027631877661484,-0.00987181095250685,0.05925000000001));
#106963=CARTESIAN_POINT('',(0.00148488323145545,-0.00934260422266922,0.05925));
#106964=CARTESIAN_POINT('',(0.00148488323146545,-0.00934260422267922,0.05925000000001));
#106965=CARTESIAN_POINT('',(0.00122574765107832,-0.0105034770962511,0.05925000000001));
#106966=CARTESIAN_POINT('',(2.21653236791089E-5,-0.00982119282448763,0.05925));
#106967=CARTESIAN_POINT('',(2.21653236891089E-5,-0.00982119282449763,0.05925000000001));
#106968=CARTESIAN_POINT('',(-0.000377663824205095,-0.010941422144828,0.05925000000001));
#106969=CARTESIAN_POINT('',(-0.00148827886307164,-0.0101164030652161,0.05925));
#106970=CARTESIAN_POINT('',(-0.00148827886308164,-0.0101164030652261,0.05925000000001));
#106971=CARTESIAN_POINT('',(-0.00202274057612456,-0.0111790072977176,0.05925000000001));
#106972=CARTESIAN_POINT('',(-0.00302355253458767,-0.010223759858526,0.05925));
#106973=CARTESIAN_POINT('',(-0.00302355253459767,-0.010223759858536,0.05925000000001));
#106974=CARTESIAN_POINT('',(-0.00368454491803983,-0.0112126310061832,0.05925000000001));
#106975=CARTESIAN_POINT('',(-0.0045603825069806,-0.0101416357848642,0.05925));
#106976=CARTESIAN_POINT('',(-0.0045603825069906,-0.0101416357848742,0.05925000000001));
#106977=CARTESIAN_POINT('',(-0.00533788559007755,-0.0110417835690786,0.05925000000001));
#106978=CARTESIAN_POINT('',(-0.00607547200442719,-0.00987127576147481,0.05925));
#106979=CARTESIAN_POINT('',(-0.00607547200443719,-0.00987127576148481,0.05925000000001));
#106980=CARTESIAN_POINT('',(-0.00695769963297234,-0.0106690548593978,0.05925000000001));
#106981=CARTESIAN_POINT('',(-0.00754585381454333,-0.00941677817072247,0.05925));
#106982=CARTESIAN_POINT('',(-0.00754585381455333,-0.00941677817073247,0.05925000000001));
#106983=CARTESIAN_POINT('',(-0.00851943231698142,-0.0101000950644411,0.05925000000001));
#106984=CARTESIAN_POINT('',(-0.00894923844791235,-0.00878503273279372,0.05925));
#106985=CARTESIAN_POINT('',(-0.00894923844792235,-0.00878503273280372,0.05925000000001));
#106986=CARTESIAN_POINT('',(-0.00999940936655784,-0.00934352903473414,0.05925000000001));
#106987=CARTESIAN_POINT('',(-0.0102643520240239,-0.0079856160645617,0.05925));
#106988=CARTESIAN_POINT('',(-0.0102643520240339,-0.0079856160645717,0.05925000000001));
#106989=CARTESIAN_POINT('',(-0.0113751958382356,-0.00841082554008646,0.05925000000001));
#106990=CARTESIAN_POINT('',(-0.0114712587616171,-0.00703064650783633,0.05925));
#106991=CARTESIAN_POINT('',(-0.0114712587616271,-0.00703064650784633,0.05925000000001));
#106992=CARTESIAN_POINT('',(-0.0126259362115035,-0.00731612341473131,0.05925000000001));
#106993=CARTESIAN_POINT('',(-0.012551663184803,-0.0059346004276552,0.05925));
#106994=CARTESIAN_POINT('',(-0.012551663184813,-0.0059346004276652,0.05925000000001));
#106995=CARTESIAN_POINT('',(-0.0137326705372373,-0.00607601722701116,0.05925000000001));
#106996=CARTESIAN_POINT('',(-0.0134891874638297,-0.004714092765346,0.05925));
#106997=CARTESIAN_POINT('',(-0.0134891874638397,-0.004714092765356,0.05925000000001));
#106998=CARTESIAN_POINT('',(-0.0146786218512019,-0.00470930572263721,0.05925000000001));
#106999=CARTESIAN_POINT('',(-0.0142696196862869,-0.00338762517295234,0.05925));
#107000=CARTESIAN_POINT('',(-0.0142696196862969,-0.00338762517296234,0.05925000000001));
#107001=CARTESIAN_POINT('',(-0.0154494504957272,-0.00323670685486675,0.05925000000001));
#107002=CARTESIAN_POINT('',(-0.0148811292952109,-0.00197530554704829,0.05925));
#107003=CARTESIAN_POINT('',(-0.0148811292952209,-0.00197530554705829,0.05925000000001));
#107004=CARTESIAN_POINT('',(-0.0160334714943015,-0.00168054372145059,0.05925000000001));
#107005=CARTESIAN_POINT('',(-0.0153144464282689,-0.0004985432135232,0.05925));
#107006=CARTESIAN_POINT('',(-0.0153144464282789,-0.0004985432135332,0.05925000000001));
#107007=CARTESIAN_POINT('',(-0.0164218316839049,-6.44061692259324E-5,0.05925000000001));
#107008=CARTESIAN_POINT('',(-0.015563002439423,0.00102027561597532,0.05925));
#107009=CARTESIAN_POINT('',(-0.015563002439433,0.00102027561598532,0.05925000000001));
#107010=CARTESIAN_POINT('',(-0.0166086439199353,0.00158720680393539,0.05925000000001));
#107011=CARTESIAN_POINT('',(-0.0156230294729081,0.00255812719619073,0.05925));
#107012=CARTESIAN_POINT('',(-0.0156230294729181,0.00255812719620073,0.05925000000001));
#107013=CARTESIAN_POINT('',(-0.0165910763193207,0.00324925842888212,0.05925000000001));
#107014=CARTESIAN_POINT('',(-0.0154936175800848,0.00409169926476658,0.05925));
#107015=CARTESIAN_POINT('',(-0.0154936175800948,0.00409169926477658,0.05925000000001));
#107016=CARTESIAN_POINT('',(-0.0163693951889787,0.00489655369720221,0.05925000000001));
#107017=CARTESIAN_POINT('',(-0.015176728513333,0.00559774443238052,0.05925));
#107018=CARTESIAN_POINT('',(-0.015176728513343,0.00559774443239052,0.05925000000001));
#107019=CARTESIAN_POINT('',(-0.0159469609888762,0.00650412129178826,0.05925000000001));
#107020=CARTESIAN_POINT('',(-0.0146771659878858,0.00705343258946943,0.05925));
#107021=CARTESIAN_POINT('',(-0.0146771659878958,0.00705343258947943,0.05925000000001));
#107022=CARTESIAN_POINT('',(-0.0153301773908809,0.0080475921265705,0.05925000000001));
#107023=CARTESIAN_POINT('',(-0.014002502862403,0.00843669698741865,0.05925));
#107024=CARTESIAN_POINT('',(-0.014002502862413,0.00843669698742865,0.05925000000001));
#107025=CARTESIAN_POINT('',(-0.0145283942056239,0.00950356875702119,0.05925000000001));
#107026=CARTESIAN_POINT('',(-0.0131629663421532,0.00972656874797738,0.05925));
#107027=CARTESIAN_POINT('',(-0.0131629663421632,0.00972656874798738,0.05925000000001));
#107028=CARTESIAN_POINT('',(-0.0135537656489009,0.0108499800615636,0.05925000000001));
#107029=CARTESIAN_POINT('',(-0.0121712829450069,0.0109034947300784,0.05925));
#107030=CARTESIAN_POINT('',(-0.0121712829450169,0.0109034947300884,0.05925000000001));
#107031=CARTESIAN_POINT('',(-0.0124210660961502,0.0120664158172769,0.05925000000001));
#107032=CARTESIAN_POINT('',(-0.0110424855803985,0.0119496339355254,0.05925));
#107033=CARTESIAN_POINT('',(-0.0110424855804085,0.0119496339355354,0.05925000000001));
#107034=CARTESIAN_POINT('',(-0.0111474661179811,0.0131344360980708,0.05925000000001));
#107035=CARTESIAN_POINT('',(-0.00979368566574272,0.0128491279603392,0.05925));
#107036=CARTESIAN_POINT('',(-0.00979368566575272,0.0128491279603492,0.05925000000001));
#107037=CARTESIAN_POINT('',(-0.00975227219182637,0.0140378508051684,0.05925000000001));
#107038=CARTESIAN_POINT('',(-0.0084438137347893,0.0135883413919976,0.05925));
#107039=CARTESIAN_POINT('',(-0.0084438137347993,0.0135883413920076,0.05925000000001));
#107040=CARTESIAN_POINT('',(-0.0082566340354241,0.0147629650925005,0.05925000000001));
#107041=CARTESIAN_POINT('',(-0.00701333247002777,0.0141560685083892,0.05925));
#107042=CARTESIAN_POINT('',(-0.00701333247003777,0.0141560685083992,0.05925000000001));
#107043=CARTESIAN_POINT('',(-0.00668322399865577,0.0152987869666117,0.05925000000001));
#107044=CARTESIAN_POINT('',(-0.0055239265092796,0.0145437031451387,0.05925));
#107045=CARTESIAN_POINT('',(-0.0055239265092896,0.0145437031451487,0.05925000000001));
#107046=CARTESIAN_POINT('',(-0.0050558933738329,0.0156371939140774,0.05925000000001));
#107047=CARTESIAN_POINT('',(-0.00399817372869307,0.014745369156286,0.05925));
#107048=CARTESIAN_POINT('',(-0.00399817372870308,0.014745369156296,0.05925000000001));
#107049=CARTESIAN_POINT('',(-0.00339931083441851,0.015773056030527,0.05925000000001));
#107050=CARTESIAN_POINT('',(-0.00245920298515479,0.014758009490669,0.05925));
#107051=CARTESIAN_POINT('',(-0.00245920298516479,0.014758009490679,0.05925000000001));
#107052=CARTESIAN_POINT('',(-0.00173858848308247,0.0157043137847654,0.05925000000001));
#107053=CARTESIAN_POINT('Origin',(-0.00312621780689159,0.00227581852803817,
0.05991));
#107054=CARTESIAN_POINT('Origin',(-0.00312621780689159,0.00227581852803817,
0.06169));
#107055=CARTESIAN_POINT('Origin',(-0.00312621780689159,0.00227581852803817,
0.06603));
#107056=CARTESIAN_POINT('Origin',(-0.00312621780689159,0.00227581852803817,
0.05925));
#107057=CARTESIAN_POINT('Origin',(-0.00399817372869307,0.014745369156286,
0.0640346847097268));
#107058=CARTESIAN_POINT('',(-0.00399817372870308,0.014745369156296,0.0640346847097368));
#107059=CARTESIAN_POINT('Origin',(-0.0033993108344085,0.015773056030517,
0.0640346847097268));
#107060=CARTESIAN_POINT('Origin',(-0.00245920298515479,0.014758009490669,
0.0640296944304324));
#107061=CARTESIAN_POINT('',(-0.00245920298516479,0.014758009490679,0.0640296944304424));
#107062=CARTESIAN_POINT('Origin',(-0.00173858848307247,0.0157043137847554,
0.0640296944304324));
#107063=CARTESIAN_POINT('Origin',(-0.0055239265092796,0.0145437031451387,
0.0640589676062757));
#107064=CARTESIAN_POINT('',(-0.0055239265092896,0.0145437031451487,0.0640589676062857));
#107065=CARTESIAN_POINT('Origin',(-0.0050558933738229,0.0156371939140674,
0.0640589676062757));
#107066=CARTESIAN_POINT('Origin',(-0.0146771659878858,0.00705343258946943,
0.0640485717989425));
#107067=CARTESIAN_POINT('',(-0.0146771659878958,0.00705343258947943,0.0640485717989525));
#107068=CARTESIAN_POINT('Origin',(-0.0153301773908709,0.0080475921265605,
0.0640485717989425));
#107069=CARTESIAN_POINT('Origin',(-0.014002502862403,0.00843669698741865,
0.0640116263041342));
#107070=CARTESIAN_POINT('',(-0.014002502862413,0.00843669698742865,0.0640116263041442));
#107071=CARTESIAN_POINT('Origin',(-0.0145283942056139,0.00950356875701119,
0.0640116263041342));
#107072=CARTESIAN_POINT('Origin',(-0.0131629663421532,0.00972656874797738,
0.0639853702628534));
#107073=CARTESIAN_POINT('',(-0.0131629663421632,0.00972656874798738,0.0639853702628634));
#107074=CARTESIAN_POINT('Origin',(-0.0135537656488909,0.0108499800615536,
0.0639853702628534));
#107075=CARTESIAN_POINT('Origin',(-0.0121712829450069,0.0109034947300784,
0.0640020568079285));
#107076=CARTESIAN_POINT('',(-0.0121712829450169,0.0109034947300884,0.0640020568079385));
#107077=CARTESIAN_POINT('Origin',(-0.0124210660961402,0.0120664158172669,
0.0640020568079285));
#107078=CARTESIAN_POINT('Origin',(-0.0110424855803985,0.0119496339355254,
0.0639946102147255));
#107079=CARTESIAN_POINT('',(-0.0110424855804085,0.0119496339355354,0.0639946102147355));
#107080=CARTESIAN_POINT('Origin',(-0.0111474661179711,0.0131344360980608,
0.0639946102147255));
#107081=CARTESIAN_POINT('Origin',(-0.00979368566574272,0.0128491279603392,
0.0639914355303126));
#107082=CARTESIAN_POINT('',(-0.00979368566575272,0.0128491279603492,0.0639914355303226));
#107083=CARTESIAN_POINT('Origin',(-0.00975227219181637,0.0140378508051584,
0.0639914355303126));
#107084=CARTESIAN_POINT('Origin',(-0.0084438137347893,0.0135883413919976,
0.0640371289970071));
#107085=CARTESIAN_POINT('',(-0.0084438137347993,0.0135883413920076,0.0640371289970171));
#107086=CARTESIAN_POINT('Origin',(-0.0082566340354141,0.0147629650924905,
0.0640371289970071));
#107087=CARTESIAN_POINT('Origin',(-0.00701333247002777,0.0141560685083892,
0.0640597876942985));
#107088=CARTESIAN_POINT('',(-0.00701333247003777,0.0141560685083992,0.0640597876943085));
#107089=CARTESIAN_POINT('Origin',(-0.00668322399864577,0.0152987869666017,
0.0640597876942985));
#107090=CARTESIAN_POINT('Origin',(-0.015176728513333,0.00559774443238052,
0.0640622576161347));
#107091=CARTESIAN_POINT('',(-0.015176728513343,0.00559774443239052,0.0640622576161447));
#107092=CARTESIAN_POINT('Origin',(-0.0159469609888662,0.00650412129177826,
0.0640622576161347));
#107093=CARTESIAN_POINT('Origin',(-0.0154936175800848,0.00409169926476658,
0.0640524165708833));
#107094=CARTESIAN_POINT('',(-0.0154936175800948,0.00409169926477658,0.0640524165708933));
#107095=CARTESIAN_POINT('Origin',(-0.0163693951889687,0.00489655369719221,
0.0640524165708833));
#107096=CARTESIAN_POINT('Origin',(-0.0156230294729081,0.00255812719619073,
0.0640221869975658));
#107097=CARTESIAN_POINT('',(-0.0156230294729181,0.00255812719620073,0.0640221869975759));
#107098=CARTESIAN_POINT('Origin',(-0.0165910763193107,0.00324925842887212,
0.0640221869975658));
#107099=CARTESIAN_POINT('Origin',(-0.015563002439423,0.00102027561597532,
0.0640429369448756));
#107100=CARTESIAN_POINT('',(-0.015563002439433,0.00102027561598532,0.0640429369448856));
#107101=CARTESIAN_POINT('Origin',(-0.0166086439199253,0.00158720680392539,
0.0640429369448756));
#107102=CARTESIAN_POINT('Origin',(-0.0153144464282689,-0.0004985432135232,
0.064061380725464));
#107103=CARTESIAN_POINT('',(-0.0153144464282789,-0.0004985432135332,0.064061380725474));
#107104=CARTESIAN_POINT('Origin',(-0.0164218316838949,-6.44061692159324E-5,
0.064061380725464));
#107105=CARTESIAN_POINT('Origin',(-0.0148811292952109,-0.00197530554704829,
0.0640563147052241));
#107106=CARTESIAN_POINT('',(-0.0148811292952209,-0.00197530554705829,0.0640563147052341));
#107107=CARTESIAN_POINT('Origin',(-0.0160334714942915,-0.00168054372144059,
0.0640563147052241));
#107108=CARTESIAN_POINT('Origin',(-0.0142696196862869,-0.00338762517295234,
0.0640278376069354));
#107109=CARTESIAN_POINT('',(-0.0142696196862969,-0.00338762517296234,0.0640278376069454));
#107110=CARTESIAN_POINT('Origin',(-0.0154494504957172,-0.00323670685485675,
0.0640278376069354));
#107111=CARTESIAN_POINT('Origin',(-0.0134891874638297,-0.004714092765346,
0.06397650941055));
#107112=CARTESIAN_POINT('',(-0.0134891874638397,-0.004714092765356,0.06397650941056));
#107113=CARTESIAN_POINT('Origin',(-0.0146786218511919,-0.00470930572262721,
0.06397650941055));
#107114=CARTESIAN_POINT('Origin',(-0.0114712587616171,-0.00703064650783633,
0.0640001436148948));
#107115=CARTESIAN_POINT('',(-0.0114712587616271,-0.00703064650784633,0.0640001436149048));
#107116=CARTESIAN_POINT('Origin',(-0.0126259362114935,-0.00731612341472131,
0.0640001436148948));
#107117=CARTESIAN_POINT('Origin',(-0.012551663184803,-0.0059346004276552,
0.0639987344374606));
#107118=CARTESIAN_POINT('',(-0.012551663184813,-0.0059346004276652,0.0639987344374706));
#107119=CARTESIAN_POINT('Origin',(-0.0137326705372273,-0.00607601722700116,
0.0639987344374606));
#107120=CARTESIAN_POINT('Origin',(-0.0102643520240239,-0.0079856160645617,
0.0639774518569439));
#107121=CARTESIAN_POINT('',(-0.0102643520240339,-0.0079856160645717,0.0639774518569539));
#107122=CARTESIAN_POINT('Origin',(-0.0113751958382256,-0.00841082554007646,
0.0639774518569439));
#107123=CARTESIAN_POINT('Origin',(-0.00894923844791235,-0.00878503273279372,
0.064023011312247));
#107124=CARTESIAN_POINT('',(-0.00894923844792235,-0.00878503273280372,0.064023011312257));
#107125=CARTESIAN_POINT('Origin',(-0.00999940936654784,-0.00934352903472414,
0.064023011312247));
#107126=CARTESIAN_POINT('Origin',(-0.00754585381454333,-0.00941677817072247,
0.0640541921468364));
#107127=CARTESIAN_POINT('',(-0.00754585381455333,-0.00941677817073247,0.0640541921468464));
#107128=CARTESIAN_POINT('Origin',(-0.00851943231697142,-0.0101000950644311,
0.0640541921468364));
#107129=CARTESIAN_POINT('Origin',(-0.00607547200442719,-0.00987127576147481,
0.0640620033446039));
#107130=CARTESIAN_POINT('',(-0.00607547200443719,-0.00987127576148481,0.0640620033446139));
#107131=CARTESIAN_POINT('Origin',(-0.00695769963296234,-0.0106690548593878,
0.0640620033446039));
#107132=CARTESIAN_POINT('Origin',(-0.0045603825069806,-0.0101416357848642,
0.0640462926264731));
#107133=CARTESIAN_POINT('',(-0.0045603825069906,-0.0101416357848742,0.0640462926264831));
#107134=CARTESIAN_POINT('Origin',(-0.00533788559006755,-0.0110417835690686,
0.0640462926264731));
#107135=CARTESIAN_POINT('Origin',(-0.00302355253458767,-0.010223759858526,
0.0640207658501684));
#107136=CARTESIAN_POINT('',(-0.00302355253459767,-0.010223759858536,0.0640207658501784));
#107137=CARTESIAN_POINT('Origin',(-0.00368454491802983,-0.0112126310061732,
0.0640207658501684));
#107138=CARTESIAN_POINT('Origin',(-0.00148827886307164,-0.0101164030652161,
0.0640497400911627));
#107139=CARTESIAN_POINT('',(-0.00148827886308164,-0.0101164030652261,0.0640497400911727));
#107140=CARTESIAN_POINT('Origin',(-0.00202274057611456,-0.0111790072977077,
0.0640497400911627));
#107141=CARTESIAN_POINT('Origin',(2.21653236791089E-5,-0.00982119282448763,
0.0640623222440536));
#107142=CARTESIAN_POINT('',(2.21653236891089E-5,-0.00982119282449763,0.0640623222440636));
#107143=CARTESIAN_POINT('Origin',(-0.000377663824195094,-0.010941422144818,
0.0640623222440536));
#107144=CARTESIAN_POINT('Origin',(0.00148488323145545,-0.00934260422266922,
0.0640513762773474));
#107145=CARTESIAN_POINT('',(0.00148488323146545,-0.00934260422267922,0.0640513762773574));
#107146=CARTESIAN_POINT('Origin',(0.00122574765106832,-0.0105034770962411,
0.0640513762773474));
#107147=CARTESIAN_POINT('Origin',(0.00287770154778802,-0.00868789217511811,
0.0640171157235525));
#107148=CARTESIAN_POINT('',(0.00287770154779802,-0.00868789217512811,0.0640171157235625));
#107149=CARTESIAN_POINT('Origin',(0.00276318776613839,-0.00987181095249685,
0.0640171157235525));
#107150=CARTESIAN_POINT('Origin',(0.00735016925076682,-0.00454292873360213,
0.0639846412562978));
#107151=CARTESIAN_POINT('',(0.00735016925077682,-0.00454292873361213,0.0639846412563078));
#107152=CARTESIAN_POINT('Origin',(0.00780938555811477,-0.00564015134578409,
0.0639846412562978));
#107153=CARTESIAN_POINT('Origin',(0.00643281938093257,-0.00577867140254061,
0.0639967221271682));
#107154=CARTESIAN_POINT('',(0.00643281938094257,-0.00577867140255061,0.0639967221271783));
#107155=CARTESIAN_POINT('Origin',(0.00675371925143076,-0.00692400993360114,
0.0639967221271682));
#107156=CARTESIAN_POINT('Origin',(0.00537056425127688,-0.00689231621442642,
0.064001351848474));
#107157=CARTESIAN_POINT('',(0.00537056425128688,-0.00689231621443642,0.064001351848484));
#107158=CARTESIAN_POINT('Origin',(0.00554828316999589,-0.00806840849972849,
0.064001351848474));
#107159=CARTESIAN_POINT('Origin',(0.00417950656676206,-0.00786698144909848,
0.0639818602956437));
#107160=CARTESIAN_POINT('',(0.00417950656677206,-0.00786698144910848,0.0639818602956537));
#107161=CARTESIAN_POINT('Origin',(0.0042113504960508,-0.00905599912843934,
0.0639818602956437));
#107162=CARTESIAN_POINT('Origin',(0.00810870777184792,-0.00320382080682545,
0.064032971803573));
#107163=CARTESIAN_POINT('',(0.00810870777185792,-0.00320382080683544,0.064032971803583));
#107164=CARTESIAN_POINT('Origin',(0.00869927926492554,-0.00423629472377529,
0.064032971803573));
#107165=CARTESIAN_POINT('Origin',(0.00869693627340787,-0.00178164713336899,
0.0640583496424));
#107166=CARTESIAN_POINT('',(0.00869693627341787,-0.00178164713337899,0.06405834964241));
#107167=CARTESIAN_POINT('Origin',(0.00940991049037555,-0.00273372110295171,
0.0640583496424));
#107168=CARTESIAN_POINT('Origin',(0.00910593781097012,-0.000297966416438346,
0.0640602767162906));
#107169=CARTESIAN_POINT('',(0.00910593781098012,-0.000297966416448346,0.0640602767163006));
#107170=CARTESIAN_POINT('Origin',(0.00993050678946452,-0.00115520796776584,
0.0640602767162906));
#107171=CARTESIAN_POINT('Origin',(0.00932951233813846,0.00122473025667865,
0.0640387154811068));
#107172=CARTESIAN_POINT('',(0.00932951233814846,0.00122473025668865,0.0640387154811168));
#107173=CARTESIAN_POINT('Origin',(0.0102531764529649,0.000475316031700583,
0.0640387154811068));
#107174=CARTESIAN_POINT('Origin',(0.00936427069298033,0.00276336035656906,
0.0640254477644175));
#107175=CARTESIAN_POINT('',(0.00936427069299033,0.00276336035657905,0.0640254477644275));
#107176=CARTESIAN_POINT('Origin',(0.0103730281376895,0.00213313381368028,
0.0640254477644175));
#107177=CARTESIAN_POINT('Origin',(0.00920968597426703,0.0042945998193117,
0.0640550858195568));
#107178=CARTESIAN_POINT('',(0.00920968597427703,0.0042945998193217,0.0640550858195668));
#107179=CARTESIAN_POINT('Origin',(0.0102882450142678,0.00379311455048486,
0.0640550858195568));
#107180=CARTESIAN_POINT('Origin',(0.0088681015287593,0.005795236615511,
0.0640617910186438));
#107181=CARTESIAN_POINT('',(0.0088681015287693,0.005795236615521,0.0640617910186538));
#107182=CARTESIAN_POINT('Origin',(0.0100001123084278,0.00543009462623556,
0.0640617910186438));
#107183=CARTESIAN_POINT('Origin',(0.00834469542845901,0.00724252262100145,
0.064044978432879));
#107184=CARTESIAN_POINT('',(0.00834469542846901,0.00724252262101145,0.064044978432889));
#107185=CARTESIAN_POINT('Origin',(0.00951299781828371,0.00701925909162959,
0.064044978432879));
#107186=CARTESIAN_POINT('Origin',(0.0076474019763159,0.00861451845522197,
0.0640049766461023));
#107187=CARTESIAN_POINT('',(0.0076474019763259,0.00861451845523197,0.0640049766461123));
#107188=CARTESIAN_POINT('Origin',(0.00883428570296894,0.00853651783327664,
0.0640049766461023));
#107189=CARTESIAN_POINT('Origin',(0.00678679143028267,0.00989042605986129,
0.0639889835233511));
#107190=CARTESIAN_POINT('',(0.00678679143029267,0.00989042605987129,0.0639889835233611));
#107191=CARTESIAN_POINT('Origin',(0.00797426454631066,0.00995887075526175,
0.0639889835233511));
#107192=CARTESIAN_POINT('Origin',(0.0057759097689791,0.0110509039762217,
0.0640024596936878));
#107193=CARTESIAN_POINT('',(0.0057759097689891,0.0110509039762317,0.0640024596936978));
#107194=CARTESIAN_POINT('Origin',(0.00694597139238648,0.0112647564371543,
0.0640024596936878));
#107195=CARTESIAN_POINT('Origin',(0.00463008092795451,0.0120783605420172,
0.0639917959462776));
#107196=CARTESIAN_POINT('',(0.00463008092796451,0.0120783605420272,0.0639917959462876));
#107197=CARTESIAN_POINT('Origin',(0.00576499411722559,0.0124343789831635,
0.0639917959462776));
#107198=CARTESIAN_POINT('Origin',(0.00336667450444523,0.0129572205630419,
0.0639988309423512));
#107199=CARTESIAN_POINT('',(0.00336667450445523,0.0129572205630519,0.0639988309423612));
#107200=CARTESIAN_POINT('Origin',(0.00444923513249744,0.0134500081077393,
0.0639988309423512));
#107201=CARTESIAN_POINT('Origin',(0.00200484245198608,0.0136741614172377,
0.0640414954613487));
#107202=CARTESIAN_POINT('',(0.00200484245199608,0.0136741614172477,0.0640414954613587));
#107203=CARTESIAN_POINT('Origin',(0.00301864000319971,0.0142962479086285,
0.0640414954613487));
#107204=CARTESIAN_POINT('Origin',(0.000565228756317156,0.0142183150120642,
0.0640610392221339));
#107205=CARTESIAN_POINT('',(0.000565228756327156,0.0142183150120742,0.0640610392221439));
#107206=CARTESIAN_POINT('Origin',(0.00149489509322412,0.014960270253059,
0.0640610392221339));
#107207=CARTESIAN_POINT('Origin',(-0.000930343506396564,0.0145814325337034,
0.0640570798288145));
#107208=CARTESIAN_POINT('',(-0.000930343506406564,0.0145814325337134,0.0640570798288245));
#107209=CARTESIAN_POINT('Origin',(-9.89011778140814E-5,0.0154320092391563,
0.0640570798288145));
#107210=CARTESIAN_POINT('',(0.,0.,0.));
#107211=CARTESIAN_POINT('Origin',(-0.0411262178068916,-0.00152418147196182,
0.079));
#107212=CARTESIAN_POINT('',(-0.0286262178069016,-0.00152418147196182,0.071));
#107213=CARTESIAN_POINT('Origin',(-0.0286262178069016,-0.00152418147197183,
0.07900000000001));
#107214=CARTESIAN_POINT('',(-0.0321262178069016,-0.00152418147196182,0.071));
#107215=CARTESIAN_POINT('',(-0.0411262178068916,-0.00152418147196182,0.071));
#107216=CARTESIAN_POINT('',(-0.0321262178068916,-0.00552418147196183,0.0859282032302755));
#107217=CARTESIAN_POINT('Origin',(-0.0321262178069016,-0.00152418147197183,
0.07900000000001));
#107218=CARTESIAN_POINT('',(-0.0381262178068916,-0.00552418147196183,0.0859282032302755));
#107219=CARTESIAN_POINT('',(0.0161247821931184,-0.00552418147197183,0.0859282032302855));
#107220=CARTESIAN_POINT('',(-0.0381262178069016,-0.00152418147196182,0.071));
#107221=CARTESIAN_POINT('Origin',(-0.0381262178069016,-0.00152418147197183,
0.07900000000001));
#107222=CARTESIAN_POINT('',(-0.0411262178069016,-0.00152418147196182,0.071));
#107223=CARTESIAN_POINT('',(-0.0411262178068916,-0.00152418147196182,0.071));
#107224=CARTESIAN_POINT('Origin',(-0.0411262178069016,-0.00152418147197183,
0.07900000000001));
#107225=CARTESIAN_POINT('',(-0.0381262178068916,0.00247581852803818,0.0859282032302755));
#107226=CARTESIAN_POINT('Origin',(-0.0381262178069016,-0.00152418147197183,
0.07900000000001));
#107227=CARTESIAN_POINT('',(-0.0321262178068916,0.00247581852803818,0.0859282032302755));
#107228=CARTESIAN_POINT('',(0.0161247821931184,0.00247581852804817,0.0859282032302855));
#107229=CARTESIAN_POINT('Origin',(-0.0321262178069016,-0.00152418147197183,
0.07900000000001));
#107230=CARTESIAN_POINT('Origin',(-0.0411262178068916,-0.00152418147196182,
0.079));
#107231=CARTESIAN_POINT('',(-0.0286262178069016,-0.00152418147196182,0.081125));
#107232=CARTESIAN_POINT('Origin',(-0.0286262178069016,-0.00152418147197183,
0.07900000000001));
#107233=CARTESIAN_POINT('',(0.0121237821931184,-0.00152418147197183,0.08112500000002));
#107234=CARTESIAN_POINT('',(-0.0411262178068916,-0.00152418147196182,0.081125));
#107235=CARTESIAN_POINT('Origin',(0.0121237821931184,-0.00152418147197183,
0.07900000000001));
#107236=CARTESIAN_POINT('',(-0.0203797546539288,-0.000224178970103186,0.0773190423874585));
#107237=CARTESIAN_POINT('Ctrl Pts',(-0.0203762178068916,-0.00022418147196183,
0.0773190404525986));
#107238=CARTESIAN_POINT('Ctrl Pts',(-0.0206041367243007,-0.00022418147196183,
0.0773190404525986));
#107239=CARTESIAN_POINT('Ctrl Pts',(-0.0208484971135947,-0.000190393504626254,
0.0773434259833289));
#107240=CARTESIAN_POINT('Ctrl Pts',(-0.0212999007338416,-5.9145278846161E-5,
0.0774582802029004));
#107241=CARTESIAN_POINT('Ctrl Pts',(-0.0215066409493357,3.78043950968824E-5,
0.0775505157144276));
#107242=CARTESIAN_POINT('Ctrl Pts',(-0.0218058691331723,0.000218825249262259,
0.0777773576396814));
#107243=CARTESIAN_POINT('Ctrl Pts',(-0.0219377558664678,0.000320335511817705,
0.0779313118315859));
#107244=CARTESIAN_POINT('Ctrl Pts',(-0.0220899352670536,0.000453326551835115,
0.0782097791064571));
#107245=CARTESIAN_POINT('Ctrl Pts',(-0.0221452961494637,0.000508622809583374,
0.078359759662944));
#107246=CARTESIAN_POINT('Ctrl Pts',(-0.0222161284923853,0.000582494315132349,
0.0786773256153168));
#107247=CARTESIAN_POINT('Ctrl Pts',(-0.0222321205521884,0.00060081852803818,
0.0788448530223251));
#107248=CARTESIAN_POINT('Ctrl Pts',(-0.0222321205521884,0.00060081852803818,
0.0791551469776749));
#107249=CARTESIAN_POINT('Ctrl Pts',(-0.0222161284923853,0.000582494315132348,
0.0793226743846832));
#107250=CARTESIAN_POINT('Ctrl Pts',(-0.0221452961494636,0.000508622809583367,
0.079640240337056));
#107251=CARTESIAN_POINT('Ctrl Pts',(-0.0220899352670536,0.000453326551835114,
0.0797902208935429));
#107252=CARTESIAN_POINT('Ctrl Pts',(-0.0219377558664678,0.000320335511817702,
0.0800686881684141));
#107253=CARTESIAN_POINT('Ctrl Pts',(-0.0218058691331723,0.000218825249262255,
0.0802226423603186));
#107254=CARTESIAN_POINT('Ctrl Pts',(-0.0215066409493357,3.78043950968792E-5,
0.0804494842855724));
#107255=CARTESIAN_POINT('Ctrl Pts',(-0.0212999007338416,-5.91452788461605E-5,
0.0805417197970996));
#107256=CARTESIAN_POINT('Ctrl Pts',(-0.0208484971135947,-0.000190393504626253,
0.0806565740166711));
#107257=CARTESIAN_POINT('Ctrl Pts',(-0.0206041367243007,-0.00022418147196183,
0.0806809595474014));
#107258=CARTESIAN_POINT('Ctrl Pts',(-0.0201482988894825,-0.00022418147196183,
0.0806809595474014));
#107259=CARTESIAN_POINT('Ctrl Pts',(-0.0199039385001885,-0.000190393504626255,
0.0806565740166711));
#107260=CARTESIAN_POINT('Ctrl Pts',(-0.0194525348799416,-5.91452788461642E-5,
0.0805417197970996));
#107261=CARTESIAN_POINT('Ctrl Pts',(-0.0192457946644475,3.78043950968792E-5,
0.0804494842855724));
#107262=CARTESIAN_POINT('Ctrl Pts',(-0.0189465664806109,0.000218825249262255,
0.0802226423603186));
#107263=CARTESIAN_POINT('Ctrl Pts',(-0.0188146797473154,0.000320335511817702,
0.0800686881684141));
#107264=CARTESIAN_POINT('Ctrl Pts',(-0.0186625003467296,0.000453326551835114,
0.0797902208935429));
#107265=CARTESIAN_POINT('Ctrl Pts',(-0.0186071394643196,0.000508622809583367,
0.079640240337056));
#107266=CARTESIAN_POINT('Ctrl Pts',(-0.0185363071213979,0.000582494315132348,
0.0793226743846832));
#107267=CARTESIAN_POINT('Ctrl Pts',(-0.0185203150615948,0.00060081852803818,
0.0791551469776749));
#107268=CARTESIAN_POINT('Ctrl Pts',(-0.0185203150615948,0.00060081852803818,
0.0788448530223251));
#107269=CARTESIAN_POINT('Ctrl Pts',(-0.0185363071213979,0.000582494315132347,
0.0786773256153168));
#107270=CARTESIAN_POINT('Ctrl Pts',(-0.0186071394643196,0.000508622809583367,
0.078359759662944));
#107271=CARTESIAN_POINT('Ctrl Pts',(-0.0186625003467296,0.000453326551835115,
0.0782097791064571));
#107272=CARTESIAN_POINT('Ctrl Pts',(-0.0188146797473154,0.000320335511817705,
0.0779313118315859));
#107273=CARTESIAN_POINT('Ctrl Pts',(-0.0189465664806109,0.000218825249262259,
0.0777773576396814));
#107274=CARTESIAN_POINT('Ctrl Pts',(-0.0192457946644475,3.78043950968827E-5,
0.0775505157144276));
#107275=CARTESIAN_POINT('Ctrl Pts',(-0.0194525348799416,-5.91452788461609E-5,
0.0774582802029004));
#107276=CARTESIAN_POINT('Ctrl Pts',(-0.0199039385001885,-0.000190393504626253,
0.0773434259833289));
#107277=CARTESIAN_POINT('Ctrl Pts',(-0.0201482988894825,-0.00022418147196183,
0.0773190404525986));
#107278=CARTESIAN_POINT('Ctrl Pts',(-0.0203762178068916,-0.00022418147196183,
0.0773190404525986));
#107279=CARTESIAN_POINT('Origin',(-0.00312621780689159,0.00227581852803817,
0.041107864376269));
#107280=CARTESIAN_POINT('',(-0.00612621780691159,0.00227581852804816,0.05525000000001));
#107281=CARTESIAN_POINT('Origin',(-0.0031262178069016,0.00227581852804816,
0.05525000000001));
#107282=CARTESIAN_POINT('',(-0.00612621780691159,0.00227581852804816,0.05660000000001));
#107283=CARTESIAN_POINT('',(-0.00612621780689159,0.00227581852803817,0.041107864376269));
#107284=CARTESIAN_POINT('Origin',(-0.0031262178069016,0.00227581852804816,
0.05660000000001));
#107285=CARTESIAN_POINT('Origin',(-0.00312621780689159,0.00227581852803817,
0.041107864376269));
#107286=CARTESIAN_POINT('',(-0.00719324679239884,0.00518430184946944,0.05525));
#107287=CARTESIAN_POINT('',(-0.00719324679239884,-0.000632664793393113,
0.05525));
#107288=CARTESIAN_POINT('Origin',(-0.0031262178069016,0.00227581852804816,
0.05525000000001));
#107289=CARTESIAN_POINT('',(-0.00719324679239884,0.00518430184946944,0.0566));
#107290=CARTESIAN_POINT('',(-0.00719324679240884,0.00518430184947944,0.05592500000001));
#107291=CARTESIAN_POINT('',(-0.00719324679239884,-0.000632664793393113,
0.0566));
#107292=CARTESIAN_POINT('Origin',(-0.0031262178069016,0.00227581852804816,
0.05660000000001));
#107293=CARTESIAN_POINT('',(-0.00719324679240884,-0.000632664793403113,
0.05592500000001));
#107294=CARTESIAN_POINT('Origin',(-0.0203762178068916,0.00227581852803817,
0.0862));
#107295=CARTESIAN_POINT('',(-0.0178762178068916,0.00227581852803817,0.08620000000001));
#107296=CARTESIAN_POINT('Origin',(-0.0203762178069016,0.00227581852804817,
0.08620000000001));
#107297=CARTESIAN_POINT('',(-0.0178762178068916,0.00227581852803817,0.07370000000001));
#107298=CARTESIAN_POINT('',(-0.0178762178068916,0.00227581852803817,0.0862));
#107299=CARTESIAN_POINT('Origin',(-0.0203762178069016,0.00227581852804817,
0.07370000000001));
#107300=CARTESIAN_POINT('Origin',(-0.0203762178068916,0.00227581852803817,
0.0637));
#107301=CARTESIAN_POINT('',(-0.0144609098358771,-0.00594152633560559,0.0586));
#107302=CARTESIAN_POINT('',(-0.0102512178068916,0.00227581852803817,0.05860000000001));
#107303=CARTESIAN_POINT('Origin',(-0.0203762178069016,0.00227581852804817,
0.05860000000001));
#107304=CARTESIAN_POINT('',(-0.00912621780688617,0.00227581852803817,0.0572499999999935));
#107305=CARTESIAN_POINT('',(-0.0145012178068916,0.00227581852803817,0.0637));
#107306=CARTESIAN_POINT('Origin',(-0.0203762178069016,0.00227581852804817,
0.05725000000001));
#107307=CARTESIAN_POINT('',(-0.0144609098358771,0.0104931633916819,0.0586));
#107308=CARTESIAN_POINT('Origin',(-0.0203762178069016,0.00227581852804817,
0.05860000000001));
#107309=CARTESIAN_POINT('',(-0.0164233917199351,0.0066559059616719,0.06367));
#107310=CARTESIAN_POINT('Ctrl Pts',(-0.0164233917199351,0.0066559059616719,
0.06367));
#107311=CARTESIAN_POINT('Ctrl Pts',(-0.0164194276971006,0.00666794003675013,
0.0636560923266654));
#107312=CARTESIAN_POINT('Ctrl Pts',(-0.0164154450144916,0.00667997579433552,
0.0636421601590875));
#107313=CARTESIAN_POINT('Ctrl Pts',(-0.0159684806507079,0.00802457625950158,
0.0620832010103005));
#107314=CARTESIAN_POINT('Ctrl Pts',(-0.0153003449699402,0.00932716537760438,
0.0603240800152843));
#107315=CARTESIAN_POINT('Ctrl Pts',(-0.0144793567578685,0.0104676731934383,
0.0586377577447297));
#107316=CARTESIAN_POINT('Ctrl Pts',(-0.0144701478215295,0.0104804208666844,
0.058618886548445));
#107317=CARTESIAN_POINT('Ctrl Pts',(-0.0144609098358771,0.0104931633916819,
0.0586));
#107318=CARTESIAN_POINT('',(-0.0262762178068916,0.00227581852803817,0.06367));
#107319=CARTESIAN_POINT('Origin',(-0.0203762178069016,0.00227581852804817,
0.06367000000001));
#107320=CARTESIAN_POINT('',(-0.0164233917199351,-0.00210426890559556,0.06367));
#107321=CARTESIAN_POINT('Origin',(-0.0203762178069016,0.00227581852804817,
0.06367000000001));
#107322=CARTESIAN_POINT('Ctrl Pts',(-0.0144609098358771,-0.00594152633560559,
0.0586));
#107323=CARTESIAN_POINT('Ctrl Pts',(-0.0144701478215295,-0.00592878381060804,
0.058618886548445));
#107324=CARTESIAN_POINT('Ctrl Pts',(-0.0144793567578685,-0.00591603613736201,
0.0586377577447297));
#107325=CARTESIAN_POINT('Ctrl Pts',(-0.0153003449699402,-0.00477552832152804,
0.0603240800152843));
#107326=CARTESIAN_POINT('Ctrl Pts',(-0.0159684806507079,-0.00347293920342524,
0.0620832010103005));
#107327=CARTESIAN_POINT('Ctrl Pts',(-0.0164154450144916,-0.00212833873825919,
0.0636421601590875));
#107328=CARTESIAN_POINT('Ctrl Pts',(-0.0164194276971006,-0.00211630298067379,
0.0636560923266654));
#107329=CARTESIAN_POINT('Ctrl Pts',(-0.0164233917199351,-0.00210426890559556,
0.06367));
#107330=CARTESIAN_POINT('Origin',(-0.0203762178068916,0.00227581852803817,
0.05725));
#107331=CARTESIAN_POINT('',(-0.0091262178068916,0.00227581852803817,0.05525000000001));
#107332=CARTESIAN_POINT('',(-0.0091262178068916,0.00227581852803817,0.05725));
#107333=CARTESIAN_POINT('Origin',(-0.0203762178069016,0.00227581852804817,
0.05525000000001));
#107334=CARTESIAN_POINT('Origin',(-0.0186262178068916,-0.0128741814719618,
0.0450676623509137));
#107335=CARTESIAN_POINT('',(-0.0201262178069116,-0.0128741814719718,0.05525000000001));
#107336=CARTESIAN_POINT('Origin',(-0.0186262178069016,-0.0128741814719718,
0.05525000000001));
#107337=CARTESIAN_POINT('',(-0.0201262178069116,-0.0128741814719718,0.05660000000001));
#107338=CARTESIAN_POINT('',(-0.0201262178068916,-0.0128741814719618,0.0450676623509137));
#107339=CARTESIAN_POINT('Origin',(-0.0186262178069016,-0.0128741814719718,
0.05660000000001));
#107340=CARTESIAN_POINT('Origin',(-0.0186262178068916,-0.0128741814719618,
0.0450676623509137));
#107341=CARTESIAN_POINT('',(-0.0159420398647638,-0.0104751840199009,0.05525));
#107342=CARTESIAN_POINT('',(-0.017783602829574,-0.0163741814719618,0.05525));
#107343=CARTESIAN_POINT('Origin',(-0.0186262178069016,-0.0128741814719718,
0.05525000000001));
#107344=CARTESIAN_POINT('',(-0.0159420398647638,-0.0104751840199009,0.06075));
#107345=CARTESIAN_POINT('',(-0.0159420398647739,-0.0104751840199109,0.05592500000001));
#107346=CARTESIAN_POINT('',(-0.017783602829574,-0.0163741814719618,0.06075));
#107347=CARTESIAN_POINT('Origin',(-0.0186262178069016,-0.0128741814719718,
0.06075000000001));
#107348=CARTESIAN_POINT('',(-0.017783602829584,-0.0163741814719718,0.0450676623509237));
#107349=CARTESIAN_POINT('Origin',(-0.00487621780689159,0.0177758185280382,
0.0566));
#107350=CARTESIAN_POINT('',(-0.00681722270126977,0.0209258185280382,0.0655));
#107351=CARTESIAN_POINT('',(-0.0084892273106359,0.0169782206808412,0.0655));
#107352=CARTESIAN_POINT('Origin',(-0.00487621780690159,0.0177758185280482,
0.06550000000001));
#107353=CARTESIAN_POINT('',(-0.00681722270126977,0.0209258185280382,0.05525));
#107354=CARTESIAN_POINT('',(-0.00681722270127977,0.0209258185280481,0.05660000000001));
#107355=CARTESIAN_POINT('',(-0.00122621780689159,0.0171696007453891,0.05525));
#107356=CARTESIAN_POINT('Origin',(-0.00487621780690159,0.0177758185280482,
0.05525000000001));
#107357=CARTESIAN_POINT('',(-0.00122621780689159,0.0171696007453891,0.0566));
#107358=CARTESIAN_POINT('',(-0.00122621780690159,0.0171696007453991,0.05660000000001));
#107359=CARTESIAN_POINT('',(-0.0084892273106359,0.0169782206808412,0.0566));
#107360=CARTESIAN_POINT('Origin',(-0.00487621780690159,0.0177758185280482,
0.05660000000001));
#107361=CARTESIAN_POINT('',(-0.0084892273106459,0.0169782206808512,0.06550000000001));
#107362=CARTESIAN_POINT('Origin',(-0.0358762178068916,0.0177758185280382,
0.08545));
#107363=CARTESIAN_POINT('',(-0.0387012178068916,0.0177758185280382,0.08545000000001));
#107364=CARTESIAN_POINT('Origin',(-0.0358762178069016,0.0177758185280482,
0.08545000000001));
#107365=CARTESIAN_POINT('',(-0.0387012178068916,0.0177758185280382,0.08925000000001));
#107366=CARTESIAN_POINT('',(-0.0387012178068916,0.0177758185280382,0.08545));
#107367=CARTESIAN_POINT('Origin',(-0.0358762178069016,0.0177758185280482,
0.08925000000001));
#107368=CARTESIAN_POINT('Origin',(-0.00487621780689159,0.0177758185280382,
0.08545));
#107369=CARTESIAN_POINT('',(-0.00770121780689159,0.0177758185280382,0.08545000000001));
#107370=CARTESIAN_POINT('Origin',(-0.00487621780690159,0.0177758185280482,
0.08545000000001));
#107371=CARTESIAN_POINT('',(-0.00770121780689159,0.0177758185280382,0.08925000000001));
#107372=CARTESIAN_POINT('',(-0.00770121780689159,0.0177758185280382,0.08545));
#107373=CARTESIAN_POINT('Origin',(-0.00487621780690159,0.0177758185280482,
0.08925000000001));
#107374=CARTESIAN_POINT('Origin',(-0.0358762178068916,-0.0132241814719618,
0.08545));
#107375=CARTESIAN_POINT('',(-0.0387012178068916,-0.0132241814719618,0.08545000000001));
#107376=CARTESIAN_POINT('Origin',(-0.0358762178069016,-0.0132241814719718,
0.08545000000001));
#107377=CARTESIAN_POINT('',(-0.0387012178068916,-0.0132241814719618,0.08925000000001));
#107378=CARTESIAN_POINT('',(-0.0387012178068916,-0.0132241814719618,0.08545));
#107379=CARTESIAN_POINT('Origin',(-0.0358762178069016,-0.0132241814719718,
0.08925000000001));
#107380=CARTESIAN_POINT('Origin',(-0.0358762178068916,-0.0132241814719618,
0.08925));
#107381=CARTESIAN_POINT('',(-0.0342762178068916,-0.0132241814719718,0.08545000000001));
#107382=CARTESIAN_POINT('Origin',(-0.0358762178069016,-0.0132241814719718,
0.08545000000001));
#107383=CARTESIAN_POINT('',(-0.0342762178068916,-0.0132241814719718,0.05525000000001));
#107384=CARTESIAN_POINT('',(-0.0342762178068916,-0.0132241814719618,0.08925));
#107385=CARTESIAN_POINT('Origin',(-0.0358762178069016,-0.0132241814719718,
0.05525000000001));
#107386=CARTESIAN_POINT('Origin',(-0.00487621780689159,0.0177758185280382,
0.08925));
#107387=CARTESIAN_POINT('',(-0.00327621780689159,0.0177758185280482,0.08545000000001));
#107388=CARTESIAN_POINT('Origin',(-0.00487621780690159,0.0177758185280482,
0.08545000000001));
#107389=CARTESIAN_POINT('',(-0.00327621780689159,0.0177758185280382,0.0677));
#107390=CARTESIAN_POINT('',(-0.00327621780689159,0.0177758185280382,0.08925));
#107391=CARTESIAN_POINT('',(-0.00647621780689159,0.0177758185280382,0.0677));
#107392=CARTESIAN_POINT('Origin',(-0.00487621780690159,0.0177758185280482,
0.06770000000001));
#107393=CARTESIAN_POINT('',(-0.00647621780689159,0.0177758185280382,0.0586));
#107394=CARTESIAN_POINT('',(-0.00647621780690159,0.0177758185280482,0.05860000000001));
#107395=CARTESIAN_POINT('',(-0.00327621780689159,0.0177758185280382,0.0586));
#107396=CARTESIAN_POINT('Origin',(-0.00487621780690159,0.0177758185280482,
0.05860000000001));
#107397=CARTESIAN_POINT('',(-0.00327621780689159,0.0177758185280482,0.05525000000001));
#107398=CARTESIAN_POINT('',(-0.00327621780689159,0.0177758185280382,0.08925));
#107399=CARTESIAN_POINT('Origin',(-0.00487621780690159,0.0177758185280482,
0.05525000000001));
#107400=CARTESIAN_POINT('',(-0.0032762178069016,0.0177758185280482,0.05860000000001));
#107401=CARTESIAN_POINT('Origin',(-0.0358762178068916,0.0177758185280382,
0.08925));
#107402=CARTESIAN_POINT('',(-0.0342762178068916,0.0177758185280482,0.08545000000001));
#107403=CARTESIAN_POINT('Origin',(-0.0358762178069016,0.0177758185280482,
0.08545000000001));
#107404=CARTESIAN_POINT('',(-0.0342762178068916,0.0177758185280482,0.05525000000001));
#107405=CARTESIAN_POINT('',(-0.0342762178068916,0.0177758185280382,0.08925));
#107406=CARTESIAN_POINT('Origin',(-0.0358762178069016,0.0177758185280482,
0.05525000000001));
#107407=CARTESIAN_POINT('Origin',(-0.0203762178068916,0.00227581852803817,
0.05525));
#107408=CARTESIAN_POINT('',(-0.0262762178069116,0.00227581852804817,0.07370000000001));
#107409=CARTESIAN_POINT('',(-0.0262762178068916,0.00227581852803817,0.05525));
#107410=CARTESIAN_POINT('Origin',(-0.0203762178069016,0.00227581852804817,
0.07370000000001));
#107411=CARTESIAN_POINT('',(-0.0164233917199351,0.0066559059616719,0.0677));
#107412=CARTESIAN_POINT('',(-0.0164233917199451,0.0066559059616819,0.06147500000001));
#107413=CARTESIAN_POINT('',(-0.0164233917199351,-0.00210426890559556,0.0677));
#107414=CARTESIAN_POINT('Origin',(-0.0203762178069016,0.00227581852804817,
0.06770000000001));
#107415=CARTESIAN_POINT('',(-0.0164233917199451,-0.00210426890560557,0.06147500000001));
#107416=CARTESIAN_POINT('Origin',(-0.0203762178068916,0.00227581852803817,
0.0566));
#107417=CARTESIAN_POINT('',(-0.0135678120097901,0.0139332457957502,0.0655));
#107418=CARTESIAN_POINT('',(-0.0256278910009942,-0.0101608180213808,0.0655));
#107419=CARTESIAN_POINT('Origin',(-0.0203762178069016,0.00227581852804817,
0.06550000000001));
#107420=CARTESIAN_POINT('',(-0.0135678120097901,0.0139332457957502,0.0566));
#107421=CARTESIAN_POINT('',(-0.0135678120098001,0.0139332457957602,0.06550000000001));
#107422=CARTESIAN_POINT('Origin',(-0.0203762178069016,0.00227581852804817,
0.05660000000001));
#107423=CARTESIAN_POINT('',(-0.0217866356183144,-0.0111503023412681,0.05525));
#107424=CARTESIAN_POINT('Origin',(-0.0203762178069016,0.00227581852804817,
0.05525000000001));
#107425=CARTESIAN_POINT('',(-0.0217866356183144,-0.0111503023412681,0.0615));
#107426=CARTESIAN_POINT('',(-0.0217866356183244,-0.0111503023412781,0.05592500000001));
#107427=CARTESIAN_POINT('',(-0.0256278910009942,-0.0101608180213808,0.0615));
#107428=CARTESIAN_POINT('Origin',(-0.0203762178069016,0.00227581852804817,
0.06150000000001));
#107429=CARTESIAN_POINT('',(-0.0256278910010042,-0.0101608180213908,0.06550000000001));
#107430=CARTESIAN_POINT('Origin',(-0.0411262178068916,-0.0144741814719618,
0.05525));
#107431=CARTESIAN_POINT('',(0.0021237821931084,-0.0144741814719618,0.06355));
#107432=CARTESIAN_POINT('',(0.00212378219310841,-0.0144741814719618,0.08475));
#107433=CARTESIAN_POINT('',(0.0021237821931184,-0.0144741814719718,0.0326378260227564));
#107434=CARTESIAN_POINT('',(0.0121237821931084,-0.0144741814719618,0.0653239130434783));
#107435=CARTESIAN_POINT('',(0.0021237821931184,-0.0144741814719718,0.06355000000001));
#107436=CARTESIAN_POINT('',(0.0121237821931084,-0.0144741814719618,0.0829760869565217));
#107437=CARTESIAN_POINT('',(0.0121237821931184,-0.0144741814719718,0.0653239130434883));
#107438=CARTESIAN_POINT('',(0.0121237821931184,-0.0144741814719718,0.0829760869565317));
#107439=CARTESIAN_POINT('Origin',(-0.0031262178068916,0.00227581852803817,
0.0586));
#107440=CARTESIAN_POINT('',(-0.0153915143789277,-0.00447418147196182,0.06355));
#107441=CARTESIAN_POINT('',(-0.0153915143789277,-0.00447418147196182,0.0677));
#107442=CARTESIAN_POINT('',(-0.0153915143789377,-0.00447418147197182,0.05860000000001));
#107443=CARTESIAN_POINT('',(0.0021237821931084,-0.0107025288243792,0.06355));
#107444=CARTESIAN_POINT('Origin',(-0.00312621780690161,0.00227581852804816,
0.06355000000001));
#107445=CARTESIAN_POINT('',(0.00212378219310841,-0.0107025288243792,0.0677));
#107446=CARTESIAN_POINT('',(0.0021237821931184,-0.0107025288243892,0.05860000000001));
#107447=CARTESIAN_POINT('',(0.00744576188789692,-0.00690204861705493,0.0677));
#107448=CARTESIAN_POINT('Origin',(-0.00312621780690161,0.00227581852804816,
0.06770000000001));
#107449=CARTESIAN_POINT('',(0.00744576188789692,-0.00690204861705493,0.0586));
#107450=CARTESIAN_POINT('',(0.00744576188790692,-0.00690204861706493,0.05860000000001));
#107451=CARTESIAN_POINT('Origin',(-0.00312621780690161,0.00227581852804816,
0.05860000000001));
#107452=CARTESIAN_POINT('Origin',(-0.00312621780690161,0.00227581852804816,
0.06770000000001));
#107453=CARTESIAN_POINT('Origin',(-0.0411262178068916,-0.0184741814719619,
0.0677));
#107454=CARTESIAN_POINT('',(0.00212378219310841,-0.00447418147196182,0.0677));
#107455=CARTESIAN_POINT('',(-0.0411262178069016,-0.00447418147197182,0.06770000000001));
#107456=CARTESIAN_POINT('',(-0.00647621780689159,0.0158691073133175,0.0677));
#107457=CARTESIAN_POINT('Origin',(-0.00312621780690161,0.00227581852804816,
0.06770000000001));
#107458=CARTESIAN_POINT('',(-0.00647621780690159,0.0177758185280482,0.06770000000001));
#107459=CARTESIAN_POINT('',(-0.00327621780689159,0.0162750149335466,0.0677));
#107460=CARTESIAN_POINT('',(-0.0032762178069016,0.0177758185280482,0.06770000000001));
#107461=CARTESIAN_POINT('',(0.000873782193108408,0.0156922263930369,0.0677));
#107462=CARTESIAN_POINT('Origin',(-0.00312621780690161,0.00227581852804816,
0.06770000000001));
#107463=CARTESIAN_POINT('',(0.000873782193108408,0.0185258185280382,0.0677));
#107464=CARTESIAN_POINT('',(0.000873782193118408,0.0185258185280481,0.06770000000001));
#107465=CARTESIAN_POINT('',(0.0112230245980259,0.00817657612312065,0.0677));
#107466=CARTESIAN_POINT('',(0.000873782193118408,0.0185258185280481,0.06770000000001));
#107467=CARTESIAN_POINT('',(0.0121237821931084,0.00427931609139309,0.0677));
#107468=CARTESIAN_POINT('',(0.0112230245980359,0.00817657612313065,0.06770000000001));
#107469=CARTESIAN_POINT('',(0.0121237821931084,-0.0115800689222664,0.0677));
#107470=CARTESIAN_POINT('',(0.0121237821931184,0.00427931609140309,0.06770000000001));
#107471=CARTESIAN_POINT('',(0.00500246184955876,-0.00445874857871678,0.06770000000001));
#107472=CARTESIAN_POINT('',(0.00212378219311841,-0.0184741814719718,0.06770000000001));
#107473=CARTESIAN_POINT('Origin',(-0.0311262178068916,-0.0144741814719618,
0.06355));
#107474=CARTESIAN_POINT('',(-0.0171262178068915,-0.00447418147196182,0.06355));
#107475=CARTESIAN_POINT('',(-0.0311262178068916,-0.0184741814719619,0.06355));
#107476=CARTESIAN_POINT('',(-0.0311262178069016,-0.0184741814719718,0.06355000000001));
#107477=CARTESIAN_POINT('',(0.0021237821931084,-0.0184741814719618,0.06355));
#107478=CARTESIAN_POINT('',(-0.0311262178069016,-0.0184741814719718,0.06355000000001));
#107479=CARTESIAN_POINT('',(0.0021237821931184,-0.0144741814719718,0.06355000000001));
#107480=CARTESIAN_POINT('',(0.0021237821931184,-0.00447418147197182,0.06355000000001));
#107481=CARTESIAN_POINT('',(-0.0171262178069015,-0.00447418147197182,0.06355000000001));
#107482=CARTESIAN_POINT('Origin',(-0.0311262178068916,-0.0144741814719618,
0.08475));
#107483=CARTESIAN_POINT('',(-0.0171262178068915,-0.00447418147196182,0.08475));
#107484=CARTESIAN_POINT('',(-0.0311262178068916,-0.0184741814719619,0.08475));
#107485=CARTESIAN_POINT('',(-0.0311262178069016,-0.0184741814719718,0.08475000000001));
#107486=CARTESIAN_POINT('',(0.00212378219310841,-0.00447418147196182,0.08475));
#107487=CARTESIAN_POINT('',(-0.0171262178069015,-0.00447418147197182,0.08475000000001));
#107488=CARTESIAN_POINT('',(0.00212378219311841,-0.00447418147197182,0.08475000000001));
#107489=CARTESIAN_POINT('',(0.0021237821931084,-0.0184741814719618,0.08475));
#107490=CARTESIAN_POINT('',(0.0021237821931184,-0.0144741814719718,0.08475000000001));
#107491=CARTESIAN_POINT('',(-0.0311262178069016,-0.0184741814719718,0.08475000000001));
#107492=CARTESIAN_POINT('Origin',(0.0121237821931084,-0.0150800689222664,
0.08925));
#107493=CARTESIAN_POINT('',(0.00872966964341299,-0.0184741814719619,0.088));
#107494=CARTESIAN_POINT('',(0.00872966964341299,-0.0184741814719618,0.0835781730088155));
#107495=CARTESIAN_POINT('',(0.00872966964342298,-0.0184741814719718,0.08925000000001));
#107496=CARTESIAN_POINT('',(0.0121237821931084,-0.0150800689222664,0.0829760869565217));
#107497=CARTESIAN_POINT('',(0.0115759331517965,-0.0156279179635983,0.0830732706125575));
#107498=CARTESIAN_POINT('',(0.0121237821931084,-0.0150800689222664,0.088));
#107499=CARTESIAN_POINT('',(0.0121237821931184,-0.0150800689222764,0.08925000000001));
#107500=CARTESIAN_POINT('',(0.0121237821931184,-0.0150800689222764,0.08800000000001));
#107501=CARTESIAN_POINT('Origin',(-0.00487621780689159,0.0177758185280382,
0.0566));
#107502=CARTESIAN_POINT('Origin',(-0.0031262178069016,0.00227581852804816,
0.05660000000001));
#107503=CARTESIAN_POINT('',(-0.0012262178068916,0.0105512709814273,0.0566));
#107504=CARTESIAN_POINT('',(-0.0012262178069016,0.0105512709814373,0.05660000000001));
#107505=CARTESIAN_POINT('',(0.000282704463412254,0.00638543403208472,0.0566));
#107506=CARTESIAN_POINT('Origin',(0.00527877065166022,0.0105512709814373,
0.05660000000001));
#107507=CARTESIAN_POINT('',(0.000905971897274149,0.00563795269990278,0.0566));
#107508=CARTESIAN_POINT('',(0.000905971897284156,0.00563795269991278,0.05660000000001));
#107509=CARTESIAN_POINT('',(0.0021237821931084,0.00227581852803816,0.0566));
#107510=CARTESIAN_POINT('Origin',(-0.0031262178069016,0.00227581852804816,
0.05660000000001));
#107511=CARTESIAN_POINT('',(0.0021237821931084,-0.00233742823514713,0.0566));
#107512=CARTESIAN_POINT('',(0.0021237821931184,0.00227581852804816,0.05660000000001));
#107513=CARTESIAN_POINT('',(0.00358824828717567,-0.00587296214107986,0.0566));
#107514=CARTESIAN_POINT('Origin',(0.00712378219311841,-0.00233742823515713,
0.05660000000001));
#107515=CARTESIAN_POINT('',(0.00719958354106424,-0.00948429739496843,0.0566));
#107516=CARTESIAN_POINT('',(0.0100237821931184,-0.0123084960470226,0.05660000000001));
#107517=CARTESIAN_POINT('',(-0.0135678120097901,-0.00938160873967384,0.0566));
#107518=CARTESIAN_POINT('Origin',(-0.0031262178069016,0.00227581852804816,
0.05660000000001));
#107519=CARTESIAN_POINT('Origin',(-0.0203762178069016,0.00227581852804817,
0.05660000000001));
#107520=CARTESIAN_POINT('Origin',(-0.0203762178068916,0.00227581852803817,
0.0566));
#107521=CARTESIAN_POINT('',(-0.0135678120097901,-0.00938160873967384,0.06075));
#107522=CARTESIAN_POINT('',(-0.0135678120098001,-0.00938160873968384,0.06075000000001));
#107523=CARTESIAN_POINT('Origin',(-0.0203762178069016,0.00227581852804817,
0.06075000000001));
#107524=CARTESIAN_POINT('Origin',(-0.0203762178069016,0.00227581852804817,
0.05525000000001));
#107525=CARTESIAN_POINT('Origin',(-0.0031262178068916,0.00227581852803817,
0.0586));
#107526=CARTESIAN_POINT('',(-0.00647621780689159,0.0158691073133175,0.0586));
#107527=CARTESIAN_POINT('Origin',(-0.00312621780690161,0.00227581852804816,
0.05860000000001));
#107528=CARTESIAN_POINT('',(-0.00647621780690159,0.0158691073133275,0.05860000000001));
#107529=CARTESIAN_POINT('Origin',(-0.0339352129125134,-0.0163741814719618,
0.0566));
#107530=CARTESIAN_POINT('',(0.00785982116242948,-0.0163741814719618,0.06075));
#107531=CARTESIAN_POINT('',(0.00785982116243948,-0.0163741814719718,0.06075000000001));
#107532=CARTESIAN_POINT('',(0.00785982116242948,-0.0163741814719618,0.05525));
#107533=CARTESIAN_POINT('',(0.00785982116243948,-0.0163741814719718,0.05660000000001));
#107534=CARTESIAN_POINT('',(-0.0339352129125234,-0.0163741814719718,0.05525000000001));
#107535=CARTESIAN_POINT('Origin',(-0.0339352129125134,-0.0163741814719618,
0.0566));
#107536=CARTESIAN_POINT('',(-0.0194688327842092,-0.0163741814719618,0.05525));
#107537=CARTESIAN_POINT('',(-0.0339352129125134,-0.0163741814719618,0.05525));
#107538=CARTESIAN_POINT('',(-0.0339352129125234,-0.0163741814719718,0.05525000000001));
#107539=CARTESIAN_POINT('',(-0.0339352129125134,-0.0163741814719618,0.0655));
#107540=CARTESIAN_POINT('',(-0.0339352129125234,-0.0163741814719718,0.05660000000001));
#107541=CARTESIAN_POINT('',(-0.0330326892153179,-0.0163741814719618,0.0655));
#107542=CARTESIAN_POINT('',(-0.0330326892153278,-0.0163741814719718,0.06550000000001));
#107543=CARTESIAN_POINT('',(-0.0330326892153179,-0.0163741814719618,0.0615));
#107544=CARTESIAN_POINT('',(-0.0330326892153278,-0.0163741814719718,0.06550000000001));
#107545=CARTESIAN_POINT('',(-0.0194688327842092,-0.0163741814719618,0.0615));
#107546=CARTESIAN_POINT('',(-0.0330326892153278,-0.0163741814719718,0.06150000000001));
#107547=CARTESIAN_POINT('',(-0.0194688327842192,-0.0163741814719718,0.0450676623509237));
#107548=CARTESIAN_POINT('Origin',(-0.0411262178068916,-0.0184741814719619,
0.08925));
#107549=CARTESIAN_POINT('',(0.0108737821931084,-0.0145623019693,0.08925));
#107550=CARTESIAN_POINT('',(0.0108737821931084,0.00675805157507176,0.08925));
#107551=CARTESIAN_POINT('',(0.0108737821931184,-0.0184741814719718,0.08925000000001));
#107552=CARTESIAN_POINT('',(-0.00414398475985796,0.0217758185280382,0.08925));
#107553=CARTESIAN_POINT('',(-0.00251010128338471,0.0201419350515649,0.08925000000001));
#107554=CARTESIAN_POINT('',(-0.0372143383042298,0.0217758185280382,0.08925));
#107555=CARTESIAN_POINT('',(-0.0411262178069016,0.0217758185280482,0.08925000000001));
#107556=CARTESIAN_POINT('',(-0.0398762178068916,0.0191139390253764,0.08925));
#107557=CARTESIAN_POINT('',(-0.0592952780555707,-0.00030512122330272,0.08925000000001));
#107558=CARTESIAN_POINT('',(-0.0398762178068916,-0.0145623019693,0.08925));
#107559=CARTESIAN_POINT('',(-0.0398762178069016,-0.0184741814719718,0.08925000000001));
#107560=CARTESIAN_POINT('',(-0.0372143383042298,-0.0172241814719618,0.08925));
#107561=CARTESIAN_POINT('',(-0.0385452780555707,-0.0158932417206409,0.08925000000001));
#107562=CARTESIAN_POINT('',(0.00821190269044663,-0.0172241814719618,0.08925));
#107563=CARTESIAN_POINT('',(-0.0411262178069016,-0.0172241814719718,0.08925000000001));
#107564=CARTESIAN_POINT('',(-0.0170821575582324,-0.0425182417206409,0.08925000000001));
#107565=CARTESIAN_POINT('',(-0.0266262178068916,0.0142758185280382,0.08925));
#107566=CARTESIAN_POINT('',(-0.0266262178068916,-0.00972418147196183,0.08925));
#107567=CARTESIAN_POINT('',(-0.0266262178069016,-0.00972418147197183,0.08925000000001));
#107568=CARTESIAN_POINT('',(-0.0246762178068916,0.0202758185280381,0.08925));
#107569=CARTESIAN_POINT('',(-0.0266262178069016,0.0142758185280482,0.08925000000001));
#107570=CARTESIAN_POINT('',(-0.0166762178068916,0.0202758185280381,0.08925));
#107571=CARTESIAN_POINT('',(-0.0246762178069016,0.0202758185280481,0.08925000000001));
#107572=CARTESIAN_POINT('',(-0.0147262178068916,0.0142758185280382,0.08925));
#107573=CARTESIAN_POINT('',(-0.0166762178069016,0.0202758185280481,0.08925000000001));
#107574=CARTESIAN_POINT('',(-0.0147262178068916,-0.00972418147196183,0.08925));
#107575=CARTESIAN_POINT('',(-0.0147262178069016,0.0142758185280482,0.08925000000001));
#107576=CARTESIAN_POINT('',(-0.0166762178068916,-0.0157241814719619,0.08925));
#107577=CARTESIAN_POINT('',(-0.0147262178069016,-0.00972418147197183,0.08925000000001));
#107578=CARTESIAN_POINT('',(-0.0246762178068916,-0.0157241814719619,0.08925));
#107579=CARTESIAN_POINT('',(-0.0166762178069016,-0.0157241814719719,0.08925000000001));
#107580=CARTESIAN_POINT('',(-0.0246762178069016,-0.0157241814719719,0.08925000000001));
#107581=CARTESIAN_POINT('Origin',(-0.0411262178068916,-0.0184741814719619,
0.05525));
#107582=CARTESIAN_POINT('',(0.00872966964341299,-0.0155043329909783,0.05525));
#107583=CARTESIAN_POINT('',(0.00785982116243948,-0.0163741814719718,0.05525000000001));
#107584=CARTESIAN_POINT('',(0.00872966964341299,-0.0184741814719618,0.05525));
#107585=CARTESIAN_POINT('',(0.00872966964342298,0.0230258185280482,0.05525000000001));
#107586=CARTESIAN_POINT('',(-0.0377321052571961,-0.0184741814719619,0.05525));
#107587=CARTESIAN_POINT('',(0.00872966964342298,-0.0184741814719718,0.05525000000001));
#107588=CARTESIAN_POINT('',(-0.0411262178068916,-0.0150800689222664,0.05525));
#107589=CARTESIAN_POINT('',(-0.0377321052572061,-0.0184741814719718,0.05525000000001));
#107590=CARTESIAN_POINT('',(-0.0411262178068916,0.0196317059783427,0.05525));
#107591=CARTESIAN_POINT('',(-0.0411262178069016,-0.0150800689222764,0.05525000000001));
#107592=CARTESIAN_POINT('',(-0.0377321052571961,0.0230258185280382,0.05525));
#107593=CARTESIAN_POINT('',(-0.0411262178069016,0.0196317059783527,0.05525000000001));
#107594=CARTESIAN_POINT('',(-0.00362621780689159,0.0230258185280382,0.05525));
#107595=CARTESIAN_POINT('',(-0.0377321052572061,0.0230258185280482,0.05525000000001));
#107596=CARTESIAN_POINT('',(0.000873782193108408,0.0185258185280382,0.05525));
#107597=CARTESIAN_POINT('',(-0.0036262178069016,0.0230258185280482,0.05525000000001));
#107598=CARTESIAN_POINT('',(0.000873782193108401,0.0102484278875892,0.05525));
#107599=CARTESIAN_POINT('',(0.000873782193118408,0.0185258185280481,0.05525000000001));
#107600=CARTESIAN_POINT('',(0.00180163765660117,0.00768680185188279,0.05525));
#107601=CARTESIAN_POINT('Origin',(0.0048737821931184,0.0102484278875992,
0.05525000000001));
#107602=CARTESIAN_POINT('',(0.00244204416552777,0.00691876571775598,0.05525));
#107603=CARTESIAN_POINT('',(0.00244204416553777,0.00691876571776598,0.05525000000001));
#107604=CARTESIAN_POINT('',(0.0041237821931084,0.00227581852803816,0.05525));
#107605=CARTESIAN_POINT('Origin',(-0.00312621780690161,0.00227581852804816,
0.05525000000001));
#107606=CARTESIAN_POINT('',(0.0041237821931084,-0.00233742823514713,0.05525));
#107607=CARTESIAN_POINT('',(0.00412378219311839,0.00227581852804816,0.05525000000001));
#107608=CARTESIAN_POINT('',(0.00500246184954876,-0.00445874857870678,0.05525));
#107609=CARTESIAN_POINT('Origin',(0.00712378219311841,-0.00233742823515713,
0.05525000000001));
#107610=CARTESIAN_POINT('',(0.00872966964341298,-0.00818595637257098,0.05525));
#107611=CARTESIAN_POINT('',(0.00500246184955876,-0.00445874857871678,0.05525000000001));
#107612=CARTESIAN_POINT('',(0.00872966964341299,-0.0110143834973172,0.05525));
#107613=CARTESIAN_POINT('',(0.00872966964342298,0.0230258185280482,0.05525000000001));
#107614=CARTESIAN_POINT('',(0.00358824828717567,-0.00587296214107986,0.05525));
#107615=CARTESIAN_POINT('',(0.0100237821931184,-0.0123084960470226,0.05525000000001));
#107616=CARTESIAN_POINT('',(0.0021237821931084,-0.00233742823514713,0.05525));
#107617=CARTESIAN_POINT('Origin',(0.00712378219311841,-0.00233742823515713,
0.05525000000001));
#107618=CARTESIAN_POINT('',(0.0021237821931084,0.00227581852803816,0.05525));
#107619=CARTESIAN_POINT('',(0.0021237821931184,0.00227581852804816,0.05525000000001));
#107620=CARTESIAN_POINT('',(0.000905971897274149,0.00563795269990278,0.05525));
#107621=CARTESIAN_POINT('Origin',(-0.0031262178069016,0.00227581852804816,
0.05525000000001));
#107622=CARTESIAN_POINT('',(0.000282704463412254,0.00638543403208472,0.05525));
#107623=CARTESIAN_POINT('',(0.000905971897284156,0.00563795269991278,0.05525000000001));
#107624=CARTESIAN_POINT('',(-0.0012262178068916,0.0105512709814273,0.05525));
#107625=CARTESIAN_POINT('Origin',(0.00527877065166022,0.0105512709814373,
0.05525000000001));
#107626=CARTESIAN_POINT('',(-0.0012262178069016,0.0105512709814373,0.05525000000001));
#107627=CARTESIAN_POINT('',(-0.0339352129125134,0.0209258185280382,0.05525));
#107628=CARTESIAN_POINT('',(-0.00681722270127977,0.0209258185280481,0.05525000000001));
#107629=CARTESIAN_POINT('',(-0.0390262178068916,0.01583481363366,0.05525));
#107630=CARTESIAN_POINT('Origin',(-0.0358762178069016,0.0177758185280482,
0.05525000000001));
#107631=CARTESIAN_POINT('',(-0.0390262178068916,-0.0112831765775837,0.05525));
#107632=CARTESIAN_POINT('',(-0.0390262178069016,0.01583481363367,0.05525000000001));
#107633=CARTESIAN_POINT('Origin',(-0.0358762178069016,-0.0132241814719718,
0.05525000000001));
#107634=CARTESIAN_POINT('Origin',(-0.0186262178069016,-0.0128741814719718,
0.05525000000001));
#107635=CARTESIAN_POINT('Origin',(-0.0377321052571961,-0.0184741814719619,
0.08925));
#107636=CARTESIAN_POINT('',(-0.0377321052571961,-0.0184741814719619,0.088));
#107637=CARTESIAN_POINT('',(-0.0377321052572061,-0.0184741814719718,0.08925000000001));
#107638=CARTESIAN_POINT('',(-0.0411262178068916,-0.0150800689222664,0.088));
#107639=CARTESIAN_POINT('',(-0.0377321052572061,-0.0184741814719718,0.08800000000001));
#107640=CARTESIAN_POINT('',(-0.0411262178069016,-0.0150800689222764,0.08925000000001));
#107641=CARTESIAN_POINT('Origin',(0.00872966964341299,-0.0184741814719619,
0.08925));
#107642=CARTESIAN_POINT('',(0.0121237821931184,-0.0184741814719718,0.0829760869565317));
#107643=CARTESIAN_POINT('',(0.00872966964342298,-0.0184741814719718,0.08800000000001));
#107644=CARTESIAN_POINT('',(0.00872966964341299,-0.0184741814719618,0.0647218269911845));
#107645=CARTESIAN_POINT('',(0.00872966964342298,-0.0184741814719718,0.08925000000001));
#107646=CARTESIAN_POINT('',(0.0021237821931184,-0.0184741814719718,0.06355000000001));
#107647=CARTESIAN_POINT('',(-0.0311262178069016,-0.0184741814719718,0.06355000000001));
#107648=CARTESIAN_POINT('Origin',(0.0121237821931084,-0.0150800689222664,
0.08925));
#107649=CARTESIAN_POINT('',(0.0121237821931084,-0.0150800689222664,0.0653239130434783));
#107650=CARTESIAN_POINT('',(0.0121237821931084,-0.0150800689222664,0.0586441125496955));
#107651=CARTESIAN_POINT('',(0.0121237821931184,-0.0150800689222764,0.08925000000001));
#107652=CARTESIAN_POINT('',(0.0142130498815413,-0.0129908012338535,0.0656945309638694));
#107653=CARTESIAN_POINT('',(0.0223257446765532,-0.0048781064388415,0.0688460750331404));
#107654=CARTESIAN_POINT('Origin',(0.0121237821931084,0.00427931609139309,
0.08925));
#107655=CARTESIAN_POINT('',(0.0121237821931184,-0.0144741814719718,0.0829760869565317));
#107656=CARTESIAN_POINT('',(0.0121237821931184,-0.0144741814719718,0.0653239130434883));
#107657=CARTESIAN_POINT('',(0.0121237821931084,-0.0115800689222664,0.0586441125496955));
#107658=CARTESIAN_POINT('',(0.0121237821931184,0.0230258185280482,0.0586441125497055));
#107659=CARTESIAN_POINT('',(0.0121237821931184,-0.0115800689222764,0.0998391810594335));
#107660=CARTESIAN_POINT('',(0.0121237821931084,0.00427931609139309,0.088));
#107661=CARTESIAN_POINT('',(0.0121237821931184,0.00427931609140309,0.08925000000001));
#107662=CARTESIAN_POINT('',(0.0121237821931184,0.00427931609140309,0.08800000000001));
#107663=CARTESIAN_POINT('Origin',(0.0112230245980259,0.00817657612312065,
0.08925));
#107664=CARTESIAN_POINT('',(0.0112230245980259,0.00817657612312065,0.088));
#107665=CARTESIAN_POINT('',(0.0112230245980359,0.00817657612313065,0.08925000000001));
#107666=CARTESIAN_POINT('',(0.0114917234185988,0.00701401121141935,0.0886320587745096));
#107667=CARTESIAN_POINT('',(0.00874560658929598,0.018895489002749,0.0821723830896977));
#107668=CARTESIAN_POINT('',(0.0167544258428938,-0.0157558437740066,0.0833693563502346));
#107669=CARTESIAN_POINT('Origin',(-0.00362621780689159,0.0230258185280382,
0.08925));
#107670=CARTESIAN_POINT('',(0.000873782193118408,0.0185258185280481,0.0998391810594335));
#107671=CARTESIAN_POINT('',(-0.00362621780689159,0.0230258185280382,0.088));
#107672=CARTESIAN_POINT('',(-0.0036262178069016,0.0230258185280482,0.08925000000001));
#107673=CARTESIAN_POINT('',(-0.0036262178069016,0.0230258185280482,0.08800000000001));
#107674=CARTESIAN_POINT('Origin',(-0.0377321052571961,0.0230258185280382,
0.08925));
#107675=CARTESIAN_POINT('',(-0.0377321052571961,0.0230258185280382,0.088));
#107676=CARTESIAN_POINT('',(-0.0377321052572061,0.0230258185280482,0.08925000000001));
#107677=CARTESIAN_POINT('',(-0.0377321052572061,0.0230258185280482,0.08800000000001));
#107678=CARTESIAN_POINT('Origin',(-0.0411262178068916,0.0196317059783427,
0.08925));
#107679=CARTESIAN_POINT('',(-0.0411262178068916,0.0196317059783427,0.088));
#107680=CARTESIAN_POINT('',(-0.0411262178069016,0.0196317059783527,0.08925000000001));
#107681=CARTESIAN_POINT('',(-0.0411262178069016,0.0196317059783527,0.08800000000001));
#107682=CARTESIAN_POINT('Origin',(-0.0411262178068916,-0.0150800689222664,
0.08925));
#107683=CARTESIAN_POINT('',(-0.0411262178069016,-0.0150800689222764,0.08800000000001));
#107684=CARTESIAN_POINT('Origin',(-0.0385452780555607,-0.0158932417206309,
0.08925));
#107685=CARTESIAN_POINT('',(-0.0406223836679862,-0.0148713739887511,0.0885038341389253));
#107686=CARTESIAN_POINT('',(-0.0370656257560876,-0.0168651576213277,0.0896090238506542));
#107687=CARTESIAN_POINT('Origin',(-0.0411262178068916,-0.0172241814719618,
0.08925));
#107688=CARTESIAN_POINT('',(0.00431376816786663,-0.00781325223958014,0.0986609292324018));
#107689=CARTESIAN_POINT('Origin',(-0.0398762178068916,-0.0184741814719619,
0.08925));
#107690=CARTESIAN_POINT('',(-0.045114550931596,0.0212837276498631,0.0840116668753155));
#107691=CARTESIAN_POINT('Origin',(-0.0170821575582224,-0.0425182417206309,
0.08925));
#107692=CARTESIAN_POINT('',(0.00333260752472027,-0.0114386451454352,0.0967911746684082));
#107693=CARTESIAN_POINT('Origin',(-0.0592952780555607,-0.00030512122329272,
0.08925));
#107694=CARTESIAN_POINT('',(-0.0375234103236808,0.0225219843891328,0.0885038341389253));
#107695=CARTESIAN_POINT('Origin',(0.0108737821931084,-0.0184741814719619,
0.08925));
#107696=CARTESIAN_POINT('',(0.00726345093845756,0.00526260340474177,0.0928603312546709));
#107697=CARTESIAN_POINT('Origin',(-0.0411262178068916,0.0217758185280382,
0.08925));
#107698=CARTESIAN_POINT('',(-0.00706589823995062,0.0147216953763519,0.0963041231517064));
#107699=CARTESIAN_POINT('Origin',(-0.00251010128337472,0.020141935051555,
0.08925));
#107700=CARTESIAN_POINT('Origin',(-0.0358762178068916,-0.0132241814719618,
0.08545));
#107701=CARTESIAN_POINT('Origin',(-0.00487621780689159,0.0177758185280382,
0.08545));
#107702=CARTESIAN_POINT('Origin',(-0.0358762178068916,0.0177758185280382,
0.08545));
#107703=CARTESIAN_POINT('Origin',(0.00500246184954876,-0.00445874857870678,
0.0998391810594235));
#107704=CARTESIAN_POINT('',(0.0211079248006548,-0.0205642115298128,0.0676282551572419));
#107705=CARTESIAN_POINT('',(0.00500246184954876,-0.00445874857870678,0.0586));
#107706=CARTESIAN_POINT('',(0.00500246184955876,-0.00445874857871678,0.0998391810594335));
#107707=CARTESIAN_POINT('',(0.00500246184955876,-0.00445874857871678,0.05860000000001));
#107708=CARTESIAN_POINT('Origin',(0.00712378219310841,-0.00233742823514713,
0.0998391810594235));
#107709=CARTESIAN_POINT('',(0.0041237821931084,-0.00233742823514714,0.0586));
#107710=CARTESIAN_POINT('',(0.0041237821931184,-0.00233742823515713,0.0998391810594335));
#107711=CARTESIAN_POINT('Origin',(0.00712378219311841,-0.00233742823515713,
0.05860000000001));
#107712=CARTESIAN_POINT('Origin',(0.00412378219310839,0.00227581852803816,
0.0998391810594235));
#107713=CARTESIAN_POINT('',(0.0041237821931084,0.00227581852803816,0.0586));
#107714=CARTESIAN_POINT('',(0.0041237821931184,0.00227581852804816,0.0998391810594335));
#107715=CARTESIAN_POINT('',(0.00412378219311839,0.00227581852804816,0.05860000000001));
#107716=CARTESIAN_POINT('Origin',(-0.0031262178068916,0.00227581852803817,
0.0998391810594235));
#107717=CARTESIAN_POINT('',(0.00244204416552777,0.00691876571775598,0.0586));
#107718=CARTESIAN_POINT('',(0.00244204416553777,0.00691876571776598,0.0998391810594335));
#107719=CARTESIAN_POINT('Origin',(-0.00312621780690161,0.00227581852804816,
0.05860000000001));
#107720=CARTESIAN_POINT('Origin',(0.00244204416552777,0.00691876571775598,
0.0998391810594235));
#107721=CARTESIAN_POINT('',(0.00180163765660117,0.00768680185188279,0.0586));
#107722=CARTESIAN_POINT('',(0.00180163765661117,0.00768680185189279,0.0998391810594335));
#107723=CARTESIAN_POINT('',(0.00244204416553777,0.00691876571776598,0.05860000000001));
#107724=CARTESIAN_POINT('Origin',(0.0048737821931084,0.0102484278875892,
0.0998391810594235));
#107725=CARTESIAN_POINT('',(0.000873782193108401,0.0102484278875892,0.0586));
#107726=CARTESIAN_POINT('',(0.000873782193118401,0.0102484278875992,0.0998391810594335));
#107727=CARTESIAN_POINT('Origin',(0.0048737821931184,0.0102484278875992,
0.05860000000001));
#107728=CARTESIAN_POINT('Origin',(0.000873782193108408,0.0185258185280382,
0.0998391810594235));
#107729=CARTESIAN_POINT('',(0.000873782193108408,0.0156922263930369,0.0586));
#107730=CARTESIAN_POINT('',(0.000873782193118408,0.0156922263930469,0.05860000000001));
#107731=CARTESIAN_POINT('',(0.000873782193118408,0.0185258185280481,0.05860000000001));
#107732=CARTESIAN_POINT('Origin',(-0.0031262178068916,0.00227581852803817,
0.0586));
#107733=CARTESIAN_POINT('',(-0.00327621780689159,0.0162750149335466,0.0586));
#107734=CARTESIAN_POINT('',(-0.0032762178069016,0.0162750149335566,0.05860000000001));
#107735=CARTESIAN_POINT('Origin',(-0.00312621780690161,0.00227581852804816,
0.05860000000001));
#107736=CARTESIAN_POINT('Origin',(-0.0031262178068916,0.00227581852803817,
0.0586));
#107737=CARTESIAN_POINT('',(-0.0032762178069016,0.0177758185280482,0.05860000000001));
#107738=CARTESIAN_POINT('',(-0.00647621780690159,0.0177758185280482,0.05860000000001));
#107739=CARTESIAN_POINT('Origin',(-0.00327621780689159,0.0177758185280382,
0.0586));
#107740=CARTESIAN_POINT('Origin',(-0.00647621780689159,0.0177758185280382,
0.0586));
#107741=CARTESIAN_POINT('Origin',(-0.00681722270126977,0.0209258185280382,
0.0566));
#107742=CARTESIAN_POINT('',(-0.0339352129125134,0.0209258185280382,0.0655));
#107743=CARTESIAN_POINT('',(-0.00681722270127977,0.0209258185280481,0.06550000000001));
#107744=CARTESIAN_POINT('',(-0.0339352129125234,0.0209258185280481,0.05660000000001));
#107745=CARTESIAN_POINT('Origin',(-0.0358762178068916,0.0177758185280382,
0.0566));
#107746=CARTESIAN_POINT('',(-0.0390262178068916,0.01583481363366,0.0655));
#107747=CARTESIAN_POINT('Origin',(-0.0358762178069016,0.0177758185280482,
0.06550000000001));
#107748=CARTESIAN_POINT('',(-0.0390262178069016,0.01583481363367,0.05660000000001));
#107749=CARTESIAN_POINT('Origin',(-0.0390262178068916,0.01583481363366,
0.0566));
#107750=CARTESIAN_POINT('',(-0.0390262178068916,-0.0112831765775837,0.0655));
#107751=CARTESIAN_POINT('',(-0.0390262178069016,0.01583481363367,0.06550000000001));
#107752=CARTESIAN_POINT('',(-0.0390262178069016,-0.0112831765775937,0.05660000000001));
#107753=CARTESIAN_POINT('Origin',(-0.0358762178068916,-0.0132241814719618,
0.0566));
#107754=CARTESIAN_POINT('Origin',(-0.0358762178069016,-0.0132241814719718,
0.06550000000001));
#107755=CARTESIAN_POINT('Origin',(0.00785982116242948,-0.0163741814719618,
0.0566));
#107756=CARTESIAN_POINT('',(0.0100237821931084,-0.0142102204412829,0.06075));
#107757=CARTESIAN_POINT('',(0.0100237821931084,-0.0142102204412829,0.0565441125496954));
#107758=CARTESIAN_POINT('',(0.0100237821931184,-0.0142102204412929,0.05660000000001));
#107759=CARTESIAN_POINT('',(0.00859977065610065,-0.0156342319783106,0.0551201010126877));
#107760=CARTESIAN_POINT('',(0.0100237821931184,-0.0142102204412929,0.06075000000001));
#107761=CARTESIAN_POINT('Origin',(0.0100237821931084,-0.0142102204412829,
0.0566));
#107762=CARTESIAN_POINT('',(0.0100237821931084,-0.0123084960470126,0.06075));
#107763=CARTESIAN_POINT('',(0.0100237821931084,-0.0123084960470126,0.0565441125496954));
#107764=CARTESIAN_POINT('',(0.0100237821931184,-0.0123084960470226,0.05660000000001));
#107765=CARTESIAN_POINT('',(0.0100237821931184,-0.0142102204412929,0.0565441125497054));
#107766=CARTESIAN_POINT('',(0.0100237821931184,-0.0123084960470226,0.06075000000001));
#107767=CARTESIAN_POINT('Origin',(0.0100237821931084,-0.0123084960470126,
0.0566));
#107768=CARTESIAN_POINT('',(0.0100424113432199,-0.0123271251971241,0.056562741699807));
#107769=CARTESIAN_POINT('',(0.00719958354106424,-0.00948429739496843,0.06075));
#107770=CARTESIAN_POINT('',(0.00719958354107424,-0.00948429739497843,0.06075000000001));
#107771=CARTESIAN_POINT('',(0.00719958354107424,-0.00948429739497843,0.06075000000001));
#107772=CARTESIAN_POINT('',(0.00358824828718567,-0.00587296214108986,0.05660000000001));
#107773=CARTESIAN_POINT('Origin',(0.00712378219310841,-0.00233742823514713,
0.0566));
#107774=CARTESIAN_POINT('',(0.0021237821931184,-0.00233742823515713,0.05660000000001));
#107775=CARTESIAN_POINT('Origin',(0.0021237821931084,0.00227581852803816,
0.0566));
#107776=CARTESIAN_POINT('',(0.0021237821931184,0.00227581852804816,0.05660000000001));
#107777=CARTESIAN_POINT('Origin',(-0.00312621780689159,0.00227581852803816,
0.0566));
#107778=CARTESIAN_POINT('',(0.000905971897284149,0.00563795269991278,0.05660000000001));
#107779=CARTESIAN_POINT('Origin',(0.000905971897274156,0.00563795269990278,
0.0566));
#107780=CARTESIAN_POINT('',(0.000282704463422255,0.00638543403209472,0.05660000000001));
#107781=CARTESIAN_POINT('Origin',(0.00527877065165022,0.0105512709814273,
0.0566));
#107782=CARTESIAN_POINT('',(-0.0012262178069016,0.0105512709814373,0.05660000000001));
#107783=CARTESIAN_POINT('Origin',(-0.0012262178068916,0.0105512709814273,
0.0566));
#107784=CARTESIAN_POINT('Origin',(0.0121237821931084,0.0230258185280382,
0.0586441125496955));
#107785=CARTESIAN_POINT('Origin',(-0.0186262178068916,-0.0128741814719618,
0.0450676623509137));
#107786=CARTESIAN_POINT('Origin',(-0.0186262178069016,-0.0128741814719718,
0.06150000000001));
#107787=CARTESIAN_POINT('Origin',(-0.00487621780689159,0.0177758185280382,
0.0566));
#107788=CARTESIAN_POINT('Origin',(-0.0203762178068916,0.00227581852803817,
0.0615));
#107789=CARTESIAN_POINT('',(-0.0256278910010042,-0.0101608180213908,0.06150000000001));
#107790=CARTESIAN_POINT('Origin',(-0.0203762178068916,0.00227581852803817,
0.0737));
#107791=CARTESIAN_POINT('Origin',(-0.0203762178068916,0.00227581852803817,
0.0862));
#107792=CARTESIAN_POINT('Origin',(-0.00487621780689159,0.0177758185280382,
0.0566));
#107793=CARTESIAN_POINT('Origin',(-0.0266262178068916,0.0142758185280382,
0.08775));
#107794=CARTESIAN_POINT('',(-0.0266262178068916,0.0142758185280382,0.08775));
#107795=CARTESIAN_POINT('',(-0.0266262178069016,0.0142758185280482,0.08775000000001));
#107796=CARTESIAN_POINT('',(-0.0246762178068916,0.0202758185280381,0.08775));
#107797=CARTESIAN_POINT('',(-0.0266262178069016,0.0142758185280482,0.08775000000001));
#107798=CARTESIAN_POINT('',(-0.0246762178069016,0.0202758185280481,0.08775000000001));
#107799=CARTESIAN_POINT('Origin',(-0.0246762178068916,0.0202758185280381,
0.08775));
#107800=CARTESIAN_POINT('',(-0.0166762178068916,0.0202758185280381,0.08775));
#107801=CARTESIAN_POINT('',(-0.0246762178069016,0.0202758185280481,0.08775000000001));
#107802=CARTESIAN_POINT('',(-0.0166762178069016,0.0202758185280481,0.08775000000001));
#107803=CARTESIAN_POINT('Origin',(-0.0166762178068916,0.0202758185280381,
0.08775));
#107804=CARTESIAN_POINT('',(-0.0147262178068916,0.0142758185280382,0.08775));
#107805=CARTESIAN_POINT('',(-0.0166762178069016,0.0202758185280481,0.08775000000001));
#107806=CARTESIAN_POINT('',(-0.0147262178069016,0.0142758185280482,0.08775000000001));
#107807=CARTESIAN_POINT('Origin',(-0.0147262178068916,0.0142758185280382,
0.08775));
#107808=CARTESIAN_POINT('',(-0.0147262178068916,-0.00972418147196183,0.08775));
#107809=CARTESIAN_POINT('',(-0.0147262178069016,0.0142758185280482,0.08775000000001));
#107810=CARTESIAN_POINT('',(-0.0147262178069016,-0.00972418147197183,0.08775000000001));
#107811=CARTESIAN_POINT('Origin',(-0.0147262178068916,-0.00972418147196183,
0.08775));
#107812=CARTESIAN_POINT('',(-0.0166762178068916,-0.0157241814719619,0.08775));
#107813=CARTESIAN_POINT('',(-0.0147262178069016,-0.00972418147197183,0.08775000000001));
#107814=CARTESIAN_POINT('',(-0.0166762178069016,-0.0157241814719719,0.08775000000001));
#107815=CARTESIAN_POINT('Origin',(-0.0166762178068916,-0.0157241814719619,
0.08775));
#107816=CARTESIAN_POINT('',(-0.0246762178068916,-0.0157241814719619,0.08775));
#107817=CARTESIAN_POINT('',(-0.0166762178069016,-0.0157241814719719,0.08775000000001));
#107818=CARTESIAN_POINT('',(-0.0246762178069016,-0.0157241814719719,0.08775000000001));
#107819=CARTESIAN_POINT('Origin',(-0.0246762178068916,-0.0157241814719619,
0.08775));
#107820=CARTESIAN_POINT('',(-0.0266262178068916,-0.00972418147196183,0.08775));
#107821=CARTESIAN_POINT('',(-0.0246762178069016,-0.0157241814719719,0.08775000000001));
#107822=CARTESIAN_POINT('',(-0.0266262178069016,-0.00972418147197183,0.08775000000001));
#107823=CARTESIAN_POINT('Origin',(-0.0266262178068916,-0.00972418147196183,
0.08775));
#107824=CARTESIAN_POINT('',(-0.0266262178069016,-0.00972418147197183,0.08775000000001));
#107825=CARTESIAN_POINT('Origin',(-0.0411262178068916,-0.0184741814719619,
0.08775));
#107826=CARTESIAN_POINT('Origin',(-0.00312621780689159,0.00227581852803817,
0.06075));
#107827=CARTESIAN_POINT('Origin',(-0.0031262178069016,0.00227581852804816,
0.06075000000001));
#107828=CARTESIAN_POINT('Origin',(-0.00312621780689159,0.00227581852803817,
0.06075));
#107829=CARTESIAN_POINT('Origin',(-0.0256278910009942,-0.0101608180213808,
0.0655));
#107830=CARTESIAN_POINT('',(-0.0311262178068916,-0.0147744620163014,0.0655));
#107831=CARTESIAN_POINT('',(-0.0256278910010042,-0.0101608180213908,0.06550000000001));
#107832=CARTESIAN_POINT('',(-0.0311262178068916,-0.0147744620163014,0.06355));
#107833=CARTESIAN_POINT('',(-0.0311262178069016,-0.0147744620163114,0.06550000000001));
#107834=CARTESIAN_POINT('',(-0.0307683573893888,-0.0144741814719618,0.06355));
#107835=CARTESIAN_POINT('',(-0.0256278910010042,-0.0101608180213908,0.06355000000001));
#107836=CARTESIAN_POINT('',(-0.0307683573893888,-0.0144741814719618,0.0655));
#107837=CARTESIAN_POINT('',(-0.0307683573893988,-0.0144741814719718,0.06550000000001));
#107838=CARTESIAN_POINT('',(-0.0256278910010042,-0.0101608180213908,0.06550000000001));
#107839=CARTESIAN_POINT('Origin',(-0.00312621780689159,0.00227581852803817,
0.0655));
#107840=CARTESIAN_POINT('Origin',(-0.0031262178069016,0.00227581852804816,
0.06550000000001));
#107841=CARTESIAN_POINT('Origin',(-0.00487621780689159,0.0177758185280382,
0.0655));
#107842=CARTESIAN_POINT('',(-0.0311262178068916,-0.0144741814719618,0.0655));
#107843=CARTESIAN_POINT('',(-0.0311262178069016,0.0177758185280482,0.06550000000001));
#107844=CARTESIAN_POINT('',(-0.00487621780690158,-0.0144741814719718,0.06550000000001));
#107845=CARTESIAN_POINT('Origin',(0.0121237821931084,-0.0144741814719618,
0.0829760869565217));
#107846=CARTESIAN_POINT('Origin',(0.0021237821931084,-0.0144741814719618,
0.06355));
#107847=CARTESIAN_POINT('Origin',(-0.0311262178068916,-0.0184741814719619,
0.0578931457505076));
#107848=CARTESIAN_POINT('',(-0.0171262178069015,-0.00447418147197182,0.0326378260227564));
#107849=CARTESIAN_POINT('Origin',(-0.0311262178068916,-0.0144741814719618,
0.06355));
#107850=CARTESIAN_POINT('',(-0.0311262178068916,-0.0144741814719618,0.06355));
#107851=CARTESIAN_POINT('',(-0.0311262178069016,-0.0144741814719718,0.06355000000001));
#107852=CARTESIAN_POINT('',(-0.0271262178069016,-0.0144741814719718,0.06355000000001));
#107853=CARTESIAN_POINT('Origin',(-0.0311262178068916,-0.0144741814719618,
0.0578931457505076));
#107854=CARTESIAN_POINT('',(-0.0311262178069016,-0.0144741814719718,0.0578931457505176));
#107855=CARTESIAN_POINT('Origin',(-0.0271262178068916,-0.0144741814719618,
0.0578931457505076));
#107856=CARTESIAN_POINT('Origin',(-0.0171262178068915,-0.00447418147196182,
0.0326378260227464));
#107857=CARTESIAN_POINT('',(0.0021237821931184,-0.00447418147197182,0.0326378260227564));
#107858=CARTESIAN_POINT('Origin',(0.0021237821931084,-0.00447418147196182,
0.0326378260227464));
#107859=CARTESIAN_POINT('Origin',(-0.0286262178068916,-0.00152418147196182,
0.071));
#107860=CARTESIAN_POINT('Origin',(-0.0381262178068916,-0.00152418147196182,
0.071));
#107861=CARTESIAN_POINT('',(-0.0381262178068916,0.00247581852803818,0.0834721359549996));
#107862=CARTESIAN_POINT('',(-0.0381262178068916,-0.00552418147196183,0.0834721359549996));
#107863=CARTESIAN_POINT('Origin',(-0.0381262178069016,-0.00152418147197183,
0.07900000000001));
#107864=CARTESIAN_POINT('',(-0.0381262178069016,0.00247581852804817,0.0819282032302855));
#107865=CARTESIAN_POINT('',(-0.0381262178069016,-0.00552418147197183,0.0859282032302855));
#107866=CARTESIAN_POINT('Origin',(-0.0411262178068916,-0.00152418147196182,
0.079));
#107867=CARTESIAN_POINT('',(-0.0321262178068916,0.00247581852803818,0.0834721359549996));
#107868=CARTESIAN_POINT('',(-0.0321262178068916,-0.00552418147196183,0.0834721359549996));
#107869=CARTESIAN_POINT('Origin',(-0.0321262178069016,-0.00152418147197183,
0.07900000000001));
#107870=CARTESIAN_POINT('',(-0.0411262178069016,0.00247581852804817,0.0834721359550096));
#107871=CARTESIAN_POINT('',(-0.0411262178069016,-0.00552418147197183,0.0834721359550096));
#107872=CARTESIAN_POINT('Origin',(-0.0321262178068916,-0.00152418147196182,
0.073));
#107873=CARTESIAN_POINT('',(-0.0321262178069016,0.00247581852804817,0.0819282032302855));
#107874=CARTESIAN_POINT('',(-0.0321262178069016,-0.00552418147197183,0.0859282032302855));
#107875=CARTESIAN_POINT('Origin',(0.0161247821931084,0.00247581852803818,
0.0819282032302755));
#107876=CARTESIAN_POINT('Origin',(0.0161247821931084,-0.00552418147196183,
0.0859282032302755));
#107877=CARTESIAN_POINT('',(0.120851271727423,0.210418128641714,0.192855924679756));
#107878=CARTESIAN_POINT('',(0.120851271727423,0.210418128641714,0.192855924679756));
#107879=CARTESIAN_POINT('',(0.120851271727423,0.210418128641714,0.192855924679756));
#107880=CARTESIAN_POINT('',(0.120851271727423,0.210418128641714,0.192855924679756));
#107881=CARTESIAN_POINT('',(0.120851271727423,0.210418128641714,0.192855924679756));
#107882=CARTESIAN_POINT('',(0.120851271727423,0.210418128641714,0.192855924679756));
#107883=CARTESIAN_POINT('',(0.120851271727423,0.210418128641714,0.192855924679756));
#107884=CARTESIAN_POINT('',(0.120851271727423,0.210418128641714,0.192855924679756));
#107885=CARTESIAN_POINT('',(0.120851271727423,0.210418128641714,0.192855924679756));
#107886=CARTESIAN_POINT('',(0.120851271727423,0.210418128641714,0.192855924679756));
#107887=UNCERTAINTY_MEASURE_WITH_UNIT(LENGTH_MEASURE(1.E-5),#107911,
'DISTANCE_ACCURACY_VALUE',
'Maximum model space distance between geometric entities at asserted c
onnectivities');
#107888=UNCERTAINTY_MEASURE_WITH_UNIT(LENGTH_MEASURE(1.E-5),#107911,
'DISTANCE_ACCURACY_VALUE',
'Maximum model space distance between geometric entities at asserted c
onnectivities');
#107889=UNCERTAINTY_MEASURE_WITH_UNIT(LENGTH_MEASURE(1.E-5),#107911,
'DISTANCE_ACCURACY_VALUE',
'Maximum model space distance between geometric entities at asserted c
onnectivities');
#107890=UNCERTAINTY_MEASURE_WITH_UNIT(LENGTH_MEASURE(1.E-5),#107911,
'DISTANCE_ACCURACY_VALUE',
'Maximum model space distance between geometric entities at asserted c
onnectivities');
#107891=UNCERTAINTY_MEASURE_WITH_UNIT(LENGTH_MEASURE(1.E-5),#107911,
'DISTANCE_ACCURACY_VALUE',
'Maximum model space distance between geometric entities at asserted c
onnectivities');
#107892=UNCERTAINTY_MEASURE_WITH_UNIT(LENGTH_MEASURE(1.E-5),#107911,
'DISTANCE_ACCURACY_VALUE',
'Maximum model space distance between geometric entities at asserted c
onnectivities');
#107893=UNCERTAINTY_MEASURE_WITH_UNIT(LENGTH_MEASURE(1.E-5),#107911,
'DISTANCE_ACCURACY_VALUE',
'Maximum model space distance between geometric entities at asserted c
onnectivities');
#107894=UNCERTAINTY_MEASURE_WITH_UNIT(LENGTH_MEASURE(1.E-5),#107911,
'DISTANCE_ACCURACY_VALUE',
'Maximum model space distance between geometric entities at asserted c
onnectivities');
#107895=UNCERTAINTY_MEASURE_WITH_UNIT(LENGTH_MEASURE(1.E-5),#107911,
'DISTANCE_ACCURACY_VALUE',
'Maximum model space distance between geometric entities at asserted c
onnectivities');
#107896=UNCERTAINTY_MEASURE_WITH_UNIT(LENGTH_MEASURE(1.E-5),#107911,
'DISTANCE_ACCURACY_VALUE',
'Maximum model space distance between geometric entities at asserted c
onnectivities');
#107897=UNCERTAINTY_MEASURE_WITH_UNIT(LENGTH_MEASURE(1.E-5),#107911,
'DISTANCE_ACCURACY_VALUE',
'Maximum model space distance between geometric entities at asserted c
onnectivities');
#107898=UNCERTAINTY_MEASURE_WITH_UNIT(LENGTH_MEASURE(1.E-5),#107911,
'DISTANCE_ACCURACY_VALUE',
'Maximum model space distance between geometric entities at asserted c
onnectivities');
#107899=(
GEOMETRIC_REPRESENTATION_CONTEXT(3)
GLOBAL_UNCERTAINTY_ASSIGNED_CONTEXT((#107887))
GLOBAL_UNIT_ASSIGNED_CONTEXT((#107911,#107912,#107913))
REPRESENTATION_CONTEXT('','3D')
);
#107900=(
GEOMETRIC_REPRESENTATION_CONTEXT(3)
GLOBAL_UNCERTAINTY_ASSIGNED_CONTEXT((#107888))
GLOBAL_UNIT_ASSIGNED_CONTEXT((#107911,#107912,#107913))
REPRESENTATION_CONTEXT('','3D')
);
#107901=(
GEOMETRIC_REPRESENTATION_CONTEXT(3)
GLOBAL_UNCERTAINTY_ASSIGNED_CONTEXT((#107889))
GLOBAL_UNIT_ASSIGNED_CONTEXT((#107911,#107912,#107913))
REPRESENTATION_CONTEXT('','3D')
);
#107902=(
GEOMETRIC_REPRESENTATION_CONTEXT(3)
GLOBAL_UNCERTAINTY_ASSIGNED_CONTEXT((#107890))
GLOBAL_UNIT_ASSIGNED_CONTEXT((#107911,#107912,#107913))
REPRESENTATION_CONTEXT('','3D')
);
#107903=(
GEOMETRIC_REPRESENTATION_CONTEXT(3)
GLOBAL_UNCERTAINTY_ASSIGNED_CONTEXT((#107891))
GLOBAL_UNIT_ASSIGNED_CONTEXT((#107911,#107912,#107913))
REPRESENTATION_CONTEXT('','3D')
);
#107904=(
GEOMETRIC_REPRESENTATION_CONTEXT(3)
GLOBAL_UNCERTAINTY_ASSIGNED_CONTEXT((#107892))
GLOBAL_UNIT_ASSIGNED_CONTEXT((#107911,#107912,#107913))
REPRESENTATION_CONTEXT('','3D')
);
#107905=(
GEOMETRIC_REPRESENTATION_CONTEXT(3)
GLOBAL_UNCERTAINTY_ASSIGNED_CONTEXT((#107893))
GLOBAL_UNIT_ASSIGNED_CONTEXT((#107911,#107912,#107913))
REPRESENTATION_CONTEXT('','3D')
);
#107906=(
GEOMETRIC_REPRESENTATION_CONTEXT(3)
GLOBAL_UNCERTAINTY_ASSIGNED_CONTEXT((#107894))
GLOBAL_UNIT_ASSIGNED_CONTEXT((#107911,#107912,#107913))
REPRESENTATION_CONTEXT('','3D')
);
#107907=(
GEOMETRIC_REPRESENTATION_CONTEXT(3)
GLOBAL_UNCERTAINTY_ASSIGNED_CONTEXT((#107895))
GLOBAL_UNIT_ASSIGNED_CONTEXT((#107911,#107912,#107913))
REPRESENTATION_CONTEXT('','3D')
);
#107908=(
GEOMETRIC_REPRESENTATION_CONTEXT(3)
GLOBAL_UNCERTAINTY_ASSIGNED_CONTEXT((#107896))
GLOBAL_UNIT_ASSIGNED_CONTEXT((#107911,#107912,#107913))
REPRESENTATION_CONTEXT('','3D')
);
#107909=(
GEOMETRIC_REPRESENTATION_CONTEXT(3)
GLOBAL_UNCERTAINTY_ASSIGNED_CONTEXT((#107897))
GLOBAL_UNIT_ASSIGNED_CONTEXT((#107911,#107912,#107913))
REPRESENTATION_CONTEXT('','3D')
);
#107910=(
GEOMETRIC_REPRESENTATION_CONTEXT(3)
GLOBAL_UNCERTAINTY_ASSIGNED_CONTEXT((#107898))
GLOBAL_UNIT_ASSIGNED_CONTEXT((#107911,#107912,#107913))
REPRESENTATION_CONTEXT('','3D')
);
#107911=(
LENGTH_UNIT()
NAMED_UNIT(*)
SI_UNIT($,.METRE.)
);
#107912=(
NAMED_UNIT(*)
PLANE_ANGLE_UNIT()
SI_UNIT($,.RADIAN.)
);
#107913=(
NAMED_UNIT(*)
SI_UNIT($,.STERADIAN.)
SOLID_ANGLE_UNIT()
);
#107914=SHAPE_DEFINITION_REPRESENTATION(#107925,#107946);
#107915=SHAPE_DEFINITION_REPRESENTATION(#107926,#107947);
#107916=SHAPE_DEFINITION_REPRESENTATION(#107927,#107948);
#107917=SHAPE_DEFINITION_REPRESENTATION(#107928,#107949);
#107918=SHAPE_DEFINITION_REPRESENTATION(#107929,#107950);
#107919=SHAPE_DEFINITION_REPRESENTATION(#107930,#107951);
#107920=SHAPE_DEFINITION_REPRESENTATION(#107931,#107952);
#107921=SHAPE_DEFINITION_REPRESENTATION(#107932,#107953);
#107922=SHAPE_DEFINITION_REPRESENTATION(#107933,#107954);
#107923=SHAPE_DEFINITION_REPRESENTATION(#107934,#107955);
#107924=SHAPE_DEFINITION_REPRESENTATION(#107935,#107956);
#107925=PRODUCT_DEFINITION_SHAPE('',$,#107958);
#107926=PRODUCT_DEFINITION_SHAPE('',$,#107959);
#107927=PRODUCT_DEFINITION_SHAPE('',$,#107960);
#107928=PRODUCT_DEFINITION_SHAPE('',$,#107961);
#107929=PRODUCT_DEFINITION_SHAPE('',$,#107962);
#107930=PRODUCT_DEFINITION_SHAPE('',$,#107963);
#107931=PRODUCT_DEFINITION_SHAPE('',$,#107964);
#107932=PRODUCT_DEFINITION_SHAPE('',$,#107965);
#107933=PRODUCT_DEFINITION_SHAPE('',$,#107966);
#107934=PRODUCT_DEFINITION_SHAPE('',$,#107967);
#107935=PRODUCT_DEFINITION_SHAPE('',$,#107968);
#107936=PRODUCT_DEFINITION_SHAPE($,$,#41);
#107937=PRODUCT_DEFINITION_SHAPE($,$,#42);
#107938=PRODUCT_DEFINITION_SHAPE($,$,#43);
#107939=PRODUCT_DEFINITION_SHAPE($,$,#44);
#107940=PRODUCT_DEFINITION_SHAPE($,$,#45);
#107941=PRODUCT_DEFINITION_SHAPE($,$,#46);
#107942=PRODUCT_DEFINITION_SHAPE($,$,#47);
#107943=PRODUCT_DEFINITION_SHAPE($,$,#48);
#107944=PRODUCT_DEFINITION_SHAPE($,$,#49);
#107945=PRODUCT_DEFINITION_SHAPE($,$,#50);
#107946=SHAPE_REPRESENTATION('',(#45658,#50366,#50367,#50368,#50369,#50370,
#50371,#50372,#50373,#50374,#50375),#107899);
#107947=SHAPE_REPRESENTATION('',(#45659),#107900);
#107948=SHAPE_REPRESENTATION('',(#45668),#107901);
#107949=SHAPE_REPRESENTATION('',(#45671),#107902);
#107950=SHAPE_REPRESENTATION('',(#45680),#107903);
#107951=SHAPE_REPRESENTATION('',(#45688),#107904);
#107952=SHAPE_REPRESENTATION('',(#45717),#107905);
#107953=SHAPE_REPRESENTATION('',(#49877),#107906);
#107954=SHAPE_REPRESENTATION('',(#49890),#107907);
#107955=SHAPE_REPRESENTATION('',(#49899),#107908);
#107956=SHAPE_REPRESENTATION('',(#50173),#107909);
#107957=PRODUCT_DEFINITION_CONTEXT('part definition',#107992,'design');
#107958=PRODUCT_DEFINITION('MAT-068','MAT-068',#107969,
#107957);
#107959=PRODUCT_DEFINITION('Washer','Washer',#107970,#107957);
#107960=PRODUCT_DEFINITION('Tension Spring','Tension Spring',#107971,#107957);
#107961=PRODUCT_DEFINITION('Pivot Pin','Pivot Pin',#107972,#107957);
#107962=PRODUCT_DEFINITION('Idler Shaft','Idler Shaft',#107973,#107957);
#107963=PRODUCT_DEFINITION('Lever','Lever',#107974,#107957);
#107964=PRODUCT_DEFINITION('Tensioner','Tensioner',#107975,#107957);
#107965=PRODUCT_DEFINITION('Filament Inlet','filament inlet',#107976,#107957);
#107966=PRODUCT_DEFINITION('Spacer','Spacer',#107977,#107957);
#107967=PRODUCT_DEFINITION('Gear','Gear',#107978,#107957);
#107968=PRODUCT_DEFINITION('Extruder Body','Extruder Body',#107979,#107957);
#107969=PRODUCT_DEFINITION_FORMATION('',$,#107994);
#107970=PRODUCT_DEFINITION_FORMATION('',$,#107995);
#107971=PRODUCT_DEFINITION_FORMATION('',$,#107996);
#107972=PRODUCT_DEFINITION_FORMATION('',$,#107997);
#107973=PRODUCT_DEFINITION_FORMATION('',$,#107998);
#107974=PRODUCT_DEFINITION_FORMATION('',$,#107999);
#107975=PRODUCT_DEFINITION_FORMATION('',$,#108000);
#107976=PRODUCT_DEFINITION_FORMATION('',$,#108001);
#107977=PRODUCT_DEFINITION_FORMATION('',$,#108002);
#107978=PRODUCT_DEFINITION_FORMATION('',$,#108003);
#107979=PRODUCT_DEFINITION_FORMATION('',$,#108004);
#107980=PRODUCT_RELATED_PRODUCT_CATEGORY('MAT-068',
'MAT-068',(#107994));
#107981=PRODUCT_RELATED_PRODUCT_CATEGORY('Washer','Washer',(#107995));
#107982=PRODUCT_RELATED_PRODUCT_CATEGORY('Tension Spring',
'Tension Spring',(#107996));
#107983=PRODUCT_RELATED_PRODUCT_CATEGORY('Pivot Pin','Pivot Pin',(#107997));
#107984=PRODUCT_RELATED_PRODUCT_CATEGORY('Idler Shaft','Idler Shaft',(#107998));
#107985=PRODUCT_RELATED_PRODUCT_CATEGORY('Lever','Lever',(#107999));
#107986=PRODUCT_RELATED_PRODUCT_CATEGORY('Tensioner','Tensioner',(#108000));
#107987=PRODUCT_RELATED_PRODUCT_CATEGORY('filament inlet',
'filament inlet',(#108001));
#107988=PRODUCT_RELATED_PRODUCT_CATEGORY('Spacer','Spacer',(#108002));
#107989=PRODUCT_RELATED_PRODUCT_CATEGORY('Gear','Gear',(#108003));
#107990=PRODUCT_RELATED_PRODUCT_CATEGORY('Extruder Body',
'Extruder Body',(#108004));
#107991=APPLICATION_PROTOCOL_DEFINITION('international standard',
'ap242_managed_model_based_3d_engineering',2011,#107992);
#107992=APPLICATION_CONTEXT('Managed model based 3d engineering');
#107993=PRODUCT_CONTEXT('part definition',#107992,'mechanical');
#107994=PRODUCT('MAT-068','MAT-068',
'LEGAL AND USAGE DISCLAIMER: this Data/Model is provided \X2\201C\X0\A
S IS\X2\201D\X0\ for informational and representational only. It is a 
geometric approximation and is NOT engineered, certified, or guarantee
d for dimensional accuracy, exact tolerances, or production-level prec
ision. Vendor disclaims all implied warranties including fitness for a
 particular purpose. DO NOT USE FOR DIRECT PHYSICAL MANUFACTURING, AUT
OMATED PRODUCTION, OR SAFETY-CRITICAL SYSTEMS without independent engi
neering verification and resolution of any design discrepancies.',(#107993));
#107995=PRODUCT('Washer','Washer',
'LEGAL AND USAGE DISCLAIMER: this Data/Model is provided \X2\201C\X0\A
S IS\X2\201D\X0\ for informational and representational only. It is a 
geometric approximation and is NOT engineered, certified, or guarantee
d for dimensional accuracy, exact tolerances, or production-level prec
ision. Vendor disclaims all implied warranties including fitness for a
 particular purpose. DO NOT USE FOR DIRECT PHYSICAL MANUFACTURING, AUT
OMATED PRODUCTION, OR SAFETY-CRITICAL SYSTEMS without independent engi
neering verification and resolution of any design discrepancies.',(#107993));
#107996=PRODUCT('Tension Spring','Tension Spring',
'LEGAL AND USAGE DISCLAIMER: this Data/Model is provided \X2\201C\X0\A
S IS\X2\201D\X0\ for informational and representational only. It is a 
geometric approximation and is NOT engineered, certified, or guarantee
d for dimensional accuracy, exact tolerances, or production-level prec
ision. Vendor disclaims all implied warranties including fitness for a
 particular purpose. DO NOT USE FOR DIRECT PHYSICAL MANUFACTURING, AUT
OMATED PRODUCTION, OR SAFETY-CRITICAL SYSTEMS without independent engi
neering verification and resolution of any design discrepancies.',(#107993));
#107997=PRODUCT('Pivot Pin','Pivot Pin',
'LEGAL AND USAGE DISCLAIMER: this Data/Model is provided \X2\201C\X0\A
S IS\X2\201D\X0\ for informational and representational only. It is a 
geometric approximation and is NOT engineered, certified, or guarantee
d for dimensional accuracy, exact tolerances, or production-level prec
ision. Vendor disclaims all implied warranties including fitness for a
 particular purpose. DO NOT USE FOR DIRECT PHYSICAL MANUFACTURING, AUT
OMATED PRODUCTION, OR SAFETY-CRITICAL SYSTEMS without independent engi
neering verification and resolution of any design discrepancies.',(#107993));
#107998=PRODUCT('Idler Shaft','Idler Shaft',
'LEGAL AND USAGE DISCLAIMER: this Data/Model is provided \X2\201C\X0\A
S IS\X2\201D\X0\ for informational and representational only. It is a 
geometric approximation and is NOT engineered, certified, or guarantee
d for dimensional accuracy, exact tolerances, or production-level prec
ision. Vendor disclaims all implied warranties including fitness for a
 particular purpose. DO NOT USE FOR DIRECT PHYSICAL MANUFACTURING, AUT
OMATED PRODUCTION, OR SAFETY-CRITICAL SYSTEMS without independent engi
neering verification and resolution of any design discrepancies.',(#107993));
#107999=PRODUCT('Lever','Lever',
'LEGAL AND USAGE DISCLAIMER: this Data/Model is provided \X2\201C\X0\A
S IS\X2\201D\X0\ for informational and representational only. It is a 
geometric approximation and is NOT engineered, certified, or guarantee
d for dimensional accuracy, exact tolerances, or production-level prec
ision. Vendor disclaims all implied warranties including fitness for a
 particular purpose. DO NOT USE FOR DIRECT PHYSICAL MANUFACTURING, AUT
OMATED PRODUCTION, OR SAFETY-CRITICAL SYSTEMS without independent engi
neering verification and resolution of any design discrepancies.',(#107993));
#108000=PRODUCT('Tensioner','Tensioner',
'LEGAL AND USAGE DISCLAIMER: this Data/Model is provided \X2\201C\X0\A
S IS\X2\201D\X0\ for informational and representational only. It is a 
geometric approximation and is NOT engineered, certified, or guarantee
d for dimensional accuracy, exact tolerances, or production-level prec
ision. Vendor disclaims all implied warranties including fitness for a
 particular purpose. DO NOT USE FOR DIRECT PHYSICAL MANUFACTURING, AUT
OMATED PRODUCTION, OR SAFETY-CRITICAL SYSTEMS without independent engi
neering verification and resolution of any design discrepancies.',(#107993));
#108001=PRODUCT('Filament Inlet','filament inlet',
'LEGAL AND USAGE DISCLAIMER: this Data/Model is provided \X2\201C\X0\A
S IS\X2\201D\X0\ for informational and representational only. It is a 
geometric approximation and is NOT engineered, certified, or guarantee
d for dimensional accuracy, exact tolerances, or production-level prec
ision. Vendor disclaims all implied warranties including fitness for a
 particular purpose. DO NOT USE FOR DIRECT PHYSICAL MANUFACTURING, AUT
OMATED PRODUCTION, OR SAFETY-CRITICAL SYSTEMS without independent engi
neering verification and resolution of any design discrepancies.',(#107993));
#108002=PRODUCT('Spacer','Spacer',
'LEGAL AND USAGE DISCLAIMER: this Data/Model is provided \X2\201C\X0\A
S IS\X2\201D\X0\ for informational and representational only. It is a 
geometric approximation and is NOT engineered, certified, or guarantee
d for dimensional accuracy, exact tolerances, or production-level prec
ision. Vendor disclaims all implied warranties including fitness for a
 particular purpose. DO NOT USE FOR DIRECT PHYSICAL MANUFACTURING, AUT
OMATED PRODUCTION, OR SAFETY-CRITICAL SYSTEMS without independent engi
neering verification and resolution of any design discrepancies.',(#107993));
#108003=PRODUCT('Gear','Gear',
'LEGAL AND USAGE DISCLAIMER: this Data/Model is provided \X2\201C\X0\A
S IS\X2\201D\X0\ for informational and representational only. It is a 
geometric approximation and is NOT engineered, certified, or guarantee
d for dimensional accuracy, exact tolerances, or production-level prec
ision. Vendor disclaims all implied warranties including fitness for a
 particular purpose. DO NOT USE FOR DIRECT PHYSICAL MANUFACTURING, AUT
OMATED PRODUCTION, OR SAFETY-CRITICAL SYSTEMS without independent engi
neering verification and resolution of any design discrepancies.',(#107993));
#108004=PRODUCT('Extruder Body','Extruder Body',
'LEGAL AND USAGE DISCLAIMER: this Data/Model is provided \X2\201C\X0\A
S IS\X2\201D\X0\ for informational and representational only. It is a 
geometric approximation and is NOT engineered, certified, or guarantee
d for dimensional accuracy, exact tolerances, or production-level prec
ision. Vendor disclaims all implied warranties including fitness for a
 particular purpose. DO NOT USE FOR DIRECT PHYSICAL MANUFACTURING, AUT
OMATED PRODUCTION, OR SAFETY-CRITICAL SYSTEMS without independent engi
neering verification and resolution of any design discrepancies.',(#107993));
#108005=PRESENTATION_STYLE_ASSIGNMENT((#108012));
#108006=PRESENTATION_STYLE_ASSIGNMENT((#108013));
#108007=PRESENTATION_STYLE_ASSIGNMENT((#108014));
#108008=PRESENTATION_STYLE_ASSIGNMENT((#108015));
#108009=PRESENTATION_STYLE_ASSIGNMENT((#108016));
#108010=PRESENTATION_STYLE_ASSIGNMENT((#108017));
#108011=PRESENTATION_STYLE_ASSIGNMENT((#108018));
#108012=SURFACE_STYLE_USAGE(.BOTH.,#108019);
#108013=SURFACE_STYLE_USAGE(.BOTH.,#108020);
#108014=SURFACE_STYLE_USAGE(.BOTH.,#108021);
#108015=SURFACE_STYLE_USAGE(.BOTH.,#108022);
#108016=SURFACE_STYLE_USAGE(.BOTH.,#108023);
#108017=SURFACE_STYLE_USAGE(.BOTH.,#108024);
#108018=SURFACE_STYLE_USAGE(.BOTH.,#108025);
#108019=SURFACE_SIDE_STYLE('',(#108026));
#108020=SURFACE_SIDE_STYLE('',(#108027));
#108021=SURFACE_SIDE_STYLE('',(#108028));
#108022=SURFACE_SIDE_STYLE('',(#108029));
#108023=SURFACE_SIDE_STYLE('',(#108030));
#108024=SURFACE_SIDE_STYLE('',(#108031));
#108025=SURFACE_SIDE_STYLE('',(#108032));
#108026=SURFACE_STYLE_FILL_AREA(#108033);
#108027=SURFACE_STYLE_FILL_AREA(#108034);
#108028=SURFACE_STYLE_FILL_AREA(#108035);
#108029=SURFACE_STYLE_FILL_AREA(#108036);
#108030=SURFACE_STYLE_FILL_AREA(#108037);
#108031=SURFACE_STYLE_FILL_AREA(#108038);
#108032=SURFACE_STYLE_FILL_AREA(#108039);
#108033=FILL_AREA_STYLE('Steel - Satin',(#108040));
#108034=FILL_AREA_STYLE('Opaque(25,25,25)',(#108041));
#108035=FILL_AREA_STYLE('Opaque(48,59,150)',(#108042));
#108036=FILL_AREA_STYLE('Opaque(246,246,243)',(#108043));
#108037=FILL_AREA_STYLE('Opaque(179,179,179)',(#108044));
#108038=FILL_AREA_STYLE('Opaque(89,149,218)',(#108045));
#108039=FILL_AREA_STYLE('Opaque(137,137,137)',(#108046));
#108040=FILL_AREA_STYLE_COLOUR('Steel - Satin',#108047);
#108041=FILL_AREA_STYLE_COLOUR('Opaque(25,25,25)',#108048);
#108042=FILL_AREA_STYLE_COLOUR('Opaque(48,59,150)',#108049);
#108043=FILL_AREA_STYLE_COLOUR('Opaque(246,246,243)',#108050);
#108044=FILL_AREA_STYLE_COLOUR('Opaque(179,179,179)',#108051);
#108045=FILL_AREA_STYLE_COLOUR('Opaque(89,149,218)',#108052);
#108046=FILL_AREA_STYLE_COLOUR('Opaque(137,137,137)',#108053);
#108047=COLOUR_RGB('Steel - Satin',0.627450980392157,0.627450980392157,
0.627450980392157);
#108048=COLOUR_RGB('Opaque(25,25,25)',0.0980392156862745,0.0980392156862745,
0.0980392156862745);
#108049=COLOUR_RGB('Opaque(48,59,150)',0.188235294117647,0.231372549019608,
0.588235294117647);
#108050=COLOUR_RGB('Opaque(246,246,243)',0.964705882352941,0.964705882352941,
0.952941176470588);
#108051=COLOUR_RGB('Opaque(179,179,179)',0.701960784313725,0.701960784313725,
0.701960784313725);
#108052=COLOUR_RGB('Opaque(89,149,218)',0.349019607843137,0.584313725490196,
0.854901960784314);
#108053=COLOUR_RGB('Opaque(137,137,137)',0.537254901960784,0.537254901960784,
0.537254901960784);
ENDSEC;
END-ISO-10303-21;
